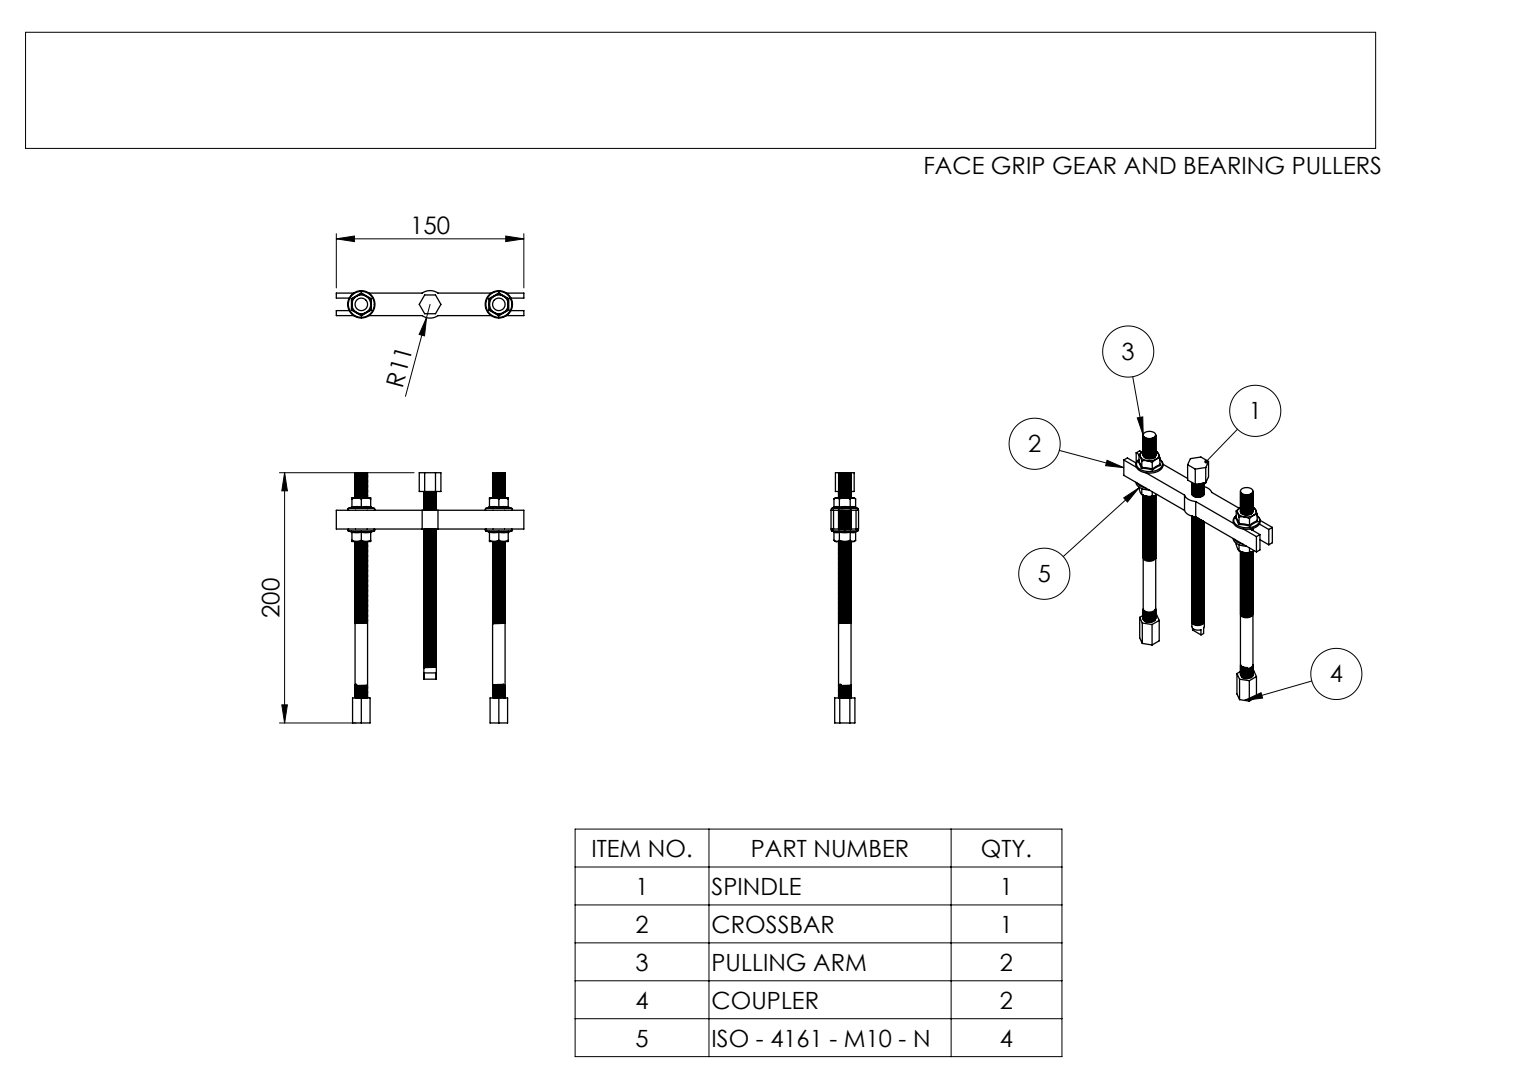
ISO-10303-21;
HEADER;
FILE_DESCRIPTION (('STEP AP214'),
    '1' );
FILE_NAME ('MAS-184',
    '2026-10-25T05:52:03',
    ( '' ),
    ( '' ),
    'SwSTEP 2.0',
    'SolidWorks 2026',
    '' );
FILE_SCHEMA (( 'AUTOMOTIVE_DESIGN' ));
ENDSEC;

DATA;
#1 = CARTESIAN_POINT ( 'NONE',  ( -5.000000000000000888, -163.4375000000000284, 2.071067811865474617 ) ) ;
#2 = AXIS2_PLACEMENT_3D ( 'NONE', #55045, #55372, #11606 ) ;
#3 = CARTESIAN_POINT ( 'NONE',  ( -59.29741812935640155, -128.8750000013656063, -2.196230717870135685 ) ) ;
#4 = ADVANCED_FACE ( 'NONE', ( #1643 ), #54385, .T. ) ;
#5 = CARTESIAN_POINT ( 'NONE',  ( -4.458734124999998549, -12.47916666530107221, 2.574251347313722516 ) ) ;
#6 = CARTESIAN_POINT ( 'NONE',  ( 2.229367062499998831, -45.89583333196774362, -3.861377020970580887 ) ) ;
#7 = ADVANCED_FACE ( 'NONE', ( #40534 ), #45685, .T. ) ;
#8 = ADVANCED_FACE ( 'NONE', ( #45365 ), #55019, .T. ) ;
#9 = CARTESIAN_POINT ( 'NONE',  ( -2.499999999999996447, -7.708333330602144429, 4.330127018922195425 ) ) ;
#10 = CARTESIAN_POINT ( 'NONE',  ( -4.458734124999999437, -146.9375000013656063, -5.460374474430324690E-16 ) ) ;
#11 = CARTESIAN_POINT ( 'NONE',  ( -4.458734124999999437, -91.56249999863440792, 0.000000000000000000 ) ) ;
#12 = CARTESIAN_POINT ( 'NONE',  ( 3.061616997868383141E-16, -166.8750000027312126, -5.000000000000000000 ) ) ;
#13 = ORIENTED_EDGE ( 'NONE', *, *, #42928, .F. ) ;
#14 = CARTESIAN_POINT ( 'NONE',  ( 4.330127018922154569, 30.00000000000000000, -7.499999999999971578 ) ) ;
#15 = CARTESIAN_POINT ( 'NONE',  ( -6.972266317189433020E-16, -69.12499999726880162, -5.000000000000000000 ) ) ;
#16 = CARTESIAN_POINT ( 'NONE',  ( -60.14911071818854538, -150.1875000027311842, 1.666127454062681368 ) ) ;
#17 = CARTESIAN_POINT ( 'NONE',  ( -6.972266317189433020E-16, -38.25000000000000000, -5.000000000000000000 ) ) ;
#18 = EDGE_LOOP ( 'NONE', ( #47508, #46479, #24387, #28082 ) ) ;
#19 = CARTESIAN_POINT ( 'NONE',  ( -2.229367062499996610, 0.8541666680322613781, 3.861377020970582219 ) ) ;
#20 = CARTESIAN_POINT ( 'NONE',  ( 0.000000000000000000, -120.0000000000000000, 0.000000000000000000 ) ) ;
#21 = CARTESIAN_POINT ( 'NONE',  ( -3.152548672688508926E-16, -17.81249999863440792, -5.148502694627439702 ) ) ;
#22 = EDGE_CURVE ( 'NONE', #55212, #17569, #39568, .T. ) ;
#23 = CARTESIAN_POINT ( 'NONE',  ( -5.000000000000000000, -51.00000000000000711, 0.000000000000000000 ) ) ;
#24 = CARTESIAN_POINT ( 'NONE',  ( -3.152548672688508926E-16, -0.5624999986344053626, -5.148502694627439702 ) ) ;
#25 = LINE ( 'NONE', #58862, #59314 ) ;
#26 = CARTESIAN_POINT ( 'NONE',  ( -8.190561711645485556E-16, -153.6875000013656063, 4.458734124999999437 ) ) ;
#27 =( BOUNDED_CURVE ( )  B_SPLINE_CURVE ( 2, ( #54507, #43875, #30044, #63521, #19445, #58375, #54824, #39058, #10756 ),
 .UNSPECIFIED., .F., .F. ) 
 B_SPLINE_CURVE_WITH_KNOTS ( ( 3, 2, 2, 2, 3 ),
 ( 0.2339285714285714302, 0.2345238095238095233, 0.2357142857142857095, 0.2369047619047618958, 0.2374999999999999889 ),
 .UNSPECIFIED. ) 
 CURVE ( )  GEOMETRIC_REPRESENTATION_ITEM ( )  RATIONAL_B_SPLINE_CURVE ( ( 0.9330127018922194093, 0.9330127018922194093, 1.000000000000000000, 0.8660254037844387076, 1.000000000000000000, 0.8660254037844387076, 1.000000000000000000, 0.9330127018922194093, 0.9330127018922194093 ) ) 
 REPRESENTATION_ITEM ( '' )  );
#28 = CARTESIAN_POINT ( 'NONE',  ( 2.229367062500001939, 22.77083333469892423, 3.861377020970579999 ) ) ;
#29 = ORIENTED_EDGE ( 'NONE', *, *, #3156, .T. ) ;
#30 = CARTESIAN_POINT ( 'NONE',  ( -2.229367062499996610, -99.14583333196773651, 3.861377020970582219 ) ) ;
#31 = CARTESIAN_POINT ( 'NONE',  ( -2.499999999999996447, -74.83333333333332860, 4.330127018922195425 ) ) ;
#32 = CARTESIAN_POINT ( 'NONE',  ( -5.000000000000000000, -103.9583333306021444, -2.886751345948128211 ) ) ;
#33 = CARTESIAN_POINT ( 'NONE',  ( -2.229367062499996610, -13.14583333196774007, 3.861377020970582219 ) ) ;
#34 = DIRECTION ( 'NONE',  ( 0.000000000000000000, 0.000000000000000000, 1.000000000000000000 ) ) ;
#35 = CARTESIAN_POINT ( 'NONE',  ( 2.499999999999998668, 29.66666666666666430, -4.330127018922193649 ) ) ;
#36 = CARTESIAN_POINT ( 'NONE',  ( 1.975475456537005874E-15, -87.75000000000001421, 5.000000000000000000 ) ) ;
#37 = CARTESIAN_POINT ( 'NONE',  ( -3.535250795749689387E-16, -41.12499999726880162, -5.773502691896257311 ) ) ;
#38 = CARTESIAN_POINT ( 'NONE',  ( -7.500000000000007105, 4.330127018922190096, -7.564335161054478895 ) ) ;
#39 = CARTESIAN_POINT ( 'NONE',  ( -4.458734124999999437, 14.68750000136559386, 0.000000000000000000 ) ) ;
#40 = CARTESIAN_POINT ( 'NONE',  ( 3.749999999999999112, -6.495190528383302464, -6.991905250253757309 ) ) ;
#41 = VERTEX_POINT ( 'NONE', #30888 ) ;
#42 = CARTESIAN_POINT ( 'NONE',  ( 4.458734124999999437, 16.18750000136559564, -5.460374474430324690E-16 ) ) ;
#43 = CARTESIAN_POINT ( 'NONE',  ( -4.458734124999999437, -60.31249999863440081, 0.000000000000000000 ) ) ;
#44 = AXIS2_PLACEMENT_3D ( 'NONE', #51313, #36828, #41317 ) ;
#45 = CARTESIAN_POINT ( 'NONE',  ( -4.458734124999999437, -10.64583333196773829, -2.574251347313719407 ) ) ;
#46 = CARTESIAN_POINT ( 'NONE',  ( 5.000000000000000888, -109.4583333306021444, 2.886751345948126879 ) ) ;
#47 = CARTESIAN_POINT ( 'NONE',  ( -5.000000000000000000, 6.999999999999999112, 0.000000000000000000 ) ) ;
#48 = CARTESIAN_POINT ( 'NONE',  ( 1.846868145590735200, -169.2500000013655779, -4.458734125000000326 ) ) ;
#49 = CARTESIAN_POINT ( 'NONE',  ( 1.339745962155612702, -63.16965819600734022, -5.000000000000000000 ) ) ;
#50 = AXIS2_PLACEMENT_3D ( 'NONE', #21966, #51867, #12316 ) ;
#51 = CARTESIAN_POINT ( 'NONE',  ( -4.458734124999998549, -53.22916666530107932, 2.574251347313722516 ) ) ;
#52 = CARTESIAN_POINT ( 'NONE',  ( 5.000000000000000000, -87.29166666393548724, -2.886751345948129988 ) ) ;
#53 = CARTESIAN_POINT ( 'NONE',  ( 4.458734124999999437, -32.81249999863440792, -5.460374474430324690E-16 ) ) ;
#54 = CARTESIAN_POINT ( 'NONE',  ( 4.336808689942017736E-16, 8.660254037844390851, -1.000000000000000888 ) ) ;
#55 = CARTESIAN_POINT ( 'NONE',  ( 0.000000000000000000, -170.0000000000000000, 5.000000000000000000 ) ) ;
#56 = CARTESIAN_POINT ( 'NONE',  ( -2.499999999999996447, -107.7083333306021444, 4.330127018922195425 ) ) ;
#57 = CARTESIAN_POINT ( 'NONE',  ( -1.846868145590734756, -152.3750000013655779, -4.458734124999999437 ) ) ;
#58 = CARTESIAN_POINT ( 'NONE',  ( -5.000000000000000000, -40.08333333333332860, -2.886751345948128211 ) ) ;
#59 = CARTESIAN_POINT ( 'NONE',  ( 5.000000000000000000, -46.50000000000000000, -6.123233995736766282E-16 ) ) ;
#60 = DIRECTION ( 'NONE',  ( -0.000000000000000000, 1.000000000000000000, -0.000000000000000000 ) ) ;
#61 = ORIENTED_EDGE ( 'NONE', *, *, #4808, .T. ) ;
#62 = CARTESIAN_POINT ( 'NONE',  ( -4.458734124999999437, -103.3958333319677365, -2.574251347313719407 ) ) ;
#63 = CARTESIAN_POINT ( 'NONE',  ( -4.458734124999999437, 1.437500001365592972, 0.000000000000000000 ) ) ;
#64 = DIRECTION ( 'NONE',  ( 0.000000000000000000, 0.000000000000000000, 1.000000000000000000 ) ) ;
#65 = CARTESIAN_POINT ( 'NONE',  ( 5.000000000000000000, -2.500000000000002220, -6.123233995736766282E-16 ) ) ;
#66 = CARTESIAN_POINT ( 'NONE',  ( 4.458734125000000326, -68.89583333196773651, 2.574251347313718519 ) ) ;
#67 = CARTESIAN_POINT ( 'NONE',  ( -6.972266317189433020E-16, -49.24999999999999289, -5.000000000000000000 ) ) ;
#68 = CARTESIAN_POINT ( 'NONE',  ( -2.499999999999996447, 0.2916666693978525737, 4.330127018922195425 ) ) ;
#70 = ORIENTED_EDGE ( 'NONE', *, *, #62981, .F. ) ;
#69 = CARTESIAN_POINT ( 'NONE',  ( -3.152548672688508926E-16, -36.56249999863441502, -5.148502694627439702 ) ) ;
#71 = CYLINDRICAL_SURFACE ( 'NONE', #27152, 5.000000000000000000 ) ;
#72 = CARTESIAN_POINT ( 'NONE',  ( 1.975475456537005874E-15, 5.250000000000000000, 5.000000000000000000 ) ) ;
#73 = CARTESIAN_POINT ( 'NONE',  ( 2.500000000000002220, -47.66666666666666430, 4.330127018922192761 ) ) ;
#75 = CARTESIAN_POINT ( 'NONE',  ( 2.229367062499998831, -23.89583333196773651, -3.861377020970580887 ) ) ;
#74 = CARTESIAN_POINT ( 'NONE',  ( 5.000000000000000000, -46.29166666393545881, -2.886751345948130876 ) ) ;
#76 = CARTESIAN_POINT ( 'NONE',  ( 1.464175926609780648E-14, 21.87500000273118062, -5.000000000000000000 ) ) ;
#77 = CARTESIAN_POINT ( 'NONE',  ( -4.458734124999999437, -71.39583333196773651, -2.574251347313719407 ) ) ;
#78 =( BOUNDED_CURVE ( )  B_SPLINE_CURVE ( 2, ( #57244, #32782, #8347, #47568, #3519, #57557, #53655, #9590, #43673 ),
 .UNSPECIFIED., .F., .F. ) 
 B_SPLINE_CURVE_WITH_KNOTS ( ( 3, 2, 2, 2, 3 ),
 ( 0.6562500000000000000, 0.6569444444444444420, 0.6583333333333333259, 0.6597222222222222099, 0.6604166666666666519 ),
 .UNSPECIFIED. ) 
 CURVE ( )  GEOMETRIC_REPRESENTATION_ITEM ( )  RATIONAL_B_SPLINE_CURVE ( ( 0.9330127018922194093, 0.9330127018922194093, 1.000000000000000000, 0.8660254037844387076, 1.000000000000000000, 0.8660254037844387076, 1.000000000000000000, 0.9330127018922194093, 0.9330127018922194093 ) ) 
 REPRESENTATION_ITEM ( '' )  );
#79 = CARTESIAN_POINT ( 'NONE',  ( 4.458734124999999437, -144.7500000013656063, 1.846868145590737864 ) ) ;
#80 = CARTESIAN_POINT ( 'NONE',  ( 2.229367062499998831, -80.64583333196773651, -3.861377020970580887 ) ) ;
#81 = CARTESIAN_POINT ( 'NONE',  ( -50.70258187064364108, -139.3750000013656063, 2.196230717870141014 ) ) ;
#82 = CARTESIAN_POINT ( 'NONE',  ( -2.229367062500000163, -28.72916666530107221, -3.861377020970580443 ) ) ;
#83 = CARTESIAN_POINT ( 'NONE',  ( 5.000000000000000888, -73.45833333060214443, 2.886751345948126879 ) ) ;
#85 = ORIENTED_EDGE ( 'NONE', *, *, #22562, .F. ) ;
#84 = ADVANCED_FACE ( 'NONE', ( #59208 ), #45044, .T. ) ;
#86 = ADVANCED_FACE ( 'NONE', ( #1332 ), #40849, .F. ) ;
#87 = CARTESIAN_POINT ( 'NONE',  ( 0.000000000000000000, -170.0000000000000000, 0.000000000000000000 ) ) ;
#88 = ORIENTED_EDGE ( 'NONE', *, *, #56635, .F. ) ;
#89 = CARTESIAN_POINT ( 'NONE',  ( -2.229367062500000163, -75.72916666530106511, -3.861377020970580443 ) ) ;
#90 = CARTESIAN_POINT ( 'NONE',  ( 0.000000000000000000, -120.0000000000000000, 5.000000000000000000 ) ) ;
#91 = EDGE_CURVE ( 'NONE', #38750, #62586, #59395, .T. ) ;
#92 = EDGE_LOOP ( 'NONE', ( #43267, #11517, #3797, #45500 ) ) ;
#93 = MECHANICAL_DESIGN_GEOMETRIC_PRESENTATION_REPRESENTATION (  '', ( #59644 ), #40104 ) ;
#94 = CARTESIAN_POINT ( 'NONE',  ( -54.60164318462004474, -140.3750000000000284, -4.984105922594373794 ) ) ;
#95 = EDGE_CURVE ( 'NONE', #8105, #59664, #19555, .T. ) ;
#96 = CARTESIAN_POINT ( 'NONE',  ( -5.000000000000000000, -83.08333333333332860, -2.886751345948128211 ) ) ;
#97 = CARTESIAN_POINT ( 'NONE',  ( -4.458734124999999437, -59.56249999863440081, 0.000000000000000000 ) ) ;
#98 = EDGE_CURVE ( 'NONE', #46757, #28361, #15466, .T. ) ;
#99 = CARTESIAN_POINT ( 'NONE',  ( -2.229367062499996610, 2.604166668032259491, 3.861377020970582219 ) ) ;
#100 = VERTEX_POINT ( 'NONE', #15137 ) ;
#101 = ADVANCED_FACE ( 'NONE', ( #35084 ), #10624, .T. ) ;
#102 = CARTESIAN_POINT ( 'NONE',  ( -5.000000000000000000, -19.99999999999999645, 0.000000000000000000 ) ) ;
#103 = CARTESIAN_POINT ( 'NONE',  ( -6.972266317189433020E-16, -41.12499999726880162, -5.000000000000000000 ) ) ;
#104 = ADVANCED_FACE ( 'NONE', ( #49860 ), #20614, .F. ) ;
#105 = CARTESIAN_POINT ( 'NONE',  ( 2.229367062500001939, 13.02083333469892779, 3.861377020970579999 ) ) ;
#106 = CARTESIAN_POINT ( 'NONE',  ( -58.39396692619412477, -139.4375000013656063, 2.891590998281057701 ) ) ;
#107 = CARTESIAN_POINT ( 'NONE',  ( 5.000000000000000888, -32.58333333333333570, 2.886751345948126879 ) ) ;
#108 = CARTESIAN_POINT ( 'NONE',  ( -4.458734124999999437, -165.9375000013655779, -5.460374474430324690E-16 ) ) ;
#110 = ADVANCED_FACE ( 'NONE', ( #11584 ), #11897, .T. ) ;
#109 = ORIENTED_EDGE ( 'NONE', *, *, #27518, .F. ) ;
#111 = CARTESIAN_POINT ( 'NONE',  ( 2.229367062500001939, -80.97916666530106511, 3.861377020970579999 ) ) ;
#112 = EDGE_CURVE ( 'NONE', #57087, #7190, #37304, .T. ) ;
#113 = CARTESIAN_POINT ( 'NONE',  ( 1.975475456537005874E-15, -0.6249999972688137229, 5.000000000000000000 ) ) ;
#114 = CARTESIAN_POINT ( 'NONE',  ( -2.229367062499996610, 0.8541666680322613781, 3.861377020970582219 ) ) ;
#115 = CARTESIAN_POINT ( 'NONE',  ( 5.000000000000000000, -83.41666666666667140, -2.886751345948129988 ) ) ;
#116 = CARTESIAN_POINT ( 'NONE',  ( -4.999999999999998224, 2.083333333333333037, 2.886751345948131764 ) ) ;
#117 = CARTESIAN_POINT ( 'NONE',  ( 4.458734125000001214, -63.14583333196774362, 2.574251347313718519 ) ) ;
#118 = CARTESIAN_POINT ( 'NONE',  ( 5.000000000000000000, -24.37499999726881228, -6.123233995736766282E-16 ) ) ;
#119 = CARTESIAN_POINT ( 'NONE',  ( 3.061616997868383141E-16, -154.8750000027311842, -5.000000000000000000 ) ) ;
#120 = CARTESIAN_POINT ( 'NONE',  ( 4.458734124999998549, 28.27083333469892779, -2.574251347313721627 ) ) ;
#121 = CARTESIAN_POINT ( 'NONE',  ( -5.000000000000000000, -64.87499999726881583, 0.000000000000000000 ) ) ;
#122 = CARTESIAN_POINT ( 'NONE',  ( -6.972266317189433020E-16, -58.24999999999999289, -5.000000000000000000 ) ) ;
#123 = CARTESIAN_POINT ( 'NONE',  ( -2.229367062499996610, -44.14583333196774362, 3.861377020970582219 ) ) ;
#124 = CARTESIAN_POINT ( 'NONE',  ( 4.458734124999998549, -31.97916666530107577, -2.574251347313721627 ) ) ;
#125 = CARTESIAN_POINT ( 'NONE',  ( 4.458734124999998549, 8.020833334698926009, -2.574251347313721627 ) ) ;
#126 = FACE_OUTER_BOUND ( 'NONE', #12177, .T. ) ;
#127 = CARTESIAN_POINT ( 'NONE',  ( -2.499999999999996447, 28.16666666666666785, 4.330127018922195425 ) ) ;
#128 = CARTESIAN_POINT ( 'NONE',  ( -9.184850993605147944E-16, -149.3750000027312126, 5.000000000000000000 ) ) ;
#129 = CARTESIAN_POINT ( 'NONE',  ( -6.972266317189433020E-16, -50.24999999999999289, -5.000000000000000000 ) ) ;
#130 = CARTESIAN_POINT ( 'NONE',  ( 4.458734124999998549, -37.72916666530107221, -2.574251347313721627 ) ) ;
#131 = CARTESIAN_POINT ( 'NONE',  ( -2.500000000000000444, -73.04166666393548724, -4.330127018922193649 ) ) ;
#132 = CARTESIAN_POINT ( 'NONE',  ( -51.60603307380591787, -145.1875000013656063, -2.891590998281053704 ) ) ;
#133 = CARTESIAN_POINT ( 'NONE',  ( -2.071067811865475061, -143.6875000000000284, -5.000000000000000888 ) ) ;
#134 = CARTESIAN_POINT ( 'NONE',  ( 9.457646018065525792E-16, -74.31249999863440792, 5.148502694627439702 ) ) ;
#135 = CARTESIAN_POINT ( 'NONE',  ( 4.458734124999999437, -165.6250000013656063, -1.846868145590734978 ) ) ;
#136 = CARTESIAN_POINT ( 'NONE',  ( 2.229367062499998831, -35.64583333196772941, -3.861377020970580887 ) ) ;
#137 = CYLINDRICAL_SURFACE ( 'NONE', #42021, 5.000000000000000000 ) ;
#138 = DIRECTION ( 'NONE',  ( 0.000000000000000000, 0.000000000000000000, 1.000000000000000000 ) ) ;
#139 = CARTESIAN_POINT ( 'NONE',  ( -5.000000000000000000, -20.08333333333333215, -2.886751345948128211 ) ) ;
#140 = CARTESIAN_POINT ( 'NONE',  ( 4.458734124999999437, -143.4375000013656063, 0.000000000000000000 ) ) ;
#141 = VERTEX_POINT ( 'NONE', #56933 ) ;
#142 = CARTESIAN_POINT ( 'NONE',  ( 4.458734125000001214, 28.85416666803225993, 2.574251347313718519 ) ) ;
#143 = VERTEX_POINT ( 'NONE', #12854 ) ;
#144 = CARTESIAN_POINT ( 'NONE',  ( -2.229367062499996610, -62.39583333196774362, 3.861377020970582219 ) ) ;
#145 = CARTESIAN_POINT ( 'NONE',  ( 5.000000000000000000, 22.70833333606451632, -2.886751345948129988 ) ) ;
#146 = CARTESIAN_POINT ( 'NONE',  ( 1.975475456537005874E-15, 4.375000002731185056, 5.000000000000000000 ) ) ;
#147 = CARTESIAN_POINT ( 'NONE',  ( -5.000000000000000000, 17.91666666666666430, -2.886751345948128211 ) ) ;
#148 = CARTESIAN_POINT ( 'NONE',  ( -3.152548672688508926E-16, -50.56249999863440792, -5.148502694627439702 ) ) ;
#149 = CARTESIAN_POINT ( 'NONE',  ( -4.458734124999999437, -8.395833331967736513, -2.574251347313719407 ) ) ;
#150 = CARTESIAN_POINT ( 'NONE',  ( 0.000000000000000000, 15.00000000000000000, 0.000000000000000000 ) ) ;
#151 = CARTESIAN_POINT ( 'NONE',  ( -4.999999999999998224, -40.79166666393548724, 2.886751345948131764 ) ) ;
#152 = CARTESIAN_POINT ( 'NONE',  ( -1.339745962155610925, 0.2053418012614791066, 5.000000000000000000 ) ) ;
#153 = CARTESIAN_POINT ( 'NONE',  ( 5.000000000000000000, -53.37499999726881583, -6.123233995736766282E-16 ) ) ;
#155 = CARTESIAN_POINT ( 'NONE',  ( 4.458734124999999437, -23.81249999863440436, -5.460374474430324690E-16 ) ) ;
#154 = CARTESIAN_POINT ( 'NONE',  ( -6.972266317189433020E-16, 0.7499999999999996669, -5.000000000000000000 ) ) ;
#156 = CARTESIAN_POINT ( 'NONE',  ( -1.339745962155613812, -72.08034179853027013, -5.000000000000000000 ) ) ;
#157 = CARTESIAN_POINT ( 'NONE',  ( -3.152548672688508926E-16, -54.56249999863439371, -5.148502694627439702 ) ) ;
#158 = CARTESIAN_POINT ( 'NONE',  ( -1.846868145590737420, -157.0000000013655779, 4.458734124999999437 ) ) ;
#159 =( BOUNDED_CURVE ( )  B_SPLINE_CURVE ( 2, ( #57542, #18604, #23441, #33707, #13470, #33086, #62682, #47554, #43658 ),
 .UNSPECIFIED., .F., .F. ) 
 B_SPLINE_CURVE_WITH_KNOTS ( ( 3, 2, 2, 2, 3 ),
 ( 0.8089285714285714413, 0.8095238095238095344, 0.8107142857142857206, 0.8119047619047619069, 0.8125000000000000000 ),
 .UNSPECIFIED. ) 
 CURVE ( )  GEOMETRIC_REPRESENTATION_ITEM ( )  RATIONAL_B_SPLINE_CURVE ( ( 0.9330127018922194093, 0.9330127018922194093, 1.000000000000000000, 0.8660254037844387076, 1.000000000000000000, 0.8660254037844387076, 1.000000000000000000, 0.9330127018922194093, 0.9330127018922194093 ) ) 
 REPRESENTATION_ITEM ( '' )  );
#160 = CARTESIAN_POINT ( 'NONE',  ( -2.500000000000000444, -56.04166666393548013, -4.330127018922193649 ) ) ;
#161 = EDGE_LOOP ( 'NONE', ( #40738, #29551, #10837, #16509 ) ) ;
#162 = CARTESIAN_POINT ( 'NONE',  ( -3.152548672688508926E-16, 6.187500001365593860, -5.148502694627439702 ) ) ;
#163 = ORIENTED_EDGE ( 'NONE', *, *, #35025, .F. ) ;
#165 = FACE_OUTER_BOUND ( 'NONE', #54429, .T. ) ;
#164 = CARTESIAN_POINT ( 'NONE',  ( 75.00000000000002842, 15.00000000000000000, -5.000000000000000000 ) ) ;
#166 = CARTESIAN_POINT ( 'NONE',  ( 2.730187237215162345E-16, -156.1875000013655779, -4.458734124999999437 ) ) ;
#167 = ORIENTED_EDGE ( 'NONE', *, *, #56942, .T. ) ;
#168 = CARTESIAN_POINT ( 'NONE',  ( 5.000000000000000000, -87.29166666393547303, -2.886751345948130876 ) ) ;
#169 = CARTESIAN_POINT ( 'NONE',  ( -50.18089887299979068, -133.6875000000000568, 2.462841084822635640 ) ) ;
#170 = CARTESIAN_POINT ( 'NONE',  ( 0.000000000000000000, -170.0000000000000000, 0.000000000000000000 ) ) ;
#171 = CARTESIAN_POINT ( 'NONE',  ( -4.458734124999999437, -45.56249999863440081, 0.000000000000000000 ) ) ;
#172 = EDGE_LOOP ( 'NONE', ( #31219, #33556, #46683, #22321 ) ) ;
#173 = CARTESIAN_POINT ( 'NONE',  ( 1.339745962155615144, 9.419658201469706782, 4.999999999999999112 ) ) ;
#174 = CARTESIAN_POINT ( 'NONE',  ( -3.152548672688508926E-16, 18.43750000136559564, -5.148502694627439702 ) ) ;
#175 = CARTESIAN_POINT ( 'NONE',  ( -5.000000000000000000, -156.6250000027311842, -6.123233995736766282E-16 ) ) ;
#176 = VERTEX_POINT ( 'NONE', #46964 ) ;
#177 = CARTESIAN_POINT ( 'NONE',  ( 9.457646018065525792E-16, -89.31249999863440792, 5.148502694627439702 ) ) ;
#178 = CARTESIAN_POINT ( 'NONE',  ( -60.14911071818854538, -125.1875000027312126, 1.666127454062681368 ) ) ;
#179 = CARTESIAN_POINT ( 'NONE',  ( -3.535533905932737309, -165.6250000000000284, -3.535533905932738197 ) ) ;
#180 = CARTESIAN_POINT ( 'NONE',  ( 75.00000000000000000, 15.00000000000000000, 8.999999999999998224 ) ) ;
#181 = CARTESIAN_POINT ( 'NONE',  ( 1.975475456537005874E-15, -52.62499999726880873, 5.000000000000000000 ) ) ;
#182 = CARTESIAN_POINT ( 'NONE',  ( 9.457646018065525792E-16, -58.06249999863440081, 5.148502694627439702 ) ) ;
#183 = DIRECTION ( 'NONE',  ( -0.000000000000000000, 1.000000000000000000, -0.000000000000000000 ) ) ;
#184 = CARTESIAN_POINT ( 'NONE',  ( -2.229367062499996610, 16.85416666803225993, 3.861377020970582219 ) ) ;
#185 = CARTESIAN_POINT ( 'NONE',  ( -5.000000000000000000, -78.95833333060213022, -2.886751345948128211 ) ) ;
#186 = ADVANCED_FACE ( 'NONE', ( #26707 ), #62074, .T. ) ;
#187 = CARTESIAN_POINT ( 'NONE',  ( 4.458734124999998549, -51.97916666530107221, -2.574251347313721627 ) ) ;
#188 = CARTESIAN_POINT ( 'NONE',  ( 5.000000000000000000, -11.37499999726881583, -6.123233995736766282E-16 ) ) ;
#189 = CARTESIAN_POINT ( 'NONE',  ( 2.500000000000002220, -42.54166666393548013, 4.330127018922192761 ) ) ;
#190 = CARTESIAN_POINT ( 'NONE',  ( -1.339745962155613812, -46.08034179853028434, -5.000000000000000000 ) ) ;
#191 = CARTESIAN_POINT ( 'NONE',  ( -2.500000000000000444, -74.16666666666665719, -4.330127018922193649 ) ) ;
#192 = CARTESIAN_POINT ( 'NONE',  ( -4.458734124999997661, -109.2291666653010509, 2.574251347313722516 ) ) ;
#193 = CARTESIAN_POINT ( 'NONE',  ( 4.458734124999998549, -12.97916666530107399, -2.574251347313721627 ) ) ;
#194 = ORIENTED_EDGE ( 'NONE', *, *, #3576, .F. ) ;
#195 = CARTESIAN_POINT ( 'NONE',  ( 1.339745962155608039, 23.29465819873852084, 5.000000000000003553 ) ) ;
#196 = CARTESIAN_POINT ( 'NONE',  ( -2.229367062500000163, -96.47916666530105090, -3.861377020970580443 ) ) ;
#197 = CARTESIAN_POINT ( 'NONE',  ( 5.000000000000000000, -162.1875000027311842, 2.071067811865478614 ) ) ;
#198 = CARTESIAN_POINT ( 'NONE',  ( 9.457646018065525792E-16, -97.31249999863440792, 5.148502694627439702 ) ) ;
#199 = FACE_OUTER_BOUND ( 'NONE', #51701, .T. ) ;
#200 = CARTESIAN_POINT ( 'NONE',  ( -2.499999999999996447, -58.70833333060214443, 4.330127018922195425 ) ) ;
#201 = CARTESIAN_POINT ( 'NONE',  ( -6.901579824520442941, 4.675625068323816080, -0.7022220667781327030 ) ) ;
#202 = CARTESIAN_POINT ( 'NONE',  ( -53.51423613279429503, -126.2500000013656063, 4.591703134518082763 ) ) ;
#203 = CARTESIAN_POINT ( 'NONE',  ( -52.10840900171896806, -147.1875000013656063, 3.393966926194110556 ) ) ;
#204 = CARTESIAN_POINT ( 'NONE',  ( -2.229367062500000163, -16.47916666530107577, -3.861377020970580443 ) ) ;
#205 = CARTESIAN_POINT ( 'NONE',  ( -3.152548672688508926E-16, 4.187500001365595637, -5.148502694627439702 ) ) ;
#206 = CARTESIAN_POINT ( 'NONE',  ( 9.457646018065525792E-16, -61.31249999863440792, 5.148502694627439702 ) ) ;
#207 = CARTESIAN_POINT ( 'NONE',  ( -6.972266317189433020E-16, -48.12499999726880873, -5.000000000000000000 ) ) ;
#208 = CARTESIAN_POINT ( 'NONE',  ( 9.457646018065525792E-16, -14.06249999863440436, 5.148502694627439702 ) ) ;
#209 = CARTESIAN_POINT ( 'NONE',  ( 2.499999999999998668, -71.33333333333332860, -4.330127018922193649 ) ) ;
#210 = CARTESIAN_POINT ( 'NONE',  ( -9.184850993605147944E-16, -153.2500000000000000, 5.000000000000000000 ) ) ;
#211 = CARTESIAN_POINT ( 'NONE',  ( -2.500000000000000444, -4.166666666666666075, -4.330127018922193649 ) ) ;
#212 = ORIENTED_EDGE ( 'NONE', *, *, #23608, .F. ) ;
#213 = CARTESIAN_POINT ( 'NONE',  ( -2.229367062499996610, -46.39583333196774362, 3.861377020970582219 ) ) ;
#214 = CARTESIAN_POINT ( 'NONE',  ( -55.35523342533222291, -125.5625000013655921, 4.444560631937231499 ) ) ;
#215 = CARTESIAN_POINT ( 'NONE',  ( -5.276498195231978272, 6.073236878017963747, -7.633618187056680604 ) ) ;
#216 = DIRECTION ( 'NONE',  ( -0.000000000000000000, 1.000000000000000000, -0.000000000000000000 ) ) ;
#217 = CARTESIAN_POINT ( 'NONE',  ( 2.229367062500001939, -84.97916666530107932, 3.861377020970579999 ) ) ;
#218 = CARTESIAN_POINT ( 'NONE',  ( -2.229367062499996610, 19.60416666803225993, 3.861377020970582219 ) ) ;
#219 = CARTESIAN_POINT ( 'NONE',  ( -2.229367062499996610, 11.85416666803225993, 3.861377020970582219 ) ) ;
#220 = CARTESIAN_POINT ( 'NONE',  ( -4.999999999999998224, -88.79166666393548724, 2.886751345948131764 ) ) ;
#221 = CYLINDRICAL_SURFACE ( 'NONE', #8092, 5.000000000000000000 ) ;
#222 = CARTESIAN_POINT ( 'NONE',  ( -2.229367062500000163, -88.72916666530106511, -3.861377020970580443 ) ) ;
#223 = CARTESIAN_POINT ( 'NONE',  ( -2.229367062500000163, 20.27083333469892779, -3.861377020970580443 ) ) ;
#224 = CARTESIAN_POINT ( 'NONE',  ( -3.535250795749689387E-16, -77.25000000000000000, -5.773502691896257311 ) ) ;
#225 = CARTESIAN_POINT ( 'NONE',  ( 5.000000000000000000, 8.708333336064518093, -2.886751345948129988 ) ) ;
#226 = ORIENTED_EDGE ( 'NONE', *, *, #26912, .F. ) ;
#227 = DIRECTION ( 'NONE',  ( 0.000000000000000000, 0.000000000000000000, 1.000000000000000000 ) ) ;
#228 = ORIENTED_EDGE ( 'NONE', *, *, #38170, .T. ) ;
#229 =( BOUNDED_CURVE ( )  B_SPLINE_CURVE ( 2, ( #7653, #61058, #50752, #27257, #26303, #46568, #45926, #60737, #46883 ),
 .UNSPECIFIED., .F., .F. ) 
 B_SPLINE_CURVE_WITH_KNOTS ( ( 3, 2, 2, 2, 3 ),
 ( 0.3562500000000000111, 0.3569444444444444531, 0.3583333333333333370, 0.3597222222222222210, 0.3604166666666666630 ),
 .UNSPECIFIED. ) 
 CURVE ( )  GEOMETRIC_REPRESENTATION_ITEM ( )  RATIONAL_B_SPLINE_CURVE ( ( 0.9330127018922194093, 0.9330127018922194093, 1.000000000000000000, 0.8660254037844387076, 1.000000000000000000, 0.8660254037844387076, 1.000000000000000000, 0.9330127018922194093, 0.9330127018922194093 ) ) 
 REPRESENTATION_ITEM ( '' )  );
#230 = CARTESIAN_POINT ( 'NONE',  ( 1.060575238724906964E-15, -36.75000000000000711, 5.773502691896257311 ) ) ;
#231 = CARTESIAN_POINT ( 'NONE',  ( 4.458734124999998549, -35.72916666530107221, -2.574251347313721627 ) ) ;
#232 = CARTESIAN_POINT ( 'NONE',  ( -3.535250795749689387E-16, -35.12499999726881583, -5.773502691896257311 ) ) ;
#234 = ORIENTED_EDGE ( 'NONE', *, *, #6265, .F. ) ;
#233 = CARTESIAN_POINT ( 'NONE',  ( -4.458734124999998549, -68.22916666530107932, 2.574251347313722516 ) ) ;
#235 = CARTESIAN_POINT ( 'NONE',  ( -59.44456063193725015, -149.8125000013656063, -0.3552334253322034230 ) ) ;
#236 = CARTESIAN_POINT ( 'NONE',  ( -3.152548672688508926E-16, -12.56249999863440081, -5.148502694627439702 ) ) ;
#238 = ORIENTED_EDGE ( 'NONE', *, *, #445, .F. ) ;
#237 = CARTESIAN_POINT ( 'NONE',  ( -3.152548672688508926E-16, -15.81249999863440436, -5.148502694627439702 ) ) ;
#239 = CARTESIAN_POINT ( 'NONE',  ( 2.500000000000002220, -83.66666666666667140, 4.330127018922192761 ) ) ;
#240 = CARTESIAN_POINT ( 'NONE',  ( -4.458734125000000326, -167.0000000013655779, -1.846868145590735644 ) ) ;
#241 = CARTESIAN_POINT ( 'NONE',  ( 2.229367062499998831, -55.89583333196773651, -3.861377020970580887 ) ) ;
#243 = CARTESIAN_POINT ( 'NONE',  ( 5.000000000000000000, -81.29166666393547303, -2.886751345948129988 ) ) ;
#242 = APPLICATION_CONTEXT ( 'automotive_design' ) ;
#245 = ORIENTED_EDGE ( 'NONE', *, *, #34105, .T. ) ;
#244 = LINE ( 'NONE', #10504, #18998 ) ;
#246 = CARTESIAN_POINT ( 'NONE',  ( -53.33387254593733928, -145.8125000000000284, 5.149110718188519620 ) ) ;
#247 = CARTESIAN_POINT ( 'NONE',  ( -4.458734124999998549, -29.47916666530106866, 2.574251347313722516 ) ) ;
#248 = VERTEX_POINT ( 'NONE', #17988 ) ;
#249 = PRODUCT_CONTEXT ( 'NONE', #29797, 'mechanical' ) ;
#250 = CARTESIAN_POINT ( 'NONE',  ( 1.846868145590736310, -167.8750000013656063, 4.458734124999999437 ) ) ;
#251 = CARTESIAN_POINT ( 'NONE',  ( 2.229367062500001939, -104.2291666653010651, 3.861377020970579999 ) ) ;
#252 = CYLINDRICAL_SURFACE ( 'NONE', #21504, 5.000000000000000000 ) ;
#253 = ORIENTED_EDGE ( 'NONE', *, *, #51599, .T. ) ;
#254 = CARTESIAN_POINT ( 'NONE',  ( -59.29741812935640155, -144.8750000013656063, -2.196230717870135685 ) ) ;
#255 = CARTESIAN_POINT ( 'NONE',  ( -49.85088928181150436, -137.6875000027312126, -1.666127454062680702 ) ) ;
#256 = CARTESIAN_POINT ( 'NONE',  ( -4.458734124999997661, -41.22916666530107932, 2.574251347313722516 ) ) ;
#257 = CARTESIAN_POINT ( 'NONE',  ( -1.846868145590734756, -147.3750000013656063, -4.458734124999999437 ) ) ;
#258 =( BOUNDED_CURVE ( )  B_SPLINE_CURVE ( 2, ( #61184, #52477, #22580, #23193, #34020, #53641, #56988, #29181, #48808 ),
 .UNSPECIFIED., .F., .F. ) 
 B_SPLINE_CURVE_WITH_KNOTS ( ( 3, 2, 2, 2, 3 ),
 ( 0.2267857142857142849, 0.2273809523809523780, 0.2285714285714285643, 0.2297619047619047505, 0.2303571428571428714 ),
 .UNSPECIFIED. ) 
 CURVE ( )  GEOMETRIC_REPRESENTATION_ITEM ( )  RATIONAL_B_SPLINE_CURVE ( ( 0.9330127018922194093, 0.9330127018922194093, 1.000000000000000000, 0.8660254037844387076, 1.000000000000000000, 0.8660254037844387076, 1.000000000000000000, 0.9330127018922178550, 0.9330127018922194093 ) ) 
 REPRESENTATION_ITEM ( '' )  );
#259 = CARTESIAN_POINT ( 'NONE',  ( 6.123233995736766282E-16, -170.0000000000000000, -5.000000000000000000 ) ) ;
#260 = CARTESIAN_POINT ( 'NONE',  ( 2.500000000000002220, 2.458333336064519870, 4.330127018922192761 ) ) ;
#261 = CARTESIAN_POINT ( 'NONE',  ( -3.152548672688508926E-16, -11.56249999863440792, -5.148502694627439702 ) ) ;
#262 = CARTESIAN_POINT ( 'NONE',  ( -4.458734124999999437, -101.5624999986344079, 0.000000000000000000 ) ) ;
#263 = ORIENTED_EDGE ( 'NONE', *, *, #11129, .F. ) ;
#264 = CARTESIAN_POINT ( 'NONE',  ( -4.458734125000001214, -141.1250000013655779, 1.846868145590734089 ) ) ;
#265 = CARTESIAN_POINT ( 'NONE',  ( 4.458734125000001214, -33.14583333196774362, 2.574251347313718519 ) ) ;
#266 = CARTESIAN_POINT ( 'NONE',  ( 1.060575238724906964E-15, 7.375000002731186832, 5.773502691896257311 ) ) ;
#267 = CARTESIAN_POINT ( 'NONE',  ( -49.85088928181150436, -153.5625000000000284, -1.666127454062680480 ) ) ;
#268 = CARTESIAN_POINT ( 'NONE',  ( -50.40829686548195099, -135.0000000013656347, -1.485763867205728284 ) ) ;
#269 = CARTESIAN_POINT ( 'NONE',  ( 4.458734125000001214, -75.14583333196775072, 2.574251347313718519 ) ) ;
#270 = DIRECTION ( 'NONE',  ( -0.000000000000000000, 1.000000000000000000, -0.000000000000000000 ) ) ;
#271 = CARTESIAN_POINT ( 'NONE',  ( 1.975475456537005874E-15, -69.74999999999998579, 5.000000000000000000 ) ) ;
#272 = CARTESIAN_POINT ( 'NONE',  ( -6.972266317189433020E-16, -58.12499999726880162, -5.000000000000000000 ) ) ;
#273 = CARTESIAN_POINT ( 'NONE',  ( 4.458734124999998549, 6.020833334698928674, -2.574251347313721627 ) ) ;
#274 = EDGE_LOOP ( 'NONE', ( #55468, #62906 ) ) ;
#275 = CARTESIAN_POINT ( 'NONE',  ( -6.972266317189433020E-16, 13.87500000273118594, -5.000000000000000000 ) ) ;
#276 = CARTESIAN_POINT ( 'NONE',  ( 1.339745962155615144, 9.294658198738520838, 4.999999999999999112 ) ) ;
#278 = CARTESIAN_POINT ( 'NONE',  ( -2.229367062499996610, -29.14583333196774007, 3.861377020970582219 ) ) ;
#277 = CARTESIAN_POINT ( 'NONE',  ( 5.000000000000000000, -96.41666666666664298, -2.886751345948129988 ) ) ;
#279 = CARTESIAN_POINT ( 'NONE',  ( -4.999999999999998224, -35.91666666666666430, 2.886751345948131764 ) ) ;
#280 = CARTESIAN_POINT ( 'NONE',  ( -3.152548672688508926E-16, -79.81249999863440792, -5.148502694627439702 ) ) ;
#281 = CARTESIAN_POINT ( 'NONE',  ( -4.458734124999999437, 16.43750000136559564, 0.000000000000000000 ) ) ;
#282 = CARTESIAN_POINT ( 'NONE',  ( 0.000000000000000000, -120.0000000000000000, 0.000000000000000000 ) ) ;
#283 = CARTESIAN_POINT ( 'NONE',  ( -59.59170313451811296, -138.5000000013656347, 1.485763867205729394 ) ) ;
#284 = CARTESIAN_POINT ( 'NONE',  ( -3.152548672688508926E-16, -3.562499998634408360, -5.148502694627439702 ) ) ;
#285 = CARTESIAN_POINT ( 'NONE',  ( 9.457646018065525792E-16, 21.68750000136559208, 5.148502694627439702 ) ) ;
#286 = CARTESIAN_POINT ( 'NONE',  ( 9.457646018065525792E-16, -42.31249999863440081, 5.148502694627439702 ) ) ;
#287 = DIRECTION ( 'NONE',  ( 0.000000000000000000, 0.000000000000000000, 1.000000000000000000 ) ) ;
#288 = CARTESIAN_POINT ( 'NONE',  ( -4.458734124999999437, 2.687500001365593860, 0.000000000000000000 ) ) ;
#289 = ORIENTED_EDGE ( 'NONE', *, *, #15037, .T. ) ;
#290 = CARTESIAN_POINT ( 'NONE',  ( 4.458734124999999437, -24.06249999863440436, -5.460374474430324690E-16 ) ) ;
#291 = CARTESIAN_POINT ( 'NONE',  ( 4.458734124999998549, -71.72916666530107932, -2.574251347313721627 ) ) ;
#292 = CARTESIAN_POINT ( 'NONE',  ( 1.060575238724906964E-15, -104.6249999972688158, 5.773502691896257311 ) ) ;
#293 = ADVANCED_FACE ( 'NONE', ( #61447 ), #37614, .T. ) ;
#294 = CARTESIAN_POINT ( 'NONE',  ( 4.458734125000001214, 25.10416666803225638, 2.574251347313718519 ) ) ;
#295 = CARTESIAN_POINT ( 'NONE',  ( -2.499999999999996447, 10.16666666666666785, 4.330127018922195425 ) ) ;
#296 = CARTESIAN_POINT ( 'NONE',  ( -4.330127018922205195, 45.00000000000000000, -7.499999999999943157 ) ) ;
#297 = CARTESIAN_POINT ( 'NONE',  ( -4.458734124999997661, -71.47916666530107932, 2.574251347313722516 ) ) ;
#298 = CARTESIAN_POINT ( 'NONE',  ( 1.060575238724906964E-15, -58.75000000000000000, 5.773502691896257311 ) ) ;
#299 = DIRECTION ( 'NONE',  ( -0.000000000000000000, 1.000000000000000000, -0.000000000000000000 ) ) ;
#300 = CARTESIAN_POINT ( 'NONE',  ( 2.499999999999998668, 27.79166666939785202, -4.330127018922193649 ) ) ;
#301 = ORIENTED_EDGE ( 'NONE', *, *, #22893, .T. ) ;
#302 = CARTESIAN_POINT ( 'NONE',  ( 2.499999999999998668, -67.33333333333332860, -4.330127018922193649 ) ) ;
#303 = CARTESIAN_POINT ( 'NONE',  ( 5.000000000000000000, -18.50000000000000355, -6.123233995736766282E-16 ) ) ;
#304 = CARTESIAN_POINT ( 'NONE',  ( -4.458734124999999437, -22.39583333196773651, -2.574251347313719407 ) ) ;
#305 = CARTESIAN_POINT ( 'NONE',  ( -2.229367062500000163, -81.47916666530106511, -3.861377020970580443 ) ) ;
#306 = CARTESIAN_POINT ( 'NONE',  ( 1.846868145590735200, -166.5000000013655779, -4.458734125000000326 ) ) ;
#307 = CARTESIAN_POINT ( 'NONE',  ( 1.060575238724906964E-15, -19.62499999726881583, 5.773502691896257311 ) ) ;
#309 = ORIENTED_EDGE ( 'NONE', *, *, #57908, .T. ) ;
#308 = CARTESIAN_POINT ( 'NONE',  ( 4.458734124999999437, -48.81249999863440792, -5.460374474430324690E-16 ) ) ;
#310 = CARTESIAN_POINT ( 'NONE',  ( -2.500000000000000444, -24.16666666666666430, -4.330127018922193649 ) ) ;
#311 = CARTESIAN_POINT ( 'NONE',  ( 5.000000000000000000, -98.50000000000000000, -6.123233995736766282E-16 ) ) ;
#313 = ORIENTED_EDGE ( 'NONE', *, *, #36524, .T. ) ;
#312 = CARTESIAN_POINT ( 'NONE',  ( -3.152548672688508926E-16, 3.187500001365594748, -5.148502694627439702 ) ) ;
#314 = CARTESIAN_POINT ( 'NONE',  ( -56.48576386720575471, -152.7500000013655779, -4.591703134518078322 ) ) ;
#315 = CARTESIAN_POINT ( 'NONE',  ( -2.500000000000000444, -64.16666666666665719, -4.330127018922193649 ) ) ;
#316 = CARTESIAN_POINT ( 'NONE',  ( -1.846868145590737420, -152.0000000013655779, 4.458734124999999437 ) ) ;
#317 = CARTESIAN_POINT ( 'NONE',  ( -3.152548672688508926E-16, -38.81249999863440081, -5.148502694627439702 ) ) ;
#318 = CARTESIAN_POINT ( 'NONE',  ( -6.972266317189433020E-16, -68.12499999726881583, -5.000000000000000000 ) ) ;
#319 = CARTESIAN_POINT ( 'NONE',  ( 5.000000000000000888, -161.9375000000000284, -2.071067811865475505 ) ) ;
#320 = FACE_OUTER_BOUND ( 'NONE', #3833, .T. ) ;
#321 = CARTESIAN_POINT ( 'NONE',  ( -57.19623071787017210, -127.6250000013656205, 4.297418129356382899 ) ) ;
#322 = CARTESIAN_POINT ( 'NONE',  ( 2.229367062499998831, -10.89583333196773829, -3.861377020970580887 ) ) ;
#323 = CARTESIAN_POINT ( 'NONE',  ( 4.458734124999998549, -45.97916666530106511, -2.574251347313721627 ) ) ;
#324 = CARTESIAN_POINT ( 'NONE',  ( -6.972266317189433020E-16, -8.124999997268814056, -5.000000000000000000 ) ) ;
#325 = CARTESIAN_POINT ( 'NONE',  ( -8.190561711645485556E-16, -149.6875000013656063, 4.458734124999999437 ) ) ;
#326 = CARTESIAN_POINT ( 'NONE',  ( -4.458734124999999437, -88.64583333196773651, -2.574251347313719407 ) ) ;
#327 = CARTESIAN_POINT ( 'NONE',  ( 6.123233995736766282E-16, -120.0000000000000000, -5.000000000000000000 ) ) ;
#328 = VERTEX_POINT ( 'NONE', #61131 ) ;
#329 = CARTESIAN_POINT ( 'NONE',  ( -6.972266317189433020E-16, -19.12499999726880873, -5.000000000000000000 ) ) ;
#330 = FACE_OUTER_BOUND ( 'NONE', #56792, .T. ) ;
#331 = CARTESIAN_POINT ( 'NONE',  ( -51.19402409849444524, -149.6250000027312126, -3.242614290531456334 ) ) ;
#332 = CARTESIAN_POINT ( 'NONE',  ( 5.000000000000000888, -29.45833333060214443, 2.886751345948126879 ) ) ;
#333 = ORIENTED_EDGE ( 'NONE', *, *, #57023, .T. ) ;
#334 =( BOUNDED_CURVE ( )  B_SPLINE_CURVE ( 2, ( #33009, #33633, #47175, #33318, #13071, #4059, #62915, #32690, #52322 ),
 .UNSPECIFIED., .F., .F. ) 
 B_SPLINE_CURVE_WITH_KNOTS ( ( 3, 2, 2, 2, 3 ),
 ( 0.05892857142857142738, 0.05952380952380952051, 0.06071428571428571369, 0.06190476190476190688, 0.06250000000000000000 ),
 .UNSPECIFIED. ) 
 CURVE ( )  GEOMETRIC_REPRESENTATION_ITEM ( )  RATIONAL_B_SPLINE_CURVE ( ( 0.9330127018922194093, 0.9330127018922194093, 1.000000000000000000, 0.8660254037844387076, 1.000000000000000000, 0.8660254037844387076, 1.000000000000000000, 0.9330127018922194093, 0.9330127018922194093 ) ) 
 REPRESENTATION_ITEM ( '' )  );
#335 = CARTESIAN_POINT ( 'NONE',  ( -3.152548672688508926E-16, 5.437500001365592084, -5.148502694627439702 ) ) ;
#336 = CARTESIAN_POINT ( 'NONE',  ( 2.500000000000002220, -1.541666663935480130, 4.330127018922192761 ) ) ;
#337 = CARTESIAN_POINT ( 'NONE',  ( -4.458734124999998549, -17.47916666530106866, 2.574251347313722516 ) ) ;
#338 = CARTESIAN_POINT ( 'NONE',  ( -5.147856630858197489E-14, 2.375000002731183724, 5.000000000000000000 ) ) ;
#339 = CARTESIAN_POINT ( 'NONE',  ( -4.458734124999999437, -4.395833331967740065, -2.574251347313719407 ) ) ;
#340 = DIRECTION ( 'NONE',  ( -0.000000000000000000, -1.000000000000000000, -0.000000000000000000 ) ) ;
#341 = CARTESIAN_POINT ( 'NONE',  ( 4.458734124999997661, -148.5000000013656347, 1.846868145590737864 ) ) ;
#342 = CARTESIAN_POINT ( 'NONE',  ( -4.458734124999999437, 21.35416666803225993, -2.574251347313719407 ) ) ;
#343 = ORIENTED_EDGE ( 'NONE', *, *, #36170, .F. ) ;
#344 = CARTESIAN_POINT ( 'NONE',  ( -4.458734124999999437, -97.31249999863440792, 0.000000000000000000 ) ) ;
#345 = CARTESIAN_POINT ( 'NONE',  ( 1.339745962155612702, -47.29465819873852439, -5.000000000000000000 ) ) ;
#346 = CARTESIAN_POINT ( 'NONE',  ( -2.499999999999996447, -103.7083333306021444, 4.330127018922195425 ) ) ;
#347 = CARTESIAN_POINT ( 'NONE',  ( -3.152548672688508926E-16, -14.56249999863440436, -5.148502694627439702 ) ) ;
#348 = CARTESIAN_POINT ( 'NONE',  ( 1.162044386198238837E-16, 28.37500000273118417, 5.000000000000000000 ) ) ;
#349 =( BOUNDED_CURVE ( )  B_SPLINE_CURVE ( 2, ( #32871, #48595, #37379, #53427, #52500, #18392, #37690, #3921, #43452 ),
 .UNSPECIFIED., .F., .F. ) 
 B_SPLINE_CURVE_WITH_KNOTS ( ( 3, 2, 2, 2, 3 ),
 ( 0.5229166666666666963, 0.5236111111111111382, 0.5250000000000000222, 0.5263888888888889062, 0.5270833333333333481 ),
 .UNSPECIFIED. ) 
 CURVE ( )  GEOMETRIC_REPRESENTATION_ITEM ( )  RATIONAL_B_SPLINE_CURVE ( ( 0.9330127018922194093, 0.9330127018922194093, 1.000000000000000000, 0.8660254037844387076, 1.000000000000000000, 0.8660254037844387076, 1.000000000000000000, 0.9330127018922194093, 0.9330127018922194093 ) ) 
 REPRESENTATION_ITEM ( '' )  );
#350 = CARTESIAN_POINT ( 'NONE',  ( -2.500000000000000444, -88.16666666666665719, -4.330127018922193649 ) ) ;
#351 = CARTESIAN_POINT ( 'NONE',  ( 2.499999999999998668, -40.20833333060214443, -4.330127018922193649 ) ) ;
#352 = CARTESIAN_POINT ( 'NONE',  ( -7.808218555861945021, 4.508077085120198113, -7.999534413642733988 ) ) ;
#353 = CARTESIAN_POINT ( 'NONE',  ( -2.229367062500000163, 11.52083333469892601, -3.861377020970580443 ) ) ;
#354 = CARTESIAN_POINT ( 'NONE',  ( 5.000000000000000888, -51.45833333060214443, 2.886751345948126879 ) ) ;
#355 = DIRECTION ( 'NONE',  ( -0.000000000000000000, 1.000000000000000000, -0.000000000000000000 ) ) ;
#356 = CARTESIAN_POINT ( 'NONE',  ( -2.229367062500000163, 18.52083333469892779, -3.861377020970580443 ) ) ;
#357 = CARTESIAN_POINT ( 'NONE',  ( -4.458734124999998549, -64.22916666530107932, 2.574251347313722516 ) ) ;
#358 = ORIENTED_EDGE ( 'NONE', *, *, #35301, .F. ) ;
#359 = CARTESIAN_POINT ( 'NONE',  ( 4.458734125000000326, -8.145833331967736513, 2.574251347313718519 ) ) ;
#360 = CARTESIAN_POINT ( 'NONE',  ( -55.00000000000002132, -155.0000000000000284, 1.734723475976807094E-15 ) ) ;
#361 = CARTESIAN_POINT ( 'NONE',  ( -4.999999999999999112, 2.083333333333333037, 2.886751345948131764 ) ) ;
#362 = CARTESIAN_POINT ( 'NONE',  ( -4.458734125000000326, -169.0000000013655779, -1.846868145590735644 ) ) ;
#363 = CARTESIAN_POINT ( 'NONE',  ( -5.000000000000000000, -59.95833333060214443, -2.886751345948128211 ) ) ;
#364 = CARTESIAN_POINT ( 'NONE',  ( -4.458734124999999437, -54.39583333196773651, -2.574251347313719407 ) ) ;
#365 = CARTESIAN_POINT ( 'NONE',  ( 2.499999999999998668, -87.20833333060214443, -4.330127018922193649 ) ) ;
#366 = ADVANCED_FACE ( 'NONE', ( #2909 ), #32473, .T. ) ;
#367 = CARTESIAN_POINT ( 'NONE',  ( 2.229367062500001939, -31.97916666530106866, 3.861377020970579999 ) ) ;
#368 = CARTESIAN_POINT ( 'NONE',  ( -5.000000000000000000, 20.12500000273118772, 0.000000000000000000 ) ) ;
#369 = CARTESIAN_POINT ( 'NONE',  ( 5.000000000000000000, -142.1875000027312126, 2.071067811865478614 ) ) ;
#370 = CARTESIAN_POINT ( 'NONE',  ( -2.500000000000000444, -108.0416666639354730, -4.330127018922193649 ) ) ;
#371 = CARTESIAN_POINT ( 'NONE',  ( 3.152801135295366208, -153.8125000013656063, 3.152801135295367985 ) ) ;
#372 = CARTESIAN_POINT ( 'NONE',  ( -4.999999999999999112, -42.91666666666665719, 2.886751345948131764 ) ) ;
#373 = CARTESIAN_POINT ( 'NONE',  ( 1.339745962155615144, -46.70534180126147561, 4.999999999999999112 ) ) ;
#374 = CARTESIAN_POINT ( 'NONE',  ( -59.77950423082105402, -135.0000000000000284, -0.4113032182319603658 ) ) ;
#375 = EDGE_LOOP ( 'NONE', ( #48769, #4276, #28632, #46133 ) ) ;
#376 = CARTESIAN_POINT ( 'NONE',  ( 4.458734124999999437, -100.8124999986344079, -5.460374474430324690E-16 ) ) ;
#377 = CARTESIAN_POINT ( 'NONE',  ( -4.458734124999999437, 3.437500001365594748, 0.000000000000000000 ) ) ;
#378 = CARTESIAN_POINT ( 'NONE',  ( 1.339745962155499015, -59.70534180126147561, 5.000000000000065725 ) ) ;
#379 = CARTESIAN_POINT ( 'NONE',  ( -2.500000000000000444, -2.166666666666663854, -4.330127018922193649 ) ) ;
#380 = EDGE_CURVE ( 'NONE', #47490, #35906, #55280, .T. ) ;
#381 = CARTESIAN_POINT ( 'NONE',  ( -4.458734124999999437, -67.39583333196773651, -2.574251347313719407 ) ) ;
#382 = AXIS2_PLACEMENT_3D ( 'NONE', #9332, #48570, #38915 ) ;
#383 = FACE_BOUND ( 'NONE', #44585, .T. ) ;
#384 = CARTESIAN_POINT ( 'NONE',  ( 5.000000000000000000, -1.291666663935479908, -2.886751345948129988 ) ) ;
#386 = ORIENTED_EDGE ( 'NONE', *, *, #25943, .F. ) ;
#385 = CARTESIAN_POINT ( 'NONE',  ( -4.458734124999999437, -36.31249999863440792, 0.000000000000000000 ) ) ;
#387 = CARTESIAN_POINT ( 'NONE',  ( -4.999999999999998224, -10.91666666666666607, 2.886751345948131764 ) ) ;
#388 = DIRECTION ( 'NONE',  ( -0.000000000000000000, 1.000000000000000000, -0.000000000000000000 ) ) ;
#389 = EDGE_CURVE ( 'NONE', #14198, #16286, #4716, .T. ) ;
#390 = ORIENTED_EDGE ( 'NONE', *, *, #14942, .T. ) ;
#391 = CARTESIAN_POINT ( 'NONE',  ( -6.972266317189433020E-16, 5.749999999999999112, -5.000000000000000000 ) ) ;
#392 = CARTESIAN_POINT ( 'NONE',  ( 2.500000000000002220, -50.66666666666666430, 4.330127018922192761 ) ) ;
#394 = CARTESIAN_POINT ( 'NONE',  ( -3.152548672688508926E-16, -22.81249999863440436, -5.148502694627439702 ) ) ;
#393 = CARTESIAN_POINT ( 'NONE',  ( 0.000000000000000000, -120.0000000000000000, 0.000000000000000000 ) ) ;
#395 = CARTESIAN_POINT ( 'NONE',  ( -5.000000000000000000, -4.083333333333334814, -2.886751345948128211 ) ) ;
#396 = CARTESIAN_POINT ( 'NONE',  ( 4.458734124999998549, -72.72916666530106511, -2.574251347313721627 ) ) ;
#397 = CARTESIAN_POINT ( 'NONE',  ( -3.152801135295367096, -143.3125000013655779, -3.152801135295367541 ) ) ;
#398 = CARTESIAN_POINT ( 'NONE',  ( -2.229367062499996610, -81.14583333196773651, 3.861377020970582219 ) ) ;
#399 = CARTESIAN_POINT ( 'NONE',  ( -51.60603307380591787, -141.1875000013656063, -2.891590998281053704 ) ) ;
#400 = CARTESIAN_POINT ( 'NONE',  ( 9.457646018065525792E-16, -31.31249999863440436, 5.148502694627439702 ) ) ;
#401 = CARTESIAN_POINT ( 'NONE',  ( -4.999999999999999112, -70.79166666393548724, 2.886751345948131764 ) ) ;
#402 = EDGE_LOOP ( 'NONE', ( #47162, #48030, #33761, #57243 ) ) ;
#403 = CARTESIAN_POINT ( 'NONE',  ( -5.000000000000000000, -82.87499999726881583, 0.000000000000000000 ) ) ;
#404 = ORIENTED_EDGE ( 'NONE', *, *, #32775, .T. ) ;
#405 = CARTESIAN_POINT ( 'NONE',  ( -2.229367062499996610, -71.39583333196773651, 3.861377020970582219 ) ) ;
#406 = CARTESIAN_POINT ( 'NONE',  ( 1.339745962155614256, 28.70534180126147561, -4.999999999999999112 ) ) ;
#407 = ORIENTED_EDGE ( 'NONE', *, *, #54703, .T. ) ;
#408 = CYLINDRICAL_SURFACE ( 'NONE', #17648, 5.000000000000000000 ) ;
#409 =( BOUNDED_CURVE ( )  B_SPLINE_CURVE ( 2, ( #59998, #10777, #6592, #50336, #36184, #21392, #31028, #50979, #30387 ),
 .UNSPECIFIED., .F., .F. ) 
 B_SPLINE_CURVE_WITH_KNOTS ( ( 3, 2, 2, 2, 3 ),
 ( 0.4083333333333336590, 0.4125000000000003109, 0.4166666666666670182, 0.4208333333333336701, 0.4250000000000003220 ),
 .UNSPECIFIED. ) 
 CURVE ( )  GEOMETRIC_REPRESENTATION_ITEM ( )  RATIONAL_B_SPLINE_CURVE ( ( 0.9999999999999938938, 0.9238795325112928447, 1.000000000000000000, 0.9238795325112867385, 1.000000000000000000, 0.9238795325112867385, 1.000000000000000000, 0.9238795325112806323, 1.000000000000005995 ) ) 
 REPRESENTATION_ITEM ( '' )  );
#410 = CARTESIAN_POINT ( 'NONE',  ( 5.000000000000000000, -31.37499999726880873, -6.123233995736766282E-16 ) ) ;
#411 = EDGE_CURVE ( 'NONE', #51356, #16274, #33465, .T. ) ;
#412 = CARTESIAN_POINT ( 'NONE',  ( 2.229367062499998831, -56.89583333196773651, -3.861377020970580887 ) ) ;
#413 = CARTESIAN_POINT ( 'NONE',  ( -3.152548672688508926E-16, -4.812499998634402587, -5.148502694627439702 ) ) ;
#414 = ORIENTED_EDGE ( 'NONE', *, *, #41306, .F. ) ;
#415 = CARTESIAN_POINT ( 'NONE',  ( -5.000000000000000888, -146.5625000000000000, -2.071067811865475949 ) ) ;
#416 = CARTESIAN_POINT ( 'NONE',  ( -1.339745962155613812, -45.20534180126146850, -5.000000000000000000 ) ) ;
#417 = CARTESIAN_POINT ( 'NONE',  ( -4.458734124999998549, 11.77083333469892601, 2.574251347313722516 ) ) ;
#418 = CARTESIAN_POINT ( 'NONE',  ( -52.10840900171896806, -139.1875000013656347, 3.393966926194110556 ) ) ;
#419 = CARTESIAN_POINT ( 'NONE',  ( -4.458734124999999437, -162.0000000013656063, -1.846868145590735644 ) ) ;
#420 = ORIENTED_EDGE ( 'NONE', *, *, #17481, .T. ) ;
#421 = CARTESIAN_POINT ( 'NONE',  ( -4.458734124999997661, -81.22916666530106511, 2.574251347313722516 ) ) ;
#422 = CARTESIAN_POINT ( 'NONE',  ( -5.000000000000000000, -69.87499999726880162, 0.000000000000000000 ) ) ;
#423 = CARTESIAN_POINT ( 'NONE',  ( 2.229367062500001939, 1.020833334698927120, 3.861377020970579999 ) ) ;
#424 = CARTESIAN_POINT ( 'NONE',  ( 5.000000000000000000, -86.50000000000000000, -6.123233995736766282E-16 ) ) ;
#425 = CARTESIAN_POINT ( 'NONE',  ( -6.972266317189433020E-16, -40.12499999726880162, -5.000000000000000000 ) ) ;
#426 = CARTESIAN_POINT ( 'NONE',  ( 9.457646018065525792E-16, -63.31249999863440081, 5.148502694627439702 ) ) ;
#427 = CARTESIAN_POINT ( 'NONE',  ( 5.000000000000000000, -27.37499999726880873, -6.123233995736766282E-16 ) ) ;
#428 = CARTESIAN_POINT ( 'NONE',  ( -6.972266317189433020E-16, 5.749999999999999112, -5.000000000000000000 ) ) ;
#429 = CARTESIAN_POINT ( 'NONE',  ( 5.000000000000000888, -78.45833333060214443, 2.886751345948126879 ) ) ;
#430 = CARTESIAN_POINT ( 'NONE',  ( 2.500000000000002220, -49.66666666666666430, 4.330127018922192761 ) ) ;
#431 =( NAMED_UNIT ( * ) SI_UNIT ( $, .STERADIAN. ) SOLID_ANGLE_UNIT ( ) );
#432 = CARTESIAN_POINT ( 'NONE',  ( -2.229367062500000163, -45.47916666530106511, -3.861377020970580443 ) ) ;
#433 = CARTESIAN_POINT ( 'NONE',  ( 9.457646018065525792E-16, -30.31249999863440436, 5.148502694627439702 ) ) ;
#434 = CARTESIAN_POINT ( 'NONE',  ( -3.152548672688508926E-16, 6.187500001365593860, -5.148502694627439702 ) ) ;
#435 = CARTESIAN_POINT ( 'NONE',  ( -4.999999999999998224, -9.791666663935476578, 2.886751345948131764 ) ) ;
#436 = CARTESIAN_POINT ( 'NONE',  ( -4.999999999999999112, 19.08333333333333570, 2.886751345948131764 ) ) ;
#437 = CARTESIAN_POINT ( 'NONE',  ( 2.071067811865475505, -147.9375000027312126, -5.000000000000000888 ) ) ;
#438 = CARTESIAN_POINT ( 'NONE',  ( 0.000000000000000000, -120.0000000000000000, 5.000000000000000000 ) ) ;
#439 = CARTESIAN_POINT ( 'NONE',  ( 2.229367062500001939, -35.97916666530107221, 3.861377020970579999 ) ) ;
#440 = CARTESIAN_POINT ( 'NONE',  ( -3.535250795749689387E-16, -73.12499999726881583, -5.773502691896257311 ) ) ;
#441 = CARTESIAN_POINT ( 'NONE',  ( -52.10840900171896806, -143.4375000013656063, 3.393966926194110556 ) ) ;
#442 = CYLINDRICAL_SURFACE ( 'NONE', #40067, 5.000000000000000000 ) ;
#443 = EDGE_CURVE ( 'NONE', #39270, #17071, #61863, .T. ) ;
#444 = CARTESIAN_POINT ( 'NONE',  ( 2.500000000000002220, -37.66666666666666430, 4.330127018922192761 ) ) ;
#445 = EDGE_CURVE ( 'NONE', #14245, #8450, #57255, .T. ) ;
#446 = CARTESIAN_POINT ( 'NONE',  ( -4.458734124999999437, -82.56249999863440792, 0.000000000000000000 ) ) ;
#447 = CARTESIAN_POINT ( 'NONE',  ( -1.846868145590737420, -166.0000000013656063, 4.458734124999997661 ) ) ;
#448 = CARTESIAN_POINT ( 'NONE',  ( -2.229367062500000163, -34.47916666530107221, -3.861377020970580443 ) ) ;
#449 = EDGE_CURVE ( 'NONE', #23480, #42348, #53192, .T. ) ;
#450 = DIRECTION ( 'NONE',  ( 0.000000000000000000, 0.000000000000000000, 1.000000000000000000 ) ) ;
#451 = FACE_OUTER_BOUND ( 'NONE', #62489, .T. ) ;
#452 = CARTESIAN_POINT ( 'NONE',  ( 2.500000000000002220, -26.66666666666666430, 4.330127018922192761 ) ) ;
#453 = CARTESIAN_POINT ( 'NONE',  ( 4.458734124999999437, -145.4375000013656063, 0.000000000000000000 ) ) ;
#454 = VERTEX_POINT ( 'NONE', #32796 ) ;
#455 = CARTESIAN_POINT ( 'NONE',  ( 2.229367062499998831, 29.10416666803225993, -3.861377020970580887 ) ) ;
#456 = VERTEX_POINT ( 'NONE', #52425 ) ;
#457 = CARTESIAN_POINT ( 'NONE',  ( -4.458734124999999437, -61.56249999863440081, 0.000000000000000000 ) ) ;
#458 = CARTESIAN_POINT ( 'NONE',  ( 5.000000000000000000, 19.62500000273118772, -6.123233995736766282E-16 ) ) ;
#459 =( BOUNDED_CURVE ( )  B_SPLINE_CURVE ( 2, ( #55262, #6684, #6374, #54615, #16335, #1554, #60409, #25980, #45595 ),
 .UNSPECIFIED., .F., .F. ) 
 B_SPLINE_CURVE_WITH_KNOTS ( ( 3, 2, 2, 2, 3 ),
 ( 0.03035714285714285685, 0.03095238095238095344, 0.03214285714285713969, 0.03333333333333333287, 0.03392857142857143293 ),
 .UNSPECIFIED. ) 
 CURVE ( )  GEOMETRIC_REPRESENTATION_ITEM ( )  RATIONAL_B_SPLINE_CURVE ( ( 0.9330127018922194093, 0.9330127018922194093, 1.000000000000000000, 0.8660254037844387076, 1.000000000000000000, 0.8660254037844387076, 1.000000000000000000, 0.9330127018922189652, 0.9330127018922194093 ) ) 
 REPRESENTATION_ITEM ( '' )  );
#460 = CARTESIAN_POINT ( 'NONE',  ( 5.000000000000000000, -48.37499999726880873, -6.123233995736766282E-16 ) ) ;
#461 = CARTESIAN_POINT ( 'NONE',  ( 5.000000000000000000, 12.58333333333333215, -2.886751345948129988 ) ) ;
#462 = ADVANCED_FACE ( 'NONE', ( #8357 ), #52728, .T. ) ;
#463 = CARTESIAN_POINT ( 'NONE',  ( -2.229367062500000163, -53.47916666530107221, -3.861377020970580443 ) ) ;
#464 = CARTESIAN_POINT ( 'NONE',  ( 2.229367062500001939, -6.979166665301073103, 3.861377020970579999 ) ) ;
#465 = CARTESIAN_POINT ( 'NONE',  ( -5.000000000000000000, 4.041666669397852019, -2.886751345948128211 ) ) ;
#466 = CARTESIAN_POINT ( 'NONE',  ( -1.339745962155610925, -8.794658198738519062, 5.000000000000000000 ) ) ;
#467 = CARTESIAN_POINT ( 'NONE',  ( -2.500000000000000444, -0.1666666666666656582, -4.330127018922193649 ) ) ;
#468 = EDGE_CURVE ( 'NONE', #15325, #14586, #24076, .T. ) ;
#469 = DIRECTION ( 'NONE',  ( -0.000000000000000000, 1.000000000000000000, -0.000000000000000000 ) ) ;
#471 = CARTESIAN_POINT ( 'NONE',  ( 4.458734124999999437, -19.81249999863440081, -5.460374474430324690E-16 ) ) ;
#470 = CARTESIAN_POINT ( 'NONE',  ( -60.14911071818854538, -151.0625000000000284, 1.666127454062681146 ) ) ;
#472 = CARTESIAN_POINT ( 'NONE',  ( 9.457646018065525792E-16, -52.06249999863440792, 5.148502694627439702 ) ) ;
#473 = CARTESIAN_POINT ( 'NONE',  ( 3.152801135295366208, -154.8125000013656063, 3.152801135295367985 ) ) ;
#474 = ADVANCED_FACE ( 'NONE', ( #38255 ), #24401, .T. ) ;
#475 = AXIS2_PLACEMENT_3D ( 'NONE', #22306, #28376, #22629 ) ;
#476 = CARTESIAN_POINT ( 'NONE',  ( 1.060575238724906964E-15, -53.62499999726880873, 5.773502691896257311 ) ) ;
#477 = ORIENTED_EDGE ( 'NONE', *, *, #63171, .F. ) ;
#478 = CARTESIAN_POINT ( 'NONE',  ( 4.458734125000001214, 2.854166668032259491, 2.574251347313718519 ) ) ;
#479 = ORIENTED_EDGE ( 'NONE', *, *, #43975, .F. ) ;
#481 = CARTESIAN_POINT ( 'NONE',  ( 5.000000000000000000, 11.70833333606451809, -2.886751345948130876 ) ) ;
#480 = CARTESIAN_POINT ( 'NONE',  ( -6.972266317189433020E-16, -87.25000000000001421, -5.000000000000000000 ) ) ;
#482 = CARTESIAN_POINT ( 'NONE',  ( 1.846868145590735200, -156.2500000013656063, -4.458734125000000326 ) ) ;
#483 = VERTEX_POINT ( 'NONE', #24090 ) ;
#484 = CARTESIAN_POINT ( 'NONE',  ( 2.499999999999998668, -83.33333333333332860, -4.330127018922193649 ) ) ;
#485 = CARTESIAN_POINT ( 'NONE',  ( -49.85088928181150436, -130.5625000000000568, -1.666127454062680702 ) ) ;
#486 = CARTESIAN_POINT ( 'NONE',  ( 2.499999999999998668, -86.33333333333332860, -4.330127018922193649 ) ) ;
#487 = CARTESIAN_POINT ( 'NONE',  ( 2.229367062499998831, -40.89583333196773651, -3.861377020970580887 ) ) ;
#488 = ORIENTED_EDGE ( 'NONE', *, *, #59618, .T. ) ;
#489 = CARTESIAN_POINT ( 'NONE',  ( -4.458734124999998549, 12.77083333469892601, 2.574251347313722516 ) ) ;
#490 = CARTESIAN_POINT ( 'NONE',  ( 1.339745962155612702, 3.830341803992665550, -5.000000000000000000 ) ) ;
#491 = ORIENTED_EDGE ( 'NONE', *, *, #46738, .F. ) ;
#492 = CARTESIAN_POINT ( 'NONE',  ( 4.458734124999999437, 28.18750000136559208, -5.460374474430324690E-16 ) ) ;
#493 = CARTESIAN_POINT ( 'NONE',  ( -51.60603307380591787, -152.9375000013656063, -2.891590998281053704 ) ) ;
#494 = CARTESIAN_POINT ( 'NONE',  ( 5.000000000000000000, -39.41666666666667851, -2.886751345948130876 ) ) ;
#495 = CARTESIAN_POINT ( 'NONE',  ( -4.999999999999998224, 24.08333333333333215, 2.886751345948131764 ) ) ;
#496 = CARTESIAN_POINT ( 'NONE',  ( 4.458734124999998549, -62.72916666530106511, -2.574251347313721627 ) ) ;
#497 = CARTESIAN_POINT ( 'NONE',  ( -2.500000000000000444, -62.04166666393547303, -4.330127018922193649 ) ) ;
#498 = CARTESIAN_POINT ( 'NONE',  ( 4.458734124999999437, 20.18750000136559208, -5.460374474430324690E-16 ) ) ;
#499 = CARTESIAN_POINT ( 'NONE',  ( 5.000000000000000000, -33.50000000000000000, -6.123233995736766282E-16 ) ) ;
#500 = CARTESIAN_POINT ( 'NONE',  ( -4.458734124999999437, -50.56249999863440792, 0.000000000000000000 ) ) ;
#501 = CARTESIAN_POINT ( 'NONE',  ( -2.500000000000000444, -12.04166666393547835, -4.330127018922193649 ) ) ;
#502 = CARTESIAN_POINT ( 'NONE',  ( -2.500000000000000444, 4.833333333333332149, -4.330127018922193649 ) ) ;
#503 = CARTESIAN_POINT ( 'NONE',  ( -5.147856630858197489E-14, 3.375000002731183280, 5.000000000000000000 ) ) ;
#504 = CARTESIAN_POINT ( 'NONE',  ( 4.458734124999999437, -88.06249999863439371, -5.460374474430324690E-16 ) ) ;
#505 = CARTESIAN_POINT ( 'NONE',  ( 1.975475456537005874E-15, -64.62499999726880162, 5.000000000000000000 ) ) ;
#506 = CARTESIAN_POINT ( 'NONE',  ( -2.229367062499996610, -15.39583333196773651, 3.861377020970582219 ) ) ;
#507 = EDGE_LOOP ( 'NONE', ( #44935, #18884, #62333, #60547 ) ) ;
#508 = CARTESIAN_POINT ( 'NONE',  ( -1.336351044127974539E-14, 23.24999999999999645, 5.000000000000000000 ) ) ;
#509 = CARTESIAN_POINT ( 'NONE',  ( -2.229367062500000163, -103.4791666653010651, -3.861377020970580443 ) ) ;
#510 = CARTESIAN_POINT ( 'NONE',  ( 2.071067811865476394, -163.3125000027311842, 5.000000000000000000 ) ) ;
#511 = CARTESIAN_POINT ( 'NONE',  ( -2.229367062500000163, -98.72916666530105090, -3.861377020970580443 ) ) ;
#512 = CARTESIAN_POINT ( 'NONE',  ( 6.123233995736766282E-16, -120.0000000000000000, -5.000000000000000000 ) ) ;
#513 = CARTESIAN_POINT ( 'NONE',  ( -3.535250795749689387E-16, -58.12499999726880162, -5.773502691896257311 ) ) ;
#514 = CARTESIAN_POINT ( 'NONE',  ( -4.999999999999998224, -66.91666666666667140, 2.886751345948131764 ) ) ;
#515 = CIRCLE ( 'NONE', #57003, 5.000000000000000000 ) ;
#516 = CARTESIAN_POINT ( 'NONE',  ( -50.70258187064364108, -154.3750000013656063, 2.196230717870141014 ) ) ;
#517 = CARTESIAN_POINT ( 'NONE',  ( -54.64476657466781973, -145.8125000013656063, -4.444560631937228834 ) ) ;
#518 = EDGE_CURVE ( 'NONE', #43968, #24595, #43685, .T. ) ;
#519 = CARTESIAN_POINT ( 'NONE',  ( 2.229367062500001939, -15.97916666530107399, 3.861377020970579999 ) ) ;
#520 = CARTESIAN_POINT ( 'NONE',  ( -4.458734124999999437, 5.437500001365592972, 0.000000000000000000 ) ) ;
#521 = CARTESIAN_POINT ( 'NONE',  ( -4.458734124999997661, -62.47916666530106511, 2.574251347313722516 ) ) ;
#522 = CARTESIAN_POINT ( 'NONE',  ( -3.535533905932737309, -141.7500000027311842, -3.535533905932738197 ) ) ;
#523 = CARTESIAN_POINT ( 'NONE',  ( -4.458734124999997661, -21.22916666530107221, 2.574251347313722516 ) ) ;
#524 = CARTESIAN_POINT ( 'NONE',  ( -5.000000000000000000, -79.95833333060213022, -2.886751345948128211 ) ) ;
#525 = CARTESIAN_POINT ( 'NONE',  ( 5.000000000000000000, -155.0625000000000284, 2.071067811865478614 ) ) ;
#526 = CARTESIAN_POINT ( 'NONE',  ( 1.060575238724906964E-15, -6.749999999999999112, 5.773502691896257311 ) ) ;
#527 = EDGE_LOOP ( 'NONE', ( #5913, #22407, #27837, #31617 ) ) ;
#528 = CARTESIAN_POINT ( 'NONE',  ( 2.229367062499998831, -45.89583333196774362, -3.861377020970580887 ) ) ;
#529 = CYLINDRICAL_SURFACE ( 'NONE', #46889, 5.000000000000000000 ) ;
#530 = CARTESIAN_POINT ( 'NONE',  ( -2.325424218463065351, 7.317669739334662360, -7.030005583190789054 ) ) ;
#531 = CARTESIAN_POINT ( 'NONE',  ( -4.999999999999999112, 28.08333333333333570, 2.886751345948131764 ) ) ;
#532 = CARTESIAN_POINT ( 'NONE',  ( -4.458734124999998549, -93.22916666530107932, 2.574251347313722516 ) ) ;
#533 = CARTESIAN_POINT ( 'NONE',  ( 9.457646018065525792E-16, 19.68750000136559208, 5.148502694627439702 ) ) ;
#534 =( BOUNDED_CURVE ( )  B_SPLINE_CURVE ( 2, ( #52700, #32767, #28246, #52401, #4434, #8333, #37911, #43043, #33393 ),
 .UNSPECIFIED., .F., .F. ) 
 B_SPLINE_CURVE_WITH_KNOTS ( ( 3, 2, 2, 2, 3 ),
 ( 0.1982142857142857040, 0.1988095238095237971, 0.2000000000000000111, 0.2011904761904761973, 0.2017857142857142905 ),
 .UNSPECIFIED. ) 
 CURVE ( )  GEOMETRIC_REPRESENTATION_ITEM ( )  RATIONAL_B_SPLINE_CURVE ( ( 0.9330127018922194093, 0.9330127018922194093, 1.000000000000000000, 0.8660254037844387076, 1.000000000000000000, 0.8660254037844387076, 1.000000000000000000, 0.9330127018922194093, 0.9330127018922194093 ) ) 
 REPRESENTATION_ITEM ( '' )  );
#535 = CARTESIAN_POINT ( 'NONE',  ( 4.458734125000001214, 8.104166668032261711, 2.574251347313718519 ) ) ;
#536 = CARTESIAN_POINT ( 'NONE',  ( 1.975475456537005874E-15, -0.7499999999999996669, 5.000000000000000000 ) ) ;
#537 = CARTESIAN_POINT ( 'NONE',  ( -5.000000000000000000, 12.00000000000000000, 0.000000000000000000 ) ) ;
#538 = CARTESIAN_POINT ( 'NONE',  ( 1.339745962155615144, -82.70534180126146850, 4.999999999999999112 ) ) ;
#539 = CARTESIAN_POINT ( 'NONE',  ( -4.458734124999999437, 19.35416666803225993, -2.574251347313719407 ) ) ;
#540 = CARTESIAN_POINT ( 'NONE',  ( -2.499999999999996447, -74.83333333333332860, 4.330127018922195425 ) ) ;
#541 = CARTESIAN_POINT ( 'NONE',  ( -3.535250795749689387E-16, 6.875000002731186832, -5.773502691896257311 ) ) ;
#543 = ORIENTED_EDGE ( 'NONE', *, *, #44898, .F. ) ;
#542 = EDGE_CURVE ( 'NONE', #41301, #34010, #1942, .T. ) ;
#544 = CARTESIAN_POINT ( 'NONE',  ( -4.999999999999998224, -97.91666666666667140, 2.886751345948131764 ) ) ;
#545 = ORIENTED_EDGE ( 'NONE', *, *, #24179, .T. ) ;
#546 = DIRECTION ( 'NONE',  ( 0.000000000000000000, -1.000000000000000000, 0.000000000000000000 ) ) ;
#547 = CARTESIAN_POINT ( 'NONE',  ( 4.458734125000001214, -40.89583333196773651, 2.574251347313718519 ) ) ;
#548 = EDGE_CURVE ( 'NONE', #7140, #8617, #11299, .T. ) ;
#549 = ADVANCED_FACE ( 'NONE', ( #45611 ), #44645, .T. ) ;
#550 = CARTESIAN_POINT ( 'NONE',  ( -2.500000000000000444, -39.04166666393548013, -4.330127018922193649 ) ) ;
#551 = VERTEX_POINT ( 'NONE', #605 ) ;
#552 = CARTESIAN_POINT ( 'NONE',  ( -52.10840900171896806, -146.4375000013656063, 3.393966926194110556 ) ) ;
#553 = CARTESIAN_POINT ( 'NONE',  ( 2.229367062500001939, -11.97916666530107044, 3.861377020970579999 ) ) ;
#555 = ORIENTED_EDGE ( 'NONE', *, *, #48721, .F. ) ;
#554 = CARTESIAN_POINT ( 'NONE',  ( 4.458734124999999437, -13.06249999863440259, -5.460374474430324690E-16 ) ) ;
#556 = CARTESIAN_POINT ( 'NONE',  ( -5.000000000000000000, -82.08333333333332860, -2.886751345948128211 ) ) ;
#557 = CARTESIAN_POINT ( 'NONE',  ( 3.152801135295366208, -168.5625000013656063, 3.152801135295367985 ) ) ;
#558 = CARTESIAN_POINT ( 'NONE',  ( 4.458734125000001214, -60.14583333196774362, 2.574251347313718519 ) ) ;
#559 = CARTESIAN_POINT ( 'NONE',  ( 2.500000000000002220, -86.54166666393547303, 4.330127018922192761 ) ) ;
#561 = ORIENTED_EDGE ( 'NONE', *, *, #9529, .F. ) ;
#560 = CARTESIAN_POINT ( 'NONE',  ( -1.339745962155613812, -18.20534180126147916, -5.000000000000000000 ) ) ;
#562 = CARTESIAN_POINT ( 'NONE',  ( -52.53715891517739323, -147.4375000000000284, -4.819101127000233298 ) ) ;
#563 = CARTESIAN_POINT ( 'NONE',  ( -2.229367062500000163, -24.72916666530106866, -3.861377020970580443 ) ) ;
#564 = CARTESIAN_POINT ( 'NONE',  ( 5.000000000000000000, -29.41666666666666785, -2.886751345948130876 ) ) ;
#565 = EDGE_LOOP ( 'NONE', ( #55291, #23421, #60900, #47144 ) ) ;
#566 = PRODUCT_CONTEXT ( 'NONE', #44181, 'mechanical' ) ;
#567 = CARTESIAN_POINT ( 'NONE',  ( 4.458734124999999437, -163.7500000013655779, 1.846868145590737864 ) ) ;
#568 = CARTESIAN_POINT ( 'NONE',  ( -4.458734124999998549, -105.4791666653010793, 2.574251347313722516 ) ) ;
#569 = CARTESIAN_POINT ( 'NONE',  ( 1.339745962155612702, -23.29465819873851729, -5.000000000000000000 ) ) ;
#570 = ORIENTED_EDGE ( 'NONE', *, *, #6344, .F. ) ;
#571 = CARTESIAN_POINT ( 'NONE',  ( -59.59170313451810586, -144.7500000013655779, 1.485763867205729394 ) ) ;
#572 = CARTESIAN_POINT ( 'NONE',  ( 2.229367062500001939, -75.22916666530106511, 3.861377020970579999 ) ) ;
#573 = CARTESIAN_POINT ( 'NONE',  ( -51.75738570946856498, -134.8750000027312126, 3.805975901505576964 ) ) ;
#574 = CARTESIAN_POINT ( 'NONE',  ( -4.458734124999999437, -44.31249999863440081, 0.000000000000000000 ) ) ;
#575 = CARTESIAN_POINT ( 'NONE',  ( 1.846868145590735200, -145.5000000013656063, -4.458734124999999437 ) ) ;
#576 = CARTESIAN_POINT ( 'NONE',  ( -7.894706624614703294, -0.7534108004380160040, -7.590222617908770175 ) ) ;
#577 = CARTESIAN_POINT ( 'NONE',  ( 2.229367062500001939, -46.97916666530106511, 3.861377020970579999 ) ) ;
#578 = CARTESIAN_POINT ( 'NONE',  ( -2.499999999999996447, -70.83333333333332860, 4.330127018922195425 ) ) ;
#579 = CARTESIAN_POINT ( 'NONE',  ( -4.458734124999999437, -10.39583333196773829, -2.574251347313719407 ) ) ;
#580 = CARTESIAN_POINT ( 'NONE',  ( 2.499999999999998668, -100.3333333333333286, -4.330127018922193649 ) ) ;
#581 = CARTESIAN_POINT ( 'NONE',  ( -3.152801135295367985, -140.0625000013655779, 3.152801135295367096 ) ) ;
#582 = CARTESIAN_POINT ( 'NONE',  ( -2.229367062499996610, -33.39583333196772941, 3.861377020970582219 ) ) ;
#583 = CARTESIAN_POINT ( 'NONE',  ( 1.060575238724906964E-15, 4.375000002731186832, 5.773502691896257311 ) ) ;
#584 = CARTESIAN_POINT ( 'NONE',  ( -1.339745962155613812, -40.08034179853028434, -5.000000000000000000 ) ) ;
#585 = CARTESIAN_POINT ( 'NONE',  ( -52.80376928212989185, -132.8750000013656063, -4.297418129356379346 ) ) ;
#586 =( BOUNDED_CURVE ( )  B_SPLINE_CURVE ( 2, ( #13509, #41564, #52436, #23474, #18325, #8370, #57884, #43077, #62715 ),
 .UNSPECIFIED., .F., .F. ) 
 B_SPLINE_CURVE_WITH_KNOTS ( ( 3, 2, 2, 2, 3 ),
 ( 0.1375000000000000111, 0.1380952380952381042, 0.1392857142857142905, 0.1404761904761904767, 0.1410714285714285698 ),
 .UNSPECIFIED. ) 
 CURVE ( )  GEOMETRIC_REPRESENTATION_ITEM ( )  RATIONAL_B_SPLINE_CURVE ( ( 0.9330127018922194093, 0.9330127018922194093, 1.000000000000000000, 0.8660254037844387076, 1.000000000000000000, 0.8660254037844387076, 1.000000000000000000, 0.9330127018922194093, 0.9330127018922194093 ) ) 
 REPRESENTATION_ITEM ( '' )  );
#587 = CARTESIAN_POINT ( 'NONE',  ( 9.457646018065525792E-16, -74.31249999863440792, 5.148502694627439702 ) ) ;
#588 = DIRECTION ( 'NONE',  ( 0.000000000000000000, 0.000000000000000000, 1.000000000000000000 ) ) ;
#589 = CARTESIAN_POINT ( 'NONE',  ( 2.499999999999998668, -54.20833333060213732, -4.330127018922193649 ) ) ;
#590 = LINE ( 'NONE', #44308, #43871 ) ;
#591 = CARTESIAN_POINT ( 'NONE',  ( -2.229367062500000163, -0.7291666653010709931, -3.861377020970580443 ) ) ;
#592 = VERTEX_POINT ( 'NONE', #20542 ) ;
#593 = DIRECTION ( 'NONE',  ( -0.000000000000000000, 1.000000000000000000, -0.000000000000000000 ) ) ;
#594 = CARTESIAN_POINT ( 'NONE',  ( -6.972266317189433020E-16, -76.24999999999998579, -5.000000000000000000 ) ) ;
#596 = CARTESIAN_POINT ( 'NONE',  ( 4.458734125000001214, -36.89583333196773651, 2.574251347313718519 ) ) ;
#595 = CARTESIAN_POINT ( 'NONE',  ( -5.000000000000000000, -95.08333333333334281, -2.886751345948128211 ) ) ;
#597 = CARTESIAN_POINT ( 'NONE',  ( -4.458734124999999437, -83.64583333196773651, -2.574251347313719407 ) ) ;
#598 = CARTESIAN_POINT ( 'NONE',  ( 4.458734124999998549, 19.02083333469892779, -2.574251347313721627 ) ) ;
#599 = CARTESIAN_POINT ( 'NONE',  ( -2.498395430326213474E-14, 20.37500000273118062, 5.000000000000000000 ) ) ;
#601 = EDGE_CURVE ( 'NONE', #58440, #60689, #40027, .T. ) ;
#600 = CARTESIAN_POINT ( 'NONE',  ( -59.44456063193725015, -138.5625000013656063, -0.3552334253322034230 ) ) ;
#602 = CARTESIAN_POINT ( 'NONE',  ( -2.229367062499996610, -0.1458333319677394824, 3.861377020970582219 ) ) ;
#603 = CARTESIAN_POINT ( 'NONE',  ( 9.457646018065525792E-16, 22.68750000136559564, 5.148502694627439702 ) ) ;
#604 = CARTESIAN_POINT ( 'NONE',  ( -2.229367062500000163, -42.72916666530107932, -3.861377020970580443 ) ) ;
#605 = CARTESIAN_POINT ( 'NONE',  ( 1.975475456537005874E-15, 19.37500000273118772, 5.000000000000000000 ) ) ;
#606 = CARTESIAN_POINT ( 'NONE',  ( -2.229367062500000163, -1.479166665301071770, -3.861377020970580443 ) ) ;
#607 = AXIS2_PLACEMENT_3D ( 'NONE', #36007, #55638, #7380 ) ;
#608 = ORIENTED_EDGE ( 'NONE', *, *, #31528, .F. ) ;
#609 = CARTESIAN_POINT ( 'NONE',  ( 4.458734124999998549, -29.97916666530107221, -2.574251347313721627 ) ) ;
#610 = CARTESIAN_POINT ( 'NONE',  ( -55.35523342533222291, -133.5625000013656063, 4.444560631937231499 ) ) ;
#611 = CARTESIAN_POINT ( 'NONE',  ( -4.458734124999999437, -76.39583333196775072, -2.574251347313719407 ) ) ;
#612 = CARTESIAN_POINT ( 'NONE',  ( -5.000000000000000000, -104.9583333306021444, -2.886751345948128211 ) ) ;
#613 = CARTESIAN_POINT ( 'NONE',  ( -4.458734124999999437, 23.68750000136559564, 0.000000000000000000 ) ) ;
#614 = CARTESIAN_POINT ( 'NONE',  ( 2.499999999999998668, 26.79166666939785202, -4.330127018922193649 ) ) ;
#615 = CARTESIAN_POINT ( 'NONE',  ( -1.975475456537005874E-15, 28.25000000000000000, 5.000000000000000000 ) ) ;
#616 = CARTESIAN_POINT ( 'NONE',  ( -2.229367062500000163, -73.72916666530106511, -3.861377020970580443 ) ) ;
#617 = CARTESIAN_POINT ( 'NONE',  ( -5.000000000000000000, -61.08333333333333570, -2.886751345948128211 ) ) ;
#618 = CARTESIAN_POINT ( 'NONE',  ( 1.975475456537005874E-15, -36.62499999726880873, 5.000000000000000000 ) ) ;
#619 = CARTESIAN_POINT ( 'NONE',  ( -5.000000000000000000, 24.12500000273118417, 0.000000000000000000 ) ) ;
#620 = ORIENTED_EDGE ( 'NONE', *, *, #55792, .F. ) ;
#621 = CARTESIAN_POINT ( 'NONE',  ( 0.000000000000000000, -120.0000000000000000, 5.000000000000000000 ) ) ;
#622 = CARTESIAN_POINT ( 'NONE',  ( -6.972266317189433020E-16, -71.12499999726878741, -5.000000000000000000 ) ) ;
#623 = CARTESIAN_POINT ( 'NONE',  ( 2.499999999999998668, -19.33333333333333570, -4.330127018922193649 ) ) ;
#624 = CARTESIAN_POINT ( 'NONE',  ( 2.229367062499998831, -20.64583333196774007, -3.861377020970580887 ) ) ;
#625 = CARTESIAN_POINT ( 'NONE',  ( 4.458734124999998549, -82.72916666530106511, -2.574251347313721627 ) ) ;
#626 = CARTESIAN_POINT ( 'NONE',  ( 5.000000000000000000, -22.29166666393548368, -2.886751345948129988 ) ) ;
#628 = EDGE_LOOP ( 'NONE', ( #892, #35676, #47248, #5295 ) ) ;
#627 = CARTESIAN_POINT ( 'NONE',  ( 4.458734125000001214, -50.89583333196772230, 2.574251347313718519 ) ) ;
#629 = CARTESIAN_POINT ( 'NONE',  ( 2.500000000000002220, -70.54166666393547303, 4.330127018922192761 ) ) ;
#630 = CARTESIAN_POINT ( 'NONE',  ( -5.000000000000000000, 11.12500000273118594, 0.000000000000000000 ) ) ;
#632 = ORIENTED_EDGE ( 'NONE', *, *, #44976, .T. ) ;
#631 = CARTESIAN_POINT ( 'NONE',  ( 4.458734124999999437, 3.937500001365595192, -5.460374474430324690E-16 ) ) ;
#633 = CARTESIAN_POINT ( 'NONE',  ( -59.44456063193725015, -151.5625000013656063, -0.3552334253322034230 ) ) ;
#634 = CARTESIAN_POINT ( 'NONE',  ( 5.000000000000000888, -68.58333333333334281, 2.886751345948126879 ) ) ;
#635 = CARTESIAN_POINT ( 'NONE',  ( 4.458734124999999437, -153.6875000013656063, 0.000000000000000000 ) ) ;
#636 = CARTESIAN_POINT ( 'NONE',  ( 9.457646018065525792E-16, -48.31249999863440081, 5.148502694627439702 ) ) ;
#637 = CARTESIAN_POINT ( 'NONE',  ( 5.000000000000000000, -23.50000000000000000, -6.123233995736766282E-16 ) ) ;
#638 =( BOUNDED_CURVE ( )  B_SPLINE_CURVE ( 2, ( #48959, #44134, #22729, #58938, #61967, #33863, #48646, #56828, #22412 ),
 .UNSPECIFIED., .F., .F. ) 
 B_SPLINE_CURVE_WITH_KNOTS ( ( 3, 2, 2, 2, 3 ),
 ( 0.4312500000000000222, 0.4319444444444444642, 0.4333333333333333481, 0.4347222222222222321, 0.4354166666666666741 ),
 .UNSPECIFIED. ) 
 CURVE ( )  GEOMETRIC_REPRESENTATION_ITEM ( )  RATIONAL_B_SPLINE_CURVE ( ( 0.9330127018922194093, 0.9330127018922194093, 1.000000000000000000, 0.8660254037844387076, 1.000000000000000000, 0.8660254037844387076, 1.000000000000000000, 0.9330127018922194093, 0.9330127018922194093 ) ) 
 REPRESENTATION_ITEM ( '' )  );
#639 = CARTESIAN_POINT ( 'NONE',  ( -3.535533905932737309, -161.6250000000000284, -3.535533905932738197 ) ) ;
#640 = DIRECTION ( 'NONE',  ( -0.000000000000000000, 1.000000000000000000, -0.000000000000000000 ) ) ;
#641 = CARTESIAN_POINT ( 'NONE',  ( -52.80376928212989185, -129.1250000013655779, -4.297418129356379346 ) ) ;
#642 = CARTESIAN_POINT ( 'NONE',  ( -2.229367062499996610, -12.39583333196774007, 3.861377020970582219 ) ) ;
#643 = CARTESIAN_POINT ( 'NONE',  ( 2.229367062499998831, -46.89583333196774362, -3.861377020970580887 ) ) ;
#644 = CARTESIAN_POINT ( 'NONE',  ( -50.01589407740564042, -136.7500000027312126, 0.3983568153799778022 ) ) ;
#645 = CARTESIAN_POINT ( 'NONE',  ( 4.458734125000000326, -145.3750000013656347, -1.846868145590734978 ) ) ;
#646 = CARTESIAN_POINT ( 'NONE',  ( -2.229367062500000163, -86.72916666530107932, -3.861377020970580443 ) ) ;
#647 = CARTESIAN_POINT ( 'NONE',  ( -2.498395430326213474E-14, 21.37500000273118062, 5.000000000000000000 ) ) ;
#648 = ORIENTED_EDGE ( 'NONE', *, *, #24773, .F. ) ;
#649 = CARTESIAN_POINT ( 'NONE',  ( 5.000000000000000000, -19.37499999726881583, -6.123233995736766282E-16 ) ) ;
#650 = CARTESIAN_POINT ( 'NONE',  ( -6.972266317189433020E-16, -12.12499999726881583, -5.000000000000000000 ) ) ;
#651 = CARTESIAN_POINT ( 'NONE',  ( -50.01589407740564042, -150.7500000027312410, 0.3983568153799778022 ) ) ;
#652 = AXIS2_PLACEMENT_3D ( 'NONE', #63511, #37888, #42069 ) ;
#653 = CARTESIAN_POINT ( 'NONE',  ( 1.339745962155612702, -38.29465819873851729, -5.000000000000000000 ) ) ;
#654 = EDGE_CURVE ( 'NONE', #27389, #30981, #20215, .T. ) ;
#655 = ORIENTED_EDGE ( 'NONE', *, *, #11941, .T. ) ;
#656 = AXIS2_PLACEMENT_3D ( 'NONE', #10891, #51098, #35667 ) ;
#657 = CARTESIAN_POINT ( 'NONE',  ( -3.152548672688508926E-16, 4.437500001365595637, -5.148502694627439702 ) ) ;
#658 = DIRECTION ( 'NONE',  ( 0.000000000000000000, 0.000000000000000000, 1.000000000000000000 ) ) ;
#659 = CARTESIAN_POINT ( 'NONE',  ( -3.152548672688508926E-16, -15.81249999863440436, -5.148502694627439702 ) ) ;
#660 = CARTESIAN_POINT ( 'NONE',  ( -1.339745962155613812, 8.794658198738519062, -5.000000000000000000 ) ) ;
#661 = CARTESIAN_POINT ( 'NONE',  ( -4.458734124999999437, -4.312499998634401699, 0.000000000000000000 ) ) ;
#662 = CARTESIAN_POINT ( 'NONE',  ( 5.000000000000000000, -73.29166666393548724, -2.886751345948130876 ) ) ;
#663 = CARTESIAN_POINT ( 'NONE',  ( -1.846868145590737420, -147.7500000013656063, 4.458734124999997661 ) ) ;
#664 = CARTESIAN_POINT ( 'NONE',  ( -4.458734124999999437, 19.35416666803225993, -2.574251347313719407 ) ) ;
#665 = ORIENTED_EDGE ( 'NONE', *, *, #42137, .T. ) ;
#666 = CARTESIAN_POINT ( 'NONE',  ( 4.458734124999999437, -96.81249999863440792, -5.460374474430324690E-16 ) ) ;
#667 = CARTESIAN_POINT ( 'NONE',  ( -4.999999999999998224, -26.79166666393547658, 2.886751345948131764 ) ) ;
#668 = CARTESIAN_POINT ( 'NONE',  ( 6.874999999999999112, 4.690970937165706900, -7.298562697733104621 ) ) ;
#669 = CARTESIAN_POINT ( 'NONE',  ( 2.229367062499998831, -15.64583333196773651, -3.861377020970580887 ) ) ;
#670 = CYLINDRICAL_SURFACE ( 'NONE', #55063, 5.000000000000000000 ) ;
#671 = CARTESIAN_POINT ( 'NONE',  ( 2.499999999999998668, 8.791666669397853795, -4.330127018922193649 ) ) ;
#672 = CARTESIAN_POINT ( 'NONE',  ( -54.64476657466781973, -150.8125000013656063, -4.444560631937228834 ) ) ;
#673 = CARTESIAN_POINT ( 'NONE',  ( 5.000000000000000000, -42.29166666393548724, -2.886751345948129988 ) ) ;
#674 = CARTESIAN_POINT ( 'NONE',  ( -50.01589407740564042, -148.6250000000000284, 0.3983568153799778022 ) ) ;
#675 = CARTESIAN_POINT ( 'NONE',  ( -2.229367062499996610, 12.85416666803226171, 3.861377020970582219 ) ) ;
#676 = CARTESIAN_POINT ( 'NONE',  ( -6.972266317189433020E-16, -90.12499999726880162, -5.000000000000000000 ) ) ;
#677 = CARTESIAN_POINT ( 'NONE',  ( -5.000000000000000000, -47.87499999726880873, 0.000000000000000000 ) ) ;
#678 = CARTESIAN_POINT ( 'NONE',  ( -4.458734124999999437, 16.60416666803225993, -2.574251347313719407 ) ) ;
#679 = CARTESIAN_POINT ( 'NONE',  ( 2.229367062499998831, -60.64583333196774362, -3.861377020970580887 ) ) ;
#680 = ORIENTED_EDGE ( 'NONE', *, *, #53512, .T. ) ;
#681 = CARTESIAN_POINT ( 'NONE',  ( 2.229367062500001939, -16.22916666530107577, 3.861377020970579999 ) ) ;
#682 = CARTESIAN_POINT ( 'NONE',  ( 5.000000000000000000, 4.583333333333331261, -2.886751345948129988 ) ) ;
#683 = CARTESIAN_POINT ( 'NONE',  ( -4.458734124999999437, -162.9375000013655779, -5.460374474430324690E-16 ) ) ;
#684 = CARTESIAN_POINT ( 'NONE',  ( -6.972266317189433020E-16, -88.25000000000000000, -5.000000000000000000 ) ) ;
#685 = CARTESIAN_POINT ( 'NONE',  ( -4.458734124999999437, -54.31249999863440081, 0.000000000000000000 ) ) ;
#686 = CARTESIAN_POINT ( 'NONE',  ( -2.500000000000000444, -88.04166666393548724, -4.330127018922193649 ) ) ;
#687 = CARTESIAN_POINT ( 'NONE',  ( 4.458734124999999437, -35.81249999863440792, -5.460374474430324690E-16 ) ) ;
#688 = CARTESIAN_POINT ( 'NONE',  ( -5.000000000000000000, -77.00000000000000000, 0.000000000000000000 ) ) ;
#689 = CARTESIAN_POINT ( 'NONE',  ( 5.000000000000000888, -142.0625000027312126, -2.071067811865475505 ) ) ;
#690 = CARTESIAN_POINT ( 'NONE',  ( -3.152801135295367096, -152.3125000013655779, -3.152801135295367541 ) ) ;
#691 = CARTESIAN_POINT ( 'NONE',  ( 2.500000000000002220, -43.66666666666665719, 4.330127018922192761 ) ) ;
#692 = CARTESIAN_POINT ( 'NONE',  ( -4.999999999999998224, -19.79166666393548013, 2.886751345948131764 ) ) ;
#693 = CARTESIAN_POINT ( 'NONE',  ( 2.499999999999998668, -6.208333330602149758, -4.330127018922193649 ) ) ;
#694 = ORIENTED_EDGE ( 'NONE', *, *, #17227, .T. ) ;
#695 = CARTESIAN_POINT ( 'NONE',  ( -2.229367062500000163, -99.47916666530106511, -3.861377020970580443 ) ) ;
#696 = CARTESIAN_POINT ( 'NONE',  ( 4.458734124999999437, 0.9375000013655959696, -5.460374474430324690E-16 ) ) ;
#697 = VECTOR ( 'NONE', #14487, 1000.000000000000114 ) ;
#698 = DIRECTION ( 'NONE',  ( -0.000000000000000000, 1.000000000000000000, -0.000000000000000000 ) ) ;
#699 = CARTESIAN_POINT ( 'NONE',  ( -3.535250795749689387E-16, -2.250000000000001776, -5.773502691896257311 ) ) ;
#700 = AXIS2_PLACEMENT_3D ( 'NONE', #30032, #21038, #15247 ) ;
#701 = CARTESIAN_POINT ( 'NONE',  ( -4.458734124999999437, -65.31249999863440792, 0.000000000000000000 ) ) ;
#702 = CARTESIAN_POINT ( 'NONE',  ( -6.972266317189433020E-16, -31.12499999726880873, -5.000000000000000000 ) ) ;
#703 = CARTESIAN_POINT ( 'NONE',  ( 5.000000000000000000, -4.374999997268816720, -6.123233995736766282E-16 ) ) ;
#705 = ORIENTED_EDGE ( 'NONE', *, *, #8739, .F. ) ;
#704 = CARTESIAN_POINT ( 'NONE',  ( 2.229367062499998831, -36.64583333196773651, -3.861377020970580887 ) ) ;
#706 = CARTESIAN_POINT ( 'NONE',  ( 5.000000000000000000, -33.41666666666666430, -2.886751345948130876 ) ) ;
#707 = CARTESIAN_POINT ( 'NONE',  ( -6.972266317189433020E-16, 12.75000000000000000, -5.000000000000000000 ) ) ;
#708 = ORIENTED_EDGE ( 'NONE', *, *, #40165, .T. ) ;
#709 = CARTESIAN_POINT ( 'NONE',  ( 1.975475456537005874E-15, -104.7500000000000000, 5.000000000000000000 ) ) ;
#710 = CARTESIAN_POINT ( 'NONE',  ( 1.060575238724906964E-15, -49.75000000000000000, 5.773502691896257311 ) ) ;
#712 = CARTESIAN_POINT ( 'NONE',  ( -2.229367062500000163, -27.72916666530107221, -3.861377020970580443 ) ) ;
#711 = CARTESIAN_POINT ( 'NONE',  ( 2.499999999999998668, -46.20833333060214443, -4.330127018922193649 ) ) ;
#713 = CARTESIAN_POINT ( 'NONE',  ( -1.049326080737009628E-13, -4.750000000000003553, 5.000000000000000000 ) ) ;
#714 = CARTESIAN_POINT ( 'NONE',  ( -2.229367062499996610, -76.14583333196773651, 3.861377020970582219 ) ) ;
#715 = CARTESIAN_POINT ( 'NONE',  ( -4.458734125000000326, -142.2500000013656063, -1.846868145590735644 ) ) ;
#716 = CARTESIAN_POINT ( 'NONE',  ( 2.229367062500001939, -82.97916666530106511, 3.861377020970579999 ) ) ;
#717 = CARTESIAN_POINT ( 'NONE',  ( -55.35523342533222291, -139.5625000013656063, 4.444560631937231499 ) ) ;
#718 =( BOUNDED_CURVE ( )  B_SPLINE_CURVE ( 2, ( #63086, #49224, #9661, #38930, #18996, #18689, #48584, #44388, #39244 ),
 .UNSPECIFIED., .F., .F. ) 
 B_SPLINE_CURVE_WITH_KNOTS ( ( 3, 2, 2, 2, 3 ),
 ( 0.4874999999999999889, 0.4880952380952380820, 0.4892857142857142683, 0.4904761904761904545, 0.4910714285714285476 ),
 .UNSPECIFIED. ) 
 CURVE ( )  GEOMETRIC_REPRESENTATION_ITEM ( )  RATIONAL_B_SPLINE_CURVE ( ( 0.9330127018922194093, 0.9330127018922194093, 1.000000000000000000, 0.8660254037844387076, 1.000000000000000000, 0.8660254037844387076, 1.000000000000000000, 0.9330127018922194093, 0.9330127018922194093 ) ) 
 REPRESENTATION_ITEM ( '' )  );
#719 = CARTESIAN_POINT ( 'NONE',  ( -4.458734124999999437, -30.56249999863440436, 0.000000000000000000 ) ) ;
#720 = CARTESIAN_POINT ( 'NONE',  ( 2.500000000000002220, -69.54166666393547303, 4.330127018922192761 ) ) ;
#721 = VERTEX_POINT ( 'NONE', #29522 ) ;
#722 = DIRECTION ( 'NONE',  ( -0.000000000000000000, 1.000000000000000000, -0.000000000000000000 ) ) ;
#723 = ORIENTED_EDGE ( 'NONE', *, *, #22917, .T. ) ;
#724 = CARTESIAN_POINT ( 'NONE',  ( 2.229367062500001939, -74.22916666530106511, 3.861377020970579999 ) ) ;
#725 = CARTESIAN_POINT ( 'NONE',  ( 4.458734124999999437, -139.4375000013656063, 0.000000000000000000 ) ) ;
#726 = SURFACE_SIDE_STYLE ('',( #44126 ) ) ;
#727 = VERTEX_POINT ( 'NONE', #55274 ) ;
#728 = CARTESIAN_POINT ( 'NONE',  ( -52.53715891517739323, -140.4375000000000000, -4.819101127000233298 ) ) ;
#729 = CARTESIAN_POINT ( 'NONE',  ( 1.975475456537005874E-15, 8.249999999999998224, 5.000000000000000000 ) ) ;
#731 = ADVANCED_FACE ( 'NONE', ( #5418 ), #49793, .T. ) ;
#730 = CARTESIAN_POINT ( 'NONE',  ( -2.229367062499996610, -57.39583333196773651, 3.861377020970582219 ) ) ;
#732 = CARTESIAN_POINT ( 'NONE',  ( 9.457646018065525792E-16, -6.312499998634404363, 5.148502694627439702 ) ) ;
#733 = VERTEX_POINT ( 'NONE', #1567 ) ;
#734 =( BOUNDED_CURVE ( )  B_SPLINE_CURVE ( 2, ( #5253, #25183, #5897, #6215, #53814, #24875, #40300, #44476, #54130 ),
 .UNSPECIFIED., .F., .F. ) 
 B_SPLINE_CURVE_WITH_KNOTS ( ( 3, 2, 2, 2, 3 ),
 ( 0.6249999999999996669, 0.6291666666666663188, 0.6333333333333328596, 0.6374999999999995115, 0.6416666666666662744 ),
 .UNSPECIFIED. ) 
 CURVE ( )  GEOMETRIC_REPRESENTATION_ITEM ( )  RATIONAL_B_SPLINE_CURVE ( ( 1.000000000000005995, 0.9238795325112806323, 1.000000000000000000, 0.9238795325112867385, 1.000000000000000000, 0.9238795325112867385, 1.000000000000000000, 0.9238795325112948431, 0.9999999999999918954 ) ) 
 REPRESENTATION_ITEM ( '' )  );
#735 = CARTESIAN_POINT ( 'NONE',  ( -3.535533905932737309, -146.6250000000000000, -3.535533905932738197 ) ) ;
#736 = CARTESIAN_POINT ( 'NONE',  ( 1.339745962155615144, -91.70534180126148271, 4.999999999999999112 ) ) ;
#737 = CARTESIAN_POINT ( 'NONE',  ( -4.458734124999999437, 13.68750000136559386, 0.000000000000000000 ) ) ;
#738 = CARTESIAN_POINT ( 'NONE',  ( -50.40829686548195099, -141.0000000013656063, -1.485763867205728284 ) ) ;
#739 = CARTESIAN_POINT ( 'NONE',  ( 1.339745962155612702, -47.16965819600733312, -5.000000000000000000 ) ) ;
#740 = CARTESIAN_POINT ( 'NONE',  ( -3.152801135295367985, -162.8125000013656063, 3.152801135295367096 ) ) ;
#741 = CARTESIAN_POINT ( 'NONE',  ( 0.000000000000000000, -170.0000000000000000, 5.000000000000000000 ) ) ;
#742 = ORIENTED_EDGE ( 'NONE', *, *, #8306, .T. ) ;
#743 = CARTESIAN_POINT ( 'NONE',  ( 4.458734125000000326, -83.89583333196773651, 2.574251347313718519 ) ) ;
#744 = CARTESIAN_POINT ( 'NONE',  ( 2.229367062500001939, 2.020833334698927786, 3.861377020970579999 ) ) ;
#745 = CARTESIAN_POINT ( 'NONE',  ( -6.972266317189433020E-16, -71.12499999726878741, -5.000000000000000000 ) ) ;
#746 = VECTOR ( 'NONE', #26616, 1000.000000000000000 ) ;
#747 = CARTESIAN_POINT ( 'NONE',  ( 2.500000000000002220, -85.66666666666667140, 4.330127018922192761 ) ) ;
#748 = EDGE_CURVE ( 'NONE', #5879, #5467, #50758, .T. ) ;
#749 = CARTESIAN_POINT ( 'NONE',  ( -7.500000000000000888, -3.608439182435167591, -7.298562697733108173 ) ) ;
#750 = CARTESIAN_POINT ( 'NONE',  ( -2.229367062499996610, -67.39583333196773651, 3.861377020970582219 ) ) ;
#751 = VECTOR ( 'NONE', #62223, 1000.000000000000000 ) ;
#752 = CARTESIAN_POINT ( 'NONE',  ( 5.000000000000000000, -26.29166666393547658, -2.886751345948129988 ) ) ;
#753 = EDGE_CURVE ( 'NONE', #43561, #42376, #30645, .T. ) ;
#754 = CARTESIAN_POINT ( 'NONE',  ( -5.000000000000000000, -21.08333333333333570, -2.886751345948128211 ) ) ;
#755 = CARTESIAN_POINT ( 'NONE',  ( 5.000000000000000000, -78.37499999726881583, -6.123233995736766282E-16 ) ) ;
#756 = CARTESIAN_POINT ( 'NONE',  ( -1.230605004983934782E-13, -37.62499999726881583, 5.000000000000000000 ) ) ;
#757 = CARTESIAN_POINT ( 'NONE',  ( 0.000000000000000000, -120.0000000000000000, 0.000000000000000000 ) ) ;
#758 = CARTESIAN_POINT ( 'NONE',  ( 4.458734125000001214, -44.89583333196774362, 2.574251347313718519 ) ) ;
#759 = CARTESIAN_POINT ( 'NONE',  ( 4.458734125000000326, -32.14583333196773651, 2.574251347313718519 ) ) ;
#760 = CARTESIAN_POINT ( 'NONE',  ( -3.152548672688508926E-16, 5.187500001365592972, -5.148502694627439702 ) ) ;
#761 = CARTESIAN_POINT ( 'NONE',  ( 3.061616997868383141E-16, -145.8750000027312126, -5.000000000000000000 ) ) ;
#762 = CARTESIAN_POINT ( 'NONE',  ( -4.999999999999999112, 18.08333333333333570, 2.886751345948131764 ) ) ;
#763 = CARTESIAN_POINT ( 'NONE',  ( 2.071067811865475505, -148.9375000027311842, -5.000000000000000888 ) ) ;
#764 = CARTESIAN_POINT ( 'NONE',  ( -49.85088928181150436, -154.5625000000000000, -1.666127454062680480 ) ) ;
#765 = CARTESIAN_POINT ( 'NONE',  ( -3.152548672688508926E-16, -37.56249999863440792, -5.148502694627439702 ) ) ;
#766 = CARTESIAN_POINT ( 'NONE',  ( 2.500000000000002220, -73.54166666393548724, 4.330127018922192761 ) ) ;
#767 = EDGE_CURVE ( 'NONE', #37188, #62028, #48666, .T. ) ;
#768 = CARTESIAN_POINT ( 'NONE',  ( -55.35523342533222291, -143.5625000013656063, 4.444560631937231499 ) ) ;
#769 = CARTESIAN_POINT ( 'NONE',  ( -55.00000000000002132, -155.0000000000000284, 1.734723475976807094E-15 ) ) ;
#770 = CARTESIAN_POINT ( 'NONE',  ( 1.211595439868046853, -7.960739084487661543, -0.4504974108212073114 ) ) ;
#771 = CARTESIAN_POINT ( 'NONE',  ( 2.229367062500001939, -81.22916666530106511, 3.861377020970579999 ) ) ;
#772 = CARTESIAN_POINT ( 'NONE',  ( 4.458734124999997661, -165.7500000013655779, 1.846868145590737864 ) ) ;
#773 = LINE ( 'NONE', #20380, #16323 ) ;
#774 = CARTESIAN_POINT ( 'NONE',  ( -58.24261429053147765, -136.2500000000000284, -3.805975901505573855 ) ) ;
#775 = CARTESIAN_POINT ( 'NONE',  ( 2.499999999999998668, -26.33333333333333215, -4.330127018922193649 ) ) ;
#776 = CARTESIAN_POINT ( 'NONE',  ( -8.190561711645485556E-16, -142.6875000013656063, 4.458734124999999437 ) ) ;
#777 = ORIENTED_EDGE ( 'NONE', *, *, #29470, .F. ) ;
#778 = CARTESIAN_POINT ( 'NONE',  ( -3.152548672688508926E-16, 27.18750000136559564, -5.148502694627439702 ) ) ;
#779 = ORIENTED_EDGE ( 'NONE', *, *, #28315, .T. ) ;
#780 = CARTESIAN_POINT ( 'NONE',  ( -4.458734124999999437, -63.56249999863440792, 0.000000000000000000 ) ) ;
#781 = CARTESIAN_POINT ( 'NONE',  ( 2.500000000000002220, 19.45833333606451632, 4.330127018922192761 ) ) ;
#782 = CARTESIAN_POINT ( 'NONE',  ( -54.60164318462004474, -138.5000000027312126, -4.984105922594373794 ) ) ;
#783 = CARTESIAN_POINT ( 'NONE',  ( -2.499999999999996447, 11.16666666666666430, 4.330127018922195425 ) ) ;
#784 = CARTESIAN_POINT ( 'NONE',  ( 2.229367062499998831, -48.64583333196772941, -3.861377020970580887 ) ) ;
#785 = CARTESIAN_POINT ( 'NONE',  ( -2.229367062499996610, -13.14583333196774007, 3.861377020970582219 ) ) ;
#786 = CARTESIAN_POINT ( 'NONE',  ( -5.000000000000000888, -168.5625000000000000, -2.071067811865475949 ) ) ;
#787 = EDGE_CURVE ( 'NONE', #24503, #3031, #46626, .T. ) ;
#788 = CARTESIAN_POINT ( 'NONE',  ( 2.499999999999998668, 15.79166666939785202, -4.330127018922193649 ) ) ;
#789 = CYLINDRICAL_SURFACE ( 'NONE', #24783, 5.000000000000000000 ) ;
#790 = FACE_OUTER_BOUND ( 'NONE', #10460, .T. ) ;
#792 = CARTESIAN_POINT ( 'NONE',  ( 4.458734124999999437, -18.81249999863440792, -5.460374474430324690E-16 ) ) ;
#791 =( BOUNDED_CURVE ( )  B_SPLINE_CURVE ( 2, ( #30635, #1396, #6523, #20997, #32143, #60247, #35791, #26135, #30955 ),
 .UNSPECIFIED., .F., .F. ) 
 B_SPLINE_CURVE_WITH_KNOTS ( ( 3, 2, 2, 2, 3 ),
 ( 0.8145833333333333259, 0.8152777777777777679, 0.8166666666666666519, 0.8180555555555555358, 0.8187499999999999778 ),
 .UNSPECIFIED. ) 
 CURVE ( )  GEOMETRIC_REPRESENTATION_ITEM ( )  RATIONAL_B_SPLINE_CURVE ( ( 0.9330127018922194093, 0.9330127018922194093, 1.000000000000000000, 0.8660254037844387076, 1.000000000000000000, 0.8660254037844387076, 1.000000000000000000, 0.9330127018922194093, 0.9330127018922194093 ) ) 
 REPRESENTATION_ITEM ( '' )  );
#793 = AXIS2_PLACEMENT_3D ( 'NONE', #44537, #6276, #15274 ) ;
#794 = CARTESIAN_POINT ( 'NONE',  ( 3.061616997868383141E-16, -140.8750000027312126, -5.000000000000000000 ) ) ;
#795 = CARTESIAN_POINT ( 'NONE',  ( -4.458734124999998549, -52.22916666530106511, 2.574251347313722516 ) ) ;
#796 = CARTESIAN_POINT ( 'NONE',  ( -4.458734124999999437, -157.1875000013655779, -5.460374474430324690E-16 ) ) ;
#797 = VECTOR ( 'NONE', #12996, 1000.000000000000000 ) ;
#798 = PRESENTATION_LAYER_ASSIGNMENT (  '', '', ( #36743 ) ) ;
#799 = CARTESIAN_POINT ( 'NONE',  ( -3.535250795749689387E-16, -56.12499999726880162, -5.773502691896257311 ) ) ;
#800 = VERTEX_POINT ( 'NONE', #21492 ) ;
#801 = CARTESIAN_POINT ( 'NONE',  ( 2.499999999999998668, 13.66666666666666785, -4.330127018922193649 ) ) ;
#802 = CARTESIAN_POINT ( 'NONE',  ( 9.457646018065525792E-16, 2.687500001365594304, 5.148502694627439702 ) ) ;
#803 = ORIENTED_EDGE ( 'NONE', *, *, #57131, .F. ) ;
#805 = CARTESIAN_POINT ( 'NONE',  ( -2.499999999999996447, -28.83333333333333570, 4.330127018922195425 ) ) ;
#804 = CARTESIAN_POINT ( 'NONE',  ( -56.66612745406293783, -141.3125000000000000, -5.149110718188535607 ) ) ;
#806 = CARTESIAN_POINT ( 'NONE',  ( -4.458734125000001214, -154.8750000013655779, 1.846868145590734089 ) ) ;
#807 = ORIENTED_EDGE ( 'NONE', *, *, #51943, .T. ) ;
#808 = CARTESIAN_POINT ( 'NONE',  ( 5.000000000000000888, -83.58333333333332860, 2.886751345948126879 ) ) ;
#809 = CARTESIAN_POINT ( 'NONE',  ( -58.80597590150559739, -130.0000000000000284, 3.242614290531460330 ) ) ;
#810 = CARTESIAN_POINT ( 'NONE',  ( 5.000000000000000888, 15.41666666666666607, 2.886751345948126879 ) ) ;
#812 = EDGE_CURVE ( 'NONE', #28481, #7216, #43781, .T. ) ;
#811 = CARTESIAN_POINT ( 'NONE',  ( -4.458734124999999437, -40.56249999863440081, 0.000000000000000000 ) ) ;
#813 = ORIENTED_EDGE ( 'NONE', *, *, #11033, .F. ) ;
#814 = EDGE_CURVE ( 'NONE', #10657, #17293, #229, .T. ) ;
#815 = EDGE_CURVE ( 'NONE', #26195, #10433, #15444, .T. ) ;
#816 = CARTESIAN_POINT ( 'NONE',  ( 1.975475456537005874E-15, 9.375000002731185944, 5.000000000000000000 ) ) ;
#817 = CARTESIAN_POINT ( 'NONE',  ( 4.458734124999998549, 12.27083333469892423, -2.574251347313721627 ) ) ;
#818 = CARTESIAN_POINT ( 'NONE',  ( -4.458734124999998549, -89.47916666530106511, 2.574251347313722516 ) ) ;
#819 = CARTESIAN_POINT ( 'NONE',  ( -57.19623071787017210, -154.3750000013656063, 4.297418129356382899 ) ) ;
#820 = CARTESIAN_POINT ( 'NONE',  ( -5.000000000000000888, -165.4375000000000284, 2.071067811865474617 ) ) ;
#821 = DIRECTION ( 'NONE',  ( 0.000000000000000000, -0.000000000000000000, -1.000000000000000000 ) ) ;
#822 = DIRECTION ( 'NONE',  ( 0.000000000000000000, -1.000000000000000000, 0.000000000000000000 ) ) ;
#823 = CARTESIAN_POINT ( 'NONE',  ( 9.457646018065525792E-16, -66.06249999863440792, 5.148502694627439702 ) ) ;
#824 = CARTESIAN_POINT ( 'NONE',  ( 6.658902113225075858, 5.287118297641098863, -7.776713651267108673 ) ) ;
#825 = CARTESIAN_POINT ( 'NONE',  ( 9.457646018065525792E-16, 17.93750000136559208, 5.148502694627439702 ) ) ;
#826 = EDGE_CURVE ( 'NONE', #33613, #46845, #17878, .T. ) ;
#827 = CARTESIAN_POINT ( 'NONE',  ( -1.339745962155613812, -79.08034179853028434, -5.000000000000000000 ) ) ;
#828 = CARTESIAN_POINT ( 'NONE',  ( 3.061616997868383141E-16, -156.8750000027311842, -5.000000000000000000 ) ) ;
#829 = CARTESIAN_POINT ( 'NONE',  ( -3.152548672688508926E-16, -47.81249999863440792, -5.148502694627439702 ) ) ;
#830 = CARTESIAN_POINT ( 'NONE',  ( 2.499999999999998668, -9.208333330602146205, -4.330127018922193649 ) ) ;
#831 = CARTESIAN_POINT ( 'NONE',  ( 2.499999999999998668, -42.20833333060214443, -4.330127018922193649 ) ) ;
#832 = ADVANCED_FACE ( 'NONE', ( #17290 ), #62370, .T. ) ;
#833 = CARTESIAN_POINT ( 'NONE',  ( 0.000000000000000000, -170.0000000000000000, 5.000000000000000000 ) ) ;
#834 = CARTESIAN_POINT ( 'NONE',  ( -3.152548672688508926E-16, -88.81249999863439371, -5.148502694627439702 ) ) ;
#835 = CARTESIAN_POINT ( 'NONE',  ( -6.972266317189433020E-16, -104.1249999972688016, -5.000000000000000000 ) ) ;
#836 = CARTESIAN_POINT ( 'NONE',  ( -4.458734124999999437, -18.56249999863440792, 0.000000000000000000 ) ) ;
#837 = ORIENTED_EDGE ( 'NONE', *, *, #19159, .T. ) ;
#838 = AXIS2_PLACEMENT_3D ( 'NONE', #60962, #8190, #7248 ) ;
#839 =( BOUNDED_CURVE ( )  B_SPLINE_CURVE ( 2, ( #2821, #22441, #42037, #31760, #12459, #52018, #26621, #2503, #46562 ),
 .UNSPECIFIED., .F., .F. ) 
 B_SPLINE_CURVE_WITH_KNOTS ( ( 3, 2, 2, 2, 3 ),
 ( 0.2232142857142857262, 0.2238095238095238193, 0.2250000000000000056, 0.2261904761904761918, 0.2267857142857142849 ),
 .UNSPECIFIED. ) 
 CURVE ( )  GEOMETRIC_REPRESENTATION_ITEM ( )  RATIONAL_B_SPLINE_CURVE ( ( 0.9330127018922194093, 0.9330127018922209636, 1.000000000000000000, 0.8660254037844387076, 1.000000000000000000, 0.8660254037844387076, 1.000000000000000000, 0.9330127018922194093, 0.9330127018922194093 ) ) 
 REPRESENTATION_ITEM ( '' )  );
#840 = CARTESIAN_POINT ( 'NONE',  ( -2.071067811865470620, -169.3125000000000000, 5.000000000000007105 ) ) ;
#841 = CARTESIAN_POINT ( 'NONE',  ( 9.457646018065525792E-16, -104.0624999986344221, 5.148502694627439702 ) ) ;
#842 = CARTESIAN_POINT ( 'NONE',  ( 3.535533905932736864, -162.2500000027312126, 3.535533905932738641 ) ) ;
#843 = ORIENTED_EDGE ( 'NONE', *, *, #20028, .F. ) ;
#844 = CARTESIAN_POINT ( 'NONE',  ( 4.458734124999998549, -95.97916666530107932, -2.574251347313721627 ) ) ;
#845 = LINE ( 'NONE', #44235, #60304 ) ;
#846 = CARTESIAN_POINT ( 'NONE',  ( 5.000000000000000000, -57.37499999726880162, -6.123233995736766282E-16 ) ) ;
#847 = FACE_OUTER_BOUND ( 'NONE', #58279, .T. ) ;
#848 = CARTESIAN_POINT ( 'NONE',  ( -56.48576386720575471, -124.7500000013655921, -4.591703134518078322 ) ) ;
#849 = CARTESIAN_POINT ( 'NONE',  ( -55.35523342533222291, -142.3125000013656063, 4.444560631937231499 ) ) ;
#850 = CARTESIAN_POINT ( 'NONE',  ( 2.229367062499998831, -19.64583333196774007, -3.861377020970580887 ) ) ;
#851 = CARTESIAN_POINT ( 'NONE',  ( -2.229367062499996610, 6.604166668032259935, 3.861377020970582219 ) ) ;
#852 = CARTESIAN_POINT ( 'NONE',  ( -3.152548672688508926E-16, -65.81249999863440792, -5.148502694627439702 ) ) ;
#853 = CYLINDRICAL_SURFACE ( 'NONE', #14086, 5.000000000000000000 ) ;
#854 = CARTESIAN_POINT ( 'NONE',  ( 9.457646018065525792E-16, -22.06249999863440436, 5.148502694627439702 ) ) ;
#855 = CYLINDRICAL_SURFACE ( 'NONE', #41979, 5.000000000000000000 ) ;
#856 = CARTESIAN_POINT ( 'NONE',  ( -2.071067811865475061, -156.6875000000000284, -5.000000000000000888 ) ) ;
#857 = CARTESIAN_POINT ( 'NONE',  ( -3.535250795749689387E-16, -11.25000000000000355, -5.773502691896257311 ) ) ;
#858 = CARTESIAN_POINT ( 'NONE',  ( -4.458734125000001214, -154.8750000013655779, 1.846868145590734089 ) ) ;
#859 = VERTEX_POINT ( 'NONE', #36915 ) ;
#860 = CARTESIAN_POINT ( 'NONE',  ( -2.229367062500000163, -44.72916666530106511, -3.861377020970580443 ) ) ;
#861 = CARTESIAN_POINT ( 'NONE',  ( -6.972266317189433020E-16, -2.250000000000000000, -5.000000000000000000 ) ) ;
#862 = CARTESIAN_POINT ( 'NONE',  ( 2.499999999999998668, -38.20833333060213732, -4.330127018922193649 ) ) ;
#863 = CARTESIAN_POINT ( 'NONE',  ( 4.458734124999998549, -89.72916666530106511, -2.574251347313721627 ) ) ;
#864 = CARTESIAN_POINT ( 'NONE',  ( 4.458734124999999437, 12.18750000136559564, -5.460374474430324690E-16 ) ) ;
#865 = CARTESIAN_POINT ( 'NONE',  ( -6.972266317189433020E-16, -89.12499999726880162, -5.000000000000000000 ) ) ;
#866 = CARTESIAN_POINT ( 'NONE',  ( -4.999999999999998224, -6.916666666666667851, 2.886751345948131764 ) ) ;
#867 = CARTESIAN_POINT ( 'NONE',  ( -5.000000000000000000, 25.91666666666666430, -2.886751345948128211 ) ) ;
#868 = CARTESIAN_POINT ( 'NONE',  ( 4.458734124999999437, 19.93750000136559208, -5.460374474430324690E-16 ) ) ;
#869 = CARTESIAN_POINT ( 'NONE',  ( 1.060575238724906964E-15, -76.74999999999998579, 5.773502691896257311 ) ) ;
#870 = CARTESIAN_POINT ( 'NONE',  ( -5.000000000000000000, 8.041666669397852019, -2.886751345948128211 ) ) ;
#871 = VERTEX_POINT ( 'NONE', #17616 ) ;
#872 = DIRECTION ( 'NONE',  ( 0.000000000000000000, 0.000000000000000000, 1.000000000000000000 ) ) ;
#873 = ORIENTED_EDGE ( 'NONE', *, *, #21285, .T. ) ;
#874 = CARTESIAN_POINT ( 'NONE',  ( 5.000000000000000888, 26.41666666666666430, 2.886751345948126879 ) ) ;
#875 = CARTESIAN_POINT ( 'NONE',  ( 2.229367062500001939, -37.97916666530107221, 3.861377020970579999 ) ) ;
#876 = CARTESIAN_POINT ( 'NONE',  ( -2.499999999999996447, -37.70833333060213732, 4.330127018922195425 ) ) ;
#877 = ORIENTED_EDGE ( 'NONE', *, *, #37498, .T. ) ;
#878 = CARTESIAN_POINT ( 'NONE',  ( 4.458734124999999437, -12.81249999863440259, -5.460374474430324690E-16 ) ) ;
#880 = EDGE_LOOP ( 'NONE', ( #32343, #38666, #26508, #29732 ) ) ;
#879 = CARTESIAN_POINT ( 'NONE',  ( -3.152548672688508926E-16, -20.81249999863440081, -5.148502694627439702 ) ) ;
#881 = CARTESIAN_POINT ( 'NONE',  ( -2.499999999999996447, -83.83333333333332860, 4.330127018922195425 ) ) ;
#882 = CARTESIAN_POINT ( 'NONE',  ( 2.730187237215162345E-16, -167.1875000013655779, -4.458734124999999437 ) ) ;
#883 = CARTESIAN_POINT ( 'NONE',  ( 2.229367062500001939, -60.22916666530106511, 3.861377020970579999 ) ) ;
#884 = VECTOR ( 'NONE', #20351, 1000.000000000000000 ) ;
#885 = CARTESIAN_POINT ( 'NONE',  ( -5.000000000000000000, -88.95833333060214443, -2.886751345948128211 ) ) ;
#887 = ORIENTED_EDGE ( 'NONE', *, *, #35445, .T. ) ;
#886 = CARTESIAN_POINT ( 'NONE',  ( -1.339745962155613812, -49.08034179853029144, -5.000000000000000000 ) ) ;
#888 = CARTESIAN_POINT ( 'NONE',  ( -51.75738570946856498, -139.7500000000000000, 3.805975901505576964 ) ) ;
#889 = VECTOR ( 'NONE', #11375, 1000.000000000000000 ) ;
#890 = CARTESIAN_POINT ( 'NONE',  ( -4.458734124999999437, -25.64583333196773651, -2.574251347313719407 ) ) ;
#891 = CARTESIAN_POINT ( 'NONE',  ( 5.000000000000000000, -5.374999997268811391, -6.123233995736766282E-16 ) ) ;
#892 = ORIENTED_EDGE ( 'NONE', *, *, #43199, .T. ) ;
#893 = EDGE_CURVE ( 'NONE', #33079, #5936, #31021, .T. ) ;
#894 = CARTESIAN_POINT ( 'NONE',  ( 3.152801135295366208, -164.8125000013656063, 3.152801135295367985 ) ) ;
#895 = CARTESIAN_POINT ( 'NONE',  ( 4.458734124999999437, -108.0624999986343937, -5.460374474430324690E-16 ) ) ;
#896 = CARTESIAN_POINT ( 'NONE',  ( 5.000000000000000000, -156.0625000000000284, 2.071067811865478614 ) ) ;
#897 = VERTEX_POINT ( 'NONE', #11818 ) ;
#898 = CARTESIAN_POINT ( 'NONE',  ( -59.59170313451810586, -146.7500000013656063, 1.485763867205729394 ) ) ;
#899 = CARTESIAN_POINT ( 'NONE',  ( -4.458734124999999437, -74.64583333196773651, -2.574251347313719407 ) ) ;
#900 = CARTESIAN_POINT ( 'NONE',  ( -60.14911071818854538, -134.1875000027312410, 1.666127454062681368 ) ) ;
#901 = CARTESIAN_POINT ( 'NONE',  ( 4.458734124999998549, -44.72916666530106511, -2.574251347313721627 ) ) ;
#902 = CARTESIAN_POINT ( 'NONE',  ( 2.730187237215162345E-16, -142.4375000013656063, -4.458734124999999437 ) ) ;
#903 = ADVANCED_FACE ( 'NONE', ( #7018 ), #46246, .T. ) ;
#904 = DIRECTION ( 'NONE',  ( -0.000000000000000000, 1.000000000000000000, -0.000000000000000000 ) ) ;
#905 = CARTESIAN_POINT ( 'NONE',  ( -4.458734124999999437, -49.39583333196772230, -2.574251347313719407 ) ) ;
#906 = CARTESIAN_POINT ( 'NONE',  ( 4.648177544792955347E-16, 29.75000000000000355, -5.000000000000000000 ) ) ;
#907 = ADVANCED_FACE ( 'NONE', ( #28824 ), #9520, .T. ) ;
#908 = CARTESIAN_POINT ( 'NONE',  ( 2.229367062499998831, -16.64583333196773651, -3.861377020970580887 ) ) ;
#909 = EDGE_CURVE ( 'NONE', #38980, #44900, #59788, .T. ) ;
#910 = AXIS2_PLACEMENT_3D ( 'NONE', #36745, #7477, #56375 ) ;
#911 = CARTESIAN_POINT ( 'NONE',  ( -2.499999999999996447, -102.8333333333333286, 4.330127018922195425 ) ) ;
#912 = CARTESIAN_POINT ( 'NONE',  ( 4.458734124999999437, -139.7500000013655779, 1.846868145590737864 ) ) ;
#913 = CARTESIAN_POINT ( 'NONE',  ( -3.152548672688508926E-16, -32.81249999863440792, -5.148502694627439702 ) ) ;
#914 = CARTESIAN_POINT ( 'NONE',  ( -2.500000000000000444, 5.958333336064519870, -4.330127018922193649 ) ) ;
#915 = CARTESIAN_POINT ( 'NONE',  ( -4.999999999999998224, -39.79166666393548013, 2.886751345948131764 ) ) ;
#916 = CARTESIAN_POINT ( 'NONE',  ( -52.80376928212989185, -128.8750000013656063, -4.297418129356379346 ) ) ;
#917 = CARTESIAN_POINT ( 'NONE',  ( 2.229367062500001939, -74.22916666530106511, 3.861377020970579999 ) ) ;
#918 = ADVANCED_FACE ( 'NONE', ( #38177 ), #14029, .T. ) ;
#919 = CARTESIAN_POINT ( 'NONE',  ( -5.000000000000000888, -166.5625000000000000, -2.071067811865475949 ) ) ;
#920 = CARTESIAN_POINT ( 'NONE',  ( -2.499999999999996447, -0.7083333306021483144, 4.330127018922195425 ) ) ;
#921 = DIRECTION ( 'NONE',  ( -0.000000000000000000, 1.000000000000000000, -0.000000000000000000 ) ) ;
#922 = CARTESIAN_POINT ( 'NONE',  ( 4.458734124999998549, -2.979166665301069106, -2.574251347313721627 ) ) ;
#923 = ORIENTED_EDGE ( 'NONE', *, *, #19611, .T. ) ;
#924 = CARTESIAN_POINT ( 'NONE',  ( 1.975475456537005874E-15, 16.37500000273118417, 5.000000000000000000 ) ) ;
#925 = ADVANCED_FACE ( 'NONE', ( #42359 ), #3454, .T. ) ;
#926 = CARTESIAN_POINT ( 'NONE',  ( -6.972266317189433020E-16, 14.87500000273118594, -5.000000000000000000 ) ) ;
#928 = CARTESIAN_POINT ( 'NONE',  ( 4.458734124999998549, -36.72916666530107221, -2.574251347313721627 ) ) ;
#927 = CARTESIAN_POINT ( 'NONE',  ( -4.458734124999998549, -90.22916666530106511, 2.574251347313722516 ) ) ;
#929 = CARTESIAN_POINT ( 'NONE',  ( -1.339745962155660663, -4.794658198738521726, 4.999999999999972466 ) ) ;
#930 = CARTESIAN_POINT ( 'NONE',  ( -3.152548672688508926E-16, -82.81249999863442213, -5.148502694627439702 ) ) ;
#931 = CARTESIAN_POINT ( 'NONE',  ( 2.229367062500001939, 18.77083333469892779, 3.861377020970579999 ) ) ;
#932 = FACE_OUTER_BOUND ( 'NONE', #29020, .T. ) ;
#933 =( BOUNDED_CURVE ( )  B_SPLINE_CURVE ( 2, ( #61186, #36731, #45181, #61505, #52157, #37669, #30381, #11955, #12285 ),
 .UNSPECIFIED., .F., .F. ) 
 B_SPLINE_CURVE_WITH_KNOTS ( ( 3, 2, 2, 2, 3 ),
 ( 0.2250000000000001998, 0.2291666666666668517, 0.2333333333333335313, 0.2375000000000001832, 0.2416666666666668628 ),
 .UNSPECIFIED. ) 
 CURVE ( )  GEOMETRIC_REPRESENTATION_ITEM ( )  RATIONAL_B_SPLINE_CURVE ( ( 0.9999999999999964473, 0.9238795325112902912, 1.000000000000000000, 0.9238795325112867385, 1.000000000000000000, 0.9238795325112867385, 1.000000000000000000, 0.9238795325112831858, 1.000000000000003553 ) ) 
 REPRESENTATION_ITEM ( '' )  );
#934 = CARTESIAN_POINT ( 'NONE',  ( -52.80376928212989185, -138.8750000013655779, -4.297418129356379346 ) ) ;
#935 = ADVANCED_FACE ( 'NONE', ( #47504 ), #8278, .T. ) ;
#936 = CARTESIAN_POINT ( 'NONE',  ( 2.229367062499998831, -0.6458333319677399542, -3.861377020970580887 ) ) ;
#937 = CARTESIAN_POINT ( 'NONE',  ( -4.458734124999999437, 19.35416666803225993, -2.574251347313719407 ) ) ;
#938 = CARTESIAN_POINT ( 'NONE',  ( -2.229367062500000163, -49.72916666530107221, -3.861377020970580443 ) ) ;
#939 = CARTESIAN_POINT ( 'NONE',  ( 1.339745962155612702, -11.29465819873852261, -5.000000000000000000 ) ) ;
#940 = CARTESIAN_POINT ( 'NONE',  ( 2.229367062500001939, -84.97916666530107932, 3.861377020970579999 ) ) ;
#941 = CARTESIAN_POINT ( 'NONE',  ( 4.458734125000000326, -2.895833331967738289, 2.574251347313718519 ) ) ;
#942 = VERTEX_POINT ( 'NONE', #28513 ) ;
#943 = CARTESIAN_POINT ( 'NONE',  ( -2.229367062499996610, -30.39583333196773651, 3.861377020970582219 ) ) ;
#944 = AXIS2_PLACEMENT_3D ( 'NONE', #18569, #57192, #3782 ) ;
#945 = CARTESIAN_POINT ( 'NONE',  ( -52.80376928212989185, -130.1250000013656347, -4.297418129356379346 ) ) ;
#946 = CARTESIAN_POINT ( 'NONE',  ( -4.458734124999998549, -73.22916666530106511, 2.574251347313722516 ) ) ;
#947 = CARTESIAN_POINT ( 'NONE',  ( -3.535250795749689387E-16, -109.1249999972687874, -5.773502691896257311 ) ) ;
#948 = VECTOR ( 'NONE', #51988, 1000.000000000000000 ) ;
#949 = CARTESIAN_POINT ( 'NONE',  ( -4.458734124999998549, 25.77083333469892779, 2.574251347313722516 ) ) ;
#950 = CARTESIAN_POINT ( 'NONE',  ( 5.000000000000000888, -58.45833333060214443, 2.886751345948126879 ) ) ;
#951 = DIRECTION ( 'NONE',  ( 0.000000000000000000, -1.000000000000000000, 0.000000000000000000 ) ) ;
#952 = CARTESIAN_POINT ( 'NONE',  ( -3.152548672688508926E-16, -80.81249999863440792, -5.148502694627439702 ) ) ;
#953 = CARTESIAN_POINT ( 'NONE',  ( -4.999999999999999112, -58.91666666666665719, 2.886751345948131764 ) ) ;
#954 = CARTESIAN_POINT ( 'NONE',  ( -5.000000000000000000, -75.08333333333332860, -2.886751345948128211 ) ) ;
#955 = CARTESIAN_POINT ( 'NONE',  ( -3.535250795749689387E-16, 21.87500000273118062, -5.773502691896257311 ) ) ;
#956 = ORIENTED_EDGE ( 'NONE', *, *, #28390, .F. ) ;
#957 = FACE_OUTER_BOUND ( 'NONE', #20802, .T. ) ;
#958 = CARTESIAN_POINT ( 'NONE',  ( 1.975475456537005874E-15, -98.74999999999998579, 5.000000000000000000 ) ) ;
#960 = CARTESIAN_POINT ( 'NONE',  ( -2.499999999999996447, -20.83333333333333570, 4.330127018922195425 ) ) ;
#959 = CARTESIAN_POINT ( 'NONE',  ( 5.000000000000000000, -170.0000000000000000, 0.000000000000000000 ) ) ;
#961 = CARTESIAN_POINT ( 'NONE',  ( 4.458734124999999437, -20.81249999863440081, -5.460374474430324690E-16 ) ) ;
#962 = CARTESIAN_POINT ( 'NONE',  ( -2.229367062499996610, -83.14583333196773651, 3.861377020970582219 ) ) ;
#963 = CARTESIAN_POINT ( 'NONE',  ( 2.499999999999998668, -26.20833333060214798, -4.330127018922193649 ) ) ;
#965 = EDGE_LOOP ( 'NONE', ( #38732, #27924, #12630, #34159 ) ) ;
#964 = CARTESIAN_POINT ( 'NONE',  ( 9.457646018065525792E-16, -52.06249999863440792, 5.148502694627439702 ) ) ;
#966 = CARTESIAN_POINT ( 'NONE',  ( 1.339745962155612702, -65.29465819873851729, -5.000000000000000000 ) ) ;
#967 = LINE ( 'NONE', #11540, #51850 ) ;
#969 = VERTEX_POINT ( 'NONE', #23705 ) ;
#968 = CARTESIAN_POINT ( 'NONE',  ( 9.457646018065525792E-16, -3.312499998634407472, 5.148502694627439702 ) ) ;
#970 = CARTESIAN_POINT ( 'NONE',  ( -59.59170313451810586, -151.5000000013655779, 1.485763867205729394 ) ) ;
#971 = CARTESIAN_POINT ( 'NONE',  ( -5.000000000000000000, -65.00000000000000000, 0.000000000000000000 ) ) ;
#972 = CARTESIAN_POINT ( 'NONE',  ( 1.846868145590735200, -153.5000000013656063, -4.458734125000000326 ) ) ;
#973 = CARTESIAN_POINT ( 'NONE',  ( 2.229367062500001939, -48.22916666530106511, 3.861377020970579999 ) ) ;
#974 = CARTESIAN_POINT ( 'NONE',  ( -4.999999999999998224, -15.79166666393548191, 2.886751345948131764 ) ) ;
#975 = CARTESIAN_POINT ( 'NONE',  ( 2.071067811865475505, -157.8125000000000284, -5.000000000000000888 ) ) ;
#976 = CARTESIAN_POINT ( 'NONE',  ( -2.500000000000000444, 10.83333333333333393, -4.330127018922193649 ) ) ;
#977 = CARTESIAN_POINT ( 'NONE',  ( -50.01589407740564042, -154.6250000000000284, 0.3983568153799778022 ) ) ;
#978 = CARTESIAN_POINT ( 'NONE',  ( 2.229367062499998831, -12.89583333196774007, -3.861377020970580887 ) ) ;
#979 = CARTESIAN_POINT ( 'NONE',  ( -2.229367062500000163, -45.72916666530106511, -3.861377020970580443 ) ) ;
#980 = CARTESIAN_POINT ( 'NONE',  ( 0.000000000000000000, -120.0000000000000000, 0.000000000000000000 ) ) ;
#981 = CARTESIAN_POINT ( 'NONE',  ( -4.458734124999999437, -145.9375000013656063, -5.460374474430324690E-16 ) ) ;
#982 = CARTESIAN_POINT ( 'NONE',  ( -4.458734124999998549, -94.47916666530106511, 2.574251347313722516 ) ) ;
#983 = CARTESIAN_POINT ( 'NONE',  ( -5.000000000000000000, 21.12500000273118417, 0.000000000000000000 ) ) ;
#984 =( BOUNDED_CURVE ( )  B_SPLINE_CURVE ( 2, ( #59068, #30097, #20468, #34605, #24972, #45223, #53603, #25608, #29453 ),
 .UNSPECIFIED., .F., .F. ) 
 B_SPLINE_CURVE_WITH_KNOTS ( ( 3, 2, 2, 2, 3 ),
 ( 0.8803571428571428381, 0.8809523809523809312, 0.8821428571428571175, 0.8833333333333333037, 0.8839285714285713969 ),
 .UNSPECIFIED. ) 
 CURVE ( )  GEOMETRIC_REPRESENTATION_ITEM ( )  RATIONAL_B_SPLINE_CURVE ( ( 0.9330127018922194093, 0.9330127018922194093, 1.000000000000000000, 0.8660254037844387076, 1.000000000000000000, 0.8660254037844387076, 1.000000000000000000, 0.9330127018922194093, 0.9330127018922194093 ) ) 
 REPRESENTATION_ITEM ( '' )  );
#985 = ORIENTED_EDGE ( 'NONE', *, *, #48987, .T. ) ;
#986 = CARTESIAN_POINT ( 'NONE',  ( 0.000000000000000000, -120.0000000000000000, 0.000000000000000000 ) ) ;
#987 = CARTESIAN_POINT ( 'NONE',  ( 2.229367062499998831, 28.10416666803225993, -3.861377020970580887 ) ) ;
#988 = CARTESIAN_POINT ( 'NONE',  ( -50.18089887299979068, -145.8125000027311842, 2.462841084822635640 ) ) ;
#989 = CARTESIAN_POINT ( 'NONE',  ( 1.975475456537005874E-15, -44.62499999726880162, 5.000000000000000000 ) ) ;
#990 = VECTOR ( 'NONE', #31777, 1000.000000000000000 ) ;
#991 = EDGE_LOOP ( 'NONE', ( #39298, #2335, #23008, #40199 ) ) ;
#992 = CARTESIAN_POINT ( 'NONE',  ( -2.229367062500000163, 4.520833334698926897, -3.861377020970580443 ) ) ;
#993 = CARTESIAN_POINT ( 'NONE',  ( 2.500000000000002220, -50.54166666393547303, 4.330127018922192761 ) ) ;
#994 = CARTESIAN_POINT ( 'NONE',  ( -2.229367062500000163, -19.72916666530107221, -3.861377020970580443 ) ) ;
#995 = CARTESIAN_POINT ( 'NONE',  ( -2.500000000000000444, -101.1666666666666572, -4.330127018922193649 ) ) ;
#996 = CARTESIAN_POINT ( 'NONE',  ( 4.458734124999999437, -7.812499998634405252, -5.460374474430324690E-16 ) ) ;
#997 = CARTESIAN_POINT ( 'NONE',  ( -5.000000000000000000, 4.041666669397852019, -2.886751345948128211 ) ) ;
#998 = CARTESIAN_POINT ( 'NONE',  ( 1.846868145590736310, -149.6250000013655779, 4.458734124999997661 ) ) ;
#999 = CARTESIAN_POINT ( 'NONE',  ( -2.229367062499996610, 16.60416666803225638, 3.861377020970582219 ) ) ;
#1000 = ORIENTED_EDGE ( 'NONE', *, *, #7134, .T. ) ;
#1001 = CARTESIAN_POINT ( 'NONE',  ( -1.339745962155613812, -19.08034179853029144, -5.000000000000000000 ) ) ;
#1002 = LINE ( 'NONE', #6128, #35999 ) ;
#1003 = CARTESIAN_POINT ( 'NONE',  ( -3.152548672688508926E-16, -21.56249999863440081, -5.148502694627439702 ) ) ;
#1004 = CARTESIAN_POINT ( 'NONE',  ( -56.66612745406288099, -143.3125000000000000, -5.149110718188529390 ) ) ;
#1005 = CARTESIAN_POINT ( 'NONE',  ( 1.339745962155614034, 29.29465819873852084, 5.000000000000000000 ) ) ;
#1006 = CARTESIAN_POINT ( 'NONE',  ( -57.89159099828107458, -149.6875000013656063, -3.393966926194107447 ) ) ;
#1007 = CARTESIAN_POINT ( 'NONE',  ( -4.999999999999999112, -44.79166666393547303, 2.886751345948131764 ) ) ;
#1008 = CARTESIAN_POINT ( 'NONE',  ( 2.500000000000002220, -67.54166666393547303, 4.330127018922192761 ) ) ;
#1009 = CARTESIAN_POINT ( 'NONE',  ( 4.458734124999998549, 14.27083333469892601, -2.574251347313721627 ) ) ;
#1010 = CARTESIAN_POINT ( 'NONE',  ( -1.339745962155610925, -8.669658196007331341, 5.000000000000000000 ) ) ;
#1011 = CARTESIAN_POINT ( 'NONE',  ( -2.500000000000000444, -48.04166666393547303, -4.330127018922193649 ) ) ;
#1012 = CARTESIAN_POINT ( 'NONE',  ( -4.458734124999999437, 10.68750000136559386, 0.000000000000000000 ) ) ;
#1013 = CARTESIAN_POINT ( 'NONE',  ( -4.458734124999998549, -69.22916666530107932, 2.574251347313722516 ) ) ;
#1014 = EDGE_LOOP ( 'NONE', ( #25292, #37955, #18501, #1392 ) ) ;
#1015 = CARTESIAN_POINT ( 'NONE',  ( -4.458734124999999437, -16.56249999863440436, 0.000000000000000000 ) ) ;
#1016 = CARTESIAN_POINT ( 'NONE',  ( -5.000000000000000000, 2.916666666666668739, -2.886751345948128211 ) ) ;
#1017 = CARTESIAN_POINT ( 'NONE',  ( 1.846868145590735200, -164.2500000013656063, -4.458734125000000326 ) ) ;
#1018 = CARTESIAN_POINT ( 'NONE',  ( -6.972266317189433020E-16, -17.25000000000000000, -5.000000000000000000 ) ) ;
#1019 = CARTESIAN_POINT ( 'NONE',  ( 4.458734125000001214, -59.89583333196774362, 2.574251347313718519 ) ) ;
#1020 = CARTESIAN_POINT ( 'NONE',  ( 5.000000000000000888, -90.45833333060214443, 2.886751345948126879 ) ) ;
#1021 = CARTESIAN_POINT ( 'NONE',  ( -4.458734124999997661, -33.22916666530106511, 2.574251347313722516 ) ) ;
#1022 = CARTESIAN_POINT ( 'NONE',  ( -1.339745962155610925, -41.66965819600731891, 5.000000000000000000 ) ) ;
#1023 = CARTESIAN_POINT ( 'NONE',  ( 1.975475456537005874E-15, -43.75000000000000000, 5.000000000000000000 ) ) ;
#1024 = CARTESIAN_POINT ( 'NONE',  ( -5.000000000000000000, -107.9583333306021444, -2.886751345948128211 ) ) ;
#1025 = CARTESIAN_POINT ( 'NONE',  ( -51.75738570946856498, -140.7500000000000000, 3.805975901505576964 ) ) ;
#1026 = CARTESIAN_POINT ( 'NONE',  ( -1.846868145590734756, -151.3750000013656063, -4.458734124999999437 ) ) ;
#1027 = CARTESIAN_POINT ( 'NONE',  ( -2.499999999999996447, -43.83333333333333570, 4.330127018922195425 ) ) ;
#1028 = CARTESIAN_POINT ( 'NONE',  ( -6.972266317189433020E-16, -14.24999999999999822, -5.000000000000000000 ) ) ;
#1029 = CARTESIAN_POINT ( 'NONE',  ( 2.499999999999998668, -68.20833333060214443, -4.330127018922193649 ) ) ;
#1030 = ORIENTED_EDGE ( 'NONE', *, *, #46844, .F. ) ;
#1031 = CARTESIAN_POINT ( 'NONE',  ( -2.229367062499996610, -106.1458333319677365, 3.861377020970582219 ) ) ;
#1032 = CARTESIAN_POINT ( 'NONE',  ( 4.458734125000001214, 3.854166668032260823, 2.574251347313718519 ) ) ;
#1033 = AXIS2_PLACEMENT_3D ( 'NONE', #4126, #23748, #43343 ) ;
#1034 =( BOUNDED_CURVE ( )  B_SPLINE_CURVE ( 2, ( #14476, #10930, #49533, #49847, #34097, #44379, #43745, #59193, #4835 ),
 .UNSPECIFIED., .F., .F. ) 
 B_SPLINE_CURVE_WITH_KNOTS ( ( 3, 2, 2, 2, 3 ),
 ( 0.6017857142857142572, 0.6023809523809523503, 0.6035714285714285365, 0.6047619047619047228, 0.6053571428571428159 ),
 .UNSPECIFIED. ) 
 CURVE ( )  GEOMETRIC_REPRESENTATION_ITEM ( )  RATIONAL_B_SPLINE_CURVE ( ( 0.9330127018922194093, 0.9330127018922194093, 1.000000000000000000, 0.8660254037844387076, 1.000000000000000000, 0.8660254037844387076, 1.000000000000000000, 0.9330127018922194093, 0.9330127018922194093 ) ) 
 REPRESENTATION_ITEM ( '' )  );
#1035 = CARTESIAN_POINT ( 'NONE',  ( -4.999999999999999112, -0.9166666666666664076, 2.886751345948131764 ) ) ;
#1036 = CARTESIAN_POINT ( 'NONE',  ( 4.458734125000000326, -66.89583333196773651, 2.574251347313718519 ) ) ;
#1037 = CARTESIAN_POINT ( 'NONE',  ( -51.19402409849444524, -147.6250000027312126, -3.242614290531456334 ) ) ;
#1038 = CARTESIAN_POINT ( 'NONE',  ( -3.535250795749689387E-16, -6.124999997268812280, -5.773502691896257311 ) ) ;
#1040 = VERTEX_POINT ( 'NONE', #58421 ) ;
#1039 = CARTESIAN_POINT ( 'NONE',  ( -4.458734124999999437, -33.31249999863440792, 0.000000000000000000 ) ) ;
#1041 = DIRECTION ( 'NONE',  ( -0.000000000000000000, 1.000000000000000000, -0.000000000000000000 ) ) ;
#1042 = CARTESIAN_POINT ( 'NONE',  ( -6.972266317189433020E-16, -6.249999999999999112, -5.000000000000000000 ) ) ;
#1043 = VERTEX_POINT ( 'NONE', #3767 ) ;
#1044 = CARTESIAN_POINT ( 'NONE',  ( -5.000000000000000000, -55.95833333060214443, -2.886751345948128211 ) ) ;
#1045 = CARTESIAN_POINT ( 'NONE',  ( 1.060575238724906964E-15, -50.75000000000000000, 5.773502691896257311 ) ) ;
#1047 = CARTESIAN_POINT ( 'NONE',  ( -4.458734124999998549, -30.47916666530107221, 2.574251347313722516 ) ) ;
#1046 = CARTESIAN_POINT ( 'NONE',  ( 2.500000000000002220, -46.54166666393547303, 4.330127018922192761 ) ) ;
#1048 = CARTESIAN_POINT ( 'NONE',  ( 0.000000000000000000, -120.0000000000000000, 0.000000000000000000 ) ) ;
#1049 = CARTESIAN_POINT ( 'NONE',  ( -3.152548672688508926E-16, -77.56249999863440792, -5.148502694627439702 ) ) ;
#1050 = CARTESIAN_POINT ( 'NONE',  ( 3.061616997868383141E-16, -169.7500000000000000, -5.000000000000000000 ) ) ;
#1051 = CARTESIAN_POINT ( 'NONE',  ( 4.458734124999998549, -81.72916666530106511, -2.574251347313721627 ) ) ;
#1052 = CARTESIAN_POINT ( 'NONE',  ( -51.60603307380591787, -134.1875000013656063, -2.891590998281053704 ) ) ;
#1053 = CARTESIAN_POINT ( 'NONE',  ( 4.458734125000001214, -32.14583333196773651, 2.574251347313718519 ) ) ;
#1054 = VERTEX_POINT ( 'NONE', #32716 ) ;
#1055 = CARTESIAN_POINT ( 'NONE',  ( 1.975475456537005874E-15, -20.62499999726881228, 5.000000000000000000 ) ) ;
#1056 = EDGE_LOOP ( 'NONE', ( #41680, #41288, #22154, #18984 ) ) ;
#1057 = CARTESIAN_POINT ( 'NONE',  ( -3.152548672688508926E-16, -78.81249999863440792, -5.148502694627439702 ) ) ;
#1058 = CARTESIAN_POINT ( 'NONE',  ( -55.00000000000002132, -155.0000000000000284, 1.734723475976807094E-15 ) ) ;
#1059 = VERTEX_POINT ( 'NONE', #43302 ) ;
#1060 = FACE_OUTER_BOUND ( 'NONE', #7597, .T. ) ;
#1061 = CARTESIAN_POINT ( 'NONE',  ( -1.339745962155613812, -76.08034179853028434, -5.000000000000000000 ) ) ;
#1062 = CARTESIAN_POINT ( 'NONE',  ( -4.458734124999999437, -64.56249999863440792, 0.000000000000000000 ) ) ;
#1063 = CARTESIAN_POINT ( 'NONE',  ( 2.229367062500001939, -3.229166665301069550, 3.861377020970579999 ) ) ;
#1064 = ORIENTED_EDGE ( 'NONE', *, *, #24039, .F. ) ;
#1065 = DIRECTION ( 'NONE',  ( -0.000000000000000000, 1.000000000000000000, -0.000000000000000000 ) ) ;
#1066 = CARTESIAN_POINT ( 'NONE',  ( 5.000000000000000000, -91.41666666666665719, -2.886751345948130876 ) ) ;
#1067 = CARTESIAN_POINT ( 'NONE',  ( 4.458734124999999437, 8.187500001365595637, -5.460374474430324690E-16 ) ) ;
#1069 = VECTOR ( 'NONE', #53193, 1000.000000000000000 ) ;
#1068 = CARTESIAN_POINT ( 'NONE',  ( -53.51423613279429503, -140.2500000013656063, 4.591703134518082763 ) ) ;
#1070 = CARTESIAN_POINT ( 'NONE',  ( 5.000000000000000000, -32.50000000000000000, -6.123233995736766282E-16 ) ) ;
#1071 = CARTESIAN_POINT ( 'NONE',  ( 4.458734124999997661, -162.5000000013655779, 1.846868145590737864 ) ) ;
#1072 = DIRECTION ( 'NONE',  ( -0.000000000000000000, 1.000000000000000000, -0.000000000000000000 ) ) ;
#1073 = ORIENTED_EDGE ( 'NONE', *, *, #41605, .F. ) ;
#1074 = CARTESIAN_POINT ( 'NONE',  ( -3.152548672688508926E-16, -80.56249999863440792, -5.148502694627439702 ) ) ;
#1075 = CYLINDRICAL_SURFACE ( 'NONE', #55203, 5.000000000000000000 ) ;
#1076 = CARTESIAN_POINT ( 'NONE',  ( -4.458734124999999437, -1.312499998634406140, 0.000000000000000000 ) ) ;
#1077 = AXIS2_PLACEMENT_3D ( 'NONE', #55433, #5576, #6538 ) ;
#1078 = CARTESIAN_POINT ( 'NONE',  ( 0.000000000000000000, -120.0000000000000000, 0.000000000000000000 ) ) ;
#1079 = CARTESIAN_POINT ( 'NONE',  ( 4.458734125000001214, -71.14583333196773651, 2.574251347313718519 ) ) ;
#1080 = CARTESIAN_POINT ( 'NONE',  ( -5.000000000000000000, -27.95833333060214798, -2.886751345948128211 ) ) ;
#1081 = CARTESIAN_POINT ( 'NONE',  ( 6.123233995736766282E-16, -170.0000000000000000, -5.000000000000000000 ) ) ;
#1082 = CARTESIAN_POINT ( 'NONE',  ( -3.152548672688508926E-16, 29.43750000136559564, -5.148502694627439702 ) ) ;
#1083 = CARTESIAN_POINT ( 'NONE',  ( -3.152548672688508926E-16, 27.43750000136559564, -5.148502694627439702 ) ) ;
#1084 = CARTESIAN_POINT ( 'NONE',  ( -2.229367062499996610, -48.14583333196772941, 3.861377020970582219 ) ) ;
#1085 = CARTESIAN_POINT ( 'NONE',  ( -2.229367062500000163, -33.72916666530107221, -3.861377020970580443 ) ) ;
#1086 = CARTESIAN_POINT ( 'NONE',  ( -2.229367062500000163, 1.270833334698927342, -3.861377020970580443 ) ) ;
#1087 = CARTESIAN_POINT ( 'NONE',  ( -1.336351044127974539E-14, 22.37500000273118417, 5.000000000000000000 ) ) ;
#1088 = CARTESIAN_POINT ( 'NONE',  ( -3.535250795749689387E-16, 18.75000000000000000, -5.773502691896257311 ) ) ;
#1089 = CARTESIAN_POINT ( 'NONE',  ( -2.071067811865475061, -146.8125000027312126, -5.000000000000000888 ) ) ;
#1090 = CARTESIAN_POINT ( 'NONE',  ( -56.66612745406272467, -154.3125000000000284, -5.149110718188517843 ) ) ;
#1091 = CARTESIAN_POINT ( 'NONE',  ( -2.229367062499996610, -42.14583333196773651, 3.861377020970582219 ) ) ;
#1092 = CARTESIAN_POINT ( 'NONE',  ( 2.499999999999998668, -73.20833333060214443, -4.330127018922193649 ) ) ;
#1093 = CARTESIAN_POINT ( 'NONE',  ( -50.55543936806279248, -145.3125000013656063, 0.3552334253322060320 ) ) ;
#1094 = DIRECTION ( 'NONE',  ( -0.000000000000000000, 1.000000000000000000, -0.000000000000000000 ) ) ;
#1095 = CARTESIAN_POINT ( 'NONE',  ( 3.535533905932736864, -141.2500000027311842, 3.535533905932738641 ) ) ;
#1096 = CARTESIAN_POINT ( 'NONE',  ( 4.458734124999999437, -78.06249999863440792, -5.460374474430324690E-16 ) ) ;
#1097 = CARTESIAN_POINT ( 'NONE',  ( -3.152801135295367096, -165.3125000013656063, -3.152801135295367541 ) ) ;
#1098 = DIRECTION ( 'NONE',  ( 0.000000000000000000, 0.000000000000000000, 1.000000000000000000 ) ) ;
#1099 = CARTESIAN_POINT ( 'NONE',  ( -6.523606932383669843, -4.893847819345372940, -7.213065638944913260 ) ) ;
#1100 = CARTESIAN_POINT ( 'NONE',  ( -2.499999999999996447, -25.83333333333333215, 4.330127018922195425 ) ) ;
#1101 = CARTESIAN_POINT ( 'NONE',  ( -4.458734125000000326, -140.0000000013655779, -1.846868145590735644 ) ) ;
#1102 = EDGE_LOOP ( 'NONE', ( #4070, #49426, #36519, #36845 ) ) ;
#1103 = CARTESIAN_POINT ( 'NONE',  ( -3.152548672688508926E-16, 22.18750000136559564, -5.148502694627439702 ) ) ;
#1104 = EDGE_LOOP ( 'NONE', ( #30665, #13987, #44017, #23834 ) ) ;
#1105 = CARTESIAN_POINT ( 'NONE',  ( -4.458734124999999437, -62.56249999863440792, 0.000000000000000000 ) ) ;
#1106 = CARTESIAN_POINT ( 'NONE',  ( -4.999999999999999112, 24.20833333606451987, 2.886751345948131764 ) ) ;
#1107 = CARTESIAN_POINT ( 'NONE',  ( 0.000000000000000000, -170.0000000000000000, 5.000000000000000000 ) ) ;
#1108 = CARTESIAN_POINT ( 'NONE',  ( -4.999999999999999112, 13.08333333333333037, 2.886751345948131764 ) ) ;
#1109 = EDGE_CURVE ( 'NONE', #6571, #34317, #42104, .T. ) ;
#1110 =( BOUNDED_CURVE ( )  B_SPLINE_CURVE ( 2, ( #33713, #52706, #63004, #19228, #38844, #58787, #33400, #14404, #9581 ),
 .UNSPECIFIED., .F., .F. ) 
 B_SPLINE_CURVE_WITH_KNOTS ( ( 3, 2, 2, 2, 3 ),
 ( 0.1267857142857142794, 0.1273809523809523725, 0.1285714285714285587, 0.1297619047619047727, 0.1303571428571428659 ),
 .UNSPECIFIED. ) 
 CURVE ( )  GEOMETRIC_REPRESENTATION_ITEM ( )  RATIONAL_B_SPLINE_CURVE ( ( 0.9330127018922194093, 0.9330127018922194093, 1.000000000000000000, 0.8660254037844387076, 1.000000000000000000, 0.8660254037844387076, 1.000000000000000000, 0.9330127018922194093, 0.9330127018922194093 ) ) 
 REPRESENTATION_ITEM ( '' )  );
#1111 = CARTESIAN_POINT ( 'NONE',  ( -3.152548672688508926E-16, -52.56249999863440792, -5.148502694627439702 ) ) ;
#1112 = CARTESIAN_POINT ( 'NONE',  ( -4.458734124999999437, -11.39583333196774007, -2.574251347313719407 ) ) ;
#1113 = CARTESIAN_POINT ( 'NONE',  ( 2.493747252781420335E-13, -91.12499999726880162, -5.000000000000000000 ) ) ;
#1114 = CARTESIAN_POINT ( 'NONE',  ( 1.339745962155612702, 15.83034180399266511, -5.000000000000000000 ) ) ;
#1115 = CARTESIAN_POINT ( 'NONE',  ( 5.000000000000000000, -33.37499999726880873, -6.123233995736766282E-16 ) ) ;
#1116 = CARTESIAN_POINT ( 'NONE',  ( -4.999999999999998224, -61.91666666666666430, 2.886751345948131764 ) ) ;
#1117 = CARTESIAN_POINT ( 'NONE',  ( 1.339745962155615144, -56.58034179853028434, 4.999999999999999112 ) ) ;
#1118 = VECTOR ( 'NONE', #28038, 1000.000000000000000 ) ;
#1120 = CARTESIAN_POINT ( 'NONE',  ( -2.229367062499996610, -15.39583333196773651, 3.861377020970582219 ) ) ;
#1119 = CARTESIAN_POINT ( 'NONE',  ( -2.500000000000000444, -79.16666666666665719, -4.330127018922193649 ) ) ;
#1121 = CARTESIAN_POINT ( 'NONE',  ( -1.339745962155497683, -78.08034179853028434, -5.000000000000066613 ) ) ;
#1122 = CARTESIAN_POINT ( 'NONE',  ( 2.229367062500001939, -57.97916666530107932, 3.861377020970579999 ) ) ;
#1123 = CARTESIAN_POINT ( 'NONE',  ( 4.458734124999999437, -155.6875000013655779, 0.000000000000000000 ) ) ;
#1124 = AXIS2_PLACEMENT_3D ( 'NONE', #5510, #698, #6795 ) ;
#1125 =( BOUNDED_CURVE ( )  B_SPLINE_CURVE ( 2, ( #57789, #19152, #62622, #58087, #43595, #52639, #43907, #62303, #18225 ),
 .UNSPECIFIED., .F., .F. ) 
 B_SPLINE_CURVE_WITH_KNOTS ( ( 3, 2, 2, 2, 3 ),
 ( 0.08958333333333333426, 0.09027777777777777624, 0.09166666666666666019, 0.09305555555555555802, 0.09375000000000000000 ),
 .UNSPECIFIED. ) 
 CURVE ( )  GEOMETRIC_REPRESENTATION_ITEM ( )  RATIONAL_B_SPLINE_CURVE ( ( 0.9330127018922194093, 0.9330127018922194093, 1.000000000000000000, 0.8660254037844387076, 1.000000000000000000, 0.8660254037844387076, 1.000000000000000000, 0.9330127018922194093, 0.9330127018922194093 ) ) 
 REPRESENTATION_ITEM ( '' )  );
#1126 = EDGE_CURVE ( 'NONE', #45557, #27450, #8856, .T. ) ;
#1127 = CARTESIAN_POINT ( 'NONE',  ( 5.000000000000000888, -54.45833333060214443, 2.886751345948126879 ) ) ;
#1128 = ORIENTED_EDGE ( 'NONE', *, *, #16124, .F. ) ;
#1129 = CARTESIAN_POINT ( 'NONE',  ( 1.339745962155615144, -26.70534180126147561, 4.999999999999999112 ) ) ;
#1131 = EDGE_CURVE ( 'NONE', #61397, #19898, #8913, .T. ) ;
#1130 = CARTESIAN_POINT ( 'NONE',  ( 9.457646018065525792E-16, 0.6875000013655957476, 5.148502694627439702 ) ) ;
#1132 = VERTEX_POINT ( 'NONE', #57799 ) ;
#1134 = CARTESIAN_POINT ( 'NONE',  ( -5.000000000000000000, -86.08333333333332860, -2.886751345948128211 ) ) ;
#1133 = CARTESIAN_POINT ( 'NONE',  ( 0.000000000000000000, 0.000000000000000000, 0.000000000000000000 ) ) ;
#1135 = CARTESIAN_POINT ( 'NONE',  ( -3.152801135295367096, -156.0625000013656063, -3.152801135295367541 ) ) ;
#1136 = ORIENTED_EDGE ( 'NONE', *, *, #27471, .T. ) ;
#1137 = CARTESIAN_POINT ( 'NONE',  ( 5.000000000000000000, -99.50000000000000000, -6.123233995736766282E-16 ) ) ;
#1138 = CARTESIAN_POINT ( 'NONE',  ( -50.01589407740564042, -128.6250000000000284, 0.3983568153799778022 ) ) ;
#1139 = CARTESIAN_POINT ( 'NONE',  ( 3.535533905932736864, -161.2500000027312126, 3.535533905932738641 ) ) ;
#1140 = CARTESIAN_POINT ( 'NONE',  ( -3.152548672688508926E-16, -46.81249999863440081, -5.148502694627439702 ) ) ;
#1141 = ORIENTED_EDGE ( 'NONE', *, *, #54678, .F. ) ;
#1142 = CARTESIAN_POINT ( 'NONE',  ( -6.972266317189433020E-16, 11.87500000273118594, -5.000000000000000000 ) ) ;
#1143 = CARTESIAN_POINT ( 'NONE',  ( -2.229367062500000163, 12.52083333469892601, -3.861377020970580443 ) ) ;
#1144 = CARTESIAN_POINT ( 'NONE',  ( -2.229367062499996610, -89.39583333196773651, 3.861377020970582219 ) ) ;
#1145 = CARTESIAN_POINT ( 'NONE',  ( -52.53715891517739323, -124.5625000027312268, -4.819101127000233298 ) ) ;
#1146 = CARTESIAN_POINT ( 'NONE',  ( 5.000000000000000000, -44.41666666666665719, -2.886751345948130876 ) ) ;
#1147 = CARTESIAN_POINT ( 'NONE',  ( 0.000000000000000000, -170.0000000000000000, 5.000000000000000000 ) ) ;
#1148 = CARTESIAN_POINT ( 'NONE',  ( 2.229367062499998831, -64.64583333196773651, -3.861377020970580887 ) ) ;
#1149 = CARTESIAN_POINT ( 'NONE',  ( -1.339745962155610925, 1.205341801261479828, 5.000000000000000000 ) ) ;
#1150 = CARTESIAN_POINT ( 'NONE',  ( -4.458734124999998549, 17.77083333469892779, 2.574251347313722516 ) ) ;
#1151 = CARTESIAN_POINT ( 'NONE',  ( -2.499999999999996447, 18.16666666666666430, 4.330127018922195425 ) ) ;
#1152 = CARTESIAN_POINT ( 'NONE',  ( 1.062108568985190270E-13, -27.25000000000000000, -4.999999999999999112 ) ) ;
#1153 = CARTESIAN_POINT ( 'NONE',  ( 2.229367062500001939, -52.22916666530107221, 3.861377020970579999 ) ) ;
#1154 = ADVANCED_FACE ( 'NONE', ( #33345 ), #853, .T. ) ;
#1155 = CARTESIAN_POINT ( 'NONE',  ( 5.000000000000000000, -7.374999997268813168, -6.123233995736766282E-16 ) ) ;
#1156 = CARTESIAN_POINT ( 'NONE',  ( -4.999999999999998224, 25.08333333333333215, 2.886751345948131764 ) ) ;
#1157 = CARTESIAN_POINT ( 'NONE',  ( 0.000000000000000000, -170.0000000000000000, 0.000000000000000000 ) ) ;
#1158 = CARTESIAN_POINT ( 'NONE',  ( 9.457646018065525792E-16, -89.31249999863440792, 5.148502694627439702 ) ) ;
#1159 = CARTESIAN_POINT ( 'NONE',  ( 0.000000000000000000, -120.0000000000000000, 5.000000000000000000 ) ) ;
#1160 = CARTESIAN_POINT ( 'NONE',  ( 9.457646018065525792E-16, -17.31249999863440792, 5.148502694627439702 ) ) ;
#1161 = ORIENTED_EDGE ( 'NONE', *, *, #40622, .F. ) ;
#1162 = CARTESIAN_POINT ( 'NONE',  ( -6.972266317189433020E-16, -47.12499999726880873, -5.000000000000000000 ) ) ;
#1163 = CARTESIAN_POINT ( 'NONE',  ( 2.229367062499998831, -105.6458333319677365, -3.861377020970580887 ) ) ;
#1164 = CARTESIAN_POINT ( 'NONE',  ( 5.000000000000000000, -157.1875000027312126, 2.071067811865478614 ) ) ;
#1165 = ORIENTED_EDGE ( 'NONE', *, *, #33801, .T. ) ;
#1166 = CARTESIAN_POINT ( 'NONE',  ( 9.457646018065525792E-16, -99.31249999863442213, 5.148502694627439702 ) ) ;
#1167 = VECTOR ( 'NONE', #55223, 1000.000000000000000 ) ;
#1168 = CARTESIAN_POINT ( 'NONE',  ( -3.535250795749689387E-16, -55.12499999726880162, -5.773502691896257311 ) ) ;
#1169 = CARTESIAN_POINT ( 'NONE',  ( -6.972266317189433020E-16, -67.25000000000000000, -5.000000000000000000 ) ) ;
#1170 = CARTESIAN_POINT ( 'NONE',  ( -55.35523342533222291, -126.3125000013655921, 4.444560631937231499 ) ) ;
#1171 = CARTESIAN_POINT ( 'NONE',  ( -55.35523342533222291, -141.3125000013656063, 4.444560631937231499 ) ) ;
#1172 = CARTESIAN_POINT ( 'NONE',  ( -2.229367062500000163, -25.47916666530106866, -3.861377020970580443 ) ) ;
#1173 = CARTESIAN_POINT ( 'NONE',  ( 9.457646018065525792E-16, 7.687500001365596525, 5.148502694627439702 ) ) ;
#1174 = CARTESIAN_POINT ( 'NONE',  ( 4.458734125000000326, -62.14583333196774362, 2.574251347313718519 ) ) ;
#1175 = FACE_OUTER_BOUND ( 'NONE', #36826, .T. ) ;
#1176 = CARTESIAN_POINT ( 'NONE',  ( 4.458734124999998549, -18.72916666530106866, -2.574251347313721627 ) ) ;
#1177 = CARTESIAN_POINT ( 'NONE',  ( 3.061616997868383141E-16, -159.7500000000000000, -5.000000000000000000 ) ) ;
#1178 = CARTESIAN_POINT ( 'NONE',  ( -9.184850993605147944E-16, -152.2500000000000000, 5.000000000000000000 ) ) ;
#1179 = CARTESIAN_POINT ( 'NONE',  ( 5.000000000000000888, -11.58333333333333570, 2.886751345948126879 ) ) ;
#1180 = CARTESIAN_POINT ( 'NONE',  ( 4.458734124999999437, -154.4375000013655779, 0.000000000000000000 ) ) ;
#1181 = EDGE_LOOP ( 'NONE', ( #9569, #56457, #6169, #33546 ) ) ;
#1182 = CARTESIAN_POINT ( 'NONE',  ( 4.458734124999999437, -44.06249999863440081, -5.460374474430324690E-16 ) ) ;
#1183 =( BOUNDED_CURVE ( )  B_SPLINE_CURVE ( 2, ( #28033, #13244, #17451, #56695, #22273, #7167, #56377, #26777, #61199 ),
 .UNSPECIFIED., .F., .F. ) 
 B_SPLINE_CURVE_WITH_KNOTS ( ( 3, 2, 2, 2, 3 ),
 ( 0.3553571428571428714, 0.3559523809523809645, 0.3571428571428571508, 0.3583333333333333370, 0.3589285714285714302 ),
 .UNSPECIFIED. ) 
 CURVE ( )  GEOMETRIC_REPRESENTATION_ITEM ( )  RATIONAL_B_SPLINE_CURVE ( ( 0.9330127018922194093, 0.9330127018922194093, 1.000000000000000000, 0.8660254037844387076, 1.000000000000000000, 0.8660254037844387076, 1.000000000000000000, 0.9330127018922194093, 0.9330127018922194093 ) ) 
 REPRESENTATION_ITEM ( '' )  );
#1184 = CARTESIAN_POINT ( 'NONE',  ( 6.123233995736766282E-16, -120.0000000000000000, -5.000000000000000000 ) ) ;
#1185 = CARTESIAN_POINT ( 'NONE',  ( 1.975475456537005874E-15, -92.74999999999998579, 5.000000000000000000 ) ) ;
#1186 = CARTESIAN_POINT ( 'NONE',  ( -2.500000000000000444, 27.83333333333333215, -4.330127018922193649 ) ) ;
#1187 = ADVANCED_FACE ( 'NONE', ( #1175 ), #59371, .T. ) ;
#1188 = CARTESIAN_POINT ( 'NONE',  ( -4.458734124999999437, 4.687500001365595637, 0.000000000000000000 ) ) ;
#1189 = LINE ( 'NONE', #15320, #62683 ) ;
#1190 = CARTESIAN_POINT ( 'NONE',  ( 1.339745962155612702, -95.16965819600731891, -5.000000000000000000 ) ) ;
#1191 = LINE ( 'NONE', #50372, #9804 ) ;
#1192 = CARTESIAN_POINT ( 'NONE',  ( -4.458734124999999437, 18.43750000136559564, 0.000000000000000000 ) ) ;
#1193 = CARTESIAN_POINT ( 'NONE',  ( -2.499999999999996447, -72.83333333333332860, 4.330127018922195425 ) ) ;
#1194 = CARTESIAN_POINT ( 'NONE',  ( 2.500000000000002220, 10.45833333606451987, 4.330127018922192761 ) ) ;
#1195 = ORIENTED_EDGE ( 'NONE', *, *, #5962, .T. ) ;
#1196 = CARTESIAN_POINT ( 'NONE',  ( -1.230605004983934782E-13, -25.75000000000000355, 5.000000000000000000 ) ) ;
#1197 = ORIENTED_EDGE ( 'NONE', *, *, #20141, .F. ) ;
#1198 = FACE_OUTER_BOUND ( 'NONE', #16752, .T. ) ;
#1199 = CARTESIAN_POINT ( 'NONE',  ( 9.457646018065525792E-16, -44.06249999863439371, 5.148502694627439702 ) ) ;
#1200 = EDGE_CURVE ( 'NONE', #32427, #18888, #37599, .T. ) ;
#1201 = CARTESIAN_POINT ( 'NONE',  ( 5.000000000000000000, -38.37499999726881583, -6.123233995736766282E-16 ) ) ;
#1202 = VERTEX_POINT ( 'NONE', #39414 ) ;
#1204 = EDGE_CURVE ( 'NONE', #32122, #25684, #59052, .T. ) ;
#1203 = CARTESIAN_POINT ( 'NONE',  ( 2.229367062500001939, -17.97916666530106866, 3.861377020970579999 ) ) ;
#1205 = ORIENTED_EDGE ( 'NONE', *, *, #3063, .F. ) ;
#1206 = CARTESIAN_POINT ( 'NONE',  ( -5.000000000000000000, -84.99999999999998579, 0.000000000000000000 ) ) ;
#1207 = CARTESIAN_POINT ( 'NONE',  ( -4.458734125000000326, -168.0000000013655779, -1.846868145590735644 ) ) ;
#1208 = EDGE_CURVE ( 'NONE', #47640, #6601, #61484, .T. ) ;
#1209 =( BOUNDED_CURVE ( )  B_SPLINE_CURVE ( 2, ( #48764, #28837, #29455, #4709, #5674, #39745, #29142, #58433, #43935 ),
 .UNSPECIFIED., .F., .F. ) 
 B_SPLINE_CURVE_WITH_KNOTS ( ( 3, 2, 2, 2, 3 ),
 ( 0.8229166666666666297, 0.8236111111111110716, 0.8249999999999999556, 0.8263888888888888395, 0.8270833333333332815 ),
 .UNSPECIFIED. ) 
 CURVE ( )  GEOMETRIC_REPRESENTATION_ITEM ( )  RATIONAL_B_SPLINE_CURVE ( ( 0.9330127018922194093, 0.9330127018922194093, 1.000000000000000000, 0.8660254037844387076, 1.000000000000000000, 0.8660254037844387076, 1.000000000000000000, 0.9330127018922194093, 0.9330127018922194093 ) ) 
 REPRESENTATION_ITEM ( '' )  );
#1210 = CARTESIAN_POINT ( 'NONE',  ( -5.000000000000000000, -87.87499999726880162, 0.000000000000000000 ) ) ;
#1211 = ORIENTED_EDGE ( 'NONE', *, *, #16225, .F. ) ;
#1212 = AXIS2_PLACEMENT_3D ( 'NONE', #22676, #47110, #1798 ) ;
#1213 = CARTESIAN_POINT ( 'NONE',  ( -58.24261429053147765, -140.2500000000000000, -3.805975901505573855 ) ) ;
#1214 = CARTESIAN_POINT ( 'NONE',  ( -4.458734124999998549, -27.47916666530106866, 2.574251347313722516 ) ) ;
#1215 = CARTESIAN_POINT ( 'NONE',  ( 0.000000000000000000, -120.0000000000000000, 0.000000000000000000 ) ) ;
#1216 = ORIENTED_EDGE ( 'NONE', *, *, #46137, .T. ) ;
#1217 = PRODUCT_CONTEXT ( 'NONE', #16684, 'mechanical' ) ;
#1218 = CARTESIAN_POINT ( 'NONE',  ( -1.846868145590737420, -164.0000000013656063, 4.458734124999999437 ) ) ;
#1219 = CARTESIAN_POINT ( 'NONE',  ( 4.458734124999999437, 29.18750000136559208, -5.460374474430324690E-16 ) ) ;
#1220 = CARTESIAN_POINT ( 'NONE',  ( 0.000000000000000000, -170.0000000000000000, 0.000000000000000000 ) ) ;
#1221 = EDGE_LOOP ( 'NONE', ( #11382, #38108, #36799, #29871 ) ) ;
#1222 = CARTESIAN_POINT ( 'NONE',  ( -3.535533905932738641, -166.5000000027312126, 3.535533905932737309 ) ) ;
#1223 = CARTESIAN_POINT ( 'NONE',  ( -57.89159099828107458, -144.9375000013656063, -3.393966926194107447 ) ) ;
#1224 = CARTESIAN_POINT ( 'NONE',  ( 9.457646018065525792E-16, -74.31249999863440792, 5.148502694627439702 ) ) ;
#1225 = CARTESIAN_POINT ( 'NONE',  ( -53.33387254593733928, -132.9375000027312126, 5.149110718188519620 ) ) ;
#1226 = CARTESIAN_POINT ( 'NONE',  ( -2.229367062500000163, -43.47916666530106511, -3.861377020970580443 ) ) ;
#1227 = CARTESIAN_POINT ( 'NONE',  ( 3.152801135295366208, -141.8125000013655779, 3.152801135295367985 ) ) ;
#1228 = CARTESIAN_POINT ( 'NONE',  ( -7.500000000000000000, -3.160302461882432024, -7.231849989190475725 ) ) ;
#1229 = CARTESIAN_POINT ( 'NONE',  ( -2.229367062500000163, -49.47916666530107221, -3.861377020970580443 ) ) ;
#1230 = LINE ( 'NONE', #50088, #56356 ) ;
#1231 = ADVANCED_FACE ( 'NONE', ( #34589 ), #45209, .T. ) ;
#1232 = CARTESIAN_POINT ( 'NONE',  ( -4.458734124999999437, -17.31249999863440792, 0.000000000000000000 ) ) ;
#1233 = CARTESIAN_POINT ( 'NONE',  ( 5.000000000000000000, -100.5000000000000000, -6.123233995736766282E-16 ) ) ;
#1234 = CARTESIAN_POINT ( 'NONE',  ( -2.229367062500000163, -35.72916666530107221, -3.861377020970580443 ) ) ;
#1235 = CARTESIAN_POINT ( 'NONE',  ( -4.999999999999999112, 4.208333336064518093, 2.886751345948131764 ) ) ;
#1236 = CARTESIAN_POINT ( 'NONE',  ( 1.975475456537005874E-15, -50.75000000000000000, 5.000000000000000000 ) ) ;
#1237 = CARTESIAN_POINT ( 'NONE',  ( -50.40829686548195099, -129.0000000013656063, -1.485763867205728284 ) ) ;
#1238 = CARTESIAN_POINT ( 'NONE',  ( -2.229367062500000163, -73.72916666530106511, -3.861377020970580443 ) ) ;
#1239 = CYLINDRICAL_SURFACE ( 'NONE', #24015, 5.000000000000000000 ) ;
#1240 = CARTESIAN_POINT ( 'NONE',  ( -6.972266317189433020E-16, -30.12499999726880873, -5.000000000000000000 ) ) ;
#1241 = CARTESIAN_POINT ( 'NONE',  ( 4.458734124999998549, -0.9791666653010712151, -2.574251347313721627 ) ) ;
#1242 = ORIENTED_EDGE ( 'NONE', *, *, #53664, .F. ) ;
#1243 = CARTESIAN_POINT ( 'NONE',  ( 5.000000000000000000, -146.0625000000000000, 2.071067811865478614 ) ) ;
#1244 = CARTESIAN_POINT ( 'NONE',  ( -6.972266317189433020E-16, -60.24999999999999289, -5.000000000000000000 ) ) ;
#1246 = CARTESIAN_POINT ( 'NONE',  ( -2.229367062500000163, -33.47916666530107221, -3.861377020970580443 ) ) ;
#1245 = CARTESIAN_POINT ( 'NONE',  ( -2.229367062500000163, -87.47916666530107932, -3.861377020970580443 ) ) ;
#1247 = CARTESIAN_POINT ( 'NONE',  ( 3.061616997868383141E-16, -167.8750000027312126, -5.000000000000000000 ) ) ;
#1248 = CARTESIAN_POINT ( 'NONE',  ( 2.229367062499998831, -83.89583333196773651, -3.861377020970580887 ) ) ;
#1249 = CARTESIAN_POINT ( 'NONE',  ( -4.458734124999999437, 16.35416666803225993, -2.574251347313719407 ) ) ;
#1250 = CARTESIAN_POINT ( 'NONE',  ( 5.000000000000000888, -77.45833333060213022, 2.886751345948126879 ) ) ;
#1251 = CARTESIAN_POINT ( 'NONE',  ( -53.51423613279429503, -138.2500000013656063, 4.591703134518082763 ) ) ;
#1252 = CARTESIAN_POINT ( 'NONE',  ( 4.458734124999998549, -5.729166665301072214, -2.574251347313721627 ) ) ;
#1253 = CARTESIAN_POINT ( 'NONE',  ( 4.458734125000001214, 21.85416666803225993, 2.574251347313718519 ) ) ;
#1254 = CARTESIAN_POINT ( 'NONE',  ( 4.458734124999999437, -49.06249999863440792, -5.460374474430324690E-16 ) ) ;
#1255 = CARTESIAN_POINT ( 'NONE',  ( -5.000000000000000000, -50.95833333060213732, -2.886751345948128211 ) ) ;
#1256 = CARTESIAN_POINT ( 'NONE',  ( 2.229367062499998831, -85.64583333196773651, -3.861377020970580887 ) ) ;
#1257 = CARTESIAN_POINT ( 'NONE',  ( 4.458734124999999437, -1.812499998634406584, -5.460374474430324690E-16 ) ) ;
#1258 = VERTEX_POINT ( 'NONE', #48750 ) ;
#1259 = CARTESIAN_POINT ( 'NONE',  ( 4.458734124999999437, -32.06249999863440792, -5.460374474430324690E-16 ) ) ;
#1260 = CARTESIAN_POINT ( 'NONE',  ( -58.39396692619412477, -133.6875000013656063, 2.891590998281057701 ) ) ;
#1261 = CARTESIAN_POINT ( 'NONE',  ( 4.458734124999999437, -76.81249999863440792, -5.460374474430324690E-16 ) ) ;
#1262 = CARTESIAN_POINT ( 'NONE',  ( 9.457646018065525792E-16, 28.68750000136559208, 5.148502694627439702 ) ) ;
#1263 = CARTESIAN_POINT ( 'NONE',  ( 4.458734124999999437, 19.18750000136559564, -5.460374474430324690E-16 ) ) ;
#1264 = EDGE_CURVE ( 'NONE', #13616, #57087, #22019, .T. ) ;
#1265 = EDGE_CURVE ( 'NONE', #38994, #15732, #40055, .T. ) ;
#1266 = CARTESIAN_POINT ( 'NONE',  ( -2.500000000000000444, 9.833333333333332149, -4.330127018922193649 ) ) ;
#1267 = CARTESIAN_POINT ( 'NONE',  ( 5.000000000000000888, -66.58333333333332860, 2.886751345948126879 ) ) ;
#1268 = CARTESIAN_POINT ( 'NONE',  ( -3.152548672688508926E-16, -79.81249999863440792, -5.148502694627439702 ) ) ;
#1269 = CARTESIAN_POINT ( 'NONE',  ( -2.500000000000000444, -58.16666666666665719, -4.330127018922193649 ) ) ;
#1270 = EDGE_CURVE ( 'NONE', #43575, #17248, #34927, .T. ) ;
#1271 = DIRECTION ( 'NONE',  ( -0.000000000000000000, 1.000000000000000000, -0.000000000000000000 ) ) ;
#1272 = CARTESIAN_POINT ( 'NONE',  ( -5.000000000000000000, 27.04166666939785202, -2.886751345948128211 ) ) ;
#1273 = ORIENTED_EDGE ( 'NONE', *, *, #56758, .T. ) ;
#1274 = CARTESIAN_POINT ( 'NONE',  ( -4.999999999999998224, -72.79166666393548724, 2.886751345948131764 ) ) ;
#1275 = CARTESIAN_POINT ( 'NONE',  ( 5.000000000000000000, -52.29166666393547303, -2.886751345948130876 ) ) ;
#1277 = CARTESIAN_POINT ( 'NONE',  ( 5.000000000000000000, -17.41666666666666430, -2.886751345948129988 ) ) ;
#1276 = CARTESIAN_POINT ( 'NONE',  ( -5.000000000000000000, -149.5000000000000284, -6.123233995736766282E-16 ) ) ;
#1278 = CARTESIAN_POINT ( 'NONE',  ( 4.458734124999998549, -20.72916666530106866, -2.574251347313721627 ) ) ;
#1279 = CARTESIAN_POINT ( 'NONE',  ( 4.458734125000000326, -87.89583333196773651, 2.574251347313718519 ) ) ;
#1280 = EDGE_CURVE ( 'NONE', #51312, #21022, #35166, .T. ) ;
#1281 = CARTESIAN_POINT ( 'NONE',  ( 1.060575238724906964E-15, -22.62499999726881228, 5.773502691896257311 ) ) ;
#1283 = ORIENTED_EDGE ( 'NONE', *, *, #51078, .F. ) ;
#1282 = CARTESIAN_POINT ( 'NONE',  ( -2.229367062500000163, -57.47916666530107932, -3.861377020970580443 ) ) ;
#1284 = CARTESIAN_POINT ( 'NONE',  ( 1.339745962155612702, -49.29465819873851018, -5.000000000000000000 ) ) ;
#1285 = FACE_OUTER_BOUND ( 'NONE', #43628, .T. ) ;
#1286 = EDGE_CURVE ( 'NONE', #12722, #37461, #37163, .T. ) ;
#1288 = ORIENTED_EDGE ( 'NONE', *, *, #28159, .F. ) ;
#1287 = CARTESIAN_POINT ( 'NONE',  ( -4.458734124999999437, -2.645833331967737845, -2.574251347313719407 ) ) ;
#1289 = CARTESIAN_POINT ( 'NONE',  ( -54.64476657466781973, -149.8125000013656063, -4.444560631937228834 ) ) ;
#1290 = CARTESIAN_POINT ( 'NONE',  ( 5.000000000000000000, -68.49999999999998579, -6.123233995736766282E-16 ) ) ;
#1291 = ADVANCED_FACE ( 'NONE', ( #21734 ), #1809, .T. ) ;
#1292 = CARTESIAN_POINT ( 'NONE',  ( 3.152801135295367541, -151.5625000013655779, -3.152801135295367541 ) ) ;
#1293 = CARTESIAN_POINT ( 'NONE',  ( 4.458734124999999437, -48.06249999863440792, -5.460374474430324690E-16 ) ) ;
#1294 = CARTESIAN_POINT ( 'NONE',  ( 5.000000000000000000, -23.41666666666667140, -2.886751345948130876 ) ) ;
#1295 = CARTESIAN_POINT ( 'NONE',  ( -9.184850993605147944E-16, -158.2500000000000000, 5.000000000000000000 ) ) ;
#1296 = EDGE_CURVE ( 'NONE', #19989, #11458, #56971, .T. ) ;
#1297 = ADVANCED_FACE ( 'NONE', ( #41638 ), #6305, .F. ) ;
#1298 = CARTESIAN_POINT ( 'NONE',  ( -6.972266317189433020E-16, 6.875000002731185944, -5.000000000000000000 ) ) ;
#1299 = CARTESIAN_POINT ( 'NONE',  ( -58.24261429053147765, -154.2500000000000284, -3.805975901505573855 ) ) ;
#1300 = CARTESIAN_POINT ( 'NONE',  ( -4.458734124999999437, -12.64583333196774007, -2.574251347313719407 ) ) ;
#1301 = CARTESIAN_POINT ( 'NONE',  ( -2.229367062499996610, -52.39583333196773651, 3.861377020970582219 ) ) ;
#1302 = CARTESIAN_POINT ( 'NONE',  ( 1.975475456537005874E-15, 10.24999999999999822, 5.000000000000000000 ) ) ;
#1303 = CARTESIAN_POINT ( 'NONE',  ( -4.458734124999999437, -143.9375000013656063, -5.460374474430324690E-16 ) ) ;
#1304 = CARTESIAN_POINT ( 'NONE',  ( 4.458734125000001214, -93.14583333196773651, 2.574251347313718519 ) ) ;
#1305 = CARTESIAN_POINT ( 'NONE',  ( 2.626220312808019583E-14, 20.87500000273118062, -5.000000000000000000 ) ) ;
#1306 = ORIENTED_EDGE ( 'NONE', *, *, #59063, .T. ) ;
#1307 = DIRECTION ( 'NONE',  ( 0.000000000000000000, 0.000000000000000000, 1.000000000000000000 ) ) ;
#1308 = CARTESIAN_POINT ( 'NONE',  ( 2.229367062499998831, 27.10416666803225993, -3.861377020970580887 ) ) ;
#1309 = CARTESIAN_POINT ( 'NONE',  ( -56.66612745406270335, -145.4375000027312694, -5.149110718188516067 ) ) ;
#1310 = CARTESIAN_POINT ( 'NONE',  ( 1.339745962155615144, -82.58034179853028434, 4.999999999999999112 ) ) ;
#1311 = ORIENTED_EDGE ( 'NONE', *, *, #48302, .T. ) ;
#1312 = CARTESIAN_POINT ( 'NONE',  ( -4.458734124999999437, -4.395833331967740065, -2.574251347313719407 ) ) ;
#1313 =( BOUNDED_CURVE ( )  B_SPLINE_CURVE ( 2, ( #50711, #6343, #25950, #564, #5379, #44604, #21127, #6654, #26260 ),
 .UNSPECIFIED., .F., .F. ) 
 B_SPLINE_CURVE_WITH_KNOTS ( ( 3, 2, 2, 2, 3 ),
 ( 0.4937500000000000222, 0.4944444444444444642, 0.4958333333333333481, 0.4972222222222222321, 0.4979166666666666741 ),
 .UNSPECIFIED. ) 
 CURVE ( )  GEOMETRIC_REPRESENTATION_ITEM ( )  RATIONAL_B_SPLINE_CURVE ( ( 0.9330127018922194093, 0.9330127018922194093, 1.000000000000000000, 0.8660254037844387076, 1.000000000000000000, 0.8660254037844387076, 1.000000000000000000, 0.9330127018922194093, 0.9330127018922194093 ) ) 
 REPRESENTATION_ITEM ( '' )  );
#1314 = CARTESIAN_POINT ( 'NONE',  ( 5.000000000000000000, -50.37499999726881583, -6.123233995736766282E-16 ) ) ;
#1315 = CARTESIAN_POINT ( 'NONE',  ( 4.458734124999998549, -19.97916666530106866, -2.574251347313721627 ) ) ;
#1316 = CARTESIAN_POINT ( 'NONE',  ( -5.000000000000000000, 2.041666669397854239, -2.886751345948128211 ) ) ;
#1317 = CARTESIAN_POINT ( 'NONE',  ( 2.229367062500001939, -7.979166665301073991, 3.861377020970579999 ) ) ;
#1318 = CARTESIAN_POINT ( 'NONE',  ( 4.599534470797546959, -6.460478697736932396, -7.590212325761396706 ) ) ;
#1319 = CARTESIAN_POINT ( 'NONE',  ( -3.152801135295367096, -148.0625000013655779, -3.152801135295367541 ) ) ;
#1320 = CARTESIAN_POINT ( 'NONE',  ( -2.229367062500000163, 15.27083333469892779, -3.861377020970580443 ) ) ;
#1321 = ORIENTED_EDGE ( 'NONE', *, *, #37875, .F. ) ;
#1322 = CARTESIAN_POINT ( 'NONE',  ( 3.749999999999998224, 6.495190528383290918, -6.991905250253753756 ) ) ;
#1323 = CARTESIAN_POINT ( 'NONE',  ( 4.458734124999998549, -21.72916666530107221, -2.574251347313721627 ) ) ;
#1324 = DIRECTION ( 'NONE',  ( -0.000000000000000000, 1.000000000000000000, -0.000000000000000000 ) ) ;
#1325 = CARTESIAN_POINT ( 'NONE',  ( -51.60603307380591787, -148.9375000013656063, -2.891590998281053704 ) ) ;
#1326 = CARTESIAN_POINT ( 'NONE',  ( 5.000000000000000000, -45.29166666393546592, -2.886751345948129988 ) ) ;
#1327 = CARTESIAN_POINT ( 'NONE',  ( -5.000000000000000000, 21.12500000273118417, 0.000000000000000000 ) ) ;
#1328 = CARTESIAN_POINT ( 'NONE',  ( -2.229367062500000163, 13.52083333469892779, -3.861377020970580443 ) ) ;
#1329 = FACE_OUTER_BOUND ( 'NONE', #38194, .T. ) ;
#1330 = AXIS2_PLACEMENT_3D ( 'NONE', #24006, #58732, #21415 ) ;
#1331 = PRODUCT_RELATED_PRODUCT_CATEGORY ( 'part', '', ( #18875 ) ) ;
#1332 = FACE_OUTER_BOUND ( 'NONE', #402, .T. ) ;
#1333 = CARTESIAN_POINT ( 'NONE',  ( -2.229367062499996610, 9.854166668032261711, 3.861377020970582219 ) ) ;
#1334 = CARTESIAN_POINT ( 'NONE',  ( -4.458734124999999437, -69.39583333196773651, -2.574251347313719407 ) ) ;
#1335 = CARTESIAN_POINT ( 'NONE',  ( -3.152548672688508926E-16, -14.81249999863440436, -5.148502694627439702 ) ) ;
#1336 = CARTESIAN_POINT ( 'NONE',  ( -5.000000000000000000, 5.000000000000000888, 0.000000000000000000 ) ) ;
#1337 = CARTESIAN_POINT ( 'NONE',  ( 4.458734124999999437, -165.5000000013655779, 1.846868145590737864 ) ) ;
#1338 = CARTESIAN_POINT ( 'NONE',  ( -4.458734124999999437, -60.39583333196773651, -2.574251347313719407 ) ) ;
#1339 = CARTESIAN_POINT ( 'NONE',  ( -4.999999999999999112, -95.79166666393548724, 2.886751345948131764 ) ) ;
#1340 = CARTESIAN_POINT ( 'NONE',  ( -4.458734124999999437, -34.31249999863440792, 0.000000000000000000 ) ) ;
#1341 = LINE ( 'NONE', #40544, #38061 ) ;
#1342 = CARTESIAN_POINT ( 'NONE',  ( -2.499999999999996447, -54.70833333060213732, 4.330127018922195425 ) ) ;
#1343 = CARTESIAN_POINT ( 'NONE',  ( 5.000000000000000000, -69.41666666666667140, -2.886751345948130876 ) ) ;
#1344 = DIRECTION ( 'NONE',  ( -1.000000000000000000, -0.000000000000000000, -0.000000000000000000 ) ) ;
#1345 = CARTESIAN_POINT ( 'NONE',  ( 4.458734124999999437, -150.6250000013655779, -1.846868145590734978 ) ) ;
#1346 = CARTESIAN_POINT ( 'NONE',  ( -4.999999999999999112, -40.91666666666667140, 2.886751345948131764 ) ) ;
#1347 = CARTESIAN_POINT ( 'NONE',  ( -1.339745962155613812, -58.08034179853029144, -5.000000000000000000 ) ) ;
#1348 = CARTESIAN_POINT ( 'NONE',  ( 1.339745962155612702, -17.16965819600733312, -5.000000000000000000 ) ) ;
#1349 = ORIENTED_EDGE ( 'NONE', *, *, #54312, .T. ) ;
#1350 = CARTESIAN_POINT ( 'NONE',  ( -4.458734124999999437, -108.3958333319677365, -2.574251347313719407 ) ) ;
#1351 = CARTESIAN_POINT ( 'NONE',  ( 2.229367062500001939, -3.229166665301069550, 3.861377020970579999 ) ) ;
#1352 = DIRECTION ( 'NONE',  ( -0.000000000000000000, 1.000000000000000000, -0.000000000000000000 ) ) ;
#1353 = CARTESIAN_POINT ( 'NONE',  ( 5.000000000000000000, -1.416666666666663188, -2.886751345948129988 ) ) ;
#1354 = CARTESIAN_POINT ( 'NONE',  ( 2.229367062499998831, -66.64583333196773651, -3.861377020970580887 ) ) ;
#1355 = CARTESIAN_POINT ( 'NONE',  ( 0.000000000000000000, -170.0000000000000000, 0.000000000000000000 ) ) ;
#1356 = CARTESIAN_POINT ( 'NONE',  ( -3.535250795749689387E-16, -10.12499999726881583, -5.773502691896257311 ) ) ;
#1358 = ORIENTED_EDGE ( 'NONE', *, *, #9494, .F. ) ;
#1357 = CARTESIAN_POINT ( 'NONE',  ( 4.458734125000001214, -41.89583333196773651, 2.574251347313718519 ) ) ;
#1359 = CARTESIAN_POINT ( 'NONE',  ( 5.000000000000000000, -33.50000000000000000, -6.123233995736766282E-16 ) ) ;
#1360 = CARTESIAN_POINT ( 'NONE',  ( -1.975475456537005874E-15, 28.37500000273118772, 5.000000000000000000 ) ) ;
#1362 = EDGE_LOOP ( 'NONE', ( #6334, #6963, #51446, #31577 ) ) ;
#1361 = CARTESIAN_POINT ( 'NONE',  ( 4.458734125000001214, 11.85416666803225993, 2.574251347313718519 ) ) ;
#1363 =( BOUNDED_CURVE ( )  B_SPLINE_CURVE ( 2, ( #26122, #14945, #56035, #36405, #34554, #39383, #16787, #16151, #11951 ),
 .UNSPECIFIED., .F., .F. ) 
 B_SPLINE_CURVE_WITH_KNOTS ( ( 3, 2, 2, 2, 3 ),
 ( 0.8196428571428571175, 0.8202380952380952106, 0.8214285714285713969, 0.8226190476190475831, 0.8232142857142856762 ),
 .UNSPECIFIED. ) 
 CURVE ( )  GEOMETRIC_REPRESENTATION_ITEM ( )  RATIONAL_B_SPLINE_CURVE ( ( 0.9330127018922194093, 0.9330127018922194093, 1.000000000000000000, 0.8660254037844387076, 1.000000000000000000, 0.8660254037844387076, 1.000000000000000000, 0.9330127018922194093, 0.9330127018922194093 ) ) 
 REPRESENTATION_ITEM ( '' )  );
#1364 = CARTESIAN_POINT ( 'NONE',  ( -57.46284108482265651, -141.0625000027312410, 4.819101127000238627 ) ) ;
#1365 = CARTESIAN_POINT ( 'NONE',  ( 2.499999999999998668, -51.33333333333332860, -4.330127018922193649 ) ) ;
#1366 = EDGE_CURVE ( 'NONE', #4014, #25951, #44155, .T. ) ;
#1367 = CARTESIAN_POINT ( 'NONE',  ( 2.229367062499998831, -32.89583333196773651, -3.861377020970580887 ) ) ;
#1368 = CARTESIAN_POINT ( 'NONE',  ( 4.458734124999999437, -77.81249999863440792, -5.460374474430324690E-16 ) ) ;
#1369 = CARTESIAN_POINT ( 'NONE',  ( -4.458734125000000326, -140.2500000013656063, -1.846868145590735644 ) ) ;
#1370 = EDGE_CURVE ( 'NONE', #3563, #63012, #37238, .T. ) ;
#1371 = CARTESIAN_POINT ( 'NONE',  ( 4.458734125000001214, -80.89583333196773651, 2.574251347313718519 ) ) ;
#1372 = CARTESIAN_POINT ( 'NONE',  ( -59.59170313451811296, -135.7500000013656063, 1.485763867205729394 ) ) ;
#1373 = CARTESIAN_POINT ( 'NONE',  ( 9.457646018065525792E-16, -35.31249999863440792, 5.148502694627439702 ) ) ;
#1374 = EDGE_CURVE ( 'NONE', #51281, #47780, #57350, .T. ) ;
#1375 = EDGE_LOOP ( 'NONE', ( #54448, #15901, #4722, #27782 ) ) ;
#1376 = CARTESIAN_POINT ( 'NONE',  ( -6.972266317189433020E-16, -51.25000000000000000, -5.000000000000000000 ) ) ;
#1377 = ORIENTED_EDGE ( 'NONE', *, *, #11489, .T. ) ;
#1378 = CARTESIAN_POINT ( 'NONE',  ( -4.458734124999998549, -76.47916666530105090, 2.574251347313722516 ) ) ;
#1379 = CARTESIAN_POINT ( 'NONE',  ( -6.972266317189433020E-16, 12.87500000273118417, -5.000000000000000000 ) ) ;
#1380 = ORIENTED_EDGE ( 'NONE', *, *, #33927, .T. ) ;
#1381 = CARTESIAN_POINT ( 'NONE',  ( 5.000000000000000000, -16.50000000000000000, -6.123233995736766282E-16 ) ) ;
#1382 = CARTESIAN_POINT ( 'NONE',  ( 1.062108568985190270E-13, -12.25000000000000000, -4.999999999999999112 ) ) ;
#1383 = CARTESIAN_POINT ( 'NONE',  ( 9.457646018065525792E-16, -64.31249999863440792, 5.148502694627439702 ) ) ;
#1384 = CARTESIAN_POINT ( 'NONE',  ( -4.458734124999998549, -4.479166665301070438, 2.574251347313722516 ) ) ;
#1385 = EDGE_LOOP ( 'NONE', ( #55922, #57745, #15564, #16254 ) ) ;
#1386 = CARTESIAN_POINT ( 'NONE',  ( 6.123233995736766282E-16, -120.0000000000000000, -5.000000000000000000 ) ) ;
#1387 = CARTESIAN_POINT ( 'NONE',  ( 9.457646018065525792E-16, 8.937500001365597413, 5.148502694627439702 ) ) ;
#1388 = CARTESIAN_POINT ( 'NONE',  ( -57.89159099828107458, -140.6875000013656063, -3.393966926194107447 ) ) ;
#1389 = CARTESIAN_POINT ( 'NONE',  ( -51.75738570946856498, -154.7500000000000284, 3.805975901505576964 ) ) ;
#1390 = CARTESIAN_POINT ( 'NONE',  ( 4.458734124999999437, -161.4375000013655779, 0.000000000000000000 ) ) ;
#1391 = FACE_OUTER_BOUND ( 'NONE', #60635, .T. ) ;
#1392 = ORIENTED_EDGE ( 'NONE', *, *, #63423, .T. ) ;
#1393 = CARTESIAN_POINT ( 'NONE',  ( 2.229367062499998831, -82.64583333196773651, -3.861377020970580887 ) ) ;
#1394 = CARTESIAN_POINT ( 'NONE',  ( -5.000000000000000000, -97.00000000000000000, 0.000000000000000000 ) ) ;
#1395 = CARTESIAN_POINT ( 'NONE',  ( 2.229367062500001939, -5.979166665301072214, 3.861377020970579999 ) ) ;
#1396 = CARTESIAN_POINT ( 'NONE',  ( -1.339745962155610925, -67.79465819873851729, 5.000000000000000000 ) ) ;
#1397 = CARTESIAN_POINT ( 'NONE',  ( -4.458734124999999437, -72.64583333196773651, -2.574251347313719407 ) ) ;
#1398 = CARTESIAN_POINT ( 'NONE',  ( -4.999999999999999112, -29.79166666393548368, 2.886751345948131764 ) ) ;
#1399 = CARTESIAN_POINT ( 'NONE',  ( 1.975475456537005874E-15, -84.74999999999998579, 5.000000000000000000 ) ) ;
#1400 = CARTESIAN_POINT ( 'NONE',  ( -2.500000000000000444, -41.16666666666667140, -4.330127018922193649 ) ) ;
#1401 = CARTESIAN_POINT ( 'NONE',  ( -1.339745962155613812, -83.08034179853028434, -5.000000000000000000 ) ) ;
#1402 = CARTESIAN_POINT ( 'NONE',  ( 4.458734124999998549, 27.27083333469892779, -2.574251347313721627 ) ) ;
#1403 = CARTESIAN_POINT ( 'NONE',  ( -4.458734124999999437, -49.39583333196773651, -2.574251347313719407 ) ) ;
#1404 = CARTESIAN_POINT ( 'NONE',  ( 4.458734124999999437, -32.06249999863440792, -5.460374474430324690E-16 ) ) ;
#1405 = CARTESIAN_POINT ( 'NONE',  ( -4.458734124999999437, 0.3541666680322609340, -2.574251347313719407 ) ) ;
#1406 =( BOUNDED_CURVE ( )  B_SPLINE_CURVE ( 2, ( #52966, #58106, #14034, #52656, #24010, #3774, #23397, #57805, #57502 ),
 .UNSPECIFIED., .F., .F. ) 
 B_SPLINE_CURVE_WITH_KNOTS ( ( 3, 2, 2, 2, 3 ),
 ( 0.8937500000000000444, 0.8944444444444444864, 0.8958333333333333703, 0.8972222222222222543, 0.8979166666666666963 ),
 .UNSPECIFIED. ) 
 CURVE ( )  GEOMETRIC_REPRESENTATION_ITEM ( )  RATIONAL_B_SPLINE_CURVE ( ( 0.9330127018922194093, 0.9330127018922194093, 1.000000000000000000, 0.8660254037844387076, 1.000000000000000000, 0.8660254037844387076, 1.000000000000000000, 0.9330127018922194093, 0.9330127018922194093 ) ) 
 REPRESENTATION_ITEM ( '' )  );
#1407 = CYLINDRICAL_SURFACE ( 'NONE', #30891, 4.250000000000000000 ) ;
#1408 = CARTESIAN_POINT ( 'NONE',  ( -4.999999999999999112, 20.08333333333333215, 2.886751345948131764 ) ) ;
#1409 = CARTESIAN_POINT ( 'NONE',  ( 5.000000000000000000, -144.1250000027312126, 0.000000000000000000 ) ) ;
#1410 = CARTESIAN_POINT ( 'NONE',  ( 0.000000000000000000, -120.0000000000000000, 0.000000000000000000 ) ) ;
#1411 = CARTESIAN_POINT ( 'NONE',  ( 2.229367062500001939, -42.97916666530107932, 3.861377020970579999 ) ) ;
#1412 = CARTESIAN_POINT ( 'NONE',  ( 1.060575238724906964E-15, -77.62499999726881583, 5.773502691896257311 ) ) ;
#1413 = CARTESIAN_POINT ( 'NONE',  ( -51.60603307380591787, -141.1875000013656063, -2.891590998281053704 ) ) ;
#1414 = AXIS2_PLACEMENT_3D ( 'NONE', #47704, #53165, #3658 ) ;
#1415 = DIRECTION ( 'NONE',  ( 0.000000000000000000, 0.000000000000000000, 1.000000000000000000 ) ) ;
#1416 = EDGE_CURVE ( 'NONE', #60061, #26022, #22367, .T. ) ;
#1417 = CARTESIAN_POINT ( 'NONE',  ( 1.339745962155615144, -37.70534180126148271, 4.999999999999999112 ) ) ;
#1418 = CARTESIAN_POINT ( 'NONE',  ( 4.458734124999998549, -79.97916666530106511, -2.574251347313721627 ) ) ;
#1419 = CARTESIAN_POINT ( 'NONE',  ( 4.458734124999999437, -161.6875000013655779, 0.000000000000000000 ) ) ;
#1420 = CARTESIAN_POINT ( 'NONE',  ( 5.000000000000000888, 7.416666666666665186, 2.886751345948126879 ) ) ;
#1421 = CARTESIAN_POINT ( 'NONE',  ( 2.499999999999998668, -29.33333333333332860, -4.330127018922193649 ) ) ;
#1422 = LINE ( 'NONE', #21021, #18188 ) ;
#1423 = VERTEX_POINT ( 'NONE', #56144 ) ;
#1424 = CARTESIAN_POINT ( 'NONE',  ( -4.458734124999998549, 24.52083333469892779, 2.574251347313722516 ) ) ;
#1425 = VERTEX_POINT ( 'NONE', #55825 ) ;
#1426 = CARTESIAN_POINT ( 'NONE',  ( 9.457646018065525792E-16, -60.31249999863441502, 5.148502694627439702 ) ) ;
#1427 = CARTESIAN_POINT ( 'NONE',  ( -5.000000000000000000, 21.04166666939785202, -2.886751345948128211 ) ) ;
#1428 = CARTESIAN_POINT ( 'NONE',  ( -2.499999999999996447, -60.70833333060214443, 4.330127018922195425 ) ) ;
#1429 = CARTESIAN_POINT ( 'NONE',  ( -5.000000000000000000, 13.00000000000000178, 0.000000000000000000 ) ) ;
#1430 = CARTESIAN_POINT ( 'NONE',  ( 4.458734124999998549, -52.72916666530107221, -2.574251347313721627 ) ) ;
#1431 = CARTESIAN_POINT ( 'NONE',  ( 4.458734125000001214, -11.89583333196774007, 2.574251347313718519 ) ) ;
#1432 = CARTESIAN_POINT ( 'NONE',  ( -58.24261429053147765, -151.3750000027312126, -3.805975901505573855 ) ) ;
#1433 = CARTESIAN_POINT ( 'NONE',  ( -4.999999999999998224, 14.08333333333333393, 2.886751345948131764 ) ) ;
#1434 = CARTESIAN_POINT ( 'NONE',  ( -1.339745962155613812, -64.20534180126146850, -5.000000000000000000 ) ) ;
#1435 = CARTESIAN_POINT ( 'NONE',  ( -1.510657702057710340E-15, 27.37500000273118417, 5.000000000000000000 ) ) ;
#1436 = CARTESIAN_POINT ( 'NONE',  ( -4.999999999999999112, -32.91666666666666430, 2.886751345948131764 ) ) ;
#1438 = CARTESIAN_POINT ( 'NONE',  ( 4.458734124999998549, -13.97916666530107221, -2.574251347313721627 ) ) ;
#1437 = CARTESIAN_POINT ( 'NONE',  ( -1.339745962155613812, -34.20534180126147561, -5.000000000000000000 ) ) ;
#1439 = CARTESIAN_POINT ( 'NONE',  ( -2.499999999999996447, -31.70833333060214798, 4.330127018922195425 ) ) ;
#1440 = CARTESIAN_POINT ( 'NONE',  ( 2.229367062500001939, -60.97916666530106511, 3.861377020970579999 ) ) ;
#1441 = CARTESIAN_POINT ( 'NONE',  ( 4.458734125000000326, -152.6250000013655495, -1.846868145590734978 ) ) ;
#1442 = CARTESIAN_POINT ( 'NONE',  ( -4.458734124999999437, -65.39583333196773651, -2.574251347313719407 ) ) ;
#1443 = CARTESIAN_POINT ( 'NONE',  ( -5.000000000000000000, -56.87499999726880162, 0.000000000000000000 ) ) ;
#1444 = AXIS2_PLACEMENT_3D ( 'NONE', #10621, #50516, #34419 ) ;
#1445 = VERTEX_POINT ( 'NONE', #31049 ) ;
#1446 = CARTESIAN_POINT ( 'NONE',  ( -54.60164318462004474, -137.3750000000000284, -4.984105922594373794 ) ) ;
#1447 = CARTESIAN_POINT ( 'NONE',  ( 4.458734124999998549, 1.020833334698927120, -2.574251347313721627 ) ) ;
#1448 = VERTEX_POINT ( 'NONE', #61609 ) ;
#1449 = CARTESIAN_POINT ( 'NONE',  ( -6.972266317189433020E-16, -58.24999999999999289, -5.000000000000000000 ) ) ;
#1450 = CARTESIAN_POINT ( 'NONE',  ( -4.458734125000001214, -152.8750000013655779, 1.846868145590734089 ) ) ;
#1451 = ORIENTED_EDGE ( 'NONE', *, *, #60890, .F. ) ;
#1452 = CARTESIAN_POINT ( 'NONE',  ( -5.000000000000000000, -10.00000000000000178, 0.000000000000000000 ) ) ;
#1453 = CARTESIAN_POINT ( 'NONE',  ( -51.19402409849444524, -129.5000000000000284, -3.242614290531456334 ) ) ;
#1454 = CARTESIAN_POINT ( 'NONE',  ( 5.000000000000000000, -161.1250000027311842, 0.000000000000000000 ) ) ;
#1455 = CARTESIAN_POINT ( 'NONE',  ( -3.152548672688508926E-16, -47.81249999863440792, -5.148502694627439702 ) ) ;
#1456 = ORIENTED_EDGE ( 'NONE', *, *, #51051, .T. ) ;
#1457 = VECTOR ( 'NONE', #822, 1000.000000000000000 ) ;
#1458 = CARTESIAN_POINT ( 'NONE',  ( 5.000000000000000000, 11.58333333333333393, -2.886751345948130876 ) ) ;
#1459 = CARTESIAN_POINT ( 'NONE',  ( -4.458734124999998549, 14.77083333469892779, 2.574251347313722516 ) ) ;
#1460 = CARTESIAN_POINT ( 'NONE',  ( 2.229367062500001939, 25.02083333469892779, 3.861377020970579999 ) ) ;
#1461 = CARTESIAN_POINT ( 'NONE',  ( -50.55543936806279248, -151.0625000013656063, 0.3552334253322060320 ) ) ;
#1462 = CARTESIAN_POINT ( 'NONE',  ( -6.972266317189433020E-16, -73.12499999726878741, -5.000000000000000000 ) ) ;
#1463 = ORIENTED_EDGE ( 'NONE', *, *, #60243, .T. ) ;
#1464 = CARTESIAN_POINT ( 'NONE',  ( -4.458734124999997661, -63.22916666530106511, 2.574251347313722516 ) ) ;
#1465 = CARTESIAN_POINT ( 'NONE',  ( 5.000000000000000000, -28.29166666393548013, -2.886751345948130876 ) ) ;
#1466 = CARTESIAN_POINT ( 'NONE',  ( -2.229367062499996610, 12.85416666803226171, 3.861377020970582219 ) ) ;
#1467 = EDGE_CURVE ( 'NONE', #46511, #2425, #9232, .T. ) ;
#1468 = CARTESIAN_POINT ( 'NONE',  ( 1.975475456537005874E-15, -80.62499999726881583, 5.000000000000000000 ) ) ;
#1469 = CARTESIAN_POINT ( 'NONE',  ( -4.458734124999998549, -52.47916666530107221, 2.574251347313722516 ) ) ;
#1470 = CARTESIAN_POINT ( 'NONE',  ( -2.500000000000000444, -15.04166666393548191, -4.330127018922193649 ) ) ;
#1471 = FACE_OUTER_BOUND ( 'NONE', #14492, .T. ) ;
#1472 = CARTESIAN_POINT ( 'NONE',  ( 7.500000000000000000, -3.988190556646209028, -0.8526458641284331286 ) ) ;
#1473 = CARTESIAN_POINT ( 'NONE',  ( 1.975475456537005874E-15, -87.75000000000001421, 5.000000000000000000 ) ) ;
#1474 = CARTESIAN_POINT ( 'NONE',  ( -4.999999999999998224, 11.20833333606451809, 2.886751345948131764 ) ) ;
#1475 = CARTESIAN_POINT ( 'NONE',  ( 9.457646018065525792E-16, -18.31249999863440792, 5.148502694627439702 ) ) ;
#1476 = ORIENTED_EDGE ( 'NONE', *, *, #16143, .T. ) ;
#1477 = CARTESIAN_POINT ( 'NONE',  ( -3.152548672688508926E-16, -102.5624999986344079, -5.148502694627439702 ) ) ;
#1478 = CARTESIAN_POINT ( 'NONE',  ( 3.535533905932738197, -156.0000000027312126, -3.535533905932738197 ) ) ;
#1479 = ORIENTED_EDGE ( 'NONE', *, *, #11487, .T. ) ;
#1480 = CARTESIAN_POINT ( 'NONE',  ( -4.458734124999999437, -100.6458333319677223, -2.574251347313719407 ) ) ;
#1481 = CARTESIAN_POINT ( 'NONE',  ( 2.229367062499998831, -25.64583333196773651, -3.861377020970580887 ) ) ;
#1482 = CARTESIAN_POINT ( 'NONE',  ( -5.000000000000000000, -58.95833333060213732, -2.886751345948128211 ) ) ;
#1483 =( BOUNDED_CURVE ( )  B_SPLINE_CURVE ( 2, ( #2069, #2377, #40642, #40955, #16522, #35830, #56083, #11368, #11053 ),
 .UNSPECIFIED., .F., .F. ) 
 B_SPLINE_CURVE_WITH_KNOTS ( ( 3, 2, 2, 2, 3 ),
 ( 0.5562500000000000222, 0.5569444444444444642, 0.5583333333333333481, 0.5597222222222222321, 0.5604166666666666741 ),
 .UNSPECIFIED. ) 
 CURVE ( )  GEOMETRIC_REPRESENTATION_ITEM ( )  RATIONAL_B_SPLINE_CURVE ( ( 0.9330127018922194093, 0.9330127018922194093, 1.000000000000000000, 0.8660254037844387076, 1.000000000000000000, 0.8660254037844387076, 1.000000000000000000, 0.9330127018922194093, 0.9330127018922194093 ) ) 
 REPRESENTATION_ITEM ( '' )  );
#1484 = CARTESIAN_POINT ( 'NONE',  ( -59.29741812935640155, -127.6250000013656205, -2.196230717870135685 ) ) ;
#1485 = CARTESIAN_POINT ( 'NONE',  ( -50.55543936806279248, -141.0625000013656063, 0.3552334253322060320 ) ) ;
#1486 = CARTESIAN_POINT ( 'NONE',  ( 2.229367062500001939, -21.97916666530107221, 3.861377020970579999 ) ) ;
#1487 = CARTESIAN_POINT ( 'NONE',  ( -4.458734124999997661, -65.47916666530106511, 2.574251347313722516 ) ) ;
#1488 = CARTESIAN_POINT ( 'NONE',  ( -50.18089887299979068, -153.8125000027311842, 2.462841084822631199 ) ) ;
#1489 = CARTESIAN_POINT ( 'NONE',  ( -2.229367062499996610, -19.14583333196774007, 3.861377020970582219 ) ) ;
#1490 = CARTESIAN_POINT ( 'NONE',  ( -4.999999999999998224, -79.79166666393545881, 2.886751345948131764 ) ) ;
#1491 = CARTESIAN_POINT ( 'NONE',  ( -2.071067811865475061, -150.6875000000000284, -5.000000000000000888 ) ) ;
#1492 = CARTESIAN_POINT ( 'NONE',  ( 5.000000000000000000, -11.49999999999999645, -6.123233995736766282E-16 ) ) ;
#1493 = CARTESIAN_POINT ( 'NONE',  ( -8.190561711645485556E-16, -153.6875000013656063, 4.458734124999999437 ) ) ;
#1494 = VERTEX_POINT ( 'NONE', #33583 ) ;
#1495 = CARTESIAN_POINT ( 'NONE',  ( 4.458734124999998549, -46.97916666530106511, -2.574251347313721627 ) ) ;
#1496 = DIRECTION ( 'NONE',  ( 0.000000000000000000, 0.000000000000000000, 1.000000000000000000 ) ) ;
#1497 = CARTESIAN_POINT ( 'NONE',  ( -6.972266317189433020E-16, -92.24999999999998579, -5.000000000000000000 ) ) ;
#1498 = CARTESIAN_POINT ( 'NONE',  ( 4.458734125000001214, -88.89583333196773651, 2.574251347313718519 ) ) ;
#1499 = AXIS2_PLACEMENT_3D ( 'NONE', #26170, #6879, #40327 ) ;
#1500 = CARTESIAN_POINT ( 'NONE',  ( 2.229367062500001939, 6.020833334698927786, 3.861377020970579999 ) ) ;
#1501 =( BOUNDED_CURVE ( )  B_SPLINE_CURVE ( 2, ( #6880, #21036, #31302, #45470, #15576, #11369, #26811, #59967, #1751 ),
 .UNSPECIFIED., .F., .F. ) 
 B_SPLINE_CURVE_WITH_KNOTS ( ( 3, 2, 2, 2, 3 ),
 ( 0.2874999999999999778, 0.2880952380952380709, 0.2892857142857143127, 0.2904761904761904989, 0.2910714285714285920 ),
 .UNSPECIFIED. ) 
 CURVE ( )  GEOMETRIC_REPRESENTATION_ITEM ( )  RATIONAL_B_SPLINE_CURVE ( ( 0.9330127018922194093, 0.9330127018922194093, 1.000000000000000000, 0.8660254037844387076, 1.000000000000000000, 0.8660254037844387076, 1.000000000000000000, 0.9330127018922194093, 0.9330127018922194093 ) ) 
 REPRESENTATION_ITEM ( '' )  );
#1502 = CYLINDRICAL_SURFACE ( 'NONE', #16298, 5.000000000000000000 ) ;
#1503 = CARTESIAN_POINT ( 'NONE',  ( -1.339745962155613812, 25.79465819873851729, -5.000000000000000000 ) ) ;
#1504 = CARTESIAN_POINT ( 'NONE',  ( -4.458734124999999437, 13.35416666803225993, -2.574251347313719407 ) ) ;
#1505 = CARTESIAN_POINT ( 'NONE',  ( 2.500000000000002220, -78.66666666666665719, 4.330127018922192761 ) ) ;
#1506 = CARTESIAN_POINT ( 'NONE',  ( -4.999999999999999112, 8.208333336064518093, 2.886751345948131764 ) ) ;
#1507 = VERTEX_POINT ( 'NONE', #19088 ) ;
#1508 = CARTESIAN_POINT ( 'NONE',  ( 5.000000000000000000, -80.29166666393547303, -2.886751345948130876 ) ) ;
#1509 = ORIENTED_EDGE ( 'NONE', *, *, #41308, .F. ) ;
#1510 = CARTESIAN_POINT ( 'NONE',  ( 4.458734124999998549, -43.72916666530106511, -2.574251347313721627 ) ) ;
#1511 = CARTESIAN_POINT ( 'NONE',  ( -8.190561711645485556E-16, -162.9375000013655779, 4.458734124999999437 ) ) ;
#1512 = CARTESIAN_POINT ( 'NONE',  ( 2.499999999999998668, -39.20833333060214443, -4.330127018922193649 ) ) ;
#1513 = VERTEX_POINT ( 'NONE', #57726 ) ;
#1514 = CARTESIAN_POINT ( 'NONE',  ( 9.457646018065525792E-16, -16.06249999863440436, 5.148502694627439702 ) ) ;
#1515 = ORIENTED_EDGE ( 'NONE', *, *, #26383, .T. ) ;
#1516 = CARTESIAN_POINT ( 'NONE',  ( -4.999999999999999112, -89.91666666666665719, 2.886751345948131764 ) ) ;
#1517 = CARTESIAN_POINT ( 'NONE',  ( 0.000000000000000000, -170.0000000000000000, 0.000000000000000000 ) ) ;
#1518 = CARTESIAN_POINT ( 'NONE',  ( 5.000000000000000888, -87.45833333060214443, 2.886751345948126879 ) ) ;
#1520 = ORIENTED_EDGE ( 'NONE', *, *, #31152, .F. ) ;
#1519 = CARTESIAN_POINT ( 'NONE',  ( -2.499999999999996447, -18.83333333333333215, 4.330127018922195425 ) ) ;
#1521 = CARTESIAN_POINT ( 'NONE',  ( -55.39835681537999790, -141.8750000000000284, 4.984105922594378235 ) ) ;
#1522 = CARTESIAN_POINT ( 'NONE',  ( 2.229367062499998831, -34.89583333196772941, -3.861377020970580887 ) ) ;
#1523 = CARTESIAN_POINT ( 'NONE',  ( -1.339745962155610925, -83.79465819873851729, 5.000000000000000000 ) ) ;
#1524 = EDGE_LOOP ( 'NONE', ( #16159, #35442, #61894, #52375 ) ) ;
#1525 = SHAPE_DEFINITION_REPRESENTATION ( #33781, #3639 ) ;
#1526 = CARTESIAN_POINT ( 'NONE',  ( -2.229367062500000163, -75.47916666530106511, -3.861377020970580443 ) ) ;
#1527 = CARTESIAN_POINT ( 'NONE',  ( 2.229367062500001939, -110.2291666653010651, 3.861377020970579999 ) ) ;
#1528 = CARTESIAN_POINT ( 'NONE',  ( 1.339745962155615144, 20.29465819873851729, 4.999999999999999112 ) ) ;
#1529 = EDGE_LOOP ( 'NONE', ( #40093, #8346, #38892, #9831 ) ) ;
#1530 = CARTESIAN_POINT ( 'NONE',  ( -57.89159099828107458, -140.9375000013656063, -3.393966926194107447 ) ) ;
#1531 = CARTESIAN_POINT ( 'NONE',  ( -4.458734124999999437, -81.56249999863440792, 0.000000000000000000 ) ) ;
#1532 = CARTESIAN_POINT ( 'NONE',  ( -50.01589407740564042, -133.7500000027312126, 0.3983568153799778022 ) ) ;
#1533 = CARTESIAN_POINT ( 'NONE',  ( 2.229367062500001939, -43.97916666530106511, 3.861377020970579999 ) ) ;
#1534 = CARTESIAN_POINT ( 'NONE',  ( -3.152801135295367096, -140.3125000013655779, -3.152801135295367541 ) ) ;
#1535 = CARTESIAN_POINT ( 'NONE',  ( -5.000000000000000000, -57.99999999999999289, 0.000000000000000000 ) ) ;
#1536 = CARTESIAN_POINT ( 'NONE',  ( 2.229367062499998831, -51.64583333196773651, -3.861377020970580887 ) ) ;
#1537 = CARTESIAN_POINT ( 'NONE',  ( 4.458734124999999437, -46.81249999863440792, -5.460374474430324690E-16 ) ) ;
#1538 = CARTESIAN_POINT ( 'NONE',  ( -5.000000000000000000, 27.99999999999999645, 0.000000000000000000 ) ) ;
#1539 = EDGE_CURVE ( 'NONE', #33853, #57375, #6812, .T. ) ;
#1540 = CARTESIAN_POINT ( 'NONE',  ( 2.229367062499998831, -15.64583333196773651, -3.861377020970580887 ) ) ;
#1541 = CARTESIAN_POINT ( 'NONE',  ( -5.000000000000000000, -102.0000000000000142, 0.000000000000000000 ) ) ;
#1542 = AXIS2_PLACEMENT_3D ( 'NONE', #31166, #26034, #35687 ) ;
#1543 = CARTESIAN_POINT ( 'NONE',  ( -3.152801135295367985, -141.0625000013655779, 3.152801135295367096 ) ) ;
#1544 = CARTESIAN_POINT ( 'NONE',  ( -4.458734124999999437, -37.64583333196773651, -2.574251347313719407 ) ) ;
#1545 = CARTESIAN_POINT ( 'NONE',  ( 5.000000000000000000, 5.708333336064518981, -2.886751345948129988 ) ) ;
#1546 = CARTESIAN_POINT ( 'NONE',  ( -1.339745962155610925, -39.66965819600733312, 5.000000000000000000 ) ) ;
#1547 = CARTESIAN_POINT ( 'NONE',  ( -55.35523342533222291, -128.3125000013656063, 4.444560631937231499 ) ) ;
#1548 = CARTESIAN_POINT ( 'NONE',  ( 2.229367062500001939, -73.22916666530107932, 3.861377020970579999 ) ) ;
#1549 = CARTESIAN_POINT ( 'NONE',  ( 5.000000000000000000, 24.58333333333333215, -2.886751345948130876 ) ) ;
#1550 = CARTESIAN_POINT ( 'NONE',  ( -6.972266317189433020E-16, -81.12499999726881583, -5.000000000000000000 ) ) ;
#1551 = CARTESIAN_POINT ( 'NONE',  ( -3.152548672688508926E-16, 1.187500001365596081, -5.148502694627439702 ) ) ;
#1552 =( BOUNDED_CURVE ( )  B_SPLINE_CURVE ( 2, ( #55304, #966, #2234, #25706, #40173, #6413, #15733, #59811, #26023 ),
 .UNSPECIFIED., .F., .F. ) 
 B_SPLINE_CURVE_WITH_KNOTS ( ( 3, 2, 2, 2, 3 ),
 ( 0.7937499999999999556, 0.7944444444444443976, 0.7958333333333332815, 0.7972222222222222765, 0.7979166666666667185 ),
 .UNSPECIFIED. ) 
 CURVE ( )  GEOMETRIC_REPRESENTATION_ITEM ( )  RATIONAL_B_SPLINE_CURVE ( ( 0.9330127018922194093, 0.9330127018922194093, 1.000000000000000000, 0.8660254037844387076, 1.000000000000000000, 0.8660254037844387076, 1.000000000000000000, 0.9330127018922194093, 0.9330127018922194093 ) ) 
 REPRESENTATION_ITEM ( '' )  );
#1553 = VERTEX_POINT ( 'NONE', #23312 ) ;
#1554 = CARTESIAN_POINT ( 'NONE',  ( 5.000000000000000888, 24.54166666939784847, 2.886751345948126879 ) ) ;
#1555 = CARTESIAN_POINT ( 'NONE',  ( 2.499999999999998668, -57.33333333333333570, -4.330127018922193649 ) ) ;
#1557 = CARTESIAN_POINT ( 'NONE',  ( -3.152548672688508926E-16, -37.56249999863440792, -5.148502694627439702 ) ) ;
#1556 = CARTESIAN_POINT ( 'NONE',  ( -2.229367062499996610, -90.14583333196773651, 3.861377020970582219 ) ) ;
#1558 = CARTESIAN_POINT ( 'NONE',  ( -2.071067811865478170, -168.4375000027311842, 5.000000000000000000 ) ) ;
#1559 = CARTESIAN_POINT ( 'NONE',  ( -2.229367062499996610, -81.39583333196773651, 3.861377020970582219 ) ) ;
#1560 = CARTESIAN_POINT ( 'NONE',  ( -2.229367062500000163, 15.27083333469892779, -3.861377020970580443 ) ) ;
#1561 = CARTESIAN_POINT ( 'NONE',  ( -4.999999999999998224, -52.91666666666666430, 2.886751345948131764 ) ) ;
#1562 = CARTESIAN_POINT ( 'NONE',  ( -50.40829686548195099, -138.0000000013656063, -1.485763867205728284 ) ) ;
#1563 = CARTESIAN_POINT ( 'NONE',  ( 9.457646018065525792E-16, -7.062499998634404363, 5.148502694627439702 ) ) ;
#1564 = CARTESIAN_POINT ( 'NONE',  ( -4.458734124999998549, 24.52083333469892779, 2.574251347313722516 ) ) ;
#1565 = EDGE_CURVE ( 'NONE', #60372, #41751, #41724, .T. ) ;
#1566 = CARTESIAN_POINT ( 'NONE',  ( 2.229367062499998831, -49.89583333196772941, -3.861377020970580887 ) ) ;
#1567 = CARTESIAN_POINT ( 'NONE',  ( 1.975475456537005874E-15, -36.75000000000000000, 5.000000000000000000 ) ) ;
#1568 = CARTESIAN_POINT ( 'NONE',  ( 4.458734124999998549, -83.72916666530107932, -2.574251347313721627 ) ) ;
#1569 = CARTESIAN_POINT ( 'NONE',  ( -4.458734124999997661, -5.229166665301072214, 2.574251347313722516 ) ) ;
#1570 = CARTESIAN_POINT ( 'NONE',  ( 1.339745962155612702, -109.1696581960073331, -5.000000000000000000 ) ) ;
#1571 = ORIENTED_EDGE ( 'NONE', *, *, #11677, .F. ) ;
#1572 = CARTESIAN_POINT ( 'NONE',  ( 2.229367062500001939, -28.22916666530107221, 3.861377020970579999 ) ) ;
#1573 = CARTESIAN_POINT ( 'NONE',  ( -52.10840900171896806, -132.4375000013656063, 3.393966926194110556 ) ) ;
#1574 = CARTESIAN_POINT ( 'NONE',  ( -2.229367062500000163, -72.47916666530107932, -3.861377020970580443 ) ) ;
#1575 = CARTESIAN_POINT ( 'NONE',  ( -4.458734124999999437, 27.43750000136559208, 0.000000000000000000 ) ) ;
#1576 = EDGE_CURVE ( 'NONE', #45853, #42676, #57102, .T. ) ;
#1577 = CARTESIAN_POINT ( 'NONE',  ( 4.458734125000001214, 22.10416666803225993, 2.574251347313718519 ) ) ;
#1578 = CARTESIAN_POINT ( 'NONE',  ( -6.972266317189433020E-16, -53.24999999999999289, -5.000000000000000000 ) ) ;
#1579 = CARTESIAN_POINT ( 'NONE',  ( 2.500000000000002220, -66.66666666666667140, 4.330127018922192761 ) ) ;
#1580 = CARTESIAN_POINT ( 'NONE',  ( -2.229367062499996610, -77.39583333196773651, 3.861377020970582219 ) ) ;
#1581 = CARTESIAN_POINT ( 'NONE',  ( 5.000000000000000888, -66.58333333333332860, 2.886751345948126879 ) ) ;
#1582 = CARTESIAN_POINT ( 'NONE',  ( 1.975475456537005874E-15, -74.75000000000000000, 5.000000000000000000 ) ) ;
#1583 = CARTESIAN_POINT ( 'NONE',  ( 2.499999999999998668, 22.79166666939785202, -4.330127018922193649 ) ) ;
#1584 = ORIENTED_EDGE ( 'NONE', *, *, #1635, .F. ) ;
#1585 = CARTESIAN_POINT ( 'NONE',  ( -4.999999999999998224, -65.91666666666667140, 2.886751345948131764 ) ) ;
#1586 =( BOUNDED_CURVE ( )  B_SPLINE_CURVE ( 2, ( #2293, #46016, #61144, #50530, #41813, #21580, #17392, #61460, #40862 ),
 .UNSPECIFIED., .F., .F. ) 
 B_SPLINE_CURVE_WITH_KNOTS ( ( 3, 2, 2, 2, 3 ),
 ( 0.7520833333333333259, 0.7527777777777777679, 0.7541666666666666519, 0.7555555555555555358, 0.7562499999999999778 ),
 .UNSPECIFIED. ) 
 CURVE ( )  GEOMETRIC_REPRESENTATION_ITEM ( )  RATIONAL_B_SPLINE_CURVE ( ( 0.9330127018922194093, 0.9330127018922194093, 1.000000000000000000, 0.8660254037844387076, 1.000000000000000000, 0.8660254037844387076, 1.000000000000000000, 0.9330127018922194093, 0.9330127018922194093 ) ) 
 REPRESENTATION_ITEM ( '' )  );
#1587 = CARTESIAN_POINT ( 'NONE',  ( 0.000000000000000000, -170.0000000000000000, 5.000000000000000000 ) ) ;
#1589 = CARTESIAN_POINT ( 'NONE',  ( 5.000000000000000000, -24.41666666666666430, -2.886751345948129988 ) ) ;
#1588 = CARTESIAN_POINT ( 'NONE',  ( -6.972266317189433020E-16, -107.1249999972687874, -5.000000000000000000 ) ) ;
#1590 = CARTESIAN_POINT ( 'NONE',  ( -4.458734124999999437, -25.31249999863440792, 0.000000000000000000 ) ) ;
#1591 = CARTESIAN_POINT ( 'NONE',  ( -6.972266317189433020E-16, -62.24999999999999289, -5.000000000000000000 ) ) ;
#1592 = CONICAL_SURFACE ( 'NONE', #39562, 7.500000000000001776, 0.8594454914424796144 ) ;
#1593 = CARTESIAN_POINT ( 'NONE',  ( 1.060575238724906964E-15, -21.62499999726881228, 5.773502691896257311 ) ) ;
#1594 = EDGE_CURVE ( 'NONE', #1054, #5665, #13371, .T. ) ;
#1596 = VERTEX_POINT ( 'NONE', #46851 ) ;
#1595 = CARTESIAN_POINT ( 'NONE',  ( 4.458734124999999437, -53.81249999863439371, -5.460374474430324690E-16 ) ) ;
#1597 = CARTESIAN_POINT ( 'NONE',  ( 0.000000000000000000, -120.0000000000000000, 5.000000000000000000 ) ) ;
#1598 = CARTESIAN_POINT ( 'NONE',  ( 5.000000000000000000, 27.62500000273118417, -6.123233995736766282E-16 ) ) ;
#1600 = ORIENTED_EDGE ( 'NONE', *, *, #34157, .F. ) ;
#1599 = CARTESIAN_POINT ( 'NONE',  ( 4.458734124999998549, -1.979166665301068662, -2.574251347313721627 ) ) ;
#1601 = CARTESIAN_POINT ( 'NONE',  ( 5.000000000000000000, -70.50000000000000000, -6.123233995736766282E-16 ) ) ;
#1602 = CARTESIAN_POINT ( 'NONE',  ( -3.152801135295367096, -151.3125000013655779, -3.152801135295367541 ) ) ;
#1603 = CARTESIAN_POINT ( 'NONE',  ( 4.458734124999998549, -43.97916666530105800, -2.574251347313721627 ) ) ;
#1604 = CARTESIAN_POINT ( 'NONE',  ( -6.972266317189433020E-16, -78.12499999726881583, -5.000000000000000000 ) ) ;
#1605 = CARTESIAN_POINT ( 'NONE',  ( -5.000000000000000000, -157.5000000000000000, -6.123233995736766282E-16 ) ) ;
#1606 = CARTESIAN_POINT ( 'NONE',  ( -6.972266317189433020E-16, -82.12499999726881583, -5.000000000000000000 ) ) ;
#1607 = CARTESIAN_POINT ( 'NONE',  ( -56.48576386720575471, -125.0000000013656205, -4.591703134518078322 ) ) ;
#1608 = CARTESIAN_POINT ( 'NONE',  ( -2.229367062499996610, -16.39583333196773651, 3.861377020970582219 ) ) ;
#1609 = CARTESIAN_POINT ( 'NONE',  ( 4.458734125000001214, -52.14583333196772941, 2.574251347313718519 ) ) ;
#1610 = PLANE ( 'NONE',  #61219 ) ;
#1611 = CARTESIAN_POINT ( 'NONE',  ( -3.152801135295367096, -146.0625000013655779, -3.152801135295367541 ) ) ;
#1612 = CARTESIAN_POINT ( 'NONE',  ( 2.229367062500001939, -95.22916666530106511, 3.861377020970579999 ) ) ;
#1613 = DIRECTION ( 'NONE',  ( -0.000000000000000000, 1.000000000000000000, -0.000000000000000000 ) ) ;
#1614 = ORIENTED_EDGE ( 'NONE', *, *, #46136, .T. ) ;
#1615 = CARTESIAN_POINT ( 'NONE',  ( -5.000000000000000000, -155.5000000000000000, -6.123233995736766282E-16 ) ) ;
#1616 = CARTESIAN_POINT ( 'NONE',  ( -4.458734124999998549, 24.52083333469892779, 2.574251347313722516 ) ) ;
#1617 = CARTESIAN_POINT ( 'NONE',  ( -58.24261429053147765, -145.3750000027312126, -3.805975901505573855 ) ) ;
#1618 = FACE_OUTER_BOUND ( 'NONE', #51809, .T. ) ;
#1619 = VERTEX_POINT ( 'NONE', #52623 ) ;
#1620 = CARTESIAN_POINT ( 'NONE',  ( -2.229367062500000163, -1.479166665301071770, -3.861377020970580443 ) ) ;
#1621 = ADVANCED_FACE ( 'NONE', ( #12750 ), #57773, .T. ) ;
#1622 = ADVANCED_FACE ( 'NONE', ( #51995 ), #17590, .T. ) ;
#1623 = CARTESIAN_POINT ( 'NONE',  ( 1.339745962155612702, -19.29465819873851729, -5.000000000000000000 ) ) ;
#1624 = CARTESIAN_POINT ( 'NONE',  ( -2.229367062499996610, -20.39583333196774007, 3.861377020970582219 ) ) ;
#1625 = CARTESIAN_POINT ( 'NONE',  ( -1.339745962155610925, 9.205341801261479162, 5.000000000000000000 ) ) ;
#1626 = CARTESIAN_POINT ( 'NONE',  ( 4.458734124999998549, -8.729166665301073991, -2.574251347313721627 ) ) ;
#1627 = CARTESIAN_POINT ( 'NONE',  ( 2.558993250143296372, -7.638875775590942219, -7.593821156097518177 ) ) ;
#1628 = CARTESIAN_POINT ( 'NONE',  ( 1.846868145590735200, -148.2500000013656347, -4.458734124999999437 ) ) ;
#1629 = CARTESIAN_POINT ( 'NONE',  ( 9.457646018065525792E-16, 17.68750000136559208, 5.148502694627439702 ) ) ;
#1630 = ORIENTED_EDGE ( 'NONE', *, *, #7870, .T. ) ;
#1631 = CARTESIAN_POINT ( 'NONE',  ( -3.535533905932738641, -148.3750000000000000, 3.535533905932737309 ) ) ;
#1632 = DIRECTION ( 'NONE',  ( -0.000000000000000000, 1.000000000000000000, -0.000000000000000000 ) ) ;
#1633 = CARTESIAN_POINT ( 'NONE',  ( 4.458734125000001214, -21.89583333196773296, 2.574251347313718519 ) ) ;
#1635 = EDGE_CURVE ( 'NONE', #41425, #23654, #2314, .T. ) ;
#1634 = CARTESIAN_POINT ( 'NONE',  ( 2.499999999999998668, -85.20833333060214443, -4.330127018922193649 ) ) ;
#1636 = CARTESIAN_POINT ( 'NONE',  ( -1.127183054612291972E-14, 25.24999999999999645, 4.999999999999999112 ) ) ;
#1637 = CARTESIAN_POINT ( 'NONE',  ( -58.39396692619412477, -149.4375000013656063, 2.891590998281057701 ) ) ;
#1638 = CARTESIAN_POINT ( 'NONE',  ( -4.999999999999999112, -48.79166666393547303, 2.886751345948131764 ) ) ;
#1639 = CARTESIAN_POINT ( 'NONE',  ( -1.339745962155585168, -2.080341798530294550, -5.000000000000015987 ) ) ;
#1640 = CARTESIAN_POINT ( 'NONE',  ( 2.229367062500001939, 9.020833334698927786, 3.861377020970579999 ) ) ;
#1641 = CARTESIAN_POINT ( 'NONE',  ( 0.000000000000000000, -120.0000000000000000, 5.000000000000000000 ) ) ;
#1642 = EDGE_CURVE ( 'NONE', #54415, #51386, #19932, .T. ) ;
#1643 = FACE_OUTER_BOUND ( 'NONE', #58770, .T. ) ;
#1644 = CARTESIAN_POINT ( 'NONE',  ( 4.458734125000000326, 12.10416666803226171, 2.574251347313718519 ) ) ;
#1645 = CARTESIAN_POINT ( 'NONE',  ( -2.229367062500000163, -69.47916666530107932, -3.861377020970580443 ) ) ;
#1646 = CARTESIAN_POINT ( 'NONE',  ( -4.458734124999999437, -11.64583333196774184, -2.574251347313719407 ) ) ;
#1647 = CARTESIAN_POINT ( 'NONE',  ( 5.000000000000000000, 0.5000000000000004441, -6.123233995736766282E-16 ) ) ;
#1648 = CARTESIAN_POINT ( 'NONE',  ( -3.152801135295367096, -165.0625000013656063, -3.152801135295367541 ) ) ;
#1649 = CARTESIAN_POINT ( 'NONE',  ( 1.255007937094098239E-14, 23.75000000000000000, -4.999999999999999112 ) ) ;
#1650 = CARTESIAN_POINT ( 'NONE',  ( -4.458734124999999437, -58.39583333196774362, -2.574251347313719407 ) ) ;
#1651 = CARTESIAN_POINT ( 'NONE',  ( 2.500000000000002220, -96.54166666393545881, 4.330127018922192761 ) ) ;
#1652 = CARTESIAN_POINT ( 'NONE',  ( -1.339745962155613812, -77.20534180126145429, -5.000000000000000000 ) ) ;
#1653 = CARTESIAN_POINT ( 'NONE',  ( -4.999999999999998224, -79.91666666666667140, 2.886751345948131764 ) ) ;
#1654 = CARTESIAN_POINT ( 'NONE',  ( 2.499999999999998668, -56.33333333333333570, -4.330127018922193649 ) ) ;
#1655 = CARTESIAN_POINT ( 'NONE',  ( 4.458734124999999437, -33.81249999863440792, -5.460374474430324690E-16 ) ) ;
#1656 = CARTESIAN_POINT ( 'NONE',  ( 1.339745962155612702, -51.16965819600732601, -5.000000000000000000 ) ) ;
#1657 = CARTESIAN_POINT ( 'NONE',  ( -5.000000000000000000, -41.08333333333333570, -2.886751345948128211 ) ) ;
#1658 = CARTESIAN_POINT ( 'NONE',  ( -4.999999999999998224, -13.91666666666666785, 2.886751345948131764 ) ) ;
#1659 = DIRECTION ( 'NONE',  ( 0.000000000000000000, 0.000000000000000000, 1.000000000000000000 ) ) ;
#1660 = VERTEX_POINT ( 'NONE', #26923 ) ;
#1661 = CARTESIAN_POINT ( 'NONE',  ( 4.458734125000001214, -107.8958333319677365, 2.574251347313718519 ) ) ;
#1662 = CARTESIAN_POINT ( 'NONE',  ( -2.229367062499996610, -1.395833331967737179, 3.861377020970582219 ) ) ;
#1663 = CARTESIAN_POINT ( 'NONE',  ( 5.000000000000000000, -59.41666666666665719, -2.886751345948130876 ) ) ;
#1664 = CARTESIAN_POINT ( 'NONE',  ( 2.499999999999998668, -9.333333333333332149, -4.330127018922193649 ) ) ;
#1665 = CARTESIAN_POINT ( 'NONE',  ( -2.229367062499996610, -73.14583333196773651, 3.861377020970582219 ) ) ;
#1666 = CARTESIAN_POINT ( 'NONE',  ( -50.01589407740564042, -147.7500000027312126, 0.3983568153799778022 ) ) ;
#1667 = CARTESIAN_POINT ( 'NONE',  ( 2.499999999999998668, -5.208333330602148870, -4.330127018922193649 ) ) ;
#1669 = ORIENTED_EDGE ( 'NONE', *, *, #62930, .T. ) ;
#1668 = CARTESIAN_POINT ( 'NONE',  ( -2.229367062499996610, -39.14583333196773651, 3.861377020970582219 ) ) ;
#1670 = CARTESIAN_POINT ( 'NONE',  ( 3.253724281355068545E-15, 27.87500000273118772, -5.000000000000000000 ) ) ;
#1672 = ORIENTED_EDGE ( 'NONE', *, *, #13075, .F. ) ;
#1671 = CARTESIAN_POINT ( 'NONE',  ( -4.458734124999999437, 11.35416666803225993, -2.574251347313719407 ) ) ;
#1673 = CARTESIAN_POINT ( 'NONE',  ( -2.500000000000000444, -56.04166666393548013, -4.330127018922193649 ) ) ;
#1674 = CARTESIAN_POINT ( 'NONE',  ( -5.000000000000000000, -50.00000000000000000, 0.000000000000000000 ) ) ;
#1675 = CARTESIAN_POINT ( 'NONE',  ( -4.458734124999999437, -29.64583333196773651, -2.574251347313719407 ) ) ;
#1676 = CARTESIAN_POINT ( 'NONE',  ( 3.061616997868383141E-16, -157.7500000000000000, -5.000000000000000000 ) ) ;
#1677 = CARTESIAN_POINT ( 'NONE',  ( 4.458734124999999437, -76.81249999863440792, -5.460374474430324690E-16 ) ) ;
#1678 = CARTESIAN_POINT ( 'NONE',  ( 3.535533905932736864, -169.1250000000000284, 3.535533905932738641 ) ) ;
#1679 = CARTESIAN_POINT ( 'NONE',  ( 9.457646018065525792E-16, -85.06249999863440792, 5.148502694627439702 ) ) ;
#1680 = CARTESIAN_POINT ( 'NONE',  ( -57.19623071787017210, -133.6250000013655779, 4.297418129356382899 ) ) ;
#1681 = VECTOR ( 'NONE', #20231, 1000.000000000000000 ) ;
#1682 = AXIS2_PLACEMENT_3D ( 'NONE', #16414, #13167, #22837 ) ;
#1683 = CARTESIAN_POINT ( 'NONE',  ( -4.458734124999999437, -37.64583333196773651, -2.574251347313719407 ) ) ;
#1684 =( BOUNDED_CURVE ( )  B_SPLINE_CURVE ( 2, ( #47397, #62205, #11707, #36481, #17177, #18121, #7537, #56747, #12671 ),
 .UNSPECIFIED., .F., .F. ) 
 B_SPLINE_CURVE_WITH_KNOTS ( ( 3, 2, 2, 2, 3 ),
 ( 0.8645833333333333703, 0.8652777777777778123, 0.8666666666666666963, 0.8680555555555555802, 0.8687500000000000222 ),
 .UNSPECIFIED. ) 
 CURVE ( )  GEOMETRIC_REPRESENTATION_ITEM ( )  RATIONAL_B_SPLINE_CURVE ( ( 0.9330127018922194093, 0.9330127018922194093, 1.000000000000000000, 0.8660254037844387076, 1.000000000000000000, 0.8660254037844387076, 1.000000000000000000, 0.9330127018922194093, 0.9330127018922194093 ) ) 
 REPRESENTATION_ITEM ( '' )  );
#1685 = CARTESIAN_POINT ( 'NONE',  ( -4.999999999999998224, -93.79166666393547303, 2.886751345948131764 ) ) ;
#1686 = ORIENTED_EDGE ( 'NONE', *, *, #60219, .F. ) ;
#1687 = CARTESIAN_POINT ( 'NONE',  ( 2.229367062500001939, -76.22916666530106511, 3.861377020970579999 ) ) ;
#1688 = CARTESIAN_POINT ( 'NONE',  ( -50.84841373685102184, -135.0000000000001137, -1.652645393539816210 ) ) ;
#1689 = ORIENTED_EDGE ( 'NONE', *, *, #14237, .T. ) ;
#1690 = CARTESIAN_POINT ( 'NONE',  ( 1.339745962155612702, -16.29465819873851729, -5.000000000000000000 ) ) ;
#1691 = LINE ( 'NONE', #11628, #28101 ) ;
#1692 = CARTESIAN_POINT ( 'NONE',  ( 4.458734124999998549, -64.97916666530106511, -2.574251347313721627 ) ) ;
#1693 = CARTESIAN_POINT ( 'NONE',  ( 4.458734124999999437, -3.062499998634407472, -5.460374474430324690E-16 ) ) ;
#1694 = ORIENTED_EDGE ( 'NONE', *, *, #16924, .F. ) ;
#1695 = CARTESIAN_POINT ( 'NONE',  ( -9.184850993605147944E-16, -156.3750000027311842, 5.000000000000000000 ) ) ;
#1696 = EDGE_CURVE ( 'NONE', #13658, #4410, #2677, .T. ) ;
#1697 = CARTESIAN_POINT ( 'NONE',  ( 5.000000000000000000, -62.50000000000000000, -6.123233995736766282E-16 ) ) ;
#1698 = VERTEX_POINT ( 'NONE', #56516 ) ;
#1699 = CYLINDRICAL_SURFACE ( 'NONE', #1770, 4.250000000000000000 ) ;
#1700 = CARTESIAN_POINT ( 'NONE',  ( -4.458734124999999437, 8.604166668032261711, -2.574251347313719407 ) ) ;
#1701 = DIRECTION ( 'NONE',  ( -0.000000000000000000, 1.000000000000000000, -0.000000000000000000 ) ) ;
#1702 = CARTESIAN_POINT ( 'NONE',  ( -3.152801135295367096, -160.0625000013656063, -3.152801135295367541 ) ) ;
#1703 = CARTESIAN_POINT ( 'NONE',  ( -6.972266317189433020E-16, 18.87500000273119127, -5.000000000000000000 ) ) ;
#1704 = ORIENTED_EDGE ( 'NONE', *, *, #34627, .F. ) ;
#1705 = CARTESIAN_POINT ( 'NONE',  ( -4.458734124999999437, -85.39583333196773651, -2.574251347313719407 ) ) ;
#1706 = CYLINDRICAL_SURFACE ( 'NONE', #25393, 5.000000000000000000 ) ;
#1707 = CARTESIAN_POINT ( 'NONE',  ( 2.229367062500001939, -2.979166665301069550, 3.861377020970579999 ) ) ;
#1708 = CARTESIAN_POINT ( 'NONE',  ( 6.042630808230842148E-15, 25.87500000273118062, -4.999999999999999112 ) ) ;
#1709 = CARTESIAN_POINT ( 'NONE',  ( -4.999999999999999112, -31.79166666393548724, 2.886751345948131764 ) ) ;
#1710 = CARTESIAN_POINT ( 'NONE',  ( 4.458734124999999437, 22.18750000136559564, -5.460374474430324690E-16 ) ) ;
#1711 = CARTESIAN_POINT ( 'NONE',  ( -1.339745962155613812, -38.08034179853029144, -5.000000000000000000 ) ) ;
#1712 = CARTESIAN_POINT ( 'NONE',  ( 4.458734124999999437, 26.18750000136559564, -5.460374474430324690E-16 ) ) ;
#1713 = ADVANCED_FACE ( 'NONE', ( #56833 ), #54171, .T. ) ;
#1714 = CARTESIAN_POINT ( 'NONE',  ( 4.458734124999998549, -51.72916666530107221, -2.574251347313721627 ) ) ;
#1715 = CARTESIAN_POINT ( 'NONE',  ( -4.458734124999997661, -37.47916666530107221, 2.574251347313722516 ) ) ;
#1716 = CARTESIAN_POINT ( 'NONE',  ( 4.458734124999998549, 1.020833334698927120, -2.574251347313721627 ) ) ;
#1717 = AXIS2_PLACEMENT_3D ( 'NONE', #19426, #24252, #13966 ) ;
#1718 = CARTESIAN_POINT ( 'NONE',  ( 6.123233995736766282E-16, -120.0000000000000000, -5.000000000000000000 ) ) ;
#1719 = CARTESIAN_POINT ( 'NONE',  ( 5.000000000000000000, 20.58333333333333570, -2.886751345948129988 ) ) ;
#1720 = EDGE_CURVE ( 'NONE', #13785, #44325, #15820, .T. ) ;
#1721 = CARTESIAN_POINT ( 'NONE',  ( -2.071067811865475061, -145.8125000027311842, -5.000000000000000888 ) ) ;
#1722 = CARTESIAN_POINT ( 'NONE',  ( 2.500000000000002220, -26.54166666393547658, 4.330127018922192761 ) ) ;
#1723 = CARTESIAN_POINT ( 'NONE',  ( -4.458734124999998549, -44.22916666530106511, 2.574251347313722516 ) ) ;
#1724 = CARTESIAN_POINT ( 'NONE',  ( -5.000000000000000000, -76.95833333060214443, -2.886751345948128211 ) ) ;
#1725 = VECTOR ( 'NONE', #54297, 1000.000000000000000 ) ;
#1726 = CARTESIAN_POINT ( 'NONE',  ( -50.40829686548195099, -141.2500000013656347, -1.485763867205728284 ) ) ;
#1727 = CARTESIAN_POINT ( 'NONE',  ( 0.000000000000000000, -170.0000000000000000, 0.000000000000000000 ) ) ;
#1728 = EDGE_CURVE ( 'NONE', #35208, #29222, #34787, .T. ) ;
#1729 = CARTESIAN_POINT ( 'NONE',  ( 7.894787914004607998, -0.7647108141804126458, -7.591390474663421095 ) ) ;
#1730 = CARTESIAN_POINT ( 'NONE',  ( 4.458734125000000326, -82.14583333196772230, 2.574251347313718519 ) ) ;
#1731 = CARTESIAN_POINT ( 'NONE',  ( 4.458734124999999437, -160.6875000013655779, 0.000000000000000000 ) ) ;
#1732 =( BOUNDED_CURVE ( )  B_SPLINE_CURVE ( 2, ( #30278, #59572, #25460, #54421, #10350, #15505, #30602, #35757, #49898 ),
 .UNSPECIFIED., .F., .F. ) 
 B_SPLINE_CURVE_WITH_KNOTS ( ( 3, 2, 2, 2, 3 ),
 ( 0.5895833333333333481, 0.5902777777777777901, 0.5916666666666666741, 0.5930555555555555580, 0.5937500000000000000 ),
 .UNSPECIFIED. ) 
 CURVE ( )  GEOMETRIC_REPRESENTATION_ITEM ( )  RATIONAL_B_SPLINE_CURVE ( ( 0.9330127018922194093, 0.9330127018922194093, 1.000000000000000000, 0.8660254037844387076, 1.000000000000000000, 0.8660254037844387076, 1.000000000000000000, 0.9330127018922194093, 0.9330127018922194093 ) ) 
 REPRESENTATION_ITEM ( '' )  );
#1733 = CARTESIAN_POINT ( 'NONE',  ( -5.335963852939856089, -6.035591050534137025, -7.593821156097342318 ) ) ;
#1734 = CARTESIAN_POINT ( 'NONE',  ( 1.060575238724906964E-15, -28.74999999999999645, 5.773502691896257311 ) ) ;
#1735 = CARTESIAN_POINT ( 'NONE',  ( 1.846868145590736310, -140.6250000013656063, 4.458734124999999437 ) ) ;
#1736 = EDGE_LOOP ( 'NONE', ( #48858, #39056, #46762, #36556 ) ) ;
#1737 = CARTESIAN_POINT ( 'NONE',  ( 9.457646018065525792E-16, 24.68750000136559208, 5.148502694627439702 ) ) ;
#1738 = VERTEX_POINT ( 'NONE', #43272 ) ;
#1739 = CARTESIAN_POINT ( 'NONE',  ( -2.229367062499996610, -90.14583333196773651, 3.861377020970582219 ) ) ;
#1740 = CARTESIAN_POINT ( 'NONE',  ( 2.229367062500001939, 14.77083333469892779, 3.861377020970579999 ) ) ;
#1741 =( BOUNDED_CURVE ( )  B_SPLINE_CURVE ( 2, ( #41175, #26079, #1654, #26718, #36681, #56315, #60187, #51171, #11275 ),
 .UNSPECIFIED., .F., .F. ) 
 B_SPLINE_CURVE_WITH_KNOTS ( ( 3, 2, 2, 2, 3 ),
 ( 0.6160714285714286031, 0.6166666666666666963, 0.6178571428571428825, 0.6190476190476190688, 0.6196428571428571619 ),
 .UNSPECIFIED. ) 
 CURVE ( )  GEOMETRIC_REPRESENTATION_ITEM ( )  RATIONAL_B_SPLINE_CURVE ( ( 0.9330127018922194093, 0.9330127018922194093, 1.000000000000000000, 0.8660254037844387076, 1.000000000000000000, 0.8660254037844387076, 1.000000000000000000, 0.9330127018922194093, 0.9330127018922194093 ) ) 
 REPRESENTATION_ITEM ( '' )  );
#1742 = CARTESIAN_POINT ( 'NONE',  ( -4.999999999999999112, 16.20833333606451987, 2.886751345948131764 ) ) ;
#1743 = CARTESIAN_POINT ( 'NONE',  ( -50.18089887299976937, -138.8125000027312126, 2.462841084822397164 ) ) ;
#1744 = CARTESIAN_POINT ( 'NONE',  ( 2.500000000000002220, 15.33333333333333215, 4.330127018922192761 ) ) ;
#1745 = CARTESIAN_POINT ( 'NONE',  ( -3.152548672688508926E-16, -56.56249999863439371, -5.148502694627439702 ) ) ;
#1746 = CARTESIAN_POINT ( 'NONE',  ( -4.458734124999999437, -10.39583333196773829, -2.574251347313719407 ) ) ;
#1747 = CARTESIAN_POINT ( 'NONE',  ( 7.499999999999999112, 4.652409454067514716, -7.929128589908465585 ) ) ;
#1748 = CARTESIAN_POINT ( 'NONE',  ( -59.44456063193725015, -136.8125000013656063, -0.3552334253322034230 ) ) ;
#1749 = CARTESIAN_POINT ( 'NONE',  ( -1.339745962155610925, -109.7946581987385315, 5.000000000000000000 ) ) ;
#1750 = CARTESIAN_POINT ( 'NONE',  ( -2.500000000000000444, -0.04166666393548221214, -4.330127018922193649 ) ) ;
#1751 = CARTESIAN_POINT ( 'NONE',  ( 1.975475456537005874E-15, -11.62499999726881406, 5.000000000000000000 ) ) ;
#1752 = CARTESIAN_POINT ( 'NONE',  ( 2.500000000000002220, -33.66666666666666430, 4.330127018922192761 ) ) ;
#1753 = CARTESIAN_POINT ( 'NONE',  ( 1.975475456537005874E-15, -74.75000000000000000, 5.000000000000000000 ) ) ;
#1755 = CARTESIAN_POINT ( 'NONE',  ( -2.229367062499996610, -16.39583333196773651, 3.861377020970582219 ) ) ;
#1754 = LINE ( 'NONE', #49662, #29496 ) ;
#1756 = CARTESIAN_POINT ( 'NONE',  ( -1.339745962155610925, -31.66965819600733312, 5.000000000000000000 ) ) ;
#1757 = CARTESIAN_POINT ( 'NONE',  ( -4.458734124999999437, -61.31249999863440081, 0.000000000000000000 ) ) ;
#1758 = CARTESIAN_POINT ( 'NONE',  ( -4.458734125000001214, -152.1250000013655779, 1.846868145590734089 ) ) ;
#1759 = CARTESIAN_POINT ( 'NONE',  ( 2.229367062500001939, -63.97916666530106511, 3.861377020970579999 ) ) ;
#1760 = CARTESIAN_POINT ( 'NONE',  ( -53.51423613279429503, -148.5000000013655779, 4.591703134518082763 ) ) ;
#1761 = CARTESIAN_POINT ( 'NONE',  ( 5.000000000000000888, -58.45833333060214443, 2.886751345948126879 ) ) ;
#1762 = VERTEX_POINT ( 'NONE', #48102 ) ;
#1763 = FACE_OUTER_BOUND ( 'NONE', #1385, .T. ) ;
#1764 = ORIENTED_EDGE ( 'NONE', *, *, #58262, .F. ) ;
#1765 =( BOUNDED_CURVE ( )  B_SPLINE_CURVE ( 2, ( #28669, #24484, #14503, #43771, #52507, #33197, #48286, #58889, #23856 ),
 .UNSPECIFIED., .F., .F. ) 
 B_SPLINE_CURVE_WITH_KNOTS ( ( 3, 2, 2, 2, 3 ),
 ( 0.3089285714285714413, 0.3095238095238095344, 0.3107142857142857206, 0.3119047619047619069, 0.3125000000000000000 ),
 .UNSPECIFIED. ) 
 CURVE ( )  GEOMETRIC_REPRESENTATION_ITEM ( )  RATIONAL_B_SPLINE_CURVE ( ( 0.9330127018922194093, 0.9330127018922194093, 1.000000000000000000, 0.8660254037844387076, 1.000000000000000000, 0.8660254037844387076, 1.000000000000000000, 0.9330127018922194093, 0.9330127018922194093 ) ) 
 REPRESENTATION_ITEM ( '' )  );
#1767 = CARTESIAN_POINT ( 'NONE',  ( 6.123233995736766282E-16, -120.0000000000000000, -5.000000000000000000 ) ) ;
#1766 = CARTESIAN_POINT ( 'NONE',  ( -1.339745962155610925, -27.79465819873851729, 5.000000000000000000 ) ) ;
#1768 = CARTESIAN_POINT ( 'NONE',  ( 2.730187237215162345E-16, -151.1875000013656063, -4.458734124999999437 ) ) ;
#1769 = VERTEX_POINT ( 'NONE', #4357 ) ;
#1770 = AXIS2_PLACEMENT_3D ( 'NONE', #29980, #60552, #44774 ) ;
#1771 = CARTESIAN_POINT ( 'NONE',  ( -4.999999999999998224, -9.916666666666662522, 2.886751345948131764 ) ) ;
#1772 = CARTESIAN_POINT ( 'NONE',  ( -59.81910112700025905, -131.1875000000000568, -2.462841084822630311 ) ) ;
#1773 = CARTESIAN_POINT ( 'NONE',  ( 2.229367062499998831, -46.89583333196774362, -3.861377020970580887 ) ) ;
#1774 = VECTOR ( 'NONE', #54158, 1000.000000000000000 ) ;
#1775 = VERTEX_POINT ( 'NONE', #23976 ) ;
#1776 = VECTOR ( 'NONE', #54934, 1000.000000000000000 ) ;
#1777 = CARTESIAN_POINT ( 'NONE',  ( -5.000000000000000888, -145.4375000000000000, 2.071067811865474617 ) ) ;
#1778 = AXIS2_PLACEMENT_3D ( 'NONE', #35397, #61762, #7412 ) ;
#1779 = CARTESIAN_POINT ( 'NONE',  ( -4.458734124999998549, 13.77083333469892779, 2.574251347313722516 ) ) ;
#1780 = CARTESIAN_POINT ( 'NONE',  ( 9.457646018065525792E-16, 24.93750000136559564, 5.148502694627439702 ) ) ;
#1781 = CARTESIAN_POINT ( 'NONE',  ( -50.55543936806279248, -153.0625000013656063, 0.3552334253322060320 ) ) ;
#1782 = CARTESIAN_POINT ( 'NONE',  ( -57.46284108482265651, -150.0625000027312126, 4.819101127000238627 ) ) ;
#1783 = CARTESIAN_POINT ( 'NONE',  ( -1.230605004983934782E-13, -25.75000000000000355, 5.000000000000000000 ) ) ;
#1784 =( BOUNDED_SURFACE ( )  B_SPLINE_SURFACE ( 1, 2, ( 
 ( #18999, #28654, #39246, #49226, #52797, #4527, #19635, #4227, #38932, #38612, #58248, #34108, #8733, #23841, #14174, #33800, #62771, #58873, #14803, #39563, #34417, #47958, #29595, #33489, #63399, #54046, #9983, #5167, #53418, #24785, #59204, #18691, #15132, #28341, #3913, #58567, #9351, #43131, #28963, #38317, #57945, #13865, #43444, #24152, #55013, #35392, #15775, #49544, #40843, #39883, #5484, #45996, #41159, #45039, #25745, #25420, #25099, #20923, #672, #10937, #60804, #16415, #55345, #35715, #50513, #45678, #26063, #36033, #11259, #54380, #6765, #30883, #55665, #6454, #11578, #1961, #1006, #34754, #20281, #30555, #1637, #21237, #50180, #6132, #60487, #31198, #44709, #50827, #1325, #40528, #26378, #45360, #35078, #54698, #21562, #10305, #29918, #59528, #60170, #20610, #30231, #15461, #16091, #10619, #49855, #5803, #40215, #59850, #11891, #21879, #61442, #22198, #12851, #31838, #32147, #7724, #27017, #46635, #2906, #55978, #17368, #51469, #16731, #36991, #32470, #37611, #42745, #36347, #42114, #41798, #22521, #27645, #52099, #12534, #51782, #2581, #27329, #46959, #61758, #17686, #52422, #8039, #31509, #37301, #17050, #56930, #56618, #47272, #3218, #22838, #42429, #51154, #62071, #26701, #2275, #36666, #7087, #41475, #27954, #17985, #57252, #13168, #8354, #46318, #32792, #47576, #3528, #23137, #61125, #56293, #12223, #7408, #14734, #53347, #43065, #43998, #24715, #53035, #43375, #62703, #33108, #18628, #18928, #19565, #8973, #62388, #9597, #19244, #52722, #29518, #38860, #58496, #9910, #9282, #14420, #38251, #57566, #63646, #34042, #53663, #63021, #8656, #48830, #18309, #28269, #28897, #24395, #29204, #24086, #13492, #4458, #4770, #13794, #14104, #48518, #28583, #48204, #43681, #37934, #38542, #33416, #47884, #58174, #39177, #58802, #3842, #23462, #63325, #23774, #34351, #53980, #49150, #33729, #5096, #4157, #57872, #15703, #35321, #50108, #16342, #35644, #59131, #30485, #44641, #6063, #20538, #25676, #5734, #25350, #934, #19882, #10868, #54298, #29843, #600, #283, #5414, #55590, #10549, #1251, #44970, #35964, #39495, #1562, #40135, #11509, #31125, #55270, #54942, #45285, #20852, #60417, #40456, #25031, #25988, #6692, #35009, #59777, #20210, #15066, #39812, #60096, #21164, #54624, #44319, #11188, #16017, #34679, #50748, #30811, #50441, #10238, #6382, #45605, #59454, #49476, #40771, #15385, #30159, #49788, #16654, #12772, #45921, #60732, #56540, #52019, #2823, #51708, #41086, #32071, #61364, #32394, #61679, #36279, #22442, #12460, #7649, #27562, #2504, #26622, #46241, #42039, #17612, #37228, #56854, #22122, #16974, #21807, #1884, #27252, #46879, #26297, #31433, #7963, #36585, #21488, #51073, #7336, #31761, #47195, #3138, #55903, #7014, #22757, #56220, #11814, #2203, #26947, #51394, #42355, #41402, #41714, #17286, #12140, #46564, #61994, #61053, #36909, #17914, #37535, #57175, #13092, #32712, #52340, #8274, #33653, #33338, #58093, #19158, #23999, #4077, #23700, #57795, #62933, #43297, #18847, #14024, #43915, #63245, #23064, #53271, #8579, #9206, #48126, #28819, #52955, #8893, #28508, #47497, #38467, #18231, #57490, #28191, #27878, #33030, #19483, #38173, #48440, #4380, #63563, #3450, #29122, #43601, #39096, #58725, #38777, #58416, #14343, #33964, #24309, #53585, #52646, #9515, #34270, #62629, #48745, #47806, #42669, #3763, #4687, #14651, #18551, #62308, #37857, #13409, #23387, #42986, #13715, #50027, #1484, #44887, #5985, #10153, #49065, #55186, #25590, #45203, #54543, #44238, #40375, #9821, #24631, #20450, #15939, #30404, #15625, #5011, #59694, #25266, #60016, #1170, #202, #20770, #40050, #35242, #11106, #30078, #54215, #29758, #35562, #30731, #50353, #6300, #49709, #44559, #49392, #29431, #10466, #25905, #19800, #45523, #5654, #21087, #40691, #60336, #848, #54861, #10792, #16264, #53896, #34583 ),
 ( #39408, #59047, #14975, #5336, #24953, #516, #20127, #39727, #59366, #15299, #34922, #36509, #26223, #22363, #55512, #6610, #2430, #61604, #12387, #61286, #50669, #41633, #7258, #41963, #7568, #45843, #32001, #22041, #17208, #37158, #12060, #36199, #55820, #51635, #27181, #46797, #2743, #31685, #26546, #31354, #11426, #36835, #56465, #35882, #41012, #17539, #46166, #31044, #60655, #16892, #41325, #56782, #50995, #51320, #26871, #2128, #21729, #12701, #1805, #56140, #6934, #21409, #46483, #32314, #51945, #61922, #16579, #7885, #60972, #27488, #47118, #3066, #22683, #42283, #11736, #8822, #52887, #28437, #23625, #53509, #9133, #32634, #4003, #18153, #43221, #57722, #37465, #32954, #62556, #52263, #23928, #22997, #8201, #29049, #24238, #28120, #48050, #8510, #27804, #9439, #28739, #62861, #18774, #38401, #33889, #58024, #62236, #63174, #43842, #47737, #18476, #37782, #47429, #57413, #38097, #38704, #3694, #17842, #48366, #13953, #3380, #48673, #33579, #53199, #4613, #4309, #43529, #13333, #13015, #19085, #58341, #14270, #13648, #42599, #57095, #52578, #23307, #42907, #33268, #39976, #25189, #14574, #5575, #34850, #5903, #35173, #9750, #59621, #30008, #49638, #1093, #39653, #132, #19726, #15553, #54789, #10719, #30326, #59290, #54136, #58968, #39026, #44805, #20375, #63488, #4937, #45129, #10075, #58654, #24560, #44482, #5260, #49950, #14896, #15221, #54471, #29687, #49317, #768, #34197, #441, #34504, #19412, #20048, #25510, #20702, #25833, #53821, #40306, #24881, #59944, #15867, #35488, #10398, #55107, #11029, #30653, #50276, #6221, #29357, #48990, #44164, #39335, #31609, #45769, #40931, #16814, #26788, #60579, #26471, #2046, #21013, #11981, #55432, #30971, #1726, #1413, #6536, #56704, #11660, #2356, #46086, #17462, #40620, #2664, #21652, #12622, #36434, #36122, #60264, #51244, #11349, #41244, #51866, #27104, #21964, #46407, #61210, #56388, #36759, #46719, #41559, #16182, #37084, #17136, #22285, #12315, #41884, #32235, #55744, #7809, #50596, #60891, #31927, #51555, #56064, #61530, #7491, #21331, #50914, #45449, #35807, #26150, #16500, #31280, #7180, #6857, #62478, #61849, #47664, #28354, #13880, #27411, #3616, #23855, #42205, #4240, #47356, #47974, #18076, #63103, #43458, #57650, #33508, #2991, #19015, #38628, #22927, #52181, #53435, #3928, #43146, #58270, #37385, #33815, #22609, #14190, #47042, #23223, #42836, #17768, #57338, #27729, #53124, #57019, #12934, #18398, #62786, #3305, #13578, #13254, #32878, #8749, #32558, #42519, #37697, #52506, #8126, #23546, #57959, #62156, #38330, #8440, #28044, #38019, #33196, #9058, #28668, #48285, #52811, #18705, #25999, #20219, #45617, #30822, #50453, #1260, #10879, #610, #15712, #11519, #1894, #36289, #30496, #21500, #28979, #25360, #54950, #24167, #16353, #15394, #43770, #41096, #16666, #20547, #6073, #1573, #10556, #40466, #40144, #35330, #55281, #48601, #5741, #59789, #50117, #39820, #6393, #40781, #60743, #21173, #4541, #50759, #54632, #20863, #60427, #35974, #55601, #25686, #31134, #6703, #59462, #26309, #45931, #9366, #60106, #45295, #35019, #16027, #30167, #49797, #44979, #35654, #945, #11200, #7345, #36921, #7024, #62004, #61064, #26633, #3461, #62319, #2515, #46890, #46574, #46253, #42048, #21816, #32081, #18244, #37545, #12782, #56864, #7974, #3149, #47206, #57185, #32404, #11824, #27888, #52031, #13104, #27572, #32722, #23074, #22131, #55912, #41413, #56550, #22769, #42365, #51718, #8284, #17923, #56231, #61374, #52350, #47510, #42678, #31443, #51086, #12471, #2213, #27264, #16984, #7659, #36596, #12152, #31771, #2833, #51403, #26956, #41725, #17295, #22451, #61691, #17622, #37239, #4391, #43928, #13418, #9833, #34283, #33351, #62641, #214, #14354, #53597, #29445, #47816, #44250, #33041, #53907, #49077, #33663, #53281, #5024, #4089, #38184, #24322 ) ),
 .UNSPECIFIED., .F., .F., .F. ) 
 B_SPLINE_SURFACE_WITH_KNOTS ( ( 2, 2 ),
 ( 3, 2, 2, 2, 2, 2, 2, 2, 2, 2, 2, 2, 2, 2, 2, 2, 2, 2, 2, 2, 2, 2, 2, 2, 2, 2, 2, 2, 2, 2, 2, 2, 2, 2, 2, 2, 2, 2, 2, 2, 2, 2, 2, 2, 2, 2, 2, 2, 2, 2, 2, 2, 2, 2, 2, 2, 2, 2, 2, 2, 2, 2, 2, 2, 2, 2, 2, 2, 2, 2, 2, 2, 2, 2, 2, 2, 2, 2, 2, 2, 2, 2, 2, 2, 2, 2, 2, 2, 2, 2, 2, 2, 2, 2, 2, 2, 2, 2, 2, 2, 2, 2, 2, 2, 2, 2, 2, 2, 2, 2, 2, 2, 2, 2, 2, 2, 2, 2, 2, 2, 2, 2, 2, 2, 2, 2, 2, 2, 2, 2, 2, 2, 2, 2, 2, 2, 2, 2, 2, 2, 2, 2, 2, 2, 2, 2, 2, 2, 2, 2, 2, 2, 2, 2, 2, 2, 2, 2, 2, 2, 2, 2, 2, 2, 2, 2, 2, 2, 2, 2, 2, 2, 2, 2, 2, 2, 2, 2, 2, 2, 2, 2, 2, 2, 2, 2, 2, 2, 2, 2, 2, 2, 2, 2, 2, 2, 2, 2, 2, 2, 2, 2, 2, 2, 2, 2, 2, 2, 2, 2, 2, 2, 2, 2, 2, 2, 2, 2, 2, 2, 2, 2, 2, 2, 2, 2, 2, 2, 2, 2, 2, 2, 2, 2, 2, 2, 2, 2, 2, 2, 3 ),
 ( 0.000000000000000000, 1.000000000000000000 ),
 ( 0.000000000000000000, 0.004166666666666666609, 0.008333333333333333218, 0.01250000000000000069, 0.01666666666666666644, 0.02083333333333333218, 0.02500000000000000139, 0.02916666666666666713, 0.03333333333333333287, 0.03749999999999999861, 0.04166666666666666435, 0.04583333333333333010, 0.05000000000000000278, 0.05416666666666666852, 0.05833333333333333426, 0.06250000000000000000, 0.06666666666666666574, 0.07083333333333333148, 0.07499999999999999722, 0.07916666666666666297, 0.08333333333333332871, 0.08749999999999999445, 0.09166666666666666019, 0.09583333333333333981, 0.1000000000000000056, 0.1041666666666666713, 0.1083333333333333370, 0.1125000000000000028, 0.1166666666666666685, 0.1208333333333333343, 0.1250000000000000000, 0.1291666666666666796, 0.1333333333333333315, 0.1375000000000000111, 0.1416666666666666630, 0.1458333333333333426, 0.1499999999999999944, 0.1541666666666666741, 0.1583333333333333259, 0.1625000000000000056, 0.1666666666666666574, 0.1708333333333333370, 0.1749999999999999889, 0.1791666666666666685, 0.1833333333333333204, 0.1875000000000000000, 0.1916666666666666796, 0.1958333333333333315, 0.2000000000000000111, 0.2041666666666666630, 0.2083333333333333426, 0.2124999999999999944, 0.2166666666666666741, 0.2208333333333333259, 0.2250000000000000056, 0.2291666666666666574, 0.2333333333333333370, 0.2374999999999999889, 0.2416666666666666685, 0.2458333333333333204, 0.2500000000000000000, 0.2541666666666666519, 0.2583333333333333592, 0.2625000000000000111, 0.2666666666666666630, 0.2708333333333333148, 0.2750000000000000222, 0.2791666666666666741, 0.2833333333333333259, 0.2874999999999999778, 0.2916666666666666852, 0.2958333333333333370, 0.2999999999999999889, 0.3041666666666666408, 0.3083333333333333481, 0.3125000000000000000, 0.3166666666666666519, 0.3208333333333333592, 0.3250000000000000111, 0.3291666666666666630, 0.3333333333333333148, 0.3375000000000000222, 0.3416666666666666741, 0.3458333333333333259, 0.3499999999999999778, 0.3541666666666666852, 0.3583333333333333370, 0.3624999999999999889, 0.3666666666666666408, 0.3708333333333333481, 0.3750000000000000000, 0.3791666666666666519, 0.3833333333333333592, 0.3875000000000000111, 0.3916666666666666630, 0.3958333333333333148, 0.4000000000000000222, 0.4041666666666666741, 0.4083333333333333259, 0.4124999999999999778, 0.4166666666666666852, 0.4208333333333333370, 0.4249999999999999889, 0.4291666666666666408, 0.4333333333333333481, 0.4375000000000000000, 0.4416666666666666519, 0.4458333333333333592, 0.4500000000000000111, 0.4541666666666666630, 0.4583333333333333148, 0.4625000000000000222, 0.4666666666666666741, 0.4708333333333333259, 0.4749999999999999778, 0.4791666666666666852, 0.4833333333333333370, 0.4874999999999999889, 0.4916666666666666408, 0.4958333333333333481, 0.5000000000000000000, 0.5041666666666666519, 0.5083333333333333037, 0.5124999999999999556, 0.5166666666666667185, 0.5208333333333333703, 0.5250000000000000222, 0.5291666666666666741, 0.5333333333333333259, 0.5374999999999999778, 0.5416666666666666297, 0.5458333333333332815, 0.5500000000000000444, 0.5541666666666666963, 0.5583333333333333481, 0.5625000000000000000, 0.5666666666666666519, 0.5708333333333333037, 0.5749999999999999556, 0.5791666666666667185, 0.5833333333333333703, 0.5875000000000000222, 0.5916666666666666741, 0.5958333333333333259, 0.5999999999999999778, 0.6041666666666666297, 0.6083333333333332815, 0.6125000000000000444, 0.6166666666666666963, 0.6208333333333333481, 0.6250000000000000000, 0.6291666666666666519, 0.6333333333333333037, 0.6374999999999999556, 0.6416666666666667185, 0.6458333333333333703, 0.6500000000000000222, 0.6541666666666666741, 0.6583333333333333259, 0.6624999999999999778, 0.6666666666666666297, 0.6708333333333332815, 0.6750000000000000444, 0.6791666666666666963, 0.6833333333333333481, 0.6875000000000000000, 0.6916666666666666519, 0.6958333333333333037, 0.6999999999999999556, 0.7041666666666667185, 0.7083333333333333703, 0.7125000000000000222, 0.7166666666666666741, 0.7208333333333333259, 0.7249999999999999778, 0.7291666666666666297, 0.7333333333333332815, 0.7375000000000000444, 0.7416666666666666963, 0.7458333333333333481, 0.7500000000000000000, 0.7541666666666666519, 0.7583333333333333037, 0.7624999999999999556, 0.7666666666666667185, 0.7708333333333333703, 0.7750000000000000222, 0.7791666666666666741, 0.7833333333333333259, 0.7874999999999999778, 0.7916666666666666297, 0.7958333333333332815, 0.8000000000000000444, 0.8041666666666666963, 0.8083333333333333481, 0.8125000000000000000, 0.8166666666666666519, 0.8208333333333333037, 0.8249999999999999556, 0.8291666666666667185, 0.8333333333333333703, 0.8375000000000000222, 0.8416666666666666741, 0.8458333333333333259, 0.8499999999999999778, 0.8541666666666666297, 0.8583333333333332815, 0.8625000000000000444, 0.8666666666666666963, 0.8708333333333333481, 0.8750000000000000000, 0.8791666666666666519, 0.8833333333333333037, 0.8874999999999999556, 0.8916666666666667185, 0.8958333333333333703, 0.9000000000000000222, 0.9041666666666666741, 0.9083333333333333259, 0.9124999999999999778, 0.9166666666666666297, 0.9208333333333332815, 0.9250000000000000444, 0.9291666666666666963, 0.9333333333333333481, 0.9375000000000000000, 0.9416666666666666519, 0.9458333333333333037, 0.9499999999999999556, 0.9541666666666667185, 0.9583333333333333703, 0.9625000000000000222, 0.9666666666666666741, 0.9708333333333333259, 0.9749999999999999778, 0.9791666666666666297, 0.9833333333333332815, 0.9875000000000000444, 0.9916666666666666963, 0.9958333333333333481, 1.000000000000000000 ),
 .UNSPECIFIED. ) 
 GEOMETRIC_REPRESENTATION_ITEM ( )  RATIONAL_B_SPLINE_SURFACE ( (
 ( 1.000000000000000000, 0.9238795325112867385, 1.000000000000000000, 0.9238795325112867385, 1.000000000000000000, 0.9238795325112867385, 1.000000000000000000, 0.9238795325112867385, 1.000000000000000000, 0.9238795325112867385, 1.000000000000000000, 0.9238795325112867385, 1.000000000000000000, 0.9238795325112867385, 1.000000000000000000, 0.9238795325112867385, 1.000000000000000000, 0.9238795325112867385, 1.000000000000000000, 0.9238795325112867385, 1.000000000000000000, 0.9238795325112867385, 1.000000000000000000, 0.9238795325112867385, 1.000000000000000000, 0.9238795325112867385, 1.000000000000000000, 0.9238795325112867385, 1.000000000000000000, 0.9238795325112867385, 1.000000000000000000, 0.9238795325112867385, 1.000000000000000000, 0.9238795325112867385, 1.000000000000000000, 0.9238795325112867385, 1.000000000000000000, 0.9238795325112867385, 1.000000000000000000, 0.9238795325112867385, 1.000000000000000000, 0.9238795325112867385, 1.000000000000000000, 0.9238795325112867385, 1.000000000000000000, 0.9238795325112867385, 1.000000000000000000, 0.9238795325112867385, 1.000000000000000000, 0.9238795325112867385, 1.000000000000000000, 0.9238795325112867385, 1.000000000000000000, 0.9238795325112867385, 1.000000000000000000, 0.9238795325112867385, 1.000000000000000000, 0.9238795325112867385, 1.000000000000000000, 0.9238795325112867385, 1.000000000000000000, 0.9238795325112867385, 1.000000000000000000, 0.9238795325112867385, 1.000000000000000000, 0.9238795325112867385, 1.000000000000000000, 0.9238795325112867385, 1.000000000000000000, 0.9238795325112867385, 1.000000000000000000, 0.9238795325112867385, 1.000000000000000000, 0.9238795325112867385, 1.000000000000000000, 0.9238795325112867385, 1.000000000000000000, 0.9238795325112867385, 1.000000000000000000, 0.9238795325112867385, 1.000000000000000000, 0.9238795325112867385, 1.000000000000000000, 0.9238795325112867385, 1.000000000000000000, 0.9238795325112867385, 1.000000000000000000, 0.9238795325112867385, 1.000000000000000000, 0.9238795325112867385, 1.000000000000000000, 0.9238795325112867385, 1.000000000000000000, 0.9238795325112867385, 1.000000000000000000, 0.9238795325112867385, 1.000000000000000000, 0.9238795325112867385, 1.000000000000000000, 0.9238795325112867385, 1.000000000000000000, 0.9238795325112867385, 1.000000000000000000, 0.9238795325112867385, 1.000000000000000000, 0.9238795325112867385, 1.000000000000000000, 0.9238795325112867385, 1.000000000000000000, 0.9238795325112867385, 1.000000000000000000, 0.9238795325112867385, 1.000000000000000000, 0.9238795325112867385, 1.000000000000000000, 0.9238795325112867385, 1.000000000000000000, 0.9238795325112867385, 1.000000000000000000, 0.9238795325112867385, 1.000000000000000000, 0.9238795325112867385, 1.000000000000000000, 0.9238795325112867385, 1.000000000000000000, 0.9238795325112867385, 1.000000000000000000, 0.9238795325112867385, 1.000000000000000000, 0.9238795325112867385, 1.000000000000000000, 0.9238795325112867385, 1.000000000000000000, 0.9238795325112867385, 1.000000000000000000, 0.9238795325112867385, 1.000000000000000000, 0.9238795325112867385, 1.000000000000000000, 0.9238795325112867385, 1.000000000000000000, 0.9238795325112867385, 1.000000000000000000, 0.9238795325112867385, 1.000000000000000000, 0.9238795325112867385, 1.000000000000000000, 0.9238795325112867385, 1.000000000000000000, 0.9238795325112867385, 1.000000000000000000, 0.9238795325112867385, 1.000000000000000000, 0.9238795325112867385, 1.000000000000000000, 0.9238795325112867385, 1.000000000000000000, 0.9238795325112867385, 1.000000000000000000, 0.9238795325112867385, 1.000000000000000000, 0.9238795325112867385, 1.000000000000000000, 0.9238795325112867385, 1.000000000000000000, 0.9238795325112867385, 1.000000000000000000, 0.9238795325112867385, 1.000000000000000000, 0.9238795325112867385, 1.000000000000000000, 0.9238795325112867385, 1.000000000000000000, 0.9238795325112867385, 1.000000000000000000, 0.9238795325112867385, 1.000000000000000000, 0.9238795325112867385, 1.000000000000000000, 0.9238795325112867385, 1.000000000000000000, 0.9238795325112867385, 1.000000000000000000, 0.9238795325112867385, 1.000000000000000000, 0.9238795325112867385, 1.000000000000000000, 0.9238795325112867385, 1.000000000000000000, 0.9238795325112867385, 1.000000000000000000, 0.9238795325112867385, 1.000000000000000000, 0.9238795325112867385, 1.000000000000000000, 0.9238795325112867385, 1.000000000000000000, 0.9238795325112867385, 1.000000000000000000, 0.9238795325112867385, 1.000000000000000000, 0.9238795325112867385, 1.000000000000000000, 0.9238795325112867385, 1.000000000000000000, 0.9238795325112867385, 1.000000000000000000, 0.9238795325112867385, 1.000000000000000000, 0.9238795325112867385, 1.000000000000000000, 0.9238795325112867385, 1.000000000000000000, 0.9238795325112867385, 1.000000000000000000, 0.9238795325112867385, 1.000000000000000000, 0.9238795325112867385, 1.000000000000000000, 0.9238795325112867385, 1.000000000000000000, 0.9238795325112867385, 1.000000000000000000, 0.9238795325112867385, 1.000000000000000000, 0.9238795325112867385, 1.000000000000000000, 0.9238795325112867385, 1.000000000000000000, 0.9238795325112867385, 1.000000000000000000, 0.9238795325112867385, 1.000000000000000000, 0.9238795325112867385, 1.000000000000000000, 0.9238795325112867385, 1.000000000000000000, 0.9238795325112867385, 1.000000000000000000, 0.9238795325112867385, 1.000000000000000000, 0.9238795325112867385, 1.000000000000000000, 0.9238795325112867385, 1.000000000000000000, 0.9238795325112867385, 1.000000000000000000, 0.9238795325112867385, 1.000000000000000000, 0.9238795325112867385, 1.000000000000000000, 0.9238795325112867385, 1.000000000000000000, 0.9238795325112867385, 1.000000000000000000, 0.9238795325112867385, 1.000000000000000000, 0.9238795325112867385, 1.000000000000000000, 0.9238795325112867385, 1.000000000000000000, 0.9238795325112867385, 1.000000000000000000, 0.9238795325112867385, 1.000000000000000000, 0.9238795325112867385, 1.000000000000000000, 0.9238795325112867385, 1.000000000000000000, 0.9238795325112867385, 1.000000000000000000, 0.9238795325112867385, 1.000000000000000000, 0.9238795325112867385, 1.000000000000000000, 0.9238795325112867385, 1.000000000000000000, 0.9238795325112867385, 1.000000000000000000, 0.9238795325112867385, 1.000000000000000000, 0.9238795325112867385, 1.000000000000000000, 0.9238795325112867385, 1.000000000000000000, 0.9238795325112867385, 1.000000000000000000, 0.9238795325112867385, 1.000000000000000000, 0.9238795325112867385, 1.000000000000000000, 0.9238795325112867385, 1.000000000000000000, 0.9238795325112867385, 1.000000000000000000, 0.9238795325112867385, 1.000000000000000000, 0.9238795325112867385, 1.000000000000000000, 0.9238795325112867385, 1.000000000000000000, 0.9238795325112867385, 1.000000000000000000, 0.9238795325112867385, 1.000000000000000000, 0.9238795325112867385, 1.000000000000000000, 0.9238795325112867385, 1.000000000000000000, 0.9238795325112867385, 1.000000000000000000, 0.9238795325112867385, 1.000000000000000000, 0.9238795325112867385, 1.000000000000000000, 0.9238795325112867385, 1.000000000000000000, 0.9238795325112867385, 1.000000000000000000, 0.9238795325112867385, 1.000000000000000000, 0.9238795325112867385, 1.000000000000000000, 0.9238795325112867385, 1.000000000000000000, 0.9238795325112867385, 1.000000000000000000, 0.9238795325112867385, 1.000000000000000000, 0.9238795325112867385, 1.000000000000000000, 0.9238795325112867385, 1.000000000000000000, 0.9238795325112867385, 1.000000000000000000, 0.9238795325112867385, 1.000000000000000000, 0.9238795325112867385, 1.000000000000000000, 0.9238795325112867385, 1.000000000000000000, 0.9238795325112867385, 1.000000000000000000, 0.9238795325112867385, 1.000000000000000000, 0.9238795325112867385, 1.000000000000000000, 0.9238795325112867385, 1.000000000000000000, 0.9238795325112867385, 1.000000000000000000, 0.9238795325112867385, 1.000000000000000000, 0.9238795325112867385, 1.000000000000000000, 0.9238795325112867385, 1.000000000000000000, 0.9238795325112867385, 1.000000000000000000, 0.9238795325112867385, 1.000000000000000000, 0.9238795325112867385, 1.000000000000000000, 0.9238795325112867385, 1.000000000000000000, 0.9238795325112867385, 1.000000000000000000, 0.9238795325112867385, 1.000000000000000000, 0.9238795325112867385, 1.000000000000000000, 0.9238795325112867385, 1.000000000000000000, 0.9238795325112867385, 1.000000000000000000, 0.9238795325112867385, 1.000000000000000000, 0.9238795325112867385, 1.000000000000000000, 0.9238795325112867385, 1.000000000000000000, 0.9238795325112867385, 1.000000000000000000, 0.9238795325112867385, 1.000000000000000000, 0.9238795325112867385, 1.000000000000000000, 0.9238795325112867385, 1.000000000000000000, 0.9238795325112867385, 1.000000000000000000, 0.9238795325112867385, 1.000000000000000000, 0.9238795325112867385, 1.000000000000000000, 0.9238795325112867385, 1.000000000000000000, 0.9238795325112867385, 1.000000000000000000, 0.9238795325112867385, 1.000000000000000000, 0.9238795325112867385, 1.000000000000000000, 0.9238795325112867385, 1.000000000000000000, 0.9238795325112867385, 1.000000000000000000, 0.9238795325112867385, 1.000000000000000000, 0.9238795325112867385, 1.000000000000000000, 0.9238795325112867385, 1.000000000000000000, 0.9238795325112867385, 1.000000000000000000, 0.9238795325112867385, 1.000000000000000000, 0.9238795325112867385, 1.000000000000000000, 0.9238795325112867385, 1.000000000000000000, 0.9238795325112867385, 1.000000000000000000, 0.9238795325112867385, 1.000000000000000000, 0.9238795325112867385, 1.000000000000000000, 0.9238795325112867385, 1.000000000000000000, 0.9238795325112867385, 1.000000000000000000, 0.9238795325112867385, 1.000000000000000000, 0.9238795325112867385, 1.000000000000000000, 0.9238795325112867385, 1.000000000000000000, 0.9238795325112867385, 1.000000000000000000, 0.9238795325112867385, 1.000000000000000000, 0.9238795325112867385, 1.000000000000000000, 0.9238795325112867385, 1.000000000000000000, 0.9238795325112867385, 1.000000000000000000, 0.9238795325112867385, 1.000000000000000000, 0.9238795325112867385, 1.000000000000000000, 0.9238795325112867385, 1.000000000000000000, 0.9238795325112867385, 1.000000000000000000, 0.9238795325112867385, 1.000000000000000000, 0.9238795325112867385, 1.000000000000000000, 0.9238795325112867385, 1.000000000000000000, 0.9238795325112867385, 1.000000000000000000, 0.9238795325112867385, 1.000000000000000000, 0.9238795325112867385, 1.000000000000000000, 0.9238795325112867385, 1.000000000000000000, 0.9238795325112867385, 1.000000000000000000, 0.9238795325112867385, 1.000000000000000000, 0.9238795325112867385, 1.000000000000000000, 0.9238795325112867385, 1.000000000000000000, 0.9238795325112867385, 1.000000000000000000, 0.9238795325112867385, 1.000000000000000000),
 ( 1.000000000000000000, 0.9238795325112867385, 1.000000000000000000, 0.9238795325112867385, 1.000000000000000000, 0.9238795325112867385, 1.000000000000000000, 0.9238795325112867385, 1.000000000000000000, 0.9238795325112867385, 1.000000000000000000, 0.9238795325112867385, 1.000000000000000000, 0.9238795325112867385, 1.000000000000000000, 0.9238795325112867385, 1.000000000000000000, 0.9238795325112867385, 1.000000000000000000, 0.9238795325112867385, 1.000000000000000000, 0.9238795325112867385, 1.000000000000000000, 0.9238795325112867385, 1.000000000000000000, 0.9238795325112867385, 1.000000000000000000, 0.9238795325112867385, 1.000000000000000000, 0.9238795325112867385, 1.000000000000000000, 0.9238795325112867385, 1.000000000000000000, 0.9238795325112867385, 1.000000000000000000, 0.9238795325112867385, 1.000000000000000000, 0.9238795325112867385, 1.000000000000000000, 0.9238795325112867385, 1.000000000000000000, 0.9238795325112867385, 1.000000000000000000, 0.9238795325112867385, 1.000000000000000000, 0.9238795325112867385, 1.000000000000000000, 0.9238795325112867385, 1.000000000000000000, 0.9238795325112867385, 1.000000000000000000, 0.9238795325112867385, 1.000000000000000000, 0.9238795325112867385, 1.000000000000000000, 0.9238795325112867385, 1.000000000000000000, 0.9238795325112867385, 1.000000000000000000, 0.9238795325112867385, 1.000000000000000000, 0.9238795325112867385, 1.000000000000000000, 0.9238795325112867385, 1.000000000000000000, 0.9238795325112867385, 1.000000000000000000, 0.9238795325112867385, 1.000000000000000000, 0.9238795325112867385, 1.000000000000000000, 0.9238795325112867385, 1.000000000000000000, 0.9238795325112867385, 1.000000000000000000, 0.9238795325112867385, 1.000000000000000000, 0.9238795325112867385, 1.000000000000000000, 0.9238795325112867385, 1.000000000000000000, 0.9238795325112867385, 1.000000000000000000, 0.9238795325112867385, 1.000000000000000000, 0.9238795325112867385, 1.000000000000000000, 0.9238795325112867385, 1.000000000000000000, 0.9238795325112867385, 1.000000000000000000, 0.9238795325112867385, 1.000000000000000000, 0.9238795325112867385, 1.000000000000000000, 0.9238795325112867385, 1.000000000000000000, 0.9238795325112867385, 1.000000000000000000, 0.9238795325112867385, 1.000000000000000000, 0.9238795325112867385, 1.000000000000000000, 0.9238795325112867385, 1.000000000000000000, 0.9238795325112867385, 1.000000000000000000, 0.9238795325112867385, 1.000000000000000000, 0.9238795325112867385, 1.000000000000000000, 0.9238795325112867385, 1.000000000000000000, 0.9238795325112867385, 1.000000000000000000, 0.9238795325112867385, 1.000000000000000000, 0.9238795325112867385, 1.000000000000000000, 0.9238795325112867385, 1.000000000000000000, 0.9238795325112867385, 1.000000000000000000, 0.9238795325112867385, 1.000000000000000000, 0.9238795325112867385, 1.000000000000000000, 0.9238795325112867385, 1.000000000000000000, 0.9238795325112867385, 1.000000000000000000, 0.9238795325112867385, 1.000000000000000000, 0.9238795325112867385, 1.000000000000000000, 0.9238795325112867385, 1.000000000000000000, 0.9238795325112867385, 1.000000000000000000, 0.9238795325112867385, 1.000000000000000000, 0.9238795325112867385, 1.000000000000000000, 0.9238795325112867385, 1.000000000000000000, 0.9238795325112867385, 1.000000000000000000, 0.9238795325112867385, 1.000000000000000000, 0.9238795325112867385, 1.000000000000000000, 0.9238795325112867385, 1.000000000000000000, 0.9238795325112867385, 1.000000000000000000, 0.9238795325112867385, 1.000000000000000000, 0.9238795325112867385, 1.000000000000000000, 0.9238795325112867385, 1.000000000000000000, 0.9238795325112867385, 1.000000000000000000, 0.9238795325112867385, 1.000000000000000000, 0.9238795325112867385, 1.000000000000000000, 0.9238795325112867385, 1.000000000000000000, 0.9238795325112867385, 1.000000000000000000, 0.9238795325112867385, 1.000000000000000000, 0.9238795325112867385, 1.000000000000000000, 0.9238795325112867385, 1.000000000000000000, 0.9238795325112867385, 1.000000000000000000, 0.9238795325112867385, 1.000000000000000000, 0.9238795325112867385, 1.000000000000000000, 0.9238795325112867385, 1.000000000000000000, 0.9238795325112867385, 1.000000000000000000, 0.9238795325112867385, 1.000000000000000000, 0.9238795325112867385, 1.000000000000000000, 0.9238795325112867385, 1.000000000000000000, 0.9238795325112867385, 1.000000000000000000, 0.9238795325112867385, 1.000000000000000000, 0.9238795325112867385, 1.000000000000000000, 0.9238795325112867385, 1.000000000000000000, 0.9238795325112867385, 1.000000000000000000, 0.9238795325112867385, 1.000000000000000000, 0.9238795325112867385, 1.000000000000000000, 0.9238795325112867385, 1.000000000000000000, 0.9238795325112867385, 1.000000000000000000, 0.9238795325112867385, 1.000000000000000000, 0.9238795325112867385, 1.000000000000000000, 0.9238795325112867385, 1.000000000000000000, 0.9238795325112867385, 1.000000000000000000, 0.9238795325112867385, 1.000000000000000000, 0.9238795325112867385, 1.000000000000000000, 0.9238795325112867385, 1.000000000000000000, 0.9238795325112867385, 1.000000000000000000, 0.9238795325112867385, 1.000000000000000000, 0.9238795325112867385, 1.000000000000000000, 0.9238795325112867385, 1.000000000000000000, 0.9238795325112867385, 1.000000000000000000, 0.9238795325112867385, 1.000000000000000000, 0.9238795325112867385, 1.000000000000000000, 0.9238795325112867385, 1.000000000000000000, 0.9238795325112867385, 1.000000000000000000, 0.9238795325112867385, 1.000000000000000000, 0.9238795325112867385, 1.000000000000000000, 0.9238795325112867385, 1.000000000000000000, 0.9238795325112867385, 1.000000000000000000, 0.9238795325112867385, 1.000000000000000000, 0.9238795325112867385, 1.000000000000000000, 0.9238795325112867385, 1.000000000000000000, 0.9238795325112867385, 1.000000000000000000, 0.9238795325112867385, 1.000000000000000000, 0.9238795325112867385, 1.000000000000000000, 0.9238795325112867385, 1.000000000000000000, 0.9238795325112867385, 1.000000000000000000, 0.9238795325112867385, 1.000000000000000000, 0.9238795325112867385, 1.000000000000000000, 0.9238795325112867385, 1.000000000000000000, 0.9238795325112867385, 1.000000000000000000, 0.9238795325112867385, 1.000000000000000000, 0.9238795325112867385, 1.000000000000000000, 0.9238795325112867385, 1.000000000000000000, 0.9238795325112867385, 1.000000000000000000, 0.9238795325112867385, 1.000000000000000000, 0.9238795325112867385, 1.000000000000000000, 0.9238795325112867385, 1.000000000000000000, 0.9238795325112867385, 1.000000000000000000, 0.9238795325112867385, 1.000000000000000000, 0.9238795325112867385, 1.000000000000000000, 0.9238795325112867385, 1.000000000000000000, 0.9238795325112867385, 1.000000000000000000, 0.9238795325112867385, 1.000000000000000000, 0.9238795325112867385, 1.000000000000000000, 0.9238795325112867385, 1.000000000000000000, 0.9238795325112867385, 1.000000000000000000, 0.9238795325112867385, 1.000000000000000000, 0.9238795325112867385, 1.000000000000000000, 0.9238795325112867385, 1.000000000000000000, 0.9238795325112867385, 1.000000000000000000, 0.9238795325112867385, 1.000000000000000000, 0.9238795325112867385, 1.000000000000000000, 0.9238795325112867385, 1.000000000000000000, 0.9238795325112867385, 1.000000000000000000, 0.9238795325112867385, 1.000000000000000000, 0.9238795325112867385, 1.000000000000000000, 0.9238795325112867385, 1.000000000000000000, 0.9238795325112867385, 1.000000000000000000, 0.9238795325112867385, 1.000000000000000000, 0.9238795325112867385, 1.000000000000000000, 0.9238795325112867385, 1.000000000000000000, 0.9238795325112867385, 1.000000000000000000, 0.9238795325112867385, 1.000000000000000000, 0.9238795325112867385, 1.000000000000000000, 0.9238795325112867385, 1.000000000000000000, 0.9238795325112867385, 1.000000000000000000, 0.9238795325112867385, 1.000000000000000000, 0.9238795325112867385, 1.000000000000000000, 0.9238795325112867385, 1.000000000000000000, 0.9238795325112867385, 1.000000000000000000, 0.9238795325112867385, 1.000000000000000000, 0.9238795325112867385, 1.000000000000000000, 0.9238795325112867385, 1.000000000000000000, 0.9238795325112867385, 1.000000000000000000, 0.9238795325112867385, 1.000000000000000000, 0.9238795325112867385, 1.000000000000000000, 0.9238795325112867385, 1.000000000000000000, 0.9238795325112867385, 1.000000000000000000, 0.9238795325112867385, 1.000000000000000000, 0.9238795325112867385, 1.000000000000000000, 0.9238795325112867385, 1.000000000000000000, 0.9238795325112867385, 1.000000000000000000, 0.9238795325112867385, 1.000000000000000000, 0.9238795325112867385, 1.000000000000000000, 0.9238795325112867385, 1.000000000000000000, 0.9238795325112867385, 1.000000000000000000, 0.9238795325112867385, 1.000000000000000000, 0.9238795325112867385, 1.000000000000000000, 0.9238795325112867385, 1.000000000000000000, 0.9238795325112867385, 1.000000000000000000, 0.9238795325112867385, 1.000000000000000000, 0.9238795325112867385, 1.000000000000000000, 0.9238795325112867385, 1.000000000000000000, 0.9238795325112867385, 1.000000000000000000, 0.9238795325112867385, 1.000000000000000000, 0.9238795325112867385, 1.000000000000000000, 0.9238795325112867385, 1.000000000000000000, 0.9238795325112867385, 1.000000000000000000, 0.9238795325112867385, 1.000000000000000000, 0.9238795325112867385, 1.000000000000000000, 0.9238795325112867385, 1.000000000000000000, 0.9238795325112867385, 1.000000000000000000, 0.9238795325112867385, 1.000000000000000000, 0.9238795325112867385, 1.000000000000000000, 0.9238795325112867385, 1.000000000000000000, 0.9238795325112867385, 1.000000000000000000, 0.9238795325112867385, 1.000000000000000000, 0.9238795325112867385, 1.000000000000000000, 0.9238795325112867385, 1.000000000000000000, 0.9238795325112867385, 1.000000000000000000, 0.9238795325112867385, 1.000000000000000000, 0.9238795325112867385, 1.000000000000000000, 0.9238795325112867385, 1.000000000000000000, 0.9238795325112867385, 1.000000000000000000, 0.9238795325112867385, 1.000000000000000000, 0.9238795325112867385, 1.000000000000000000, 0.9238795325112867385, 1.000000000000000000, 0.9238795325112867385, 1.000000000000000000, 0.9238795325112867385, 1.000000000000000000, 0.9238795325112867385, 1.000000000000000000, 0.9238795325112867385, 1.000000000000000000, 0.9238795325112867385, 1.000000000000000000, 0.9238795325112867385, 1.000000000000000000, 0.9238795325112867385, 1.000000000000000000, 0.9238795325112867385, 1.000000000000000000, 0.9238795325112867385, 1.000000000000000000, 0.9238795325112867385, 1.000000000000000000, 0.9238795325112867385, 1.000000000000000000, 0.9238795325112867385, 1.000000000000000000, 0.9238795325112867385, 1.000000000000000000, 0.9238795325112867385, 1.000000000000000000, 0.9238795325112867385, 1.000000000000000000, 0.9238795325112867385, 1.000000000000000000) ) ) 
 REPRESENTATION_ITEM ( '' )  SURFACE ( )  );
#1785 = ORIENTED_EDGE ( 'NONE', *, *, #19975, .F. ) ;
#1786 = CARTESIAN_POINT ( 'NONE',  ( -4.458734124999999437, -67.31249999863440792, 0.000000000000000000 ) ) ;
#1787 = CARTESIAN_POINT ( 'NONE',  ( 1.975475456537005874E-15, -28.62499999726881583, 5.000000000000000000 ) ) ;
#1788 = CARTESIAN_POINT ( 'NONE',  ( 4.458734125000001214, 15.10416666803225993, 2.574251347313718519 ) ) ;
#1789 = CARTESIAN_POINT ( 'NONE',  ( 5.000000000000000000, -63.50000000000000000, -6.123233995736766282E-16 ) ) ;
#1790 = CARTESIAN_POINT ( 'NONE',  ( -1.339745962155613812, -2.080341798530293662, -5.000000000000000000 ) ) ;
#1791 = CARTESIAN_POINT ( 'NONE',  ( 2.229367062499998831, -54.89583333196773651, -3.861377020970580887 ) ) ;
#1792 = CARTESIAN_POINT ( 'NONE',  ( -4.999999999999999112, -13.79166666393548191, 2.886751345948131764 ) ) ;
#1793 = CARTESIAN_POINT ( 'NONE',  ( -6.972266317189433020E-16, -77.25000000000000000, -5.000000000000000000 ) ) ;
#1794 = CARTESIAN_POINT ( 'NONE',  ( 7.500000000000001776, 0.000000000000000000, 0.000000000000000000 ) ) ;
#1795 = LINE ( 'NONE', #34911, #26498 ) ;
#1796 = CARTESIAN_POINT ( 'NONE',  ( -4.458734124999999437, -17.64583333196773651, -2.574251347313719407 ) ) ;
#1797 = ORIENTED_EDGE ( 'NONE', *, *, #35457, .F. ) ;
#1798 = DIRECTION ( 'NONE',  ( 0.000000000000000000, 0.000000000000000000, 1.000000000000000000 ) ) ;
#1799 = CARTESIAN_POINT ( 'NONE',  ( -4.458734124999999437, -101.3958333319677365, -2.574251347313719407 ) ) ;
#1800 = CARTESIAN_POINT ( 'NONE',  ( -2.071067811865478170, -159.4375000027312694, 5.000000000000000000 ) ) ;
#1801 = ORIENTED_EDGE ( 'NONE', *, *, #51159, .T. ) ;
#1802 = CARTESIAN_POINT ( 'NONE',  ( -4.458734124999999437, -104.6458333319677365, -2.574251347313719407 ) ) ;
#1803 = CARTESIAN_POINT ( 'NONE',  ( -2.229367062499996610, -29.14583333196774007, 3.861377020970582219 ) ) ;
#1804 = CARTESIAN_POINT ( 'NONE',  ( 5.000000000000000888, -61.45833333060214443, 2.886751345948126879 ) ) ;
#1805 = CARTESIAN_POINT ( 'NONE',  ( -54.64476657466781973, -151.0625000013656063, -4.444560631937228834 ) ) ;
#1806 = CARTESIAN_POINT ( 'NONE',  ( -50.70258187064364108, -142.1250000013656063, 2.196230717870141014 ) ) ;
#1807 = CARTESIAN_POINT ( 'NONE',  ( 4.458734125000000326, -21.89583333196773296, 2.574251347313718519 ) ) ;
#1808 = CARTESIAN_POINT ( 'NONE',  ( -4.458734124999999437, -65.64583333196773651, -2.574251347313719407 ) ) ;
#1809 = CYLINDRICAL_SURFACE ( 'NONE', #53128, 5.000000000000000000 ) ;
#1810 = CARTESIAN_POINT ( 'NONE',  ( 9.457646018065525792E-16, -19.06249999863440792, 5.148502694627439702 ) ) ;
#1811 = CARTESIAN_POINT ( 'NONE',  ( 0.000000000000000000, -170.0000000000000000, 0.000000000000000000 ) ) ;
#1812 = CARTESIAN_POINT ( 'NONE',  ( 2.071067811865476394, -149.1875000000000000, 5.000000000000000000 ) ) ;
#1813 = CARTESIAN_POINT ( 'NONE',  ( -2.500000000000000444, -10.16666666666666430, -4.330127018922193649 ) ) ;
#1814 = CARTESIAN_POINT ( 'NONE',  ( 1.846868145590736310, -153.6250000013655779, 4.458734124999999437 ) ) ;
#1815 = ORIENTED_EDGE ( 'NONE', *, *, #30216, .T. ) ;
#1816 = CARTESIAN_POINT ( 'NONE',  ( 4.458734124999999437, -51.06249999863440792, -5.460374474430324690E-16 ) ) ;
#1817 = CARTESIAN_POINT ( 'NONE',  ( 1.975475456537005874E-15, -84.62499999726880162, 5.000000000000000000 ) ) ;
#1818 = CARTESIAN_POINT ( 'NONE',  ( -58.24261429053147765, -136.2500000000000284, -3.805975901505573855 ) ) ;
#1819 = CARTESIAN_POINT ( 'NONE',  ( -4.458734124999999437, -89.31249999863440792, 0.000000000000000000 ) ) ;
#1820 = AXIS2_PLACEMENT_3D ( 'NONE', #30255, #49878, #35415 ) ;
#1821 = AXIS2_PLACEMENT_3D ( 'NONE', #44111, #19357, #38655 ) ;
#1822 = CARTESIAN_POINT ( 'NONE',  ( -4.458734124999999437, 2.604166668032263043, -2.574251347313719407 ) ) ;
#1823 = CARTESIAN_POINT ( 'NONE',  ( -4.729367062499999719, -90.15624999931721106, 0.000000000000000000 ) ) ;
#1824 = AXIS2_PLACEMENT_3D ( 'NONE', #23045, #61972, #17893 ) ;
#1825 = CARTESIAN_POINT ( 'NONE',  ( 5.000000000000000888, -95.45833333060213022, 2.886751345948126879 ) ) ;
#1826 = FACE_OUTER_BOUND ( 'NONE', #36269, .T. ) ;
#1827 = CARTESIAN_POINT ( 'NONE',  ( 4.458734124999999437, 12.93750000136559208, -5.460374474430324690E-16 ) ) ;
#1828 = CARTESIAN_POINT ( 'NONE',  ( 2.499999999999998668, 3.791666669397852019, -4.330127018922193649 ) ) ;
#1829 = ORIENTED_EDGE ( 'NONE', *, *, #16228, .T. ) ;
#1830 = DIRECTION ( 'NONE',  ( -0.000000000000000000, 1.000000000000000000, -0.000000000000000000 ) ) ;
#1831 = ORIENTED_EDGE ( 'NONE', *, *, #12665, .F. ) ;
#1832 = CARTESIAN_POINT ( 'NONE',  ( 1.339745962155616255, 26.70534180126147561, -4.999999999999997335 ) ) ;
#1833 = CARTESIAN_POINT ( 'NONE',  ( 4.458734124999999437, -43.81249999863440081, -5.460374474430324690E-16 ) ) ;
#1834 = CARTESIAN_POINT ( 'NONE',  ( 1.846868145590736310, -164.8750000013655779, 4.458734124999999437 ) ) ;
#1835 = CARTESIAN_POINT ( 'NONE',  ( 5.000000000000000000, -39.29166666393548724, -2.886751345948129988 ) ) ;
#1836 = EDGE_LOOP ( 'NONE', ( #48086, #31159, #39054, #10785 ) ) ;
#1837 = CARTESIAN_POINT ( 'NONE',  ( -2.229367062499996610, -16.14583333196773651, 3.861377020970582219 ) ) ;
#1838 = ORIENTED_EDGE ( 'NONE', *, *, #53172, .T. ) ;
#1839 = CARTESIAN_POINT ( 'NONE',  ( -6.972266317189433020E-16, -109.1249999972688016, -5.000000000000000000 ) ) ;
#1840 = CARTESIAN_POINT ( 'NONE',  ( -3.152801135295367985, -162.8125000013656063, 3.152801135295367096 ) ) ;
#1841 = CARTESIAN_POINT ( 'NONE',  ( -5.000000000000000000, -85.87499999726880162, 0.000000000000000000 ) ) ;
#1843 = VERTEX_POINT ( 'NONE', #9800 ) ;
#1842 = CARTESIAN_POINT ( 'NONE',  ( -6.972266317189433020E-16, -62.12499999726880162, -5.000000000000000000 ) ) ;
#1844 = CARTESIAN_POINT ( 'NONE',  ( -54.60164318462004474, -142.3750000000000284, -4.984105922594373794 ) ) ;
#1845 = CARTESIAN_POINT ( 'NONE',  ( 4.458734124999999437, -32.06249999863440792, -5.460374474430324690E-16 ) ) ;
#1846 = CARTESIAN_POINT ( 'NONE',  ( 3.061616997868383141E-16, -147.8750000027312126, -5.000000000000000000 ) ) ;
#1847 = ORIENTED_EDGE ( 'NONE', *, *, #37550, .T. ) ;
#1848 = CARTESIAN_POINT ( 'NONE',  ( -4.458734124999999437, -77.31249999863440792, 0.000000000000000000 ) ) ;
#1849 = CARTESIAN_POINT ( 'NONE',  ( 2.229367062499998831, 29.35416666803225993, -3.861377020970580887 ) ) ;
#1850 = CARTESIAN_POINT ( 'NONE',  ( -2.499999999999996447, -53.83333333333332860, 4.330127018922195425 ) ) ;
#1851 = ORIENTED_EDGE ( 'NONE', *, *, #12605, .F. ) ;
#1852 = CARTESIAN_POINT ( 'NONE',  ( -5.000000000000000888, -166.5625000027312126, 2.071067811865474617 ) ) ;
#1853 = CARTESIAN_POINT ( 'NONE',  ( -55.35523342533222291, -141.5625000013656063, 4.444560631937231499 ) ) ;
#1854 = CARTESIAN_POINT ( 'NONE',  ( 2.229367062500001939, -81.22916666530106511, 3.861377020970579999 ) ) ;
#1855 = CARTESIAN_POINT ( 'NONE',  ( -60.14911071818854538, -135.1875000027312410, 1.666127454062681368 ) ) ;
#1856 = CARTESIAN_POINT ( 'NONE',  ( 2.229367062500001939, -44.97916666530106511, 3.861377020970579999 ) ) ;
#1857 = CARTESIAN_POINT ( 'NONE',  ( -4.458734125000000326, -141.1250000013656063, 1.846868145590734089 ) ) ;
#1858 = DIRECTION ( 'NONE',  ( -0.000000000000000000, 1.000000000000000000, -0.000000000000000000 ) ) ;
#1859 = CARTESIAN_POINT ( 'NONE',  ( 4.458734125000000326, -48.89583333196772941, 2.574251347313718519 ) ) ;
#1860 = CARTESIAN_POINT ( 'NONE',  ( -4.458734124999999437, -43.31249999863440081, 0.000000000000000000 ) ) ;
#1861 = CARTESIAN_POINT ( 'NONE',  ( -4.458734124999999437, 26.60416666803225993, -2.574251347313719407 ) ) ;
#1862 = AXIS2_PLACEMENT_3D ( 'NONE', #35867, #40358, #56122 ) ;
#1863 =( BOUNDED_CURVE ( )  B_SPLINE_CURVE ( 2, ( #28925, #43403, #33446, #9938, #18656, #38574, #49187, #5125, #34710 ),
 .UNSPECIFIED., .F., .F. ) 
 B_SPLINE_CURVE_WITH_KNOTS ( ( 3, 2, 2, 2, 3 ),
 ( 0.3687500000000000222, 0.3694444444444444642, 0.3708333333333333481, 0.3722222222222222321, 0.3729166666666666741 ),
 .UNSPECIFIED. ) 
 CURVE ( )  GEOMETRIC_REPRESENTATION_ITEM ( )  RATIONAL_B_SPLINE_CURVE ( ( 0.9330127018922194093, 0.9330127018922194093, 1.000000000000000000, 0.8660254037844387076, 1.000000000000000000, 0.8660254037844387076, 1.000000000000000000, 0.9330127018922194093, 0.9330127018922194093 ) ) 
 REPRESENTATION_ITEM ( '' )  );
#1864 = CARTESIAN_POINT ( 'NONE',  ( -5.000000000000000000, -107.9999999999999858, 0.000000000000000000 ) ) ;
#1865 = DIRECTION ( 'NONE',  ( 0.000000000000000000, 0.000000000000000000, 1.000000000000000000 ) ) ;
#1866 = CARTESIAN_POINT ( 'NONE',  ( -4.458734124999999437, -39.64583333196774362, -2.574251347313719407 ) ) ;
#1867 = CARTESIAN_POINT ( 'NONE',  ( 2.500000000000002220, 2.458333336064519870, 4.330127018922192761 ) ) ;
#1868 = CARTESIAN_POINT ( 'NONE',  ( 75.00000000000002842, 15.00000000000000000, -5.000000000000000000 ) ) ;
#1869 = CARTESIAN_POINT ( 'NONE',  ( -50.55543936806279248, -127.0625000013655921, 0.3552334253322060320 ) ) ;
#1870 = CARTESIAN_POINT ( 'NONE',  ( 4.458734124999998549, -76.97916666530106511, -2.574251347313721627 ) ) ;
#1871 = CARTESIAN_POINT ( 'NONE',  ( 1.975475456537005874E-15, -34.75000000000000000, 5.000000000000000000 ) ) ;
#1872 = CARTESIAN_POINT ( 'NONE',  ( -3.152548672688508926E-16, -96.56249999863440792, -5.148502694627439702 ) ) ;
#1873 = CARTESIAN_POINT ( 'NONE',  ( 1.464175926609780648E-14, 24.74999999999999645, -5.000000000000000000 ) ) ;
#1874 = CARTESIAN_POINT ( 'NONE',  ( -4.458734124999997661, -0.4791666653010707710, 2.574251347313722516 ) ) ;
#1875 = ORIENTED_EDGE ( 'NONE', *, *, #27621, .F. ) ;
#1876 = LINE ( 'NONE', #21481, #1776 ) ;
#1877 = CARTESIAN_POINT ( 'NONE',  ( -5.000000000000000000, -76.00000000000000000, 0.000000000000000000 ) ) ;
#1878 = CARTESIAN_POINT ( 'NONE',  ( -2.229367062500000163, -85.47916666530107932, -3.861377020970580443 ) ) ;
#1879 = CARTESIAN_POINT ( 'NONE',  ( -2.071067811865475061, -167.8125000027311842, -5.000000000000000888 ) ) ;
#1880 = CARTESIAN_POINT ( 'NONE',  ( 9.457646018065525792E-16, -88.31249999863439371, 5.148502694627439702 ) ) ;
#1881 = CARTESIAN_POINT ( 'NONE',  ( -2.229367062500000163, 12.27083333469892601, -3.861377020970580443 ) ) ;
#1882 = CARTESIAN_POINT ( 'NONE',  ( 5.000000000000000000, -77.29166666393547303, -2.886751345948130876 ) ) ;
#1883 = AXIS2_PLACEMENT_3D ( 'NONE', #26755, #6824, #31573 ) ;
#1884 = CARTESIAN_POINT ( 'NONE',  ( -51.60603307380591787, -133.9375000013656063, -2.891590998281053704 ) ) ;
#1885 =( BOUNDED_CURVE ( )  B_SPLINE_CURVE ( 2, ( #3552, #23160, #24107, #63667, #58515, #8378, #8993, #44019, #34062 ),
 .UNSPECIFIED., .F., .F. ) 
 B_SPLINE_CURVE_WITH_KNOTS ( ( 3, 2, 2, 2, 3 ),
 ( 0.2937500000000000111, 0.2944444444444444531, 0.2958333333333333370, 0.2972222222222222210, 0.2979166666666666630 ),
 .UNSPECIFIED. ) 
 CURVE ( )  GEOMETRIC_REPRESENTATION_ITEM ( )  RATIONAL_B_SPLINE_CURVE ( ( 0.9330127018922194093, 0.9330127018922194093, 1.000000000000000000, 0.8660254037844387076, 1.000000000000000000, 0.8660254037844387076, 1.000000000000000000, 0.9330127018922194093, 0.9330127018922194093 ) ) 
 REPRESENTATION_ITEM ( '' )  );
#1886 = CARTESIAN_POINT ( 'NONE',  ( 4.458734125000000326, -7.895833331967735624, 2.574251347313718519 ) ) ;
#1887 = CARTESIAN_POINT ( 'NONE',  ( 4.458734124999998549, 19.02083333469892779, -2.574251347313721627 ) ) ;
#1888 = CARTESIAN_POINT ( 'NONE',  ( -2.229367062499996610, -50.39583333196772941, 3.861377020970582219 ) ) ;
#1889 = CARTESIAN_POINT ( 'NONE',  ( 4.458734125000001214, -82.89583333196772230, 2.574251347313718519 ) ) ;
#1890 = CARTESIAN_POINT ( 'NONE',  ( -4.458734124999999437, -5.395833331967740953, -2.574251347313719407 ) ) ;
#1891 = DIRECTION ( 'NONE',  ( -0.000000000000000000, -1.000000000000000000, -0.000000000000000000 ) ) ;
#1892 = ORIENTED_EDGE ( 'NONE', *, *, #62648, .T. ) ;
#1893 = CARTESIAN_POINT ( 'NONE',  ( -2.229367062500000163, -28.72916666530107221, -3.861377020970580443 ) ) ;
#1894 = CARTESIAN_POINT ( 'NONE',  ( -50.70258187064364108, -133.3750000013656063, 2.196230717870141014 ) ) ;
#1895 = CARTESIAN_POINT ( 'NONE',  ( -4.458734124999998549, -74.22916666530106511, 2.574251347313722516 ) ) ;
#1896 = CARTESIAN_POINT ( 'NONE',  ( 1.060575238724906964E-15, -109.6249999972688016, 5.773502691896257311 ) ) ;
#1897 = CARTESIAN_POINT ( 'NONE',  ( -2.229367062500000163, 18.52083333469892779, -3.861377020970580443 ) ) ;
#1898 = CARTESIAN_POINT ( 'NONE',  ( -2.499999999999996447, -43.70833333060214443, 4.330127018922195425 ) ) ;
#1899 = CARTESIAN_POINT ( 'NONE',  ( -2.500000000000000444, -26.04166666393547658, -4.330127018922193649 ) ) ;
#1900 = CARTESIAN_POINT ( 'NONE',  ( 2.229367062499998831, -75.89583333196773651, -3.861377020970580887 ) ) ;
#1901 = CARTESIAN_POINT ( 'NONE',  ( 1.060575238724906964E-15, -62.75000000000000000, 5.773502691896257311 ) ) ;
#1902 = CARTESIAN_POINT ( 'NONE',  ( 5.000000000000000888, -90.45833333060214443, 2.886751345948126879 ) ) ;
#1903 = CARTESIAN_POINT ( 'NONE',  ( -2.500000000000000444, 23.95833333606451987, -4.330127018922193649 ) ) ;
#1904 = ORIENTED_EDGE ( 'NONE', *, *, #54985, .T. ) ;
#1905 = DIRECTION ( 'NONE',  ( -0.000000000000000000, 1.000000000000000000, -0.000000000000000000 ) ) ;
#1906 = AXIS2_PLACEMENT_3D ( 'NONE', #49615, #58077, #23369 ) ;
#1907 = CARTESIAN_POINT ( 'NONE',  ( -53.33387254593710480, -138.9375000027312126, 5.149110718188539160 ) ) ;
#1909 = CARTESIAN_POINT ( 'NONE',  ( -5.000000000000000000, -26.08333333333333215, -2.886751345948128211 ) ) ;
#1908 = CARTESIAN_POINT ( 'NONE',  ( -6.972266317189433020E-16, -0.2500000000000001665, -5.000000000000000000 ) ) ;
#1910 = CARTESIAN_POINT ( 'NONE',  ( -4.458734124999999437, -29.39583333196773296, -2.574251347313719407 ) ) ;
#1911 = EDGE_CURVE ( 'NONE', #45549, #35107, #10129, .T. ) ;
#1912 = CARTESIAN_POINT ( 'NONE',  ( 9.457646018065525792E-16, -87.06249999863439371, 5.148502694627439702 ) ) ;
#1913 = CARTESIAN_POINT ( 'NONE',  ( -5.000000000000000000, -23.87499999726881228, 0.000000000000000000 ) ) ;
#1915 = ORIENTED_EDGE ( 'NONE', *, *, #21762, .T. ) ;
#1914 = CARTESIAN_POINT ( 'NONE',  ( 2.229367062499998831, -53.64583333196773651, -3.861377020970580887 ) ) ;
#1916 = CARTESIAN_POINT ( 'NONE',  ( 1.339745962155615144, -27.70534180126147561, 4.999999999999999112 ) ) ;
#1917 = CARTESIAN_POINT ( 'NONE',  ( 5.000000000000000888, -59.45833333060214443, 2.886751345948126879 ) ) ;
#1919 = VERTEX_POINT ( 'NONE', #29736 ) ;
#1918 = CARTESIAN_POINT ( 'NONE',  ( 4.458734124999998549, -2.979166665301069994, -2.574251347313721627 ) ) ;
#1920 = CARTESIAN_POINT ( 'NONE',  ( 5.000000000000000000, -73.41666666666665719, -2.886751345948129988 ) ) ;
#1921 = CARTESIAN_POINT ( 'NONE',  ( -58.39396692619412477, -138.4375000013656063, 2.891590998281057701 ) ) ;
#1922 = CARTESIAN_POINT ( 'NONE',  ( -3.152548672688508926E-16, -45.81249999863440081, -5.148502694627439702 ) ) ;
#1923 = CARTESIAN_POINT ( 'NONE',  ( -5.000000000000000000, -96.00000000000000000, 0.000000000000000000 ) ) ;
#1924 = CARTESIAN_POINT ( 'NONE',  ( -3.535533905932738641, -160.3750000000000284, 3.535533905932737309 ) ) ;
#1925 = CARTESIAN_POINT ( 'NONE',  ( 5.000000000000000888, -69.45833333060214443, 2.886751345948126879 ) ) ;
#1926 = CARTESIAN_POINT ( 'NONE',  ( -4.999999999999998224, -81.79166666393547303, 2.886751345948131764 ) ) ;
#1927 = CARTESIAN_POINT ( 'NONE',  ( -50.01589407740564042, -153.6250000000000284, 0.3983568153799778022 ) ) ;
#1928 = CARTESIAN_POINT ( 'NONE',  ( -4.458734124999999437, -14.64583333196773474, -2.574251347313719407 ) ) ;
#1929 = AXIS2_PLACEMENT_3D ( 'NONE', #26212, #25893, #35870 ) ;
#1930 = CARTESIAN_POINT ( 'NONE',  ( -4.458734124999999437, -50.56249999863440792, 0.000000000000000000 ) ) ;
#1931 = EDGE_CURVE ( 'NONE', #35992, #58774, #49368, .T. ) ;
#1932 = CARTESIAN_POINT ( 'NONE',  ( -6.972266317189433020E-16, -59.12499999726880873, -5.000000000000000000 ) ) ;
#1933 = PRESENTATION_STYLE_ASSIGNMENT (( #51754 ) ) ;
#1934 = CARTESIAN_POINT ( 'NONE',  ( 1.846868145590736310, -144.6250000013655779, 4.458734124999999437 ) ) ;
#1935 = EDGE_CURVE ( 'NONE', #9299, #58694, #23674, .T. ) ;
#1936 = CARTESIAN_POINT ( 'NONE',  ( -2.229367062500000163, -94.72916666530106511, -3.861377020970580443 ) ) ;
#1937 = CARTESIAN_POINT ( 'NONE',  ( 3.061616997868383141E-16, -157.7500000000000000, -5.000000000000000000 ) ) ;
#1938 = EDGE_LOOP ( 'NONE', ( #30187, #28325, #36191, #40566 ) ) ;
#1939 = CARTESIAN_POINT ( 'NONE',  ( -55.35523342533222291, -154.5625000013656347, 4.444560631937231499 ) ) ;
#1940 = CARTESIAN_POINT ( 'NONE',  ( 9.457646018065525792E-16, 24.68750000136559208, 5.148502694627439702 ) ) ;
#1941 = CARTESIAN_POINT ( 'NONE',  ( -59.98410592259440222, -145.2500000027312126, -0.3983568153799752487 ) ) ;
#1942 =( BOUNDED_CURVE ( )  B_SPLINE_CURVE ( 2, ( #9601, #63025, #14108, #63650, #63332, #34046, #28273, #4774, #47888 ),
 .UNSPECIFIED., .F., .F. ) 
 B_SPLINE_CURVE_WITH_KNOTS ( ( 3, 2, 2, 2, 3 ),
 ( 0.3416666666666669516, 0.3458333333333336035, 0.3500000000000002554, 0.3541666666666669627, 0.3583333333333336146 ),
 .UNSPECIFIED. ) 
 CURVE ( )  GEOMETRIC_REPRESENTATION_ITEM ( )  RATIONAL_B_SPLINE_CURVE ( ( 0.9999999999999948930, 0.9238795325112918455, 1.000000000000000000, 0.9238795325112867385, 1.000000000000000000, 0.9238795325112867385, 1.000000000000000000, 0.9238795325112816315, 1.000000000000005107 ) ) 
 REPRESENTATION_ITEM ( '' )  );
#1943 = CARTESIAN_POINT ( 'NONE',  ( 5.000000000000000888, -60.58333333333332860, 2.886751345948126879 ) ) ;
#1944 = EDGE_CURVE ( 'NONE', #5440, #14049, #63525, .T. ) ;
#1945 = CARTESIAN_POINT ( 'NONE',  ( -4.458734124999999437, -2.395833331967737845, -2.574251347313719407 ) ) ;
#1946 = CARTESIAN_POINT ( 'NONE',  ( 4.458734124999999437, -149.6875000013656063, 0.000000000000000000 ) ) ;
#1947 = CARTESIAN_POINT ( 'NONE',  ( -4.458734124999999437, -22.64583333196773296, -2.574251347313719407 ) ) ;
#1948 = CARTESIAN_POINT ( 'NONE',  ( 4.458734124999998549, -61.97916666530106511, -2.574251347313721627 ) ) ;
#1949 = CARTESIAN_POINT ( 'NONE',  ( -4.999999999999998224, -83.79166666393545881, 2.886751345948131764 ) ) ;
#1950 = CARTESIAN_POINT ( 'NONE',  ( -2.229367062499996610, -9.145833331967736513, 3.861377020970582219 ) ) ;
#1951 = CARTESIAN_POINT ( 'NONE',  ( 1.975475456537005874E-15, 17.25000000000000000, 5.000000000000000000 ) ) ;
#1952 = CARTESIAN_POINT ( 'NONE',  ( -1.846868145590734756, -145.1250000013656063, -4.458734124999999437 ) ) ;
#1953 = CARTESIAN_POINT ( 'NONE',  ( 2.229367062500001939, 14.77083333469892779, 3.861377020970579999 ) ) ;
#1954 = ORIENTED_EDGE ( 'NONE', *, *, #56312, .F. ) ;
#1955 = DIRECTION ( 'NONE',  ( 0.000000000000000000, 0.000000000000000000, 1.000000000000000000 ) ) ;
#1956 = CARTESIAN_POINT ( 'NONE',  ( 1.975475456537005874E-15, -57.62499999726880873, 5.000000000000000000 ) ) ;
#1958 = CARTESIAN_POINT ( 'NONE',  ( 4.458734125000001214, -17.89583333196774007, 2.574251347313718519 ) ) ;
#1957 = CARTESIAN_POINT ( 'NONE',  ( 1.060575238724906964E-15, -83.75000000000000000, 5.773502691896257311 ) ) ;
#1959 = CARTESIAN_POINT ( 'NONE',  ( 7.500000000000000888, 3.639598441879751345, -0.7155132341745285007 ) ) ;
#1960 = CARTESIAN_POINT ( 'NONE',  ( 2.500000000000002220, 1.458333336064519203, 4.330127018922192761 ) ) ;
#1961 = CARTESIAN_POINT ( 'NONE',  ( -56.48576386720575471, -149.7500000013656063, -4.591703134518078322 ) ) ;
#1962 = EDGE_CURVE ( 'NONE', #14760, #21496, #4343, .T. ) ;
#1963 = CARTESIAN_POINT ( 'NONE',  ( 2.500000000000002220, -47.54166666393547303, 4.330127018922192761 ) ) ;
#1964 = CARTESIAN_POINT ( 'NONE',  ( -4.458734124999999437, 9.604166668032259935, -2.574251347313719407 ) ) ;
#1965 = DIRECTION ( 'NONE',  ( 0.000000000000000000, 0.000000000000000000, 1.000000000000000000 ) ) ;
#1966 = CARTESIAN_POINT ( 'NONE',  ( -2.499999999999996447, -14.83333333333333037, 4.330127018922195425 ) ) ;
#1967 = CARTESIAN_POINT ( 'NONE',  ( 9.457646018065525792E-16, 12.93750000136559208, 5.148502694627439702 ) ) ;
#1968 = CARTESIAN_POINT ( 'NONE',  ( 4.458734124999998549, -65.72916666530106511, -2.574251347313721627 ) ) ;
#1969 = CARTESIAN_POINT ( 'NONE',  ( 4.458734125000000326, -15.14583333196773474, 2.574251347313718519 ) ) ;
#1970 =( BOUNDED_CURVE ( )  B_SPLINE_CURVE ( 2, ( #17741, #57310, #27074, #3587, #32207, #17106, #58472, #63300, #19219 ),
 .UNSPECIFIED., .F., .F. ) 
 B_SPLINE_CURVE_WITH_KNOTS ( ( 3, 2, 2, 2, 3 ),
 ( 0.7416666666666664742, 0.7458333333333331261, 0.7499999999999997780, 0.7541666666666664298, 0.7583333333333330817 ),
 .UNSPECIFIED. ) 
 CURVE ( )  GEOMETRIC_REPRESENTATION_ITEM ( )  RATIONAL_B_SPLINE_CURVE ( ( 1.000000000000003997, 0.9238795325112826307, 1.000000000000000000, 0.9238795325112867385, 1.000000000000000000, 0.9238795325112867385, 1.000000000000000000, 0.9238795325112908463, 0.9999999999999958922 ) ) 
 REPRESENTATION_ITEM ( '' )  );
#1971 = CARTESIAN_POINT ( 'NONE',  ( -2.500000000000000444, -2.166666666666663854, -4.330127018922193649 ) ) ;
#1972 = CARTESIAN_POINT ( 'NONE',  ( -8.190561711645485556E-16, -162.6875000013655779, 4.458734124999999437 ) ) ;
#1973 = CARTESIAN_POINT ( 'NONE',  ( -5.000000000000000000, -38.08333333333333570, -2.886751345948128211 ) ) ;
#1974 = CARTESIAN_POINT ( 'NONE',  ( -4.458734124999999437, -59.39583333196773651, -2.574251347313719407 ) ) ;
#1975 = CARTESIAN_POINT ( 'NONE',  ( -3.535250795749689387E-16, -97.12499999726881583, -5.773502691896257311 ) ) ;
#1976 = CARTESIAN_POINT ( 'NONE',  ( -2.500000000000000444, -28.16666666666666785, -4.330127018922193649 ) ) ;
#1977 = CARTESIAN_POINT ( 'NONE',  ( -58.80597590150559739, -152.1250000027312126, 3.242614290531460330 ) ) ;
#1978 = CARTESIAN_POINT ( 'NONE',  ( 9.457646018065525792E-16, -33.06249999863440792, 5.148502694627439702 ) ) ;
#1979 = CARTESIAN_POINT ( 'NONE',  ( -2.500000000000000444, -49.16666666666666430, -4.330127018922193649 ) ) ;
#1980 = LINE ( 'NONE', #21582, #16163 ) ;
#1981 = CARTESIAN_POINT ( 'NONE',  ( -5.000000000000000000, -108.0833333333333712, -2.886751345948128211 ) ) ;
#1982 = ORIENTED_EDGE ( 'NONE', *, *, #32984, .F. ) ;
#1983 = CARTESIAN_POINT ( 'NONE',  ( 4.458734124999999437, -106.8124999986343937, -5.460374474430324690E-16 ) ) ;
#1984 = CARTESIAN_POINT ( 'NONE',  ( -2.229367062500000163, -0.7291666653010709931, -3.861377020970580443 ) ) ;
#1985 = CARTESIAN_POINT ( 'NONE',  ( -5.000000000000000000, -67.87499999726881583, 0.000000000000000000 ) ) ;
#1986 = CARTESIAN_POINT ( 'NONE',  ( -2.499999999999996447, -5.833333333333336590, 4.330127018922195425 ) ) ;
#1987 = EDGE_CURVE ( 'NONE', #29821, #727, #46303, .T. ) ;
#1988 = CARTESIAN_POINT ( 'NONE',  ( 4.458734125000000326, -73.89583333196773651, 2.574251347313718519 ) ) ;
#1989 = CARTESIAN_POINT ( 'NONE',  ( 2.499999999999998668, -22.20833333060215153, -4.330127018922193649 ) ) ;
#1990 = CARTESIAN_POINT ( 'NONE',  ( 5.000000000000000000, -9.374999997268814056, -6.123233995736766282E-16 ) ) ;
#1992 = VERTEX_POINT ( 'NONE', #55165 ) ;
#1991 = CARTESIAN_POINT ( 'NONE',  ( -4.458734124999999437, -40.39583333196773651, -2.574251347313719407 ) ) ;
#1993 = CARTESIAN_POINT ( 'NONE',  ( 0.000000000000000000, -120.0000000000000000, 0.000000000000000000 ) ) ;
#1995 = EDGE_LOOP ( 'NONE', ( #51913, #30074, #14352, #18115 ) ) ;
#1994 = CARTESIAN_POINT ( 'NONE',  ( 2.229367062500001939, 13.77083333469892779, 3.861377020970579999 ) ) ;
#1996 = CARTESIAN_POINT ( 'NONE',  ( -1.339745962155610925, -48.66965819600732601, 5.000000000000000000 ) ) ;
#1997 = CARTESIAN_POINT ( 'NONE',  ( 5.000000000000000000, -54.41666666666666430, -2.886751345948129988 ) ) ;
#1998 = CARTESIAN_POINT ( 'NONE',  ( -2.229367062500000163, -30.72916666530107221, -3.861377020970580443 ) ) ;
#1999 = PRESENTATION_LAYER_ASSIGNMENT (  '', '', ( #14305 ) ) ;
#2000 = CARTESIAN_POINT ( 'NONE',  ( 3.535533905932738197, -144.8750000000000000, -3.535533905932738197 ) ) ;
#2001 = CARTESIAN_POINT ( 'NONE',  ( -2.229367062499996610, -77.14583333196773651, 3.861377020970582219 ) ) ;
#2002 = CARTESIAN_POINT ( 'NONE',  ( 3.152801135295366208, -141.8125000013655779, 3.152801135295367985 ) ) ;
#2003 = CARTESIAN_POINT ( 'NONE',  ( 2.229367062500001939, -87.97916666530107932, 3.861377020970579999 ) ) ;
#2004 = VECTOR ( 'NONE', #7384, 1000.000000000000000 ) ;
#2005 = CARTESIAN_POINT ( 'NONE',  ( -58.39396692619412477, -136.6875000013656063, 2.891590998281057701 ) ) ;
#2006 = CARTESIAN_POINT ( 'NONE',  ( 4.458734124999999437, -33.06249999863440792, -5.460374474430324690E-16 ) ) ;
#2007 = DIRECTION ( 'NONE',  ( 0.000000000000000000, 0.000000000000000000, 1.000000000000000000 ) ) ;
#2009 = EDGE_CURVE ( 'NONE', #54337, #24836, #6435, .T. ) ;
#2008 = ORIENTED_EDGE ( 'NONE', *, *, #60078, .F. ) ;
#2010 = CARTESIAN_POINT ( 'NONE',  ( 4.458734124999999437, -78.06249999863440792, -5.460374474430324690E-16 ) ) ;
#2011 = CARTESIAN_POINT ( 'NONE',  ( -1.339745962155613812, 12.91965820146970678, -5.000000000000000000 ) ) ;
#2012 = VERTEX_POINT ( 'NONE', #6586 ) ;
#2013 = CARTESIAN_POINT ( 'NONE',  ( 1.339745962155615144, -16.70534180126147561, 4.999999999999999112 ) ) ;
#2014 = CARTESIAN_POINT ( 'NONE',  ( 1.975475456537005874E-15, -11.62499999726881406, 5.000000000000000000 ) ) ;
#2015 = CARTESIAN_POINT ( 'NONE',  ( -2.229367062499996610, -65.39583333196773651, 3.861377020970582219 ) ) ;
#2016 = CARTESIAN_POINT ( 'NONE',  ( 4.458734124999999437, -8.062499998634404363, -5.460374474430324690E-16 ) ) ;
#2017 = EDGE_LOOP ( 'NONE', ( #6645, #32915, #9936, #10300 ) ) ;
#2018 = DIRECTION ( 'NONE',  ( 0.000000000000000000, 0.000000000000000000, -1.000000000000000000 ) ) ;
#2019 = CARTESIAN_POINT ( 'NONE',  ( -6.972266317189433020E-16, -62.24999999999999289, -5.000000000000000000 ) ) ;
#2020 = ORIENTED_EDGE ( 'NONE', *, *, #41778, .F. ) ;
#2021 = CARTESIAN_POINT ( 'NONE',  ( -2.229367062499996610, -4.395833331967740065, 3.861377020970582219 ) ) ;
#2022 = CARTESIAN_POINT ( 'NONE',  ( -3.152548672688508926E-16, 8.437500001365595637, -5.148502694627439702 ) ) ;
#2023 = CARTESIAN_POINT ( 'NONE',  ( -9.184850993605147944E-16, -154.2500000000000000, 5.000000000000000000 ) ) ;
#2024 = CARTESIAN_POINT ( 'NONE',  ( -8.190561711645485556E-16, -157.6875000013655779, 4.458734124999999437 ) ) ;
#2025 = DIRECTION ( 'NONE',  ( -0.000000000000000000, 1.000000000000000000, -0.000000000000000000 ) ) ;
#2026 = ORIENTED_EDGE ( 'NONE', *, *, #62327, .F. ) ;
#2027 = CARTESIAN_POINT ( 'NONE',  ( -4.458734124999999437, -89.31249999863440792, 0.000000000000000000 ) ) ;
#2028 = CARTESIAN_POINT ( 'NONE',  ( 5.000000000000000000, -164.1875000027312126, 2.071067811865478614 ) ) ;
#2029 = CARTESIAN_POINT ( 'NONE',  ( 4.458734124999998549, -0.7291666653010709931, -2.574251347313721627 ) ) ;
#2030 = FACE_OUTER_BOUND ( 'NONE', #31095, .T. ) ;
#2031 = CARTESIAN_POINT ( 'NONE',  ( -2.499999999999996447, -31.70833333060214798, 4.330127018922195425 ) ) ;
#2032 = CYLINDRICAL_SURFACE ( 'NONE', #39898, 5.000000000000000000 ) ;
#2033 = CARTESIAN_POINT ( 'NONE',  ( 2.229367062500001939, 26.02083333469892779, 3.861377020970579999 ) ) ;
#2034 = CARTESIAN_POINT ( 'NONE',  ( -1.339745962155613812, -56.20534180126148271, -5.000000000000000000 ) ) ;
#2035 = CARTESIAN_POINT ( 'NONE',  ( 4.458734125000000326, 29.10416666803226349, 2.574251347313718519 ) ) ;
#2036 = CARTESIAN_POINT ( 'NONE',  ( 2.229367062500001939, -51.97916666530107221, 3.861377020970579999 ) ) ;
#2037 = CARTESIAN_POINT ( 'NONE',  ( 4.458734124999998549, -37.97916666530107221, -2.574251347313721627 ) ) ;
#2038 = CARTESIAN_POINT ( 'NONE',  ( 4.458734125000000326, 3.854166668032260823, 2.574251347313718519 ) ) ;
#2039 = CARTESIAN_POINT ( 'NONE',  ( -2.229367062499996610, -39.39583333196773651, 3.861377020970582219 ) ) ;
#2040 = CARTESIAN_POINT ( 'NONE',  ( 5.000000000000000000, -160.1250000027311842, 0.000000000000000000 ) ) ;
#2041 = CARTESIAN_POINT ( 'NONE',  ( 5.000000000000000000, 13.58333333333333215, -2.886751345948129988 ) ) ;
#2042 = CARTESIAN_POINT ( 'NONE',  ( 2.071067811865476394, -144.3125000027312126, 5.000000000000000000 ) ) ;
#2043 = CARTESIAN_POINT ( 'NONE',  ( -8.660254037844341113, 45.00000000000000000, 6.047423072554883697E-14 ) ) ;
#2044 = CARTESIAN_POINT ( 'NONE',  ( -2.229367062499996610, -40.14583333196773651, 3.861377020970582219 ) ) ;
#2045 = CARTESIAN_POINT ( 'NONE',  ( -4.999999999999999112, -76.79166666393547303, 2.886751345948131764 ) ) ;
#2046 = CARTESIAN_POINT ( 'NONE',  ( -55.35523342533222291, -141.5625000013656063, 4.444560631937231499 ) ) ;
#2047 = DIRECTION ( 'NONE',  ( 0.8191520442889907994, 0.000000000000000000, 0.5735764363510474917 ) ) ;
#2048 = CARTESIAN_POINT ( 'NONE',  ( -6.972266317189433020E-16, -59.25000000000000000, -5.000000000000000000 ) ) ;
#2049 = CARTESIAN_POINT ( 'NONE',  ( 2.229367062499998831, -83.89583333196773651, -3.861377020970580887 ) ) ;
#2050 = CARTESIAN_POINT ( 'NONE',  ( 3.152801135295366208, -162.8125000013656063, 3.152801135295367985 ) ) ;
#2051 = CARTESIAN_POINT ( 'NONE',  ( -0.6169862416623524970, -8.783631307150855605, -7.913704048099795330 ) ) ;
#2052 = CARTESIAN_POINT ( 'NONE',  ( 2.499999999999998668, -30.33333333333332860, -4.330127018922193649 ) ) ;
#2053 = CARTESIAN_POINT ( 'NONE',  ( 1.846868145590735200, -140.2500000013656063, -4.458734125000000326 ) ) ;
#2054 = ORIENTED_EDGE ( 'NONE', *, *, #50275, .T. ) ;
#2055 = CARTESIAN_POINT ( 'NONE',  ( -2.229367062499996610, 22.60416666803225993, 3.861377020970582219 ) ) ;
#2056 = VERTEX_POINT ( 'NONE', #16554 ) ;
#2057 = CARTESIAN_POINT ( 'NONE',  ( -4.458734124999999437, -90.39583333196773651, -2.574251347313719407 ) ) ;
#2058 = CARTESIAN_POINT ( 'NONE',  ( 4.458734125000001214, 11.85416666803225993, 2.574251347313718519 ) ) ;
#2059 = VECTOR ( 'NONE', #54352, 1000.000000000000000 ) ;
#2060 = CARTESIAN_POINT ( 'NONE',  ( -5.000000000000000000, 18.04166666939785557, -2.886751345948128211 ) ) ;
#2061 = CARTESIAN_POINT ( 'NONE',  ( -5.000000000000000000, 8.916666666666666075, -2.886751345948128211 ) ) ;
#2062 = CARTESIAN_POINT ( 'NONE',  ( -2.229367062499996610, -58.14583333196773651, 3.861377020970582219 ) ) ;
#2063 = CARTESIAN_POINT ( 'NONE',  ( 9.457646018065525792E-16, -11.06249999863440969, 5.148502694627439702 ) ) ;
#2064 =( BOUNDED_CURVE ( )  B_SPLINE_CURVE ( 2, ( #15831, #36724, #60226, #50561, #56355, #55394, #50238, #25801, #36084 ),
 .UNSPECIFIED., .F., .F. ) 
 B_SPLINE_CURVE_WITH_KNOTS ( ( 3, 2, 2, 2, 3 ),
 ( 0.3125000000000000000, 0.3130952380952380931, 0.3142857142857142794, 0.3154761904761904656, 0.3160714285714285587 ),
 .UNSPECIFIED. ) 
 CURVE ( )  GEOMETRIC_REPRESENTATION_ITEM ( )  RATIONAL_B_SPLINE_CURVE ( ( 0.9330127018922194093, 0.9330127018922194093, 1.000000000000000000, 0.8660254037844387076, 1.000000000000000000, 0.8660254037844387076, 1.000000000000000000, 0.9330127018922194093, 0.9330127018922194093 ) ) 
 REPRESENTATION_ITEM ( '' )  );
#2065 = FACE_OUTER_BOUND ( 'NONE', #4715, .T. ) ;
#2066 = EDGE_CURVE ( 'NONE', #55117, #44647, #33098, .T. ) ;
#2067 = ADVANCED_FACE ( 'NONE', ( #50003 ), #60949, .T. ) ;
#2068 = CARTESIAN_POINT ( 'NONE',  ( -6.972266317189433020E-16, -52.12499999726880873, -5.000000000000000000 ) ) ;
#2069 = CARTESIAN_POINT ( 'NONE',  ( 1.975475456537005874E-15, -36.75000000000000000, 5.000000000000000000 ) ) ;
#2070 = EDGE_CURVE ( 'NONE', #4248, #1202, #45820, .T. ) ;
#2071 = CARTESIAN_POINT ( 'NONE',  ( 5.000000000000000000, 28.70833333606451987, -2.886751345948130876 ) ) ;
#2072 = CARTESIAN_POINT ( 'NONE',  ( 2.500000000000002220, -39.66666666666667140, 4.330127018922192761 ) ) ;
#2073 = CARTESIAN_POINT ( 'NONE',  ( -6.972266317189433020E-16, -96.25000000000000000, -5.000000000000000000 ) ) ;
#2075 = CARTESIAN_POINT ( 'NONE',  ( 4.458734125000001214, -17.14583333196773651, 2.574251347313718519 ) ) ;
#2074 = CYLINDRICAL_SURFACE ( 'NONE', #5782, 5.000000000000000000 ) ;
#2076 = EDGE_CURVE ( 'NONE', #14691, #5147, #48299, .T. ) ;
#2077 = FACE_OUTER_BOUND ( 'NONE', #22962, .T. ) ;
#2078 = CARTESIAN_POINT ( 'NONE',  ( 9.457646018065525792E-16, -57.06249999863440081, 5.148502694627439702 ) ) ;
#2079 = CARTESIAN_POINT ( 'NONE',  ( 4.458734124999999437, -151.7500000013655779, 1.846868145590737864 ) ) ;
#2080 = CARTESIAN_POINT ( 'NONE',  ( 2.229367062500001939, -69.97916666530107932, 3.861377020970579999 ) ) ;
#2081 = CARTESIAN_POINT ( 'NONE',  ( -54.64476657466781973, -148.0625000013656063, -4.444560631937228834 ) ) ;
#2082 = EDGE_CURVE ( 'NONE', #53065, #23818, #20747, .T. ) ;
#2083 = ADVANCED_FACE ( 'NONE', ( #40990 ), #34899, .T. ) ;
#2084 = CARTESIAN_POINT ( 'NONE',  ( 2.229367062500001939, -22.22916666530107221, 3.861377020970579999 ) ) ;
#2085 = CARTESIAN_POINT ( 'NONE',  ( -5.000000000000000000, -60.95833333060214443, -2.886751345948128211 ) ) ;
#2086 = ORIENTED_EDGE ( 'NONE', *, *, #4425, .T. ) ;
#2087 = CARTESIAN_POINT ( 'NONE',  ( 5.000000000000000888, -31.45833333060214798, 2.886751345948126879 ) ) ;
#2088 = ORIENTED_EDGE ( 'NONE', *, *, #51233, .T. ) ;
#2089 = CARTESIAN_POINT ( 'NONE',  ( -4.458734124999999437, -60.56249999863440081, 0.000000000000000000 ) ) ;
#2091 = CARTESIAN_POINT ( 'NONE',  ( 1.975475456537005874E-15, -85.75000000000000000, 5.000000000000000000 ) ) ;
#2090 = CARTESIAN_POINT ( 'NONE',  ( -3.535533905932737309, -157.7500000027312126, -3.535533905932738197 ) ) ;
#2092 = CARTESIAN_POINT ( 'NONE',  ( 3.152801135295367541, -154.3125000013656063, -3.152801135295367541 ) ) ;
#2093 = EDGE_CURVE ( 'NONE', #6014, #15910, #20426, .T. ) ;
#2094 = ORIENTED_EDGE ( 'NONE', *, *, #48422, .T. ) ;
#2095 = EDGE_CURVE ( 'NONE', #34156, #19872, #30705, .T. ) ;
#2096 = ADVANCED_FACE ( 'NONE', ( #27466 ), #7234, .T. ) ;
#2097 = CARTESIAN_POINT ( 'NONE',  ( -53.33387254593733928, -125.8125000000000142, 5.149110718188519620 ) ) ;
#2099 = AXIS2_PLACEMENT_3D ( 'NONE', #63432, #44421, #34786 ) ;
#2098 = DIRECTION ( 'NONE',  ( -0.000000000000000000, 1.000000000000000000, -0.000000000000000000 ) ) ;
#2100 = CARTESIAN_POINT ( 'NONE',  ( 4.458734124999999437, -49.06249999863440792, -5.460374474430324690E-16 ) ) ;
#2101 = ORIENTED_EDGE ( 'NONE', *, *, #34250, .F. ) ;
#2102 = CARTESIAN_POINT ( 'NONE',  ( -5.000000000000000888, -145.5625000000000568, -2.071067811865475949 ) ) ;
#2103 = CARTESIAN_POINT ( 'NONE',  ( -2.229367062500000163, 6.520833334698928674, -3.861377020970580443 ) ) ;
#2104 = CARTESIAN_POINT ( 'NONE',  ( -4.458734124999999437, 24.68750000136559208, 0.000000000000000000 ) ) ;
#2105 = CARTESIAN_POINT ( 'NONE',  ( -59.29741812935640155, -147.6250000013655779, -2.196230717870135685 ) ) ;
#2106 = CARTESIAN_POINT ( 'NONE',  ( -59.98410592259440222, -150.2500000027312126, -0.3983568153799752487 ) ) ;
#2107 = CARTESIAN_POINT ( 'NONE',  ( 0.000000000000000000, -170.0000000000000000, 0.000000000000000000 ) ) ;
#2108 = ORIENTED_EDGE ( 'NONE', *, *, #38873, .F. ) ;
#2109 = CARTESIAN_POINT ( 'NONE',  ( 2.229367062500001939, -72.97916666530107932, 3.861377020970579999 ) ) ;
#2110 = CARTESIAN_POINT ( 'NONE',  ( 6.123233995736766282E-16, -120.0000000000000000, -5.000000000000000000 ) ) ;
#2111 = CARTESIAN_POINT ( 'NONE',  ( 2.229367062500001939, 11.02083333469892956, 3.861377020970579999 ) ) ;
#2112 = CARTESIAN_POINT ( 'NONE',  ( -52.53715891517739323, -152.5625000027311842, -4.819101127000233298 ) ) ;
#2113 = CARTESIAN_POINT ( 'NONE',  ( 4.458734125000001214, -57.14583333196773651, 2.574251347313718519 ) ) ;
#2114 = CARTESIAN_POINT ( 'NONE',  ( -5.000000000000000000, -15.87499999726881406, 0.000000000000000000 ) ) ;
#2115 = CARTESIAN_POINT ( 'NONE',  ( -2.499999999999996447, -32.70833333060215153, 4.330127018922195425 ) ) ;
#2116 = CARTESIAN_POINT ( 'NONE',  ( -5.000000000000000000, -139.6250000027312126, -6.123233995736766282E-16 ) ) ;
#2117 =( BOUNDED_CURVE ( )  B_SPLINE_CURVE ( 2, ( #62044, #16709, #36324, #11866, #63613, #29175, #43653, #48492, #33082 ),
 .UNSPECIFIED., .F., .F. ) 
 B_SPLINE_CURVE_WITH_KNOTS ( ( 3, 2, 2, 2, 3 ),
 ( 0.3104166666666666741, 0.3111111111111111160, 0.3125000000000000000, 0.3138888888888888840, 0.3145833333333333259 ),
 .UNSPECIFIED. ) 
 CURVE ( )  GEOMETRIC_REPRESENTATION_ITEM ( )  RATIONAL_B_SPLINE_CURVE ( ( 0.9330127018922194093, 0.9330127018922194093, 1.000000000000000000, 0.8660254037844387076, 1.000000000000000000, 0.8660254037844387076, 1.000000000000000000, 0.9330127018922194093, 0.9330127018922194093 ) ) 
 REPRESENTATION_ITEM ( '' )  );
#2118 = DIRECTION ( 'NONE',  ( -0.000000000000000000, 1.000000000000000000, -0.000000000000000000 ) ) ;
#2119 = CARTESIAN_POINT ( 'NONE',  ( -3.152548672688508926E-16, -20.81249999863440081, -5.148502694627439702 ) ) ;
#2120 =( BOUNDED_CURVE ( )  B_SPLINE_CURVE ( 2, ( #43014, #52673, #32419, #36938, #12485, #62018, #61390, #32098, #52980 ),
 .UNSPECIFIED., .F., .F. ) 
 B_SPLINE_CURVE_WITH_KNOTS ( ( 3, 2, 2, 2, 3 ),
 ( 0.7267857142857142572, 0.7273809523809523503, 0.7285714285714285365, 0.7297619047619047228, 0.7303571428571428159 ),
 .UNSPECIFIED. ) 
 CURVE ( )  GEOMETRIC_REPRESENTATION_ITEM ( )  RATIONAL_B_SPLINE_CURVE ( ( 0.9330127018922194093, 0.9330127018922194093, 1.000000000000000000, 0.8660254037844387076, 1.000000000000000000, 0.8660254037844387076, 1.000000000000000000, 0.9330127018922194093, 0.9330127018922194093 ) ) 
 REPRESENTATION_ITEM ( '' )  );
#2121 = ORIENTED_EDGE ( 'NONE', *, *, #20497, .F. ) ;
#2122 = CARTESIAN_POINT ( 'NONE',  ( 2.229367062499998831, -108.6458333319677365, -3.861377020970580887 ) ) ;
#2123 = CARTESIAN_POINT ( 'NONE',  ( 3.535533905932738197, -157.0000000027312126, -3.535533905932738197 ) ) ;
#2124 = EDGE_LOOP ( 'NONE', ( #16966, #31387, #25754, #11709 ) ) ;
#2125 = CARTESIAN_POINT ( 'NONE',  ( -4.458734124999999437, -102.5624999986344079, 0.000000000000000000 ) ) ;
#2126 = CARTESIAN_POINT ( 'NONE',  ( -4.458734124999998549, -24.22916666530107577, 2.574251347313722516 ) ) ;
#2127 = CARTESIAN_POINT ( 'NONE',  ( 2.500000000000002220, -60.54166666393547303, 4.330127018922192761 ) ) ;
#2128 = CARTESIAN_POINT ( 'NONE',  ( -50.40829686548195099, -151.2500000013656063, -1.485763867205728284 ) ) ;
#2129 = CARTESIAN_POINT ( 'NONE',  ( -52.10840900171896806, -142.1875000013656063, 3.393966926194110556 ) ) ;
#2130 = CARTESIAN_POINT ( 'NONE',  ( 4.458734124999999437, -24.81249999863440436, -5.460374474430324690E-16 ) ) ;
#2131 = CARTESIAN_POINT ( 'NONE',  ( -3.152548672688508926E-16, -67.81249999863440792, -5.148502694627439702 ) ) ;
#2132 = CARTESIAN_POINT ( 'NONE',  ( 4.458734124999999437, -23.81249999863440436, -5.460374474430324690E-16 ) ) ;
#2133 = CARTESIAN_POINT ( 'NONE',  ( 2.071067811865392461, -147.1875000000000853, 5.000000000000084377 ) ) ;
#2134 = CARTESIAN_POINT ( 'NONE',  ( 3.535533905932738197, -152.8750000000000000, -3.535533905932738197 ) ) ;
#2135 = CARTESIAN_POINT ( 'NONE',  ( 1.060575238724906964E-15, -12.74999999999999822, 5.773502691896257311 ) ) ;
#2136 = CARTESIAN_POINT ( 'NONE',  ( 4.458734124999999437, -151.4375000013655779, 0.000000000000000000 ) ) ;
#2137 = ORIENTED_EDGE ( 'NONE', *, *, #32329, .T. ) ;
#2138 = CARTESIAN_POINT ( 'NONE',  ( -2.229367062499996610, -49.39583333196772941, 3.861377020970582219 ) ) ;
#2139 = CARTESIAN_POINT ( 'NONE',  ( 5.000000000000000888, -84.45833333060214443, 2.886751345948126879 ) ) ;
#2140 = CARTESIAN_POINT ( 'NONE',  ( -4.999999999999999112, 23.08333333333332860, 2.886751345948131764 ) ) ;
#2141 = VECTOR ( 'NONE', #37387, 1000.000000000000000 ) ;
#2142 = CARTESIAN_POINT ( 'NONE',  ( 1.975475456537005874E-15, 13.24999999999999822, 5.000000000000000000 ) ) ;
#2143 = CARTESIAN_POINT ( 'NONE',  ( -2.229367062500000163, 3.520833334698929118, -3.861377020970580443 ) ) ;
#2144 = CARTESIAN_POINT ( 'NONE',  ( 6.324555320336760822, 15.00000000000000000, 8.999999999999998224 ) ) ;
#2145 = CARTESIAN_POINT ( 'NONE',  ( -6.972266317189433020E-16, -41.12499999726880162, -5.000000000000000000 ) ) ;
#2146 = CARTESIAN_POINT ( 'NONE',  ( 0.000000000000000000, -120.0000000000000000, 0.000000000000000000 ) ) ;
#2147 = CARTESIAN_POINT ( 'NONE',  ( -3.152548672688508926E-16, 14.18750000136559386, -5.148502694627439702 ) ) ;
#2148 = CARTESIAN_POINT ( 'NONE',  ( 2.500000000000002220, 2.458333336064519870, 4.330127018922192761 ) ) ;
#2149 = ORIENTED_EDGE ( 'NONE', *, *, #40155, .F. ) ;
#2150 = CARTESIAN_POINT ( 'NONE',  ( 2.500000000000002220, 26.33333333333333215, 4.330127018922192761 ) ) ;
#2151 = VERTEX_POINT ( 'NONE', #8487 ) ;
#2152 = CARTESIAN_POINT ( 'NONE',  ( 1.975475456537005874E-15, -85.75000000000000000, 5.000000000000000000 ) ) ;
#2153 = CARTESIAN_POINT ( 'NONE',  ( -2.229367062500000163, -42.47916666530107932, -3.861377020970580443 ) ) ;
#2154 = AXIS2_PLACEMENT_3D ( 'NONE', #31969, #51605, #37127 ) ;
#2155 = CARTESIAN_POINT ( 'NONE',  ( -8.190561711645485556E-16, -163.9375000013655779, 4.458734124999999437 ) ) ;
#2156 = CARTESIAN_POINT ( 'NONE',  ( 2.500000000000002220, -45.54166666393547303, 4.330127018922192761 ) ) ;
#2157 = ORIENTED_EDGE ( 'NONE', *, *, #39804, .T. ) ;
#2158 = CARTESIAN_POINT ( 'NONE',  ( -4.458734124999999437, -19.31249999863440081, 0.000000000000000000 ) ) ;
#2159 = ORIENTED_EDGE ( 'NONE', *, *, #22101, .F. ) ;
#2160 = CARTESIAN_POINT ( 'NONE',  ( -5.000000000000000000, -87.08333333333331439, -2.886751345948128211 ) ) ;
#2161 = CARTESIAN_POINT ( 'NONE',  ( 4.458734124999999437, -165.4375000013655779, 0.000000000000000000 ) ) ;
#2162 =( BOUNDED_CURVE ( )  B_SPLINE_CURVE ( 2, ( #4261, #52529, #43482, #28999, #4563, #18103, #63127, #34147, #32905 ),
 .UNSPECIFIED., .F., .F. ) 
 B_SPLINE_CURVE_WITH_KNOTS ( ( 3, 2, 2, 2, 3 ),
 ( 0.1589285714285714191, 0.1595238095238095122, 0.1607142857142857262, 0.1619047619047619124, 0.1625000000000000056 ),
 .UNSPECIFIED. ) 
 CURVE ( )  GEOMETRIC_REPRESENTATION_ITEM ( )  RATIONAL_B_SPLINE_CURVE ( ( 0.9330127018922194093, 0.9330127018922194093, 1.000000000000000000, 0.8660254037844387076, 1.000000000000000000, 0.8660254037844387076, 1.000000000000000000, 0.9330127018922194093, 0.9330127018922194093 ) ) 
 REPRESENTATION_ITEM ( '' )  );
#2164 = ORIENTED_EDGE ( 'NONE', *, *, #52265, .F. ) ;
#2163 = LINE ( 'NONE', #41362, #48744 ) ;
#2165 = CARTESIAN_POINT ( 'NONE',  ( -56.66612745406270335, -139.3125000000000284, -5.149110718188516067 ) ) ;
#2166 = CARTESIAN_POINT ( 'NONE',  ( -4.458734124999999437, -33.56249999863440792, 0.000000000000000000 ) ) ;
#2167 = CARTESIAN_POINT ( 'NONE',  ( -2.071067811865306307, -147.8125000027311842, -5.000000000000171418 ) ) ;
#2168 = ORIENTED_EDGE ( 'NONE', *, *, #7515, .F. ) ;
#2169 = EDGE_CURVE ( 'NONE', #2464, #30447, #54888, .T. ) ;
#2170 = CARTESIAN_POINT ( 'NONE',  ( 4.458734124999999437, -77.81249999863440792, -5.460374474430324690E-16 ) ) ;
#2171 = CARTESIAN_POINT ( 'NONE',  ( -4.458734124999998549, 23.77083333469892423, 2.574251347313722516 ) ) ;
#2172 = CARTESIAN_POINT ( 'NONE',  ( 5.000000000000000888, -18.58333333333333215, 2.886751345948126879 ) ) ;
#2173 = ORIENTED_EDGE ( 'NONE', *, *, #3151, .F. ) ;
#2174 = CARTESIAN_POINT ( 'NONE',  ( -5.000000000000000000, 5.125000002731184168, 0.000000000000000000 ) ) ;
#2175 = CARTESIAN_POINT ( 'NONE',  ( -52.80376928212989185, -144.1250000013656063, -4.297418129356378458 ) ) ;
#2176 = PRESENTATION_LAYER_ASSIGNMENT (  '', '', ( #34979 ) ) ;
#2177 = CARTESIAN_POINT ( 'NONE',  ( 4.458734125000001214, -83.14583333196773651, 2.574251347313718519 ) ) ;
#2178 = CARTESIAN_POINT ( 'NONE',  ( -51.75738570946856498, -130.8750000027312126, 3.805975901505576964 ) ) ;
#2179 = CARTESIAN_POINT ( 'NONE',  ( 0.000000000000000000, 45.00000000000000000, 0.000000000000000000 ) ) ;
#2180 = CARTESIAN_POINT ( 'NONE',  ( 2.730187237215162345E-16, -143.4375000013656063, -4.458734124999999437 ) ) ;
#2181 = CARTESIAN_POINT ( 'NONE',  ( -2.499999999999996447, 6.291666669397851130, 4.330127018922195425 ) ) ;
#2182 = CARTESIAN_POINT ( 'NONE',  ( 4.458734124999999437, -56.81249999863440081, -5.460374474430324690E-16 ) ) ;
#2183 = CARTESIAN_POINT ( 'NONE',  ( 9.457646018065525792E-16, -47.06249999863440792, 5.148502694627439702 ) ) ;
#2184 = CARTESIAN_POINT ( 'NONE',  ( -3.152548672688508926E-16, 27.43750000136559564, -5.148502694627439702 ) ) ;
#2185 = CARTESIAN_POINT ( 'NONE',  ( 1.060575238724906964E-15, -105.7500000000000000, 5.773502691896257311 ) ) ;
#2186 = CARTESIAN_POINT ( 'NONE',  ( 1.339745962155615144, -3.705341801261480494, 4.999999999999999112 ) ) ;
#2187 = CARTESIAN_POINT ( 'NONE',  ( 4.458734124999999437, -37.06249999863440792, -5.460374474430324690E-16 ) ) ;
#2188 = CARTESIAN_POINT ( 'NONE',  ( -4.999999999999999112, 1.208333336064518759, 2.886751345948131764 ) ) ;
#2189 = CARTESIAN_POINT ( 'NONE',  ( -75.00000000000001421, 15.00000000000000000, -9.000000000000001776 ) ) ;
#2190 = CARTESIAN_POINT ( 'NONE',  ( -57.19623071787017210, -128.3750000013656631, 4.297418129356382899 ) ) ;
#2191 = CARTESIAN_POINT ( 'NONE',  ( 4.458734125000001214, -77.14583333196775072, 2.574251347313718519 ) ) ;
#2192 = CARTESIAN_POINT ( 'NONE',  ( 5.000000000000000000, -71.50000000000000000, -6.123233995736766282E-16 ) ) ;
#2193 = CARTESIAN_POINT ( 'NONE',  ( -2.229367062500000163, -98.47916666530105090, -3.861377020970580443 ) ) ;
#2194 = CARTESIAN_POINT ( 'NONE',  ( -2.229367062500000163, -7.729166665301073991, -3.861377020970580443 ) ) ;
#2195 = VERTEX_POINT ( 'NONE', #36812 ) ;
#2196 = CYLINDRICAL_SURFACE ( 'NONE', #3727, 5.000000000000000000 ) ;
#2197 = CARTESIAN_POINT ( 'NONE',  ( -4.999999999999998224, -85.79166666393547303, 2.886751345948131764 ) ) ;
#2198 = CARTESIAN_POINT ( 'NONE',  ( 2.229367062499998831, -89.64583333196773651, -3.861377020970580887 ) ) ;
#2199 = CARTESIAN_POINT ( 'NONE',  ( 5.000000000000000888, 27.41666666666666430, 2.886751345948126879 ) ) ;
#2200 = CARTESIAN_POINT ( 'NONE',  ( -4.458734124999999437, -88.64583333196773651, -2.574251347313719407 ) ) ;
#2201 = CARTESIAN_POINT ( 'NONE',  ( -2.229367062500000163, 10.27083333469892779, -3.861377020970580443 ) ) ;
#2202 = FACE_OUTER_BOUND ( 'NONE', #31709, .T. ) ;
#2203 = CARTESIAN_POINT ( 'NONE',  ( -54.64476657466781973, -132.8125000013656063, -4.444560631937228834 ) ) ;
#2204 = CARTESIAN_POINT ( 'NONE',  ( -4.458734124999997661, -7.229166665301073103, 2.574251347313722516 ) ) ;
#2205 = CARTESIAN_POINT ( 'NONE',  ( 2.229367062499998831, 16.10416666803225993, -3.861377020970580887 ) ) ;
#2206 = CARTESIAN_POINT ( 'NONE',  ( -3.152548672688508926E-16, -50.81249999863440792, -5.148502694627439702 ) ) ;
#2207 = CARTESIAN_POINT ( 'NONE',  ( -1.339745962155613812, -16.08034179853029499, -5.000000000000000000 ) ) ;
#2208 = CARTESIAN_POINT ( 'NONE',  ( 4.458734125000001214, -86.89583333196773651, 2.574251347313718519 ) ) ;
#2209 = CARTESIAN_POINT ( 'NONE',  ( 2.229367062500001939, -9.979166665301068662, 3.861377020970579999 ) ) ;
#2210 = FACE_OUTER_BOUND ( 'NONE', #52909, .T. ) ;
#2211 = EDGE_LOOP ( 'NONE', ( #28542, #61628, #21308, #51062 ) ) ;
#2212 = CARTESIAN_POINT ( 'NONE',  ( 4.458734125000000326, -38.14583333196773651, 2.574251347313718519 ) ) ;
#2213 = CARTESIAN_POINT ( 'NONE',  ( -56.48576386720575471, -127.0000000013656063, -4.591703134518078322 ) ) ;
#2214 = CARTESIAN_POINT ( 'NONE',  ( 4.458734124999999437, -78.81249999863440792, -5.460374474430324690E-16 ) ) ;
#2215 = CARTESIAN_POINT ( 'NONE',  ( 5.000000000000000888, -108.4583333306021444, 2.886751345948126879 ) ) ;
#2216 = CARTESIAN_POINT ( 'NONE',  ( 2.229367062500001939, 18.02083333469892779, 3.861377020970579999 ) ) ;
#2217 = CARTESIAN_POINT ( 'NONE',  ( 5.000000000000000000, -53.41666666666667140, -2.886751345948130876 ) ) ;
#2218 = CARTESIAN_POINT ( 'NONE',  ( 5.000000000000000000, 1.583333333333332371, -2.886751345948130876 ) ) ;
#2219 = CARTESIAN_POINT ( 'NONE',  ( 9.457646018065525792E-16, -81.31249999863440792, 5.148502694627439702 ) ) ;
#2220 = CARTESIAN_POINT ( 'NONE',  ( -5.000000000000000000, -65.00000000000000000, 0.000000000000000000 ) ) ;
#2221 = CARTESIAN_POINT ( 'NONE',  ( 1.339745962155615144, -63.58034179853028434, 4.999999999999999112 ) ) ;
#2222 = CARTESIAN_POINT ( 'NONE',  ( 5.000000000000000000, 18.62500000273118772, -6.123233995736766282E-16 ) ) ;
#2223 = ORIENTED_EDGE ( 'NONE', *, *, #18261, .T. ) ;
#2224 = CARTESIAN_POINT ( 'NONE',  ( -5.000000000000000000, -66.08333333333332860, -2.886751345948128211 ) ) ;
#2225 = CARTESIAN_POINT ( 'NONE',  ( -6.972266317189433020E-16, 7.750000000000000000, -5.000000000000000000 ) ) ;
#2227 = CARTESIAN_POINT ( 'NONE',  ( 1.060575238724906964E-15, -24.75000000000000355, 5.773502691896257311 ) ) ;
#2226 = CARTESIAN_POINT ( 'NONE',  ( -2.071067811865604735, -149.3125000000000284, 4.999999999999872990 ) ) ;
#2228 = CARTESIAN_POINT ( 'NONE',  ( 4.458734125000001214, -25.89583333196774007, 2.574251347313718519 ) ) ;
#2229 = AXIS2_PLACEMENT_3D ( 'NONE', #52684, #57525, #63602 ) ;
#2230 = CARTESIAN_POINT ( 'NONE',  ( -4.458734124999999437, -87.39583333196773651, -2.574251347313719407 ) ) ;
#2231 = CARTESIAN_POINT ( 'NONE',  ( 1.060575238724906964E-15, -28.62499999726881228, 5.773502691896257311 ) ) ;
#2233 = ORIENTED_EDGE ( 'NONE', *, *, #6777, .F. ) ;
#2232 = CARTESIAN_POINT ( 'NONE',  ( -4.458734124999999437, -55.39583333196773651, -2.574251347313719407 ) ) ;
#2234 = CARTESIAN_POINT ( 'NONE',  ( 2.499999999999998668, -65.33333333333332860, -4.330127018922193649 ) ) ;
#2235 = CARTESIAN_POINT ( 'NONE',  ( 1.339745962155612702, -28.29465819873851729, -5.000000000000000000 ) ) ;
#2237 = ORIENTED_EDGE ( 'NONE', *, *, #6708, .F. ) ;
#2236 = CARTESIAN_POINT ( 'NONE',  ( -3.152548672688508926E-16, -1.812499998634406362, -5.148502694627439702 ) ) ;
#2238 = CARTESIAN_POINT ( 'NONE',  ( -5.000000000000000000, -73.08333333333334281, -2.886751345948128211 ) ) ;
#2239 = CARTESIAN_POINT ( 'NONE',  ( -52.80376928212989185, -138.8750000013656063, -4.297418129356378458 ) ) ;
#2240 = CARTESIAN_POINT ( 'NONE',  ( -4.458734124999998549, -50.47916666530107221, 2.574251347313722516 ) ) ;
#2241 = DIRECTION ( 'NONE',  ( -0.000000000000000000, 1.000000000000000000, -0.000000000000000000 ) ) ;
#2242 = CARTESIAN_POINT ( 'NONE',  ( 5.000000000000000000, -69.29166666393548724, -2.886751345948129988 ) ) ;
#2243 = CARTESIAN_POINT ( 'NONE',  ( -51.75738570946856498, -148.7500000000000284, 3.805975901505576964 ) ) ;
#2244 = CARTESIAN_POINT ( 'NONE',  ( -59.81910112700025905, -154.1875000000000000, -2.462841084822630311 ) ) ;
#2245 = CARTESIAN_POINT ( 'NONE',  ( 4.458734124999999437, -14.06249999863440436, -5.460374474430324690E-16 ) ) ;
#2246 = CARTESIAN_POINT ( 'NONE',  ( 4.458734124999999437, -49.06249999863440792, -5.460374474430324690E-16 ) ) ;
#2247 =( BOUNDED_CURVE ( )  B_SPLINE_CURVE ( 2, ( #54981, #10910, #2547, #1926, #41127, #11859, #41443, #31475, #1606 ),
 .UNSPECIFIED., .F., .F. ) 
 B_SPLINE_CURVE_WITH_KNOTS ( ( 3, 2, 2, 2, 3 ),
 ( 0.7910714285714285365, 0.7916666666666666297, 0.7928571428571428159, 0.7940476190476190022, 0.7946428571428570953 ),
 .UNSPECIFIED. ) 
 CURVE ( )  GEOMETRIC_REPRESENTATION_ITEM ( )  RATIONAL_B_SPLINE_CURVE ( ( 0.9330127018922194093, 0.9330127018922194093, 1.000000000000000000, 0.8660254037844387076, 1.000000000000000000, 0.8660254037844387076, 1.000000000000000000, 0.9330127018922194093, 0.9330127018922194093 ) ) 
 REPRESENTATION_ITEM ( '' )  );
#2248 = CARTESIAN_POINT ( 'NONE',  ( 1.339745962155637349, 10.70534180126147739, -4.999999999999985789 ) ) ;
#2249 = CARTESIAN_POINT ( 'NONE',  ( 4.458734125000000326, -169.6250000013656063, -1.846868145590734978 ) ) ;
#2250 = CARTESIAN_POINT ( 'NONE',  ( 9.457646018065525792E-16, -92.31249999863439371, 5.148502694627439702 ) ) ;
#2251 = CARTESIAN_POINT ( 'NONE',  ( 5.000000000000000000, -158.0000000000000000, 0.000000000000000000 ) ) ;
#2252 = VERTEX_POINT ( 'NONE', #27158 ) ;
#2253 = LINE ( 'NONE', #6744, #62191 ) ;
#2254 = CARTESIAN_POINT ( 'NONE',  ( -2.229367062499996610, 23.60416666803225993, 3.861377020970582219 ) ) ;
#2255 = CARTESIAN_POINT ( 'NONE',  ( -50.18089887299979068, -147.8125000027312126, 2.462841084822635640 ) ) ;
#2256 = DIRECTION ( 'NONE',  ( -0.000000000000000000, 1.000000000000000000, -0.000000000000000000 ) ) ;
#2257 = CARTESIAN_POINT ( 'NONE',  ( 9.457646018065525792E-16, -1.062499998634405696, 5.148502694627439702 ) ) ;
#2258 = CARTESIAN_POINT ( 'NONE',  ( 4.458734125000000326, -97.14583333196773651, 2.574251347313718519 ) ) ;
#2259 =( BOUNDED_CURVE ( )  B_SPLINE_CURVE ( 2, ( #52182, #8127, #46720, #6858, #3306, #7493, #62158, #18077, #26472 ),
 .UNSPECIFIED., .F., .F. ) 
 B_SPLINE_CURVE_WITH_KNOTS ( ( 3, 2, 2, 2, 3 ),
 ( 0.9729166666666666519, 0.9736111111111110938, 0.9749999999999999778, 0.9763888888888888618, 0.9770833333333333037 ),
 .UNSPECIFIED. ) 
 CURVE ( )  GEOMETRIC_REPRESENTATION_ITEM ( )  RATIONAL_B_SPLINE_CURVE ( ( 0.9330127018922194093, 0.9330127018922194093, 1.000000000000000000, 0.8660254037844387076, 1.000000000000000000, 0.8660254037844387076, 1.000000000000000000, 0.9330127018922194093, 0.9330127018922194093 ) ) 
 REPRESENTATION_ITEM ( '' )  );
#2260 = CARTESIAN_POINT ( 'NONE',  ( -3.152801135295367985, -148.0625000013655779, 3.152801135295367096 ) ) ;
#2261 = CARTESIAN_POINT ( 'NONE',  ( 4.458734124999998549, -22.97916666530107221, -2.574251347313721627 ) ) ;
#2262 = CARTESIAN_POINT ( 'NONE',  ( -7.499999999999999112, 0.3744244963005040061, 1.590163186312071526E-15 ) ) ;
#2263 = CARTESIAN_POINT ( 'NONE',  ( -2.229367062500000163, -65.72916666530106511, -3.861377020970580443 ) ) ;
#2264 = CARTESIAN_POINT ( 'NONE',  ( -6.972266317189433020E-16, -72.25000000000000000, -5.000000000000000000 ) ) ;
#2265 = CARTESIAN_POINT ( 'NONE',  ( 1.975475456537005874E-15, 23.37500000273118417, 5.000000000000000000 ) ) ;
#2266 = CARTESIAN_POINT ( 'NONE',  ( -1.846868145590737420, -143.7500000013655779, 4.458734124999997661 ) ) ;
#2267 = CARTESIAN_POINT ( 'NONE',  ( -2.229367062499996610, 15.60416666803225993, 3.861377020970582219 ) ) ;
#2268 = ORIENTED_EDGE ( 'NONE', *, *, #4808, .F. ) ;
#2269 = CARTESIAN_POINT ( 'NONE',  ( -2.499999999999996447, -80.83333333333332860, 4.330127018922195425 ) ) ;
#2270 = CARTESIAN_POINT ( 'NONE',  ( 5.000000000000000888, 16.41666666666666785, 2.886751345948126879 ) ) ;
#2272 = CARTESIAN_POINT ( 'NONE',  ( -4.458734124999999437, -17.31249999863440792, 0.000000000000000000 ) ) ;
#2271 = CARTESIAN_POINT ( 'NONE',  ( 2.499999999999998668, -85.33333333333332860, -4.330127018922193649 ) ) ;
#2273 = ADVANCED_FACE ( 'NONE', ( #17818 ), #37443, .T. ) ;
#2274 = CARTESIAN_POINT ( 'NONE',  ( 4.458734125000000326, 26.85416666803225993, 2.574251347313718519 ) ) ;
#2275 = CARTESIAN_POINT ( 'NONE',  ( -54.64476657466781973, -144.8125000013656063, -4.444560631937228834 ) ) ;
#2276 = CARTESIAN_POINT ( 'NONE',  ( 5.000000000000000000, -48.37499999726880873, -6.123233995736766282E-16 ) ) ;
#2277 = CARTESIAN_POINT ( 'NONE',  ( 5.000000000000000888, -150.0625000027312126, -2.071067811865475505 ) ) ;
#2278 = CARTESIAN_POINT ( 'NONE',  ( -2.229367062500000163, 9.520833334698927786, -3.861377020970580443 ) ) ;
#2279 = CARTESIAN_POINT ( 'NONE',  ( -2.499999999999996447, -62.70833333060214443, 4.330127018922195425 ) ) ;
#2280 = CARTESIAN_POINT ( 'NONE',  ( -58.24261429053147765, -141.3750000027312126, -3.805975901505573855 ) ) ;
#2281 = CARTESIAN_POINT ( 'NONE',  ( -2.229367062500000163, 12.52083333469892601, -3.861377020970580443 ) ) ;
#2282 = CARTESIAN_POINT ( 'NONE',  ( 4.458734124999999437, -65.81249999863440792, -5.460374474430324690E-16 ) ) ;
#2283 = AXIS2_PLACEMENT_3D ( 'NONE', #9713, #54096, #35441 ) ;
#2284 = CARTESIAN_POINT ( 'NONE',  ( -4.458734124999999437, -19.64583333196774362, -2.574251347313719407 ) ) ;
#2285 = CARTESIAN_POINT ( 'NONE',  ( 5.000000000000000000, 1.583333333333332593, -2.886751345948129988 ) ) ;
#2286 = CARTESIAN_POINT ( 'NONE',  ( -3.152801135295367096, -161.0625000013656063, -3.152801135295367541 ) ) ;
#2287 = DIRECTION ( 'NONE',  ( -0.000000000000000000, 1.000000000000000000, -0.000000000000000000 ) ) ;
#2288 = CARTESIAN_POINT ( 'NONE',  ( -4.458734124999998549, -58.22916666530105800, 2.574251347313722516 ) ) ;
#2289 = CARTESIAN_POINT ( 'NONE',  ( -5.000000000000000000, -93.87499999726881583, 0.000000000000000000 ) ) ;
#2290 = CARTESIAN_POINT ( 'NONE',  ( 0.000000000000000000, -170.0000000000000000, 5.000000000000000000 ) ) ;
#2291 = CARTESIAN_POINT ( 'NONE',  ( -5.000000000000000000, -88.87499999726880162, 0.000000000000000000 ) ) ;
#2292 = CARTESIAN_POINT ( 'NONE',  ( -2.229367062500000163, -33.47916666530107221, -3.861377020970580443 ) ) ;
#2293 = CARTESIAN_POINT ( 'NONE',  ( -6.972266317189433020E-16, -60.24999999999999289, -5.000000000000000000 ) ) ;
#2294 = CARTESIAN_POINT ( 'NONE',  ( -5.000000000000000000, -49.00000000000000000, 0.000000000000000000 ) ) ;
#2295 = CARTESIAN_POINT ( 'NONE',  ( -1.339745962155599601, 18.79465819873852084, -5.000000000000007994 ) ) ;
#2296 = CARTESIAN_POINT ( 'NONE',  ( 1.975475456537005874E-15, -36.62499999726880873, 5.000000000000000000 ) ) ;
#2297 = ORIENTED_EDGE ( 'NONE', *, *, #4813, .T. ) ;
#2298 = CARTESIAN_POINT ( 'NONE',  ( -2.229367062500000163, -108.4791666653010651, -3.861377020970580443 ) ) ;
#2299 = CARTESIAN_POINT ( 'NONE',  ( 2.229367062500001939, -0.2291666653010705768, 3.861377020970579999 ) ) ;
#2300 = CARTESIAN_POINT ( 'NONE',  ( -2.499999999999996447, -99.70833333060214443, 4.330127018922195425 ) ) ;
#2301 = CARTESIAN_POINT ( 'NONE',  ( -5.000000000000000000, -10.08333333333333393, -2.886751345948128211 ) ) ;
#2302 = CARTESIAN_POINT ( 'NONE',  ( 4.458734124999998549, -74.72916666530106511, -2.574251347313721627 ) ) ;
#2303 = CARTESIAN_POINT ( 'NONE',  ( 0.000000000000000000, -170.0000000000000000, 0.000000000000000000 ) ) ;
#2304 = CARTESIAN_POINT ( 'NONE',  ( 2.499999999999998668, -7.208333330602150646, -4.330127018922193649 ) ) ;
#2306 = ORIENTED_EDGE ( 'NONE', *, *, #44904, .F. ) ;
#2305 = CARTESIAN_POINT ( 'NONE',  ( 2.229367062500001939, -37.97916666530107221, 3.861377020970579999 ) ) ;
#2308 = ORIENTED_EDGE ( 'NONE', *, *, #9368, .T. ) ;
#2307 = CARTESIAN_POINT ( 'NONE',  ( -2.229367062499996610, 13.60416666803226171, 3.861377020970582219 ) ) ;
#2309 = CARTESIAN_POINT ( 'NONE',  ( 2.499999999999998668, -81.33333333333332860, -4.330127018922193649 ) ) ;
#2310 = CARTESIAN_POINT ( 'NONE',  ( 2.500000000000002220, -54.66666666666667140, 4.330127018922192761 ) ) ;
#2311 = CARTESIAN_POINT ( 'NONE',  ( 3.152801135295367541, -159.5625000013656063, -3.152801135295367541 ) ) ;
#2312 = CARTESIAN_POINT ( 'NONE',  ( 9.457646018065525792E-16, -31.31249999863440436, 5.148502694627439702 ) ) ;
#2313 = CARTESIAN_POINT ( 'NONE',  ( 2.229367062499998831, -78.64583333196773651, -3.861377020970580887 ) ) ;
#2314 =( BOUNDED_CURVE ( )  B_SPLINE_CURVE ( 2, ( #47785, #3742, #23363, #32049, #7626, #12437, #37513, #42962, #27854 ),
 .UNSPECIFIED., .F., .F. ) 
 B_SPLINE_CURVE_WITH_KNOTS ( ( 3, 2, 2, 2, 3 ),
 ( 0.3416666666666669516, 0.3458333333333336035, 0.3500000000000002554, 0.3541666666666669627, 0.3583333333333336146 ),
 .UNSPECIFIED. ) 
 CURVE ( )  GEOMETRIC_REPRESENTATION_ITEM ( )  RATIONAL_B_SPLINE_CURVE ( ( 0.9999999999999948930, 0.9238795325112918455, 1.000000000000000000, 0.9238795325112867385, 1.000000000000000000, 0.9238795325112867385, 1.000000000000000000, 0.9238795325112816315, 1.000000000000005107 ) ) 
 REPRESENTATION_ITEM ( '' )  );
#2315 = CARTESIAN_POINT ( 'NONE',  ( 4.458734124999999437, -141.6875000013656063, 0.000000000000000000 ) ) ;
#2316 = CARTESIAN_POINT ( 'NONE',  ( 4.458734124999998549, -85.72916666530106511, -2.574251347313721627 ) ) ;
#2317 = CARTESIAN_POINT ( 'NONE',  ( -57.19623071787017210, -134.6250000013656347, 4.297418129356382899 ) ) ;
#2318 = CARTESIAN_POINT ( 'NONE',  ( 4.458734124999998549, -34.97916666530107221, -2.574251347313721627 ) ) ;
#2319 = CARTESIAN_POINT ( 'NONE',  ( -4.458734124999999437, -77.56249999863440792, 0.000000000000000000 ) ) ;
#2320 = CARTESIAN_POINT ( 'NONE',  ( 2.499999999999998668, -86.33333333333332860, -4.330127018922193649 ) ) ;
#2321 = EDGE_LOOP ( 'NONE', ( #44063, #41136, #26482, #32285 ) ) ;
#2322 = DIRECTION ( 'NONE',  ( -0.000000000000000000, 1.000000000000000000, -0.000000000000000000 ) ) ;
#2323 = CARTESIAN_POINT ( 'NONE',  ( -4.458734124999999437, -65.56249999863440792, 0.000000000000000000 ) ) ;
#2324 = CARTESIAN_POINT ( 'NONE',  ( -3.152548672688508926E-16, -8.812499998634406140, -5.148502694627439702 ) ) ;
#2325 = VERTEX_POINT ( 'NONE', #3356 ) ;
#2326 = DIRECTION ( 'NONE',  ( 0.000000000000000000, 0.000000000000000000, 1.000000000000000000 ) ) ;
#2327 = CARTESIAN_POINT ( 'NONE',  ( -2.499999999999996447, -92.70833333060214443, 4.330127018922195425 ) ) ;
#2328 = CARTESIAN_POINT ( 'NONE',  ( -4.458734124999999437, -8.562499998634406140, 0.000000000000000000 ) ) ;
#2329 = CARTESIAN_POINT ( 'NONE',  ( -6.972266317189433020E-16, 2.750000000000000000, -5.000000000000000000 ) ) ;
#2330 = CARTESIAN_POINT ( 'NONE',  ( 4.458734124999999437, 9.187500001365592084, -5.460374474430324690E-16 ) ) ;
#2331 = CARTESIAN_POINT ( 'NONE',  ( 2.071067811865645591, -154.1874999999999716, 4.999999999999830358 ) ) ;
#2332 = CARTESIAN_POINT ( 'NONE',  ( -4.458734124999999437, -156.0000000013656063, -1.846868145590735644 ) ) ;
#2333 =( BOUNDED_CURVE ( )  B_SPLINE_CURVE ( 2, ( #55407, #45107, #30628, #45749, #7157, #50250, #40911, #26767, #1703 ),
 .UNSPECIFIED., .F., .F. ) 
 B_SPLINE_CURVE_WITH_KNOTS ( ( 3, 2, 2, 2, 3 ),
 ( 0.08125000000000000278, 0.08194444444444444475, 0.08333333333333332871, 0.08472222222222222654, 0.08541666666666666852 ),
 .UNSPECIFIED. ) 
 CURVE ( )  GEOMETRIC_REPRESENTATION_ITEM ( )  RATIONAL_B_SPLINE_CURVE ( ( 0.9330127018922194093, 0.9330127018922194093, 1.000000000000000000, 0.8660254037844387076, 1.000000000000000000, 0.8660254037844387076, 1.000000000000000000, 0.9330127018922194093, 0.9330127018922194093 ) ) 
 REPRESENTATION_ITEM ( '' )  );
#2334 = CYLINDRICAL_SURFACE ( 'NONE', #24456, 5.000000000000000000 ) ;
#2335 = ORIENTED_EDGE ( 'NONE', *, *, #44341, .T. ) ;
#2336 = CARTESIAN_POINT ( 'NONE',  ( 4.458734124999998549, -87.72916666530107932, -2.574251347313721627 ) ) ;
#2337 = CARTESIAN_POINT ( 'NONE',  ( 0.000000000000000000, -120.0000000000000000, 0.000000000000000000 ) ) ;
#2338 = CARTESIAN_POINT ( 'NONE',  ( -2.229367062499996610, -1.145833331967736957, 3.861377020970582219 ) ) ;
#2339 = EDGE_CURVE ( 'NONE', #12432, #15117, #26524, .T. ) ;
#2340 = CARTESIAN_POINT ( 'NONE',  ( 6.902527771671632451, 4.675077770780898589, -0.7026937717022819774 ) ) ;
#2341 = CARTESIAN_POINT ( 'NONE',  ( 5.000000000000000888, -29.45833333060214798, 2.886751345948126879 ) ) ;
#2342 = CARTESIAN_POINT ( 'NONE',  ( 1.975475456537005874E-15, -78.74999999999998579, 5.000000000000000000 ) ) ;
#2343 = CARTESIAN_POINT ( 'NONE',  ( 2.229367062500001939, 23.02083333469892423, 3.861377020970579999 ) ) ;
#2344 = CARTESIAN_POINT ( 'NONE',  ( 2.500000000000002220, -10.66666666666666430, 4.330127018922192761 ) ) ;
#2345 = CARTESIAN_POINT ( 'NONE',  ( -2.229367062499996610, 27.85416666803225993, 3.861377020970582219 ) ) ;
#2346 = CARTESIAN_POINT ( 'NONE',  ( 4.458734125000001214, -49.89583333196772941, 2.574251347313718519 ) ) ;
#2347 = CARTESIAN_POINT ( 'NONE',  ( -4.458734124999997661, -39.47916666530106511, 2.574251347313722516 ) ) ;
#2348 = CARTESIAN_POINT ( 'NONE',  ( -2.229367062500000163, -0.7291666653010709931, -3.861377020970580443 ) ) ;
#2349 = CARTESIAN_POINT ( 'NONE',  ( -5.000000000000000000, -18.00000000000000355, 0.000000000000000000 ) ) ;
#2350 = CARTESIAN_POINT ( 'NONE',  ( 5.000000000000000888, 15.41666666666666607, 2.886751345948126879 ) ) ;
#2351 = CARTESIAN_POINT ( 'NONE',  ( -2.071067811865478170, -141.4375000027312410, 5.000000000000000000 ) ) ;
#2353 = EDGE_CURVE ( 'NONE', #27072, #23020, #12987, .T. ) ;
#2352 = DIRECTION ( 'NONE',  ( -0.000000000000000000, 1.000000000000000000, -0.000000000000000000 ) ) ;
#2354 = CARTESIAN_POINT ( 'NONE',  ( -3.152548672688508926E-16, -43.56249999863440081, -5.148502694627439702 ) ) ;
#2355 = CARTESIAN_POINT ( 'NONE',  ( -5.000000000000000000, -77.95833333060214443, -2.886751345948128211 ) ) ;
#2356 = CARTESIAN_POINT ( 'NONE',  ( -57.89159099828107458, -140.9375000013656063, -3.393966926194107447 ) ) ;
#2357 = CARTESIAN_POINT ( 'NONE',  ( 1.339745962155615144, -65.58034179853029855, 4.999999999999999112 ) ) ;
#2358 = CARTESIAN_POINT ( 'NONE',  ( -1.339745962155610925, -63.66965819600734022, 5.000000000000000000 ) ) ;
#2359 = ADVANCED_FACE ( 'NONE', ( #20525 ), #50429, .T. ) ;
#2360 = CARTESIAN_POINT ( 'NONE',  ( 9.457646018065525792E-16, -84.31249999863440792, 5.148502694627439702 ) ) ;
#2361 = CARTESIAN_POINT ( 'NONE',  ( 2.730187237215162345E-16, -161.4375000013655779, -4.458734124999999437 ) ) ;
#2362 = CARTESIAN_POINT ( 'NONE',  ( -6.972266317189433020E-16, -64.24999999999998579, -5.000000000000000000 ) ) ;
#2363 = CARTESIAN_POINT ( 'NONE',  ( 2.499999999999998668, -34.33333333333332860, -4.330127018922193649 ) ) ;
#2364 = CARTESIAN_POINT ( 'NONE',  ( 1.846868145590735200, -141.2500000013656063, -4.458734125000000326 ) ) ;
#2365 = ORIENTED_EDGE ( 'NONE', *, *, #42129, .T. ) ;
#2366 = CARTESIAN_POINT ( 'NONE',  ( 4.458734124999998549, 21.02083333469892779, -2.574251347313721627 ) ) ;
#2367 = VERTEX_POINT ( 'NONE', #20840 ) ;
#2368 = CARTESIAN_POINT ( 'NONE',  ( 4.458734125000001214, -90.89583333196772230, 2.574251347313718519 ) ) ;
#2369 = CARTESIAN_POINT ( 'NONE',  ( -3.152548672688508926E-16, 12.18750000136559564, -5.148502694627439702 ) ) ;
#2370 = CARTESIAN_POINT ( 'NONE',  ( -4.999999999999999112, 14.20833333606451809, 2.886751345948131764 ) ) ;
#2371 = CARTESIAN_POINT ( 'NONE',  ( -2.500000000000000444, -44.04166666393546592, -4.330127018922193649 ) ) ;
#2372 = CARTESIAN_POINT ( 'NONE',  ( 2.500000000000002220, 6.333333333333333037, 4.330127018922192761 ) ) ;
#2373 = CARTESIAN_POINT ( 'NONE',  ( 4.458734125000000326, -56.89583333196774362, 2.574251347313718519 ) ) ;
#2374 = CARTESIAN_POINT ( 'NONE',  ( -6.972266317189433020E-16, -89.24999999999998579, -5.000000000000000000 ) ) ;
#2375 = CARTESIAN_POINT ( 'NONE',  ( -5.000000000000000000, -52.00000000000000711, 0.000000000000000000 ) ) ;
#2376 = DIRECTION ( 'NONE',  ( 0.000000000000000000, 0.000000000000000000, 1.000000000000000000 ) ) ;
#2377 = CARTESIAN_POINT ( 'NONE',  ( -1.339745962155610925, -36.79465819873852439, 5.000000000000000000 ) ) ;
#2378 = CARTESIAN_POINT ( 'NONE',  ( 2.499999999999998668, -109.3333333333333428, -4.330127018922193649 ) ) ;
#2379 = CARTESIAN_POINT ( 'NONE',  ( -3.535250795749689387E-16, -39.24999999999999289, -5.773502691896257311 ) ) ;
#2380 = CARTESIAN_POINT ( 'NONE',  ( -9.184850993605147944E-16, -163.2500000000000000, 5.000000000000000000 ) ) ;
#2382 = CARTESIAN_POINT ( 'NONE',  ( 9.457646018065525792E-16, -16.31249999863440436, 5.148502694627439702 ) ) ;
#2381 = CARTESIAN_POINT ( 'NONE',  ( -2.500000000000000444, -43.16666666666665719, -4.330127018922193649 ) ) ;
#2383 = CARTESIAN_POINT ( 'NONE',  ( -6.972266317189433020E-16, 12.75000000000000178, -5.000000000000000000 ) ) ;
#2384 = CARTESIAN_POINT ( 'NONE',  ( 2.229367062499998831, -57.64583333196773651, -3.861377020970580887 ) ) ;
#2385 = CARTESIAN_POINT ( 'NONE',  ( -3.152801135295367985, -152.0625000013655779, 3.152801135295367096 ) ) ;
#2386 = CARTESIAN_POINT ( 'NONE',  ( -4.458734124999999437, -73.39583333196773651, -2.574251347313719407 ) ) ;
#2387 = CARTESIAN_POINT ( 'NONE',  ( -58.39396692619412477, -148.6875000013656063, 2.891590998281057701 ) ) ;
#2388 = CARTESIAN_POINT ( 'NONE',  ( 4.458734124999999437, -19.06249999863440792, -5.460374474430324690E-16 ) ) ;
#2389 = CARTESIAN_POINT ( 'NONE',  ( 1.060575238724906964E-15, -59.62499999726880873, 5.773502691896257311 ) ) ;
#2390 = ORIENTED_EDGE ( 'NONE', *, *, #52798, .F. ) ;
#2391 = CARTESIAN_POINT ( 'NONE',  ( -9.184850993605147944E-16, -150.2500000000000284, 5.000000000000000000 ) ) ;
#2392 = VERTEX_POINT ( 'NONE', #53967 ) ;
#2393 = CARTESIAN_POINT ( 'NONE',  ( 4.458734124999998549, -63.97916666530107221, -2.574251347313721627 ) ) ;
#2394 = DIRECTION ( 'NONE',  ( 0.000000000000000000, 1.000000000000000000, 0.000000000000000000 ) ) ;
#2395 = CARTESIAN_POINT ( 'NONE',  ( 4.458734125000000326, -151.3750000013656063, -1.846868145590734978 ) ) ;
#2396 = ORIENTED_EDGE ( 'NONE', *, *, #23242, .T. ) ;
#2397 = CARTESIAN_POINT ( 'NONE',  ( 5.000000000000000888, 25.41666666666666430, 2.886751345948126879 ) ) ;
#2398 = CARTESIAN_POINT ( 'NONE',  ( -59.98410592259440222, -126.1250000000000142, -0.3983568153799752487 ) ) ;
#2399 = CARTESIAN_POINT ( 'NONE',  ( -1.339745962155610925, -77.66965819600730470, 5.000000000000000000 ) ) ;
#2400 = CARTESIAN_POINT ( 'NONE',  ( 4.458734124999998549, -46.97916666530106511, -2.574251347313721627 ) ) ;
#2401 = ORIENTED_EDGE ( 'NONE', *, *, #36542, .T. ) ;
#2402 = CARTESIAN_POINT ( 'NONE',  ( 4.458734124999999437, 8.187500001365595637, -5.460374474430324690E-16 ) ) ;
#2403 = CARTESIAN_POINT ( 'NONE',  ( -4.458734124999998549, 23.77083333469892423, 2.574251347313722516 ) ) ;
#2404 = CARTESIAN_POINT ( 'NONE',  ( -59.29741812935640155, -148.6250000013656063, -2.196230717870135685 ) ) ;
#2405 = CARTESIAN_POINT ( 'NONE',  ( -1.846868145590734756, -167.1250000013656063, -4.458734124999999437 ) ) ;
#2406 = ORIENTED_EDGE ( 'NONE', *, *, #12488, .F. ) ;
#2407 = CARTESIAN_POINT ( 'NONE',  ( 2.229367062499998831, -70.64583333196773651, -3.861377020970580887 ) ) ;
#2408 = CARTESIAN_POINT ( 'NONE',  ( 2.229367062499998831, 12.35416666803226171, -3.861377020970580887 ) ) ;
#2409 =( BOUNDED_CURVE ( )  B_SPLINE_CURVE ( 2, ( #60001, #11092, #55497, #10139, #59678, #19788, #50339, #25575, #24940 ),
 .UNSPECIFIED., .F., .F. ) 
 B_SPLINE_CURVE_WITH_KNOTS ( ( 3, 2, 2, 2, 3 ),
 ( 0.3875000000000000111, 0.3880952380952381042, 0.3892857142857142905, 0.3904761904761904767, 0.3910714285714285698 ),
 .UNSPECIFIED. ) 
 CURVE ( )  GEOMETRIC_REPRESENTATION_ITEM ( )  RATIONAL_B_SPLINE_CURVE ( ( 0.9330127018922194093, 0.9330127018922194093, 1.000000000000000000, 0.8660254037844387076, 1.000000000000000000, 0.8660254037844387076, 1.000000000000000000, 0.9330127018922194093, 0.9330127018922194093 ) ) 
 REPRESENTATION_ITEM ( '' )  );
#2410 = CARTESIAN_POINT ( 'NONE',  ( 1.975475456537005874E-15, -69.62499999726880162, 5.000000000000000000 ) ) ;
#2411 = ADVANCED_FACE ( 'NONE', ( #60084 ), #30472, .T. ) ;
#2412 = CARTESIAN_POINT ( 'NONE',  ( -5.000000000000000000, -42.08333333333333570, -2.886751345948128211 ) ) ;
#2413 = EDGE_CURVE ( 'NONE', #58748, #60011, #44630, .T. ) ;
#2414 = CARTESIAN_POINT ( 'NONE',  ( -4.458734124999998549, -54.47916666530107932, 2.574251347313722516 ) ) ;
#2415 = CARTESIAN_POINT ( 'NONE',  ( -2.499999999999996447, -14.70833333060214976, 4.330127018922195425 ) ) ;
#2416 = CARTESIAN_POINT ( 'NONE',  ( -1.339745962155613812, -100.2053418012614685, -5.000000000000000000 ) ) ;
#2417 = CARTESIAN_POINT ( 'NONE',  ( 1.339745962155612702, -45.29465819873851729, -5.000000000000000000 ) ) ;
#2418 = EDGE_CURVE ( 'NONE', #23656, #50923, #19369, .T. ) ;
#2419 = DIRECTION ( 'NONE',  ( -1.000000000000000000, -0.000000000000000000, -0.000000000000000000 ) ) ;
#2420 = CARTESIAN_POINT ( 'NONE',  ( -4.458734124999999437, -19.64583333196774362, -2.574251347313719407 ) ) ;
#2421 = ORIENTED_EDGE ( 'NONE', *, *, #48347, .F. ) ;
#2422 = CARTESIAN_POINT ( 'NONE',  ( -4.999999999999998224, -101.9166666666666572, 2.886751345948131764 ) ) ;
#2423 = CARTESIAN_POINT ( 'NONE',  ( 4.458734125000001214, -106.8958333319677649, 2.574251347313718519 ) ) ;
#2424 = CARTESIAN_POINT ( 'NONE',  ( -5.000000000000000888, -157.5625000027311842, 2.071067811865474617 ) ) ;
#2425 = VERTEX_POINT ( 'NONE', #30148 ) ;
#2426 = CARTESIAN_POINT ( 'NONE',  ( 2.229367062500001939, -102.2291666653010651, 3.861377020970579999 ) ) ;
#2427 = CARTESIAN_POINT ( 'NONE',  ( -2.229367062500000163, -26.47916666530106866, -3.861377020970580443 ) ) ;
#2428 = CARTESIAN_POINT ( 'NONE',  ( 2.499999999999998668, -65.20833333060213022, -4.330127018922193649 ) ) ;
#2429 = EDGE_CURVE ( 'NONE', #8193, #59584, #22402, .T. ) ;
#2430 = CARTESIAN_POINT ( 'NONE',  ( -58.39396692619412477, -153.6875000013656063, 2.891590998281057701 ) ) ;
#2431 =( BOUNDED_SURFACE ( )  B_SPLINE_SURFACE ( 1, 2, ( 
 ( #33164, #56669, #12587, #31891, #32200, #8091, #7769, #8706, #32842, #52778, #12897, #52470, #7460, #32519, #52149, #37662, #57303, #8406, #28007, #47625, #3581, #23188, #18359, #37984, #28634, #33782, #10289, #29894, #39543, #4826, #5146, #58226, #49524, #24446, #9331, #53399, #48569, #44049, #24766, #5465, #53088, #4509, #59181, #15115, #24135, #34399, #13844, #34732, #54359, #63381, #9024, #19617, #25081, #44690, #651, #33464, #28944, #48251, #4207, #43738, #20263, #57926, #23820, #16, #44370, #14155, #43424, #39229, #19296, #38914, #58548, #58853, #331, #63068, #18980, #14470, #38593, #34090, #53714, #9646, #29576, #14784, #29255, #48880, #54027, #9963, #49207, #19931, #26354, #36014, #25402, #10598, #20905, #15443, #16071, #41139, #6114, #11560, #30865, #49838, #30538, #2255, #35062, #11870, #25729, #35699, #54994, #21216, #60787, #26045, #6746, #10920, #40508, #31486, #60150, #5781, #45660, #54674, #50159, #46298, #55326, #30213, #50494, #45976, #39862, #51131, #45340, #55646, #35371, #6434, #16395, #45021, #16712, #988, #20591, #11241, #36328, #40197, #7066, #1309, #1617, #40824, #1941, #59833, #60470, #31179, #50809, #21543, #15755, #55956, #26679, #59506, #42404, #47250, #2559, #36642, #26994, #47552, #32446, #3502, #41771, #27620, #42720, #46613, #22173, #37910, #61420, #17663, #31813, #18286, #22812, #17344, #57541, #3196, #22496, #12513, #36963, #28245, #32124, #56593, #51760, #56907, #7387, #47859, #7704, #23116, #13467, #33085, #56274, #62363, #52699, #8016, #27307, #8633, #12197, #46932, #62047, #21859, #17963, #37279, #41454, #2882, #61103, #17028, #42092, #51448, #61734, #12826, #37586, #52075, #57227, #13146, #32766, #52397, #8332, #27931, #18905, #28873, #48180, #53638, #48804, #58147, #23440, #4743, #34016, #63616, #34325, #53325, #9881, #19853, #9571, #10211, #57851, #59104, #53950, #48495, #18603, #14394, #29178, #38229, #39467, #19215, #14076, #8945, #19537, #24368, #15031, #29487, #4432, #24059, #49123, #43970, #38832, #13769, #43656, #39151, #33705, #34647, #63297, #33391, #58776, #14706, #58469, #255, #5065, #9258, #54271, #53006, #23754, #24685, #44293, #29814, #28559, #3817, #43041, #62681, #4132, #43349, #62995, #38519, #49761, #55564, #5388, #50720, #54913, #26271, #6664, #49446, #45893, #40106, #60065, #25003, #6355, #30132, #41061, #16315, #25643, #20182, #20824, #55240, #21137, #44613, #25959, #1855, #21461, #45576, #11162, #5707, #573, #54596, #11479, #15989, #31099, #25322, #30784, #60708, #10518, #44942, #16628, #900, #45259, #59427, #36249, #50407, #55876, #15674, #1532, #39780, #11788, #15356, #10840, #34981, #40742, #20507, #59749, #35293, #30456, #50081, #6038, #1225, #40425, #35614, #60389, #35936, #42014, #42330, #31738, #47473, #61654, #46538, #7309, #22092, #17588, #61970, #42646, #26599, #41691, #13066, #61338, #26922, #17261, #3114, #37205, #41375, #2479, #36884, #46215, #32686, #12435, #17891, #27539, #16947, #2178, #32047, #6987, #7624, #52317, #56514, #22732, #22415, #61021, #51683, #57464, #21783, #3427, #27228, #46849, #2796, #12749, #8252, #56831, #37511, #32369, #51993, #23043, #7937, #36560, #47171, #56191, #57151, #37830, #27852, #12111, #62287, #18209, #31406, #51044, #51368, #29096, #8869, #4355, #53560, #62603, #53871, #8555, #28168, #48411, #9798, #3740, #24607, #43270, #14001, #48100, #19459, #47783, #23975, #19135, #34242, #28484, #38442, #57771, #63220, #58391, #4054, #33004, #14317, #43577, #9485, #43888, #62910, #39073, #29406, #38752, #19778, #23361, #4984, #63536, #58069, #42960, #33939, #48723, #18526, #49039, #28795, #23672, #38146, #4663, #24285, #44213, #58701, #33628, #53247, #14629, #178, #39386, #13693, #9183, #13383, #18823, #52621, #33312, #52932, #25562, #1145, #40024, #55484, #20745, #49685, #31018, #24928, #15273 ),
 ( #60311, #819, #35858, #16239, #59017, #11400, #5630, #5952, #34558, #15914, #39702, #50646, #25881, #35217, #29734, #30378, #59342, #6584, #40349, #59668, #25241, #54519, #1781, #44856, #493, #20424, #50001, #44536, #21381, #15599, #40667, #26199, #45819, #49366, #21062, #14948, #45179, #10442, #54189, #5310, #30056, #59991, #10127, #35535, #10767, #20096, #34897, #54837, #55163, #11082, #30704, #50329, #6275, #45497, #1461, #36486, #36810, #56754, #3041, #55797, #17514, #41298, #47093, #60632, #42257, #46460, #17816, #61898, #40988, #37441, #31661, #51611, #16552, #61579, #21706, #32609, #7858, #17184, #11714, #12362, #60947, #57072, #46772, #41610, #51297, #56112, #47403, #7233, #46139, #26847, #31976, #26521, #3354, #2404, #22659, #52235, #12984, #31332, #8177, #27779, #27156, #12036, #36176, #50967, #22016, #22340, #6910, #2718, #56440, #2105, #16868, #61260, #7544, #41938, #37134, #12677, #32291, #51917, #27464, #18447, #18751, #38678, #48648, #37754, #43819, #38070, #48027, #3667, #9108, #4285, #13624, #42571, #23904, #53174, #19060, #53485, #8795, #29024, #39000, #28715, #29331, #13307, #14552, #9413, #3977, #57386, #33553, #48338, #32930, #58632, #38375, #33242, #28094, #58317, #43504, #34171, #4590, #23597, #43194, #24213, #63149, #58002, #52553, #62836, #14242, #52862, #53794, #13928, #8485, #33865, #63465, #19384, #9728, #48961, #28407, #22971, #47712, #42883, #62211, #18127, #23280, #62528, #57698, #55081, #4913, #5550, #40592, #39946, #12207, #58940, #61111, #35460, #49611, #19702, #15527, #54763, #39312, #20989, #20347, #15197, #10050, #20675, #10691, #17036, #30625, #29982, #25162, #11003, #49921, #59594, #14869, #44776, #30301, #59265, #36651, #738, #34478, #35147, #5874, #25482, #1388, #45103, #34822, #56281, #54110, #24854, #54445, #1068, #40281, #29663, #59920, #50247, #24533, #15841, #31825, #6195, #25810, #5234, #45423, #44136, #106, #10373, #49294, #44458, #418, #20021, #39627, #62056, #27001, #8339, #32131, #43049, #18295, #27629, #22180, #22823, #51767, #3826, #57237, #52085, #42098, #46943, #57858, #61744, #56603, #17672, #42413, #36975, #13779, #37286, #33092, #62689, #23446, #41783, #13476, #18610, #37593, #2891, #8641, #61428, #22503, #32773, #38238, #13153, #3203, #51457, #12520, #7394, #46620, #7711, #17351, #2566, #27315, #52408, #52707, #56915, #47258, #3512, #28254, #12833, #47867, #32453, #8023, #17969, #27938, #47562, #23123, #42727, #62372, #37918, #57548, #268, #19229, #39480, #49460, #63629, #58479, #14089, #19549, #14718, #24070, #53016, #34338, #39163, #29503, #19866, #38845, #59116, #5400, #58788, #39795, #23761, #25016, #15045, #14405, #48188, #43982, #53962, #4141, #44626, #48815, #43666, #38528, #49135, #9894, #585, #34664, #34027, #53648, #54283, #5078, #4753, #43358, #9582, #24700, #63307, #20193, #29188, #63005, #44304, #10221, #24381, #29827, #59441, #33401, #8957, #18914, #53333, #28567, #58156, #33714, #9267, #28882, #48503, #4440, #16003, #51057, #50425, #55577, #15687, #21473, #34993, #16641, #20837, #55889, #36263, #15370, #11803, #6050, #25973, #54608, #35949, #59761, #7001, #45907, #55255, #49773, #6368, #35307, #31418, #21151, #35627, #25658, #10853, #21794, #45271, #20521, #1237, #45589, #916, #41389, #40439, #60718, #26610, #46227, #5719, #41072, #2190, #1547, #30468, #10532, #25334, #50096, #60404, #30144, #40755, #30797, #44956, #40120, #54927, #60081, #11174, #16329, #11495, #31111, #50733, #6677, #26284, #1869, #13079, #23054, #12126, #18220, #12447, #41702, #52634, #27866, #37217, #31749, #32383, #61350, #13395, #3125, #61668, #51695, #56527, #3752, #7636, #2493, #27241, #52008, #46550, #23374, #46865, #42659, #8568, #33018, #51381, #62298, #28179, #47183, #32059, #37846, #7323, #2809, #42343, #47795, #22746, #12760, #61037, #22109 ) ),
 .UNSPECIFIED., .F., .F., .F. ) 
 B_SPLINE_SURFACE_WITH_KNOTS ( ( 2, 2 ),
 ( 3, 2, 2, 2, 2, 2, 2, 2, 2, 2, 2, 2, 2, 2, 2, 2, 2, 2, 2, 2, 2, 2, 2, 2, 2, 2, 2, 2, 2, 2, 2, 2, 2, 2, 2, 2, 2, 2, 2, 2, 2, 2, 2, 2, 2, 2, 2, 2, 2, 2, 2, 2, 2, 2, 2, 2, 2, 2, 2, 2, 2, 2, 2, 2, 2, 2, 2, 2, 2, 2, 2, 2, 2, 2, 2, 2, 2, 2, 2, 2, 2, 2, 2, 2, 2, 2, 2, 2, 2, 2, 2, 2, 2, 2, 2, 2, 2, 2, 2, 2, 2, 2, 2, 2, 2, 2, 2, 2, 2, 2, 2, 2, 2, 2, 2, 2, 2, 2, 2, 2, 2, 2, 2, 2, 2, 2, 2, 2, 2, 2, 2, 2, 2, 2, 2, 2, 2, 2, 2, 2, 2, 2, 2, 2, 2, 2, 2, 2, 2, 2, 2, 2, 2, 2, 2, 2, 2, 2, 2, 2, 2, 2, 2, 2, 2, 2, 2, 2, 2, 2, 2, 2, 2, 2, 2, 2, 2, 2, 2, 2, 2, 2, 2, 2, 2, 2, 2, 2, 2, 2, 2, 2, 2, 2, 2, 2, 2, 2, 2, 2, 2, 2, 2, 2, 2, 2, 2, 2, 2, 2, 2, 2, 2, 2, 2, 2, 2, 2, 2, 2, 2, 2, 2, 2, 2, 2, 2, 2, 2, 2, 2, 2, 2, 2, 2, 2, 2, 2, 2, 2, 3 ),
 ( 0.000000000000000000, 1.000000000000000000 ),
 ( 0.000000000000000000, 0.004166666666666666609, 0.008333333333333333218, 0.01250000000000000069, 0.01666666666666666644, 0.02083333333333333218, 0.02500000000000000139, 0.02916666666666666713, 0.03333333333333333287, 0.03749999999999999861, 0.04166666666666666435, 0.04583333333333333010, 0.05000000000000000278, 0.05416666666666666852, 0.05833333333333333426, 0.06250000000000000000, 0.06666666666666666574, 0.07083333333333333148, 0.07499999999999999722, 0.07916666666666666297, 0.08333333333333332871, 0.08749999999999999445, 0.09166666666666666019, 0.09583333333333333981, 0.1000000000000000056, 0.1041666666666666713, 0.1083333333333333370, 0.1125000000000000028, 0.1166666666666666685, 0.1208333333333333343, 0.1250000000000000000, 0.1291666666666666796, 0.1333333333333333315, 0.1375000000000000111, 0.1416666666666666630, 0.1458333333333333426, 0.1499999999999999944, 0.1541666666666666741, 0.1583333333333333259, 0.1625000000000000056, 0.1666666666666666574, 0.1708333333333333370, 0.1749999999999999889, 0.1791666666666666685, 0.1833333333333333204, 0.1875000000000000000, 0.1916666666666666796, 0.1958333333333333315, 0.2000000000000000111, 0.2041666666666666630, 0.2083333333333333426, 0.2124999999999999944, 0.2166666666666666741, 0.2208333333333333259, 0.2250000000000000056, 0.2291666666666666574, 0.2333333333333333370, 0.2374999999999999889, 0.2416666666666666685, 0.2458333333333333204, 0.2500000000000000000, 0.2541666666666666519, 0.2583333333333333592, 0.2625000000000000111, 0.2666666666666666630, 0.2708333333333333148, 0.2750000000000000222, 0.2791666666666666741, 0.2833333333333333259, 0.2874999999999999778, 0.2916666666666666852, 0.2958333333333333370, 0.2999999999999999889, 0.3041666666666666408, 0.3083333333333333481, 0.3125000000000000000, 0.3166666666666666519, 0.3208333333333333592, 0.3250000000000000111, 0.3291666666666666630, 0.3333333333333333148, 0.3375000000000000222, 0.3416666666666666741, 0.3458333333333333259, 0.3499999999999999778, 0.3541666666666666852, 0.3583333333333333370, 0.3624999999999999889, 0.3666666666666666408, 0.3708333333333333481, 0.3750000000000000000, 0.3791666666666666519, 0.3833333333333333592, 0.3875000000000000111, 0.3916666666666666630, 0.3958333333333333148, 0.4000000000000000222, 0.4041666666666666741, 0.4083333333333333259, 0.4124999999999999778, 0.4166666666666666852, 0.4208333333333333370, 0.4249999999999999889, 0.4291666666666666408, 0.4333333333333333481, 0.4375000000000000000, 0.4416666666666666519, 0.4458333333333333592, 0.4500000000000000111, 0.4541666666666666630, 0.4583333333333333148, 0.4625000000000000222, 0.4666666666666666741, 0.4708333333333333259, 0.4749999999999999778, 0.4791666666666666852, 0.4833333333333333370, 0.4874999999999999889, 0.4916666666666666408, 0.4958333333333333481, 0.5000000000000000000, 0.5041666666666666519, 0.5083333333333333037, 0.5124999999999999556, 0.5166666666666667185, 0.5208333333333333703, 0.5250000000000000222, 0.5291666666666666741, 0.5333333333333333259, 0.5374999999999999778, 0.5416666666666666297, 0.5458333333333332815, 0.5500000000000000444, 0.5541666666666666963, 0.5583333333333333481, 0.5625000000000000000, 0.5666666666666666519, 0.5708333333333333037, 0.5749999999999999556, 0.5791666666666667185, 0.5833333333333333703, 0.5875000000000000222, 0.5916666666666666741, 0.5958333333333333259, 0.5999999999999999778, 0.6041666666666666297, 0.6083333333333332815, 0.6125000000000000444, 0.6166666666666666963, 0.6208333333333333481, 0.6250000000000000000, 0.6291666666666666519, 0.6333333333333333037, 0.6374999999999999556, 0.6416666666666667185, 0.6458333333333333703, 0.6500000000000000222, 0.6541666666666666741, 0.6583333333333333259, 0.6624999999999999778, 0.6666666666666666297, 0.6708333333333332815, 0.6750000000000000444, 0.6791666666666666963, 0.6833333333333333481, 0.6875000000000000000, 0.6916666666666666519, 0.6958333333333333037, 0.6999999999999999556, 0.7041666666666667185, 0.7083333333333333703, 0.7125000000000000222, 0.7166666666666666741, 0.7208333333333333259, 0.7249999999999999778, 0.7291666666666666297, 0.7333333333333332815, 0.7375000000000000444, 0.7416666666666666963, 0.7458333333333333481, 0.7500000000000000000, 0.7541666666666666519, 0.7583333333333333037, 0.7624999999999999556, 0.7666666666666667185, 0.7708333333333333703, 0.7750000000000000222, 0.7791666666666666741, 0.7833333333333333259, 0.7874999999999999778, 0.7916666666666666297, 0.7958333333333332815, 0.8000000000000000444, 0.8041666666666666963, 0.8083333333333333481, 0.8125000000000000000, 0.8166666666666666519, 0.8208333333333333037, 0.8249999999999999556, 0.8291666666666667185, 0.8333333333333333703, 0.8375000000000000222, 0.8416666666666666741, 0.8458333333333333259, 0.8499999999999999778, 0.8541666666666666297, 0.8583333333333332815, 0.8625000000000000444, 0.8666666666666666963, 0.8708333333333333481, 0.8750000000000000000, 0.8791666666666666519, 0.8833333333333333037, 0.8874999999999999556, 0.8916666666666667185, 0.8958333333333333703, 0.9000000000000000222, 0.9041666666666666741, 0.9083333333333333259, 0.9124999999999999778, 0.9166666666666666297, 0.9208333333333332815, 0.9250000000000000444, 0.9291666666666666963, 0.9333333333333333481, 0.9375000000000000000, 0.9416666666666666519, 0.9458333333333333037, 0.9499999999999999556, 0.9541666666666667185, 0.9583333333333333703, 0.9625000000000000222, 0.9666666666666666741, 0.9708333333333333259, 0.9749999999999999778, 0.9791666666666666297, 0.9833333333333332815, 0.9875000000000000444, 0.9916666666666666963, 0.9958333333333333481, 1.000000000000000000 ),
 .UNSPECIFIED. ) 
 GEOMETRIC_REPRESENTATION_ITEM ( )  RATIONAL_B_SPLINE_SURFACE ( (
 ( 1.000000000000000000, 0.9238795325112867385, 1.000000000000000000, 0.9238795325112867385, 1.000000000000000000, 0.9238795325112867385, 1.000000000000000000, 0.9238795325112867385, 1.000000000000000000, 0.9238795325112867385, 1.000000000000000000, 0.9238795325112867385, 1.000000000000000000, 0.9238795325112867385, 1.000000000000000000, 0.9238795325112867385, 1.000000000000000000, 0.9238795325112867385, 1.000000000000000000, 0.9238795325112867385, 1.000000000000000000, 0.9238795325112867385, 1.000000000000000000, 0.9238795325112867385, 1.000000000000000000, 0.9238795325112867385, 1.000000000000000000, 0.9238795325112867385, 1.000000000000000000, 0.9238795325112867385, 1.000000000000000000, 0.9238795325112867385, 1.000000000000000000, 0.9238795325112867385, 1.000000000000000000, 0.9238795325112867385, 1.000000000000000000, 0.9238795325112867385, 1.000000000000000000, 0.9238795325112867385, 1.000000000000000000, 0.9238795325112867385, 1.000000000000000000, 0.9238795325112867385, 1.000000000000000000, 0.9238795325112867385, 1.000000000000000000, 0.9238795325112867385, 1.000000000000000000, 0.9238795325112867385, 1.000000000000000000, 0.9238795325112867385, 1.000000000000000000, 0.9238795325112867385, 1.000000000000000000, 0.9238795325112867385, 1.000000000000000000, 0.9238795325112867385, 1.000000000000000000, 0.9238795325112867385, 1.000000000000000000, 0.9238795325112867385, 1.000000000000000000, 0.9238795325112867385, 1.000000000000000000, 0.9238795325112867385, 1.000000000000000000, 0.9238795325112867385, 1.000000000000000000, 0.9238795325112867385, 1.000000000000000000, 0.9238795325112867385, 1.000000000000000000, 0.9238795325112867385, 1.000000000000000000, 0.9238795325112867385, 1.000000000000000000, 0.9238795325112867385, 1.000000000000000000, 0.9238795325112867385, 1.000000000000000000, 0.9238795325112867385, 1.000000000000000000, 0.9238795325112867385, 1.000000000000000000, 0.9238795325112867385, 1.000000000000000000, 0.9238795325112867385, 1.000000000000000000, 0.9238795325112867385, 1.000000000000000000, 0.9238795325112867385, 1.000000000000000000, 0.9238795325112867385, 1.000000000000000000, 0.9238795325112867385, 1.000000000000000000, 0.9238795325112867385, 1.000000000000000000, 0.9238795325112867385, 1.000000000000000000, 0.9238795325112867385, 1.000000000000000000, 0.9238795325112867385, 1.000000000000000000, 0.9238795325112867385, 1.000000000000000000, 0.9238795325112867385, 1.000000000000000000, 0.9238795325112867385, 1.000000000000000000, 0.9238795325112867385, 1.000000000000000000, 0.9238795325112867385, 1.000000000000000000, 0.9238795325112867385, 1.000000000000000000, 0.9238795325112867385, 1.000000000000000000, 0.9238795325112867385, 1.000000000000000000, 0.9238795325112867385, 1.000000000000000000, 0.9238795325112867385, 1.000000000000000000, 0.9238795325112867385, 1.000000000000000000, 0.9238795325112867385, 1.000000000000000000, 0.9238795325112867385, 1.000000000000000000, 0.9238795325112867385, 1.000000000000000000, 0.9238795325112867385, 1.000000000000000000, 0.9238795325112867385, 1.000000000000000000, 0.9238795325112867385, 1.000000000000000000, 0.9238795325112867385, 1.000000000000000000, 0.9238795325112867385, 1.000000000000000000, 0.9238795325112867385, 1.000000000000000000, 0.9238795325112867385, 1.000000000000000000, 0.9238795325112867385, 1.000000000000000000, 0.9238795325112867385, 1.000000000000000000, 0.9238795325112867385, 1.000000000000000000, 0.9238795325112867385, 1.000000000000000000, 0.9238795325112867385, 1.000000000000000000, 0.9238795325112867385, 1.000000000000000000, 0.9238795325112867385, 1.000000000000000000, 0.9238795325112867385, 1.000000000000000000, 0.9238795325112867385, 1.000000000000000000, 0.9238795325112867385, 1.000000000000000000, 0.9238795325112867385, 1.000000000000000000, 0.9238795325112867385, 1.000000000000000000, 0.9238795325112867385, 1.000000000000000000, 0.9238795325112867385, 1.000000000000000000, 0.9238795325112867385, 1.000000000000000000, 0.9238795325112867385, 1.000000000000000000, 0.9238795325112867385, 1.000000000000000000, 0.9238795325112867385, 1.000000000000000000, 0.9238795325112867385, 1.000000000000000000, 0.9238795325112867385, 1.000000000000000000, 0.9238795325112867385, 1.000000000000000000, 0.9238795325112867385, 1.000000000000000000, 0.9238795325112867385, 1.000000000000000000, 0.9238795325112867385, 1.000000000000000000, 0.9238795325112867385, 1.000000000000000000, 0.9238795325112867385, 1.000000000000000000, 0.9238795325112867385, 1.000000000000000000, 0.9238795325112867385, 1.000000000000000000, 0.9238795325112867385, 1.000000000000000000, 0.9238795325112867385, 1.000000000000000000, 0.9238795325112867385, 1.000000000000000000, 0.9238795325112867385, 1.000000000000000000, 0.9238795325112867385, 1.000000000000000000, 0.9238795325112867385, 1.000000000000000000, 0.9238795325112867385, 1.000000000000000000, 0.9238795325112867385, 1.000000000000000000, 0.9238795325112867385, 1.000000000000000000, 0.9238795325112867385, 1.000000000000000000, 0.9238795325112867385, 1.000000000000000000, 0.9238795325112867385, 1.000000000000000000, 0.9238795325112867385, 1.000000000000000000, 0.9238795325112867385, 1.000000000000000000, 0.9238795325112867385, 1.000000000000000000, 0.9238795325112867385, 1.000000000000000000, 0.9238795325112867385, 1.000000000000000000, 0.9238795325112867385, 1.000000000000000000, 0.9238795325112867385, 1.000000000000000000, 0.9238795325112867385, 1.000000000000000000, 0.9238795325112867385, 1.000000000000000000, 0.9238795325112867385, 1.000000000000000000, 0.9238795325112867385, 1.000000000000000000, 0.9238795325112867385, 1.000000000000000000, 0.9238795325112867385, 1.000000000000000000, 0.9238795325112867385, 1.000000000000000000, 0.9238795325112867385, 1.000000000000000000, 0.9238795325112867385, 1.000000000000000000, 0.9238795325112867385, 1.000000000000000000, 0.9238795325112867385, 1.000000000000000000, 0.9238795325112867385, 1.000000000000000000, 0.9238795325112867385, 1.000000000000000000, 0.9238795325112867385, 1.000000000000000000, 0.9238795325112867385, 1.000000000000000000, 0.9238795325112867385, 1.000000000000000000, 0.9238795325112867385, 1.000000000000000000, 0.9238795325112867385, 1.000000000000000000, 0.9238795325112867385, 1.000000000000000000, 0.9238795325112867385, 1.000000000000000000, 0.9238795325112867385, 1.000000000000000000, 0.9238795325112867385, 1.000000000000000000, 0.9238795325112867385, 1.000000000000000000, 0.9238795325112867385, 1.000000000000000000, 0.9238795325112867385, 1.000000000000000000, 0.9238795325112867385, 1.000000000000000000, 0.9238795325112867385, 1.000000000000000000, 0.9238795325112867385, 1.000000000000000000, 0.9238795325112867385, 1.000000000000000000, 0.9238795325112867385, 1.000000000000000000, 0.9238795325112867385, 1.000000000000000000, 0.9238795325112867385, 1.000000000000000000, 0.9238795325112867385, 1.000000000000000000, 0.9238795325112867385, 1.000000000000000000, 0.9238795325112867385, 1.000000000000000000, 0.9238795325112867385, 1.000000000000000000, 0.9238795325112867385, 1.000000000000000000, 0.9238795325112867385, 1.000000000000000000, 0.9238795325112867385, 1.000000000000000000, 0.9238795325112867385, 1.000000000000000000, 0.9238795325112867385, 1.000000000000000000, 0.9238795325112867385, 1.000000000000000000, 0.9238795325112867385, 1.000000000000000000, 0.9238795325112867385, 1.000000000000000000, 0.9238795325112867385, 1.000000000000000000, 0.9238795325112867385, 1.000000000000000000, 0.9238795325112867385, 1.000000000000000000, 0.9238795325112867385, 1.000000000000000000, 0.9238795325112867385, 1.000000000000000000, 0.9238795325112867385, 1.000000000000000000, 0.9238795325112867385, 1.000000000000000000, 0.9238795325112867385, 1.000000000000000000, 0.9238795325112867385, 1.000000000000000000, 0.9238795325112867385, 1.000000000000000000, 0.9238795325112867385, 1.000000000000000000, 0.9238795325112867385, 1.000000000000000000, 0.9238795325112867385, 1.000000000000000000, 0.9238795325112867385, 1.000000000000000000, 0.9238795325112867385, 1.000000000000000000, 0.9238795325112867385, 1.000000000000000000, 0.9238795325112867385, 1.000000000000000000, 0.9238795325112867385, 1.000000000000000000, 0.9238795325112867385, 1.000000000000000000, 0.9238795325112867385, 1.000000000000000000, 0.9238795325112867385, 1.000000000000000000, 0.9238795325112867385, 1.000000000000000000, 0.9238795325112867385, 1.000000000000000000, 0.9238795325112867385, 1.000000000000000000, 0.9238795325112867385, 1.000000000000000000, 0.9238795325112867385, 1.000000000000000000, 0.9238795325112867385, 1.000000000000000000, 0.9238795325112867385, 1.000000000000000000, 0.9238795325112867385, 1.000000000000000000, 0.9238795325112867385, 1.000000000000000000, 0.9238795325112867385, 1.000000000000000000, 0.9238795325112867385, 1.000000000000000000, 0.9238795325112867385, 1.000000000000000000, 0.9238795325112867385, 1.000000000000000000, 0.9238795325112867385, 1.000000000000000000, 0.9238795325112867385, 1.000000000000000000, 0.9238795325112867385, 1.000000000000000000, 0.9238795325112867385, 1.000000000000000000, 0.9238795325112867385, 1.000000000000000000, 0.9238795325112867385, 1.000000000000000000, 0.9238795325112867385, 1.000000000000000000, 0.9238795325112867385, 1.000000000000000000, 0.9238795325112867385, 1.000000000000000000, 0.9238795325112867385, 1.000000000000000000, 0.9238795325112867385, 1.000000000000000000, 0.9238795325112867385, 1.000000000000000000, 0.9238795325112867385, 1.000000000000000000, 0.9238795325112867385, 1.000000000000000000, 0.9238795325112867385, 1.000000000000000000, 0.9238795325112867385, 1.000000000000000000, 0.9238795325112867385, 1.000000000000000000, 0.9238795325112867385, 1.000000000000000000, 0.9238795325112867385, 1.000000000000000000, 0.9238795325112867385, 1.000000000000000000, 0.9238795325112867385, 1.000000000000000000, 0.9238795325112867385, 1.000000000000000000, 0.9238795325112867385, 1.000000000000000000, 0.9238795325112867385, 1.000000000000000000, 0.9238795325112867385, 1.000000000000000000, 0.9238795325112867385, 1.000000000000000000, 0.9238795325112867385, 1.000000000000000000, 0.9238795325112867385, 1.000000000000000000, 0.9238795325112867385, 1.000000000000000000, 0.9238795325112867385, 1.000000000000000000, 0.9238795325112867385, 1.000000000000000000, 0.9238795325112867385, 1.000000000000000000, 0.9238795325112867385, 1.000000000000000000, 0.9238795325112867385, 1.000000000000000000, 0.9238795325112867385, 1.000000000000000000, 0.9238795325112867385, 1.000000000000000000, 0.9238795325112867385, 1.000000000000000000, 0.9238795325112867385, 1.000000000000000000, 0.9238795325112867385, 1.000000000000000000, 0.9238795325112867385, 1.000000000000000000, 0.9238795325112867385, 1.000000000000000000, 0.9238795325112867385, 1.000000000000000000),
 ( 1.000000000000000000, 0.9238795325112867385, 1.000000000000000000, 0.9238795325112867385, 1.000000000000000000, 0.9238795325112867385, 1.000000000000000000, 0.9238795325112867385, 1.000000000000000000, 0.9238795325112867385, 1.000000000000000000, 0.9238795325112867385, 1.000000000000000000, 0.9238795325112867385, 1.000000000000000000, 0.9238795325112867385, 1.000000000000000000, 0.9238795325112867385, 1.000000000000000000, 0.9238795325112867385, 1.000000000000000000, 0.9238795325112867385, 1.000000000000000000, 0.9238795325112867385, 1.000000000000000000, 0.9238795325112867385, 1.000000000000000000, 0.9238795325112867385, 1.000000000000000000, 0.9238795325112867385, 1.000000000000000000, 0.9238795325112867385, 1.000000000000000000, 0.9238795325112867385, 1.000000000000000000, 0.9238795325112867385, 1.000000000000000000, 0.9238795325112867385, 1.000000000000000000, 0.9238795325112867385, 1.000000000000000000, 0.9238795325112867385, 1.000000000000000000, 0.9238795325112867385, 1.000000000000000000, 0.9238795325112867385, 1.000000000000000000, 0.9238795325112867385, 1.000000000000000000, 0.9238795325112867385, 1.000000000000000000, 0.9238795325112867385, 1.000000000000000000, 0.9238795325112867385, 1.000000000000000000, 0.9238795325112867385, 1.000000000000000000, 0.9238795325112867385, 1.000000000000000000, 0.9238795325112867385, 1.000000000000000000, 0.9238795325112867385, 1.000000000000000000, 0.9238795325112867385, 1.000000000000000000, 0.9238795325112867385, 1.000000000000000000, 0.9238795325112867385, 1.000000000000000000, 0.9238795325112867385, 1.000000000000000000, 0.9238795325112867385, 1.000000000000000000, 0.9238795325112867385, 1.000000000000000000, 0.9238795325112867385, 1.000000000000000000, 0.9238795325112867385, 1.000000000000000000, 0.9238795325112867385, 1.000000000000000000, 0.9238795325112867385, 1.000000000000000000, 0.9238795325112867385, 1.000000000000000000, 0.9238795325112867385, 1.000000000000000000, 0.9238795325112867385, 1.000000000000000000, 0.9238795325112867385, 1.000000000000000000, 0.9238795325112867385, 1.000000000000000000, 0.9238795325112867385, 1.000000000000000000, 0.9238795325112867385, 1.000000000000000000, 0.9238795325112867385, 1.000000000000000000, 0.9238795325112867385, 1.000000000000000000, 0.9238795325112867385, 1.000000000000000000, 0.9238795325112867385, 1.000000000000000000, 0.9238795325112867385, 1.000000000000000000, 0.9238795325112867385, 1.000000000000000000, 0.9238795325112867385, 1.000000000000000000, 0.9238795325112867385, 1.000000000000000000, 0.9238795325112867385, 1.000000000000000000, 0.9238795325112867385, 1.000000000000000000, 0.9238795325112867385, 1.000000000000000000, 0.9238795325112867385, 1.000000000000000000, 0.9238795325112867385, 1.000000000000000000, 0.9238795325112867385, 1.000000000000000000, 0.9238795325112867385, 1.000000000000000000, 0.9238795325112867385, 1.000000000000000000, 0.9238795325112867385, 1.000000000000000000, 0.9238795325112867385, 1.000000000000000000, 0.9238795325112867385, 1.000000000000000000, 0.9238795325112867385, 1.000000000000000000, 0.9238795325112867385, 1.000000000000000000, 0.9238795325112867385, 1.000000000000000000, 0.9238795325112867385, 1.000000000000000000, 0.9238795325112867385, 1.000000000000000000, 0.9238795325112867385, 1.000000000000000000, 0.9238795325112867385, 1.000000000000000000, 0.9238795325112867385, 1.000000000000000000, 0.9238795325112867385, 1.000000000000000000, 0.9238795325112867385, 1.000000000000000000, 0.9238795325112867385, 1.000000000000000000, 0.9238795325112867385, 1.000000000000000000, 0.9238795325112867385, 1.000000000000000000, 0.9238795325112867385, 1.000000000000000000, 0.9238795325112867385, 1.000000000000000000, 0.9238795325112867385, 1.000000000000000000, 0.9238795325112867385, 1.000000000000000000, 0.9238795325112867385, 1.000000000000000000, 0.9238795325112867385, 1.000000000000000000, 0.9238795325112867385, 1.000000000000000000, 0.9238795325112867385, 1.000000000000000000, 0.9238795325112867385, 1.000000000000000000, 0.9238795325112867385, 1.000000000000000000, 0.9238795325112867385, 1.000000000000000000, 0.9238795325112867385, 1.000000000000000000, 0.9238795325112867385, 1.000000000000000000, 0.9238795325112867385, 1.000000000000000000, 0.9238795325112867385, 1.000000000000000000, 0.9238795325112867385, 1.000000000000000000, 0.9238795325112867385, 1.000000000000000000, 0.9238795325112867385, 1.000000000000000000, 0.9238795325112867385, 1.000000000000000000, 0.9238795325112867385, 1.000000000000000000, 0.9238795325112867385, 1.000000000000000000, 0.9238795325112867385, 1.000000000000000000, 0.9238795325112867385, 1.000000000000000000, 0.9238795325112867385, 1.000000000000000000, 0.9238795325112867385, 1.000000000000000000, 0.9238795325112867385, 1.000000000000000000, 0.9238795325112867385, 1.000000000000000000, 0.9238795325112867385, 1.000000000000000000, 0.9238795325112867385, 1.000000000000000000, 0.9238795325112867385, 1.000000000000000000, 0.9238795325112867385, 1.000000000000000000, 0.9238795325112867385, 1.000000000000000000, 0.9238795325112867385, 1.000000000000000000, 0.9238795325112867385, 1.000000000000000000, 0.9238795325112867385, 1.000000000000000000, 0.9238795325112867385, 1.000000000000000000, 0.9238795325112867385, 1.000000000000000000, 0.9238795325112867385, 1.000000000000000000, 0.9238795325112867385, 1.000000000000000000, 0.9238795325112867385, 1.000000000000000000, 0.9238795325112867385, 1.000000000000000000, 0.9238795325112867385, 1.000000000000000000, 0.9238795325112867385, 1.000000000000000000, 0.9238795325112867385, 1.000000000000000000, 0.9238795325112867385, 1.000000000000000000, 0.9238795325112867385, 1.000000000000000000, 0.9238795325112867385, 1.000000000000000000, 0.9238795325112867385, 1.000000000000000000, 0.9238795325112867385, 1.000000000000000000, 0.9238795325112867385, 1.000000000000000000, 0.9238795325112867385, 1.000000000000000000, 0.9238795325112867385, 1.000000000000000000, 0.9238795325112867385, 1.000000000000000000, 0.9238795325112867385, 1.000000000000000000, 0.9238795325112867385, 1.000000000000000000, 0.9238795325112867385, 1.000000000000000000, 0.9238795325112867385, 1.000000000000000000, 0.9238795325112867385, 1.000000000000000000, 0.9238795325112867385, 1.000000000000000000, 0.9238795325112867385, 1.000000000000000000, 0.9238795325112867385, 1.000000000000000000, 0.9238795325112867385, 1.000000000000000000, 0.9238795325112867385, 1.000000000000000000, 0.9238795325112867385, 1.000000000000000000, 0.9238795325112867385, 1.000000000000000000, 0.9238795325112867385, 1.000000000000000000, 0.9238795325112867385, 1.000000000000000000, 0.9238795325112867385, 1.000000000000000000, 0.9238795325112867385, 1.000000000000000000, 0.9238795325112867385, 1.000000000000000000, 0.9238795325112867385, 1.000000000000000000, 0.9238795325112867385, 1.000000000000000000, 0.9238795325112867385, 1.000000000000000000, 0.9238795325112867385, 1.000000000000000000, 0.9238795325112867385, 1.000000000000000000, 0.9238795325112867385, 1.000000000000000000, 0.9238795325112867385, 1.000000000000000000, 0.9238795325112867385, 1.000000000000000000, 0.9238795325112867385, 1.000000000000000000, 0.9238795325112867385, 1.000000000000000000, 0.9238795325112867385, 1.000000000000000000, 0.9238795325112867385, 1.000000000000000000, 0.9238795325112867385, 1.000000000000000000, 0.9238795325112867385, 1.000000000000000000, 0.9238795325112867385, 1.000000000000000000, 0.9238795325112867385, 1.000000000000000000, 0.9238795325112867385, 1.000000000000000000, 0.9238795325112867385, 1.000000000000000000, 0.9238795325112867385, 1.000000000000000000, 0.9238795325112867385, 1.000000000000000000, 0.9238795325112867385, 1.000000000000000000, 0.9238795325112867385, 1.000000000000000000, 0.9238795325112867385, 1.000000000000000000, 0.9238795325112867385, 1.000000000000000000, 0.9238795325112867385, 1.000000000000000000, 0.9238795325112867385, 1.000000000000000000, 0.9238795325112867385, 1.000000000000000000, 0.9238795325112867385, 1.000000000000000000, 0.9238795325112867385, 1.000000000000000000, 0.9238795325112867385, 1.000000000000000000, 0.9238795325112867385, 1.000000000000000000, 0.9238795325112867385, 1.000000000000000000, 0.9238795325112867385, 1.000000000000000000, 0.9238795325112867385, 1.000000000000000000, 0.9238795325112867385, 1.000000000000000000, 0.9238795325112867385, 1.000000000000000000, 0.9238795325112867385, 1.000000000000000000, 0.9238795325112867385, 1.000000000000000000, 0.9238795325112867385, 1.000000000000000000, 0.9238795325112867385, 1.000000000000000000, 0.9238795325112867385, 1.000000000000000000, 0.9238795325112867385, 1.000000000000000000, 0.9238795325112867385, 1.000000000000000000, 0.9238795325112867385, 1.000000000000000000, 0.9238795325112867385, 1.000000000000000000, 0.9238795325112867385, 1.000000000000000000, 0.9238795325112867385, 1.000000000000000000, 0.9238795325112867385, 1.000000000000000000, 0.9238795325112867385, 1.000000000000000000, 0.9238795325112867385, 1.000000000000000000, 0.9238795325112867385, 1.000000000000000000, 0.9238795325112867385, 1.000000000000000000, 0.9238795325112867385, 1.000000000000000000, 0.9238795325112867385, 1.000000000000000000, 0.9238795325112867385, 1.000000000000000000, 0.9238795325112867385, 1.000000000000000000, 0.9238795325112867385, 1.000000000000000000, 0.9238795325112867385, 1.000000000000000000, 0.9238795325112867385, 1.000000000000000000, 0.9238795325112867385, 1.000000000000000000, 0.9238795325112867385, 1.000000000000000000, 0.9238795325112867385, 1.000000000000000000, 0.9238795325112867385, 1.000000000000000000, 0.9238795325112867385, 1.000000000000000000, 0.9238795325112867385, 1.000000000000000000, 0.9238795325112867385, 1.000000000000000000, 0.9238795325112867385, 1.000000000000000000, 0.9238795325112867385, 1.000000000000000000, 0.9238795325112867385, 1.000000000000000000, 0.9238795325112867385, 1.000000000000000000, 0.9238795325112867385, 1.000000000000000000, 0.9238795325112867385, 1.000000000000000000, 0.9238795325112867385, 1.000000000000000000, 0.9238795325112867385, 1.000000000000000000, 0.9238795325112867385, 1.000000000000000000, 0.9238795325112867385, 1.000000000000000000, 0.9238795325112867385, 1.000000000000000000, 0.9238795325112867385, 1.000000000000000000, 0.9238795325112867385, 1.000000000000000000, 0.9238795325112867385, 1.000000000000000000, 0.9238795325112867385, 1.000000000000000000, 0.9238795325112867385, 1.000000000000000000, 0.9238795325112867385, 1.000000000000000000, 0.9238795325112867385, 1.000000000000000000, 0.9238795325112867385, 1.000000000000000000, 0.9238795325112867385, 1.000000000000000000, 0.9238795325112867385, 1.000000000000000000, 0.9238795325112867385, 1.000000000000000000, 0.9238795325112867385, 1.000000000000000000, 0.9238795325112867385, 1.000000000000000000) ) ) 
 REPRESENTATION_ITEM ( '' )  SURFACE ( )  );
#2432 = CARTESIAN_POINT ( 'NONE',  ( 3.535533905932736864, -147.1250000000000000, 3.535533905932738641 ) ) ;
#2433 = CARTESIAN_POINT ( 'NONE',  ( 4.458734124999998549, -25.72916666530107221, -2.574251347313721627 ) ) ;
#2434 = EDGE_CURVE ( 'NONE', #16392, #5665, #590, .T. ) ;
#2435 = CARTESIAN_POINT ( 'NONE',  ( 4.458734124999999437, -70.06249999863439371, -5.460374474430324690E-16 ) ) ;
#2436 = CARTESIAN_POINT ( 'NONE',  ( -2.499999999999996447, -89.83333333333332860, 4.330127018922195425 ) ) ;
#2437 = CARTESIAN_POINT ( 'NONE',  ( -2.229367062500000163, -23.47916666530107221, -3.861377020970580443 ) ) ;
#2438 = CARTESIAN_POINT ( 'NONE',  ( -6.972266317189433020E-16, 6.750000000000000000, -5.000000000000000000 ) ) ;
#2439 = CARTESIAN_POINT ( 'NONE',  ( -5.000000000000000888, -152.4375000000000284, 2.071067811865474617 ) ) ;
#2440 = CARTESIAN_POINT ( 'NONE',  ( 5.000000000000000000, -17.50000000000000000, -6.123233995736766282E-16 ) ) ;
#2441 = CARTESIAN_POINT ( 'NONE',  ( 4.458734124999999437, -153.4375000013655779, 0.000000000000000000 ) ) ;
#2442 = VERTEX_POINT ( 'NONE', #272 ) ;
#2443 = CARTESIAN_POINT ( 'NONE',  ( 3.061616997868383141E-16, -149.7500000000000284, -5.000000000000000000 ) ) ;
#2444 = CARTESIAN_POINT ( 'NONE',  ( 4.458734125000000326, -51.14583333196772941, 2.574251347313718519 ) ) ;
#2445 = LINE ( 'NONE', #36848, #63314 ) ;
#2446 = CARTESIAN_POINT ( 'NONE',  ( 0.000000000000000000, -120.0000000000000000, 0.000000000000000000 ) ) ;
#2447 = ADVANCED_FACE ( 'NONE', ( #11177 ), #20197, .T. ) ;
#2448 = CARTESIAN_POINT ( 'NONE',  ( 2.500000000000002220, 26.33333333333333215, 4.330127018922192761 ) ) ;
#2449 = DIRECTION ( 'NONE',  ( -0.000000000000000000, 1.000000000000000000, -0.000000000000000000 ) ) ;
#2450 = CARTESIAN_POINT ( 'NONE',  ( -2.229367062499996610, 4.854166668032261711, 3.861377020970582219 ) ) ;
#2451 = CARTESIAN_POINT ( 'NONE',  ( 1.975475456537005874E-15, -5.750000000000000000, 5.000000000000000000 ) ) ;
#2452 = CARTESIAN_POINT ( 'NONE',  ( 5.000000000000000888, -11.45833333060214976, 2.886751345948126879 ) ) ;
#2453 = CARTESIAN_POINT ( 'NONE',  ( 9.457646018065525792E-16, 17.68750000136559564, 5.148502694627439702 ) ) ;
#2454 = CARTESIAN_POINT ( 'NONE',  ( -4.999999999999999112, 1.208333336064518759, 2.886751345948131764 ) ) ;
#2455 = ORIENTED_EDGE ( 'NONE', *, *, #3063, .T. ) ;
#2456 = CARTESIAN_POINT ( 'NONE',  ( 5.000000000000000000, -42.41666666666667140, -2.886751345948130876 ) ) ;
#2457 = ORIENTED_EDGE ( 'NONE', *, *, #26383, .F. ) ;
#2458 = CARTESIAN_POINT ( 'NONE',  ( -58.39396692619412477, -154.6875000013656063, 2.891590998281057701 ) ) ;
#2459 = CARTESIAN_POINT ( 'NONE',  ( 9.457646018065525792E-16, -41.06249999863440792, 5.148502694627439702 ) ) ;
#2460 = CARTESIAN_POINT ( 'NONE',  ( 4.458734124999999437, -165.7500000013655495, 1.846868145590737864 ) ) ;
#2461 = CARTESIAN_POINT ( 'NONE',  ( -4.999999999999999112, -45.79166666393547303, 2.886751345948131764 ) ) ;
#2462 = ORIENTED_EDGE ( 'NONE', *, *, #3084, .T. ) ;
#2463 = CARTESIAN_POINT ( 'NONE',  ( 4.458734124999998549, -19.72916666530107221, -2.574251347313721627 ) ) ;
#2464 = VERTEX_POINT ( 'NONE', #59765 ) ;
#2465 = CARTESIAN_POINT ( 'NONE',  ( -5.000000000000000000, -86.08333333333334281, -2.886751345948128211 ) ) ;
#2466 = CARTESIAN_POINT ( 'NONE',  ( 4.458734124999999437, -166.4375000013655779, 0.000000000000000000 ) ) ;
#2468 = ORIENTED_EDGE ( 'NONE', *, *, #14861, .T. ) ;
#2467 = CARTESIAN_POINT ( 'NONE',  ( 2.500000000000002220, -20.54166666393548013, 4.330127018922192761 ) ) ;
#2469 = CARTESIAN_POINT ( 'NONE',  ( -55.39835681537999790, -135.8750000000000284, 4.984105922594378235 ) ) ;
#2470 = CARTESIAN_POINT ( 'NONE',  ( -4.458734124999998549, -30.47916666530107221, 2.574251347313722516 ) ) ;
#2471 = ORIENTED_EDGE ( 'NONE', *, *, #25040, .T. ) ;
#2472 = CARTESIAN_POINT ( 'NONE',  ( -2.229367062500000163, -78.47916666530106511, -3.861377020970580443 ) ) ;
#2473 = CARTESIAN_POINT ( 'NONE',  ( -4.458734124999999437, 25.60416666803225993, -2.574251347313719407 ) ) ;
#2474 = CARTESIAN_POINT ( 'NONE',  ( 5.000000000000000000, 24.62500000273118417, -6.123233995736766282E-16 ) ) ;
#2475 = ORIENTED_EDGE ( 'NONE', *, *, #50260, .T. ) ;
#2476 = DIRECTION ( 'NONE',  ( -0.000000000000000000, 1.000000000000000000, -0.000000000000000000 ) ) ;
#2477 = CARTESIAN_POINT ( 'NONE',  ( -52.80376928212989185, -141.1250000013656063, -4.297418129356378458 ) ) ;
#2478 = CARTESIAN_POINT ( 'NONE',  ( 4.458734124999998549, -77.97916666530106511, -2.574251347313721627 ) ) ;
#2479 = CARTESIAN_POINT ( 'NONE',  ( -58.24261429053147765, -131.3750000027312126, -3.805975901505573855 ) ) ;
#2480 = CARTESIAN_POINT ( 'NONE',  ( 2.500000000000002220, 0.4583333360645182042, 4.330127018922192761 ) ) ;
#2481 = CARTESIAN_POINT ( 'NONE',  ( -1.339745962155610925, -82.79465819873851729, 5.000000000000000000 ) ) ;
#2482 =( BOUNDED_CURVE ( )  B_SPLINE_CURVE ( 2, ( #63473, #34830, #58640, #14878, #24220, #10058, #34486, #54120, #53802 ),
 .UNSPECIFIED., .F., .F. ) 
 B_SPLINE_CURVE_WITH_KNOTS ( ( 3, 2, 2, 2, 3 ),
 ( 0.5124999999999999556, 0.5130952380952380487, 0.5142857142857142350, 0.5154761904761904212, 0.5160714285714286254 ),
 .UNSPECIFIED. ) 
 CURVE ( )  GEOMETRIC_REPRESENTATION_ITEM ( )  RATIONAL_B_SPLINE_CURVE ( ( 0.9330127018922194093, 0.9330127018922194093, 1.000000000000000000, 0.8660254037844387076, 1.000000000000000000, 0.8660254037844387076, 1.000000000000000000, 0.9330127018922130810, 0.9330127018922194093 ) ) 
 REPRESENTATION_ITEM ( '' )  );
#2483 = CARTESIAN_POINT ( 'NONE',  ( 6.123233995736766282E-16, -170.0000000000000000, -5.000000000000000000 ) ) ;
#2484 = CARTESIAN_POINT ( 'NONE',  ( 9.457646018065525792E-16, -54.06249999863440081, 5.148502694627439702 ) ) ;
#2485 = CARTESIAN_POINT ( 'NONE',  ( 2.229367062500001939, -42.97916666530107932, 3.861377020970579999 ) ) ;
#2486 = CARTESIAN_POINT ( 'NONE',  ( -4.458734124999999437, 28.60416666803226349, -2.574251347313719407 ) ) ;
#2487 = CARTESIAN_POINT ( 'NONE',  ( -2.499999999999996447, -106.8333333333333428, 4.330127018922195425 ) ) ;
#2488 = CARTESIAN_POINT ( 'NONE',  ( -6.972266317189433020E-16, 20.74999999999999645, -5.000000000000000000 ) ) ;
#2489 = ADVANCED_FACE ( 'NONE', ( #10225 ), #15050, .T. ) ;
#2490 = CARTESIAN_POINT ( 'NONE',  ( 2.229367062500001939, -36.22916666530107221, 3.861377020970579999 ) ) ;
#2491 = CARTESIAN_POINT ( 'NONE',  ( 2.500000000000002220, 3.458333336064517205, 4.330127018922192761 ) ) ;
#2492 = CARTESIAN_POINT ( 'NONE',  ( -3.535533905932737309, -153.7500000027312126, -3.535533905932738197 ) ) ;
#2493 = CARTESIAN_POINT ( 'NONE',  ( -54.64476657466781973, -125.8125000013655921, -4.444560631937228834 ) ) ;
#2494 = CARTESIAN_POINT ( 'NONE',  ( -2.229367062500000163, -78.72916666530106511, -3.861377020970580443 ) ) ;
#2495 = CARTESIAN_POINT ( 'NONE',  ( -51.75738570946856498, -141.8750000027312126, 3.805975901505576964 ) ) ;
#2496 = CARTESIAN_POINT ( 'NONE',  ( 4.458734124999999437, -104.8124999986344079, -5.460374474430324690E-16 ) ) ;
#2497 = CARTESIAN_POINT ( 'NONE',  ( 4.458734124999998549, -7.979166665301073991, -2.574251347313721627 ) ) ;
#2498 = ORIENTED_EDGE ( 'NONE', *, *, #33570, .T. ) ;
#2499 = CARTESIAN_POINT ( 'NONE',  ( -2.229367062500000163, -95.47916666530107932, -3.861377020970580443 ) ) ;
#2500 = CYLINDRICAL_SURFACE ( 'NONE', #20251, 5.000000000000000000 ) ;
#2501 = CARTESIAN_POINT ( 'NONE',  ( -4.458734124999999437, -87.64583333196773651, -2.574251347313719407 ) ) ;
#2502 = CARTESIAN_POINT ( 'NONE',  ( -4.458734124999999437, 11.43750000136559564, 0.000000000000000000 ) ) ;
#2503 = CARTESIAN_POINT ( 'NONE',  ( 1.339745962155615144, -2.580341798530292774, 4.999999999999999112 ) ) ;
#2504 = CARTESIAN_POINT ( 'NONE',  ( -59.44456063193725015, -134.5625000013656063, -0.3552334253322034230 ) ) ;
#2505 = CARTESIAN_POINT ( 'NONE',  ( 4.458734125000000326, -9.895833331967738289, 2.574251347313718519 ) ) ;
#2506 = CARTESIAN_POINT ( 'NONE',  ( 9.457646018065525792E-16, 17.68750000136559564, 5.148502694627439702 ) ) ;
#2507 = CARTESIAN_POINT ( 'NONE',  ( -2.229367062500000163, -51.72916666530107221, -3.861377020970580443 ) ) ;
#2508 = CARTESIAN_POINT ( 'NONE',  ( -2.916731409357579869E-14, 17.37500000273118417, 5.000000000000000888 ) ) ;
#2509 = FACE_OUTER_BOUND ( 'NONE', #36769, .T. ) ;
#2510 = CARTESIAN_POINT ( 'NONE',  ( -2.229367062500000163, -11.47916666530107044, -3.861377020970580443 ) ) ;
#2511 = CARTESIAN_POINT ( 'NONE',  ( 1.975475456537005874E-15, -38.75000000000000000, 5.000000000000000000 ) ) ;
#2512 = EDGE_CURVE ( 'NONE', #22662, #34612, #29831, .T. ) ;
#2513 = ORIENTED_EDGE ( 'NONE', *, *, #57459, .T. ) ;
#2514 = CARTESIAN_POINT ( 'NONE',  ( 4.458734125000000326, -34.14583333196772941, 2.574251347313718519 ) ) ;
#2515 = CARTESIAN_POINT ( 'NONE',  ( -53.51423613279429503, -129.5000000013656347, 4.591703134518082763 ) ) ;
#2516 = EDGE_CURVE ( 'NONE', #47219, #23230, #28945, .T. ) ;
#2517 = CARTESIAN_POINT ( 'NONE',  ( -4.458734124999999437, -82.39583333196773651, -2.574251347313719407 ) ) ;
#2518 = CARTESIAN_POINT ( 'NONE',  ( 4.458734124999999437, 22.93750000136559564, -5.460374474430324690E-16 ) ) ;
#2519 = CARTESIAN_POINT ( 'NONE',  ( 2.730187237215162345E-16, -149.4375000013656063, -4.458734124999999437 ) ) ;
#2520 = CARTESIAN_POINT ( 'NONE',  ( -4.458734124999998549, 22.77083333469892423, 2.574251347313722516 ) ) ;
#2521 = EDGE_CURVE ( 'NONE', #37292, #8165, #8808, .T. ) ;
#2522 = CARTESIAN_POINT ( 'NONE',  ( 1.975475456537005874E-15, -93.74999999999998579, 5.000000000000000000 ) ) ;
#2523 = CARTESIAN_POINT ( 'NONE',  ( 0.000000000000000000, 0.000000000000000000, 0.000000000000000000 ) ) ;
#2524 = CARTESIAN_POINT ( 'NONE',  ( -3.152548672688508926E-16, -82.81249999863442213, -5.148502694627439702 ) ) ;
#2525 = CARTESIAN_POINT ( 'NONE',  ( -5.000000000000000000, -64.00000000000000000, 0.000000000000000000 ) ) ;
#2526 = FACE_OUTER_BOUND ( 'NONE', #42486, .T. ) ;
#2527 = CARTESIAN_POINT ( 'NONE',  ( 2.499999999999998668, 16.79166666939785202, -4.330127018922193649 ) ) ;
#2528 = ORIENTED_EDGE ( 'NONE', *, *, #40622, .T. ) ;
#2529 = CARTESIAN_POINT ( 'NONE',  ( 1.975475456537005874E-15, -25.75000000000000355, 5.000000000000000000 ) ) ;
#2530 = CARTESIAN_POINT ( 'NONE',  ( -1.339745962155610259, 27.79465819873852084, -5.000000000000002665 ) ) ;
#2531 =( BOUNDED_CURVE ( )  B_SPLINE_CURVE ( 2, ( #32216, #12913, #12603, #36739, #8107, #51537, #61827, #28338, #3597 ),
 .UNSPECIFIED., .F., .F. ) 
 B_SPLINE_CURVE_WITH_KNOTS ( ( 3, 2, 2, 2, 3 ),
 ( 0.4562499999999999889, 0.4569444444444444309, 0.4583333333333333148, 0.4597222222222221988, 0.4604166666666666963 ),
 .UNSPECIFIED. ) 
 CURVE ( )  GEOMETRIC_REPRESENTATION_ITEM ( )  RATIONAL_B_SPLINE_CURVE ( ( 0.9330127018922194093, 0.9330127018922194093, 1.000000000000000000, 0.8660254037844387076, 1.000000000000000000, 0.8660254037844387076, 1.000000000000000000, 0.9330127018922167448, 0.9330127018922194093 ) ) 
 REPRESENTATION_ITEM ( '' )  );
#2533 = CARTESIAN_POINT ( 'NONE',  ( -5.000000000000000000, -24.00000000000000000, 0.000000000000000000 ) ) ;
#2532 = CARTESIAN_POINT ( 'NONE',  ( 2.500000000000002220, -52.66666666666666430, 4.330127018922192761 ) ) ;
#2534 = CARTESIAN_POINT ( 'NONE',  ( -2.229367062500000163, -26.47916666530106866, -3.861377020970580443 ) ) ;
#2535 = CARTESIAN_POINT ( 'NONE',  ( 9.457646018065525792E-16, -86.06249999863439371, 5.148502694627439702 ) ) ;
#2536 = CARTESIAN_POINT ( 'NONE',  ( 2.499999999999998668, -31.20833333060214443, -4.330127018922193649 ) ) ;
#2538 = VERTEX_POINT ( 'NONE', #1873 ) ;
#2537 = CARTESIAN_POINT ( 'NONE',  ( -2.229367062499996610, -56.14583333196773651, 3.861377020970582219 ) ) ;
#2539 = CARTESIAN_POINT ( 'NONE',  ( -51.75738570946856498, -137.8750000027312126, 3.805975901505576964 ) ) ;
#2541 = ORIENTED_EDGE ( 'NONE', *, *, #4646, .T. ) ;
#2540 = CARTESIAN_POINT ( 'NONE',  ( -3.152548672688508926E-16, -9.812499998634406140, -5.148502694627439702 ) ) ;
#2542 = CARTESIAN_POINT ( 'NONE',  ( 5.000000000000000000, -73.50000000000000000, -6.123233995736766282E-16 ) ) ;
#2543 = CARTESIAN_POINT ( 'NONE',  ( -59.59170313451810586, -137.5000000013656063, 1.485763867205729394 ) ) ;
#2544 = CARTESIAN_POINT ( 'NONE',  ( -2.229367062499996610, -51.39583333196773651, 3.861377020970582219 ) ) ;
#2545 = CARTESIAN_POINT ( 'NONE',  ( 0.000000000000000000, -170.0000000000000000, 0.000000000000000000 ) ) ;
#2546 = CARTESIAN_POINT ( 'NONE',  ( 2.500000000000002220, -77.54166666393547303, 4.330127018922192761 ) ) ;
#2548 = ORIENTED_EDGE ( 'NONE', *, *, #10235, .T. ) ;
#2547 = CARTESIAN_POINT ( 'NONE',  ( -2.499999999999996447, -81.70833333060213022, 4.330127018922195425 ) ) ;
#2549 = CARTESIAN_POINT ( 'NONE',  ( -51.19402409849444524, -149.5000000000000284, -3.242614290531456334 ) ) ;
#2550 = CARTESIAN_POINT ( 'NONE',  ( 4.458734124999998549, -15.97916666530107221, -2.574251347313721627 ) ) ;
#2551 = CARTESIAN_POINT ( 'NONE',  ( -2.229367062499996610, -51.39583333196773651, 3.861377020970582219 ) ) ;
#2552 = CARTESIAN_POINT ( 'NONE',  ( 1.975475456537005874E-15, 1.250000000000000000, 5.000000000000000000 ) ) ;
#2553 = PRESENTATION_STYLE_ASSIGNMENT (( #31807 ) ) ;
#2554 = CARTESIAN_POINT ( 'NONE',  ( -4.458734125000001214, -139.8750000013656063, 1.846868145590734089 ) ) ;
#2555 = CARTESIAN_POINT ( 'NONE',  ( 2.229367062500001939, -99.22916666530105090, 3.861377020970579999 ) ) ;
#2556 = CARTESIAN_POINT ( 'NONE',  ( 1.975475456537005874E-15, -35.62499999726880162, 5.000000000000000000 ) ) ;
#2557 = VERTEX_POINT ( 'NONE', #32302 ) ;
#2558 = CARTESIAN_POINT ( 'NONE',  ( -57.19623071787016499, -154.6250000013656063, 4.297418129356382899 ) ) ;
#2559 = CARTESIAN_POINT ( 'NONE',  ( -54.60164318462004474, -144.5000000027312126, -4.984105922594373794 ) ) ;
#2560 = CARTESIAN_POINT ( 'NONE',  ( 5.000000000000000000, -60.41666666666665719, -2.886751345948130876 ) ) ;
#2561 = CARTESIAN_POINT ( 'NONE',  ( 2.229367062499998831, 0.3541666680322609340, -3.861377020970580887 ) ) ;
#2562 = CARTESIAN_POINT ( 'NONE',  ( 9.457646018065525792E-16, -94.31249999863440792, 5.148502694627439702 ) ) ;
#2563 = CARTESIAN_POINT ( 'NONE',  ( 4.458734125000000326, -148.6250000013655779, -1.846868145590734978 ) ) ;
#2564 = CARTESIAN_POINT ( 'NONE',  ( 9.457646018065525792E-16, -21.31249999863440081, 5.148502694627439702 ) ) ;
#2565 = CARTESIAN_POINT ( 'NONE',  ( -5.000000000000000000, -67.08333333333332860, -2.886751345948128211 ) ) ;
#2566 = CARTESIAN_POINT ( 'NONE',  ( -53.51423613279429503, -136.2500000013656063, 4.591703134518082763 ) ) ;
#2567 = CARTESIAN_POINT ( 'NONE',  ( 9.457646018065525792E-16, -61.31249999863440792, 5.148502694627439702 ) ) ;
#2568 = CARTESIAN_POINT ( 'NONE',  ( -5.000000000000000888, -154.6875000027312126, -2.071067811865475949 ) ) ;
#2569 = CARTESIAN_POINT ( 'NONE',  ( 5.000000000000000000, 23.62500000273118417, -6.123233995736766282E-16 ) ) ;
#2570 = CARTESIAN_POINT ( 'NONE',  ( 4.458734124999997661, -146.5000000013656347, 1.846868145590737864 ) ) ;
#2571 = CARTESIAN_POINT ( 'NONE',  ( 2.229367062500001939, 11.77083333469892601, 3.861377020970579999 ) ) ;
#2572 = VERTEX_POINT ( 'NONE', #1550 ) ;
#2573 = CARTESIAN_POINT ( 'NONE',  ( -1.339745962155610925, -4.794658198738520838, 5.000000000000000000 ) ) ;
#2574 = CARTESIAN_POINT ( 'NONE',  ( 1.339745962155612702, -61.29465819873851729, -5.000000000000000000 ) ) ;
#2576 = CARTESIAN_POINT ( 'NONE',  ( -4.458734124999999437, -27.31249999863440081, 0.000000000000000000 ) ) ;
#2575 = CARTESIAN_POINT ( 'NONE',  ( -2.500000000000000444, -92.16666666666665719, -4.330127018922193649 ) ) ;
#2577 = CARTESIAN_POINT ( 'NONE',  ( 0.000000000000000000, -170.0000000000000000, 0.000000000000000000 ) ) ;
#2578 = CARTESIAN_POINT ( 'NONE',  ( -4.458734124999999437, -70.64583333196773651, -2.574251347313719407 ) ) ;
#2579 = CARTESIAN_POINT ( 'NONE',  ( 4.458734124999998549, 28.02083333469893134, -2.574251347313721627 ) ) ;
#2580 = DIRECTION ( 'NONE',  ( -0.000000000000000000, 1.000000000000000000, -0.000000000000000000 ) ) ;
#2581 = CARTESIAN_POINT ( 'NONE',  ( -50.40829686548195099, -146.0000000013656347, -1.485763867205728284 ) ) ;
#2582 = CARTESIAN_POINT ( 'NONE',  ( -3.535250795749689387E-16, -52.12499999726881583, -5.773502691896257311 ) ) ;
#2583 = CARTESIAN_POINT ( 'NONE',  ( 5.000000000000000000, -24.41666666666666430, -2.886751345948130876 ) ) ;
#2584 = CARTESIAN_POINT ( 'NONE',  ( -2.229367062500000163, 10.52083333469892779, -3.861377020970580443 ) ) ;
#2585 = CARTESIAN_POINT ( 'NONE',  ( 0.000000000000000000, -120.0000000000000000, 0.000000000000000000 ) ) ;
#2586 = CARTESIAN_POINT ( 'NONE',  ( 4.458734124999998549, 9.270833334698927786, -2.574251347313721627 ) ) ;
#2587 = CARTESIAN_POINT ( 'NONE',  ( 4.458734124999999437, -73.81249999863440792, -5.460374474430324690E-16 ) ) ;
#2588 = CARTESIAN_POINT ( 'NONE',  ( -3.152548672688508926E-16, -19.81249999863440081, -5.148502694627439702 ) ) ;
#2589 = CARTESIAN_POINT ( 'NONE',  ( 5.000000000000000888, 1.416666666666666741, 2.886751345948126879 ) ) ;
#2590 = CARTESIAN_POINT ( 'NONE',  ( -3.152801135295367985, -160.8125000013656063, 3.152801135295367096 ) ) ;
#2591 = CARTESIAN_POINT ( 'NONE',  ( 5.000000000000000888, 15.54166666939785202, 2.886751345948126879 ) ) ;
#2592 = CARTESIAN_POINT ( 'NONE',  ( -4.458734124999998549, -65.22916666530106511, 2.574251347313722516 ) ) ;
#2593 = CARTESIAN_POINT ( 'NONE',  ( 5.000000000000000000, -94.29166666393547303, -2.886751345948129988 ) ) ;
#2594 = AXIS2_PLACEMENT_3D ( 'NONE', #44281, #15661, #14382 ) ;
#2595 = CARTESIAN_POINT ( 'NONE',  ( -2.500000000000000444, -36.16666666666666430, -4.330127018922193649 ) ) ;
#2596 = CARTESIAN_POINT ( 'NONE',  ( 4.458734125000000326, -39.89583333196772941, 2.574251347313718519 ) ) ;
#2597 = CARTESIAN_POINT ( 'NONE',  ( -2.229367062499996610, -68.39583333196773651, 3.861377020970582219 ) ) ;
#2598 = CARTESIAN_POINT ( 'NONE',  ( 5.000000000000000000, -49.41666666666667140, -2.886751345948129988 ) ) ;
#2599 = CARTESIAN_POINT ( 'NONE',  ( 1.975475456537005874E-15, -22.74999999999999645, 5.000000000000000000 ) ) ;
#2600 = CARTESIAN_POINT ( 'NONE',  ( -6.972266317189433020E-16, 15.75000000000000000, -5.000000000000000000 ) ) ;
#2601 = ORIENTED_EDGE ( 'NONE', *, *, #27108, .F. ) ;
#2602 = CARTESIAN_POINT ( 'NONE',  ( -2.500000000000000444, -85.16666666666667140, -4.330127018922193649 ) ) ;
#2603 = CARTESIAN_POINT ( 'NONE',  ( -3.152548672688508926E-16, 0.1875000013655953035, -5.148502694627439702 ) ) ;
#2604 = CARTESIAN_POINT ( 'NONE',  ( -2.500000000000000444, -68.04166666393547303, -4.330127018922193649 ) ) ;
#2605 = CARTESIAN_POINT ( 'NONE',  ( -4.999999999999999112, -6.916666666666667851, 2.886751345948131764 ) ) ;
#2606 = CARTESIAN_POINT ( 'NONE',  ( 4.458734124999998549, -71.72916666530107932, -2.574251347313721627 ) ) ;
#2607 =( BOUNDED_CURVE ( )  B_SPLINE_CURVE ( 2, ( #61040, #21796, #55579, #1549, #16331, #26935, #56529, #55891, #51697 ),
 .UNSPECIFIED., .F., .F. ) 
 B_SPLINE_CURVE_WITH_KNOTS ( ( 3, 2, 2, 2, 3 ),
 ( 0.03750000000000000555, 0.03809523809523809867, 0.03928571428571428492, 0.04047619047619047811, 0.04107142857142857123 ),
 .UNSPECIFIED. ) 
 CURVE ( )  GEOMETRIC_REPRESENTATION_ITEM ( )  RATIONAL_B_SPLINE_CURVE ( ( 0.9330127018922194093, 0.9330127018922197424, 1.000000000000000000, 0.8660254037844387076, 1.000000000000000000, 0.8660254037844387076, 1.000000000000000000, 0.9330127018922194093, 0.9330127018922194093 ) ) 
 REPRESENTATION_ITEM ( '' )  );
#2608 = CARTESIAN_POINT ( 'NONE',  ( -4.999999999999998224, -5.916666666666666963, 2.886751345948131764 ) ) ;
#2609 = CARTESIAN_POINT ( 'NONE',  ( 1.060575238724906964E-15, -13.62499999726881050, 5.773502691896257311 ) ) ;
#2611 = VERTEX_POINT ( 'NONE', #13635 ) ;
#2610 = CARTESIAN_POINT ( 'NONE',  ( -4.458734124999999437, -41.31249999863440081, 0.000000000000000000 ) ) ;
#2612 = CARTESIAN_POINT ( 'NONE',  ( 2.500000000000002220, -100.5416666639354588, 4.330127018922192761 ) ) ;
#2614 = ORIENTED_EDGE ( 'NONE', *, *, #24363, .T. ) ;
#2613 = CARTESIAN_POINT ( 'NONE',  ( 4.458734124999999437, 9.937500001365593860, -5.460374474430324690E-16 ) ) ;
#2615 = CARTESIAN_POINT ( 'NONE',  ( -6.972266317189433020E-16, -53.24999999999999289, -5.000000000000000000 ) ) ;
#2616 = CARTESIAN_POINT ( 'NONE',  ( 2.499999999999998668, -53.33333333333332860, -4.330127018922193649 ) ) ;
#2617 = CARTESIAN_POINT ( 'NONE',  ( 1.846868145590735200, -160.5000000013656347, -4.458734125000000326 ) ) ;
#2618 = CARTESIAN_POINT ( 'NONE',  ( -2.229367062499996610, -36.39583333196773651, 3.861377020970582219 ) ) ;
#2619 = CARTESIAN_POINT ( 'NONE',  ( 0.000000000000000000, -170.0000000000000000, 5.000000000000000000 ) ) ;
#2620 = CARTESIAN_POINT ( 'NONE',  ( 4.458734124999999437, -80.81249999863440792, -5.460374474430324690E-16 ) ) ;
#2621 = CARTESIAN_POINT ( 'NONE',  ( -5.000000000000000888, -165.4375000000000000, 2.071067811865474617 ) ) ;
#2623 = ADVANCED_FACE ( 'NONE', ( #52248 ), #45910, .T. ) ;
#2622 = CARTESIAN_POINT ( 'NONE',  ( -4.458734124999998549, -88.22916666530107932, 2.574251347313722516 ) ) ;
#2624 = CARTESIAN_POINT ( 'NONE',  ( -57.89159099828107458, -130.9375000013656063, -3.393966926194107447 ) ) ;
#2625 = CARTESIAN_POINT ( 'NONE',  ( 4.458734125000001214, -1.145833331967740509, 2.574251347313718519 ) ) ;
#2626 = CARTESIAN_POINT ( 'NONE',  ( 4.458734124999998549, -36.97916666530107221, -2.574251347313721627 ) ) ;
#2627 = CARTESIAN_POINT ( 'NONE',  ( 5.000000000000000000, -70.29166666393547303, -2.886751345948130876 ) ) ;
#2628 = CARTESIAN_POINT ( 'NONE',  ( 9.457646018065525792E-16, -83.31249999863440792, 5.148502694627439702 ) ) ;
#2629 = CARTESIAN_POINT ( 'NONE',  ( -5.000000000000000000, 16.12500000273118417, 0.000000000000000000 ) ) ;
#2630 = ORIENTED_EDGE ( 'NONE', *, *, #56762, .F. ) ;
#2631 = LINE ( 'NONE', #27695, #20357 ) ;
#2632 = DIRECTION ( 'NONE',  ( -0.000000000000000000, 1.000000000000000000, -0.000000000000000000 ) ) ;
#2633 = CARTESIAN_POINT ( 'NONE',  ( 4.458734124999998549, -71.97916666530107932, -2.574251347313721627 ) ) ;
#2634 = CARTESIAN_POINT ( 'NONE',  ( -4.458734124999999437, -8.562499998634406140, 0.000000000000000000 ) ) ;
#2635 = ORIENTED_EDGE ( 'NONE', *, *, #62620, .F. ) ;
#2636 = VECTOR ( 'NONE', #36962, 1000.000000000000000 ) ;
#2637 = CARTESIAN_POINT ( 'NONE',  ( 2.500000000000002220, -5.666666666666666963, 4.330127018922192761 ) ) ;
#2638 = CARTESIAN_POINT ( 'NONE',  ( 2.499999999999998668, 2.791666669397851130, -4.330127018922193649 ) ) ;
#2639 = CARTESIAN_POINT ( 'NONE',  ( 4.458734124999998549, -6.979166665301073103, -2.574251347313721627 ) ) ;
#2640 = CARTESIAN_POINT ( 'NONE',  ( -58.24261429053147765, -148.3750000027312126, -3.805975901505573855 ) ) ;
#2641 = CARTESIAN_POINT ( 'NONE',  ( 2.229367062500001939, 5.020833334698926897, 3.861377020970579999 ) ) ;
#2642 = CARTESIAN_POINT ( 'NONE',  ( -2.499999999999996447, -32.70833333060215153, 4.330127018922195425 ) ) ;
#2643 = CARTESIAN_POINT ( 'NONE',  ( 1.846868145590735200, -155.2500000013656063, -4.458734124999999437 ) ) ;
#2644 = CARTESIAN_POINT ( 'NONE',  ( -2.229367062499996610, 26.60416666803225993, 3.861377020970582219 ) ) ;
#2645 = VERTEX_POINT ( 'NONE', #57400 ) ;
#2646 = CARTESIAN_POINT ( 'NONE',  ( -4.458734124999997661, -86.22916666530107932, 2.574251347313722516 ) ) ;
#2647 = CARTESIAN_POINT ( 'NONE',  ( -6.972266317189433020E-16, -97.24999999999998579, -5.000000000000000000 ) ) ;
#2648 = CARTESIAN_POINT ( 'NONE',  ( -4.458734124999999437, -10.31249999863440792, 0.000000000000000000 ) ) ;
#2649 = DIRECTION ( 'NONE',  ( -0.000000000000000000, 1.000000000000000000, -0.000000000000000000 ) ) ;
#2650 = FACE_OUTER_BOUND ( 'NONE', #1836, .T. ) ;
#2651 = CARTESIAN_POINT ( 'NONE',  ( 2.500000000000002220, -31.54166666393548724, 4.330127018922192761 ) ) ;
#2652 = CARTESIAN_POINT ( 'NONE',  ( -6.972266317189433020E-16, -23.24999999999999645, -5.000000000000000000 ) ) ;
#2653 = CARTESIAN_POINT ( 'NONE',  ( 2.229367062499998831, 24.35416666803225993, -3.861377020970580887 ) ) ;
#2654 = CARTESIAN_POINT ( 'NONE',  ( 5.000000000000000000, -7.500000000000000000, -6.123233995736766282E-16 ) ) ;
#2655 = CARTESIAN_POINT ( 'NONE',  ( 4.458734125000000326, 22.10416666803225993, 2.574251347313718519 ) ) ;
#2656 = CARTESIAN_POINT ( 'NONE',  ( 4.458734125000001214, -51.89583333196773651, 2.574251347313718519 ) ) ;
#2657 = CARTESIAN_POINT ( 'NONE',  ( -2.229367062499996610, -5.395833331967740953, 3.861377020970582219 ) ) ;
#2658 = FACE_OUTER_BOUND ( 'NONE', #50703, .T. ) ;
#2659 = CARTESIAN_POINT ( 'NONE',  ( -5.000000000000000000, 12.91666666666666785, -2.886751345948128211 ) ) ;
#2660 = CARTESIAN_POINT ( 'NONE',  ( 2.071067811865476394, -143.3125000027312126, 5.000000000000000000 ) ) ;
#2661 = CARTESIAN_POINT ( 'NONE',  ( 5.000000000000000000, -159.0625000000000284, 2.071067811865478614 ) ) ;
#2662 = CARTESIAN_POINT ( 'NONE',  ( -2.229367062499996610, -49.14583333196772941, 3.861377020970582219 ) ) ;
#2663 = CARTESIAN_POINT ( 'NONE',  ( -3.535250795749689387E-16, -81.12499999726881583, -5.773502691896257311 ) ) ;
#2664 = CARTESIAN_POINT ( 'NONE',  ( -58.39396692619412477, -140.6875000013656063, 2.891590998281057701 ) ) ;
#2665 = CARTESIAN_POINT ( 'NONE',  ( 0.000000000000000000, 0.000000000000000000, -9.974600000000000577 ) ) ;
#2666 = CARTESIAN_POINT ( 'NONE',  ( -4.999999999999998224, -87.91666666666667140, 2.886751345948131764 ) ) ;
#2667 = CARTESIAN_POINT ( 'NONE',  ( -2.229367062499996610, -83.39583333196773651, 3.861377020970582219 ) ) ;
#2668 = CARTESIAN_POINT ( 'NONE',  ( -3.152801135295367096, -163.3125000013656063, -3.152801135295367541 ) ) ;
#2669 = CARTESIAN_POINT ( 'NONE',  ( -2.499999999999996447, -30.83333333333333215, 4.330127018922195425 ) ) ;
#2670 = CARTESIAN_POINT ( 'NONE',  ( 0.000000000000000000, -120.0000000000000000, 0.000000000000000000 ) ) ;
#2671 = ORIENTED_EDGE ( 'NONE', *, *, #9855, .T. ) ;
#2672 = CARTESIAN_POINT ( 'NONE',  ( 9.457646018065525792E-16, 15.68750000136559386, 5.148502694627439702 ) ) ;
#2673 = ORIENTED_EDGE ( 'NONE', *, *, #4895, .F. ) ;
#2674 = CARTESIAN_POINT ( 'NONE',  ( 2.229367062499998831, -88.64583333196773651, -3.861377020970580887 ) ) ;
#2675 = CARTESIAN_POINT ( 'NONE',  ( 2.229367062499998831, 15.10416666803225993, -3.861377020970580887 ) ) ;
#2676 = CARTESIAN_POINT ( 'NONE',  ( -2.500000000000000444, 16.95833333606451987, -4.330127018922193649 ) ) ;
#2677 =( BOUNDED_CURVE ( )  B_SPLINE_CURVE ( 2, ( #42016, #2481, #46540, #61656, #22094, #18211, #37832, #41693, #37207 ),
 .UNSPECIFIED., .F., .F. ) 
 B_SPLINE_CURVE_WITH_KNOTS ( ( 3, 2, 2, 2, 3 ),
 ( 0.8053571428571428825, 0.8059523809523809756, 0.8071428571428571619, 0.8083333333333333481, 0.8089285714285714413 ),
 .UNSPECIFIED. ) 
 CURVE ( )  GEOMETRIC_REPRESENTATION_ITEM ( )  RATIONAL_B_SPLINE_CURVE ( ( 0.9330127018922194093, 0.9330127018922194093, 1.000000000000000000, 0.8660254037844387076, 1.000000000000000000, 0.8660254037844387076, 1.000000000000000000, 0.9330127018922194093, 0.9330127018922194093 ) ) 
 REPRESENTATION_ITEM ( '' )  );
#2678 = CARTESIAN_POINT ( 'NONE',  ( -2.499999999999996447, -34.70833333060213732, 4.330127018922195425 ) ) ;
#2679 = CARTESIAN_POINT ( 'NONE',  ( 1.060575238724906964E-15, 10.24999999999999822, 5.773502691896257311 ) ) ;
#2680 = CARTESIAN_POINT ( 'NONE',  ( -2.229367062499996610, -56.14583333196773651, 3.861377020970582219 ) ) ;
#2681 = AXIS2_PLACEMENT_3D ( 'NONE', #2146, #22705, #31706 ) ;
#2682 = CARTESIAN_POINT ( 'NONE',  ( -1.339745962155613812, 14.91965820146970678, -5.000000000000000000 ) ) ;
#2683 = CARTESIAN_POINT ( 'NONE',  ( 5.000000000000000000, -79.50000000000000000, -6.123233995736766282E-16 ) ) ;
#2684 = CARTESIAN_POINT ( 'NONE',  ( -5.000000000000000000, 19.99999999999999645, 0.000000000000000000 ) ) ;
#2685 = DIRECTION ( 'NONE',  ( 0.000000000000000000, 0.000000000000000000, 1.000000000000000000 ) ) ;
#2686 = FACE_OUTER_BOUND ( 'NONE', #1104, .T. ) ;
#2687 = CYLINDRICAL_SURFACE ( 'NONE', #7363, 5.000000000000000000 ) ;
#2688 = CARTESIAN_POINT ( 'NONE',  ( 2.500000000000002220, -40.66666666666667140, 4.330127018922192761 ) ) ;
#2689 = CARTESIAN_POINT ( 'NONE',  ( 3.535533905932736864, -149.1250000000000000, 3.535533905932738641 ) ) ;
#2691 = CARTESIAN_POINT ( 'NONE',  ( 4.458734124999999437, -19.06249999863440792, -5.460374474430324690E-16 ) ) ;
#2690 = CARTESIAN_POINT ( 'NONE',  ( -4.999999999999998224, -47.91666666666667140, 2.886751345948131764 ) ) ;
#2692 = CARTESIAN_POINT ( 'NONE',  ( -5.000000000000000888, -143.5625000000000568, -2.071067811865475949 ) ) ;
#2693 = CARTESIAN_POINT ( 'NONE',  ( 4.458734125000001214, -62.89583333196775072, 2.574251347313718519 ) ) ;
#2694 = CARTESIAN_POINT ( 'NONE',  ( 4.458734124999999437, -150.6875000013656063, 0.000000000000000000 ) ) ;
#2696 = EDGE_CURVE ( 'NONE', #42590, #21128, #32721, .T. ) ;
#2695 = CARTESIAN_POINT ( 'NONE',  ( -4.458734124999998549, -71.22916666530106511, 2.574251347313722516 ) ) ;
#2697 = CARTESIAN_POINT ( 'NONE',  ( -51.60603307380591787, -149.1875000013656063, -2.891590998281053704 ) ) ;
#2698 = CARTESIAN_POINT ( 'NONE',  ( -2.229367062499996610, -20.39583333196774007, 3.861377020970582219 ) ) ;
#2699 = CARTESIAN_POINT ( 'NONE',  ( -2.500000000000000444, -62.04166666393547303, -4.330127018922193649 ) ) ;
#2700 = VERTEX_POINT ( 'NONE', #3054 ) ;
#2701 = CARTESIAN_POINT ( 'NONE',  ( 6.123233995736766282E-16, -120.0000000000000000, -5.000000000000000000 ) ) ;
#2702 = ORIENTED_EDGE ( 'NONE', *, *, #18187, .T. ) ;
#2703 = CARTESIAN_POINT ( 'NONE',  ( 2.229367062499998831, -60.89583333196774362, -3.861377020970580887 ) ) ;
#2704 = CARTESIAN_POINT ( 'NONE',  ( 1.339745962155612702, -7.169658196007335782, -5.000000000000000000 ) ) ;
#2705 = CARTESIAN_POINT ( 'NONE',  ( 7.914973979435151463, 3.817460047930444134, -7.907502498112419786 ) ) ;
#2706 = CARTESIAN_POINT ( 'NONE',  ( 4.458734124999999437, -151.5000000013655779, 1.846868145590737864 ) ) ;
#2707 = VERTEX_POINT ( 'NONE', #13002 ) ;
#2708 =( BOUNDED_CURVE ( )  B_SPLINE_CURVE ( 2, ( #53966, #14408, #34030, #29830, #49462, #25019, #53651, #49138, #58791 ),
 .UNSPECIFIED., .F., .F. ) 
 B_SPLINE_CURVE_WITH_KNOTS ( ( 3, 2, 2, 2, 3 ),
 ( 0.2416666666666668628, 0.2458333333333335147, 0.2500000000000002220, 0.2541666666666668739, 0.2583333333333335813 ),
 .UNSPECIFIED. ) 
 CURVE ( )  GEOMETRIC_REPRESENTATION_ITEM ( )  RATIONAL_B_SPLINE_CURVE ( ( 0.9999999999999964473, 0.9238795325112902912, 1.000000000000000000, 0.9238795325112867385, 1.000000000000000000, 0.9238795325112867385, 1.000000000000000000, 0.9238795325112826307, 1.000000000000003997 ) ) 
 REPRESENTATION_ITEM ( '' )  );
#2709 = CARTESIAN_POINT ( 'NONE',  ( -54.60164318462004474, -127.3750000000000142, -4.984105922594373794 ) ) ;
#2710 = DIRECTION ( 'NONE',  ( 0.000000000000000000, 0.000000000000000000, 1.000000000000000000 ) ) ;
#2711 = CARTESIAN_POINT ( 'NONE',  ( 2.229367062499998831, -54.89583333196773651, -3.861377020970580887 ) ) ;
#2712 = ORIENTED_EDGE ( 'NONE', *, *, #56737, .T. ) ;
#2713 = EDGE_CURVE ( 'NONE', #51834, #61074, #13321, .T. ) ;
#2714 = CARTESIAN_POINT ( 'NONE',  ( 1.975475456537005874E-15, -45.74999999999999289, 5.000000000000000000 ) ) ;
#2715 = EDGE_CURVE ( 'NONE', #21692, #17887, #31115, .T. ) ;
#2716 = CARTESIAN_POINT ( 'NONE',  ( 2.229367062499998831, 9.354166668032261711, -3.861377020970580887 ) ) ;
#2717 = CARTESIAN_POINT ( 'NONE',  ( -2.229367062499996610, 23.85416666803225993, 3.861377020970582219 ) ) ;
#2718 = CARTESIAN_POINT ( 'NONE',  ( -56.48576386720575471, -147.7500000013655779, -4.591703134518078322 ) ) ;
#2719 = CARTESIAN_POINT ( 'NONE',  ( -4.458734124999999437, -169.0000000013655779, -1.846868145590735644 ) ) ;
#2720 = AXIS2_PLACEMENT_3D ( 'NONE', #6000, #60350, #59706 ) ;
#2721 = VERTEX_POINT ( 'NONE', #47104 ) ;
#2722 = CARTESIAN_POINT ( 'NONE',  ( 4.458734124999998549, -68.72916666530107932, -2.574251347313721627 ) ) ;
#2723 = CARTESIAN_POINT ( 'NONE',  ( 5.000000000000000000, -10.29166666393547658, -2.886751345948130876 ) ) ;
#2724 = CARTESIAN_POINT ( 'NONE',  ( 2.229367062499998831, 11.35416666803225993, -3.861377020970580887 ) ) ;
#2725 = AXIS2_PLACEMENT_3D ( 'NONE', #11968, #7798, #51231 ) ;
#2726 = EDGE_CURVE ( 'NONE', #20337, #16995, #39645, .T. ) ;
#2727 = VECTOR ( 'NONE', #57635, 1000.000000000000000 ) ;
#2728 = CARTESIAN_POINT ( 'NONE',  ( 5.000000000000000000, -69.29166666393547303, -2.886751345948130876 ) ) ;
#2729 = CARTESIAN_POINT ( 'NONE',  ( -4.458734124999999437, -57.64583333196773651, -2.574251347313719407 ) ) ;
#2730 = CARTESIAN_POINT ( 'NONE',  ( -3.535250795749689387E-16, -16.12499999726881228, -5.773502691896257311 ) ) ;
#2731 = CARTESIAN_POINT ( 'NONE',  ( -6.972266317189433020E-16, -77.12499999726881583, -5.000000000000000000 ) ) ;
#2732 = CARTESIAN_POINT ( 'NONE',  ( 1.975475456537005874E-15, -57.62499999726880873, 5.000000000000000000 ) ) ;
#2733 = CARTESIAN_POINT ( 'NONE',  ( -4.458734124999999437, -34.39583333196772941, -2.574251347313719407 ) ) ;
#2734 = CARTESIAN_POINT ( 'NONE',  ( 4.458734124999998549, -23.97916666530107577, -2.574251347313721627 ) ) ;
#2735 = ORIENTED_EDGE ( 'NONE', *, *, #20076, .F. ) ;
#2736 = CARTESIAN_POINT ( 'NONE',  ( -5.000000000000000000, -4.874999997268810503, 0.000000000000000000 ) ) ;
#2737 = CARTESIAN_POINT ( 'NONE',  ( 2.229367062500001939, -107.9791666653010651, 3.861377020970579999 ) ) ;
#2738 = CARTESIAN_POINT ( 'NONE',  ( -5.000000000000000000, -153.6250000027312126, -6.123233995736766282E-16 ) ) ;
#2739 = ORIENTED_EDGE ( 'NONE', *, *, #44055, .F. ) ;
#2740 = CARTESIAN_POINT ( 'NONE',  ( -2.229367062500000163, -103.7291666653010651, -3.861377020970580443 ) ) ;
#2741 = CARTESIAN_POINT ( 'NONE',  ( -4.458734124999999437, -25.31249999863440792, 0.000000000000000000 ) ) ;
#2742 = CARTESIAN_POINT ( 'NONE',  ( 5.000000000000000000, -61.37499999726880873, -6.123233995736766282E-16 ) ) ;
#2743 = CARTESIAN_POINT ( 'NONE',  ( -52.10840900171896806, -152.4375000013656063, 3.393966926194110556 ) ) ;
#2744 = CARTESIAN_POINT ( 'NONE',  ( 2.071067811865476394, -146.1875000000000284, 5.000000000000000000 ) ) ;
#2745 = EDGE_CURVE ( 'NONE', #1059, #23096, #39273, .T. ) ;
#2746 = CARTESIAN_POINT ( 'NONE',  ( -2.229367062499996610, -31.14583333196773651, 3.861377020970582219 ) ) ;
#2747 = CARTESIAN_POINT ( 'NONE',  ( 9.457646018065525792E-16, -72.31249999863439371, 5.148502694627439702 ) ) ;
#2748 = CARTESIAN_POINT ( 'NONE',  ( -1.339745962155613812, -40.08034179853028434, -5.000000000000000000 ) ) ;
#2749 = CARTESIAN_POINT ( 'NONE',  ( 4.458734125000000326, -24.89583333196773651, 2.574251347313718519 ) ) ;
#2750 = CARTESIAN_POINT ( 'NONE',  ( 5.000000000000000000, -32.29166666393548724, -2.886751345948130876 ) ) ;
#2751 = FACE_OUTER_BOUND ( 'NONE', #28852, .T. ) ;
#2752 = CARTESIAN_POINT ( 'NONE',  ( -4.999999999999999112, -16.91666666666666430, 2.886751345948131764 ) ) ;
#2753 = CARTESIAN_POINT ( 'NONE',  ( 1.846868145590735200, -151.2500000013656063, -4.458734125000000326 ) ) ;
#2754 = VERTEX_POINT ( 'NONE', #18463 ) ;
#2755 = CARTESIAN_POINT ( 'NONE',  ( -4.458734124999999437, -49.64583333196772941, -2.574251347313719407 ) ) ;
#2756 = CYLINDRICAL_SURFACE ( 'NONE', #57184, 5.000000000000000000 ) ;
#2757 = CARTESIAN_POINT ( 'NONE',  ( -6.972266317189433020E-16, -8.124999997268814056, -5.000000000000000000 ) ) ;
#2758 = CARTESIAN_POINT ( 'NONE',  ( 2.500000000000002220, 25.33333333333333215, 4.330127018922192761 ) ) ;
#2759 = CARTESIAN_POINT ( 'NONE',  ( -6.972266317189433020E-16, 7.750000000000000000, -5.000000000000000000 ) ) ;
#2760 = CARTESIAN_POINT ( 'NONE',  ( -4.458734124999998549, -0.2291666653010705768, 2.574251347313722516 ) ) ;
#2761 = CARTESIAN_POINT ( 'NONE',  ( 1.243387493232115550E-13, -20.12499999726881228, -5.000000000000000000 ) ) ;
#2762 = CARTESIAN_POINT ( 'NONE',  ( -5.000000000000000000, -80.95833333060214443, -2.886751345948128211 ) ) ;
#2763 = CARTESIAN_POINT ( 'NONE',  ( 0.000000000000000000, -120.0000000000000000, 5.000000000000000000 ) ) ;
#2764 = CARTESIAN_POINT ( 'NONE',  ( 4.458734124999998549, 15.02083333469892601, -2.574251347313721627 ) ) ;
#2765 = CARTESIAN_POINT ( 'NONE',  ( -4.999999999999999112, 5.208333336064518981, 2.886751345948131764 ) ) ;
#2766 = ORIENTED_EDGE ( 'NONE', *, *, #63624, .T. ) ;
#2767 = CARTESIAN_POINT ( 'NONE',  ( -2.500000000000000444, -30.04166666393548013, -4.330127018922193649 ) ) ;
#2768 = ORIENTED_EDGE ( 'NONE', *, *, #17370, .T. ) ;
#2769 = VECTOR ( 'NONE', #9044, 1000.000000000000000 ) ;
#2770 = CARTESIAN_POINT ( 'NONE',  ( -2.499999999999996447, -23.70833333060214443, 4.330127018922195425 ) ) ;
#2771 = CARTESIAN_POINT ( 'NONE',  ( -3.152548672688508926E-16, -50.56249999863440792, -5.148502694627439702 ) ) ;
#2772 = CARTESIAN_POINT ( 'NONE',  ( 4.458734124999999437, -163.6875000013655779, 0.000000000000000000 ) ) ;
#2773 = ADVANCED_FACE ( 'NONE', ( #21478 ), #57710, .T. ) ;
#2774 = EDGE_CURVE ( 'NONE', #57091, #47264, #46252, .T. ) ;
#2775 = CARTESIAN_POINT ( 'NONE',  ( -3.535250795749689387E-16, -46.12499999726881583, -5.773502691896257311 ) ) ;
#2776 = EDGE_CURVE ( 'NONE', #21697, #14134, #35538, .T. ) ;
#2777 = ORIENTED_EDGE ( 'NONE', *, *, #27801, .T. ) ;
#2778 = CARTESIAN_POINT ( 'NONE',  ( -4.458734124999999437, -22.31249999863440436, 0.000000000000000000 ) ) ;
#2779 = ORIENTED_EDGE ( 'NONE', *, *, #35022, .F. ) ;
#2780 = CARTESIAN_POINT ( 'NONE',  ( 5.000000000000000888, -85.58333333333332860, 2.886751345948126879 ) ) ;
#2781 = CARTESIAN_POINT ( 'NONE',  ( -8.190561711645485556E-16, -162.6875000013655779, 4.458734124999999437 ) ) ;
#2782 = CARTESIAN_POINT ( 'NONE',  ( -1.339745962155613812, -39.08034179853028434, -5.000000000000000000 ) ) ;
#2783 = CARTESIAN_POINT ( 'NONE',  ( -56.66612745406270335, -136.3125000000000000, -5.149110718188516067 ) ) ;
#2784 = CARTESIAN_POINT ( 'NONE',  ( -4.458734124999999437, -34.64583333196773651, -2.574251347313719407 ) ) ;
#2785 = CARTESIAN_POINT ( 'NONE',  ( -2.498395430326213474E-14, 20.37500000273118062, 5.000000000000000000 ) ) ;
#2786 = VERTEX_POINT ( 'NONE', #4602 ) ;
#2787 =( BOUNDED_CURVE ( )  B_SPLINE_CURVE ( 2, ( #37216, #12125, #52328, #56842, #41071, #47485, #2808, #51056, #7000 ),
 .UNSPECIFIED., .F., .F. ) 
 B_SPLINE_CURVE_WITH_KNOTS ( ( 3, 2, 2, 2, 3 ),
 ( 0.8562499999999999556, 0.8569444444444443976, 0.8583333333333332815, 0.8597222222222222765, 0.8604166666666667185 ),
 .UNSPECIFIED. ) 
 CURVE ( )  GEOMETRIC_REPRESENTATION_ITEM ( )  RATIONAL_B_SPLINE_CURVE ( ( 0.9330127018922194093, 0.9330127018922194093, 1.000000000000000000, 0.8660254037844387076, 1.000000000000000000, 0.8660254037844387076, 1.000000000000000000, 0.9330127018922194093, 0.9330127018922194093 ) ) 
 REPRESENTATION_ITEM ( '' )  );
#2788 = CARTESIAN_POINT ( 'NONE',  ( -2.229367062500000163, -81.47916666530106511, -3.861377020970580443 ) ) ;
#2789 = ADVANCED_FACE ( 'NONE', ( #54460 ), #39016, .F. ) ;
#2790 = CARTESIAN_POINT ( 'NONE',  ( 9.457646018065525792E-16, 21.93750000136559208, 5.148502694627439702 ) ) ;
#2791 = CARTESIAN_POINT ( 'NONE',  ( 1.339745962155612702, -18.29465819873851729, -5.000000000000000000 ) ) ;
#2792 = VERTEX_POINT ( 'NONE', #19715 ) ;
#2793 = DIRECTION ( 'NONE',  ( -0.000000000000000000, 1.000000000000000000, -0.000000000000000000 ) ) ;
#2794 = CARTESIAN_POINT ( 'NONE',  ( -53.51423613279429503, -140.5000000013655779, 4.591703134518083651 ) ) ;
#2795 = CARTESIAN_POINT ( 'NONE',  ( -4.458734124999999437, -78.64583333196773651, -2.574251347313719407 ) ) ;
#2796 = CARTESIAN_POINT ( 'NONE',  ( -53.33387254593733928, -129.9375000027312126, 5.149110718188519620 ) ) ;
#2797 = CARTESIAN_POINT ( 'NONE',  ( 5.000000000000000000, -74.37499999726880162, -6.123233995736766282E-16 ) ) ;
#2798 = CARTESIAN_POINT ( 'NONE',  ( -6.972266317189433020E-16, -9.250000000000000000, -5.000000000000000000 ) ) ;
#2799 = CARTESIAN_POINT ( 'NONE',  ( 2.071067811865560326, -144.9375000027311842, -4.999999999999914735 ) ) ;
#2800 = CARTESIAN_POINT ( 'NONE',  ( -2.229367062500000163, -53.47916666530107221, -3.861377020970580443 ) ) ;
#2801 = CARTESIAN_POINT ( 'NONE',  ( -1.339745962155613812, -85.08034179853028434, -5.000000000000000000 ) ) ;
#2802 = CARTESIAN_POINT ( 'NONE',  ( -2.229367062499996610, 28.85416666803226349, 3.861377020970582219 ) ) ;
#2803 = CARTESIAN_POINT ( 'NONE',  ( -3.535250795749689387E-16, -109.2499999999999858, -5.773502691896257311 ) ) ;
#2804 =( BOUNDED_CURVE ( )  B_SPLINE_CURVE ( 2, ( #31119, #16336, #45915, #49468, #1877, #39488, #54616, #15057, #594 ),
 .UNSPECIFIED., .F., .F. ) 
 B_SPLINE_CURVE_WITH_KNOTS ( ( 3, 2, 2, 2, 3 ),
 ( 0.7553571428571428381, 0.7559523809523809312, 0.7571428571428571175, 0.7583333333333333037, 0.7589285714285713969 ),
 .UNSPECIFIED. ) 
 CURVE ( )  GEOMETRIC_REPRESENTATION_ITEM ( )  RATIONAL_B_SPLINE_CURVE ( ( 0.9330127018922194093, 0.9330127018922194093, 1.000000000000000000, 0.8660254037844387076, 1.000000000000000000, 0.8660254037844387076, 1.000000000000000000, 0.9330127018922194093, 0.9330127018922194093 ) ) 
 REPRESENTATION_ITEM ( '' )  );
#2805 = CARTESIAN_POINT ( 'NONE',  ( 0.000000000000000000, -120.0000000000000000, 5.000000000000000000 ) ) ;
#2806 = CARTESIAN_POINT ( 'NONE',  ( 4.458734124999999437, -38.06249999863440792, -5.460374474430324690E-16 ) ) ;
#2807 = CARTESIAN_POINT ( 'NONE',  ( 1.060575238724906964E-15, 0.3750000027311871098, 5.773502691896257311 ) ) ;
#2808 = CARTESIAN_POINT ( 'NONE',  ( -2.500000000000000444, -73.16666666666665719, -4.330127018922193649 ) ) ;
#2809 = CARTESIAN_POINT ( 'NONE',  ( -54.64476657466781973, -124.8125000013655921, -4.444560631937228834 ) ) ;
#2810 = CARTESIAN_POINT ( 'NONE',  ( 2.229367062500001939, -80.22916666530106511, 3.861377020970579999 ) ) ;
#2811 = CARTESIAN_POINT ( 'NONE',  ( 4.458734124999999437, -102.8124999986344079, -5.460374474430324690E-16 ) ) ;
#2812 = CARTESIAN_POINT ( 'NONE',  ( -4.458734124999999437, -4.645833331967739177, -2.574251347313719407 ) ) ;
#2813 = ORIENTED_EDGE ( 'NONE', *, *, #32159, .F. ) ;
#2814 = CIRCLE ( 'NONE', #11006, 5.000000000000000000 ) ;
#2815 = CARTESIAN_POINT ( 'NONE',  ( 0.000000000000000000, -170.0000000000000000, 5.000000000000000000 ) ) ;
#2816 = CARTESIAN_POINT ( 'NONE',  ( 4.458734124999999437, -93.81249999863440792, -5.460374474430324690E-16 ) ) ;
#2817 = CARTESIAN_POINT ( 'NONE',  ( 3.535533905932736864, -164.2500000027312126, 3.535533905932738641 ) ) ;
#2818 = CARTESIAN_POINT ( 'NONE',  ( -3.152548672688508926E-16, -88.81249999863439371, -5.148502694627439702 ) ) ;
#2819=STYLED_ITEM('',(#63698),#7586);
#2820 = CARTESIAN_POINT ( 'NONE',  ( 9.457646018065525792E-16, 12.68750000136559208, 5.148502694627439702 ) ) ;
#2821 = CARTESIAN_POINT ( 'NONE',  ( 6.158835246850667461E-14, -2.124999997268816276, -4.999999999999999112 ) ) ;
#2822 = VECTOR ( 'NONE', #33796, 1000.000000000000000 ) ;
#2823 = CARTESIAN_POINT ( 'NONE',  ( -55.35523342533222291, -135.3125000013656063, 4.444560631937231499 ) ) ;
#2824 = CARTESIAN_POINT ( 'NONE',  ( 2.229367062500001939, -11.97916666530107044, 3.861377020970579999 ) ) ;
#2825 = CARTESIAN_POINT ( 'NONE',  ( -4.458734124999999437, 18.35416666803225993, -2.574251347313719407 ) ) ;
#2826 = CARTESIAN_POINT ( 'NONE',  ( 4.458734124999999437, -52.06249999863440792, -5.460374474430324690E-16 ) ) ;
#2827 = DIRECTION ( 'NONE',  ( 0.000000000000000000, 0.000000000000000000, -1.000000000000000000 ) ) ;
#2828 = CARTESIAN_POINT ( 'NONE',  ( -1.339745962155610925, -105.7946581987385315, 5.000000000000000000 ) ) ;
#2829 = CARTESIAN_POINT ( 'NONE',  ( 9.457646018065525792E-16, -8.062499998634404363, 5.148502694627439702 ) ) ;
#2830 = DIRECTION ( 'NONE',  ( -0.000000000000000000, 1.000000000000000000, -0.000000000000000000 ) ) ;
#2831 = ORIENTED_EDGE ( 'NONE', *, *, #18533, .T. ) ;
#2832 = CARTESIAN_POINT ( 'NONE',  ( -2.229367062499996610, -34.39583333196772941, 3.861377020970582219 ) ) ;
#2833 = CARTESIAN_POINT ( 'NONE',  ( -55.35523342533222291, -126.5625000013655921, 4.444560631937231499 ) ) ;
#2834 = CARTESIAN_POINT ( 'NONE',  ( 5.000000000000000000, 26.70833333606451632, -2.886751345948130876 ) ) ;
#2835 = CARTESIAN_POINT ( 'NONE',  ( -3.152548672688508926E-16, -77.56249999863440792, -5.148502694627439702 ) ) ;
#2836 = CARTESIAN_POINT ( 'NONE',  ( -3.152548672688508926E-16, 24.18750000136559564, -5.148502694627439702 ) ) ;
#2837 = CARTESIAN_POINT ( 'NONE',  ( -4.458734124999999437, -149.1875000013656063, -5.460374474430324690E-16 ) ) ;
#2838 = CARTESIAN_POINT ( 'NONE',  ( -2.229367062500000163, 17.52083333469892779, -3.861377020970580443 ) ) ;
#2839 = LINE ( 'NONE', #37245, #25673 ) ;
#2840 = CARTESIAN_POINT ( 'NONE',  ( -54.60164318462004474, -137.5000000027312126, -4.984105922594373794 ) ) ;
#2841 = CARTESIAN_POINT ( 'NONE',  ( -4.458734124999997661, -82.47916666530106511, 2.574251347313722516 ) ) ;
#2842 = CARTESIAN_POINT ( 'NONE',  ( 5.000000000000000888, -62.58333333333333570, 2.886751345948126879 ) ) ;
#2843 = CARTESIAN_POINT ( 'NONE',  ( 0.000000000000000000, -120.0000000000000000, 0.000000000000000000 ) ) ;
#2844 = CARTESIAN_POINT ( 'NONE',  ( 5.000000000000000888, 16.54166666939785202, 2.886751345948126879 ) ) ;
#2845 = ORIENTED_EDGE ( 'NONE', *, *, #59869, .T. ) ;
#2846 = CARTESIAN_POINT ( 'NONE',  ( 1.975475456537005874E-15, -18.62499999726881228, 5.000000000000000000 ) ) ;
#2847 = CARTESIAN_POINT ( 'NONE',  ( 2.500000000000002220, 7.333333333333333925, 4.330127018922192761 ) ) ;
#2849 = CARTESIAN_POINT ( 'NONE',  ( 2.500000000000002220, -21.66666666666666785, 4.330127018922192761 ) ) ;
#2848 = CARTESIAN_POINT ( 'NONE',  ( -5.000000000000000000, -108.9583333306021586, -2.886751345948128211 ) ) ;
#2850 = CARTESIAN_POINT ( 'NONE',  ( -3.152548672688508926E-16, -25.56249999863440436, -5.148502694627439702 ) ) ;
#2851 = CYLINDRICAL_SURFACE ( 'NONE', #652, 5.000000000000000000 ) ;
#2852 = ADVANCED_FACE ( 'NONE', ( #39324 ), #58956, .T. ) ;
#2853 = CARTESIAN_POINT ( 'NONE',  ( -4.999999999999999112, -28.79166666393548013, 2.886751345948131764 ) ) ;
#2855 = VERTEX_POINT ( 'NONE', #34186 ) ;
#2854 = CARTESIAN_POINT ( 'NONE',  ( 4.458734124999998549, -61.72916666530106511, -2.574251347313721627 ) ) ;
#2856 = CARTESIAN_POINT ( 'NONE',  ( -59.44456063193725015, -153.8125000013656347, -0.3552334253322034230 ) ) ;
#2858 = EDGE_LOOP ( 'NONE', ( #51614, #47847, #21108, #28499 ) ) ;
#2857 = CARTESIAN_POINT ( 'NONE',  ( -3.152548672688508926E-16, -10.81249999863440792, -5.148502694627439702 ) ) ;
#2859 = CARTESIAN_POINT ( 'NONE',  ( 5.000000000000000888, -69.58333333333332860, 2.886751345948126879 ) ) ;
#2860 = CARTESIAN_POINT ( 'NONE',  ( -50.55543936806279248, -138.0625000013656063, 0.3552334253322060320 ) ) ;
#2861 = CARTESIAN_POINT ( 'NONE',  ( -4.458734124999998549, -53.47916666530106511, 2.574251347313722516 ) ) ;
#2862 =( BOUNDED_CURVE ( )  B_SPLINE_CURVE ( 2, ( #8989, #13814, #33746, #53363, #39511, #63346, #14749, #23478, #43081 ),
 .UNSPECIFIED., .F., .F. ) 
 B_SPLINE_CURVE_WITH_KNOTS ( ( 3, 2, 2, 2, 3 ),
 ( 0.8604166666666667185, 0.8611111111111111605, 0.8625000000000000444, 0.8638888888888889284, 0.8645833333333333703 ),
 .UNSPECIFIED. ) 
 CURVE ( )  GEOMETRIC_REPRESENTATION_ITEM ( )  RATIONAL_B_SPLINE_CURVE ( ( 0.9330127018922194093, 0.9330127018922194093, 1.000000000000000000, 0.8660254037844387076, 1.000000000000000000, 0.8660254037844387076, 1.000000000000000000, 0.9330127018922194093, 0.9330127018922194093 ) ) 
 REPRESENTATION_ITEM ( '' )  );
#2863 = EDGE_CURVE ( 'NONE', #20764, #3550, #59279, .T. ) ;
#2864 = AXIS2_PLACEMENT_3D ( 'NONE', #6988, #26600, #46216 ) ;
#2865 = CARTESIAN_POINT ( 'NONE',  ( -5.000000000000000000, -74.95833333060214443, -2.886751345948128211 ) ) ;
#2867 = VERTEX_POINT ( 'NONE', #53808 ) ;
#2866 = CARTESIAN_POINT ( 'NONE',  ( -6.972266317189433020E-16, -86.25000000000001421, -5.000000000000000000 ) ) ;
#2868 = CARTESIAN_POINT ( 'NONE',  ( -51.19402409849444524, -148.5000000000000284, -3.242614290531456334 ) ) ;
#2869 = VECTOR ( 'NONE', #6150, 1000.000000000000000 ) ;
#2870 = EDGE_CURVE ( 'NONE', #45174, #20081, #52824, .T. ) ;
#2871 = CARTESIAN_POINT ( 'NONE',  ( 2.229367062499998831, -13.89583333196774184, -3.861377020970580887 ) ) ;
#2872 = ADVANCED_FACE ( 'NONE', ( #4299 ), #23612, .T. ) ;
#2873 = CARTESIAN_POINT ( 'NONE',  ( 9.457646018065525792E-16, -58.31249999863440792, 5.148502694627439702 ) ) ;
#2874 = CARTESIAN_POINT ( 'NONE',  ( 1.975475456537005874E-15, -23.75000000000000000, 5.000000000000000000 ) ) ;
#2875 = SURFACE_SIDE_STYLE ('',( #16706 ) ) ;
#2876 = CARTESIAN_POINT ( 'NONE',  ( -3.152801135295367985, -169.0625000013656063, 3.152801135295367096 ) ) ;
#2877 = CARTESIAN_POINT ( 'NONE',  ( 9.457646018065525792E-16, -99.31249999863442213, 5.148502694627439702 ) ) ;
#2878 = CARTESIAN_POINT ( 'NONE',  ( 5.000000000000000000, -148.1875000027312126, 2.071067811865478614 ) ) ;
#2879 = ORIENTED_EDGE ( 'NONE', *, *, #15258, .F. ) ;
#2880 = EDGE_CURVE ( 'NONE', #63081, #9589, #45866, .T. ) ;
#2881 = CARTESIAN_POINT ( 'NONE',  ( -58.39396692619412477, -153.6875000013656063, 2.891590998281057701 ) ) ;
#2882 = CARTESIAN_POINT ( 'NONE',  ( -52.53715891517739323, -141.5625000027312126, -4.819101127000233298 ) ) ;
#2883 = EDGE_CURVE ( 'NONE', #30981, #63093, #28573, .T. ) ;
#2884 = CARTESIAN_POINT ( 'NONE',  ( -6.972266317189433020E-16, -60.24999999999999289, -5.000000000000000000 ) ) ;
#2885 = CARTESIAN_POINT ( 'NONE',  ( 2.229367062500001939, -6.979166665301073103, 3.861377020970579999 ) ) ;
#2886 = CARTESIAN_POINT ( 'NONE',  ( -4.458734124999997661, -94.47916666530106511, 2.574251347313722516 ) ) ;
#2887 = EDGE_CURVE ( 'NONE', #483, #4248, #10921, .T. ) ;
#2888 = CARTESIAN_POINT ( 'NONE',  ( 3.152801135295367541, -146.5625000013655779, -3.152801135295367541 ) ) ;
#2889 = CARTESIAN_POINT ( 'NONE',  ( -4.458734124999999437, -20.64583333196774007, -2.574251347313719407 ) ) ;
#2890 = CARTESIAN_POINT ( 'NONE',  ( -7.500000000000000000, 0.7513028741560130452, -0.02472015219302865774 ) ) ;
#2891 = CARTESIAN_POINT ( 'NONE',  ( -50.70258187064364108, -137.1250000013655779, 2.196230717870141014 ) ) ;
#2892 = CARTESIAN_POINT ( 'NONE',  ( 4.458734125000001214, -61.14583333196773651, 2.574251347313718519 ) ) ;
#2893 = CARTESIAN_POINT ( 'NONE',  ( 7.808623696107353851, 4.508310992947591522, -7.999704684617483963 ) ) ;
#2894 = CYLINDRICAL_SURFACE ( 'NONE', #47020, 5.000000000000000000 ) ;
#2895 = CARTESIAN_POINT ( 'NONE',  ( 4.458734124999999437, -145.3750000013656063, -1.846868145590734978 ) ) ;
#2896 = CARTESIAN_POINT ( 'NONE',  ( 9.457646018065525792E-16, 9.687500001365593860, 5.148502694627439702 ) ) ;
#2897 = VERTEX_POINT ( 'NONE', #40295 ) ;
#2898 = DIRECTION ( 'NONE',  ( 0.000000000000000000, 0.000000000000000000, 1.000000000000000000 ) ) ;
#2899 = CARTESIAN_POINT ( 'NONE',  ( 1.975475456537005874E-15, -61.74999999999999289, 5.000000000000000000 ) ) ;
#2901 = CARTESIAN_POINT ( 'NONE',  ( -2.229367062499996610, -23.14583333196773651, 3.861377020970582219 ) ) ;
#2900 = CARTESIAN_POINT ( 'NONE',  ( 2.500000000000002220, -91.66666666666665719, 4.330127018922192761 ) ) ;
#2902 = FACE_OUTER_BOUND ( 'NONE', #19370, .T. ) ;
#2903 = CARTESIAN_POINT ( 'NONE',  ( 2.229367062500001939, -73.22916666530107932, 3.861377020970579999 ) ) ;
#2904 = CARTESIAN_POINT ( 'NONE',  ( 2.229367062500001939, 27.77083333469892779, 3.861377020970579999 ) ) ;
#2905 = CARTESIAN_POINT ( 'NONE',  ( 0.000000000000000000, -170.0000000000000000, 0.000000000000000000 ) ) ;
#2906 = CARTESIAN_POINT ( 'NONE',  ( -50.55543936806279248, -147.0625000013656063, 0.3552334253322060320 ) ) ;
#2907 = CARTESIAN_POINT ( 'NONE',  ( 4.458734125000000326, 6.104166668032262599, 2.574251347313718519 ) ) ;
#2908 = DIRECTION ( 'NONE',  ( 0.000000000000000000, 0.000000000000000000, 1.000000000000000000 ) ) ;
#2909 = FACE_OUTER_BOUND ( 'NONE', #15655, .T. ) ;
#2910 = CARTESIAN_POINT ( 'NONE',  ( -4.458734124999997661, 8.770833334698927786, 2.574251347313722516 ) ) ;
#2911 = CARTESIAN_POINT ( 'NONE',  ( -4.458734124999999437, -73.39583333196773651, -2.574251347313719407 ) ) ;
#2912 = CARTESIAN_POINT ( 'NONE',  ( 9.457646018065525792E-16, -17.31249999863440792, 5.148502694627439702 ) ) ;
#2913 = VECTOR ( 'NONE', #14624, 1000.000000000000000 ) ;
#2914 =( BOUNDED_CURVE ( )  B_SPLINE_CURVE ( 2, ( #20101, #5316, #49689, #59673, #5635, #48416, #53876, #63225, #24933 ),
 .UNSPECIFIED., .F., .F. ) 
 B_SPLINE_CURVE_WITH_KNOTS ( ( 3, 2, 2, 2, 3 ),
 ( 0.2916666666666669072, 0.2958333333333335591, 0.3000000000000002665, 0.3041666666666669183, 0.3083333333333336257 ),
 .UNSPECIFIED. ) 
 CURVE ( )  GEOMETRIC_REPRESENTATION_ITEM ( )  RATIONAL_B_SPLINE_CURVE ( ( 0.9999999999999958922, 0.9238795325112908463, 1.000000000000000000, 0.9238795325112867385, 1.000000000000000000, 0.9238795325112867385, 1.000000000000000000, 0.9238795325112816315, 1.000000000000005107 ) ) 
 REPRESENTATION_ITEM ( '' )  );
#2915 = CARTESIAN_POINT ( 'NONE',  ( 2.499999999999998668, -1.333333333333332149, -4.330127018922193649 ) ) ;
#2916 = CARTESIAN_POINT ( 'NONE',  ( 1.846868145590736310, -158.6250000013655779, 4.458734124999999437 ) ) ;
#2917 = CARTESIAN_POINT ( 'NONE',  ( -9.184850993605147944E-16, -158.2500000000000000, 5.000000000000000000 ) ) ;
#2918 = CARTESIAN_POINT ( 'NONE',  ( 4.458734124999998549, -66.72916666530106511, -2.574251347313721627 ) ) ;
#2919 = CARTESIAN_POINT ( 'NONE',  ( 5.000000000000000000, -100.3749999972688158, -6.123233995736766282E-16 ) ) ;
#2920 = CARTESIAN_POINT ( 'NONE',  ( 1.975475456537005874E-15, -37.74999999999999289, 5.000000000000000000 ) ) ;
#2921 = CARTESIAN_POINT ( 'NONE',  ( 2.229367062499998831, -41.64583333196773651, -3.861377020970580887 ) ) ;
#2922 = CARTESIAN_POINT ( 'NONE',  ( 1.339745962155612702, 19.83034180399266688, -5.000000000000000000 ) ) ;
#2923 = CARTESIAN_POINT ( 'NONE',  ( -4.458734124999999437, -69.64583333196773651, -2.574251347313719407 ) ) ;
#2924 = CARTESIAN_POINT ( 'NONE',  ( -3.535250795749689387E-16, -46.25000000000000000, -5.773502691896257311 ) ) ;
#2925 = CARTESIAN_POINT ( 'NONE',  ( -1.339745962155610925, -22.79465819873851729, 5.000000000000000000 ) ) ;
#2926 = CARTESIAN_POINT ( 'NONE',  ( -1.339745962155610925, 16.20534180126147916, 5.000000000000000000 ) ) ;
#2927 = ORIENTED_EDGE ( 'NONE', *, *, #14223, .F. ) ;
#2928 = CARTESIAN_POINT ( 'NONE',  ( -2.480964764533239819E-13, -94.75000000000000000, 5.000000000000000000 ) ) ;
#2929 = CARTESIAN_POINT ( 'NONE',  ( 6.123233995736766282E-16, -170.0000000000000000, -5.000000000000000000 ) ) ;
#2930 = CARTESIAN_POINT ( 'NONE',  ( 1.060575238724906964E-15, -5.749999999999998224, 5.773502691896257311 ) ) ;
#2931 = CARTESIAN_POINT ( 'NONE',  ( 2.229367062500001939, -70.97916666530107932, 3.861377020970579999 ) ) ;
#2932 = AXIS2_PLACEMENT_3D ( 'NONE', #9738, #29342, #44147 ) ;
#2933 = CARTESIAN_POINT ( 'NONE',  ( 1.975475456537005874E-15, -5.750000000000000000, 5.000000000000000000 ) ) ;
#2934 = CARTESIAN_POINT ( 'NONE',  ( -3.535250795749689387E-16, -14.12499999726881050, -5.773502691896257311 ) ) ;
#2936 = ORIENTED_EDGE ( 'NONE', *, *, #22841, .T. ) ;
#2935 = CARTESIAN_POINT ( 'NONE',  ( 2.229367062500001939, -46.97916666530106511, 3.861377020970579999 ) ) ;
#2937 = CARTESIAN_POINT ( 'NONE',  ( 5.000000000000000000, -41.49999999999999289, -6.123233995736766282E-16 ) ) ;
#2939 = ORIENTED_EDGE ( 'NONE', *, *, #37679, .T. ) ;
#2938 = CARTESIAN_POINT ( 'NONE',  ( -3.152548672688508926E-16, 5.187500001365592972, -5.148502694627439702 ) ) ;
#2940 = CARTESIAN_POINT ( 'NONE',  ( 3.061616997868383141E-16, -151.7500000000000284, -5.000000000000000000 ) ) ;
#2941 = CARTESIAN_POINT ( 'NONE',  ( -5.000000000000000000, -55.08333333333332860, -2.886751345948128211 ) ) ;
#2942 = CARTESIAN_POINT ( 'NONE',  ( -4.458734125000000326, -161.2500000013655779, -1.846868145590735644 ) ) ;
#2943 = CARTESIAN_POINT ( 'NONE',  ( 2.229367062500001939, -36.22916666530107221, 3.861377020970579999 ) ) ;
#2944 = LINE ( 'NONE', #61166, #46103 ) ;
#2945 = CARTESIAN_POINT ( 'NONE',  ( -2.229367062500000163, -80.47916666530106511, -3.861377020970580443 ) ) ;
#2946 = CARTESIAN_POINT ( 'NONE',  ( -5.000000000000000888, -167.4375000000000284, 2.071067811865474617 ) ) ;
#2947 = CARTESIAN_POINT ( 'NONE',  ( -3.152548672688508926E-16, -87.56249999863440792, -5.148502694627439702 ) ) ;
#2948 = CARTESIAN_POINT ( 'NONE',  ( -56.48576386720575471, -131.0000000013656063, -4.591703134518078322 ) ) ;
#2949 = CARTESIAN_POINT ( 'NONE',  ( 4.458734125000001214, 0.8541666680322613781, 2.574251347313718519 ) ) ;
#2950 = CARTESIAN_POINT ( 'NONE',  ( 4.458734124999999437, -39.06249999863440081, -5.460374474430324690E-16 ) ) ;
#2951 = CARTESIAN_POINT ( 'NONE',  ( -2.500000000000000444, 23.95833333606451987, -4.330127018922193649 ) ) ;
#2952 = CARTESIAN_POINT ( 'NONE',  ( 2.229367062500001939, -82.22916666530106511, 3.861377020970579999 ) ) ;
#2953 = CARTESIAN_POINT ( 'NONE',  ( -1.339745962155610925, 16.33034180399266333, 5.000000000000000000 ) ) ;
#2954 = ORIENTED_EDGE ( 'NONE', *, *, #32208, .T. ) ;
#2955 = FACE_OUTER_BOUND ( 'NONE', #59978, .T. ) ;
#2956 = AXIS2_PLACEMENT_3D ( 'NONE', #15838, #36406, #16471 ) ;
#2957 = DIRECTION ( 'NONE',  ( -0.000000000000000000, 1.000000000000000000, -0.000000000000000000 ) ) ;
#2958 = CARTESIAN_POINT ( 'NONE',  ( -2.229367062499996610, -72.39583333196773651, 3.861377020970582219 ) ) ;
#2959 = CARTESIAN_POINT ( 'NONE',  ( 4.458734124999999437, -39.81249999863440081, -5.460374474430324690E-16 ) ) ;
#2960 = CARTESIAN_POINT ( 'NONE',  ( 4.458734124999998549, -10.97916666530107044, -2.574251347313721627 ) ) ;
#2961 = ORIENTED_EDGE ( 'NONE', *, *, #12199, .F. ) ;
#2962 = DIRECTION ( 'NONE',  ( -0.000000000000000000, 1.000000000000000000, -0.000000000000000000 ) ) ;
#2963 = EDGE_CURVE ( 'NONE', #7464, #1553, #17517, .T. ) ;
#2964 = DIRECTION ( 'NONE',  ( -0.000000000000000000, 1.000000000000000000, -0.000000000000000000 ) ) ;
#2965 = CARTESIAN_POINT ( 'NONE',  ( 2.229367062499998831, -4.895833331967740065, -3.861377020970580887 ) ) ;
#2966 = CARTESIAN_POINT ( 'NONE',  ( -52.53715891517739323, -148.5625000027311842, -4.819101127000233298 ) ) ;
#2967 = CARTESIAN_POINT ( 'NONE',  ( 9.457646018065525792E-16, 0.9375000013655959696, 5.148502694627439702 ) ) ;
#2968 = CARTESIAN_POINT ( 'NONE',  ( -4.999999999999998224, -75.91666666666665719, 2.886751345948131764 ) ) ;
#2969 = CARTESIAN_POINT ( 'NONE',  ( 2.730187237215162345E-16, -155.1875000013655779, -4.458734124999999437 ) ) ;
#2970 = CARTESIAN_POINT ( 'NONE',  ( 4.458734124999999437, 26.93750000136559564, -5.460374474430324690E-16 ) ) ;
#2971 = ORIENTED_EDGE ( 'NONE', *, *, #32783, .T. ) ;
#2972 = CARTESIAN_POINT ( 'NONE',  ( 4.458734124999999437, -86.81249999863439371, -5.460374474430324690E-16 ) ) ;
#2973 = CARTESIAN_POINT ( 'NONE',  ( -2.499999999999996447, -46.83333333333333570, 4.330127018922195425 ) ) ;
#2974 = CARTESIAN_POINT ( 'NONE',  ( 2.229367062500001939, -10.97916666530107044, 3.861377020970579999 ) ) ;
#2975 = FACE_OUTER_BOUND ( 'NONE', #41973, .T. ) ;
#2976 = CARTESIAN_POINT ( 'NONE',  ( -55.00000000000002132, -155.0000000000000284, 1.734723475976807094E-15 ) ) ;
#2977 = CARTESIAN_POINT ( 'NONE',  ( 5.000000000000000000, -67.50000000000000000, -6.123233995736766282E-16 ) ) ;
#2978 = CARTESIAN_POINT ( 'NONE',  ( 2.500000000000002220, -35.54166666393547303, 4.330127018922192761 ) ) ;
#2979 = CARTESIAN_POINT ( 'NONE',  ( -51.75738570946856498, -138.8750000027312126, 3.805975901505576964 ) ) ;
#2980 = CARTESIAN_POINT ( 'NONE',  ( -4.458734124999997661, 24.77083333469893134, 2.574251347313722516 ) ) ;
#2981 = CYLINDRICAL_SURFACE ( 'NONE', #2725, 5.000000000000000000 ) ;
#2982 = CARTESIAN_POINT ( 'NONE',  ( -2.229367062499996610, 22.85416666803225993, 3.861377020970582219 ) ) ;
#2983 = CARTESIAN_POINT ( 'NONE',  ( -2.229367062499996610, -59.14583333196773651, 3.861377020970582219 ) ) ;
#2984 = CARTESIAN_POINT ( 'NONE',  ( 2.229367062499998831, -4.895833331967740065, -3.861377020970580887 ) ) ;
#2985 = CARTESIAN_POINT ( 'NONE',  ( 2.500000000000002220, -0.5416666639354792423, 4.330127018922192761 ) ) ;
#2986 = CARTESIAN_POINT ( 'NONE',  ( 2.500000000000002220, 16.33333333333333215, 4.330127018922192761 ) ) ;
#2987 = CARTESIAN_POINT ( 'NONE',  ( -5.000000000000000888, -141.5625000027312126, 2.071067811865474617 ) ) ;
#2988 = CARTESIAN_POINT ( 'NONE',  ( -5.000000000000000000, -46.08333333333333570, -2.886751345948128211 ) ) ;
#2989 = CARTESIAN_POINT ( 'NONE',  ( -4.458734124999999437, -48.39583333196772941, -2.574251347313719407 ) ) ;
#2990 = CARTESIAN_POINT ( 'NONE',  ( 5.000000000000000000, -84.37499999726880162, -6.123233995736766282E-16 ) ) ;
#2991 = CARTESIAN_POINT ( 'NONE',  ( -57.89159099828107458, -136.9375000013655779, -3.393966926194107447 ) ) ;
#2992 =( BOUNDED_CURVE ( )  B_SPLINE_CURVE ( 2, ( #61025, #56194, #7312, #27231, #25962, #11791, #15993, #31740, #46541 ),
 .UNSPECIFIED., .F., .F. ) 
 B_SPLINE_CURVE_WITH_KNOTS ( ( 3, 2, 2, 2, 3 ),
 ( 0.9437499999999999778, 0.9444444444444444198, 0.9458333333333333037, 0.9472222222222221877, 0.9479166666666666297 ),
 .UNSPECIFIED. ) 
 CURVE ( )  GEOMETRIC_REPRESENTATION_ITEM ( )  RATIONAL_B_SPLINE_CURVE ( ( 0.9330127018922194093, 0.9330127018922194093, 1.000000000000000000, 0.8660254037844387076, 1.000000000000000000, 0.8660254037844387076, 1.000000000000000000, 0.9330127018922194093, 0.9330127018922194093 ) ) 
 REPRESENTATION_ITEM ( '' )  );
#2993 = CARTESIAN_POINT ( 'NONE',  ( 5.000000000000000000, -37.37499999726881583, -6.123233995736766282E-16 ) ) ;
#2994 = CARTESIAN_POINT ( 'NONE',  ( 1.975475456537005874E-15, -63.62499999726880873, 5.000000000000000000 ) ) ;
#2995 = CARTESIAN_POINT ( 'NONE',  ( -4.458734124999997661, -84.47916666530107932, 2.574251347313722516 ) ) ;
#2996 = CARTESIAN_POINT ( 'NONE',  ( 3.152801135295366208, -156.8125000013656063, 3.152801135295367985 ) ) ;
#2997 = CARTESIAN_POINT ( 'NONE',  ( -4.999999999999999112, -33.91666666666666430, 2.886751345948131764 ) ) ;
#2998 = CARTESIAN_POINT ( 'NONE',  ( 5.000000000000000888, 8.541666669397853795, 2.886751345948126879 ) ) ;
#2999 = EDGE_LOOP ( 'NONE', ( #61011, #60381, #46824, #52985 ) ) ;
#3000 = CARTESIAN_POINT ( 'NONE',  ( 2.229367062500001939, 18.77083333469892779, 3.861377020970579999 ) ) ;
#3001 = EDGE_LOOP ( 'NONE', ( #31996, #50141, #52598, #35426 ) ) ;
#3002 = CARTESIAN_POINT ( 'NONE',  ( -4.458734124999999437, -94.39583333196773651, -2.574251347313719407 ) ) ;
#3003 = CARTESIAN_POINT ( 'NONE',  ( -4.458734124999999437, 13.43750000136559386, 0.000000000000000000 ) ) ;
#3004 = CARTESIAN_POINT ( 'NONE',  ( -2.500000000000000444, 17.95833333606451632, -4.330127018922193649 ) ) ;
#3005 = CARTESIAN_POINT ( 'NONE',  ( 1.339745962155612702, -16.29465819873851729, -5.000000000000000000 ) ) ;
#3006 = CARTESIAN_POINT ( 'NONE',  ( 2.500000000000002220, 10.33333333333333393, 4.330127018922192761 ) ) ;
#3007 = VECTOR ( 'NONE', #37825, 1000.000000000000000 ) ;
#3008 = CARTESIAN_POINT ( 'NONE',  ( 9.457646018065525792E-16, -58.06249999863440081, 5.148502694627439702 ) ) ;
#3009 = CARTESIAN_POINT ( 'NONE',  ( -5.000000000000000000, -52.87499999726881583, 0.000000000000000000 ) ) ;
#3010 = CARTESIAN_POINT ( 'NONE',  ( -5.000000000000000000, -82.08333333333332860, -2.886751345948128211 ) ) ;
#3011 = CARTESIAN_POINT ( 'NONE',  ( 0.000000000000000000, -170.0000000000000000, 0.000000000000000000 ) ) ;
#3012 = CARTESIAN_POINT ( 'NONE',  ( 5.000000000000000888, -40.45833333060214443, 2.886751345948126879 ) ) ;
#3013 = CARTESIAN_POINT ( 'NONE',  ( -1.339745962155610925, -25.66965819600733312, 5.000000000000000000 ) ) ;
#3014 = CARTESIAN_POINT ( 'NONE',  ( 5.000000000000000000, -109.4166666666666572, -2.886751345948130876 ) ) ;
#3015 = CARTESIAN_POINT ( 'NONE',  ( -2.499999999999996447, -41.83333333333333570, 4.330127018922195425 ) ) ;
#3016 = CARTESIAN_POINT ( 'NONE',  ( 0.000000000000000000, -170.0000000000000000, 0.000000000000000000 ) ) ;
#3018 = CARTESIAN_POINT ( 'NONE',  ( -2.229367062499996610, -21.39583333196774007, 3.861377020970582219 ) ) ;
#3017 = CARTESIAN_POINT ( 'NONE',  ( -5.000000000000000000, -43.00000000000000000, 0.000000000000000000 ) ) ;
#3019 = PLANE ( 'NONE',  #29643 ) ;
#3020 = CARTESIAN_POINT ( 'NONE',  ( 4.458734125000001214, -66.89583333196773651, 2.574251347313718519 ) ) ;
#3021 = CARTESIAN_POINT ( 'NONE',  ( 4.458734124999999437, -146.7500000013656063, 1.846868145590737864 ) ) ;
#3022 = CARTESIAN_POINT ( 'NONE',  ( -3.152548672688508926E-16, -70.56249999863439371, -5.148502694627439702 ) ) ;
#3023 = CARTESIAN_POINT ( 'NONE',  ( -50.40829686548195099, -142.2500000013656063, -1.485763867205728284 ) ) ;
#3024 = CARTESIAN_POINT ( 'NONE',  ( 4.458734124999999437, -21.06249999863440436, -5.460374474430324690E-16 ) ) ;
#3025 = CARTESIAN_POINT ( 'NONE',  ( -3.535250795749689387E-16, -61.12499999726880873, -5.773502691896257311 ) ) ;
#3026 = EDGE_LOOP ( 'NONE', ( #61086, #11746, #10990, #62857 ) ) ;
#3027 = CARTESIAN_POINT ( 'NONE',  ( -5.000000000000000000, -150.5000000000000284, -6.123233995736766282E-16 ) ) ;
#3028 = ORIENTED_EDGE ( 'NONE', *, *, #23709, .F. ) ;
#3029 = CARTESIAN_POINT ( 'NONE',  ( 2.229367062500001939, -66.22916666530106511, 3.861377020970579999 ) ) ;
#3030 = CARTESIAN_POINT ( 'NONE',  ( 7.894787914004607998, 0.7661396099416312166, -7.591390474663430865 ) ) ;
#3031 = VERTEX_POINT ( 'NONE', #49628 ) ;
#3032 = CARTESIAN_POINT ( 'NONE',  ( 2.071067811865645591, -155.3125000027311557, 4.999999999999830358 ) ) ;
#3033 = CARTESIAN_POINT ( 'NONE',  ( -51.75738570946856498, -126.7500000000000284, 3.805975901505576964 ) ) ;
#3034 = DIRECTION ( 'NONE',  ( -0.000000000000000000, 1.000000000000000000, -0.000000000000000000 ) ) ;
#3035 = CARTESIAN_POINT ( 'NONE',  ( 4.458734124999998549, -52.97916666530107932, -2.574251347313721627 ) ) ;
#3036 = ORIENTED_EDGE ( 'NONE', *, *, #29373, .T. ) ;
#3037 = FACE_OUTER_BOUND ( 'NONE', #57444, .T. ) ;
#3038 = CARTESIAN_POINT ( 'NONE',  ( -4.458734124999999437, 9.604166668032259935, -2.574251347313719407 ) ) ;
#3039 =( BOUNDED_CURVE ( )  B_SPLINE_CURVE ( 2, ( #29731, #490, #20093, #40587, #60232, #35777, #55399, #11316, #18043 ),
 .UNSPECIFIED., .F., .F. ) 
 B_SPLINE_CURVE_WITH_KNOTS ( ( 3, 2, 2, 2, 3 ),
 ( 0.2104166666666666685, 0.2111111111111111105, 0.2124999999999999944, 0.2138888888888888784, 0.2145833333333333481 ),
 .UNSPECIFIED. ) 
 CURVE ( )  GEOMETRIC_REPRESENTATION_ITEM ( )  RATIONAL_B_SPLINE_CURVE ( ( 0.9330127018922194093, 0.9330127018922194093, 1.000000000000000000, 0.8660254037844387076, 1.000000000000000000, 0.8660254037844387076, 1.000000000000000000, 0.9330127018922180770, 0.9330127018922194093 ) ) 
 REPRESENTATION_ITEM ( '' )  );
#3040 = CARTESIAN_POINT ( 'NONE',  ( 2.229367062499998831, 19.35416666803225993, -3.861377020970580887 ) ) ;
#3041 = CARTESIAN_POINT ( 'NONE',  ( -54.64476657466781973, -150.8125000013656063, -4.444560631937228834 ) ) ;
#3042 = CARTESIAN_POINT ( 'NONE',  ( 1.975475456537005874E-15, -77.75000000000000000, 5.000000000000000000 ) ) ;
#3043 = CARTESIAN_POINT ( 'NONE',  ( 0.000000000000000000, -120.0000000000000000, 0.000000000000000000 ) ) ;
#3044 = EDGE_LOOP ( 'NONE', ( #48836, #28789, #53241 ) ) ;
#3045 = CARTESIAN_POINT ( 'NONE',  ( -4.458734124999999437, -70.39583333196773651, -2.574251347313719407 ) ) ;
#3046 = CARTESIAN_POINT ( 'NONE',  ( -1.339745962155610925, -39.79465819873851729, 5.000000000000000000 ) ) ;
#3047 = CARTESIAN_POINT ( 'NONE',  ( 9.457646018065525792E-16, 7.937500001365594748, 5.148502694627439702 ) ) ;
#3048 = AXIS2_PLACEMENT_3D ( 'NONE', #19419, #24888, #38709 ) ;
#3049 = CARTESIAN_POINT ( 'NONE',  ( -6.972266317189433020E-16, -89.24999999999998579, -5.000000000000000000 ) ) ;
#3050 = CARTESIAN_POINT ( 'NONE',  ( 2.229367062499998831, -59.89583333196774362, -3.861377020970580887 ) ) ;
#3051 = CARTESIAN_POINT ( 'NONE',  ( -3.535250795749689387E-16, -20.12499999726881228, -5.773502691896257311 ) ) ;
#3052 = DIRECTION ( 'NONE',  ( 1.000000000000000000, -0.000000000000000000, -0.000000000000000000 ) ) ;
#3053 = CARTESIAN_POINT ( 'NONE',  ( -5.000000000000000888, -139.6875000027311842, -2.071067811865475949 ) ) ;
#3054 = CARTESIAN_POINT ( 'NONE',  ( -5.000000000000000000, 29.12500000273118417, 0.000000000000000000 ) ) ;
#3055 = CARTESIAN_POINT ( 'NONE',  ( -4.458734124999999437, -38.39583333196773651, -2.574251347313719407 ) ) ;
#3056 = CARTESIAN_POINT ( 'NONE',  ( 2.229367062499998831, -23.89583333196773651, -3.861377020970580887 ) ) ;
#3057 = ORIENTED_EDGE ( 'NONE', *, *, #41664, .F. ) ;
#3058 = CARTESIAN_POINT ( 'NONE',  ( -1.339745962155610925, -4.669658196007337558, 5.000000000000000000 ) ) ;
#3059 = CARTESIAN_POINT ( 'NONE',  ( 9.457646018065525792E-16, -108.0624999986343937, 5.148502694627439702 ) ) ;
#3060 = CARTESIAN_POINT ( 'NONE',  ( 3.535533905932736864, -154.2500000027312126, 3.535533905932738641 ) ) ;
#3061 = ORIENTED_EDGE ( 'NONE', *, *, #32988, .F. ) ;
#3062 = CARTESIAN_POINT ( 'NONE',  ( 2.229367062499998831, -108.8958333319677365, -3.861377020970580887 ) ) ;
#3063 = EDGE_CURVE ( 'NONE', #59413, #24823, #50379, .T. ) ;
#3064 = CARTESIAN_POINT ( 'NONE',  ( 2.229367062499998831, -31.64583333196773651, -3.861377020970580887 ) ) ;
#3065 = CARTESIAN_POINT ( 'NONE',  ( -2.499999999999996447, -61.70833333060214443, 4.330127018922195425 ) ) ;
#3066 = CARTESIAN_POINT ( 'NONE',  ( -50.40829686548195099, -150.2500000013656063, -1.485763867205728284 ) ) ;
#3067 = CARTESIAN_POINT ( 'NONE',  ( -5.000000000000000888, -145.4375000000000000, 2.071067811865474617 ) ) ;
#3068 = CARTESIAN_POINT ( 'NONE',  ( -4.458734124999999437, -30.39583333196773651, -2.574251347313719407 ) ) ;
#3069 = CARTESIAN_POINT ( 'NONE',  ( 2.229367062500001939, -67.22916666530106511, 3.861377020970579999 ) ) ;
#3070 = CARTESIAN_POINT ( 'NONE',  ( 2.499999999999998668, 22.79166666939785202, -4.330127018922193649 ) ) ;
#3071 = CARTESIAN_POINT ( 'NONE',  ( 4.458734125000000326, -22.89583333196773651, 2.574251347313718519 ) ) ;
#3072 = CARTESIAN_POINT ( 'NONE',  ( 1.339745962155615144, -32.70534180126148271, 4.999999999999999112 ) ) ;
#3073 = LINE ( 'NONE', #22370, #17419 ) ;
#3074 = CARTESIAN_POINT ( 'NONE',  ( -2.499999999999996447, -16.83333333333333215, 4.330127018922195425 ) ) ;
#3075 = CARTESIAN_POINT ( 'NONE',  ( 4.458734124999999437, -147.4375000013656063, 0.000000000000000000 ) ) ;
#3076 = ORIENTED_EDGE ( 'NONE', *, *, #62096, .F. ) ;
#3077 = CARTESIAN_POINT ( 'NONE',  ( -2.499999999999996447, -81.83333333333332860, 4.330127018922195425 ) ) ;
#3078 = CARTESIAN_POINT ( 'NONE',  ( 4.458734125000000326, -50.14583333196772230, 2.574251347313718519 ) ) ;
#3079 = CARTESIAN_POINT ( 'NONE',  ( -4.999999999999998224, -86.79166666393547303, 2.886751345948131764 ) ) ;
#3080 = DIRECTION ( 'NONE',  ( -0.000000000000000000, 1.000000000000000000, -0.000000000000000000 ) ) ;
#3081 = CARTESIAN_POINT ( 'NONE',  ( -3.535250795749689387E-16, 24.75000000000000355, -5.773502691896257311 ) ) ;
#3082 = CARTESIAN_POINT ( 'NONE',  ( 2.500000000000002220, 25.33333333333333215, 4.330127018922192761 ) ) ;
#3083 = CARTESIAN_POINT ( 'NONE',  ( -4.458734124999999437, -0.3124999986344051406, 0.000000000000000000 ) ) ;
#3084 = EDGE_CURVE ( 'NONE', #41255, #41671, #52460, .T. ) ;
#3085 = CARTESIAN_POINT ( 'NONE',  ( 1.339745962155615144, 19.29465819873852439, 4.999999999999999112 ) ) ;
#3086 = CARTESIAN_POINT ( 'NONE',  ( 1.339745962155615144, -14.70534180126147916, 4.999999999999999112 ) ) ;
#3087 = CARTESIAN_POINT ( 'NONE',  ( -6.972266317189433020E-16, -74.25000000000000000, -5.000000000000000000 ) ) ;
#3088 = CARTESIAN_POINT ( 'NONE',  ( 9.457646018065525792E-16, 7.687500001365596525, 5.148502694627439702 ) ) ;
#3089 = ORIENTED_EDGE ( 'NONE', *, *, #49591, .T. ) ;
#3090 = DIRECTION ( 'NONE',  ( -1.000000000000000000, 0.000000000000000000, 0.000000000000000000 ) ) ;
#3091 = ORIENTED_EDGE ( 'NONE', *, *, #41313, .T. ) ;
#3092 =( BOUNDED_CURVE ( )  B_SPLINE_CURVE ( 2, ( #13625, #47713, #12985, #33243, #9109, #33866, #32610, #52236, #13929 ),
 .UNSPECIFIED., .F., .F. ) 
 B_SPLINE_CURVE_WITH_KNOTS ( ( 3, 2, 2, 2, 3 ),
 ( 0.06875000000000000555, 0.06944444444444444753, 0.07083333333333333148, 0.07222222222222221544, 0.07291666666666667129 ),
 .UNSPECIFIED. ) 
 CURVE ( )  GEOMETRIC_REPRESENTATION_ITEM ( )  RATIONAL_B_SPLINE_CURVE ( ( 0.9330127018922194093, 0.9330127018922200755, 1.000000000000000000, 0.8660254037844387076, 1.000000000000000000, 0.8660254037844387076, 1.000000000000000000, 0.9330127018922187432, 0.9330127018922194093 ) ) 
 REPRESENTATION_ITEM ( '' )  );
#3093 = CYLINDRICAL_SURFACE ( 'NONE', #39880, 5.000000000000000000 ) ;
#3094 = CARTESIAN_POINT ( 'NONE',  ( -3.152548672688508926E-16, -46.56249999863440792, -5.148502694627439702 ) ) ;
#3095 = CARTESIAN_POINT ( 'NONE',  ( 4.458734125000000326, -159.6250000013656063, -1.846868145590734978 ) ) ;
#3096 = CIRCLE ( 'NONE', #24648, 4.250000000000000000 ) ;
#3097 = CARTESIAN_POINT ( 'NONE',  ( 2.500000000000002220, -43.54166666393548013, 4.330127018922192761 ) ) ;
#3098 = ORIENTED_EDGE ( 'NONE', *, *, #19331, .F. ) ;
#3099 = CARTESIAN_POINT ( 'NONE',  ( -4.458734124999999437, -24.39583333196773651, -2.574251347313719407 ) ) ;
#3100 = ORIENTED_EDGE ( 'NONE', *, *, #5883, .T. ) ;
#3101 = CARTESIAN_POINT ( 'NONE',  ( -5.000000000000000000, -12.08333333333333570, -2.886751345948128211 ) ) ;
#3102 = CARTESIAN_POINT ( 'NONE',  ( -4.458734124999999437, -164.9375000013655779, -5.460374474430324690E-16 ) ) ;
#3103 = CARTESIAN_POINT ( 'NONE',  ( 1.975475456537005874E-15, -12.74999999999999822, 5.000000000000000000 ) ) ;
#3104 = CARTESIAN_POINT ( 'NONE',  ( -56.66612745406270335, -137.3125000000000284, -5.149110718188516067 ) ) ;
#3105 = CARTESIAN_POINT ( 'NONE',  ( 4.458734125000001214, -40.14583333196772941, 2.574251347313718519 ) ) ;
#3106 = CARTESIAN_POINT ( 'NONE',  ( -2.500000000000000444, 22.95833333606451632, -4.330127018922193649 ) ) ;
#3107 = VERTEX_POINT ( 'NONE', #21320 ) ;
#3108 = CARTESIAN_POINT ( 'NONE',  ( -2.229367062499996610, -81.14583333196773651, 3.861377020970582219 ) ) ;
#3109 = CARTESIAN_POINT ( 'NONE',  ( 2.229367062499998831, 26.35416666803225993, -3.861377020970580887 ) ) ;
#3110 = CARTESIAN_POINT ( 'NONE',  ( -2.499999999999996447, -28.70833333060214798, 4.330127018922195425 ) ) ;
#3111 = EDGE_LOOP ( 'NONE', ( #55303, #24448, #48634, #52654 ) ) ;
#3112 = CARTESIAN_POINT ( 'NONE',  ( -58.39396692619412477, -137.6875000013656063, 2.891590998281057701 ) ) ;
#3113 = CARTESIAN_POINT ( 'NONE',  ( 9.457646018065525792E-16, -84.31249999863437949, 5.148502694627439702 ) ) ;
#3114 = CARTESIAN_POINT ( 'NONE',  ( -52.53715891517739323, -131.5625000027312410, -4.819101127000233298 ) ) ;
#3115 = CARTESIAN_POINT ( 'NONE',  ( 0.000000000000000000, -170.0000000000000000, 0.000000000000000000 ) ) ;
#3116 = DIRECTION ( 'NONE',  ( -0.000000000000000000, -0.000000000000000000, 1.000000000000000000 ) ) ;
#3117 = CARTESIAN_POINT ( 'NONE',  ( 9.457646018065525792E-16, -56.06249999863440792, 5.148502694627439702 ) ) ;
#3118 = CARTESIAN_POINT ( 'NONE',  ( -4.999999999999998224, -71.79166666393547303, 2.886751345948131764 ) ) ;
#3119 = CARTESIAN_POINT ( 'NONE',  ( 2.229367062500001939, 22.02083333469892779, 3.861377020970579999 ) ) ;
#3120 = CARTESIAN_POINT ( 'NONE',  ( -2.500000000000000444, -107.1666666666666572, -4.330127018922193649 ) ) ;
#3121 = CARTESIAN_POINT ( 'NONE',  ( 3.061616997868383141E-16, -158.8750000027311842, -5.000000000000000000 ) ) ;
#3122 = CARTESIAN_POINT ( 'NONE',  ( -3.152548672688508926E-16, -46.81249999863440081, -5.148502694627439702 ) ) ;
#3123 = CARTESIAN_POINT ( 'NONE',  ( -2.499999999999996447, -3.708333330602147537, 4.330127018922195425 ) ) ;
#3124 = DIRECTION ( 'NONE',  ( -0.000000000000000000, 1.000000000000000000, -0.000000000000000000 ) ) ;
#3125 = CARTESIAN_POINT ( 'NONE',  ( -52.10840900171896806, -126.1875000013656063, 3.393966926194110556 ) ) ;
#3126 = CARTESIAN_POINT ( 'NONE',  ( -4.458734124999999437, -81.64583333196773651, -2.574251347313719407 ) ) ;
#3127 = CARTESIAN_POINT ( 'NONE',  ( 4.458734124999998549, -103.7291666653010651, -2.574251347313721627 ) ) ;
#3128 = AXIS2_PLACEMENT_3D ( 'NONE', #42970, #38155, #52942 ) ;
#3129 = CARTESIAN_POINT ( 'NONE',  ( -4.458734124999999437, -6.645833331967741842, -2.574251347313719407 ) ) ;
#3130 = VERTEX_POINT ( 'NONE', #11648 ) ;
#3131 = CARTESIAN_POINT ( 'NONE',  ( -1.339745962155610925, -35.66965819600732601, 5.000000000000000000 ) ) ;
#3132 = CARTESIAN_POINT ( 'NONE',  ( 4.458734124999998549, -95.72916666530109353, -2.574251347313721627 ) ) ;
#3133 = CARTESIAN_POINT ( 'NONE',  ( -9.184850993605147944E-16, -167.3750000027312126, 5.000000000000000000 ) ) ;
#3134 = CARTESIAN_POINT ( 'NONE',  ( -2.229367062500000163, -91.72916666530106511, -3.861377020970580443 ) ) ;
#3135 = EDGE_CURVE ( 'NONE', #43948, #34069, #59007, .T. ) ;
#3136 = CARTESIAN_POINT ( 'NONE',  ( -3.152548672688508926E-16, 10.18750000136559208, -5.148502694627439702 ) ) ;
#3137 = DIRECTION ( 'NONE',  ( -0.000000000000000000, 1.000000000000000000, -0.000000000000000000 ) ) ;
#3138 = CARTESIAN_POINT ( 'NONE',  ( -52.10840900171896806, -133.1875000013656063, 3.393966926194110556 ) ) ;
#3139 = AXIS2_PLACEMENT_3D ( 'NONE', #24468, #52495, #62143 ) ;
#3140 = CARTESIAN_POINT ( 'NONE',  ( -2.229367062499996610, -14.14583333196774184, 3.861377020970582219 ) ) ;
#3141 = CARTESIAN_POINT ( 'NONE',  ( -4.458734124999998549, 17.52083333469892779, 2.574251347313722516 ) ) ;
#3142 = CARTESIAN_POINT ( 'NONE',  ( -4.458734124999999437, -55.64583333196773651, -2.574251347313719407 ) ) ;
#3143 = CARTESIAN_POINT ( 'NONE',  ( 1.975475456537005874E-15, -68.74999999999998579, 5.000000000000000000 ) ) ;
#3144 = CARTESIAN_POINT ( 'NONE',  ( -5.000000000000000888, -152.5625000000000284, -2.071067811865475949 ) ) ;
#3145 = CARTESIAN_POINT ( 'NONE',  ( 4.458734125000000326, -9.895833331967738289, 2.574251347313718519 ) ) ;
#3146 = DIRECTION ( 'NONE',  ( 0.000000000000000000, 0.000000000000000000, 1.000000000000000000 ) ) ;
#3147 = ORIENTED_EDGE ( 'NONE', *, *, #61347, .F. ) ;
#3148 = CARTESIAN_POINT ( 'NONE',  ( 4.458734124999999437, -35.06249999863440792, -5.460374474430324690E-16 ) ) ;
#3149 = CARTESIAN_POINT ( 'NONE',  ( -59.59170313451811296, -128.7500000013656063, 1.485763867205729394 ) ) ;
#3150 = CARTESIAN_POINT ( 'NONE',  ( 5.000000000000000888, -76.58333333333335702, 2.886751345948126879 ) ) ;
#3151 = EDGE_CURVE ( 'NONE', #26615, #14537, #10538, .T. ) ;
#3152 = CARTESIAN_POINT ( 'NONE',  ( -2.229367062499996610, -80.14583333196773651, 3.861377020970582219 ) ) ;
#3153 = CARTESIAN_POINT ( 'NONE',  ( -2.229367062499996610, 23.60416666803225993, 3.861377020970582219 ) ) ;
#3154 = CARTESIAN_POINT ( 'NONE',  ( 9.457646018065525792E-16, 13.93750000136559564, 5.148502694627439702 ) ) ;
#3155 = LINE ( 'NONE', #28527, #6161 ) ;
#3156 = EDGE_CURVE ( 'NONE', #49359, #15910, #1183, .T. ) ;
#3157 = CARTESIAN_POINT ( 'NONE',  ( -49.85088928181150436, -137.6875000027311842, -1.666127454062680480 ) ) ;
#3158 = CARTESIAN_POINT ( 'NONE',  ( -2.229367062500000163, -81.72916666530106511, -3.861377020970580443 ) ) ;
#3159 = CARTESIAN_POINT ( 'NONE',  ( -5.000000000000000000, -68.99999999999998579, 0.000000000000000000 ) ) ;
#3160 = LINE ( 'NONE', #37555, #39787 ) ;
#3161 = CARTESIAN_POINT ( 'NONE',  ( -5.000000000000000000, 19.04166666939785202, -2.886751345948128211 ) ) ;
#3162 = ORIENTED_EDGE ( 'NONE', *, *, #43472, .F. ) ;
#3163 = ADVANCED_FACE ( 'NONE', ( #21952 ), #2981, .F. ) ;
#3164 = CARTESIAN_POINT ( 'NONE',  ( -6.972266317189433020E-16, -34.25000000000000000, -5.000000000000000000 ) ) ;
#3166 = CARTESIAN_POINT ( 'NONE',  ( -2.500000000000000444, -27.16666666666666430, -4.330127018922193649 ) ) ;
#3165 = CARTESIAN_POINT ( 'NONE',  ( 2.499999999999998668, -40.33333333333332860, -4.330127018922193649 ) ) ;
#3167 = CARTESIAN_POINT ( 'NONE',  ( 4.458734125000001214, -30.89583333196773296, 2.574251347313718519 ) ) ;
#3168 = CARTESIAN_POINT ( 'NONE',  ( -7.922281120364393914, -4.573931137438277617, -8.047472243342932430 ) ) ;
#3169 =( BOUNDED_CURVE ( )  B_SPLINE_CURVE ( 2, ( #33180, #43129, #53730, #23839, #4843, #14172, #43442, #9981, #28961 ),
 .UNSPECIFIED., .F., .F. ) 
 B_SPLINE_CURVE_WITH_KNOTS ( ( 3, 2, 2, 2, 3 ),
 ( 0.8125000000000000000, 0.8130952380952380931, 0.8142857142857142794, 0.8154761904761904656, 0.8160714285714285587 ),
 .UNSPECIFIED. ) 
 CURVE ( )  GEOMETRIC_REPRESENTATION_ITEM ( )  RATIONAL_B_SPLINE_CURVE ( ( 0.9330127018922194093, 0.9330127018922194093, 1.000000000000000000, 0.8660254037844387076, 1.000000000000000000, 0.8660254037844387076, 1.000000000000000000, 0.9330127018922194093, 0.9330127018922194093 ) ) 
 REPRESENTATION_ITEM ( '' )  );
#3170 = CARTESIAN_POINT ( 'NONE',  ( -4.999999999999999112, -29.79166666393548368, 2.886751345948131764 ) ) ;
#3172 = ORIENTED_EDGE ( 'NONE', *, *, #35301, .T. ) ;
#3171 = CARTESIAN_POINT ( 'NONE',  ( -4.458734124999999437, -61.31249999863440081, 0.000000000000000000 ) ) ;
#3173 = CARTESIAN_POINT ( 'NONE',  ( -50.55543936806279248, -154.3125000013656347, 0.3552334253322060320 ) ) ;
#3175 = ORIENTED_EDGE ( 'NONE', *, *, #41664, .T. ) ;
#3174 = CARTESIAN_POINT ( 'NONE',  ( 2.229367062499998831, -9.895833331967738289, -3.861377020970580887 ) ) ;
#3176 = CARTESIAN_POINT ( 'NONE',  ( -2.500000000000000444, -76.16666666666665719, -4.330127018922193649 ) ) ;
#3177 = CARTESIAN_POINT ( 'NONE',  ( -55.35523342533222291, -139.3125000013656063, 4.444560631937231499 ) ) ;
#3178 = VECTOR ( 'NONE', #16349, 1000.000000000000000 ) ;
#3179 = CARTESIAN_POINT ( 'NONE',  ( -3.152548672688508926E-16, -53.81249999863439371, -5.148502694627439702 ) ) ;
#3180 = CARTESIAN_POINT ( 'NONE',  ( 1.060575238724906964E-15, -74.62499999726880162, 5.773502691896257311 ) ) ;
#3182 = ORIENTED_EDGE ( 'NONE', *, *, #38985, .T. ) ;
#3181 = CYLINDRICAL_SURFACE ( 'NONE', #41592, 5.000000000000000000 ) ;
#3183 = AXIS2_PLACEMENT_3D ( 'NONE', #41821, #17708, #61467 ) ;
#3184 = CARTESIAN_POINT ( 'NONE',  ( -53.33387254593733928, -150.8125000000000000, 5.149110718188519620 ) ) ;
#3185 = ADVANCED_FACE ( 'NONE', ( #41874 ), #52171, .T. ) ;
#3186 = CARTESIAN_POINT ( 'NONE',  ( -4.458734124999999437, -19.64583333196774362, -2.574251347313719407 ) ) ;
#3188 = ORIENTED_EDGE ( 'NONE', *, *, #35006, .T. ) ;
#3187 = CARTESIAN_POINT ( 'NONE',  ( -3.152548672688508926E-16, -58.81249999863440081, -5.148502694627439702 ) ) ;
#3189 =( BOUNDED_CURVE ( )  B_SPLINE_CURVE ( 2, ( #4670, #33948, #14009, #23050, #53256, #33013, #3435, #63229, #23680 ),
 .UNSPECIFIED., .F., .F. ) 
 B_SPLINE_CURVE_WITH_KNOTS ( ( 3, 2, 2, 2, 3 ),
 ( 0.9312500000000000222, 0.9319444444444444642, 0.9333333333333333481, 0.9347222222222222321, 0.9354166666666666741 ),
 .UNSPECIFIED. ) 
 CURVE ( )  GEOMETRIC_REPRESENTATION_ITEM ( )  RATIONAL_B_SPLINE_CURVE ( ( 0.9330127018922194093, 0.9330127018922194093, 1.000000000000000000, 0.8660254037844387076, 1.000000000000000000, 0.8660254037844387076, 1.000000000000000000, 0.9330127018922194093, 0.9330127018922194093 ) ) 
 REPRESENTATION_ITEM ( '' )  );
#3190 = FACE_OUTER_BOUND ( 'NONE', #21725, .T. ) ;
#3191 = CARTESIAN_POINT ( 'NONE',  ( 4.458734124999999437, -139.5000000013655779, 1.846868145590737864 ) ) ;
#3192 = CARTESIAN_POINT ( 'NONE',  ( 4.458734124999999437, -98.06249999863440792, -5.460374474430324690E-16 ) ) ;
#3193 = CARTESIAN_POINT ( 'NONE',  ( -58.24261429053147765, -149.3750000027312126, -3.805975901505573855 ) ) ;
#3194 = ORIENTED_EDGE ( 'NONE', *, *, #27163, .F. ) ;
#3195 = CARTESIAN_POINT ( 'NONE',  ( -50.70258187064364108, -151.3750000013656063, 2.196230717870141014 ) ) ;
#3196 = CARTESIAN_POINT ( 'NONE',  ( -59.81910112700025905, -143.3125000027312126, -2.462841084822630311 ) ) ;
#3197 = CYLINDRICAL_SURFACE ( 'NONE', #58905, 5.000000000000000000 ) ;
#3198 = CARTESIAN_POINT ( 'NONE',  ( 2.229367062499998831, -6.645833331967741842, -3.861377020970580887 ) ) ;
#3199 = CARTESIAN_POINT ( 'NONE',  ( 2.229367062500001939, -93.22916666530106511, 3.861377020970579999 ) ) ;
#3200 = CARTESIAN_POINT ( 'NONE',  ( 4.458734125000000326, -149.6250000013655779, -1.846868145590734978 ) ) ;
#3201 = CARTESIAN_POINT ( 'NONE',  ( 4.458734124999999437, -28.06249999863440081, -5.460374474430324690E-16 ) ) ;
#3202 = CARTESIAN_POINT ( 'NONE',  ( -6.972266317189433020E-16, -69.24999999999998579, -5.000000000000000000 ) ) ;
#3203 = CARTESIAN_POINT ( 'NONE',  ( -57.89159099828107458, -136.6875000013656063, -3.393966926194107447 ) ) ;
#3204 = CARTESIAN_POINT ( 'NONE',  ( -4.458734124999998549, -64.47916666530106511, 2.574251347313722516 ) ) ;
#3205 = CARTESIAN_POINT ( 'NONE',  ( 0.000000000000000000, -170.0000000000000000, 0.000000000000000000 ) ) ;
#3206 = CARTESIAN_POINT ( 'NONE',  ( -6.972266317189433020E-16, -43.12499999726880873, -5.000000000000000000 ) ) ;
#3207 = CARTESIAN_POINT ( 'NONE',  ( 3.152801135295366208, -146.5625000013655779, 3.152801135295367985 ) ) ;
#3208 = CARTESIAN_POINT ( 'NONE',  ( -2.229367062499996610, 11.60416666803225993, 3.861377020970582219 ) ) ;
#3209 = ORIENTED_EDGE ( 'NONE', *, *, #53820, .F. ) ;
#3210 = CARTESIAN_POINT ( 'NONE',  ( -1.339745962155610925, -52.66965819600733312, 5.000000000000000000 ) ) ;
#3211 = CARTESIAN_POINT ( 'NONE',  ( 2.499999999999998668, -61.33333333333333570, -4.330127018922193649 ) ) ;
#3213 = CARTESIAN_POINT ( 'NONE',  ( 9.457646018065525792E-16, -27.06249999863440081, 5.148502694627439702 ) ) ;
#3212 = CARTESIAN_POINT ( 'NONE',  ( 5.000000000000000000, -92.50000000000000000, -6.123233995736766282E-16 ) ) ;
#3214 = CARTESIAN_POINT ( 'NONE',  ( -1.339745962155613812, 6.919658201469707670, -5.000000000000000000 ) ) ;
#3215 = CARTESIAN_POINT ( 'NONE',  ( 4.458734125000001214, -70.14583333196773651, 2.574251347313718519 ) ) ;
#3216 = CYLINDRICAL_SURFACE ( 'NONE', #48840, 5.000000000000000000 ) ;
#3217 = CARTESIAN_POINT ( 'NONE',  ( -75.00000000000002842, 15.00000000000000000, 5.000000000000000000 ) ) ;
#3218 = CARTESIAN_POINT ( 'NONE',  ( -52.10840900171896806, -145.1875000013656063, 3.393966926194110556 ) ) ;
#3219 = EDGE_CURVE ( 'NONE', #28403, #43327, #40978, .T. ) ;
#3220 = EDGE_CURVE ( 'NONE', #61158, #22662, #34388, .T. ) ;
#3221 = CARTESIAN_POINT ( 'NONE',  ( -3.152548672688508926E-16, 4.437500001365595637, -5.148502694627439702 ) ) ;
#3222 = CARTESIAN_POINT ( 'NONE',  ( 0.000000000000000000, -170.0000000000000000, 0.000000000000000000 ) ) ;
#3224 = EDGE_CURVE ( 'NONE', #42594, #4186, #20892, .T. ) ;
#3223 = CARTESIAN_POINT ( 'NONE',  ( -5.000000000000000000, -15.00000000000000000, 0.000000000000000000 ) ) ;
#3225 = CARTESIAN_POINT ( 'NONE',  ( 2.229367062500001939, 6.020833334698927786, 3.861377020970579999 ) ) ;
#3226 = CARTESIAN_POINT ( 'NONE',  ( -4.458734124999998549, -72.22916666530107932, 2.574251347313722516 ) ) ;
#3227 = CARTESIAN_POINT ( 'NONE',  ( 4.458734125000000326, -19.14583333196774007, 2.574251347313718519 ) ) ;
#3228 = CARTESIAN_POINT ( 'NONE',  ( 2.500000000000002220, -4.666666666666666075, 4.330127018922192761 ) ) ;
#3229 = CARTESIAN_POINT ( 'NONE',  ( -3.152801135295367096, -158.0625000013656063, -3.152801135295367541 ) ) ;
#3230 = CARTESIAN_POINT ( 'NONE',  ( 1.339745962155609149, 23.29465819873852084, 5.000000000000003553 ) ) ;
#3231 = CARTESIAN_POINT ( 'NONE',  ( 2.229367062500001939, -61.97916666530106511, 3.861377020970579999 ) ) ;
#3232 = CARTESIAN_POINT ( 'NONE',  ( 5.000000000000000000, -98.37499999726881583, -6.123233995736766282E-16 ) ) ;
#3233 = EDGE_CURVE ( 'NONE', #4714, #42402, #36478, .T. ) ;
#3234 = CARTESIAN_POINT ( 'NONE',  ( -59.98410592259440222, -149.1250000000000284, -0.3983568153799752487 ) ) ;
#3235 = CARTESIAN_POINT ( 'NONE',  ( 4.458734124999999437, -39.81249999863440081, -5.460374474430324690E-16 ) ) ;
#3236 = EDGE_CURVE ( 'NONE', #13010, #29821, #22475, .T. ) ;
#3237 = CARTESIAN_POINT ( 'NONE',  ( -2.229367062499996610, -106.3958333319677365, 3.861377020970582219 ) ) ;
#3238 = CARTESIAN_POINT ( 'NONE',  ( 4.458734125000000326, -65.14583333196773651, 2.574251347313718519 ) ) ;
#3239 = CARTESIAN_POINT ( 'NONE',  ( 5.000000000000000000, -47.50000000000000000, -6.123233995736766282E-16 ) ) ;
#3240 = CARTESIAN_POINT ( 'NONE',  ( -1.339745962155610925, -40.79465819873852439, 5.000000000000000000 ) ) ;
#3241 = EDGE_CURVE ( 'NONE', #14051, #10657, #38007, .T. ) ;
#3242 = CARTESIAN_POINT ( 'NONE',  ( 2.071067811865645591, -152.3125000027312126, 4.999999999999830358 ) ) ;
#3243 = ORIENTED_EDGE ( 'NONE', *, *, #3971, .F. ) ;
#3244 = CARTESIAN_POINT ( 'NONE',  ( -1.339745962155623360, 15.33034180399266333, 4.999999999999991118 ) ) ;
#3245 =( BOUNDED_CURVE ( )  B_SPLINE_CURVE ( 2, ( #58511, #49491, #63036, #53680, #5112, #33433, #48536, #14120, #59148 ),
 .UNSPECIFIED., .F., .F. ) 
 B_SPLINE_CURVE_WITH_KNOTS ( ( 3, 2, 2, 2, 3 ),
 ( 0.6839285714285714413, 0.6845238095238095344, 0.6857142857142857206, 0.6869047619047619069, 0.6875000000000000000 ),
 .UNSPECIFIED. ) 
 CURVE ( )  GEOMETRIC_REPRESENTATION_ITEM ( )  RATIONAL_B_SPLINE_CURVE ( ( 0.9330127018922194093, 0.9330127018922194093, 1.000000000000000000, 0.8660254037844387076, 1.000000000000000000, 0.8660254037844387076, 1.000000000000000000, 0.9330127018922194093, 0.9330127018922194093 ) ) 
 REPRESENTATION_ITEM ( '' )  );
#3246 = CARTESIAN_POINT ( 'NONE',  ( 0.000000000000000000, -120.0000000000000000, 0.000000000000000000 ) ) ;
#3247 = CARTESIAN_POINT ( 'NONE',  ( -3.535250795749689387E-16, -13.24999999999999822, -5.773502691896257311 ) ) ;
#3248 = CARTESIAN_POINT ( 'NONE',  ( 2.229367062499998831, -18.64583333196774007, -3.861377020970580887 ) ) ;
#3249 = EDGE_CURVE ( 'NONE', #40250, #22002, #18796, .T. ) ;
#3250 = CARTESIAN_POINT ( 'NONE',  ( 4.458734125000000326, -74.89583333196773651, 2.574251347313718519 ) ) ;
#3251 = CARTESIAN_POINT ( 'NONE',  ( 6.123233995736766282E-16, -120.0000000000000000, -5.000000000000000000 ) ) ;
#3252 = CARTESIAN_POINT ( 'NONE',  ( -2.499999999999996447, -11.70833333060214798, 4.330127018922195425 ) ) ;
#3254 = ORIENTED_EDGE ( 'NONE', *, *, #38398, .T. ) ;
#3253 = CARTESIAN_POINT ( 'NONE',  ( 4.458734125000001214, -44.89583333196774362, 2.574251347313718519 ) ) ;
#3255 = CARTESIAN_POINT ( 'NONE',  ( 5.000000000000000000, -144.0625000000000000, 2.071067811865478614 ) ) ;
#3257 = ORIENTED_EDGE ( 'NONE', *, *, #9421, .F. ) ;
#3256 = CARTESIAN_POINT ( 'NONE',  ( -4.458734124999999437, 4.354166668032260823, -2.574251347313719407 ) ) ;
#3258 = CARTESIAN_POINT ( 'NONE',  ( -2.071067811865604735, -151.3125000000000284, 4.999999999999872990 ) ) ;
#3259 = CARTESIAN_POINT ( 'NONE',  ( 2.500000000000002220, -55.66666666666667140, 4.330127018922192761 ) ) ;
#3260 = CARTESIAN_POINT ( 'NONE',  ( 3.152801135295367541, -158.5625000013656063, -3.152801135295367541 ) ) ;
#3261 = CARTESIAN_POINT ( 'NONE',  ( 4.458734124999998549, -37.97916666530107932, -2.574251347313721627 ) ) ;
#3262 = CARTESIAN_POINT ( 'NONE',  ( 3.535533905932736864, -145.1250000000000000, 3.535533905932738641 ) ) ;
#3263 = CARTESIAN_POINT ( 'NONE',  ( -4.458734124999999437, -79.31249999863440792, 0.000000000000000000 ) ) ;
#3264 = CARTESIAN_POINT ( 'NONE',  ( -2.071067811865478170, -165.3125000000000284, 5.000000000000000000 ) ) ;
#3265 = CARTESIAN_POINT ( 'NONE',  ( 1.339745962155612702, -11.29465819873852261, -5.000000000000000000 ) ) ;
#3266 = CARTESIAN_POINT ( 'NONE',  ( -53.51423613279429503, -130.5000000013656063, 4.591703134518082763 ) ) ;
#3267 = CARTESIAN_POINT ( 'NONE',  ( 2.229367062499998831, -2.895833331967738289, -3.861377020970580887 ) ) ;
#3268 = CARTESIAN_POINT ( 'NONE',  ( -2.229367062500000163, -41.72916666530107932, -3.861377020970580443 ) ) ;
#3269 = CARTESIAN_POINT ( 'NONE',  ( -9.184850993605147944E-16, -151.3750000027311842, 5.000000000000000000 ) ) ;
#3270 = CARTESIAN_POINT ( 'NONE',  ( -3.152548672688508926E-16, -84.81249999863439371, -5.148502694627439702 ) ) ;
#3271 = CARTESIAN_POINT ( 'NONE',  ( -4.999999999999998224, 16.20833333606451987, 2.886751345948131764 ) ) ;
#3272 = EDGE_LOOP ( 'NONE', ( #36500, #63136, #61501, #59483 ) ) ;
#3273 = CARTESIAN_POINT ( 'NONE',  ( -1.339745962155613812, -95.08034179853028434, -5.000000000000000000 ) ) ;
#3274 =( BOUNDED_CURVE ( )  B_SPLINE_CURVE ( 2, ( #8834, #9451, #48378, #50200, #20630, #53210, #55033, #5824, #28753 ),
 .UNSPECIFIED., .F., .F. ) 
 B_SPLINE_CURVE_WITH_KNOTS ( ( 3, 2, 2, 2, 3 ),
 ( 0.2017857142857142905, 0.2023809523809523836, 0.2035714285714285698, 0.2047619047619047561, 0.2053571428571428492 ),
 .UNSPECIFIED. ) 
 CURVE ( )  GEOMETRIC_REPRESENTATION_ITEM ( )  RATIONAL_B_SPLINE_CURVE ( ( 0.9330127018922194093, 0.9330127018922194093, 1.000000000000000000, 0.8660254037844387076, 1.000000000000000000, 0.8660254037844387076, 1.000000000000000000, 0.9330127018922194093, 0.9330127018922194093 ) ) 
 REPRESENTATION_ITEM ( '' )  );
#3275 = VECTOR ( 'NONE', #5087, 1000.000000000000000 ) ;
#3276 = CARTESIAN_POINT ( 'NONE',  ( 4.458734125000001214, -71.14583333196773651, 2.574251347313718519 ) ) ;
#3277 = CARTESIAN_POINT ( 'NONE',  ( 4.458734124999998549, -8.979166665301073991, -2.574251347313721627 ) ) ;
#3278 = EDGE_LOOP ( 'NONE', ( #3963, #17331, #27113 ) ) ;
#3279 = CARTESIAN_POINT ( 'NONE',  ( 1.975475456537005874E-15, -5.750000000000000000, 5.000000000000000000 ) ) ;
#3280 = CARTESIAN_POINT ( 'NONE',  ( 2.229367062499998831, -6.895833331967741842, -3.861377020970580887 ) ) ;
#3281 = CARTESIAN_POINT ( 'NONE',  ( -51.19402409849444524, -148.6250000027312126, -3.242614290531456334 ) ) ;
#3282 = CARTESIAN_POINT ( 'NONE',  ( -2.229367062500000163, 3.520833334698929118, -3.861377020970580443 ) ) ;
#3283 = CARTESIAN_POINT ( 'NONE',  ( -1.339745962155613812, -43.20534180126148271, -5.000000000000000000 ) ) ;
#3284 = CARTESIAN_POINT ( 'NONE',  ( -1.846868145590734756, -157.1250000013656063, -4.458734124999999437 ) ) ;
#3285 = CARTESIAN_POINT ( 'NONE',  ( 4.458734124999999437, 27.93750000136559208, -5.460374474430324690E-16 ) ) ;
#3286 = ORIENTED_EDGE ( 'NONE', *, *, #61844, .F. ) ;
#3287 = CARTESIAN_POINT ( 'NONE',  ( 9.457646018065525792E-16, -92.06249999863439371, 5.148502694627439702 ) ) ;
#3288 = CARTESIAN_POINT ( 'NONE',  ( -5.000000000000000000, -47.00000000000000000, 0.000000000000000000 ) ) ;
#3289 = CARTESIAN_POINT ( 'NONE',  ( 4.458734125000001214, -9.895833331967736513, 2.574251347313718519 ) ) ;
#3290 = CARTESIAN_POINT ( 'NONE',  ( 5.000000000000000000, -140.0000000000000000, 0.000000000000000000 ) ) ;
#3291 = DIRECTION ( 'NONE',  ( 0.000000000000000000, 1.000000000000000000, 0.000000000000000000 ) ) ;
#3292 = CARTESIAN_POINT ( 'NONE',  ( -2.500000000000000444, 14.83333333333333215, -4.330127018922193649 ) ) ;
#3293 = CARTESIAN_POINT ( 'NONE',  ( 5.000000000000000888, -33.45833333060215153, 2.886751345948126879 ) ) ;
#3294 = CARTESIAN_POINT ( 'NONE',  ( 1.339745962155612702, -78.29465819873851729, -5.000000000000000000 ) ) ;
#3295 = CARTESIAN_POINT ( 'NONE',  ( -4.458734124999997661, 18.77083333469892779, 2.574251347313722516 ) ) ;
#3296 = CARTESIAN_POINT ( 'NONE',  ( -2.229367062500000163, 20.52083333469892779, -3.861377020970580443 ) ) ;
#3297 = CARTESIAN_POINT ( 'NONE',  ( 4.458734125000001214, -55.89583333196773651, 2.574251347313718519 ) ) ;
#3298 = CARTESIAN_POINT ( 'NONE',  ( 2.229367062499998831, -5.895833331967740953, -3.861377020970580887 ) ) ;
#3299 = DIRECTION ( 'NONE',  ( 0.8660254037844382635, 0.5000000000000004441, 0.000000000000000000 ) ) ;
#3300 = CARTESIAN_POINT ( 'NONE',  ( 5.000000000000000000, 12.58333333333333215, -2.886751345948129988 ) ) ;
#3301 = CARTESIAN_POINT ( 'NONE',  ( 2.071067811865475505, -140.9375000027311842, -5.000000000000000888 ) ) ;
#3302 = CARTESIAN_POINT ( 'NONE',  ( -5.000000000000000000, -46.00000000000000000, 0.000000000000000000 ) ) ;
#3303 = CARTESIAN_POINT ( 'NONE',  ( 4.458734124999998549, -50.72916666530107932, -2.574251347313721627 ) ) ;
#3304 = CARTESIAN_POINT ( 'NONE',  ( 2.500000000000002220, -85.54166666393547303, 4.330127018922192761 ) ) ;
#3305 = CARTESIAN_POINT ( 'NONE',  ( -52.10840900171896806, -135.4375000013656063, 3.393966926194110556 ) ) ;
#3306 = CARTESIAN_POINT ( 'NONE',  ( -5.000000000000000000, -87.00000000000000000, 0.000000000000000000 ) ) ;
#3307 = CARTESIAN_POINT ( 'NONE',  ( -56.66612745406286678, -145.3125000000000284, -5.149110718188528502 ) ) ;
#3308 = CARTESIAN_POINT ( 'NONE',  ( -3.152548672688508926E-16, -86.81249999863439371, -5.148502694627439702 ) ) ;
#3309 = CARTESIAN_POINT ( 'NONE',  ( 4.458734124999997661, -157.7500000013656063, 1.846868145590737864 ) ) ;
#3310 = CARTESIAN_POINT ( 'NONE',  ( 5.000000000000000888, -33.58333333333332860, 2.886751345948126879 ) ) ;
#3311 = DIRECTION ( 'NONE',  ( -0.000000000000000000, 1.000000000000000000, -0.000000000000000000 ) ) ;
#3312 = ORIENTED_EDGE ( 'NONE', *, *, #48802, .F. ) ;
#3313 = EDGE_CURVE ( 'NONE', #44876, #44350, #45106, .T. ) ;
#3314 = CARTESIAN_POINT ( 'NONE',  ( 4.458734124999998549, 15.02083333469892601, -2.574251347313721627 ) ) ;
#3315 = ORIENTED_EDGE ( 'NONE', *, *, #51602, .T. ) ;
#3316 = CARTESIAN_POINT ( 'NONE',  ( -2.229367062499996610, -98.14583333196773651, 3.861377020970582219 ) ) ;
#3317 = CARTESIAN_POINT ( 'NONE',  ( 2.229367062499998831, 7.104166668032259935, -3.861377020970580887 ) ) ;
#3318 = CARTESIAN_POINT ( 'NONE',  ( -2.499999999999996447, 10.29166666939785024, 4.330127018922195425 ) ) ;
#3319 = CARTESIAN_POINT ( 'NONE',  ( -4.999999999999998224, -43.79166666393546592, 2.886751345948131764 ) ) ;
#3320 = EDGE_CURVE ( 'NONE', #51834, #16219, #36862, .T. ) ;
#3321 = CARTESIAN_POINT ( 'NONE',  ( 5.000000000000000000, 8.583333333333330373, -2.886751345948129988 ) ) ;
#3322 = CARTESIAN_POINT ( 'NONE',  ( 4.458734124999999437, -59.81249999863440081, -5.460374474430324690E-16 ) ) ;
#3323 = CARTESIAN_POINT ( 'NONE',  ( -4.999999999999998224, -39.91666666666667140, 2.886751345948131764 ) ) ;
#3324 = CARTESIAN_POINT ( 'NONE',  ( -2.499999999999996447, -80.83333333333332860, 4.330127018922195425 ) ) ;
#3325 = EDGE_CURVE ( 'NONE', #42376, #58224, #10165, .T. ) ;
#3326 = CARTESIAN_POINT ( 'NONE',  ( -2.229367062500000163, -26.47916666530106866, -3.861377020970580443 ) ) ;
#3327 = CARTESIAN_POINT ( 'NONE',  ( -6.972266317189433020E-16, 7.875000002731185056, -5.000000000000000000 ) ) ;
#3328 = CARTESIAN_POINT ( 'NONE',  ( 1.339745962155612702, -63.29465819873851729, -5.000000000000000000 ) ) ;
#3329 = DIRECTION ( 'NONE',  ( -0.6485228581062915110, 0.000000000000000000, -0.7611951803011149931 ) ) ;
#3330 = CARTESIAN_POINT ( 'NONE',  ( 2.500000000000002220, -37.66666666666666430, 4.330127018922192761 ) ) ;
#3331 = CARTESIAN_POINT ( 'NONE',  ( 5.000000000000000000, -149.0000000000000284, 0.000000000000000000 ) ) ;
#3333 = CARTESIAN_POINT ( 'NONE',  ( 2.229367062500001939, -19.22916666530106866, 3.861377020970579999 ) ) ;
#3332 = CARTESIAN_POINT ( 'NONE',  ( -6.972266317189433020E-16, -48.24999999999999289, -5.000000000000000000 ) ) ;
#3334 = CARTESIAN_POINT ( 'NONE',  ( 3.061616997868383141E-16, -143.7500000000000284, -5.000000000000000000 ) ) ;
#3335 = CARTESIAN_POINT ( 'NONE',  ( -4.458734124999998549, -66.22916666530107932, 2.574251347313722516 ) ) ;
#3336 = CARTESIAN_POINT ( 'NONE',  ( 4.458734125000000326, -147.6250000013655779, -1.846868145590734978 ) ) ;
#3337 = CARTESIAN_POINT ( 'NONE',  ( 2.229367062499998831, -76.64583333196773651, -3.861377020970580887 ) ) ;
#3338 = CARTESIAN_POINT ( 'NONE',  ( -52.10840900171896806, -144.4375000013656063, 3.393966926194110556 ) ) ;
#3339 = CARTESIAN_POINT ( 'NONE',  ( 2.229367062500001939, -26.22916666530106866, 3.861377020970579999 ) ) ;
#3340 = CARTESIAN_POINT ( 'NONE',  ( 5.000000000000000888, -64.45833333060213022, 2.886751345948126879 ) ) ;
#3341 = ORIENTED_EDGE ( 'NONE', *, *, #11857, .F. ) ;
#3342 = CARTESIAN_POINT ( 'NONE',  ( -5.000000000000000000, -22.08333333333333215, -2.886751345948128211 ) ) ;
#3343 = ORIENTED_EDGE ( 'NONE', *, *, #42928, .T. ) ;
#3344 = CARTESIAN_POINT ( 'NONE',  ( -4.458734124999999437, -67.56249999863440792, 0.000000000000000000 ) ) ;
#3345 = CARTESIAN_POINT ( 'NONE',  ( -6.972266317189433020E-16, -16.25000000000000000, -5.000000000000000000 ) ) ;
#3346 = ORIENTED_EDGE ( 'NONE', *, *, #38919, .T. ) ;
#3347 = CARTESIAN_POINT ( 'NONE',  ( -54.60164318462004474, -125.3750000000000142, -4.984105922594373794 ) ) ;
#3348 = CARTESIAN_POINT ( 'NONE',  ( -5.000000000000000000, -55.95833333060214443, -2.886751345948128211 ) ) ;
#3349 = CARTESIAN_POINT ( 'NONE',  ( -2.229367062499996610, -52.39583333196773651, 3.861377020970582219 ) ) ;
#3350 = ORIENTED_EDGE ( 'NONE', *, *, #9525, .T. ) ;
#3351 = CARTESIAN_POINT ( 'NONE',  ( 0.000000000000000000, -120.0000000000000000, 0.000000000000000000 ) ) ;
#3352 = CARTESIAN_POINT ( 'NONE',  ( -4.458734124999999437, 10.60416666803225993, -2.574251347313719407 ) ) ;
#3353 = CARTESIAN_POINT ( 'NONE',  ( -4.458734124999999437, 20.60416666803225993, -2.574251347313719407 ) ) ;
#3354 = CARTESIAN_POINT ( 'NONE',  ( -57.89159099828107458, -148.6875000013656063, -3.393966926194107447 ) ) ;
#3355 = CARTESIAN_POINT ( 'NONE',  ( -5.000000000000000000, 6.125000002731185056, 0.000000000000000000 ) ) ;
#3356 = CARTESIAN_POINT ( 'NONE',  ( 1.975475456537005874E-15, -8.750000000000000000, 5.000000000000000000 ) ) ;
#3357 = ORIENTED_EDGE ( 'NONE', *, *, #61839, .F. ) ;
#3358 = CARTESIAN_POINT ( 'NONE',  ( -4.458734124999999437, -72.39583333196773651, -2.574251347313719407 ) ) ;
#3359 = CARTESIAN_POINT ( 'NONE',  ( -1.336351044127974539E-14, 22.24999999999999645, 5.000000000000000000 ) ) ;
#3360 = CARTESIAN_POINT ( 'NONE',  ( -2.229367062500000163, 8.520833334698926009, -3.861377020970580443 ) ) ;
#3361 =( BOUNDED_CURVE ( )  B_SPLINE_CURVE ( 2, ( #35283, #15978, #15021, #54904, #15347, #39769, #55229, #31088, #45247 ),
 .UNSPECIFIED., .F., .F. ) 
 B_SPLINE_CURVE_WITH_KNOTS ( ( 3, 2, 2, 2, 3 ),
 ( 0.6645833333333333037, 0.6652777777777777457, 0.6666666666666666297, 0.6680555555555555136, 0.6687499999999999556 ),
 .UNSPECIFIED. ) 
 CURVE ( )  GEOMETRIC_REPRESENTATION_ITEM ( )  RATIONAL_B_SPLINE_CURVE ( ( 0.9330127018922194093, 0.9330127018922194093, 1.000000000000000000, 0.8660254037844387076, 1.000000000000000000, 0.8660254037844387076, 1.000000000000000000, 0.9330127018922194093, 0.9330127018922194093 ) ) 
 REPRESENTATION_ITEM ( '' )  );
#3362 = CARTESIAN_POINT ( 'NONE',  ( 1.975475456537005874E-15, -88.74999999999998579, 5.000000000000000000 ) ) ;
#3363 = CARTESIAN_POINT ( 'NONE',  ( 2.229367062500001939, -60.22916666530106511, 3.861377020970579999 ) ) ;
#3364 = CARTESIAN_POINT ( 'NONE',  ( 2.499999999999998668, -19.20833333060214798, -4.330127018922193649 ) ) ;
#3365 = CARTESIAN_POINT ( 'NONE',  ( 5.000000000000000888, 4.416666666666666075, 2.886751345948126879 ) ) ;
#3366 = LINE ( 'NONE', #35310, #56306 ) ;
#3367 = CARTESIAN_POINT ( 'NONE',  ( 5.000000000000000000, -30.37499999726881228, -6.123233995736766282E-16 ) ) ;
#3368 = DIRECTION ( 'NONE',  ( -0.000000000000000000, 1.000000000000000000, -0.000000000000000000 ) ) ;
#3369 = CARTESIAN_POINT ( 'NONE',  ( -52.53715891517739323, -146.4375000000000000, -4.819101127000233298 ) ) ;
#3370 = CARTESIAN_POINT ( 'NONE',  ( -4.458734124999998549, -43.22916666530105800, 2.574251347313722516 ) ) ;
#3371 = CARTESIAN_POINT ( 'NONE',  ( 4.458734125000000326, -23.14583333196772941, 2.574251347313718519 ) ) ;
#3372 = ORIENTED_EDGE ( 'NONE', *, *, #49435, .T. ) ;
#3373 = DIRECTION ( 'NONE',  ( -0.000000000000000000, 1.000000000000000000, -0.000000000000000000 ) ) ;
#3374 = CARTESIAN_POINT ( 'NONE',  ( -2.229367062500000163, -108.4791666653010651, -3.861377020970580443 ) ) ;
#3375 = CARTESIAN_POINT ( 'NONE',  ( -3.535533905932737309, -152.7500000027312126, -3.535533905932738197 ) ) ;
#3376 = EDGE_LOOP ( 'NONE', ( #43952, #19473, #42253, #25414 ) ) ;
#3377 = CARTESIAN_POINT ( 'NONE',  ( -2.229367062499996610, -108.3958333319677365, 3.861377020970582219 ) ) ;
#3378 = CARTESIAN_POINT ( 'NONE',  ( 2.229367062500001939, -30.97916666530107221, 3.861377020970579999 ) ) ;
#3379 = CARTESIAN_POINT ( 'NONE',  ( -5.000000000000000000, -66.95833333060214443, -2.886751345948128211 ) ) ;
#3380 = CARTESIAN_POINT ( 'NONE',  ( -51.60603307380591787, -147.1875000013656063, -2.891590998281053704 ) ) ;
#3381 = CARTESIAN_POINT ( 'NONE',  ( -2.071067811865475061, -148.6875000000000568, -5.000000000000000888 ) ) ;
#3382 = ADVANCED_BREP_SHAPE_REPRESENTATION ( '', ( #7586, #43054 ), #38957 ) ;
#3383 = CARTESIAN_POINT ( 'NONE',  ( 4.458734124999998549, -29.72916666530107221, -2.574251347313721627 ) ) ;
#3384 = CARTESIAN_POINT ( 'NONE',  ( 2.229367062499998831, -69.89583333196773651, -3.861377020970580887 ) ) ;
#3385 = CARTESIAN_POINT ( 'NONE',  ( -51.75738570946856498, -136.7500000000000284, 3.805975901505576964 ) ) ;
#3386 = CARTESIAN_POINT ( 'NONE',  ( 4.458734125000000326, -26.89583333196774007, 2.574251347313718519 ) ) ;
#3387 = CARTESIAN_POINT ( 'NONE',  ( 5.000000000000000000, -32.37499999726880873, -6.123233995736766282E-16 ) ) ;
#3388 = CARTESIAN_POINT ( 'NONE',  ( 0.000000000000000000, -120.0000000000000000, 0.000000000000000000 ) ) ;
#3389 = CARTESIAN_POINT ( 'NONE',  ( 1.060575238724906964E-15, -14.75000000000000000, 5.773502691896257311 ) ) ;
#3390 = CARTESIAN_POINT ( 'NONE',  ( 1.846868145590736310, -147.6250000013655779, 4.458734124999999437 ) ) ;
#3391 = ORIENTED_EDGE ( 'NONE', *, *, #468, .F. ) ;
#3392 = CARTESIAN_POINT ( 'NONE',  ( -4.999999999999998224, -81.91666666666667140, 2.886751345948131764 ) ) ;
#3393 = CARTESIAN_POINT ( 'NONE',  ( -2.229367062499996610, -55.39583333196773651, 3.861377020970582219 ) ) ;
#3394 = CARTESIAN_POINT ( 'NONE',  ( -3.535250795749689387E-16, 25.87500000273118772, -5.773502691896257311 ) ) ;
#3395 = CARTESIAN_POINT ( 'NONE',  ( 1.339745962155612702, -81.16965819600734733, -5.000000000000000000 ) ) ;
#3396 = CARTESIAN_POINT ( 'NONE',  ( 2.499999999999998668, 21.66666666666666785, -4.330127018922193649 ) ) ;
#3397 = CARTESIAN_POINT ( 'NONE',  ( -50.01589407740564042, -152.6250000000000284, 0.3983568153799778022 ) ) ;
#3398 = CARTESIAN_POINT ( 'NONE',  ( 4.458734124999999437, 0.1875000013655953035, -5.460374474430324690E-16 ) ) ;
#3399 = CARTESIAN_POINT ( 'NONE',  ( 1.975475456537005874E-15, -48.74999999999999289, 5.000000000000000000 ) ) ;
#3400 = CARTESIAN_POINT ( 'NONE',  ( -5.000000000000000000, -164.5000000000000000, -6.123233995736766282E-16 ) ) ;
#3401 = CARTESIAN_POINT ( 'NONE',  ( -2.229367062499996610, 11.60416666803225993, 3.861377020970582219 ) ) ;
#3402 = ORIENTED_EDGE ( 'NONE', *, *, #2883, .F. ) ;
#3403 = CARTESIAN_POINT ( 'NONE',  ( 1.975475456537005874E-15, -32.74999999999999289, 5.000000000000000000 ) ) ;
#3404 = ORIENTED_EDGE ( 'NONE', *, *, #38840, .T. ) ;
#3405 = CARTESIAN_POINT ( 'NONE',  ( 5.000000000000000000, -168.1250000027312126, 0.000000000000000000 ) ) ;
#3406 = CARTESIAN_POINT ( 'NONE',  ( 9.457646018065525792E-16, -51.06249999863440792, 5.148502694627439702 ) ) ;
#3407 = CARTESIAN_POINT ( 'NONE',  ( 3.152801135295366208, -159.8125000013656063, 3.152801135295367985 ) ) ;
#3408 = CARTESIAN_POINT ( 'NONE',  ( -5.000000000000000000, -46.87499999726880873, 0.000000000000000000 ) ) ;
#3409 = ORIENTED_EDGE ( 'NONE', *, *, #31803, .T. ) ;
#3410 = CARTESIAN_POINT ( 'NONE',  ( 4.458734124999998549, -21.72916666530107221, -2.574251347313721627 ) ) ;
#3411 = ORIENTED_EDGE ( 'NONE', *, *, #17799, .F. ) ;
#3412 =( BOUNDED_CURVE ( )  B_SPLINE_CURVE ( 2, ( #11523, #60747, #55607, #7351, #45622, #16672, #21820, #27272, #36293 ),
 .UNSPECIFIED., .F., .F. ) 
 B_SPLINE_CURVE_WITH_KNOTS ( ( 3, 2, 2, 2, 3 ),
 ( 0.6196428571428571619, 0.6202380952380952550, 0.6214285714285714413, 0.6226190476190476275, 0.6232142857142857206 ),
 .UNSPECIFIED. ) 
 CURVE ( )  GEOMETRIC_REPRESENTATION_ITEM ( )  RATIONAL_B_SPLINE_CURVE ( ( 0.9330127018922194093, 0.9330127018922194093, 1.000000000000000000, 0.8660254037844387076, 1.000000000000000000, 0.8660254037844387076, 1.000000000000000000, 0.9330127018922194093, 0.9330127018922194093 ) ) 
 REPRESENTATION_ITEM ( '' )  );
#3413 = CARTESIAN_POINT ( 'NONE',  ( 1.975475456537005874E-15, -11.74999999999999645, 5.000000000000000000 ) ) ;
#3414 = CARTESIAN_POINT ( 'NONE',  ( -4.458734124999999437, -159.9375000013655779, -5.460374474430324690E-16 ) ) ;
#3415 = CARTESIAN_POINT ( 'NONE',  ( -50.01589407740564042, -136.6250000000000284, 0.3983568153799778022 ) ) ;
#3416 = EDGE_CURVE ( 'NONE', #54097, #21555, #54510, .T. ) ;
#3417 = CARTESIAN_POINT ( 'NONE',  ( 2.229367062500001939, -38.22916666530107221, 3.861377020970579999 ) ) ;
#3418 = CARTESIAN_POINT ( 'NONE',  ( -50.01589407740564042, -140.6250000000000284, 0.3983568153799778022 ) ) ;
#3419 = ORIENTED_EDGE ( 'NONE', *, *, #28398, .T. ) ;
#3420 = CARTESIAN_POINT ( 'NONE',  ( 2.229367062499998831, -80.64583333196773651, -3.861377020970580887 ) ) ;
#3421 = CARTESIAN_POINT ( 'NONE',  ( 4.458734124999999437, 23.18750000136559564, -5.460374474430324690E-16 ) ) ;
#3422 = DIRECTION ( 'NONE',  ( 0.000000000000000000, 0.000000000000000000, 1.000000000000000000 ) ) ;
#3423 = ORIENTED_EDGE ( 'NONE', *, *, #31816, .F. ) ;
#3424 = CARTESIAN_POINT ( 'NONE',  ( 2.499999999999998668, -69.20833333060214443, -4.330127018922193649 ) ) ;
#3425 = CARTESIAN_POINT ( 'NONE',  ( -56.48576386720575471, -138.0000000013656063, -4.591703134518078322 ) ) ;
#3426 = CARTESIAN_POINT ( 'NONE',  ( 4.458734125000001214, -84.14583333196772230, 2.574251347313718519 ) ) ;
#3427 = CARTESIAN_POINT ( 'NONE',  ( -58.80597590150559739, -130.1250000027312126, 3.242614290531460330 ) ) ;
#3428 = DIRECTION ( 'NONE',  ( -0.000000000000000000, 1.000000000000000000, -0.000000000000000000 ) ) ;
#3429 = CARTESIAN_POINT ( 'NONE',  ( 3.152801135295366208, -139.8125000013655779, 3.152801135295367985 ) ) ;
#3430 = CARTESIAN_POINT ( 'NONE',  ( 2.500000000000002220, 4.333333333333331261, 4.330127018922192761 ) ) ;
#3431 = CARTESIAN_POINT ( 'NONE',  ( 4.458734124999998549, -53.72916666530107932, -2.574251347313721627 ) ) ;
#3432 = CARTESIAN_POINT ( 'NONE',  ( -6.972266317189433020E-16, -72.12499999726878741, -5.000000000000000000 ) ) ;
#3433 = CARTESIAN_POINT ( 'NONE',  ( -4.458734124999999437, 22.68750000136559564, 0.000000000000000000 ) ) ;
#3434 = CARTESIAN_POINT ( 'NONE',  ( 5.000000000000000888, -97.58333333333332860, 2.886751345948126879 ) ) ;
#3435 = CARTESIAN_POINT ( 'NONE',  ( -2.500000000000000444, -82.16666666666667140, -4.330127018922193649 ) ) ;
#3436 = CARTESIAN_POINT ( 'NONE',  ( 2.229367062499998831, -42.89583333196773651, -3.861377020970580887 ) ) ;
#3437 = CARTESIAN_POINT ( 'NONE',  ( -2.499999999999996447, -2.708333330602146649, 4.330127018922195425 ) ) ;
#3438 = CARTESIAN_POINT ( 'NONE',  ( 0.000000000000000000, -170.0000000000000000, 5.000000000000000000 ) ) ;
#3439 = CARTESIAN_POINT ( 'NONE',  ( -4.999999999999998224, -45.79166666393547303, 2.886751345948131764 ) ) ;
#3440 = CARTESIAN_POINT ( 'NONE',  ( 2.229367062499998831, -86.89583333196773651, -3.861377020970580887 ) ) ;
#3441 = CARTESIAN_POINT ( 'NONE',  ( -4.458734124999999437, -100.3958333319677365, -2.574251347313719407 ) ) ;
#3442 = CARTESIAN_POINT ( 'NONE',  ( 4.458734124999998549, -6.979166665301073103, -2.574251347313721627 ) ) ;
#3443 = ORIENTED_EDGE ( 'NONE', *, *, #61012, .T. ) ;
#3444 = CARTESIAN_POINT ( 'NONE',  ( 1.339745962155615144, -9.580341798530296771, 4.999999999999999112 ) ) ;
#3445 = CARTESIAN_POINT ( 'NONE',  ( 9.457646018065525792E-16, -91.06249999863439371, 5.148502694627439702 ) ) ;
#3446 = CARTESIAN_POINT ( 'NONE',  ( -3.535533905932737309, -163.7500000027312126, -3.535533905932738197 ) ) ;
#3447 = CARTESIAN_POINT ( 'NONE',  ( -3.152548672688508926E-16, -93.81249999863440792, -5.148502694627439702 ) ) ;
#3448 = CARTESIAN_POINT ( 'NONE',  ( 9.457646018065525792E-16, 6.687500001365594748, 5.148502694627439702 ) ) ;
#3449 = CARTESIAN_POINT ( 'NONE',  ( -5.000000000000000000, -16.00000000000000000, 0.000000000000000000 ) ) ;
#3450 = CARTESIAN_POINT ( 'NONE',  ( -58.39396692619412477, -129.4375000013656063, 2.891590998281057701 ) ) ;
#3451 = CARTESIAN_POINT ( 'NONE',  ( -4.458734124999999437, -12.31249999863440259, 0.000000000000000000 ) ) ;
#3452 = CARTESIAN_POINT ( 'NONE',  ( -3.152548672688508926E-16, 11.18750000136559564, -5.148502694627439702 ) ) ;
#3453 = CARTESIAN_POINT ( 'NONE',  ( -4.458734124999999437, -53.56249999863439371, 0.000000000000000000 ) ) ;
#3454 = CYLINDRICAL_SURFACE ( 'NONE', #36649, 5.000000000000000000 ) ;
#3455 = DIRECTION ( 'NONE',  ( 0.000000000000000000, 0.000000000000000000, 1.000000000000000000 ) ) ;
#3456 = CARTESIAN_POINT ( 'NONE',  ( 2.229367062499998831, -10.64583333196773829, -3.861377020970580887 ) ) ;
#3457 = LINE ( 'NONE', #27885, #15470 ) ;
#3458 = ORIENTED_EDGE ( 'NONE', *, *, #37048, .T. ) ;
#3459 = CARTESIAN_POINT ( 'NONE',  ( -4.458734124999999437, -37.64583333196774362, -2.574251347313719407 ) ) ;
#3460 =( BOUNDED_CURVE ( )  B_SPLINE_CURVE ( 2, ( #45855, #29770, #14987, #34597, #54227, #49404, #30417, #25604, #5348 ),
 .UNSPECIFIED., .F., .F. ) 
 B_SPLINE_CURVE_WITH_KNOTS ( ( 3, 2, 2, 2, 3 ),
 ( 0.03125000000000000000, 0.03194444444444444198, 0.03333333333333333287, 0.03472222222222222376, 0.03541666666666666574 ),
 .UNSPECIFIED. ) 
 CURVE ( )  GEOMETRIC_REPRESENTATION_ITEM ( )  RATIONAL_B_SPLINE_CURVE ( ( 0.9330127018922194093, 0.9330127018922195203, 1.000000000000000000, 0.8660254037844387076, 1.000000000000000000, 0.8660254037844387076, 1.000000000000000000, 0.9330127018922194093, 0.9330127018922194093 ) ) 
 REPRESENTATION_ITEM ( '' )  );
#3461 = CARTESIAN_POINT ( 'NONE',  ( -57.19623071787017210, -129.6250000013655779, 4.297418129356382899 ) ) ;
#3462 = CYLINDRICAL_SURFACE ( 'NONE', #45221, 5.000000000000000000 ) ;
#3463 = DIRECTION ( 'NONE',  ( -0.000000000000000000, 1.000000000000000000, -0.000000000000000000 ) ) ;
#3464 = CARTESIAN_POINT ( 'NONE',  ( -4.458734124999999437, -81.39583333196773651, -2.574251347313719407 ) ) ;
#3465 = CARTESIAN_POINT ( 'NONE',  ( -4.458734124999998549, 24.52083333469892779, 2.574251347313722516 ) ) ;
#3466 = AXIS2_PLACEMENT_3D ( 'NONE', #63142, #28087, #43187 ) ;
#3467 = CARTESIAN_POINT ( 'NONE',  ( 4.458734124999999437, 14.18750000136559386, -5.460374474430324690E-16 ) ) ;
#3468 = CYLINDRICAL_SURFACE ( 'NONE', #13361, 5.000000000000000000 ) ;
#3469 = CARTESIAN_POINT ( 'NONE',  ( -6.972266317189433020E-16, -55.24999999999999289, -5.000000000000000000 ) ) ;
#3470 = CARTESIAN_POINT ( 'NONE',  ( -4.458734124999999437, -81.64583333196773651, -2.574251347313719407 ) ) ;
#3471 = CARTESIAN_POINT ( 'NONE',  ( -5.000000000000000000, -72.08333333333332860, -2.886751345948128211 ) ) ;
#3472 = CARTESIAN_POINT ( 'NONE',  ( 5.000000000000000888, 18.54166666939785202, 2.886751345948126879 ) ) ;
#3473 = ORIENTED_EDGE ( 'NONE', *, *, #45337, .F. ) ;
#3474 = CARTESIAN_POINT ( 'NONE',  ( 1.062108568985190270E-13, -25.25000000000000355, -4.999999999999999112 ) ) ;
#3475 = CARTESIAN_POINT ( 'NONE',  ( 0.000000000000000000, -120.0000000000000000, 0.000000000000000000 ) ) ;
#3477 = CARTESIAN_POINT ( 'NONE',  ( 2.500000000000002220, -26.66666666666666430, 4.330127018922192761 ) ) ;
#3476 = CARTESIAN_POINT ( 'NONE',  ( -4.999999999999998224, -108.7916666639354730, 2.886751345948131764 ) ) ;
#3478 = CARTESIAN_POINT ( 'NONE',  ( 2.229367062500001939, -30.97916666530107221, 3.861377020970579999 ) ) ;
#3479 = LINE ( 'NONE', #12803, #11933 ) ;
#3480 = CARTESIAN_POINT ( 'NONE',  ( -2.499999999999996447, -30.70833333060214443, 4.330127018922195425 ) ) ;
#3482 = VERTEX_POINT ( 'NONE', #15779 ) ;
#3481 = CARTESIAN_POINT ( 'NONE',  ( 9.457646018065525792E-16, -59.06249999863439371, 5.148502694627439702 ) ) ;
#3483 = FACE_OUTER_BOUND ( 'NONE', #3376, .T. ) ;
#3485 = ORIENTED_EDGE ( 'NONE', *, *, #31168, .F. ) ;
#3484 = CARTESIAN_POINT ( 'NONE',  ( 2.229367062499998831, -6.895833331967741842, -3.861377020970580887 ) ) ;
#3486 = CARTESIAN_POINT ( 'NONE',  ( 1.060575238724906964E-15, -75.75000000000000000, 5.773502691896257311 ) ) ;
#3487 = CARTESIAN_POINT ( 'NONE',  ( -2.499999999999996447, 1.291666669397853351, 4.330127018922195425 ) ) ;
#3488 = CARTESIAN_POINT ( 'NONE',  ( 2.229367062500001939, -51.22916666530107221, 3.861377020970579999 ) ) ;
#3489 = CARTESIAN_POINT ( 'NONE',  ( -2.499999999999996447, -77.70833333060214443, 4.330127018922195425 ) ) ;
#3491 = VERTEX_POINT ( 'NONE', #6771 ) ;
#3490 = CARTESIAN_POINT ( 'NONE',  ( 2.500000000000002220, -65.54166666393547303, 4.330127018922192761 ) ) ;
#3492 = CARTESIAN_POINT ( 'NONE',  ( -58.24261429053147765, -150.2500000000000284, -3.805975901505573855 ) ) ;
#3493 = EDGE_CURVE ( 'NONE', #57905, #6259, #7745, .T. ) ;
#3494 = CARTESIAN_POINT ( 'NONE',  ( -4.458734124999999437, -22.56249999863440436, 0.000000000000000000 ) ) ;
#3496 = ORIENTED_EDGE ( 'NONE', *, *, #18968, .T. ) ;
#3495 = CARTESIAN_POINT ( 'NONE',  ( -2.229367062499996610, -59.39583333196773651, 3.861377020970582219 ) ) ;
#3497 = CARTESIAN_POINT ( 'NONE',  ( -4.458734125000000326, -140.0000000013655779, -1.846868145590735644 ) ) ;
#3498 = CARTESIAN_POINT ( 'NONE',  ( -2.229367062499996610, -99.39583333196773651, 3.861377020970582219 ) ) ;
#3499 = CARTESIAN_POINT ( 'NONE',  ( -1.339745962155613812, 17.79465819873852439, -5.000000000000000000 ) ) ;
#3500 = ORIENTED_EDGE ( 'NONE', *, *, #62930, .F. ) ;
#3501 = CARTESIAN_POINT ( 'NONE',  ( -59.59170313451810586, -150.7500000013655779, 1.485763867205729394 ) ) ;
#3502 = CARTESIAN_POINT ( 'NONE',  ( -60.14911071818854538, -144.1875000027312410, 1.666127454062681368 ) ) ;
#3503 = CARTESIAN_POINT ( 'NONE',  ( 6.123233995736766282E-16, -120.0000000000000000, -5.000000000000000000 ) ) ;
#3504 = CARTESIAN_POINT ( 'NONE',  ( 2.229367062499998831, -7.645833331967735624, -3.861377020970580887 ) ) ;
#3505 = CARTESIAN_POINT ( 'NONE',  ( 2.229367062499998831, -92.89583333196773651, -3.861377020970580887 ) ) ;
#3506 = AXIS2_PLACEMENT_3D ( 'NONE', #21936, #46383, #51216 ) ;
#3507 = EDGE_CURVE ( 'NONE', #8539, #41687, #56207, .T. ) ;
#3508 = CARTESIAN_POINT ( 'NONE',  ( 1.846868145590736310, -143.8750000013656063, 4.458734124999999437 ) ) ;
#3509 = CARTESIAN_POINT ( 'NONE',  ( 9.457646018065525792E-16, -30.31249999863440436, 5.148502694627439702 ) ) ;
#3510 = ADVANCED_FACE ( 'NONE', ( #1329 ), #16096, .T. ) ;
#3511 = CARTESIAN_POINT ( 'NONE',  ( -2.499999999999996447, -66.83333333333332860, 4.330127018922195425 ) ) ;
#3512 = CARTESIAN_POINT ( 'NONE',  ( -52.80376928212989185, -135.8750000013655779, -4.297418129356379346 ) ) ;
#3513 = CARTESIAN_POINT ( 'NONE',  ( 4.458734124999999437, -67.06249999863440792, -5.460374474430324690E-16 ) ) ;
#3514 = CARTESIAN_POINT ( 'NONE',  ( 5.000000000000000000, -43.50000000000000000, -6.123233995736766282E-16 ) ) ;
#3515 = CARTESIAN_POINT ( 'NONE',  ( -5.000000000000000000, -34.00000000000000000, 0.000000000000000000 ) ) ;
#3516 = CARTESIAN_POINT ( 'NONE',  ( -4.458734124999999437, -140.0000000013655779, -1.846868145590735644 ) ) ;
#3517 = CARTESIAN_POINT ( 'NONE',  ( 4.458734125000000326, 10.85416666803225993, 2.574251347313718519 ) ) ;
#3518 = ORIENTED_EDGE ( 'NONE', *, *, #54318, .F. ) ;
#3519 = CARTESIAN_POINT ( 'NONE',  ( -5.000000000000000000, -49.87499999726881583, 0.000000000000000000 ) ) ;
#3520 = CARTESIAN_POINT ( 'NONE',  ( 0.000000000000000000, -170.0000000000000000, 0.000000000000000000 ) ) ;
#3522 = CARTESIAN_POINT ( 'NONE',  ( -3.152548672688508926E-16, -24.56249999863440792, -5.148502694627439702 ) ) ;
#3521 = CARTESIAN_POINT ( 'NONE',  ( 1.060575238724906964E-15, -88.74999999999998579, 5.773502691896257311 ) ) ;
#3523 = FACE_OUTER_BOUND ( 'NONE', #29654, .T. ) ;
#3524 = CARTESIAN_POINT ( 'NONE',  ( 2.229367062499998831, -73.89583333196773651, -3.861377020970580887 ) ) ;
#3525 = CARTESIAN_POINT ( 'NONE',  ( 2.229367062499998831, 27.10416666803225993, -3.861377020970580887 ) ) ;
#3526 = DIRECTION ( 'NONE',  ( 1.000000000000000000, 0.000000000000000000, 0.000000000000000000 ) ) ;
#3527 = EDGE_CURVE ( 'NONE', #39251, #38768, #46894, .T. ) ;
#3528 = CARTESIAN_POINT ( 'NONE',  ( -50.55543936806279248, -144.0625000013656063, 0.3552334253322060320 ) ) ;
#3529 = CARTESIAN_POINT ( 'NONE',  ( -4.458734124999999437, 0.6875000013655957476, 0.000000000000000000 ) ) ;
#3530 = CARTESIAN_POINT ( 'NONE',  ( 4.458734124999998549, 28.02083333469892779, -2.574251347313721627 ) ) ;
#3531 = CARTESIAN_POINT ( 'NONE',  ( -4.458734124999999437, -36.56249999863440792, 0.000000000000000000 ) ) ;
#3532 = CARTESIAN_POINT ( 'NONE',  ( -1.339745962155610925, -3.669658196007335338, 5.000000000000000000 ) ) ;
#3533 = CARTESIAN_POINT ( 'NONE',  ( 4.458734124999998549, 7.270833334698930450, -2.574251347313721627 ) ) ;
#3534 = CARTESIAN_POINT ( 'NONE',  ( -2.229367062500000163, -70.47916666530107932, -3.861377020970580443 ) ) ;
#3535 = CARTESIAN_POINT ( 'NONE',  ( -3.152548672688508926E-16, -21.81249999863440436, -5.148502694627439702 ) ) ;
#3536 = CARTESIAN_POINT ( 'NONE',  ( -5.000000000000000000, -8.000000000000000000, 0.000000000000000000 ) ) ;
#3537 = CARTESIAN_POINT ( 'NONE',  ( -8.190561711645485556E-16, -161.6875000013655779, 4.458734124999999437 ) ) ;
#3538 = CARTESIAN_POINT ( 'NONE',  ( -3.535533905932738641, -158.3750000000000284, 3.535533905932737309 ) ) ;
#3539 = CARTESIAN_POINT ( 'NONE',  ( -2.229367062499996610, -65.14583333196773651, 3.861377020970582219 ) ) ;
#3540 = CARTESIAN_POINT ( 'NONE',  ( -5.000000000000000000, -100.8749999972688158, 0.000000000000000000 ) ) ;
#3541 =( BOUNDED_CURVE ( )  B_SPLINE_CURVE ( 2, ( #44303, #29187, #48814, #267, #63628, #38527, #9893, #19548, #58155 ),
 .UNSPECIFIED., .F., .F. ) 
 B_SPLINE_CURVE_WITH_KNOTS ( ( 3, 2, 2, 2, 3 ),
 ( 0.04166666666666670599, 0.04583333333333337173, 0.05000000000000004441, 0.05416666666666671709, 0.05833333333333338283 ),
 .UNSPECIFIED. ) 
 CURVE ( )  GEOMETRIC_REPRESENTATION_ITEM ( )  RATIONAL_B_SPLINE_CURVE ( ( 0.9999999999999992228, 0.9238795325112875156, 1.000000000000000000, 0.9238795325112867385, 1.000000000000000000, 0.9238795325112867385, 1.000000000000000000, 0.9238795325112858503, 1.000000000000000888 ) ) 
 REPRESENTATION_ITEM ( '' )  );
#3542 = CARTESIAN_POINT ( 'NONE',  ( 2.500000000000002220, 15.33333333333333215, 4.330127018922192761 ) ) ;
#3543 = CARTESIAN_POINT ( 'NONE',  ( 2.229367062500001939, -41.97916666530107932, 3.861377020970579999 ) ) ;
#3544 = EDGE_CURVE ( 'NONE', #28828, #31465, #43411, .T. ) ;
#3545 = CARTESIAN_POINT ( 'NONE',  ( -4.458734124999999437, -106.5624999986343937, 0.000000000000000000 ) ) ;
#3546 = CARTESIAN_POINT ( 'NONE',  ( 9.457646018065525792E-16, -66.31249999863440792, 5.148502694627439702 ) ) ;
#3547 = CARTESIAN_POINT ( 'NONE',  ( -2.500000000000000444, -56.16666666666667140, -4.330127018922193649 ) ) ;
#3548 = CARTESIAN_POINT ( 'NONE',  ( -5.000000000000000000, -23.00000000000000000, 0.000000000000000000 ) ) ;
#3549 = CARTESIAN_POINT ( 'NONE',  ( 2.499999999999998668, -89.33333333333332860, -4.330127018922193649 ) ) ;
#3550 = VERTEX_POINT ( 'NONE', #54702 ) ;
#3551 = DIRECTION ( 'NONE',  ( -0.000000000000000000, 1.000000000000000000, -0.000000000000000000 ) ) ;
#3552 = CARTESIAN_POINT ( 'NONE',  ( -6.972266317189433020E-16, -6.124999997268813168, -5.000000000000000000 ) ) ;
#3553 = CARTESIAN_POINT ( 'NONE',  ( 5.000000000000000000, -13.41666666666666607, -2.886751345948129988 ) ) ;
#3554 = CARTESIAN_POINT ( 'NONE',  ( -4.458734124999999437, -17.39583333196773651, -2.574251347313719407 ) ) ;
#3555 = CARTESIAN_POINT ( 'NONE',  ( 9.457646018065525792E-16, -75.06249999863440792, 5.148502694627439702 ) ) ;
#3556 = AXIS2_PLACEMENT_3D ( 'NONE', #37023, #17408, #27355 ) ;
#3557 =( BOUNDED_CURVE ( )  B_SPLINE_CURVE ( 2, ( #44109, #54085, #44430, #14210, #58912, #49269, #53145, #34453, #53456 ),
 .UNSPECIFIED., .F., .F. ) 
 B_SPLINE_CURVE_WITH_KNOTS ( ( 3, 2, 2, 2, 3 ),
 ( 0.3589285714285714302, 0.3595238095238095233, 0.3607142857142857095, 0.3619047619047618958, 0.3624999999999999889 ),
 .UNSPECIFIED. ) 
 CURVE ( )  GEOMETRIC_REPRESENTATION_ITEM ( )  RATIONAL_B_SPLINE_CURVE ( ( 0.9330127018922194093, 0.9330127018922194093, 1.000000000000000000, 0.8660254037844387076, 1.000000000000000000, 0.8660254037844387076, 1.000000000000000000, 0.9330127018922194093, 0.9330127018922194093 ) ) 
 REPRESENTATION_ITEM ( '' )  );
#3558 = CARTESIAN_POINT ( 'NONE',  ( 2.500000000000002220, -10.54166666393547835, 4.330127018922192761 ) ) ;
#3560 = VERTEX_POINT ( 'NONE', #46000 ) ;
#3559 = CARTESIAN_POINT ( 'NONE',  ( -2.229367062499996610, -46.14583333196774362, 3.861377020970582219 ) ) ;
#3561 = CARTESIAN_POINT ( 'NONE',  ( -9.184850993605147944E-16, -144.2500000000000284, 5.000000000000000000 ) ) ;
#3563 = VERTEX_POINT ( 'NONE', #50518 ) ;
#3562 = CARTESIAN_POINT ( 'NONE',  ( 4.458734124999999437, 4.937500001365595637, -5.460374474430324690E-16 ) ) ;
#3564 = LINE ( 'NONE', #42782, #39141 ) ;
#3565 = CARTESIAN_POINT ( 'NONE',  ( 2.500000000000002220, -62.66666666666666430, 4.330127018922192761 ) ) ;
#3566 = CARTESIAN_POINT ( 'NONE',  ( 2.730187237215162345E-16, -159.4375000013655779, -4.458734124999999437 ) ) ;
#3567 = CARTESIAN_POINT ( 'NONE',  ( -4.458734124999999437, -36.64583333196773651, -2.574251347313719407 ) ) ;
#3568 = CARTESIAN_POINT ( 'NONE',  ( 1.975475456537005874E-15, -14.74999999999999822, 5.000000000000000000 ) ) ;
#3569 = CARTESIAN_POINT ( 'NONE',  ( 3.061616997868383141E-16, -167.7500000000000000, -5.000000000000000000 ) ) ;
#3570 = CARTESIAN_POINT ( 'NONE',  ( 5.000000000000000888, -11.58333333333333393, 2.886751345948126879 ) ) ;
#3571 = CARTESIAN_POINT ( 'NONE',  ( -59.44456063193725015, -130.8125000013656063, -0.3552334253322034230 ) ) ;
#3572 = EDGE_CURVE ( 'NONE', #48999, #18747, #6817, .T. ) ;
#3573 = CARTESIAN_POINT ( 'NONE',  ( 4.458734124999998549, -3.979166665301070438, -2.574251347313721627 ) ) ;
#3574 = CARTESIAN_POINT ( 'NONE',  ( -4.458734124999999437, -41.56249999863440081, 0.000000000000000000 ) ) ;
#3575 = ADVANCED_FACE ( 'NONE', ( #59207 ), #26067, .T. ) ;
#3576 = EDGE_CURVE ( 'NONE', #36690, #31117, #59855, .T. ) ;
#3577 = CARTESIAN_POINT ( 'NONE',  ( 2.499999999999998668, -67.20833333060214443, -4.330127018922193649 ) ) ;
#3578 = CARTESIAN_POINT ( 'NONE',  ( 4.458734125000001214, -84.14583333196772230, 2.574251347313718519 ) ) ;
#3579 = CARTESIAN_POINT ( 'NONE',  ( 2.500000000000002220, -84.66666666666667140, 4.330127018922192761 ) ) ;
#3580 = EDGE_LOOP ( 'NONE', ( #14311, #22974, #57435, #14940 ) ) ;
#3581 = CARTESIAN_POINT ( 'NONE',  ( -51.75738570946856498, -152.8750000027312126, 3.805975901505576964 ) ) ;
#3582 = CARTESIAN_POINT ( 'NONE',  ( -2.500000000000000444, -12.04166666393547835, -4.330127018922193649 ) ) ;
#3583 = CARTESIAN_POINT ( 'NONE',  ( -4.458734124999999437, -67.64583333196773651, -2.574251347313719407 ) ) ;
#3584 = CARTESIAN_POINT ( 'NONE',  ( -8.190561711645485556E-16, -146.9375000013656063, 4.458734124999999437 ) ) ;
#3585 = VERTEX_POINT ( 'NONE', #15136 ) ;
#3586 = ADVANCED_FACE ( 'NONE', ( #34758 ), #29922, .T. ) ;
#3587 = CARTESIAN_POINT ( 'NONE',  ( -5.000000000000000888, -146.6875000027312126, -2.071067811865475949 ) ) ;
#3588 = CARTESIAN_POINT ( 'NONE',  ( -3.152548672688508926E-16, -14.81249999863440436, -5.148502694627439702 ) ) ;
#3589 = ADVANCED_FACE ( 'NONE', ( #5807 ), #25424, .T. ) ;
#3590 = CARTESIAN_POINT ( 'NONE',  ( 0.000000000000000000, -120.0000000000000000, 0.000000000000000000 ) ) ;
#3591 = CARTESIAN_POINT ( 'NONE',  ( -4.458734124999999437, 0.6041666680322611560, -2.574251347313719407 ) ) ;
#3592 = CARTESIAN_POINT ( 'NONE',  ( 5.000000000000000000, -30.37499999726881228, -6.123233995736766282E-16 ) ) ;
#3593 = CARTESIAN_POINT ( 'NONE',  ( -4.458734124999999437, -153.0000000013656063, -1.846868145590735644 ) ) ;
#3594 = CARTESIAN_POINT ( 'NONE',  ( 9.457646018065525792E-16, 24.68750000136559208, 5.148502694627439702 ) ) ;
#3595 = ORIENTED_EDGE ( 'NONE', *, *, #20124, .T. ) ;
#3596 = CARTESIAN_POINT ( 'NONE',  ( -3.152548672688508926E-16, -91.56249999863440792, -5.148502694627439702 ) ) ;
#3597 = CARTESIAN_POINT ( 'NONE',  ( 1.062108568985190270E-13, -25.25000000000000355, -4.999999999999999112 ) ) ;
#3598 = DIRECTION ( 'NONE',  ( 0.000000000000000000, 0.000000000000000000, 1.000000000000000000 ) ) ;
#3599 = CARTESIAN_POINT ( 'NONE',  ( -4.458734124999998549, -6.229166665301072214, 2.574251347313722516 ) ) ;
#3600 = CARTESIAN_POINT ( 'NONE',  ( 1.975475456537005874E-15, -51.75000000000000000, 5.000000000000000000 ) ) ;
#3601 = CARTESIAN_POINT ( 'NONE',  ( 1.339745962155612702, -87.29465819873851729, -5.000000000000000000 ) ) ;
#3602 = CARTESIAN_POINT ( 'NONE',  ( 5.000000000000000888, -36.45833333060214443, 2.886751345948126879 ) ) ;
#3603 = CARTESIAN_POINT ( 'NONE',  ( 5.000000000000000000, -64.37499999726881583, -6.123233995736766282E-16 ) ) ;
#3604 = CARTESIAN_POINT ( 'NONE',  ( -4.458734124999997661, 19.77083333469893134, 2.574251347313722516 ) ) ;
#3605 = CARTESIAN_POINT ( 'NONE',  ( -2.500000000000000444, -4.166666666666666075, -4.330127018922193649 ) ) ;
#3606 = CARTESIAN_POINT ( 'NONE',  ( 4.458734124999998549, 24.27083333469892779, -2.574251347313721627 ) ) ;
#3607 = CARTESIAN_POINT ( 'NONE',  ( 2.229367062499998831, -58.64583333196773651, -3.861377020970580887 ) ) ;
#3608 = CARTESIAN_POINT ( 'NONE',  ( 2.229367062500001939, -3.229166665301069550, 3.861377020970579999 ) ) ;
#3609 =( BOUNDED_CURVE ( )  B_SPLINE_CURVE ( 2, ( #25379, #18102, #57358, #58524, #13279, #44669, #629, #49502, #53693 ),
 .UNSPECIFIED., .F., .F. ) 
 B_SPLINE_CURVE_WITH_KNOTS ( ( 3, 2, 2, 2, 3 ),
 ( 0.8270833333333332815, 0.8277777777777777235, 0.8291666666666667185, 0.8305555555555556024, 0.8312500000000000444 ),
 .UNSPECIFIED. ) 
 CURVE ( )  GEOMETRIC_REPRESENTATION_ITEM ( )  RATIONAL_B_SPLINE_CURVE ( ( 0.9330127018922194093, 0.9330127018922194093, 1.000000000000000000, 0.8660254037844387076, 1.000000000000000000, 0.8660254037844387076, 1.000000000000000000, 0.9330127018922194093, 0.9330127018922194093 ) ) 
 REPRESENTATION_ITEM ( '' )  );
#3610 = CYLINDRICAL_SURFACE ( 'NONE', #49380, 5.000000000000000000 ) ;
#3611 = CARTESIAN_POINT ( 'NONE',  ( 2.500000000000002220, 9.333333333333332149, 4.330127018922192761 ) ) ;
#3612 = CARTESIAN_POINT ( 'NONE',  ( -3.535533905932737309, -139.7500000027311842, -3.535533905932738197 ) ) ;
#3613 = CARTESIAN_POINT ( 'NONE',  ( -6.972266317189433020E-16, -52.25000000000000711, -5.000000000000000000 ) ) ;
#3614 = CARTESIAN_POINT ( 'NONE',  ( 2.229367062500001939, -45.97916666530106511, 3.861377020970579999 ) ) ;
#3615 = CARTESIAN_POINT ( 'NONE',  ( -3.535250795749689387E-16, -86.12499999726880162, -5.773502691896257311 ) ) ;
#3616 = CARTESIAN_POINT ( 'NONE',  ( -57.19623071787017210, -137.6250000013655779, 4.297418129356382899 ) ) ;
#3617 = CARTESIAN_POINT ( 'NONE',  ( -51.75738570946856498, -155.0000000000000284, 3.805975901505577408 ) ) ;
#3618 = CARTESIAN_POINT ( 'NONE',  ( -5.000000000000000000, -104.9583333306021444, -2.886751345948128211 ) ) ;
#3619 = CARTESIAN_POINT ( 'NONE',  ( -4.458734124999997661, -88.47916666530107932, 2.574251347313722516 ) ) ;
#3620 = CARTESIAN_POINT ( 'NONE',  ( -4.458734124999999437, -159.1875000013655779, -5.460374474430324690E-16 ) ) ;
#3621 = CARTESIAN_POINT ( 'NONE',  ( 5.000000000000000000, -37.50000000000000711, -6.123233995736766282E-16 ) ) ;
#3622 = CARTESIAN_POINT ( 'NONE',  ( 1.339745962155615144, 8.419658201469706782, 4.999999999999999112 ) ) ;
#3623 = VERTEX_POINT ( 'NONE', #56622 ) ;
#3624 = CARTESIAN_POINT ( 'NONE',  ( -4.458734124999998549, 17.52083333469892779, 2.574251347313722516 ) ) ;
#3625 = ORIENTED_EDGE ( 'NONE', *, *, #53182, .F. ) ;
#3626 = CARTESIAN_POINT ( 'NONE',  ( -4.458734124999998549, -97.22916666530105090, 2.574251347313722516 ) ) ;
#3627 = CARTESIAN_POINT ( 'NONE',  ( -4.458734124999999437, 6.437500001365593860, 0.000000000000000000 ) ) ;
#3628 = CARTESIAN_POINT ( 'NONE',  ( 5.000000000000000000, 10.70833333606452165, -2.886751345948129988 ) ) ;
#3629 = LINE ( 'NONE', #22939, #55570 ) ;
#3630 = CARTESIAN_POINT ( 'NONE',  ( 2.500000000000002220, 1.333333333333332149, 4.330127018922192761 ) ) ;
#3631 = CARTESIAN_POINT ( 'NONE',  ( -3.152548672688508926E-16, -63.56249999863440792, -5.148502694627439702 ) ) ;
#3632 = DIRECTION ( 'NONE',  ( -0.000000000000000000, 1.000000000000000000, -0.000000000000000000 ) ) ;
#3633 = CARTESIAN_POINT ( 'NONE',  ( 2.229367062500001939, -28.97916666530107221, 3.861377020970579999 ) ) ;
#3634 = CARTESIAN_POINT ( 'NONE',  ( 1.975475456537005874E-15, 5.249999999999999112, 5.000000000000000000 ) ) ;
#3635 = LINE ( 'NONE', #27749, #37437 ) ;
#3636 = CARTESIAN_POINT ( 'NONE',  ( -6.972266317189433020E-16, -109.2499999999999716, -5.000000000000000000 ) ) ;
#3637 = CARTESIAN_POINT ( 'NONE',  ( 1.060575238724906964E-15, -43.75000000000000000, 5.773502691896257311 ) ) ;
#3638 = CARTESIAN_POINT ( 'NONE',  ( -6.972266317189433020E-16, -101.1249999972688158, -5.000000000000000000 ) ) ;
#3639 = SHAPE_REPRESENTATION ( 'spindle', ( #43054 ), #29681 ) ;
#3641 = CARTESIAN_POINT ( 'NONE',  ( 9.457646018065525792E-16, -17.31249999863440436, 5.148502694627439702 ) ) ;
#3640 = CARTESIAN_POINT ( 'NONE',  ( -5.000000000000000000, 24.04166666939785202, -2.886751345948128211 ) ) ;
#3642 = DIRECTION ( 'NONE',  ( -0.000000000000000000, 1.000000000000000000, -0.000000000000000000 ) ) ;
#3643 = CARTESIAN_POINT ( 'NONE',  ( -2.229367062500000163, -62.47916666530106511, -3.861377020970580443 ) ) ;
#3644 = CARTESIAN_POINT ( 'NONE',  ( -1.846868145590737420, -147.0000000013655779, 4.458734124999999437 ) ) ;
#3645 = CARTESIAN_POINT ( 'NONE',  ( 9.457646018065525792E-16, -77.06249999863440792, 5.148502694627439702 ) ) ;
#3646 = CARTESIAN_POINT ( 'NONE',  ( -55.35523342533222291, -143.5625000013656063, 4.444560631937231499 ) ) ;
#3647 = AXIS2_PLACEMENT_3D ( 'NONE', #57760, #4043, #23031 ) ;
#3648 = CARTESIAN_POINT ( 'NONE',  ( -4.458734124999999437, -24.64583333196773651, -2.574251347313719407 ) ) ;
#3649 = CARTESIAN_POINT ( 'NONE',  ( -4.999999999999999112, -63.79166666393547303, 2.886751345948131764 ) ) ;
#3651 = ORIENTED_EDGE ( 'NONE', *, *, #41308, .T. ) ;
#3650 = ADVANCED_FACE ( 'NONE', ( #11895 ), #17987, .T. ) ;
#3652 = CARTESIAN_POINT ( 'NONE',  ( -1.339745962155613812, -22.20534180126147561, -5.000000000000000000 ) ) ;
#3653 = ORIENTED_EDGE ( 'NONE', *, *, #12294, .F. ) ;
#3654 = CARTESIAN_POINT ( 'NONE',  ( -4.458734124999998549, -70.47916666530107932, 2.574251347313722516 ) ) ;
#3655 = CARTESIAN_POINT ( 'NONE',  ( -9.184850993605147944E-16, -149.3750000027312126, 5.000000000000000000 ) ) ;
#3656 = ORIENTED_EDGE ( 'NONE', *, *, #55776, .F. ) ;
#3657 = EDGE_CURVE ( 'NONE', #44744, #47006, #61104, .T. ) ;
#3658 = DIRECTION ( 'NONE',  ( 0.000000000000000000, 0.000000000000000000, 1.000000000000000000 ) ) ;
#3659 = CARTESIAN_POINT ( 'NONE',  ( 4.458734124999998549, -51.97916666530107221, -2.574251347313721627 ) ) ;
#3660 = EDGE_CURVE ( 'NONE', #11945, #53004, #27021, .T. ) ;
#3661 = CARTESIAN_POINT ( 'NONE',  ( -3.152548672688508926E-16, 3.187500001365594748, -5.148502694627439702 ) ) ;
#3662 = ORIENTED_EDGE ( 'NONE', *, *, #24049, .T. ) ;
#3663 = CARTESIAN_POINT ( 'NONE',  ( -5.000000000000000000, -54.99999999999999289, 0.000000000000000000 ) ) ;
#3664 = CARTESIAN_POINT ( 'NONE',  ( -4.458734124999999437, 1.687500001365593194, 0.000000000000000000 ) ) ;
#3665 = ADVANCED_FACE ( 'NONE', ( #60808 ), #27647, .T. ) ;
#3666 = CARTESIAN_POINT ( 'NONE',  ( -4.458734124999999437, 20.68750000136559208, 0.000000000000000000 ) ) ;
#3667 = CARTESIAN_POINT ( 'NONE',  ( -59.59170313451811296, -146.5000000013656347, 1.485763867205729394 ) ) ;
#3668 = CARTESIAN_POINT ( 'NONE',  ( -6.972266317189433020E-16, 5.875000002731184168, -5.000000000000000000 ) ) ;
#3669 = CARTESIAN_POINT ( 'NONE',  ( 4.458734124999997661, -167.5000000013655779, 1.846868145590737864 ) ) ;
#3671 = EDGE_CURVE ( 'NONE', #62900, #4805, #57254, .T. ) ;
#3670 = VERTEX_POINT ( 'NONE', #17374 ) ;
#3672 = CARTESIAN_POINT ( 'NONE',  ( 4.458734125000000326, -73.89583333196773651, 2.574251347313718519 ) ) ;
#3673 = CYLINDRICAL_SURFACE ( 'NONE', #48970, 5.000000000000000000 ) ;
#3674 = CARTESIAN_POINT ( 'NONE',  ( -2.229367062499996610, 4.854166668032261711, 3.861377020970582219 ) ) ;
#3675 = ADVANCED_FACE ( 'NONE', ( #17688 ), #16735, .T. ) ;
#3676 = CARTESIAN_POINT ( 'NONE',  ( 5.000000000000000000, -140.1875000027311842, 2.071067811865478614 ) ) ;
#3677 = CARTESIAN_POINT ( 'NONE',  ( -4.458734124999999437, -58.56249999863440081, 0.000000000000000000 ) ) ;
#3678 = CARTESIAN_POINT ( 'NONE',  ( -5.000000000000000000, -18.87499999726881583, 0.000000000000000000 ) ) ;
#3679 = CARTESIAN_POINT ( 'NONE',  ( -49.85088928181150436, -142.6875000027312126, -1.666127454062680480 ) ) ;
#3680 = CARTESIAN_POINT ( 'NONE',  ( 5.000000000000000000, -42.29166666393548724, -2.886751345948130876 ) ) ;
#3681 = CARTESIAN_POINT ( 'NONE',  ( 5.000000000000000000, -76.50000000000000000, -6.123233995736766282E-16 ) ) ;
#3682 = CARTESIAN_POINT ( 'NONE',  ( -6.972266317189433020E-16, -106.1249999972688016, -5.000000000000000000 ) ) ;
#3683 = LINE ( 'NONE', #52876, #59319 ) ;
#3684 = CARTESIAN_POINT ( 'NONE',  ( 4.458734125000001214, -41.89583333196773651, 2.574251347313718519 ) ) ;
#3685 = CARTESIAN_POINT ( 'NONE',  ( -3.152548672688508926E-16, -28.81249999863440792, -5.148502694627439702 ) ) ;
#3686 = CARTESIAN_POINT ( 'NONE',  ( -58.80597590150559739, -140.1250000027312126, 3.242614290531460330 ) ) ;
#3687 = CARTESIAN_POINT ( 'NONE',  ( -5.000000000000000000, 25.91666666666666430, -2.886751345948128211 ) ) ;
#3688 = CARTESIAN_POINT ( 'NONE',  ( -5.000000000000000888, -153.6875000027312126, -2.071067811865475949 ) ) ;
#3689 = ORIENTED_EDGE ( 'NONE', *, *, #18863, .F. ) ;
#3690 = CARTESIAN_POINT ( 'NONE',  ( 4.458734125000001214, -110.1458333319677507, 2.574251347313718519 ) ) ;
#3691 = CARTESIAN_POINT ( 'NONE',  ( 2.229367062499998831, -34.64583333196772941, -3.861377020970580887 ) ) ;
#3692 = CARTESIAN_POINT ( 'NONE',  ( -2.499999999999996447, -68.70833333060214443, 4.330127018922195425 ) ) ;
#3693 = VECTOR ( 'NONE', #27014, 1000.000000000000000 ) ;
#3694 = CARTESIAN_POINT ( 'NONE',  ( -52.10840900171896806, -147.4375000013656063, 3.393966926194110556 ) ) ;
#3695 = CARTESIAN_POINT ( 'NONE',  ( -3.535533905932737309, -148.6250000000000000, -3.535533905932738197 ) ) ;
#3696 = CARTESIAN_POINT ( 'NONE',  ( -3.152548672688508926E-16, -27.56249999863440081, -5.148502694627439702 ) ) ;
#3697 = CARTESIAN_POINT ( 'NONE',  ( -2.229367062500000163, -72.72916666530107932, -3.861377020970580443 ) ) ;
#3698 = CARTESIAN_POINT ( 'NONE',  ( -4.999999999999998224, -54.91666666666667140, 2.886751345948131764 ) ) ;
#3699 = CARTESIAN_POINT ( 'NONE',  ( 9.457646018065525792E-16, -30.06249999863440436, 5.148502694627439702 ) ) ;
#3700 = CARTESIAN_POINT ( 'NONE',  ( -57.46284108482265651, -147.9375000000000284, 4.819101127000238627 ) ) ;
#3701 = DIRECTION ( 'NONE',  ( 0.000000000000000000, 0.000000000000000000, -1.000000000000000000 ) ) ;
#3702 = CARTESIAN_POINT ( 'NONE',  ( -5.000000000000000000, -18.99999999999999645, 0.000000000000000000 ) ) ;
#3703 = CARTESIAN_POINT ( 'NONE',  ( 3.152801135295367541, -148.3125000013655779, -3.152801135295367541 ) ) ;
#3704 = ORIENTED_EDGE ( 'NONE', *, *, #49603, .T. ) ;
#3705 = LINE ( 'NONE', #27815, #46142 ) ;
#3706 = CARTESIAN_POINT ( 'NONE',  ( -2.229367062499996610, -58.39583333196773651, 3.861377020970582219 ) ) ;
#3707 = CARTESIAN_POINT ( 'NONE',  ( -2.499999999999996447, 26.29166666939785202, 4.330127018922195425 ) ) ;
#3708 = DIRECTION ( 'NONE',  ( 0.000000000000000000, 0.000000000000000000, 1.000000000000000000 ) ) ;
#3709 = CARTESIAN_POINT ( 'NONE',  ( -5.000000000000000000, 19.99999999999999645, 0.000000000000000000 ) ) ;
#3710 = FACE_OUTER_BOUND ( 'NONE', #8135, .T. ) ;
#3711 = CARTESIAN_POINT ( 'NONE',  ( -2.229367062500000163, -1.479166665301071770, -3.861377020970580443 ) ) ;
#3712 = CARTESIAN_POINT ( 'NONE',  ( 5.000000000000000000, -48.50000000000000000, -6.123233995736766282E-16 ) ) ;
#3713 = CARTESIAN_POINT ( 'NONE',  ( 1.975475456537005874E-15, -80.62499999726881583, 5.000000000000000000 ) ) ;
#3714 = CARTESIAN_POINT ( 'NONE',  ( -4.458734124999999437, 9.354166668032261711, -2.574251347313719407 ) ) ;
#3715 = CARTESIAN_POINT ( 'NONE',  ( -6.972266317189433020E-16, -12.24999999999999645, -5.000000000000000000 ) ) ;
#3716 = ORIENTED_EDGE ( 'NONE', *, *, #34943, .F. ) ;
#3717 = CARTESIAN_POINT ( 'NONE',  ( 4.458734124999999437, -169.4375000013656063, 0.000000000000000000 ) ) ;
#3718 = CARTESIAN_POINT ( 'NONE',  ( 2.229367062500001939, -47.97916666530106511, 3.861377020970579999 ) ) ;
#3719 = CARTESIAN_POINT ( 'NONE',  ( -1.846868145590737420, -162.0000000013655779, 4.458734124999999437 ) ) ;
#3720 = CARTESIAN_POINT ( 'NONE',  ( -5.000000000000000000, -48.87499999726880873, 0.000000000000000000 ) ) ;
#3721 = EDGE_LOOP ( 'NONE', ( #43039, #8029, #29160, #50605 ) ) ;
#3722 = CARTESIAN_POINT ( 'NONE',  ( 9.457646018065525792E-16, -24.06249999863440436, 5.148502694627439702 ) ) ;
#3723 = ORIENTED_EDGE ( 'NONE', *, *, #46043, .F. ) ;
#3725 = CARTESIAN_POINT ( 'NONE',  ( -1.339745962155610925, -102.6696581960073331, 5.000000000000000000 ) ) ;
#3724 = CARTESIAN_POINT ( 'NONE',  ( 0.000000000000000000, 15.00000000000000000, 0.000000000000000000 ) ) ;
#3726 = CARTESIAN_POINT ( 'NONE',  ( -4.458734125000001214, -160.8750000013655779, 1.846868145590734089 ) ) ;
#3727 = AXIS2_PLACEMENT_3D ( 'NONE', #32943, #41395, #36578 ) ;
#3728 = CARTESIAN_POINT ( 'NONE',  ( -6.972266317189433020E-16, -46.12499999726880873, -5.000000000000000000 ) ) ;
#3729 = CARTESIAN_POINT ( 'NONE',  ( -49.85088928181150436, -134.5625000000000568, -1.666127454062680702 ) ) ;
#3730 = CARTESIAN_POINT ( 'NONE',  ( 4.458734124999998549, -38.97916666530107221, -2.574251347313721627 ) ) ;
#3731 = ORIENTED_EDGE ( 'NONE', *, *, #30650, .F. ) ;
#3732 = VECTOR ( 'NONE', #38002, 1000.000000000000000 ) ;
#3733 =( BOUNDED_CURVE ( )  B_SPLINE_CURVE ( 2, ( #10042, #45096, #29974, #49601, #16147, #26118, #5543, #1061, #20667 ),
 .UNSPECIFIED., .F., .F. ) 
 B_SPLINE_CURVE_WITH_KNOTS ( ( 3, 2, 2, 2, 3 ),
 ( 0.8729166666666666741, 0.8736111111111111160, 0.8750000000000000000, 0.8763888888888888840, 0.8770833333333333259 ),
 .UNSPECIFIED. ) 
 CURVE ( )  GEOMETRIC_REPRESENTATION_ITEM ( )  RATIONAL_B_SPLINE_CURVE ( ( 0.9330127018922194093, 0.9330127018922194093, 1.000000000000000000, 0.8660254037844387076, 1.000000000000000000, 0.8660254037844387076, 1.000000000000000000, 0.9330127018922194093, 0.9330127018922194093 ) ) 
 REPRESENTATION_ITEM ( '' )  );
#3734 = CARTESIAN_POINT ( 'NONE',  ( -2.229367062499996610, -84.14583333196773651, 3.861377020970582219 ) ) ;
#3735 = CARTESIAN_POINT ( 'NONE',  ( 2.229367062499998831, 20.35416666803225993, -3.861377020970580887 ) ) ;
#3736 = CARTESIAN_POINT ( 'NONE',  ( 5.000000000000000000, -12.37499999726881050, -6.123233995736766282E-16 ) ) ;
#3737 = ORIENTED_EDGE ( 'NONE', *, *, #54173, .F. ) ;
#3738 = CARTESIAN_POINT ( 'NONE',  ( -52.80376928212989185, -138.1250000013656063, -4.297418129356378458 ) ) ;
#3739 = CARTESIAN_POINT ( 'NONE',  ( -4.458734124999998549, -84.47916666530107932, 2.574251347313722516 ) ) ;
#3740 = CARTESIAN_POINT ( 'NONE',  ( -55.39835681537999790, -128.0000000027312126, 4.984105922594378235 ) ) ;
#3741 = CARTESIAN_POINT ( 'NONE',  ( -6.972266317189433020E-16, -35.12499999726880873, -5.000000000000000000 ) ) ;
#3742 = CARTESIAN_POINT ( 'NONE',  ( -2.071067811865580754, -158.8125000027312126, -4.999999999999894307 ) ) ;
#3743 = CARTESIAN_POINT ( 'NONE',  ( 2.500000000000002220, -57.66666666666667140, 4.330127018922192761 ) ) ;
#3744 = CARTESIAN_POINT ( 'NONE',  ( 9.457646018065525792E-16, -61.06249999863440081, 5.148502694627439702 ) ) ;
#3745 = CARTESIAN_POINT ( 'NONE',  ( 5.000000000000000888, -37.58333333333332860, 2.886751345948126879 ) ) ;
#3746 = CARTESIAN_POINT ( 'NONE',  ( 4.458734125000001214, 24.10416666803226349, 2.574251347313718519 ) ) ;
#3747 = CARTESIAN_POINT ( 'NONE',  ( 2.493747252781420335E-13, -42.25000000000000711, -5.000000000000000000 ) ) ;
#3748 = DIRECTION ( 'NONE',  ( 0.000000000000000000, 1.000000000000000000, 0.000000000000000000 ) ) ;
#3749 = CARTESIAN_POINT ( 'NONE',  ( -2.229367062500000163, -44.72916666530106511, -3.861377020970580443 ) ) ;
#3750 = CARTESIAN_POINT ( 'NONE',  ( 5.000000000000000000, -3.291666663935477910, -2.886751345948129988 ) ) ;
#3751 = DIRECTION ( 'NONE',  ( -0.000000000000000000, 1.000000000000000000, -0.000000000000000000 ) ) ;
#3752 = CARTESIAN_POINT ( 'NONE',  ( -51.60603307380591787, -125.9375000013656063, -2.891590998281053704 ) ) ;
#3753 = CARTESIAN_POINT ( 'NONE',  ( 9.457646018065525792E-16, -87.31249999863440792, 5.148502694627439702 ) ) ;
#3754 = CARTESIAN_POINT ( 'NONE',  ( 4.458734125000000326, -104.8958333319677365, 2.574251347313718519 ) ) ;
#3755 = CARTESIAN_POINT ( 'NONE',  ( -2.229367062499996610, -12.39583333196774007, 3.861377020970582219 ) ) ;
#3756 = VERTEX_POINT ( 'NONE', #41479 ) ;
#3757 = LINE ( 'NONE', #9200, #47426 ) ;
#3758 = CARTESIAN_POINT ( 'NONE',  ( 4.458734124999999437, -90.81249999863440792, -5.460374474430324690E-16 ) ) ;
#3759 = CARTESIAN_POINT ( 'NONE',  ( 3.061616997868383141E-16, -165.8750000027312126, -5.000000000000000000 ) ) ;
#3760 = CARTESIAN_POINT ( 'NONE',  ( -2.229367062500000163, -89.72916666530106511, -3.861377020970580443 ) ) ;
#3761 = CARTESIAN_POINT ( 'NONE',  ( 2.499999999999998668, -53.20833333060213732, -4.330127018922193649 ) ) ;
#3762 = CARTESIAN_POINT ( 'NONE',  ( -6.972266317189433020E-16, -23.24999999999999645, -5.000000000000000000 ) ) ;
#3763 = CARTESIAN_POINT ( 'NONE',  ( -55.35523342533222291, -128.3125000013656063, 4.444560631937231499 ) ) ;
#3764 = CARTESIAN_POINT ( 'NONE',  ( -2.229367062500000163, -11.47916666530107044, -3.861377020970580443 ) ) ;
#3765 = CARTESIAN_POINT ( 'NONE',  ( 4.458734124999999437, 10.93750000136559386, -5.460374474430324690E-16 ) ) ;
#3766 = CARTESIAN_POINT ( 'NONE',  ( 9.457646018065525792E-16, -56.31249999863440081, 5.148502694627439702 ) ) ;
#3767 = CARTESIAN_POINT ( 'NONE',  ( -6.972266317189433020E-16, -46.24999999999999289, -5.000000000000000000 ) ) ;
#3768 = CARTESIAN_POINT ( 'NONE',  ( 3.061616997868383141E-16, -152.7500000000000000, -5.000000000000000000 ) ) ;
#3769 = CARTESIAN_POINT ( 'NONE',  ( 2.229367062499998831, -12.64583333196774007, -3.861377020970580887 ) ) ;
#3770 = CARTESIAN_POINT ( 'NONE',  ( 1.975475456537005874E-15, -63.74999999999998579, 5.000000000000000000 ) ) ;
#3771 = EDGE_LOOP ( 'NONE', ( #48876, #9479, #16547, #41357 ) ) ;
#3772 = CARTESIAN_POINT ( 'NONE',  ( 4.458734124999998549, -39.97916666530107221, -2.574251347313721627 ) ) ;
#3773 = VECTOR ( 'NONE', #60, 1000.000000000000000 ) ;
#3774 = CARTESIAN_POINT ( 'NONE',  ( 5.000000000000000888, -77.58333333333334281, 2.886751345948126879 ) ) ;
#3775 = CARTESIAN_POINT ( 'NONE',  ( -2.500000000000000444, 26.95833333606451632, -4.330127018922193649 ) ) ;
#3776 = CARTESIAN_POINT ( 'NONE',  ( -4.458734124999999437, -84.39583333196773651, -2.574251347313719407 ) ) ;
#3777 = CARTESIAN_POINT ( 'NONE',  ( -3.152548672688508926E-16, 23.18750000136559208, -5.148502694627439702 ) ) ;
#3778 = AXIS2_PLACEMENT_3D ( 'NONE', #53921, #5360, #48770 ) ;
#3779 = AXIS2_PLACEMENT_3D ( 'NONE', #35008, #30158, #5733 ) ;
#3780 = CARTESIAN_POINT ( 'NONE',  ( 4.458734124999998549, 15.27083333469893134, -2.574251347313721627 ) ) ;
#3781 = CARTESIAN_POINT ( 'NONE',  ( 6.123233995736766282E-16, -120.0000000000000000, -5.000000000000000000 ) ) ;
#3782 = DIRECTION ( 'NONE',  ( 0.000000000000000000, 0.000000000000000000, 1.000000000000000000 ) ) ;
#3783 = CARTESIAN_POINT ( 'NONE',  ( 9.457646018065525792E-16, -88.31249999863439371, 5.148502694627439702 ) ) ;
#3784 = CARTESIAN_POINT ( 'NONE',  ( 5.000000000000000888, -70.58333333333332860, 2.886751345948126879 ) ) ;
#3785 =( BOUNDED_CURVE ( )  B_SPLINE_CURVE ( 2, ( #4565, #34149, #24511, #19040, #23253, #43796, #38972, #38044, #28383 ),
 .UNSPECIFIED., .F., .F. ) 
 B_SPLINE_CURVE_WITH_KNOTS ( ( 3, 2, 2, 2, 3 ),
 ( 0.2770833333333333481, 0.2777777777777777901, 0.2791666666666666741, 0.2805555555555555580, 0.2812500000000000000 ),
 .UNSPECIFIED. ) 
 CURVE ( )  GEOMETRIC_REPRESENTATION_ITEM ( )  RATIONAL_B_SPLINE_CURVE ( ( 0.9330127018922194093, 0.9330127018922194093, 1.000000000000000000, 0.8660254037844387076, 1.000000000000000000, 0.8660254037844387076, 1.000000000000000000, 0.9330127018922194093, 0.9330127018922194093 ) ) 
 REPRESENTATION_ITEM ( '' )  );
#3786 = CARTESIAN_POINT ( 'NONE',  ( -4.999999999999999112, 12.20833333606451632, 2.886751345948131764 ) ) ;
#3787 = ORIENTED_EDGE ( 'NONE', *, *, #58331, .F. ) ;
#3788 = CARTESIAN_POINT ( 'NONE',  ( 5.000000000000000000, -18.37499999726881583, -6.123233995736766282E-16 ) ) ;
#3789 =( BOUNDED_CURVE ( )  B_SPLINE_CURVE ( 2, ( #49664, #35512, #6562, #55133, #25220, #50944, #34876, #26499, #46114 ),
 .UNSPECIFIED., .F., .F. ) 
 B_SPLINE_CURVE_WITH_KNOTS ( ( 3, 2, 2, 2, 3 ),
 ( 0.08035714285714286309, 0.08095238095238095621, 0.08214285714285714246, 0.08333333333333332871, 0.08392857142857143571 ),
 .UNSPECIFIED. ) 
 CURVE ( )  GEOMETRIC_REPRESENTATION_ITEM ( )  RATIONAL_B_SPLINE_CURVE ( ( 0.9330127018922192983, 0.9330127018922200755, 1.000000000000000000, 0.8660254037844387076, 1.000000000000000000, 0.8660254037844387076, 1.000000000000000000, 0.9330127018922185211, 0.9330127018922192983 ) ) 
 REPRESENTATION_ITEM ( '' )  );
#3790 = CARTESIAN_POINT ( 'NONE',  ( -5.000000000000000000, 15.91666666666666430, -2.886751345948128211 ) ) ;
#3792 = CARTESIAN_POINT ( 'NONE',  ( -3.535250795749689387E-16, -29.25000000000000000, -5.773502691896257311 ) ) ;
#3791 = CARTESIAN_POINT ( 'NONE',  ( 1.975475456537005874E-15, 16.24999999999999645, 5.000000000000000000 ) ) ;
#3793 = CARTESIAN_POINT ( 'NONE',  ( 4.458734125000001214, -32.89583333196774362, 2.574251347313718519 ) ) ;
#3794 = FACE_OUTER_BOUND ( 'NONE', #3890, .T. ) ;
#3795 = CARTESIAN_POINT ( 'NONE',  ( -2.499999999999996447, -31.70833333060214798, 4.330127018922195425 ) ) ;
#3797 = ORIENTED_EDGE ( 'NONE', *, *, #28405, .T. ) ;
#3796 = CARTESIAN_POINT ( 'NONE',  ( -4.458734124999999437, -62.39583333196774362, -2.574251347313719407 ) ) ;
#3798 = CARTESIAN_POINT ( 'NONE',  ( -57.19623071787017210, -150.6250000013656063, 4.297418129356382899 ) ) ;
#3800 = VERTEX_POINT ( 'NONE', #61130 ) ;
#3799 = CARTESIAN_POINT ( 'NONE',  ( -4.458734124999998549, -8.479166665301073991, 2.574251347313722516 ) ) ;
#3801 = CARTESIAN_POINT ( 'NONE',  ( -2.500000000000000444, -77.16666666666665719, -4.330127018922193649 ) ) ;
#3802 = CARTESIAN_POINT ( 'NONE',  ( 9.457646018065525792E-16, -57.31249999863440081, 5.148502694627439702 ) ) ;
#3803 = CARTESIAN_POINT ( 'NONE',  ( -3.535250795749689387E-16, -76.12499999726881583, -5.773502691896257311 ) ) ;
#3805 = VERTEX_POINT ( 'NONE', #8356 ) ;
#3804 = CARTESIAN_POINT ( 'NONE',  ( 2.500000000000002220, -13.66666666666666785, 4.330127018922192761 ) ) ;
#3806 = CARTESIAN_POINT ( 'NONE',  ( -52.53715891517739323, -150.4375000000000000, -4.819101127000233298 ) ) ;
#3807 = CARTESIAN_POINT ( 'NONE',  ( -2.229367062500000163, -19.72916666530107221, -3.861377020970580443 ) ) ;
#3809 = VERTEX_POINT ( 'NONE', #46639 ) ;
#3808 = CARTESIAN_POINT ( 'NONE',  ( -4.458734124999998549, -55.47916666530107221, 2.574251347313722516 ) ) ;
#3810 = CARTESIAN_POINT ( 'NONE',  ( -55.00000000000002132, 14.99999999999998934, 1.734723475976807094E-15 ) ) ;
#3811 = CARTESIAN_POINT ( 'NONE',  ( -4.458734125000001214, -168.1250000013656063, 1.846868145590734089 ) ) ;
#3812 = CARTESIAN_POINT ( 'NONE',  ( 2.229367062500001939, -102.2291666653010651, 3.861377020970579999 ) ) ;
#3813 = CARTESIAN_POINT ( 'NONE',  ( -6.972266317189433020E-16, -50.12499999726881583, -5.000000000000000000 ) ) ;
#3814 =( BOUNDED_CURVE ( )  B_SPLINE_CURVE ( 2, ( #34936, #29771, #43310, #63576, #15314, #5349, #54228, #62945, #24011 ),
 .UNSPECIFIED., .F., .F. ) 
 B_SPLINE_CURVE_WITH_KNOTS ( ( 3, 2, 2, 2, 3 ),
 ( 0.6875000000000000000, 0.6880952380952380931, 0.6892857142857142794, 0.6904761904761904656, 0.6910714285714285587 ),
 .UNSPECIFIED. ) 
 CURVE ( )  GEOMETRIC_REPRESENTATION_ITEM ( )  RATIONAL_B_SPLINE_CURVE ( ( 0.9330127018922194093, 0.9330127018922194093, 1.000000000000000000, 0.8660254037844387076, 1.000000000000000000, 0.8660254037844387076, 1.000000000000000000, 0.9330127018922194093, 0.9330127018922194093 ) ) 
 REPRESENTATION_ITEM ( '' )  );
#3815 = EDGE_LOOP ( 'NONE', ( #61954, #23823, #32039, #46530 ) ) ;
#3816 = CARTESIAN_POINT ( 'NONE',  ( -56.48576386720575471, -149.0000000013656063, -4.591703134518078322 ) ) ;
#3817 = CARTESIAN_POINT ( 'NONE',  ( -57.46284108482265651, -137.0625000027312126, 4.819101127000239515 ) ) ;
#3818 = VECTOR ( 'NONE', #8253, 1000.000000000000000 ) ;
#3819 = DIRECTION ( 'NONE',  ( -0.8660254037844382635, -0.5000000000000004441, 0.000000000000000000 ) ) ;
#3820 = VECTOR ( 'NONE', #27949, 1000.000000000000000 ) ;
#3821 = CARTESIAN_POINT ( 'NONE',  ( -4.458734124999999437, -6.395833331967740953, -2.574251347313719407 ) ) ;
#3822 = CARTESIAN_POINT ( 'NONE',  ( -3.152548672688508926E-16, -102.8124999986344079, -5.148502694627439702 ) ) ;
#3823 = CARTESIAN_POINT ( 'NONE',  ( -3.152801135295367096, -145.3125000013655779, -3.152801135295367541 ) ) ;
#3824 = CARTESIAN_POINT ( 'NONE',  ( 4.458734125000001214, -29.14583333196774362, 2.574251347313718519 ) ) ;
#3825 = LINE ( 'NONE', #57857, #26262 ) ;
#3826 = CARTESIAN_POINT ( 'NONE',  ( -57.19623071787017210, -138.3750000013656063, 4.297418129356382899 ) ) ;
#3827 = CARTESIAN_POINT ( 'NONE',  ( 4.458734124999999437, -71.06249999863439371, -5.460374474430324690E-16 ) ) ;
#3828 = CARTESIAN_POINT ( 'NONE',  ( -2.499999999999996447, -90.83333333333332860, 4.330127018922195425 ) ) ;
#3829 = FACE_OUTER_BOUND ( 'NONE', #54106, .T. ) ;
#3830 = CARTESIAN_POINT ( 'NONE',  ( 3.152801135295366208, -140.5625000013655779, 3.152801135295367985 ) ) ;
#3831 =( BOUNDED_CURVE ( )  B_SPLINE_CURVE ( 2, ( #6948, #60984, #12074, #46811, #26559, #52277, #8214, #27817, #46178 ),
 .UNSPECIFIED., .F., .F. ) 
 B_SPLINE_CURVE_WITH_KNOTS ( ( 3, 2, 2, 2, 3 ),
 ( 0.2267857142857142849, 0.2273809523809523780, 0.2285714285714285643, 0.2297619047619047505, 0.2303571428571428714 ),
 .UNSPECIFIED. ) 
 CURVE ( )  GEOMETRIC_REPRESENTATION_ITEM ( )  RATIONAL_B_SPLINE_CURVE ( ( 0.9330127018922194093, 0.9330127018922194093, 1.000000000000000000, 0.8660254037844387076, 1.000000000000000000, 0.8660254037844387076, 1.000000000000000000, 0.9330127018922178550, 0.9330127018922194093 ) ) 
 REPRESENTATION_ITEM ( '' )  );
#3832 = CARTESIAN_POINT ( 'NONE',  ( 4.458734125000000326, 5.854166668032262599, 2.574251347313718519 ) ) ;
#3833 = EDGE_LOOP ( 'NONE', ( #26978, #17584, #61966, #11244 ) ) ;
#3834 = CARTESIAN_POINT ( 'NONE',  ( 1.975475456537005874E-15, -7.624999997268812280, 5.000000000000000000 ) ) ;
#3835 = FACE_OUTER_BOUND ( 'NONE', #45418, .T. ) ;
#3837 = CARTESIAN_POINT ( 'NONE',  ( 9.457646018065525792E-16, -26.06249999863440792, 5.148502694627439702 ) ) ;
#3836 = CARTESIAN_POINT ( 'NONE',  ( -5.000000000000000000, -91.00000000000000000, 0.000000000000000000 ) ) ;
#3838 = CARTESIAN_POINT ( 'NONE',  ( -5.000000000000000000, -76.95833333060214443, -2.886751345948128211 ) ) ;
#3839 = CARTESIAN_POINT ( 'NONE',  ( -4.458734124999999437, -75.64583333196775072, -2.574251347313719407 ) ) ;
#3840 = CARTESIAN_POINT ( 'NONE',  ( 4.458734124999999437, 21.93750000136559208, -5.460374474430324690E-16 ) ) ;
#3841 = CARTESIAN_POINT ( 'NONE',  ( 1.975475456537005874E-15, -79.62499999726881583, 5.000000000000000000 ) ) ;
#3842 = CARTESIAN_POINT ( 'NONE',  ( -57.19623071787017210, -140.3750000013656063, 4.297418129356382899 ) ) ;
#3843 = CARTESIAN_POINT ( 'NONE',  ( -2.229367062500000163, 5.520833334698927786, -3.861377020970580443 ) ) ;
#3844 = CARTESIAN_POINT ( 'NONE',  ( 9.457646018065525792E-16, 27.68750000136559208, 5.148502694627439702 ) ) ;
#3845 = CARTESIAN_POINT ( 'NONE',  ( 2.229367062499998831, -39.89583333196773651, -3.861377020970580887 ) ) ;
#3846 = CARTESIAN_POINT ( 'NONE',  ( -2.229367062500000163, 4.520833334698926897, -3.861377020970580443 ) ) ;
#3847 = CARTESIAN_POINT ( 'NONE',  ( -4.458734124999999437, -26.56249999863440792, 0.000000000000000000 ) ) ;
#3848 = CARTESIAN_POINT ( 'NONE',  ( -8.190561711645485556E-16, -155.6875000013655779, 4.458734124999999437 ) ) ;
#3849 = CARTESIAN_POINT ( 'NONE',  ( 9.457646018065525792E-16, -63.06249999863440081, 5.148502694627439702 ) ) ;
#3850 = CARTESIAN_POINT ( 'NONE',  ( 1.060575238724906964E-15, -99.62499999726880162, 5.773502691896257311 ) ) ;
#3851 = EDGE_CURVE ( 'NONE', #63425, #7768, #63152, .T. ) ;
#3852 = CARTESIAN_POINT ( 'NONE',  ( 1.339745962155615144, -41.70534180126147561, 4.999999999999999112 ) ) ;
#3853 = CARTESIAN_POINT ( 'NONE',  ( -1.339745962155613812, -64.20534180126146850, -5.000000000000000000 ) ) ;
#3854 = CARTESIAN_POINT ( 'NONE',  ( 4.458734124999999437, -105.0624999986344079, -5.460374474430324690E-16 ) ) ;
#3855 = CARTESIAN_POINT ( 'NONE',  ( 2.229367062499998831, -67.89583333196773651, -3.861377020970580887 ) ) ;
#3856 = CARTESIAN_POINT ( 'NONE',  ( 5.000000000000000000, -52.41666666666666430, -2.886751345948129988 ) ) ;
#3857 = CARTESIAN_POINT ( 'NONE',  ( -6.972266317189433020E-16, -75.25000000000000000, -5.000000000000000000 ) ) ;
#3858 = CARTESIAN_POINT ( 'NONE',  ( 5.000000000000000000, 27.62500000273118417, -6.123233995736766282E-16 ) ) ;
#3859 = VERTEX_POINT ( 'NONE', #36670 ) ;
#3860 = LINE ( 'NONE', #27040, #55105 ) ;
#3861 = AXIS2_PLACEMENT_3D ( 'NONE', #23044, #42647, #37831 ) ;
#3862 = CARTESIAN_POINT ( 'NONE',  ( -5.000000000000000000, -13.99999999999999822, 0.000000000000000000 ) ) ;
#3863 = CARTESIAN_POINT ( 'NONE',  ( -4.458734124999998549, -19.22916666530106866, 2.574251347313722516 ) ) ;
#3864 = CARTESIAN_POINT ( 'NONE',  ( 2.229367062499998831, -79.64583333196773651, -3.861377020970580887 ) ) ;
#3865 = VECTOR ( 'NONE', #61236, 1000.000000000000000 ) ;
#3866 = CARTESIAN_POINT ( 'NONE',  ( -5.000000000000000000, -30.87499999726881228, 0.000000000000000000 ) ) ;
#3867 = EDGE_CURVE ( 'NONE', #42419, #44127, #7727, .T. ) ;
#3868 = CARTESIAN_POINT ( 'NONE',  ( 5.000000000000000000, -15.37499999726881228, -6.123233995736766282E-16 ) ) ;
#3870 = ORIENTED_EDGE ( 'NONE', *, *, #62642, .T. ) ;
#3869 = CARTESIAN_POINT ( 'NONE',  ( -2.229367062500000163, -44.47916666530106511, -3.861377020970580443 ) ) ;
#3871 = DIRECTION ( 'NONE',  ( 0.000000000000000000, 0.000000000000000000, 1.000000000000000000 ) ) ;
#3872 = EDGE_CURVE ( 'NONE', #35072, #29621, #51785, .T. ) ;
#3874 = EDGE_LOOP ( 'NONE', ( #21814, #9313, #31557, #7235 ) ) ;
#3873 = CARTESIAN_POINT ( 'NONE',  ( -3.152548672688508926E-16, 6.187500001365593860, -5.148502694627439702 ) ) ;
#3875 = CARTESIAN_POINT ( 'NONE',  ( -55.35523342533222291, -153.3125000013656063, 4.444560631937231499 ) ) ;
#3876 = CARTESIAN_POINT ( 'NONE',  ( 2.499999999999998668, -60.33333333333333570, -4.330127018922193649 ) ) ;
#3877 = CARTESIAN_POINT ( 'NONE',  ( -4.458734125000000326, -157.2500000013656063, -1.846868145590735644 ) ) ;
#3878 = CARTESIAN_POINT ( 'NONE',  ( -4.458734124999998549, -33.47916666530107221, 2.574251347313722516 ) ) ;
#3879 = FACE_OUTER_BOUND ( 'NONE', #42621, .T. ) ;
#3880 = CARTESIAN_POINT ( 'NONE',  ( -2.071067811865475061, -165.6875000000000284, -5.000000000000000888 ) ) ;
#3881 = DIRECTION ( 'NONE',  ( -0.000000000000000000, 1.000000000000000000, -0.000000000000000000 ) ) ;
#3882 = CARTESIAN_POINT ( 'NONE',  ( -52.80376928212989185, -132.1250000013656347, -4.297418129356379346 ) ) ;
#3883 = CARTESIAN_POINT ( 'NONE',  ( 2.229367062500001939, -8.229166665301073991, 3.861377020970579999 ) ) ;
#3884 = EDGE_CURVE ( 'NONE', #23270, #21555, #26706, .T. ) ;
#3885 = CARTESIAN_POINT ( 'NONE',  ( -4.458734124999999437, -38.64583333196772941, -2.574251347313719407 ) ) ;
#3886 = CARTESIAN_POINT ( 'NONE',  ( -1.339745962155610925, -24.66965819600733667, 5.000000000000000000 ) ) ;
#3887 = CARTESIAN_POINT ( 'NONE',  ( 3.152801135295367541, -150.3125000013655779, -3.152801135295367541 ) ) ;
#3888 = CARTESIAN_POINT ( 'NONE',  ( -4.458734124999999437, -84.56249999863439371, 0.000000000000000000 ) ) ;
#3889 = CARTESIAN_POINT ( 'NONE',  ( 2.071067811865455077, -166.9375000027312126, -5.000000000000022204 ) ) ;
#3890 = EDGE_LOOP ( 'NONE', ( #53784, #7300, #13847, #48952 ) ) ;
#3891 = CARTESIAN_POINT ( 'NONE',  ( -3.535533905932738641, -148.5000000027311842, 3.535533905932737309 ) ) ;
#3892 = CARTESIAN_POINT ( 'NONE',  ( -7.914984360234579519, 3.818534719232089980, -7.907701344400639876 ) ) ;
#3893 = CARTESIAN_POINT ( 'NONE',  ( 9.457646018065525792E-16, -70.31249999863439371, 5.148502694627439702 ) ) ;
#3894 = CARTESIAN_POINT ( 'NONE',  ( 3.152801135295366208, -144.8125000013655779, 3.152801135295367985 ) ) ;
#3895 = ORIENTED_EDGE ( 'NONE', *, *, #27956, .F. ) ;
#3896 = LINE ( 'NONE', #58858, #7240 ) ;
#3897 = ADVANCED_FACE ( 'NONE', ( #56299 ), #22203, .T. ) ;
#3898 = CARTESIAN_POINT ( 'NONE',  ( 4.458734125000001214, -12.14583333196774007, 2.574251347313718519 ) ) ;
#3899 = CARTESIAN_POINT ( 'NONE',  ( -58.24261429053147765, -150.3750000027312126, -3.805975901505573855 ) ) ;
#3900 = CARTESIAN_POINT ( 'NONE',  ( -2.229367062499996610, 4.854166668032261711, 3.861377020970582219 ) ) ;
#3901 = CARTESIAN_POINT ( 'NONE',  ( -6.972266317189433020E-16, -77.12499999726881583, -5.000000000000000000 ) ) ;
#3902 = CARTESIAN_POINT ( 'NONE',  ( -1.846868145590734756, -153.1250000013656063, -4.458734124999999437 ) ) ;
#3903 = CARTESIAN_POINT ( 'NONE',  ( 4.458734124999998549, 24.02083333469892423, -2.574251347313721627 ) ) ;
#3904 = EDGE_LOOP ( 'NONE', ( #33694, #33349, #12495, #21799 ) ) ;
#3905 = CARTESIAN_POINT ( 'NONE',  ( 2.229367062499998831, -92.64583333196773651, -3.861377020970580887 ) ) ;
#3906 = CARTESIAN_POINT ( 'NONE',  ( -6.972266317189433020E-16, -75.25000000000000000, -5.000000000000000000 ) ) ;
#3907 = CARTESIAN_POINT ( 'NONE',  ( 3.288228914120474133, -7.217643567644815406, -7.591235721156641247 ) ) ;
#3908 = CARTESIAN_POINT ( 'NONE',  ( -4.458734124999998549, -7.229166665301073103, 2.574251347313722516 ) ) ;
#3909 = AXIS2_PLACEMENT_3D ( 'NONE', #38429, #62589, #42632 ) ;
#3910 = DIRECTION ( 'NONE',  ( 0.000000000000000000, 0.000000000000000000, 1.000000000000000000 ) ) ;
#3911 = DIRECTION ( 'NONE',  ( 0.000000000000000000, 0.000000000000000000, 1.000000000000000000 ) ) ;
#3912 =( BOUNDED_CURVE ( )  B_SPLINE_CURVE ( 2, ( #6243, #25853, #21987, #45469, #17155, #21351, #56411, #1434, #60603 ),
 .UNSPECIFIED., .F., .F. ) 
 B_SPLINE_CURVE_WITH_KNOTS ( ( 3, 2, 2, 2, 3 ),
 ( 0.7812500000000000000, 0.7819444444444444420, 0.7833333333333333259, 0.7847222222222222099, 0.7854166666666666519 ),
 .UNSPECIFIED. ) 
 CURVE ( )  GEOMETRIC_REPRESENTATION_ITEM ( )  RATIONAL_B_SPLINE_CURVE ( ( 0.9330127018922194093, 0.9330127018922194093, 1.000000000000000000, 0.8660254037844387076, 1.000000000000000000, 0.8660254037844387076, 1.000000000000000000, 0.9330127018922194093, 0.9330127018922194093 ) ) 
 REPRESENTATION_ITEM ( '' )  );
#3913 = CARTESIAN_POINT ( 'NONE',  ( -55.35523342533222291, -152.3125000013656063, 4.444560631937231499 ) ) ;
#3914 = CARTESIAN_POINT ( 'NONE',  ( 1.060575238724906964E-15, -35.62499999726881583, 5.773502691896257311 ) ) ;
#3915 = CARTESIAN_POINT ( 'NONE',  ( 1.339745962155612702, -29.29465819873852084, -5.000000000000000000 ) ) ;
#3916 = CARTESIAN_POINT ( 'NONE',  ( -3.152548672688508926E-16, 17.43750000136559564, -5.148502694627439702 ) ) ;
#3917 = CARTESIAN_POINT ( 'NONE',  ( -2.499999999999996447, -71.83333333333332860, 4.330127018922195425 ) ) ;
#3918 = CARTESIAN_POINT ( 'NONE',  ( -2.229367062500000163, 25.52083333469892779, -3.861377020970580443 ) ) ;
#3919 = CARTESIAN_POINT ( 'NONE',  ( 4.458734124999999437, -55.81249999863440081, -5.460374474430324690E-16 ) ) ;
#3920 = CARTESIAN_POINT ( 'NONE',  ( 4.458734124999999437, -5.062499998634402587, -5.460374474430324690E-16 ) ) ;
#3921 = CARTESIAN_POINT ( 'NONE',  ( -1.339745962155613812, -34.08034179853029144, -5.000000000000000000 ) ) ;
#3922 = CARTESIAN_POINT ( 'NONE',  ( 2.499999999999998668, 8.666666666666666075, -4.330127018922193649 ) ) ;
#3923 = CARTESIAN_POINT ( 'NONE',  ( 1.846868145590736310, -168.6250000013655779, 4.458734124999999437 ) ) ;
#3924 = CARTESIAN_POINT ( 'NONE',  ( -1.339745962155613812, -46.20534180126146850, -5.000000000000000000 ) ) ;
#3925 = CARTESIAN_POINT ( 'NONE',  ( -3.152548672688508926E-16, -46.56249999863440792, -5.148502694627439702 ) ) ;
#3926 = CARTESIAN_POINT ( 'NONE',  ( -5.000000000000000000, -81.95833333060213022, -2.886751345948128211 ) ) ;
#3927 = EDGE_CURVE ( 'NONE', #5440, #34951, #42747, .T. ) ;
#3928 = CARTESIAN_POINT ( 'NONE',  ( -55.35523342533222291, -136.5625000013656063, 4.444560631937231499 ) ) ;
#3929 = FACE_OUTER_BOUND ( 'NONE', #47982, .T. ) ;
#3930 =( BOUNDED_CURVE ( )  B_SPLINE_CURVE ( 2, ( #62335, #13119, #63270, #38196, #4404, #18256, #62960, #37559, #52671 ),
 .UNSPECIFIED., .F., .F. ) 
 B_SPLINE_CURVE_WITH_KNOTS ( ( 3, 2, 2, 2, 3 ),
 ( 0.8553571428571428159, 0.8559523809523809090, 0.8571428571428570953, 0.8583333333333332815, 0.8589285714285714857 ),
 .UNSPECIFIED. ) 
 CURVE ( )  GEOMETRIC_REPRESENTATION_ITEM ( )  RATIONAL_B_SPLINE_CURVE ( ( 0.9330127018922194093, 0.9330127018922194093, 1.000000000000000000, 0.8660254037844387076, 1.000000000000000000, 0.8660254037844387076, 1.000000000000000000, 0.9330127018922130810, 0.9330127018922194093 ) ) 
 REPRESENTATION_ITEM ( '' )  );
#3931 = CARTESIAN_POINT ( 'NONE',  ( -1.339745962155613812, -105.0803417985302843, -5.000000000000000000 ) ) ;
#3932 = CARTESIAN_POINT ( 'NONE',  ( -4.458734124999999437, -88.56249999863439371, 0.000000000000000000 ) ) ;
#3933 = CARTESIAN_POINT ( 'NONE',  ( -4.458734124999999437, -157.1875000013655779, -5.460374474430324690E-16 ) ) ;
#3934 = CARTESIAN_POINT ( 'NONE',  ( 1.060575238724906964E-15, -36.75000000000000711, 5.773502691896257311 ) ) ;
#3935 = FACE_OUTER_BOUND ( 'NONE', #43740, .T. ) ;
#3936 = ORIENTED_EDGE ( 'NONE', *, *, #8369, .T. ) ;
#3937 = CARTESIAN_POINT ( 'NONE',  ( 2.500000000000002220, -22.66666666666666785, 4.330127018922192761 ) ) ;
#3938 = VERTEX_POINT ( 'NONE', #53983 ) ;
#3939 = CARTESIAN_POINT ( 'NONE',  ( 4.458734124999998549, -93.72916666530105090, -2.574251347313721627 ) ) ;
#3940 = CARTESIAN_POINT ( 'NONE',  ( 4.458734125000001214, 5.854166668032262599, 2.574251347313718519 ) ) ;
#3941 = CARTESIAN_POINT ( 'NONE',  ( 5.000000000000000000, 13.70833333606451987, -2.886751345948129988 ) ) ;
#3942 = CARTESIAN_POINT ( 'NONE',  ( 5.000000000000000888, 12.41666666666666607, 2.886751345948126879 ) ) ;
#3943 = CARTESIAN_POINT ( 'NONE',  ( 5.000000000000000000, 2.499999999999998668, -6.123233995736766282E-16 ) ) ;
#3944 = CARTESIAN_POINT ( 'NONE',  ( 4.458734125000000326, -63.89583333196772941, 2.574251347313718519 ) ) ;
#3945 = DIRECTION ( 'NONE',  ( 0.000000000000000000, -1.000000000000000000, 0.000000000000000000 ) ) ;
#3946 = CARTESIAN_POINT ( 'NONE',  ( 2.499999999999998668, 1.791666669397853795, -4.330127018922193649 ) ) ;
#3947 = CARTESIAN_POINT ( 'NONE',  ( 4.458734124999999437, -26.81249999863440081, -5.460374474430324690E-16 ) ) ;
#3948 = DIRECTION ( 'NONE',  ( -0.000000000000000000, 1.000000000000000000, -0.000000000000000000 ) ) ;
#3949 = CARTESIAN_POINT ( 'NONE',  ( -1.339745962155611370, 25.91965820146970856, -5.000000000000000888 ) ) ;
#3950 = ADVANCED_FACE ( 'NONE', ( #14736 ), #30260, .T. ) ;
#3951 = CARTESIAN_POINT ( 'NONE',  ( 2.499999999999998668, -19.33333333333333570, -4.330127018922193649 ) ) ;
#3952 = CARTESIAN_POINT ( 'NONE',  ( 2.499999999999998668, -44.33333333333333570, -4.330127018922193649 ) ) ;
#3954 = CARTESIAN_POINT ( 'NONE',  ( -4.458734124999998549, -17.47916666530106866, 2.574251347313722516 ) ) ;
#3953 = DIRECTION ( 'NONE',  ( -1.000000000000000000, 0.000000000000000000, 0.000000000000000000 ) ) ;
#3955 = VECTOR ( 'NONE', #24371, 1000.000000000000000 ) ;
#3956 = CARTESIAN_POINT ( 'NONE',  ( 4.458734124999999437, -63.81249999863440792, -5.460374474430324690E-16 ) ) ;
#3957 = CARTESIAN_POINT ( 'NONE',  ( -3.152801135295367985, -146.0625000013655779, 3.152801135295367096 ) ) ;
#3958 = CARTESIAN_POINT ( 'NONE',  ( -4.458734124999998549, -75.22916666530106511, 2.574251347313722516 ) ) ;
#3959 = VECTOR ( 'NONE', #9156, 1000.000000000000000 ) ;
#3960 = CARTESIAN_POINT ( 'NONE',  ( -51.60603307380591787, -145.1875000013656063, -2.891590998281053704 ) ) ;
#3961 = CARTESIAN_POINT ( 'NONE',  ( -4.458734124999998549, -27.47916666530106866, 2.574251347313722516 ) ) ;
#3962 = CARTESIAN_POINT ( 'NONE',  ( -5.000000000000000000, -65.95833333060213022, -2.886751345948128211 ) ) ;
#3963 = ORIENTED_EDGE ( 'NONE', *, *, #10765, .T. ) ;
#3964 = CARTESIAN_POINT ( 'NONE',  ( 1.975475456537005874E-15, -51.75000000000000711, 5.000000000000000000 ) ) ;
#3965 = ORIENTED_EDGE ( 'NONE', *, *, #22115, .F. ) ;
#3966 = CARTESIAN_POINT ( 'NONE',  ( 9.457646018065525792E-16, -65.31249999863440792, 5.148502694627439702 ) ) ;
#3967 = CARTESIAN_POINT ( 'NONE',  ( 2.788906526875773208E-15, 28.75000000000000000, -5.000000000000000000 ) ) ;
#3968 = DIRECTION ( 'NONE',  ( -1.000000000000000000, 0.000000000000000000, 0.000000000000000000 ) ) ;
#3969 = ORIENTED_EDGE ( 'NONE', *, *, #18886, .T. ) ;
#3970 = CARTESIAN_POINT ( 'NONE',  ( -58.24261429053147765, -143.3750000027312126, -3.805975901505573855 ) ) ;
#3971 = EDGE_CURVE ( 'NONE', #35606, #62202, #62722, .T. ) ;
#3972 = CARTESIAN_POINT ( 'NONE',  ( 2.229367062500001939, -52.22916666530107221, 3.861377020970579999 ) ) ;
#3973 = CARTESIAN_POINT ( 'NONE',  ( 4.458734125000001214, -0.1458333319677394824, 2.574251347313718519 ) ) ;
#3974 = ORIENTED_EDGE ( 'NONE', *, *, #52664, .F. ) ;
#3975 = CARTESIAN_POINT ( 'NONE',  ( -1.339745962155610925, -54.79465819873851018, 5.000000000000000000 ) ) ;
#3976 = CARTESIAN_POINT ( 'NONE',  ( -4.458734124999999437, 17.68750000136559208, 0.000000000000000000 ) ) ;
#3977 = CARTESIAN_POINT ( 'NONE',  ( -58.39396692619412477, -145.4375000013656063, 2.891590998281057701 ) ) ;
#3978 = CARTESIAN_POINT ( 'NONE',  ( -6.972266317189433020E-16, 16.74999999999999645, -5.000000000000000000 ) ) ;
#3979 = CARTESIAN_POINT ( 'NONE',  ( -1.846868145590737420, -165.7500000013655779, 4.458734124999997661 ) ) ;
#3980 =( BOUNDED_CURVE ( )  B_SPLINE_CURVE ( 2, ( #21109, #20796, #40399, #544, #6324, #16287, #49735, #50056, #25615 ),
 .UNSPECIFIED., .F., .F. ) 
 B_SPLINE_CURVE_WITH_KNOTS ( ( 3, 2, 2, 2, 3 ),
 ( 0.9124999999999999778, 0.9130952380952380709, 0.9142857142857142572, 0.9154761904761904434, 0.9160714285714285365 ),
 .UNSPECIFIED. ) 
 CURVE ( )  GEOMETRIC_REPRESENTATION_ITEM ( )  RATIONAL_B_SPLINE_CURVE ( ( 0.9330127018922194093, 0.9330127018922194093, 1.000000000000000000, 0.8660254037844387076, 1.000000000000000000, 0.8660254037844387076, 1.000000000000000000, 0.9330127018922194093, 0.9330127018922194093 ) ) 
 REPRESENTATION_ITEM ( '' )  );
#3981 = ORIENTED_EDGE ( 'NONE', *, *, #60913, .F. ) ;
#3982 = CARTESIAN_POINT ( 'NONE',  ( -2.229367062500000163, -78.47916666530106511, -3.861377020970580443 ) ) ;
#3983 = CARTESIAN_POINT ( 'NONE',  ( 3.750000000000004441, -6.495190528383289141, 0.000000000000000000 ) ) ;
#3984 = CARTESIAN_POINT ( 'NONE',  ( 9.457646018065525792E-16, 9.937500001365592084, 5.148502694627439702 ) ) ;
#3985 = CARTESIAN_POINT ( 'NONE',  ( 5.000000000000000000, -19.37499999726881583, -6.123233995736766282E-16 ) ) ;
#3986 = CARTESIAN_POINT ( 'NONE',  ( 2.229367062499998831, -57.89583333196773651, -3.861377020970580887 ) ) ;
#3987 = CARTESIAN_POINT ( 'NONE',  ( -2.499999999999996447, -21.70833333060214798, 4.330127018922195425 ) ) ;
#3988 = CYLINDRICAL_SURFACE ( 'NONE', #2932, 5.000000000000000000 ) ;
#3989 = CARTESIAN_POINT ( 'NONE',  ( 5.000000000000000000, -42.37499999726880873, -6.123233995736766282E-16 ) ) ;
#3990 = CARTESIAN_POINT ( 'NONE',  ( -4.458734124999999437, 29.68750000136559208, 0.000000000000000000 ) ) ;
#3991 = CARTESIAN_POINT ( 'NONE',  ( 4.458734124999998549, -38.72916666530106511, -2.574251347313721627 ) ) ;
#3992 = PRODUCT_DEFINITION_SHAPE ( 'NONE', 'NONE',  #63681 ) ;
#3993 = CARTESIAN_POINT ( 'NONE',  ( 4.458734124999998549, -28.97916666530108287, -2.574251347313721627 ) ) ;
#3994 = AXIS2_PLACEMENT_3D ( 'NONE', #44911, #63582, #30098 ) ;
#3995 = CARTESIAN_POINT ( 'NONE',  ( -59.98410592259440222, -140.2500000027312126, -0.3983568153799752487 ) ) ;
#3996 = CARTESIAN_POINT ( 'NONE',  ( -2.499999999999996447, 24.16666666666666785, 4.330127018922195425 ) ) ;
#3997 = CARTESIAN_POINT ( 'NONE',  ( -5.000000000000000888, -151.5625000027311842, 2.071067811865474617 ) ) ;
#3998 = ORIENTED_EDGE ( 'NONE', *, *, #41247, .T. ) ;
#3999 = CARTESIAN_POINT ( 'NONE',  ( -2.229367062499996610, -109.3958333319677365, 3.861377020970582219 ) ) ;
#4000 = AXIS2_PLACEMENT_3D ( 'NONE', #37123, #42246, #17171 ) ;
#4001 = CARTESIAN_POINT ( 'NONE',  ( 2.229367062499998831, -32.64583333196773651, -3.861377020970580887 ) ) ;
#4002 = CARTESIAN_POINT ( 'NONE',  ( 1.060575238724906964E-15, -68.62499999726881583, 5.773502691896257311 ) ) ;
#4003 = CARTESIAN_POINT ( 'NONE',  ( -55.35523342533222291, -149.5625000013656063, 4.444560631937231499 ) ) ;
#4004 = CARTESIAN_POINT ( 'NONE',  ( 3.535533905932738197, -141.8750000000000000, -3.535533905932738197 ) ) ;
#4005 = EDGE_CURVE ( 'NONE', #32177, #5681, #30432, .T. ) ;
#4006 = EDGE_CURVE ( 'NONE', #37366, #29442, #57589, .T. ) ;
#4007 = CARTESIAN_POINT ( 'NONE',  ( 9.457646018065525792E-16, -77.31249999863440792, 5.148502694627439702 ) ) ;
#4008 = CARTESIAN_POINT ( 'NONE',  ( -1.339745962155610925, -54.79465819873851018, 5.000000000000000000 ) ) ;
#4009 = CARTESIAN_POINT ( 'NONE',  ( 4.458734125000000326, -32.89583333196774362, 2.574251347313718519 ) ) ;
#4010 = EDGE_CURVE ( 'NONE', #37866, #62194, #3860, .T. ) ;
#4011 = CARTESIAN_POINT ( 'NONE',  ( -5.000000000000000000, -27.87499999726880873, 0.000000000000000000 ) ) ;
#4012 = CARTESIAN_POINT ( 'NONE',  ( 5.000000000000000888, -21.58333333333332860, 2.886751345948126879 ) ) ;
#4013 = CARTESIAN_POINT ( 'NONE',  ( 4.458734124999999437, -146.4375000013656063, 0.000000000000000000 ) ) ;
#4014 = VERTEX_POINT ( 'NONE', #61779 ) ;
#4015 = CARTESIAN_POINT ( 'NONE',  ( 2.229367062499998831, -58.89583333196773651, -3.861377020970580887 ) ) ;
#4016 =( BOUNDED_CURVE ( )  B_SPLINE_CURVE ( 2, ( #2019, #35455, #45100, #56036, #1697, #31253, #20986, #54760, #46058 ),
 .UNSPECIFIED., .F., .F. ) 
 B_SPLINE_CURVE_WITH_KNOTS ( ( 3, 2, 2, 2, 3 ),
 ( 0.7687500000000000444, 0.7694444444444444864, 0.7708333333333333703, 0.7722222222222222543, 0.7729166666666666963 ),
 .UNSPECIFIED. ) 
 CURVE ( )  GEOMETRIC_REPRESENTATION_ITEM ( )  RATIONAL_B_SPLINE_CURVE ( ( 0.9330127018922194093, 0.9330127018922194093, 1.000000000000000000, 0.8660254037844387076, 1.000000000000000000, 0.8660254037844387076, 1.000000000000000000, 0.9330127018922194093, 0.9330127018922194093 ) ) 
 REPRESENTATION_ITEM ( '' )  );
#4017 = EDGE_CURVE ( 'NONE', #61397, #8313, #22859, .T. ) ;
#4018 = CARTESIAN_POINT ( 'NONE',  ( 2.499999999999998668, 24.79166666939785202, -4.330127018922193649 ) ) ;
#4019 = CARTESIAN_POINT ( 'NONE',  ( -6.972266317189433020E-16, 0.8750000027311866102, -5.000000000000000000 ) ) ;
#4020 = CARTESIAN_POINT ( 'NONE',  ( -3.535250795749689387E-16, 17.75000000000000355, -5.773502691896257311 ) ) ;
#4021 = ADVANCED_FACE ( 'NONE', ( #41819 ), #33436, .T. ) ;
#4022 = EDGE_CURVE ( 'NONE', #24536, #2392, #18332, .T. ) ;
#4023 = CARTESIAN_POINT ( 'NONE',  ( -2.229367062499996610, -8.145833331967736513, 3.861377020970582219 ) ) ;
#4024 = CARTESIAN_POINT ( 'NONE',  ( -4.999999999999998224, -51.79166666393547303, 2.886751345948131764 ) ) ;
#4025 = CARTESIAN_POINT ( 'NONE',  ( 5.000000000000000888, -14.58333333333333215, 2.886751345948126879 ) ) ;
#4026 = CARTESIAN_POINT ( 'NONE',  ( 4.458734125000001214, 9.854166668032263487, 2.574251347313718519 ) ) ;
#4027 = EDGE_CURVE ( 'NONE', #31959, #12417, #29881, .T. ) ;
#4028 = ORIENTED_EDGE ( 'NONE', *, *, #7875, .T. ) ;
#4029 = CARTESIAN_POINT ( 'NONE',  ( -50.01589407740564042, -135.6250000000000284, 0.3983568153799778022 ) ) ;
#4030 = CARTESIAN_POINT ( 'NONE',  ( -4.458734124999999437, -47.31249999863440792, 0.000000000000000000 ) ) ;
#4031 = EDGE_CURVE ( 'NONE', #49961, #4714, #8119, .T. ) ;
#4032 = CARTESIAN_POINT ( 'NONE',  ( -1.846868145590734756, -160.3750000013656063, -4.458734125000000326 ) ) ;
#4033 = EDGE_CURVE ( 'NONE', #13136, #8193, #38898, .T. ) ;
#4034 = CARTESIAN_POINT ( 'NONE',  ( 2.500000000000002220, -48.54166666393547303, 4.330127018922192761 ) ) ;
#4035 = ORIENTED_EDGE ( 'NONE', *, *, #40149, .T. ) ;
#4036 = CARTESIAN_POINT ( 'NONE',  ( -4.458734124999999437, -21.39583333196774007, -2.574251347313719407 ) ) ;
#4037 = ORIENTED_EDGE ( 'NONE', *, *, #26102, .F. ) ;
#4039 = CARTESIAN_POINT ( 'NONE',  ( -1.339745962155613812, -12.20534180126147739, -5.000000000000000000 ) ) ;
#4038 = DIRECTION ( 'NONE',  ( -0.000000000000000000, 1.000000000000000000, -0.000000000000000000 ) ) ;
#4040 = CARTESIAN_POINT ( 'NONE',  ( 1.846868145590736310, -161.6250000013656063, 4.458734124999999437 ) ) ;
#4041 = ORIENTED_EDGE ( 'NONE', *, *, #59246, .F. ) ;
#4042 = AXIS2_PLACEMENT_3D ( 'NONE', #23320, #42921, #28447 ) ;
#4043 = DIRECTION ( 'NONE',  ( -0.000000000000000000, 1.000000000000000000, -0.000000000000000000 ) ) ;
#4044 = CARTESIAN_POINT ( 'NONE',  ( -54.60164318462004474, -132.3750000000000284, -4.984105922594373794 ) ) ;
#4045 = VECTOR ( 'NONE', #49167, 1000.000000000000000 ) ;
#4046 = CARTESIAN_POINT ( 'NONE',  ( 9.457646018065525792E-16, -37.31249999863440792, 5.148502694627439702 ) ) ;
#4047 = EDGE_LOOP ( 'NONE', ( #37236, #3028, #58834, #32365 ) ) ;
#4048 = CARTESIAN_POINT ( 'NONE',  ( -4.458734124999998549, -84.22916666530107932, 2.574251347313722516 ) ) ;
#4049 = CARTESIAN_POINT ( 'NONE',  ( 2.229367062499998831, 19.35416666803225993, -3.861377020970580887 ) ) ;
#4050 = CARTESIAN_POINT ( 'NONE',  ( -6.972266317189433020E-16, -18.12499999726881228, -5.000000000000000000 ) ) ;
#4051 = EDGE_LOOP ( 'NONE', ( #543, #39844, #14713 ) ) ;
#4052 = CARTESIAN_POINT ( 'NONE',  ( -53.51423613279429503, -137.5000000013656063, 4.591703134518083651 ) ) ;
#4053 = CARTESIAN_POINT ( 'NONE',  ( 9.457646018065525792E-16, -86.31249999863440792, 5.148502694627439702 ) ) ;
#4054 = CARTESIAN_POINT ( 'NONE',  ( -57.46284108482265651, -127.0625000027312410, 4.819101127000239515 ) ) ;
#4055 = CARTESIAN_POINT ( 'NONE',  ( 1.339745962155615144, -4.580341798530294994, 4.999999999999999112 ) ) ;
#4056 = CARTESIAN_POINT ( 'NONE',  ( -5.000000000000000000, -6.999999999999999112, 0.000000000000000000 ) ) ;
#4057 = CARTESIAN_POINT ( 'NONE',  ( -1.339745962155610925, -44.66965819600733312, 5.000000000000000000 ) ) ;
#4058 = CARTESIAN_POINT ( 'NONE',  ( -4.458734124999997661, -61.22916666530106511, 2.574251347313722516 ) ) ;
#4059 = CARTESIAN_POINT ( 'NONE',  ( 5.000000000000000888, 21.41666666666666430, 2.886751345948126879 ) ) ;
#4060 = CARTESIAN_POINT ( 'NONE',  ( 4.458734124999999437, 23.18750000136559564, -5.460374474430324690E-16 ) ) ;
#4061 = CARTESIAN_POINT ( 'NONE',  ( 5.000000000000000000, -42.41666666666667140, -2.886751345948130876 ) ) ;
#4062 = DIRECTION ( 'NONE',  ( -0.000000000000000000, -0.000000000000000000, 1.000000000000000000 ) ) ;
#4063 = CARTESIAN_POINT ( 'NONE',  ( -4.458734124999999437, -44.56249999863440081, 0.000000000000000000 ) ) ;
#4064 = CARTESIAN_POINT ( 'NONE',  ( 5.000000000000000000, -2.291666663935477466, -2.886751345948129988 ) ) ;
#4065 = CARTESIAN_POINT ( 'NONE',  ( 0.000000000000000000, -170.0000000000000000, 5.000000000000000000 ) ) ;
#4066 = CARTESIAN_POINT ( 'NONE',  ( -1.339745962155613812, -61.20534180126147561, -5.000000000000000000 ) ) ;
#4067 = CARTESIAN_POINT ( 'NONE',  ( 2.229367062500001939, -85.22916666530107932, 3.861377020970579999 ) ) ;
#4068 = CARTESIAN_POINT ( 'NONE',  ( -4.458734124999999437, -106.3958333319677365, -2.574251347313719407 ) ) ;
#4069 = CARTESIAN_POINT ( 'NONE',  ( -2.229367062500000163, -9.729166665301068662, -3.861377020970580443 ) ) ;
#4070 = ORIENTED_EDGE ( 'NONE', *, *, #3320, .F. ) ;
#4071 = CARTESIAN_POINT ( 'NONE',  ( -6.972266317189433020E-16, -46.24999999999999289, -5.000000000000000000 ) ) ;
#4072 = CARTESIAN_POINT ( 'NONE',  ( 9.457646018065525792E-16, -98.06249999863440792, 5.148502694627439702 ) ) ;
#4073 = CARTESIAN_POINT ( 'NONE',  ( 3.061616997868383141E-16, -166.8750000027312126, -5.000000000000000000 ) ) ;
#4074 = CARTESIAN_POINT ( 'NONE',  ( 4.458734124999998549, -91.97916666530107932, -2.574251347313721627 ) ) ;
#4075 = CARTESIAN_POINT ( 'NONE',  ( 2.499999999999998668, -54.20833333060213732, -4.330127018922193649 ) ) ;
#4076 = CARTESIAN_POINT ( 'NONE',  ( -5.047120108843199837, 5.746297884371392328, -0.1007566405101777279 ) ) ;
#4077 = CARTESIAN_POINT ( 'NONE',  ( -55.35523342533222291, -131.3125000013656063, 4.444560631937231499 ) ) ;
#4078 = CARTESIAN_POINT ( 'NONE',  ( -59.29741812935640155, -147.6250000013655779, -2.196230717870135685 ) ) ;
#4079 = CARTESIAN_POINT ( 'NONE',  ( -4.458734124999999437, -13.39583333196774007, -2.574251347313719407 ) ) ;
#4080 = CARTESIAN_POINT ( 'NONE',  ( 2.229367062499998831, 10.10416666803225993, -3.861377020970580887 ) ) ;
#4081 = CARTESIAN_POINT ( 'NONE',  ( -2.229367062499996610, -59.39583333196773651, 3.861377020970582219 ) ) ;
#4082 = CARTESIAN_POINT ( 'NONE',  ( -1.339745962155610925, -68.79465819873850307, 5.000000000000000000 ) ) ;
#4083 = CARTESIAN_POINT ( 'NONE',  ( 2.499999999999998668, -15.20833333060214443, -4.330127018922193649 ) ) ;
#4084 = CARTESIAN_POINT ( 'NONE',  ( 2.229367062499998831, -13.64583333196774184, -3.861377020970580887 ) ) ;
#4085 = DIRECTION ( 'NONE',  ( -0.000000000000000000, 1.000000000000000000, -0.000000000000000000 ) ) ;
#4086 = VERTEX_POINT ( 'NONE', #53998 ) ;
#4087 = CARTESIAN_POINT ( 'NONE',  ( 9.457646018065525792E-16, -40.31249999863440081, 5.148502694627439702 ) ) ;
#4088 = AXIS2_PLACEMENT_3D ( 'NONE', #52390, #18899, #38513 ) ;
#4089 = CARTESIAN_POINT ( 'NONE',  ( -59.44456063193725015, -124.8125000013655921, -0.3552334253322034230 ) ) ;
#4090 = DIRECTION ( 'NONE',  ( 0.000000000000000000, 1.000000000000000000, 0.000000000000000000 ) ) ;
#4091 = CARTESIAN_POINT ( 'NONE',  ( -1.305263714129178521, 8.377797850839286298, -7.792447862505335721 ) ) ;
#4092 = CARTESIAN_POINT ( 'NONE',  ( 4.458734124999998549, -84.72916666530106511, -2.574251347313721627 ) ) ;
#4093 = CARTESIAN_POINT ( 'NONE',  ( -2.229367062499996610, 18.60416666803225993, 3.861377020970582219 ) ) ;
#4094 = AXIS2_PLACEMENT_3D ( 'NONE', #55763, #7197, #55125 ) ;
#4095 = CARTESIAN_POINT ( 'NONE',  ( 2.229367062500001939, 14.02083333469892779, 3.861377020970579999 ) ) ;
#4096 = CARTESIAN_POINT ( 'NONE',  ( -5.000000000000000000, -81.87499999726881583, 0.000000000000000000 ) ) ;
#4097 = CARTESIAN_POINT ( 'NONE',  ( -51.19402409849444524, -137.6250000027312410, -3.242614290531456334 ) ) ;
#4098 = CARTESIAN_POINT ( 'NONE',  ( -4.458734124999997661, -88.47916666530107932, 2.574251347313722516 ) ) ;
#4099 = CARTESIAN_POINT ( 'NONE',  ( 2.499999999999998668, -70.33333333333332860, -4.330127018922193649 ) ) ;
#4100 = CARTESIAN_POINT ( 'NONE',  ( 5.000000000000000000, 13.70833333606451987, -2.886751345948129988 ) ) ;
#4102 = VERTEX_POINT ( 'NONE', #44018 ) ;
#4101 = ADVANCED_FACE ( 'NONE', ( #8992 ), #37608, .T. ) ;
#4103 = CARTESIAN_POINT ( 'NONE',  ( 2.500000000000002220, -79.66666666666665719, 4.330127018922192761 ) ) ;
#4104 = CARTESIAN_POINT ( 'NONE',  ( -4.999999999999998224, -79.79166666393545881, 2.886751345948131764 ) ) ;
#4106 = CARTESIAN_POINT ( 'NONE',  ( -2.499999999999996447, -28.83333333333333570, 4.330127018922195425 ) ) ;
#4105 = FACE_BOUND ( 'NONE', #26594, .T. ) ;
#4107 = CARTESIAN_POINT ( 'NONE',  ( -4.458734124999998549, -31.22916666530107221, 2.574251347313722516 ) ) ;
#4108 =( BOUNDED_CURVE ( )  B_SPLINE_CURVE ( 2, ( #46172, #57105, #55827, #11742, #32007, #13022, #23004, #3072, #17545 ),
 .UNSPECIFIED., .F., .F. ) 
 B_SPLINE_CURVE_WITH_KNOTS ( ( 3, 2, 2, 2, 3 ),
 ( 0.4446428571428571175, 0.4452380952380952106, 0.4464285714285714524, 0.4476190476190476386, 0.4482142857142857317 ),
 .UNSPECIFIED. ) 
 CURVE ( )  GEOMETRIC_REPRESENTATION_ITEM ( )  RATIONAL_B_SPLINE_CURVE ( ( 0.9330127018922194093, 0.9330127018922194093, 1.000000000000000000, 0.8660254037844387076, 1.000000000000000000, 0.8660254037844387076, 1.000000000000000000, 0.9330127018922194093, 0.9330127018922194093 ) ) 
 REPRESENTATION_ITEM ( '' )  );
#4109 = EDGE_CURVE ( 'NONE', #44442, #20861, #49990, .T. ) ;
#4110 = CARTESIAN_POINT ( 'NONE',  ( 2.499999999999998668, -36.20833333060213732, -4.330127018922193649 ) ) ;
#4112 = ORIENTED_EDGE ( 'NONE', *, *, #40875, .F. ) ;
#4111 = CARTESIAN_POINT ( 'NONE',  ( 9.457646018065525792E-16, -63.06249999863440081, 5.148502694627439702 ) ) ;
#4113 = CARTESIAN_POINT ( 'NONE',  ( -52.80376928212989185, -151.1250000013655779, -4.297418129356379346 ) ) ;
#4115 = VERTEX_POINT ( 'NONE', #5115 ) ;
#4114 = CARTESIAN_POINT ( 'NONE',  ( -3.152548672688508926E-16, -13.81249999863440436, -5.148502694627439702 ) ) ;
#4116 = CARTESIAN_POINT ( 'NONE',  ( -4.999999999999999112, -78.91666666666665719, 2.886751345948131764 ) ) ;
#4117 = CARTESIAN_POINT ( 'NONE',  ( -50.55543936806279248, -135.0625000013656063, 0.3552334253322060320 ) ) ;
#4118 = CARTESIAN_POINT ( 'NONE',  ( 2.229367062500001939, -57.22916666530107932, 3.861377020970579999 ) ) ;
#4119 = CARTESIAN_POINT ( 'NONE',  ( 5.000000000000000888, -83.45833333060213022, 2.886751345948126879 ) ) ;
#4121 = ORIENTED_EDGE ( 'NONE', *, *, #11770, .F. ) ;
#4120 = LINE ( 'NONE', #8622, #6672 ) ;
#4122 = CARTESIAN_POINT ( 'NONE',  ( -58.80597590150559739, -146.0000000000000284, 3.242614290531460330 ) ) ;
#4123 = CARTESIAN_POINT ( 'NONE',  ( -4.458734124999998549, -22.47916666530107577, 2.574251347313722516 ) ) ;
#4125 = ORIENTED_EDGE ( 'NONE', *, *, #22819, .T. ) ;
#4124 = CARTESIAN_POINT ( 'NONE',  ( -4.458734124999999437, -55.56249999863440081, 0.000000000000000000 ) ) ;
#4126 = CARTESIAN_POINT ( 'NONE',  ( 0.000000000000000000, 0.000000000000000000, 0.000000000000000000 ) ) ;
#4127 = CARTESIAN_POINT ( 'NONE',  ( -8.190561711645485556E-16, -167.9375000013655779, 4.458734124999999437 ) ) ;
#4128 = CARTESIAN_POINT ( 'NONE',  ( 2.229367062499998831, -104.8958333319677365, -3.861377020970580887 ) ) ;
#4129 = CARTESIAN_POINT ( 'NONE',  ( -2.499999999999996447, 18.16666666666666430, 4.330127018922195425 ) ) ;
#4130 = ORIENTED_EDGE ( 'NONE', *, *, #42035, .F. ) ;
#4131 = CARTESIAN_POINT ( 'NONE',  ( -52.80376928212989185, -152.1250000013656063, -4.297418129356378458 ) ) ;
#4132 = CARTESIAN_POINT ( 'NONE',  ( -51.75738570946856498, -136.8750000027312126, 3.805975901505576964 ) ) ;
#4133 = CARTESIAN_POINT ( 'NONE',  ( -2.229367062499996610, -39.14583333196773651, 3.861377020970582219 ) ) ;
#4134 = CARTESIAN_POINT ( 'NONE',  ( -55.00000000000002132, -155.0000000000000284, 1.734723475976807094E-15 ) ) ;
#4135 = VECTOR ( 'NONE', #36854, 1000.000000000000000 ) ;
#4136 = CARTESIAN_POINT ( 'NONE',  ( 2.229367062499998831, -12.64583333196774007, -3.861377020970580887 ) ) ;
#4137 = CARTESIAN_POINT ( 'NONE',  ( 4.458734124999999437, -99.06249999863440792, -5.460374474430324690E-16 ) ) ;
#4138 = CARTESIAN_POINT ( 'NONE',  ( 4.458734124999999437, -142.7500000013656063, 1.846868145590737864 ) ) ;
#4139 = CARTESIAN_POINT ( 'NONE',  ( 4.458734125000001214, -28.14583333196774007, 2.574251347313718519 ) ) ;
#4140 = CARTESIAN_POINT ( 'NONE',  ( 1.339745962155615144, -70.70534180126148271, 4.999999999999999112 ) ) ;
#4141 = CARTESIAN_POINT ( 'NONE',  ( -55.35523342533222291, -133.3125000013656063, 4.444560631937231499 ) ) ;
#4142 = CARTESIAN_POINT ( 'NONE',  ( -2.229367062500000163, -69.72916666530107932, -3.861377020970580443 ) ) ;
#4143 = CARTESIAN_POINT ( 'NONE',  ( 1.339745962155615144, -21.58034179853029855, 4.999999999999999112 ) ) ;
#4144 = CARTESIAN_POINT ( 'NONE',  ( -1.339745962155610925, -42.66965819600731891, 5.000000000000000000 ) ) ;
#4145 = CARTESIAN_POINT ( 'NONE',  ( -4.458734125000000326, -141.8750000013656063, 1.846868145590734089 ) ) ;
#4146 = CARTESIAN_POINT ( 'NONE',  ( 9.457646018065525792E-16, 3.687500001365594748, 5.148502694627439702 ) ) ;
#4147 = ORIENTED_EDGE ( 'NONE', *, *, #28311, .F. ) ;
#4148 = FACE_OUTER_BOUND ( 'NONE', #35499, .T. ) ;
#4149 = AXIS2_PLACEMENT_3D ( 'NONE', #6578, #3034, #22009 ) ;
#4150 = CARTESIAN_POINT ( 'NONE',  ( -5.000000000000000000, 16.12500000273118417, 0.000000000000000000 ) ) ;
#4152 = CARTESIAN_POINT ( 'NONE',  ( 4.458734124999998549, -30.72916666530107221, -2.574251347313721627 ) ) ;
#4151 = CARTESIAN_POINT ( 'NONE',  ( 5.000000000000000000, -95.41666666666667140, -2.886751345948129988 ) ) ;
#4153 = CARTESIAN_POINT ( 'NONE',  ( 5.000000000000000000, -14.37499999726881228, -6.123233995736766282E-16 ) ) ;
#4154 = CARTESIAN_POINT ( 'NONE',  ( 9.457646018065525792E-16, -76.31249999863439371, 5.148502694627439702 ) ) ;
#4155 = CARTESIAN_POINT ( 'NONE',  ( 9.457646018065525792E-16, 22.68750000136559564, 5.148502694627439702 ) ) ;
#4156 = CARTESIAN_POINT ( 'NONE',  ( 0.000000000000000000, -170.0000000000000000, 0.000000000000000000 ) ) ;
#4157 = CARTESIAN_POINT ( 'NONE',  ( -54.64476657466781973, -139.8125000013656063, -4.444560631937228834 ) ) ;
#4158 = CARTESIAN_POINT ( 'NONE',  ( -2.229367062500000163, 4.520833334698926897, -3.861377020970580443 ) ) ;
#4159 = CARTESIAN_POINT ( 'NONE',  ( -2.229367062500000163, 29.27083333469892779, -3.861377020970580443 ) ) ;
#4160 = CARTESIAN_POINT ( 'NONE',  ( 4.458734124999999437, -44.06249999863440081, -5.460374474430324690E-16 ) ) ;
#4161 =( BOUNDED_CURVE ( )  B_SPLINE_CURVE ( 2, ( #3655, #12351, #13294, #7532, #42558, #27144, #42872, #37429, #18435 ),
 .UNSPECIFIED., .F., .F. ) 
 B_SPLINE_CURVE_WITH_KNOTS ( ( 3, 2, 2, 2, 3 ),
 ( 0.6583333333333329929, 0.6624999999999996447, 0.6666666666666662966, 0.6708333333333328374, 0.6749999999999996003 ),
 .UNSPECIFIED. ) 
 CURVE ( )  GEOMETRIC_REPRESENTATION_ITEM ( )  RATIONAL_B_SPLINE_CURVE ( ( 1.000000000000005995, 0.9238795325112806323, 1.000000000000000000, 0.9238795325112867385, 1.000000000000000000, 0.9238795325112867385, 1.000000000000000000, 0.9238795325112948431, 0.9999999999999918954 ) ) 
 REPRESENTATION_ITEM ( '' )  );
#4162 = CARTESIAN_POINT ( 'NONE',  ( 1.975475456537005874E-15, -60.62499999726880162, 5.000000000000000000 ) ) ;
#4163 = CARTESIAN_POINT ( 'NONE',  ( 4.458734124999998549, 0.2708333346989263979, -2.574251347313721627 ) ) ;
#4164 = CARTESIAN_POINT ( 'NONE',  ( 2.229367062499998831, -24.89583333196773651, -3.861377020970580887 ) ) ;
#4165 =( BOUNDED_CURVE ( )  B_SPLINE_CURVE ( 2, ( #57438, #37183, #17238, #56808, #3405, #41661, #62580, #42624, #47762 ),
 .UNSPECIFIED., .F., .F. ) 
 B_SPLINE_CURVE_WITH_KNOTS ( ( 3, 2, 2, 2, 3 ),
 ( 0.02500000000000002220, 0.02916666666666669488, 0.03333333333333336757, 0.03750000000000003331, 0.04166666666666670599 ),
 .UNSPECIFIED. ) 
 CURVE ( )  GEOMETRIC_REPRESENTATION_ITEM ( )  RATIONAL_B_SPLINE_CURVE ( ( 0.9999999999999996669, 0.9238795325112870716, 1.000000000000000000, 0.9238795325112867385, 1.000000000000000000, 0.9238795325112867385, 1.000000000000000000, 0.9238795325112859613, 1.000000000000000666 ) ) 
 REPRESENTATION_ITEM ( '' )  );
#4166 = CARTESIAN_POINT ( 'NONE',  ( 2.730187237215162345E-16, -155.1875000013655779, -4.458734124999999437 ) ) ;
#4167 = CARTESIAN_POINT ( 'NONE',  ( 4.458734124999999437, -66.81249999863440792, -5.460374474430324690E-16 ) ) ;
#4168 = CARTESIAN_POINT ( 'NONE',  ( 5.000000000000000888, -102.4583333306021444, 2.886751345948126879 ) ) ;
#4169 = FACE_OUTER_BOUND ( 'NONE', #6587, .T. ) ;
#4170 = CARTESIAN_POINT ( 'NONE',  ( 0.000000000000000000, -120.0000000000000000, 0.000000000000000000 ) ) ;
#4171 = CARTESIAN_POINT ( 'NONE',  ( -4.458734124999997661, -107.4791666653010651, 2.574251347313722516 ) ) ;
#4172 = CARTESIAN_POINT ( 'NONE',  ( 4.458734125000000326, -74.14583333196773651, 2.574251347313718519 ) ) ;
#4173 = CARTESIAN_POINT ( 'NONE',  ( -2.499999999999996447, -55.83333333333332860, 4.330127018922195425 ) ) ;
#4174 = CARTESIAN_POINT ( 'NONE',  ( -6.972266317189433020E-16, -66.12499999726881583, -5.000000000000000000 ) ) ;
#4175 = CARTESIAN_POINT ( 'NONE',  ( -5.000000000000000000, 27.12500000273118772, 0.000000000000000000 ) ) ;
#4176 = ORIENTED_EDGE ( 'NONE', *, *, #46858, .F. ) ;
#4177 = CARTESIAN_POINT ( 'NONE',  ( 5.000000000000000000, 6.583333333333333037, -2.886751345948130876 ) ) ;
#4178 = CARTESIAN_POINT ( 'NONE',  ( -6.972266317189433020E-16, 20.74999999999999645, -5.000000000000000000 ) ) ;
#4179 = CARTESIAN_POINT ( 'NONE',  ( 5.000000000000000888, -11.58333333333333570, 2.886751345948126879 ) ) ;
#4180 = CARTESIAN_POINT ( 'NONE',  ( 2.229367062500001939, -14.97916666530107399, 3.861377020970579999 ) ) ;
#4181 = VECTOR ( 'NONE', #37085, 1000.000000000000000 ) ;
#4182 = CARTESIAN_POINT ( 'NONE',  ( 2.229367062499998831, -76.64583333196773651, -3.861377020970580887 ) ) ;
#4183 = CARTESIAN_POINT ( 'NONE',  ( 2.730187237215162345E-16, -166.4375000013655779, -4.458734124999999437 ) ) ;
#4184 = CARTESIAN_POINT ( 'NONE',  ( -5.000000000000000000, -17.95833333060214798, -2.886751345948128211 ) ) ;
#4186 = VERTEX_POINT ( 'NONE', #38565 ) ;
#4185 = CARTESIAN_POINT ( 'NONE',  ( 4.458734124999998549, -44.72916666530106511, -2.574251347313721627 ) ) ;
#4187 = LINE ( 'NONE', #19596, #44621 ) ;
#4189 = ORIENTED_EDGE ( 'NONE', *, *, #46406, .F. ) ;
#4188 = CARTESIAN_POINT ( 'NONE',  ( 4.458734124999999437, 7.937500001365595637, -5.460374474430324690E-16 ) ) ;
#4190 =( BOUNDED_CURVE ( )  B_SPLINE_CURVE ( 2, ( #42932, #33286, #52905, #27508, #13972, #48069, #53219, #9151, #28763 ),
 .UNSPECIFIED., .F., .F. ) 
 B_SPLINE_CURVE_WITH_KNOTS ( ( 3, 2, 2, 2, 3 ),
 ( 0.5083333333333337478, 0.5125000000000003997, 0.5166666666666671626, 0.5208333333333338144, 0.5250000000000004663 ),
 .UNSPECIFIED. ) 
 CURVE ( )  GEOMETRIC_REPRESENTATION_ITEM ( )  RATIONAL_B_SPLINE_CURVE ( ( 0.9999999999999918954, 0.9238795325112948431, 1.000000000000000000, 0.9238795325112867385, 1.000000000000000000, 0.9238795325112867385, 1.000000000000000000, 0.9238795325112786339, 1.000000000000008216 ) ) 
 REPRESENTATION_ITEM ( '' )  );
#4191 = CARTESIAN_POINT ( 'NONE',  ( -52.10840900171896806, -153.1875000013656063, 3.393966926194110556 ) ) ;
#4192 = CARTESIAN_POINT ( 'NONE',  ( -5.000000000000000000, -62.08333333333332860, -2.886751345948128211 ) ) ;
#4193 = CARTESIAN_POINT ( 'NONE',  ( 1.846868145590736310, -154.8750000013655779, 4.458734124999999437 ) ) ;
#4194 = CARTESIAN_POINT ( 'NONE',  ( -2.229367062499996610, -40.39583333196773651, 3.861377020970582219 ) ) ;
#4195 = CARTESIAN_POINT ( 'NONE',  ( -4.999999999999998224, -78.91666666666665719, 2.886751345948131764 ) ) ;
#4196 = CARTESIAN_POINT ( 'NONE',  ( -5.000000000000000000, -163.5000000000000000, -6.123233995736766282E-16 ) ) ;
#4197 = CARTESIAN_POINT ( 'NONE',  ( 1.975475456537005874E-15, 5.375000002731185944, 5.000000000000000000 ) ) ;
#4198 = CARTESIAN_POINT ( 'NONE',  ( -59.44456063193725015, -125.8125000013655921, -0.3552334253322034230 ) ) ;
#4199 = CARTESIAN_POINT ( 'NONE',  ( -4.458734124999998549, -8.479166665301073991, 2.574251347313722516 ) ) ;
#4200 = CARTESIAN_POINT ( 'NONE',  ( -2.229367062499996610, -41.39583333196773651, 3.861377020970582219 ) ) ;
#4201 = CARTESIAN_POINT ( 'NONE',  ( 1.975475456537005874E-15, -26.74999999999999645, 5.000000000000000000 ) ) ;
#4202 = CARTESIAN_POINT ( 'NONE',  ( -4.458734124999999437, -148.9375000013656063, -5.460374474430324690E-16 ) ) ;
#4203 = CARTESIAN_POINT ( 'NONE',  ( -3.152548672688508926E-16, -89.81249999863439371, -5.148502694627439702 ) ) ;
#4204 = DIRECTION ( 'NONE',  ( -0.6485228581062915110, 0.000000000000000000, -0.7611951803011149931 ) ) ;
#4205 = ORIENTED_EDGE ( 'NONE', *, *, #4017, .F. ) ;
#4206 = LINE ( 'NONE', #29253, #60123 ) ;
#4207 = CARTESIAN_POINT ( 'NONE',  ( -54.60164318462004474, -150.5000000027312126, -4.984105922594373794 ) ) ;
#4208 =( BOUNDED_CURVE ( )  B_SPLINE_CURVE ( 2, ( #32220, #57004, #37682, #42504, #2977, #22594, #56691, #61833, #42191 ),
 .UNSPECIFIED., .F., .F. ) 
 B_SPLINE_CURVE_WITH_KNOTS ( ( 3, 2, 2, 2, 3 ),
 ( 0.8104166666666666741, 0.8111111111111111160, 0.8125000000000000000, 0.8138888888888888840, 0.8145833333333333259 ),
 .UNSPECIFIED. ) 
 CURVE ( )  GEOMETRIC_REPRESENTATION_ITEM ( )  RATIONAL_B_SPLINE_CURVE ( ( 0.9330127018922194093, 0.9330127018922194093, 1.000000000000000000, 0.8660254037844387076, 1.000000000000000000, 0.8660254037844387076, 1.000000000000000000, 0.9330127018922194093, 0.9330127018922194093 ) ) 
 REPRESENTATION_ITEM ( '' )  );
#4209 = CARTESIAN_POINT ( 'NONE',  ( 1.975475456537005874E-15, -104.7500000000000000, 5.000000000000000000 ) ) ;
#4211 = EDGE_CURVE ( 'NONE', #8687, #17322, #47553, .T. ) ;
#4210 = CARTESIAN_POINT ( 'NONE',  ( -2.229367062499996610, -76.39583333196773651, 3.861377020970582219 ) ) ;
#4212 = ORIENTED_EDGE ( 'NONE', *, *, #58230, .T. ) ;
#4213 = CARTESIAN_POINT ( 'NONE',  ( -5.000000000000000000, -14.08333333333333037, -2.886751345948128211 ) ) ;
#4214 = CARTESIAN_POINT ( 'NONE',  ( -3.152548672688508926E-16, -9.812499998634406140, -5.148502694627439702 ) ) ;
#4215 = CARTESIAN_POINT ( 'NONE',  ( 2.500000000000002220, -79.54166666393547303, 4.330127018922192761 ) ) ;
#4216 = CARTESIAN_POINT ( 'NONE',  ( 4.458734125000001214, -2.895833331967738289, 2.574251347313718519 ) ) ;
#4217 = CARTESIAN_POINT ( 'NONE',  ( -5.000000000000000000, -43.00000000000000000, 0.000000000000000000 ) ) ;
#4218 = CARTESIAN_POINT ( 'NONE',  ( -8.190561711645485556E-16, -152.6875000013656063, 4.458734124999999437 ) ) ;
#4219 = CARTESIAN_POINT ( 'NONE',  ( 2.229367062500001939, 18.77083333469892779, 3.861377020970579999 ) ) ;
#4220 = EDGE_LOOP ( 'NONE', ( #33309, #40510, #36918, #37503 ) ) ;
#4221 = CARTESIAN_POINT ( 'NONE',  ( -2.229367062499996610, -93.14583333196773651, 3.861377020970582219 ) ) ;
#4222 = DIRECTION ( 'NONE',  ( -0.000000000000000000, 1.000000000000000000, -0.000000000000000000 ) ) ;
#4223 = LINE ( 'NONE', #9039, #45216 ) ;
#4224 = CARTESIAN_POINT ( 'NONE',  ( 4.458734124999998549, -11.72916666530107044, -2.574251347313721627 ) ) ;
#4225 = VECTOR ( 'NONE', #31624, 1000.000000000000000 ) ;
#4226 = LINE ( 'NONE', #49225, #63324 ) ;
#4227 = CARTESIAN_POINT ( 'NONE',  ( -50.40829686548195099, -154.0000000013655779, -1.485763867205728284 ) ) ;
#4228 = CARTESIAN_POINT ( 'NONE',  ( -3.535250795749689387E-16, -43.12499999726880162, -5.773502691896257311 ) ) ;
#4229 = CARTESIAN_POINT ( 'NONE',  ( 2.229367062499998831, 17.35416666803225993, -3.861377020970580887 ) ) ;
#4230 = CARTESIAN_POINT ( 'NONE',  ( 5.000000000000000888, -46.45833333060214443, 2.886751345948126879 ) ) ;
#4231 = CARTESIAN_POINT ( 'NONE',  ( 2.229367062500001939, 17.02083333469892779, 3.861377020970579999 ) ) ;
#4232 = CARTESIAN_POINT ( 'NONE',  ( 2.229367062499998831, -57.64583333196773651, -3.861377020970580887 ) ) ;
#4233 = CARTESIAN_POINT ( 'NONE',  ( -4.458734124999999437, -6.562499998634403475, 0.000000000000000000 ) ) ;
#4234 = PLANE ( 'NONE',  #54494 ) ;
#4235 = CARTESIAN_POINT ( 'NONE',  ( -5.000000000000000000, 8.000000000000000000, 0.000000000000000000 ) ) ;
#4236 = CARTESIAN_POINT ( 'NONE',  ( 5.000000000000000000, -139.1875000027312126, 2.071067811865478614 ) ) ;
#4237 = CARTESIAN_POINT ( 'NONE',  ( -56.66612745406288099, -142.3125000000000000, -5.149110718188529390 ) ) ;
#4238 = CARTESIAN_POINT ( 'NONE',  ( -2.229367062500000163, -51.47916666530107221, -3.861377020970580443 ) ) ;
#4239 = CARTESIAN_POINT ( 'NONE',  ( -4.999999999999999112, -82.79166666393547303, 2.886751345948131764 ) ) ;
#4240 = CARTESIAN_POINT ( 'NONE',  ( -52.10840900171896806, -137.4375000013656063, 3.393966926194110556 ) ) ;
#4241 = CARTESIAN_POINT ( 'NONE',  ( -6.972266317189433020E-16, -87.25000000000001421, -5.000000000000000000 ) ) ;
#4242 = CARTESIAN_POINT ( 'NONE',  ( 6.123233995736766282E-16, -170.0000000000000000, -5.000000000000000000 ) ) ;
#4243 = CARTESIAN_POINT ( 'NONE',  ( -3.152548672688508926E-16, -90.81249999863440792, -5.148502694627439702 ) ) ;
#4244 = CARTESIAN_POINT ( 'NONE',  ( 4.458734124999999437, -153.6875000013656063, 0.000000000000000000 ) ) ;
#4245 = CARTESIAN_POINT ( 'NONE',  ( 5.000000000000000888, -36.58333333333332149, 2.886751345948126879 ) ) ;
#4246 = CARTESIAN_POINT ( 'NONE',  ( -2.499999999999996447, -19.70833333060214798, 4.330127018922195425 ) ) ;
#4247 = LINE ( 'NONE', #34777, #3773 ) ;
#4248 = VERTEX_POINT ( 'NONE', #38880 ) ;
#4249 = CARTESIAN_POINT ( 'NONE',  ( 2.229367062499998831, -93.64583333196772230, -3.861377020970580887 ) ) ;
#4250 = CARTESIAN_POINT ( 'NONE',  ( 2.229367062500001939, 9.770833334698927786, 3.861377020970579999 ) ) ;
#4251 = CARTESIAN_POINT ( 'NONE',  ( 2.500000000000002220, 13.45833333606451987, 4.330127018922192761 ) ) ;
#4252 = LINE ( 'NONE', #33520, #41171 ) ;
#4253 = CARTESIAN_POINT ( 'NONE',  ( 2.499999999999998668, 0.6666666666666660745, -4.330127018922193649 ) ) ;
#4254 = CARTESIAN_POINT ( 'NONE',  ( -2.229367062500000163, -59.47916666530106511, -3.861377020970580443 ) ) ;
#4255 = CARTESIAN_POINT ( 'NONE',  ( -1.339745962155640457, 3.205341801261477830, 4.999999999999984901 ) ) ;
#4256 = CARTESIAN_POINT ( 'NONE',  ( 1.060575238724906964E-15, 0.3750000027311871098, 5.773502691896257311 ) ) ;
#4257 = CARTESIAN_POINT ( 'NONE',  ( -3.152548672688508926E-16, -26.56249999863440792, -5.148502694627439702 ) ) ;
#4258 = CARTESIAN_POINT ( 'NONE',  ( 5.000000000000000888, -153.0625000027311842, -2.071067811865475505 ) ) ;
#4259 = CARTESIAN_POINT ( 'NONE',  ( 0.000000000000000000, 0.000000000000000000, -9.974600000000000577 ) ) ;
#4260 = CARTESIAN_POINT ( 'NONE',  ( 5.000000000000000888, -45.58333333333333570, 2.886751345948126879 ) ) ;
#4262 = CARTESIAN_POINT ( 'NONE',  ( 9.457646018065525792E-16, -23.31249999863440436, 5.148502694627439702 ) ) ;
#4261 = CARTESIAN_POINT ( 'NONE',  ( -6.972266317189433020E-16, 6.875000002731185944, -5.000000000000000000 ) ) ;
#4263 = CARTESIAN_POINT ( 'NONE',  ( -2.499999999999996447, 22.29166666939785202, 4.330127018922195425 ) ) ;
#4264 = CARTESIAN_POINT ( 'NONE',  ( 4.458734124999999437, -70.81249999863439371, -5.460374474430324690E-16 ) ) ;
#4265 = CARTESIAN_POINT ( 'NONE',  ( -4.458734125000000326, -146.2500000013656063, -1.846868145590735644 ) ) ;
#4266 = AXIS2_PLACEMENT_3D ( 'NONE', #61233, #17156, #22307 ) ;
#4267 = CARTESIAN_POINT ( 'NONE',  ( 2.229367062499998831, -74.64583333196773651, -3.861377020970580887 ) ) ;
#4268 = CARTESIAN_POINT ( 'NONE',  ( -52.80376928212989185, -144.1250000013656063, -4.297418129356379346 ) ) ;
#4269 = CARTESIAN_POINT ( 'NONE',  ( -4.458734124999998549, -24.47916666530107577, 2.574251347313722516 ) ) ;
#4270 = CARTESIAN_POINT ( 'NONE',  ( -4.999999999999999112, -64.79166666393547303, 2.886751345948131764 ) ) ;
#4271 = VERTEX_POINT ( 'NONE', #14437 ) ;
#4272 = CARTESIAN_POINT ( 'NONE',  ( -5.000000000000000000, -22.00000000000000000, 0.000000000000000000 ) ) ;
#4273 = EDGE_LOOP ( 'NONE', ( #27067, #46203, #5073, #44052 ) ) ;
#4274 = CARTESIAN_POINT ( 'NONE',  ( -4.458734124999999437, -69.56249999863439371, 0.000000000000000000 ) ) ;
#4275 = SURFACE_SIDE_STYLE ('',( #38986 ) ) ;
#4276 = ORIENTED_EDGE ( 'NONE', *, *, #50870, .F. ) ;
#4277 = DIRECTION ( 'NONE',  ( 0.000000000000000000, 1.000000000000000000, 0.000000000000000000 ) ) ;
#4279 = EDGE_CURVE ( 'NONE', #42594, #6575, #53054, .T. ) ;
#4278 = CARTESIAN_POINT ( 'NONE',  ( -2.229367062500000163, -60.72916666530106511, -3.861377020970580443 ) ) ;
#4280 = CARTESIAN_POINT ( 'NONE',  ( -4.458734124999999437, -0.6458333319677399542, -2.574251347313719407 ) ) ;
#4281 = ORIENTED_EDGE ( 'NONE', *, *, #45553, .F. ) ;
#4282 =( BOUNDED_CURVE ( )  B_SPLINE_CURVE ( 2, ( #21909, #41506, #35428, #23169, #42152, #27674, #27049, #32823, #13201 ),
 .UNSPECIFIED., .F., .F. ) 
 B_SPLINE_CURVE_WITH_KNOTS ( ( 3, 2, 2, 2, 3 ),
 ( 0.7946428571428570953, 0.7952380952380951884, 0.7964285714285713746, 0.7976190476190476719, 0.7982142857142857650 ),
 .UNSPECIFIED. ) 
 CURVE ( )  GEOMETRIC_REPRESENTATION_ITEM ( )  RATIONAL_B_SPLINE_CURVE ( ( 0.9330127018922194093, 0.9330127018922194093, 1.000000000000000000, 0.8660254037844387076, 1.000000000000000000, 0.8660254037844387076, 1.000000000000000000, 0.9330127018922194093, 0.9330127018922194093 ) ) 
 REPRESENTATION_ITEM ( '' )  );
#4283 = LINE ( 'NONE', #9725, #17313 ) ;
#4284 = CARTESIAN_POINT ( 'NONE',  ( -4.458734124999999437, 16.68750000136559564, 0.000000000000000000 ) ) ;
#4285 = CARTESIAN_POINT ( 'NONE',  ( -57.19623071787017210, -146.3750000013655779, 4.297418129356382899 ) ) ;
#4286 = CARTESIAN_POINT ( 'NONE',  ( 1.339745962155615144, 16.29465819873851729, 4.999999999999999112 ) ) ;
#4287 = CARTESIAN_POINT ( 'NONE',  ( -3.152801135295367096, -164.0625000013656063, -3.152801135295367541 ) ) ;
#4288 = ORIENTED_EDGE ( 'NONE', *, *, #9399, .F. ) ;
#4289 = CARTESIAN_POINT ( 'NONE',  ( -2.229367062499996610, -75.14583333196773651, 3.861377020970582219 ) ) ;
#4290 = ADVANCED_FACE ( 'NONE', ( #24734 ), #34369, .T. ) ;
#4291 = CARTESIAN_POINT ( 'NONE',  ( -4.458734124999999437, 6.687500001365593860, 0.000000000000000000 ) ) ;
#4292 =( BOUNDED_CURVE ( )  B_SPLINE_CURVE ( 2, ( #59380, #14035, #53282, #53908, #54557, #19174, #10480, #48758, #10167 ),
 .UNSPECIFIED., .F., .F. ) 
 B_SPLINE_CURVE_WITH_KNOTS ( ( 3, 2, 2, 2, 3 ),
 ( 0.8625000000000000444, 0.8630952380952381375, 0.8642857142857143238, 0.8654761904761905100, 0.8660714285714286031 ),
 .UNSPECIFIED. ) 
 CURVE ( )  GEOMETRIC_REPRESENTATION_ITEM ( )  RATIONAL_B_SPLINE_CURVE ( ( 0.9330127018922194093, 0.9330127018922194093, 1.000000000000000000, 0.8660254037844387076, 1.000000000000000000, 0.8660254037844387076, 1.000000000000000000, 0.9330127018922194093, 0.9330127018922194093 ) ) 
 REPRESENTATION_ITEM ( '' )  );
#4293 = DIRECTION ( 'NONE',  ( -0.000000000000000000, 1.000000000000000000, -0.000000000000000000 ) ) ;
#4294 = CARTESIAN_POINT ( 'NONE',  ( 4.458734125000001214, -66.14583333196772230, 2.574251347313718519 ) ) ;
#4295 = CARTESIAN_POINT ( 'NONE',  ( 5.000000000000000000, -18.37499999726881583, -6.123233995736766282E-16 ) ) ;
#4296 = EDGE_CURVE ( 'NONE', #61790, #9668, #31966, .T. ) ;
#4297 = CARTESIAN_POINT ( 'NONE',  ( -50.01589407740564042, -142.7500000027312126, 0.3983568153799778022 ) ) ;
#4298 = FACE_OUTER_BOUND ( 'NONE', #20781, .T. ) ;
#4299 = FACE_OUTER_BOUND ( 'NONE', #41758, .T. ) ;
#4300 = CARTESIAN_POINT ( 'NONE',  ( -2.071067811865622943, -156.6875000000000000, -4.999999999999850786 ) ) ;
#4301 = CARTESIAN_POINT ( 'NONE',  ( -2.229367062500000163, -42.47916666530107932, -3.861377020970580443 ) ) ;
#4302 = CARTESIAN_POINT ( 'NONE',  ( -4.458734124999999437, -29.56249999863440436, 0.000000000000000000 ) ) ;
#4303 = CYLINDRICAL_SURFACE ( 'NONE', #56576, 5.000000000000000000 ) ;
#4304 = CARTESIAN_POINT ( 'NONE',  ( 5.000000000000000000, 23.50000000000000000, -6.123233995736766282E-16 ) ) ;
#4305 = CARTESIAN_POINT ( 'NONE',  ( -5.000000000000000000, -150.6250000027312126, -6.123233995736766282E-16 ) ) ;
#4306 = CARTESIAN_POINT ( 'NONE',  ( -2.229367062500000163, -107.7291666653010651, -3.861377020970580443 ) ) ;
#4307 = CARTESIAN_POINT ( 'NONE',  ( -4.458734124999999437, -37.39583333196773651, -2.574251347313719407 ) ) ;
#4308 = CARTESIAN_POINT ( 'NONE',  ( 2.499999999999998668, -68.20833333060214443, -4.330127018922193649 ) ) ;
#4309 = CARTESIAN_POINT ( 'NONE',  ( -59.29741812935640155, -146.8750000013656063, -2.196230717870135685 ) ) ;
#4310 = CARTESIAN_POINT ( 'NONE',  ( -3.535533905932737309, -141.6250000000000000, -3.535533905932738197 ) ) ;
#4311 = CARTESIAN_POINT ( 'NONE',  ( -3.152548672688508926E-16, -72.81249999863439371, -5.148502694627439702 ) ) ;
#4312 = CARTESIAN_POINT ( 'NONE',  ( 3.152801135295366208, -168.8125000013656063, 3.152801135295367985 ) ) ;
#4313 = CARTESIAN_POINT ( 'NONE',  ( -4.458734124999999437, -29.39583333196773296, -2.574251347313719407 ) ) ;
#4314 = CARTESIAN_POINT ( 'NONE',  ( 6.123233995736766282E-16, -170.0000000000000000, -5.000000000000000000 ) ) ;
#4315 = CARTESIAN_POINT ( 'NONE',  ( 5.000000000000000000, -45.29166666393547303, -2.886751345948130876 ) ) ;
#4316 = CARTESIAN_POINT ( 'NONE',  ( -5.000000000000000000, -20.99999999999999645, 0.000000000000000000 ) ) ;
#4317 = CARTESIAN_POINT ( 'NONE',  ( -4.458734124999999437, -144.9375000013656063, -5.460374474430324690E-16 ) ) ;
#4318 = EDGE_LOOP ( 'NONE', ( #52133, #40142, #37149, #20318 ) ) ;
#4319 = CARTESIAN_POINT ( 'NONE',  ( 4.458734124999999437, 28.93750000136559208, -5.460374474430324690E-16 ) ) ;
#4320 = CARTESIAN_POINT ( 'NONE',  ( -6.972266317189433020E-16, -16.12499999726881228, -5.000000000000000000 ) ) ;
#4321 = CARTESIAN_POINT ( 'NONE',  ( -4.458734124999999437, -58.56249999863440081, 0.000000000000000000 ) ) ;
#4322 = FACE_OUTER_BOUND ( 'NONE', #21709, .T. ) ;
#4323 = CARTESIAN_POINT ( 'NONE',  ( -5.000000000000000000, -110.8749999972688016, 0.000000000000000000 ) ) ;
#4324 = CARTESIAN_POINT ( 'NONE',  ( -4.999999999999999112, 18.08333333333333570, 2.886751345948131764 ) ) ;
#4325 = DIRECTION ( 'NONE',  ( 0.8660254037844385966, 0.000000000000000000, 0.4999999999999999445 ) ) ;
#4326 = CARTESIAN_POINT ( 'NONE',  ( -3.152548672688508926E-16, -6.562499998634404363, -5.148502694627439702 ) ) ;
#4327 = CARTESIAN_POINT ( 'NONE',  ( -6.972266317189433020E-16, 3.875000002731185500, -5.000000000000000000 ) ) ;
#4328 = ADVANCED_FACE ( 'NONE', ( #29223 ), #33749, .T. ) ;
#4329 = CARTESIAN_POINT ( 'NONE',  ( -2.499999999999996447, -8.833333333333332149, 4.330127018922195425 ) ) ;
#4330 = CARTESIAN_POINT ( 'NONE',  ( 2.229367062500001939, 12.77083333469892779, 3.861377020970579999 ) ) ;
#4331 = CARTESIAN_POINT ( 'NONE',  ( -2.499999999999996447, -87.70833333060214443, 4.330127018922195425 ) ) ;
#4332 = CARTESIAN_POINT ( 'NONE',  ( 1.975475456537005874E-15, 0.2500000000000001665, 5.000000000000000000 ) ) ;
#4333 = CARTESIAN_POINT ( 'NONE',  ( -2.229367062499996610, -55.14583333196773651, 3.861377020970582219 ) ) ;
#4334 = CARTESIAN_POINT ( 'NONE',  ( -8.190561711645485556E-16, -158.9375000013655779, 4.458734124999999437 ) ) ;
#4335 = CARTESIAN_POINT ( 'NONE',  ( -2.499999999999996447, -52.70833333060213732, 4.330127018922195425 ) ) ;
#4336 = ORIENTED_EDGE ( 'NONE', *, *, #30666, .F. ) ;
#4337 = CARTESIAN_POINT ( 'NONE',  ( 4.458734125000001214, 4.854166668032262599, 2.574251347313718519 ) ) ;
#4338 = ORIENTED_EDGE ( 'NONE', *, *, #22028, .T. ) ;
#4340 = DIRECTION ( 'NONE',  ( -0.000000000000000000, 1.000000000000000000, -0.000000000000000000 ) ) ;
#4339 = CYLINDRICAL_SURFACE ( 'NONE', #40947, 5.000000000000000000 ) ;
#4341 = CARTESIAN_POINT ( 'NONE',  ( -4.458734124999999437, -158.9375000013655779, -5.460374474430324690E-16 ) ) ;
#4342 = ORIENTED_EDGE ( 'NONE', *, *, #36617, .T. ) ;
#4343 =( BOUNDED_CURVE ( )  B_SPLINE_CURVE ( 2, ( #33941, #24287, #39075, #58703, #29408, #49041, #4986, #24609, #35860 ),
 .UNSPECIFIED., .F., .F. ) 
 B_SPLINE_CURVE_WITH_KNOTS ( ( 3, 2, 2, 2, 3 ),
 ( 0.9303571428571428825, 0.9309523809523809756, 0.9321428571428571619, 0.9333333333333333481, 0.9339285714285714413 ),
 .UNSPECIFIED. ) 
 CURVE ( )  GEOMETRIC_REPRESENTATION_ITEM ( )  RATIONAL_B_SPLINE_CURVE ( ( 0.9330127018922194093, 0.9330127018922194093, 1.000000000000000000, 0.8660254037844387076, 1.000000000000000000, 0.8660254037844387076, 1.000000000000000000, 0.9330127018922194093, 0.9330127018922194093 ) ) 
 REPRESENTATION_ITEM ( '' )  );
#4344 = CARTESIAN_POINT ( 'NONE',  ( -53.33387254593733928, -131.8125000000000284, 5.149110718188519620 ) ) ;
#4345 = CARTESIAN_POINT ( 'NONE',  ( 1.339745962155615144, -47.58034179853029144, 4.999999999999999112 ) ) ;
#4346 = CARTESIAN_POINT ( 'NONE',  ( 4.458734125000001214, -38.14583333196773651, 2.574251347313718519 ) ) ;
#4347 = EDGE_LOOP ( 'NONE', ( #43672, #54574, #61495, #61330, #10180, #1892, #43428 ) ) ;
#4348 = EDGE_CURVE ( 'NONE', #55556, #52254, #44659, .T. ) ;
#4349 = EDGE_CURVE ( 'NONE', #40158, #8193, #15408, .T. ) ;
#4350 = FACE_OUTER_BOUND ( 'NONE', #34825, .T. ) ;
#4351 = CARTESIAN_POINT ( 'NONE',  ( -3.152548672688508926E-16, 21.43750000136559564, -5.148502694627439702 ) ) ;
#4352 = CARTESIAN_POINT ( 'NONE',  ( 5.000000000000000000, -59.41666666666665719, -2.886751345948130876 ) ) ;
#4353 = ORIENTED_EDGE ( 'NONE', *, *, #25660, .T. ) ;
#4354 = CARTESIAN_POINT ( 'NONE',  ( -4.458734124999999437, -85.56249999863439371, 0.000000000000000000 ) ) ;
#4355 = CARTESIAN_POINT ( 'NONE',  ( -54.60164318462004474, -128.5000000027312126, -4.984105922594373794 ) ) ;
#4356 = CARTESIAN_POINT ( 'NONE',  ( 5.000000000000000000, -4.374999997268816720, -6.123233995736766282E-16 ) ) ;
#4357 = CARTESIAN_POINT ( 'NONE',  ( -6.972266317189433020E-16, -26.25000000000000355, -5.000000000000000000 ) ) ;
#4358 = CARTESIAN_POINT ( 'NONE',  ( 5.000000000000000000, -52.37499999726881583, -6.123233995736766282E-16 ) ) ;
#4359 = CARTESIAN_POINT ( 'NONE',  ( 4.458734125000000326, -61.89583333196774362, 2.574251347313718519 ) ) ;
#4360 = CARTESIAN_POINT ( 'NONE',  ( 5.275681513340003914E-14, 9.875000002731184168, -5.000000000000000000 ) ) ;
#4361 = CARTESIAN_POINT ( 'NONE',  ( 2.229367062499998831, 22.35416666803225993, -3.861377020970580887 ) ) ;
#4362 = EDGE_CURVE ( 'NONE', #12432, #1054, #9300, .T. ) ;
#4363 = CARTESIAN_POINT ( 'NONE',  ( 2.499999999999998668, -102.2083333306021444, -4.330127018922193649 ) ) ;
#4364 = DIRECTION ( 'NONE',  ( 0.000000000000000000, 1.000000000000000000, 0.000000000000000000 ) ) ;
#4365 = CARTESIAN_POINT ( 'NONE',  ( -4.458734124999999437, -46.56249999863440792, 0.000000000000000000 ) ) ;
#4366 = CARTESIAN_POINT ( 'NONE',  ( -4.999999999999999112, -1.791666663935480353, 2.886751345948131764 ) ) ;
#4367 = CARTESIAN_POINT ( 'NONE',  ( -1.339745962155617365, 25.20534180126147916, 4.999999999999998224 ) ) ;
#4368 = ADVANCED_FACE ( 'NONE', ( #10568 ), #5753, .F. ) ;
#4369 = DIRECTION ( 'NONE',  ( -0.000000000000000000, 1.000000000000000000, -0.000000000000000000 ) ) ;
#4370 = CARTESIAN_POINT ( 'NONE',  ( 4.458734124999999437, -85.06249999863439371, -5.460374474430324690E-16 ) ) ;
#4371 = CARTESIAN_POINT ( 'NONE',  ( 6.123233995736766282E-16, -120.0000000000000000, -5.000000000000000000 ) ) ;
#4372 =( BOUNDED_CURVE ( )  B_SPLINE_CURVE ( 2, ( #32527, #42177, #2638, #37359, #60071, #30461, #260, #9886, #20830 ),
 .UNSPECIFIED., .F., .F. ) 
 B_SPLINE_CURVE_WITH_KNOTS ( ( 3, 2, 2, 2, 3 ),
 ( 0.1875000000000000000, 0.1880952380952380931, 0.1892857142857142794, 0.1904761904761904656, 0.1910714285714285865 ),
 .UNSPECIFIED. ) 
 CURVE ( )  GEOMETRIC_REPRESENTATION_ITEM ( )  RATIONAL_B_SPLINE_CURVE ( ( 0.9330127018922194093, 0.9330127018922194093, 1.000000000000000000, 0.8660254037844387076, 1.000000000000000000, 0.8660254037844387076, 1.000000000000000000, 0.9330127018922178550, 0.9330127018922194093 ) ) 
 REPRESENTATION_ITEM ( '' )  );
#4373 = CARTESIAN_POINT ( 'NONE',  ( -3.152548672688508926E-16, -12.81249999863440259, -5.148502694627439702 ) ) ;
#4374 = ORIENTED_EDGE ( 'NONE', *, *, #21746, .T. ) ;
#4375 = CARTESIAN_POINT ( 'NONE',  ( -4.458734124999998549, -98.22916666530105090, 2.574251347313722516 ) ) ;
#4376 = CARTESIAN_POINT ( 'NONE',  ( -5.000000000000000000, -162.6250000027311842, -6.123233995736766282E-16 ) ) ;
#4377 = CARTESIAN_POINT ( 'NONE',  ( 4.458734124999998549, -89.97916666530105090, -2.574251347313721627 ) ) ;
#4378 = CARTESIAN_POINT ( 'NONE',  ( -5.000000000000000000, -52.95833333060214443, -2.886751345948128211 ) ) ;
#4379 = CARTESIAN_POINT ( 'NONE',  ( -4.999999999999998224, -36.79166666393548013, 2.886751345948131764 ) ) ;
#4380 = CARTESIAN_POINT ( 'NONE',  ( -59.44456063193725015, -129.5625000013656063, -0.3552334253322034230 ) ) ;
#4381 = CARTESIAN_POINT ( 'NONE',  ( -50.40829686548195099, -147.0000000013656063, -1.485763867205728284 ) ) ;
#4382 = CARTESIAN_POINT ( 'NONE',  ( -4.458734124999999437, -19.39583333196774007, -2.574251347313719407 ) ) ;
#4383 = CARTESIAN_POINT ( 'NONE',  ( 4.458734125000001214, 8.854166668032261711, 2.574251347313718519 ) ) ;
#4384 = CARTESIAN_POINT ( 'NONE',  ( 2.229367062499998831, -58.89583333196773651, -3.861377020970580887 ) ) ;
#4385 = CARTESIAN_POINT ( 'NONE',  ( -6.972266317189433020E-16, -20.24999999999999289, -5.000000000000000000 ) ) ;
#4386 = CARTESIAN_POINT ( 'NONE',  ( -4.458734124999999437, -14.31249999863440436, 0.000000000000000000 ) ) ;
#4387 = CARTESIAN_POINT ( 'NONE',  ( -6.972266317189433020E-16, -71.25000000000000000, -5.000000000000000000 ) ) ;
#4388 = CARTESIAN_POINT ( 'NONE',  ( 3.535533905932738197, -153.8750000000000000, -3.535533905932738197 ) ) ;
#4389 = ORIENTED_EDGE ( 'NONE', *, *, #22773, .T. ) ;
#4390 = CARTESIAN_POINT ( 'NONE',  ( -2.229367062499996610, -38.39583333196773651, 3.861377020970582219 ) ) ;
#4391 = CARTESIAN_POINT ( 'NONE',  ( -56.48576386720575471, -126.0000000013656063, -4.591703134518078322 ) ) ;
#4392 = CARTESIAN_POINT ( 'NONE',  ( -1.339745962155610925, -8.794658198738519062, 5.000000000000000000 ) ) ;
#4393 = CARTESIAN_POINT ( 'NONE',  ( -4.999999999999998224, 27.20833333606451276, 2.886751345948131764 ) ) ;
#4394 = CARTESIAN_POINT ( 'NONE',  ( 4.458734124999999437, -86.81249999863439371, -5.460374474430324690E-16 ) ) ;
#4395 = CARTESIAN_POINT ( 'NONE',  ( -4.458734124999998549, 17.52083333469892779, 2.574251347313722516 ) ) ;
#4396 = CARTESIAN_POINT ( 'NONE',  ( -2.229367062499996610, 9.854166668032261711, 3.861377020970582219 ) ) ;
#4397 = DIRECTION ( 'NONE',  ( -0.000000000000000000, 1.000000000000000000, -0.000000000000000000 ) ) ;
#4398 = CARTESIAN_POINT ( 'NONE',  ( -2.499999999999996447, 12.16666666666666607, 4.330127018922195425 ) ) ;
#4399 = CARTESIAN_POINT ( 'NONE',  ( -4.458734124999999437, -87.56249999863439371, 0.000000000000000000 ) ) ;
#4400 = CARTESIAN_POINT ( 'NONE',  ( 5.000000000000000000, -70.50000000000000000, -6.123233995736766282E-16 ) ) ;
#4401 = CARTESIAN_POINT ( 'NONE',  ( 5.000000000000000888, 12.54166666939785202, 2.886751345948126879 ) ) ;
#4402 = ORIENTED_EDGE ( 'NONE', *, *, #62174, .F. ) ;
#4403 = ORIENTED_EDGE ( 'NONE', *, *, #35438, .F. ) ;
#4404 = CARTESIAN_POINT ( 'NONE',  ( -5.000000000000000000, -90.00000000000000000, 0.000000000000000000 ) ) ;
#4406 = CARTESIAN_POINT ( 'NONE',  ( 2.500000000000002220, -30.66666666666666785, 4.330127018922192761 ) ) ;
#4405 = CARTESIAN_POINT ( 'NONE',  ( 1.339745962155612702, -85.29465819873851729, -5.000000000000000000 ) ) ;
#4407 = CARTESIAN_POINT ( 'NONE',  ( 2.229367062500001939, -33.97916666530107221, 3.861377020970579999 ) ) ;
#4408 = CARTESIAN_POINT ( 'NONE',  ( 5.000000000000000000, -35.37499999726881583, -6.123233995736766282E-16 ) ) ;
#4410 = VERTEX_POINT ( 'NONE', #35985 ) ;
#4409 = CARTESIAN_POINT ( 'NONE',  ( -2.229367062500000163, -66.47916666530106511, -3.861377020970580443 ) ) ;
#4411 = CARTESIAN_POINT ( 'NONE',  ( -57.89159099828107458, -149.9375000013656063, -3.393966926194107447 ) ) ;
#4412 = CARTESIAN_POINT ( 'NONE',  ( -3.152548672688508926E-16, -11.56249999863440792, -5.148502694627439702 ) ) ;
#4414 = ORIENTED_EDGE ( 'NONE', *, *, #12655, .F. ) ;
#4413 = CARTESIAN_POINT ( 'NONE',  ( 2.229367062499998831, -15.89583333196773651, -3.861377020970580887 ) ) ;
#4415 = CARTESIAN_POINT ( 'NONE',  ( -4.999999999999999112, -77.91666666666665719, 2.886751345948131764 ) ) ;
#4416 = DIRECTION ( 'NONE',  ( -0.000000000000000000, 1.000000000000000000, -0.000000000000000000 ) ) ;
#4417 = CARTESIAN_POINT ( 'NONE',  ( -2.229367062499996610, -59.39583333196773651, 3.861377020970582219 ) ) ;
#4418 = CARTESIAN_POINT ( 'NONE',  ( -5.000000000000000000, -83.87499999726880162, 0.000000000000000000 ) ) ;
#4420 = ORIENTED_EDGE ( 'NONE', *, *, #6002, .F. ) ;
#4419 = DIRECTION ( 'NONE',  ( 0.000000000000000000, 0.000000000000000000, 1.000000000000000000 ) ) ;
#4421 = CARTESIAN_POINT ( 'NONE',  ( -57.46284108482265651, -146.9375000000000284, 4.819101127000239515 ) ) ;
#4422 = CARTESIAN_POINT ( 'NONE',  ( 4.458734124999998549, -23.97916666530107221, -2.574251347313721627 ) ) ;
#4424 = ORIENTED_EDGE ( 'NONE', *, *, #9501, .T. ) ;
#4423 = CARTESIAN_POINT ( 'NONE',  ( -4.458734124999998549, -60.47916666530105800, 2.574251347313722516 ) ) ;
#4425 = EDGE_CURVE ( 'NONE', #2855, #56096, #38521, .T. ) ;
#4426 = CARTESIAN_POINT ( 'NONE',  ( 0.000000000000000000, 0.000000000000000000, 0.000000000000000000 ) ) ;
#4427 = CARTESIAN_POINT ( 'NONE',  ( 4.458734124999999437, -167.6875000013655779, 0.000000000000000000 ) ) ;
#4428 = CARTESIAN_POINT ( 'NONE',  ( -4.458734124999998549, -104.4791666653010651, 2.574251347313722516 ) ) ;
#4429 = CARTESIAN_POINT ( 'NONE',  ( -2.500000000000000444, -27.04166666393548013, -4.330127018922193649 ) ) ;
#4430 = ORIENTED_EDGE ( 'NONE', *, *, #31510, .F. ) ;
#4431 = CARTESIAN_POINT ( 'NONE',  ( -50.70258187064364108, -150.3750000013656063, 2.196230717870141014 ) ) ;
#4432 = CARTESIAN_POINT ( 'NONE',  ( -51.19402409849444524, -138.6250000027312410, -3.242614290531456334 ) ) ;
#4433 = CARTESIAN_POINT ( 'NONE',  ( -2.229367062499996610, -38.14583333196773651, 3.861377020970582219 ) ) ;
#4434 = CARTESIAN_POINT ( 'NONE',  ( -5.000000000000000000, 1.125000002731184390, 0.000000000000000000 ) ) ;
#4435 = CARTESIAN_POINT ( 'NONE',  ( 4.458734124999998549, -12.72916666530107044, -2.574251347313721627 ) ) ;
#4436 = CARTESIAN_POINT ( 'NONE',  ( 4.458734124999999437, -103.0624999986344079, -5.460374474430324690E-16 ) ) ;
#4437 = CARTESIAN_POINT ( 'NONE',  ( 4.458734124999999437, -145.6875000013656063, 0.000000000000000000 ) ) ;
#4438 = CARTESIAN_POINT ( 'NONE',  ( 4.458734125000001214, -27.14583333196774717, 2.574251347313718519 ) ) ;
#4439 = CARTESIAN_POINT ( 'NONE',  ( -55.00000000000001421, -155.0000000000000284, 8.082903768654762899 ) ) ;
#4440 = CARTESIAN_POINT ( 'NONE',  ( -50.55543936806279248, -131.0625000013656063, 0.3552334253322060320 ) ) ;
#4441 = CARTESIAN_POINT ( 'NONE',  ( 4.458734124999998549, -68.97916666530106511, -2.574251347313721627 ) ) ;
#4442 = ADVANCED_FACE ( 'NONE', ( #957 ), #31457, .T. ) ;
#4443 = CARTESIAN_POINT ( 'NONE',  ( 2.499999999999998668, -17.33333333333333215, -4.330127018922193649 ) ) ;
#4444 = CARTESIAN_POINT ( 'NONE',  ( -1.339745962155610925, -0.6696581960073348938, 5.000000000000000000 ) ) ;
#4445 = CARTESIAN_POINT ( 'NONE',  ( 4.458734124999997661, -140.5000000013655779, 1.846868145590737864 ) ) ;
#4446 = CARTESIAN_POINT ( 'NONE',  ( 4.458734124999999437, 2.937500001365594304, -5.460374474430324690E-16 ) ) ;
#4447 = EDGE_LOOP ( 'NONE', ( #60557, #30535, #51293, #60827 ) ) ;
#4448 = CARTESIAN_POINT ( 'NONE',  ( -2.499999999999996447, -70.70833333060214443, 4.330127018922195425 ) ) ;
#4449 = ADVANCED_FACE ( 'NONE', ( #41426 ), #20557, .T. ) ;
#4450 = CARTESIAN_POINT ( 'NONE',  ( 6.123233995736766282E-16, -120.0000000000000000, -5.000000000000000000 ) ) ;
#4452 = CARTESIAN_POINT ( 'NONE',  ( 4.458734125000001214, -27.89583333196774007, 2.574251347313718519 ) ) ;
#4451 = CARTESIAN_POINT ( 'NONE',  ( 2.499999999999998668, -96.33333333333332860, -4.330127018922193649 ) ) ;
#4453 = CARTESIAN_POINT ( 'NONE',  ( 5.000000000000000000, -73.50000000000000000, -6.123233995736766282E-16 ) ) ;
#4454 = CARTESIAN_POINT ( 'NONE',  ( -2.229367062500000163, -74.72916666530106511, -3.861377020970580443 ) ) ;
#4455 = CARTESIAN_POINT ( 'NONE',  ( 4.458734124999999437, 23.93750000136559564, -5.460374474430324690E-16 ) ) ;
#4456 = DIRECTION ( 'NONE',  ( 0.000000000000000000, 0.000000000000000000, 1.000000000000000000 ) ) ;
#4457 = AXIS2_PLACEMENT_3D ( 'NONE', #16713, #2256, #46299 ) ;
#4458 = CARTESIAN_POINT ( 'NONE',  ( -55.35523342533222291, -141.3125000013656063, 4.444560631937231499 ) ) ;
#4459 = ADVANCED_FACE ( 'NONE', ( #60754 ), #40792, .T. ) ;
#4460 = CARTESIAN_POINT ( 'NONE',  ( 2.229367062499998831, 2.354166668032262599, -3.861377020970580887 ) ) ;
#4461 = CARTESIAN_POINT ( 'NONE',  ( -2.229367062500000163, 25.27083333469892779, -3.861377020970580443 ) ) ;
#4462 = CARTESIAN_POINT ( 'NONE',  ( 4.458734125000000326, -45.14583333196774362, 2.574251347313718519 ) ) ;
#4463 = DIRECTION ( 'NONE',  ( -0.000000000000000000, 1.000000000000000000, -0.000000000000000000 ) ) ;
#4464 = CARTESIAN_POINT ( 'NONE',  ( 4.458734125000000326, -0.8958333319677401763, 2.574251347313718519 ) ) ;
#4465 = ORIENTED_EDGE ( 'NONE', *, *, #63072, .T. ) ;
#4466 = CARTESIAN_POINT ( 'NONE',  ( 9.457646018065525792E-16, -27.31249999863440081, 5.148502694627439702 ) ) ;
#4467 = CARTESIAN_POINT ( 'NONE',  ( 1.846868145590736310, -157.6250000013655779, 4.458734124999999437 ) ) ;
#4468 = CARTESIAN_POINT ( 'NONE',  ( 4.458734125000001214, -70.89583333196773651, 2.574251347313718519 ) ) ;
#4469 = CARTESIAN_POINT ( 'NONE',  ( 5.000000000000000000, -104.3749999972688158, -6.123233995736766282E-16 ) ) ;
#4470 =( BOUNDED_CURVE ( )  B_SPLINE_CURVE ( 2, ( #42801, #56981, #17427, #42482, #62121, #37042, #62753, #3273, #37351 ),
 .UNSPECIFIED., .F., .F. ) 
 B_SPLINE_CURVE_WITH_KNOTS ( ( 3, 2, 2, 2, 3 ),
 ( 0.8839285714285713969, 0.8845238095238094900, 0.8857142857142856762, 0.8869047619047618625, 0.8874999999999999556 ),
 .UNSPECIFIED. ) 
 CURVE ( )  GEOMETRIC_REPRESENTATION_ITEM ( )  RATIONAL_B_SPLINE_CURVE ( ( 0.9330127018922194093, 0.9330127018922194093, 1.000000000000000000, 0.8660254037844387076, 1.000000000000000000, 0.8660254037844387076, 1.000000000000000000, 0.9330127018922194093, 0.9330127018922194093 ) ) 
 REPRESENTATION_ITEM ( '' )  );
#4471 = CARTESIAN_POINT ( 'NONE',  ( 2.229367062499998831, 24.35416666803225993, -3.861377020970580887 ) ) ;
#4472 = CARTESIAN_POINT ( 'NONE',  ( 0.000000000000000000, -170.0000000000000000, 0.000000000000000000 ) ) ;
#4473 = CARTESIAN_POINT ( 'NONE',  ( 2.229367062500001939, -74.22916666530106511, 3.861377020970579999 ) ) ;
#4474 = CARTESIAN_POINT ( 'NONE',  ( -4.999999999999999112, -51.91666666666667140, 2.886751345948131764 ) ) ;
#4475 = DIRECTION ( 'NONE',  ( -0.000000000000000000, 1.000000000000000000, -0.000000000000000000 ) ) ;
#4476 = CARTESIAN_POINT ( 'NONE',  ( 0.000000000000000000, -170.0000000000000000, 0.000000000000000000 ) ) ;
#4477 = ORIENTED_EDGE ( 'NONE', *, *, #9853, .F. ) ;
#4478 = CARTESIAN_POINT ( 'NONE',  ( 5.000000000000000888, 6.416666666666667851, 2.886751345948126879 ) ) ;
#4479 = CARTESIAN_POINT ( 'NONE',  ( 1.339745962155615144, -89.58034179853028434, 4.999999999999999112 ) ) ;
#4480 = CARTESIAN_POINT ( 'NONE',  ( -2.500000000000000444, -15.16666666666666785, -4.330127018922193649 ) ) ;
#4481 = CARTESIAN_POINT ( 'NONE',  ( -4.458734124999999437, -15.39583333196773474, -2.574251347313719407 ) ) ;
#4482 = CARTESIAN_POINT ( 'NONE',  ( 2.229367062499998831, -78.64583333196773651, -3.861377020970580887 ) ) ;
#4483 = CARTESIAN_POINT ( 'NONE',  ( -1.846868145590734756, -168.3750000013655779, -4.458734125000000326 ) ) ;
#4484 = CARTESIAN_POINT ( 'NONE',  ( 1.060575238724906964E-15, -15.62499999726881406, 5.773502691896257311 ) ) ;
#4486 = ORIENTED_EDGE ( 'NONE', *, *, #55946, .T. ) ;
#4485 = CARTESIAN_POINT ( 'NONE',  ( 2.229367062499998831, -47.64583333196774362, -3.861377020970580887 ) ) ;
#4487 = DIRECTION ( 'NONE',  ( -0.000000000000000000, 1.000000000000000000, -0.000000000000000000 ) ) ;
#4489 = ORIENTED_EDGE ( 'NONE', *, *, #23699, .T. ) ;
#4488 = CARTESIAN_POINT ( 'NONE',  ( -4.458734124999998549, -0.4791666653010707710, 2.574251347313722516 ) ) ;
#4490 = CARTESIAN_POINT ( 'NONE',  ( -50.55543936806279248, -152.0625000013656063, 0.3552334253322060320 ) ) ;
#4491 = CARTESIAN_POINT ( 'NONE',  ( 5.000000000000000888, -59.58333333333334281, 2.886751345948126879 ) ) ;
#4492 = CARTESIAN_POINT ( 'NONE',  ( -1.846868145590734756, -154.3750000013655779, -4.458734125000000326 ) ) ;
#4493 = CARTESIAN_POINT ( 'NONE',  ( -4.458734124999999437, -42.64583333196773651, -2.574251347313719407 ) ) ;
#4494 = CARTESIAN_POINT ( 'NONE',  ( -2.500000000000000444, -65.16666666666667140, -4.330127018922193649 ) ) ;
#4495 = CARTESIAN_POINT ( 'NONE',  ( -5.000000000000000000, -162.5000000000000000, -6.123233995736766282E-16 ) ) ;
#4496 = CARTESIAN_POINT ( 'NONE',  ( 1.975475456537005874E-15, -29.74999999999999645, 5.000000000000000000 ) ) ;
#4497 = CARTESIAN_POINT ( 'NONE',  ( -50.40829686548195099, -125.2500000013656347, -1.485763867205728284 ) ) ;
#4498 = CARTESIAN_POINT ( 'NONE',  ( 2.229367062499998831, -3.895833331967739177, -3.861377020970580887 ) ) ;
#4499 = CARTESIAN_POINT ( 'NONE',  ( -2.229367062499996610, -45.39583333196774362, 3.861377020970582219 ) ) ;
#4500 = AXIS2_PLACEMENT_3D ( 'NONE', #34995, #35309, #54285 ) ;
#4501 = EDGE_CURVE ( 'NONE', #36690, #26096, #27451, .T. ) ;
#4502 = CARTESIAN_POINT ( 'NONE',  ( 0.000000000000000000, -170.0000000000000000, 5.000000000000000000 ) ) ;
#4503 = CARTESIAN_POINT ( 'NONE',  ( 4.458734124999999437, -149.5000000013655779, 1.846868145590737864 ) ) ;
#4504 = CARTESIAN_POINT ( 'NONE',  ( 4.458734125000001214, -88.14583333196773651, 2.574251347313718519 ) ) ;
#4505 = CARTESIAN_POINT ( 'NONE',  ( -57.46284108482265651, -142.9375000000000000, 4.819101127000238627 ) ) ;
#4506 = ORIENTED_EDGE ( 'NONE', *, *, #59887, .F. ) ;
#4507 = CARTESIAN_POINT ( 'NONE',  ( 2.071067811865306751, -154.9375000027311842, -5.000000000000171418 ) ) ;
#4508 = CARTESIAN_POINT ( 'NONE',  ( -5.000000000000000000, -68.95833333060214443, -2.886751345948128211 ) ) ;
#4509 = CARTESIAN_POINT ( 'NONE',  ( -52.53715891517739323, -151.5625000027312126, -4.819101127000233298 ) ) ;
#4510 = CARTESIAN_POINT ( 'NONE',  ( -6.972266317189433020E-16, -12.12499999726881406, -5.000000000000000000 ) ) ;
#4511 = ORIENTED_EDGE ( 'NONE', *, *, #52265, .T. ) ;
#4512 = CARTESIAN_POINT ( 'NONE',  ( -6.972266317189433020E-16, -71.12499999726878741, -5.000000000000000000 ) ) ;
#4513 = CARTESIAN_POINT ( 'NONE',  ( -2.229367062500000163, -12.72916666530107044, -3.861377020970580443 ) ) ;
#4514 = CYLINDRICAL_SURFACE ( 'NONE', #46662, 5.000000000000000000 ) ;
#4515 = CARTESIAN_POINT ( 'NONE',  ( 9.457646018065525792E-16, -3.062499998634407472, 5.148502694627439702 ) ) ;
#4516 = CARTESIAN_POINT ( 'NONE',  ( -1.339745962155613812, 3.919658201469705894, -5.000000000000000000 ) ) ;
#4517 = CARTESIAN_POINT ( 'NONE',  ( -4.458734124999999437, -152.9375000013655779, -5.460374474430324690E-16 ) ) ;
#4518 =( BOUNDED_CURVE ( )  B_SPLINE_CURVE ( 2, ( #45378, #35100, #56, #10638, #10956, #1024, #370, #39583, #10326 ),
 .UNSPECIFIED., .F., .F. ) 
 B_SPLINE_CURVE_WITH_KNOTS ( ( 3, 2, 2, 2, 3 ),
 ( 0.9767857142857142572, 0.9773809523809523503, 0.9785714285714285365, 0.9797619047619047228, 0.9803571428571428159 ),
 .UNSPECIFIED. ) 
 CURVE ( )  GEOMETRIC_REPRESENTATION_ITEM ( )  RATIONAL_B_SPLINE_CURVE ( ( 0.9330127018922194093, 0.9330127018922194093, 1.000000000000000000, 0.8660254037844387076, 1.000000000000000000, 0.8660254037844387076, 1.000000000000000000, 0.9330127018922194093, 0.9330127018922194093 ) ) 
 REPRESENTATION_ITEM ( '' )  );
#4519 = CARTESIAN_POINT ( 'NONE',  ( 4.458734125000000326, 21.85416666803225993, 2.574251347313718519 ) ) ;
#4520 = ORIENTED_EDGE ( 'NONE', *, *, #47358, .F. ) ;
#4521 = CARTESIAN_POINT ( 'NONE',  ( 4.458734125000000326, -90.89583333196773651, 2.574251347313718519 ) ) ;
#4522 = CARTESIAN_POINT ( 'NONE',  ( -5.000000000000000000, -47.08333333333333570, -2.886751345948128211 ) ) ;
#4523 = CARTESIAN_POINT ( 'NONE',  ( 5.000000000000000000, -40.41666666666667140, -2.886751345948130876 ) ) ;
#4524 = CARTESIAN_POINT ( 'NONE',  ( 9.457646018065525792E-16, -15.06249999863440259, 5.148502694627439702 ) ) ;
#4525 = CARTESIAN_POINT ( 'NONE',  ( 3.253724281355068545E-15, 28.75000000000000000, -5.000000000000000000 ) ) ;
#4526 = DIRECTION ( 'NONE',  ( -0.000000000000000000, 1.000000000000000000, -0.000000000000000000 ) ) ;
#4527 = CARTESIAN_POINT ( 'NONE',  ( -50.70258187064364108, -154.1250000013656347, 2.196230717870141014 ) ) ;
#4528 = CARTESIAN_POINT ( 'NONE',  ( 1.060575238724906964E-15, -40.62499999726880162, 5.773502691896257311 ) ) ;
#4529 = CARTESIAN_POINT ( 'NONE',  ( 2.500000000000002220, -49.54166666393547303, 4.330127018922192761 ) ) ;
#4530 = CARTESIAN_POINT ( 'NONE',  ( -2.229367062499996610, 16.85416666803225993, 3.861377020970582219 ) ) ;
#4531 = CARTESIAN_POINT ( 'NONE',  ( -5.000000000000000000, 12.04166666939785202, -2.886751345948128211 ) ) ;
#4532 = ORIENTED_EDGE ( 'NONE', *, *, #9074, .T. ) ;
#4533 = CARTESIAN_POINT ( 'NONE',  ( 2.229367062499998831, 18.35416666803225993, -3.861377020970580887 ) ) ;
#4534 = CARTESIAN_POINT ( 'NONE',  ( 2.229367062499998831, -64.64583333196773651, -3.861377020970580887 ) ) ;
#4535 = CARTESIAN_POINT ( 'NONE',  ( 2.229367062500001939, -7.229166665301073103, 3.861377020970579999 ) ) ;
#4536 = CARTESIAN_POINT ( 'NONE',  ( -2.500000000000000444, 8.833333333333332149, -4.330127018922193649 ) ) ;
#4537 = CARTESIAN_POINT ( 'NONE',  ( -4.458734125000001214, -165.8750000013656063, 1.846868145590734089 ) ) ;
#4538 = CARTESIAN_POINT ( 'NONE',  ( 1.975475456537005874E-15, -35.62499999726880162, 5.000000000000000000 ) ) ;
#4539 = CARTESIAN_POINT ( 'NONE',  ( 2.229367062499998831, -53.64583333196773651, -3.861377020970580887 ) ) ;
#4540 = CARTESIAN_POINT ( 'NONE',  ( 1.060575238724906964E-15, -89.62499999726881583, 5.773502691896257311 ) ) ;
#4541 = CARTESIAN_POINT ( 'NONE',  ( -53.51423613279429503, -131.5000000013656347, 4.591703134518082763 ) ) ;
#4542 = AXIS2_PLACEMENT_3D ( 'NONE', #54084, #58911, #24822 ) ;
#4543 = DIRECTION ( 'NONE',  ( -0.6485228581062915110, 0.000000000000000000, -0.7611951803011149931 ) ) ;
#4544 = CARTESIAN_POINT ( 'NONE',  ( 9.457646018065525792E-16, -90.31249999863439371, 5.148502694627439702 ) ) ;
#4545 = CARTESIAN_POINT ( 'NONE',  ( -4.458734124999999437, -152.2500000013656063, -1.846868145590735644 ) ) ;
#4546 = CARTESIAN_POINT ( 'NONE',  ( 5.000000000000000888, -35.58333333333332860, 2.886751345948126879 ) ) ;
#4547 = CARTESIAN_POINT ( 'NONE',  ( -1.339745962155610925, 19.20534180126147916, 5.000000000000000000 ) ) ;
#4548 = CARTESIAN_POINT ( 'NONE',  ( 0.000000000000000000, -170.0000000000000000, 5.000000000000000000 ) ) ;
#4549 = ORIENTED_EDGE ( 'NONE', *, *, #748, .T. ) ;
#4550 = CARTESIAN_POINT ( 'NONE',  ( -4.458734124999998549, -103.2291666653010509, 2.574251347313722516 ) ) ;
#4551 = CARTESIAN_POINT ( 'NONE',  ( 9.457646018065525792E-16, 10.68750000136559386, 5.148502694627439702 ) ) ;
#4552 = CARTESIAN_POINT ( 'NONE',  ( -1.339745962155613812, -44.08034179853027723, -5.000000000000000000 ) ) ;
#4553 = CARTESIAN_POINT ( 'NONE',  ( -4.999999999999999112, 1.083333333333331927, 2.886751345948131764 ) ) ;
#4554 = CARTESIAN_POINT ( 'NONE',  ( -3.152548672688508926E-16, -62.56249999863440792, -5.148502694627439702 ) ) ;
#4555 = CARTESIAN_POINT ( 'NONE',  ( -5.000000000000000000, 19.99999999999999645, 0.000000000000000000 ) ) ;
#4556 = CARTESIAN_POINT ( 'NONE',  ( 5.000000000000000000, -3.374999997268816276, -6.123233995736766282E-16 ) ) ;
#4558 = ORIENTED_EDGE ( 'NONE', *, *, #49892, .T. ) ;
#4557 = CARTESIAN_POINT ( 'NONE',  ( -3.152548672688508926E-16, -30.56249999863440436, -5.148502694627439702 ) ) ;
#4559 = CARTESIAN_POINT ( 'NONE',  ( -1.339745962155610925, -10.79465819873852261, 5.000000000000000000 ) ) ;
#4560 = CARTESIAN_POINT ( 'NONE',  ( 5.000000000000000000, -157.0000000000000000, 0.000000000000000000 ) ) ;
#4561 = CARTESIAN_POINT ( 'NONE',  ( 0.000000000000000000, -170.0000000000000000, 0.000000000000000000 ) ) ;
#4562 = CARTESIAN_POINT ( 'NONE',  ( 2.499999999999998668, -46.33333333333333570, -4.330127018922193649 ) ) ;
#4564 = CARTESIAN_POINT ( 'NONE',  ( -2.229367062500000163, -26.72916666530106866, -3.861377020970580443 ) ) ;
#4563 = CARTESIAN_POINT ( 'NONE',  ( 5.000000000000000000, 6.625000002731185944, -6.123233995736766282E-16 ) ) ;
#4565 = CARTESIAN_POINT ( 'NONE',  ( -6.972266317189433020E-16, -4.124999997268814056, -5.000000000000000000 ) ) ;
#4566 = CARTESIAN_POINT ( 'NONE',  ( 4.458734125000001214, -67.89583333196773651, 2.574251347313718519 ) ) ;
#4567 =( BOUNDED_CURVE ( )  B_SPLINE_CURVE ( 2, ( #7718, #31832, #2269, #22511, #32460, #42106, #12215, #7401, #37601 ),
 .UNSPECIFIED., .F., .F. ) 
 B_SPLINE_CURVE_WITH_KNOTS ( ( 3, 2, 2, 2, 3 ),
 ( 0.7910714285714285365, 0.7916666666666666297, 0.7928571428571428159, 0.7940476190476190022, 0.7946428571428570953 ),
 .UNSPECIFIED. ) 
 CURVE ( )  GEOMETRIC_REPRESENTATION_ITEM ( )  RATIONAL_B_SPLINE_CURVE ( ( 0.9330127018922194093, 0.9330127018922194093, 1.000000000000000000, 0.8660254037844387076, 1.000000000000000000, 0.8660254037844387076, 1.000000000000000000, 0.9330127018922194093, 0.9330127018922194093 ) ) 
 REPRESENTATION_ITEM ( '' )  );
#4568 = CARTESIAN_POINT ( 'NONE',  ( 3.152801135295367541, -143.5625000013655779, -3.152801135295367541 ) ) ;
#4569 = CARTESIAN_POINT ( 'NONE',  ( -2.229367062499996610, -75.14583333196773651, 3.861377020970582219 ) ) ;
#4570 = CARTESIAN_POINT ( 'NONE',  ( -54.64476657466781973, -141.0625000013656063, -4.444560631937228834 ) ) ;
#4571 = CARTESIAN_POINT ( 'NONE',  ( 4.458734124999998549, -24.97916666530106511, -2.574251347313721627 ) ) ;
#4572 = CARTESIAN_POINT ( 'NONE',  ( -2.499999999999996447, -67.70833333060214443, 4.330127018922195425 ) ) ;
#4573 = VERTEX_POINT ( 'NONE', #11211 ) ;
#4574 = CARTESIAN_POINT ( 'NONE',  ( -2.071067811865308972, -152.4375000027312126, 5.000000000000169642 ) ) ;
#4575 = ORIENTED_EDGE ( 'NONE', *, *, #26301, .F. ) ;
#4576 = CARTESIAN_POINT ( 'NONE',  ( 2.229367062499998831, -73.89583333196773651, -3.861377020970580887 ) ) ;
#4577 = CARTESIAN_POINT ( 'NONE',  ( 3.061616997868383141E-16, -147.8750000027312126, -5.000000000000000000 ) ) ;
#4578 = PRESENTATION_STYLE_ASSIGNMENT (( #54434 ) ) ;
#4579 = VERTEX_POINT ( 'NONE', #61075 ) ;
#4580 = EDGE_CURVE ( 'NONE', #35184, #13144, #21644, .T. ) ;
#4581 = CARTESIAN_POINT ( 'NONE',  ( -5.000000000000000000, -39.08333333333332860, -2.886751345948128211 ) ) ;
#4582 = CYLINDRICAL_SURFACE ( 'NONE', #14733, 5.000000000000000000 ) ;
#4583 = CARTESIAN_POINT ( 'NONE',  ( 4.458734125000001214, -59.14583333196773651, 2.574251347313718519 ) ) ;
#4584 = CARTESIAN_POINT ( 'NONE',  ( -2.229367062499996610, -0.3958333319677397322, 3.861377020970582219 ) ) ;
#4585 = ORIENTED_EDGE ( 'NONE', *, *, #50779, .F. ) ;
#4586 = VECTOR ( 'NONE', #28624, 1000.000000000000000 ) ;
#4587 = CARTESIAN_POINT ( 'NONE',  ( -2.071067811865562991, -146.3124999999999716, 4.999999999999913847 ) ) ;
#4588 = CARTESIAN_POINT ( 'NONE',  ( 5.000000000000000000, -69.37499999726880162, -6.123233995736766282E-16 ) ) ;
#4589 = CARTESIAN_POINT ( 'NONE',  ( -4.458734124999998549, 10.77083333469892956, 2.574251347313722516 ) ) ;
#4590 = CARTESIAN_POINT ( 'NONE',  ( -57.89159099828107458, -144.6875000013656063, -3.393966926194107447 ) ) ;
#4591 = CARTESIAN_POINT ( 'NONE',  ( 1.975475456537005874E-15, 6.375000002731185944, 5.000000000000000000 ) ) ;
#4592 = CARTESIAN_POINT ( 'NONE',  ( -1.846868145590737420, -164.7500000013655779, 4.458734124999997661 ) ) ;
#4593 = VERTEX_POINT ( 'NONE', #54961 ) ;
#4594 = CARTESIAN_POINT ( 'NONE',  ( 4.458734124999999437, -73.81249999863440792, -5.460374474430324690E-16 ) ) ;
#4595 = DIRECTION ( 'NONE',  ( -0.000000000000000000, 1.000000000000000000, -0.000000000000000000 ) ) ;
#4596 = CARTESIAN_POINT ( 'NONE',  ( 9.457646018065525792E-16, 1.937500001365593416, 5.148502694627439702 ) ) ;
#4597 = CARTESIAN_POINT ( 'NONE',  ( -3.535533905932737309, -162.7500000027312126, -3.535533905932738197 ) ) ;
#4598 = CARTESIAN_POINT ( 'NONE',  ( 9.457646018065525792E-16, -67.31249999863440792, 5.148502694627439702 ) ) ;
#4599 = CARTESIAN_POINT ( 'NONE',  ( -3.535250795749689387E-16, -27.12499999726881583, -5.773502691896257311 ) ) ;
#4600 = CARTESIAN_POINT ( 'NONE',  ( -5.000000000000000000, 5.999999999999998224, 0.000000000000000000 ) ) ;
#4601 = FACE_OUTER_BOUND ( 'NONE', #46987, .T. ) ;
#4602 = CARTESIAN_POINT ( 'NONE',  ( -6.972266317189433020E-16, -31.24999999999999645, -5.000000000000000000 ) ) ;
#4603 = CARTESIAN_POINT ( 'NONE',  ( 2.499999999999998668, -58.33333333333333570, -4.330127018922193649 ) ) ;
#4604 = CARTESIAN_POINT ( 'NONE',  ( 4.458734124999998549, -45.72916666530106511, -2.574251347313721627 ) ) ;
#4605 = CARTESIAN_POINT ( 'NONE',  ( 4.458734124999999437, -28.06249999863440081, -5.460374474430324690E-16 ) ) ;
#4606 = CARTESIAN_POINT ( 'NONE',  ( 2.229367062499998831, 8.104166668032261711, -3.861377020970580887 ) ) ;
#4607 = CYLINDRICAL_SURFACE ( 'NONE', #25713, 5.000000000000000000 ) ;
#4608 = CARTESIAN_POINT ( 'NONE',  ( 1.060575238724906964E-15, 28.24999999999999645, 5.773502691896257311 ) ) ;
#4609 = CARTESIAN_POINT ( 'NONE',  ( -3.535533905932738641, -150.5000000027312126, 3.535533905932737309 ) ) ;
#4610 = CARTESIAN_POINT ( 'NONE',  ( -6.972266317189433020E-16, -54.12499999726880162, -5.000000000000000000 ) ) ;
#4611 = CARTESIAN_POINT ( 'NONE',  ( -3.152548672688508926E-16, -35.56249999863440792, -5.148502694627439702 ) ) ;
#4612 = CARTESIAN_POINT ( 'NONE',  ( -2.500000000000000444, -67.04166666393547303, -4.330127018922193649 ) ) ;
#4613 = CARTESIAN_POINT ( 'NONE',  ( -57.89159099828107458, -146.9375000013656063, -3.393966926194107447 ) ) ;
#4614 = CARTESIAN_POINT ( 'NONE',  ( 3.535533905932738197, -143.8750000000000000, -3.535533905932738197 ) ) ;
#4615 = CARTESIAN_POINT ( 'NONE',  ( -3.152548672688508926E-16, -76.81249999863440792, -5.148502694627439702 ) ) ;
#4616 = CARTESIAN_POINT ( 'NONE',  ( 1.846868145590736310, -164.8750000013656063, 4.458734124999997661 ) ) ;
#4617 = CARTESIAN_POINT ( 'NONE',  ( -4.458734124999999437, -31.31249999863440436, 0.000000000000000000 ) ) ;
#4618 = CARTESIAN_POINT ( 'NONE',  ( -4.999999999999998224, -27.79166666393548013, 2.886751345948131764 ) ) ;
#4619 = CARTESIAN_POINT ( 'NONE',  ( 0.000000000000000000, -120.0000000000000000, 0.000000000000000000 ) ) ;
#4620 = CARTESIAN_POINT ( 'NONE',  ( -5.000000000000000000, -21.08333333333333570, -2.886751345948128211 ) ) ;
#4621 = CARTESIAN_POINT ( 'NONE',  ( 4.458734124999999437, -144.4375000013656063, 0.000000000000000000 ) ) ;
#4622 = ORIENTED_EDGE ( 'NONE', *, *, #18187, .F. ) ;
#4623 = CARTESIAN_POINT ( 'NONE',  ( 4.458734124999998549, 27.02083333469892423, -2.574251347313721627 ) ) ;
#4624 = CARTESIAN_POINT ( 'NONE',  ( 1.975475456537005874E-15, -58.75000000000000000, 5.000000000000000000 ) ) ;
#4625 = CARTESIAN_POINT ( 'NONE',  ( 4.458734124999998549, -54.97916666530107221, -2.574251347313721627 ) ) ;
#4626 = CARTESIAN_POINT ( 'NONE',  ( 1.060575238724906964E-15, 26.37500000273118417, 5.773502691896257311 ) ) ;
#4627 = CARTESIAN_POINT ( 'NONE',  ( 1.339745962155612702, -90.16965819600733312, -5.000000000000000000 ) ) ;
#4628 = CARTESIAN_POINT ( 'NONE',  ( 2.499999999999998668, 19.66666666666666430, -4.330127018922193649 ) ) ;
#4629 = EDGE_CURVE ( 'NONE', #51386, #30756, #25696, .T. ) ;
#4630 = LINE ( 'NONE', #19429, #48024 ) ;
#4631 = AXIS2_PLACEMENT_3D ( 'NONE', #62462, #13238, #51848 ) ;
#4632 = CARTESIAN_POINT ( 'NONE',  ( -2.229367062500000163, -4.479166665301070438, -3.861377020970580443 ) ) ;
#4633 = CARTESIAN_POINT ( 'NONE',  ( 5.000000000000000000, -166.1875000027311842, 2.071067811865478614 ) ) ;
#4634 = LINE ( 'NONE', #24258, #26583 ) ;
#4635 = CARTESIAN_POINT ( 'NONE',  ( 5.000000000000000000, -89.29166666393547303, -2.886751345948130876 ) ) ;
#4636 = CARTESIAN_POINT ( 'NONE',  ( -6.972266317189433020E-16, -51.12499999726880873, -5.000000000000000000 ) ) ;
#4637 = CARTESIAN_POINT ( 'NONE',  ( 9.457646018065525792E-16, -23.06249999863440792, 5.148502694627439702 ) ) ;
#4638 = CARTESIAN_POINT ( 'NONE',  ( 1.339745962155615144, -97.58034179853028434, 4.999999999999999112 ) ) ;
#4639 = CARTESIAN_POINT ( 'NONE',  ( 4.458734124999999437, -52.81249999863440792, -5.460374474430324690E-16 ) ) ;
#4640 = CARTESIAN_POINT ( 'NONE',  ( 3.152801135295366208, -156.8125000013656063, 3.152801135295367985 ) ) ;
#4641 =( BOUNDED_CURVE ( )  B_SPLINE_CURVE ( 2, ( #31113, #51383, #56204, #45591, #21476, #6679, #36266, #16963, #2495 ),
 .UNSPECIFIED., .F., .F. ) 
 B_SPLINE_CURVE_WITH_KNOTS ( ( 3, 2, 2, 2, 3 ),
 ( 0.3916666666666669960, 0.3958333333333336479, 0.4000000000000003553, 0.4041666666666670071, 0.4083333333333336590 ),
 .UNSPECIFIED. ) 
 CURVE ( )  GEOMETRIC_REPRESENTATION_ITEM ( )  RATIONAL_B_SPLINE_CURVE ( ( 0.9999999999999938938, 0.9238795325112928447, 1.000000000000000000, 0.9238795325112867385, 1.000000000000000000, 0.9238795325112867385, 1.000000000000000000, 0.9238795325112806323, 1.000000000000005995 ) ) 
 REPRESENTATION_ITEM ( '' )  );
#4642 = EDGE_CURVE ( 'NONE', #5304, #16689, #28201, .T. ) ;
#4643 = CARTESIAN_POINT ( 'NONE',  ( 2.500000000000002220, -49.54166666393547303, 4.330127018922192761 ) ) ;
#4644 = ORIENTED_EDGE ( 'NONE', *, *, #1370, .F. ) ;
#4646 = EDGE_CURVE ( 'NONE', #26438, #46520, #27830, .T. ) ;
#4645 = CARTESIAN_POINT ( 'NONE',  ( -4.458734124999999437, 6.437500001365593860, 0.000000000000000000 ) ) ;
#4647 = EDGE_LOOP ( 'NONE', ( #40631, #25304, #24848, #59086 ) ) ;
#4649 = CARTESIAN_POINT ( 'NONE',  ( -5.000000000000000000, -28.99999999999999645, 0.000000000000000000 ) ) ;
#4648 = FACE_OUTER_BOUND ( 'NONE', #37201, .T. ) ;
#4650 = CARTESIAN_POINT ( 'NONE',  ( 4.458734125000000326, -159.3750000013656347, -1.846868145590734978 ) ) ;
#4651 = ORIENTED_EDGE ( 'NONE', *, *, #26359, .F. ) ;
#4652 = DIRECTION ( 'NONE',  ( 1.000000000000000000, 0.000000000000000000, 0.000000000000000000 ) ) ;
#4653 = CARTESIAN_POINT ( 'NONE',  ( -50.01589407740564042, -131.6250000000000284, 0.3983568153799778022 ) ) ;
#4654 = CARTESIAN_POINT ( 'NONE',  ( 1.975475456537005874E-15, -86.62499999726880162, 5.000000000000000000 ) ) ;
#4655 = CARTESIAN_POINT ( 'NONE',  ( 4.458734125000001214, -43.14583333196773651, 2.574251347313718519 ) ) ;
#4656 = VERTEX_POINT ( 'NONE', #47828 ) ;
#4657 = ADVANCED_FACE ( 'NONE', ( #61388 ), #27902, .T. ) ;
#4658 = CARTESIAN_POINT ( 'NONE',  ( 5.000000000000000000, -143.1250000027312126, 0.000000000000000000 ) ) ;
#4659 = CARTESIAN_POINT ( 'NONE',  ( -4.458734124999998549, 19.77083333469892779, 2.574251347313722516 ) ) ;
#4660 = CARTESIAN_POINT ( 'NONE',  ( -51.75738570946856498, -155.0000000000000284, 3.805975901505577408 ) ) ;
#4661 = ORIENTED_EDGE ( 'NONE', *, *, #53617, .T. ) ;
#4662 = CARTESIAN_POINT ( 'NONE',  ( -4.458734124999999437, -90.56249999863440792, 0.000000000000000000 ) ) ;
#4663 = CARTESIAN_POINT ( 'NONE',  ( -51.19402409849444524, -125.6250000027312126, -3.242614290531456334 ) ) ;
#4664 = CARTESIAN_POINT ( 'NONE',  ( -6.972266317189433020E-16, -79.12499999726881583, -5.000000000000000000 ) ) ;
#4665 = CARTESIAN_POINT ( 'NONE',  ( 2.071067811865484387, -169.1875000000000284, 4.999999999999991118 ) ) ;
#4666 = CARTESIAN_POINT ( 'NONE',  ( 2.229367062500001939, -57.97916666530107932, 3.861377020970579999 ) ) ;
#4667 = CARTESIAN_POINT ( 'NONE',  ( -4.999999999999998224, -61.79166666393547303, 2.886751345948131764 ) ) ;
#4668 = CARTESIAN_POINT ( 'NONE',  ( -4.458734124999999437, 16.68750000136559564, 0.000000000000000000 ) ) ;
#4669 = AXIS2_PLACEMENT_3D ( 'NONE', #35470, #40289, #55413 ) ;
#4670 = CARTESIAN_POINT ( 'NONE',  ( 1.975475456537005874E-15, -81.74999999999998579, 5.000000000000000000 ) ) ;
#4671 = CARTESIAN_POINT ( 'NONE',  ( -3.152548672688508926E-16, -49.81249999863440081, -5.148502694627439702 ) ) ;
#4672 = EDGE_CURVE ( 'NONE', #33371, #35072, #62779, .T. ) ;
#4673 = CARTESIAN_POINT ( 'NONE',  ( -5.000000000000000000, -9.958333330602144429, -2.886751345948128211 ) ) ;
#4674 = LINE ( 'NONE', #9194, #23240 ) ;
#4675 = CARTESIAN_POINT ( 'NONE',  ( 1.975475456537005874E-15, -19.62499999726881228, 5.000000000000000000 ) ) ;
#4676 = CARTESIAN_POINT ( 'NONE',  ( -4.458734124999999437, -82.56249999863440792, 0.000000000000000000 ) ) ;
#4677 = CARTESIAN_POINT ( 'NONE',  ( -4.458734124999997661, -108.2291666653010651, 2.574251347313722516 ) ) ;
#4678 = CARTESIAN_POINT ( 'NONE',  ( 4.458734124999998549, -9.979166665301068662, -2.574251347313721627 ) ) ;
#4679 = ORIENTED_EDGE ( 'NONE', *, *, #8923, .F. ) ;
#4680 = CARTESIAN_POINT ( 'NONE',  ( 5.000000000000000000, -9.374999997268814056, -6.123233995736766282E-16 ) ) ;
#4681 = CARTESIAN_POINT ( 'NONE',  ( 4.458734125000001214, -100.8958333319677365, 2.574251347313718519 ) ) ;
#4682 = CARTESIAN_POINT ( 'NONE',  ( 2.071067811865475505, -161.9375000027311842, -5.000000000000000888 ) ) ;
#4683 = CARTESIAN_POINT ( 'NONE',  ( -4.458734124999999437, -95.56249999863440792, 0.000000000000000000 ) ) ;
#4684 = CARTESIAN_POINT ( 'NONE',  ( 5.000000000000000888, -163.0625000027312410, -2.071067811865475505 ) ) ;
#4685 = CARTESIAN_POINT ( 'NONE',  ( -3.535250795749689387E-16, -50.12499999726881583, -5.773502691896257311 ) ) ;
#4686 = CARTESIAN_POINT ( 'NONE',  ( -1.339745962155610925, -36.66965819600732601, 5.000000000000000000 ) ) ;
#4687 = CARTESIAN_POINT ( 'NONE',  ( -53.51423613279429503, -128.2500000013656063, 4.591703134518082763 ) ) ;
#4688 = CARTESIAN_POINT ( 'NONE',  ( -50.55543936806279248, -145.0625000013656063, 0.3552334253322060320 ) ) ;
#4689 = CARTESIAN_POINT ( 'NONE',  ( -2.229367062500000163, -20.47916666530107221, -3.861377020970580443 ) ) ;
#4690 = CARTESIAN_POINT ( 'NONE',  ( -2.229367062500000163, 11.27083333469892601, -3.861377020970580443 ) ) ;
#4691 = CARTESIAN_POINT ( 'NONE',  ( 2.229367062500001939, -61.22916666530106511, 3.861377020970579999 ) ) ;
#4692 = CARTESIAN_POINT ( 'NONE',  ( -2.499999999999996447, -53.83333333333332860, 4.330127018922195425 ) ) ;
#4693 = CARTESIAN_POINT ( 'NONE',  ( -4.458734124999997661, -14.22916666530107221, 2.574251347313722516 ) ) ;
#4694 = CARTESIAN_POINT ( 'NONE',  ( -9.184850993605147944E-16, -146.2500000000000284, 5.000000000000000000 ) ) ;
#4695 = CARTESIAN_POINT ( 'NONE',  ( -2.071067811865478170, -155.3125000000000284, 5.000000000000000000 ) ) ;
#4696 = CARTESIAN_POINT ( 'NONE',  ( -5.000000000000000000, -3.999999999999996447, 0.000000000000000000 ) ) ;
#4697 = EDGE_LOOP ( 'NONE', ( #61118, #37356, #57344, #313 ) ) ;
#4698 = CARTESIAN_POINT ( 'NONE',  ( -4.458734124999999437, -40.56249999863440081, 0.000000000000000000 ) ) ;
#4699 = CARTESIAN_POINT ( 'NONE',  ( 2.500000000000002220, -83.54166666393547303, 4.330127018922192761 ) ) ;
#4700 = CARTESIAN_POINT ( 'NONE',  ( -4.999999999999998224, -8.916666666666662522, 2.886751345948131764 ) ) ;
#4701 = CARTESIAN_POINT ( 'NONE',  ( -6.972266317189433020E-16, -67.12499999726881583, -5.000000000000000000 ) ) ;
#4702 = CARTESIAN_POINT ( 'NONE',  ( 4.458734124999999437, -82.81249999863440792, -5.460374474430324690E-16 ) ) ;
#4703 = CARTESIAN_POINT ( 'NONE',  ( 4.458734125000001214, 20.85416666803226349, 2.574251347313718519 ) ) ;
#4704 = EDGE_CURVE ( 'NONE', #42419, #7188, #6055, .T. ) ;
#4705 = CARTESIAN_POINT ( 'NONE',  ( -4.458734124999999437, 11.60416666803225993, -2.574251347313719407 ) ) ;
#4706 = EDGE_CURVE ( 'NONE', #54885, #42214, #34018, .T. ) ;
#4707 = EDGE_CURVE ( 'NONE', #63145, #49750, #17126, .T. ) ;
#4708 = CARTESIAN_POINT ( 'NONE',  ( -5.000000000000000000, -44.08333333333333570, -2.886751345948128211 ) ) ;
#4709 = CARTESIAN_POINT ( 'NONE',  ( -4.999999999999998224, -68.91666666666667140, 2.886751345948131764 ) ) ;
#4710 = CARTESIAN_POINT ( 'NONE',  ( 2.229367062500001939, -89.22916666530106511, 3.861377020970579999 ) ) ;
#4711 = CARTESIAN_POINT ( 'NONE',  ( 9.457646018065525792E-16, 21.68750000136559208, 5.148502694627439702 ) ) ;
#4712 = CARTESIAN_POINT ( 'NONE',  ( 2.500000000000002220, -73.66666666666665719, 4.330127018922192761 ) ) ;
#4713 = CARTESIAN_POINT ( 'NONE',  ( 1.060575238724906964E-15, 12.37500000273118417, 5.773502691896257311 ) ) ;
#4714 = VERTEX_POINT ( 'NONE', #22466 ) ;
#4715 = EDGE_LOOP ( 'NONE', ( #9155, #47606, #55221, #837 ) ) ;
#4716 =( BOUNDED_CURVE ( )  B_SPLINE_CURVE ( 2, ( #51475, #50833, #56300, #27648, #22842, #46640, #31843, #27333, #2280 ),
 .UNSPECIFIED., .F., .F. ) 
 B_SPLINE_CURVE_WITH_KNOTS ( ( 3, 2, 2, 2, 3 ),
 ( 0.4083333333333336590, 0.4125000000000003109, 0.4166666666666670182, 0.4208333333333336701, 0.4250000000000003220 ),
 .UNSPECIFIED. ) 
 CURVE ( )  GEOMETRIC_REPRESENTATION_ITEM ( )  RATIONAL_B_SPLINE_CURVE ( ( 0.9999999999999938938, 0.9238795325112928447, 1.000000000000000000, 0.9238795325112867385, 1.000000000000000000, 0.9238795325112867385, 1.000000000000000000, 0.9238795325112806323, 1.000000000000005995 ) ) 
 REPRESENTATION_ITEM ( '' )  );
#4718 = CARTESIAN_POINT ( 'NONE',  ( 5.000000000000000000, -32.41666666666665719, -2.886751345948129988 ) ) ;
#4717 = CARTESIAN_POINT ( 'NONE',  ( -6.972266317189433020E-16, -82.24999999999998579, -5.000000000000000000 ) ) ;
#4719 = CARTESIAN_POINT ( 'NONE',  ( 4.458734125000001214, -37.89583333196772941, 2.574251347313718519 ) ) ;
#4720 = CARTESIAN_POINT ( 'NONE',  ( 5.000000000000000000, -32.37499999726880873, -6.123233995736766282E-16 ) ) ;
#4722 = ORIENTED_EDGE ( 'NONE', *, *, #40871, .T. ) ;
#4721 = CARTESIAN_POINT ( 'NONE',  ( 2.229367062499998831, -67.64583333196773651, -3.861377020970580887 ) ) ;
#4723 = CARTESIAN_POINT ( 'NONE',  ( -50.70258187064364108, -151.3750000013656063, 2.196230717870141014 ) ) ;
#4725 = EDGE_CURVE ( 'NONE', #3130, #12680, #47922, .T. ) ;
#4724 = CARTESIAN_POINT ( 'NONE',  ( 4.458734124999999437, -10.81249999863440792, -5.460374474430324690E-16 ) ) ;
#4727 = EDGE_LOOP ( 'NONE', ( #46555, #26307, #57460, #4558 ) ) ;
#4726 = CARTESIAN_POINT ( 'NONE',  ( 4.458734124999999437, -14.06249999863440436, -5.460374474430324690E-16 ) ) ;
#4728 = CARTESIAN_POINT ( 'NONE',  ( 1.060575238724906964E-15, -80.75000000000000000, 5.773502691896257311 ) ) ;
#4729 = DIRECTION ( 'NONE',  ( -0.000000000000000000, 1.000000000000000000, -0.000000000000000000 ) ) ;
#4730 = CARTESIAN_POINT ( 'NONE',  ( -4.458734124999998549, -57.47916666530108643, 2.574251347313722516 ) ) ;
#4732 = CARTESIAN_POINT ( 'NONE',  ( -5.000000000000000000, -80.95833333060214443, -2.886751345948128211 ) ) ;
#4731 = APPLICATION_CONTEXT ( 'automotive_design' ) ;
#4733 = ORIENTED_EDGE ( 'NONE', *, *, #14068, .T. ) ;
#4734 = CARTESIAN_POINT ( 'NONE',  ( -58.80597590150559739, -147.0000000000000284, 3.242614290531460330 ) ) ;
#4735 = CARTESIAN_POINT ( 'NONE',  ( -2.229367062499996610, -27.39583333196774007, 3.861377020970582219 ) ) ;
#4736 = ORIENTED_EDGE ( 'NONE', *, *, #23349, .F. ) ;
#4737 = DIRECTION ( 'NONE',  ( 0.000000000000000000, 1.000000000000000000, 0.000000000000000000 ) ) ;
#4738 = CARTESIAN_POINT ( 'NONE',  ( 4.458734124999999437, -165.6875000013655779, 0.000000000000000000 ) ) ;
#4739 = CARTESIAN_POINT ( 'NONE',  ( 9.457646018065525792E-16, -103.3124999986344079, 5.148502694627439702 ) ) ;
#4740 = CARTESIAN_POINT ( 'NONE',  ( -58.80597590150559739, -135.1250000027312410, 3.242614290531460330 ) ) ;
#4741 = EDGE_LOOP ( 'NONE', ( #40553, #39140, #17407, #11318, #17810, #18038, #21123, #14304, #38965, #6332, #38364, #22396, #29462, #54225, #15827, #36407, #47450, #1288, #39597, #40912, #28006, #36483, #19441, #10313, #7657, #33022, #5219, #41022, #16609, #56847, #45706, #8481, #54766, #25915, #21213, #23735, #9959, #31393, #30071, #7284, #52065, #32630, #1584, #42554, #10046, #50286, #44747, #30436, #18795, #45138, #5370, #17571, #33589, #14298, #17359, #3076, #15012, #38277, #20556, #62956, #1128, #25257, #40097, #6743 ) ) ;
#4742 = CARTESIAN_POINT ( 'NONE',  ( -53.51423613279429503, -144.5000000013656063, 4.591703134518083651 ) ) ;
#4743 = CARTESIAN_POINT ( 'NONE',  ( -60.14911071818854538, -140.1875000027312126, 1.666127454062681368 ) ) ;
#4744 = CARTESIAN_POINT ( 'NONE',  ( 4.458734124999999437, -38.81249999863440081, -5.460374474430324690E-16 ) ) ;
#4745 =( BOUNDED_CURVE ( )  B_SPLINE_CURVE ( 2, ( #21784, #37206, #7938, #17892, #31407, #17262, #32370, #41376, #51684 ),
 .UNSPECIFIED., .F., .F. ) 
 B_SPLINE_CURVE_WITH_KNOTS ( ( 3, 2, 2, 2, 3 ),
 ( 0.8916666666666664964, 0.8958333333333331483, 0.8999999999999999112, 0.9041666666666665630, 0.9083333333333332149 ),
 .UNSPECIFIED. ) 
 CURVE ( )  GEOMETRIC_REPRESENTATION_ITEM ( )  RATIONAL_B_SPLINE_CURVE ( ( 1.000000000000003997, 0.9238795325112826307, 1.000000000000000000, 0.9238795325112867385, 1.000000000000000000, 0.9238795325112867385, 1.000000000000000000, 0.9238795325112887369, 0.9999999999999980016 ) ) 
 REPRESENTATION_ITEM ( '' )  );
#4746 = CARTESIAN_POINT ( 'NONE',  ( -7.894955577759523280, 1.603085139988202901, -7.593799241562120272 ) ) ;
#4747 = CARTESIAN_POINT ( 'NONE',  ( -4.458734124999998549, -13.22916666530107221, 2.574251347313722516 ) ) ;
#4748 = CARTESIAN_POINT ( 'NONE',  ( -3.152548672688508926E-16, -100.8124999986343937, -5.148502694627439702 ) ) ;
#4749 = ORIENTED_EDGE ( 'NONE', *, *, #23243, .F. ) ;
#4750 = CARTESIAN_POINT ( 'NONE',  ( 3.152801135295367541, -145.5625000013655779, -3.152801135295367541 ) ) ;
#4751 = CARTESIAN_POINT ( 'NONE',  ( 2.229367062499998831, -33.89583333196772941, -3.861377020970580887 ) ) ;
#4752 = DIRECTION ( 'NONE',  ( 1.000000000000000000, 0.000000000000000000, -3.614007241618347908E-17 ) ) ;
#4753 = CARTESIAN_POINT ( 'NONE',  ( -59.59170313451811296, -132.5000000013656063, 1.485763867205729394 ) ) ;
#4754 = CARTESIAN_POINT ( 'NONE',  ( -2.229367062500000163, -68.72916666530107932, -3.861377020970580443 ) ) ;
#4755 = CARTESIAN_POINT ( 'NONE',  ( -9.184850993605147944E-16, -154.2500000000000000, 5.000000000000000000 ) ) ;
#4756 = CARTESIAN_POINT ( 'NONE',  ( 5.000000000000000000, -54.37499999726880162, -6.123233995736766282E-16 ) ) ;
#4757 = CARTESIAN_POINT ( 'NONE',  ( -4.458734124999999437, 2.354166668032262599, -2.574251347313719407 ) ) ;
#4758 = ORIENTED_EDGE ( 'NONE', *, *, #48798, .T. ) ;
#4759 = VECTOR ( 'NONE', #48137, 1000.000000000000000 ) ;
#4760 = CARTESIAN_POINT ( 'NONE',  ( -2.499999999999996447, 2.166666666666667407, 4.330127018922195425 ) ) ;
#4761 = CARTESIAN_POINT ( 'NONE',  ( -1.339745962155610925, 16.33034180399266333, 5.000000000000000000 ) ) ;
#4763 = CARTESIAN_POINT ( 'NONE',  ( -3.152548672688508926E-16, -32.56249999863440792, -5.148502694627439702 ) ) ;
#4762 = CARTESIAN_POINT ( 'NONE',  ( -3.535250795749689387E-16, -94.25000000000000000, -5.773502691896257311 ) ) ;
#4764 = CARTESIAN_POINT ( 'NONE',  ( -1.127183054612291972E-14, 23.37500000273118772, 4.999999999999999112 ) ) ;
#4765 = CARTESIAN_POINT ( 'NONE',  ( 4.458734125000001214, -78.14583333196775072, 2.574251347313718519 ) ) ;
#4766 = VECTOR ( 'NONE', #3551, 1000.000000000000000 ) ;
#4767 = CARTESIAN_POINT ( 'NONE',  ( 9.457646018065525792E-16, 21.68750000136559208, 5.148502694627439702 ) ) ;
#4768 = CARTESIAN_POINT ( 'NONE',  ( -4.999999999999998224, 27.08333333333333215, 2.886751345948131764 ) ) ;
#4769 = VECTOR ( 'NONE', #10133, 1000.000000000000000 ) ;
#4770 = CARTESIAN_POINT ( 'NONE',  ( -53.51423613279429503, -141.2500000013656347, 4.591703134518082763 ) ) ;
#4771 = CARTESIAN_POINT ( 'NONE',  ( 4.458734124999999437, 0.1875000013655953035, -5.460374474430324690E-16 ) ) ;
#4772 = CARTESIAN_POINT ( 'NONE',  ( 4.458734125000001214, 24.85416666803225993, 2.574251347313718519 ) ) ;
#4773 = CARTESIAN_POINT ( 'NONE',  ( 2.229367062500001939, -42.22916666530107932, 3.861377020970579999 ) ) ;
#4774 = CARTESIAN_POINT ( 'NONE',  ( -56.66612745406286678, -144.3125000000000000, -5.149110718188528502 ) ) ;
#4775 = CARTESIAN_POINT ( 'NONE',  ( 4.458734124999999437, 1.187500001365596081, -5.460374474430324690E-16 ) ) ;
#4776 = EDGE_LOOP ( 'NONE', ( #31730, #57028, #46594, #62025 ) ) ;
#4777 = CARTESIAN_POINT ( 'NONE',  ( 2.229367062499998831, -22.89583333196773651, -3.861377020970580887 ) ) ;
#4778 = CARTESIAN_POINT ( 'NONE',  ( 4.458734124999998549, -69.72916666530107932, -2.574251347313721627 ) ) ;
#4779 = CARTESIAN_POINT ( 'NONE',  ( -2.500000000000000444, -108.0416666639354730, -4.330127018922193649 ) ) ;
#4780 = CARTESIAN_POINT ( 'NONE',  ( -2.229367062500000163, 26.52083333469892779, -3.861377020970580443 ) ) ;
#4781 = ADVANCED_FACE ( 'NONE', ( #34298 ), #62655, .T. ) ;
#4782 = ADVANCED_FACE ( 'NONE', ( #9229 ), #29148, .T. ) ;
#4783 = CARTESIAN_POINT ( 'NONE',  ( -6.972266317189433020E-16, -58.12499999726880162, -5.000000000000000000 ) ) ;
#4784 = CARTESIAN_POINT ( 'NONE',  ( 2.229367062500001939, -109.2291666653010651, 3.861377020970579999 ) ) ;
#4785 = CARTESIAN_POINT ( 'NONE',  ( 2.229367062499998831, -73.89583333196773651, -3.861377020970580887 ) ) ;
#4786 = CARTESIAN_POINT ( 'NONE',  ( -5.000000000000000000, -55.08333333333332860, -2.886751345948128211 ) ) ;
#4787 = ADVANCED_FACE ( 'NONE', ( #49417 ), #53293, .T. ) ;
#4788 = CARTESIAN_POINT ( 'NONE',  ( 6.123233995736766282E-16, -120.0000000000000000, -5.000000000000000000 ) ) ;
#4789 = CARTESIAN_POINT ( 'NONE',  ( -4.999999999999998224, -10.79166666393547835, 2.886751345948131764 ) ) ;
#4790 = ORIENTED_EDGE ( 'NONE', *, *, #47134, .T. ) ;
#4791 = DIRECTION ( 'NONE',  ( 0.000000000000000000, 0.000000000000000000, 1.000000000000000000 ) ) ;
#4792 = CARTESIAN_POINT ( 'NONE',  ( -2.499999999999996447, 13.16666666666666607, 4.330127018922195425 ) ) ;
#4793 = CARTESIAN_POINT ( 'NONE',  ( -2.500000000000000444, -16.16666666666666785, -4.330127018922193649 ) ) ;
#4794 = CARTESIAN_POINT ( 'NONE',  ( 2.229367062500001939, -21.97916666530107221, 3.861377020970579999 ) ) ;
#4795 = EDGE_CURVE ( 'NONE', #456, #10433, #18874, .T. ) ;
#4796 = CARTESIAN_POINT ( 'NONE',  ( -4.458734124999999437, -82.39583333196773651, -2.574251347313719407 ) ) ;
#4797 = EDGE_CURVE ( 'NONE', #26724, #14472, #25387, .T. ) ;
#4798 = CARTESIAN_POINT ( 'NONE',  ( 3.152801135295367541, -167.5625000013656063, -3.152801135295367541 ) ) ;
#4799 = CARTESIAN_POINT ( 'NONE',  ( -4.999999999999999112, -16.79166666393548368, 2.886751345948131764 ) ) ;
#4801 = ORIENTED_EDGE ( 'NONE', *, *, #10679, .F. ) ;
#4800 = CARTESIAN_POINT ( 'NONE',  ( 2.229367062499998831, -49.64583333196772941, -3.861377020970580887 ) ) ;
#4802 = CARTESIAN_POINT ( 'NONE',  ( 1.339745962155615144, 5.294658198738519950, 4.999999999999999112 ) ) ;
#4803 = CARTESIAN_POINT ( 'NONE',  ( -4.999999999999998224, -27.79166666393548013, 2.886751345948131764 ) ) ;
#4805 = VERTEX_POINT ( 'NONE', #8919 ) ;
#4804 = CARTESIAN_POINT ( 'NONE',  ( 4.458734124999999437, -0.06249999863440491854, -5.460374474430324690E-16 ) ) ;
#4806 = CARTESIAN_POINT ( 'NONE',  ( -50.40829686548195099, -153.0000000013656063, -1.485763867205728284 ) ) ;
#4807 = CARTESIAN_POINT ( 'NONE',  ( -2.499999999999996447, -60.83333333333333570, 4.330127018922195425 ) ) ;
#4808 = EDGE_CURVE ( 'NONE', #33230, #23099, #14292, .T. ) ;
#4809 = CARTESIAN_POINT ( 'NONE',  ( -4.458734125000000326, -155.2500000013656063, -1.846868145590735644 ) ) ;
#4810 = CARTESIAN_POINT ( 'NONE',  ( -4.458734124999999437, -40.56249999863440081, 0.000000000000000000 ) ) ;
#4811 = CARTESIAN_POINT ( 'NONE',  ( -50.01589407740564042, -149.7500000027312126, 0.3983568153799778022 ) ) ;
#4812 = CARTESIAN_POINT ( 'NONE',  ( 5.000000000000000000, -161.0000000000000000, 0.000000000000000000 ) ) ;
#4813 = EDGE_CURVE ( 'NONE', #27768, #11599, #43042, .T. ) ;
#4814 = CARTESIAN_POINT ( 'NONE',  ( -5.000000000000000000, -56.95833333060214443, -2.886751345948128211 ) ) ;
#4815 = CARTESIAN_POINT ( 'NONE',  ( -59.44456063193725015, -126.8125000013655921, -0.3552334253322034230 ) ) ;
#4816 = CIRCLE ( 'NONE', #6856, 4.250000000000000000 ) ;
#4817 = CARTESIAN_POINT ( 'NONE',  ( 2.229367062500001939, -5.229166665301071326, 3.861377020970579999 ) ) ;
#4818 = CARTESIAN_POINT ( 'NONE',  ( -3.152548672688508926E-16, -48.81249999863440792, -5.148502694627439702 ) ) ;
#4819 = ADVANCED_FACE ( 'NONE', ( #49092 ), #5038, .T. ) ;
#4820 = CARTESIAN_POINT ( 'NONE',  ( -52.53715891517739323, -136.5625000027311842, -4.819101127000233298 ) ) ;
#4821 = CARTESIAN_POINT ( 'NONE',  ( -4.458734125000000326, -147.0000000013655779, -1.846868145590735644 ) ) ;
#4822 = CARTESIAN_POINT ( 'NONE',  ( 4.458734125000001214, -91.14583333196773651, 2.574251347313718519 ) ) ;
#4823 = CARTESIAN_POINT ( 'NONE',  ( 1.339745962155612702, -108.2946581987385315, -5.000000000000000000 ) ) ;
#4824 = EDGE_LOOP ( 'NONE', ( #234, #18241, #24008, #34143 ) ) ;
#4825 = CARTESIAN_POINT ( 'NONE',  ( -2.500000000000000444, -69.04166666393547303, -4.330127018922193649 ) ) ;
#4826 = CARTESIAN_POINT ( 'NONE',  ( -59.81910112700025905, -152.3125000027312410, -2.462841084822630311 ) ) ;
#4827 = DIRECTION ( 'NONE',  ( -0.000000000000000000, 1.000000000000000000, -0.000000000000000000 ) ) ;
#4828 = ORIENTED_EDGE ( 'NONE', *, *, #39442, .T. ) ;
#4829 =( BOUNDED_CURVE ( )  B_SPLINE_CURVE ( 2, ( #15131, #20280, #59203, #33488, #38931, #53107, #9982, #33799, #48585 ),
 .UNSPECIFIED., .F., .F. ) 
 B_SPLINE_CURVE_WITH_KNOTS ( ( 3, 2, 2, 2, 3 ),
 ( 0.3562500000000000111, 0.3569444444444444531, 0.3583333333333333370, 0.3597222222222222210, 0.3604166666666666630 ),
 .UNSPECIFIED. ) 
 CURVE ( )  GEOMETRIC_REPRESENTATION_ITEM ( )  RATIONAL_B_SPLINE_CURVE ( ( 0.9330127018922194093, 0.9330127018922194093, 1.000000000000000000, 0.8660254037844387076, 1.000000000000000000, 0.8660254037844387076, 1.000000000000000000, 0.9330127018922194093, 0.9330127018922194093 ) ) 
 REPRESENTATION_ITEM ( '' )  );
#4830 = CARTESIAN_POINT ( 'NONE',  ( 4.458734124999999437, 4.187500001365595637, -5.460374474430324690E-16 ) ) ;
#4831 = CARTESIAN_POINT ( 'NONE',  ( -1.339745962155610925, -70.66965819600731891, 5.000000000000000000 ) ) ;
#4832 = CARTESIAN_POINT ( 'NONE',  ( -2.229367062499996610, -14.39583333196774184, 3.861377020970582219 ) ) ;
#4833 = CARTESIAN_POINT ( 'NONE',  ( 1.975475456537005874E-15, -105.6249999972688016, 5.000000000000000000 ) ) ;
#4834 = CARTESIAN_POINT ( 'NONE',  ( 9.457646018065525792E-16, -4.062499998634408804, 5.148502694627439702 ) ) ;
#4835 = CARTESIAN_POINT ( 'NONE',  ( 1.975475456537005874E-15, -55.62499999726880873, 5.000000000000000000 ) ) ;
#4836 = CARTESIAN_POINT ( 'NONE',  ( -3.152801135295367985, -153.8125000013656063, 3.152801135295367096 ) ) ;
#4837 = CARTESIAN_POINT ( 'NONE',  ( 4.458734124999999437, 20.93750000136559208, -5.460374474430324690E-16 ) ) ;
#4838 = EDGE_LOOP ( 'NONE', ( #46377, #17472, #45316, #21399 ) ) ;
#4839 = CARTESIAN_POINT ( 'NONE',  ( 4.458734125000000326, -98.89583333196773651, 2.574251347313718519 ) ) ;
#4840 = LINE ( 'NONE', #59199, #11013 ) ;
#4841 = DIRECTION ( 'NONE',  ( -0.000000000000000000, 1.000000000000000000, -0.000000000000000000 ) ) ;
#4842 = CARTESIAN_POINT ( 'NONE',  ( 2.229367062499998831, -13.64583333196774184, -3.861377020970580887 ) ) ;
#4843 = CARTESIAN_POINT ( 'NONE',  ( -5.000000000000000000, -84.87499999726880162, 0.000000000000000000 ) ) ;
#4844 = CARTESIAN_POINT ( 'NONE',  ( 5.000000000000000888, 8.541666669397853795, 2.886751345948126879 ) ) ;
#4845 =( BOUNDED_CURVE ( )  B_SPLINE_CURVE ( 2, ( #53265, #24302, #38166, #62926, #38770, #29115, #53889, #63556, #13402 ),
 .UNSPECIFIED., .F., .F. ) 
 B_SPLINE_CURVE_WITH_KNOTS ( ( 3, 2, 2, 2, 3 ),
 ( 0.9229166666666667185, 0.9236111111111111605, 0.9250000000000000444, 0.9263888888888889284, 0.9270833333333333703 ),
 .UNSPECIFIED. ) 
 CURVE ( )  GEOMETRIC_REPRESENTATION_ITEM ( )  RATIONAL_B_SPLINE_CURVE ( ( 0.9330127018922194093, 0.9330127018922194093, 1.000000000000000000, 0.8660254037844387076, 1.000000000000000000, 0.8660254037844387076, 1.000000000000000000, 0.9330127018922194093, 0.9330127018922194093 ) ) 
 REPRESENTATION_ITEM ( '' )  );
#4846 = CARTESIAN_POINT ( 'NONE',  ( -5.000000000000000000, -88.08333333333332860, -2.886751345948128211 ) ) ;
#4847 = CARTESIAN_POINT ( 'NONE',  ( -3.535250795749689387E-16, -42.12499999726880873, -5.773502691896257311 ) ) ;
#4848 = CARTESIAN_POINT ( 'NONE',  ( 1.339745962155612702, -64.16965819600731891, -5.000000000000000000 ) ) ;
#4849 = CARTESIAN_POINT ( 'NONE',  ( 2.229367062500001939, 13.02083333469892779, 3.861377020970579999 ) ) ;
#4850 = CARTESIAN_POINT ( 'NONE',  ( 2.499999999999998668, -44.33333333333333570, -4.330127018922193649 ) ) ;
#4851 = VERTEX_POINT ( 'NONE', #19825 ) ;
#4852 = CARTESIAN_POINT ( 'NONE',  ( 9.457646018065525792E-16, 18.93750000136559564, 5.148502694627439702 ) ) ;
#4853 = CARTESIAN_POINT ( 'NONE',  ( 4.458734125000001214, -63.89583333196772941, 2.574251347313718519 ) ) ;
#4854 = CARTESIAN_POINT ( 'NONE',  ( 4.458734124999998549, -8.979166665301075767, -2.574251347313721627 ) ) ;
#4855 = VECTOR ( 'NONE', #17110, 1000.000000000000000 ) ;
#4856 = CARTESIAN_POINT ( 'NONE',  ( 1.975475456537005874E-15, -45.74999999999999289, 5.000000000000000000 ) ) ;
#4857 = CARTESIAN_POINT ( 'NONE',  ( -5.000000000000000000, 12.00000000000000000, 0.000000000000000000 ) ) ;
#4858 = CARTESIAN_POINT ( 'NONE',  ( 2.730187237215162345E-16, -167.1875000013655779, -4.458734124999999437 ) ) ;
#4859 = CARTESIAN_POINT ( 'NONE',  ( 2.229367062500001939, -50.97916666530107221, 3.861377020970579999 ) ) ;
#4860 = CARTESIAN_POINT ( 'NONE',  ( -5.000000000000000000, -91.87499999726880162, 0.000000000000000000 ) ) ;
#4861 = AXIS2_PLACEMENT_3D ( 'NONE', #9735, #23910, #29031 ) ;
#4862 = CARTESIAN_POINT ( 'NONE',  ( -3.152548672688508926E-16, -26.56249999863440436, -5.148502694627439702 ) ) ;
#4863 = AXIS2_PLACEMENT_3D ( 'NONE', #49467, #40127, #50432 ) ;
#4864 = CARTESIAN_POINT ( 'NONE',  ( -1.339745962155610925, -16.79465819873852084, 5.000000000000000000 ) ) ;
#4865 = CARTESIAN_POINT ( 'NONE',  ( -5.000000000000000000, -54.87499999726880162, 0.000000000000000000 ) ) ;
#4866 = CARTESIAN_POINT ( 'NONE',  ( -56.66612745406274598, -151.4375000027312126, -5.149110718188520508 ) ) ;
#4867 = VECTOR ( 'NONE', #28108, 1000.000000000000000 ) ;
#4868 = CARTESIAN_POINT ( 'NONE',  ( 3.152801135295366208, -154.8125000013656063, 3.152801135295367985 ) ) ;
#4869 = CARTESIAN_POINT ( 'NONE',  ( -2.500000000000000444, -36.16666666666666430, -4.330127018922193649 ) ) ;
#4870 = CARTESIAN_POINT ( 'NONE',  ( 2.499999999999998668, -46.33333333333333570, -4.330127018922193649 ) ) ;
#4871 = DIRECTION ( 'NONE',  ( -0.000000000000000000, 1.000000000000000000, -0.000000000000000000 ) ) ;
#4872 = ORIENTED_EDGE ( 'NONE', *, *, #43262, .T. ) ;
#4873 = CARTESIAN_POINT ( 'NONE',  ( -4.458734124999999437, -99.31249999863440792, 0.000000000000000000 ) ) ;
#4874 = CARTESIAN_POINT ( 'NONE',  ( -4.458734124999999437, 2.354166668032262599, -2.574251347313719407 ) ) ;
#4875 = CARTESIAN_POINT ( 'NONE',  ( 1.975475456537005874E-15, -87.62499999726880162, 5.000000000000000000 ) ) ;
#4876 = CARTESIAN_POINT ( 'NONE',  ( 2.499999999999998668, -4.333333333333334814, -4.330127018922193649 ) ) ;
#4877 = CARTESIAN_POINT ( 'NONE',  ( -4.458734124999997661, -65.22916666530106511, 2.574251347313722516 ) ) ;
#4878 = CARTESIAN_POINT ( 'NONE',  ( -4.999999999999998224, -30.79166666393548013, 2.886751345948131764 ) ) ;
#4879 = CARTESIAN_POINT ( 'NONE',  ( 2.499999999999998668, -0.2083333306021478704, -4.330127018922193649 ) ) ;
#4881 = VERTEX_POINT ( 'NONE', #39435 ) ;
#4880 = CARTESIAN_POINT ( 'NONE',  ( -4.458734124999999437, -36.39583333196772941, -2.574251347313719407 ) ) ;
#4882 = LINE ( 'NONE', #58910, #22508 ) ;
#4883 = FACE_OUTER_BOUND ( 'NONE', #375, .T. ) ;
#4884 = CARTESIAN_POINT ( 'NONE',  ( 2.499999999999998668, 5.666666666666666963, -4.330127018922193649 ) ) ;
#4885 = CARTESIAN_POINT ( 'NONE',  ( -4.999999999999999112, -44.91666666666666430, 2.886751345948131764 ) ) ;
#4887 = CARTESIAN_POINT ( 'NONE',  ( -4.458734124999999437, -22.64583333196773296, -2.574251347313719407 ) ) ;
#4886 = CARTESIAN_POINT ( 'NONE',  ( -1.339745962155610925, -89.66965819600733312, 5.000000000000000000 ) ) ;
#4888 = CARTESIAN_POINT ( 'NONE',  ( -1.339745962155618253, 22.33034180399266333, 4.999999999999996447 ) ) ;
#4889 = CARTESIAN_POINT ( 'NONE',  ( 2.229367062500001939, -69.97916666530107932, 3.861377020970579999 ) ) ;
#4890 = CARTESIAN_POINT ( 'NONE',  ( 1.846868145590736310, -144.8750000013655779, 4.458734124999999437 ) ) ;
#4891 = CARTESIAN_POINT ( 'NONE',  ( -3.152548672688508926E-16, -84.56249999863439371, -5.148502694627439702 ) ) ;
#4892 = CARTESIAN_POINT ( 'NONE',  ( -56.48576386720575471, -140.0000000013656063, -4.591703134518078322 ) ) ;
#4893 = CARTESIAN_POINT ( 'NONE',  ( -4.458734124999999437, -32.64583333196774362, -2.574251347313719407 ) ) ;
#4894 = CARTESIAN_POINT ( 'NONE',  ( 2.499999999999998668, -73.20833333060214443, -4.330127018922193649 ) ) ;
#4895 = EDGE_CURVE ( 'NONE', #11599, #62971, #59075, .T. ) ;
#4896 = ORIENTED_EDGE ( 'NONE', *, *, #62203, .T. ) ;
#4897 = CARTESIAN_POINT ( 'NONE',  ( 1.975475456537005874E-15, -51.75000000000000000, 5.000000000000000000 ) ) ;
#4898 = EDGE_LOOP ( 'NONE', ( #55155, #25428, #63452, #40701 ) ) ;
#4899 = CARTESIAN_POINT ( 'NONE',  ( -4.458734124999999437, -75.64583333196775072, -2.574251347313719407 ) ) ;
#4900 = CARTESIAN_POINT ( 'NONE',  ( -49.85088928181150436, -150.5625000000000284, -1.666127454062680480 ) ) ;
#4901 =( LENGTH_UNIT ( ) NAMED_UNIT ( * ) SI_UNIT ( .MILLI., .METRE. ) );
#4902 = VERTEX_POINT ( 'NONE', #50377 ) ;
#4903 = CARTESIAN_POINT ( 'NONE',  ( 5.000000000000000888, 12.41666666666666607, 2.886751345948126879 ) ) ;
#4904 =( BOUNDED_CURVE ( )  B_SPLINE_CURVE ( 2, ( #9818, #29428, #20122, #5979, #34919, #39405, #48741, #39724, #25587 ),
 .UNSPECIFIED., .F., .F. ) 
 B_SPLINE_CURVE_WITH_KNOTS ( ( 3, 2, 2, 2, 3 ),
 ( 0.2696428571428571286, 0.2702380952380952217, 0.2714285714285714080, 0.2726190476190475942, 0.2732142857142857428 ),
 .UNSPECIFIED. ) 
 CURVE ( )  GEOMETRIC_REPRESENTATION_ITEM ( )  RATIONAL_B_SPLINE_CURVE ( ( 0.9330127018922194093, 0.9330127018922194093, 1.000000000000000000, 0.8660254037844387076, 1.000000000000000000, 0.8660254037844387076, 1.000000000000000000, 0.9330127018922163007, 0.9330127018922194093 ) ) 
 REPRESENTATION_ITEM ( '' )  );
#4905 = VECTOR ( 'NONE', #10783, 1000.000000000000000 ) ;
#4906 = CARTESIAN_POINT ( 'NONE',  ( -5.000000000000000000, -3.083333333333333925, -2.886751345948128211 ) ) ;
#4907 = CARTESIAN_POINT ( 'NONE',  ( -4.458734124999998549, -60.47916666530105800, 2.574251347313722516 ) ) ;
#4908 = CARTESIAN_POINT ( 'NONE',  ( 2.229367062500001939, 3.770833334698926009, 3.861377020970579999 ) ) ;
#4909 = ORIENTED_EDGE ( 'NONE', *, *, #60890, .T. ) ;
#4910 = FACE_OUTER_BOUND ( 'NONE', #50234, .T. ) ;
#4911 = DIRECTION ( 'NONE',  ( 0.000000000000000000, -1.000000000000000000, 0.000000000000000000 ) ) ;
#4912 = CARTESIAN_POINT ( 'NONE',  ( 9.457646018065525792E-16, 13.93750000136559564, 5.148502694627439702 ) ) ;
#4913 = CARTESIAN_POINT ( 'NONE',  ( -51.60603307380591787, -142.9375000013656063, -2.891590998281053704 ) ) ;
#4914 = CARTESIAN_POINT ( 'NONE',  ( 2.500000000000002220, -24.66666666666666430, 4.330127018922192761 ) ) ;
#4915 = CARTESIAN_POINT ( 'NONE',  ( 4.458734124999999437, -164.3750000013656063, -1.846868145590734978 ) ) ;
#4916 = VECTOR ( 'NONE', #24128, 1000.000000000000000 ) ;
#4917 = EDGE_LOOP ( 'NONE', ( #4281, #56889, #33435, #10917 ) ) ;
#4918 = CARTESIAN_POINT ( 'NONE',  ( 9.457646018065525792E-16, -77.06249999863440792, 5.148502694627439702 ) ) ;
#4919 = CARTESIAN_POINT ( 'NONE',  ( -5.000000000000000888, -153.4375000000000000, 2.071067811865474617 ) ) ;
#4920 = CARTESIAN_POINT ( 'NONE',  ( -2.229367062500000163, 1.520833334698927564, -3.861377020970580443 ) ) ;
#4921 = CARTESIAN_POINT ( 'NONE',  ( 2.500000000000002220, -87.66666666666667140, 4.330127018922192761 ) ) ;
#4922 = DIRECTION ( 'NONE',  ( -0.000000000000000000, 1.000000000000000000, -0.000000000000000000 ) ) ;
#4923 = CARTESIAN_POINT ( 'NONE',  ( -3.152548672688508926E-16, -63.81249999863440792, -5.148502694627439702 ) ) ;
#4924 = CARTESIAN_POINT ( 'NONE',  ( -2.500000000000000444, -24.04166666393548368, -4.330127018922193649 ) ) ;
#4925 = DIRECTION ( 'NONE',  ( 0.000000000000000000, 0.000000000000000000, 1.000000000000000000 ) ) ;
#4926 = CARTESIAN_POINT ( 'NONE',  ( -6.972266317189433020E-16, -0.2500000000000001665, -5.000000000000000000 ) ) ;
#4927 = CARTESIAN_POINT ( 'NONE',  ( 2.500000000000002220, -61.66666666666666430, 4.330127018922192761 ) ) ;
#4928 = CARTESIAN_POINT ( 'NONE',  ( 5.000000000000000000, -3.374999997268816276, -6.123233995736766282E-16 ) ) ;
#4929 = CARTESIAN_POINT ( 'NONE',  ( 2.229367062500001939, -47.97916666530106511, 3.861377020970579999 ) ) ;
#4930 = CARTESIAN_POINT ( 'NONE',  ( 4.458734124999999437, -31.06249999863440436, -5.460374474430324690E-16 ) ) ;
#4931 = CARTESIAN_POINT ( 'NONE',  ( 2.229367062500001939, 8.770833334698927786, 3.861377020970579999 ) ) ;
#4932 = CARTESIAN_POINT ( 'NONE',  ( 1.975475456537005874E-15, -96.75000000000000000, 5.000000000000000000 ) ) ;
#4933 = CARTESIAN_POINT ( 'NONE',  ( 1.060575238724906964E-15, 26.25000000000000000, 5.773502691896257311 ) ) ;
#4934 = CARTESIAN_POINT ( 'NONE',  ( 2.071067811865476394, -151.3125000027311842, 5.000000000000000000 ) ) ;
#4935 = CARTESIAN_POINT ( 'NONE',  ( 9.457646018065525792E-16, -40.06249999863439371, 5.148502694627439702 ) ) ;
#4936 = CARTESIAN_POINT ( 'NONE',  ( 5.000000000000000888, -72.45833333060213022, 2.886751345948126879 ) ) ;
#4937 = CARTESIAN_POINT ( 'NONE',  ( -50.70258187064364108, -144.3750000013656063, 2.196230717870141014 ) ) ;
#4938 = CARTESIAN_POINT ( 'NONE',  ( -2.071067811865475061, -141.6875000000000000, -5.000000000000000888 ) ) ;
#4939 = CARTESIAN_POINT ( 'NONE',  ( 9.457646018065525792E-16, -73.31249999863439371, 5.148502694627439702 ) ) ;
#4940 = CARTESIAN_POINT ( 'NONE',  ( -3.152801135295367985, -167.0625000013656063, 3.152801135295367096 ) ) ;
#4941 = CARTESIAN_POINT ( 'NONE',  ( 4.458734125000000326, -30.89583333196773651, 2.574251347313718519 ) ) ;
#4942 = CYLINDRICAL_SURFACE ( 'NONE', #62573, 5.000000000000000000 ) ;
#4943 = DIRECTION ( 'NONE',  ( -0.000000000000000000, 1.000000000000000000, -0.000000000000000000 ) ) ;
#4944 = CARTESIAN_POINT ( 'NONE',  ( -3.535250795749689387E-16, -22.24999999999999645, -5.773502691896257311 ) ) ;
#4945 = CARTESIAN_POINT ( 'NONE',  ( -3.152801135295367985, -143.8125000013655779, 3.152801135295367096 ) ) ;
#4946 = ORIENTED_EDGE ( 'NONE', *, *, #24234, .F. ) ;
#4947 = CARTESIAN_POINT ( 'NONE',  ( 9.457646018065525792E-16, 25.68750000136559208, 5.148502694627439702 ) ) ;
#4948 = VERTEX_POINT ( 'NONE', #45229 ) ;
#4949 = CARTESIAN_POINT ( 'NONE',  ( 4.458734124999999437, -60.06249999863440081, -5.460374474430324690E-16 ) ) ;
#4950 = CARTESIAN_POINT ( 'NONE',  ( -5.000000000000000000, 21.12500000273118417, 0.000000000000000000 ) ) ;
#4951 =( BOUNDED_CURVE ( )  B_SPLINE_CURVE ( 2, ( #23525, #15127, #31, #24781, #58867, #5161, #34748, #14169, #3906 ),
 .UNSPECIFIED., .F., .F. ) 
 B_SPLINE_CURVE_WITH_KNOTS ( ( 3, 2, 2, 2, 3 ),
 ( 0.8729166666666666741, 0.8736111111111111160, 0.8750000000000000000, 0.8763888888888888840, 0.8770833333333333259 ),
 .UNSPECIFIED. ) 
 CURVE ( )  GEOMETRIC_REPRESENTATION_ITEM ( )  RATIONAL_B_SPLINE_CURVE ( ( 0.9330127018922194093, 0.9330127018922194093, 1.000000000000000000, 0.8660254037844387076, 1.000000000000000000, 0.8660254037844387076, 1.000000000000000000, 0.9330127018922194093, 0.9330127018922194093 ) ) 
 REPRESENTATION_ITEM ( '' )  );
#4952 = CARTESIAN_POINT ( 'NONE',  ( 5.000000000000000000, -90.29166666393547303, -2.886751345948130876 ) ) ;
#4953 = CARTESIAN_POINT ( 'NONE',  ( 2.500000000000002220, 19.33333333333333570, 4.330127018922192761 ) ) ;
#4954 = AXIS2_PLACEMENT_3D ( 'NONE', #40234, #59871, #15793 ) ;
#4955 = CYLINDRICAL_SURFACE ( 'NONE', #56267, 5.000000000000000000 ) ;
#4956 = CARTESIAN_POINT ( 'NONE',  ( 2.229367062499998831, -3.645833331967739177, -3.861377020970580887 ) ) ;
#4957 = CYLINDRICAL_SURFACE ( 'NONE', #7226, 5.000000000000000000 ) ;
#4958 = CYLINDRICAL_SURFACE ( 'NONE', #33783, 5.000000000000000000 ) ;
#4959 = LINE ( 'NONE', #19748, #50802 ) ;
#4960 = DIRECTION ( 'NONE',  ( -0.000000000000000000, 1.000000000000000000, -0.000000000000000000 ) ) ;
#4962 = CARTESIAN_POINT ( 'NONE',  ( 2.229367062499998831, -23.64583333196773651, -3.861377020970580887 ) ) ;
#4961 = CARTESIAN_POINT ( 'NONE',  ( 2.500000000000002220, 0.3333333333333348136, 4.330127018922192761 ) ) ;
#4963 = CARTESIAN_POINT ( 'NONE',  ( -2.499999999999996447, -71.70833333060214443, 4.330127018922195425 ) ) ;
#4964 = CARTESIAN_POINT ( 'NONE',  ( 4.458734124999999437, -53.81249999863439371, -5.460374474430324690E-16 ) ) ;
#4965 = CARTESIAN_POINT ( 'NONE',  ( -3.152801135295367096, -157.3125000013656063, -3.152801135295367541 ) ) ;
#4966 = CARTESIAN_POINT ( 'NONE',  ( -5.000000000000000000, -50.95833333060213732, -2.886751345948128211 ) ) ;
#4967 = ORIENTED_EDGE ( 'NONE', *, *, #23606, .F. ) ;
#4968 = CARTESIAN_POINT ( 'NONE',  ( 2.229367062500001939, 6.770833334698928674, 3.861377020970579999 ) ) ;
#4969 = ORIENTED_EDGE ( 'NONE', *, *, #42806, .T. ) ;
#4971 = CARTESIAN_POINT ( 'NONE',  ( -1.339745962155610925, -67.66965819600733312, 5.000000000000000000 ) ) ;
#4970 = CARTESIAN_POINT ( 'NONE',  ( -6.972266317189433020E-16, -87.25000000000001421, -5.000000000000000000 ) ) ;
#4972 = CARTESIAN_POINT ( 'NONE',  ( 1.846868145590736310, -157.6250000013655779, 4.458734124999999437 ) ) ;
#4973 = VERTEX_POINT ( 'NONE', #40714 ) ;
#4974 = CARTESIAN_POINT ( 'NONE',  ( -5.000000000000000000, 11.00000000000000000, 0.000000000000000000 ) ) ;
#4975 = CARTESIAN_POINT ( 'NONE',  ( -49.85088928181150436, -135.5625000000000284, -1.666127454062680702 ) ) ;
#4976 = CARTESIAN_POINT ( 'NONE',  ( 5.000000000000000888, -47.45833333060215153, 2.886751345948126879 ) ) ;
#4977 = CARTESIAN_POINT ( 'NONE',  ( -3.152548672688508926E-16, -41.81249999863440081, -5.148502694627439702 ) ) ;
#4978 = VERTEX_POINT ( 'NONE', #31380 ) ;
#4979 = CARTESIAN_POINT ( 'NONE',  ( -5.000000000000000000, -46.08333333333333570, -2.886751345948128211 ) ) ;
#4980 = CARTESIAN_POINT ( 'NONE',  ( -2.229367062500000163, 20.52083333469892779, -3.861377020970580443 ) ) ;
#4981 = CARTESIAN_POINT ( 'NONE',  ( -3.535533905932738641, -156.5000000027312126, 3.535533905932737309 ) ) ;
#4982 = ORIENTED_EDGE ( 'NONE', *, *, #60733, .T. ) ;
#4983 = CARTESIAN_POINT ( 'NONE',  ( 4.458734124999998549, -89.97916666530105090, -2.574251347313721627 ) ) ;
#4984 = CARTESIAN_POINT ( 'NONE',  ( -59.81910112700025905, -126.3125000027312268, -2.462841084822630311 ) ) ;
#4985 = DIRECTION ( 'NONE',  ( 0.000000000000000000, 0.000000000000000000, 1.000000000000000000 ) ) ;
#4986 = CARTESIAN_POINT ( 'NONE',  ( 2.500000000000002220, -100.6666666666666572, 4.330127018922192761 ) ) ;
#4987 = VECTOR ( 'NONE', #27748, 1000.000000000000000 ) ;
#4988 = CARTESIAN_POINT ( 'NONE',  ( -6.972266317189433020E-16, -70.25000000000000000, -5.000000000000000000 ) ) ;
#4989 = CARTESIAN_POINT ( 'NONE',  ( 4.458734125000000326, -58.89583333196773651, 2.574251347313718519 ) ) ;
#4990 = CARTESIAN_POINT ( 'NONE',  ( -5.000000000000000000, 10.12500000273118594, 0.000000000000000000 ) ) ;
#4991 = CARTESIAN_POINT ( 'NONE',  ( -4.458734124999998549, 16.77083333469892779, 2.574251347313722516 ) ) ;
#4992 = EDGE_CURVE ( 'NONE', #46250, #43716, #54886, .T. ) ;
#4993 = VECTOR ( 'NONE', #2241, 1000.000000000000000 ) ;
#4994 = B_SPLINE_CURVE_WITH_KNOTS ( 'NONE', 3,
 ( #55712, #30933, #50559, #60223, #11625, #44764, #20979, #36082, #31245, #25152, #30290, #59909, #26116, #50879, #6503, #20335, #1688, #39937 ),
 .UNSPECIFIED., .F., .F.,
 ( 4, 2, 2, 2, 2, 2, 2, 2, 4 ),
 ( 0.000000000000000000, 0.0008814191908704200945, 0.001762838381740840189, 0.002644257572611260609, 0.003525676763481680378, 0.004407095954352101448, 0.005288515145222522085, 0.006169934336092942721, 0.007051353526963364225 ),
 .UNSPECIFIED. ) ;
#4995 = CARTESIAN_POINT ( 'NONE',  ( -1.339745962155625802, 18.20534180126147206, 4.999999999999991118 ) ) ;
#4996 = CARTESIAN_POINT ( 'NONE',  ( -2.229367062500000163, -51.72916666530107221, -3.861377020970580443 ) ) ;
#4997 = CARTESIAN_POINT ( 'NONE',  ( -3.535250795749689387E-16, -8.124999997268814056, -5.773502691896257311 ) ) ;
#4998 = CARTESIAN_POINT ( 'NONE',  ( -2.480964764533239819E-13, -72.75000000000000000, 5.000000000000000000 ) ) ;
#4999 = CARTESIAN_POINT ( 'NONE',  ( 0.000000000000000000, 30.00000000000000000, 0.000000000000000000 ) ) ;
#5000 = CARTESIAN_POINT ( 'NONE',  ( -5.000000000000000000, -74.08333333333330017, -2.886751345948128211 ) ) ;
#5001 = CARTESIAN_POINT ( 'NONE',  ( -2.229367062499996610, -106.1458333319677365, 3.861377020970582219 ) ) ;
#5002 = CARTESIAN_POINT ( 'NONE',  ( 9.457646018065525792E-16, -11.31249999863440792, 5.148502694627439702 ) ) ;
#5003 = ORIENTED_EDGE ( 'NONE', *, *, #14955, .T. ) ;
#5004 = CARTESIAN_POINT ( 'NONE',  ( 2.499999999999998668, 23.66666666666666430, -4.330127018922193649 ) ) ;
#5005 = CARTESIAN_POINT ( 'NONE',  ( -4.458734124999999437, -96.39583333196772230, -2.574251347313719407 ) ) ;
#5006 = CARTESIAN_POINT ( 'NONE',  ( -5.000000000000000888, -159.6875000027312126, -2.071067811865475949 ) ) ;
#5007 = CARTESIAN_POINT ( 'NONE',  ( 2.229367062499998831, -97.89583333196773651, -3.861377020970580887 ) ) ;
#5008 = CARTESIAN_POINT ( 'NONE',  ( 5.000000000000000000, -163.1250000027311842, 0.000000000000000000 ) ) ;
#5009 = CARTESIAN_POINT ( 'NONE',  ( -5.000000000000000000, -55.95833333060215153, -2.886751345948128211 ) ) ;
#5010 = CARTESIAN_POINT ( 'NONE',  ( -7.914973979435149687, -3.817460047930451239, -7.907502498112421563 ) ) ;
#5011 = CARTESIAN_POINT ( 'NONE',  ( -59.44456063193725015, -126.5625000013655921, -0.3552334253322034230 ) ) ;
#5012 = EDGE_CURVE ( 'NONE', #58623, #8918, #16755, .T. ) ;
#5013 = CARTESIAN_POINT ( 'NONE',  ( -52.80376928212989185, -145.8750000013655779, -4.297418129356378458 ) ) ;
#5014 = CARTESIAN_POINT ( 'NONE',  ( -2.229367062500000163, -17.47916666530106866, -3.861377020970580443 ) ) ;
#5015 = CARTESIAN_POINT ( 'NONE',  ( -2.229367062500000163, 7.270833334698929562, -3.861377020970580443 ) ) ;
#5016 = CARTESIAN_POINT ( 'NONE',  ( 9.457646018065525792E-16, -59.31249999863440081, 5.148502694627439702 ) ) ;
#5017 = DIRECTION ( 'NONE',  ( 0.000000000000000000, 0.000000000000000000, 1.000000000000000000 ) ) ;
#5018 = CARTESIAN_POINT ( 'NONE',  ( -2.229367062499996610, -13.14583333196774007, 3.861377020970582219 ) ) ;
#5019 = CARTESIAN_POINT ( 'NONE',  ( -6.972266317189433020E-16, -8.124999997268814056, -5.000000000000000000 ) ) ;
#5020 = CARTESIAN_POINT ( 'NONE',  ( 2.071067811865475505, -154.8125000000000000, -5.000000000000000888 ) ) ;
#5021 = CARTESIAN_POINT ( 'NONE',  ( -5.000000000000000000, -4.083333333333334814, -2.886751345948128211 ) ) ;
#5022 = VERTEX_POINT ( 'NONE', #11450 ) ;
#5023 = CARTESIAN_POINT ( 'NONE',  ( -4.458734124999999437, -38.64583333196773651, -2.574251347313719407 ) ) ;
#5024 = CARTESIAN_POINT ( 'NONE',  ( -59.29741812935640155, -124.8750000013656205, -2.196230717870135685 ) ) ;
#5025 = CARTESIAN_POINT ( 'NONE',  ( -2.352174619740013739, 7.302225387956623237, -7.450218641348505422 ) ) ;
#5026 = CARTESIAN_POINT ( 'NONE',  ( -5.276765049035075705, 6.073111908730296271, -7.634085501268424778 ) ) ;
#5027 = CARTESIAN_POINT ( 'NONE',  ( -4.458734124999998549, -83.22916666530106511, 2.574251347313722516 ) ) ;
#5028 = CARTESIAN_POINT ( 'NONE',  ( -3.152548672688508926E-16, 21.18750000136559208, -5.148502694627439702 ) ) ;
#5029 =( BOUNDED_CURVE ( )  B_SPLINE_CURVE ( 2, ( #25087, #49845, #10606, #24774, #20599, #45028, #995, #40203, #59839 ),
 .UNSPECIFIED., .F., .F. ) 
 B_SPLINE_CURVE_WITH_KNOTS ( ( 3, 2, 2, 2, 3 ),
 ( 0.9339285714285714413, 0.9345238095238095344, 0.9357142857142857206, 0.9369047619047619069, 0.9375000000000000000 ),
 .UNSPECIFIED. ) 
 CURVE ( )  GEOMETRIC_REPRESENTATION_ITEM ( )  RATIONAL_B_SPLINE_CURVE ( ( 0.9330127018922194093, 0.9330127018922194093, 1.000000000000000000, 0.8660254037844387076, 1.000000000000000000, 0.8660254037844387076, 1.000000000000000000, 0.9330127018922194093, 0.9330127018922194093 ) ) 
 REPRESENTATION_ITEM ( '' )  );
#5030 = CARTESIAN_POINT ( 'NONE',  ( -4.458734124999998549, 10.77083333469892956, 2.574251347313722516 ) ) ;
#5031 = CARTESIAN_POINT ( 'NONE',  ( 1.975475456537005874E-15, -48.62499999726880162, 5.000000000000000000 ) ) ;
#5032 = CARTESIAN_POINT ( 'NONE',  ( -2.071067811865507036, -165.8125000027312126, -4.999999999999968914 ) ) ;
#5033 = CARTESIAN_POINT ( 'NONE',  ( 2.229367062499998831, -89.89583333196773651, -3.861377020970580887 ) ) ;
#5034 = CARTESIAN_POINT ( 'NONE',  ( -4.458734124999998549, 21.52083333469893134, 2.574251347313722516 ) ) ;
#5035 = CARTESIAN_POINT ( 'NONE',  ( 5.000000000000000888, -75.58333333333334281, 2.886751345948126879 ) ) ;
#5036 = CARTESIAN_POINT ( 'NONE',  ( -5.000000000000000000, 8.125000002731187720, 0.000000000000000000 ) ) ;
#5037 = VERTEX_POINT ( 'NONE', #30104 ) ;
#5038 = CYLINDRICAL_SURFACE ( 'NONE', #33560, 5.000000000000000000 ) ;
#5039 = PRODUCT ( 'spindle', 'spindle', '', ( #1217 ) ) ;
#5040 = ORIENTED_EDGE ( 'NONE', *, *, #13898, .F. ) ;
#5042 = CARTESIAN_POINT ( 'NONE',  ( 5.000000000000000000, -36.50000000000000711, -6.123233995736766282E-16 ) ) ;
#5041 = CARTESIAN_POINT ( 'NONE',  ( 3.061616997868383141E-16, -160.8750000027311842, -5.000000000000000000 ) ) ;
#5043 = CARTESIAN_POINT ( 'NONE',  ( -4.458734124999998549, -39.22916666530107221, 2.574251347313722516 ) ) ;
#5044 = CARTESIAN_POINT ( 'NONE',  ( -5.000000000000000000, -33.95833333060213732, -2.886751345948128211 ) ) ;
#5046 = ORIENTED_EDGE ( 'NONE', *, *, #53080, .F. ) ;
#5045 = CARTESIAN_POINT ( 'NONE',  ( 2.229367062500001939, -65.97916666530106511, 3.861377020970579999 ) ) ;
#5047 = CARTESIAN_POINT ( 'NONE',  ( -50.70258187064364108, -150.3750000013656063, 2.196230717870141014 ) ) ;
#5048 = CARTESIAN_POINT ( 'NONE',  ( -2.229367062499996610, -11.14583333196773829, 3.861377020970582219 ) ) ;
#5050 = ORIENTED_EDGE ( 'NONE', *, *, #43708, .F. ) ;
#5049 = CARTESIAN_POINT ( 'NONE',  ( -3.152548672688508926E-16, -14.81249999863440436, -5.148502694627439702 ) ) ;
#5051 = CARTESIAN_POINT ( 'NONE',  ( -2.499999999999996447, -81.83333333333332860, 4.330127018922195425 ) ) ;
#5052 = CARTESIAN_POINT ( 'NONE',  ( -8.190561711645485556E-16, -167.6875000013655779, 4.458734124999999437 ) ) ;
#5053 = CARTESIAN_POINT ( 'NONE',  ( -4.458734124999999437, -55.64583333196773651, -2.574251347313719407 ) ) ;
#5054 = CARTESIAN_POINT ( 'NONE',  ( -2.500000000000000444, -83.04166666393547303, -4.330127018922193649 ) ) ;
#5056 = ORIENTED_EDGE ( 'NONE', *, *, #8243, .T. ) ;
#5055 = CARTESIAN_POINT ( 'NONE',  ( 0.000000000000000000, -170.0000000000000000, 0.000000000000000000 ) ) ;
#5057 = CARTESIAN_POINT ( 'NONE',  ( -51.75738570946856498, -146.7500000000000284, 3.805975901505576964 ) ) ;
#5058 = CARTESIAN_POINT ( 'NONE',  ( -2.229367062499996610, -25.39583333196773651, 3.861377020970582219 ) ) ;
#5059 = ORIENTED_EDGE ( 'NONE', *, *, #55068, .F. ) ;
#5060 = CARTESIAN_POINT ( 'NONE',  ( 1.846868145590735200, -167.5000000013655779, -4.458734125000000326 ) ) ;
#5061 = CARTESIAN_POINT ( 'NONE',  ( -3.152548672688508926E-16, -103.8124999986344221, -5.148502694627439702 ) ) ;
#5062 = CARTESIAN_POINT ( 'NONE',  ( 5.000000000000000000, -55.29166666393548013, -2.886751345948130876 ) ) ;
#5063 = ORIENTED_EDGE ( 'NONE', *, *, #11108, .T. ) ;
#5064 = CARTESIAN_POINT ( 'NONE',  ( -51.60603307380591787, -145.1875000013656063, -2.891590998281053704 ) ) ;
#5065 = CARTESIAN_POINT ( 'NONE',  ( -51.19402409849444524, -137.6250000027312410, -3.242614290531456334 ) ) ;
#5066 = CARTESIAN_POINT ( 'NONE',  ( 9.457646018065525792E-16, -41.06249999863440081, 5.148502694627439702 ) ) ;
#5067 = CARTESIAN_POINT ( 'NONE',  ( -4.458734124999999437, -145.2500000013656347, -1.846868145590735644 ) ) ;
#5068 = CARTESIAN_POINT ( 'NONE',  ( -7.922811899608408481, -4.628803996615321381, -8.057669882367649805 ) ) ;
#5069 = DIRECTION ( 'NONE',  ( -0.000000000000000000, 1.000000000000000000, -0.000000000000000000 ) ) ;
#5070 = EDGE_CURVE ( 'NONE', #28793, #57369, #3980, .T. ) ;
#5071 = CARTESIAN_POINT ( 'NONE',  ( 4.458734125000001214, -10.89583333196773651, 2.574251347313718519 ) ) ;
#5072 = CARTESIAN_POINT ( 'NONE',  ( -2.229367062500000163, -102.7291666653010651, -3.861377020970580443 ) ) ;
#5073 = ORIENTED_EDGE ( 'NONE', *, *, #45977, .T. ) ;
#5074 = CARTESIAN_POINT ( 'NONE',  ( 4.458734124999999437, -141.6875000013656063, 0.000000000000000000 ) ) ;
#5075 = CARTESIAN_POINT ( 'NONE',  ( 2.229367062500001939, -33.22916666530106511, 3.861377020970579999 ) ) ;
#5076 = CARTESIAN_POINT ( 'NONE',  ( -5.000000000000000000, 5.041666669397853795, -2.886751345948128211 ) ) ;
#5077 = CARTESIAN_POINT ( 'NONE',  ( 1.975475456537005874E-15, -19.75000000000000000, 5.000000000000000000 ) ) ;
#5078 = CARTESIAN_POINT ( 'NONE',  ( -59.44456063193725015, -132.5625000013656063, -0.3552334253322034230 ) ) ;
#5079 =( BOUNDED_CURVE ( )  B_SPLINE_CURVE ( 2, ( #35669, #21831, #6716, #12168, #50775, #7360, #30837, #26969, #1588 ),
 .UNSPECIFIED., .F., .F. ) 
 B_SPLINE_CURVE_WITH_KNOTS ( ( 3, 2, 2, 2, 3 ),
 ( 0.9696428571428571397, 0.9702380952380952328, 0.9714285714285714191, 0.9726190476190476053, 0.9732142857142856984 ),
 .UNSPECIFIED. ) 
 CURVE ( )  GEOMETRIC_REPRESENTATION_ITEM ( )  RATIONAL_B_SPLINE_CURVE ( ( 0.9330127018922194093, 0.9330127018922194093, 1.000000000000000000, 0.8660254037844387076, 1.000000000000000000, 0.8660254037844387076, 1.000000000000000000, 0.9330127018922194093, 0.9330127018922194093 ) ) 
 REPRESENTATION_ITEM ( '' )  );
#5080 = CARTESIAN_POINT ( 'NONE',  ( -4.458734124999999437, -74.56249999863440792, 0.000000000000000000 ) ) ;
#5081 = CARTESIAN_POINT ( 'NONE',  ( 1.339745962155615144, -54.58034179853029144, 4.999999999999999112 ) ) ;
#5082 = CARTESIAN_POINT ( 'NONE',  ( 5.000000000000000000, 14.70833333606451809, -2.886751345948130876 ) ) ;
#5083 = MECHANICAL_DESIGN_GEOMETRIC_PRESENTATION_REPRESENTATION (  '', ( #31814 ), #11284 ) ;
#5084 = CARTESIAN_POINT ( 'NONE',  ( 2.229367062499998831, 4.104166668032260823, -3.861377020970580887 ) ) ;
#5085 = EDGE_LOOP ( 'NONE', ( #50063, #46655, #12453, #6831 ) ) ;
#5086 = CARTESIAN_POINT ( 'NONE',  ( -5.000000000000000000, -70.95833333060214443, -2.886751345948128211 ) ) ;
#5087 = DIRECTION ( 'NONE',  ( -1.000000000000000000, -0.000000000000000000, -0.000000000000000000 ) ) ;
#5089 = CARTESIAN_POINT ( 'NONE',  ( 2.229367062500001939, -29.97916666530107221, 3.861377020970579999 ) ) ;
#5088 = CARTESIAN_POINT ( 'NONE',  ( 1.060575238724906964E-15, -93.75000000000000000, 5.773502691896257311 ) ) ;
#5090 = EDGE_CURVE ( 'NONE', #34156, #11358, #12615, .T. ) ;
#5091 = CARTESIAN_POINT ( 'NONE',  ( -2.499999999999996447, -35.83333333333332860, 4.330127018922195425 ) ) ;
#5092 = CARTESIAN_POINT ( 'NONE',  ( -2.229367062500000163, -82.72916666530106511, -3.861377020970580443 ) ) ;
#5093 = AXIS2_PLACEMENT_3D ( 'NONE', #29055, #58348, #19091 ) ;
#5094 = CARTESIAN_POINT ( 'NONE',  ( -2.229367062499996610, 20.60416666803225993, 3.861377020970582219 ) ) ;
#5095 = LINE ( 'NONE', #62702, #1725 ) ;
#5096 = CARTESIAN_POINT ( 'NONE',  ( -52.80376928212989185, -139.8750000013655779, -4.297418129356379346 ) ) ;
#5097 = CARTESIAN_POINT ( 'NONE',  ( -4.458734124999997661, -3.229166665301069550, 2.574251347313722516 ) ) ;
#5098 = CARTESIAN_POINT ( 'NONE',  ( 4.458734124999998549, 24.02083333469892423, -2.574251347313721627 ) ) ;
#5099 = EDGE_CURVE ( 'NONE', #22073, #56652, #45864, .T. ) ;
#5100 = CARTESIAN_POINT ( 'NONE',  ( -3.152548672688508926E-16, -41.81249999863440081, -5.148502694627439702 ) ) ;
#5101 = CARTESIAN_POINT ( 'NONE',  ( -2.500000000000000444, -46.04166666393547303, -4.330127018922193649 ) ) ;
#5102 = CARTESIAN_POINT ( 'NONE',  ( -3.152548672688508926E-16, 0.4375000013655955255, -5.148502694627439702 ) ) ;
#5103 = ORIENTED_EDGE ( 'NONE', *, *, #28849, .F. ) ;
#5104 = CARTESIAN_POINT ( 'NONE',  ( -4.458734124999999437, -24.64583333196773651, -2.574251347313719407 ) ) ;
#5105 = CARTESIAN_POINT ( 'NONE',  ( -3.152548672688508926E-16, -71.56249999863440792, -5.148502694627439702 ) ) ;
#5106 = CARTESIAN_POINT ( 'NONE',  ( 5.000000000000000888, -105.4583333306021444, 2.886751345948126879 ) ) ;
#5107 = CARTESIAN_POINT ( 'NONE',  ( 2.229367062500001939, 24.02083333469892779, 3.861377020970579999 ) ) ;
#5108 = CARTESIAN_POINT ( 'NONE',  ( 7.204675194429079505E-15, 26.74999999999999645, -5.000000000000000000 ) ) ;
#5109 = CARTESIAN_POINT ( 'NONE',  ( 0.000000000000000000, -120.0000000000000000, 5.000000000000000000 ) ) ;
#5110 = CARTESIAN_POINT ( 'NONE',  ( 4.458734124999999437, -71.06249999863439371, -5.460374474430324690E-16 ) ) ;
#5111 = CARTESIAN_POINT ( 'NONE',  ( -2.499999999999996447, -61.83333333333333570, 4.330127018922195425 ) ) ;
#5112 = CARTESIAN_POINT ( 'NONE',  ( -5.000000000000000000, -66.00000000000000000, 0.000000000000000000 ) ) ;
#5113 = CARTESIAN_POINT ( 'NONE',  ( -5.000000000000000000, -10.87499999726881583, 0.000000000000000000 ) ) ;
#5114 = ORIENTED_EDGE ( 'NONE', *, *, #48302, .F. ) ;
#5115 = CARTESIAN_POINT ( 'NONE',  ( 1.975475456537005874E-15, -62.74999999999998579, 5.000000000000000000 ) ) ;
#5116 = CARTESIAN_POINT ( 'NONE',  ( -1.339745962155610925, -56.66965819600733312, 5.000000000000000000 ) ) ;
#5117 = CARTESIAN_POINT ( 'NONE',  ( -2.499999999999996447, -17.83333333333333215, 4.330127018922195425 ) ) ;
#5118 = CARTESIAN_POINT ( 'NONE',  ( 2.229367062499998831, -23.64583333196773651, -3.861377020970580887 ) ) ;
#5119 = EDGE_CURVE ( 'NONE', #32095, #51645, #58259, .T. ) ;
#5120 = CARTESIAN_POINT ( 'NONE',  ( -4.458734124999999437, -81.31249999863440792, 0.000000000000000000 ) ) ;
#5121 = CARTESIAN_POINT ( 'NONE',  ( -5.000000000000000000, -19.87499999726880873, 0.000000000000000000 ) ) ;
#5123 = ORIENTED_EDGE ( 'NONE', *, *, #19159, .F. ) ;
#5122 = CARTESIAN_POINT ( 'NONE',  ( 4.458734124999998549, -47.72916666530106511, -2.574251347313721627 ) ) ;
#5124 = DIRECTION ( 'NONE',  ( -0.000000000000000000, 1.000000000000000000, -0.000000000000000000 ) ) ;
#5125 = CARTESIAN_POINT ( 'NONE',  ( 1.339745962155615144, -15.58034179853029499, 4.999999999999999112 ) ) ;
#5127 = ORIENTED_EDGE ( 'NONE', *, *, #40874, .T. ) ;
#5126 = CARTESIAN_POINT ( 'NONE',  ( -4.458734124999999437, 1.354166668032261933, -2.574251347313719407 ) ) ;
#5128 = CARTESIAN_POINT ( 'NONE',  ( -53.51423613279429503, -152.2500000013656063, 4.591703134518083651 ) ) ;
#5129 = CARTESIAN_POINT ( 'NONE',  ( -2.499999999999996447, -67.83333333333332860, 4.330127018922195425 ) ) ;
#5130 = CARTESIAN_POINT ( 'NONE',  ( 4.458734125000000326, -156.6250000013655779, -1.846868145590734978 ) ) ;
#5131 = CARTESIAN_POINT ( 'NONE',  ( -4.458734124999999437, -43.64583333196774362, -2.574251347313719407 ) ) ;
#5132 = CARTESIAN_POINT ( 'NONE',  ( -2.500000000000000444, -16.04166666393548368, -4.330127018922193649 ) ) ;
#5133 =( BOUNDED_CURVE ( )  B_SPLINE_CURVE ( 2, ( #15915, #49367, #54520, #1146, #35536, #35859, #55485, #55164, #49686 ),
 .UNSPECIFIED., .F., .F. ) 
 B_SPLINE_CURVE_WITH_KNOTS ( ( 3, 2, 2, 2, 3 ),
 ( 0.5303571428571428603, 0.5309523809523809534, 0.5321428571428571397, 0.5333333333333333259, 0.5339285714285714191 ),
 .UNSPECIFIED. ) 
 CURVE ( )  GEOMETRIC_REPRESENTATION_ITEM ( )  RATIONAL_B_SPLINE_CURVE ( ( 0.9330127018922194093, 0.9330127018922194093, 1.000000000000000000, 0.8660254037844387076, 1.000000000000000000, 0.8660254037844387076, 1.000000000000000000, 0.9330127018922194093, 0.9330127018922194093 ) ) 
 REPRESENTATION_ITEM ( '' )  );
#5134 = CARTESIAN_POINT ( 'NONE',  ( 5.000000000000000000, -163.0000000000000000, 0.000000000000000000 ) ) ;
#5135 = CARTESIAN_POINT ( 'NONE',  ( -2.500000000000000444, -57.04166666393548013, -4.330127018922193649 ) ) ;
#5136 = VECTOR ( 'NONE', #40247, 1000.000000000000000 ) ;
#5137 = CARTESIAN_POINT ( 'NONE',  ( -50.55543936806279248, -128.3125000013656063, 0.3552334253322060320 ) ) ;
#5138 = CARTESIAN_POINT ( 'NONE',  ( 4.458734124999998549, -11.97916666530107044, -2.574251347313721627 ) ) ;
#5139 = CARTESIAN_POINT ( 'NONE',  ( 2.229367062500001939, -45.22916666530106511, 3.861377020970579999 ) ) ;
#5140 = CARTESIAN_POINT ( 'NONE',  ( 2.071067811865602959, -150.9375000027312126, -4.999999999999874767 ) ) ;
#5141 = CARTESIAN_POINT ( 'NONE',  ( 4.458734124999999437, -150.4375000013656063, 0.000000000000000000 ) ) ;
#5142 = CARTESIAN_POINT ( 'NONE',  ( 4.458734125000001214, -87.14583333196772230, 2.574251347313718519 ) ) ;
#5143 = CARTESIAN_POINT ( 'NONE',  ( -3.093157300003891663, -6.874418838041293611, -6.051203375184721622E-15 ) ) ;
#5144 = ORIENTED_EDGE ( 'NONE', *, *, #11330, .T. ) ;
#5145 = CARTESIAN_POINT ( 'NONE',  ( -1.339745962155613812, 13.91965820146970678, -5.000000000000000000 ) ) ;
#5146 = CARTESIAN_POINT ( 'NONE',  ( -59.98410592259440222, -152.2500000027312410, -0.3983568153799752487 ) ) ;
#5147 = VERTEX_POINT ( 'NONE', #1196 ) ;
#5148 = CARTESIAN_POINT ( 'NONE',  ( 2.229367062499998831, 3.354166668032259935, -3.861377020970580887 ) ) ;
#5149 = EDGE_CURVE ( 'NONE', #28986, #55261, #41034, .T. ) ;
#5150 = ADVANCED_FACE ( 'NONE', ( #55845 ), #11761, .T. ) ;
#5151 = CARTESIAN_POINT ( 'NONE',  ( 0.000000000000000000, 15.00000000000000000, 0.000000000000000000 ) ) ;
#5152 = CARTESIAN_POINT ( 'NONE',  ( -2.229367062500000163, -18.72916666530106866, -3.861377020970580443 ) ) ;
#5153 = EDGE_CURVE ( 'NONE', #63596, #53365, #15649, .T. ) ;
#5154 = CARTESIAN_POINT ( 'NONE',  ( -2.499999999999996447, 2.291666669397850686, 4.330127018922195425 ) ) ;
#5155 = CARTESIAN_POINT ( 'NONE',  ( -3.152548672688508926E-16, -3.562499998634408360, -5.148502694627439702 ) ) ;
#5156 = CARTESIAN_POINT ( 'NONE',  ( -6.972266317189433020E-16, -49.24999999999999289, -5.000000000000000000 ) ) ;
#5157 = CARTESIAN_POINT ( 'NONE',  ( -3.152801135295367096, -151.0625000013655779, -3.152801135295367541 ) ) ;
#5158 = CARTESIAN_POINT ( 'NONE',  ( -4.458734124999999437, 23.35416666803226349, -2.574251347313719407 ) ) ;
#5159 = ORIENTED_EDGE ( 'NONE', *, *, #57455, .F. ) ;
#5160 = CARTESIAN_POINT ( 'NONE',  ( 4.458734124999999437, -98.81249999863440792, -5.460374474430324690E-16 ) ) ;
#5161 = CARTESIAN_POINT ( 'NONE',  ( -5.000000000000000000, -75.08333333333332860, -2.886751345948128211 ) ) ;
#5162 = CARTESIAN_POINT ( 'NONE',  ( 1.975475456537005874E-15, -12.62499999726881050, 5.000000000000000000 ) ) ;
#5163 = CARTESIAN_POINT ( 'NONE',  ( -4.458734124999999437, -13.31249999863440259, 0.000000000000000000 ) ) ;
#5165 = EDGE_CURVE ( 'NONE', #10357, #48933, #56594, .T. ) ;
#5164 = CARTESIAN_POINT ( 'NONE',  ( -6.972266317189433020E-16, -110.1249999972688158, -5.000000000000000000 ) ) ;
#5166 = CARTESIAN_POINT ( 'NONE',  ( 0.000000000000000000, -170.0000000000000000, 0.000000000000000000 ) ) ;
#5167 = CARTESIAN_POINT ( 'NONE',  ( -56.48576386720575471, -152.7500000013655779, -4.591703134518078322 ) ) ;
#5168 = CARTESIAN_POINT ( 'NONE',  ( -4.999999999999999112, -42.79166666393548013, 2.886751345948131764 ) ) ;
#5169 = DIRECTION ( 'NONE',  ( -0.000000000000000000, 1.000000000000000000, -0.000000000000000000 ) ) ;
#5170 = CARTESIAN_POINT ( 'NONE',  ( -4.458734124999997661, 11.77083333469892601, 2.574251347313722516 ) ) ;
#5171 = CARTESIAN_POINT ( 'NONE',  ( 0.6249999999999994449, -8.299410119600885594, -7.298562697733110838 ) ) ;
#5172 = EDGE_CURVE ( 'NONE', #61334, #29222, #35640, .T. ) ;
#5173 = CARTESIAN_POINT ( 'NONE',  ( 5.000000000000000000, 9.583333333333332149, -2.886751345948130876 ) ) ;
#5174 = CARTESIAN_POINT ( 'NONE',  ( 2.229367062499998831, 17.35416666803225993, -3.861377020970580887 ) ) ;
#5175 = CARTESIAN_POINT ( 'NONE',  ( -4.458734124999999437, -64.39583333196772230, -2.574251347313719407 ) ) ;
#5176 = EDGE_LOOP ( 'NONE', ( #57452, #32675, #25731, #15825 ) ) ;
#5177 = VECTOR ( 'NONE', #6927, 1000.000000000000000 ) ;
#5178 = CARTESIAN_POINT ( 'NONE',  ( -2.229367062499996610, -6.395833331967741842, 3.861377020970582219 ) ) ;
#5179 = CARTESIAN_POINT ( 'NONE',  ( 2.500000000000002220, 6.333333333333333037, 4.330127018922192761 ) ) ;
#5180 = CARTESIAN_POINT ( 'NONE',  ( -4.458734125000000326, -167.0000000013655779, -1.846868145590735644 ) ) ;
#5182 = EDGE_CURVE ( 'NONE', #15732, #14179, #58448, .T. ) ;
#5181 = FACE_OUTER_BOUND ( 'NONE', #38865, .T. ) ;
#5183 = AXIS2_PLACEMENT_3D ( 'NONE', #63256, #44573, #39422 ) ;
#5184 = CARTESIAN_POINT ( 'NONE',  ( -4.458734124999999437, -52.31249999863440792, 0.000000000000000000 ) ) ;
#5185 = CARTESIAN_POINT ( 'NONE',  ( 5.000000000000000000, -91.29166666393547303, -2.886751345948129988 ) ) ;
#5186 = CARTESIAN_POINT ( 'NONE',  ( -3.152548672688508926E-16, -33.56249999863440792, -5.148502694627439702 ) ) ;
#5187 = CARTESIAN_POINT ( 'NONE',  ( 5.000000000000000000, -38.49999999999999289, -6.123233995736766282E-16 ) ) ;
#5188 = CARTESIAN_POINT ( 'NONE',  ( 5.000000000000000000, 25.62500000273118417, -6.123233995736766282E-16 ) ) ;
#5189 = CARTESIAN_POINT ( 'NONE',  ( 2.499999999999998668, -69.33333333333332860, -4.330127018922193649 ) ) ;
#5190 = CARTESIAN_POINT ( 'NONE',  ( -4.458734125000000326, -154.1250000013655779, 1.846868145590734089 ) ) ;
#5191 = CARTESIAN_POINT ( 'NONE',  ( -3.535250795749689387E-16, -43.24999999999999289, -5.773502691896257311 ) ) ;
#5192 = CARTESIAN_POINT ( 'NONE',  ( -59.80389192646541119, -135.0000000000000853, 0.7536779647045089847 ) ) ;
#5193 = ORIENTED_EDGE ( 'NONE', *, *, #9420, .F. ) ;
#5194 = CARTESIAN_POINT ( 'NONE',  ( -4.458734124999998549, -100.2291666653010509, 2.574251347313722516 ) ) ;
#5195 = CARTESIAN_POINT ( 'NONE',  ( -2.229367062499996610, 5.604166668032261711, 3.861377020970582219 ) ) ;
#5196 = CARTESIAN_POINT ( 'NONE',  ( 0.000000000000000000, -170.0000000000000000, 0.000000000000000000 ) ) ;
#5197 = CARTESIAN_POINT ( 'NONE',  ( 2.500000000000002220, -1.666666666666663410, 4.330127018922192761 ) ) ;
#5198 = CARTESIAN_POINT ( 'NONE',  ( 4.458734124999999437, -68.81249999863439371, -5.460374474430324690E-16 ) ) ;
#5199 = CARTESIAN_POINT ( 'NONE',  ( -6.972266317189433020E-16, 19.75000000000000000, -5.000000000000000000 ) ) ;
#5200 = CARTESIAN_POINT ( 'NONE',  ( 1.060575238724906964E-15, -0.6249999972688138339, 5.773502691896257311 ) ) ;
#5202 = ORIENTED_EDGE ( 'NONE', *, *, #13548, .T. ) ;
#5201 = CARTESIAN_POINT ( 'NONE',  ( 2.229367062499998831, -34.64583333196772941, -3.861377020970580887 ) ) ;
#5203 = CYLINDRICAL_SURFACE ( 'NONE', #18360, 5.000000000000000000 ) ;
#5204 = DIRECTION ( 'NONE',  ( -0.000000000000000000, 1.000000000000000000, -0.000000000000000000 ) ) ;
#5205 = VERTEX_POINT ( 'NONE', #36860 ) ;
#5206 = CARTESIAN_POINT ( 'NONE',  ( 5.000000000000000888, -51.58333333333332149, 2.886751345948126879 ) ) ;
#5208 = CARTESIAN_POINT ( 'NONE',  ( -2.229367062499996610, -24.39583333196773651, 3.861377020970582219 ) ) ;
#5207 = CYLINDRICAL_SURFACE ( 'NONE', #34656, 5.000000000000000000 ) ;
#5209 = CARTESIAN_POINT ( 'NONE',  ( -6.972266317189433020E-16, -81.24999999999998579, -5.000000000000000000 ) ) ;
#5210 = CARTESIAN_POINT ( 'NONE',  ( -4.458734124999999437, -72.39583333196775072, -2.574251347313719407 ) ) ;
#5211 = CARTESIAN_POINT ( 'NONE',  ( 4.458734124999999437, -142.7500000013656063, 1.846868145590737864 ) ) ;
#5212 = CARTESIAN_POINT ( 'NONE',  ( 9.457646018065525792E-16, -83.06249999863439371, 5.148502694627439702 ) ) ;
#5213 = CARTESIAN_POINT ( 'NONE',  ( -57.89159099828107458, -140.9375000013656063, -3.393966926194107447 ) ) ;
#5214 =( BOUNDED_CURVE ( )  B_SPLINE_CURVE ( 2, ( #32754, #57215, #12814, #57529, #47540, #56894, #42080, #13451, #23104 ),
 .UNSPECIFIED., .F., .F. ) 
 B_SPLINE_CURVE_WITH_KNOTS ( ( 3, 2, 2, 2, 3 ),
 ( 0.5982142857142856984, 0.5988095238095237915, 0.5999999999999999778, 0.6011904761904761640, 0.6017857142857142572 ),
 .UNSPECIFIED. ) 
 CURVE ( )  GEOMETRIC_REPRESENTATION_ITEM ( )  RATIONAL_B_SPLINE_CURVE ( ( 0.9330127018922194093, 0.9330127018922194093, 1.000000000000000000, 0.8660254037844387076, 1.000000000000000000, 0.8660254037844387076, 1.000000000000000000, 0.9330127018922194093, 0.9330127018922194093 ) ) 
 REPRESENTATION_ITEM ( '' )  );
#5215 = CARTESIAN_POINT ( 'NONE',  ( -2.229367062499996610, -29.39583333196774007, 3.861377020970582219 ) ) ;
#5216 = CARTESIAN_POINT ( 'NONE',  ( -4.999999999999999112, -73.79166666393547303, 2.886751345948131764 ) ) ;
#5217 = ORIENTED_EDGE ( 'NONE', *, *, #31984, .F. ) ;
#5218 = DIRECTION ( 'NONE',  ( -0.000000000000000000, 1.000000000000000000, -0.000000000000000000 ) ) ;
#5219 = ORIENTED_EDGE ( 'NONE', *, *, #16937, .F. ) ;
#5220 = CARTESIAN_POINT ( 'NONE',  ( -2.229367062499996610, -72.39583333196773651, 3.861377020970582219 ) ) ;
#5221 = CARTESIAN_POINT ( 'NONE',  ( -58.24261429053147765, -150.2500000000000284, -3.805975901505573855 ) ) ;
#5222 = CARTESIAN_POINT ( 'NONE',  ( 0.000000000000000000, 0.000000000000000000, 0.000000000000000000 ) ) ;
#5223 = EDGE_LOOP ( 'NONE', ( #33673, #19911, #54933, #8223 ) ) ;
#5224 = CARTESIAN_POINT ( 'NONE',  ( -55.00000000000002132, -155.0000000000000284, 1.734723475976807094E-15 ) ) ;
#5225 = AXIS2_PLACEMENT_3D ( 'NONE', #12714, #42297, #61937 ) ;
#5226 = CARTESIAN_POINT ( 'NONE',  ( -3.152548672688508926E-16, -58.81249999863440081, -5.148502694627439702 ) ) ;
#5227 = CARTESIAN_POINT ( 'NONE',  ( 4.458734124999998549, -2.979166665301069994, -2.574251347313721627 ) ) ;
#5228 = ORIENTED_EDGE ( 'NONE', *, *, #42909, .F. ) ;
#5229 =( BOUNDED_CURVE ( )  B_SPLINE_CURVE ( 2, ( #36501, #6602, #46476, #36192, #61279, #31993, #7251, #55813, #37150 ),
 .UNSPECIFIED., .F., .F. ) 
 B_SPLINE_CURVE_WITH_KNOTS ( ( 3, 2, 2, 2, 3 ),
 ( 0.6482142857142857428, 0.6488095238095238360, 0.6500000000000000222, 0.6511904761904762085, 0.6517857142857143016 ),
 .UNSPECIFIED. ) 
 CURVE ( )  GEOMETRIC_REPRESENTATION_ITEM ( )  RATIONAL_B_SPLINE_CURVE ( ( 0.9330127018922194093, 0.9330127018922194093, 1.000000000000000000, 0.8660254037844387076, 1.000000000000000000, 0.8660254037844387076, 1.000000000000000000, 0.9330127018922194093, 0.9330127018922194093 ) ) 
 REPRESENTATION_ITEM ( '' )  );
#5230 = ADVANCED_FACE ( 'NONE', ( #37181 ), #37808, .T. ) ;
#5231 = DIRECTION ( 'NONE',  ( -0.000000000000000000, 1.000000000000000000, -0.000000000000000000 ) ) ;
#5232 = CYLINDRICAL_SURFACE ( 'NONE', #55149, 5.000000000000000000 ) ;
#5233 = CARTESIAN_POINT ( 'NONE',  ( 4.458734124999999437, 12.18750000136559564, -5.460374474430324690E-16 ) ) ;
#5234 = CARTESIAN_POINT ( 'NONE',  ( -59.29741812935640155, -139.6250000013655779, -2.196230717870135685 ) ) ;
#5235 = CARTESIAN_POINT ( 'NONE',  ( 5.000000000000000000, -24.50000000000000000, -6.123233995736766282E-16 ) ) ;
#5236 = CARTESIAN_POINT ( 'NONE',  ( -1.846868145590734756, -166.1250000013656063, -4.458734124999999437 ) ) ;
#5237 = VERTEX_POINT ( 'NONE', #17235 ) ;
#5238 = CARTESIAN_POINT ( 'NONE',  ( -2.229367062499996610, -83.14583333196773651, 3.861377020970582219 ) ) ;
#5239 = CARTESIAN_POINT ( 'NONE',  ( -3.535533905932737309, -153.6250000000000000, -3.535533905932738197 ) ) ;
#5240 = CARTESIAN_POINT ( 'NONE',  ( 4.458734125000001214, 4.104166668032260823, 2.574251347313718519 ) ) ;
#5241 = CARTESIAN_POINT ( 'NONE',  ( 2.500000000000002220, -84.66666666666667140, 4.330127018922192761 ) ) ;
#5242 = CARTESIAN_POINT ( 'NONE',  ( 4.458734124999999437, -67.06249999863440792, -5.460374474430324690E-16 ) ) ;
#5243 = CARTESIAN_POINT ( 'NONE',  ( -2.499999999999996447, -24.70833333060214443, 4.330127018922195425 ) ) ;
#5244 = CARTESIAN_POINT ( 'NONE',  ( -2.500000000000000444, -29.16666666666666785, -4.330127018922193649 ) ) ;
#5245 = CARTESIAN_POINT ( 'NONE',  ( 4.458734125000000326, 28.10416666803225993, 2.574251347313718519 ) ) ;
#5246 = CARTESIAN_POINT ( 'NONE',  ( -1.339745962155613812, -65.08034179853029855, -5.000000000000000000 ) ) ;
#5247 = CARTESIAN_POINT ( 'NONE',  ( 6.158835246850667461E-14, -3.124999997268814944, -4.999999999999999112 ) ) ;
#5248 = EDGE_CURVE ( 'NONE', #27379, #22002, #36533, .T. ) ;
#5249 = CARTESIAN_POINT ( 'NONE',  ( -4.458734124999999437, -47.39583333196774362, -2.574251347313719407 ) ) ;
#5250 = EDGE_CURVE ( 'NONE', #39875, #21118, #5667, .T. ) ;
#5251 = CARTESIAN_POINT ( 'NONE',  ( 4.458734125000000326, -34.14583333196772941, 2.574251347313718519 ) ) ;
#5252 = CARTESIAN_POINT ( 'NONE',  ( 4.458734124999998549, 5.020833334698926897, -2.574251347313721627 ) ) ;
#5253 = CARTESIAN_POINT ( 'NONE',  ( -9.184850993605147944E-16, -151.2500000000000284, 5.000000000000000000 ) ) ;
#5254 = CARTESIAN_POINT ( 'NONE',  ( 1.060575238724906964E-15, 21.24999999999999645, 5.773502691896257311 ) ) ;
#5255 = EDGE_CURVE ( 'NONE', #61639, #47219, #12249, .T. ) ;
#5256 = CARTESIAN_POINT ( 'NONE',  ( 3.535533905932738197, -149.0000000027311842, -3.535533905932738197 ) ) ;
#5257 = CARTESIAN_POINT ( 'NONE',  ( 5.000000000000000000, -54.29166666393549434, -2.886751345948130876 ) ) ;
#5258 = CARTESIAN_POINT ( 'NONE',  ( 4.458734124999999437, -34.81249999863440792, -5.460374474430324690E-16 ) ) ;
#5259 = CARTESIAN_POINT ( 'NONE',  ( -4.999999999999999112, -72.79166666393547303, 2.886751345948131764 ) ) ;
#5260 = CARTESIAN_POINT ( 'NONE',  ( -56.48576386720575471, -144.0000000013656063, -4.591703134518078322 ) ) ;
#5261 = CARTESIAN_POINT ( 'NONE',  ( 0.000000000000000000, -170.0000000000000000, 0.000000000000000000 ) ) ;
#5262 = ADVANCED_FACE ( 'NONE', ( #56806 ), #20206, .T. ) ;
#5263 = CARTESIAN_POINT ( 'NONE',  ( -7.500000000000000000, -4.330127018922198090, -7.422398894150034288 ) ) ;
#5264 = CARTESIAN_POINT ( 'NONE',  ( 4.458734124999998549, -78.97916666530106511, -2.574251347313721627 ) ) ;
#5265 = CARTESIAN_POINT ( 'NONE',  ( -3.152801135295367096, -164.3125000013656063, -3.152801135295367541 ) ) ;
#5266 = CARTESIAN_POINT ( 'NONE',  ( 4.458734125000000326, -36.89583333196773651, 2.574251347313718519 ) ) ;
#5267 = DIRECTION ( 'NONE',  ( 0.000000000000000000, 0.000000000000000000, 1.000000000000000000 ) ) ;
#5268 = CARTESIAN_POINT ( 'NONE',  ( 5.000000000000000000, -23.50000000000000000, -6.123233995736766282E-16 ) ) ;
#5269 = CARTESIAN_POINT ( 'NONE',  ( 4.458734125000000326, -142.3750000013656063, -1.846868145590734978 ) ) ;
#5270 = VERTEX_POINT ( 'NONE', #3403 ) ;
#5271 = CARTESIAN_POINT ( 'NONE',  ( 4.458734124999998549, 28.02083333469892779, -2.574251347313721627 ) ) ;
#5272 = ORIENTED_EDGE ( 'NONE', *, *, #34846, .F. ) ;
#5273 = CARTESIAN_POINT ( 'NONE',  ( -2.229367062499996610, -61.39583333196774362, 3.861377020970582219 ) ) ;
#5274 = CARTESIAN_POINT ( 'NONE',  ( -3.535250795749689387E-16, 19.87500000273118417, -5.773502691896257311 ) ) ;
#5275 = CARTESIAN_POINT ( 'NONE',  ( -6.972266317189433020E-16, -48.12499999726880873, -5.000000000000000000 ) ) ;
#5276 = CARTESIAN_POINT ( 'NONE',  ( -2.500000000000000444, 15.83333333333333037, -4.330127018922193649 ) ) ;
#5277 = VECTOR ( 'NONE', #27237, 1000.000000000000000 ) ;
#5278 = CARTESIAN_POINT ( 'NONE',  ( -4.458734124999999437, -52.31249999863440792, 0.000000000000000000 ) ) ;
#5279 = CARTESIAN_POINT ( 'NONE',  ( -2.229367062499996610, -7.145833331967735624, 3.861377020970582219 ) ) ;
#5280 = CARTESIAN_POINT ( 'NONE',  ( -1.339745962155613812, 3.794658198738521282, -5.000000000000000000 ) ) ;
#5281 = CARTESIAN_POINT ( 'NONE',  ( -2.500000000000000444, -9.166666666666662522, -4.330127018922193649 ) ) ;
#5282 = DIRECTION ( 'NONE',  ( -0.000000000000000000, 1.000000000000000000, -0.000000000000000000 ) ) ;
#5283 = CARTESIAN_POINT ( 'NONE',  ( -4.999999999999998224, -9.916666666666662522, 2.886751345948131764 ) ) ;
#5284 = VECTOR ( 'NONE', #17882, 1000.000000000000000 ) ;
#5287 = CARTESIAN_POINT ( 'NONE',  ( 2.229367062500001939, -21.97916666530107221, 3.861377020970579999 ) ) ;
#5286 =( BOUNDED_CURVE ( )  B_SPLINE_CURVE ( 2, ( #30713, #59675, #45186, #54845, #40675, #36493, #20435, #15922, #1152 ),
 .UNSPECIFIED., .F., .F. ) 
 B_SPLINE_CURVE_WITH_KNOTS ( ( 3, 2, 2, 2, 3 ),
 ( 0.4729166666666666519, 0.4736111111111110938, 0.4749999999999999778, 0.4763888888888888618, 0.4770833333333333592 ),
 .UNSPECIFIED. ) 
 CURVE ( )  GEOMETRIC_REPRESENTATION_ITEM ( )  RATIONAL_B_SPLINE_CURVE ( ( 0.9330127018922194093, 0.9330127018922194093, 1.000000000000000000, 0.8660254037844387076, 1.000000000000000000, 0.8660254037844387076, 1.000000000000000000, 0.9330127018922167448, 0.9330127018922194093 ) ) 
 REPRESENTATION_ITEM ( '' )  );
#5285 = CARTESIAN_POINT ( 'NONE',  ( -58.80597590150559739, -151.0000000000000284, 3.242614290531460330 ) ) ;
#5288 = CARTESIAN_POINT ( 'NONE',  ( -58.24261429053147765, -135.2500000000000284, -3.805975901505573855 ) ) ;
#5289 = CARTESIAN_POINT ( 'NONE',  ( -4.458734124999999437, -54.39583333196773651, -2.574251347313719407 ) ) ;
#5290 = CARTESIAN_POINT ( 'NONE',  ( -8.190561711645485556E-16, -154.9375000013655779, 4.458734124999999437 ) ) ;
#5291 = CARTESIAN_POINT ( 'NONE',  ( -5.000000000000000000, -54.95833333060213732, -2.886751345948128211 ) ) ;
#5292 = VERTEX_POINT ( 'NONE', #23019 ) ;
#5293 = CARTESIAN_POINT ( 'NONE',  ( 1.975475456537005874E-15, -48.74999999999999289, 5.000000000000000000 ) ) ;
#5294 = CARTESIAN_POINT ( 'NONE',  ( 9.457646018065525792E-16, 3.687500001365594748, 5.148502694627439702 ) ) ;
#5295 = ORIENTED_EDGE ( 'NONE', *, *, #1204, .T. ) ;
#5297 = CARTESIAN_POINT ( 'NONE',  ( 3.044556291839386294E-14, 11.87500000273118417, -5.000000000000000000 ) ) ;
#5296 = CARTESIAN_POINT ( 'NONE',  ( 2.499999999999998668, -56.33333333333333570, -4.330127018922193649 ) ) ;
#5298 = CARTESIAN_POINT ( 'NONE',  ( 3.152801135295367541, -156.3125000013656063, -3.152801135295367541 ) ) ;
#5299 = EDGE_LOOP ( 'NONE', ( #56424, #10490, #36132, #61597 ) ) ;
#5300 = CARTESIAN_POINT ( 'NONE',  ( -75.00000000000002842, 15.00000000000000000, -5.000000000000000000 ) ) ;
#5301 = CARTESIAN_POINT ( 'NONE',  ( -51.75738570946856498, -129.7500000000000284, 3.805975901505576964 ) ) ;
#5302 = CARTESIAN_POINT ( 'NONE',  ( 0.000000000000000000, -120.0000000000000000, 0.000000000000000000 ) ) ;
#5303 = CARTESIAN_POINT ( 'NONE',  ( -4.458734124999999437, -41.64583333196773651, -2.574251347313719407 ) ) ;
#5304 = VERTEX_POINT ( 'NONE', #42622 ) ;
#5305 = DIRECTION ( 'NONE',  ( 0.000000000000000000, 0.000000000000000000, 1.000000000000000000 ) ) ;
#5306 = CARTESIAN_POINT ( 'NONE',  ( 2.229367062499998831, 12.35416666803226171, -3.861377020970580887 ) ) ;
#5307 = CARTESIAN_POINT ( 'NONE',  ( 6.123233995736766282E-16, -170.0000000000000000, -5.000000000000000000 ) ) ;
#5308 = VERTEX_POINT ( 'NONE', #62260 ) ;
#5309 = CARTESIAN_POINT ( 'NONE',  ( 4.458734125000001214, 29.10416666803225993, 2.574251347313718519 ) ) ;
#5310 = CARTESIAN_POINT ( 'NONE',  ( -50.40829686548195099, -152.0000000013655779, -1.485763867205728284 ) ) ;
#5311 = FACE_OUTER_BOUND ( 'NONE', #50057, .T. ) ;
#5312 = DIRECTION ( 'NONE',  ( -0.000000000000000000, 1.000000000000000000, -0.000000000000000000 ) ) ;
#5313 =( BOUNDED_CURVE ( )  B_SPLINE_CURVE ( 2, ( #59547, #24249, #33591, #20946, #15482, #19096, #14281, #9144, #13659 ),
 .UNSPECIFIED., .F., .F. ) 
 B_SPLINE_CURVE_WITH_KNOTS ( ( 3, 2, 2, 2, 3 ),
 ( 0.5625000000000000000, 0.5630952380952380931, 0.5642857142857142794, 0.5654761904761904656, 0.5660714285714285587 ),
 .UNSPECIFIED. ) 
 CURVE ( )  GEOMETRIC_REPRESENTATION_ITEM ( )  RATIONAL_B_SPLINE_CURVE ( ( 0.9330127018922194093, 0.9330127018922194093, 1.000000000000000000, 0.8660254037844387076, 1.000000000000000000, 0.8660254037844387076, 1.000000000000000000, 0.9330127018922194093, 0.9330127018922194093 ) ) 
 REPRESENTATION_ITEM ( '' )  );
#5314 = CARTESIAN_POINT ( 'NONE',  ( 5.000000000000000000, -169.0000000000000000, 0.000000000000000000 ) ) ;
#5315 = CARTESIAN_POINT ( 'NONE',  ( -4.458734124999999437, -66.39583333196773651, -2.574251347313719407 ) ) ;
#5316 = CARTESIAN_POINT ( 'NONE',  ( -59.81910112700026616, -146.1875000000000000, -2.462841084822510851 ) ) ;
#5317 = CARTESIAN_POINT ( 'NONE',  ( -4.458734124999999437, 19.60416666803225993, -2.574251347313719407 ) ) ;
#5318 = CARTESIAN_POINT ( 'NONE',  ( 1.339745962155612702, -33.29465819873851729, -5.000000000000000000 ) ) ;
#5319 = CARTESIAN_POINT ( 'NONE',  ( -2.229367062499996610, -47.39583333196774362, 3.861377020970582219 ) ) ;
#5320 = CARTESIAN_POINT ( 'NONE',  ( 2.499999999999998668, -8.208333330602144429, -4.330127018922193649 ) ) ;
#5321 = CARTESIAN_POINT ( 'NONE',  ( -5.000000000000000000, 5.000000000000000888, 0.000000000000000000 ) ) ;
#5322 = CARTESIAN_POINT ( 'NONE',  ( -6.972266317189433020E-16, -67.12499999726881583, -5.000000000000000000 ) ) ;
#5323 = CARTESIAN_POINT ( 'NONE',  ( -2.229367062500000163, -89.72916666530106511, -3.861377020970580443 ) ) ;
#5324 = CARTESIAN_POINT ( 'NONE',  ( 4.458734124999999437, -107.8124999986343937, -5.460374474430324690E-16 ) ) ;
#5325 = VECTOR ( 'NONE', #49906, 1000.000000000000000 ) ;
#5326 = CARTESIAN_POINT ( 'NONE',  ( -2.229367062500000163, -13.72916666530107221, -3.861377020970580443 ) ) ;
#5327 = ORIENTED_EDGE ( 'NONE', *, *, #61815, .T. ) ;
#5328 =( BOUNDED_CURVE ( )  B_SPLINE_CURVE ( 2, ( #12991, #46777, #32614, #2723, #56760, #47717, #12682, #52240, #22345 ),
 .UNSPECIFIED., .F., .F. ) 
 B_SPLINE_CURVE_WITH_KNOTS ( ( 3, 2, 2, 2, 3 ),
 ( 0.2803571428571428603, 0.2809523809523809534, 0.2821428571428571397, 0.2833333333333333259, 0.2839285714285714191 ),
 .UNSPECIFIED. ) 
 CURVE ( )  GEOMETRIC_REPRESENTATION_ITEM ( )  RATIONAL_B_SPLINE_CURVE ( ( 0.9330127018922194093, 0.9330127018922194093, 1.000000000000000000, 0.8660254037844387076, 1.000000000000000000, 0.8660254037844387076, 1.000000000000000000, 0.9330127018922194093, 0.9330127018922194093 ) ) 
 REPRESENTATION_ITEM ( '' )  );
#5329 = CARTESIAN_POINT ( 'NONE',  ( -1.339745962155613812, -47.08034179853029144, -5.000000000000000000 ) ) ;
#5330 = CARTESIAN_POINT ( 'NONE',  ( -4.458734124999998549, -100.2291666653010509, 2.574251347313722516 ) ) ;
#5331 = CARTESIAN_POINT ( 'NONE',  ( -5.000000000000000888, -160.6875000027311842, -2.071067811865475949 ) ) ;
#5332 = CARTESIAN_POINT ( 'NONE',  ( -2.229367062499996610, -97.39583333196773651, 3.861377020970582219 ) ) ;
#5333 = CARTESIAN_POINT ( 'NONE',  ( 1.975475456537005874E-15, -49.62499999726880873, 5.000000000000000000 ) ) ;
#5334 = CARTESIAN_POINT ( 'NONE',  ( 5.000000000000000888, -57.45833333060214443, 2.886751345948126879 ) ) ;
#5335 = DIRECTION ( 'NONE',  ( -0.000000000000000000, 1.000000000000000000, -0.000000000000000000 ) ) ;
#5336 = CARTESIAN_POINT ( 'NONE',  ( -53.51423613279429503, -154.5000000013655779, 4.591703134518082763 ) ) ;
#5337 = CARTESIAN_POINT ( 'NONE',  ( -50.70258187064364108, -148.1250000013656063, 2.196230717870141014 ) ) ;
#5338 = CARTESIAN_POINT ( 'NONE',  ( -2.229367062500000163, -19.47916666530106866, -3.861377020970580443 ) ) ;
#5339 = CARTESIAN_POINT ( 'NONE',  ( -4.458734124999999437, 6.437500001365593860, 0.000000000000000000 ) ) ;
#5340 = CARTESIAN_POINT ( 'NONE',  ( -4.458734124999997661, -58.47916666530106511, 2.574251347313722516 ) ) ;
#5341 = DIRECTION ( 'NONE',  ( -0.000000000000000000, 1.000000000000000000, -0.000000000000000000 ) ) ;
#5342 = CARTESIAN_POINT ( 'NONE',  ( -3.152548672688508926E-16, -18.56249999863440792, -5.148502694627439702 ) ) ;
#5343 = CARTESIAN_POINT ( 'NONE',  ( -1.127183054612291972E-14, 23.25000000000000000, 4.999999999999999112 ) ) ;
#5344 = CARTESIAN_POINT ( 'NONE',  ( -5.000000000000000000, -155.5000000000000000, -6.123233995736766282E-16 ) ) ;
#5345 = CARTESIAN_POINT ( 'NONE',  ( 5.000000000000000000, -4.499999999999997335, -6.123233995736766282E-16 ) ) ;
#5346 = ORIENTED_EDGE ( 'NONE', *, *, #1728, .T. ) ;
#5347 = CARTESIAN_POINT ( 'NONE',  ( -2.229367062500000163, -46.72916666530106511, -3.861377020970580443 ) ) ;
#5348 = CARTESIAN_POINT ( 'NONE',  ( -6.972266317189433020E-16, 25.74999999999999645, -5.000000000000000000 ) ) ;
#5349 = CARTESIAN_POINT ( 'NONE',  ( 5.000000000000000888, -66.58333333333332860, 2.886751345948126879 ) ) ;
#5350 = CARTESIAN_POINT ( 'NONE',  ( 9.457646018065525792E-16, -89.06249999863439371, 5.148502694627439702 ) ) ;
#5351 = CARTESIAN_POINT ( 'NONE',  ( 4.458734124999999437, -91.81249999863440792, -5.460374474430324690E-16 ) ) ;
#5352 = CARTESIAN_POINT ( 'NONE',  ( -2.229367062500000163, 17.27083333469892779, -3.861377020970580443 ) ) ;
#5353 = CARTESIAN_POINT ( 'NONE',  ( -4.458734124999998549, 7.770833334698925121, 2.574251347313722516 ) ) ;
#5354 = CARTESIAN_POINT ( 'NONE',  ( -6.972266317189433020E-16, -48.24999999999999289, -5.000000000000000000 ) ) ;
#5355 = CARTESIAN_POINT ( 'NONE',  ( -9.184850993605147944E-16, -165.3750000027312126, 5.000000000000000000 ) ) ;
#5356 = CARTESIAN_POINT ( 'NONE',  ( -2.229367062499996610, 21.60416666803226349, 3.861377020970582219 ) ) ;
#5357 = CARTESIAN_POINT ( 'NONE',  ( 5.000000000000000888, -77.58333333333334281, 2.886751345948126879 ) ) ;
#5358 = CARTESIAN_POINT ( 'NONE',  ( -2.499999999999996447, 9.291666669397853795, 4.330127018922195425 ) ) ;
#5359 = ORIENTED_EDGE ( 'NONE', *, *, #46706, .T. ) ;
#5360 = DIRECTION ( 'NONE',  ( -0.000000000000000000, 1.000000000000000000, -0.000000000000000000 ) ) ;
#5361 = ORIENTED_EDGE ( 'NONE', *, *, #55412, .T. ) ;
#5362 = CARTESIAN_POINT ( 'NONE',  ( 5.000000000000000000, -85.49999999999998579, -6.123233995736766282E-16 ) ) ;
#5363 = CARTESIAN_POINT ( 'NONE',  ( 2.229367062499998831, -40.64583333196773651, -3.861377020970580887 ) ) ;
#5364 = EDGE_CURVE ( 'NONE', #32593, #49211, #46190, .T. ) ;
#5365 = CARTESIAN_POINT ( 'NONE',  ( -5.000000000000000000, -39.95833333060213732, -2.886751345948128211 ) ) ;
#5366 = ORIENTED_EDGE ( 'NONE', *, *, #26102, .T. ) ;
#5367 = CARTESIAN_POINT ( 'NONE',  ( -59.44456063193725015, -146.8125000013656063, -0.3552334253322034230 ) ) ;
#5368 = CARTESIAN_POINT ( 'NONE',  ( -4.458734124999999437, -11.31249999863440792, 0.000000000000000000 ) ) ;
#5370 = ORIENTED_EDGE ( 'NONE', *, *, #6689, .F. ) ;
#5369 = CARTESIAN_POINT ( 'NONE',  ( -4.458734124999999437, -12.56249999863440259, 0.000000000000000000 ) ) ;
#5371 = CARTESIAN_POINT ( 'NONE',  ( 1.060575238724906964E-15, -82.75000000000001421, 5.773502691896257311 ) ) ;
#5372 = CARTESIAN_POINT ( 'NONE',  ( -3.152801135295367985, -168.8125000013656063, 3.152801135295367096 ) ) ;
#5373 = CARTESIAN_POINT ( 'NONE',  ( -2.229367062500000163, -64.72916666530106511, -3.861377020970580443 ) ) ;
#5374 = CARTESIAN_POINT ( 'NONE',  ( -2.499999999999996447, -83.70833333060214443, 4.330127018922195425 ) ) ;
#5376 = ORIENTED_EDGE ( 'NONE', *, *, #35458, .F. ) ;
#5375 = CARTESIAN_POINT ( 'NONE',  ( -2.500000000000000444, -32.16666666666666430, -4.330127018922193649 ) ) ;
#5377 = CARTESIAN_POINT ( 'NONE',  ( -53.33387254593733928, -143.8125000000000000, 5.149110718188519620 ) ) ;
#5378 = CARTESIAN_POINT ( 'NONE',  ( -3.152548672688508926E-16, -26.81249999863440436, -5.148502694627439702 ) ) ;
#5379 = CARTESIAN_POINT ( 'NONE',  ( 5.000000000000000000, -29.50000000000000000, -6.123233995736766282E-16 ) ) ;
#5380 = ORIENTED_EDGE ( 'NONE', *, *, #29018, .F. ) ;
#5381 = DIRECTION ( 'NONE',  ( 1.000000000000000000, 0.000000000000000000, 0.000000000000000000 ) ) ;
#5382 = CARTESIAN_POINT ( 'NONE',  ( 4.458734125000000326, -164.6250000013655779, -1.846868145590734978 ) ) ;
#5383 = CARTESIAN_POINT ( 'NONE',  ( 9.457646018065525792E-16, -105.3124999986344221, 5.148502694627439702 ) ) ;
#5384 = CARTESIAN_POINT ( 'NONE',  ( 1.339745962155612702, 20.70534180126147916, -5.000000000000000000 ) ) ;
#5385 = ORIENTED_EDGE ( 'NONE', *, *, #27823, .F. ) ;
#5386 = CARTESIAN_POINT ( 'NONE',  ( -50.40829686548195099, -146.2500000013656347, -1.485763867205728284 ) ) ;
#5387 = CARTESIAN_POINT ( 'NONE',  ( 4.458734124999998549, -72.97916666530107932, -2.574251347313721627 ) ) ;
#5388 = CARTESIAN_POINT ( 'NONE',  ( -54.60164318462004474, -136.5000000027312126, -4.984105922594373794 ) ) ;
#5389 = CARTESIAN_POINT ( 'NONE',  ( 9.457646018065525792E-16, -42.06249999863440081, 5.148502694627439702 ) ) ;
#5390 = CARTESIAN_POINT ( 'NONE',  ( -4.458734124999999437, -147.1875000013656063, -5.460374474430324690E-16 ) ) ;
#5391 = CARTESIAN_POINT ( 'NONE',  ( -7.500000000000000000, 1.644753667986373458, -7.029983668655349405 ) ) ;
#5392 = CARTESIAN_POINT ( 'NONE',  ( -2.499999999999996447, 28.16666666666666785, 4.330127018922195425 ) ) ;
#5393 = CARTESIAN_POINT ( 'NONE',  ( 4.458734124999999437, -10.81249999863440792, -5.460374474430324690E-16 ) ) ;
#5394 = CARTESIAN_POINT ( 'NONE',  ( -5.000000000000000000, -103.0833333333333428, -2.886751345948128211 ) ) ;
#5395 = ORIENTED_EDGE ( 'NONE', *, *, #23605, .F. ) ;
#5396 = CARTESIAN_POINT ( 'NONE',  ( -4.458734125000001214, -142.1250000013656063, 1.846868145590734089 ) ) ;
#5397 = CARTESIAN_POINT ( 'NONE',  ( 4.458734124999999437, -33.06249999863440792, -5.460374474430324690E-16 ) ) ;
#5398 = CARTESIAN_POINT ( 'NONE',  ( -4.999999999999999112, 7.208333336064517205, 2.886751345948131764 ) ) ;
#5399 = CARTESIAN_POINT ( 'NONE',  ( -5.000000000000000000, -53.08333333333332860, -2.886751345948128211 ) ) ;
#5400 = CARTESIAN_POINT ( 'NONE',  ( -51.60603307380591787, -133.9375000013656063, -2.891590998281053704 ) ) ;
#5401 = CARTESIAN_POINT ( 'NONE',  ( -2.229367062500000163, -71.72916666530107932, -3.861377020970580443 ) ) ;
#5402 = CARTESIAN_POINT ( 'NONE',  ( -2.071067811865562991, -144.4375000027311842, 4.999999999999913847 ) ) ;
#5403 = CARTESIAN_POINT ( 'NONE',  ( -2.500000000000000444, -70.16666666666667140, -4.330127018922193649 ) ) ;
#5404 = CARTESIAN_POINT ( 'NONE',  ( -4.458734124999999437, 1.354166668032261933, -2.574251347313719407 ) ) ;
#5405 = ORIENTED_EDGE ( 'NONE', *, *, #46516, .T. ) ;
#5406 = CARTESIAN_POINT ( 'NONE',  ( 5.000000000000000000, -30.50000000000000000, -6.123233995736766282E-16 ) ) ;
#5407 = CARTESIAN_POINT ( 'NONE',  ( 1.339745962155612702, -57.29465819873851729, -5.000000000000000000 ) ) ;
#5409 = CARTESIAN_POINT ( 'NONE',  ( 4.458734125000001214, -31.89583333196773651, 2.574251347313718519 ) ) ;
#5408 = CARTESIAN_POINT ( 'NONE',  ( 5.000000000000000000, -94.50000000000000000, -6.123233995736766282E-16 ) ) ;
#5410 = CARTESIAN_POINT ( 'NONE',  ( 4.458734124999998549, -79.97916666530107932, -2.574251347313721627 ) ) ;
#5411 = CARTESIAN_POINT ( 'NONE',  ( -4.458734124999997661, 19.52083333469893134, 2.574251347313722516 ) ) ;
#5412 = CARTESIAN_POINT ( 'NONE',  ( -6.972266317189433020E-16, -63.12499999726880873, -5.000000000000000000 ) ) ;
#5413 =( BOUNDED_CURVE ( )  B_SPLINE_CURVE ( 2, ( #22723, #7299, #16618, #27220, #13057, #42321, #3106, #41051, #16936 ),
 .UNSPECIFIED., .F., .F. ) 
 B_SPLINE_CURVE_WITH_KNOTS ( ( 3, 2, 2, 2, 3 ),
 ( 0.04107142857142857123, 0.04166666666666666435, 0.04285714285714285754, 0.04404761904761905073, 0.04464285714285714385 ),
 .UNSPECIFIED. ) 
 CURVE ( )  GEOMETRIC_REPRESENTATION_ITEM ( )  RATIONAL_B_SPLINE_CURVE ( ( 0.9330127018922194093, 0.9330127018922194093, 1.000000000000000000, 0.8660254037844387076, 1.000000000000000000, 0.8660254037844387076, 1.000000000000000000, 0.9330127018922194093, 0.9330127018922194093 ) ) 
 REPRESENTATION_ITEM ( '' )  );
#5414 = CARTESIAN_POINT ( 'NONE',  ( -58.39396692619412477, -138.4375000013656063, 2.891590998281057701 ) ) ;
#5415 = CARTESIAN_POINT ( 'NONE',  ( 2.229367062499998831, -2.645833331967738289, -3.861377020970580887 ) ) ;
#5416 = CARTESIAN_POINT ( 'NONE',  ( -4.458734124999999437, 22.35416666803225638, -2.574251347313719407 ) ) ;
#5417 = CARTESIAN_POINT ( 'NONE',  ( -4.458734124999999437, -41.56249999863440081, 0.000000000000000000 ) ) ;
#5418 = FACE_OUTER_BOUND ( 'NONE', #40906, .T. ) ;
#5419 = CARTESIAN_POINT ( 'NONE',  ( -4.458734124999999437, 1.687500001365593194, 0.000000000000000000 ) ) ;
#5420 = ORIENTED_EDGE ( 'NONE', *, *, #35544, .T. ) ;
#5421 = CARTESIAN_POINT ( 'NONE',  ( 4.458734124999998549, -31.97916666530107577, -2.574251347313721627 ) ) ;
#5422 = CARTESIAN_POINT ( 'NONE',  ( 2.229367062500001939, -75.97916666530106511, 3.861377020970579999 ) ) ;
#5423 = CARTESIAN_POINT ( 'NONE',  ( 2.499999999999998668, -107.2083333306021444, -4.330127018922193649 ) ) ;
#5424 = CARTESIAN_POINT ( 'NONE',  ( -2.229367062499996610, 27.85416666803225993, 3.861377020970582219 ) ) ;
#5425 = CARTESIAN_POINT ( 'NONE',  ( 1.975475456537005874E-15, -64.74999999999998579, 5.000000000000000000 ) ) ;
#5426 = CARTESIAN_POINT ( 'NONE',  ( -4.458734124999999437, -109.6458333319677365, -2.574251347313719407 ) ) ;
#5427 = CARTESIAN_POINT ( 'NONE',  ( -2.229367062499996610, -74.39583333196773651, 3.861377020970582219 ) ) ;
#5428 = CARTESIAN_POINT ( 'NONE',  ( -5.000000000000000000, -60.00000000000000000, 0.000000000000000000 ) ) ;
#5429 = CARTESIAN_POINT ( 'NONE',  ( 2.500000000000002220, -36.54166666393547303, 4.330127018922192761 ) ) ;
#5430 = CARTESIAN_POINT ( 'NONE',  ( -3.535250795749689387E-16, 25.87500000273118772, -5.773502691896257311 ) ) ;
#5431 = ORIENTED_EDGE ( 'NONE', *, *, #47833, .T. ) ;
#5432 = DIRECTION ( 'NONE',  ( -0.000000000000000000, 1.000000000000000000, -0.000000000000000000 ) ) ;
#5433 = CARTESIAN_POINT ( 'NONE',  ( 5.000000000000000888, -67.58333333333332860, 2.886751345948126879 ) ) ;
#5434 = CARTESIAN_POINT ( 'NONE',  ( -2.500000000000000444, -18.16666666666666430, -4.330127018922193649 ) ) ;
#5435 = CARTESIAN_POINT ( 'NONE',  ( 4.458734125000001214, -21.89583333196773296, 2.574251347313718519 ) ) ;
#5436 = EDGE_CURVE ( 'NONE', #10376, #41255, #21756, .T. ) ;
#5437 = CARTESIAN_POINT ( 'NONE',  ( -4.458734124999997661, -81.22916666530106511, 2.574251347313722516 ) ) ;
#5438 = CARTESIAN_POINT ( 'NONE',  ( -2.500000000000000444, -19.04166666393547658, -4.330127018922193649 ) ) ;
#5440 = VERTEX_POINT ( 'NONE', #28143 ) ;
#5439 = CARTESIAN_POINT ( 'NONE',  ( -4.458734124999999437, -51.31249999863440792, 0.000000000000000000 ) ) ;
#5441 = CARTESIAN_POINT ( 'NONE',  ( 2.499999999999998668, -35.20833333060213732, -4.330127018922193649 ) ) ;
#5442 = CARTESIAN_POINT ( 'NONE',  ( -2.500000000000000444, -28.04166666393548013, -4.330127018922193649 ) ) ;
#5444 = ORIENTED_EDGE ( 'NONE', *, *, #33469, .F. ) ;
#5443 = CARTESIAN_POINT ( 'NONE',  ( 4.458734124999998549, 0.02083333469892617584, -2.574251347313721627 ) ) ;
#5445 = CARTESIAN_POINT ( 'NONE',  ( -55.35523342533222291, -151.3125000013656063, 4.444560631937231499 ) ) ;
#5446 = CARTESIAN_POINT ( 'NONE',  ( 2.500000000000002220, -64.66666666666665719, 4.330127018922192761 ) ) ;
#5447 = CARTESIAN_POINT ( 'NONE',  ( -4.458734124999999437, -153.1875000013656063, -5.460374474430324690E-16 ) ) ;
#5448 = CARTESIAN_POINT ( 'NONE',  ( 4.458734124999999437, -42.06249999863440081, -5.460374474430324690E-16 ) ) ;
#5449 = CARTESIAN_POINT ( 'NONE',  ( 1.339745962155615144, -68.58034179853028434, 4.999999999999999112 ) ) ;
#5450 = CARTESIAN_POINT ( 'NONE',  ( 3.535533905932736864, -161.1250000000000284, 3.535533905932738641 ) ) ;
#5451 = CARTESIAN_POINT ( 'NONE',  ( -1.339745962155610925, 7.330341803992665994, 5.000000000000000000 ) ) ;
#5452 = CARTESIAN_POINT ( 'NONE',  ( -57.89159099828107458, -126.9375000013656063, -3.393966926194107447 ) ) ;
#5453 = CARTESIAN_POINT ( 'NONE',  ( 4.458734124999999437, -9.062499998634406140, -5.460374474430324690E-16 ) ) ;
#5454 = CARTESIAN_POINT ( 'NONE',  ( -4.458734124999999437, -46.64583333196774362, -2.574251347313719407 ) ) ;
#5455 = EDGE_CURVE ( 'NONE', #16461, #59581, #51700, .T. ) ;
#5456 = FACE_OUTER_BOUND ( 'NONE', #61812, .T. ) ;
#5457 = CARTESIAN_POINT ( 'NONE',  ( -4.458734125000000326, -145.0000000013656063, -1.846868145590735644 ) ) ;
#5458 = EDGE_CURVE ( 'NONE', #29318, #50188, #38121, .T. ) ;
#5459 = CARTESIAN_POINT ( 'NONE',  ( 9.457646018065525792E-16, -91.31249999863440792, 5.148502694627439702 ) ) ;
#5460 = CARTESIAN_POINT ( 'NONE',  ( -6.972266317189433020E-16, -107.2499999999999858, -5.000000000000000000 ) ) ;
#5461 =( BOUNDED_CURVE ( )  B_SPLINE_CURVE ( 2, ( #62403, #8671, #38557, #28284, #37949, #47897, #47592, #37625, #43694 ),
 .UNSPECIFIED., .F., .F. ) 
 B_SPLINE_CURVE_WITH_KNOTS ( ( 3, 2, 2, 2, 3 ),
 ( 0.9479166666666666297, 0.9486111111111110716, 0.9499999999999999556, 0.9513888888888888395, 0.9520833333333332815 ),
 .UNSPECIFIED. ) 
 CURVE ( )  GEOMETRIC_REPRESENTATION_ITEM ( )  RATIONAL_B_SPLINE_CURVE ( ( 0.9330127018922194093, 0.9330127018922194093, 1.000000000000000000, 0.8660254037844387076, 1.000000000000000000, 0.8660254037844387076, 1.000000000000000000, 0.9330127018922194093, 0.9330127018922194093 ) ) 
 REPRESENTATION_ITEM ( '' )  );
#5462 = ORIENTED_EDGE ( 'NONE', *, *, #3884, .F. ) ;
#5463 = CARTESIAN_POINT ( 'NONE',  ( -4.999999999999998224, -31.91666666666666430, 2.886751345948131764 ) ) ;
#5464 = CARTESIAN_POINT ( 'NONE',  ( -2.229367062499996610, 28.60416666803226349, 3.861377020970582219 ) ) ;
#5465 = CARTESIAN_POINT ( 'NONE',  ( -49.85088928181150436, -151.6875000027311842, -1.666127454062680702 ) ) ;
#5466 = CARTESIAN_POINT ( 'NONE',  ( 1.339745962155612702, -30.29465819873851729, -5.000000000000000000 ) ) ;
#5467 = VERTEX_POINT ( 'NONE', #4636 ) ;
#5468 = ADVANCED_FACE ( 'NONE', ( #33910 ), #9771, .F. ) ;
#5469 = CARTESIAN_POINT ( 'NONE',  ( 2.229367062500001939, 4.020833334698926009, 3.861377020970579999 ) ) ;
#5470 = CARTESIAN_POINT ( 'NONE',  ( -6.972266317189433020E-16, -50.12499999726881583, -5.000000000000000000 ) ) ;
#5471 = CARTESIAN_POINT ( 'NONE',  ( 9.457646018065525792E-16, -19.31249999863440792, 5.148502694627439702 ) ) ;
#5472 = CARTESIAN_POINT ( 'NONE',  ( -1.339745962155610925, -100.6696581960073331, 5.000000000000000000 ) ) ;
#5473 = CARTESIAN_POINT ( 'NONE',  ( 2.229367062499998831, -4.645833331967740065, -3.861377020970580887 ) ) ;
#5474 = DIRECTION ( 'NONE',  ( -0.000000000000000000, 1.000000000000000000, -0.000000000000000000 ) ) ;
#5475 = CARTESIAN_POINT ( 'NONE',  ( 2.730187237215162345E-16, -148.1875000013656063, -4.458734124999999437 ) ) ;
#5476 = CARTESIAN_POINT ( 'NONE',  ( -2.229367062499996610, 23.60416666803225993, 3.861377020970582219 ) ) ;
#5477 = ORIENTED_EDGE ( 'NONE', *, *, #18788, .T. ) ;
#5478 = CARTESIAN_POINT ( 'NONE',  ( 4.458734125000000326, -96.89583333196773651, 2.574251347313718519 ) ) ;
#5479 = FACE_OUTER_BOUND ( 'NONE', #12056, .T. ) ;
#5480 = CARTESIAN_POINT ( 'NONE',  ( -5.000000000000000000, -20.99999999999999645, 0.000000000000000000 ) ) ;
#5481 = CARTESIAN_POINT ( 'NONE',  ( -4.458734124999998549, -15.22916666530107754, 2.574251347313722516 ) ) ;
#5482 = CARTESIAN_POINT ( 'NONE',  ( 1.339745962155615144, -85.58034179853028434, 4.999999999999999112 ) ) ;
#5483 = DIRECTION ( 'NONE',  ( -0.000000000000000000, 1.000000000000000000, -0.000000000000000000 ) ) ;
#5484 = CARTESIAN_POINT ( 'NONE',  ( -55.35523342533222291, -151.3125000013656063, 4.444560631937231499 ) ) ;
#5485 = EDGE_CURVE ( 'NONE', #53762, #22221, #7088, .T. ) ;
#5486 = CARTESIAN_POINT ( 'NONE',  ( 5.000000000000000888, -40.45833333060214443, 2.886751345948126879 ) ) ;
#5487 = CARTESIAN_POINT ( 'NONE',  ( 1.975475456537005874E-15, -22.74999999999999645, 5.000000000000000000 ) ) ;
#5488 = CARTESIAN_POINT ( 'NONE',  ( 2.229367062499998831, 12.35416666803226171, -3.861377020970580887 ) ) ;
#5489 = CARTESIAN_POINT ( 'NONE',  ( -2.499999999999996447, -89.70833333060214443, 4.330127018922195425 ) ) ;
#5490 = DIRECTION ( 'NONE',  ( -0.000000000000000000, 1.000000000000000000, -0.000000000000000000 ) ) ;
#5491 = CARTESIAN_POINT ( 'NONE',  ( 2.229367062499998831, 16.35416666803225993, -3.861377020970580887 ) ) ;
#5492 = CARTESIAN_POINT ( 'NONE',  ( -4.458734124999998549, -60.22916666530106511, 2.574251347313722516 ) ) ;
#5493 = VERTEX_POINT ( 'NONE', #38419 ) ;
#5494 = CARTESIAN_POINT ( 'NONE',  ( 2.229367062499998831, -10.89583333196773829, -3.861377020970580887 ) ) ;
#5495 = CARTESIAN_POINT ( 'NONE',  ( -2.499999999999996447, 5.166666666666666963, 4.330127018922195425 ) ) ;
#5496 = CARTESIAN_POINT ( 'NONE',  ( -4.458734124999999437, -164.9375000013655779, -5.460374474430324690E-16 ) ) ;
#5497 = CARTESIAN_POINT ( 'NONE',  ( 3.061616997868383141E-16, -166.8750000027312126, -5.000000000000000000 ) ) ;
#5498 = CARTESIAN_POINT ( 'NONE',  ( -3.152548672688508926E-16, -53.56249999863439371, -5.148502694627439702 ) ) ;
#5499 = CARTESIAN_POINT ( 'NONE',  ( -2.499999999999996447, -89.70833333060214443, 4.330127018922195425 ) ) ;
#5500 = CARTESIAN_POINT ( 'NONE',  ( 2.229367062500001939, -32.97916666530106511, 3.861377020970579999 ) ) ;
#5501 = DIRECTION ( 'NONE',  ( 0.000000000000000000, 0.000000000000000000, 1.000000000000000000 ) ) ;
#5502 = CARTESIAN_POINT ( 'NONE',  ( -4.458734124999999437, -154.2500000013656063, -1.846868145590735644 ) ) ;
#5503 = CARTESIAN_POINT ( 'NONE',  ( -5.000000000000000000, -41.99999999999999289, 0.000000000000000000 ) ) ;
#5504 = CARTESIAN_POINT ( 'NONE',  ( -5.000000000000000000, -110.8749999972688016, 0.000000000000000000 ) ) ;
#5505 = DIRECTION ( 'NONE',  ( 0.000000000000000000, 0.000000000000000000, 1.000000000000000000 ) ) ;
#5506 = ORIENTED_EDGE ( 'NONE', *, *, #4027, .T. ) ;
#5507 = CARTESIAN_POINT ( 'NONE',  ( 4.458734125000001214, -98.89583333196775072, 2.574251347313718519 ) ) ;
#5508 = CARTESIAN_POINT ( 'NONE',  ( 9.457646018065525792E-16, 1.687500001365593194, 5.148502694627439702 ) ) ;
#5509 =( BOUNDED_CURVE ( )  B_SPLINE_CURVE ( 2, ( #12049, #41622, #10856, #3053, #2116, #59764, #22030, #30471, #32301 ),
 .UNSPECIFIED., .F., .F. ) 
 B_SPLINE_CURVE_WITH_KNOTS ( ( 3, 2, 2, 2, 3 ),
 ( 0.9749999999999998668, 0.9791666666666665186, 0.9833333333333331705, 0.9874999999999999334, 0.9916666666666665853 ),
 .UNSPECIFIED. ) 
 CURVE ( )  GEOMETRIC_REPRESENTATION_ITEM ( )  RATIONAL_B_SPLINE_CURVE ( ( 1.000000000000001998, 0.9238795325112847401, 1.000000000000000000, 0.9238795325112867385, 1.000000000000000000, 0.9238795325112867385, 1.000000000000000000, 0.9238795325112887369, 0.9999999999999980016 ) ) 
 REPRESENTATION_ITEM ( '' )  );
#5510 = CARTESIAN_POINT ( 'NONE',  ( 0.000000000000000000, -120.0000000000000000, 0.000000000000000000 ) ) ;
#5511 = CARTESIAN_POINT ( 'NONE',  ( 5.000000000000000888, -4.583333333333334814, 2.886751345948126879 ) ) ;
#5512 = EDGE_CURVE ( 'NONE', #6430, #63596, #49614, .T. ) ;
#5513 = CARTESIAN_POINT ( 'NONE',  ( 4.458734124999998549, -65.72916666530106511, -2.574251347313721627 ) ) ;
#5514 = VECTOR ( 'NONE', #57229, 1000.000000000000114 ) ;
#5515 = EDGE_CURVE ( 'NONE', #8855, #5467, #9154, .T. ) ;
#5516 = EDGE_CURVE ( 'NONE', #27844, #32427, #58675, .T. ) ;
#5517 = CARTESIAN_POINT ( 'NONE',  ( -3.535250795749689387E-16, -4.124999997268816720, -5.773502691896257311 ) ) ;
#5519 = EDGE_LOOP ( 'NONE', ( #51401, #36659, #50820, #39465 ) ) ;
#5518 = CARTESIAN_POINT ( 'NONE',  ( -4.458734124999999437, -35.39583333196773651, -2.574251347313719407 ) ) ;
#5520 = DIRECTION ( 'NONE',  ( 0.000000000000000000, 0.000000000000000000, 1.000000000000000000 ) ) ;
#5521 = CARTESIAN_POINT ( 'NONE',  ( -2.499999999999996447, -47.70833333060215153, 4.330127018922195425 ) ) ;
#5522 = ORIENTED_EDGE ( 'NONE', *, *, #1296, .F. ) ;
#5523 = CARTESIAN_POINT ( 'NONE',  ( 5.000000000000000888, -48.58333333333332149, 2.886751345948126879 ) ) ;
#5525 = CARTESIAN_POINT ( 'NONE',  ( -4.458734124999999437, -27.64583333196774007, -2.574251347313719407 ) ) ;
#5524 = DIRECTION ( 'NONE',  ( -0.000000000000000000, 1.000000000000000000, -0.000000000000000000 ) ) ;
#5526 = CARTESIAN_POINT ( 'NONE',  ( 5.000000000000000000, -4.499999999999997335, -6.123233995736766282E-16 ) ) ;
#5527 = CARTESIAN_POINT ( 'NONE',  ( -4.458734124999999437, -70.39583333196773651, -2.574251347313719407 ) ) ;
#5528 = CARTESIAN_POINT ( 'NONE',  ( 4.458734124999999437, -143.7500000013655779, 1.846868145590737864 ) ) ;
#5529 = CARTESIAN_POINT ( 'NONE',  ( 4.458734124999998549, -79.72916666530107932, -2.574251347313721627 ) ) ;
#5530 = CARTESIAN_POINT ( 'NONE',  ( -52.80376928212989185, -140.1250000013655779, -4.297418129356379346 ) ) ;
#5531 = ADVANCED_FACE ( 'NONE', ( #28768 ), #34217, .T. ) ;
#5532 = CARTESIAN_POINT ( 'NONE',  ( 4.458734124999998549, -31.97916666530107577, -2.574251347313721627 ) ) ;
#5533 = CARTESIAN_POINT ( 'NONE',  ( 2.500000000000002220, -73.54166666393548724, 4.330127018922192761 ) ) ;
#5534 = EDGE_LOOP ( 'NONE', ( #22129, #51968, #9111, #25877 ) ) ;
#5535 = CARTESIAN_POINT ( 'NONE',  ( 2.500000000000002220, -20.54166666393548013, 4.330127018922192761 ) ) ;
#5537 = EDGE_CURVE ( 'NONE', #34977, #43111, #40595, .T. ) ;
#5536 = ORIENTED_EDGE ( 'NONE', *, *, #40165, .F. ) ;
#5538 = CARTESIAN_POINT ( 'NONE',  ( -2.229367062500000163, -73.72916666530106511, -3.861377020970580443 ) ) ;
#5539 = DIRECTION ( 'NONE',  ( -0.000000000000000000, 1.000000000000000000, -0.000000000000000000 ) ) ;
#5540 =( NAMED_UNIT ( * ) PLANE_ANGLE_UNIT ( ) SI_UNIT ( $, .RADIAN. ) );
#5541 = ORIENTED_EDGE ( 'NONE', *, *, #48776, .T. ) ;
#5542 = CARTESIAN_POINT ( 'NONE',  ( -1.339745962155613812, -39.20534180126147561, -5.000000000000000000 ) ) ;
#5543 = CARTESIAN_POINT ( 'NONE',  ( -2.500000000000000444, -76.04166666393547303, -4.330127018922193649 ) ) ;
#5544 = CARTESIAN_POINT ( 'NONE',  ( 4.458734124999998549, -57.97916666530107221, -2.574251347313721627 ) ) ;
#5545 = CARTESIAN_POINT ( 'NONE',  ( 4.458734124999999437, -6.062499998634403475, -5.460374474430324690E-16 ) ) ;
#5546 = ORIENTED_EDGE ( 'NONE', *, *, #50260, .F. ) ;
#5547 = CARTESIAN_POINT ( 'NONE',  ( -2.500000000000000444, -20.16666666666666430, -4.330127018922193649 ) ) ;
#5548 = DIRECTION ( 'NONE',  ( -0.000000000000000000, 1.000000000000000000, -0.000000000000000000 ) ) ;
#5549 = CARTESIAN_POINT ( 'NONE',  ( -2.229367062500000163, 15.52083333469892779, -3.861377020970580443 ) ) ;
#5550 = CARTESIAN_POINT ( 'NONE',  ( -52.80376928212989185, -142.8750000013656063, -4.297418129356379346 ) ) ;
#5551 = CARTESIAN_POINT ( 'NONE',  ( -5.000000000000000000, -1.000000000000000888, 0.000000000000000000 ) ) ;
#5552 = CARTESIAN_POINT ( 'NONE',  ( 2.730187237215162345E-16, -159.1875000013655779, -4.458734124999999437 ) ) ;
#5553 = CARTESIAN_POINT ( 'NONE',  ( 0.000000000000000000, -170.0000000000000000, 0.000000000000000000 ) ) ;
#5554 = ORIENTED_EDGE ( 'NONE', *, *, #59026, .F. ) ;
#5555 = CARTESIAN_POINT ( 'NONE',  ( 4.458734124999998549, -83.72916666530106511, -2.574251347313721627 ) ) ;
#5556 = CARTESIAN_POINT ( 'NONE',  ( 5.000000000000000000, -0.2916666639354824619, -2.886751345948130876 ) ) ;
#5557 = CARTESIAN_POINT ( 'NONE',  ( -2.229367062500000163, 0.5208333346989266754, -3.861377020970580443 ) ) ;
#5558 = CYLINDRICAL_SURFACE ( 'NONE', #63274, 5.000000000000000000 ) ;
#5559 = CARTESIAN_POINT ( 'NONE',  ( -2.500000000000000444, -84.16666666666667140, -4.330127018922193649 ) ) ;
#5560 = FACE_OUTER_BOUND ( 'NONE', #9988, .T. ) ;
#5561 = CARTESIAN_POINT ( 'NONE',  ( -4.458734124999999437, -66.64583333196773651, -2.574251347313719407 ) ) ;
#5562 = CARTESIAN_POINT ( 'NONE',  ( -3.535250795749689387E-16, -23.12499999726881228, -5.773502691896257311 ) ) ;
#5563 = CARTESIAN_POINT ( 'NONE',  ( -5.000000000000000000, -41.08333333333333570, -2.886751345948128211 ) ) ;
#5564 = CARTESIAN_POINT ( 'NONE',  ( -2.499999999999996447, -37.70833333060213732, 4.330127018922195425 ) ) ;
#5565 = CARTESIAN_POINT ( 'NONE',  ( 2.500000000000002220, -43.54166666393548013, 4.330127018922192761 ) ) ;
#5566 = CARTESIAN_POINT ( 'NONE',  ( 9.457646018065525792E-16, -44.06249999863439371, 5.148502694627439702 ) ) ;
#5567 = CARTESIAN_POINT ( 'NONE',  ( -2.229367062499996610, -33.39583333196772941, 3.861377020970582219 ) ) ;
#5568 = CARTESIAN_POINT ( 'NONE',  ( 2.229367062500001939, 4.770833334698926897, 3.861377020970579999 ) ) ;
#5569 = DIRECTION ( 'NONE',  ( 0.000000000000000000, 0.000000000000000000, 1.000000000000000000 ) ) ;
#5570 = CARTESIAN_POINT ( 'NONE',  ( -2.499999999999996447, 18.16666666666666430, 4.330127018922195425 ) ) ;
#5571 = CARTESIAN_POINT ( 'NONE',  ( 3.061616997868383141E-16, -148.8750000027312126, -5.000000000000000000 ) ) ;
#5572 = DIRECTION ( 'NONE',  ( -0.000000000000000000, 1.000000000000000000, -0.000000000000000000 ) ) ;
#5573 = CARTESIAN_POINT ( 'NONE',  ( -4.458734124999999437, -38.31249999863439371, 0.000000000000000000 ) ) ;
#5574 = CARTESIAN_POINT ( 'NONE',  ( 5.000000000000000000, -75.29166666393547303, -2.886751345948129988 ) ) ;
#5575 = CARTESIAN_POINT ( 'NONE',  ( -59.44456063193725015, -145.8125000013656063, -0.3552334253322034230 ) ) ;
#5576 = DIRECTION ( 'NONE',  ( -0.000000000000000000, 1.000000000000000000, -0.000000000000000000 ) ) ;
#5577 = CARTESIAN_POINT ( 'NONE',  ( 0.000000000000000000, -120.0000000000000000, 5.000000000000000000 ) ) ;
#5578 = CARTESIAN_POINT ( 'NONE',  ( 2.229367062499998831, -82.89583333196773651, -3.861377020970580887 ) ) ;
#5579 = CARTESIAN_POINT ( 'NONE',  ( -4.458734125000000326, -166.1250000013656063, 1.846868145590734089 ) ) ;
#5580 = CARTESIAN_POINT ( 'NONE',  ( -3.535533905932737309, -160.6250000000000284, -3.535533905932738197 ) ) ;
#5581 = CARTESIAN_POINT ( 'NONE',  ( 1.339745962155615144, -45.58034179853028434, 4.999999999999999112 ) ) ;
#5582 = CARTESIAN_POINT ( 'NONE',  ( -5.000000000000000000, -27.99999999999999645, 0.000000000000000000 ) ) ;
#5583 = CARTESIAN_POINT ( 'NONE',  ( 3.152801135295366208, -142.5625000013655779, 3.152801135295367985 ) ) ;
#5584 = ORIENTED_EDGE ( 'NONE', *, *, #62908, .T. ) ;
#5585 = CARTESIAN_POINT ( 'NONE',  ( -4.458734124999999437, 27.43750000136559208, 0.000000000000000000 ) ) ;
#5586 = ORIENTED_EDGE ( 'NONE', *, *, #55068, .T. ) ;
#5587 = CARTESIAN_POINT ( 'NONE',  ( 4.458734125000000326, -64.14583333196773651, 2.574251347313718519 ) ) ;
#5588 = CARTESIAN_POINT ( 'NONE',  ( -2.500000000000000444, 21.95833333606451987, -4.330127018922193649 ) ) ;
#5589 = CARTESIAN_POINT ( 'NONE',  ( -5.000000000000000000, -60.95833333060214443, -2.886751345948128211 ) ) ;
#5590 = CARTESIAN_POINT ( 'NONE',  ( -4.999999999999999112, 12.08333333333333037, 2.886751345948131764 ) ) ;
#5591 = APPLICATION_CONTEXT ( 'automotive_design' ) ;
#5592 =( BOUNDED_CURVE ( )  B_SPLINE_CURVE ( 2, ( #49355, #63526, #28785, #15264, #34888, #43565, #58691, #49030, #39691 ),
 .UNSPECIFIED., .F., .F. ) 
 B_SPLINE_CURVE_WITH_KNOTS ( ( 3, 2, 2, 2, 3 ),
 ( 0.3732142857142857206, 0.3738095238095238138, 0.3750000000000000000, 0.3761904761904761862, 0.3767857142857142794 ),
 .UNSPECIFIED. ) 
 CURVE ( )  GEOMETRIC_REPRESENTATION_ITEM ( )  RATIONAL_B_SPLINE_CURVE ( ( 0.9330127018922194093, 0.9330127018922194093, 1.000000000000000000, 0.8660254037844387076, 1.000000000000000000, 0.8660254037844387076, 1.000000000000000000, 0.9330127018922194093, 0.9330127018922194093 ) ) 
 REPRESENTATION_ITEM ( '' )  );
#5593 = CARTESIAN_POINT ( 'NONE',  ( 2.229367062499998831, -50.64583333196772941, -3.861377020970580887 ) ) ;
#5594 = CARTESIAN_POINT ( 'NONE',  ( -4.458734124999999437, -12.39583333196774184, -2.574251347313719407 ) ) ;
#5595 = CARTESIAN_POINT ( 'NONE',  ( -5.000000000000000000, -168.5000000000000000, -6.123233995736766282E-16 ) ) ;
#5596 = EDGE_CURVE ( 'NONE', #1202, #31117, #8488, .T. ) ;
#5597 = CARTESIAN_POINT ( 'NONE',  ( 1.975475456537005874E-15, -22.62499999726880873, 5.000000000000000000 ) ) ;
#5598 = CARTESIAN_POINT ( 'NONE',  ( 6.293430271071537518, -5.026740376715104652, -0.4524126574264552558 ) ) ;
#5599 = CARTESIAN_POINT ( 'NONE',  ( -1.339745962155610925, -79.66965819600731891, 5.000000000000000000 ) ) ;
#5600 = CARTESIAN_POINT ( 'NONE',  ( 1.339745962155615144, -74.70534180126148271, 4.999999999999999112 ) ) ;
#5602 = CARTESIAN_POINT ( 'NONE',  ( -4.458734124999999437, -22.31249999863440436, 0.000000000000000000 ) ) ;
#5601 = CARTESIAN_POINT ( 'NONE',  ( -53.33387254593727533, -150.8125000000000000, 5.149110718188522284 ) ) ;
#5603 = EDGE_CURVE ( 'NONE', #51386, #61158, #23712, .T. ) ;
#5604 = CARTESIAN_POINT ( 'NONE',  ( -5.000000000000000000, -77.95833333060214443, -2.886751345948128211 ) ) ;
#5605 = CARTESIAN_POINT ( 'NONE',  ( -4.458734124999999437, -56.31249999863440081, 0.000000000000000000 ) ) ;
#5606 = CARTESIAN_POINT ( 'NONE',  ( -3.152801135295367096, -155.3125000013656063, -3.152801135295367541 ) ) ;
#5607 = ADVANCED_FACE ( 'NONE', ( #790 ), #25535, .T. ) ;
#5608 = VECTOR ( 'NONE', #49659, 1000.000000000000000 ) ;
#5609 =( BOUNDED_CURVE ( )  B_SPLINE_CURVE ( 2, ( #30992, #39996, #21352, #1116, #11684, #40957, #16523, #20722, #55453 ),
 .UNSPECIFIED., .F., .F. ) 
 B_SPLINE_CURVE_WITH_KNOTS ( ( 3, 2, 2, 2, 3 ),
 ( 0.6553571428571428603, 0.6559523809523809534, 0.6571428571428571397, 0.6583333333333333259, 0.6589285714285714191 ),
 .UNSPECIFIED. ) 
 CURVE ( )  GEOMETRIC_REPRESENTATION_ITEM ( )  RATIONAL_B_SPLINE_CURVE ( ( 0.9330127018922194093, 0.9330127018922194093, 1.000000000000000000, 0.8660254037844387076, 1.000000000000000000, 0.8660254037844387076, 1.000000000000000000, 0.9330127018922194093, 0.9330127018922194093 ) ) 
 REPRESENTATION_ITEM ( '' )  );
#5610 = CARTESIAN_POINT ( 'NONE',  ( 1.060575238724906964E-15, -56.62499999726880162, 5.773502691896257311 ) ) ;
#5611 = EDGE_LOOP ( 'NONE', ( #59915, #55148, #5619, #18113 ) ) ;
#5612 = CARTESIAN_POINT ( 'NONE',  ( 1.339745962155612702, 13.70534180126148094, -5.000000000000000000 ) ) ;
#5613 = CARTESIAN_POINT ( 'NONE',  ( -4.458734124999998549, 2.520833334698928674, 2.574251347313722516 ) ) ;
#5614 = ORIENTED_EDGE ( 'NONE', *, *, #35780, .T. ) ;
#5616 = DIRECTION ( 'NONE',  ( 0.000000000000000000, 0.000000000000000000, 1.000000000000000000 ) ) ;
#5615 = CARTESIAN_POINT ( 'NONE',  ( 5.000000000000000888, -21.58333333333332860, 2.886751345948126879 ) ) ;
#5617 = CARTESIAN_POINT ( 'NONE',  ( -4.458734124999999437, -154.9375000013655779, -5.460374474430324690E-16 ) ) ;
#5618 = EDGE_CURVE ( 'NONE', #33683, #29077, #21354, .T. ) ;
#5619 = ORIENTED_EDGE ( 'NONE', *, *, #41684, .T. ) ;
#5620 = ADVANCED_FACE ( 'NONE', ( #39675 ), #59311, .T. ) ;
#5621 = CARTESIAN_POINT ( 'NONE',  ( -2.499999999999996447, 11.16666666666666430, 4.330127018922195425 ) ) ;
#5622 = CARTESIAN_POINT ( 'NONE',  ( -55.39835681537999790, -130.8750000000000284, 4.984105922594378235 ) ) ;
#5623 = CARTESIAN_POINT ( 'NONE',  ( 1.339745962155615144, -86.70534180126148271, 4.999999999999999112 ) ) ;
#5624 = CARTESIAN_POINT ( 'NONE',  ( 9.457646018065525792E-16, -44.31249999863440081, 5.148502694627439702 ) ) ;
#5625 = ORIENTED_EDGE ( 'NONE', *, *, #19746, .F. ) ;
#5626 = EDGE_CURVE ( 'NONE', #47522, #36723, #20723, .T. ) ;
#5627 = CYLINDRICAL_SURFACE ( 'NONE', #49055, 5.000000000000000000 ) ;
#5628 = CARTESIAN_POINT ( 'NONE',  ( -2.229367062499996610, 13.85416666803226171, 3.861377020970582219 ) ) ;
#5629 = CARTESIAN_POINT ( 'NONE',  ( -4.458734124999999437, -89.56249999863440792, 0.000000000000000000 ) ) ;
#5630 = CARTESIAN_POINT ( 'NONE',  ( -50.55543936806279248, -154.0625000013656347, 0.3552334253322060320 ) ) ;
#5631 = CARTESIAN_POINT ( 'NONE',  ( 2.499999999999998668, 12.79166666939785379, -4.330127018922193649 ) ) ;
#5632 = CARTESIAN_POINT ( 'NONE',  ( 0.000000000000000000, -170.0000000000000000, 0.000000000000000000 ) ) ;
#5633 = LINE ( 'NONE', #44859, #1457 ) ;
#5634 = CARTESIAN_POINT ( 'NONE',  ( 4.458734124999998549, -67.72916666530106511, -2.574251347313721627 ) ) ;
#5635 = CARTESIAN_POINT ( 'NONE',  ( -58.80597590150559739, -146.0000000000000284, 3.242614290531460330 ) ) ;
#5636 = CARTESIAN_POINT ( 'NONE',  ( 4.458734125000001214, 19.10416666803225638, 2.574251347313718519 ) ) ;
#5637 = CARTESIAN_POINT ( 'NONE',  ( 4.458734124999999437, -50.06249999863440792, -5.460374474430324690E-16 ) ) ;
#5638 = CARTESIAN_POINT ( 'NONE',  ( 1.060575238724906964E-15, -8.624999997268814056, 5.773502691896257311 ) ) ;
#5639 = CARTESIAN_POINT ( 'NONE',  ( 1.255007937094098239E-14, 24.75000000000000000, -4.999999999999999112 ) ) ;
#5640 = CARTESIAN_POINT ( 'NONE',  ( 0.000000000000000000, -170.0000000000000000, 0.000000000000000000 ) ) ;
#5641 = DIRECTION ( 'NONE',  ( -0.000000000000000000, 1.000000000000000000, -0.000000000000000000 ) ) ;
#5642 = CARTESIAN_POINT ( 'NONE',  ( 1.339745962155615144, -64.58034179853029855, 4.999999999999999112 ) ) ;
#5643 = CARTESIAN_POINT ( 'NONE',  ( -4.458734124999997661, -18.47916666530106511, 2.574251347313722516 ) ) ;
#5644 = VERTEX_POINT ( 'NONE', #34873 ) ;
#5645 = CARTESIAN_POINT ( 'NONE',  ( 5.000000000000000000, 23.50000000000000000, -6.123233995736766282E-16 ) ) ;
#5646 = CARTESIAN_POINT ( 'NONE',  ( -4.458734124999999437, -102.3958333319677365, -2.574251347313719407 ) ) ;
#5647 = CARTESIAN_POINT ( 'NONE',  ( -5.000000000000000000, -159.6250000027311842, -6.123233995736766282E-16 ) ) ;
#5648 = ORIENTED_EDGE ( 'NONE', *, *, #47152, .T. ) ;
#5649 = CARTESIAN_POINT ( 'NONE',  ( 2.229367062500001939, -97.22916666530105090, 3.861377020970579999 ) ) ;
#5650 = CARTESIAN_POINT ( 'NONE',  ( -1.339745962155623360, 22.20534180126147561, 4.999999999999991118 ) ) ;
#5651 = CARTESIAN_POINT ( 'NONE',  ( -5.000000000000000000, -54.87499999726880162, 0.000000000000000000 ) ) ;
#5652 = CARTESIAN_POINT ( 'NONE',  ( -1.339745962155610925, -71.66965819600733312, 5.000000000000000000 ) ) ;
#5653 = VECTOR ( 'NONE', #54026, 1000.000000000000000 ) ;
#5654 = CARTESIAN_POINT ( 'NONE',  ( -50.40829686548195099, -125.0000000013656205, -1.485763867205728284 ) ) ;
#5655 = CARTESIAN_POINT ( 'NONE',  ( -56.48576386720575471, -143.7500000013656063, -4.591703134518078322 ) ) ;
#5656 = CARTESIAN_POINT ( 'NONE',  ( -3.152548672688508926E-16, -17.56249999863440792, -5.148502694627439702 ) ) ;
#5657 = CARTESIAN_POINT ( 'NONE',  ( -4.458734124999998549, 8.520833334698926009, 2.574251347313722516 ) ) ;
#5658 = CARTESIAN_POINT ( 'NONE',  ( -2.229367062500000163, -65.72916666530106511, -3.861377020970580443 ) ) ;
#5659 = DIRECTION ( 'NONE',  ( -0.000000000000000000, -1.000000000000000000, -0.000000000000000000 ) ) ;
#5660 = CARTESIAN_POINT ( 'NONE',  ( 4.458734125000000326, -21.89583333196773296, 2.574251347313718519 ) ) ;
#5661 = CARTESIAN_POINT ( 'NONE',  ( 2.500000000000002220, -75.66666666666665719, 4.330127018922192761 ) ) ;
#5662 = CARTESIAN_POINT ( 'NONE',  ( -5.000000000000000888, -155.5625000000000568, -2.071067811865475949 ) ) ;
#5663 = CARTESIAN_POINT ( 'NONE',  ( 5.000000000000000000, -9.416666666666662522, -2.886751345948129988 ) ) ;
#5664 = CARTESIAN_POINT ( 'NONE',  ( 3.152801135295367541, -155.3125000013656063, -3.152801135295367541 ) ) ;
#5665 = VERTEX_POINT ( 'NONE', #30994 ) ;
#5666 = CARTESIAN_POINT ( 'NONE',  ( 4.458734125000000326, -47.14583333196774362, 2.574251347313718519 ) ) ;
#5667 =( BOUNDED_CURVE ( )  B_SPLINE_CURVE ( 2, ( #26572, #12411, #22708, #2456, #57436, #32659, #52287, #7908, #32023 ),
 .UNSPECIFIED., .F., .F. ) 
 B_SPLINE_CURVE_WITH_KNOTS ( ( 3, 2, 2, 2, 3 ),
 ( 0.6020833333333333037, 0.6027777777777777457, 0.6041666666666666297, 0.6055555555555555136, 0.6062499999999999556 ),
 .UNSPECIFIED. ) 
 CURVE ( )  GEOMETRIC_REPRESENTATION_ITEM ( )  RATIONAL_B_SPLINE_CURVE ( ( 0.9330127018922194093, 0.9330127018922194093, 1.000000000000000000, 0.8660254037844387076, 1.000000000000000000, 0.8660254037844387076, 1.000000000000000000, 0.9330127018922194093, 0.9330127018922194093 ) ) 
 REPRESENTATION_ITEM ( '' )  );
#5668 = CARTESIAN_POINT ( 'NONE',  ( 1.339745962155615144, -44.58034179853027723, 4.999999999999999112 ) ) ;
#5669 = CARTESIAN_POINT ( 'NONE',  ( -5.000000000000000000, -9.083333333333333925, -2.886751345948128211 ) ) ;
#5670 = CARTESIAN_POINT ( 'NONE',  ( -3.535250795749689387E-16, 27.75000000000000000, -5.773502691896257311 ) ) ;
#5671 = CARTESIAN_POINT ( 'NONE',  ( 2.229367062500001939, -89.97916666530106511, 3.861377020970579999 ) ) ;
#5672 = CARTESIAN_POINT ( 'NONE',  ( -4.458734124999998549, 8.770833334698927786, 2.574251347313722516 ) ) ;
#5673 = CARTESIAN_POINT ( 'NONE',  ( 5.000000000000000888, -0.5833333333333350357, 2.886751345948126879 ) ) ;
#5674 = CARTESIAN_POINT ( 'NONE',  ( -5.000000000000000000, -68.99999999999998579, 0.000000000000000000 ) ) ;
#5675 = CARTESIAN_POINT ( 'NONE',  ( 5.000000000000000888, 20.54166666939784847, 2.886751345948126879 ) ) ;
#5676 = CARTESIAN_POINT ( 'NONE',  ( -4.458734124999998549, 20.52083333469892423, 2.574251347313722516 ) ) ;
#5677 = CARTESIAN_POINT ( 'NONE',  ( 2.500000000000002220, -76.66666666666665719, 4.330127018922192761 ) ) ;
#5678 = CARTESIAN_POINT ( 'NONE',  ( -2.499999999999996447, 6.291666669397851130, 4.330127018922195425 ) ) ;
#5679 = EDGE_LOOP ( 'NONE', ( #1672, #52977, #6660, #48571 ) ) ;
#5680 = CARTESIAN_POINT ( 'NONE',  ( 5.000000000000000000, -162.1875000027311842, 2.071067811865478614 ) ) ;
#5681 = VERTEX_POINT ( 'NONE', #11056 ) ;
#5682 = CARTESIAN_POINT ( 'NONE',  ( 5.000000000000000000, 26.58333333333333215, -2.886751345948130876 ) ) ;
#5683 = CARTESIAN_POINT ( 'NONE',  ( 4.458734124999999437, -39.81249999863440081, -5.460374474430324690E-16 ) ) ;
#5684 = CARTESIAN_POINT ( 'NONE',  ( -5.000000000000000000, -40.95833333060215153, -2.886751345948128211 ) ) ;
#5685 = ORIENTED_EDGE ( 'NONE', *, *, #21379, .F. ) ;
#5686 = CARTESIAN_POINT ( 'NONE',  ( -2.229367062500000163, -12.47916666530107044, -3.861377020970580443 ) ) ;
#5688 = ORIENTED_EDGE ( 'NONE', *, *, #24345, .F. ) ;
#5687 = CARTESIAN_POINT ( 'NONE',  ( -2.229367062499996610, -17.39583333196773651, 3.861377020970582219 ) ) ;
#5689 = CARTESIAN_POINT ( 'NONE',  ( 2.499999999999998668, -83.33333333333332860, -4.330127018922193649 ) ) ;
#5690 = CARTESIAN_POINT ( 'NONE',  ( -3.152801135295367985, -166.8125000013656063, 3.152801135295367096 ) ) ;
#5691 = CARTESIAN_POINT ( 'NONE',  ( 2.229367062500001939, -61.22916666530106511, 3.861377020970579999 ) ) ;
#5692 =( BOUNDED_CURVE ( )  B_SPLINE_CURVE ( 2, ( #34292, #49729, #20469, #9840, #19819, #39428, #59069, #35899, #56160 ),
 .UNSPECIFIED., .F., .F. ) 
 B_SPLINE_CURVE_WITH_KNOTS ( ( 3, 2, 2, 2, 3 ),
 ( 0.5520833333333333703, 0.5527777777777778123, 0.5541666666666666963, 0.5555555555555555802, 0.5562500000000000222 ),
 .UNSPECIFIED. ) 
 CURVE ( )  GEOMETRIC_REPRESENTATION_ITEM ( )  RATIONAL_B_SPLINE_CURVE ( ( 0.9330127018922194093, 0.9330127018922194093, 1.000000000000000000, 0.8660254037844387076, 1.000000000000000000, 0.8660254037844387076, 1.000000000000000000, 0.9330127018922194093, 0.9330127018922194093 ) ) 
 REPRESENTATION_ITEM ( '' )  );
#5693 = CARTESIAN_POINT ( 'NONE',  ( 2.500000000000002220, -88.54166666393548724, 4.330127018922192761 ) ) ;
#5695 = ORIENTED_EDGE ( 'NONE', *, *, #31000, .T. ) ;
#5694 = CARTESIAN_POINT ( 'NONE',  ( -2.500000000000000444, -49.04166666393547303, -4.330127018922193649 ) ) ;
#5696 = CARTESIAN_POINT ( 'NONE',  ( -57.46284108482265651, -141.9375000000000000, 4.819101127000239515 ) ) ;
#5697 = CARTESIAN_POINT ( 'NONE',  ( 4.458734125000001214, -29.14583333196774362, 2.574251347313718519 ) ) ;
#5698 = CARTESIAN_POINT ( 'NONE',  ( -51.75738570946856498, -143.8750000027312126, 3.805975901505576964 ) ) ;
#5699 = ORIENTED_EDGE ( 'NONE', *, *, #44705, .T. ) ;
#5700 = VECTOR ( 'NONE', #12295, 1000.000000000000000 ) ;
#5701 = CARTESIAN_POINT ( 'NONE',  ( 1.846868145590735200, -162.5000000013655779, -4.458734125000000326 ) ) ;
#5702 = CARTESIAN_POINT ( 'NONE',  ( 4.458734125000001214, 28.10416666803225993, 2.574251347313718519 ) ) ;
#5703 = CARTESIAN_POINT ( 'NONE',  ( 2.499999999999998668, -23.33333333333333215, -4.330127018922193649 ) ) ;
#5704 = ORIENTED_EDGE ( 'NONE', *, *, #7073, .T. ) ;
#5705 = CARTESIAN_POINT ( 'NONE',  ( -56.48576386720575471, -145.0000000013656063, -4.591703134518078322 ) ) ;
#5706 = CARTESIAN_POINT ( 'NONE',  ( -2.229367062500000163, -76.72916666530106511, -3.861377020970580443 ) ) ;
#5707 = CARTESIAN_POINT ( 'NONE',  ( -53.33387254593733928, -134.9375000027312126, 5.149110718188519620 ) ) ;
#5708 = CARTESIAN_POINT ( 'NONE',  ( 4.458734124999998549, -41.72916666530107932, -2.574251347313721627 ) ) ;
#5709 = CARTESIAN_POINT ( 'NONE',  ( 2.730187237215162345E-16, -145.4375000013656063, -4.458734124999999437 ) ) ;
#5710 = DIRECTION ( 'NONE',  ( -0.000000000000000000, 1.000000000000000000, -0.000000000000000000 ) ) ;
#5711 = CARTESIAN_POINT ( 'NONE',  ( 2.229367062500001939, -47.97916666530106511, 3.861377020970579999 ) ) ;
#5712 = CARTESIAN_POINT ( 'NONE',  ( 1.975475456537005874E-15, -70.75000000000000000, 5.000000000000000000 ) ) ;
#5713 = CARTESIAN_POINT ( 'NONE',  ( 4.458734124999999437, -15.81249999863440436, -5.460374474430324690E-16 ) ) ;
#5714 = CARTESIAN_POINT ( 'NONE',  ( 5.000000000000000888, -101.5833333333333286, 2.886751345948126879 ) ) ;
#5715 = CARTESIAN_POINT ( 'NONE',  ( 2.730187237215162345E-16, -140.4375000013656063, -4.458734124999999437 ) ) ;
#5716 = CARTESIAN_POINT ( 'NONE',  ( 4.458734125000001214, -32.14583333196773651, 2.574251347313718519 ) ) ;
#5717 = CARTESIAN_POINT ( 'NONE',  ( 2.499999999999998668, 7.791666669397852019, -4.330127018922193649 ) ) ;
#5718 = DIRECTION ( 'NONE',  ( -0.000000000000000000, 1.000000000000000000, -0.000000000000000000 ) ) ;
#5719 = CARTESIAN_POINT ( 'NONE',  ( -59.59170313451811296, -128.5000000013656063, 1.485763867205729394 ) ) ;
#5720 = CARTESIAN_POINT ( 'NONE',  ( -4.458734124999999437, -75.56249999863440792, 0.000000000000000000 ) ) ;
#5721 = CARTESIAN_POINT ( 'NONE',  ( 0.000000000000000000, -120.0000000000000000, 0.000000000000000000 ) ) ;
#5722 = DIRECTION ( 'NONE',  ( 0.000000000000000000, 0.000000000000000000, 1.000000000000000000 ) ) ;
#5723 = CARTESIAN_POINT ( 'NONE',  ( 2.499999999999998668, 14.79166666939785202, -4.330127018922193649 ) ) ;
#5724 = CARTESIAN_POINT ( 'NONE',  ( 2.229367062500001939, -2.229166665301068662, 3.861377020970579999 ) ) ;
#5725 = ORIENTED_EDGE ( 'NONE', *, *, #56583, .F. ) ;
#5726 = CARTESIAN_POINT ( 'NONE',  ( 5.000000000000000000, 16.62500000273118417, -6.123233995736766282E-16 ) ) ;
#5727 = CARTESIAN_POINT ( 'NONE',  ( -2.499999999999996447, -14.70833333060214976, 4.330127018922195425 ) ) ;
#5729 = CARTESIAN_POINT ( 'NONE',  ( 2.229367062500001939, -37.97916666530107221, 3.861377020970579999 ) ) ;
#5728 = CARTESIAN_POINT ( 'NONE',  ( -4.458734124999999437, -88.39583333196773651, -2.574251347313719407 ) ) ;
#5730 = CARTESIAN_POINT ( 'NONE',  ( -1.339745962155613812, -36.20534180126147561, -5.000000000000000000 ) ) ;
#5731 = CARTESIAN_POINT ( 'NONE',  ( -2.229367062499996610, -79.39583333196773651, 3.861377020970582219 ) ) ;
#5732 = CARTESIAN_POINT ( 'NONE',  ( -4.458734124999997661, 16.52083333469892779, 2.574251347313722516 ) ) ;
#5733 = DIRECTION ( 'NONE',  ( 0.000000000000000000, 0.000000000000000000, 1.000000000000000000 ) ) ;
#5734 = CARTESIAN_POINT ( 'NONE',  ( -50.40829686548195099, -139.0000000013655779, -1.485763867205728284 ) ) ;
#5735 = CARTESIAN_POINT ( 'NONE',  ( 4.458734124999998549, 0.2708333346989263979, -2.574251347313721627 ) ) ;
#5736 = CARTESIAN_POINT ( 'NONE',  ( -2.229367062499996610, 19.60416666803225993, 3.861377020970582219 ) ) ;
#5737 = CARTESIAN_POINT ( 'NONE',  ( 2.229367062500001939, -47.22916666530106511, 3.861377020970579999 ) ) ;
#5738 = CARTESIAN_POINT ( 'NONE',  ( 5.000000000000000000, -15.41666666666666963, -2.886751345948130876 ) ) ;
#5739 = CARTESIAN_POINT ( 'NONE',  ( 9.457646018065525792E-16, -6.062499998634404363, 5.148502694627439702 ) ) ;
#5740 = CARTESIAN_POINT ( 'NONE',  ( -4.458734124999999437, -30.64583333196774007, -2.574251347313719407 ) ) ;
#5741 = CARTESIAN_POINT ( 'NONE',  ( -56.48576386720575471, -132.0000000013656063, -4.591703134518078322 ) ) ;
#5742 = CARTESIAN_POINT ( 'NONE',  ( -2.229367062499996610, -76.14583333196773651, 3.861377020970582219 ) ) ;
#5743 = CARTESIAN_POINT ( 'NONE',  ( -5.000000000000000000, -105.9583333306021586, -2.886751345948128211 ) ) ;
#5744 = AXIS2_PLACEMENT_3D ( 'NONE', #48462, #49087, #39429 ) ;
#5745 = CARTESIAN_POINT ( 'NONE',  ( -3.152548672688508926E-16, 23.43750000136559564, -5.148502694627439702 ) ) ;
#5746 = FACE_OUTER_BOUND ( 'NONE', #38244, .T. ) ;
#5747 = CARTESIAN_POINT ( 'NONE',  ( -2.229367062499996610, -109.3958333319677365, 3.861377020970582219 ) ) ;
#5748 = CARTESIAN_POINT ( 'NONE',  ( -4.458734124999999437, -77.56249999863440792, 0.000000000000000000 ) ) ;
#5749 = CARTESIAN_POINT ( 'NONE',  ( 2.500000000000002220, -61.66666666666666430, 4.330127018922192761 ) ) ;
#5750 = CYLINDRICAL_SURFACE ( 'NONE', #54165, 5.000000000000000000 ) ;
#5751 = CARTESIAN_POINT ( 'NONE',  ( 2.499999999999998668, 23.79166666939785202, -4.330127018922193649 ) ) ;
#5752 = ORIENTED_EDGE ( 'NONE', *, *, #13866, .F. ) ;
#5753 = CYLINDRICAL_SURFACE ( 'NONE', #656, 5.000000000000000000 ) ;
#5754 = CARTESIAN_POINT ( 'NONE',  ( -1.339745962155613812, -57.08034179853028434, -5.000000000000000000 ) ) ;
#5755 = CARTESIAN_POINT ( 'NONE',  ( -5.000000000000000000, -19.08333333333333570, -2.886751345948128211 ) ) ;
#5756 = CARTESIAN_POINT ( 'NONE',  ( -3.152548672688508926E-16, -24.56249999863440792, -5.148502694627439702 ) ) ;
#5757 = CARTESIAN_POINT ( 'NONE',  ( 9.457646018065525792E-16, -84.06249999863439371, 5.148502694627439702 ) ) ;
#5758 = CARTESIAN_POINT ( 'NONE',  ( 2.499999999999998668, -25.20833333060214443, -4.330127018922193649 ) ) ;
#5760 = VERTEX_POINT ( 'NONE', #49661 ) ;
#5759 = CARTESIAN_POINT ( 'NONE',  ( 4.458734124999999437, -47.81249999863440792, -5.460374474430324690E-16 ) ) ;
#5761 = CARTESIAN_POINT ( 'NONE',  ( -1.339745962155613812, -76.08034179853028434, -5.000000000000000000 ) ) ;
#5762 = CARTESIAN_POINT ( 'NONE',  ( 0.000000000000000000, -170.0000000000000000, 0.000000000000000000 ) ) ;
#5764 = ORIENTED_EDGE ( 'NONE', *, *, #35467, .F. ) ;
#5763 = CARTESIAN_POINT ( 'NONE',  ( 2.229367062499998831, -1.895833331967737623, -3.861377020970580887 ) ) ;
#5765 = CARTESIAN_POINT ( 'NONE',  ( -50.55543936806279248, -150.0625000013656063, 0.3552334253322060320 ) ) ;
#5766 = CARTESIAN_POINT ( 'NONE',  ( -4.999999999999999112, -65.91666666666665719, 2.886751345948131764 ) ) ;
#5767 = CARTESIAN_POINT ( 'NONE',  ( 4.458734125000000326, -151.6250000013656063, -1.846868145590734978 ) ) ;
#5768 = CARTESIAN_POINT ( 'NONE',  ( -3.152548672688508926E-16, -48.81249999863440792, -5.148502694627439702 ) ) ;
#5769 = LINE ( 'NONE', #30523, #9089 ) ;
#5770 = CARTESIAN_POINT ( 'NONE',  ( 5.000000000000000888, -159.9375000000000000, -2.071067811865475505 ) ) ;
#5771 = CARTESIAN_POINT ( 'NONE',  ( -1.339745962155613812, 6.919658201469707670, -5.000000000000000000 ) ) ;
#5772 = CARTESIAN_POINT ( 'NONE',  ( -54.60164318462004474, -153.3750000000000284, -4.984105922594373794 ) ) ;
#5773 = CARTESIAN_POINT ( 'NONE',  ( -3.152548672688508926E-16, -12.81249999863440259, -5.148502694627439702 ) ) ;
#5774 = CARTESIAN_POINT ( 'NONE',  ( 4.458734124999998549, -44.97916666530107221, -2.574251347313721627 ) ) ;
#5775 = CARTESIAN_POINT ( 'NONE',  ( -1.846868145590737420, -142.7500000013656063, 4.458734124999999437 ) ) ;
#5776 = CARTESIAN_POINT ( 'NONE',  ( 2.229367062500001939, -93.22916666530106511, 3.861377020970579999 ) ) ;
#5777 = CARTESIAN_POINT ( 'NONE',  ( 1.975475456537005874E-15, 4.375000002731185056, 5.000000000000000000 ) ) ;
#5778 = ORIENTED_EDGE ( 'NONE', *, *, #50340, .T. ) ;
#5779 = CARTESIAN_POINT ( 'NONE',  ( -6.972266317189433020E-16, -33.12499999726880873, -5.000000000000000000 ) ) ;
#5780 = DIRECTION ( 'NONE',  ( -0.8660254037844505870, -0.4999999999999792388, 0.000000000000000000 ) ) ;
#5781 = CARTESIAN_POINT ( 'NONE',  ( -53.33387254593733928, -146.9375000027311842, 5.149110718188519620 ) ) ;
#5782 = AXIS2_PLACEMENT_3D ( 'NONE', #31949, #11687, #57048 ) ;
#5783 = CARTESIAN_POINT ( 'NONE',  ( -2.499999999999996447, -61.83333333333333570, 4.330127018922195425 ) ) ;
#5784 = EDGE_LOOP ( 'NONE', ( #54539, #7926, #8477, #60385 ) ) ;
#5785 = AXIS2_PLACEMENT_3D ( 'NONE', #45684, #30236, #40848 ) ;
#5786 = CARTESIAN_POINT ( 'NONE',  ( 9.457646018065525792E-16, 1.937500001365593416, 5.148502694627439702 ) ) ;
#5787 = VECTOR ( 'NONE', #42026, 1000.000000000000000 ) ;
#5788 =( BOUNDED_CURVE ( )  B_SPLINE_CURVE ( 2, ( #47931, #62748, #18355, #47621, #8701, #13538, #47319, #43107, #28316 ),
 .UNSPECIFIED., .F., .F. ) 
 B_SPLINE_CURVE_WITH_KNOTS ( ( 3, 2, 2, 2, 3 ),
 ( 0.6017857142857142572, 0.6023809523809523503, 0.6035714285714285365, 0.6047619047619047228, 0.6053571428571428159 ),
 .UNSPECIFIED. ) 
 CURVE ( )  GEOMETRIC_REPRESENTATION_ITEM ( )  RATIONAL_B_SPLINE_CURVE ( ( 0.9330127018922194093, 0.9330127018922194093, 1.000000000000000000, 0.8660254037844387076, 1.000000000000000000, 0.8660254037844387076, 1.000000000000000000, 0.9330127018922194093, 0.9330127018922194093 ) ) 
 REPRESENTATION_ITEM ( '' )  );
#5789 = CARTESIAN_POINT ( 'NONE',  ( 1.975475456537005874E-15, -1.624999997268813834, 5.000000000000000000 ) ) ;
#5790 = CARTESIAN_POINT ( 'NONE',  ( -4.458734124999999437, -16.64583333196773651, -2.574251347313719407 ) ) ;
#5791 = CARTESIAN_POINT ( 'NONE',  ( -2.500000000000000444, 1.958333336064519647, -4.330127018922193649 ) ) ;
#5792 = CARTESIAN_POINT ( 'NONE',  ( -4.458734124999999437, -7.395833331967734736, -2.574251347313719407 ) ) ;
#5793 = CARTESIAN_POINT ( 'NONE',  ( -2.499999999999996447, -73.70833333060214443, 4.330127018922195425 ) ) ;
#5794 = CARTESIAN_POINT ( 'NONE',  ( 4.458734124999999437, -150.4375000013656063, 0.000000000000000000 ) ) ;
#5795 = CARTESIAN_POINT ( 'NONE',  ( -4.458734124999997661, 16.52083333469892779, 2.574251347313722516 ) ) ;
#5796 = ORIENTED_EDGE ( 'NONE', *, *, #47579, .F. ) ;
#5797 = CARTESIAN_POINT ( 'NONE',  ( -5.000000000000000000, -13.87499999726881228, 0.000000000000000000 ) ) ;
#5798 = CARTESIAN_POINT ( 'NONE',  ( 6.250000000000000888, 5.051814855409225480, -7.198902722707425816 ) ) ;
#5799 = CARTESIAN_POINT ( 'NONE',  ( -2.229367062499996610, -20.14583333196774007, 3.861377020970582219 ) ) ;
#5800 = EDGE_CURVE ( 'NONE', #58830, #45091, #15052, .T. ) ;
#5801 = CARTESIAN_POINT ( 'NONE',  ( 7.499999999999999112, 2.575910028905302074, -0.3641256808890108720 ) ) ;
#5802 = CARTESIAN_POINT ( 'NONE',  ( 6.123233995736766282E-16, -120.0000000000000000, -5.000000000000000000 ) ) ;
#5803 = CARTESIAN_POINT ( 'NONE',  ( -52.80376928212989185, -147.8750000013656063, -4.297418129356379346 ) ) ;
#5804 = CARTESIAN_POINT ( 'NONE',  ( -5.000000000000000000, -45.95833333060214443, -2.886751345948128211 ) ) ;
#5805 = CARTESIAN_POINT ( 'NONE',  ( -75.00000000000000000, 15.00000000000000000, 8.999999999999998224 ) ) ;
#5806 = CARTESIAN_POINT ( 'NONE',  ( -4.458734124999999437, 15.68750000136559564, 0.000000000000000000 ) ) ;
#5807 = FACE_OUTER_BOUND ( 'NONE', #9168, .T. ) ;
#5808 = DIRECTION ( 'NONE',  ( 0.8660254037844387076, 0.000000000000000000, 0.4999999999999997780 ) ) ;
#5809 = CARTESIAN_POINT ( 'NONE',  ( 2.229367062500001939, 12.02083333469892601, 3.861377020970579999 ) ) ;
#5810 = CARTESIAN_POINT ( 'NONE',  ( -2.229367062499996610, -60.14583333196774362, 3.861377020970582219 ) ) ;
#5811 = EDGE_LOOP ( 'NONE', ( #46094, #27357, #2845, #56498 ) ) ;
#5812 = CARTESIAN_POINT ( 'NONE',  ( -4.458734124999999437, -14.56249999863440436, 0.000000000000000000 ) ) ;
#5813 = CARTESIAN_POINT ( 'NONE',  ( -3.535250795749689387E-16, 4.750000000000000888, -5.773502691896257311 ) ) ;
#5814 = CARTESIAN_POINT ( 'NONE',  ( 4.458734124999999437, -165.4375000013655779, 0.000000000000000000 ) ) ;
#5815 = CARTESIAN_POINT ( 'NONE',  ( 1.975475456537005874E-15, -40.62499999726879452, 5.000000000000000000 ) ) ;
#5816 = CARTESIAN_POINT ( 'NONE',  ( 4.458734124999998549, -59.72916666530106511, -2.574251347313721627 ) ) ;
#5817 = CARTESIAN_POINT ( 'NONE',  ( -2.500000000000000444, -92.04166666393547303, -4.330127018922193649 ) ) ;
#5818 = CARTESIAN_POINT ( 'NONE',  ( -4.458734124999999437, -32.39583333196773651, -2.574251347313719407 ) ) ;
#5819 = CARTESIAN_POINT ( 'NONE',  ( -6.972266317189433020E-16, -9.250000000000000000, -5.000000000000000000 ) ) ;
#5820 = EDGE_CURVE ( 'NONE', #23906, #25310, #54113, .T. ) ;
#5821 = CARTESIAN_POINT ( 'NONE',  ( -4.729367062499999719, 29.28125000204839168, 0.000000000000000000 ) ) ;
#5822 = DIRECTION ( 'NONE',  ( 0.000000000000000000, 0.000000000000000000, 1.000000000000000000 ) ) ;
#5823 = EDGE_CURVE ( 'NONE', #49290, #19824, #4816, .T. ) ;
#5824 = CARTESIAN_POINT ( 'NONE',  ( 1.339745962155615144, 1.294658198738520172, 4.999999999999999112 ) ) ;
#5825 = CARTESIAN_POINT ( 'NONE',  ( 2.730187237215162345E-16, -151.4375000013656063, -4.458734124999999437 ) ) ;
#5826 = CARTESIAN_POINT ( 'NONE',  ( -5.000000000000000000, -45.08333333333333570, -2.886751345948128211 ) ) ;
#5827 = CARTESIAN_POINT ( 'NONE',  ( 6.123233995736766282E-16, -170.0000000000000000, -5.000000000000000000 ) ) ;
#5828 = FACE_OUTER_BOUND ( 'NONE', #991, .T. ) ;
#5829 = ORIENTED_EDGE ( 'NONE', *, *, #57324, .F. ) ;
#5830 = CARTESIAN_POINT ( 'NONE',  ( 2.229367062499998831, -99.64583333196773651, -3.861377020970580887 ) ) ;
#5831 = CARTESIAN_POINT ( 'NONE',  ( -2.229367062500000163, 4.270833334698926897, -3.861377020970580443 ) ) ;
#5832 = VECTOR ( 'NONE', #14664, 1000.000000000000000 ) ;
#5833 = CARTESIAN_POINT ( 'NONE',  ( -4.999999999999998224, -8.791666663935483683, 2.886751345948131764 ) ) ;
#5834 = CARTESIAN_POINT ( 'NONE',  ( -4.999999999999999112, 0.08333333333333457771, 2.886751345948131764 ) ) ;
#5835 = VECTOR ( 'NONE', #27828, 1000.000000000000000 ) ;
#5836 = CARTESIAN_POINT ( 'NONE',  ( -2.229367062499996610, -66.14583333196773651, 3.861377020970582219 ) ) ;
#5837 = VECTOR ( 'NONE', #57469, 1000.000000000000000 ) ;
#5838 = CARTESIAN_POINT ( 'NONE',  ( -56.66612745406280993, -147.4375000027312126, -5.149110718188524061 ) ) ;
#5839 = CARTESIAN_POINT ( 'NONE',  ( 2.499999999999998668, -9.208333330602146205, -4.330127018922193649 ) ) ;
#5841 = VERTEX_POINT ( 'NONE', #16206 ) ;
#5840 = CARTESIAN_POINT ( 'NONE',  ( -4.458734124999998549, -33.22916666530107221, 2.574251347313722516 ) ) ;
#5842 = CLOSED_SHELL ( 'NONE', ( #55137, #46871, #24407, #32603, #18518, #104, #37699, #36450, #47631, #44739, #46150, #20564, #58599, #28766, #21225, #20217, #86, #5468, #41517, #20481, #33343, #2789, #18178, #60671, #7509, #8261, #25863, #50241, #15404, #14683, #10685, #11137, #25934, #15056, #3163, #43204, #19589, #4368, #25135, #60551, #32523, #11935, #7795, #60536, #40952, #14676, #101, #27875, #40956, #53092, #30827, #38078, #7160 ) ) ;
#5843 = CARTESIAN_POINT ( 'NONE',  ( 1.975475456537005874E-15, -33.75000000000000000, 5.000000000000000000 ) ) ;
#5844 = CYLINDRICAL_SURFACE ( 'NONE', #63146, 5.000000000000000000 ) ;
#5845 = ORIENTED_EDGE ( 'NONE', *, *, #2776, .T. ) ;
#5846 =( BOUNDED_CURVE ( )  B_SPLINE_CURVE ( 2, ( #39289, #4888, #4263, #23881, #54088, #53771, #44113, #18730, #76 ),
 .UNSPECIFIED., .F., .F. ) 
 B_SPLINE_CURVE_WITH_KNOTS ( ( 3, 2, 2, 2, 3 ),
 ( 0.04821428571428571647, 0.04880952380952380959, 0.05000000000000000278, 0.05119047619047618902, 0.05178571428571428908 ),
 .UNSPECIFIED. ) 
 CURVE ( )  GEOMETRIC_REPRESENTATION_ITEM ( )  RATIONAL_B_SPLINE_CURVE ( ( 0.9330127018922194093, 0.9330127018922197424, 1.000000000000000000, 0.8660254037844387076, 1.000000000000000000, 0.8660254037844387076, 1.000000000000000000, 0.9330127018922189652, 0.9330127018922194093 ) ) 
 REPRESENTATION_ITEM ( '' )  );
#5847 = CARTESIAN_POINT ( 'NONE',  ( -5.000000000000000000, -48.87499999726880873, 0.000000000000000000 ) ) ;
#5848 = CARTESIAN_POINT ( 'NONE',  ( 2.499999999999998668, -52.33333333333332860, -4.330127018922193649 ) ) ;
#5851 = CARTESIAN_POINT ( 'NONE',  ( -4.458734124999999437, -29.56249999863440436, 0.000000000000000000 ) ) ;
#5850 =( BOUNDED_CURVE ( )  B_SPLINE_CURVE ( 2, ( #3334, #27131, #7206, #2692, #12961, #22634, #42233, #26817, #61238 ),
 .UNSPECIFIED., .F., .F. ) 
 B_SPLINE_CURVE_WITH_KNOTS ( ( 3, 2, 2, 2, 3 ),
 ( 0.8749999999999998890, 0.8791666666666665408, 0.8833333333333330817, 0.8874999999999997335, 0.8916666666666664964 ),
 .UNSPECIFIED. ) 
 CURVE ( )  GEOMETRIC_REPRESENTATION_ITEM ( )  RATIONAL_B_SPLINE_CURVE ( ( 1.000000000000001998, 0.9238795325112847401, 1.000000000000000000, 0.9238795325112867385, 1.000000000000000000, 0.9238795325112867385, 1.000000000000000000, 0.9238795325112908463, 0.9999999999999958922 ) ) 
 REPRESENTATION_ITEM ( '' )  );
#5849 = DIRECTION ( 'NONE',  ( -0.000000000000000000, 1.000000000000000000, -0.000000000000000000 ) ) ;
#5852 = FACE_OUTER_BOUND ( 'NONE', #56182, .T. ) ;
#5853 = CARTESIAN_POINT ( 'NONE',  ( -2.229367062500000163, -77.47916666530106511, -3.861377020970580443 ) ) ;
#5854 = CARTESIAN_POINT ( 'NONE',  ( -1.846868145590737420, -144.0000000013655779, 4.458734124999999437 ) ) ;
#5855 = CARTESIAN_POINT ( 'NONE',  ( 2.229367062499998831, -82.64583333196773651, -3.861377020970580887 ) ) ;
#5856 = CARTESIAN_POINT ( 'NONE',  ( -50.70258187064364108, -137.3750000013656063, 2.196230717870141014 ) ) ;
#5857 = CARTESIAN_POINT ( 'NONE',  ( -2.229367062499996610, -30.39583333196773651, 3.861377020970582219 ) ) ;
#5858 = EDGE_LOOP ( 'NONE', ( #24339, #2168, #263, #56580 ) ) ;
#5859 = ADVANCED_FACE ( 'NONE', ( #35834 ), #55455, .T. ) ;
#5860 = CARTESIAN_POINT ( 'NONE',  ( 0.000000000000000000, -120.0000000000000000, 5.000000000000000000 ) ) ;
#5861 = ORIENTED_EDGE ( 'NONE', *, *, #52575, .T. ) ;
#5862 = CARTESIAN_POINT ( 'NONE',  ( 4.458734125000001214, -72.14583333196773651, 2.574251347313718519 ) ) ;
#5863 = FACE_OUTER_BOUND ( 'NONE', #9027, .T. ) ;
#5864 = VERTEX_POINT ( 'NONE', #50940 ) ;
#5865 = CARTESIAN_POINT ( 'NONE',  ( 1.975475456537005874E-15, -16.74999999999999645, 5.000000000000000000 ) ) ;
#5866 = DIRECTION ( 'NONE',  ( 0.000000000000000000, -1.000000000000000000, 0.000000000000000000 ) ) ;
#5867 = CARTESIAN_POINT ( 'NONE',  ( -2.229367062500000163, -62.72916666530106511, -3.861377020970580443 ) ) ;
#5868 = CARTESIAN_POINT ( 'NONE',  ( -4.458734124999998549, -2.479166665301069550, 2.574251347313722516 ) ) ;
#5869 = ORIENTED_EDGE ( 'NONE', *, *, #23163, .F. ) ;
#5870 = CARTESIAN_POINT ( 'NONE',  ( 6.123233995736766282E-16, -170.0000000000000000, -5.000000000000000000 ) ) ;
#5871 = CARTESIAN_POINT ( 'NONE',  ( 5.000000000000000888, -27.58333333333333570, 2.886751345948126879 ) ) ;
#5872 =( BOUNDED_CURVE ( )  B_SPLINE_CURVE ( 2, ( #28992, #15163, #48616, #19665, #4555, #24180, #53140, #43475, #5199 ),
 .UNSPECIFIED., .F., .F. ) 
 B_SPLINE_CURVE_WITH_KNOTS ( ( 3, 2, 2, 2, 3 ),
 ( 0.08125000000000000278, 0.08194444444444444475, 0.08333333333333332871, 0.08472222222222222654, 0.08541666666666666852 ),
 .UNSPECIFIED. ) 
 CURVE ( )  GEOMETRIC_REPRESENTATION_ITEM ( )  RATIONAL_B_SPLINE_CURVE ( ( 0.9330127018922194093, 0.9330127018922194093, 1.000000000000000000, 0.8660254037844387076, 1.000000000000000000, 0.8660254037844387076, 1.000000000000000000, 0.9330127018922194093, 0.9330127018922194093 ) ) 
 REPRESENTATION_ITEM ( '' )  );
#5873 = CARTESIAN_POINT ( 'NONE',  ( 9.457646018065525792E-16, 10.93750000136559208, 5.148502694627439702 ) ) ;
#5874 = CARTESIAN_POINT ( 'NONE',  ( -54.64476657466781973, -140.8125000013656063, -4.444560631937228834 ) ) ;
#5875 = CARTESIAN_POINT ( 'NONE',  ( 1.975475456537005874E-15, -47.62499999726880873, 5.000000000000000000 ) ) ;
#5876 = CARTESIAN_POINT ( 'NONE',  ( -4.458734124999999437, -160.0000000013656063, -1.846868145590735644 ) ) ;
#5877 = VECTOR ( 'NONE', #8745, 1000.000000000000000 ) ;
#5878 = FACE_OUTER_BOUND ( 'NONE', #9161, .T. ) ;
#5879 = VERTEX_POINT ( 'NONE', #46433 ) ;
#5880 = CARTESIAN_POINT ( 'NONE',  ( 4.458734125000000326, -81.89583333196773651, 2.574251347313718519 ) ) ;
#5881 = FACE_OUTER_BOUND ( 'NONE', #33937, .T. ) ;
#5882 = CARTESIAN_POINT ( 'NONE',  ( 4.458734124999998549, -4.729166665301071326, -2.574251347313721627 ) ) ;
#5883 = EDGE_CURVE ( 'NONE', #60539, #47703, #34781, .T. ) ;
#5884 = DIRECTION ( 'NONE',  ( -0.000000000000000000, 1.000000000000000000, -0.000000000000000000 ) ) ;
#5885 = COLOUR_RGB ( '',1.000000000000000000, 0.9490196078431372140, 0.9098039215686274384 ) ;
#5886 = CYLINDRICAL_SURFACE ( 'NONE', #51068, 5.000000000000000000 ) ;
#5887 = CARTESIAN_POINT ( 'NONE',  ( -3.152548672688508926E-16, -69.81249999863439371, -5.148502694627439702 ) ) ;
#5888 = CARTESIAN_POINT ( 'NONE',  ( 5.000000000000000000, -26.37499999726881583, -6.123233995736766282E-16 ) ) ;
#5889 = CARTESIAN_POINT ( 'NONE',  ( -1.339745962155613812, -73.08034179853029855, -5.000000000000000000 ) ) ;
#5890 = CARTESIAN_POINT ( 'NONE',  ( 4.458734124999999437, 29.18750000136559208, -5.460374474430324690E-16 ) ) ;
#5891 = CARTESIAN_POINT ( 'NONE',  ( -1.339745962155606929, 22.79465819873851729, -5.000000000000004441 ) ) ;
#5892 = CARTESIAN_POINT ( 'NONE',  ( 1.975475456537005874E-15, -58.75000000000000000, 5.000000000000000000 ) ) ;
#5893 = CARTESIAN_POINT ( 'NONE',  ( 4.458734125000001214, -47.89583333196775072, 2.574251347313718519 ) ) ;
#5894 = CARTESIAN_POINT ( 'NONE',  ( 4.458734124999998549, -29.97916666530107221, -2.574251347313721627 ) ) ;
#5895 = CARTESIAN_POINT ( 'NONE',  ( -3.152548672688508926E-16, -0.8124999986344056957, -5.148502694627439702 ) ) ;
#5896 =( BOUNDED_CURVE ( )  B_SPLINE_CURVE ( 2, ( #54711, #58264, #23852, #24164, #44084, #44722, #14499, #4237, #15145 ),
 .UNSPECIFIED., .F., .F. ) 
 B_SPLINE_CURVE_WITH_KNOTS ( ( 3, 2, 2, 2, 3 ),
 ( 0.4083333333333336590, 0.4125000000000003109, 0.4166666666666670182, 0.4208333333333336701, 0.4250000000000003220 ),
 .UNSPECIFIED. ) 
 CURVE ( )  GEOMETRIC_REPRESENTATION_ITEM ( )  RATIONAL_B_SPLINE_CURVE ( ( 0.9999999999999938938, 0.9238795325112928447, 1.000000000000000000, 0.9238795325112867385, 1.000000000000000000, 0.9238795325112867385, 1.000000000000000000, 0.9238795325112806323, 1.000000000000005995 ) ) 
 REPRESENTATION_ITEM ( '' )  );
#5897 = CARTESIAN_POINT ( 'NONE',  ( 3.535533905932736864, -151.1250000000000000, 3.535533905932738641 ) ) ;
#5898 = CARTESIAN_POINT ( 'NONE',  ( -5.000000000000000000, 21.91666666666666785, -2.886751345948128211 ) ) ;
#5899 = CARTESIAN_POINT ( 'NONE',  ( 3.535533905932738197, -147.0000000027311842, -3.535533905932738197 ) ) ;
#5900 = CARTESIAN_POINT ( 'NONE',  ( -54.60164318462004474, -154.3750000000000284, -4.984105922594373794 ) ) ;
#5901 = CARTESIAN_POINT ( 'NONE',  ( 4.458734124999999437, -43.81249999863440081, -5.460374474430324690E-16 ) ) ;
#5902 = CARTESIAN_POINT ( 'NONE',  ( 2.500000000000002220, -72.54166666393548724, 4.330127018922192761 ) ) ;
#5903 = CARTESIAN_POINT ( 'NONE',  ( -58.39396692619412477, -145.6875000013656063, 2.891590998281057701 ) ) ;
#5904 = FACE_OUTER_BOUND ( 'NONE', #55077, .T. ) ;
#5905 = CARTESIAN_POINT ( 'NONE',  ( 1.975475456537005874E-15, -37.74999999999999289, 5.000000000000000000 ) ) ;
#5906 = EDGE_CURVE ( 'NONE', #29467, #44762, #17789, .T. ) ;
#5907 = CARTESIAN_POINT ( 'NONE',  ( -4.458734124999997661, -82.47916666530106511, 2.574251347313722516 ) ) ;
#5908 = CARTESIAN_POINT ( 'NONE',  ( 1.846868145590736310, -163.8750000013656063, 4.458734124999997661 ) ) ;
#5909 = CARTESIAN_POINT ( 'NONE',  ( -6.972266317189433020E-16, -33.24999999999999289, -5.000000000000000000 ) ) ;
#5910 = FACE_OUTER_BOUND ( 'NONE', #10291, .T. ) ;
#5911 = CARTESIAN_POINT ( 'NONE',  ( 2.500000000000002220, -28.66666666666666785, 4.330127018922192761 ) ) ;
#5912 = CARTESIAN_POINT ( 'NONE',  ( 4.458734124999999437, -139.4375000013656063, 0.000000000000000000 ) ) ;
#5913 = ORIENTED_EDGE ( 'NONE', *, *, #1944, .F. ) ;
#5914 = CARTESIAN_POINT ( 'NONE',  ( 4.458734125000001214, 20.85416666803226349, 2.574251347313718519 ) ) ;
#5916 = EDGE_CURVE ( 'NONE', #8062, #45518, #32583, .T. ) ;
#5915 = ORIENTED_EDGE ( 'NONE', *, *, #30182, .F. ) ;
#5917 = CARTESIAN_POINT ( 'NONE',  ( 2.229367062500001939, -63.22916666530106511, 3.861377020970579999 ) ) ;
#5918 = CARTESIAN_POINT ( 'NONE',  ( -5.000000000000000000, 24.04166666939785202, -2.886751345948128211 ) ) ;
#5919 = CARTESIAN_POINT ( 'NONE',  ( -50.01589407740564042, -138.7500000027312126, 0.3983568153799778022 ) ) ;
#5920 = CARTESIAN_POINT ( 'NONE',  ( -4.999999999999999112, 16.08333333333333215, 2.886751345948131764 ) ) ;
#5921 = CARTESIAN_POINT ( 'NONE',  ( 2.229367062500001939, -49.97916666530107221, 3.861377020970579999 ) ) ;
#5922 = CARTESIAN_POINT ( 'NONE',  ( -3.152548672688508926E-16, -10.56249999863440792, -5.148502694627439702 ) ) ;
#5923 = CARTESIAN_POINT ( 'NONE',  ( 7.499999999999999112, 3.105728215500122680, -7.659336188854854122 ) ) ;
#5924 = CARTESIAN_POINT ( 'NONE',  ( -9.184850993605147944E-16, -158.3750000027311842, 5.000000000000000000 ) ) ;
#5925 = CARTESIAN_POINT ( 'NONE',  ( -9.184850993605147944E-16, -147.2500000000000284, 5.000000000000000000 ) ) ;
#5926 = CARTESIAN_POINT ( 'NONE',  ( -2.500000000000000444, -10.16666666666666430, -4.330127018922193649 ) ) ;
#5928 = CARTESIAN_POINT ( 'NONE',  ( -3.152548672688508926E-16, -19.56249999863440081, -5.148502694627439702 ) ) ;
#5927 = CARTESIAN_POINT ( 'NONE',  ( -2.499999999999996447, -58.83333333333333570, 4.330127018922195425 ) ) ;
#5929 = VECTOR ( 'NONE', #48890, 1000.000000000000000 ) ;
#5930 = CARTESIAN_POINT ( 'NONE',  ( 2.493747252781420335E-13, -78.12499999726881583, -5.000000000000000000 ) ) ;
#5931 = CARTESIAN_POINT ( 'NONE',  ( -2.229367062499996610, -59.14583333196773651, 3.861377020970582219 ) ) ;
#5932 = CARTESIAN_POINT ( 'NONE',  ( 4.458734124999999437, -156.6875000013655779, 0.000000000000000000 ) ) ;
#5933 = EDGE_CURVE ( 'NONE', #31664, #15327, #31304, .T. ) ;
#5934 = VECTOR ( 'NONE', #43303, 1000.000000000000000 ) ;
#5935 = CARTESIAN_POINT ( 'NONE',  ( 5.000000000000000000, -54.37499999726880162, -6.123233995736766282E-16 ) ) ;
#5936 = VERTEX_POINT ( 'NONE', #2380 ) ;
#5937 = CARTESIAN_POINT ( 'NONE',  ( 5.000000000000000000, 13.58333333333333215, -2.886751345948130876 ) ) ;
#5938 = CARTESIAN_POINT ( 'NONE',  ( 4.458734124999998549, -2.979166665301069994, -2.574251347313721627 ) ) ;
#5939 = ORIENTED_EDGE ( 'NONE', *, *, #49606, .F. ) ;
#5941 = DIRECTION ( 'NONE',  ( 0.000000000000000000, -1.000000000000000000, 0.000000000000000000 ) ) ;
#5940 = CARTESIAN_POINT ( 'NONE',  ( 3.061616997868383141E-16, -157.8750000027311842, -5.000000000000000000 ) ) ;
#5942 = CARTESIAN_POINT ( 'NONE',  ( -4.458734124999999437, -155.9375000013655779, -5.460374474430324690E-16 ) ) ;
#5943 = ORIENTED_EDGE ( 'NONE', *, *, #56408, .T. ) ;
#5944 = CARTESIAN_POINT ( 'NONE',  ( 1.339745962155612702, -99.29465819873853150, -5.000000000000000000 ) ) ;
#5945 = CARTESIAN_POINT ( 'NONE',  ( -59.81910112700025905, -129.1875000000000284, -2.462841084822630311 ) ) ;
#5946 = CARTESIAN_POINT ( 'NONE',  ( 1.339745962155615144, 15.29465819873851906, 4.999999999999999112 ) ) ;
#5947 = CARTESIAN_POINT ( 'NONE',  ( 2.229367062500001939, -45.22916666530106511, 3.861377020970579999 ) ) ;
#5948 = ORIENTED_EDGE ( 'NONE', *, *, #20136, .T. ) ;
#5949 = CARTESIAN_POINT ( 'NONE',  ( 2.500000000000002220, 10.45833333606451987, 4.330127018922192761 ) ) ;
#5950 = CARTESIAN_POINT ( 'NONE',  ( 2.229367062500001939, 13.02083333469892779, 3.861377020970579999 ) ) ;
#5951 = CARTESIAN_POINT ( 'NONE',  ( 2.229367062500001939, 27.02083333469892423, 3.861377020970579999 ) ) ;
#5952 = CARTESIAN_POINT ( 'NONE',  ( -50.40829686548195099, -154.0000000013655779, -1.485763867205728284 ) ) ;
#5953 = CARTESIAN_POINT ( 'NONE',  ( 0.000000000000000000, -120.0000000000000000, 0.000000000000000000 ) ) ;
#5954 = DIRECTION ( 'NONE',  ( 0.000000000000000000, 0.000000000000000000, 1.000000000000000000 ) ) ;
#5955 = CARTESIAN_POINT ( 'NONE',  ( 0.000000000000000000, -120.0000000000000000, 0.000000000000000000 ) ) ;
#5956 = CARTESIAN_POINT ( 'NONE',  ( 2.229367062500001939, -67.97916666530106511, 3.861377020970579999 ) ) ;
#5957 = LINE ( 'NONE', #40993, #25349 ) ;
#5958 = CARTESIAN_POINT ( 'NONE',  ( 9.457646018065525792E-16, 18.93750000136559208, 5.148502694627439702 ) ) ;
#5959 = CARTESIAN_POINT ( 'NONE',  ( 1.975475456537005874E-15, -33.75000000000000000, 5.000000000000000000 ) ) ;
#5960 = ADVANCED_FACE ( 'NONE', ( #42543 ), #61235, .T. ) ;
#5961 = CARTESIAN_POINT ( 'NONE',  ( -56.66612745406273888, -152.4375000027312126, -5.149110718188518732 ) ) ;
#5962 = EDGE_CURVE ( 'NONE', #35597, #28144, #52076, .T. ) ;
#5963 = CARTESIAN_POINT ( 'NONE',  ( 4.458734124999999437, -48.06249999863440792, -5.460374474430324690E-16 ) ) ;
#5964 = CARTESIAN_POINT ( 'NONE',  ( 5.000000000000000000, -8.291666663935481907, -2.886751345948129988 ) ) ;
#5965 = CARTESIAN_POINT ( 'NONE',  ( -5.000000000000000000, -108.9999999999999858, 0.000000000000000000 ) ) ;
#5966 = FACE_OUTER_BOUND ( 'NONE', #28260, .T. ) ;
#5967 = CARTESIAN_POINT ( 'NONE',  ( 2.229367062500001939, -88.22916666530107932, 3.861377020970579999 ) ) ;
#5968 = EDGE_CURVE ( 'NONE', #62355, #55212, #41352, .T. ) ;
#5969 = CARTESIAN_POINT ( 'NONE',  ( 5.000000000000000000, -64.29166666393547303, -2.886751345948130876 ) ) ;
#5970 = CARTESIAN_POINT ( 'NONE',  ( 4.458734125000000326, -16.14583333196773651, 2.574251347313718519 ) ) ;
#5972 = VERTEX_POINT ( 'NONE', #27128 ) ;
#5971 = EDGE_CURVE ( 'NONE', #39210, #32568, #60723, .T. ) ;
#5973 = CARTESIAN_POINT ( 'NONE',  ( -2.071067811865562991, -143.4375000027312410, 4.999999999999913847 ) ) ;
#5974 = CARTESIAN_POINT ( 'NONE',  ( 2.229367062499998831, -104.6458333319677365, -3.861377020970580887 ) ) ;
#5975 = CARTESIAN_POINT ( 'NONE',  ( 5.000000000000000888, -156.0625000027312126, -2.071067811865475505 ) ) ;
#5976 = ORIENTED_EDGE ( 'NONE', *, *, #8142, .T. ) ;
#5977 = CARTESIAN_POINT ( 'NONE',  ( -2.229367062499996610, -95.39583333196773651, 3.861377020970582219 ) ) ;
#5978 = VECTOR ( 'NONE', #17876, 1000.000000000000000 ) ;
#5979 = CARTESIAN_POINT ( 'NONE',  ( -4.999999999999998224, -7.916666666666668739, 2.886751345948131764 ) ) ;
#5981 = ADVANCED_FACE ( 'NONE', ( #42230 ), #46744, .T. ) ;
#5980 = CARTESIAN_POINT ( 'NONE',  ( -2.500000000000000444, -60.04166666393547303, -4.330127018922193649 ) ) ;
#5982 = CARTESIAN_POINT ( 'NONE',  ( -5.000000000000000000, -67.00000000000000000, 0.000000000000000000 ) ) ;
#5983 = EDGE_CURVE ( 'NONE', #28793, #28403, #23250, .T. ) ;
#5984 =( BOUNDED_CURVE ( )  B_SPLINE_CURVE ( 2, ( #22550, #12256, #37642, #57598, #47914 ),
 .UNSPECIFIED., .F., .F. ) 
 B_SPLINE_CURVE_WITH_KNOTS ( ( 3, 2, 3 ),
 ( 0.000000000000000000, 0.001388888888888888942, 0.002083333333333333738 ),
 .UNSPECIFIED. ) 
 CURVE ( )  GEOMETRIC_REPRESENTATION_ITEM ( )  RATIONAL_B_SPLINE_CURVE ( ( 1.000000000000000000, 0.8660254037844387076, 1.000000000000000000, 0.9330127018922192983, 0.9330127018922194093 ) ) 
 REPRESENTATION_ITEM ( '' )  );
#5985 = CARTESIAN_POINT ( 'NONE',  ( -59.59170313451811296, -127.5000000013656347, 1.485763867205729394 ) ) ;
#5986 = CARTESIAN_POINT ( 'NONE',  ( -59.59170313451810586, -141.5000000013656063, 1.485763867205729394 ) ) ;
#5987 = CARTESIAN_POINT ( 'NONE',  ( 4.458734125000000326, -20.89583333196774007, 2.574251347313718519 ) ) ;
#5988 = CARTESIAN_POINT ( 'NONE',  ( 2.229367062499998831, 7.104166668032259935, -3.861377020970580887 ) ) ;
#5989 = EDGE_CURVE ( 'NONE', #57220, #57225, #52079, .T. ) ;
#5990 = CARTESIAN_POINT ( 'NONE',  ( -4.458734124999997661, -63.47916666530106511, 2.574251347313722516 ) ) ;
#5991 = CARTESIAN_POINT ( 'NONE',  ( 1.975475456537005874E-15, -48.62499999726880162, 5.000000000000000000 ) ) ;
#5992 = CARTESIAN_POINT ( 'NONE',  ( 2.229367062499998831, -18.64583333196774007, -3.861377020970580887 ) ) ;
#5993 = CARTESIAN_POINT ( 'NONE',  ( -2.499999999999996447, -32.83333333333332860, 4.330127018922195425 ) ) ;
#5994 = CARTESIAN_POINT ( 'NONE',  ( 2.071067811865475505, -149.8125000000000284, -5.000000000000000888 ) ) ;
#5995 = CARTESIAN_POINT ( 'NONE',  ( 2.500000000000002220, -13.66666666666666785, 4.330127018922192761 ) ) ;
#5996 = EDGE_CURVE ( 'NONE', #43569, #38517, #19171, .T. ) ;
#5997 = CARTESIAN_POINT ( 'NONE',  ( -4.458734125000001214, -153.8750000013655779, 1.846868145590734089 ) ) ;
#5998 = ORIENTED_EDGE ( 'NONE', *, *, #53865, .T. ) ;
#5999 = CARTESIAN_POINT ( 'NONE',  ( -4.458734124999997661, -48.47916666530106511, 2.574251347313722516 ) ) ;
#6000 = CARTESIAN_POINT ( 'NONE',  ( 0.000000000000000000, -120.0000000000000000, 0.000000000000000000 ) ) ;
#6001 = EDGE_CURVE ( 'NONE', #20671, #10973, #3609, .T. ) ;
#6002 = EDGE_CURVE ( 'NONE', #52361, #5879, #47687, .T. ) ;
#6003 = CARTESIAN_POINT ( 'NONE',  ( -2.229367062499996610, -90.14583333196773651, 3.861377020970582219 ) ) ;
#6004 = CARTESIAN_POINT ( 'NONE',  ( 2.229367062499998831, 5.354166668032261711, -3.861377020970580887 ) ) ;
#6005 =( BOUNDED_CURVE ( )  B_SPLINE_CURVE ( 2, ( #33676, #23726, #54492, #43629, #43013, #18575, #48468, #38802, #33057 ),
 .UNSPECIFIED., .F., .F. ) 
 B_SPLINE_CURVE_WITH_KNOTS ( ( 3, 2, 2, 2, 3 ),
 ( 0.3083333333333336257, 0.3125000000000002776, 0.3166666666666669294, 0.3208333333333336368, 0.3250000000000002887 ),
 .UNSPECIFIED. ) 
 CURVE ( )  GEOMETRIC_REPRESENTATION_ITEM ( )  RATIONAL_B_SPLINE_CURVE ( ( 0.9999999999999948930, 0.9238795325112918455, 1.000000000000000000, 0.9238795325112867385, 1.000000000000000000, 0.9238795325112867385, 1.000000000000000000, 0.9238795325112816315, 1.000000000000005107 ) ) 
 REPRESENTATION_ITEM ( '' )  );
#6006 = CARTESIAN_POINT ( 'NONE',  ( -1.339745962155613812, -44.20534180126147561, -5.000000000000000000 ) ) ;
#6007 = CARTESIAN_POINT ( 'NONE',  ( 0.000000000000000000, -120.0000000000000000, 0.000000000000000000 ) ) ;
#6008 = CARTESIAN_POINT ( 'NONE',  ( 1.975475456537005874E-15, -82.74999999999998579, 5.000000000000000000 ) ) ;
#6009 = CARTESIAN_POINT ( 'NONE',  ( -4.458734124999998549, 18.52083333469892779, 2.574251347313722516 ) ) ;
#6010 = CARTESIAN_POINT ( 'NONE',  ( -4.999999999999999112, -72.91666666666665719, 2.886751345948131764 ) ) ;
#6011 = CARTESIAN_POINT ( 'NONE',  ( 5.000000000000000000, 10.70833333606452165, -2.886751345948129988 ) ) ;
#6012 = EDGE_LOOP ( 'NONE', ( #16142, #7599, #62247, #13225 ) ) ;
#6013 = CARTESIAN_POINT ( 'NONE',  ( -5.000000000000000000, 7.916666666666665186, -2.886751345948128211 ) ) ;
#6014 = VERTEX_POINT ( 'NONE', #28070 ) ;
#6015 = CARTESIAN_POINT ( 'NONE',  ( -1.339745962155610925, -53.66965819600733312, 5.000000000000000000 ) ) ;
#6016 = CARTESIAN_POINT ( 'NONE',  ( -4.458734124999999437, -45.39583333196773651, -2.574251347313719407 ) ) ;
#6017 = CARTESIAN_POINT ( 'NONE',  ( -3.535250795749689387E-16, -38.12499999726881583, -5.773502691896257311 ) ) ;
#6018 = ORIENTED_EDGE ( 'NONE', *, *, #18800, .T. ) ;
#6019 = CARTESIAN_POINT ( 'NONE',  ( 4.458734125000001214, -16.89583333196773651, 2.574251347313718519 ) ) ;
#6020 = ORIENTED_EDGE ( 'NONE', *, *, #25040, .F. ) ;
#6021 = CARTESIAN_POINT ( 'NONE',  ( -4.999999999999999112, -81.91666666666665719, 2.886751345948131764 ) ) ;
#6022 = CARTESIAN_POINT ( 'NONE',  ( 3.152801135295367541, -168.3125000013656063, -3.152801135295367541 ) ) ;
#6023 = AXIS2_PLACEMENT_3D ( 'NONE', #38676, #58315, #24210 ) ;
#6024 = CARTESIAN_POINT ( 'NONE',  ( 5.000000000000000000, -85.29166666393547303, -2.886751345948129988 ) ) ;
#6026 = VERTEX_POINT ( 'NONE', #3638 ) ;
#6025 = CARTESIAN_POINT ( 'NONE',  ( 5.000000000000000000, -20.37499999726880873, -6.123233995736766282E-16 ) ) ;
#6027 = CARTESIAN_POINT ( 'NONE',  ( -50.18089887299979068, -142.6875000000000284, 2.462841084822635640 ) ) ;
#6028 = VECTOR ( 'NONE', #41913, 1000.000000000000000 ) ;
#6029 = CARTESIAN_POINT ( 'NONE',  ( -4.458734124999998549, -26.47916666530107221, 2.574251347313722516 ) ) ;
#6030 = CARTESIAN_POINT ( 'NONE',  ( -2.500000000000000444, -84.16666666666667140, -4.330127018922193649 ) ) ;
#6031 = ORIENTED_EDGE ( 'NONE', *, *, #18172, .F. ) ;
#6032 = PRODUCT_CONTEXT ( 'NONE', #56132, 'mechanical' ) ;
#6033 = CARTESIAN_POINT ( 'NONE',  ( -1.846868145590734756, -164.3750000013656063, -4.458734125000000326 ) ) ;
#6034 = CARTESIAN_POINT ( 'NONE',  ( -2.229367062500000163, 27.52083333469892779, -3.861377020970580443 ) ) ;
#6035 = ORIENTED_EDGE ( 'NONE', *, *, #23566, .T. ) ;
#6036 = CARTESIAN_POINT ( 'NONE',  ( -50.70258187064364108, -148.3750000013656063, 2.196230717870141014 ) ) ;
#6037 = CARTESIAN_POINT ( 'NONE',  ( 4.458734125000001214, -76.14583333196773651, 2.574251347313718519 ) ) ;
#6038 = CARTESIAN_POINT ( 'NONE',  ( -55.39835681537999790, -133.0000000027312126, 4.984105922594378235 ) ) ;
#6039 = CARTESIAN_POINT ( 'NONE',  ( 4.458734125000000326, -42.89583333196773651, 2.574251347313718519 ) ) ;
#6040 = CARTESIAN_POINT ( 'NONE',  ( -4.458734125000000326, -143.1250000013656063, 1.846868145590734089 ) ) ;
#6041 = CARTESIAN_POINT ( 'NONE',  ( -4.999999999999998224, 23.08333333333333215, 2.886751345948131764 ) ) ;
#6042 = CARTESIAN_POINT ( 'NONE',  ( 4.458734124999999437, -46.81249999863440792, -5.460374474430324690E-16 ) ) ;
#6043 = CARTESIAN_POINT ( 'NONE',  ( -2.352990130084580066E-16, 8.660254037844390851, -10.00000000000000000 ) ) ;
#6044 = CARTESIAN_POINT ( 'NONE',  ( -2.229367062499996610, -16.14583333196773651, 3.861377020970582219 ) ) ;
#6045 = CARTESIAN_POINT ( 'NONE',  ( 5.000000000000000888, -103.5833333333333428, 2.886751345948126879 ) ) ;
#6046 = CARTESIAN_POINT ( 'NONE',  ( 2.730187237215162345E-16, -141.4375000013656063, -4.458734124999999437 ) ) ;
#6047 = CARTESIAN_POINT ( 'NONE',  ( 2.229367062500001939, -35.22916666530107221, 3.861377020970579999 ) ) ;
#6048 = CARTESIAN_POINT ( 'NONE',  ( 2.500000000000002220, 6.458333336064519870, 4.330127018922192761 ) ) ;
#6049 = CARTESIAN_POINT ( 'NONE',  ( -6.972266317189433020E-16, -40.12499999726880162, -5.000000000000000000 ) ) ;
#6050 = CARTESIAN_POINT ( 'NONE',  ( -52.10840900171896806, -130.1875000013656063, 3.393966926194110556 ) ) ;
#6051 = CARTESIAN_POINT ( 'NONE',  ( 4.458734124999998549, -75.97916666530106511, -2.574251347313721627 ) ) ;
#6052 = CARTESIAN_POINT ( 'NONE',  ( -55.39835681537999790, -146.0000000027312126, 4.984105922594378235 ) ) ;
#6053 = CARTESIAN_POINT ( 'NONE',  ( 1.339745962155602488, 14.41965820146970501, 5.000000000000007105 ) ) ;
#6054 = CARTESIAN_POINT ( 'NONE',  ( -3.152548672688508926E-16, 2.187500001365593416, -5.148502694627439702 ) ) ;
#6055 =( BOUNDED_CURVE ( )  B_SPLINE_CURVE ( 2, ( #62334, #17310, #18255, #36936, #42063, #27585, #52670, #37882, #61705 ),
 .UNSPECIFIED., .F., .F. ) 
 B_SPLINE_CURVE_WITH_KNOTS ( ( 3, 2, 2, 2, 3 ),
 ( 0.5437499999999999556, 0.5444444444444443976, 0.5458333333333332815, 0.5472222222222222765, 0.5479166666666667185 ),
 .UNSPECIFIED. ) 
 CURVE ( )  GEOMETRIC_REPRESENTATION_ITEM ( )  RATIONAL_B_SPLINE_CURVE ( ( 0.9330127018922194093, 0.9330127018922194093, 1.000000000000000000, 0.8660254037844387076, 1.000000000000000000, 0.8660254037844387076, 1.000000000000000000, 0.9330127018922194093, 0.9330127018922194093 ) ) 
 REPRESENTATION_ITEM ( '' )  );
#6056 = VERTEX_POINT ( 'NONE', #54334 ) ;
#6057 = CARTESIAN_POINT ( 'NONE',  ( -3.535533905932737309, -159.6250000000000284, -3.535533905932738197 ) ) ;
#6058 = CARTESIAN_POINT ( 'NONE',  ( -5.000000000000000000, -60.00000000000000000, 0.000000000000000000 ) ) ;
#6060 = CARTESIAN_POINT ( 'NONE',  ( -4.458734124999998549, -33.22916666530107221, 2.574251347313722516 ) ) ;
#6059 = CARTESIAN_POINT ( 'NONE',  ( -2.229367062500000163, -88.47916666530106511, -3.861377020970580443 ) ) ;
#6061 = CARTESIAN_POINT ( 'NONE',  ( 2.229367062500001939, -82.22916666530106511, 3.861377020970579999 ) ) ;
#6062 = CARTESIAN_POINT ( 'NONE',  ( -4.458734124999999437, 19.35416666803225993, -2.574251347313719407 ) ) ;
#6063 = CARTESIAN_POINT ( 'NONE',  ( -52.10840900171896806, -139.1875000013656347, 3.393966926194110556 ) ) ;
#6064 = CARTESIAN_POINT ( 'NONE',  ( 4.458734125000000326, -3.895833331967739177, 2.574251347313718519 ) ) ;
#6065 = CARTESIAN_POINT ( 'NONE',  ( -4.458734124999999437, 23.35416666803226349, -2.574251347313719407 ) ) ;
#6066 = CARTESIAN_POINT ( 'NONE',  ( -2.229367062500000163, -45.72916666530106511, -3.861377020970580443 ) ) ;
#6067 = DIRECTION ( 'NONE',  ( -0.000000000000000000, 1.000000000000000000, -0.000000000000000000 ) ) ;
#6068 = CARTESIAN_POINT ( 'NONE',  ( 4.458734124999999437, -87.81249999863439371, -5.460374474430324690E-16 ) ) ;
#6069 = CARTESIAN_POINT ( 'NONE',  ( -4.458734124999999437, -4.395833331967740065, -2.574251347313719407 ) ) ;
#6070 = EDGE_CURVE ( 'NONE', #29896, #2056, #23333, .T. ) ;
#6071 = ORIENTED_EDGE ( 'NONE', *, *, #30714, .F. ) ;
#6072 = CARTESIAN_POINT ( 'NONE',  ( -4.458734124999997661, -30.47916666530107221, 2.574251347313722516 ) ) ;
#6073 = CARTESIAN_POINT ( 'NONE',  ( -53.51423613279429503, -132.5000000013656063, 4.591703134518082763 ) ) ;
#6074 = CARTESIAN_POINT ( 'NONE',  ( 2.229367062499998831, -76.64583333196773651, -3.861377020970580887 ) ) ;
#6075 = CARTESIAN_POINT ( 'NONE',  ( 4.458734125000001214, 28.85416666803225993, 2.574251347313718519 ) ) ;
#6076 = AXIS2_PLACEMENT_3D ( 'NONE', #33000, #47468, #33308 ) ;
#6077 = CARTESIAN_POINT ( 'NONE',  ( 4.458734124999998549, 19.27083333469893134, -2.574251347313721627 ) ) ;
#6078 = EDGE_CURVE ( 'NONE', #2252, #14226, #25775, .T. ) ;
#6079 = DIRECTION ( 'NONE',  ( 0.000000000000000000, 1.000000000000000000, 0.000000000000000000 ) ) ;
#6080 = CARTESIAN_POINT ( 'NONE',  ( -2.499999999999996447, -25.70833333060214798, 4.330127018922195425 ) ) ;
#6081 = CARTESIAN_POINT ( 'NONE',  ( 2.229367062500001939, -79.22916666530106511, 3.861377020970579999 ) ) ;
#6082 = CARTESIAN_POINT ( 'NONE',  ( -5.000000000000000000, -57.08333333333333570, -2.886751345948128211 ) ) ;
#6083 = CARTESIAN_POINT ( 'NONE',  ( 5.000000000000000888, 24.54166666939784847, 2.886751345948126879 ) ) ;
#6084 = ORIENTED_EDGE ( 'NONE', *, *, #7605, .F. ) ;
#6085 =( BOUNDED_CURVE ( )  B_SPLINE_CURVE ( 2, ( #6787, #1656, #16748, #12241, #16110, #55681, #31854, #35736, #36365 ),
 .UNSPECIFIED., .F., .F. ) 
 B_SPLINE_CURVE_WITH_KNOTS ( ( 3, 2, 2, 2, 3 ),
 ( 0.6687499999999999556, 0.6694444444444443976, 0.6708333333333332815, 0.6722222222222222765, 0.6729166666666667185 ),
 .UNSPECIFIED. ) 
 CURVE ( )  GEOMETRIC_REPRESENTATION_ITEM ( )  RATIONAL_B_SPLINE_CURVE ( ( 0.9330127018922194093, 0.9330127018922194093, 1.000000000000000000, 0.8660254037844387076, 1.000000000000000000, 0.8660254037844387076, 1.000000000000000000, 0.9330127018922194093, 0.9330127018922194093 ) ) 
 REPRESENTATION_ITEM ( '' )  );
#6087 = CARTESIAN_POINT ( 'NONE',  ( -3.535250795749689387E-16, -17.25000000000000000, -5.773502691896257311 ) ) ;
#6086 = CARTESIAN_POINT ( 'NONE',  ( 2.499999999999998668, -0.3333333333333348136, -4.330127018922193649 ) ) ;
#6088 = CARTESIAN_POINT ( 'NONE',  ( -2.229367062499996610, -21.14583333196774007, 3.861377020970582219 ) ) ;
#6089 = CARTESIAN_POINT ( 'NONE',  ( 2.229367062500001939, -84.97916666530107932, 3.861377020970579999 ) ) ;
#6090 = CARTESIAN_POINT ( 'NONE',  ( 2.499999999999998668, -24.20833333060214443, -4.330127018922193649 ) ) ;
#6092 = ORIENTED_EDGE ( 'NONE', *, *, #29563, .F. ) ;
#6091 = CARTESIAN_POINT ( 'NONE',  ( 2.229367062500001939, -56.97916666530107932, 3.861377020970579999 ) ) ;
#6093 = CARTESIAN_POINT ( 'NONE',  ( 5.000000000000000000, -49.41666666666666430, -2.886751345948130876 ) ) ;
#6094 = CARTESIAN_POINT ( 'NONE',  ( -6.972266317189433020E-16, -59.12499999726880873, -5.000000000000000000 ) ) ;
#6096 = ORIENTED_EDGE ( 'NONE', *, *, #9100, .T. ) ;
#6095 = CARTESIAN_POINT ( 'NONE',  ( -4.458734124999999437, -1.645833331967737401, -2.574251347313719407 ) ) ;
#6097 = CARTESIAN_POINT ( 'NONE',  ( -53.51423613279429503, -149.2500000013656063, 4.591703134518083651 ) ) ;
#6098 = CARTESIAN_POINT ( 'NONE',  ( 1.060575238724906964E-15, -66.75000000000000000, 5.773502691896257311 ) ) ;
#6099 = CARTESIAN_POINT ( 'NONE',  ( 3.152801135295367541, -153.5625000013656063, -3.152801135295367541 ) ) ;
#6100 = CARTESIAN_POINT ( 'NONE',  ( -4.458734124999999437, -45.64583333196774362, -2.574251347313719407 ) ) ;
#6101 = CARTESIAN_POINT ( 'NONE',  ( 2.500000000000002220, -23.66666666666666785, 4.330127018922192761 ) ) ;
#6102 = CARTESIAN_POINT ( 'NONE',  ( -3.535533905932738641, -158.3750000000000284, 3.535533905932737309 ) ) ;
#6103 = DIRECTION ( 'NONE',  ( -0.6485228581062915110, 0.000000000000000000, -0.7611951803011149931 ) ) ;
#6104 = CARTESIAN_POINT ( 'NONE',  ( -49.85088928181150436, -152.5625000000000284, -1.666127454062680702 ) ) ;
#6105 = CARTESIAN_POINT ( 'NONE',  ( -4.458734124999999437, -12.56249999863440259, 0.000000000000000000 ) ) ;
#6106 = CARTESIAN_POINT ( 'NONE',  ( -2.229367062499996610, -49.39583333196772941, 3.861377020970582219 ) ) ;
#6107 = CARTESIAN_POINT ( 'NONE',  ( 1.339745962155615144, -89.70534180126146850, 4.999999999999999112 ) ) ;
#6108 = CARTESIAN_POINT ( 'NONE',  ( 1.846868145590735200, -145.2500000013655779, -4.458734125000000326 ) ) ;
#6109 = CARTESIAN_POINT ( 'NONE',  ( -2.229367062500000163, -95.72916666530107932, -3.861377020970580443 ) ) ;
#6110 = CARTESIAN_POINT ( 'NONE',  ( -1.339745962155623360, 21.33034180399265978, 4.999999999999991118 ) ) ;
#6111 = ORIENTED_EDGE ( 'NONE', *, *, #3135, .T. ) ;
#6112 = CARTESIAN_POINT ( 'NONE',  ( -1.339745962155610259, 26.91965820146970501, -5.000000000000002665 ) ) ;
#6113 = CARTESIAN_POINT ( 'NONE',  ( -4.458734124999999437, 26.35416666803226349, -2.574251347313719407 ) ) ;
#6114 = CARTESIAN_POINT ( 'NONE',  ( -58.80597590150559739, -148.1250000027312126, 3.242614290531460330 ) ) ;
#6115 = CARTESIAN_POINT ( 'NONE',  ( 1.975475456537005874E-15, -30.74999999999999645, 5.000000000000000000 ) ) ;
#6116 = AXIS2_PLACEMENT_3D ( 'NONE', #16506, #11988, #35494 ) ;
#6117 = ORIENTED_EDGE ( 'NONE', *, *, #42476, .F. ) ;
#6118 = CARTESIAN_POINT ( 'NONE',  ( 2.229367062499998831, -2.645833331967738289, -3.861377020970580887 ) ) ;
#6119 = EDGE_CURVE ( 'NONE', #17008, #41671, #14761, .T. ) ;
#6120 = CARTESIAN_POINT ( 'NONE',  ( 1.339745962155612702, -106.2946581987385173, -5.000000000000000000 ) ) ;
#6121 = CARTESIAN_POINT ( 'NONE',  ( 2.229367062499998831, -19.89583333196774007, -3.861377020970580887 ) ) ;
#6122 = CARTESIAN_POINT ( 'NONE',  ( 1.975475456537005874E-15, 11.37500000273118239, 5.000000000000000000 ) ) ;
#6123 = CARTESIAN_POINT ( 'NONE',  ( 4.458734124999998549, -6.729166665301073103, -2.574251347313721627 ) ) ;
#6124 = CARTESIAN_POINT ( 'NONE',  ( 2.730187237215162345E-16, -149.1875000013656063, -4.458734124999999437 ) ) ;
#6125 = CARTESIAN_POINT ( 'NONE',  ( -3.152548672688508926E-16, 15.18750000136559564, -5.148502694627439702 ) ) ;
#6126 = ORIENTED_EDGE ( 'NONE', *, *, #31958, .F. ) ;
#6127 = CARTESIAN_POINT ( 'NONE',  ( -5.000000000000000000, -13.95833333060214976, -2.886751345948128211 ) ) ;
#6128 = CARTESIAN_POINT ( 'NONE',  ( 6.123233995736766282E-16, -120.0000000000000000, -5.000000000000000000 ) ) ;
#6129 = CARTESIAN_POINT ( 'NONE',  ( -3.152548672688508926E-16, -19.56249999863440081, -5.148502694627439702 ) ) ;
#6130 = CARTESIAN_POINT ( 'NONE',  ( 7.500000000000001776, 0.000000000000000000, 0.000000000000000000 ) ) ;
#6131 = CARTESIAN_POINT ( 'NONE',  ( 5.000000000000000888, -88.45833333060214443, 2.886751345948126879 ) ) ;
#6132 = CARTESIAN_POINT ( 'NONE',  ( -53.51423613279429503, -149.2500000013655779, 4.591703134518082763 ) ) ;
#6133 = CARTESIAN_POINT ( 'NONE',  ( -5.000000000000000000, -45.87499999726880873, 0.000000000000000000 ) ) ;
#6134 = CARTESIAN_POINT ( 'NONE',  ( -6.972266317189433020E-16, 20.87500000273118062, -5.000000000000000000 ) ) ;
#6135 = CARTESIAN_POINT ( 'NONE',  ( 2.229367062499998831, 15.35416666803225993, -3.861377020970580887 ) ) ;
#6136 = DIRECTION ( 'NONE',  ( 0.000000000000000000, 0.000000000000000000, 1.000000000000000000 ) ) ;
#6137 = DIRECTION ( 'NONE',  ( 0.000000000000000000, 1.000000000000000000, 0.000000000000000000 ) ) ;
#6138 = CARTESIAN_POINT ( 'NONE',  ( -4.458734124999997661, 13.77083333469892779, 2.574251347313722516 ) ) ;
#6139 = CARTESIAN_POINT ( 'NONE',  ( -4.458734124999999437, -67.39583333196773651, -2.574251347313719407 ) ) ;
#6140 = ORIENTED_EDGE ( 'NONE', *, *, #30712, .T. ) ;
#6141 = CARTESIAN_POINT ( 'NONE',  ( 4.458734124999998549, -13.97916666530107221, -2.574251347313721627 ) ) ;
#6142 = CARTESIAN_POINT ( 'NONE',  ( 5.000000000000000888, 2.416666666666667851, 2.886751345948126879 ) ) ;
#6143 = CARTESIAN_POINT ( 'NONE',  ( 4.458734124999999437, -162.4375000013655779, 0.000000000000000000 ) ) ;
#6144 = CARTESIAN_POINT ( 'NONE',  ( -5.000000000000000000, 21.91666666666666785, -2.886751345948128211 ) ) ;
#6145 = CARTESIAN_POINT ( 'NONE',  ( 2.229367062499998831, -59.64583333196774362, -3.861377020970580887 ) ) ;
#6146 = CARTESIAN_POINT ( 'NONE',  ( 5.000000000000000888, -95.45833333060213022, 2.886751345948126879 ) ) ;
#6147 = CARTESIAN_POINT ( 'NONE',  ( 4.458734125000000326, -34.89583333196772941, 2.574251347313718519 ) ) ;
#6148 = CARTESIAN_POINT ( 'NONE',  ( -4.999999999999998224, -41.79166666393548013, 2.886751345948131764 ) ) ;
#6149 = CARTESIAN_POINT ( 'NONE',  ( 1.339745962155616255, 25.83034180399265622, -4.999999999999997335 ) ) ;
#6150 = DIRECTION ( 'NONE',  ( -0.000000000000000000, 1.000000000000000000, -0.000000000000000000 ) ) ;
#6151 = CARTESIAN_POINT ( 'NONE',  ( -6.972266317189433020E-16, -18.12499999726881228, -5.000000000000000000 ) ) ;
#6152 = CARTESIAN_POINT ( 'NONE',  ( 4.458734124999997661, -148.7500000013656063, 1.846868145590737864 ) ) ;
#6153 = CARTESIAN_POINT ( 'NONE',  ( 5.000000000000000888, -43.58333333333333570, 2.886751345948126879 ) ) ;
#6154 = CARTESIAN_POINT ( 'NONE',  ( -5.000000000000000000, 19.00000000000000000, 0.000000000000000000 ) ) ;
#6155 = CARTESIAN_POINT ( 'NONE',  ( 1.339745962155615144, -86.58034179853028434, 4.999999999999999112 ) ) ;
#6156 = ORIENTED_EDGE ( 'NONE', *, *, #32619, .F. ) ;
#6157 = CARTESIAN_POINT ( 'NONE',  ( 4.458734124999999437, -104.8124999986344079, -5.460374474430324690E-16 ) ) ;
#6158 = CARTESIAN_POINT ( 'NONE',  ( 2.229367062499998831, 2.104166668032262599, -3.861377020970580887 ) ) ;
#6159 = CARTESIAN_POINT ( 'NONE',  ( -1.339745962155613812, -9.080341798530296771, -5.000000000000000000 ) ) ;
#6160 = CARTESIAN_POINT ( 'NONE',  ( 5.000000000000000000, -1.500000000000001332, -6.123233995736766282E-16 ) ) ;
#6161 = VECTOR ( 'NONE', #8598, 1000.000000000000000 ) ;
#6162 = CARTESIAN_POINT ( 'NONE',  ( 2.229367062499998831, -67.64583333196773651, -3.861377020970580887 ) ) ;
#6163 = CARTESIAN_POINT ( 'NONE',  ( -5.000000000000000000, -8.958333330602146205, -2.886751345948128211 ) ) ;
#6165 = VERTEX_POINT ( 'NONE', #34379 ) ;
#6164 = CARTESIAN_POINT ( 'NONE',  ( 2.229367062500001939, -35.97916666530107221, 3.861377020970579999 ) ) ;
#6166 = CARTESIAN_POINT ( 'NONE',  ( -6.972266317189433020E-16, -33.24999999999999289, -5.000000000000000000 ) ) ;
#6167 = DIRECTION ( 'NONE',  ( -0.000000000000000000, 1.000000000000000000, -0.000000000000000000 ) ) ;
#6169 = ORIENTED_EDGE ( 'NONE', *, *, #35440, .T. ) ;
#6168 = CARTESIAN_POINT ( 'NONE',  ( -4.458734124999999437, 13.43750000136559386, 0.000000000000000000 ) ) ;
#6170 = CARTESIAN_POINT ( 'NONE',  ( -60.14911071818854538, -141.1875000027312126, 1.666127454062681146 ) ) ;
#6171 = CARTESIAN_POINT ( 'NONE',  ( 5.000000000000000000, -52.41666666666666430, -2.886751345948129988 ) ) ;
#6172 = CARTESIAN_POINT ( 'NONE',  ( -4.458734124999999437, -32.56249999863440792, 0.000000000000000000 ) ) ;
#6173 = LINE ( 'NONE', #59898, #18364 ) ;
#6174 = CARTESIAN_POINT ( 'NONE',  ( -4.458734124999999437, -76.31249999863440792, 0.000000000000000000 ) ) ;
#6175 = CARTESIAN_POINT ( 'NONE',  ( -3.152801135295367985, -141.0625000013655779, 3.152801135295367096 ) ) ;
#6177 = EDGE_CURVE ( 'NONE', #19698, #15898, #32346, .T. ) ;
#6176 = CARTESIAN_POINT ( 'NONE',  ( 4.458734125000001214, -82.89583333196772230, 2.574251347313718519 ) ) ;
#6178 = CARTESIAN_POINT ( 'NONE',  ( -54.64476657466781973, -135.0625000013656063, -4.444560631937228834 ) ) ;
#6179 = AXIS2_PLACEMENT_3D ( 'NONE', #13849, #9335, #58552 ) ;
#6180 = CARTESIAN_POINT ( 'NONE',  ( -4.458734124999999437, -31.56249999863440436, 0.000000000000000000 ) ) ;
#6181 =( BOUNDED_CURVE ( )  B_SPLINE_CURVE ( 2, ( #50341, #25577, #15611, #20438, #24941, #35229, #30067, #30391, #60002 ),
 .UNSPECIFIED., .F., .F. ) 
 B_SPLINE_CURVE_WITH_KNOTS ( ( 3, 2, 2, 2, 3 ),
 ( 0.6767857142857143238, 0.6773809523809524169, 0.6785714285714286031, 0.6797619047619047894, 0.6803571428571428825 ),
 .UNSPECIFIED. ) 
 CURVE ( )  GEOMETRIC_REPRESENTATION_ITEM ( )  RATIONAL_B_SPLINE_CURVE ( ( 0.9330127018922194093, 0.9330127018922194093, 1.000000000000000000, 0.8660254037844387076, 1.000000000000000000, 0.8660254037844387076, 1.000000000000000000, 0.9330127018922194093, 0.9330127018922194093 ) ) 
 REPRESENTATION_ITEM ( '' )  );
#6182 = ORIENTED_EDGE ( 'NONE', *, *, #11770, .T. ) ;
#6183 = CARTESIAN_POINT ( 'NONE',  ( 8.660254037844342889, 45.00000000000000000, 0.000000000000000000 ) ) ;
#6184 = ORIENTED_EDGE ( 'NONE', *, *, #35022, .T. ) ;
#6185 = CARTESIAN_POINT ( 'NONE',  ( -4.458734124999999437, -76.64583333196775072, -2.574251347313719407 ) ) ;
#6186 = DIRECTION ( 'NONE',  ( 0.000000000000000000, 1.000000000000000000, 0.000000000000000000 ) ) ;
#6187 = ORIENTED_EDGE ( 'NONE', *, *, #1987, .T. ) ;
#6188 = CYLINDRICAL_SURFACE ( 'NONE', #1883, 5.000000000000000000 ) ;
#6189 = CARTESIAN_POINT ( 'NONE',  ( -62.00000000000001421, -135.0000000000000284, 4.041451884327384114 ) ) ;
#6190 = CARTESIAN_POINT ( 'NONE',  ( 4.458734124999998549, -63.97916666530107221, -2.574251347313721627 ) ) ;
#6191 = CARTESIAN_POINT ( 'NONE',  ( -4.458734124999999437, -3.562499998634407916, 0.000000000000000000 ) ) ;
#6192 = ORIENTED_EDGE ( 'NONE', *, *, #29090, .T. ) ;
#6193 = CARTESIAN_POINT ( 'NONE',  ( -1.339745962155613812, 4.919658201469705006, -5.000000000000000000 ) ) ;
#6194 = CARTESIAN_POINT ( 'NONE',  ( -4.458734124999999437, 9.604166668032259935, -2.574251347313719407 ) ) ;
#6195 = CARTESIAN_POINT ( 'NONE',  ( -56.48576386720575471, -139.7500000013656347, -4.591703134518078322 ) ) ;
#6196 = CARTESIAN_POINT ( 'NONE',  ( -1.339745962155613812, -1.205341801261479828, -5.000000000000000000 ) ) ;
#6197 = CARTESIAN_POINT ( 'NONE',  ( 1.846868145590736310, -161.6250000013656063, 4.458734124999997661 ) ) ;
#6198 = DIRECTION ( 'NONE',  ( -0.000000000000000000, 1.000000000000000000, -0.000000000000000000 ) ) ;
#6199 = EDGE_LOOP ( 'NONE', ( #49567, #694, #63153, #44672 ) ) ;
#6200 = CARTESIAN_POINT ( 'NONE',  ( 9.457646018065525792E-16, -80.06249999863440792, 5.148502694627439702 ) ) ;
#6201 = CARTESIAN_POINT ( 'NONE',  ( 2.071067811865540342, -164.3125000027312410, 4.999999999999936051 ) ) ;
#6202 = CARTESIAN_POINT ( 'NONE',  ( -4.458734124999998549, -1.229166665301071326, 2.574251347313722516 ) ) ;
#6203 = VECTOR ( 'NONE', #42521, 1000.000000000000000 ) ;
#6204 = CARTESIAN_POINT ( 'NONE',  ( 5.000000000000000888, 25.54166666939784847, 2.886751345948126879 ) ) ;
#6205 = DIRECTION ( 'NONE',  ( -0.000000000000000000, 1.000000000000000000, -0.000000000000000000 ) ) ;
#6206 = CARTESIAN_POINT ( 'NONE',  ( 9.457646018065525792E-16, -68.31249999863442213, 5.148502694627439702 ) ) ;
#6207 = CARTESIAN_POINT ( 'NONE',  ( 5.000000000000000000, -33.29166666393547303, -2.886751345948129988 ) ) ;
#6208 = CARTESIAN_POINT ( 'NONE',  ( -5.000000000000000000, -28.99999999999999645, 0.000000000000000000 ) ) ;
#6209 = CARTESIAN_POINT ( 'NONE',  ( -2.229367062500000163, 29.52083333469892779, -3.861377020970580443 ) ) ;
#6210 = CARTESIAN_POINT ( 'NONE',  ( -5.000000000000000000, -82.95833333060214443, -2.886751345948128211 ) ) ;
#6211 = CARTESIAN_POINT ( 'NONE',  ( 9.457646018065525792E-16, 26.93750000136559564, 5.148502694627439702 ) ) ;
#6212 = CARTESIAN_POINT ( 'NONE',  ( -4.458734124999999437, -51.39583333196772941, -2.574251347313719407 ) ) ;
#6213 = CARTESIAN_POINT ( 'NONE',  ( 4.458734124999999437, -33.06249999863440792, -5.460374474430324690E-16 ) ) ;
#6214 = CARTESIAN_POINT ( 'NONE',  ( 2.229367062499998831, 1.104166668032261711, -3.861377020970580887 ) ) ;
#6215 = CARTESIAN_POINT ( 'NONE',  ( 5.000000000000000000, -151.0625000000000284, 2.071067811865478614 ) ) ;
#6216 = CARTESIAN_POINT ( 'NONE',  ( -2.499999999999996447, 21.16666666666666785, 4.330127018922195425 ) ) ;
#6217 = CARTESIAN_POINT ( 'NONE',  ( 2.071067811865475505, -144.9375000027311842, -5.000000000000000888 ) ) ;
#6218 = FACE_OUTER_BOUND ( 'NONE', #42278, .T. ) ;
#6219 = CARTESIAN_POINT ( 'NONE',  ( -4.458734124999999437, -41.31249999863440081, 0.000000000000000000 ) ) ;
#6220 = CARTESIAN_POINT ( 'NONE',  ( -4.999999999999999112, -78.79166666393547303, 2.886751345948131764 ) ) ;
#6221 = CARTESIAN_POINT ( 'NONE',  ( -50.55543936806279248, -142.3125000013656063, 0.3552334253322060320 ) ) ;
#6222 = LINE ( 'NONE', #40621, #2141 ) ;
#6223 = CARTESIAN_POINT ( 'NONE',  ( 2.499999999999998668, 3.666666666666665186, -4.330127018922193649 ) ) ;
#6224 = CARTESIAN_POINT ( 'NONE',  ( -4.458734124999999437, -79.64583333196773651, -2.574251347313719407 ) ) ;
#6225 = CARTESIAN_POINT ( 'NONE',  ( -3.152801135295367985, -162.0625000013656063, 3.152801135295367096 ) ) ;
#6226 =( BOUNDED_CURVE ( )  B_SPLINE_CURVE ( 2, ( #57614, #52776, #14779, #48248, #28319, #44045, #47936, #3889, #12 ),
 .UNSPECIFIED., .F., .F. ) 
 B_SPLINE_CURVE_WITH_KNOTS ( ( 3, 2, 2, 2, 3 ),
 ( 0.05833333333333338283, 0.06250000000000005551, 0.06666666666666672125, 0.07083333333333338699, 0.07500000000000005274 ),
 .UNSPECIFIED. ) 
 CURVE ( )  GEOMETRIC_REPRESENTATION_ITEM ( )  RATIONAL_B_SPLINE_CURVE ( ( 0.9999999999999991118, 0.9238795325112876267, 1.000000000000000000, 0.9238795325112867385, 1.000000000000000000, 0.9238795325112867385, 1.000000000000000000, 0.9238795325112857393, 1.000000000000001110 ) ) 
 REPRESENTATION_ITEM ( '' )  );
#6227 = CARTESIAN_POINT ( 'NONE',  ( 1.975475456537005874E-15, -43.75000000000000000, 5.000000000000000000 ) ) ;
#6228 = CARTESIAN_POINT ( 'NONE',  ( -2.621328321948020346, -7.606199919102354379, -7.633618187056584681 ) ) ;
#6229 = CARTESIAN_POINT ( 'NONE',  ( -4.999999999999999112, -24.91666666666666075, 2.886751345948131764 ) ) ;
#6230 = CARTESIAN_POINT ( 'NONE',  ( 1.975475456537005874E-15, -90.62499999726880162, 5.000000000000000000 ) ) ;
#6231 = ORIENTED_EDGE ( 'NONE', *, *, #36604, .T. ) ;
#6232 = CARTESIAN_POINT ( 'NONE',  ( -4.458734124999998549, 25.52083333469893134, 2.574251347313722516 ) ) ;
#6233 = ORIENTED_EDGE ( 'NONE', *, *, #13436, .T. ) ;
#6234 = CARTESIAN_POINT ( 'NONE',  ( 9.457646018065525792E-16, -64.31249999863440792, 5.148502694627439702 ) ) ;
#6235 =( BOUNDED_CURVE ( )  B_SPLINE_CURVE ( 2, ( #22534, #8669, #63031, #42130, #62084, #18000, #13507, #3852, #48214 ),
 .UNSPECIFIED., .F., .F. ) 
 B_SPLINE_CURVE_WITH_KNOTS ( ( 3, 2, 2, 2, 3 ),
 ( 0.5089285714285713969, 0.5095238095238094900, 0.5107142857142856762, 0.5119047619047618625, 0.5124999999999999556 ),
 .UNSPECIFIED. ) 
 CURVE ( )  GEOMETRIC_REPRESENTATION_ITEM ( )  RATIONAL_B_SPLINE_CURVE ( ( 0.9330127018922194093, 0.9330127018922194093, 1.000000000000000000, 0.8660254037844387076, 1.000000000000000000, 0.8660254037844387076, 1.000000000000000000, 0.9330127018922194093, 0.9330127018922194093 ) ) 
 REPRESENTATION_ITEM ( '' )  );
#6236 = CARTESIAN_POINT ( 'NONE',  ( -3.535250795749689387E-16, 20.87500000273118417, -5.773502691896257311 ) ) ;
#6237 = CARTESIAN_POINT ( 'NONE',  ( -6.972266317189433020E-16, -3.124999997268813612, -5.000000000000000000 ) ) ;
#6238 = CARTESIAN_POINT ( 'NONE',  ( -5.000000000000000000, 15.91666666666666430, -2.886751345948128211 ) ) ;
#6239 = CARTESIAN_POINT ( 'NONE',  ( 4.458734124999999437, -50.81249999863440792, -5.460374474430324690E-16 ) ) ;
#6240 = CARTESIAN_POINT ( 'NONE',  ( -4.458734124999999437, -13.39583333196774184, -2.574251347313719407 ) ) ;
#6241 = CARTESIAN_POINT ( 'NONE',  ( 1.975475456537005874E-15, -6.749999999999999112, 5.000000000000000000 ) ) ;
#6242 = CARTESIAN_POINT ( 'NONE',  ( 5.000000000000000888, -99.45833333060214443, 2.886751345948126879 ) ) ;
#6243 = CARTESIAN_POINT ( 'NONE',  ( 1.975475456537005874E-15, -63.74999999999998579, 5.000000000000000000 ) ) ;
#6244 = LINE ( 'NONE', #25854, #41211 ) ;
#6245 = CARTESIAN_POINT ( 'NONE',  ( 2.499999999999998668, -34.33333333333332860, -4.330127018922193649 ) ) ;
#6246 = CARTESIAN_POINT ( 'NONE',  ( 2.500000000000002220, -66.54166666393547303, 4.330127018922192761 ) ) ;
#6248 = CARTESIAN_POINT ( 'NONE',  ( 9.457646018065525792E-16, -12.31249999863440259, 5.148502694627439702 ) ) ;
#6247 = CARTESIAN_POINT ( 'NONE',  ( -2.500000000000000444, -34.16666666666666430, -4.330127018922193649 ) ) ;
#6249 = CARTESIAN_POINT ( 'NONE',  ( -6.972266317189433020E-16, 2.875000002731185500, -5.000000000000000000 ) ) ;
#6250 = CARTESIAN_POINT ( 'NONE',  ( 4.458734124999998549, -60.72916666530106511, -2.574251347313721627 ) ) ;
#6251 = CARTESIAN_POINT ( 'NONE',  ( -4.458734125000001214, -150.1250000013655779, 1.846868145590734089 ) ) ;
#6252 = VECTOR ( 'NONE', #19345, 1000.000000000000000 ) ;
#6254 = ADVANCED_FACE ( 'NONE', ( #50474 ), #10900, .T. ) ;
#6253 = CARTESIAN_POINT ( 'NONE',  ( 9.457646018065525792E-16, -64.06249999863440792, 5.148502694627439702 ) ) ;
#6255 = CARTESIAN_POINT ( 'NONE',  ( -4.999999999999999112, -56.79166666393548013, 2.886751345948131764 ) ) ;
#6256 = VERTEX_POINT ( 'NONE', #31156 ) ;
#6257 = CARTESIAN_POINT ( 'NONE',  ( -6.972266317189433020E-16, 13.74999999999999822, -5.000000000000000000 ) ) ;
#6258 = CARTESIAN_POINT ( 'NONE',  ( -2.229367062499996610, -1.395833331967737179, 3.861377020970582219 ) ) ;
#6259 = VERTEX_POINT ( 'NONE', #50138 ) ;
#6260 =( BOUNDED_CURVE ( )  B_SPLINE_CURVE ( 2, ( #14284, #4627, #63503, #4952, #34520, #39667, #49332, #38413, #15237 ),
 .UNSPECIFIED., .F., .F. ) 
 B_SPLINE_CURVE_WITH_KNOTS ( ( 3, 2, 2, 2, 3 ),
 ( 0.9937500000000000222, 0.9944444444444444642, 0.9958333333333333481, 0.9972222222222222321, 0.9979166666666666741 ),
 .UNSPECIFIED. ) 
 CURVE ( )  GEOMETRIC_REPRESENTATION_ITEM ( )  RATIONAL_B_SPLINE_CURVE ( ( 0.9330127018922194093, 0.9330127018922194093, 1.000000000000000000, 0.8660254037844387076, 1.000000000000000000, 0.8660254037844387076, 1.000000000000000000, 0.9330127018922194093, 0.9330127018922194093 ) ) 
 REPRESENTATION_ITEM ( '' )  );
#6262 = CARTESIAN_POINT ( 'NONE',  ( 1.975475456537005874E-15, -70.62499999726880162, 5.000000000000000000 ) ) ;
#6261 = CARTESIAN_POINT ( 'NONE',  ( -1.339745962155613812, -28.20534180126147916, -5.000000000000000000 ) ) ;
#6263 = CARTESIAN_POINT ( 'NONE',  ( -4.458734125000000326, -157.0000000013655779, -1.846868145590735644 ) ) ;
#6264 = ORIENTED_EDGE ( 'NONE', *, *, #13364, .T. ) ;
#6265 = EDGE_CURVE ( 'NONE', #19960, #43823, #45488, .T. ) ;
#6266 = CARTESIAN_POINT ( 'NONE',  ( -1.339745962155610925, -7.669658196007332229, 5.000000000000000000 ) ) ;
#6267 = CARTESIAN_POINT ( 'NONE',  ( -56.66612745406270335, -128.3125000000000284, -5.149110718188516067 ) ) ;
#6268 = CARTESIAN_POINT ( 'NONE',  ( 2.499999999999998668, -80.20833333060213022, -4.330127018922193649 ) ) ;
#6269 = CARTESIAN_POINT ( 'NONE',  ( 9.457646018065525792E-16, -50.31249999863440792, 5.148502694627439702 ) ) ;
#6270 = EDGE_LOOP ( 'NONE', ( #20058, #30046, #61888, #24145 ) ) ;
#6271 = CARTESIAN_POINT ( 'NONE',  ( -1.339745962155610925, 17.33034180399266688, 5.000000000000000000 ) ) ;
#6272 = EDGE_CURVE ( 'NONE', #47088, #29634, #54076, .T. ) ;
#6273 = CARTESIAN_POINT ( 'NONE',  ( 4.458734125000001214, 15.10416666803225993, 2.574251347313718519 ) ) ;
#6274 = CARTESIAN_POINT ( 'NONE',  ( 4.458734125000001214, 23.10416666803225993, 2.574251347313718519 ) ) ;
#6275 = CARTESIAN_POINT ( 'NONE',  ( -52.10840900171896806, -151.1875000013656063, 3.393966926194110556 ) ) ;
#6276 = DIRECTION ( 'NONE',  ( -0.000000000000000000, 1.000000000000000000, -0.000000000000000000 ) ) ;
#6277 = CARTESIAN_POINT ( 'NONE',  ( 5.000000000000000000, -25.41666666666666430, -2.886751345948130876 ) ) ;
#6278 =( BOUNDED_CURVE ( )  B_SPLINE_CURVE ( 2, ( #59878, #15799, #35739, #25120, #50205, #20634, #49566, #6155, #45705 ),
 .UNSPECIFIED., .F., .F. ) 
 B_SPLINE_CURVE_WITH_KNOTS ( ( 3, 2, 2, 2, 3 ),
 ( 0.8232142857142856762, 0.8238095238095237693, 0.8249999999999999556, 0.8261904761904761418, 0.8267857142857142350 ),
 .UNSPECIFIED. ) 
 CURVE ( )  GEOMETRIC_REPRESENTATION_ITEM ( )  RATIONAL_B_SPLINE_CURVE ( ( 0.9330127018922194093, 0.9330127018922194093, 1.000000000000000000, 0.8660254037844387076, 1.000000000000000000, 0.8660254037844387076, 1.000000000000000000, 0.9330127018922194093, 0.9330127018922194093 ) ) 
 REPRESENTATION_ITEM ( '' )  );
#6279 = CARTESIAN_POINT ( 'NONE',  ( -4.458734124999999437, -65.31249999863440792, 0.000000000000000000 ) ) ;
#6280 = FACE_OUTER_BOUND ( 'NONE', #42689, .T. ) ;
#6281 = CARTESIAN_POINT ( 'NONE',  ( 2.229367062500001939, 15.02083333469892779, 3.861377020970579999 ) ) ;
#6282 = EDGE_CURVE ( 'NONE', #14071, #897, #58635, .T. ) ;
#6283 = CARTESIAN_POINT ( 'NONE',  ( -1.339745962155610925, -78.66965819600731891, 5.000000000000000000 ) ) ;
#6284 = CARTESIAN_POINT ( 'NONE',  ( 5.000000000000000000, -157.1875000027312126, 2.071067811865478614 ) ) ;
#6285 = CARTESIAN_POINT ( 'NONE',  ( 4.458734124999998549, -55.97916666530107932, -2.574251347313721627 ) ) ;
#6286 = CARTESIAN_POINT ( 'NONE',  ( 1.060575238724906964E-15, -13.62499999726881050, 5.773502691896257311 ) ) ;
#6287 = CARTESIAN_POINT ( 'NONE',  ( -4.999999999999998224, -108.9166666666666572, 2.886751345948131764 ) ) ;
#6288 = CARTESIAN_POINT ( 'NONE',  ( -6.972266317189433020E-16, -9.124999997268814056, -5.000000000000000000 ) ) ;
#6289 = DIRECTION ( 'NONE',  ( -0.000000000000000000, 1.000000000000000000, -0.000000000000000000 ) ) ;
#6290 = DIRECTION ( 'NONE',  ( 0.000000000000000000, 1.000000000000000000, 0.000000000000000000 ) ) ;
#6291 = CARTESIAN_POINT ( 'NONE',  ( 4.458734124999998549, -16.97916666530107577, -2.574251347313721627 ) ) ;
#6292 = ORIENTED_EDGE ( 'NONE', *, *, #4725, .F. ) ;
#6293 = CARTESIAN_POINT ( 'NONE',  ( -6.972266317189433020E-16, 23.75000000000000000, -5.000000000000000000 ) ) ;
#6294 = CARTESIAN_POINT ( 'NONE',  ( -4.458734124999998549, -103.2291666653010509, 2.574251347313722516 ) ) ;
#6295 = CARTESIAN_POINT ( 'NONE',  ( 3.535533905932736864, -156.2500000027312126, 3.535533905932738641 ) ) ;
#6296 = VERTEX_POINT ( 'NONE', #26657 ) ;
#6297 = CARTESIAN_POINT ( 'NONE',  ( 9.457646018065525792E-16, -105.3124999986344221, 5.148502694627439702 ) ) ;
#6298 = CARTESIAN_POINT ( 'NONE',  ( -2.229367062500000163, -24.47916666530106866, -3.861377020970580443 ) ) ;
#6299 = CARTESIAN_POINT ( 'NONE',  ( 2.499999999999998668, -56.20833333060214443, -4.330127018922193649 ) ) ;
#6300 = CARTESIAN_POINT ( 'NONE',  ( -59.44456063193725015, -125.5625000013655921, -0.3552334253322034230 ) ) ;
#6301 = CARTESIAN_POINT ( 'NONE',  ( -59.29741812935640155, -141.6250000013655495, -2.196230717870135685 ) ) ;
#6302 = EDGE_CURVE ( 'NONE', #9342, #5864, #16048, .T. ) ;
#6303 = CARTESIAN_POINT ( 'NONE',  ( -4.458734124999999437, -21.31249999863440436, 0.000000000000000000 ) ) ;
#6304 = CARTESIAN_POINT ( 'NONE',  ( -3.152548672688508926E-16, -64.81249999863440792, -5.148502694627439702 ) ) ;
#6305 = PLANE ( 'NONE',  #50048 ) ;
#6306 = CARTESIAN_POINT ( 'NONE',  ( 2.229367062500001939, -20.97916666530107221, 3.861377020970579999 ) ) ;
#6307 = DIRECTION ( 'NONE',  ( 0.000000000000000000, 0.000000000000000000, 1.000000000000000000 ) ) ;
#6308 = CARTESIAN_POINT ( 'NONE',  ( 3.061616997868383141E-16, -151.7500000000000284, -5.000000000000000000 ) ) ;
#6309 = CARTESIAN_POINT ( 'NONE',  ( 2.499999999999998668, -12.33333333333333570, -4.330127018922193649 ) ) ;
#6310 = CARTESIAN_POINT ( 'NONE',  ( -3.152801135295367096, -150.0625000013655779, -3.152801135295367541 ) ) ;
#6311 = ORIENTED_EDGE ( 'NONE', *, *, #16922, .T. ) ;
#6312 = CARTESIAN_POINT ( 'NONE',  ( -4.458734124999999437, -48.56249999863440792, 0.000000000000000000 ) ) ;
#6313 = DIRECTION ( 'NONE',  ( -0.000000000000000000, 1.000000000000000000, -0.000000000000000000 ) ) ;
#6314 = CARTESIAN_POINT ( 'NONE',  ( 1.339745962155615144, -90.70534180126146850, 4.999999999999999112 ) ) ;
#6315 = CARTESIAN_POINT ( 'NONE',  ( 2.499999999999998668, 29.66666666666666430, -4.330127018922193649 ) ) ;
#6316 = CARTESIAN_POINT ( 'NONE',  ( 2.229367062499998831, 2.354166668032262599, -3.861377020970580887 ) ) ;
#6317 = CARTESIAN_POINT ( 'NONE',  ( -6.972266317189433020E-16, 1.875000002731185722, -5.000000000000000000 ) ) ;
#6318 = CARTESIAN_POINT ( 'NONE',  ( 2.499999999999998668, 13.66666666666666785, -4.330127018922193649 ) ) ;
#6319 = CARTESIAN_POINT ( 'NONE',  ( 1.339745962155615144, 20.41965820146970501, 4.999999999999999112 ) ) ;
#6320 = CARTESIAN_POINT ( 'NONE',  ( -2.229367062499996610, 13.60416666803226171, 3.861377020970582219 ) ) ;
#6321 = CARTESIAN_POINT ( 'NONE',  ( 1.060575238724906964E-15, -79.74999999999998579, 5.773502691896257311 ) ) ;
#6322 = CARTESIAN_POINT ( 'NONE',  ( 2.499999999999998668, 10.79166666939785202, -4.330127018922193649 ) ) ;
#6323 = ORIENTED_EDGE ( 'NONE', *, *, #11677, .T. ) ;
#6324 = CARTESIAN_POINT ( 'NONE',  ( -5.000000000000000000, -98.00000000000000000, 0.000000000000000000 ) ) ;
#6325 = ORIENTED_EDGE ( 'NONE', *, *, #26107, .F. ) ;
#6326 = CARTESIAN_POINT ( 'NONE',  ( -5.000000000000000000, -53.87499999726880162, 0.000000000000000000 ) ) ;
#6327 = CARTESIAN_POINT ( 'NONE',  ( 2.229367062499998831, -43.64583333196773651, -3.861377020970580887 ) ) ;
#6328 = CARTESIAN_POINT ( 'NONE',  ( 3.152801135295367541, -165.5625000013656063, -3.152801135295367541 ) ) ;
#6329 = EDGE_CURVE ( 'NONE', #49174, #48477, #45639, .T. ) ;
#6330 = CARTESIAN_POINT ( 'NONE',  ( 2.500000000000002220, -40.54166666393548013, 4.330127018922192761 ) ) ;
#6331 = EDGE_CURVE ( 'NONE', #3031, #48295, #35677, .T. ) ;
#6332 = ORIENTED_EDGE ( 'NONE', *, *, #11330, .F. ) ;
#6333 = CARTESIAN_POINT ( 'NONE',  ( 2.229367062500001939, -16.97916666530106866, 3.861377020970579999 ) ) ;
#6334 = ORIENTED_EDGE ( 'NONE', *, *, #4349, .F. ) ;
#6335 = CARTESIAN_POINT ( 'NONE',  ( 2.500000000000002220, -85.66666666666667140, 4.330127018922192761 ) ) ;
#6336 = CARTESIAN_POINT ( 'NONE',  ( 4.458734124999999437, -168.4375000013656063, 0.000000000000000000 ) ) ;
#6337 = CARTESIAN_POINT ( 'NONE',  ( 2.499999999999998668, -87.20833333060214443, -4.330127018922193649 ) ) ;
#6339 = VERTEX_POINT ( 'NONE', #55933 ) ;
#6338 = CARTESIAN_POINT ( 'NONE',  ( -6.972266317189433020E-16, -35.12499999726880873, -5.000000000000000000 ) ) ;
#6340 = AXIS2_PLACEMENT_3D ( 'NONE', #55896, #51702, #27556 ) ;
#6341 = CARTESIAN_POINT ( 'NONE',  ( -52.53715891517739323, -141.4375000000000284, -4.819101127000233298 ) ) ;
#6342 = CARTESIAN_POINT ( 'NONE',  ( -4.458734124999998549, -34.47916666530107221, 2.574251347313722516 ) ) ;
#6343 = CARTESIAN_POINT ( 'NONE',  ( 1.339745962155612702, -29.29465819873852084, -5.000000000000000000 ) ) ;
#6344 = EDGE_CURVE ( 'NONE', #38431, #5304, #1552, .T. ) ;
#6345 = ORIENTED_EDGE ( 'NONE', *, *, #52295, .T. ) ;
#6346 = CONTEXT_DEPENDENT_SHAPE_REPRESENTATION ( #14592, #58959 ) ;
#6347 = CARTESIAN_POINT ( 'NONE',  ( -4.458734124999998549, -78.22916666530106511, 2.574251347313722516 ) ) ;
#6348 = EDGE_CURVE ( 'NONE', #49819, #11304, #14663, .T. ) ;
#6349 = CARTESIAN_POINT ( 'NONE',  ( 4.458734124999998549, -108.9791666653010651, -2.574251347313721627 ) ) ;
#6350 = CARTESIAN_POINT ( 'NONE',  ( 3.061616997868383141E-16, -147.7500000000000284, -5.000000000000000000 ) ) ;
#6351 = ORIENTED_EDGE ( 'NONE', *, *, #40525, .F. ) ;
#6352 = FACE_OUTER_BOUND ( 'NONE', #5519, .T. ) ;
#6353 = CARTESIAN_POINT ( 'NONE',  ( -58.39396692619412477, -141.6875000013656063, 2.891590998281057701 ) ) ;
#6354 = CARTESIAN_POINT ( 'NONE',  ( -4.458734124999999437, -72.56249999863439371, 0.000000000000000000 ) ) ;
#6355 = CARTESIAN_POINT ( 'NONE',  ( -51.75738570946856498, -135.8750000027312410, 3.805975901505576964 ) ) ;
#6356 = CARTESIAN_POINT ( 'NONE',  ( -2.229367062500000163, -41.47916666530107932, -3.861377020970580443 ) ) ;
#6357 = CARTESIAN_POINT ( 'NONE',  ( 1.846868145590735200, -140.5000000013655779, -4.458734124999999437 ) ) ;
#6358 = CARTESIAN_POINT ( 'NONE',  ( -2.499999999999996447, -57.83333333333333570, 4.330127018922195425 ) ) ;
#6359 = CARTESIAN_POINT ( 'NONE',  ( 4.458734125000000326, -51.89583333196773651, 2.574251347313718519 ) ) ;
#6360 = CARTESIAN_POINT ( 'NONE',  ( -3.152548672688508926E-16, -44.56249999863440081, -5.148502694627439702 ) ) ;
#6361 = CARTESIAN_POINT ( 'NONE',  ( -6.972266317189433020E-16, -41.12499999726880162, -5.000000000000000000 ) ) ;
#6362 = CARTESIAN_POINT ( 'NONE',  ( 2.229367062500001939, -16.97916666530106866, 3.861377020970579999 ) ) ;
#6363 =( BOUNDED_CURVE ( )  B_SPLINE_CURVE ( 2, ( #12659, #7843, #27445, #12017, #3027, #42243, #22643, #60617, #2391 ),
 .UNSPECIFIED., .F., .F. ) 
 B_SPLINE_CURVE_WITH_KNOTS ( ( 3, 2, 2, 2, 3 ),
 ( 0.6416666666666662744, 0.6458333333333329263, 0.6499999999999996891, 0.6541666666666663410, 0.6583333333333329929 ),
 .UNSPECIFIED. ) 
 CURVE ( )  GEOMETRIC_REPRESENTATION_ITEM ( )  RATIONAL_B_SPLINE_CURVE ( ( 1.000000000000008216, 0.9238795325112786339, 1.000000000000000000, 0.9238795325112867385, 1.000000000000000000, 0.9238795325112867385, 1.000000000000000000, 0.9238795325112928447, 0.9999999999999938938 ) ) 
 REPRESENTATION_ITEM ( '' )  );
#6364 = CARTESIAN_POINT ( 'NONE',  ( -2.500000000000000444, -99.16666666666665719, -4.330127018922193649 ) ) ;
#6365 = LINE ( 'NONE', #60400, #57679 ) ;
#6366 = CARTESIAN_POINT ( 'NONE',  ( -2.229367062500000163, -36.72916666530107221, -3.861377020970580443 ) ) ;
#6367 = CARTESIAN_POINT ( 'NONE',  ( 5.000000000000000000, 6.625000002731185944, -6.123233995736766282E-16 ) ) ;
#6368 = CARTESIAN_POINT ( 'NONE',  ( -59.29741812935640155, -129.6250000013655779, -2.196230717870135685 ) ) ;
#6369 = CARTESIAN_POINT ( 'NONE',  ( 2.229367062500001939, -72.22916666530107932, 3.861377020970579999 ) ) ;
#6370 = CYLINDRICAL_SURFACE ( 'NONE', #50747, 5.000000000000000000 ) ;
#6371 = CARTESIAN_POINT ( 'NONE',  ( -2.498395430326213474E-14, 14.37500000273118417, 5.000000000000000000 ) ) ;
#6372 = CARTESIAN_POINT ( 'NONE',  ( 2.229367062500001939, 1.770833334698927786, 3.861377020970579999 ) ) ;
#6373 = ORIENTED_EDGE ( 'NONE', *, *, #40167, .T. ) ;
#6374 = CARTESIAN_POINT ( 'NONE',  ( 2.499999999999998668, 24.79166666939785202, -4.330127018922193649 ) ) ;
#6375 = CARTESIAN_POINT ( 'NONE',  ( 5.000000000000000000, 23.62500000273118417, -6.123233995736766282E-16 ) ) ;
#6377 = CARTESIAN_POINT ( 'NONE',  ( -2.229367062500000163, -37.47916666530107221, -3.861377020970580443 ) ) ;
#6376 = CARTESIAN_POINT ( 'NONE',  ( -4.458734124999999437, -87.31249999863439371, 0.000000000000000000 ) ) ;
#6378 = FACE_OUTER_BOUND ( 'NONE', #1014, .T. ) ;
#6379 = CARTESIAN_POINT ( 'NONE',  ( -4.458734124999999437, -80.56249999863440792, 0.000000000000000000 ) ) ;
#6380 = CARTESIAN_POINT ( 'NONE',  ( 4.458734125000000326, 16.85416666803225993, 2.574251347313718519 ) ) ;
#6381 = CARTESIAN_POINT ( 'NONE',  ( 1.975475456537005874E-15, -49.74999999999999289, 5.000000000000000000 ) ) ;
#6382 = CARTESIAN_POINT ( 'NONE',  ( -52.10840900171896806, -136.1875000013656063, 3.393966926194110556 ) ) ;
#6383 =( BOUNDED_CURVE ( )  B_SPLINE_CURVE ( 2, ( #36773, #8454, #17780, #32251, #37399, #32573, #52194, #56404, #57351 ),
 .UNSPECIFIED., .F., .F. ) 
 B_SPLINE_CURVE_WITH_KNOTS ( ( 3, 2, 2, 2, 3 ),
 ( 0.4124999999999999778, 0.4130952380952380709, 0.4142857142857143127, 0.4154761904761904989, 0.4160714285714285920 ),
 .UNSPECIFIED. ) 
 CURVE ( )  GEOMETRIC_REPRESENTATION_ITEM ( )  RATIONAL_B_SPLINE_CURVE ( ( 0.9330127018922194093, 0.9330127018922194093, 1.000000000000000000, 0.8660254037844387076, 1.000000000000000000, 0.8660254037844387076, 1.000000000000000000, 0.9330127018922194093, 0.9330127018922194093 ) ) 
 REPRESENTATION_ITEM ( '' )  );
#6384 = CARTESIAN_POINT ( 'NONE',  ( 9.457646018065525792E-16, -10.06249999863440614, 5.148502694627439702 ) ) ;
#6385 = CARTESIAN_POINT ( 'NONE',  ( -4.458734124999999437, 19.43750000136559208, 0.000000000000000000 ) ) ;
#6386 = CARTESIAN_POINT ( 'NONE',  ( 4.458734125000000326, -47.14583333196774362, 2.574251347313718519 ) ) ;
#6387 = CARTESIAN_POINT ( 'NONE',  ( 1.339745962155615144, -105.7053418012614685, 4.999999999999999112 ) ) ;
#6388 = CARTESIAN_POINT ( 'NONE',  ( 2.229367062500001939, -87.97916666530107932, 3.861377020970579999 ) ) ;
#6389 = CARTESIAN_POINT ( 'NONE',  ( 2.229367062500001939, -3.979166665301070438, 3.861377020970579999 ) ) ;
#6390 = LINE ( 'NONE', #55597, #29862 ) ;
#6391 = EDGE_LOOP ( 'NONE', ( #33069, #16377, #9474, #4205 ) ) ;
#6392 = CARTESIAN_POINT ( 'NONE',  ( 4.458734125000000326, -29.14583333196774007, 2.574251347313718519 ) ) ;
#6393 = CARTESIAN_POINT ( 'NONE',  ( -59.59170313451811296, -131.7500000013656063, 1.485763867205729394 ) ) ;
#6394 = CARTESIAN_POINT ( 'NONE',  ( 4.458734125000001214, -74.89583333196773651, 2.574251347313718519 ) ) ;
#6395 = CARTESIAN_POINT ( 'NONE',  ( 9.457646018065525792E-16, 27.68750000136559208, 5.148502694627439702 ) ) ;
#6396 = CARTESIAN_POINT ( 'NONE',  ( 4.458734124999998549, 18.27083333469893134, -2.574251347313721627 ) ) ;
#6397 = DIRECTION ( 'NONE',  ( -0.000000000000000000, 1.000000000000000000, -0.000000000000000000 ) ) ;
#6398 = CARTESIAN_POINT ( 'NONE',  ( -6.972266317189433020E-16, -44.12499999726880162, -5.000000000000000000 ) ) ;
#6399 = CARTESIAN_POINT ( 'NONE',  ( -2.229367062500000163, -77.72916666530106511, -3.861377020970580443 ) ) ;
#6400 = CARTESIAN_POINT ( 'NONE',  ( -5.000000000000000000, -62.08333333333332860, -2.886751345948128211 ) ) ;
#6401 = CARTESIAN_POINT ( 'NONE',  ( 1.339745962155612702, -90.16965819600733312, -5.000000000000000000 ) ) ;
#6402 = CARTESIAN_POINT ( 'NONE',  ( 5.000000000000000000, 24.62500000273118417, -6.123233995736766282E-16 ) ) ;
#6403 = VERTEX_POINT ( 'NONE', #24950 ) ;
#6404 = CARTESIAN_POINT ( 'NONE',  ( 1.975475456537005874E-15, -65.74999999999998579, 5.000000000000000000 ) ) ;
#6406 = CARTESIAN_POINT ( 'NONE',  ( -2.500000000000000444, -21.16666666666666785, -4.330127018922193649 ) ) ;
#6405 = CARTESIAN_POINT ( 'NONE',  ( -59.81910112700027327, -138.3125000027311842, -2.462841084822392279 ) ) ;
#6407 = CARTESIAN_POINT ( 'NONE',  ( -4.458734124999999437, -28.31249999863440081, 0.000000000000000000 ) ) ;
#6408 = CARTESIAN_POINT ( 'NONE',  ( -4.458734124999999437, -90.31249999863440792, 0.000000000000000000 ) ) ;
#6409 = EDGE_CURVE ( 'NONE', #54241, #47490, #21262, .T. ) ;
#6410 = CARTESIAN_POINT ( 'NONE',  ( 2.500000000000002220, -23.54166666393548368, 4.330127018922192761 ) ) ;
#6412 = ORIENTED_EDGE ( 'NONE', *, *, #48712, .T. ) ;
#6411 = CARTESIAN_POINT ( 'NONE',  ( -2.229367062500000163, -55.47916666530107221, -3.861377020970580443 ) ) ;
#6413 = CARTESIAN_POINT ( 'NONE',  ( 5.000000000000000888, -65.58333333333332860, 2.886751345948126879 ) ) ;
#6414 = CARTESIAN_POINT ( 'NONE',  ( 0.000000000000000000, -170.0000000000000000, 0.000000000000000000 ) ) ;
#6415 = AXIS2_PLACEMENT_3D ( 'NONE', #29129, #48752, #18855 ) ;
#6417 = ORIENTED_EDGE ( 'NONE', *, *, #28314, .F. ) ;
#6416 = CARTESIAN_POINT ( 'NONE',  ( 9.457646018065525792E-16, -1.312499998634405918, 5.148502694627439702 ) ) ;
#6418 = CARTESIAN_POINT ( 'NONE',  ( 5.000000000000000000, -66.50000000000000000, -6.123233995736766282E-16 ) ) ;
#6419 = CARTESIAN_POINT ( 'NONE',  ( 4.458734124999999437, -151.6875000013656063, 0.000000000000000000 ) ) ;
#6420 = CARTESIAN_POINT ( 'NONE',  ( 4.458734125000001214, -48.14583333196773651, 2.574251347313718519 ) ) ;
#6421 = CARTESIAN_POINT ( 'NONE',  ( 5.000000000000000000, -157.0625000000000000, 2.071067811865478614 ) ) ;
#6422 = CARTESIAN_POINT ( 'NONE',  ( 1.339745962155615144, -10.58034179853029144, 4.999999999999999112 ) ) ;
#6423 = CARTESIAN_POINT ( 'NONE',  ( -50.01589407740564042, -151.6250000000000284, 0.3983568153799778022 ) ) ;
#6424 = CARTESIAN_POINT ( 'NONE',  ( -4.458734124999999437, -18.64583333196774007, -2.574251347313719407 ) ) ;
#6425 = CARTESIAN_POINT ( 'NONE',  ( -2.229367062500000163, -53.72916666530107221, -3.861377020970580443 ) ) ;
#6426 = CARTESIAN_POINT ( 'NONE',  ( -5.000000000000000000, 1.000000000000000888, 0.000000000000000000 ) ) ;
#6427 = CARTESIAN_POINT ( 'NONE',  ( -4.458734124999999437, -142.9375000013656063, -5.460374474430324690E-16 ) ) ;
#6428 = CARTESIAN_POINT ( 'NONE',  ( -2.229367062499996610, -93.39583333196773651, 3.861377020970582219 ) ) ;
#6429 = DIRECTION ( 'NONE',  ( 0.000000000000000000, -1.000000000000000000, 0.000000000000000000 ) ) ;
#6430 = VERTEX_POINT ( 'NONE', #15296 ) ;
#6431 = EDGE_CURVE ( 'NONE', #45099, #23665, #20510, .T. ) ;
#6432 = CARTESIAN_POINT ( 'NONE',  ( -58.39396692619412477, -154.6875000013656063, 2.891590998281057701 ) ) ;
#6433 = CARTESIAN_POINT ( 'NONE',  ( -4.458734124999998549, 27.52083333469892779, 2.574251347313722516 ) ) ;
#6434 = CARTESIAN_POINT ( 'NONE',  ( -57.46284108482265651, -146.0625000027312126, 4.819101127000239515 ) ) ;
#6435 =( BOUNDED_CURVE ( )  B_SPLINE_CURVE ( 2, ( #30058, #46141, #35219, #54839, #55799, #54521, #60634, #25883, #55486 ),
 .UNSPECIFIED., .F., .F. ) 
 B_SPLINE_CURVE_WITH_KNOTS ( ( 3, 2, 2, 2, 3 ),
 ( 0.5395833333333333037, 0.5402777777777777457, 0.5416666666666666297, 0.5430555555555555136, 0.5437499999999999556 ),
 .UNSPECIFIED. ) 
 CURVE ( )  GEOMETRIC_REPRESENTATION_ITEM ( )  RATIONAL_B_SPLINE_CURVE ( ( 0.9330127018922194093, 0.9330127018922194093, 1.000000000000000000, 0.8660254037844387076, 1.000000000000000000, 0.8660254037844387076, 1.000000000000000000, 0.9330127018922194093, 0.9330127018922194093 ) ) 
 REPRESENTATION_ITEM ( '' )  );
#6436 = EDGE_CURVE ( 'NONE', #33038, #16025, #845, .T. ) ;
#6437 = CARTESIAN_POINT ( 'NONE',  ( -6.972266317189433020E-16, -63.25000000000000000, -5.000000000000000000 ) ) ;
#6438 = EDGE_LOOP ( 'NONE', ( #8572, #17535, #31971, #23025 ) ) ;
#6439 = CARTESIAN_POINT ( 'NONE',  ( -2.229367062500000163, -2.479166665301069106, -3.861377020970580443 ) ) ;
#6440 = EDGE_CURVE ( 'NONE', #14985, #43493, #63560, .T. ) ;
#6441 = CARTESIAN_POINT ( 'NONE',  ( 5.000000000000000000, -1.374999997268814500, -6.123233995736766282E-16 ) ) ;
#6442 = CARTESIAN_POINT ( 'NONE',  ( 4.458734125000001214, -18.14583333196773651, 2.574251347313718519 ) ) ;
#6443 = CARTESIAN_POINT ( 'NONE',  ( 1.339745962155615144, 11.41965820146970501, 4.999999999999999112 ) ) ;
#6444 = CARTESIAN_POINT ( 'NONE',  ( -2.229367062499996610, -8.145833331967736513, 3.861377020970582219 ) ) ;
#6445 = CARTESIAN_POINT ( 'NONE',  ( 2.325424218458714165, -7.317669739337183898, -7.030005583191490715 ) ) ;
#6446 = CARTESIAN_POINT ( 'NONE',  ( -4.458734125000000326, -150.8750000013655779, 1.846868145590734089 ) ) ;
#6447 = CARTESIAN_POINT ( 'NONE',  ( 4.458734124999998549, 15.02083333469892779, -2.574251347313721627 ) ) ;
#6448 = ORIENTED_EDGE ( 'NONE', *, *, #8391, .T. ) ;
#6449 = CARTESIAN_POINT ( 'NONE',  ( 1.975475456537005874E-15, -62.62499999726880873, 5.000000000000000000 ) ) ;
#6450 = CARTESIAN_POINT ( 'NONE',  ( -51.75738570946856498, -144.8750000027312126, 3.805975901505576964 ) ) ;
#6451 = CARTESIAN_POINT ( 'NONE',  ( 2.229367062500001939, -18.97916666530106866, 3.861377020970579999 ) ) ;
#6452 = DIRECTION ( 'NONE',  ( -0.000000000000000000, 1.000000000000000000, -0.000000000000000000 ) ) ;
#6453 = CARTESIAN_POINT ( 'NONE',  ( -6.972266317189433020E-16, -88.12499999726880162, -5.000000000000000000 ) ) ;
#6454 = CARTESIAN_POINT ( 'NONE',  ( -52.80376928212989185, -149.8750000013655779, -4.297418129356379346 ) ) ;
#6455 = CARTESIAN_POINT ( 'NONE',  ( 5.000000000000000888, -45.45833333060214443, 2.886751345948126879 ) ) ;
#6456 = CARTESIAN_POINT ( 'NONE',  ( 5.000000000000000000, -67.37499999726881583, -6.123233995736766282E-16 ) ) ;
#6457 = CARTESIAN_POINT ( 'NONE',  ( -4.458734124999999437, 7.687500001365594748, 0.000000000000000000 ) ) ;
#6458 = DIRECTION ( 'NONE',  ( 0.000000000000000000, 0.000000000000000000, 1.000000000000000000 ) ) ;
#6459 = DIRECTION ( 'NONE',  ( 0.000000000000000000, 0.000000000000000000, 1.000000000000000000 ) ) ;
#6460 = CARTESIAN_POINT ( 'NONE',  ( 4.458734125000000326, 14.10416666803226349, 2.574251347313718519 ) ) ;
#6461 = CARTESIAN_POINT ( 'NONE',  ( -3.152548672688508926E-16, -67.56249999863440792, -5.148502694627439702 ) ) ;
#6462 = CARTESIAN_POINT ( 'NONE',  ( 9.457646018065525792E-16, -15.31249999863440436, 5.148502694627439702 ) ) ;
#6463 =( BOUNDED_CURVE ( )  B_SPLINE_CURVE ( 2, ( #22984, #12050, #37146, #56770, #51932, #37770, #57401, #22031, #57084 ),
 .UNSPECIFIED., .F., .F. ) 
 B_SPLINE_CURVE_WITH_KNOTS ( ( 3, 2, 2, 2, 3 ),
 ( 0.8053571428571428825, 0.8059523809523809756, 0.8071428571428571619, 0.8083333333333333481, 0.8089285714285714413 ),
 .UNSPECIFIED. ) 
 CURVE ( )  GEOMETRIC_REPRESENTATION_ITEM ( )  RATIONAL_B_SPLINE_CURVE ( ( 0.9330127018922194093, 0.9330127018922194093, 1.000000000000000000, 0.8660254037844387076, 1.000000000000000000, 0.8660254037844387076, 1.000000000000000000, 0.9330127018922194093, 0.9330127018922194093 ) ) 
 REPRESENTATION_ITEM ( '' )  );
#6464 = CARTESIAN_POINT ( 'NONE',  ( -5.000000000000000000, 4.916666666666666075, -2.886751345948128211 ) ) ;
#6465 = CARTESIAN_POINT ( 'NONE',  ( 3.152801135295367541, -162.3125000013656063, -3.152801135295367541 ) ) ;
#6466 = CARTESIAN_POINT ( 'NONE',  ( -4.999999999999998224, 22.08333333333333215, 2.886751345948131764 ) ) ;
#6467 = CARTESIAN_POINT ( 'NONE',  ( 4.458734124999999437, -56.81249999863440081, -5.460374474430324690E-16 ) ) ;
#6468 = CARTESIAN_POINT ( 'NONE',  ( -2.499999999999996447, -95.70833333060213022, 4.330127018922195425 ) ) ;
#6469 = CARTESIAN_POINT ( 'NONE',  ( 5.000000000000000888, -38.58333333333332149, 2.886751345948126879 ) ) ;
#6470 = CARTESIAN_POINT ( 'NONE',  ( -5.000000000000000000, -80.08333333333332860, -2.886751345948128211 ) ) ;
#6471 = DIRECTION ( 'NONE',  ( 0.000000000000000000, 0.000000000000000000, 1.000000000000000000 ) ) ;
#6472 = CARTESIAN_POINT ( 'NONE',  ( -2.229367062499996610, -37.14583333196773651, 3.861377020970582219 ) ) ;
#6473 = DIRECTION ( 'NONE',  ( -0.000000000000000000, 1.000000000000000000, -0.000000000000000000 ) ) ;
#6474 = CARTESIAN_POINT ( 'NONE',  ( 1.060575238724906964E-15, -41.74999999999999289, 5.773502691896257311 ) ) ;
#6475 = DIRECTION ( 'NONE',  ( -0.000000000000000000, 1.000000000000000000, -0.000000000000000000 ) ) ;
#6476 = DIRECTION ( 'NONE',  ( -0.000000000000000000, 1.000000000000000000, -0.000000000000000000 ) ) ;
#6477 = ORIENTED_EDGE ( 'NONE', *, *, #36714, .F. ) ;
#6478 = CARTESIAN_POINT ( 'NONE',  ( -2.229367062500000163, -104.4791666653010651, -3.861377020970580443 ) ) ;
#6479 = CARTESIAN_POINT ( 'NONE',  ( -2.229367062499996610, -2.395833331967737845, 3.861377020970582219 ) ) ;
#6480 = FACE_OUTER_BOUND ( 'NONE', #27499, .T. ) ;
#6481 = CARTESIAN_POINT ( 'NONE',  ( 1.060575238724906964E-15, -7.749999999999999112, 5.773502691896257311 ) ) ;
#6482 = CARTESIAN_POINT ( 'NONE',  ( 2.229367062500001939, -71.97916666530107932, 3.861377020970579999 ) ) ;
#6483 = CARTESIAN_POINT ( 'NONE',  ( 2.500000000000002220, -22.54166666393548013, 4.330127018922192761 ) ) ;
#6484 = CARTESIAN_POINT ( 'NONE',  ( -2.499999999999996447, -7.708333330602144429, 4.330127018922195425 ) ) ;
#6486 = ORIENTED_EDGE ( 'NONE', *, *, #58534, .T. ) ;
#6485 = CARTESIAN_POINT ( 'NONE',  ( 4.458734124999998549, -39.72916666530107932, -2.574251347313721627 ) ) ;
#6487 = CARTESIAN_POINT ( 'NONE',  ( 5.000000000000000888, -22.45833333060214443, 2.886751345948126879 ) ) ;
#6489 = ORIENTED_EDGE ( 'NONE', *, *, #19267, .T. ) ;
#6488 = CARTESIAN_POINT ( 'NONE',  ( 9.457646018065525792E-16, 11.68750000136559564, 5.148502694627439702 ) ) ;
#6490 = DIRECTION ( 'NONE',  ( -0.000000000000000000, 1.000000000000000000, -0.000000000000000000 ) ) ;
#6491 = CARTESIAN_POINT ( 'NONE',  ( -4.999999999999999112, -47.91666666666667140, 2.886751345948131764 ) ) ;
#6492 = CARTESIAN_POINT ( 'NONE',  ( 4.458734124999999437, -29.06249999863440436, -5.460374474430324690E-16 ) ) ;
#6493 = DIRECTION ( 'NONE',  ( -0.000000000000000000, 1.000000000000000000, -0.000000000000000000 ) ) ;
#6494 = CARTESIAN_POINT ( 'NONE',  ( -4.458734124999998549, -73.22916666530106511, 2.574251347313722516 ) ) ;
#6495 = CARTESIAN_POINT ( 'NONE',  ( 4.458734124999999437, -140.6875000013656063, 0.000000000000000000 ) ) ;
#6496 = CARTESIAN_POINT ( 'NONE',  ( -2.229367062499996610, -86.14583333196773651, 3.861377020970582219 ) ) ;
#6497 = CARTESIAN_POINT ( 'NONE',  ( -59.44456063193725015, -135.8125000013656063, -0.3552334253322034230 ) ) ;
#6498 = CARTESIAN_POINT ( 'NONE',  ( 2.229367062500001939, -37.22916666530107221, 3.861377020970579999 ) ) ;
#6499 = ORIENTED_EDGE ( 'NONE', *, *, #23952, .T. ) ;
#6500 = CARTESIAN_POINT ( 'NONE',  ( 2.499999999999998668, -70.20833333060214443, -4.330127018922193649 ) ) ;
#6501 = ORIENTED_EDGE ( 'NONE', *, *, #15413, .F. ) ;
#6502 = CARTESIAN_POINT ( 'NONE',  ( -2.229367062499996610, -79.39583333196773651, 3.861377020970582219 ) ) ;
#6503 = CARTESIAN_POINT ( 'NONE',  ( -51.25142410359330114, -135.0000000000000568, -2.431704782982593294 ) ) ;
#6504 = ORIENTED_EDGE ( 'NONE', *, *, #27461, .T. ) ;
#6505 = DIRECTION ( 'NONE',  ( -0.000000000000000000, 1.000000000000000000, -0.000000000000000000 ) ) ;
#6506 = DIRECTION ( 'NONE',  ( 0.000000000000000000, 1.000000000000000000, 0.000000000000000000 ) ) ;
#6507 = CARTESIAN_POINT ( 'NONE',  ( 4.458734124999999437, -62.06249999863440792, -5.460374474430324690E-16 ) ) ;
#6508 = CARTESIAN_POINT ( 'NONE',  ( 9.457646018065525792E-16, -5.312499998634402587, 5.148502694627439702 ) ) ;
#6509 = ORIENTED_EDGE ( 'NONE', *, *, #18968, .F. ) ;
#6510 = DIRECTION ( 'NONE',  ( 0.000000000000000000, -1.000000000000000000, 0.000000000000000000 ) ) ;
#6511 = DIRECTION ( 'NONE',  ( -0.000000000000000000, 1.000000000000000000, -0.000000000000000000 ) ) ;
#6512 = ORIENTED_EDGE ( 'NONE', *, *, #41590, .T. ) ;
#6513 = CARTESIAN_POINT ( 'NONE',  ( 2.499999999999998668, -91.33333333333334281, -4.330127018922193649 ) ) ;
#6514 = CARTESIAN_POINT ( 'NONE',  ( 2.229367062499998831, 6.354166668032262599, -3.861377020970580887 ) ) ;
#6515 = CARTESIAN_POINT ( 'NONE',  ( -2.500000000000000444, -76.16666666666665719, -4.330127018922193649 ) ) ;
#6516 = CARTESIAN_POINT ( 'NONE',  ( -1.846868145590734756, -159.1250000013656063, -4.458734124999999437 ) ) ;
#6517 = DIRECTION ( 'NONE',  ( 0.000000000000000000, 0.000000000000000000, 1.000000000000000000 ) ) ;
#6518 = ORIENTED_EDGE ( 'NONE', *, *, #58551, .F. ) ;
#6519 = CARTESIAN_POINT ( 'NONE',  ( -4.458734124999997661, -83.22916666530106511, 2.574251347313722516 ) ) ;
#6520 = CARTESIAN_POINT ( 'NONE',  ( -9.184850993605147944E-16, -164.3750000027311842, 5.000000000000000000 ) ) ;
#6521 = CARTESIAN_POINT ( 'NONE',  ( 4.458734124999999437, -3.812499998634408360, -5.460374474430324690E-16 ) ) ;
#6522 = CARTESIAN_POINT ( 'NONE',  ( -4.764381983412779477E-15, 25.37500000273118062, 5.000000000000000000 ) ) ;
#6523 = CARTESIAN_POINT ( 'NONE',  ( -2.499999999999996447, -67.83333333333332860, 4.330127018922195425 ) ) ;
#6524 = CARTESIAN_POINT ( 'NONE',  ( -2.499999999999996447, -30.70833333060214443, 4.330127018922195425 ) ) ;
#6525 = CARTESIAN_POINT ( 'NONE',  ( 2.229367062500001939, 24.02083333469892779, 3.861377020970579999 ) ) ;
#6526 = CARTESIAN_POINT ( 'NONE',  ( 1.339745962155612702, -104.2946581987385315, -5.000000000000000000 ) ) ;
#6527 = CARTESIAN_POINT ( 'NONE',  ( 2.229367062499998831, -53.64583333196773651, -3.861377020970580887 ) ) ;
#6528 = CARTESIAN_POINT ( 'NONE',  ( -2.229367062499996610, -36.39583333196773651, 3.861377020970582219 ) ) ;
#6529 = CARTESIAN_POINT ( 'NONE',  ( -3.152548672688508926E-16, 3.187500001365594304, -5.148502694627439702 ) ) ;
#6530 = CARTESIAN_POINT ( 'NONE',  ( -4.999999999999998224, -17.91666666666666430, 2.886751345948131764 ) ) ;
#6531 = CARTESIAN_POINT ( 'NONE',  ( -5.000000000000000000, 22.00000000000000000, 0.000000000000000000 ) ) ;
#6532 = CARTESIAN_POINT ( 'NONE',  ( -5.000000000000000888, -146.5625000027311842, 2.071067811865474617 ) ) ;
#6533 = CARTESIAN_POINT ( 'NONE',  ( 5.000000000000000000, -33.29166666393547303, -2.886751345948130876 ) ) ;
#6534 = CARTESIAN_POINT ( 'NONE',  ( 2.229367062499998831, -43.64583333196773651, -3.861377020970580887 ) ) ;
#6535 = CARTESIAN_POINT ( 'NONE',  ( 5.000000000000000000, -76.29166666393547303, -2.886751345948129988 ) ) ;
#6536 = CARTESIAN_POINT ( 'NONE',  ( -52.80376928212989185, -141.1250000013655779, -4.297418129356379346 ) ) ;
#6537 = VECTOR ( 'NONE', #21294, 1000.000000000000000 ) ;
#6538 = DIRECTION ( 'NONE',  ( 0.000000000000000000, 0.000000000000000000, 1.000000000000000000 ) ) ;
#6539 = CARTESIAN_POINT ( 'NONE',  ( 7.922281120364393914, -4.573931137438282057, -8.047472243342932430 ) ) ;
#6540 = CARTESIAN_POINT ( 'NONE',  ( 2.229367062499998831, -80.89583333196773651, -3.861377020970580887 ) ) ;
#6541 = CARTESIAN_POINT ( 'NONE',  ( -4.458734125000000326, -161.1250000013656063, 1.846868145590734089 ) ) ;
#6542 = CARTESIAN_POINT ( 'NONE',  ( 1.060575238724906964E-15, -27.74999999999999645, 5.773502691896257311 ) ) ;
#6543 = CARTESIAN_POINT ( 'NONE',  ( 1.975475456537005874E-15, -26.74999999999999645, 5.000000000000000000 ) ) ;
#6544 = VERTEX_POINT ( 'NONE', #10149 ) ;
#6545 = CARTESIAN_POINT ( 'NONE',  ( 2.229367062499998831, 23.10416666803225993, -3.861377020970580887 ) ) ;
#6546 = ORIENTED_EDGE ( 'NONE', *, *, #54313, .F. ) ;
#6547 = CARTESIAN_POINT ( 'NONE',  ( 4.458734124999998549, 13.02083333469892779, -2.574251347313721627 ) ) ;
#6548 = CARTESIAN_POINT ( 'NONE',  ( 5.000000000000000000, 16.62500000273118417, -6.123233995736766282E-16 ) ) ;
#6549 = CARTESIAN_POINT ( 'NONE',  ( -2.480964764533239819E-13, -60.62499999726880873, 5.000000000000000000 ) ) ;
#6550 = CARTESIAN_POINT ( 'NONE',  ( -4.999999999999999112, 14.08333333333333393, 2.886751345948131764 ) ) ;
#6551 = CARTESIAN_POINT ( 'NONE',  ( -4.458734124999999437, -58.31249999863440081, 0.000000000000000000 ) ) ;
#6552 = CARTESIAN_POINT ( 'NONE',  ( -4.458734124999999437, -9.395833331967736513, -2.574251347313719407 ) ) ;
#6553 =( BOUNDED_CURVE ( )  B_SPLINE_CURVE ( 2, ( #18693, #4848, #23843, #19318, #3603, #62466, #14489, #23210, #57947 ),
 .UNSPECIFIED., .F., .F. ) 
 B_SPLINE_CURVE_WITH_KNOTS ( ( 3, 2, 2, 2, 3 ),
 ( 0.7770833333333333481, 0.7777777777777777901, 0.7791666666666666741, 0.7805555555555555580, 0.7812500000000000000 ),
 .UNSPECIFIED. ) 
 CURVE ( )  GEOMETRIC_REPRESENTATION_ITEM ( )  RATIONAL_B_SPLINE_CURVE ( ( 0.9330127018922194093, 0.9330127018922194093, 1.000000000000000000, 0.8660254037844387076, 1.000000000000000000, 0.8660254037844387076, 1.000000000000000000, 0.9330127018922194093, 0.9330127018922194093 ) ) 
 REPRESENTATION_ITEM ( '' )  );
#6554 = CARTESIAN_POINT ( 'NONE',  ( -50.70258187064364108, -136.3750000013656063, 2.196230717870141014 ) ) ;
#6555 = CARTESIAN_POINT ( 'NONE',  ( 1.975475456537005874E-15, -109.7499999999999858, 5.000000000000000000 ) ) ;
#6556 = CYLINDRICAL_SURFACE ( 'NONE', #11753, 5.000000000000000000 ) ;
#6557 = CARTESIAN_POINT ( 'NONE',  ( 0.000000000000000000, -170.0000000000000000, 5.000000000000000000 ) ) ;
#6558 = CARTESIAN_POINT ( 'NONE',  ( -2.500000000000000444, -36.16666666666666430, -4.330127018922193649 ) ) ;
#6559 = CARTESIAN_POINT ( 'NONE',  ( 0.000000000000000000, -170.0000000000000000, 0.000000000000000000 ) ) ;
#6561 = CARTESIAN_POINT ( 'NONE',  ( 4.458734125000001214, -13.14583333196774184, 2.574251347313718519 ) ) ;
#6560 = CARTESIAN_POINT ( 'NONE',  ( -4.999999999999998224, -58.91666666666665009, 2.886751345948131764 ) ) ;
#6562 = CARTESIAN_POINT ( 'NONE',  ( 2.499999999999998668, 17.79166666939785557, -4.330127018922193649 ) ) ;
#6563 = CARTESIAN_POINT ( 'NONE',  ( -2.229367062500000163, -58.47916666530106511, -3.861377020970580443 ) ) ;
#6564 = CARTESIAN_POINT ( 'NONE',  ( -8.190561711645485556E-16, -152.9375000013655779, 4.458734124999999437 ) ) ;
#6565 = CARTESIAN_POINT ( 'NONE',  ( -4.458734124999999437, -67.31249999863440792, 0.000000000000000000 ) ) ;
#6566 = CARTESIAN_POINT ( 'NONE',  ( -56.48576386720575471, -149.0000000013656063, -4.591703134518078322 ) ) ;
#6567 = CARTESIAN_POINT ( 'NONE',  ( -5.000000000000000000, -57.95833333060215153, -2.886751345948128211 ) ) ;
#6568 = VECTOR ( 'NONE', #5169, 1000.000000000000000 ) ;
#6569 = ORIENTED_EDGE ( 'NONE', *, *, #40160, .T. ) ;
#6570 = CARTESIAN_POINT ( 'NONE',  ( -4.999999999999998224, 25.20833333606451987, 2.886751345948131764 ) ) ;
#6571 = VERTEX_POINT ( 'NONE', #40047 ) ;
#6573 = CARTESIAN_POINT ( 'NONE',  ( 5.000000000000000000, -103.5000000000000142, -6.123233995736766282E-16 ) ) ;
#6572 = CARTESIAN_POINT ( 'NONE',  ( -55.39835681537999790, -149.0000000027312126, 4.984105922594378235 ) ) ;
#6574 = CARTESIAN_POINT ( 'NONE',  ( -4.458734125000001214, -151.8750000013655779, 1.846868145590734089 ) ) ;
#6575 = VERTEX_POINT ( 'NONE', #29755 ) ;
#6576 = CARTESIAN_POINT ( 'NONE',  ( 0.000000000000000000, -170.0000000000000000, 0.000000000000000000 ) ) ;
#6577 = CARTESIAN_POINT ( 'NONE',  ( -60.14911071818854538, -128.0625000000000284, 1.666127454062681368 ) ) ;
#6578 = CARTESIAN_POINT ( 'NONE',  ( 0.000000000000000000, -120.0000000000000000, 0.000000000000000000 ) ) ;
#6579 = CARTESIAN_POINT ( 'NONE',  ( -3.152548672688508926E-16, -49.81249999863440081, -5.148502694627439702 ) ) ;
#6580 = ORIENTED_EDGE ( 'NONE', *, *, #62460, .T. ) ;
#6581 = CARTESIAN_POINT ( 'NONE',  ( 75.00000000000002842, 15.00000000000000000, 5.000000000000000000 ) ) ;
#6582 = CARTESIAN_POINT ( 'NONE',  ( -4.458734124999999437, 14.60416666803226171, -2.574251347313719407 ) ) ;
#6583 = CARTESIAN_POINT ( 'NONE',  ( 4.458734124999998549, 22.27083333469893134, -2.574251347313721627 ) ) ;
#6584 = CARTESIAN_POINT ( 'NONE',  ( -57.19623071787017210, -153.3750000013656347, 4.297418129356382899 ) ) ;
#6585 = CARTESIAN_POINT ( 'NONE',  ( -1.339745962155613812, -24.08034179853029499, -5.000000000000000000 ) ) ;
#6586 = CARTESIAN_POINT ( 'NONE',  ( 5.275681513340003914E-14, 10.74999999999999645, -5.000000000000000000 ) ) ;
#6587 = EDGE_LOOP ( 'NONE', ( #2879, #11073, #18018, #13981 ) ) ;
#6588 = CARTESIAN_POINT ( 'NONE',  ( -4.458734124999997661, -65.22916666530106511, 2.574251347313722516 ) ) ;
#6589 = CARTESIAN_POINT ( 'NONE',  ( -6.972266317189433020E-16, -19.12499999726880873, -5.000000000000000000 ) ) ;
#6590 = CARTESIAN_POINT ( 'NONE',  ( 4.458734124999999437, 15.18750000136559564, -5.460374474430324690E-16 ) ) ;
#6591 = CARTESIAN_POINT ( 'NONE',  ( 5.000000000000000000, -63.41666666666666430, -2.886751345948130876 ) ) ;
#6592 = CARTESIAN_POINT ( 'NONE',  ( -3.535533905932737309, -157.6250000000000284, -3.535533905932738197 ) ) ;
#6593 = CARTESIAN_POINT ( 'NONE',  ( -2.229367062500000163, -52.72916666530107221, -3.861377020970580443 ) ) ;
#6594 = CARTESIAN_POINT ( 'NONE',  ( 5.000000000000000888, -16.45833333060214443, 2.886751345948126879 ) ) ;
#6595 = CARTESIAN_POINT ( 'NONE',  ( 0.000000000000000000, -120.0000000000000000, 0.000000000000000000 ) ) ;
#6596 = CARTESIAN_POINT ( 'NONE',  ( -2.500000000000000444, -20.04166666393548013, -4.330127018922193649 ) ) ;
#6597 = CARTESIAN_POINT ( 'NONE',  ( -51.75738570946856498, -138.7500000000000000, 3.805975901505576964 ) ) ;
#6598 = CARTESIAN_POINT ( 'NONE',  ( 1.339745962155612702, -64.16965819600731891, -5.000000000000000000 ) ) ;
#6599 = CARTESIAN_POINT ( 'NONE',  ( -4.458734124999997661, -15.47916666530107399, 2.574251347313722516 ) ) ;
#6600 =( BOUNDED_CURVE ( )  B_SPLINE_CURVE ( 2, ( #49563, #25117, #44728, #20944, #2291, #21578, #46649, #36051, #31214 ),
 .UNSPECIFIED., .F., .F. ) 
 B_SPLINE_CURVE_WITH_KNOTS ( ( 3, 2, 2, 2, 3 ),
 ( 0.9812499999999999556, 0.9819444444444443976, 0.9833333333333332815, 0.9847222222222222765, 0.9854166666666667185 ),
 .UNSPECIFIED. ) 
 CURVE ( )  GEOMETRIC_REPRESENTATION_ITEM ( )  RATIONAL_B_SPLINE_CURVE ( ( 0.9330127018922194093, 0.9330127018922194093, 1.000000000000000000, 0.8660254037844387076, 1.000000000000000000, 0.8660254037844387076, 1.000000000000000000, 0.9330127018922194093, 0.9330127018922194093 ) ) 
 REPRESENTATION_ITEM ( '' )  );
#6601 = VERTEX_POINT ( 'NONE', #34265 ) ;
#6602 = CARTESIAN_POINT ( 'NONE',  ( -1.339745962155610925, -60.79465819873851729, 5.000000000000000000 ) ) ;
#6603 = CARTESIAN_POINT ( 'NONE',  ( 4.458734124999999437, -105.8124999986344221, -5.460374474430324690E-16 ) ) ;
#6604 = CARTESIAN_POINT ( 'NONE',  ( 5.000000000000000000, -158.1250000027311842, 0.000000000000000000 ) ) ;
#6605 = ORIENTED_EDGE ( 'NONE', *, *, #9441, .T. ) ;
#6606 = CARTESIAN_POINT ( 'NONE',  ( -2.229367062499996610, -103.3958333319677365, 3.861377020970582219 ) ) ;
#6607 = ADVANCED_FACE ( 'NONE', ( #199 ), #9510, .T. ) ;
#6608 = CARTESIAN_POINT ( 'NONE',  ( 4.458734125000001214, -28.89583333196774007, 2.574251347313718519 ) ) ;
#6609 = CARTESIAN_POINT ( 'NONE',  ( -2.500000000000000444, -62.04166666393547303, -4.330127018922193649 ) ) ;
#6610 = CARTESIAN_POINT ( 'NONE',  ( -59.59170313451811296, -153.7500000013656063, 1.485763867205729394 ) ) ;
#6611 = CARTESIAN_POINT ( 'NONE',  ( -54.64476657466781973, -140.8125000013656063, -4.444560631937228834 ) ) ;
#6612 = CARTESIAN_POINT ( 'NONE',  ( -4.458734124999997661, -24.22916666530107577, 2.574251347313722516 ) ) ;
#6613 = CARTESIAN_POINT ( 'NONE',  ( 2.229367062500001939, -65.22916666530106511, 3.861377020970579999 ) ) ;
#6614 = CARTESIAN_POINT ( 'NONE',  ( -58.24261429053147765, -137.2500000000000000, -3.805975901505573855 ) ) ;
#6615 = CARTESIAN_POINT ( 'NONE',  ( 9.457646018065525792E-16, -17.06249999863440792, 5.148502694627439702 ) ) ;
#6616 = DIRECTION ( 'NONE',  ( 0.000000000000000000, 0.000000000000000000, 1.000000000000000000 ) ) ;
#6617 = CARTESIAN_POINT ( 'NONE',  ( 2.071067811865475505, -150.8125000000000000, -5.000000000000000888 ) ) ;
#6618 = CARTESIAN_POINT ( 'NONE',  ( -3.535250795749689387E-16, -12.24999999999999645, -5.773502691896257311 ) ) ;
#6619 = CARTESIAN_POINT ( 'NONE',  ( 3.152801135295367541, -152.3125000013655779, -3.152801135295367541 ) ) ;
#6620 = ORIENTED_EDGE ( 'NONE', *, *, #63624, .F. ) ;
#6621 = CARTESIAN_POINT ( 'NONE',  ( -4.458734124999997661, -46.47916666530106511, 2.574251347313722516 ) ) ;
#6622 = CARTESIAN_POINT ( 'NONE',  ( 2.500000000000002220, 21.45833333606451987, 4.330127018922192761 ) ) ;
#6623 = CYLINDRICAL_SURFACE ( 'NONE', #62727, 5.000000000000000000 ) ;
#6624 = CARTESIAN_POINT ( 'NONE',  ( 5.000000000000000888, 27.41666666666666785, 2.886751345948126879 ) ) ;
#6625 = VECTOR ( 'NONE', #29553, 1000.000000000000000 ) ;
#6626 = CARTESIAN_POINT ( 'NONE',  ( -3.152548672688508926E-16, 4.437500001365595637, -5.148502694627439702 ) ) ;
#6627 = EDGE_CURVE ( 'NONE', #61600, #26190, #59691, .T. ) ;
#6628 = CARTESIAN_POINT ( 'NONE',  ( -9.184850993605147944E-16, -142.2500000000000284, 5.000000000000000000 ) ) ;
#6629 = EDGE_CURVE ( 'NONE', #4186, #12980, #4904, .T. ) ;
#6630 = CARTESIAN_POINT ( 'NONE',  ( 1.975475456537005874E-15, -11.62499999726881406, 5.000000000000000000 ) ) ;
#6631 = DIRECTION ( 'NONE',  ( 0.000000000000000000, 1.000000000000000000, 0.000000000000000000 ) ) ;
#6632 = CARTESIAN_POINT ( 'NONE',  ( -2.229367062499996610, 17.60416666803225993, 3.861377020970582219 ) ) ;
#6633 = CARTESIAN_POINT ( 'NONE',  ( -5.000000000000000000, -80.00000000000000000, 0.000000000000000000 ) ) ;
#6634 = CARTESIAN_POINT ( 'NONE',  ( 5.000000000000000000, 4.708333336064518093, -2.886751345948129988 ) ) ;
#6635 = ORIENTED_EDGE ( 'NONE', *, *, #1911, .F. ) ;
#6636 = CARTESIAN_POINT ( 'NONE',  ( 5.000000000000000000, -162.1250000027311842, 0.000000000000000000 ) ) ;
#6637 = ORIENTED_EDGE ( 'NONE', *, *, #2863, .T. ) ;
#6638 = CARTESIAN_POINT ( 'NONE',  ( 2.788906526875773208E-15, 27.87500000273118417, -5.000000000000000000 ) ) ;
#6639 = CARTESIAN_POINT ( 'NONE',  ( -4.458734124999999437, -43.31249999863440081, 0.000000000000000000 ) ) ;
#6640 = CARTESIAN_POINT ( 'NONE',  ( -1.846868145590734756, -162.3750000013655779, -4.458734125000000326 ) ) ;
#6641 = EDGE_CURVE ( 'NONE', #51343, #59835, #22586, .T. ) ;
#6642 = CARTESIAN_POINT ( 'NONE',  ( -5.000000000000000000, -36.95833333060213732, -2.886751345948128211 ) ) ;
#6643 = ORIENTED_EDGE ( 'NONE', *, *, #9778, .T. ) ;
#6644 = CARTESIAN_POINT ( 'NONE',  ( -4.458734124999999437, -18.39583333196774007, -2.574251347313719407 ) ) ;
#6645 = ORIENTED_EDGE ( 'NONE', *, *, #33048, .F. ) ;
#6646 = CARTESIAN_POINT ( 'NONE',  ( -2.499999999999996447, -88.83333333333332860, 4.330127018922195425 ) ) ;
#6647 = CARTESIAN_POINT ( 'NONE',  ( -4.458734125000001214, -162.8750000013655779, 1.846868145590734089 ) ) ;
#6648 =( BOUNDED_CURVE ( )  B_SPLINE_CURVE ( 2, ( #13559, #41541, #47338, #41866, #61193, #61513, #17442, #37060, #22590 ),
 .UNSPECIFIED., .F., .F. ) 
 B_SPLINE_CURVE_WITH_KNOTS ( ( 3, 2, 2, 2, 3 ),
 ( 0.7696428571428571841, 0.7702380952380952772, 0.7714285714285714635, 0.7726190476190476497, 0.7732142857142857428 ),
 .UNSPECIFIED. ) 
 CURVE ( )  GEOMETRIC_REPRESENTATION_ITEM ( )  RATIONAL_B_SPLINE_CURVE ( ( 0.9330127018922194093, 0.9330127018922194093, 1.000000000000000000, 0.8660254037844387076, 1.000000000000000000, 0.8660254037844387076, 1.000000000000000000, 0.9330127018922194093, 0.9330127018922194093 ) ) 
 REPRESENTATION_ITEM ( '' )  );
#6649 = CARTESIAN_POINT ( 'NONE',  ( 5.000000000000000000, -87.37499999726880162, -6.123233995736766282E-16 ) ) ;
#6651 = VERTEX_POINT ( 'NONE', #48034 ) ;
#6650 = CARTESIAN_POINT ( 'NONE',  ( 1.975475456537005874E-15, -75.74999999999998579, 5.000000000000000000 ) ) ;
#6652 = CARTESIAN_POINT ( 'NONE',  ( -57.46284108482265651, -142.9375000000000000, 4.819101127000239515 ) ) ;
#6653 = CARTESIAN_POINT ( 'NONE',  ( -3.152548672688508926E-16, -32.81249999863440792, -5.148502694627439702 ) ) ;
#6654 = CARTESIAN_POINT ( 'NONE',  ( 1.339745962155615144, -29.70534180126147561, 4.999999999999999112 ) ) ;
#6655 = ORIENTED_EDGE ( 'NONE', *, *, #2082, .F. ) ;
#6656 = ADVANCED_FACE ( 'NONE', ( #39635 ), #33873, .T. ) ;
#6657 = CARTESIAN_POINT ( 'NONE',  ( 4.458734124999998549, -75.72916666530106511, -2.574251347313721627 ) ) ;
#6658 = CARTESIAN_POINT ( 'NONE',  ( -4.458734124999999437, -110.5624999986343937, 0.000000000000000000 ) ) ;
#6659 = CARTESIAN_POINT ( 'NONE',  ( 5.000000000000000000, -18.50000000000000355, -6.123233995736766282E-16 ) ) ;
#6660 = ORIENTED_EDGE ( 'NONE', *, *, #32321, .T. ) ;
#6661 = CARTESIAN_POINT ( 'NONE',  ( -5.000000000000000888, -161.5625000000000284, -2.071067811865475949 ) ) ;
#6662 = CARTESIAN_POINT ( 'NONE',  ( -50.40829686548195099, -142.2500000013656063, -1.485763867205728284 ) ) ;
#6663 = CARTESIAN_POINT ( 'NONE',  ( 4.458734124999998549, -82.97916666530107932, -2.574251347313721627 ) ) ;
#6664 = CARTESIAN_POINT ( 'NONE',  ( -59.98410592259440222, -136.2500000027312126, -0.3983568153799752487 ) ) ;
#6665 = CARTESIAN_POINT ( 'NONE',  ( -3.152548672688508926E-16, -45.56249999863439371, -5.148502694627439702 ) ) ;
#6666 = CARTESIAN_POINT ( 'NONE',  ( -4.458734125000000326, -144.1250000013655779, 1.846868145590734089 ) ) ;
#6667 = CARTESIAN_POINT ( 'NONE',  ( -2.500000000000000444, 5.958333336064519870, -4.330127018922193649 ) ) ;
#6668 = CARTESIAN_POINT ( 'NONE',  ( 9.457646018065525792E-16, -48.06249999863440792, 5.148502694627439702 ) ) ;
#6669 = CARTESIAN_POINT ( 'NONE',  ( 9.457646018065525792E-16, -45.06249999863440081, 5.148502694627439702 ) ) ;
#6670 = CARTESIAN_POINT ( 'NONE',  ( 4.458734124999998549, 29.27083333469892423, -2.574251347313721627 ) ) ;
#6671 = CARTESIAN_POINT ( 'NONE',  ( -4.999999999999999112, -103.9166666666666430, 2.886751345948131764 ) ) ;
#6672 = VECTOR ( 'NONE', #33074, 1000.000000000000000 ) ;
#6673 = DIRECTION ( 'NONE',  ( 0.000000000000000000, 0.000000000000000000, 1.000000000000000000 ) ) ;
#6674 = CARTESIAN_POINT ( 'NONE',  ( 2.229367062500001939, -37.22916666530107221, 3.861377020970579999 ) ) ;
#6675 = CARTESIAN_POINT ( 'NONE',  ( 5.000000000000000000, -0.2916666639354824619, -2.886751345948129988 ) ) ;
#6676 = LINE ( 'NONE', #34663, #50977 ) ;
#6677 = CARTESIAN_POINT ( 'NONE',  ( -52.10840900171896806, -127.1875000013656063, 3.393966926194110556 ) ) ;
#6678 = CARTESIAN_POINT ( 'NONE',  ( -4.458734124999999437, -80.64583333196773651, -2.574251347313719407 ) ) ;
#6679 = CARTESIAN_POINT ( 'NONE',  ( -57.46284108482265651, -142.0625000027312126, 4.819101127000238627 ) ) ;
#6680 = CARTESIAN_POINT ( 'NONE',  ( -3.152548672688508926E-16, -95.56249999863439371, -5.148502694627439702 ) ) ;
#6681 = CARTESIAN_POINT ( 'NONE',  ( 1.339745962155612702, -76.29465819873853150, -5.000000000000000000 ) ) ;
#6682 = CARTESIAN_POINT ( 'NONE',  ( 2.229367062499998831, 2.104166668032262599, -3.861377020970580887 ) ) ;
#6683 = ORIENTED_EDGE ( 'NONE', *, *, #39433, .F. ) ;
#6684 = CARTESIAN_POINT ( 'NONE',  ( 1.339745962155612702, 24.83034180399266333, -5.000000000000000000 ) ) ;
#6685 = CARTESIAN_POINT ( 'NONE',  ( -1.339745962155610925, -59.79465819873851729, 5.000000000000000000 ) ) ;
#6686 = CARTESIAN_POINT ( 'NONE',  ( -3.152548672688508926E-16, -87.56249999863440792, -5.148502694627439702 ) ) ;
#6687 = CARTESIAN_POINT ( 'NONE',  ( 5.000000000000000000, -168.1875000027311842, 2.071067811865478614 ) ) ;
#6688 = CARTESIAN_POINT ( 'NONE',  ( -2.229367062500000163, -87.72916666530107932, -3.861377020970580443 ) ) ;
#6689 = EDGE_CURVE ( 'NONE', #23665, #34156, #18438, .T. ) ;
#6690 = CARTESIAN_POINT ( 'NONE',  ( 2.229367062499998831, 13.10416666803226171, -3.861377020970580887 ) ) ;
#6691 = DIRECTION ( 'NONE',  ( -0.000000000000000000, 1.000000000000000000, -0.000000000000000000 ) ) ;
#6692 = CARTESIAN_POINT ( 'NONE',  ( -53.51423613279429503, -137.2500000013656063, 4.591703134518082763 ) ) ;
#6693 = EDGE_CURVE ( 'NONE', #35135, #9375, #28418, .T. ) ;
#6694 = CARTESIAN_POINT ( 'NONE',  ( -3.152548672688508926E-16, -6.562499998634404363, -5.148502694627439702 ) ) ;
#6695 = CARTESIAN_POINT ( 'NONE',  ( 4.458734124999998549, 16.02083333469892423, -2.574251347313721627 ) ) ;
#6696 = CARTESIAN_POINT ( 'NONE',  ( 4.458734124999998549, -45.97916666530106511, -2.574251347313721627 ) ) ;
#6697 = CARTESIAN_POINT ( 'NONE',  ( -9.184850993605147944E-16, -163.2500000000000000, 5.000000000000000000 ) ) ;
#6698 = CARTESIAN_POINT ( 'NONE',  ( -4.458734124999998549, -86.22916666530106511, 2.574251347313722516 ) ) ;
#6699 = CARTESIAN_POINT ( 'NONE',  ( -3.152548672688508926E-16, -4.562499998634401699, -5.148502694627439702 ) ) ;
#6700 = DIRECTION ( 'NONE',  ( -0.6485228581062915110, 0.000000000000000000, -0.7611951803011149931 ) ) ;
#6701 = EDGE_LOOP ( 'NONE', ( #51330, #53753, #24980, #13443 ) ) ;
#6702 = CARTESIAN_POINT ( 'NONE',  ( -2.229367062500000163, -32.72916666530106511, -3.861377020970580443 ) ) ;
#6703 = CARTESIAN_POINT ( 'NONE',  ( -57.89159099828107458, -130.9375000013656063, -3.393966926194107447 ) ) ;
#6704 = CARTESIAN_POINT ( 'NONE',  ( -4.458734124999998549, -76.22916666530107932, 2.574251347313722516 ) ) ;
#6705 = CARTESIAN_POINT ( 'NONE',  ( 2.229367062499998831, 27.10416666803225993, -3.861377020970580887 ) ) ;
#6706 = CARTESIAN_POINT ( 'NONE',  ( -2.229367062500000163, 19.52083333469893134, -3.861377020970580443 ) ) ;
#6707 = DIRECTION ( 'NONE',  ( -0.000000000000000000, 1.000000000000000000, -0.000000000000000000 ) ) ;
#6708 = EDGE_CURVE ( 'NONE', #12164, #37331, #57892, .T. ) ;
#6709 = CARTESIAN_POINT ( 'NONE',  ( 1.339745962155615144, -28.70534180126147561, 4.999999999999999112 ) ) ;
#6710 = CARTESIAN_POINT ( 'NONE',  ( 4.458734125000000326, -80.14583333196773651, 2.574251347313718519 ) ) ;
#6711 = CARTESIAN_POINT ( 'NONE',  ( -2.500000000000000444, -67.16666666666667140, -4.330127018922193649 ) ) ;
#6712 = CARTESIAN_POINT ( 'NONE',  ( 1.975475456537005874E-15, -103.6249999972688016, 5.000000000000000000 ) ) ;
#6713 = CARTESIAN_POINT ( 'NONE',  ( 2.500000000000002220, 25.45833333606451987, 4.330127018922192761 ) ) ;
#6714 = ORIENTED_EDGE ( 'NONE', *, *, #31089, .F. ) ;
#6715 = CARTESIAN_POINT ( 'NONE',  ( -1.339745962155610925, -72.66965819600733312, 5.000000000000000000 ) ) ;
#6717 = CARTESIAN_POINT ( 'NONE',  ( 2.500000000000002220, -25.66666666666666430, 4.330127018922192761 ) ) ;
#6716 = CARTESIAN_POINT ( 'NONE',  ( -2.499999999999996447, -106.7083333306021444, 4.330127018922195425 ) ) ;
#6718 = CARTESIAN_POINT ( 'NONE',  ( -2.229367062499996610, -26.14583333196773651, 3.861377020970582219 ) ) ;
#6719 = CARTESIAN_POINT ( 'NONE',  ( 2.229367062499998831, -88.64583333196773651, -3.861377020970580887 ) ) ;
#6720 = AXIS2_PLACEMENT_3D ( 'NONE', #6576, #55787, #30697 ) ;
#6721 = CARTESIAN_POINT ( 'NONE',  ( -2.500000000000000444, -23.04166666393548013, -4.330127018922193649 ) ) ;
#6723 = EDGE_LOOP ( 'NONE', ( #29423, #58239, #51661, #15930 ) ) ;
#6722 = CARTESIAN_POINT ( 'NONE',  ( -2.229367062499996610, -57.14583333196773651, 3.861377020970582219 ) ) ;
#6724 = CARTESIAN_POINT ( 'NONE',  ( 1.339745962155661996, -27.29465819873851729, -4.999999999999970690 ) ) ;
#6725 = DIRECTION ( 'NONE',  ( -0.000000000000000000, 1.000000000000000000, -0.000000000000000000 ) ) ;
#6727 = VERTEX_POINT ( 'NONE', #14559 ) ;
#6726 = CARTESIAN_POINT ( 'NONE',  ( -4.458734124999999437, -3.645833331967739621, -2.574251347313719407 ) ) ;
#6728 = CARTESIAN_POINT ( 'NONE',  ( -2.500000000000000444, -70.16666666666667140, -4.330127018922193649 ) ) ;
#6729 = CARTESIAN_POINT ( 'NONE',  ( -3.152801135295367096, -153.3125000013656063, -3.152801135295367541 ) ) ;
#6730 = CARTESIAN_POINT ( 'NONE',  ( 2.229367062500001939, -45.22916666530106511, 3.861377020970579999 ) ) ;
#6731 = LINE ( 'NONE', #58055, #10135 ) ;
#6732 = CARTESIAN_POINT ( 'NONE',  ( 3.061616997868383141E-16, -158.7500000000000000, -5.000000000000000000 ) ) ;
#6733 = CARTESIAN_POINT ( 'NONE',  ( 5.000000000000000000, -72.29166666393547303, -2.886751345948129988 ) ) ;
#6734 = CARTESIAN_POINT ( 'NONE',  ( 2.500000000000002220, -10.54166666393547835, 4.330127018922192761 ) ) ;
#6735 = CARTESIAN_POINT ( 'NONE',  ( -60.14911071818854538, -154.0625000000000000, 1.666127454062681368 ) ) ;
#6736 = CARTESIAN_POINT ( 'NONE',  ( -3.152548672688508926E-16, -15.81249999863440436, -5.148502694627439702 ) ) ;
#6737 = CARTESIAN_POINT ( 'NONE',  ( 9.457646018065525792E-16, -49.31249999863441502, 5.148502694627439702 ) ) ;
#6738 =( BOUNDED_CURVE ( )  B_SPLINE_CURVE ( 2, ( #2014, #27696, #21617, #41210, #22252, #42802, #3582, #18982, #4510 ),
 .UNSPECIFIED., .F., .F. ) 
 B_SPLINE_CURVE_WITH_KNOTS ( ( 3, 2, 2, 2, 3 ),
 ( 0.3395833333333333481, 0.3402777777777777901, 0.3416666666666666741, 0.3430555555555555580, 0.3437500000000000000 ),
 .UNSPECIFIED. ) 
 CURVE ( )  GEOMETRIC_REPRESENTATION_ITEM ( )  RATIONAL_B_SPLINE_CURVE ( ( 0.9330127018922194093, 0.9330127018922194093, 1.000000000000000000, 0.8660254037844387076, 1.000000000000000000, 0.8660254037844387076, 1.000000000000000000, 0.9330127018922194093, 0.9330127018922194093 ) ) 
 REPRESENTATION_ITEM ( '' )  );
#6739 = CARTESIAN_POINT ( 'NONE',  ( 2.500000000000002220, 10.33333333333333393, 4.330127018922192761 ) ) ;
#6740 = CARTESIAN_POINT ( 'NONE',  ( 3.152801135295367541, -144.3125000013655779, -3.152801135295367541 ) ) ;
#6741 = CARTESIAN_POINT ( 'NONE',  ( -3.152548672688508926E-16, -92.81249999863439371, -5.148502694627439702 ) ) ;
#6742 = CARTESIAN_POINT ( 'NONE',  ( 5.000000000000000000, -158.0625000000000284, 2.071067811865478614 ) ) ;
#6743 = ORIENTED_EDGE ( 'NONE', *, *, #28771, .F. ) ;
#6744 = CARTESIAN_POINT ( 'NONE',  ( 6.123233995736766282E-16, -120.0000000000000000, -5.000000000000000000 ) ) ;
#6745 = CARTESIAN_POINT ( 'NONE',  ( 4.458734125000001214, 26.85416666803225993, 2.574251347313718519 ) ) ;
#6746 = CARTESIAN_POINT ( 'NONE',  ( -59.98410592259440222, -147.2500000027312126, -0.3983568153799752487 ) ) ;
#6747 = DIRECTION ( 'NONE',  ( -0.000000000000000000, 1.000000000000000000, -0.000000000000000000 ) ) ;
#6748 = CARTESIAN_POINT ( 'NONE',  ( -2.229367062500000163, -0.4791666653010707710, -3.861377020970580443 ) ) ;
#6749 = CARTESIAN_POINT ( 'NONE',  ( 6.123233995736766282E-16, -120.0000000000000000, -5.000000000000000000 ) ) ;
#6750 = CARTESIAN_POINT ( 'NONE',  ( 4.458734124999999437, -24.06249999863440436, -5.460374474430324690E-16 ) ) ;
#6751 = CARTESIAN_POINT ( 'NONE',  ( 4.458734125000001214, -63.14583333196774362, 2.574251347313718519 ) ) ;
#6752 = DIRECTION ( 'NONE',  ( -0.000000000000000000, 1.000000000000000000, -0.000000000000000000 ) ) ;
#6753 = CARTESIAN_POINT ( 'NONE',  ( 9.457646018065525792E-16, -9.062499998634406140, 5.148502694627439702 ) ) ;
#6754 = CARTESIAN_POINT ( 'NONE',  ( 0.9763930676190096802, -8.096533237419681228, -7.213065638943101376 ) ) ;
#6755 = CARTESIAN_POINT ( 'NONE',  ( 2.730187237215162345E-16, -144.1875000013656063, -4.458734124999999437 ) ) ;
#6756 = CARTESIAN_POINT ( 'NONE',  ( -4.458734124999997661, 15.52083333469892779, 2.574251347313722516 ) ) ;
#6757 = ORIENTED_EDGE ( 'NONE', *, *, #44391, .F. ) ;
#6758 = LINE ( 'NONE', #26371, #63417 ) ;
#6759 = CARTESIAN_POINT ( 'NONE',  ( 5.000000000000000000, -71.29166666393547303, -2.886751345948130876 ) ) ;
#6761 = CARTESIAN_POINT ( 'NONE',  ( 9.457646018065525792E-16, -19.06249999863440792, 5.148502694627439702 ) ) ;
#6760 = CARTESIAN_POINT ( 'NONE',  ( -3.535250795749689387E-16, -84.24999999999998579, -5.773502691896257311 ) ) ;
#6762 = CARTESIAN_POINT ( 'NONE',  ( -62.00000000000001421, -135.0000000000000284, 4.041451884327384114 ) ) ;
#6763 = CARTESIAN_POINT ( 'NONE',  ( 1.975475456537005874E-15, -3.750000000000001776, 5.000000000000000000 ) ) ;
#6764 = AXIS2_PLACEMENT_3D ( 'NONE', #48268, #9348, #63397 ) ;
#6765 = CARTESIAN_POINT ( 'NONE',  ( -50.55543936806279248, -150.0625000013656063, 0.3552334253322060320 ) ) ;
#6766 = EDGE_CURVE ( 'NONE', #26829, #43493, #2482, .T. ) ;
#6767 = EDGE_CURVE ( 'NONE', #61101, #6968, #11482, .T. ) ;
#6768 = CARTESIAN_POINT ( 'NONE',  ( 5.000000000000000000, -46.29166666393547303, -2.886751345948129988 ) ) ;
#6769 = CARTESIAN_POINT ( 'NONE',  ( -1.339745962155610925, -1.669658196007333784, 5.000000000000000000 ) ) ;
#6770 = CARTESIAN_POINT ( 'NONE',  ( 4.458734125000000326, 11.10416666803225993, 2.574251347313718519 ) ) ;
#6771 = CARTESIAN_POINT ( 'NONE',  ( 1.975475456537005874E-15, -3.750000000000001776, 5.000000000000000000 ) ) ;
#6773 = EDGE_CURVE ( 'NONE', #53481, #48999, #58010, .T. ) ;
#6772 = CARTESIAN_POINT ( 'NONE',  ( 1.975475456537005874E-15, -14.74999999999999822, 5.000000000000000000 ) ) ;
#6774 = CARTESIAN_POINT ( 'NONE',  ( -3.152548672688508926E-16, 14.43750000136559386, -5.148502694627439702 ) ) ;
#6775 = CARTESIAN_POINT ( 'NONE',  ( 9.457646018065525792E-16, -69.06249999863439371, 5.148502694627439702 ) ) ;
#6776 = CARTESIAN_POINT ( 'NONE',  ( -4.458734124999999437, -13.56249999863440259, 0.000000000000000000 ) ) ;
#6777 = EDGE_CURVE ( 'NONE', #13925, #63218, #50045, .T. ) ;
#6778 = CARTESIAN_POINT ( 'NONE',  ( 5.000000000000000000, -1.416666666666663188, -2.886751345948129988 ) ) ;
#6779 = CARTESIAN_POINT ( 'NONE',  ( 3.152801135295367541, -163.3125000013656063, -3.152801135295367541 ) ) ;
#6780 = CARTESIAN_POINT ( 'NONE',  ( 4.458734124999999437, -58.81249999863440081, -5.460374474430324690E-16 ) ) ;
#6781 = CARTESIAN_POINT ( 'NONE',  ( -5.000000000000000000, -96.95833333060213022, -2.886751345948128211 ) ) ;
#6782 = EDGE_CURVE ( 'NONE', #10271, #5022, #29113, .T. ) ;
#6783 = ADVANCED_FACE ( 'NONE', ( #5560 ), #39957, .T. ) ;
#6784 = CARTESIAN_POINT ( 'NONE',  ( -5.000000000000000000, 9.916666666666667851, -2.886751345948128211 ) ) ;
#6785 = CYLINDRICAL_SURFACE ( 'NONE', #22423, 5.000000000000000000 ) ;
#6786 = CARTESIAN_POINT ( 'NONE',  ( -4.458734124999999437, -36.31249999863440792, 0.000000000000000000 ) ) ;
#6787 = CARTESIAN_POINT ( 'NONE',  ( -6.972266317189433020E-16, -51.12499999726880873, -5.000000000000000000 ) ) ;
#6788 = CARTESIAN_POINT ( 'NONE',  ( 2.500000000000002220, -49.66666666666666430, 4.330127018922192761 ) ) ;
#6789 = CARTESIAN_POINT ( 'NONE',  ( 5.000000000000000000, -13.49999999999999822, -6.123233995736766282E-16 ) ) ;
#6790 = EDGE_CURVE ( 'NONE', #37182, #733, #9406, .T. ) ;
#6791 = CYLINDRICAL_SURFACE ( 'NONE', #40716, 5.000000000000000000 ) ;
#6792 = ORIENTED_EDGE ( 'NONE', *, *, #48143, .F. ) ;
#6793 = CARTESIAN_POINT ( 'NONE',  ( -2.229367062500000163, -105.4791666653010651, -3.861377020970580443 ) ) ;
#6794 = CARTESIAN_POINT ( 'NONE',  ( -3.152548672688508926E-16, -1.812499998634406362, -5.148502694627439702 ) ) ;
#6795 = DIRECTION ( 'NONE',  ( 0.000000000000000000, 0.000000000000000000, 1.000000000000000000 ) ) ;
#6796 = ADVANCED_FACE ( 'NONE', ( #2902 ), #40602, .T. ) ;
#6797 = CARTESIAN_POINT ( 'NONE',  ( 2.499999999999998668, -5.333333333333335702, -4.330127018922193649 ) ) ;
#6798 = ADVANCED_FACE ( 'NONE', ( #20684 ), #30310, .T. ) ;
#6799 = CARTESIAN_POINT ( 'NONE',  ( 2.229367062499998831, -72.64583333196773651, -3.861377020970580887 ) ) ;
#6800 = DIRECTION ( 'NONE',  ( 0.000000000000000000, 1.000000000000000000, 0.000000000000000000 ) ) ;
#6801 = CARTESIAN_POINT ( 'NONE',  ( -2.500000000000000444, -5.041666663935480130, -4.330127018922193649 ) ) ;
#6803 = ORIENTED_EDGE ( 'NONE', *, *, #28742, .F. ) ;
#6802 = CARTESIAN_POINT ( 'NONE',  ( -2.229367062499996610, -37.14583333196773651, 3.861377020970582219 ) ) ;
#6804 = CARTESIAN_POINT ( 'NONE',  ( -5.000000000000000000, -16.95833333060214443, -2.886751345948128211 ) ) ;
#6806 = ORIENTED_EDGE ( 'NONE', *, *, #30575, .T. ) ;
#6805 = CARTESIAN_POINT ( 'NONE',  ( -4.458734124999999437, 10.35416666803225816, -2.574251347313719407 ) ) ;
#6807 = CARTESIAN_POINT ( 'NONE',  ( -1.339745962155610925, -55.66965819600732601, 5.000000000000000000 ) ) ;
#6808 = CARTESIAN_POINT ( 'NONE',  ( -2.500000000000000444, -54.16666666666667140, -4.330127018922193649 ) ) ;
#6809 = CARTESIAN_POINT ( 'NONE',  ( 9.457646018065525792E-16, -28.31249999863440081, 5.148502694627439702 ) ) ;
#6810 = CARTESIAN_POINT ( 'NONE',  ( -6.972266317189433020E-16, -60.24999999999999289, -5.000000000000000000 ) ) ;
#6811 = CARTESIAN_POINT ( 'NONE',  ( 9.457646018065525792E-16, -78.06249999863440792, 5.148502694627439702 ) ) ;
#6812 =( BOUNDED_CURVE ( )  B_SPLINE_CURVE ( 2, ( #32319, #4008, #7889, #3698, #13652, #38102, #23629, #63177, #33272 ),
 .UNSPECIFIED., .F., .F. ) 
 B_SPLINE_CURVE_WITH_KNOTS ( ( 3, 2, 2, 2, 3 ),
 ( 0.7062500000000000444, 0.7069444444444444864, 0.7083333333333333703, 0.7097222222222222543, 0.7104166666666666963 ),
 .UNSPECIFIED. ) 
 CURVE ( )  GEOMETRIC_REPRESENTATION_ITEM ( )  RATIONAL_B_SPLINE_CURVE ( ( 0.9330127018922194093, 0.9330127018922194093, 1.000000000000000000, 0.8660254037844387076, 1.000000000000000000, 0.8660254037844387076, 1.000000000000000000, 0.9330127018922194093, 0.9330127018922194093 ) ) 
 REPRESENTATION_ITEM ( '' )  );
#6813 = AXIS2_PLACEMENT_3D ( 'NONE', #52280, #23014, #13033 ) ;
#6814 = CARTESIAN_POINT ( 'NONE',  ( 2.071067811865475505, -168.8125000000000000, -5.000000000000000888 ) ) ;
#6815 = CARTESIAN_POINT ( 'NONE',  ( -4.458734124999999437, -87.31249999863439371, 0.000000000000000000 ) ) ;
#6816 = CARTESIAN_POINT ( 'NONE',  ( -56.48576386720575471, -136.0000000013656063, -4.591703134518078322 ) ) ;
#6817 = CIRCLE ( 'NONE', #53030, 5.000000000000000000 ) ;
#6818 = CARTESIAN_POINT ( 'NONE',  ( 4.458734124999999437, -35.06249999863440792, -5.460374474430324690E-16 ) ) ;
#6819 = CARTESIAN_POINT ( 'NONE',  ( 1.975475456537005874E-15, -74.62499999726880162, 5.000000000000000000 ) ) ;
#6820 = ORIENTED_EDGE ( 'NONE', *, *, #62648, .F. ) ;
#6821 = CARTESIAN_POINT ( 'NONE',  ( -4.458734124999998549, -77.47916666530106511, 2.574251347313722516 ) ) ;
#6822 = CARTESIAN_POINT ( 'NONE',  ( -2.499999999999996447, 13.29166666939785379, 4.330127018922195425 ) ) ;
#6823 = ORIENTED_EDGE ( 'NONE', *, *, #7951, .T. ) ;
#6824 = DIRECTION ( 'NONE',  ( -0.000000000000000000, 1.000000000000000000, -0.000000000000000000 ) ) ;
#6825 = CARTESIAN_POINT ( 'NONE',  ( -1.049326080737009628E-13, -18.62499999726881583, 5.000000000000000000 ) ) ;
#6826 = CARTESIAN_POINT ( 'NONE',  ( -4.458734124999999437, -63.64583333196773651, -2.574251347313719407 ) ) ;
#6827 = CARTESIAN_POINT ( 'NONE',  ( 2.229367062499998831, -6.895833331967741842, -3.861377020970580887 ) ) ;
#6828 = ORIENTED_EDGE ( 'NONE', *, *, #27140, .T. ) ;
#6829 = CARTESIAN_POINT ( 'NONE',  ( -1.975475456537005874E-15, 27.37500000273118417, 5.000000000000000000 ) ) ;
#6830 = CARTESIAN_POINT ( 'NONE',  ( -5.000000000000000000, 3.125000002731185944, 0.000000000000000000 ) ) ;
#6831 = ORIENTED_EDGE ( 'NONE', *, *, #11412, .F. ) ;
#6832 = CARTESIAN_POINT ( 'NONE',  ( 9.457646018065525792E-16, -7.312499998634405252, 5.148502694627439702 ) ) ;
#6833 = CARTESIAN_POINT ( 'NONE',  ( -4.458734124999999437, 5.687500001365592972, 0.000000000000000000 ) ) ;
#6834 = CARTESIAN_POINT ( 'NONE',  ( -5.000000000000000000, -32.95833333060215153, -2.886751345948128211 ) ) ;
#6835 = CARTESIAN_POINT ( 'NONE',  ( 4.458734124999999437, -160.4375000013655779, 0.000000000000000000 ) ) ;
#6836 =( BOUNDED_CURVE ( )  B_SPLINE_CURVE ( 2, ( #50726, #7630, #17266, #41382, #41696, #56837, #36891, #51050, #56520 ),
 .UNSPECIFIED., .F., .F. ) 
 B_SPLINE_CURVE_WITH_KNOTS ( ( 3, 2, 2, 2, 3 ),
 ( 0.07291666666666667129, 0.07361111111111111327, 0.07499999999999999722, 0.07638888888888889506, 0.07708333333333333703 ),
 .UNSPECIFIED. ) 
 CURVE ( )  GEOMETRIC_REPRESENTATION_ITEM ( )  RATIONAL_B_SPLINE_CURVE ( ( 0.9330127018922194093, 0.9330127018922200755, 1.000000000000000000, 0.8660254037844387076, 1.000000000000000000, 0.8660254037844387076, 1.000000000000000000, 0.9330127018922194093, 0.9330127018922194093 ) ) 
 REPRESENTATION_ITEM ( '' )  );
#6837 = DIRECTION ( 'NONE',  ( 0.000000000000000000, 0.000000000000000000, 1.000000000000000000 ) ) ;
#6838 = ORIENTED_EDGE ( 'NONE', *, *, #22536, .T. ) ;
#6839 = CARTESIAN_POINT ( 'NONE',  ( -2.229367062499996610, -87.14583333196773651, 3.861377020970582219 ) ) ;
#6840 = CARTESIAN_POINT ( 'NONE',  ( 1.975475456537005874E-15, -31.62499999726880873, 5.000000000000000000 ) ) ;
#6841 = CARTESIAN_POINT ( 'NONE',  ( 4.458734124999999437, -2.812499998634407472, -5.460374474430324690E-16 ) ) ;
#6842 = CARTESIAN_POINT ( 'NONE',  ( 5.000000000000000000, -28.37499999726881228, -6.123233995736766282E-16 ) ) ;
#6843 = DIRECTION ( 'NONE',  ( 0.000000000000000000, 0.000000000000000000, 1.000000000000000000 ) ) ;
#6844 = CARTESIAN_POINT ( 'NONE',  ( 9.457646018065525792E-16, 26.93750000136559564, 5.148502694627439702 ) ) ;
#6845 = CARTESIAN_POINT ( 'NONE',  ( 1.464175926609780648E-14, 22.74999999999999645, -5.000000000000000000 ) ) ;
#6846 = CARTESIAN_POINT ( 'NONE',  ( -2.229367062500000163, 29.52083333469892779, -3.861377020970580443 ) ) ;
#6847 = CARTESIAN_POINT ( 'NONE',  ( 4.458734125000001214, -48.89583333196772941, 2.574251347313718519 ) ) ;
#6848 = CARTESIAN_POINT ( 'NONE',  ( -4.458734124999999437, -36.64583333196773651, -2.574251347313719407 ) ) ;
#6849 = CARTESIAN_POINT ( 'NONE',  ( 4.458734124999999437, -0.06249999863440491854, -5.460374474430324690E-16 ) ) ;
#6850 = CARTESIAN_POINT ( 'NONE',  ( -1.339745962155585168, 8.919658201469705006, -5.000000000000015987 ) ) ;
#6851 = CARTESIAN_POINT ( 'NONE',  ( -2.499999999999996447, 16.16666666666666430, 4.330127018922195425 ) ) ;
#6852 = CARTESIAN_POINT ( 'NONE',  ( -2.071067811865475061, -144.8125000027312410, -5.000000000000000888 ) ) ;
#6853 = CARTESIAN_POINT ( 'NONE',  ( 0.000000000000000000, -170.0000000000000000, 0.000000000000000000 ) ) ;
#6854 = CARTESIAN_POINT ( 'NONE',  ( 4.458734124999998549, -44.72916666530106511, -2.574251347313721627 ) ) ;
#6855 = CARTESIAN_POINT ( 'NONE',  ( -4.999999999999999112, -77.79166666393547303, 2.886751345948131764 ) ) ;
#6856 = AXIS2_PLACEMENT_3D ( 'NONE', #50299, #45472, #60284 ) ;
#6857 = CARTESIAN_POINT ( 'NONE',  ( -54.64476657466781973, -138.0625000013656063, -4.444560631937228834 ) ) ;
#6858 = CARTESIAN_POINT ( 'NONE',  ( -4.999999999999998224, -86.91666666666667140, 2.886751345948131764 ) ) ;
#6859 = CARTESIAN_POINT ( 'NONE',  ( 7.914984360234579519, -3.818534719232097974, -7.907701344400643428 ) ) ;
#6860 = CARTESIAN_POINT ( 'NONE',  ( 2.229367062500001939, -84.22916666530107932, 3.861377020970579999 ) ) ;
#6861 = CARTESIAN_POINT ( 'NONE',  ( -4.458734124999999437, -162.1875000013655779, -5.460374474430324690E-16 ) ) ;
#6862 = CARTESIAN_POINT ( 'NONE',  ( -3.535533905932737309, -159.7500000027312126, -3.535533905932738197 ) ) ;
#6863 = CARTESIAN_POINT ( 'NONE',  ( 2.499999999999998668, -25.33333333333333215, -4.330127018922193649 ) ) ;
#6864 = CARTESIAN_POINT ( 'NONE',  ( -4.458734125000001214, -140.8750000013656063, 1.846868145590734089 ) ) ;
#6865 = ORIENTED_EDGE ( 'NONE', *, *, #49530, .F. ) ;
#6866 = CARTESIAN_POINT ( 'NONE',  ( 4.458734124999999437, 22.93750000136559564, -5.460374474430324690E-16 ) ) ;
#6867 = ORIENTED_EDGE ( 'NONE', *, *, #23901, .T. ) ;
#6868 = CARTESIAN_POINT ( 'NONE',  ( 4.458734124999999437, -88.81249999863439371, -5.460374474430324690E-16 ) ) ;
#6869 = CARTESIAN_POINT ( 'NONE',  ( 4.458734124999998549, 12.02083333469892601, -2.574251347313721627 ) ) ;
#6870 = CARTESIAN_POINT ( 'NONE',  ( 1.060575238724906964E-15, 17.37500000273118417, 5.773502691896257311 ) ) ;
#6871 = CARTESIAN_POINT ( 'NONE',  ( -51.19402409849444524, -138.6250000027312410, -3.242614290531456334 ) ) ;
#6872 = CARTESIAN_POINT ( 'NONE',  ( -2.499999999999996447, 10.16666666666666785, 4.330127018922195425 ) ) ;
#6873 = CARTESIAN_POINT ( 'NONE',  ( -4.458734124999997661, -55.22916666530107932, 2.574251347313722516 ) ) ;
#6874 = CARTESIAN_POINT ( 'NONE',  ( 9.457646018065525792E-16, -14.06249999863440259, 5.148502694627439702 ) ) ;
#6875 = CARTESIAN_POINT ( 'NONE',  ( 5.000000000000000000, -6.499999999999999112, -6.123233995736766282E-16 ) ) ;
#6876 = EDGE_CURVE ( 'NONE', #4851, #38994, #17237, .T. ) ;
#6877 = CARTESIAN_POINT ( 'NONE',  ( -59.59170313451810586, -135.7500000013656063, 1.485763867205729394 ) ) ;
#6878 = CARTESIAN_POINT ( 'NONE',  ( -2.499999999999996447, 14.16666666666666785, 4.330127018922195425 ) ) ;
#6879 = DIRECTION ( 'NONE',  ( -0.000000000000000000, 1.000000000000000000, -0.000000000000000000 ) ) ;
#6880 = CARTESIAN_POINT ( 'NONE',  ( -6.972266317189433020E-16, -11.12499999726881406, -5.000000000000000000 ) ) ;
#6881 = CARTESIAN_POINT ( 'NONE',  ( 1.060575238724906964E-15, -38.74999999999998579, 5.773502691896257311 ) ) ;
#6882 = CARTESIAN_POINT ( 'NONE',  ( 3.535533905932738197, -148.8750000000000000, -3.535533905932738197 ) ) ;
#6884 = CARTESIAN_POINT ( 'NONE',  ( 4.458734124999999437, -17.06249999863440792, -5.460374474430324690E-16 ) ) ;
#6883 = CARTESIAN_POINT ( 'NONE',  ( -60.14911071818854538, -139.0625000000000284, 1.666127454062681146 ) ) ;
#6885 = CARTESIAN_POINT ( 'NONE',  ( 6.123233995736766282E-16, -170.0000000000000000, -5.000000000000000000 ) ) ;
#6886 = CARTESIAN_POINT ( 'NONE',  ( -4.458734124999999437, -60.39583333196773651, -2.574251347313719407 ) ) ;
#6887 = CARTESIAN_POINT ( 'NONE',  ( 4.458734124999999437, -152.7500000013656063, 1.846868145590737864 ) ) ;
#6888 = CARTESIAN_POINT ( 'NONE',  ( -2.229367062499996610, -71.14583333196773651, 3.861377020970582219 ) ) ;
#6889 = CARTESIAN_POINT ( 'NONE',  ( -59.44456063193725015, -148.8125000013656063, -0.3552334253322034230 ) ) ;
#6890 = CARTESIAN_POINT ( 'NONE',  ( 2.229367062499998831, -18.89583333196774007, -3.861377020970580887 ) ) ;
#6891 = CARTESIAN_POINT ( 'NONE',  ( 5.000000000000000000, -60.37499999726880873, -6.123233995736766282E-16 ) ) ;
#6892 = ORIENTED_EDGE ( 'NONE', *, *, #42758, .F. ) ;
#6893 = DIRECTION ( 'NONE',  ( -0.000000000000000000, 1.000000000000000000, -0.000000000000000000 ) ) ;
#6894 = ORIENTED_EDGE ( 'NONE', *, *, #41762, .T. ) ;
#6895 = CARTESIAN_POINT ( 'NONE',  ( 4.458734125000001214, -64.14583333196773651, 2.574251347313718519 ) ) ;
#6896 = CARTESIAN_POINT ( 'NONE',  ( 1.975475456537005874E-15, 11.37500000273118239, 5.000000000000000000 ) ) ;
#6897 = CARTESIAN_POINT ( 'NONE',  ( 3.152801135295366208, -152.5625000013655779, 3.152801135295367985 ) ) ;
#6898 = VERTEX_POINT ( 'NONE', #15537 ) ;
#6899 = AXIS2_PLACEMENT_3D ( 'NONE', #61335, #2476, #60062 ) ;
#6900 = CARTESIAN_POINT ( 'NONE',  ( -2.500000000000000444, -8.041666663935481907, -4.330127018922193649 ) ) ;
#6901 = CARTESIAN_POINT ( 'NONE',  ( -59.81910112700025905, -126.1875000000000426, -2.462841084822630311 ) ) ;
#6902 = DIRECTION ( 'NONE',  ( -0.000000000000000000, 1.000000000000000000, -0.000000000000000000 ) ) ;
#6903 = CARTESIAN_POINT ( 'NONE',  ( -4.458734124999999437, -48.64583333196773651, -2.574251347313719407 ) ) ;
#6904 = AXIS2_PLACEMENT_3D ( 'NONE', #9613, #24414, #53996 ) ;
#6905 = EDGE_LOOP ( 'NONE', ( #29170, #59405, #17218, #45973 ) ) ;
#6906 = VECTOR ( 'NONE', #29987, 1000.000000000000000 ) ;
#6907 = DIRECTION ( 'NONE',  ( -1.000000000000000000, 0.000000000000000000, 0.000000000000000000 ) ) ;
#6908 = CARTESIAN_POINT ( 'NONE',  ( 4.458734124999999437, 6.187500001365593860, -5.460374474430324690E-16 ) ) ;
#6909 = CARTESIAN_POINT ( 'NONE',  ( 2.229367062500001939, 23.02083333469892423, 3.861377020970579999 ) ) ;
#6910 = CARTESIAN_POINT ( 'NONE',  ( -54.64476657466781973, -147.8125000013656063, -4.444560631937228834 ) ) ;
#6911 = CARTESIAN_POINT ( 'NONE',  ( 5.000000000000000000, -108.3749999972688016, -6.123233995736766282E-16 ) ) ;
#6912 = CARTESIAN_POINT ( 'NONE',  ( 2.499999999999998668, -25.33333333333333215, -4.330127018922193649 ) ) ;
#6913 = ORIENTED_EDGE ( 'NONE', *, *, #28761, .F. ) ;
#6914 = CARTESIAN_POINT ( 'NONE',  ( 4.458734125000000326, -72.89583333196775072, 2.574251347313718519 ) ) ;
#6915 = LINE ( 'NONE', #35540, #12994 ) ;
#6916 = CARTESIAN_POINT ( 'NONE',  ( -3.152548672688508926E-16, 13.43750000136559386, -5.148502694627439702 ) ) ;
#6917 =( BOUNDED_SURFACE ( )  B_SPLINE_SURFACE ( 3, 2, ( 
 ( #43893, #44861, #44218 ),
 ( #39707, #10773, #824 ),
 ( #59347, #53565, #9490 ),
 ( #63542, #19463, #59022 ),
 ( #14953, #59995, #60953 ),
 ( #31666, #31336, #16244 ),
 ( #51303, #55489, #60637 ),
 ( #21387, #56117, #26852 ) ),
 .UNSPECIFIED., .F., .F., .F. ) 
 B_SPLINE_SURFACE_WITH_KNOTS ( ( 4, 2, 2, 4 ),
 ( 3, 3 ),
 ( 0.03861844051980969222, 0.04325213341840641185, 0.04556897986770477166, 0.04788582631700313147 ),
 ( 0.000000000000000000, 1.000000000000000000 ),
 .UNSPECIFIED. ) 
 GEOMETRIC_REPRESENTATION_ITEM ( )  RATIONAL_B_SPLINE_SURFACE ( (
 ( 1.000000000000000000, 0.8047781759831921233, 1.000000000000000000),
 ( 1.000000000000000000, 0.8123762462806503049, 1.000000000000000000),
 ( 1.000000000000000000, 0.8190659850614813164, 1.000000000000000000),
 ( 1.000000000000000000, 0.8191937571014595854, 1.000000000000000000),
 ( 1.000000000000000000, 0.8176092952779865364, 1.000000000000000000),
 ( 1.000000000000000000, 0.8122962088597069918, 1.000000000000000000),
 ( 1.000000000000000000, 0.8086311330827506971, 1.000000000000000000),
 ( 1.000000000000000000, 0.8047712282214323221, 1.000000000000000000) ) ) 
 REPRESENTATION_ITEM ( '' )  SURFACE ( )  );
#6918 = CARTESIAN_POINT ( 'NONE',  ( 1.975475456537005874E-15, -31.75000000000000000, 5.000000000000000000 ) ) ;
#6919 = CARTESIAN_POINT ( 'NONE',  ( -58.24261429053147765, -152.3750000027312126, -3.805975901505573855 ) ) ;
#6920 = CARTESIAN_POINT ( 'NONE',  ( -2.229367062499996610, -56.39583333196773651, 3.861377020970582219 ) ) ;
#6921 = CARTESIAN_POINT ( 'NONE',  ( -5.000000000000000000, -13.95833333060215153, -2.886751345948128211 ) ) ;
#6922 = DIRECTION ( 'NONE',  ( -0.000000000000000000, 1.000000000000000000, -0.000000000000000000 ) ) ;
#6923 = CARTESIAN_POINT ( 'NONE',  ( 1.975475456537005874E-15, -89.62499999726880162, 5.000000000000000000 ) ) ;
#6924 = DIRECTION ( 'NONE',  ( -0.000000000000000000, 1.000000000000000000, -0.000000000000000000 ) ) ;
#6925 = CARTESIAN_POINT ( 'NONE',  ( -3.152548672688508926E-16, -21.81249999863440436, -5.148502694627439702 ) ) ;
#6926 = ORIENTED_EDGE ( 'NONE', *, *, #26360, .F. ) ;
#6927 = DIRECTION ( 'NONE',  ( -0.000000000000000000, 1.000000000000000000, -0.000000000000000000 ) ) ;
#6928 = CARTESIAN_POINT ( 'NONE',  ( 2.229367062499998831, -107.6458333319677365, -3.861377020970580887 ) ) ;
#6929 = CARTESIAN_POINT ( 'NONE',  ( 3.061616997868383141E-16, -156.8750000027311842, -5.000000000000000000 ) ) ;
#6930 = ORIENTED_EDGE ( 'NONE', *, *, #14786, .F. ) ;
#6931 = CARTESIAN_POINT ( 'NONE',  ( 2.229367062500001939, -103.2291666653010651, 3.861377020970579999 ) ) ;
#6932 = CARTESIAN_POINT ( 'NONE',  ( 2.229367062499998831, -27.64583333196774007, -3.861377020970580887 ) ) ;
#6933 = CARTESIAN_POINT ( 'NONE',  ( -4.999999999999999112, -61.79166666393546592, 2.886751345948131764 ) ) ;
#6934 = CARTESIAN_POINT ( 'NONE',  ( -57.89159099828107458, -150.9375000013656063, -3.393966926194107447 ) ) ;
#6935 =( BOUNDED_CURVE ( )  B_SPLINE_CURVE ( 2, ( #55425, #51549, #21325, #11654, #27097, #11342, #30965, #31274, #62780 ),
 .UNSPECIFIED., .F., .F. ) 
 B_SPLINE_CURVE_WITH_KNOTS ( ( 3, 2, 2, 2, 3 ),
 ( 0.6416666666666662744, 0.6458333333333329263, 0.6499999999999996891, 0.6541666666666663410, 0.6583333333333329929 ),
 .UNSPECIFIED. ) 
 CURVE ( )  GEOMETRIC_REPRESENTATION_ITEM ( )  RATIONAL_B_SPLINE_CURVE ( ( 1.000000000000008216, 0.9238795325112786339, 1.000000000000000000, 0.9238795325112867385, 1.000000000000000000, 0.9238795325112867385, 1.000000000000000000, 0.9238795325112928447, 0.9999999999999938938 ) ) 
 REPRESENTATION_ITEM ( '' )  );
#6936 = CARTESIAN_POINT ( 'NONE',  ( -57.19623071787016499, -143.3750000013656063, 4.297418129356382899 ) ) ;
#6937 = CARTESIAN_POINT ( 'NONE',  ( 4.458734124999998549, -22.72916666530107221, -2.574251347313721627 ) ) ;
#6938 = CARTESIAN_POINT ( 'NONE',  ( -4.458734124999999437, -71.64583333196773651, -2.574251347313719407 ) ) ;
#6939 = CARTESIAN_POINT ( 'NONE',  ( -57.46284108482265651, -136.9375000000000000, 4.819101127000238627 ) ) ;
#6940 = CARTESIAN_POINT ( 'NONE',  ( 4.458734124999999437, -26.81249999863440081, -5.460374474430324690E-16 ) ) ;
#6941 = LINE ( 'NONE', #51001, #60502 ) ;
#6942 = CARTESIAN_POINT ( 'NONE',  ( -5.000000000000000888, -150.4375000000000000, 2.071067811865474617 ) ) ;
#6943 = CARTESIAN_POINT ( 'NONE',  ( 5.000000000000000000, -12.41666666666666607, -2.886751345948129988 ) ) ;
#6944 = CARTESIAN_POINT ( 'NONE',  ( -3.152801135295367096, -153.0625000013656063, -3.152801135295367541 ) ) ;
#6945 = ORIENTED_EDGE ( 'NONE', *, *, #33776, .T. ) ;
#6946 = CARTESIAN_POINT ( 'NONE',  ( -2.229367062499996610, -52.39583333196773651, 3.861377020970582219 ) ) ;
#6947 = AXIS2_PLACEMENT_3D ( 'NONE', #49216, #5474, #20271 ) ;
#6948 = CARTESIAN_POINT ( 'NONE',  ( 1.975475456537005874E-15, -2.624999997268813168, 5.000000000000000000 ) ) ;
#6949 = CARTESIAN_POINT ( 'NONE',  ( 2.499999999999998668, -92.33333333333334281, -4.330127018922193649 ) ) ;
#6950 = CARTESIAN_POINT ( 'NONE',  ( -2.499999999999996447, 22.16666666666666785, 4.330127018922195425 ) ) ;
#6951 = VECTOR ( 'NONE', #299, 1000.000000000000000 ) ;
#6952 = VECTOR ( 'NONE', #37802, 1000.000000000000000 ) ;
#6953 = CARTESIAN_POINT ( 'NONE',  ( 0.000000000000000000, -170.0000000000000000, 0.000000000000000000 ) ) ;
#6954 = CARTESIAN_POINT ( 'NONE',  ( 9.457646018065525792E-16, 6.937500001365594748, 5.148502694627439702 ) ) ;
#6955 = CARTESIAN_POINT ( 'NONE',  ( -6.972266317189433020E-16, 19.75000000000000000, -5.000000000000000000 ) ) ;
#6956 = VECTOR ( 'NONE', #5341, 1000.000000000000000 ) ;
#6957 = CARTESIAN_POINT ( 'NONE',  ( 5.000000000000000000, 13.49999999999999822, -6.123233995736766282E-16 ) ) ;
#6958 = CARTESIAN_POINT ( 'NONE',  ( 1.339745962155612702, -7.294658198738518173, -5.000000000000000000 ) ) ;
#6959 = CARTESIAN_POINT ( 'NONE',  ( 2.229367062500001939, 17.77083333469892779, 3.861377020970579999 ) ) ;
#6960 = CARTESIAN_POINT ( 'NONE',  ( -5.000000000000000000, 5.125000002731184168, 0.000000000000000000 ) ) ;
#6961 = EDGE_LOOP ( 'NONE', ( #31831, #62520 ) ) ;
#6962 = DIRECTION ( 'NONE',  ( -0.000000000000000000, 1.000000000000000000, -0.000000000000000000 ) ) ;
#6963 = ORIENTED_EDGE ( 'NONE', *, *, #51137, .F. ) ;
#6964 = CARTESIAN_POINT ( 'NONE',  ( -5.926426369611017623E-15, 26.25000000000000000, 5.000000000000000000 ) ) ;
#6965 = CARTESIAN_POINT ( 'NONE',  ( -2.229367062500000163, -41.47916666530107932, -3.861377020970580443 ) ) ;
#6966 = CARTESIAN_POINT ( 'NONE',  ( -3.152801135295367096, -164.3125000013656063, -3.152801135295367541 ) ) ;
#6967 = CARTESIAN_POINT ( 'NONE',  ( 5.000000000000000888, -44.45833333060214443, 2.886751345948126879 ) ) ;
#6968 = VERTEX_POINT ( 'NONE', #49931 ) ;
#6969 = CARTESIAN_POINT ( 'NONE',  ( 4.458734125000001214, -15.89583333196773651, 2.574251347313718519 ) ) ;
#6970 = ORIENTED_EDGE ( 'NONE', *, *, #36265, .T. ) ;
#6971 = CARTESIAN_POINT ( 'NONE',  ( -3.535250795749689387E-16, -88.25000000000000000, -5.773502691896257311 ) ) ;
#6972 = CARTESIAN_POINT ( 'NONE',  ( 1.846868145590736310, -163.6250000013656063, 4.458734124999999437 ) ) ;
#6974 = ORIENTED_EDGE ( 'NONE', *, *, #32342, .T. ) ;
#6973 = CARTESIAN_POINT ( 'NONE',  ( -4.999999999999998224, -18.91666666666666430, 2.886751345948131764 ) ) ;
#6975 = CARTESIAN_POINT ( 'NONE',  ( -59.98410592259440222, -141.1250000000000284, -0.3983568153799752487 ) ) ;
#6976 = ADVANCED_FACE ( 'NONE', ( #25819 ), #5886, .T. ) ;
#6977 = CARTESIAN_POINT ( 'NONE',  ( 2.229367062499998831, -29.89583333196773296, -3.861377020970580887 ) ) ;
#6978 = CYLINDRICAL_SURFACE ( 'NONE', #18647, 5.000000000000000000 ) ;
#6979 = ORIENTED_EDGE ( 'NONE', *, *, #15409, .T. ) ;
#6980 = CARTESIAN_POINT ( 'NONE',  ( -3.152548672688508926E-16, -77.56249999863440792, -5.148502694627439702 ) ) ;
#6981 = CARTESIAN_POINT ( 'NONE',  ( 2.229367062500001939, 29.02083333469892779, 3.861377020970579999 ) ) ;
#6982 = CARTESIAN_POINT ( 'NONE',  ( -60.14911071818854538, -137.1875000027312126, 1.666127454062681146 ) ) ;
#6983 = ORIENTED_EDGE ( 'NONE', *, *, #7932, .F. ) ;
#6984 = CARTESIAN_POINT ( 'NONE',  ( -3.535533905932737309, -166.7500000027312126, -3.535533905932738197 ) ) ;
#6985 = CARTESIAN_POINT ( 'NONE',  ( -56.48576386720575471, -144.0000000013656063, -4.591703134518078322 ) ) ;
#6986 = CARTESIAN_POINT ( 'NONE',  ( 4.458734125000001214, -82.14583333196772230, 2.574251347313718519 ) ) ;
#6987 = CARTESIAN_POINT ( 'NONE',  ( -50.01589407740564042, -130.7500000027312126, 0.3983568153799778022 ) ) ;
#6988 = CARTESIAN_POINT ( 'NONE',  ( 0.000000000000000000, -120.0000000000000000, 0.000000000000000000 ) ) ;
#6989 = CARTESIAN_POINT ( 'NONE',  ( -8.190561711645485556E-16, -140.9375000013656063, 4.458734124999999437 ) ) ;
#6990 =( BOUNDED_CURVE ( )  B_SPLINE_CURVE ( 2, ( #19561, #39173, #25026, #45281, #25344, #53976, #15060, #44315, #49471 ),
 .UNSPECIFIED., .F., .F. ) 
 B_SPLINE_CURVE_WITH_KNOTS ( ( 3, 2, 2, 2, 3 ),
 ( 0.8946428571428571841, 0.8952380952380952772, 0.8964285714285714635, 0.8976190476190476497, 0.8982142857142857428 ),
 .UNSPECIFIED. ) 
 CURVE ( )  GEOMETRIC_REPRESENTATION_ITEM ( )  RATIONAL_B_SPLINE_CURVE ( ( 0.9330127018922194093, 0.9330127018922194093, 1.000000000000000000, 0.8660254037844387076, 1.000000000000000000, 0.8660254037844387076, 1.000000000000000000, 0.9330127018922194093, 0.9330127018922194093 ) ) 
 REPRESENTATION_ITEM ( '' )  );
#6991 = VECTOR ( 'NONE', #45192, 1000.000000000000000 ) ;
#6992 = DIRECTION ( 'NONE',  ( -0.000000000000000000, 1.000000000000000000, -0.000000000000000000 ) ) ;
#6993 = CARTESIAN_POINT ( 'NONE',  ( 4.458734124999999437, -53.81249999863439371, -5.460374474430324690E-16 ) ) ;
#6994 = CARTESIAN_POINT ( 'NONE',  ( 4.458734124999998549, -44.72916666530106511, -2.574251347313721627 ) ) ;
#6995 = CARTESIAN_POINT ( 'NONE',  ( 4.458734125000001214, 29.10416666803225993, 2.574251347313718519 ) ) ;
#6996 = CARTESIAN_POINT ( 'NONE',  ( 2.499999999999998668, -107.3333333333333428, -4.330127018922193649 ) ) ;
#6997 = CARTESIAN_POINT ( 'NONE',  ( 5.000000000000000888, -3.583333333333333925, 2.886751345948126879 ) ) ;
#6998 = CARTESIAN_POINT ( 'NONE',  ( -2.229367062499996610, -41.39583333196773651, 3.861377020970582219 ) ) ;
#6999 = CARTESIAN_POINT ( 'NONE',  ( -5.000000000000000000, 2.041666669397854239, -2.886751345948128211 ) ) ;
#7000 = CARTESIAN_POINT ( 'NONE',  ( -6.972266317189433020E-16, -73.25000000000000000, -5.000000000000000000 ) ) ;
#7001 = CARTESIAN_POINT ( 'NONE',  ( -52.80376928212989185, -129.8750000013656063, -4.297418129356379346 ) ) ;
#7002 = CARTESIAN_POINT ( 'NONE',  ( -3.152548672688508926E-16, -76.81249999863440792, -5.148502694627439702 ) ) ;
#7003 = CARTESIAN_POINT ( 'NONE',  ( -5.000000000000000000, 5.916666666666666963, -2.886751345948128211 ) ) ;
#7004 = CARTESIAN_POINT ( 'NONE',  ( 2.229367062500001939, -94.97916666530106511, 3.861377020970579999 ) ) ;
#7005 = CARTESIAN_POINT ( 'NONE',  ( -2.229367062499996610, -7.395833331967735624, 3.861377020970582219 ) ) ;
#7006 = ORIENTED_EDGE ( 'NONE', *, *, #38613, .F. ) ;
#7007 = CARTESIAN_POINT ( 'NONE',  ( -54.60164318462004474, -146.3750000000000284, -4.984105922594373794 ) ) ;
#7008 = CARTESIAN_POINT ( 'NONE',  ( 5.000000000000000000, -47.50000000000000000, -6.123233995736766282E-16 ) ) ;
#7009 = CARTESIAN_POINT ( 'NONE',  ( -3.152548672688508926E-16, -88.56249999863439371, -5.148502694627439702 ) ) ;
#7010 = CARTESIAN_POINT ( 'NONE',  ( 5.000000000000000000, 27.50000000000000000, -6.123233995736766282E-16 ) ) ;
#7011 = CARTESIAN_POINT ( 'NONE',  ( -4.458734124999999437, -88.56249999863439371, 0.000000000000000000 ) ) ;
#7012 = CARTESIAN_POINT ( 'NONE',  ( 4.458734125000000326, 13.85416666803225993, 2.574251347313718519 ) ) ;
#7013 = CARTESIAN_POINT ( 'NONE',  ( 6.123233995736766282E-16, -120.0000000000000000, -5.000000000000000000 ) ) ;
#7014 = CARTESIAN_POINT ( 'NONE',  ( -50.55543936806279248, -133.0625000013656063, 0.3552334253322060320 ) ) ;
#7015 = CARTESIAN_POINT ( 'NONE',  ( 4.458734125000000326, -5.895833331967740953, 2.574251347313718519 ) ) ;
#7016 = CARTESIAN_POINT ( 'NONE',  ( 4.458734124999999437, 18.93750000136559564, -5.460374474430324690E-16 ) ) ;
#7017 = CARTESIAN_POINT ( 'NONE',  ( -4.458734124999999437, -50.64583333196773651, -2.574251347313719407 ) ) ;
#7018 = FACE_OUTER_BOUND ( 'NONE', #47108, .T. ) ;
#7019 = CARTESIAN_POINT ( 'NONE',  ( 2.229367062500001939, -85.97916666530107932, 3.861377020970579999 ) ) ;
#7020 = CARTESIAN_POINT ( 'NONE',  ( 2.229367062500001939, -10.97916666530107044, 3.861377020970579999 ) ) ;
#7021 = CARTESIAN_POINT ( 'NONE',  ( 1.339745962155612702, -84.29465819873850307, -5.000000000000000000 ) ) ;
#7022 = VERTEX_POINT ( 'NONE', #35472 ) ;
#7023 = CARTESIAN_POINT ( 'NONE',  ( 2.229367062499998831, -33.89583333196772941, -3.861377020970580887 ) ) ;
#7024 = CARTESIAN_POINT ( 'NONE',  ( -59.29741812935640155, -129.8750000013656063, -2.196230717870135685 ) ) ;
#7025 = CARTESIAN_POINT ( 'NONE',  ( -2.229367062499996610, -79.14583333196773651, 3.861377020970582219 ) ) ;
#7026 = CARTESIAN_POINT ( 'NONE',  ( -2.229367062500000163, 28.27083333469892779, -3.861377020970580443 ) ) ;
#7027 = CARTESIAN_POINT ( 'NONE',  ( 4.458734124999999437, 18.18750000136559564, -5.460374474430324690E-16 ) ) ;
#7028 = CARTESIAN_POINT ( 'NONE',  ( -5.000000000000000000, -94.00000000000000000, 0.000000000000000000 ) ) ;
#7029 = CARTESIAN_POINT ( 'NONE',  ( 0.000000000000000000, -120.0000000000000000, 5.000000000000000000 ) ) ;
#7030 = CARTESIAN_POINT ( 'NONE',  ( 4.458734124999998549, -77.97916666530106511, -2.574251347313721627 ) ) ;
#7031 = CARTESIAN_POINT ( 'NONE',  ( -2.500000000000000444, -63.16666666666666430, -4.330127018922193649 ) ) ;
#7032 = CARTESIAN_POINT ( 'NONE',  ( 0.000000000000000000, -170.0000000000000000, 5.000000000000000000 ) ) ;
#7033 = CARTESIAN_POINT ( 'NONE',  ( 5.000000000000000000, 21.70833333606451987, -2.886751345948129988 ) ) ;
#7034 = ORIENTED_EDGE ( 'NONE', *, *, #40264, .T. ) ;
#7035 = CARTESIAN_POINT ( 'NONE',  ( 5.000000000000000000, -1.374999997268814500, -6.123233995736766282E-16 ) ) ;
#7036 = CARTESIAN_POINT ( 'NONE',  ( 1.339745962155615144, 7.294658198738519950, 4.999999999999999112 ) ) ;
#7037 =( BOUNDED_CURVE ( )  B_SPLINE_CURVE ( 2, ( #51336, #36213, #57117, #8218, #56481, #12404, #32652, #26886, #60988 ),
 .UNSPECIFIED., .F., .F. ) 
 B_SPLINE_CURVE_WITH_KNOTS ( ( 3, 2, 2, 2, 3 ),
 ( 0.7517857142857142794, 0.7523809523809523725, 0.7535714285714285587, 0.7547619047619047450, 0.7553571428571428381 ),
 .UNSPECIFIED. ) 
 CURVE ( )  GEOMETRIC_REPRESENTATION_ITEM ( )  RATIONAL_B_SPLINE_CURVE ( ( 0.9330127018922194093, 0.9330127018922194093, 1.000000000000000000, 0.8660254037844387076, 1.000000000000000000, 0.8660254037844387076, 1.000000000000000000, 0.9330127018922194093, 0.9330127018922194093 ) ) 
 REPRESENTATION_ITEM ( '' )  );
#7039 = CARTESIAN_POINT ( 'NONE',  ( -2.499999999999996447, -22.83333333333333215, 4.330127018922195425 ) ) ;
#7038 = CYLINDRICAL_SURFACE ( 'NONE', #15382, 5.000000000000000000 ) ;
#7040 = CARTESIAN_POINT ( 'NONE',  ( -2.229367062499996610, -27.14583333196774007, 3.861377020970582219 ) ) ;
#7041 = CARTESIAN_POINT ( 'NONE',  ( 2.229367062500001939, -88.97916666530106511, 3.861377020970579999 ) ) ;
#7042 = CARTESIAN_POINT ( 'NONE',  ( -4.999999999999999112, -30.79166666393548013, 2.886751345948131764 ) ) ;
#7044 = VERTEX_POINT ( 'NONE', #55089 ) ;
#7043 = CARTESIAN_POINT ( 'NONE',  ( -2.229367062499996610, -55.14583333196773651, 3.861377020970582219 ) ) ;
#7045 = CARTESIAN_POINT ( 'NONE',  ( 5.000000000000000000, -27.49999999999999645, -6.123233995736766282E-16 ) ) ;
#7047 = ORIENTED_EDGE ( 'NONE', *, *, #58246, .T. ) ;
#7046 = CARTESIAN_POINT ( 'NONE',  ( -3.152548672688508926E-16, -4.812499998634402587, -5.148502694627439702 ) ) ;
#7048 = CARTESIAN_POINT ( 'NONE',  ( -2.499999999999996447, -69.83333333333332860, 4.330127018922195425 ) ) ;
#7049 = CARTESIAN_POINT ( 'NONE',  ( -51.60603307380591787, -136.9375000013655779, -2.891590998281053704 ) ) ;
#7050 = CARTESIAN_POINT ( 'NONE',  ( -3.152548672688508926E-16, -44.81249999863440792, -5.148502694627439702 ) ) ;
#7051 = FACE_OUTER_BOUND ( 'NONE', #53473, .T. ) ;
#7052 = CARTESIAN_POINT ( 'NONE',  ( -4.999999999999999112, -69.79166666393547303, 2.886751345948131764 ) ) ;
#7053 = CARTESIAN_POINT ( 'NONE',  ( -1.339745962155613812, -22.08034179853029855, -5.000000000000000000 ) ) ;
#7054 = CARTESIAN_POINT ( 'NONE',  ( -57.46284108482265651, -152.9375000000000000, 4.819101127000239515 ) ) ;
#7055 = EDGE_CURVE ( 'NONE', #59659, #27072, #791, .T. ) ;
#7056 = CARTESIAN_POINT ( 'NONE',  ( 4.458734125000001214, -14.14583333196774184, 2.574251347313718519 ) ) ;
#7057 = AXIS2_PLACEMENT_3D ( 'NONE', #35794, #34833, #44470 ) ;
#7058 = CARTESIAN_POINT ( 'NONE',  ( -4.458734124999999437, -52.64583333196773651, -2.574251347313719407 ) ) ;
#7059 = CARTESIAN_POINT ( 'NONE',  ( -4.999999999999998224, -58.79166666393546592, 2.886751345948131764 ) ) ;
#7060 = CARTESIAN_POINT ( 'NONE',  ( -3.152801135295367985, -141.8125000013655779, 3.152801135295367096 ) ) ;
#7061 = CARTESIAN_POINT ( 'NONE',  ( 4.458734125000001214, -95.14583333196772230, 2.574251347313718519 ) ) ;
#7062 = CARTESIAN_POINT ( 'NONE',  ( 2.071067811865603403, -158.1874999999999716, 4.999999999999872990 ) ) ;
#7063 = ORIENTED_EDGE ( 'NONE', *, *, #49954, .F. ) ;
#7064 = CARTESIAN_POINT ( 'NONE',  ( -50.40829686548195099, -154.2500000013656063, -1.485763867205728284 ) ) ;
#7065 = CARTESIAN_POINT ( 'NONE',  ( 4.458734125000001214, 23.85416666803225993, 2.574251347313718519 ) ) ;
#7066 = CARTESIAN_POINT ( 'NONE',  ( -54.60164318462004474, -145.5000000027312126, -4.984105922594373794 ) ) ;
#7067 = ADVANCED_FACE ( 'NONE', ( #45755 ), #17364, .T. ) ;
#7068 = CARTESIAN_POINT ( 'NONE',  ( 1.339745962155615144, -50.70534180126148271, 4.999999999999999112 ) ) ;
#7069 = CARTESIAN_POINT ( 'NONE',  ( -4.458734124999998549, -1.229166665301071326, 2.574251347313722516 ) ) ;
#7070 = CARTESIAN_POINT ( 'NONE',  ( 2.229367062499998831, -97.89583333196773651, -3.861377020970580887 ) ) ;
#7071 = CARTESIAN_POINT ( 'NONE',  ( 2.730187237215162345E-16, -147.4375000013656063, -4.458734124999999437 ) ) ;
#7072 = CARTESIAN_POINT ( 'NONE',  ( -3.152548672688508926E-16, -24.81249999863440436, -5.148502694627439702 ) ) ;
#7073 = EDGE_CURVE ( 'NONE', #17293, #53696, #25006, .T. ) ;
#7074 = DIRECTION ( 'NONE',  ( 0.000000000000000000, 0.000000000000000000, 1.000000000000000000 ) ) ;
#7075 = CARTESIAN_POINT ( 'NONE',  ( 4.458734124999999437, -63.06249999863440792, -5.460374474430324690E-16 ) ) ;
#7076 = CARTESIAN_POINT ( 'NONE',  ( 1.975475456537005874E-15, -70.75000000000000000, 5.000000000000000000 ) ) ;
#7077 = CARTESIAN_POINT ( 'NONE',  ( 4.419133455864432847, -6.108866147516184952, -7.026396753507086146 ) ) ;
#7078 = CARTESIAN_POINT ( 'NONE',  ( 4.458734124999999437, -144.4375000013656063, 0.000000000000000000 ) ) ;
#7079 = AXIS2_PLACEMENT_3D ( 'NONE', #8521, #31696, #46808 ) ;
#7080 = CARTESIAN_POINT ( 'NONE',  ( -2.229367062499996610, 13.60416666803226171, 3.861377020970582219 ) ) ;
#7081 = EDGE_LOOP ( 'NONE', ( #54082, #49054, #26434, #5050 ) ) ;
#7082 = CARTESIAN_POINT ( 'NONE',  ( -3.535533905932737309, -164.7500000027312126, -3.535533905932738197 ) ) ;
#7084 = CARTESIAN_POINT ( 'NONE',  ( 2.229367062500001939, -19.97916666530107221, 3.861377020970579999 ) ) ;
#7083 = CARTESIAN_POINT ( 'NONE',  ( -2.499999999999996447, -84.83333333333332860, 4.330127018922195425 ) ) ;
#7085 = CARTESIAN_POINT ( 'NONE',  ( -4.458734124999999437, 28.35416666803225993, -2.574251347313719407 ) ) ;
#7086 = CARTESIAN_POINT ( 'NONE',  ( -6.972266317189433020E-16, -3.250000000000001332, -5.000000000000000000 ) ) ;
#7087 = CARTESIAN_POINT ( 'NONE',  ( -57.89159099828107458, -144.6875000013656063, -3.393966926194107447 ) ) ;
#7088 = B_SPLINE_CURVE_WITH_KNOTS ( 'NONE', 3,
 ( #24260, #13975, #53222, #14920, #39046, #34526 ),
 .UNSPECIFIED., .F., .F.,
 ( 4, 2, 4 ),
 ( -5.145455527296316946E-06, 0.0004153350442917489458, 0.0008358155441107941331 ),
 .UNSPECIFIED. ) ;
#7089 = CARTESIAN_POINT ( 'NONE',  ( 1.060575238724906964E-15, -46.62499999726880873, 5.773502691896257311 ) ) ;
#7090 = CARTESIAN_POINT ( 'NONE',  ( -2.500000000000000444, -2.041666663935480575, -4.330127018922193649 ) ) ;
#7091 = CARTESIAN_POINT ( 'NONE',  ( -2.229367062499996610, 7.854166668032260823, 3.861377020970582219 ) ) ;
#7092 = DIRECTION ( 'NONE',  ( -0.000000000000000000, 1.000000000000000000, -0.000000000000000000 ) ) ;
#7093 = CARTESIAN_POINT ( 'NONE',  ( 2.626220312808019583E-14, 21.75000000000000000, -5.000000000000000000 ) ) ;
#7094 = CARTESIAN_POINT ( 'NONE',  ( 9.457646018065525792E-16, 10.93750000136559208, 5.148502694627439702 ) ) ;
#7095 = CARTESIAN_POINT ( 'NONE',  ( 2.229367062499998831, -66.64583333196773651, -3.861377020970580887 ) ) ;
#7096 = CARTESIAN_POINT ( 'NONE',  ( 4.458734125000000326, -14.14583333196774184, 2.574251347313718519 ) ) ;
#7097 = CARTESIAN_POINT ( 'NONE',  ( 1.060575238724906964E-15, -0.7500000000000007772, 5.773502691896257311 ) ) ;
#7098 = CARTESIAN_POINT ( 'NONE',  ( -4.458734125000001214, -160.8750000013655779, 1.846868145590734089 ) ) ;
#7099 = CARTESIAN_POINT ( 'NONE',  ( -1.336351044127974539E-14, 22.24999999999999645, 5.000000000000000000 ) ) ;
#7100 = CARTESIAN_POINT ( 'NONE',  ( 2.229367062499998831, -57.64583333196773651, -3.861377020970580887 ) ) ;
#7101 = CARTESIAN_POINT ( 'NONE',  ( 5.000000000000000000, -92.37499999726880162, -6.123233995736766282E-16 ) ) ;
#7102 = ADVANCED_FACE ( 'NONE', ( #28579 ), #53343, .T. ) ;
#7103 = CARTESIAN_POINT ( 'NONE',  ( -2.500000000000000444, -80.16666666666665719, -4.330127018922193649 ) ) ;
#7104 = CARTESIAN_POINT ( 'NONE',  ( -5.000000000000000000, -36.00000000000000711, 0.000000000000000000 ) ) ;
#7105 = CARTESIAN_POINT ( 'NONE',  ( 2.229367062500001939, -34.97916666530107221, 3.861377020970579999 ) ) ;
#7106 = CARTESIAN_POINT ( 'NONE',  ( -1.339745962155610925, -90.66965819600733312, 5.000000000000000000 ) ) ;
#7107 = CARTESIAN_POINT ( 'NONE',  ( -5.000000000000000000, -51.00000000000000711, 0.000000000000000000 ) ) ;
#7108 = DIRECTION ( 'NONE',  ( -0.000000000000000000, 1.000000000000000000, -0.000000000000000000 ) ) ;
#7109 = ORIENTED_EDGE ( 'NONE', *, *, #23709, .T. ) ;
#7110 = CARTESIAN_POINT ( 'NONE',  ( 9.457646018065525792E-16, -109.0624999986344221, 5.148502694627439702 ) ) ;
#7111 = CARTESIAN_POINT ( 'NONE',  ( 9.457646018065525792E-16, -0.3124999986344051961, 5.148502694627439702 ) ) ;
#7112 = CARTESIAN_POINT ( 'NONE',  ( 2.071067811865392461, -144.3125000027312410, 5.000000000000084377 ) ) ;
#7113 = CARTESIAN_POINT ( 'NONE',  ( 2.500000000000002220, -8.666666666666669627, 4.330127018922192761 ) ) ;
#7114 = CARTESIAN_POINT ( 'NONE',  ( -3.152548672688508926E-16, -74.56249999863442213, -5.148502694627439702 ) ) ;
#7115 =( BOUNDED_CURVE ( )  B_SPLINE_CURVE ( 2, ( #57774, #14004, #13695, #37514, #23675, #28487, #3430, #33007, #51996 ),
 .UNSPECIFIED., .F., .F. ) 
 B_SPLINE_CURVE_WITH_KNOTS ( ( 3, 2, 2, 2, 3 ),
 ( 0.1803571428571428548, 0.1809523809523809479, 0.1821428571428571341, 0.1833333333333333204, 0.1839285714285714413 ),
 .UNSPECIFIED. ) 
 CURVE ( )  GEOMETRIC_REPRESENTATION_ITEM ( )  RATIONAL_B_SPLINE_CURVE ( ( 0.9330127018922194093, 0.9330127018922194093, 1.000000000000000000, 0.8660254037844387076, 1.000000000000000000, 0.8660254037844387076, 1.000000000000000000, 0.9330127018922178550, 0.9330127018922194093 ) ) 
 REPRESENTATION_ITEM ( '' )  );
#7116 = CARTESIAN_POINT ( 'NONE',  ( -5.000000000000000000, -26.08333333333332860, -2.886751345948128211 ) ) ;
#7117 = CARTESIAN_POINT ( 'NONE',  ( -4.999999999999999112, -6.791666663935481907, 2.886751345948131764 ) ) ;
#7119 = ORIENTED_EDGE ( 'NONE', *, *, #52826, .F. ) ;
#7118 = CARTESIAN_POINT ( 'NONE',  ( 4.458734125000001214, -38.89583333196773651, 2.574251347313718519 ) ) ;
#7120 = CARTESIAN_POINT ( 'NONE',  ( -2.500000000000000444, 27.95833333606451987, -4.330127018922193649 ) ) ;
#7122 = EDGE_LOOP ( 'NONE', ( #38425, #4575, #40285, #11179 ) ) ;
#7121 = CARTESIAN_POINT ( 'NONE',  ( 2.229367062500001939, 12.77083333469892779, 3.861377020970579999 ) ) ;
#7123 = CARTESIAN_POINT ( 'NONE',  ( 2.500000000000002220, -81.54166666393547303, 4.330127018922192761 ) ) ;
#7124 = CARTESIAN_POINT ( 'NONE',  ( 5.000000000000000000, -56.49999999999999289, -6.123233995736766282E-16 ) ) ;
#7125 = CARTESIAN_POINT ( 'NONE',  ( 3.152801135295366208, -161.8125000013656063, 3.152801135295367985 ) ) ;
#7126 = CARTESIAN_POINT ( 'NONE',  ( 4.458734124999998549, -31.97916666530107577, -2.574251347313721627 ) ) ;
#7127 = CARTESIAN_POINT ( 'NONE',  ( -6.972266317189433020E-16, -35.25000000000000000, -5.000000000000000000 ) ) ;
#7128 = CARTESIAN_POINT ( 'NONE',  ( -2.229367062500000163, -82.47916666530106511, -3.861377020970580443 ) ) ;
#7129 = CARTESIAN_POINT ( 'NONE',  ( 5.000000000000000000, -170.0000000000000000, 0.000000000000000000 ) ) ;
#7130 = CARTESIAN_POINT ( 'NONE',  ( 4.458734124999999437, -88.81249999863439371, -5.460374474430324690E-16 ) ) ;
#7131 = CARTESIAN_POINT ( 'NONE',  ( -57.19623071787017210, -136.6250000013655779, 4.297418129356382899 ) ) ;
#7132 = CARTESIAN_POINT ( 'NONE',  ( -3.152548672688508926E-16, -34.81249999863440792, -5.148502694627439702 ) ) ;
#7133 = EDGE_CURVE ( 'NONE', #7022, #25814, #18624, .T. ) ;
#7134 = EDGE_CURVE ( 'NONE', #9564, #32043, #18051, .T. ) ;
#7135 = CARTESIAN_POINT ( 'NONE',  ( 5.000000000000000000, -83.37499999726881583, -6.123233995736766282E-16 ) ) ;
#7136 = ORIENTED_EDGE ( 'NONE', *, *, #12788, .T. ) ;
#7137 = CARTESIAN_POINT ( 'NONE',  ( -4.458734124999998549, -78.47916666530107932, 2.574251347313722516 ) ) ;
#7138 = CARTESIAN_POINT ( 'NONE',  ( -1.250000000000000444, 7.938566201357357244, -7.198902722707429369 ) ) ;
#7139 = EDGE_CURVE ( 'NONE', #57442, #9470, #33280, .T. ) ;
#7140 = VERTEX_POINT ( 'NONE', #52418 ) ;
#7141 = CARTESIAN_POINT ( 'NONE',  ( -5.000000000000000000, -3.874999997268816720, 0.000000000000000000 ) ) ;
#7142 = DIRECTION ( 'NONE',  ( 0.000000000000000000, 0.000000000000000000, 1.000000000000000000 ) ) ;
#7143 = CARTESIAN_POINT ( 'NONE',  ( -4.458734124999999437, -66.64583333196773651, -2.574251347313719407 ) ) ;
#7144 = CARTESIAN_POINT ( 'NONE',  ( 4.458734124999998549, -6.979166665301073103, -2.574251347313721627 ) ) ;
#7145 = ORIENTED_EDGE ( 'NONE', *, *, #28761, .T. ) ;
#7146 = EDGE_CURVE ( 'NONE', #60305, #27444, #38164, .T. ) ;
#7147 = VECTOR ( 'NONE', #44056, 1000.000000000000114 ) ;
#7148 = DIRECTION ( 'NONE',  ( -0.000000000000000000, 1.000000000000000000, -0.000000000000000000 ) ) ;
#7149 = CARTESIAN_POINT ( 'NONE',  ( -5.000000000000000000, -92.95833333060214443, -2.886751345948128211 ) ) ;
#7150 = ORIENTED_EDGE ( 'NONE', *, *, #21762, .F. ) ;
#7151 = CARTESIAN_POINT ( 'NONE',  ( 2.229367062500001939, -8.229166665301073991, 3.861377020970579999 ) ) ;
#7152 = EDGE_CURVE ( 'NONE', #11069, #32964, #37297, .T. ) ;
#7153 = FACE_OUTER_BOUND ( 'NONE', #24183, .T. ) ;
#7154 = CARTESIAN_POINT ( 'NONE',  ( -2.229367062500000163, 9.520833334698927786, -3.861377020970580443 ) ) ;
#7155 = DIRECTION ( 'NONE',  ( 0.000000000000000000, 0.000000000000000000, 1.000000000000000000 ) ) ;
#7156 = CARTESIAN_POINT ( 'NONE',  ( -4.458734125000000326, -156.8750000013655779, 1.846868145590734089 ) ) ;
#7157 = CARTESIAN_POINT ( 'NONE',  ( -5.000000000000000000, 19.12500000273118772, 0.000000000000000000 ) ) ;
#7158 = VERTEX_POINT ( 'NONE', #47572 ) ;
#7159 = CARTESIAN_POINT ( 'NONE',  ( 4.458734124999998549, -84.72916666530106511, -2.574251347313721627 ) ) ;
#7160 = ADVANCED_FACE ( 'NONE', ( #3523 ), #23133, .T. ) ;
#7161 = DIRECTION ( 'NONE',  ( 0.000000000000000000, 0.000000000000000000, 1.000000000000000000 ) ) ;
#7162 = CARTESIAN_POINT ( 'NONE',  ( -4.458734124999999437, -1.395833331967737179, -2.574251347313719407 ) ) ;
#7163 = CARTESIAN_POINT ( 'NONE',  ( 5.000000000000000888, -51.58333333333332149, 2.886751345948126879 ) ) ;
#7164 = CARTESIAN_POINT ( 'NONE',  ( -3.535250795749689387E-16, -29.12499999726881228, -5.773502691896257311 ) ) ;
#7165 = DIRECTION ( 'NONE',  ( 0.000000000000000000, -1.000000000000000000, 0.000000000000000000 ) ) ;
#7166 = CARTESIAN_POINT ( 'NONE',  ( 2.229367062499998831, 26.35416666803225993, -3.861377020970580887 ) ) ;
#7167 = CARTESIAN_POINT ( 'NONE',  ( -5.000000000000000000, -20.95833333060214798, -2.886751345948128211 ) ) ;
#7168 =( BOUNDED_CURVE ( )  B_SPLINE_CURVE ( 2, ( #61930, #8208, #32008, #57106, #37790, #18780, #23316, #12393, #62868 ),
 .UNSPECIFIED., .F., .F. ) 
 B_SPLINE_CURVE_WITH_KNOTS ( ( 3, 2, 2, 2, 3 ),
 ( 0.2446428571428571341, 0.2452380952380952273, 0.2464285714285714413, 0.2476190476190476275, 0.2482142857142857206 ),
 .UNSPECIFIED. ) 
 CURVE ( )  GEOMETRIC_REPRESENTATION_ITEM ( )  RATIONAL_B_SPLINE_CURVE ( ( 0.9330127018922194093, 0.9330127018922194093, 1.000000000000000000, 0.8660254037844387076, 1.000000000000000000, 0.8660254037844387076, 1.000000000000000000, 0.9330127018922194093, 0.9330127018922194093 ) ) 
 REPRESENTATION_ITEM ( '' )  );
#7169 = CARTESIAN_POINT ( 'NONE',  ( 4.458734124999999437, 29.18750000136559208, -5.460374474430324690E-16 ) ) ;
#7170 = CARTESIAN_POINT ( 'NONE',  ( 2.229367062500001939, -53.97916666530107221, 3.861377020970579999 ) ) ;
#7171 = CARTESIAN_POINT ( 'NONE',  ( 2.229367062500001939, -39.22916666530107221, 3.861377020970579999 ) ) ;
#7172 = CARTESIAN_POINT ( 'NONE',  ( -4.458734124999997661, 3.520833334698929118, 2.574251347313722516 ) ) ;
#7173 = CYLINDRICAL_SURFACE ( 'NONE', #14438, 5.000000000000000888 ) ;
#7174 = CARTESIAN_POINT ( 'NONE',  ( 2.499999999999998668, 17.66666666666666430, -4.330127018922193649 ) ) ;
#7175 = CARTESIAN_POINT ( 'NONE',  ( 3.061616997868383141E-16, -146.8750000027312126, -5.000000000000000000 ) ) ;
#7176 = CYLINDRICAL_SURFACE ( 'NONE', #32549, 5.000000000000000000 ) ;
#7177 = VECTOR ( 'NONE', #35024, 1000.000000000000000 ) ;
#7178 = CARTESIAN_POINT ( 'NONE',  ( -4.458734124999999437, -45.31249999863440081, 0.000000000000000000 ) ) ;
#7179 = CARTESIAN_POINT ( 'NONE',  ( 5.000000000000000000, -80.37499999726881583, -6.123233995736766282E-16 ) ) ;
#7180 = CARTESIAN_POINT ( 'NONE',  ( -52.80376928212989185, -138.1250000013656063, -4.297418129356379346 ) ) ;
#7181 = CARTESIAN_POINT ( 'NONE',  ( 1.339745962155612702, -65.16965819600733312, -5.000000000000000000 ) ) ;
#7182 = CARTESIAN_POINT ( 'NONE',  ( -1.339745962155613812, -88.20534180126146850, -5.000000000000000000 ) ) ;
#7183 = CARTESIAN_POINT ( 'NONE',  ( 4.458734125000000326, -88.14583333196773651, 2.574251347313718519 ) ) ;
#7184 = CARTESIAN_POINT ( 'NONE',  ( 4.458734124999999437, -163.6250000013656063, -1.846868145590734978 ) ) ;
#7185 = CARTESIAN_POINT ( 'NONE',  ( -6.972266317189433020E-16, 13.87500000273118594, -5.000000000000000000 ) ) ;
#7186 = CARTESIAN_POINT ( 'NONE',  ( 2.500000000000002220, -30.66666666666666785, 4.330127018922192761 ) ) ;
#7187 = CARTESIAN_POINT ( 'NONE',  ( -4.458734125000001214, -139.8750000013656063, 1.846868145590734089 ) ) ;
#7188 = VERTEX_POINT ( 'NONE', #37929 ) ;
#7189 = CARTESIAN_POINT ( 'NONE',  ( -4.458734124999999437, 21.43750000136559208, 0.000000000000000000 ) ) ;
#7190 = VERTEX_POINT ( 'NONE', #57562 ) ;
#7191 = CARTESIAN_POINT ( 'NONE',  ( -3.152548672688508926E-16, -88.56249999863439371, -5.148502694627439702 ) ) ;
#7192 = CARTESIAN_POINT ( 'NONE',  ( -4.458734124999999437, 11.43750000136559564, 0.000000000000000000 ) ) ;
#7193 = CARTESIAN_POINT ( 'NONE',  ( 2.500000000000002220, 14.45833333606451809, 4.330127018922192761 ) ) ;
#7194 = CARTESIAN_POINT ( 'NONE',  ( 1.975475456537005874E-15, -101.6249999972688158, 5.000000000000000000 ) ) ;
#7195 = CARTESIAN_POINT ( 'NONE',  ( -3.535250795749689387E-16, 6.749999999999999112, -5.773502691896257311 ) ) ;
#7196 = CARTESIAN_POINT ( 'NONE',  ( 4.458734124999998549, -53.72916666530107932, -2.574251347313721627 ) ) ;
#7197 = DIRECTION ( 'NONE',  ( -0.000000000000000000, 1.000000000000000000, -0.000000000000000000 ) ) ;
#7198 = FACE_OUTER_BOUND ( 'NONE', #59652, .T. ) ;
#7199 = CARTESIAN_POINT ( 'NONE',  ( 5.000000000000000888, 7.541666669397851130, 2.886751345948126879 ) ) ;
#7200 = CARTESIAN_POINT ( 'NONE',  ( -6.972266317189433020E-16, -0.1249999972688142363, -5.000000000000000000 ) ) ;
#7201 = CARTESIAN_POINT ( 'NONE',  ( -2.500000000000000444, 17.95833333606451632, -4.330127018922193649 ) ) ;
#7202 = CARTESIAN_POINT ( 'NONE',  ( -5.000000000000000000, -41.08333333333333570, -2.886751345948128211 ) ) ;
#7203 = CARTESIAN_POINT ( 'NONE',  ( 1.339745962155499015, -107.7053418012614543, 5.000000000000065725 ) ) ;
#7205 = CARTESIAN_POINT ( 'NONE',  ( -2.229367062499996610, -14.39583333196774184, 3.861377020970582219 ) ) ;
#7204 = CARTESIAN_POINT ( 'NONE',  ( -5.000000000000000000, -45.08333333333333570, -2.886751345948128211 ) ) ;
#7206 = CARTESIAN_POINT ( 'NONE',  ( -3.535533905932737309, -143.6250000000000000, -3.535533905932738197 ) ) ;
#7207 = CARTESIAN_POINT ( 'NONE',  ( 4.458734124999999437, -60.81249999863440081, -5.460374474430324690E-16 ) ) ;
#7208 = CARTESIAN_POINT ( 'NONE',  ( -4.458734124999999437, -151.1875000013656063, -5.460374474430324690E-16 ) ) ;
#7209 = CARTESIAN_POINT ( 'NONE',  ( 4.458734124999999437, -70.81249999863439371, -5.460374474430324690E-16 ) ) ;
#7210 = CARTESIAN_POINT ( 'NONE',  ( -52.10840900171896806, -145.4375000013656063, 3.393966926194110556 ) ) ;
#7211 = CARTESIAN_POINT ( 'NONE',  ( 2.229367062500001939, -17.22916666530106866, 3.861377020970579999 ) ) ;
#7212 = CARTESIAN_POINT ( 'NONE',  ( 5.000000000000000000, -58.29166666393548724, -2.886751345948129988 ) ) ;
#7214 = ORIENTED_EDGE ( 'NONE', *, *, #4813, .F. ) ;
#7213 = EDGE_CURVE ( 'NONE', #32181, #39986, #13487, .T. ) ;
#7215 = DIRECTION ( 'NONE',  ( 0.000000000000000000, 0.000000000000000000, 1.000000000000000000 ) ) ;
#7216 = VERTEX_POINT ( 'NONE', #10233 ) ;
#7217 = CARTESIAN_POINT ( 'NONE',  ( -3.152548672688508926E-16, -60.81249999863440081, -5.148502694627439702 ) ) ;
#7219 = CARTESIAN_POINT ( 'NONE',  ( 5.000000000000000888, -8.583333333333332149, 2.886751345948126879 ) ) ;
#7218 = CARTESIAN_POINT ( 'NONE',  ( -62.00000000000001421, -135.0000000000000284, 4.041451884327384114 ) ) ;
#7220 = CARTESIAN_POINT ( 'NONE',  ( 2.730187237215162345E-16, -154.1875000013656063, -4.458734124999999437 ) ) ;
#7221 = VERTEX_POINT ( 'NONE', #58491 ) ;
#7222 =( BOUNDED_CURVE ( )  B_SPLINE_CURVE ( 2, ( #20987, #40590, #16154, #30299, #49919, #5871, #42015, #32048, #7310 ),
 .UNSPECIFIED., .F., .F. ) 
 B_SPLINE_CURVE_WITH_KNOTS ( ( 3, 2, 2, 2, 3 ),
 ( 0.4089285714285714191, 0.4095238095238095122, 0.4107142857142856984, 0.4119047619047618847, 0.4124999999999999778 ),
 .UNSPECIFIED. ) 
 CURVE ( )  GEOMETRIC_REPRESENTATION_ITEM ( )  RATIONAL_B_SPLINE_CURVE ( ( 0.9330127018922194093, 0.9330127018922194093, 1.000000000000000000, 0.8660254037844387076, 1.000000000000000000, 0.8660254037844387076, 1.000000000000000000, 0.9330127018922194093, 0.9330127018922194093 ) ) 
 REPRESENTATION_ITEM ( '' )  );
#7223 = LINE ( 'NONE', #46452, #57055 ) ;
#7224 = CARTESIAN_POINT ( 'NONE',  ( -50.18089887299979068, -126.6875000000000426, 2.462841084822635640 ) ) ;
#7226 = AXIS2_PLACEMENT_3D ( 'NONE', #34869, #25212, #39043 ) ;
#7225 = CARTESIAN_POINT ( 'NONE',  ( 1.339745962155612702, -8.294658198738519062, -5.000000000000000000 ) ) ;
#7227 = CARTESIAN_POINT ( 'NONE',  ( 4.458734124999999437, -46.06249999863440081, -5.460374474430324690E-16 ) ) ;
#7228 = ORIENTED_EDGE ( 'NONE', *, *, #10330, .F. ) ;
#7229 = CARTESIAN_POINT ( 'NONE',  ( 1.975475456537005874E-15, -77.75000000000000000, 5.000000000000000000 ) ) ;
#7230 = CARTESIAN_POINT ( 'NONE',  ( -3.152548672688508926E-16, 6.437500001365592972, -5.148502694627439702 ) ) ;
#7231 = EDGE_CURVE ( 'NONE', #21367, #721, #49236, .T. ) ;
#7232 = CARTESIAN_POINT ( 'NONE',  ( 4.458734125000001214, 22.10416666803225993, 2.574251347313718519 ) ) ;
#7233 = CARTESIAN_POINT ( 'NONE',  ( -50.40829686548195099, -149.0000000013656063, -1.485763867205728284 ) ) ;
#7234 = CYLINDRICAL_SURFACE ( 'NONE', #30532, 5.000000000000000000 ) ;
#7236 = EDGE_CURVE ( 'NONE', #41687, #27676, #7375, .T. ) ;
#7235 = ORIENTED_EDGE ( 'NONE', *, *, #10335, .T. ) ;
#7237 = CARTESIAN_POINT ( 'NONE',  ( -2.229367062499996610, -68.14583333196773651, 3.861377020970582219 ) ) ;
#7238 = LINE ( 'NONE', #2110, #54078 ) ;
#7239 = CARTESIAN_POINT ( 'NONE',  ( 4.458734124999999437, 14.18750000136559386, -5.460374474430324690E-16 ) ) ;
#7240 = VECTOR ( 'NONE', #14790, 1000.000000000000000 ) ;
#7241 = CARTESIAN_POINT ( 'NONE',  ( 1.339745962155612702, -63.29465819873851729, -5.000000000000000000 ) ) ;
#7242 = EDGE_CURVE ( 'NONE', #42402, #17975, #6990, .T. ) ;
#7243 = CARTESIAN_POINT ( 'NONE',  ( 3.535533905932738197, -157.0000000027312126, -3.535533905932738197 ) ) ;
#7244 = CARTESIAN_POINT ( 'NONE',  ( 4.458734124999999437, -54.06249999863440081, -5.460374474430324690E-16 ) ) ;
#7245 = CARTESIAN_POINT ( 'NONE',  ( 1.060575238724906964E-15, -15.62499999726881406, 5.773502691896257311 ) ) ;
#7246 = CARTESIAN_POINT ( 'NONE',  ( -2.499999999999996447, -99.83333333333332860, 4.330127018922195425 ) ) ;
#7247 = LINE ( 'NONE', #15690, #15188 ) ;
#7248 = DIRECTION ( 'NONE',  ( 0.000000000000000000, 0.000000000000000000, 1.000000000000000000 ) ) ;
#7249 = CARTESIAN_POINT ( 'NONE',  ( -2.229367062500000163, -20.72916666530107221, -3.861377020970580443 ) ) ;
#7250 = VERTEX_POINT ( 'NONE', #44637 ) ;
#7251 = CARTESIAN_POINT ( 'NONE',  ( -2.500000000000000444, -61.16666666666666430, -4.330127018922193649 ) ) ;
#7252 = CARTESIAN_POINT ( 'NONE',  ( -3.152548672688508926E-16, -108.5624999986343937, -5.148502694627439702 ) ) ;
#7253 = CARTESIAN_POINT ( 'NONE',  ( -9.184850993605147944E-16, -159.3750000027311842, 5.000000000000000000 ) ) ;
#7254 = VERTEX_POINT ( 'NONE', #39808 ) ;
#7255 = CARTESIAN_POINT ( 'NONE',  ( -3.152548672688508926E-16, -100.8124999986343937, -5.148502694627439702 ) ) ;
#7256 = CARTESIAN_POINT ( 'NONE',  ( -4.458734124999999437, -25.39583333196773651, -2.574251347313719407 ) ) ;
#7257 = CARTESIAN_POINT ( 'NONE',  ( -5.000000000000000000, -61.87499999726880873, 0.000000000000000000 ) ) ;
#7258 = CARTESIAN_POINT ( 'NONE',  ( -50.55543936806279248, -153.3125000013656063, 0.3552334253322060320 ) ) ;
#7259 = CARTESIAN_POINT ( 'NONE',  ( -2.071067811865475061, -147.6875000000000284, -5.000000000000000888 ) ) ;
#7260 = CARTESIAN_POINT ( 'NONE',  ( -3.152548672688508926E-16, -25.56249999863440792, -5.148502694627439702 ) ) ;
#7261 = CARTESIAN_POINT ( 'NONE',  ( 2.229367062499998831, -71.89583333196773651, -3.861377020970580887 ) ) ;
#7262 = CARTESIAN_POINT ( 'NONE',  ( -2.499999999999996447, -39.70833333060214443, 4.330127018922195425 ) ) ;
#7263 = CARTESIAN_POINT ( 'NONE',  ( 2.229367062499998831, -24.64583333196773651, -3.861377020970580887 ) ) ;
#7264 = DIRECTION ( 'NONE',  ( -0.000000000000000000, 1.000000000000000000, -0.000000000000000000 ) ) ;
#7265 = CARTESIAN_POINT ( 'NONE',  ( -5.000000000000000888, -150.5625000000000284, -2.071067811865475949 ) ) ;
#7266 = CARTESIAN_POINT ( 'NONE',  ( -4.999999999999999112, -14.91666666666666785, 2.886751345948131764 ) ) ;
#7267 = CARTESIAN_POINT ( 'NONE',  ( -1.846868145590737420, -153.7500000013656063, 4.458734124999999437 ) ) ;
#7268 = ORIENTED_EDGE ( 'NONE', *, *, #54712, .F. ) ;
#7269 = CARTESIAN_POINT ( 'NONE',  ( -59.81910112700025905, -153.1875000000000000, -2.462841084822604110 ) ) ;
#7270 = CARTESIAN_POINT ( 'NONE',  ( 4.458734124999998549, -50.97916666530107221, -2.574251347313721627 ) ) ;
#7271 = DIRECTION ( 'NONE',  ( 0.000000000000000000, 0.000000000000000000, 1.000000000000000000 ) ) ;
#7272 = CARTESIAN_POINT ( 'NONE',  ( -2.499999999999996447, -110.7083333306021444, 4.330127018922195425 ) ) ;
#7273 = CARTESIAN_POINT ( 'NONE',  ( -4.999999999999999112, 25.08333333333333215, 2.886751345948131764 ) ) ;
#7274 = CIRCLE ( 'NONE', #28774, 7.500000000000001776 ) ;
#7275 = DIRECTION ( 'NONE',  ( -0.000000000000000000, 1.000000000000000000, 0.000000000000000000 ) ) ;
#7276 = CARTESIAN_POINT ( 'NONE',  ( -4.458734124999998549, 6.770833334698928674, 2.574251347313722516 ) ) ;
#7277 = CARTESIAN_POINT ( 'NONE',  ( 5.000000000000000000, 19.58333333333333215, -2.886751345948130876 ) ) ;
#7278 = CARTESIAN_POINT ( 'NONE',  ( 5.000000000000000000, -11.29166666393547835, -2.886751345948130876 ) ) ;
#7279 = DIRECTION ( 'NONE',  ( -0.000000000000000000, 1.000000000000000000, -0.000000000000000000 ) ) ;
#7280 = CARTESIAN_POINT ( 'NONE',  ( 4.458734124999998549, 16.02083333469892423, -2.574251347313721627 ) ) ;
#7281 = CARTESIAN_POINT ( 'NONE',  ( -4.999999999999999112, 2.208333336064519870, 2.886751345948131764 ) ) ;
#7282 = ORIENTED_EDGE ( 'NONE', *, *, #53511, .T. ) ;
#7283 = CARTESIAN_POINT ( 'NONE',  ( -7.500000000000000000, -2.571118828324945760, -0.3627527587569098766 ) ) ;
#7284 = ORIENTED_EDGE ( 'NONE', *, *, #8824, .F. ) ;
#7285 = CARTESIAN_POINT ( 'NONE',  ( -5.000000000000000000, -71.00000000000000000, 0.000000000000000000 ) ) ;
#7286 = CARTESIAN_POINT ( 'NONE',  ( 9.457646018065525792E-16, -43.06249999863440081, 5.148502694627439702 ) ) ;
#7287 = CARTESIAN_POINT ( 'NONE',  ( 3.152801135295366208, -164.8125000013656063, 3.152801135295367985 ) ) ;
#7288 = EDGE_CURVE ( 'NONE', #62194, #4978, #15992, .T. ) ;
#7289 = CARTESIAN_POINT ( 'NONE',  ( -5.000000000000000000, -45.95833333060214443, -2.886751345948128211 ) ) ;
#7290 = ORIENTED_EDGE ( 'NONE', *, *, #29069, .F. ) ;
#7291 = CARTESIAN_POINT ( 'NONE',  ( -3.152548672688508926E-16, -15.56249999863440614, -5.148502694627439702 ) ) ;
#7292 = ORIENTED_EDGE ( 'NONE', *, *, #44069, .T. ) ;
#7293 = CARTESIAN_POINT ( 'NONE',  ( -4.999999999999999112, -86.91666666666667140, 2.886751345948131764 ) ) ;
#7294 = CARTESIAN_POINT ( 'NONE',  ( -1.846868145590737420, -162.7500000013655779, 4.458734124999999437 ) ) ;
#7296 = ORIENTED_EDGE ( 'NONE', *, *, #26443, .F. ) ;
#7295 = CARTESIAN_POINT ( 'NONE',  ( -5.000000000000000000, -60.95833333060214443, -2.886751345948128211 ) ) ;
#7297 = CARTESIAN_POINT ( 'NONE',  ( -58.80597590150559739, -136.0000000000000284, 3.242614290531460330 ) ) ;
#7298 = CARTESIAN_POINT ( 'NONE',  ( -2.229367062499996610, -33.39583333196772941, 3.861377020970582219 ) ) ;
#7299 = CARTESIAN_POINT ( 'NONE',  ( -1.339745962155610925, 23.33034180399266333, 5.000000000000000000 ) ) ;
#7300 = ORIENTED_EDGE ( 'NONE', *, *, #3671, .T. ) ;
#7301 =( BOUNDED_CURVE ( )  B_SPLINE_CURVE ( 2, ( #20279, #54695, #10935, #39881, #40524, #25418, #16089, #1004, #45036 ),
 .UNSPECIFIED., .F., .F. ) 
 B_SPLINE_CURVE_WITH_KNOTS ( ( 3, 2, 2, 2, 3 ),
 ( 0.3750000000000002776, 0.3791666666666669294, 0.3833333333333336368, 0.3875000000000003442, 0.3916666666666669960 ),
 .UNSPECIFIED. ) 
 CURVE ( )  GEOMETRIC_REPRESENTATION_ITEM ( )  RATIONAL_B_SPLINE_CURVE ( ( 0.9999999999999948930, 0.9238795325112918455, 1.000000000000000000, 0.9238795325112867385, 1.000000000000000000, 0.9238795325112867385, 1.000000000000000000, 0.9238795325112806323, 1.000000000000005995 ) ) 
 REPRESENTATION_ITEM ( '' )  );
#7302 = CARTESIAN_POINT ( 'NONE',  ( 4.458734125000001214, -75.89583333196775072, 2.574251347313718519 ) ) ;
#7303 = CARTESIAN_POINT ( 'NONE',  ( 4.458734125000001214, 24.10416666803226349, 2.574251347313718519 ) ) ;
#7304 = CARTESIAN_POINT ( 'NONE',  ( -4.999999999999998224, -53.91666666666667140, 2.886751345948131764 ) ) ;
#7305 = VERTEX_POINT ( 'NONE', #4764 ) ;
#7306 = CARTESIAN_POINT ( 'NONE',  ( -5.000000000000000888, -166.6875000027311842, -2.071067811865475949 ) ) ;
#7307 = CARTESIAN_POINT ( 'NONE',  ( -53.51423613279429503, -141.5000000013656063, 4.591703134518083651 ) ) ;
#7308 = CARTESIAN_POINT ( 'NONE',  ( -4.458734124999999437, -81.64583333196773651, -2.574251347313719407 ) ) ;
#7309 = CARTESIAN_POINT ( 'NONE',  ( -59.98410592259440222, -132.2500000027312126, -0.3983568153799752487 ) ) ;
#7310 = CARTESIAN_POINT ( 'NONE',  ( 1.975475456537005874E-15, -27.74999999999999645, 5.000000000000000000 ) ) ;
#7311 = CARTESIAN_POINT ( 'NONE',  ( 4.458734124999999437, -139.6875000013656063, 0.000000000000000000 ) ) ;
#7312 = CARTESIAN_POINT ( 'NONE',  ( 2.499999999999998668, -84.20833333060214443, -4.330127018922193649 ) ) ;
#7313 = CARTESIAN_POINT ( 'NONE',  ( -4.458734124999997661, -52.22916666530107932, 2.574251347313722516 ) ) ;
#7314 = CARTESIAN_POINT ( 'NONE',  ( 4.458734125000000326, -44.89583333196774362, 2.574251347313718519 ) ) ;
#7315 = AXIS2_PLACEMENT_3D ( 'NONE', #51495, #56326, #31542 ) ;
#7316 = CARTESIAN_POINT ( 'NONE',  ( 4.458734124999999437, 26.18750000136559564, -5.460374474430324690E-16 ) ) ;
#7317 = CARTESIAN_POINT ( 'NONE',  ( -5.000000000000000000, -105.0833333333333286, -2.886751345948128211 ) ) ;
#7318 =( BOUNDED_CURVE ( )  B_SPLINE_CURVE ( 2, ( #19474, #23991, #8573, #63238, #42979, #33023, #39088, #14018, #34261 ),
 .UNSPECIFIED., .F., .F. ) 
 B_SPLINE_CURVE_WITH_KNOTS ( ( 3, 2, 2, 2, 3 ),
 ( 0.3812499999999999778, 0.3819444444444444198, 0.3833333333333333592, 0.3847222222222222432, 0.3854166666666666852 ),
 .UNSPECIFIED. ) 
 CURVE ( )  GEOMETRIC_REPRESENTATION_ITEM ( )  RATIONAL_B_SPLINE_CURVE ( ( 0.9330127018922194093, 0.9330127018922194093, 1.000000000000000000, 0.8660254037844387076, 1.000000000000000000, 0.8660254037844387076, 1.000000000000000000, 0.9330127018922194093, 0.9330127018922194093 ) ) 
 REPRESENTATION_ITEM ( '' )  );
#7319 = CARTESIAN_POINT ( 'NONE',  ( 0.000000000000000000, -170.0000000000000000, 0.000000000000000000 ) ) ;
#7320 = CARTESIAN_POINT ( 'NONE',  ( -4.458734124999998549, -40.47916666530107221, 2.574251347313722516 ) ) ;
#7321 = CARTESIAN_POINT ( 'NONE',  ( -3.535250795749689387E-16, 1.875000002731185056, -5.773502691896257311 ) ) ;
#7322 = CARTESIAN_POINT ( 'NONE',  ( -59.98410592259440222, -154.1250000000000284, -0.3983568153799752487 ) ) ;
#7323 = CARTESIAN_POINT ( 'NONE',  ( -52.80376928212989185, -124.8750000013656205, -4.297418129356379346 ) ) ;
#7324 = CARTESIAN_POINT ( 'NONE',  ( 2.229367062500001939, -79.22916666530106511, 3.861377020970579999 ) ) ;
#7325 = CARTESIAN_POINT ( 'NONE',  ( -2.499999999999996447, 6.166666666666667851, 4.330127018922195425 ) ) ;
#7326 = CARTESIAN_POINT ( 'NONE',  ( -3.152548672688508926E-16, -100.5624999986344079, -5.148502694627439702 ) ) ;
#7327 = CARTESIAN_POINT ( 'NONE',  ( -3.152548672688508926E-16, -7.812499998634405252, -5.148502694627439702 ) ) ;
#7328 = ORIENTED_EDGE ( 'NONE', *, *, #60224, .T. ) ;
#7329 = CARTESIAN_POINT ( 'NONE',  ( 0.000000000000000000, -120.0000000000000000, 0.000000000000000000 ) ) ;
#7330 = CARTESIAN_POINT ( 'NONE',  ( 1.975475456537005874E-15, -35.62499999726880162, 5.000000000000000000 ) ) ;
#7331 = CARTESIAN_POINT ( 'NONE',  ( -4.458734124999999437, -93.31249999863440792, 0.000000000000000000 ) ) ;
#7332 = CARTESIAN_POINT ( 'NONE',  ( -5.000000000000000888, -167.6875000027311842, -2.071067811865475949 ) ) ;
#7333 = CARTESIAN_POINT ( 'NONE',  ( -2.229367062499996610, -87.39583333196773651, 3.861377020970582219 ) ) ;
#7334 = CARTESIAN_POINT ( 'NONE',  ( -3.152548672688508926E-16, 14.18750000136559386, -5.148502694627439702 ) ) ;
#7335 = LINE ( 'NONE', #56539, #62325 ) ;
#7336 = CARTESIAN_POINT ( 'NONE',  ( -57.19623071787017210, -133.3750000013656063, 4.297418129356382899 ) ) ;
#7337 = CARTESIAN_POINT ( 'NONE',  ( -3.152548672688508926E-16, -9.562499998634409692, -5.148502694627439702 ) ) ;
#7338 = CARTESIAN_POINT ( 'NONE',  ( -4.458734124999998549, 15.52083333469892779, 2.574251347313722516 ) ) ;
#7339 = CARTESIAN_POINT ( 'NONE',  ( 4.458734125000000326, -54.14583333196773651, 2.574251347313718519 ) ) ;
#7340 = CARTESIAN_POINT ( 'NONE',  ( 9.457646018065525792E-16, -85.06249999863440792, 5.148502694627439702 ) ) ;
#7341 = CARTESIAN_POINT ( 'NONE',  ( -2.229367062500000163, -10.47916666530106866, -3.861377020970580443 ) ) ;
#7342 = CARTESIAN_POINT ( 'NONE',  ( 2.500000000000002220, -84.66666666666667140, 4.330127018922192761 ) ) ;
#7343 = ORIENTED_EDGE ( 'NONE', *, *, #7055, .T. ) ;
#7344 = CARTESIAN_POINT ( 'NONE',  ( -3.152548672688508926E-16, -34.81249999863440792, -5.148502694627439702 ) ) ;
#7345 = CARTESIAN_POINT ( 'NONE',  ( -56.48576386720575471, -130.0000000013656063, -4.591703134518078322 ) ) ;
#7346 = CARTESIAN_POINT ( 'NONE',  ( 2.229367062499998831, -80.64583333196773651, -3.861377020970580887 ) ) ;
#7347 = CARTESIAN_POINT ( 'NONE',  ( 4.458734124999998549, 23.02083333469892423, -2.574251347313721627 ) ) ;
#7348 = EDGE_CURVE ( 'NONE', #32996, #25453, #13921, .T. ) ;
#7349 = CARTESIAN_POINT ( 'NONE',  ( 3.152801135295366208, -150.8125000013655779, 3.152801135295367985 ) ) ;
#7350 = CARTESIAN_POINT ( 'NONE',  ( -4.458734124999998549, 17.77083333469892779, 2.574251347313722516 ) ) ;
#7351 = CARTESIAN_POINT ( 'NONE',  ( -4.999999999999998224, -57.79166666393548013, 2.886751345948131764 ) ) ;
#7352 = CARTESIAN_POINT ( 'NONE',  ( 1.975475456537005874E-15, -25.62499999726881228, 5.000000000000000000 ) ) ;
#7353 = CARTESIAN_POINT ( 'NONE',  ( 2.229367062500001939, -84.22916666530107932, 3.861377020970579999 ) ) ;
#7354 = CARTESIAN_POINT ( 'NONE',  ( 2.500000000000002220, -62.66666666666666430, 4.330127018922192761 ) ) ;
#7355 = CARTESIAN_POINT ( 'NONE',  ( 2.500000000000002220, -72.54166666393548724, 4.330127018922192761 ) ) ;
#7356 = CARTESIAN_POINT ( 'NONE',  ( 2.499999999999998668, 18.79166666939785202, -4.330127018922193649 ) ) ;
#7357 = ORIENTED_EDGE ( 'NONE', *, *, #29069, .T. ) ;
#7358 = CARTESIAN_POINT ( 'NONE',  ( 5.000000000000000000, -147.1250000027312126, 0.000000000000000000 ) ) ;
#7359 = CARTESIAN_POINT ( 'NONE',  ( -2.499999999999996447, 28.16666666666666785, 4.330127018922195425 ) ) ;
#7361 = CARTESIAN_POINT ( 'NONE',  ( -5.000000000000000000, -21.08333333333333570, -2.886751345948128211 ) ) ;
#7360 = CARTESIAN_POINT ( 'NONE',  ( -5.000000000000000000, -106.9583333306021444, -2.886751345948128211 ) ) ;
#7362 = CARTESIAN_POINT ( 'NONE',  ( -4.458734124999999437, -27.39583333196773651, -2.574251347313719407 ) ) ;
#7363 = AXIS2_PLACEMENT_3D ( 'NONE', #32581, #8769, #52835 ) ;
#7364 = CARTESIAN_POINT ( 'NONE',  ( -4.458734124999997661, -87.22916666530107932, 2.574251347313722516 ) ) ;
#7365 = CARTESIAN_POINT ( 'NONE',  ( -2.500000000000000444, -27.04166666393548013, -4.330127018922193649 ) ) ;
#7367 = EDGE_LOOP ( 'NONE', ( #14906, #42399, #35386, #23747 ) ) ;
#7366 = CARTESIAN_POINT ( 'NONE',  ( 4.458734124999998549, -55.72916666530107221, -2.574251347313721627 ) ) ;
#7368 = CARTESIAN_POINT ( 'NONE',  ( -50.55543936806279248, -153.3125000013656063, 0.3552334253322060320 ) ) ;
#7370 = ORIENTED_EDGE ( 'NONE', *, *, #33473, .T. ) ;
#7369 = CARTESIAN_POINT ( 'NONE',  ( 9.457646018065525792E-16, -7.312499998634405252, 5.148502694627439702 ) ) ;
#7371 = CARTESIAN_POINT ( 'NONE',  ( -5.000000000000000000, -72.08333333333332860, -2.886751345948128211 ) ) ;
#7372 = CARTESIAN_POINT ( 'NONE',  ( -59.29741812935640155, -137.6250000013655779, -2.196230717870135685 ) ) ;
#7373 = CARTESIAN_POINT ( 'NONE',  ( -4.458734124999998549, -54.47916666530107932, 2.574251347313722516 ) ) ;
#7374 = CARTESIAN_POINT ( 'NONE',  ( 6.123233995736766282E-16, -170.0000000000000000, -5.000000000000000000 ) ) ;
#7375 =( BOUNDED_CURVE ( )  B_SPLINE_CURVE ( 2, ( #30155, #49145, #5091, #279, #35318, #29839, #20204, #5730, #29201 ),
 .UNSPECIFIED., .F., .F. ) 
 B_SPLINE_CURVE_WITH_KNOTS ( ( 3, 2, 2, 2, 3 ),
 ( 0.4696428571428571397, 0.4702380952380952328, 0.4714285714285714191, 0.4726190476190476053, 0.4732142857142856984 ),
 .UNSPECIFIED. ) 
 CURVE ( )  GEOMETRIC_REPRESENTATION_ITEM ( )  RATIONAL_B_SPLINE_CURVE ( ( 0.9330127018922194093, 0.9330127018922194093, 1.000000000000000000, 0.8660254037844387076, 1.000000000000000000, 0.8660254037844387076, 1.000000000000000000, 0.9330127018922194093, 0.9330127018922194093 ) ) 
 REPRESENTATION_ITEM ( '' )  );
#7376 = CARTESIAN_POINT ( 'NONE',  ( -5.000000000000000000, -77.95833333060214443, -2.886751345948128211 ) ) ;
#7377 = CARTESIAN_POINT ( 'NONE',  ( -55.39835681537999790, -150.8750000000000284, 4.984105922594378235 ) ) ;
#7378 = CARTESIAN_POINT ( 'NONE',  ( 2.229367062499998831, -16.89583333196773651, -3.861377020970580887 ) ) ;
#7379 = CARTESIAN_POINT ( 'NONE',  ( -2.229367062499996610, -50.39583333196772941, 3.861377020970582219 ) ) ;
#7380 = DIRECTION ( 'NONE',  ( 0.000000000000000000, 0.000000000000000000, 1.000000000000000000 ) ) ;
#7381 = FILL_AREA_STYLE ('',( #46291 ) ) ;
#7382 = CARTESIAN_POINT ( 'NONE',  ( -3.152801135295367096, -142.0625000013655779, -3.152801135295367541 ) ) ;
#7383 = CARTESIAN_POINT ( 'NONE',  ( -4.458734124999998549, -97.47916666530106511, 2.574251347313722516 ) ) ;
#7384 = DIRECTION ( 'NONE',  ( -0.000000000000000000, 1.000000000000000000, -0.000000000000000000 ) ) ;
#7385 = ORIENTED_EDGE ( 'NONE', *, *, #6790, .F. ) ;
#7386 = CARTESIAN_POINT ( 'NONE',  ( 0.000000000000000000, -170.0000000000000000, 0.000000000000000000 ) ) ;
#7387 = CARTESIAN_POINT ( 'NONE',  ( -50.01589407740564042, -142.7500000027312126, 0.3983568153799778022 ) ) ;
#7388 = CARTESIAN_POINT ( 'NONE',  ( 0.000000000000000000, -170.0000000000000000, 0.000000000000000000 ) ) ;
#7389 = CARTESIAN_POINT ( 'NONE',  ( 4.458734124999998549, -0.7291666653010709931, -2.574251347313721627 ) ) ;
#7390 = CARTESIAN_POINT ( 'NONE',  ( 9.457646018065525792E-16, -97.31249999863440792, 5.148502694627439702 ) ) ;
#7391 = CARTESIAN_POINT ( 'NONE',  ( -4.458734124999999437, -148.1875000013656063, -5.460374474430324690E-16 ) ) ;
#7392 = CARTESIAN_POINT ( 'NONE',  ( -2.229367062499996610, -25.39583333196773651, 3.861377020970582219 ) ) ;
#7393 = CARTESIAN_POINT ( 'NONE',  ( 1.339745962155612702, -46.29465819873851729, -5.000000000000000000 ) ) ;
#7394 = CARTESIAN_POINT ( 'NONE',  ( -59.59170313451811296, -136.5000000013656347, 1.485763867205729394 ) ) ;
#7395 = CARTESIAN_POINT ( 'NONE',  ( -4.458734124999999437, -62.64583333196774362, -2.574251347313719407 ) ) ;
#7396 = CARTESIAN_POINT ( 'NONE',  ( -5.000000000000000000, -154.6250000027311842, -6.123233995736766282E-16 ) ) ;
#7397 = CARTESIAN_POINT ( 'NONE',  ( 6.123233995736766282E-16, -170.0000000000000000, -5.000000000000000000 ) ) ;
#7398 = CARTESIAN_POINT ( 'NONE',  ( 4.458734124999997661, -143.5000000013655779, 1.846868145590737864 ) ) ;
#7399 = CARTESIAN_POINT ( 'NONE',  ( -4.458734124999997661, 8.520833334698926009, 2.574251347313722516 ) ) ;
#7400 = ORIENTED_EDGE ( 'NONE', *, *, #6641, .F. ) ;
#7401 = CARTESIAN_POINT ( 'NONE',  ( -1.339745962155613812, -81.20534180126146850, -5.000000000000000000 ) ) ;
#7402 = CARTESIAN_POINT ( 'NONE',  ( 5.000000000000000888, -66.45833333060213022, 2.886751345948126879 ) ) ;
#7404 = CARTESIAN_POINT ( 'NONE',  ( 2.229367062499998831, -23.64583333196773651, -3.861377020970580887 ) ) ;
#7403 = CARTESIAN_POINT ( 'NONE',  ( -3.535250795749689387E-16, -89.25000000000000000, -5.773502691896257311 ) ) ;
#7405 = CARTESIAN_POINT ( 'NONE',  ( -2.229367062499996610, -71.39583333196773651, 3.861377020970582219 ) ) ;
#7406 = CARTESIAN_POINT ( 'NONE',  ( -6.972266317189433020E-16, -7.249999999999998224, -5.000000000000000000 ) ) ;
#7407 = CARTESIAN_POINT ( 'NONE',  ( 5.000000000000000000, -76.37499999726880162, -6.123233995736766282E-16 ) ) ;
#7408 = CARTESIAN_POINT ( 'NONE',  ( -56.48576386720575471, -143.7500000013656063, -4.591703134518078322 ) ) ;
#7409 = CARTESIAN_POINT ( 'NONE',  ( 5.000000000000000888, -51.45833333060214443, 2.886751345948126879 ) ) ;
#7410 = CARTESIAN_POINT ( 'NONE',  ( 2.229367062499998831, 8.354166668032261711, -3.861377020970580887 ) ) ;
#7411 = CARTESIAN_POINT ( 'NONE',  ( 6.123233995736766282E-16, -170.0000000000000000, -5.000000000000000000 ) ) ;
#7412 = DIRECTION ( 'NONE',  ( -0.6485228581062915110, 0.000000000000000000, -0.7611951803011149931 ) ) ;
#7413 = CARTESIAN_POINT ( 'NONE',  ( -2.229367062499996610, 6.854166668032259935, 3.861377020970582219 ) ) ;
#7414 = CARTESIAN_POINT ( 'NONE',  ( -2.229367062499996610, -69.14583333196773651, 3.861377020970582219 ) ) ;
#7415 = CARTESIAN_POINT ( 'NONE',  ( -4.458734124999999437, -18.64583333196774362, -2.574251347313719407 ) ) ;
#7416 =( BOUNDED_CURVE ( )  B_SPLINE_CURVE ( 2, ( #12138, #17912, #52339, #8273, #3449, #23063, #42668, #46878, #18230 ),
 .UNSPECIFIED., .F., .F. ) 
 B_SPLINE_CURVE_WITH_KNOTS ( ( 3, 2, 2, 2, 3 ),
 ( 0.3812499999999999778, 0.3819444444444444198, 0.3833333333333333592, 0.3847222222222222432, 0.3854166666666666852 ),
 .UNSPECIFIED. ) 
 CURVE ( )  GEOMETRIC_REPRESENTATION_ITEM ( )  RATIONAL_B_SPLINE_CURVE ( ( 0.9330127018922194093, 0.9330127018922194093, 1.000000000000000000, 0.8660254037844387076, 1.000000000000000000, 0.8660254037844387076, 1.000000000000000000, 0.9330127018922194093, 0.9330127018922194093 ) ) 
 REPRESENTATION_ITEM ( '' )  );
#7417 = CARTESIAN_POINT ( 'NONE',  ( -3.535250795749689387E-16, 0.7500000000000007772, -5.773502691896257311 ) ) ;
#7418 = CARTESIAN_POINT ( 'NONE',  ( 3.152801135295366208, -160.5625000013656063, 3.152801135295367985 ) ) ;
#7419 = CARTESIAN_POINT ( 'NONE',  ( -6.972266317189433020E-16, -31.24999999999999645, -5.000000000000000000 ) ) ;
#7420 = CARTESIAN_POINT ( 'NONE',  ( 2.229367062499998831, -63.64583333196772941, -3.861377020970580887 ) ) ;
#7421 = CARTESIAN_POINT ( 'NONE',  ( -2.499999999999996447, -94.70833333060213022, 4.330127018922195425 ) ) ;
#7422 = ADVANCED_FACE ( 'NONE', ( #54938 ), #63640, .T. ) ;
#7423 = CARTESIAN_POINT ( 'NONE',  ( 6.123233995736766282E-16, -120.0000000000000000, -5.000000000000000000 ) ) ;
#7424 = CARTESIAN_POINT ( 'NONE',  ( 2.229367062500001939, -37.97916666530107221, 3.861377020970579999 ) ) ;
#7425 = CARTESIAN_POINT ( 'NONE',  ( -55.00000000000002132, -155.0000000000000284, 1.734723475976807094E-15 ) ) ;
#7426 = CARTESIAN_POINT ( 'NONE',  ( 2.229367062499998831, -65.89583333196773651, -3.861377020970580887 ) ) ;
#7427 = CARTESIAN_POINT ( 'NONE',  ( 5.000000000000000000, -48.50000000000000000, -6.123233995736766282E-16 ) ) ;
#7428 = CARTESIAN_POINT ( 'NONE',  ( -2.500000000000000444, 15.83333333333333037, -4.330127018922193649 ) ) ;
#7429 = VERTEX_POINT ( 'NONE', #54620 ) ;
#7430 = DIRECTION ( 'NONE',  ( 0.000000000000000000, 0.000000000000000000, 1.000000000000000000 ) ) ;
#7431 = CARTESIAN_POINT ( 'NONE',  ( -4.458734124999998549, -2.479166665301069550, 2.574251347313722516 ) ) ;
#7432 = CARTESIAN_POINT ( 'NONE',  ( -9.184850993605147944E-16, -144.3750000027312126, 5.000000000000000000 ) ) ;
#7433 = CARTESIAN_POINT ( 'NONE',  ( 5.000000000000000888, -6.583333333333329485, 2.886751345948126879 ) ) ;
#7434 = CARTESIAN_POINT ( 'NONE',  ( -2.229367062499996610, -71.14583333196773651, 3.861377020970582219 ) ) ;
#7435 = CARTESIAN_POINT ( 'NONE',  ( 0.000000000000000000, -120.0000000000000000, 0.000000000000000000 ) ) ;
#7436 = EDGE_CURVE ( 'NONE', #38838, #51005, #27080, .T. ) ;
#7437 = CARTESIAN_POINT ( 'NONE',  ( -5.000000000000000000, -11.95833333060214976, -2.886751345948128211 ) ) ;
#7439 = VERTEX_POINT ( 'NONE', #40766 ) ;
#7438 = CARTESIAN_POINT ( 'NONE',  ( 2.229367062499998831, -38.64583333196773651, -3.861377020970580887 ) ) ;
#7440 = FACE_OUTER_BOUND ( 'NONE', #1102, .T. ) ;
#7441 = ADVANCED_FACE ( 'NONE', ( #31428 ), #2500, .T. ) ;
#7443 = VERTEX_POINT ( 'NONE', #26293 ) ;
#7442 = CARTESIAN_POINT ( 'NONE',  ( -3.152548672688508926E-16, 10.18750000136559564, -5.148502694627439702 ) ) ;
#7444 = CARTESIAN_POINT ( 'NONE',  ( 1.339745962155612702, -81.29465819873850307, -5.000000000000000000 ) ) ;
#7445 = CARTESIAN_POINT ( 'NONE',  ( 5.000000000000000000, -53.49999999999999289, -6.123233995736766282E-16 ) ) ;
#7446 = CARTESIAN_POINT ( 'NONE',  ( -4.458734124999999437, -161.1875000013655779, -5.460374474430324690E-16 ) ) ;
#7447 = CARTESIAN_POINT ( 'NONE',  ( 4.458734124999999437, -37.06249999863440792, -5.460374474430324690E-16 ) ) ;
#7448 = CARTESIAN_POINT ( 'NONE',  ( 5.000000000000000888, -144.9375000000000000, -2.071067811865475505 ) ) ;
#7449 = CARTESIAN_POINT ( 'NONE',  ( 4.458734125000001214, -78.89583333196772230, 2.574251347313718519 ) ) ;
#7450 = CARTESIAN_POINT ( 'NONE',  ( -9.184850993605147944E-16, -165.2500000000000000, 5.000000000000000000 ) ) ;
#7451 = CARTESIAN_POINT ( 'NONE',  ( 2.229367062499998831, -87.64583333196773651, -3.861377020970580887 ) ) ;
#7452 = CARTESIAN_POINT ( 'NONE',  ( -53.51423613279429503, -133.5000000013656347, 4.591703134518082763 ) ) ;
#7453 = CARTESIAN_POINT ( 'NONE',  ( -2.229367062499996610, 0.6041666680322611560, 3.861377020970582219 ) ) ;
#7454 = ADVANCED_FACE ( 'NONE', ( #6378 ), #16650, .T. ) ;
#7455 = CARTESIAN_POINT ( 'NONE',  ( 2.229367062500001939, -33.22916666530106511, 3.861377020970579999 ) ) ;
#7456 = CARTESIAN_POINT ( 'NONE',  ( 1.975475456537005874E-15, -72.75000000000000000, 5.000000000000000000 ) ) ;
#7457 = CARTESIAN_POINT ( 'NONE',  ( 9.457646018065525792E-16, -77.31249999863440792, 5.148502694627439702 ) ) ;
#7458 = CARTESIAN_POINT ( 'NONE',  ( 1.975475456537005874E-15, -86.75000000000001421, 5.000000000000000000 ) ) ;
#7459 = ORIENTED_EDGE ( 'NONE', *, *, #34461, .F. ) ;
#7460 = CARTESIAN_POINT ( 'NONE',  ( -58.24261429053147765, -153.3750000027312126, -3.805975901505573855 ) ) ;
#7461 = FACE_OUTER_BOUND ( 'NONE', #2999, .T. ) ;
#7462 = CARTESIAN_POINT ( 'NONE',  ( -2.229367062500000163, -71.72916666530107932, -3.861377020970580443 ) ) ;
#7463 = CARTESIAN_POINT ( 'NONE',  ( 9.457646018065525792E-16, -7.312499998634405252, 5.148502694627439702 ) ) ;
#7464 = VERTEX_POINT ( 'NONE', #41710 ) ;
#7465 = ADVANCED_FACE ( 'NONE', ( #55898 ), #30806, .T. ) ;
#7466 = CARTESIAN_POINT ( 'NONE',  ( 4.458734124999998549, -8.979166665301073991, -2.574251347313721627 ) ) ;
#7467 = DIRECTION ( 'NONE',  ( 0.000000000000000000, -0.000000000000000000, 1.000000000000000000 ) ) ;
#7468 = CARTESIAN_POINT ( 'NONE',  ( 4.458734124999998549, 10.27083333469892779, -2.574251347313721627 ) ) ;
#7469 = LINE ( 'NONE', #47018, #56261 ) ;
#7470 = CARTESIAN_POINT ( 'NONE',  ( -3.152801135295367096, -157.0625000013656063, -3.152801135295367541 ) ) ;
#7471 = CARTESIAN_POINT ( 'NONE',  ( -2.229367062500000163, 26.27083333469892779, -3.861377020970580443 ) ) ;
#7472 = ORIENTED_EDGE ( 'NONE', *, *, #43238, .T. ) ;
#7473 = CARTESIAN_POINT ( 'NONE',  ( -3.152548672688508926E-16, -85.56249999863439371, -5.148502694627439702 ) ) ;
#7474 = CARTESIAN_POINT ( 'NONE',  ( 4.458734125000001214, -8.895833331967736513, 2.574251347313718519 ) ) ;
#7475 = CARTESIAN_POINT ( 'NONE',  ( 5.000000000000000000, -140.0625000000000000, 2.071067811865478614 ) ) ;
#7476 = CARTESIAN_POINT ( 'NONE',  ( -4.999999999999999112, -32.79166666393547303, 2.886751345948131764 ) ) ;
#7477 = DIRECTION ( 'NONE',  ( -0.000000000000000000, 0.000000000000000000, -1.000000000000000000 ) ) ;
#7478 = CARTESIAN_POINT ( 'NONE',  ( -4.458734124999999437, 23.68750000136559564, 0.000000000000000000 ) ) ;
#7479 = CARTESIAN_POINT ( 'NONE',  ( 5.000000000000000000, -7.416666666666667851, -2.886751345948130876 ) ) ;
#7480 = CARTESIAN_POINT ( 'NONE',  ( -4.458734124999999437, 24.60416666803225993, -2.574251347313719407 ) ) ;
#7481 = CARTESIAN_POINT ( 'NONE',  ( -4.458734124999998549, -51.22916666530107221, 2.574251347313722516 ) ) ;
#7482 = CARTESIAN_POINT ( 'NONE',  ( 4.458734124999998549, -35.97916666530107221, -2.574251347313721627 ) ) ;
#7483 = CARTESIAN_POINT ( 'NONE',  ( 2.229367062499998831, -3.895833331967739177, -3.861377020970580887 ) ) ;
#7484 = CARTESIAN_POINT ( 'NONE',  ( 5.000000000000000000, -0.2916666639354824619, -2.886751345948130876 ) ) ;
#7485 = CARTESIAN_POINT ( 'NONE',  ( 1.060575238724906964E-15, 16.25000000000000000, 5.773502691896257311 ) ) ;
#7486 = CARTESIAN_POINT ( 'NONE',  ( 5.000000000000000000, -141.1875000027312126, 2.071067811865478614 ) ) ;
#7487 = CARTESIAN_POINT ( 'NONE',  ( 2.499999999999998668, -33.20833333060215153, -4.330127018922193649 ) ) ;
#7488 = CARTESIAN_POINT ( 'NONE',  ( 9.457646018065525792E-16, -47.06249999863440792, 5.148502694627439702 ) ) ;
#7489 = CARTESIAN_POINT ( 'NONE',  ( -3.535250795749689387E-16, -76.12499999726881583, -5.773502691896257311 ) ) ;
#7490 = EDGE_CURVE ( 'NONE', #20484, #35996, #24622, .T. ) ;
#7491 = CARTESIAN_POINT ( 'NONE',  ( -57.19623071787017210, -138.6250000013655779, 4.297418129356382899 ) ) ;
#7492 =( BOUNDED_CURVE ( )  B_SPLINE_CURVE ( 2, ( #22897, #56039, #38305, #23828, #23195, #28951, #9337, #8414, #3899 ),
 .UNSPECIFIED., .F., .F. ) 
 B_SPLINE_CURVE_WITH_KNOTS ( ( 3, 2, 2, 2, 3 ),
 ( 0.1083333333333334203, 0.1125000000000000999, 0.1166666666666667657, 0.1208333333333334314, 0.1250000000000001110 ),
 .UNSPECIFIED. ) 
 CURVE ( )  GEOMETRIC_REPRESENTATION_ITEM ( )  RATIONAL_B_SPLINE_CURVE ( ( 0.9999999999999984457, 0.9238795325112882928, 1.000000000000000000, 0.9238795325112867385, 1.000000000000000000, 0.9238795325112867385, 1.000000000000000000, 0.9238795325112847401, 1.000000000000001998 ) ) 
 REPRESENTATION_ITEM ( '' )  );
#7493 = CARTESIAN_POINT ( 'NONE',  ( -5.000000000000000000, -87.08333333333331439, -2.886751345948128211 ) ) ;
#7494 = ADVANCED_FACE ( 'NONE', ( #25984 ), #33644, .T. ) ;
#7495 = CARTESIAN_POINT ( 'NONE',  ( -2.499999999999996447, -63.70833333060215153, 4.330127018922195425 ) ) ;
#7496 = EDGE_CURVE ( 'NONE', #20545, #11671, #31207, .T. ) ;
#7497 = CARTESIAN_POINT ( 'NONE',  ( 4.458734125000000326, -83.14583333196773651, 2.574251347313718519 ) ) ;
#7498 = CARTESIAN_POINT ( 'NONE',  ( 1.846868145590735200, -163.5000000013655779, -4.458734124999999437 ) ) ;
#7499 = CARTESIAN_POINT ( 'NONE',  ( 5.000000000000000000, -35.41666666666667140, -2.886751345948129988 ) ) ;
#7500 = CARTESIAN_POINT ( 'NONE',  ( -5.000000000000000888, -147.4375000000000000, 2.071067811865474617 ) ) ;
#7501 = ORIENTED_EDGE ( 'NONE', *, *, #29899, .F. ) ;
#7502 = CARTESIAN_POINT ( 'NONE',  ( 2.229367062500001939, 17.77083333469892779, 3.861377020970579999 ) ) ;
#7503 = ORIENTED_EDGE ( 'NONE', *, *, #45964, .F. ) ;
#7504 = CARTESIAN_POINT ( 'NONE',  ( -4.458734124999998549, -91.22916666530106511, 2.574251347313722516 ) ) ;
#7505 = CARTESIAN_POINT ( 'NONE',  ( -3.152548672688508926E-16, 15.18750000136559386, -5.148502694627439702 ) ) ;
#7506 = CARTESIAN_POINT ( 'NONE',  ( 5.000000000000000888, 16.54166666939785202, 2.886751345948126879 ) ) ;
#7507 = CARTESIAN_POINT ( 'NONE',  ( -6.972266317189433020E-16, -35.12499999726880873, -5.000000000000000000 ) ) ;
#7508 = CARTESIAN_POINT ( 'NONE',  ( 1.060575238724906964E-15, 7.249999999999999112, 5.773502691896257311 ) ) ;
#7509 = ADVANCED_FACE ( 'NONE', ( #55751 ), #49960, .F. ) ;
#7510 = CARTESIAN_POINT ( 'NONE',  ( 2.229367062500001939, -56.97916666530107932, 3.861377020970579999 ) ) ;
#7511 = CARTESIAN_POINT ( 'NONE',  ( -5.000000000000000000, 15.12500000273118417, 0.000000000000000000 ) ) ;
#7512 = CARTESIAN_POINT ( 'NONE',  ( 1.975475456537005874E-15, -45.62499999726880873, 5.000000000000000000 ) ) ;
#7513 = CARTESIAN_POINT ( 'NONE',  ( -1.339745962155613812, -38.08034179853029144, -5.000000000000000000 ) ) ;
#7514 = CARTESIAN_POINT ( 'NONE',  ( -6.972266317189433020E-16, -26.12499999726881583, -5.000000000000000000 ) ) ;
#7515 = EDGE_CURVE ( 'NONE', #8991, #14704, #1422, .T. ) ;
#7516 = DIRECTION ( 'NONE',  ( -0.000000000000000000, 1.000000000000000000, -0.000000000000000000 ) ) ;
#7517 = CARTESIAN_POINT ( 'NONE',  ( -4.999999999999999112, -38.91666666666667140, 2.886751345948131764 ) ) ;
#7518 = CARTESIAN_POINT ( 'NONE',  ( -6.972266317189433020E-16, 12.87500000273118417, -5.000000000000000000 ) ) ;
#7520 = CARTESIAN_POINT ( 'NONE',  ( -2.229367062500000163, -21.72916666530107221, -3.861377020970580443 ) ) ;
#7519 = CARTESIAN_POINT ( 'NONE',  ( 1.975475456537005874E-15, -47.74999999999999289, 5.000000000000000000 ) ) ;
#7521 = DIRECTION ( 'NONE',  ( 1.000000000000000000, 0.000000000000000000, -0.000000000000000000 ) ) ;
#7522 = CARTESIAN_POINT ( 'NONE',  ( -2.229367062499996610, -67.14583333196773651, 3.861377020970582219 ) ) ;
#7523 = CARTESIAN_POINT ( 'NONE',  ( 2.730187237215162345E-16, -151.4375000013656063, -4.458734124999999437 ) ) ;
#7524 = CARTESIAN_POINT ( 'NONE',  ( 4.458734124999998549, -68.72916666530106511, -2.574251347313721627 ) ) ;
#7525 = CARTESIAN_POINT ( 'NONE',  ( -52.10840900171896806, -148.4375000013656063, 3.393966926194110556 ) ) ;
#7526 = CARTESIAN_POINT ( 'NONE',  ( -3.152548672688508926E-16, -19.81249999863440436, -5.148502694627439702 ) ) ;
#7527 = CARTESIAN_POINT ( 'NONE',  ( -3.535250795749689387E-16, -62.12499999726880873, -5.773502691896257311 ) ) ;
#7528 = VERTEX_POINT ( 'NONE', #21973 ) ;
#7529 = CARTESIAN_POINT ( 'NONE',  ( -1.339745962155613812, -49.20534180126148271, -5.000000000000000000 ) ) ;
#7530 = ORIENTED_EDGE ( 'NONE', *, *, #27611, .T. ) ;
#7531 = CARTESIAN_POINT ( 'NONE',  ( -4.458734124999999437, -62.56249999863440792, 0.000000000000000000 ) ) ;
#7532 = CARTESIAN_POINT ( 'NONE',  ( 5.000000000000000000, -149.1875000027312410, 2.071067811865478614 ) ) ;
#7533 = CARTESIAN_POINT ( 'NONE',  ( -1.846868145590737420, -153.7500000013656063, 4.458734124999999437 ) ) ;
#7534 = ORIENTED_EDGE ( 'NONE', *, *, #56397, .T. ) ;
#7535 = LINE ( 'NONE', #43736, #59097 ) ;
#7536 = CARTESIAN_POINT ( 'NONE',  ( -59.81910112700025905, -125.1875000000000284, -2.462841084822630311 ) ) ;
#7537 = CARTESIAN_POINT ( 'NONE',  ( -2.500000000000000444, -75.04166666393547303, -4.330127018922193649 ) ) ;
#7538 = CARTESIAN_POINT ( 'NONE',  ( -3.152548672688508926E-16, -55.81249999863440081, -5.148502694627439702 ) ) ;
#7539 = ORIENTED_EDGE ( 'NONE', *, *, #27180, .T. ) ;
#7540 = CYLINDRICAL_SURFACE ( 'NONE', #55243, 5.000000000000000000 ) ;
#7541 = CARTESIAN_POINT ( 'NONE',  ( -4.458734124999998549, 6.770833334698928674, 2.574251347313722516 ) ) ;
#7542 =( BOUNDED_CURVE ( )  B_SPLINE_CURVE ( 2, ( #49728, #53913, #58743, #9839, #14670, #5673, #48763, #49084, #536 ),
 .UNSPECIFIED., .F., .F. ) 
 B_SPLINE_CURVE_WITH_KNOTS ( ( 3, 2, 2, 2, 3 ),
 ( 0.2160714285714285809, 0.2166666666666666741, 0.2178571428571428603, 0.2190476190476190466, 0.2196428571428571397 ),
 .UNSPECIFIED. ) 
 CURVE ( )  GEOMETRIC_REPRESENTATION_ITEM ( )  RATIONAL_B_SPLINE_CURVE ( ( 0.9330127018922194093, 0.9330127018922194093, 1.000000000000000000, 0.8660254037844387076, 1.000000000000000000, 0.8660254037844387076, 1.000000000000000000, 0.9330127018922194093, 0.9330127018922194093 ) ) 
 REPRESENTATION_ITEM ( '' )  );
#7543 = CARTESIAN_POINT ( 'NONE',  ( -3.152548672688508926E-16, 21.43750000136559564, -5.148502694627439702 ) ) ;
#7544 = CARTESIAN_POINT ( 'NONE',  ( -58.39396692619412477, -147.4375000013656063, 2.891590998281057701 ) ) ;
#7545 = CARTESIAN_POINT ( 'NONE',  ( 2.500000000000002220, -77.66666666666665719, 4.330127018922192761 ) ) ;
#7546 = CARTESIAN_POINT ( 'NONE',  ( -1.846868145590737420, -167.7500000013655779, 4.458734124999997661 ) ) ;
#7547 = ORIENTED_EDGE ( 'NONE', *, *, #25532, .T. ) ;
#7548 = CARTESIAN_POINT ( 'NONE',  ( 2.229367062499998831, -68.64583333196773651, -3.861377020970580887 ) ) ;
#7549 = CARTESIAN_POINT ( 'NONE',  ( 2.499999999999998668, 14.79166666939785202, -4.330127018922193649 ) ) ;
#7550 = CARTESIAN_POINT ( 'NONE',  ( -4.458734124999999437, 14.68750000136559386, 0.000000000000000000 ) ) ;
#7551 = AXIS2_PLACEMENT_3D ( 'NONE', #61178, #17101, #36085 ) ;
#7552 = CARTESIAN_POINT ( 'NONE',  ( 0.000000000000000000, -170.0000000000000000, 0.000000000000000000 ) ) ;
#7553 = CARTESIAN_POINT ( 'NONE',  ( 2.229367062500001939, -56.22916666530107221, 3.861377020970579999 ) ) ;
#7554 = CARTESIAN_POINT ( 'NONE',  ( 2.499999999999998668, -16.20833333060214443, -4.330127018922193649 ) ) ;
#7555 = CARTESIAN_POINT ( 'NONE',  ( -5.000000000000000000, -100.0833333333333144, -2.886751345948128211 ) ) ;
#7556 = CARTESIAN_POINT ( 'NONE',  ( 2.071067811865370256, -160.8125000000000284, -5.000000000000105693 ) ) ;
#7557 = CARTESIAN_POINT ( 'NONE',  ( -4.769696007084728073, -120.0000000000000000, -1.500000000000000000 ) ) ;
#7558 = CARTESIAN_POINT ( 'NONE',  ( 4.458734125000001214, -33.89583333196773651, 2.574251347313718519 ) ) ;
#7559 = CARTESIAN_POINT ( 'NONE',  ( 4.458734124999998549, -22.97916666530107221, -2.574251347313721627 ) ) ;
#7560 = VERTEX_POINT ( 'NONE', #6543 ) ;
#7561 = CARTESIAN_POINT ( 'NONE',  ( 1.975475456537005874E-15, -26.62499999726881228, 5.000000000000000000 ) ) ;
#7562 = CARTESIAN_POINT ( 'NONE',  ( 9.457646018065525792E-16, -110.0624999986343795, 5.148502694627439702 ) ) ;
#7563 = CARTESIAN_POINT ( 'NONE',  ( -3.535533905932737309, -154.7500000027312126, -3.535533905932738197 ) ) ;
#7564 = ORIENTED_EDGE ( 'NONE', *, *, #48070, .F. ) ;
#7565 = CARTESIAN_POINT ( 'NONE',  ( -4.458734124999998549, -101.4791666653010651, 2.574251347313722516 ) ) ;
#7566 = CARTESIAN_POINT ( 'NONE',  ( -3.152548672688508926E-16, -28.56249999863440436, -5.148502694627439702 ) ) ;
#7567 = CARTESIAN_POINT ( 'NONE',  ( -4.999999999999999112, -62.79166666393546592, 2.886751345948131764 ) ) ;
#7568 = CARTESIAN_POINT ( 'NONE',  ( -51.60603307380591787, -153.1875000013656063, -2.891590998281053704 ) ) ;
#7569 = CARTESIAN_POINT ( 'NONE',  ( -3.535533905932738641, -148.3750000000000000, 3.535533905932737309 ) ) ;
#7570 = EDGE_CURVE ( 'NONE', #39600, #9299, #35724, .T. ) ;
#7571 = CARTESIAN_POINT ( 'NONE',  ( 2.229367062499998831, -26.64583333196774007, -3.861377020970580887 ) ) ;
#7572 = CARTESIAN_POINT ( 'NONE',  ( -3.152548672688508926E-16, -68.81249999863439371, -5.148502694627439702 ) ) ;
#7573 = CARTESIAN_POINT ( 'NONE',  ( 1.975475456537005874E-15, 8.249999999999998224, 5.000000000000000000 ) ) ;
#7574 = CARTESIAN_POINT ( 'NONE',  ( 4.458734125000000326, -23.89583333196773651, 2.574251347313718519 ) ) ;
#7575 = CARTESIAN_POINT ( 'NONE',  ( -6.972266317189433020E-16, -32.12499999726880873, -5.000000000000000000 ) ) ;
#7576 = CARTESIAN_POINT ( 'NONE',  ( -58.80597590150559739, -138.1250000027312410, 3.242614290531460330 ) ) ;
#7577 = CARTESIAN_POINT ( 'NONE',  ( 1.060575238724906964E-15, -16.75000000000000355, 5.773502691896257311 ) ) ;
#7578 = CARTESIAN_POINT ( 'NONE',  ( -3.152801135295367096, -152.0625000013655779, -3.152801135295367541 ) ) ;
#7579 = ORIENTED_EDGE ( 'NONE', *, *, #51779, .T. ) ;
#7580 = CYLINDRICAL_SURFACE ( 'NONE', #7079, 5.000000000000000000 ) ;
#7581 = CARTESIAN_POINT ( 'NONE',  ( -2.229367062500000163, -49.72916666530107221, -3.861377020970580443 ) ) ;
#7582 = ADVANCED_FACE ( 'NONE', ( #3935 ), #42210, .T. ) ;
#7583 = CARTESIAN_POINT ( 'NONE',  ( -5.000000000000000000, -86.87499999726880162, 0.000000000000000000 ) ) ;
#7584 = CARTESIAN_POINT ( 'NONE',  ( 0.000000000000000000, -120.0000000000000000, 0.000000000000000000 ) ) ;
#7585 = CARTESIAN_POINT ( 'NONE',  ( -5.000000000000000000, 22.00000000000000000, 0.000000000000000000 ) ) ;
#7586 = MANIFOLD_SOLID_BREP ( 'Thread2', #31553 ) ;
#7587 = EDGE_CURVE ( 'NONE', #58058, #25203, #37796, .T. ) ;
#7588 = EDGE_CURVE ( 'NONE', #51364, #24132, #31586, .T. ) ;
#7589 = CARTESIAN_POINT ( 'NONE',  ( 0.000000000000000000, -170.0000000000000000, 5.000000000000000000 ) ) ;
#7590 = CARTESIAN_POINT ( 'NONE',  ( 4.458734124999998549, 1.270833334698927342, -2.574251347313721627 ) ) ;
#7591 = CARTESIAN_POINT ( 'NONE',  ( -2.071067811865559882, -160.8125000027312126, -4.999999999999914735 ) ) ;
#7592 = CARTESIAN_POINT ( 'NONE',  ( -2.500000000000000444, -81.04166666393547303, -4.330127018922193649 ) ) ;
#7593 = DIRECTION ( 'NONE',  ( -0.6485228581062915110, 0.000000000000000000, -0.7611951803011149931 ) ) ;
#7594 = CARTESIAN_POINT ( 'NONE',  ( -4.458734124999999437, 15.35416666803225993, -2.574251347313719407 ) ) ;
#7595 = CARTESIAN_POINT ( 'NONE',  ( -2.499999999999996447, 3.291666669397851575, 4.330127018922195425 ) ) ;
#7597 = EDGE_LOOP ( 'NONE', ( #55390, #56950, #21620, #62267 ) ) ;
#7596 = ADVANCED_FACE ( 'NONE', ( #62792 ), #18404, .T. ) ;
#7598 = CARTESIAN_POINT ( 'NONE',  ( -7.500000000000000000, -4.330127018922199866, -1.000000000000000888 ) ) ;
#7599 = ORIENTED_EDGE ( 'NONE', *, *, #21436, .T. ) ;
#7600 =( BOUNDED_CURVE ( )  B_SPLINE_CURVE ( 2, ( #34406, #9973, #53722, #662, #35069, #59841, #54686, #63389, #20601 ),
 .UNSPECIFIED., .F., .F. ) 
 B_SPLINE_CURVE_WITH_KNOTS ( ( 3, 2, 2, 2, 3 ),
 ( 0.8520833333333333037, 0.8527777777777777457, 0.8541666666666666297, 0.8555555555555555136, 0.8562499999999999556 ),
 .UNSPECIFIED. ) 
 CURVE ( )  GEOMETRIC_REPRESENTATION_ITEM ( )  RATIONAL_B_SPLINE_CURVE ( ( 0.9330127018922194093, 0.9330127018922194093, 1.000000000000000000, 0.8660254037844387076, 1.000000000000000000, 0.8660254037844387076, 1.000000000000000000, 0.9330127018922194093, 0.9330127018922194093 ) ) 
 REPRESENTATION_ITEM ( '' )  );
#7601 = CARTESIAN_POINT ( 'NONE',  ( -2.229367062500000163, -46.47916666530106511, -3.861377020970580443 ) ) ;
#7602 = ADVANCED_FACE ( 'NONE', ( #27112 ), #47981, .T. ) ;
#7603 = CARTESIAN_POINT ( 'NONE',  ( 3.152801135295366208, -162.8125000013656063, 3.152801135295367985 ) ) ;
#7604 = AXIS2_PLACEMENT_3D ( 'NONE', #9971, #34740, #45349 ) ;
#7605 = EDGE_CURVE ( 'NONE', #37393, #59890, #22963, .T. ) ;
#7606 = CARTESIAN_POINT ( 'NONE',  ( 2.499999999999998668, -43.20833333060214443, -4.330127018922193649 ) ) ;
#7607 = VERTEX_POINT ( 'NONE', #39586 ) ;
#7608 = CARTESIAN_POINT ( 'NONE',  ( -4.458734124999999437, -24.31249999863440436, 0.000000000000000000 ) ) ;
#7609 = EDGE_LOOP ( 'NONE', ( #34633, #61310, #4342, #27176 ) ) ;
#7610 = CARTESIAN_POINT ( 'NONE',  ( 1.060575238724906964E-15, -85.74999999999998579, 5.773502691896257311 ) ) ;
#7611 = CARTESIAN_POINT ( 'NONE',  ( 2.730187237215162345E-16, -164.1875000013655779, -4.458734124999999437 ) ) ;
#7612 = CARTESIAN_POINT ( 'NONE',  ( -4.999999999999998224, -50.79166666393547303, 2.886751345948131764 ) ) ;
#7613 = CARTESIAN_POINT ( 'NONE',  ( -59.81910112700025905, -139.1874999999999716, -2.462841084822630311 ) ) ;
#7614 = CARTESIAN_POINT ( 'NONE',  ( 9.457646018065525792E-16, -33.31249999863440792, 5.148502694627439702 ) ) ;
#7615 = CARTESIAN_POINT ( 'NONE',  ( -9.184850993605147944E-16, -147.3750000027312126, 5.000000000000000000 ) ) ;
#7616 = VERTEX_POINT ( 'NONE', #59223 ) ;
#7617 = CARTESIAN_POINT ( 'NONE',  ( -2.229367062499996610, -77.14583333196773651, 3.861377020970582219 ) ) ;
#7618 = CARTESIAN_POINT ( 'NONE',  ( -3.152548672688508926E-16, 22.43750000136559208, -5.148502694627439702 ) ) ;
#7619 = CARTESIAN_POINT ( 'NONE',  ( -2.500000000000000444, -29.04166666393548013, -4.330127018922193649 ) ) ;
#7620 = ORIENTED_EDGE ( 'NONE', *, *, #10529, .T. ) ;
#7621 = CARTESIAN_POINT ( 'NONE',  ( 1.339745962155615144, 14.29465819873852084, 4.999999999999999112 ) ) ;
#7622 = CARTESIAN_POINT ( 'NONE',  ( -50.55543936806279248, -141.3125000013656063, 0.3552334253322060320 ) ) ;
#7623 = CARTESIAN_POINT ( 'NONE',  ( 2.229367062499998831, -78.89583333196773651, -3.861377020970580887 ) ) ;
#7624 = CARTESIAN_POINT ( 'NONE',  ( -49.85088928181150436, -130.6875000027312410, -1.666127454062680702 ) ) ;
#7625 = PLANE ( 'NONE',  #49014 ) ;
#7626 = CARTESIAN_POINT ( 'NONE',  ( -5.000000000000000000, -158.6250000027311842, -6.123233995736766282E-16 ) ) ;
#7627 = CARTESIAN_POINT ( 'NONE',  ( 5.000000000000000000, 20.58333333333333215, -2.886751345948130876 ) ) ;
#7628 = CARTESIAN_POINT ( 'NONE',  ( -2.229367062500000163, -55.47916666530107221, -3.861377020970580443 ) ) ;
#7629 = CARTESIAN_POINT ( 'NONE',  ( 9.457646018065525792E-16, -48.06249999863440792, 5.148502694627439702 ) ) ;
#7630 = CARTESIAN_POINT ( 'NONE',  ( -1.339745962155623360, 21.20534180126147561, 4.999999999999991118 ) ) ;
#7631 = CARTESIAN_POINT ( 'NONE',  ( -5.000000000000000000, -108.9999999999999858, 0.000000000000000000 ) ) ;
#7632 = CARTESIAN_POINT ( 'NONE',  ( -1.339745962155636017, 4.205341801261478274, 4.999999999999985789 ) ) ;
#7633 = CARTESIAN_POINT ( 'NONE',  ( 2.229367062500001939, -39.22916666530107221, 3.861377020970579999 ) ) ;
#7634 = CARTESIAN_POINT ( 'NONE',  ( -2.499999999999996447, 2.291666669397850686, 4.330127018922195425 ) ) ;
#7635 = CARTESIAN_POINT ( 'NONE',  ( 6.123233995736766282E-16, -170.0000000000000000, -5.000000000000000000 ) ) ;
#7636 = CARTESIAN_POINT ( 'NONE',  ( -52.80376928212989185, -125.8750000013656063, -4.297418129356379346 ) ) ;
#7637 = CARTESIAN_POINT ( 'NONE',  ( -3.152548672688508926E-16, -78.81249999863440792, -5.148502694627439702 ) ) ;
#7638 = FACE_OUTER_BOUND ( 'NONE', #18358, .T. ) ;
#7639 = CARTESIAN_POINT ( 'NONE',  ( 4.458734125000000326, -101.8958333319677365, 2.574251347313718519 ) ) ;
#7640 = CARTESIAN_POINT ( 'NONE',  ( 4.458734124999999437, -3.062499998634407472, -5.460374474430324690E-16 ) ) ;
#7641 = VERTEX_POINT ( 'NONE', #33514 ) ;
#7642 = CARTESIAN_POINT ( 'NONE',  ( -51.75738570946856498, -139.8750000027312126, 3.805975901505576964 ) ) ;
#7643 = CARTESIAN_POINT ( 'NONE',  ( -2.229367062499996610, -92.14583333196773651, 3.861377020970582219 ) ) ;
#7644 = DIRECTION ( 'NONE',  ( 0.000000000000000000, 0.000000000000000000, 1.000000000000000000 ) ) ;
#7645 = CARTESIAN_POINT ( 'NONE',  ( 2.229367062500001939, -84.22916666530107932, 3.861377020970579999 ) ) ;
#7646 = CARTESIAN_POINT ( 'NONE',  ( 4.458734124999999437, 14.93750000136559386, -5.460374474430324690E-16 ) ) ;
#7647 = DIRECTION ( 'NONE',  ( 0.000000000000000000, 1.000000000000000000, 0.000000000000000000 ) ) ;
#7648 = AXIS2_PLACEMENT_3D ( 'NONE', #10110, #15256, #40334 ) ;
#7649 = CARTESIAN_POINT ( 'NONE',  ( -57.89159099828107458, -134.6875000013656063, -3.393966926194107447 ) ) ;
#7650 = CARTESIAN_POINT ( 'NONE',  ( 9.457646018065525792E-16, -11.06249999863440969, 5.148502694627439702 ) ) ;
#7651 = CARTESIAN_POINT ( 'NONE',  ( 9.457646018065525792E-16, 15.68750000136559386, 5.148502694627439702 ) ) ;
#7652 = CARTESIAN_POINT ( 'NONE',  ( 4.458734124999999437, -51.06249999863440792, -5.460374474430324690E-16 ) ) ;
#7653 = CARTESIAN_POINT ( 'NONE',  ( 1.975475456537005874E-15, -13.62499999726881228, 5.000000000000000000 ) ) ;
#7654 = CARTESIAN_POINT ( 'NONE',  ( 1.339745962155615144, 17.29465819873852084, 4.999999999999999112 ) ) ;
#7655 = CARTESIAN_POINT ( 'NONE',  ( -2.229367062500000163, -6.479166665301072214, -3.861377020970580443 ) ) ;
#7656 = CARTESIAN_POINT ( 'NONE',  ( 2.499999999999998668, -84.33333333333332860, -4.330127018922193649 ) ) ;
#7657 = ORIENTED_EDGE ( 'NONE', *, *, #28417, .F. ) ;
#7658 = CARTESIAN_POINT ( 'NONE',  ( 2.229367062500001939, -33.22916666530106511, 3.861377020970579999 ) ) ;
#7659 = CARTESIAN_POINT ( 'NONE',  ( -59.44456063193725015, -126.8125000013655921, -0.3552334253322034230 ) ) ;
#7660 = CARTESIAN_POINT ( 'NONE',  ( -6.972266317189433020E-16, -76.24999999999998579, -5.000000000000000000 ) ) ;
#7661 = CARTESIAN_POINT ( 'NONE',  ( 4.458734124999999437, -81.81249999863440792, -5.460374474430324690E-16 ) ) ;
#7662 = CARTESIAN_POINT ( 'NONE',  ( -4.458734124999999437, 23.35416666803226349, -2.574251347313719407 ) ) ;
#7663 = CARTESIAN_POINT ( 'NONE',  ( -4.458734125000000326, -150.1250000013655779, 1.846868145590734089 ) ) ;
#7664 = CARTESIAN_POINT ( 'NONE',  ( -3.152548672688508926E-16, 12.43750000136559564, -5.148502694627439702 ) ) ;
#7665 = LINE ( 'NONE', #16358, #990 ) ;
#7666 = CARTESIAN_POINT ( 'NONE',  ( 1.975475456537005874E-15, -28.74999999999999645, 5.000000000000000000 ) ) ;
#7667 = CARTESIAN_POINT ( 'NONE',  ( -4.458734124999999437, -85.64583333196773651, -2.574251347313719407 ) ) ;
#7668 = CARTESIAN_POINT ( 'NONE',  ( 2.500000000000002220, -63.66666666666666430, 4.330127018922192761 ) ) ;
#7669 = DIRECTION ( 'NONE',  ( 0.000000000000000000, 0.000000000000000000, 1.000000000000000000 ) ) ;
#7670 = CARTESIAN_POINT ( 'NONE',  ( -5.000000000000000000, 19.12500000273118772, 0.000000000000000000 ) ) ;
#7671 = ORIENTED_EDGE ( 'NONE', *, *, #38989, .T. ) ;
#7672 = CARTESIAN_POINT ( 'NONE',  ( -5.000000000000000000, -61.95833333060213732, -2.886751345948128211 ) ) ;
#7673 = CARTESIAN_POINT ( 'NONE',  ( 1.975475456537005874E-15, 9.250000000000000000, 5.000000000000000000 ) ) ;
#7675 = CARTESIAN_POINT ( 'NONE',  ( 2.500000000000002220, -23.66666666666666785, 4.330127018922192761 ) ) ;
#7674 = CARTESIAN_POINT ( 'NONE',  ( -2.499999999999996447, -108.7083333306021444, 4.330127018922195425 ) ) ;
#7676 = CARTESIAN_POINT ( 'NONE',  ( -4.458734124999998549, -30.22916666530106866, 2.574251347313722516 ) ) ;
#7677 = CARTESIAN_POINT ( 'NONE',  ( 1.339745962155615144, 0.2946581987385212820, 4.999999999999999112 ) ) ;
#7678 =( BOUNDED_CURVE ( )  B_SPLINE_CURVE ( 2, ( #31110, #1546, #59440, #915, #30796, #40754, #45906, #584, #6049 ),
 .UNSPECIFIED., .F., .F. ) 
 B_SPLINE_CURVE_WITH_KNOTS ( ( 3, 2, 2, 2, 3 ),
 ( 0.5729166666666666297, 0.5736111111111110716, 0.5749999999999999556, 0.5763888888888888395, 0.5770833333333332815 ),
 .UNSPECIFIED. ) 
 CURVE ( )  GEOMETRIC_REPRESENTATION_ITEM ( )  RATIONAL_B_SPLINE_CURVE ( ( 0.9330127018922194093, 0.9330127018922194093, 1.000000000000000000, 0.8660254037844387076, 1.000000000000000000, 0.8660254037844387076, 1.000000000000000000, 0.9330127018922194093, 0.9330127018922194093 ) ) 
 REPRESENTATION_ITEM ( '' )  );
#7679 = EDGE_CURVE ( 'NONE', #43327, #11325, #44337, .T. ) ;
#7680 = CARTESIAN_POINT ( 'NONE',  ( 5.000000000000000888, -28.45833333060214443, 2.886751345948126879 ) ) ;
#7682 = ORIENTED_EDGE ( 'NONE', *, *, #52400, .T. ) ;
#7681 = CARTESIAN_POINT ( 'NONE',  ( 2.229367062499998831, -58.64583333196773651, -3.861377020970580887 ) ) ;
#7683 = DIRECTION ( 'NONE',  ( -0.4999999999999998890, 0.000000000000000000, -0.8660254037844387076 ) ) ;
#7685 = ORIENTED_EDGE ( 'NONE', *, *, #50325, .T. ) ;
#7684 = CARTESIAN_POINT ( 'NONE',  ( 2.229367062500001939, -10.22916666530106866, 3.861377020970579999 ) ) ;
#7686 = CARTESIAN_POINT ( 'NONE',  ( 5.000000000000000000, -71.41666666666665719, -2.886751345948129988 ) ) ;
#7687 = CARTESIAN_POINT ( 'NONE',  ( -57.89159099828107458, -137.6875000013656063, -3.393966926194107447 ) ) ;
#7688 = CARTESIAN_POINT ( 'NONE',  ( -4.458734124999999437, -52.64583333196773651, -2.574251347313719407 ) ) ;
#7689 = CARTESIAN_POINT ( 'NONE',  ( 5.000000000000000000, -79.29166666393548724, -2.886751345948129988 ) ) ;
#7691 = ORIENTED_EDGE ( 'NONE', *, *, #22457, .F. ) ;
#7690 = CARTESIAN_POINT ( 'NONE',  ( 5.000000000000000000, -10.29166666393547658, -2.886751345948130876 ) ) ;
#7692 = CARTESIAN_POINT ( 'NONE',  ( -60.14911071818854538, -150.0625000000000000, 1.666127454062681368 ) ) ;
#7693 = CARTESIAN_POINT ( 'NONE',  ( -4.458734124999999437, -14.56249999863440436, 0.000000000000000000 ) ) ;
#7694 = CARTESIAN_POINT ( 'NONE',  ( 2.229367062500001939, -58.22916666530107932, 3.861377020970579999 ) ) ;
#7695 = VECTOR ( 'NONE', #640, 1000.000000000000000 ) ;
#7696 =( BOUNDED_CURVE ( )  B_SPLINE_CURVE ( 2, ( #21390, #7241, #23203, #6591, #1789, #18378, #26207, #60955, #11407 ),
 .UNSPECIFIED., .F., .F. ) 
 B_SPLINE_CURVE_WITH_KNOTS ( ( 3, 2, 2, 2, 3 ),
 ( 0.7770833333333333481, 0.7777777777777777901, 0.7791666666666666741, 0.7805555555555555580, 0.7812500000000000000 ),
 .UNSPECIFIED. ) 
 CURVE ( )  GEOMETRIC_REPRESENTATION_ITEM ( )  RATIONAL_B_SPLINE_CURVE ( ( 0.9330127018922194093, 0.9330127018922194093, 1.000000000000000000, 0.8660254037844387076, 1.000000000000000000, 0.8660254037844387076, 1.000000000000000000, 0.9330127018922194093, 0.9330127018922194093 ) ) 
 REPRESENTATION_ITEM ( '' )  );
#7697 = CARTESIAN_POINT ( 'NONE',  ( -5.000000000000000000, -29.95833333060214443, -2.886751345948128211 ) ) ;
#7698 =( LENGTH_UNIT ( ) NAMED_UNIT ( * ) SI_UNIT ( .MILLI., .METRE. ) );
#7699 = CARTESIAN_POINT ( 'NONE',  ( 2.730187237215162345E-16, -169.4375000013656063, -4.458734124999999437 ) ) ;
#7700 = CARTESIAN_POINT ( 'NONE',  ( 2.229367062499998831, -100.8958333319677365, -3.861377020970580887 ) ) ;
#7701 = CARTESIAN_POINT ( 'NONE',  ( 5.000000000000000000, -2.500000000000002220, -6.123233995736766282E-16 ) ) ;
#7702 = ORIENTED_EDGE ( 'NONE', *, *, #33394, .F. ) ;
#7703 = CARTESIAN_POINT ( 'NONE',  ( -59.59170313451810586, -153.7500000013656063, 1.485763867205729394 ) ) ;
#7704 = CARTESIAN_POINT ( 'NONE',  ( -51.19402409849444524, -142.6250000027312126, -3.242614290531456334 ) ) ;
#7705 = FACE_OUTER_BOUND ( 'NONE', #62871, .T. ) ;
#7706 = CARTESIAN_POINT ( 'NONE',  ( 4.458734124999998549, -6.729166665301073103, -2.574251347313721627 ) ) ;
#7707 = CARTESIAN_POINT ( 'NONE',  ( 4.458734125000000326, -94.14583333196772230, 2.574251347313718519 ) ) ;
#7708 = CARTESIAN_POINT ( 'NONE',  ( -8.190561711645485556E-16, -146.9375000013656063, 4.458734124999999437 ) ) ;
#7709 = CARTESIAN_POINT ( 'NONE',  ( 4.458734124999999437, -21.06249999863440436, -5.460374474430324690E-16 ) ) ;
#7710 = CYLINDRICAL_SURFACE ( 'NONE', #45786, 5.000000000000000000 ) ;
#7711 = CARTESIAN_POINT ( 'NONE',  ( -57.19623071787017210, -136.3750000013656063, 4.297418129356382899 ) ) ;
#7712 = CARTESIAN_POINT ( 'NONE',  ( -2.229367062499996610, -62.39583333196774362, 3.861377020970582219 ) ) ;
#7713 = DIRECTION ( 'NONE',  ( 0.000000000000000000, 0.000000000000000000, -1.000000000000000000 ) ) ;
#7714 = CARTESIAN_POINT ( 'NONE',  ( -2.499999999999996447, 17.16666666666666430, 4.330127018922195425 ) ) ;
#7715 = CARTESIAN_POINT ( 'NONE',  ( -4.458734124999999437, -146.9375000013656063, -5.460374474430324690E-16 ) ) ;
#7716 = CARTESIAN_POINT ( 'NONE',  ( 4.458734124999998549, 10.02083333469892779, -2.574251347313721627 ) ) ;
#7717 = ORIENTED_EDGE ( 'NONE', *, *, #5820, .T. ) ;
#7718 = CARTESIAN_POINT ( 'NONE',  ( 1.975475456537005874E-15, -80.74999999999998579, 5.000000000000000000 ) ) ;
#7719 = FACE_OUTER_BOUND ( 'NONE', #31648, .T. ) ;
#7721 = CARTESIAN_POINT ( 'NONE',  ( -2.229367062500000163, -23.47916666530107221, -3.861377020970580443 ) ) ;
#7720 = CARTESIAN_POINT ( 'NONE',  ( 2.499999999999998668, -92.33333333333334281, -4.330127018922193649 ) ) ;
#7722 = CARTESIAN_POINT ( 'NONE',  ( 4.458734124999999437, -72.06249999863439371, -5.460374474430324690E-16 ) ) ;
#7723 = CARTESIAN_POINT ( 'NONE',  ( -4.458734124999997661, 28.52083333469892423, 2.574251347313722516 ) ) ;
#7724 = CARTESIAN_POINT ( 'NONE',  ( -53.51423613279429503, -147.2500000013656063, 4.591703134518082763 ) ) ;
#7725 = CARTESIAN_POINT ( 'NONE',  ( -5.000000000000000000, -1.958333330602145983, -2.886751345948128211 ) ) ;
#7726 = CARTESIAN_POINT ( 'NONE',  ( 4.458734124999998549, 6.270833334698928674, -2.574251347313721627 ) ) ;
#7727 = LINE ( 'NONE', #41802, #61268 ) ;
#7728 = CARTESIAN_POINT ( 'NONE',  ( -2.500000000000000444, -15.16666666666666785, -4.330127018922193649 ) ) ;
#7729 = CARTESIAN_POINT ( 'NONE',  ( 4.458734125000000326, 9.104166668032261711, 2.574251347313718519 ) ) ;
#7730 = CARTESIAN_POINT ( 'NONE',  ( -3.152548672688508926E-16, -71.56249999863440792, -5.148502694627439702 ) ) ;
#7731 = CARTESIAN_POINT ( 'NONE',  ( -4.458734124999999437, -19.56249999863440081, 0.000000000000000000 ) ) ;
#7732 = CARTESIAN_POINT ( 'NONE',  ( -4.999999999999999112, -1.916666666666663854, 2.886751345948131764 ) ) ;
#7733 = CARTESIAN_POINT ( 'NONE',  ( -1.846868145590737420, -161.7500000013655495, 4.458734124999999437 ) ) ;
#7734 = CARTESIAN_POINT ( 'NONE',  ( 1.975475456537005874E-15, -61.62499999726880162, 5.000000000000000000 ) ) ;
#7735 = CARTESIAN_POINT ( 'NONE',  ( 2.229367062499998831, -65.64583333196773651, -3.861377020970580887 ) ) ;
#7736 = CARTESIAN_POINT ( 'NONE',  ( -5.000000000000000000, -98.87499999726881583, 0.000000000000000000 ) ) ;
#7737 = CARTESIAN_POINT ( 'NONE',  ( 5.000000000000000000, -139.1250000027312126, 0.000000000000000000 ) ) ;
#7738 = CARTESIAN_POINT ( 'NONE',  ( -4.458734124999999437, -39.31249999863440081, 0.000000000000000000 ) ) ;
#7739 = CARTESIAN_POINT ( 'NONE',  ( -7.894787914004607998, -1.230850257101226302E-13, -7.591390474663425536 ) ) ;
#7740 = CARTESIAN_POINT ( 'NONE',  ( -4.458734124999999437, -65.56249999863440792, 0.000000000000000000 ) ) ;
#7741 = CARTESIAN_POINT ( 'NONE',  ( -4.999999999999999112, -48.91666666666666430, 2.886751345948131764 ) ) ;
#7742 = CARTESIAN_POINT ( 'NONE',  ( 7.204675194429079505E-15, 25.87500000273118062, -5.000000000000000000 ) ) ;
#7743 = ORIENTED_EDGE ( 'NONE', *, *, #13991, .T. ) ;
#7744 = DIRECTION ( 'NONE',  ( -0.000000000000000000, 1.000000000000000000, -0.000000000000000000 ) ) ;
#7745 =( BOUNDED_CURVE ( )  B_SPLINE_CURVE ( 2, ( #54384, #25103, #5489, #10623, #35396, #39887, #26382, #50831, #676 ),
 .UNSPECIFIED., .F., .F. ) 
 B_SPLINE_CURVE_WITH_KNOTS ( ( 3, 2, 2, 2, 3 ),
 ( 0.9895833333333333703, 0.9902777777777778123, 0.9916666666666666963, 0.9930555555555555802, 0.9937500000000000222 ),
 .UNSPECIFIED. ) 
 CURVE ( )  GEOMETRIC_REPRESENTATION_ITEM ( )  RATIONAL_B_SPLINE_CURVE ( ( 0.9330127018922194093, 0.9330127018922194093, 1.000000000000000000, 0.8660254037844387076, 1.000000000000000000, 0.8660254037844387076, 1.000000000000000000, 0.9330127018922194093, 0.9330127018922194093 ) ) 
 REPRESENTATION_ITEM ( '' )  );
#7746 = CARTESIAN_POINT ( 'NONE',  ( -4.999999999999999112, -9.916666666666662522, 2.886751345948131764 ) ) ;
#7747 = CARTESIAN_POINT ( 'NONE',  ( -4.458734124999999437, -72.39583333196773651, -2.574251347313719407 ) ) ;
#7748 = DIRECTION ( 'NONE',  ( 0.000000000000000000, 0.000000000000000000, 1.000000000000000000 ) ) ;
#7749 = CARTESIAN_POINT ( 'NONE',  ( -4.999999999999999112, -13.79166666393548191, 2.886751345948131764 ) ) ;
#7751 = ORIENTED_EDGE ( 'NONE', *, *, #5971, .T. ) ;
#7750 = CARTESIAN_POINT ( 'NONE',  ( 2.229367062500001939, -41.97916666530107932, 3.861377020970579999 ) ) ;
#7752 = DIRECTION ( 'NONE',  ( 0.000000000000000000, 0.000000000000000000, 1.000000000000000000 ) ) ;
#7754 = VERTEX_POINT ( 'NONE', #10007 ) ;
#7753 = CARTESIAN_POINT ( 'NONE',  ( 2.229367062499998831, 8.104166668032261711, -3.861377020970580887 ) ) ;
#7755 = CARTESIAN_POINT ( 'NONE',  ( 5.000000000000000000, -34.29166666393547303, -2.886751345948130876 ) ) ;
#7756 = CARTESIAN_POINT ( 'NONE',  ( 5.000000000000000888, -54.58333333333332860, 2.886751345948126879 ) ) ;
#7757 = CARTESIAN_POINT ( 'NONE',  ( 4.458734125000000326, -161.6250000013656063, -1.846868145590734978 ) ) ;
#7758 = CARTESIAN_POINT ( 'NONE',  ( 9.457646018065525792E-16, -33.31249999863440792, 5.148502694627439702 ) ) ;
#7759 = CARTESIAN_POINT ( 'NONE',  ( 2.500000000000002220, -10.66666666666666430, 4.330127018922192761 ) ) ;
#7760 = CARTESIAN_POINT ( 'NONE',  ( 2.229367062500001939, -81.97916666530106511, 3.861377020970579999 ) ) ;
#7761 = CARTESIAN_POINT ( 'NONE',  ( -5.000000000000000888, -164.4375000000000284, 2.071067811865474617 ) ) ;
#7762 = CARTESIAN_POINT ( 'NONE',  ( 9.457646018065525792E-16, -89.06249999863439371, 5.148502694627439702 ) ) ;
#7763 = CARTESIAN_POINT ( 'NONE',  ( -55.35523342533222291, -129.5625000013656063, 4.444560631937231499 ) ) ;
#7764 = CARTESIAN_POINT ( 'NONE',  ( -4.458734124999999437, -1.645833331967737401, -2.574251347313719407 ) ) ;
#7765 = CARTESIAN_POINT ( 'NONE',  ( 4.458734124999999437, -42.06249999863440081, -5.460374474430324690E-16 ) ) ;
#7766 = CARTESIAN_POINT ( 'NONE',  ( 2.500000000000002220, -16.54166666393548368, 4.330127018922192761 ) ) ;
#7767 = CARTESIAN_POINT ( 'NONE',  ( 4.458734124999999437, -85.06249999863439371, -5.460374474430324690E-16 ) ) ;
#7768 = VERTEX_POINT ( 'NONE', #58277 ) ;
#7769 = CARTESIAN_POINT ( 'NONE',  ( -50.01589407740564042, -153.7500000027312410, 0.3983568153799778022 ) ) ;
#7770 =( BOUNDED_CURVE ( )  B_SPLINE_CURVE ( 2, ( #52851, #42873, #12974, #8785, #17502, #27449, #23589, #43184, #57374 ),
 .UNSPECIFIED., .F., .F. ) 
 B_SPLINE_CURVE_WITH_KNOTS ( ( 3, 2, 2, 2, 3 ),
 ( 0.2482142857142857206, 0.2488095238095238138, 0.2500000000000000000, 0.2511904761904761862, 0.2517857142857142794 ),
 .UNSPECIFIED. ) 
 CURVE ( )  GEOMETRIC_REPRESENTATION_ITEM ( )  RATIONAL_B_SPLINE_CURVE ( ( 0.9330127018922194093, 0.9330127018922194093, 1.000000000000000000, 0.8660254037844387076, 1.000000000000000000, 0.8660254037844387076, 1.000000000000000000, 0.9330127018922194093, 0.9330127018922194093 ) ) 
 REPRESENTATION_ITEM ( '' )  );
#7771 = LINE ( 'NONE', #56030, #16815 ) ;
#7773 = ADVANCED_FACE ( 'NONE', ( #44412 ), #19656, .T. ) ;
#7772 = CARTESIAN_POINT ( 'NONE',  ( -2.229367062500000163, -67.72916666530106511, -3.861377020970580443 ) ) ;
#7774 = CARTESIAN_POINT ( 'NONE',  ( 9.457646018065525792E-16, -37.06249999863440792, 5.148502694627439702 ) ) ;
#7775 = CARTESIAN_POINT ( 'NONE',  ( -2.229367062500000163, -10.72916666530106866, -3.861377020970580443 ) ) ;
#7776 = ORIENTED_EDGE ( 'NONE', *, *, #57913, .T. ) ;
#7777 = AXIS2_PLACEMENT_3D ( 'NONE', #22627, #12641, #32256 ) ;
#7778 = LINE ( 'NONE', #17740, #12268 ) ;
#7779 = CARTESIAN_POINT ( 'NONE',  ( 3.044556291839386294E-14, 17.75000000000000355, -5.000000000000000000 ) ) ;
#7780 = CARTESIAN_POINT ( 'NONE',  ( -2.229367062500000163, -7.729166665301073991, -3.861377020970580443 ) ) ;
#7781 = CYLINDRICAL_SURFACE ( 'NONE', #34289, 5.000000000000000000 ) ;
#7782 = CARTESIAN_POINT ( 'NONE',  ( -3.152548672688508926E-16, 4.437500001365595637, -5.148502694627439702 ) ) ;
#7783 = CARTESIAN_POINT ( 'NONE',  ( 3.535533905932736864, -154.1250000000000000, 3.535533905932738641 ) ) ;
#7784 = CARTESIAN_POINT ( 'NONE',  ( -3.152801135295367096, -158.0625000013656063, -3.152801135295367541 ) ) ;
#7785 = CARTESIAN_POINT ( 'NONE',  ( 2.229367062500001939, 27.77083333469892779, 3.861377020970579999 ) ) ;
#7786 = ORIENTED_EDGE ( 'NONE', *, *, #39305, .T. ) ;
#7787 = CARTESIAN_POINT ( 'NONE',  ( -4.458734124999999437, -84.39583333196773651, -2.574251347313719407 ) ) ;
#7788 = CARTESIAN_POINT ( 'NONE',  ( 4.250000000000000000, 0.000000000000000000, -9.449444346342714240 ) ) ;
#7789 = CARTESIAN_POINT ( 'NONE',  ( 4.458734124999998549, -10.72916666530106866, -2.574251347313721627 ) ) ;
#7790 = CARTESIAN_POINT ( 'NONE',  ( 1.339745962155612702, -51.29465819873851729, -5.000000000000000000 ) ) ;
#7791 = CARTESIAN_POINT ( 'NONE',  ( 5.000000000000000000, -48.41666666666666430, -2.886751345948130876 ) ) ;
#7792 = ADVANCED_FACE ( 'NONE', ( #10329 ), #29619, .T. ) ;
#7793 = CARTESIAN_POINT ( 'NONE',  ( -52.53715891517739323, -138.4375000000000000, -4.819101127000233298 ) ) ;
#7794 = CARTESIAN_POINT ( 'NONE',  ( -5.000000000000000000, -33.87499999726880873, 0.000000000000000000 ) ) ;
#7795 = ADVANCED_FACE ( 'NONE', ( #44732 ), #63422, .T. ) ;
#7796 = CARTESIAN_POINT ( 'NONE',  ( 1.975475456537005874E-15, -16.74999999999999645, 5.000000000000000000 ) ) ;
#7797 = CARTESIAN_POINT ( 'NONE',  ( 2.229367062500001939, 25.02083333469892779, 3.861377020970579999 ) ) ;
#7798 = DIRECTION ( 'NONE',  ( 0.000000000000000000, 1.000000000000000000, 0.000000000000000000 ) ) ;
#7799 = CARTESIAN_POINT ( 'NONE',  ( 4.458734124999998549, 23.27083333469892423, -2.574251347313721627 ) ) ;
#7800 = CARTESIAN_POINT ( 'NONE',  ( 2.229367062499998831, -56.64583333196773651, -3.861377020970580887 ) ) ;
#7801 = CARTESIAN_POINT ( 'NONE',  ( -3.152548672688508926E-16, -2.812499998634407472, -5.148502694627439702 ) ) ;
#7802 = CARTESIAN_POINT ( 'NONE',  ( -1.339745962155610925, -17.79465819873852439, 5.000000000000000000 ) ) ;
#7803 = CARTESIAN_POINT ( 'NONE',  ( 5.000000000000000888, 17.41666666666666430, 2.886751345948126879 ) ) ;
#7804 = CARTESIAN_POINT ( 'NONE',  ( 3.061616997868383141E-16, -140.8750000027312126, -5.000000000000000000 ) ) ;
#7806 = VECTOR ( 'NONE', #32542, 1000.000000000000000 ) ;
#7805 = CARTESIAN_POINT ( 'NONE',  ( -4.999999999999998224, -20.79166666393548013, 2.886751345948131764 ) ) ;
#7807 = CARTESIAN_POINT ( 'NONE',  ( 4.458734124999998549, -48.72916666530107221, -2.574251347313721627 ) ) ;
#7808 = CARTESIAN_POINT ( 'NONE',  ( 1.060575238724906964E-15, -81.62499999726881583, 5.773502691896257311 ) ) ;
#7809 = CARTESIAN_POINT ( 'NONE',  ( -54.64476657466781973, -139.0625000013656063, -4.444560631937228834 ) ) ;
#7810 = CARTESIAN_POINT ( 'NONE',  ( 0.000000000000000000, -170.0000000000000000, 5.000000000000000000 ) ) ;
#7811 = CARTESIAN_POINT ( 'NONE',  ( 2.500000000000002220, -36.66666666666666430, 4.330127018922192761 ) ) ;
#7812 = CARTESIAN_POINT ( 'NONE',  ( -2.229367062499996610, -85.39583333196773651, 3.861377020970582219 ) ) ;
#7813 = CARTESIAN_POINT ( 'NONE',  ( -4.458734124999999437, -156.1875000013655779, -5.460374474430324690E-16 ) ) ;
#7814 = CARTESIAN_POINT ( 'NONE',  ( -5.000000000000000000, -32.00000000000000000, 0.000000000000000000 ) ) ;
#7815 = ORIENTED_EDGE ( 'NONE', *, *, #31398, .F. ) ;
#7816 = CARTESIAN_POINT ( 'NONE',  ( -2.229367062500000163, 16.27083333469892779, -3.861377020970580443 ) ) ;
#7817 = ORIENTED_EDGE ( 'NONE', *, *, #51420, .F. ) ;
#7818 = CARTESIAN_POINT ( 'NONE',  ( 4.458734124999999437, -97.81249999863440792, -5.460374474430324690E-16 ) ) ;
#7819 = CARTESIAN_POINT ( 'NONE',  ( -4.458734124999999437, 15.43750000136559386, 0.000000000000000000 ) ) ;
#7820 = CARTESIAN_POINT ( 'NONE',  ( 2.500000000000002220, 18.45833333606451632, 4.330127018922192761 ) ) ;
#7821 = DIRECTION ( 'NONE',  ( -0.000000000000000000, 1.000000000000000000, -0.000000000000000000 ) ) ;
#7822 = CARTESIAN_POINT ( 'NONE',  ( -5.000000000000000000, 5.916666666666666963, -2.886751345948128211 ) ) ;
#7823 = CARTESIAN_POINT ( 'NONE',  ( 4.458734124999999437, -57.81249999863440081, -5.460374474430324690E-16 ) ) ;
#7824 = VECTOR ( 'NONE', #35713, 1000.000000000000000 ) ;
#7825 = CARTESIAN_POINT ( 'NONE',  ( 5.000000000000000000, -61.29166666393548013, -2.886751345948130876 ) ) ;
#7826 = CARTESIAN_POINT ( 'NONE',  ( 5.000000000000000000, -82.41666666666665719, -2.886751345948129988 ) ) ;
#7827 = CARTESIAN_POINT ( 'NONE',  ( -50.70258187064364108, -135.3750000013656063, 2.196230717870141014 ) ) ;
#7828 = CARTESIAN_POINT ( 'NONE',  ( 1.975475456537005874E-15, -40.62499999726879452, 5.000000000000000000 ) ) ;
#7829 = CARTESIAN_POINT ( 'NONE',  ( 2.499999999999998668, -63.33333333333332149, -4.330127018922193649 ) ) ;
#7830 = CARTESIAN_POINT ( 'NONE',  ( -1.339745962155599601, 17.91965820146970501, -5.000000000000007994 ) ) ;
#7831 = CARTESIAN_POINT ( 'NONE',  ( -5.000000000000000000, -38.08333333333333570, -2.886751345948128211 ) ) ;
#7832 = CARTESIAN_POINT ( 'NONE',  ( -5.000000000000000000, 13.12500000273118417, 0.000000000000000000 ) ) ;
#7834 = CARTESIAN_POINT ( 'NONE',  ( -3.152548672688508926E-16, -19.81249999863440436, -5.148502694627439702 ) ) ;
#7833 = CARTESIAN_POINT ( 'NONE',  ( -1.339745962155613812, -43.20534180126148271, -5.000000000000000000 ) ) ;
#7835 = CARTESIAN_POINT ( 'NONE',  ( 1.339745962155612702, -107.1696581960073189, -5.000000000000000000 ) ) ;
#7836 = CARTESIAN_POINT ( 'NONE',  ( -2.229367062499996610, -64.14583333196773651, 3.861377020970582219 ) ) ;
#7837 = CARTESIAN_POINT ( 'NONE',  ( -8.190561711645485556E-16, -148.9375000013656063, 4.458734124999999437 ) ) ;
#7838 = CARTESIAN_POINT ( 'NONE',  ( 4.458734124999999437, -72.81249999863439371, -5.460374474430324690E-16 ) ) ;
#7839 = CARTESIAN_POINT ( 'NONE',  ( -52.10840900171896806, -143.4375000013656063, 3.393966926194110556 ) ) ;
#7840 = CARTESIAN_POINT ( 'NONE',  ( -4.458734124999999437, -17.64583333196773651, -2.574251347313719407 ) ) ;
#7841 = CARTESIAN_POINT ( 'NONE',  ( 5.000000000000000888, -60.45833333060213732, 2.886751345948126879 ) ) ;
#7842 = ORIENTED_EDGE ( 'NONE', *, *, #38979, .T. ) ;
#7843 = CARTESIAN_POINT ( 'NONE',  ( -2.071067811865306307, -150.6875000000000853, -5.000000000000171418 ) ) ;
#7844 = VERTEX_POINT ( 'NONE', #5504 ) ;
#7845 = CARTESIAN_POINT ( 'NONE',  ( 9.457646018065525792E-16, -66.31249999863440792, 5.148502694627439702 ) ) ;
#7846 = LINE ( 'NONE', #57062, #15281 ) ;
#7847 = CARTESIAN_POINT ( 'NONE',  ( -5.000000000000000888, 6.123233995736767268E-16, -10.00000000000000000 ) ) ;
#7848 = ORIENTED_EDGE ( 'NONE', *, *, #43115, .T. ) ;
#7849 = CARTESIAN_POINT ( 'NONE',  ( -58.80597590150559739, -152.0000000000000284, 3.242614290531460330 ) ) ;
#7850 = CARTESIAN_POINT ( 'NONE',  ( -55.39835681537999790, -126.8750000000000142, 4.984105922594378235 ) ) ;
#7851 = CARTESIAN_POINT ( 'NONE',  ( -6.972266317189433020E-16, -43.25000000000000000, -5.000000000000000000 ) ) ;
#7853 = EDGE_CURVE ( 'NONE', #1043, #21692, #26711, .T. ) ;
#7852 = CARTESIAN_POINT ( 'NONE',  ( 4.458734124999999437, -56.06249999863440081, -5.460374474430324690E-16 ) ) ;
#7854 = ORIENTED_EDGE ( 'NONE', *, *, #10968, .F. ) ;
#7855 = CARTESIAN_POINT ( 'NONE',  ( 5.000000000000000000, -45.41666666666665719, -2.886751345948130876 ) ) ;
#7856 = CARTESIAN_POINT ( 'NONE',  ( 4.458734125000001214, 10.10416666803226171, 2.574251347313718519 ) ) ;
#7857 = CARTESIAN_POINT ( 'NONE',  ( -4.458734124999998549, 18.77083333469893134, 2.574251347313722516 ) ) ;
#7858 = CARTESIAN_POINT ( 'NONE',  ( -57.89159099828107458, -149.6875000013656063, -3.393966926194107447 ) ) ;
#7859 = CARTESIAN_POINT ( 'NONE',  ( 1.339745962155615144, -13.58034179853029322, 4.999999999999999112 ) ) ;
#7860 = CARTESIAN_POINT ( 'NONE',  ( 4.458734124999999437, -168.4375000013656063, 0.000000000000000000 ) ) ;
#7861 = EDGE_LOOP ( 'NONE', ( #46627, #11784, #26267, #6913, #29257, #27467 ) ) ;
#7862 = CARTESIAN_POINT ( 'NONE',  ( 2.229367062500001939, -69.97916666530107932, 3.861377020970579999 ) ) ;
#7863 = EDGE_CURVE ( 'NONE', #41928, #19133, #42663, .T. ) ;
#7864 = CARTESIAN_POINT ( 'NONE',  ( 1.975475456537005874E-15, -30.62499999726881228, 5.000000000000000000 ) ) ;
#7865 = CARTESIAN_POINT ( 'NONE',  ( -2.229367062499996610, 9.854166668032261711, 3.861377020970582219 ) ) ;
#7866 =( BOUNDED_CURVE ( )  B_SPLINE_CURVE ( 2, ( #36668, #6769, #16417, #31200, #61444, #7725, #7090, #1639, #56297 ),
 .UNSPECIFIED., .F., .F. ) 
 B_SPLINE_CURVE_WITH_KNOTS ( ( 3, 2, 2, 2, 3 ),
 ( 0.2196428571428571397, 0.2202380952380952328, 0.2214285714285714191, 0.2226190476190476053, 0.2232142857142857262 ),
 .UNSPECIFIED. ) 
 CURVE ( )  GEOMETRIC_REPRESENTATION_ITEM ( )  RATIONAL_B_SPLINE_CURVE ( ( 0.9330127018922194093, 0.9330127018922194093, 1.000000000000000000, 0.8660254037844387076, 1.000000000000000000, 0.8660254037844387076, 1.000000000000000000, 0.9330127018922178550, 0.9330127018922194093 ) ) 
 REPRESENTATION_ITEM ( '' )  );
#7867 = CARTESIAN_POINT ( 'NONE',  ( -4.999999999999998224, -88.91666666666667140, 2.886751345948131764 ) ) ;
#7868 = CARTESIAN_POINT ( 'NONE',  ( -4.458734124999998549, -61.47916666530107221, 2.574251347313722516 ) ) ;
#7869 = CARTESIAN_POINT ( 'NONE',  ( -4.999999999999999112, -20.79166666393548013, 2.886751345948131764 ) ) ;
#7870 = EDGE_CURVE ( 'NONE', #10962, #58935, #40226, .T. ) ;
#7871 = FACE_OUTER_BOUND ( 'NONE', #44717, .T. ) ;
#7872 = CARTESIAN_POINT ( 'NONE',  ( -56.66612745406293783, -140.4375000027311842, -5.149110718188535607 ) ) ;
#7873 = CARTESIAN_POINT ( 'NONE',  ( 2.499999999999998668, -65.33333333333332860, -4.330127018922193649 ) ) ;
#7874 = CARTESIAN_POINT ( 'NONE',  ( 2.229367062500001939, -39.97916666530107221, 3.861377020970579999 ) ) ;
#7875 = EDGE_CURVE ( 'NONE', #52469, #4573, #44719, .T. ) ;
#7876 = CARTESIAN_POINT ( 'NONE',  ( 2.229367062500001939, -19.22916666530106866, 3.861377020970579999 ) ) ;
#7877 = EDGE_LOOP ( 'NONE', ( #5385, #57966, #29265, #47841 ) ) ;
#7878 = CARTESIAN_POINT ( 'NONE',  ( -2.499999999999996447, -101.8333333333333286, 4.330127018922195425 ) ) ;
#7879 = CARTESIAN_POINT ( 'NONE',  ( -2.229367062499996610, -110.1458333319677365, 3.861377020970582219 ) ) ;
#7880 = CARTESIAN_POINT ( 'NONE',  ( 3.061616997868383141E-16, -153.8750000027311842, -5.000000000000000000 ) ) ;
#7881 = VERTEX_POINT ( 'NONE', #20949 ) ;
#7882 = CARTESIAN_POINT ( 'NONE',  ( -2.229367062500000163, -108.7291666653010651, -3.861377020970580443 ) ) ;
#7883 = CARTESIAN_POINT ( 'NONE',  ( -4.458734124999999437, -33.39583333196772941, -2.574251347313719407 ) ) ;
#7884 = CARTESIAN_POINT ( 'NONE',  ( -5.000000000000000000, -60.95833333060214443, -2.886751345948128211 ) ) ;
#7885 = CARTESIAN_POINT ( 'NONE',  ( -53.51423613279429503, -150.5000000013655779, 4.591703134518082763 ) ) ;
#7886 = CARTESIAN_POINT ( 'NONE',  ( 2.071067811865475505, -145.8125000000000284, -5.000000000000000888 ) ) ;
#7887 = CARTESIAN_POINT ( 'NONE',  ( -4.458734124999997661, -28.22916666530107221, 2.574251347313722516 ) ) ;
#7888 = CARTESIAN_POINT ( 'NONE',  ( 4.458734124999999437, -67.06249999863440792, -5.460374474430324690E-16 ) ) ;
#7889 = CARTESIAN_POINT ( 'NONE',  ( -2.499999999999996447, -54.83333333333332860, 4.330127018922195425 ) ) ;
#7890 = CARTESIAN_POINT ( 'NONE',  ( -3.152548672688508926E-16, -25.56249999863440792, -5.148502694627439702 ) ) ;
#7891 = CARTESIAN_POINT ( 'NONE',  ( -4.999999999999998224, 9.208333336064519870, 2.886751345948131764 ) ) ;
#7892 = CARTESIAN_POINT ( 'NONE',  ( -2.499999999999996447, -18.83333333333333215, 4.330127018922195425 ) ) ;
#7893 = CARTESIAN_POINT ( 'NONE',  ( 3.152801135295366208, -148.5625000013655779, 3.152801135295367985 ) ) ;
#7894 = ORIENTED_EDGE ( 'NONE', *, *, #55866, .F. ) ;
#7895 = CARTESIAN_POINT ( 'NONE',  ( -59.98410592259440222, -153.1250000000000284, -0.3983568153799752487 ) ) ;
#7896 = CARTESIAN_POINT ( 'NONE',  ( -4.458734124999997661, -53.47916666530107221, 2.574251347313722516 ) ) ;
#7897 = CARTESIAN_POINT ( 'NONE',  ( 5.000000000000000000, -58.37499999726880873, -6.123233995736766282E-16 ) ) ;
#7898 = DIRECTION ( 'NONE',  ( -0.000000000000000000, 1.000000000000000000, -0.000000000000000000 ) ) ;
#7899 = CARTESIAN_POINT ( 'NONE',  ( 5.000000000000000888, 25.41666666666666430, 2.886751345948126879 ) ) ;
#7900 = EDGE_CURVE ( 'NONE', #56115, #33543, #15104, .T. ) ;
#7901 = CARTESIAN_POINT ( 'NONE',  ( 1.339745962155612702, 25.70534180126147916, -5.000000000000000000 ) ) ;
#7902 = CARTESIAN_POINT ( 'NONE',  ( 4.458734124999999437, -2.812499998634407472, -5.460374474430324690E-16 ) ) ;
#7903 = CARTESIAN_POINT ( 'NONE',  ( -6.972266317189433020E-16, -52.12499999726880873, -5.000000000000000000 ) ) ;
#7904 = CARTESIAN_POINT ( 'NONE',  ( 3.535533905932738197, -140.8750000000000000, -3.535533905932738197 ) ) ;
#7905 = CARTESIAN_POINT ( 'NONE',  ( 1.975475456537005874E-15, -60.75000000000000000, 5.000000000000000000 ) ) ;
#7906 = CARTESIAN_POINT ( 'NONE',  ( 4.458734125000001214, 7.854166668032260823, 2.574251347313718519 ) ) ;
#7907 = ORIENTED_EDGE ( 'NONE', *, *, #12317, .T. ) ;
#7908 = CARTESIAN_POINT ( 'NONE',  ( 1.339745962155615144, -42.70534180126148982, 4.999999999999999112 ) ) ;
#7909 = ORIENTED_EDGE ( 'NONE', *, *, #37702, .T. ) ;
#7910 = CARTESIAN_POINT ( 'NONE',  ( 0.000000000000000000, -120.0000000000000000, 0.000000000000000000 ) ) ;
#7911 = CARTESIAN_POINT ( 'NONE',  ( 4.458734125000001214, -46.89583333196773651, 2.574251347313718519 ) ) ;
#7912 = CARTESIAN_POINT ( 'NONE',  ( -3.152801135295367985, -159.0625000013656063, 3.152801135295367096 ) ) ;
#7913 = AXIS2_PLACEMENT_3D ( 'NONE', #6559, #26173, #46111 ) ;
#7914 = VECTOR ( 'NONE', #41713, 1000.000000000000000 ) ;
#7915 = CARTESIAN_POINT ( 'NONE',  ( 2.499999999999998668, -44.20833333060214443, -4.330127018922193649 ) ) ;
#7916 = ORIENTED_EDGE ( 'NONE', *, *, #37869, .F. ) ;
#7917 = CARTESIAN_POINT ( 'NONE',  ( -2.229367062500000163, -25.47916666530106866, -3.861377020970580443 ) ) ;
#7918 = VERTEX_POINT ( 'NONE', #40239 ) ;
#7919 =( BOUNDED_CURVE ( )  B_SPLINE_CURVE ( 2, ( #37666, #8097, #12903, #31898, #61502, #27381, #28013, #41853, #17432 ),
 .UNSPECIFIED., .F., .F. ) 
 B_SPLINE_CURVE_WITH_KNOTS ( ( 3, 2, 2, 2, 3 ),
 ( 0.1916666666666668462, 0.1958333333333334980, 0.2000000000000001776, 0.2041666666666668295, 0.2083333333333335091 ),
 .UNSPECIFIED. ) 
 CURVE ( )  GEOMETRIC_REPRESENTATION_ITEM ( )  RATIONAL_B_SPLINE_CURVE ( ( 0.9999999999999970024, 0.9238795325112897361, 1.000000000000000000, 0.9238795325112867385, 1.000000000000000000, 0.9238795325112867385, 1.000000000000000000, 0.9238795325112837409, 1.000000000000003109 ) ) 
 REPRESENTATION_ITEM ( '' )  );
#7920 = CARTESIAN_POINT ( 'NONE',  ( -1.339745962155610925, -11.79465819873851906, 5.000000000000000000 ) ) ;
#7921 = CARTESIAN_POINT ( 'NONE',  ( -3.152801135295367985, -165.8125000013656063, 3.152801135295367096 ) ) ;
#7922 = DIRECTION ( 'NONE',  ( 0.000000000000000000, 0.000000000000000000, 1.000000000000000000 ) ) ;
#7923 = CARTESIAN_POINT ( 'NONE',  ( -53.33387254593733928, -138.8125000000000284, 5.149110718188519620 ) ) ;
#7924 = CARTESIAN_POINT ( 'NONE',  ( 2.229367062499998831, -39.89583333196773651, -3.861377020970580887 ) ) ;
#7925 = DIRECTION ( 'NONE',  ( 0.000000000000000000, 0.000000000000000000, 1.000000000000000000 ) ) ;
#7926 = ORIENTED_EDGE ( 'NONE', *, *, #13807, .F. ) ;
#7927 = EDGE_CURVE ( 'NONE', #14051, #592, #46810, .T. ) ;
#7928 = EDGE_CURVE ( 'NONE', #13658, #49915, #21257, .T. ) ;
#7929 = CARTESIAN_POINT ( 'NONE',  ( 4.458734124999999437, -82.81249999863440792, -5.460374474430324690E-16 ) ) ;
#7930 = CARTESIAN_POINT ( 'NONE',  ( 4.458734124999999437, 24.18750000136559564, -5.460374474430324690E-16 ) ) ;
#7931 = CARTESIAN_POINT ( 'NONE',  ( 5.000000000000000000, -140.0000000000000000, 0.000000000000000000 ) ) ;
#7932 = EDGE_CURVE ( 'NONE', #33925, #20951, #50532, .T. ) ;
#7933 = VERTEX_POINT ( 'NONE', #59876 ) ;
#7934 = DIRECTION ( 'NONE',  ( 0.000000000000000000, 1.000000000000000000, 0.000000000000000000 ) ) ;
#7935 = CARTESIAN_POINT ( 'NONE',  ( -52.80376928212989185, -137.1250000013656063, -4.297418129356378458 ) ) ;
#7936 = CARTESIAN_POINT ( 'NONE',  ( 4.458734125000001214, -81.14583333196773651, 2.574251347313718519 ) ) ;
#7937 = CARTESIAN_POINT ( 'NONE',  ( -56.66612745406270335, -129.4375000027312126, -5.149110718188516067 ) ) ;
#7938 = CARTESIAN_POINT ( 'NONE',  ( 3.535533905932736864, -143.1250000000000000, 3.535533905932738641 ) ) ;
#7939 = CARTESIAN_POINT ( 'NONE',  ( 4.458734125000000326, -54.89583333196774362, 2.574251347313718519 ) ) ;
#7940 = CARTESIAN_POINT ( 'NONE',  ( 1.339745962155612702, 10.70534180126147739, -5.000000000000000000 ) ) ;
#7941 = CARTESIAN_POINT ( 'NONE',  ( 4.458734125000001214, 21.10416666803226349, 2.574251347313718519 ) ) ;
#7942 = EDGE_CURVE ( 'NONE', #29821, #3756, #60198, .T. ) ;
#7943 = CARTESIAN_POINT ( 'NONE',  ( 2.500000000000002220, -106.6666666666666572, 4.330127018922192761 ) ) ;
#7944 = CARTESIAN_POINT ( 'NONE',  ( 1.339745962155612702, -3.294658198738522170, -5.000000000000000000 ) ) ;
#7945 = CARTESIAN_POINT ( 'NONE',  ( -3.152548672688508926E-16, -45.81249999863440081, -5.148502694627439702 ) ) ;
#7946 = CARTESIAN_POINT ( 'NONE',  ( -5.000000000000000000, 0.1250000027311869155, 0.000000000000000000 ) ) ;
#7947 = LINE ( 'NONE', #27550, #16077 ) ;
#7948 = EDGE_CURVE ( 'NONE', #51032, #3809, #50848, .T. ) ;
#7949 = DIRECTION ( 'NONE',  ( 0.000000000000000000, 0.000000000000000000, 1.000000000000000000 ) ) ;
#7950 = CARTESIAN_POINT ( 'NONE',  ( 4.458734124999999437, -81.06249999863440792, -5.460374474430324690E-16 ) ) ;
#7951 = EDGE_CURVE ( 'NONE', #49521, #2442, #39832, .T. ) ;
#7952 = CARTESIAN_POINT ( 'NONE',  ( -2.229367062499996610, -100.1458333319677365, 3.861377020970582219 ) ) ;
#7953 = CARTESIAN_POINT ( 'NONE',  ( -2.229367062499996610, -6.395833331967741842, 3.861377020970582219 ) ) ;
#7954 = ORIENTED_EDGE ( 'NONE', *, *, #58672, .T. ) ;
#7955 = CARTESIAN_POINT ( 'NONE',  ( -5.000000000000000000, -85.95833333060214443, -2.886751345948128211 ) ) ;
#7956 = CARTESIAN_POINT ( 'NONE',  ( 2.229367062499998831, -92.64583333196773651, -3.861377020970580887 ) ) ;
#7957 = EDGE_CURVE ( 'NONE', #34574, #52846, #53739, .T. ) ;
#7958 = CARTESIAN_POINT ( 'NONE',  ( -5.000000000000000888, -163.6875000027311842, -2.071067811865475949 ) ) ;
#7959 = CARTESIAN_POINT ( 'NONE',  ( 9.457646018065525792E-16, -86.31249999863440792, 5.148502694627439702 ) ) ;
#7960 = CARTESIAN_POINT ( 'NONE',  ( 4.458734124999998549, 15.02083333469892779, -2.574251347313721627 ) ) ;
#7961 = DIRECTION ( 'NONE',  ( 0.000000000000000000, 0.000000000000000000, 1.000000000000000000 ) ) ;
#7962 = AXIS2_PLACEMENT_3D ( 'NONE', #30879, #20276, #1955 ) ;
#7963 = CARTESIAN_POINT ( 'NONE',  ( -59.29741812935640155, -133.6250000013655779, -2.196230717870135685 ) ) ;
#7964 = VECTOR ( 'NONE', #29763, 1000.000000000000000 ) ;
#7965 = CARTESIAN_POINT ( 'NONE',  ( 4.458734124999998549, -10.72916666530106866, -2.574251347313721627 ) ) ;
#7966 = CARTESIAN_POINT ( 'NONE',  ( 4.458734124999998549, 15.02083333469892601, -2.574251347313721627 ) ) ;
#7967 = CARTESIAN_POINT ( 'NONE',  ( 4.458734124999998549, -54.97916666530107221, -2.574251347313721627 ) ) ;
#7968 = CARTESIAN_POINT ( 'NONE',  ( -6.972266317189433020E-16, 17.75000000000000355, -5.000000000000000000 ) ) ;
#7969 = CARTESIAN_POINT ( 'NONE',  ( -2.229367062500000163, -9.479166665301068662, -3.861377020970580443 ) ) ;
#7970 = CARTESIAN_POINT ( 'NONE',  ( -5.000000000000000000, -39.08333333333332860, -2.886751345948128211 ) ) ;
#7971 = ORIENTED_EDGE ( 'NONE', *, *, #21290, .F. ) ;
#7972 = CARTESIAN_POINT ( 'NONE',  ( 4.458734124999999437, -37.06249999863440792, -5.460374474430324690E-16 ) ) ;
#7973 =( BOUNDED_CURVE ( )  B_SPLINE_CURVE ( 2, ( #18561, #43613, #63255, #8904, #48757, #28520, #4699, #19173, #38788 ),
 .UNSPECIFIED., .F., .F. ) 
 B_SPLINE_CURVE_WITH_KNOTS ( ( 3, 2, 2, 2, 3 ),
 ( 0.9354166666666666741, 0.9361111111111111160, 0.9375000000000000000, 0.9388888888888888840, 0.9395833333333333259 ),
 .UNSPECIFIED. ) 
 CURVE ( )  GEOMETRIC_REPRESENTATION_ITEM ( )  RATIONAL_B_SPLINE_CURVE ( ( 0.9330127018922194093, 0.9330127018922194093, 1.000000000000000000, 0.8660254037844387076, 1.000000000000000000, 0.8660254037844387076, 1.000000000000000000, 0.9330127018922194093, 0.9330127018922194093 ) ) 
 REPRESENTATION_ITEM ( '' )  );
#7974 = CARTESIAN_POINT ( 'NONE',  ( -59.44456063193725015, -128.8125000013656063, -0.3552334253322034230 ) ) ;
#7975 = DIRECTION ( 'NONE',  ( -0.000000000000000000, 1.000000000000000000, -0.000000000000000000 ) ) ;
#7976 = CARTESIAN_POINT ( 'NONE',  ( -2.229367062499996610, -78.14583333196773651, 3.861377020970582219 ) ) ;
#7977 = CARTESIAN_POINT ( 'NONE',  ( 4.458734124999999437, 26.93750000136559564, -5.460374474430324690E-16 ) ) ;
#7978 = CARTESIAN_POINT ( 'NONE',  ( -4.458734124999999437, -150.1875000013656063, -5.460374474430324690E-16 ) ) ;
#7979 = CARTESIAN_POINT ( 'NONE',  ( -4.458734124999999437, 14.68750000136559386, 0.000000000000000000 ) ) ;
#7980 = CARTESIAN_POINT ( 'NONE',  ( -6.972266317189433020E-16, -82.12499999726881583, -5.000000000000000000 ) ) ;
#7981 = CARTESIAN_POINT ( 'NONE',  ( 6.123233995736766282E-16, -120.0000000000000000, -5.000000000000000000 ) ) ;
#7982 = CARTESIAN_POINT ( 'NONE',  ( -3.152548672688508926E-16, -85.81249999863440792, -5.148502694627439702 ) ) ;
#7983 = CARTESIAN_POINT ( 'NONE',  ( -2.499999999999996447, -64.83333333333332860, 4.330127018922195425 ) ) ;
#7984 = CARTESIAN_POINT ( 'NONE',  ( -2.499999999999996447, -1.708333330602145761, 4.330127018922195425 ) ) ;
#7985 = CARTESIAN_POINT ( 'NONE',  ( -4.999999999999999112, 21.20833333606451987, 2.886751345948131764 ) ) ;
#7986 = ORIENTED_EDGE ( 'NONE', *, *, #53178, .T. ) ;
#7987 = CARTESIAN_POINT ( 'NONE',  ( -55.39835681537999790, -139.0000000027312126, 4.984105922594378235 ) ) ;
#7989 = CARTESIAN_POINT ( 'NONE',  ( 5.000000000000000000, -27.41666666666666785, -2.886751345948129988 ) ) ;
#7988 = CARTESIAN_POINT ( 'NONE',  ( 1.975475456537005874E-15, -52.75000000000000000, 5.000000000000000000 ) ) ;
#7990 = CARTESIAN_POINT ( 'NONE',  ( -2.229367062499996610, -33.14583333196772941, 3.861377020970582219 ) ) ;
#7991 = CYLINDRICAL_SURFACE ( 'NONE', #57279, 5.000000000000000000 ) ;
#7992 = CARTESIAN_POINT ( 'NONE',  ( -3.535250795749689387E-16, -29.12499999726881228, -5.773502691896257311 ) ) ;
#7994 = ORIENTED_EDGE ( 'NONE', *, *, #3657, .T. ) ;
#7993 = CARTESIAN_POINT ( 'NONE',  ( 2.229367062499998831, -59.64583333196774362, -3.861377020970580887 ) ) ;
#7995 = CARTESIAN_POINT ( 'NONE',  ( 5.000000000000000000, -62.29166666393547303, -2.886751345948130876 ) ) ;
#7997 = EDGE_LOOP ( 'NONE', ( #47229, #56548, #6979, #55844 ) ) ;
#7996 = CARTESIAN_POINT ( 'NONE',  ( -4.458734124999999437, -9.562499998634406140, 0.000000000000000000 ) ) ;
#7998 = CARTESIAN_POINT ( 'NONE',  ( -3.535250795749689387E-16, -75.25000000000001421, -5.773502691896257311 ) ) ;
#7999 = CARTESIAN_POINT ( 'NONE',  ( -57.89159099828107458, -138.6875000013656347, -3.393966926194107447 ) ) ;
#8000 = CARTESIAN_POINT ( 'NONE',  ( -2.229367062500000163, -50.72916666530107221, -3.861377020970580443 ) ) ;
#8001 = VECTOR ( 'NONE', #51309, 1000.000000000000114 ) ;
#8002 = CARTESIAN_POINT ( 'NONE',  ( 1.060575238724906964E-15, -76.62499999726881583, 5.773502691896257311 ) ) ;
#8004 = ORIENTED_EDGE ( 'NONE', *, *, #14116, .T. ) ;
#8003 = DIRECTION ( 'NONE',  ( -0.000000000000000000, 1.000000000000000000, -0.000000000000000000 ) ) ;
#8005 = CARTESIAN_POINT ( 'NONE',  ( -51.75738570946856498, -148.7500000000000284, 3.805975901505576964 ) ) ;
#8006 = VECTOR ( 'NONE', #19017, 1000.000000000000000 ) ;
#8007 = CARTESIAN_POINT ( 'NONE',  ( -2.229367062499996610, -19.39583333196774007, 3.861377020970582219 ) ) ;
#8008 = CARTESIAN_POINT ( 'NONE',  ( 4.458734124999998549, -56.97916666530107932, -2.574251347313721627 ) ) ;
#8009 = DIRECTION ( 'NONE',  ( -0.000000000000000000, 1.000000000000000000, -0.000000000000000000 ) ) ;
#8010 = FILL_AREA_STYLE ('',( #27613 ) ) ;
#8011 = CARTESIAN_POINT ( 'NONE',  ( 3.152801135295366208, -141.5625000013655779, 3.152801135295367985 ) ) ;
#8012 = CARTESIAN_POINT ( 'NONE',  ( 9.457646018065525792E-16, -101.3124999986344079, 5.148502694627439702 ) ) ;
#8013 = LINE ( 'NONE', #60783, #15331 ) ;
#8014 = ORIENTED_EDGE ( 'NONE', *, *, #26443, .T. ) ;
#8015 = CARTESIAN_POINT ( 'NONE',  ( -53.51423613279429503, -151.5000000013655779, 4.591703134518083651 ) ) ;
#8016 = CARTESIAN_POINT ( 'NONE',  ( -60.14911071818854538, -142.1875000027312410, 1.666127454062681368 ) ) ;
#8017 = CARTESIAN_POINT ( 'NONE',  ( -2.229367062500000163, -6.479166665301072214, -3.861377020970580443 ) ) ;
#8018 = VECTOR ( 'NONE', #40272, 1000.000000000000000 ) ;
#8019 = CARTESIAN_POINT ( 'NONE',  ( -2.229367062500000163, -95.72916666530107932, -3.861377020970580443 ) ) ;
#8020 = CARTESIAN_POINT ( 'NONE',  ( -1.846868145590734756, -146.3750000013655779, -4.458734125000000326 ) ) ;
#8021 = CARTESIAN_POINT ( 'NONE',  ( -2.229367062500000163, -22.72916666530107221, -3.861377020970580443 ) ) ;
#8022 = FACE_OUTER_BOUND ( 'NONE', #92, .T. ) ;
#8023 = CARTESIAN_POINT ( 'NONE',  ( -59.44456063193725015, -135.5625000013656063, -0.3552334253322034230 ) ) ;
#8024 = CARTESIAN_POINT ( 'NONE',  ( -3.152548672688508926E-16, -63.81249999863440792, -5.148502694627439702 ) ) ;
#8025 = EDGE_CURVE ( 'NONE', #53443, #38064, #1980, .T. ) ;
#8026 = FACE_OUTER_BOUND ( 'NONE', #10163, .T. ) ;
#8027 = CARTESIAN_POINT ( 'NONE',  ( 1.846868145590736310, -144.6250000013655779, 4.458734124999997661 ) ) ;
#8028 = CARTESIAN_POINT ( 'NONE',  ( -2.229367062499996610, 8.604166668032261711, 3.861377020970582219 ) ) ;
#8029 = ORIENTED_EDGE ( 'NONE', *, *, #60224, .F. ) ;
#8030 = CARTESIAN_POINT ( 'NONE',  ( -6.972266317189433020E-16, -58.12499999726880162, -5.000000000000000000 ) ) ;
#8031 = EDGE_CURVE ( 'NONE', #34574, #62346, #36367, .T. ) ;
#8032 = CARTESIAN_POINT ( 'NONE',  ( 1.339745962155602488, 16.29465819873851373, 5.000000000000007105 ) ) ;
#8034 = CARTESIAN_POINT ( 'NONE',  ( -4.458734124999998549, -25.22916666530106866, 2.574251347313722516 ) ) ;
#8033 = CARTESIAN_POINT ( 'NONE',  ( -3.535250795749689387E-16, -91.25000000000000000, -5.773502691896257311 ) ) ;
#8035 = CARTESIAN_POINT ( 'NONE',  ( 1.975475456537005874E-15, -73.75000000000000000, 5.000000000000000000 ) ) ;
#8036 = CARTESIAN_POINT ( 'NONE',  ( -2.229367062500000163, -72.72916666530107932, -3.861377020970580443 ) ) ;
#8037 = CARTESIAN_POINT ( 'NONE',  ( -2.229367062500000163, 26.27083333469892779, -3.861377020970580443 ) ) ;
#8038 = CARTESIAN_POINT ( 'NONE',  ( 1.975475456537005874E-15, -17.62499999726881938, 5.000000000000000000 ) ) ;
#8039 = CARTESIAN_POINT ( 'NONE',  ( -59.29741812935640155, -145.6250000013655779, -2.196230717870135685 ) ) ;
#8040 = EDGE_CURVE ( 'NONE', #42363, #2855, #51332, .T. ) ;
#8041 = CARTESIAN_POINT ( 'NONE',  ( -2.229367062500000163, 1.520833334698927564, -3.861377020970580443 ) ) ;
#8042 = CARTESIAN_POINT ( 'NONE',  ( 6.123233995736766282E-16, -120.0000000000000000, -5.000000000000000000 ) ) ;
#8043 = DIRECTION ( 'NONE',  ( -0.000000000000000000, 1.000000000000000000, -0.000000000000000000 ) ) ;
#8044 = CARTESIAN_POINT ( 'NONE',  ( -4.458734124999999437, 5.604166668032261711, -2.574251347313719407 ) ) ;
#8045 = CARTESIAN_POINT ( 'NONE',  ( -2.229367062499996610, -74.14583333196773651, 3.861377020970582219 ) ) ;
#8046 = CARTESIAN_POINT ( 'NONE',  ( -2.229367062500000163, -20.72916666530107221, -3.861377020970580443 ) ) ;
#8047 = AXIS2_PLACEMENT_3D ( 'NONE', #4472, #38874, #54638 ) ;
#8048 = CARTESIAN_POINT ( 'NONE',  ( 2.500000000000002220, -3.666666666666665186, 4.330127018922192761 ) ) ;
#8049 = CARTESIAN_POINT ( 'NONE',  ( 2.730187237215162345E-16, -159.1875000013655779, -4.458734124999999437 ) ) ;
#8050 = DIRECTION ( 'NONE',  ( -0.000000000000000000, 1.000000000000000000, -0.000000000000000000 ) ) ;
#8051 = CARTESIAN_POINT ( 'NONE',  ( 4.458734124999999437, -62.81249999863440792, -5.460374474430324690E-16 ) ) ;
#8052 = CARTESIAN_POINT ( 'NONE',  ( -2.499999999999996447, -98.70833333060214443, 4.330127018922195425 ) ) ;
#8053 = VECTOR ( 'NONE', #36163, 1000.000000000000000 ) ;
#8054 =( BOUNDED_CURVE ( )  B_SPLINE_CURVE ( 2, ( #49891, #25455, #10975, #51188, #16448, #6487, #59892, #55376, #40879 ),
 .UNSPECIFIED., .F., .F. ) 
 B_SPLINE_CURVE_WITH_KNOTS ( ( 3, 2, 2, 2, 3 ),
 ( 0.3660714285714285476, 0.3666666666666666408, 0.3678571428571428825, 0.3690476190476190688, 0.3696428571428571619 ),
 .UNSPECIFIED. ) 
 CURVE ( )  GEOMETRIC_REPRESENTATION_ITEM ( )  RATIONAL_B_SPLINE_CURVE ( ( 0.9330127018922194093, 0.9330127018922194093, 1.000000000000000000, 0.8660254037844387076, 1.000000000000000000, 0.8660254037844387076, 1.000000000000000000, 0.9330127018922194093, 0.9330127018922194093 ) ) 
 REPRESENTATION_ITEM ( '' )  );
#8055 = CARTESIAN_POINT ( 'NONE',  ( -59.81910112700027327, -149.1875000000000284, -2.462841084822540605 ) ) ;
#8056 = CARTESIAN_POINT ( 'NONE',  ( -2.229367062500000163, -40.47916666530107221, -3.861377020970580443 ) ) ;
#8057 = CARTESIAN_POINT ( 'NONE',  ( -2.229367062500000163, -104.7291666653010651, -3.861377020970580443 ) ) ;
#8058 = CARTESIAN_POINT ( 'NONE',  ( 4.458734125000000326, -70.14583333196773651, 2.574251347313718519 ) ) ;
#8059 = CARTESIAN_POINT ( 'NONE',  ( -2.500000000000000444, -51.16666666666666430, -4.330127018922193649 ) ) ;
#8060 = CARTESIAN_POINT ( 'NONE',  ( -4.999999999999998224, 27.08333333333333215, 2.886751345948131764 ) ) ;
#8061 = CARTESIAN_POINT ( 'NONE',  ( 5.000000000000000000, -36.29166666393547303, -2.886751345948130876 ) ) ;
#8062 = VERTEX_POINT ( 'NONE', #3857 ) ;
#8063 = CARTESIAN_POINT ( 'NONE',  ( -2.229367062499996610, -110.1458333319677365, 3.861377020970582219 ) ) ;
#8064 = CARTESIAN_POINT ( 'NONE',  ( -6.972266317189433020E-16, -100.1249999972688016, -5.000000000000000000 ) ) ;
#8065 = CARTESIAN_POINT ( 'NONE',  ( -5.000000000000000000, -15.00000000000000000, 0.000000000000000000 ) ) ;
#8066 = CARTESIAN_POINT ( 'NONE',  ( -4.458734124999998549, -16.22916666530107577, 2.574251347313722516 ) ) ;
#8067 = CARTESIAN_POINT ( 'NONE',  ( 2.229367062500001939, -76.97916666530106511, 3.861377020970579999 ) ) ;
#8069 = LINE ( 'NONE', #52755, #13406 ) ;
#8068 =( BOUNDED_CURVE ( )  B_SPLINE_CURVE ( 2, ( #60282, #55128, #60917, #2071, #35194, #11055, #10741, #30349, #30678 ),
 .UNSPECIFIED., .F., .F. ) 
 B_SPLINE_CURVE_WITH_KNOTS ( ( 3, 2, 2, 2, 3 ),
 ( 0.001785714285714286092, 0.002380952380952381167, 0.003571428571428571317, 0.004761904761904762334, 0.005357142857142858060 ),
 .UNSPECIFIED. ) 
 CURVE ( )  GEOMETRIC_REPRESENTATION_ITEM ( )  RATIONAL_B_SPLINE_CURVE ( ( 0.9330127018922194093, 0.9330127018922194093, 1.000000000000000000, 0.8660254037844387076, 1.000000000000000000, 0.8660254037844387076, 1.000000000000000000, 0.9330127018922191873, 0.9330127018922192983 ) ) 
 REPRESENTATION_ITEM ( '' )  );
#8070 = CARTESIAN_POINT ( 'NONE',  ( -3.535250795749689387E-16, -15.12499999726881406, -5.773502691896257311 ) ) ;
#8072 = ORIENTED_EDGE ( 'NONE', *, *, #17948, .T. ) ;
#8071 = CARTESIAN_POINT ( 'NONE',  ( -4.458734124999999437, -45.31249999863440081, 0.000000000000000000 ) ) ;
#8073 = CARTESIAN_POINT ( 'NONE',  ( 2.071067811865517694, -143.8125000000000000, -4.999999999999958256 ) ) ;
#8075 = ORIENTED_EDGE ( 'NONE', *, *, #61113, .F. ) ;
#8074 = CARTESIAN_POINT ( 'NONE',  ( -2.229367062499996610, 6.604166668032259935, 3.861377020970582219 ) ) ;
#8076 = CARTESIAN_POINT ( 'NONE',  ( -5.000000000000000000, -151.5000000000000284, -6.123233995736766282E-16 ) ) ;
#8077 = CARTESIAN_POINT ( 'NONE',  ( 2.500000000000002220, -53.66666666666667140, 4.330127018922192761 ) ) ;
#8078 = CARTESIAN_POINT ( 'NONE',  ( 2.730187237215162345E-16, -160.4375000013655779, -4.458734124999999437 ) ) ;
#8079 = CARTESIAN_POINT ( 'NONE',  ( 4.458734124999999437, -38.06249999863440792, -5.460374474430324690E-16 ) ) ;
#8080 = CARTESIAN_POINT ( 'NONE',  ( -2.499999999999996447, -10.70833333060214621, 4.330127018922195425 ) ) ;
#8081 = CARTESIAN_POINT ( 'NONE',  ( -3.152548672688508926E-16, -78.56249999863440792, -5.148502694627439702 ) ) ;
#8082 = CARTESIAN_POINT ( 'NONE',  ( -3.535533905932738641, -167.3750000000000284, 3.535533905932737309 ) ) ;
#8083 = CARTESIAN_POINT ( 'NONE',  ( -1.339745962155610925, -29.79465819873851729, 5.000000000000000000 ) ) ;
#8084 = CARTESIAN_POINT ( 'NONE',  ( -50.55543936806279248, -132.3125000013656063, 0.3552334253322060320 ) ) ;
#8085 = CARTESIAN_POINT ( 'NONE',  ( -2.229367062500000163, -2.729166665301069550, -3.861377020970580443 ) ) ;
#8086 = CARTESIAN_POINT ( 'NONE',  ( 4.458734124999999437, -41.06249999863440081, -5.460374474430324690E-16 ) ) ;
#8087 = CARTESIAN_POINT ( 'NONE',  ( -6.972266317189433020E-16, -47.25000000000000000, -5.000000000000000000 ) ) ;
#8088 = CARTESIAN_POINT ( 'NONE',  ( -4.458734124999999437, -85.64583333196773651, -2.574251347313719407 ) ) ;
#8089 = DIRECTION ( 'NONE',  ( -0.000000000000000000, 1.000000000000000000, -0.000000000000000000 ) ) ;
#8090 = ORIENTED_EDGE ( 'NONE', *, *, #33768, .F. ) ;
#8091 = CARTESIAN_POINT ( 'NONE',  ( -50.18089887299979068, -153.8125000027312126, 2.462841084822635640 ) ) ;
#8092 = AXIS2_PLACEMENT_3D ( 'NONE', #59387, #53604, #54563 ) ;
#8093 = CARTESIAN_POINT ( 'NONE',  ( -4.458734124999999437, -67.56249999863440792, 0.000000000000000000 ) ) ;
#8094 = AXIS2_PLACEMENT_3D ( 'NONE', #33290, #39363, #28769 ) ;
#8095 = CARTESIAN_POINT ( 'NONE',  ( -4.458734124999999437, -7.645833331967735624, -2.574251347313719407 ) ) ;
#8096 = ORIENTED_EDGE ( 'NONE', *, *, #14246, .T. ) ;
#8097 = CARTESIAN_POINT ( 'NONE',  ( 2.071067811865540342, -164.1875000000000000, 4.999999999999936051 ) ) ;
#8098 = DIRECTION ( 'NONE',  ( 0.000000000000000000, 0.000000000000000000, 1.000000000000000000 ) ) ;
#8099 = CARTESIAN_POINT ( 'NONE',  ( -3.152548672688508926E-16, -5.812499998634404363, -5.148502694627439702 ) ) ;
#8100 = DIRECTION ( 'NONE',  ( 1.000000000000000000, 0.000000000000000000, -0.000000000000000000 ) ) ;
#8101 = CARTESIAN_POINT ( 'NONE',  ( 4.458734124999999437, 0.1875000013655953035, -5.460374474430324690E-16 ) ) ;
#8102 = CARTESIAN_POINT ( 'NONE',  ( 1.975475456537005874E-15, -42.75000000000000000, 5.000000000000000000 ) ) ;
#8103 = CARTESIAN_POINT ( 'NONE',  ( -8.190561711645485556E-16, -156.6875000013655779, 4.458734124999999437 ) ) ;
#8104 = CARTESIAN_POINT ( 'NONE',  ( -2.229367062499996610, 25.60416666803225993, 3.861377020970582219 ) ) ;
#8105 = VERTEX_POINT ( 'NONE', #37010 ) ;
#8106 = CARTESIAN_POINT ( 'NONE',  ( -2.229367062499996610, -90.14583333196773651, 3.861377020970582219 ) ) ;
#8107 = CARTESIAN_POINT ( 'NONE',  ( -5.000000000000000000, -25.00000000000000000, 0.000000000000000000 ) ) ;
#8108 = CARTESIAN_POINT ( 'NONE',  ( -2.229367062500000163, -8.479166665301073991, -3.861377020970580443 ) ) ;
#8109 = CARTESIAN_POINT ( 'NONE',  ( 5.040301471719072168, 5.750234626350511746, -0.09933465333851003443 ) ) ;
#8110 = DIRECTION ( 'NONE',  ( -0.000000000000000000, 1.000000000000000000, -0.000000000000000000 ) ) ;
#8111 = DIRECTION ( 'NONE',  ( 0.000000000000000000, 0.000000000000000000, 1.000000000000000000 ) ) ;
#8112 = CARTESIAN_POINT ( 'NONE',  ( 1.060575238724906964E-15, -37.62499999726881583, 5.773502691896257311 ) ) ;
#8113 = CARTESIAN_POINT ( 'NONE',  ( 0.000000000000000000, -120.0000000000000000, 0.000000000000000000 ) ) ;
#8114 = CARTESIAN_POINT ( 'NONE',  ( -2.229367062499996610, 19.85416666803225993, 3.861377020970582219 ) ) ;
#8115 = CARTESIAN_POINT ( 'NONE',  ( -2.499999999999996447, -97.70833333060213022, 4.330127018922195425 ) ) ;
#8116 = CARTESIAN_POINT ( 'NONE',  ( -4.458734124999997661, 20.77083333469892779, 2.574251347313722516 ) ) ;
#8117 = CARTESIAN_POINT ( 'NONE',  ( 4.458734124999998549, -56.72916666530107932, -2.574251347313721627 ) ) ;
#8118 = CARTESIAN_POINT ( 'NONE',  ( 4.458734125000000326, -3.145833331967738289, 2.574251347313718519 ) ) ;
#8119 =( BOUNDED_CURVE ( )  B_SPLINE_CURVE ( 2, ( #62410, #56642, #12556, #13516, #8678, #32814, #56951, #46980, #2928 ),
 .UNSPECIFIED., .F., .F. ) 
 B_SPLINE_CURVE_WITH_KNOTS ( ( 3, 2, 2, 2, 3 ),
 ( 0.8874999999999999556, 0.8880952380952380487, 0.8892857142857142350, 0.8904761904761904212, 0.8910714285714286254 ),
 .UNSPECIFIED. ) 
 CURVE ( )  GEOMETRIC_REPRESENTATION_ITEM ( )  RATIONAL_B_SPLINE_CURVE ( ( 0.9330127018922194093, 0.9330127018922194093, 1.000000000000000000, 0.8660254037844387076, 1.000000000000000000, 0.8660254037844387076, 1.000000000000000000, 0.9330127018922130810, 0.9330127018922194093 ) ) 
 REPRESENTATION_ITEM ( '' )  );
#8120 = LINE ( 'NONE', #42828, #48329 ) ;
#8121 = CARTESIAN_POINT ( 'NONE',  ( -2.500000000000000444, 12.83333333333333215, -4.330127018922193649 ) ) ;
#8122 = CARTESIAN_POINT ( 'NONE',  ( 5.000000000000000000, -143.1875000027312126, 2.071067811865478614 ) ) ;
#8123 = CARTESIAN_POINT ( 'NONE',  ( 0.000000000000000000, -170.0000000000000000, 5.000000000000000000 ) ) ;
#8124 = CARTESIAN_POINT ( 'NONE',  ( -4.458734124999998549, -50.22916666530107221, 2.574251347313722516 ) ) ;
#8125 = CARTESIAN_POINT ( 'NONE',  ( -5.000000000000000000, -83.87499999726880162, 0.000000000000000000 ) ) ;
#8126 = CARTESIAN_POINT ( 'NONE',  ( -59.29741812935640155, -134.8750000013656063, -2.196230717870135685 ) ) ;
#8127 = CARTESIAN_POINT ( 'NONE',  ( -1.339745962155610925, -86.79465819873851729, 5.000000000000000000 ) ) ;
#8128 = DIRECTION ( 'NONE',  ( -0.000000000000000000, 1.000000000000000000, -0.000000000000000000 ) ) ;
#8129 = CARTESIAN_POINT ( 'NONE',  ( -4.458734124999999437, -85.56249999863439371, 0.000000000000000000 ) ) ;
#8130 = CARTESIAN_POINT ( 'NONE',  ( 4.458734124999997661, -155.7500000013656063, 1.846868145590737864 ) ) ;
#8131 = CARTESIAN_POINT ( 'NONE',  ( -2.499999999999996447, -33.83333333333332860, 4.330127018922195425 ) ) ;
#8132 = CARTESIAN_POINT ( 'NONE',  ( -5.000000000000000000, -147.5000000000000284, -6.123233995736766282E-16 ) ) ;
#8133 = ORIENTED_EDGE ( 'NONE', *, *, #7073, .F. ) ;
#8134 = CARTESIAN_POINT ( 'NONE',  ( 4.458734125000001214, 17.85416666803225993, 2.574251347313718519 ) ) ;
#8135 = EDGE_LOOP ( 'NONE', ( #50665, #37197, #38735 ) ) ;
#8136 = CARTESIAN_POINT ( 'NONE',  ( 2.229367062500001939, -93.97916666530106511, 3.861377020970579999 ) ) ;
#8137 = CARTESIAN_POINT ( 'NONE',  ( -4.458734124999999437, 7.437500001365594748, 0.000000000000000000 ) ) ;
#8138 = VECTOR ( 'NONE', #55451, 1000.000000000000000 ) ;
#8139 = CARTESIAN_POINT ( 'NONE',  ( -2.500000000000000444, 11.95833333606451809, -4.330127018922193649 ) ) ;
#8140 = CARTESIAN_POINT ( 'NONE',  ( -1.339745962155610925, -43.66965819600732601, 5.000000000000000000 ) ) ;
#8141 = CARTESIAN_POINT ( 'NONE',  ( -2.500000000000000444, 8.833333333333332149, -4.330127018922193649 ) ) ;
#8142 = EDGE_CURVE ( 'NONE', #35996, #18224, #60348, .T. ) ;
#8143 = AXIS2_PLACEMENT_3D ( 'NONE', #43885, #39069, #58698 ) ;
#8144 = CARTESIAN_POINT ( 'NONE',  ( -4.458734124999999437, -61.31249999863440081, 0.000000000000000000 ) ) ;
#8145 = CARTESIAN_POINT ( 'NONE',  ( -6.972266317189433020E-16, -8.249999999999998224, -5.000000000000000000 ) ) ;
#8146 = CARTESIAN_POINT ( 'NONE',  ( -3.535250795749689387E-16, -79.25000000000000000, -5.773502691896257311 ) ) ;
#8147 = CARTESIAN_POINT ( 'NONE',  ( 4.458734124999999437, -30.81249999863440436, -5.460374474430324690E-16 ) ) ;
#8148 = CARTESIAN_POINT ( 'NONE',  ( -6.972266317189433020E-16, -38.12499999726880873, -5.000000000000000000 ) ) ;
#8149 = CARTESIAN_POINT ( 'NONE',  ( -2.499999999999996447, -12.70833333060214798, 4.330127018922195425 ) ) ;
#8150 = CARTESIAN_POINT ( 'NONE',  ( -55.00000000000002132, -155.0000000000000284, 1.734723475976807094E-15 ) ) ;
#8151 = CARTESIAN_POINT ( 'NONE',  ( -2.499999999999996447, -40.83333333333333570, 4.330127018922195425 ) ) ;
#8152 = CARTESIAN_POINT ( 'NONE',  ( 1.339745962155612702, -107.2946581987385315, -5.000000000000000000 ) ) ;
#8153 =( BOUNDED_CURVE ( )  B_SPLINE_CURVE ( 2, ( #22628, #37407, #57042, #29632, #59234, #4258, #47996, #48620, #23873 ),
 .UNSPECIFIED., .F., .F. ) 
 B_SPLINE_CURVE_WITH_KNOTS ( ( 3, 2, 2, 2, 3 ),
 ( 0.5250000000000004663, 0.5291666666666671182, 0.5333333333333338810, 0.5375000000000005329, 0.5416666666666671848 ),
 .UNSPECIFIED. ) 
 CURVE ( )  GEOMETRIC_REPRESENTATION_ITEM ( )  RATIONAL_B_SPLINE_CURVE ( ( 0.9999999999999918954, 0.9238795325112948431, 1.000000000000000000, 0.9238795325112867385, 1.000000000000000000, 0.9238795325112867385, 1.000000000000000000, 0.9238795325112766355, 1.000000000000010214 ) ) 
 REPRESENTATION_ITEM ( '' )  );
#8155 = CARTESIAN_POINT ( 'NONE',  ( -2.229367062499996610, -22.39583333196773651, 3.861377020970582219 ) ) ;
#8154 = CARTESIAN_POINT ( 'NONE',  ( -5.000000000000000000, -48.08333333333332860, -2.886751345948128211 ) ) ;
#8156 = CARTESIAN_POINT ( 'NONE',  ( -2.500000000000000444, 12.83333333333333215, -4.330127018922193649 ) ) ;
#8157 = CARTESIAN_POINT ( 'NONE',  ( -2.229367062500000163, -67.47916666530106511, -3.861377020970580443 ) ) ;
#8158 = CARTESIAN_POINT ( 'NONE',  ( -1.846868145590737420, -148.0000000013655779, 4.458734124999999437 ) ) ;
#8159 = CARTESIAN_POINT ( 'NONE',  ( -4.458734124999998549, -72.22916666530107932, 2.574251347313722516 ) ) ;
#8160 = CARTESIAN_POINT ( 'NONE',  ( -59.44456063193725015, -142.8125000013656063, -0.3552334253322034230 ) ) ;
#8161 = CARTESIAN_POINT ( 'NONE',  ( 4.458734124999998549, -25.97916666530106866, -2.574251347313721627 ) ) ;
#8162 = CARTESIAN_POINT ( 'NONE',  ( -3.535250795749689387E-16, -64.12499999726881583, -5.773502691896257311 ) ) ;
#8163 = ORIENTED_EDGE ( 'NONE', *, *, #20453, .F. ) ;
#8164 = CARTESIAN_POINT ( 'NONE',  ( -55.39835681537999790, -148.0000000027312126, 4.984105922594378235 ) ) ;
#8165 = VERTEX_POINT ( 'NONE', #32166 ) ;
#8166 = CARTESIAN_POINT ( 'NONE',  ( -4.458734124999998549, -66.47916666530106511, 2.574251347313722516 ) ) ;
#8167 = CARTESIAN_POINT ( 'NONE',  ( 2.500000000000002220, -21.54166666393548013, 4.330127018922192761 ) ) ;
#8168 = CARTESIAN_POINT ( 'NONE',  ( 0.000000000000000000, 0.000000000000000000, -9.974600000000000577 ) ) ;
#8169 = ORIENTED_EDGE ( 'NONE', *, *, #43621, .T. ) ;
#8170 = CARTESIAN_POINT ( 'NONE',  ( -60.14911071818854538, -125.0625000000000142, 1.666127454062681368 ) ) ;
#8171 = PLANE ( 'NONE',  #2154 ) ;
#8172 = CARTESIAN_POINT ( 'NONE',  ( -4.458734124999998549, -52.47916666530107221, 2.574251347313722516 ) ) ;
#8173 = VERTEX_POINT ( 'NONE', #57586 ) ;
#8174 = DIRECTION ( 'NONE',  ( -0.000000000000000000, 1.000000000000000000, -0.000000000000000000 ) ) ;
#8175 = CARTESIAN_POINT ( 'NONE',  ( 4.458734124999998549, 7.270833334698928674, -2.574251347313721627 ) ) ;
#8176 = CARTESIAN_POINT ( 'NONE',  ( -4.458734124999999437, 18.60416666803225993, -2.574251347313719407 ) ) ;
#8177 = CARTESIAN_POINT ( 'NONE',  ( -55.35523342533222291, -148.3125000013656063, 4.444560631937231499 ) ) ;
#8178 = DIRECTION ( 'NONE',  ( -0.000000000000000000, 1.000000000000000000, -0.000000000000000000 ) ) ;
#8179 = ORIENTED_EDGE ( 'NONE', *, *, #36256, .F. ) ;
#8180 = CARTESIAN_POINT ( 'NONE',  ( -4.458734124999997661, -72.22916666530107932, 2.574251347313722516 ) ) ;
#8181 = CARTESIAN_POINT ( 'NONE',  ( -1.339745962155613812, -40.20534180126147561, -5.000000000000000000 ) ) ;
#8182 = CARTESIAN_POINT ( 'NONE',  ( -4.458734124999999437, 5.687500001365592972, 0.000000000000000000 ) ) ;
#8183 = VECTOR ( 'NONE', #20867, 1000.000000000000000 ) ;
#8184 = CARTESIAN_POINT ( 'NONE',  ( 2.499999999999998668, -69.20833333060214443, -4.330127018922193649 ) ) ;
#8185 = CARTESIAN_POINT ( 'NONE',  ( 4.458734125000001214, -62.14583333196774362, 2.574251347313718519 ) ) ;
#8186 = CARTESIAN_POINT ( 'NONE',  ( -3.535250795749689387E-16, -21.12499999726881228, -5.773502691896257311 ) ) ;
#8187 = CARTESIAN_POINT ( 'NONE',  ( 2.500000000000002220, 4.333333333333331261, 4.330127018922192761 ) ) ;
#8188 = LINE ( 'NONE', #46155, #22418 ) ;
#8189 = CARTESIAN_POINT ( 'NONE',  ( 5.000000000000000000, -76.41666666666665719, -2.886751345948130876 ) ) ;
#8190 = DIRECTION ( 'NONE',  ( -0.000000000000000000, 1.000000000000000000, -0.000000000000000000 ) ) ;
#8191 = CARTESIAN_POINT ( 'NONE',  ( 4.458734124999998549, -42.72916666530107221, -2.574251347313721627 ) ) ;
#8192 = CARTESIAN_POINT ( 'NONE',  ( -4.458734124999999437, -22.56249999863440436, 0.000000000000000000 ) ) ;
#8193 = VERTEX_POINT ( 'NONE', #32811 ) ;
#8194 = DIRECTION ( 'NONE',  ( 0.000000000000000000, 1.000000000000000000, 0.000000000000000000 ) ) ;
#8195 = CARTESIAN_POINT ( 'NONE',  ( 4.458734124999998549, -108.7291666653010651, -2.574251347313721627 ) ) ;
#8196 = CARTESIAN_POINT ( 'NONE',  ( 2.071067811865476394, -153.3125000027311842, 5.000000000000000000 ) ) ;
#8197 = ORIENTED_EDGE ( 'NONE', *, *, #14608, .F. ) ;
#8198 = CARTESIAN_POINT ( 'NONE',  ( 4.458734124999999437, -109.0624999986343937, -5.460374474430324690E-16 ) ) ;
#8199 = CARTESIAN_POINT ( 'NONE',  ( 9.457646018065525792E-16, -32.06249999863440792, 5.148502694627439702 ) ) ;
#8200 = CARTESIAN_POINT ( 'NONE',  ( 5.000000000000000888, -68.45833333060214443, 2.886751345948126879 ) ) ;
#8201 = CARTESIAN_POINT ( 'NONE',  ( -57.89159099828107458, -148.9375000013656063, -3.393966926194107447 ) ) ;
#8202 = CARTESIAN_POINT ( 'NONE',  ( 3.535533905932736864, -146.1250000000000000, 3.535533905932738641 ) ) ;
#8203 = CARTESIAN_POINT ( 'NONE',  ( 2.229367062499998831, -27.64583333196774007, -3.861377020970580887 ) ) ;
#8204 = CARTESIAN_POINT ( 'NONE',  ( 2.229367062499998831, -70.89583333196773651, -3.861377020970580887 ) ) ;
#8205 = CARTESIAN_POINT ( 'NONE',  ( 4.458734124999999437, -168.6875000013656063, 0.000000000000000000 ) ) ;
#8206 = CARTESIAN_POINT ( 'NONE',  ( -4.458734124999999437, -22.39583333196773651, -2.574251347313719407 ) ) ;
#8207 = CARTESIAN_POINT ( 'NONE',  ( 5.000000000000000000, -147.0625000000000000, 2.071067811865478614 ) ) ;
#8208 = CARTESIAN_POINT ( 'NONE',  ( 1.339745962155612702, -5.169658196007333117, -5.000000000000000000 ) ) ;
#8209 = CARTESIAN_POINT ( 'NONE',  ( 2.500000000000002220, -16.66666666666666430, 4.330127018922192761 ) ) ;
#8210 = CARTESIAN_POINT ( 'NONE',  ( -4.458734125000000326, -147.0000000013655779, -1.846868145590735644 ) ) ;
#8211 = ORIENTED_EDGE ( 'NONE', *, *, #29539, .F. ) ;
#8212 = LINE ( 'NONE', #37170, #54307 ) ;
#8213 = CARTESIAN_POINT ( 'NONE',  ( 4.458734124999999437, -54.06249999863440081, -5.460374474430324690E-16 ) ) ;
#8214 = CARTESIAN_POINT ( 'NONE',  ( -2.500000000000000444, -3.041666663935477910, -4.330127018922193649 ) ) ;
#8215 = CARTESIAN_POINT ( 'NONE',  ( -2.500000000000000444, -1.166666666666666519, -4.330127018922193649 ) ) ;
#8216 = CARTESIAN_POINT ( 'NONE',  ( -5.000000000000000000, 23.91666666666666785, -2.886751345948128211 ) ) ;
#8217 = EDGE_CURVE ( 'NONE', #4014, #57905, #47290, .T. ) ;
#8218 = CARTESIAN_POINT ( 'NONE',  ( 5.000000000000000000, -76.29166666393547303, -2.886751345948130876 ) ) ;
#8219 = CARTESIAN_POINT ( 'NONE',  ( -4.458734124999998549, -1.229166665301071326, 2.574251347313722516 ) ) ;
#8220 = CARTESIAN_POINT ( 'NONE',  ( 1.975475456537005874E-15, -51.62499999726880873, 5.000000000000000000 ) ) ;
#8221 = CARTESIAN_POINT ( 'NONE',  ( 5.000000000000000000, -14.41666666666666785, -2.886751345948130876 ) ) ;
#8222 = CARTESIAN_POINT ( 'NONE',  ( -4.458734124999999437, 12.43750000136559564, 0.000000000000000000 ) ) ;
#8223 = ORIENTED_EDGE ( 'NONE', *, *, #10605, .T. ) ;
#8224 = ORIENTED_EDGE ( 'NONE', *, *, #42758, .T. ) ;
#8225 = AXIS2_PLACEMENT_3D ( 'NONE', #57221, #8325, #48489 ) ;
#8226 = DIRECTION ( 'NONE',  ( -1.000000000000000000, 0.000000000000000000, 0.000000000000000000 ) ) ;
#8227 = CARTESIAN_POINT ( 'NONE',  ( 2.229367062499998831, -47.64583333196774362, -3.861377020970580887 ) ) ;
#8228 = CARTESIAN_POINT ( 'NONE',  ( -4.458734124999999437, -161.1875000013655779, -5.460374474430324690E-16 ) ) ;
#8229 = VECTOR ( 'NONE', #45713, 1000.000000000000000 ) ;
#8230 = EDGE_CURVE ( 'NONE', #1775, #52605, #53367, .T. ) ;
#8231 = CARTESIAN_POINT ( 'NONE',  ( -5.000000000000000000, -42.95833333060214443, -2.886751345948128211 ) ) ;
#8232 = ORIENTED_EDGE ( 'NONE', *, *, #2887, .T. ) ;
#8234 = EDGE_CURVE ( 'NONE', #37866, #31992, #42295, .T. ) ;
#8233 = CARTESIAN_POINT ( 'NONE',  ( -2.229367062500000163, -24.47916666530106866, -3.861377020970580443 ) ) ;
#8235 = EDGE_LOOP ( 'NONE', ( #8723, #3372, #29083, #6820, #20413, #58877, #47439 ) ) ;
#8236 = CARTESIAN_POINT ( 'NONE',  ( 1.339745962155612702, -53.29465819873850307, -5.000000000000000000 ) ) ;
#8237 = CARTESIAN_POINT ( 'NONE',  ( 2.730187237215162345E-16, -162.1875000013655779, -4.458734124999999437 ) ) ;
#8238 = CARTESIAN_POINT ( 'NONE',  ( -58.24261429053147765, -155.0000000000000284, -3.805975901505573411 ) ) ;
#8239 = CARTESIAN_POINT ( 'NONE',  ( -54.60164318462004474, -139.3750000000000284, -4.984105922594373794 ) ) ;
#8240 = CARTESIAN_POINT ( 'NONE',  ( -4.458734124999999437, -39.56249999863440081, 0.000000000000000000 ) ) ;
#8241 = CARTESIAN_POINT ( 'NONE',  ( -5.000000000000000000, 20.12500000273118772, 0.000000000000000000 ) ) ;
#8242 = ORIENTED_EDGE ( 'NONE', *, *, #4501, .F. ) ;
#8243 = EDGE_CURVE ( 'NONE', #58694, #49521, #62411, .T. ) ;
#8244 =( BOUNDED_CURVE ( )  B_SPLINE_CURVE ( 2, ( #44129, #38369, #57995, #43498, #48020, #96, #57378, #58310, #33858 ),
 .UNSPECIFIED., .F., .F. ) 
 B_SPLINE_CURVE_WITH_KNOTS ( ( 3, 2, 2, 2, 3 ),
 ( 0.9395833333333333259, 0.9402777777777777679, 0.9416666666666666519, 0.9430555555555555358, 0.9437499999999999778 ),
 .UNSPECIFIED. ) 
 CURVE ( )  GEOMETRIC_REPRESENTATION_ITEM ( )  RATIONAL_B_SPLINE_CURVE ( ( 0.9330127018922194093, 0.9330127018922194093, 1.000000000000000000, 0.8660254037844387076, 1.000000000000000000, 0.8660254037844387076, 1.000000000000000000, 0.9330127018922194093, 0.9330127018922194093 ) ) 
 REPRESENTATION_ITEM ( '' )  );
#8245 = CARTESIAN_POINT ( 'NONE',  ( 9.457646018065525792E-16, -85.06249999863440792, 5.148502694627439702 ) ) ;
#8246 = CARTESIAN_POINT ( 'NONE',  ( -2.229367062499996610, 23.85416666803225993, 3.861377020970582219 ) ) ;
#8247 = DIRECTION ( 'NONE',  ( -0.000000000000000000, 1.000000000000000000, -0.000000000000000000 ) ) ;
#8248 = ORIENTED_EDGE ( 'NONE', *, *, #20126, .T. ) ;
#8249 = FACE_OUTER_BOUND ( 'NONE', #52274, .T. ) ;
#8250 = CARTESIAN_POINT ( 'NONE',  ( -50.55543936806279248, -140.3125000013656063, 0.3552334253322060320 ) ) ;
#8251 = CARTESIAN_POINT ( 'NONE',  ( -4.458734124999998549, -88.47916666530107932, 2.574251347313722516 ) ) ;
#8252 = CARTESIAN_POINT ( 'NONE',  ( -50.18089887299979068, -129.8125000027312126, 2.462841084822635640 ) ) ;
#8253 = DIRECTION ( 'NONE',  ( -0.000000000000000000, 1.000000000000000000, -0.000000000000000000 ) ) ;
#8254 = CARTESIAN_POINT ( 'NONE',  ( -4.458734125000000326, -140.1250000013656347, 1.846868145590734089 ) ) ;
#8255 = CARTESIAN_POINT ( 'NONE',  ( 1.975475456537005874E-15, -57.74999999999999289, 5.000000000000000000 ) ) ;
#8256 = CARTESIAN_POINT ( 'NONE',  ( -4.458734124999999437, -52.39583333196773651, -2.574251347313719407 ) ) ;
#8257 = CARTESIAN_POINT ( 'NONE',  ( 2.229367062499998831, 23.35416666803225993, -3.861377020970580887 ) ) ;
#8258 = CARTESIAN_POINT ( 'NONE',  ( -2.499999999999996447, -107.8333333333333428, 4.330127018922195425 ) ) ;
#8259 = CARTESIAN_POINT ( 'NONE',  ( -5.000000000000000000, -44.08333333333333570, -2.886751345948128211 ) ) ;
#8260 = CARTESIAN_POINT ( 'NONE',  ( 9.457646018065525792E-16, -43.31249999863440792, 5.148502694627439702 ) ) ;
#8261 = ADVANCED_FACE ( 'NONE', ( #61147 ), #52440, .F. ) ;
#8262 = CARTESIAN_POINT ( 'NONE',  ( -5.000000000000000000, -5.874999997268811391, 0.000000000000000000 ) ) ;
#8263 = DIRECTION ( 'NONE',  ( -0.000000000000000000, 1.000000000000000000, -0.000000000000000000 ) ) ;
#8264 = CARTESIAN_POINT ( 'NONE',  ( -1.339745962155610925, -45.66965819600733312, 5.000000000000000000 ) ) ;
#8265 = CARTESIAN_POINT ( 'NONE',  ( 2.229367062499998831, -84.89583333196773651, -3.861377020970580887 ) ) ;
#8266 = CARTESIAN_POINT ( 'NONE',  ( -4.458734124999999437, -103.3124999986344079, 0.000000000000000000 ) ) ;
#8267 = CARTESIAN_POINT ( 'NONE',  ( 4.458734125000000326, -5.145833331967740065, 2.574251347313718519 ) ) ;
#8268 = ORIENTED_EDGE ( 'NONE', *, *, #7152, .F. ) ;
#8269 = CARTESIAN_POINT ( 'NONE',  ( -2.229367062500000163, -91.47916666530106511, -3.861377020970580443 ) ) ;
#8270 = CARTESIAN_POINT ( 'NONE',  ( 3.535533905932738197, -167.0000000027312126, -3.535533905932738197 ) ) ;
#8271 = CARTESIAN_POINT ( 'NONE',  ( -3.152548672688508926E-16, -90.81249999863440792, -5.148502694627439702 ) ) ;
#8272 = CARTESIAN_POINT ( 'NONE',  ( -4.458734124999999437, 8.354166668032261711, -2.574251347313719407 ) ) ;
#8273 = CARTESIAN_POINT ( 'NONE',  ( -4.999999999999998224, -15.91666666666666963, 2.886751345948131764 ) ) ;
#8274 = CARTESIAN_POINT ( 'NONE',  ( -57.89159099828107458, -131.6875000013656063, -3.393966926194107447 ) ) ;
#8275 = CARTESIAN_POINT ( 'NONE',  ( 4.458734124999998549, -13.72916666530107399, -2.574251347313721627 ) ) ;
#8276 = CARTESIAN_POINT ( 'NONE',  ( 4.458734125000001214, 13.85416666803226171, 2.574251347313718519 ) ) ;
#8277 = CARTESIAN_POINT ( 'NONE',  ( 4.458734124999999437, -56.06249999863440081, -5.460374474430324690E-16 ) ) ;
#8278 = CYLINDRICAL_SURFACE ( 'NONE', #24380, 5.000000000000000000 ) ;
#8279 = CARTESIAN_POINT ( 'NONE',  ( -6.972266317189433020E-16, -57.25000000000000000, -5.000000000000000000 ) ) ;
#8280 = CARTESIAN_POINT ( 'NONE',  ( 9.457646018065525792E-16, -7.062499998634404363, 5.148502694627439702 ) ) ;
#8281 = CARTESIAN_POINT ( 'NONE',  ( -6.972266317189433020E-16, -84.24999999999998579, -5.000000000000000000 ) ) ;
#8282 = ORIENTED_EDGE ( 'NONE', *, *, #6766, .F. ) ;
#8283 = CARTESIAN_POINT ( 'NONE',  ( 9.457646018065525792E-16, -33.31249999863440792, 5.148502694627439702 ) ) ;
#8284 = CARTESIAN_POINT ( 'NONE',  ( -57.19623071787017210, -127.6250000013656205, 4.297418129356382899 ) ) ;
#8285 = CARTESIAN_POINT ( 'NONE',  ( 2.500000000000002220, 26.45833333606451632, 4.330127018922192761 ) ) ;
#8286 = LINE ( 'NONE', #21893, #25476 ) ;
#8287 = CARTESIAN_POINT ( 'NONE',  ( -3.152548672688508926E-16, -78.56249999863440792, -5.148502694627439702 ) ) ;
#8288 = CARTESIAN_POINT ( 'NONE',  ( -3.152548672688508926E-16, 25.18750000136558853, -5.148502694627439702 ) ) ;
#8289 = EDGE_CURVE ( 'NONE', #29366, #24051, #59970, .T. ) ;
#8290 = CARTESIAN_POINT ( 'NONE',  ( -4.458734124999999437, 17.60416666803225993, -2.574251347313719407 ) ) ;
#8291 = EDGE_CURVE ( 'NONE', #39751, #32568, #34366, .T. ) ;
#8292 = EDGE_CURVE ( 'NONE', #34281, #23906, #46435, .T. ) ;
#8293 = CARTESIAN_POINT ( 'NONE',  ( -1.339745962155613812, 6.794658198738520838, -5.000000000000000000 ) ) ;
#8294 = FACE_OUTER_BOUND ( 'NONE', #507, .T. ) ;
#8295 = CARTESIAN_POINT ( 'NONE',  ( -4.458734124999999437, -83.64583333196773651, -2.574251347313719407 ) ) ;
#8296 = CARTESIAN_POINT ( 'NONE',  ( -5.000000000000000000, -68.08333333333332860, -2.886751345948128211 ) ) ;
#8297 =( BOUNDED_CURVE ( )  B_SPLINE_CURVE ( 2, ( #21604, #27682, #27056, #17089, #42159, #36710, #18027, #11931, #32186 ),
 .UNSPECIFIED., .F., .F. ) 
 B_SPLINE_CURVE_WITH_KNOTS ( ( 3, 2, 2, 2, 3 ),
 ( 0.8339285714285714635, 0.8345238095238095566, 0.8357142857142857428, 0.8369047619047619291, 0.8375000000000000222 ),
 .UNSPECIFIED. ) 
 CURVE ( )  GEOMETRIC_REPRESENTATION_ITEM ( )  RATIONAL_B_SPLINE_CURVE ( ( 0.9330127018922194093, 0.9330127018922194093, 1.000000000000000000, 0.8660254037844387076, 1.000000000000000000, 0.8660254037844387076, 1.000000000000000000, 0.9330127018922194093, 0.9330127018922194093 ) ) 
 REPRESENTATION_ITEM ( '' )  );
#8298 = CARTESIAN_POINT ( 'NONE',  ( -2.499999999999996447, 18.29166666939785202, 4.330127018922195425 ) ) ;
#8299 = EDGE_LOOP ( 'NONE', ( #44587, #31261, #60241, #38502 ) ) ;
#8300 = CARTESIAN_POINT ( 'NONE',  ( 0.000000000000000000, -120.0000000000000000, 0.000000000000000000 ) ) ;
#8301 =( BOUNDED_CURVE ( )  B_SPLINE_CURVE ( 2, ( #19496, #38790, #57807, #54229, #39111, #43311, #23399, #18860, #4701 ),
 .UNSPECIFIED., .F., .F. ) 
 B_SPLINE_CURVE_WITH_KNOTS ( ( 3, 2, 2, 2, 3 ),
 ( 0.6839285714285714413, 0.6845238095238095344, 0.6857142857142857206, 0.6869047619047619069, 0.6875000000000000000 ),
 .UNSPECIFIED. ) 
 CURVE ( )  GEOMETRIC_REPRESENTATION_ITEM ( )  RATIONAL_B_SPLINE_CURVE ( ( 0.9330127018922194093, 0.9330127018922194093, 1.000000000000000000, 0.8660254037844387076, 1.000000000000000000, 0.8660254037844387076, 1.000000000000000000, 0.9330127018922194093, 0.9330127018922194093 ) ) 
 REPRESENTATION_ITEM ( '' )  );
#8302 = FACE_OUTER_BOUND ( 'NONE', #42062, .T. ) ;
#8304 = CARTESIAN_POINT ( 'NONE',  ( -2.499999999999996447, -30.83333333333333215, 4.330127018922195425 ) ) ;
#8303 = DIRECTION ( 'NONE',  ( -0.000000000000000000, 1.000000000000000000, -0.000000000000000000 ) ) ;
#8305 = CARTESIAN_POINT ( 'NONE',  ( -4.458734124999999437, -35.31249999863440792, 0.000000000000000000 ) ) ;
#8306 = EDGE_CURVE ( 'NONE', #35972, #37904, #3245, .T. ) ;
#8307 = CARTESIAN_POINT ( 'NONE',  ( 5.000000000000000000, -30.29166666393548013, -2.886751345948129988 ) ) ;
#8309 = ORIENTED_EDGE ( 'NONE', *, *, #27600, .T. ) ;
#8308 = CARTESIAN_POINT ( 'NONE',  ( 4.458734124999998549, -58.72916666530106511, -2.574251347313721627 ) ) ;
#8310 = CARTESIAN_POINT ( 'NONE',  ( 1.339745962155615144, -62.58034179853028434, 4.999999999999999112 ) ) ;
#8311 = ADVANCED_FACE ( 'NONE', ( #34058 ), #44333, .F. ) ;
#8313 = VERTEX_POINT ( 'NONE', #9924 ) ;
#8312 = CARTESIAN_POINT ( 'NONE',  ( -2.229367062500000163, -6.729166665301073103, -3.861377020970580443 ) ) ;
#8314 = CARTESIAN_POINT ( 'NONE',  ( -5.000000000000000000, -78.00000000000000000, 0.000000000000000000 ) ) ;
#8315 = CARTESIAN_POINT ( 'NONE',  ( -56.48576386720575471, -139.7500000013656347, -4.591703134518078322 ) ) ;
#8316 = VECTOR ( 'NONE', #18699, 1000.000000000000000 ) ;
#8317 = CARTESIAN_POINT ( 'NONE',  ( 4.458734125000001214, -53.14583333196773651, 2.574251347313718519 ) ) ;
#8318 = CARTESIAN_POINT ( 'NONE',  ( -2.499999999999996447, -76.70833333060214443, 4.330127018922195425 ) ) ;
#8319 = ORIENTED_EDGE ( 'NONE', *, *, #60942, .F. ) ;
#8320 = VECTOR ( 'NONE', #20232, 1000.000000000000000 ) ;
#8321 = CARTESIAN_POINT ( 'NONE',  ( -54.60164318462004474, -150.3750000000000284, -4.984105922594373794 ) ) ;
#8322 = CARTESIAN_POINT ( 'NONE',  ( -2.229367062499996610, -22.39583333196773651, 3.861377020970582219 ) ) ;
#8324 = EDGE_LOOP ( 'NONE', ( #18507, #1669, #56165, #24416 ) ) ;
#8323 = CARTESIAN_POINT ( 'NONE',  ( -4.458734124999999437, -58.64583333196774362, -2.574251347313719407 ) ) ;
#8325 = DIRECTION ( 'NONE',  ( 0.000000000000000000, -1.000000000000000000, 0.000000000000000000 ) ) ;
#8326 = CARTESIAN_POINT ( 'NONE',  ( -3.152801135295367096, -169.3125000013656063, -3.152801135295367541 ) ) ;
#8327 = CARTESIAN_POINT ( 'NONE',  ( -4.458734124999999437, -98.56249999863440792, 0.000000000000000000 ) ) ;
#8328 = CARTESIAN_POINT ( 'NONE',  ( -1.339745962155610925, -68.66965819600733312, 5.000000000000000000 ) ) ;
#8329 =( BOUNDED_CURVE ( )  B_SPLINE_CURVE ( 2, ( #12623, #32237, #27412, #47043, #2993, #22610, #28355, #13881, #23224 ),
 .UNSPECIFIED., .F., .F. ) 
 B_SPLINE_CURVE_WITH_KNOTS ( ( 3, 2, 2, 2, 3 ),
 ( 0.4732142857142856984, 0.4738095238095237915, 0.4749999999999999778, 0.4761904761904761640, 0.4767857142857143127 ),
 .UNSPECIFIED. ) 
 CURVE ( )  GEOMETRIC_REPRESENTATION_ITEM ( )  RATIONAL_B_SPLINE_CURVE ( ( 0.9330127018922194093, 0.9330127018922194093, 1.000000000000000000, 0.8660254037844387076, 1.000000000000000000, 0.8660254037844387076, 1.000000000000000000, 0.9330127018922163007, 0.9330127018922194093 ) ) 
 REPRESENTATION_ITEM ( '' )  );
#8330 = ORIENTED_EDGE ( 'NONE', *, *, #25196, .T. ) ;
#8331 = CARTESIAN_POINT ( 'NONE',  ( -59.29741812935640155, -149.8750000013655779, -2.196230717870135685 ) ) ;
#8332 = CARTESIAN_POINT ( 'NONE',  ( -50.01589407740564042, -140.7500000027312126, 0.3983568153799778022 ) ) ;
#8333 = CARTESIAN_POINT ( 'NONE',  ( -5.000000000000000000, 1.041666669397853351, -2.886751345948128211 ) ) ;
#8334 = CARTESIAN_POINT ( 'NONE',  ( 2.229367062499998831, -9.645833331967738289, -3.861377020970580887 ) ) ;
#8335 = CARTESIAN_POINT ( 'NONE',  ( 4.458734125000000326, -95.14583333196772230, 2.574251347313718519 ) ) ;
#8336 = CARTESIAN_POINT ( 'NONE',  ( -4.458734125000000326, -147.2500000013656063, -1.846868145590735644 ) ) ;
#8337 = CARTESIAN_POINT ( 'NONE',  ( 2.229367062500001939, -27.22916666530106866, 3.861377020970579999 ) ) ;
#8338 = CARTESIAN_POINT ( 'NONE',  ( 0.000000000000000000, -170.0000000000000000, 5.000000000000000000 ) ) ;
#8339 = CARTESIAN_POINT ( 'NONE',  ( -52.80376928212989185, -138.8750000013655779, -4.297418129356379346 ) ) ;
#8340 = CARTESIAN_POINT ( 'NONE',  ( 9.457646018065525792E-16, -69.31249999863440792, 5.148502694627439702 ) ) ;
#8341 = CARTESIAN_POINT ( 'NONE',  ( 1.975475456537005874E-15, -21.62499999726880873, 5.000000000000000000 ) ) ;
#8342 = DIRECTION ( 'NONE',  ( 0.000000000000000000, 0.000000000000000000, 1.000000000000000000 ) ) ;
#8343 = CARTESIAN_POINT ( 'NONE',  ( -3.152801135295367096, -142.0625000013655779, -3.152801135295367541 ) ) ;
#8344 =( BOUNDED_CURVE ( )  B_SPLINE_CURVE ( 2, ( #26235, #59060, #31058, #50680, #35254, #54874, #6622, #49722, #20140 ),
 .UNSPECIFIED., .F., .F. ) 
 B_SPLINE_CURVE_WITH_KNOTS ( ( 3, 2, 2, 2, 3 ),
 ( 0.05178571428571428908, 0.05238095238095238221, 0.05357142857142856845, 0.05476190476190476164, 0.05535714285714286170 ),
 .UNSPECIFIED. ) 
 CURVE ( )  GEOMETRIC_REPRESENTATION_ITEM ( )  RATIONAL_B_SPLINE_CURVE ( ( 0.9330127018922194093, 0.9330127018922197424, 1.000000000000000000, 0.8660254037844387076, 1.000000000000000000, 0.8660254037844387076, 1.000000000000000000, 0.9330127018922189652, 0.9330127018922194093 ) ) 
 REPRESENTATION_ITEM ( '' )  );
#8345 = CARTESIAN_POINT ( 'NONE',  ( -4.458734124999999437, 12.35416666803226171, -2.574251347313719407 ) ) ;
#8346 = ORIENTED_EDGE ( 'NONE', *, *, #18460, .T. ) ;
#8347 = CARTESIAN_POINT ( 'NONE',  ( -2.499999999999996447, -49.70833333060213732, 4.330127018922195425 ) ) ;
#8348 = CYLINDRICAL_SURFACE ( 'NONE', #53566, 5.000000000000000000 ) ;
#8350 = CARTESIAN_POINT ( 'NONE',  ( -2.229367062500000163, -24.47916666530106866, -3.861377020970580443 ) ) ;
#8349 = CARTESIAN_POINT ( 'NONE',  ( 5.000000000000000888, -90.58333333333334281, 2.886751345948126879 ) ) ;
#8351 = CARTESIAN_POINT ( 'NONE',  ( -4.458734124999998549, -78.47916666530107932, 2.574251347313722516 ) ) ;
#8352 = CARTESIAN_POINT ( 'NONE',  ( 2.229367062499998831, 28.10416666803225993, -3.861377020970580887 ) ) ;
#8353 = DIRECTION ( 'NONE',  ( 0.000000000000000000, 0.000000000000000000, 1.000000000000000000 ) ) ;
#8354 = CARTESIAN_POINT ( 'NONE',  ( -55.35523342533222291, -144.3125000013656063, 4.444560631937231499 ) ) ;
#8355 = CARTESIAN_POINT ( 'NONE',  ( -3.152548672688508926E-16, 2.437500001365593860, -5.148502694627439702 ) ) ;
#8356 = CARTESIAN_POINT ( 'NONE',  ( -51.75738570946856498, -135.8750000027312410, 3.805975901505576964 ) ) ;
#8357 = FACE_OUTER_BOUND ( 'NONE', #53938, .T. ) ;
#8358 = CARTESIAN_POINT ( 'NONE',  ( -4.458734124999997661, 7.770833334698926009, 2.574251347313722516 ) ) ;
#8359 = CARTESIAN_POINT ( 'NONE',  ( -4.458734124999999437, -70.31249999863439371, 0.000000000000000000 ) ) ;
#8360 = CARTESIAN_POINT ( 'NONE',  ( 2.229367062500001939, -19.22916666530106866, 3.861377020970579999 ) ) ;
#8361 = CARTESIAN_POINT ( 'NONE',  ( 5.000000000000000888, -4.583333333333334814, 2.886751345948126879 ) ) ;
#8362 = CARTESIAN_POINT ( 'NONE',  ( 1.846868145590735200, -160.2500000013656063, -4.458734125000000326 ) ) ;
#8363 = DIRECTION ( 'NONE',  ( -0.000000000000000000, 1.000000000000000000, -0.000000000000000000 ) ) ;
#8364 = AXIS2_PLACEMENT_3D ( 'NONE', #23248, #7516, #52526 ) ;
#8365 = CARTESIAN_POINT ( 'NONE',  ( -4.458734124999998549, -64.22916666530107932, 2.574251347313722516 ) ) ;
#8366 = CARTESIAN_POINT ( 'NONE',  ( 2.500000000000002220, -99.54166666393545881, 4.330127018922192761 ) ) ;
#8367 = CARTESIAN_POINT ( 'NONE',  ( -2.229367062500000163, 29.52083333469892779, -3.861377020970580443 ) ) ;
#8368 = CARTESIAN_POINT ( 'NONE',  ( 4.458734125000000326, -41.89583333196772941, 2.574251347313718519 ) ) ;
#8369 = EDGE_CURVE ( 'NONE', #2611, #56591, #2862, .T. ) ;
#8370 = CARTESIAN_POINT ( 'NONE',  ( 5.000000000000000888, 9.541666669397852019, 2.886751345948126879 ) ) ;
#8371 = CARTESIAN_POINT ( 'NONE',  ( -4.458734124999999437, -108.6458333319677365, -2.574251347313719407 ) ) ;
#8372 = CARTESIAN_POINT ( 'NONE',  ( -4.458734124999999437, -66.56249999863440792, 0.000000000000000000 ) ) ;
#8373 = CARTESIAN_POINT ( 'NONE',  ( -2.500000000000000444, -54.16666666666667140, -4.330127018922193649 ) ) ;
#8374 = CARTESIAN_POINT ( 'NONE',  ( 1.339745962155612702, -72.16965819600733312, -5.000000000000000000 ) ) ;
#8375 = CARTESIAN_POINT ( 'NONE',  ( 5.000000000000000000, -89.50000000000000000, -6.123233995736766282E-16 ) ) ;
#8376 = ORIENTED_EDGE ( 'NONE', *, *, #7957, .F. ) ;
#8377 = CARTESIAN_POINT ( 'NONE',  ( -1.339745962155610925, -84.79465819873851729, 5.000000000000000000 ) ) ;
#8378 = CARTESIAN_POINT ( 'NONE',  ( 5.000000000000000888, -6.458333330602150646, 2.886751345948126879 ) ) ;
#8379 = CARTESIAN_POINT ( 'NONE',  ( 5.000000000000000888, -12.58333333333333570, 2.886751345948126879 ) ) ;
#8380 = CARTESIAN_POINT ( 'NONE',  ( 4.458734124999999437, -16.81249999863440436, -5.460374474430324690E-16 ) ) ;
#8381 = ADVANCED_FACE ( 'NONE', ( #18644 ), #29220, .T. ) ;
#8382 = CARTESIAN_POINT ( 'NONE',  ( 4.458734124999998549, -79.72916666530106511, -2.574251347313721627 ) ) ;
#8383 = CARTESIAN_POINT ( 'NONE',  ( -1.339745962155610925, -5.794658198738521726, 5.000000000000000000 ) ) ;
#8384 = CARTESIAN_POINT ( 'NONE',  ( -4.999999999999999112, -10.79166666393547658, 2.886751345948131764 ) ) ;
#8386 = EDGE_LOOP ( 'NONE', ( #30287, #34861, #16786, #58999 ) ) ;
#8385 = CARTESIAN_POINT ( 'NONE',  ( 9.457646018065525792E-16, -46.06249999863440081, 5.148502694627439702 ) ) ;
#8388 = ORIENTED_EDGE ( 'NONE', *, *, #2963, .T. ) ;
#8387 = CARTESIAN_POINT ( 'NONE',  ( -2.229367062500000163, 5.270833334698927786, -3.861377020970580443 ) ) ;
#8389 = CARTESIAN_POINT ( 'NONE',  ( -51.75738570946856498, -140.8750000027312126, 3.805975901505576964 ) ) ;
#8390 = CARTESIAN_POINT ( 'NONE',  ( -2.499999999999996447, -61.83333333333333570, 4.330127018922195425 ) ) ;
#8391 = EDGE_CURVE ( 'NONE', #46887, #26939, #38877, .T. ) ;
#8392 = CARTESIAN_POINT ( 'NONE',  ( -3.152801135295367096, -161.3125000013656063, -3.152801135295367541 ) ) ;
#8393 = CARTESIAN_POINT ( 'NONE',  ( -4.458734124999998549, -37.47916666530107221, 2.574251347313722516 ) ) ;
#8394 = CARTESIAN_POINT ( 'NONE',  ( 5.000000000000000000, -14.49999999999999822, -6.123233995736766282E-16 ) ) ;
#8395 = CARTESIAN_POINT ( 'NONE',  ( 9.457646018065525792E-16, -81.06249999863440792, 5.148502694627439702 ) ) ;
#8396 = CARTESIAN_POINT ( 'NONE',  ( -5.000000000000000000, -164.5000000000000000, -6.123233995736766282E-16 ) ) ;
#8397 = ADVANCED_FACE ( 'NONE', ( #44015 ), #49172, .T. ) ;
#8398 = CARTESIAN_POINT ( 'NONE',  ( 5.000000000000000888, 0.000000000000000000, -10.00000000000000000 ) ) ;
#8399 = CARTESIAN_POINT ( 'NONE',  ( -52.80376928212989185, -130.1250000013656347, -4.297418129356379346 ) ) ;
#8400 = CARTESIAN_POINT ( 'NONE',  ( -4.458734124999999437, -3.645833331967739621, -2.574251347313719407 ) ) ;
#8401 = CARTESIAN_POINT ( 'NONE',  ( -2.229367062499996610, -39.39583333196773651, 3.861377020970582219 ) ) ;
#8402 = EDGE_CURVE ( 'NONE', #15905, #1425, #48850, .T. ) ;
#8403 = CARTESIAN_POINT ( 'NONE',  ( -2.500000000000000444, -25.04166666393547658, -4.330127018922193649 ) ) ;
#8404 = CARTESIAN_POINT ( 'NONE',  ( -4.458734124999999437, -82.56249999863440792, 0.000000000000000000 ) ) ;
#8405 = ORIENTED_EDGE ( 'NONE', *, *, #34651, .F. ) ;
#8406 = CARTESIAN_POINT ( 'NONE',  ( -57.46284108482265651, -153.0625000027312126, 4.819101127000239515 ) ) ;
#8407 = CARTESIAN_POINT ( 'NONE',  ( 5.000000000000000000, -43.50000000000000000, -6.123233995736766282E-16 ) ) ;
#8408 = CARTESIAN_POINT ( 'NONE',  ( 9.457646018065525792E-16, -69.31249999863440792, 5.148502694627439702 ) ) ;
#8409 = CARTESIAN_POINT ( 'NONE',  ( -4.458734124999999437, -148.2500000013656347, -1.846868145590735644 ) ) ;
#8410 = EDGE_LOOP ( 'NONE', ( #34007, #59252, #7370, #43942 ) ) ;
#8411 = CYLINDRICAL_SURFACE ( 'NONE', #43103, 5.000000000000000000 ) ;
#8412 = DIRECTION ( 'NONE',  ( -0.000000000000000000, 1.000000000000000000, -0.000000000000000000 ) ) ;
#8413 = CARTESIAN_POINT ( 'NONE',  ( -4.458734124999999437, -14.64583333196773474, -2.574251347313719407 ) ) ;
#8414 = CARTESIAN_POINT ( 'NONE',  ( -56.66612745406273888, -150.4375000027311842, -5.149110718188520508 ) ) ;
#8415 = CARTESIAN_POINT ( 'NONE',  ( 9.457646018065525792E-16, -0.06249999863440491854, 5.148502694627439702 ) ) ;
#8416 = CARTESIAN_POINT ( 'NONE',  ( -3.152801135295367096, -155.0625000013656063, -3.152801135295367541 ) ) ;
#8417 = CARTESIAN_POINT ( 'NONE',  ( 2.229367062500001939, 25.77083333469892779, 3.861377020970579999 ) ) ;
#8418 = ORIENTED_EDGE ( 'NONE', *, *, #39340, .F. ) ;
#8419 = CARTESIAN_POINT ( 'NONE',  ( -2.229367062500000163, -94.47916666530106511, -3.861377020970580443 ) ) ;
#8420 = CARTESIAN_POINT ( 'NONE',  ( 1.975475456537005874E-15, -30.74999999999999645, 5.000000000000000000 ) ) ;
#8421 = CARTESIAN_POINT ( 'NONE',  ( -6.972266317189433020E-16, -85.12499999726880162, -5.000000000000000000 ) ) ;
#8422 = CARTESIAN_POINT ( 'NONE',  ( 2.229367062500001939, -8.979166665301075767, 3.861377020970579999 ) ) ;
#8423 = DIRECTION ( 'NONE',  ( -0.000000000000000000, 1.000000000000000000, -0.000000000000000000 ) ) ;
#8424 = LINE ( 'NONE', #45831, #45826 ) ;
#8425 =( BOUNDED_CURVE ( )  B_SPLINE_CURVE ( 2, ( #6094, #60450, #15734, #11848, #31467, #1917, #11221, #35351, #20884 ),
 .UNSPECIFIED., .F., .F. ) 
 B_SPLINE_CURVE_WITH_KNOTS ( ( 3, 2, 2, 2, 3 ),
 ( 0.6303571428571428381, 0.6309523809523809312, 0.6321428571428571175, 0.6333333333333333037, 0.6339285714285713969 ),
 .UNSPECIFIED. ) 
 CURVE ( )  GEOMETRIC_REPRESENTATION_ITEM ( )  RATIONAL_B_SPLINE_CURVE ( ( 0.9330127018922194093, 0.9330127018922194093, 1.000000000000000000, 0.8660254037844387076, 1.000000000000000000, 0.8660254037844387076, 1.000000000000000000, 0.9330127018922194093, 0.9330127018922194093 ) ) 
 REPRESENTATION_ITEM ( '' )  );
#8426 = CARTESIAN_POINT ( 'NONE',  ( -5.000000000000000000, 14.91666666666666607, -2.886751345948128211 ) ) ;
#8427 = CARTESIAN_POINT ( 'NONE',  ( 2.499999999999998668, -35.20833333060213732, -4.330127018922193649 ) ) ;
#8428 = CARTESIAN_POINT ( 'NONE',  ( -6.972266317189433020E-16, -49.12499999726880162, -5.000000000000000000 ) ) ;
#8429 = CARTESIAN_POINT ( 'NONE',  ( -2.229367062500000163, 16.52083333469892779, -3.861377020970580443 ) ) ;
#8430 = CARTESIAN_POINT ( 'NONE',  ( 5.000000000000000000, -10.50000000000000178, -6.123233995736766282E-16 ) ) ;
#8431 = CARTESIAN_POINT ( 'NONE',  ( -4.458734124999999437, 20.60416666803225993, -2.574251347313719407 ) ) ;
#8432 = CARTESIAN_POINT ( 'NONE',  ( -3.152548672688508926E-16, -55.56249999863440081, -5.148502694627439702 ) ) ;
#8433 = CARTESIAN_POINT ( 'NONE',  ( 2.229367062500001939, -1.229166665301071548, 3.861377020970579999 ) ) ;
#8434 = CARTESIAN_POINT ( 'NONE',  ( -5.000000000000000000, -63.08333333333331439, -2.886751345948128211 ) ) ;
#8435 = CARTESIAN_POINT ( 'NONE',  ( -2.499999999999996447, 11.16666666666666430, 4.330127018922195425 ) ) ;
#8436 = CARTESIAN_POINT ( 'NONE',  ( 3.061616997868383141E-16, -142.8750000027312126, -5.000000000000000000 ) ) ;
#8437 = CARTESIAN_POINT ( 'NONE',  ( -58.80597590150559739, -145.1250000027312126, 3.242614290531460330 ) ) ;
#8438 = CARTESIAN_POINT ( 'NONE',  ( 4.458734124999998549, -47.72916666530106511, -2.574251347313721627 ) ) ;
#8439 = CARTESIAN_POINT ( 'NONE',  ( 2.499999999999998668, -84.20833333060214443, -4.330127018922193649 ) ) ;
#8440 = CARTESIAN_POINT ( 'NONE',  ( -55.35523342533222291, -134.5625000013656063, 4.444560631937231499 ) ) ;
#8441 = DIRECTION ( 'NONE',  ( 0.000000000000000000, 0.000000000000000000, 1.000000000000000000 ) ) ;
#8442 = ADVANCED_FACE ( 'NONE', ( #40789 ), #5750, .T. ) ;
#8443 =( BOUNDED_CURVE ( )  B_SPLINE_CURVE ( 2, ( #44417, #39910, #45386, #5833, #54727, #35110, #60199, #6159, #16440 ),
 .UNSPECIFIED., .F., .F. ) 
 B_SPLINE_CURVE_WITH_KNOTS ( ( 3, 2, 2, 2, 3 ),
 ( 0.3145833333333333259, 0.3152777777777777679, 0.3166666666666666519, 0.3180555555555555358, 0.3187499999999999778 ),
 .UNSPECIFIED. ) 
 CURVE ( )  GEOMETRIC_REPRESENTATION_ITEM ( )  RATIONAL_B_SPLINE_CURVE ( ( 0.9330127018922194093, 0.9330127018922194093, 1.000000000000000000, 0.8660254037844387076, 1.000000000000000000, 0.8660254037844387076, 1.000000000000000000, 0.9330127018922194093, 0.9330127018922194093 ) ) 
 REPRESENTATION_ITEM ( '' )  );
#8444 = CARTESIAN_POINT ( 'NONE',  ( 2.229367062499998831, -90.89583333196773651, -3.861377020970580887 ) ) ;
#8445 = CARTESIAN_POINT ( 'NONE',  ( 2.730187237215162345E-16, -156.4375000013655779, -4.458734124999999437 ) ) ;
#8446 = CARTESIAN_POINT ( 'NONE',  ( 1.060575238724906964E-15, -34.75000000000000711, 5.773502691896257311 ) ) ;
#8447 = DIRECTION ( 'NONE',  ( -0.000000000000000000, 1.000000000000000000, -0.000000000000000000 ) ) ;
#8448 = ORIENTED_EDGE ( 'NONE', *, *, #12788, .F. ) ;
#8449 = CARTESIAN_POINT ( 'NONE',  ( -4.458734124999998549, 16.52083333469892779, 2.574251347313722516 ) ) ;
#8450 = VERTEX_POINT ( 'NONE', #60436 ) ;
#8451 = CARTESIAN_POINT ( 'NONE',  ( 4.458734124999999437, -94.81249999863440792, -5.460374474430324690E-16 ) ) ;
#8452 = CARTESIAN_POINT ( 'NONE',  ( -2.229367062500000163, 8.270833334698926009, -3.861377020970580443 ) ) ;
#8453 = CARTESIAN_POINT ( 'NONE',  ( -5.000000000000000000, 10.04166666939785202, -2.886751345948128211 ) ) ;
#8454 = CARTESIAN_POINT ( 'NONE',  ( -1.339745962155610925, -28.66965819600733312, 5.000000000000000000 ) ) ;
#8455 = CARTESIAN_POINT ( 'NONE',  ( 5.000000000000000000, 4.500000000000000888, -6.123233995736766282E-16 ) ) ;
#8456 = CARTESIAN_POINT ( 'NONE',  ( -4.458734124999997661, -61.22916666530106511, 2.574251347313722516 ) ) ;
#8457 = CARTESIAN_POINT ( 'NONE',  ( 1.339745962155615144, -61.58034179853027723, 4.999999999999999112 ) ) ;
#8458 = CARTESIAN_POINT ( 'NONE',  ( 9.457646018065525792E-16, -28.06249999863440081, 5.148502694627439702 ) ) ;
#8459 = CARTESIAN_POINT ( 'NONE',  ( 5.000000000000000000, 7.708333336064518093, -2.886751345948130876 ) ) ;
#8460 = CARTESIAN_POINT ( 'NONE',  ( -4.999999999999998224, -25.79166666393547658, 2.886751345948131764 ) ) ;
#8461 = CARTESIAN_POINT ( 'NONE',  ( -3.535250795749689387E-16, -46.25000000000000000, -5.773502691896257311 ) ) ;
#8462 = CARTESIAN_POINT ( 'NONE',  ( -2.499999999999996447, -75.70833333060214443, 4.330127018922195425 ) ) ;
#8464 = CARTESIAN_POINT ( 'NONE',  ( -4.458734124999999437, -17.64583333196773651, -2.574251347313719407 ) ) ;
#8463 = CARTESIAN_POINT ( 'NONE',  ( 1.339745962155661996, -26.16965819600733667, -4.999999999999970690 ) ) ;
#8465 = DIRECTION ( 'NONE',  ( 0.000000000000000000, 0.000000000000000000, 1.000000000000000000 ) ) ;
#8466 = CARTESIAN_POINT ( 'NONE',  ( -4.458734124999999437, -63.31249999863440792, 0.000000000000000000 ) ) ;
#8467 = CARTESIAN_POINT ( 'NONE',  ( -3.152801135295367985, -147.0625000013655779, 3.152801135295367096 ) ) ;
#8468 = CARTESIAN_POINT ( 'NONE',  ( -4.458734124999998549, -74.22916666530106511, 2.574251347313722516 ) ) ;
#8469 = CARTESIAN_POINT ( 'NONE',  ( -58.39396692619412477, -141.6875000013656063, 2.891590998281057701 ) ) ;
#8470 = CARTESIAN_POINT ( 'NONE',  ( -3.152548672688508926E-16, -23.81249999863440792, -5.148502694627439702 ) ) ;
#8471 = CARTESIAN_POINT ( 'NONE',  ( 5.000000000000000888, -67.45833333060213022, 2.886751345948126879 ) ) ;
#8472 = ORIENTED_EDGE ( 'NONE', *, *, #10072, .F. ) ;
#8473 = CARTESIAN_POINT ( 'NONE',  ( -51.75738570946856498, -147.8750000027312126, 3.805975901505576964 ) ) ;
#8474 = ORIENTED_EDGE ( 'NONE', *, *, #24306, .F. ) ;
#8475 = CARTESIAN_POINT ( 'NONE',  ( 4.458734125000001214, -70.14583333196773651, 2.574251347313718519 ) ) ;
#8476 = CARTESIAN_POINT ( 'NONE',  ( 1.975475456537005874E-15, -21.62499999726880873, 5.000000000000000000 ) ) ;
#8477 = ORIENTED_EDGE ( 'NONE', *, *, #59318, .F. ) ;
#8478 = CARTESIAN_POINT ( 'NONE',  ( 0.000000000000000000, -170.0000000000000000, 0.000000000000000000 ) ) ;
#8479 = CARTESIAN_POINT ( 'NONE',  ( 4.458734124999999437, -53.06249999863440792, -5.460374474430324690E-16 ) ) ;
#8480 = CARTESIAN_POINT ( 'NONE',  ( -4.458734124999998549, 0.5208333346989265644, 2.574251347313722516 ) ) ;
#8481 = ORIENTED_EDGE ( 'NONE', *, *, #62538, .F. ) ;
#8482 = CARTESIAN_POINT ( 'NONE',  ( -1.339745962155497683, -55.20534180126147561, -5.000000000000066613 ) ) ;
#8483 = CARTESIAN_POINT ( 'NONE',  ( 4.458734124999998549, 2.270833334698928230, -2.574251347313721627 ) ) ;
#8484 = CARTESIAN_POINT ( 'NONE',  ( -4.458734124999999437, 18.68750000136559564, 0.000000000000000000 ) ) ;
#8485 = CARTESIAN_POINT ( 'NONE',  ( -51.60603307380591787, -143.9375000013656063, -2.891590998281053704 ) ) ;
#8486 = CARTESIAN_POINT ( 'NONE',  ( 1.975475456537005874E-15, 16.24999999999999645, 5.000000000000000000 ) ) ;
#8487 = CARTESIAN_POINT ( 'NONE',  ( -9.184850993605147944E-16, -148.2500000000000284, 5.000000000000000000 ) ) ;
#8488 =( BOUNDED_CURVE ( )  B_SPLINE_CURVE ( 2, ( #39360, #48389, #14291, #49975, #15577, #45152, #11371, #1117, #16525 ),
 .UNSPECIFIED., .F., .F. ) 
 B_SPLINE_CURVE_WITH_KNOTS ( ( 3, 2, 2, 2, 3 ),
 ( 0.6089285714285714857, 0.6095238095238095788, 0.6107142857142857650, 0.6119047619047619513, 0.6125000000000000444 ),
 .UNSPECIFIED. ) 
 CURVE ( )  GEOMETRIC_REPRESENTATION_ITEM ( )  RATIONAL_B_SPLINE_CURVE ( ( 0.9330127018922194093, 0.9330127018922256266, 1.000000000000000000, 0.8660254037844387076, 1.000000000000000000, 0.8660254037844387076, 1.000000000000000000, 0.9330127018922194093, 0.9330127018922194093 ) ) 
 REPRESENTATION_ITEM ( '' )  );
#8489 = ORIENTED_EDGE ( 'NONE', *, *, #16582, .T. ) ;
#8490 = CARTESIAN_POINT ( 'NONE',  ( 2.229367062499998831, -77.64583333196773651, -3.861377020970580887 ) ) ;
#8491 = CARTESIAN_POINT ( 'NONE',  ( -2.500000000000000444, -40.16666666666667140, -4.330127018922193649 ) ) ;
#8492 = CARTESIAN_POINT ( 'NONE',  ( 4.458734124999998549, 7.270833334698928674, -2.574251347313721627 ) ) ;
#8493 = CARTESIAN_POINT ( 'NONE',  ( -1.339745962155610925, -88.79465819873851729, 5.000000000000000000 ) ) ;
#8494 = CARTESIAN_POINT ( 'NONE',  ( -2.229367062500000163, -62.72916666530106511, -3.861377020970580443 ) ) ;
#8495 = CARTESIAN_POINT ( 'NONE',  ( 1.060575238724906964E-15, -22.62499999726881228, 5.773502691896257311 ) ) ;
#8496 = FACE_OUTER_BOUND ( 'NONE', #9398, .T. ) ;
#8497 = CARTESIAN_POINT ( 'NONE',  ( 1.339745962155612702, -42.16965819600732601, -5.000000000000000000 ) ) ;
#8498 = CARTESIAN_POINT ( 'NONE',  ( 6.123233995736766282E-16, -170.0000000000000000, -5.000000000000000000 ) ) ;
#8499 = FACE_OUTER_BOUND ( 'NONE', #46368, .T. ) ;
#8500 = CARTESIAN_POINT ( 'NONE',  ( -5.000000000000000888, -159.4375000000000000, 2.071067811865474617 ) ) ;
#8501 = CARTESIAN_POINT ( 'NONE',  ( -4.458734124999999437, -39.39583333196773651, -2.574251347313719407 ) ) ;
#8502 = CARTESIAN_POINT ( 'NONE',  ( 4.458734125000000326, -28.14583333196774007, 2.574251347313718519 ) ) ;
#8503 = DIRECTION ( 'NONE',  ( 0.000000000000000000, 0.000000000000000000, 1.000000000000000000 ) ) ;
#8504 = CARTESIAN_POINT ( 'NONE',  ( 2.500000000000002220, 24.33333333333333215, 4.330127018922192761 ) ) ;
#8505 = CARTESIAN_POINT ( 'NONE',  ( 3.535533905932736864, -152.2500000027312126, 3.535533905932738641 ) ) ;
#8506 = ORIENTED_EDGE ( 'NONE', *, *, #13449, .T. ) ;
#8507 = CARTESIAN_POINT ( 'NONE',  ( 4.458734124999998549, -109.9791666653010793, -2.574251347313721627 ) ) ;
#8508 = CARTESIAN_POINT ( 'NONE',  ( 4.458734124999999437, -31.81249999863440436, -5.460374474430324690E-16 ) ) ;
#8509 = CARTESIAN_POINT ( 'NONE',  ( 2.499999999999998668, -70.20833333060214443, -4.330127018922193649 ) ) ;
#8510 = CARTESIAN_POINT ( 'NONE',  ( -57.19623071787017210, -148.6250000013656063, 4.297418129356382899 ) ) ;
#8511 = CARTESIAN_POINT ( 'NONE',  ( 5.000000000000000888, -147.9374999999999716, -2.071067811865475505 ) ) ;
#8512 = CARTESIAN_POINT ( 'NONE',  ( 4.458734124999998549, -27.72916666530107221, -2.574251347313721627 ) ) ;
#8513 = CARTESIAN_POINT ( 'NONE',  ( -4.458734124999999437, -75.56249999863440792, 0.000000000000000000 ) ) ;
#8514 = CARTESIAN_POINT ( 'NONE',  ( 1.255007937094098239E-14, 22.87500000273118772, -4.999999999999999112 ) ) ;
#8515 = CARTESIAN_POINT ( 'NONE',  ( -3.152548672688508926E-16, -28.56249999863440081, -5.148502694627439702 ) ) ;
#8516 = CARTESIAN_POINT ( 'NONE',  ( -58.80597590150559739, -136.1250000027312410, 3.242614290531460330 ) ) ;
#8517 = CARTESIAN_POINT ( 'NONE',  ( 1.975475456537005874E-15, 9.375000002731185944, 5.000000000000000000 ) ) ;
#8518 = CARTESIAN_POINT ( 'NONE',  ( 5.000000000000000000, -15.41666666666666963, -2.886751345948129988 ) ) ;
#8519 = CARTESIAN_POINT ( 'NONE',  ( -1.846868145590737420, -149.7500000013656063, 4.458734124999999437 ) ) ;
#8520 = ORIENTED_EDGE ( 'NONE', *, *, #63627, .T. ) ;
#8521 = CARTESIAN_POINT ( 'NONE',  ( 0.000000000000000000, -120.0000000000000000, 0.000000000000000000 ) ) ;
#8522 = CARTESIAN_POINT ( 'NONE',  ( -3.152548672688508926E-16, -58.81249999863440081, -5.148502694627439702 ) ) ;
#8523 =( BOUNDED_CURVE ( )  B_SPLINE_CURVE ( 2, ( #59796, #15717, #35336, #10885, #41420, #16673, #12159, #26640, #11831 ),
 .UNSPECIFIED., .F., .F. ) 
 B_SPLINE_CURVE_WITH_KNOTS ( ( 3, 2, 2, 2, 3 ),
 ( 0.7749999999999998002, 0.7791666666666664520, 0.7833333333333331039, 0.7874999999999997558, 0.7916666666666664076 ),
 .UNSPECIFIED. ) 
 CURVE ( )  GEOMETRIC_REPRESENTATION_ITEM ( )  RATIONAL_B_SPLINE_CURVE ( ( 1.000000000000003997, 0.9238795325112826307, 1.000000000000000000, 0.9238795325112867385, 1.000000000000000000, 0.9238795325112867385, 1.000000000000000000, 0.9238795325112908463, 0.9999999999999958922 ) ) 
 REPRESENTATION_ITEM ( '' )  );
#8524 = CARTESIAN_POINT ( 'NONE',  ( -2.499999999999996447, 25.29166666939785202, 4.330127018922195425 ) ) ;
#8525 = LINE ( 'NONE', #17856, #20668 ) ;
#8526 = CARTESIAN_POINT ( 'NONE',  ( -4.999999999999999112, 20.08333333333333215, 2.886751345948131764 ) ) ;
#8527 = LINE ( 'NONE', #14595, #49941 ) ;
#8528 = CARTESIAN_POINT ( 'NONE',  ( 2.229367062499998831, 1.354166668032261933, -3.861377020970580887 ) ) ;
#8529 = CARTESIAN_POINT ( 'NONE',  ( 1.975475456537005874E-15, -10.75000000000000000, 5.000000000000000000 ) ) ;
#8530 = CYLINDRICAL_SURFACE ( 'NONE', #11199, 5.000000000000000000 ) ;
#8531 = CARTESIAN_POINT ( 'NONE',  ( -2.229367062500000163, 9.270833334698927786, -3.861377020970580443 ) ) ;
#8532 = ORIENTED_EDGE ( 'NONE', *, *, #1374, .F. ) ;
#8533 = CARTESIAN_POINT ( 'NONE',  ( 5.000000000000000000, -12.49999999999999645, -6.123233995736766282E-16 ) ) ;
#8534 = ORIENTED_EDGE ( 'NONE', *, *, #19984, .F. ) ;
#8535 = CARTESIAN_POINT ( 'NONE',  ( 5.000000000000000888, -7.458333330602142652, 2.886751345948126879 ) ) ;
#8536 = CARTESIAN_POINT ( 'NONE',  ( 2.229367062500001939, -48.97916666530107221, 3.861377020970579999 ) ) ;
#8537 = CARTESIAN_POINT ( 'NONE',  ( 4.458734124999999437, -160.6875000013655779, 0.000000000000000000 ) ) ;
#8538 = CARTESIAN_POINT ( 'NONE',  ( 1.060575238724906964E-15, -51.62499999726881583, 5.773502691896257311 ) ) ;
#8539 = VERTEX_POINT ( 'NONE', #30175 ) ;
#8540 = CARTESIAN_POINT ( 'NONE',  ( 4.458734124999999437, -20.81249999863440081, -5.460374474430324690E-16 ) ) ;
#8541 = VERTEX_POINT ( 'NONE', #15405 ) ;
#8543 = CARTESIAN_POINT ( 'NONE',  ( -4.999999999999998224, -102.7916666639354730, 2.886751345948131764 ) ) ;
#8542 = CARTESIAN_POINT ( 'NONE',  ( -6.972266317189433020E-16, -0.1249999972688142363, -5.000000000000000000 ) ) ;
#8544 = CARTESIAN_POINT ( 'NONE',  ( 3.152801135295366208, -161.5625000013656063, 3.152801135295367985 ) ) ;
#8545 = CARTESIAN_POINT ( 'NONE',  ( -6.972266317189433020E-16, -39.12499999726880162, -5.000000000000000000 ) ) ;
#8546 = CARTESIAN_POINT ( 'NONE',  ( -59.98410592259440222, -136.1250000000000284, -0.3983568153799752487 ) ) ;
#8547 = CARTESIAN_POINT ( 'NONE',  ( 2.229367062500001939, -36.22916666530107221, 3.861377020970579999 ) ) ;
#8548 = ORIENTED_EDGE ( 'NONE', *, *, #51420, .T. ) ;
#8549 = CARTESIAN_POINT ( 'NONE',  ( -3.152548672688508926E-16, -83.56249999863440792, -5.148502694627439702 ) ) ;
#8550 = CARTESIAN_POINT ( 'NONE',  ( 9.457646018065525792E-16, 22.93750000136559919, 5.148502694627439702 ) ) ;
#8551 = CARTESIAN_POINT ( 'NONE',  ( 2.499999999999998668, -12.20833333060214798, -4.330127018922193649 ) ) ;
#8552 = ORIENTED_EDGE ( 'NONE', *, *, #13887, .F. ) ;
#8553 = CARTESIAN_POINT ( 'NONE',  ( -57.19623071787016499, -139.6250000013655779, 4.297418129356382899 ) ) ;
#8554 = CARTESIAN_POINT ( 'NONE',  ( 4.458734125000001214, -86.14583333196775072, 2.574251347313718519 ) ) ;
#8555 = CARTESIAN_POINT ( 'NONE',  ( -59.98410592259440222, -128.2500000027312126, -0.3983568153799752487 ) ) ;
#8556 = CARTESIAN_POINT ( 'NONE',  ( 5.000000000000000000, -88.41666666666665719, -2.886751345948130876 ) ) ;
#8557 = CARTESIAN_POINT ( 'NONE',  ( -4.458734124999999437, -140.2500000013656063, -1.846868145590735644 ) ) ;
#8558 = CARTESIAN_POINT ( 'NONE',  ( 5.000000000000000888, -57.58333333333332860, 2.886751345948126879 ) ) ;
#8559 = CARTESIAN_POINT ( 'NONE',  ( -4.458734124999999437, -57.39583333196773651, -2.574251347313719407 ) ) ;
#8560 = CARTESIAN_POINT ( 'NONE',  ( -51.75738570946856498, -150.8750000027312126, 3.805975901505576964 ) ) ;
#8561 = CARTESIAN_POINT ( 'NONE',  ( -4.458734124999998549, 25.77083333469892779, 2.574251347313722516 ) ) ;
#8562 = ADVANCED_FACE ( 'NONE', ( #40156 ), #60114, .T. ) ;
#8563 = DIRECTION ( 'NONE',  ( -0.000000000000000000, 1.000000000000000000, -0.000000000000000000 ) ) ;
#8564 = DIRECTION ( 'NONE',  ( 0.000000000000000000, 1.000000000000000000, 0.000000000000000000 ) ) ;
#8565 = CARTESIAN_POINT ( 'NONE',  ( -4.458734124999999437, -44.64583333196773651, -2.574251347313719407 ) ) ;
#8566 = CARTESIAN_POINT ( 'NONE',  ( -4.999999999999999112, -2.791666663935477466, 2.886751345948131764 ) ) ;
#8567 = CARTESIAN_POINT ( 'NONE',  ( 5.000000000000000000, -31.50000000000000000, -6.123233995736766282E-16 ) ) ;
#8568 = CARTESIAN_POINT ( 'NONE',  ( -57.19623071787017210, -125.3750000013656205, 4.297418129356382899 ) ) ;
#8569 = CARTESIAN_POINT ( 'NONE',  ( 4.458734124999999437, -87.06249999863439371, -5.460374474430324690E-16 ) ) ;
#8570 = CARTESIAN_POINT ( 'NONE',  ( 9.457646018065525792E-16, -101.0624999986344079, 5.148502694627439702 ) ) ;
#8571 = CARTESIAN_POINT ( 'NONE',  ( 2.229367062500001939, -12.22916666530107044, 3.861377020970579999 ) ) ;
#8572 = ORIENTED_EDGE ( 'NONE', *, *, #60231, .F. ) ;
#8573 = CARTESIAN_POINT ( 'NONE',  ( -2.499999999999996447, -16.70833333060214443, 4.330127018922195425 ) ) ;
#8574 = CARTESIAN_POINT ( 'NONE',  ( -4.458734124999998549, -94.22916666530106511, 2.574251347313722516 ) ) ;
#8575 = CARTESIAN_POINT ( 'NONE',  ( 2.071067811865476394, -166.3125000027312410, 5.000000000000000000 ) ) ;
#8576 = CARTESIAN_POINT ( 'NONE',  ( 2.229367062499998831, -89.89583333196773651, -3.861377020970580887 ) ) ;
#8577 = CARTESIAN_POINT ( 'NONE',  ( -5.000000000000000000, -50.87499999726881583, 0.000000000000000000 ) ) ;
#8578 = CARTESIAN_POINT ( 'NONE',  ( -2.500000000000000444, -30.16666666666666785, -4.330127018922193649 ) ) ;
#8579 = CARTESIAN_POINT ( 'NONE',  ( -59.29741812935640155, -130.6250000013656347, -2.196230717870135685 ) ) ;
#8580 = EDGE_CURVE ( 'NONE', #46979, #24361, #55833, .T. ) ;
#8581 = CARTESIAN_POINT ( 'NONE',  ( 9.457646018065525792E-16, -15.06249999863440259, 5.148502694627439702 ) ) ;
#8582 = CARTESIAN_POINT ( 'NONE',  ( 2.229367062500001939, 12.77083333469892779, 3.861377020970579999 ) ) ;
#8583 = EDGE_CURVE ( 'NONE', #45091, #8062, #55457, .T. ) ;
#8584 = CARTESIAN_POINT ( 'NONE',  ( -2.229367062500000163, -54.72916666530107221, -3.861377020970580443 ) ) ;
#8585 = CARTESIAN_POINT ( 'NONE',  ( 1.975475456537005874E-15, -86.62499999726880162, 5.000000000000000000 ) ) ;
#8586 = CARTESIAN_POINT ( 'NONE',  ( -9.184850993605147944E-16, -152.2500000000000000, 5.000000000000000000 ) ) ;
#8587 = CARTESIAN_POINT ( 'NONE',  ( 2.229367062500001939, -13.97916666530107221, 3.861377020970579999 ) ) ;
#8588 = CYLINDRICAL_SURFACE ( 'NONE', #36041, 5.000000000000000000 ) ;
#8589 = VERTEX_POINT ( 'NONE', #6712 ) ;
#8590 = CARTESIAN_POINT ( 'NONE',  ( -4.458734124999999437, -39.64583333196773651, -2.574251347313719407 ) ) ;
#8591 = UNCERTAINTY_MEASURE_WITH_UNIT (LENGTH_MEASURE( 1.000000000000000082E-05 ), #9273, 'distance_accuracy_value', 'NONE');
#8592 = CYLINDRICAL_SURFACE ( 'NONE', #41772, 5.000000000000000000 ) ;
#8593 = CARTESIAN_POINT ( 'NONE',  ( -6.972266317189433020E-16, -28.25000000000000000, -5.000000000000000000 ) ) ;
#8594 = CARTESIAN_POINT ( 'NONE',  ( 2.229367062499998831, -84.64583333196773651, -3.861377020970580887 ) ) ;
#8595 = CARTESIAN_POINT ( 'NONE',  ( 4.458734125000001214, 24.85416666803225993, 2.574251347313718519 ) ) ;
#8596 = EDGE_CURVE ( 'NONE', #49029, #53577, #52992, .T. ) ;
#8597 = CARTESIAN_POINT ( 'NONE',  ( 2.229367062499998831, 16.35416666803225993, -3.861377020970580887 ) ) ;
#8598 = DIRECTION ( 'NONE',  ( 1.000000000000000000, 0.000000000000000000, -1.061635649774262664E-14 ) ) ;
#8599 = CARTESIAN_POINT ( 'NONE',  ( -2.499999999999996447, -64.70833333060213022, 4.330127018922195425 ) ) ;
#8600 = CARTESIAN_POINT ( 'NONE',  ( 4.458734125000000326, -84.14583333196773651, 2.574251347313718519 ) ) ;
#8601 = CARTESIAN_POINT ( 'NONE',  ( -2.500000000000000444, -69.16666666666667140, -4.330127018922193649 ) ) ;
#8602 = CARTESIAN_POINT ( 'NONE',  ( -2.499999999999996447, 13.29166666939785379, 4.330127018922195425 ) ) ;
#8603 = VERTEX_POINT ( 'NONE', #26321 ) ;
#8604 = CARTESIAN_POINT ( 'NONE',  ( 1.339745962155661996, -25.29465819873852794, -4.999999999999970690 ) ) ;
#8605 = CARTESIAN_POINT ( 'NONE',  ( -2.498395430326213474E-14, 16.24999999999999645, 5.000000000000000000 ) ) ;
#8607 = CARTESIAN_POINT ( 'NONE',  ( 2.499999999999998668, -30.33333333333332860, -4.330127018922193649 ) ) ;
#8606 = CARTESIAN_POINT ( 'NONE',  ( -6.972266317189433020E-16, -109.1249999972688016, -5.000000000000000000 ) ) ;
#8608 = CARTESIAN_POINT ( 'NONE',  ( -4.458734124999999437, -30.31249999863440436, 0.000000000000000000 ) ) ;
#8609 = DIRECTION ( 'NONE',  ( 0.000000000000000000, 0.000000000000000000, 1.000000000000000000 ) ) ;
#8610 =( BOUNDED_CURVE ( )  B_SPLINE_CURVE ( 2, ( #32960, #53826, #9445, #38406, #8516, #38708, #28126, #13654, #14275 ),
 .UNSPECIFIED., .F., .F. ) 
 B_SPLINE_CURVE_WITH_KNOTS ( ( 3, 2, 2, 2, 3 ),
 ( 0.5916666666666671182, 0.5958333333333335480, 0.6000000000000000888, 0.6041666666666665186, 0.6083333333333329485 ),
 .UNSPECIFIED. ) 
 CURVE ( )  GEOMETRIC_REPRESENTATION_ITEM ( )  RATIONAL_B_SPLINE_CURVE ( ( 0.9999999999999918954, 0.9238795325112948431, 1.000000000000000000, 0.9238795325112867385, 1.000000000000000000, 0.9238795325112867385, 1.000000000000000000, 0.9238795325112928447, 0.9999999999999938938 ) ) 
 REPRESENTATION_ITEM ( '' )  );
#8611 = CARTESIAN_POINT ( 'NONE',  ( -4.999999999999999112, -32.79166666393547303, 2.886751345948131764 ) ) ;
#8612 = EDGE_CURVE ( 'NONE', #51084, #29252, #62032, .T. ) ;
#8614 = ORIENTED_EDGE ( 'NONE', *, *, #449, .F. ) ;
#8613 = CARTESIAN_POINT ( 'NONE',  ( 9.457646018065525792E-16, -61.06249999863440081, 5.148502694627439702 ) ) ;
#8615 = CARTESIAN_POINT ( 'NONE',  ( -58.39396692619412477, -151.6875000013656063, 2.891590998281057701 ) ) ;
#8617 = VERTEX_POINT ( 'NONE', #20872 ) ;
#8616 = CARTESIAN_POINT ( 'NONE',  ( -4.458734124999999437, -7.562499998634404363, 0.000000000000000000 ) ) ;
#8618 = CARTESIAN_POINT ( 'NONE',  ( 5.000000000000000000, -75.41666666666667140, -2.886751345948129988 ) ) ;
#8619 = CARTESIAN_POINT ( 'NONE',  ( -59.44456063193725015, -135.5625000013656063, -0.3552334253322034230 ) ) ;
#8620 = CARTESIAN_POINT ( 'NONE',  ( -2.229367062500000163, -56.72916666530107221, -3.861377020970580443 ) ) ;
#8621 = CARTESIAN_POINT ( 'NONE',  ( 5.000000000000000888, -74.45833333060214443, 2.886751345948126879 ) ) ;
#8623 = ORIENTED_EDGE ( 'NONE', *, *, #7348, .T. ) ;
#8622 = CARTESIAN_POINT ( 'NONE',  ( 6.123233995736766282E-16, -170.0000000000000000, -5.000000000000000000 ) ) ;
#8624 = CARTESIAN_POINT ( 'NONE',  ( -50.18089887299979068, -147.6875000000000284, 2.462841084822635640 ) ) ;
#8625 = CARTESIAN_POINT ( 'NONE',  ( 2.229367062500001939, -23.22916666530107221, 3.861377020970579999 ) ) ;
#8627 = ORIENTED_EDGE ( 'NONE', *, *, #6629, .T. ) ;
#8626 = CARTESIAN_POINT ( 'NONE',  ( 2.229367062499998831, -56.89583333196773651, -3.861377020970580887 ) ) ;
#8628 = CARTESIAN_POINT ( 'NONE',  ( -1.846868145590737420, -167.0000000013655779, 4.458734124999999437 ) ) ;
#8629 = CARTESIAN_POINT ( 'NONE',  ( 4.458734125000001214, -102.1458333319677365, 2.574251347313718519 ) ) ;
#8630 = CARTESIAN_POINT ( 'NONE',  ( -2.071067811865459518, -167.4375000027312126, 5.000000000000019540 ) ) ;
#8631 = ORIENTED_EDGE ( 'NONE', *, *, #61486, .T. ) ;
#8632 = CARTESIAN_POINT ( 'NONE',  ( -52.10840900171896806, -151.4375000013656063, 3.393966926194110556 ) ) ;
#8633 = CARTESIAN_POINT ( 'NONE',  ( -57.46284108482265651, -142.0625000027311842, 4.819101127000239515 ) ) ;
#8634 = DIRECTION ( 'NONE',  ( -0.000000000000000000, 1.000000000000000000, -0.000000000000000000 ) ) ;
#8635 = EDGE_CURVE ( 'NONE', #45572, #20487, #59586, .T. ) ;
#8636 = CARTESIAN_POINT ( 'NONE',  ( 4.458734124999998549, -9.729166665301068662, -2.574251347313721627 ) ) ;
#8637 = CARTESIAN_POINT ( 'NONE',  ( 4.458734124999999437, -100.0624999986344079, -5.460374474430324690E-16 ) ) ;
#8638 = CARTESIAN_POINT ( 'NONE',  ( 4.458734125000000326, -144.6250000013655779, -1.846868145590734978 ) ) ;
#8639 = CARTESIAN_POINT ( 'NONE',  ( -4.458734124999998549, -28.47916666530107221, 2.574251347313722516 ) ) ;
#8640 = CARTESIAN_POINT ( 'NONE',  ( 6.123233995736766282E-16, -170.0000000000000000, -5.000000000000000000 ) ) ;
#8641 = CARTESIAN_POINT ( 'NONE',  ( -50.55543936806279248, -137.0625000013656063, 0.3552334253322060320 ) ) ;
#8642 = CARTESIAN_POINT ( 'NONE',  ( -4.458734124999999437, -70.64583333196773651, -2.574251347313719407 ) ) ;
#8643 = CARTESIAN_POINT ( 'NONE',  ( -1.339745962155610925, -90.79465819873853150, 5.000000000000000000 ) ) ;
#8644 = CARTESIAN_POINT ( 'NONE',  ( 1.975475456537005874E-15, -33.75000000000000000, 5.000000000000000000 ) ) ;
#8645 = CARTESIAN_POINT ( 'NONE',  ( -1.846868145590737420, -141.7500000013655779, 4.458734124999997661 ) ) ;
#8646 = CARTESIAN_POINT ( 'NONE',  ( -4.458734124999999437, 11.35416666803225993, -2.574251347313719407 ) ) ;
#8647 = ORIENTED_EDGE ( 'NONE', *, *, #35025, .T. ) ;
#8648 = CARTESIAN_POINT ( 'NONE',  ( -5.926426369611017623E-15, 26.25000000000000000, 5.000000000000000000 ) ) ;
#8649 = CARTESIAN_POINT ( 'NONE',  ( 5.000000000000000000, 2.583333333333333481, -2.886751345948130876 ) ) ;
#8651 = CARTESIAN_POINT ( 'NONE',  ( 2.229367062500001939, -23.97916666530107577, 3.861377020970579999 ) ) ;
#8650 = CARTESIAN_POINT ( 'NONE',  ( 1.060575238724906964E-15, -90.75000000000000000, 5.773502691896257311 ) ) ;
#8652 = CARTESIAN_POINT ( 'NONE',  ( -4.999999999999998224, 7.208333336064517205, 2.886751345948131764 ) ) ;
#8653 = CARTESIAN_POINT ( 'NONE',  ( 4.458734125000001214, -76.14583333196773651, 2.574251347313718519 ) ) ;
#8654 = CARTESIAN_POINT ( 'NONE',  ( -4.458734124999999437, 23.43750000136559564, 0.000000000000000000 ) ) ;
#8655 = CARTESIAN_POINT ( 'NONE',  ( 5.000000000000000888, -79.45833333060213022, 2.886751345948126879 ) ) ;
#8656 = CARTESIAN_POINT ( 'NONE',  ( -52.80376928212989185, -141.8750000013655779, -4.297418129356379346 ) ) ;
#8657 = CARTESIAN_POINT ( 'NONE',  ( 9.457646018065525792E-16, 4.937500001365595637, 5.148502694627439702 ) ) ;
#8658 = EDGE_CURVE ( 'NONE', #47006, #50188, #50942, .T. ) ;
#8659 = CARTESIAN_POINT ( 'NONE',  ( -4.458734124999999437, -35.64583333196772941, -2.574251347313719407 ) ) ;
#8660 =( BOUNDED_CURVE ( )  B_SPLINE_CURVE ( 2, ( #48800, #53322, #28870, #33702, #4740, #18283, #58144 ),
 .UNSPECIFIED., .F., .F. ) 
 B_SPLINE_CURVE_WITH_KNOTS ( ( 3, 2, 2, 3 ),
 ( 0.6249999999999996669, 0.6291666666666664298, 0.6333333333333331927, 0.6375000000985409088 ),
 .UNSPECIFIED. ) 
 CURVE ( )  GEOMETRIC_REPRESENTATION_ITEM ( )  RATIONAL_B_SPLINE_CURVE ( ( 1.000000000000005995, 0.9238795325112806323, 1.000000000000000000, 0.9238795325112867385, 1.000000000000000000, 0.9238795325112867385, 1.000000000000000000 ) ) 
 REPRESENTATION_ITEM ( '' )  );
#8661 = DIRECTION ( 'NONE',  ( 0.000000000000000000, 0.000000000000000000, 1.000000000000000000 ) ) ;
#8662 = CARTESIAN_POINT ( 'NONE',  ( 9.457646018065525792E-16, 4.937500001365595637, 5.148502694627439702 ) ) ;
#8663 = CARTESIAN_POINT ( 'NONE',  ( -2.229367062500000163, -73.47916666530106511, -3.861377020970580443 ) ) ;
#8664 = CARTESIAN_POINT ( 'NONE',  ( -2.229367062500000163, -25.72916666530106866, -3.861377020970580443 ) ) ;
#8665 =( BOUNDED_CURVE ( )  B_SPLINE_CURVE ( 2, ( #52364, #42693, #7674, #3476, #37560, #2848, #38197, #22469, #8606 ),
 .UNSPECIFIED., .F., .F. ) 
 B_SPLINE_CURVE_WITH_KNOTS ( ( 3, 2, 2, 2, 3 ),
 ( 0.9839285714285714857, 0.9845238095238095788, 0.9857142857142857650, 0.9869047619047619513, 0.9875000000000000444 ),
 .UNSPECIFIED. ) 
 CURVE ( )  GEOMETRIC_REPRESENTATION_ITEM ( )  RATIONAL_B_SPLINE_CURVE ( ( 0.9330127018922194093, 0.9330127018922256266, 1.000000000000000000, 0.8660254037844387076, 1.000000000000000000, 0.8660254037844387076, 1.000000000000000000, 0.9330127018922194093, 0.9330127018922194093 ) ) 
 REPRESENTATION_ITEM ( '' )  );
#8666 = CARTESIAN_POINT ( 'NONE',  ( 1.846868145590735200, -157.2500000013656063, -4.458734125000000326 ) ) ;
#8667 = CARTESIAN_POINT ( 'NONE',  ( -2.229367062500000163, -64.47916666530106511, -3.861377020970580443 ) ) ;
#8668 = CARTESIAN_POINT ( 'NONE',  ( 2.499999999999998668, -99.20833333060214443, -4.330127018922193649 ) ) ;
#8669 = CARTESIAN_POINT ( 'NONE',  ( 1.339745962155612702, -41.29465819873852439, -5.000000000000000000 ) ) ;
#8670 = CARTESIAN_POINT ( 'NONE',  ( 2.229367062499998831, -39.64583333196773651, -3.861377020970580887 ) ) ;
#8671 = CARTESIAN_POINT ( 'NONE',  ( -1.339745962155610925, -83.79465819873851729, 5.000000000000000000 ) ) ;
#8672 = CARTESIAN_POINT ( 'NONE',  ( 4.458734124999998549, -105.9791666653010651, -2.574251347313721627 ) ) ;
#8673 = CARTESIAN_POINT ( 'NONE',  ( 2.229367062500001939, -69.22916666530107932, 3.861377020970579999 ) ) ;
#8674 = CARTESIAN_POINT ( 'NONE',  ( 1.060575238724906964E-15, -56.74999999999999289, 5.773502691896257311 ) ) ;
#8675 = CARTESIAN_POINT ( 'NONE',  ( 5.000000000000000000, -72.29166666393548724, -2.886751345948130876 ) ) ;
#8676 = CYLINDRICAL_SURFACE ( 'NONE', #15054, 5.000000000000000000 ) ;
#8677 = ORIENTED_EDGE ( 'NONE', *, *, #59480, .T. ) ;
#8678 = CARTESIAN_POINT ( 'NONE',  ( 5.000000000000000000, -94.50000000000000000, -6.123233995736766282E-16 ) ) ;
#8679 = CARTESIAN_POINT ( 'NONE',  ( -5.147856630858197489E-14, 2.375000002731183724, 5.000000000000000000 ) ) ;
#8680 = CARTESIAN_POINT ( 'NONE',  ( 5.000000000000000000, -15.50000000000000000, -6.123233995736766282E-16 ) ) ;
#8681 = CARTESIAN_POINT ( 'NONE',  ( 4.458734125000001214, -18.89583333196773651, 2.574251347313718519 ) ) ;
#8682 = EDGE_CURVE ( 'NONE', #54505, #38362, #17307, .T. ) ;
#8683 = CARTESIAN_POINT ( 'NONE',  ( 4.458734125000000326, -78.89583333196775072, 2.574251347313718519 ) ) ;
#8684 = CARTESIAN_POINT ( 'NONE',  ( -6.972266317189433020E-16, -59.12499999726880873, -5.000000000000000000 ) ) ;
#8685 = CARTESIAN_POINT ( 'NONE',  ( 2.499999999999998668, -14.20833333060214976, -4.330127018922193649 ) ) ;
#8687 = VERTEX_POINT ( 'NONE', #12480 ) ;
#8686 = CARTESIAN_POINT ( 'NONE',  ( 4.458734125000001214, -46.89583333196773651, 2.574251347313718519 ) ) ;
#8688 = CARTESIAN_POINT ( 'NONE',  ( 0.000000000000000000, -120.0000000000000000, 0.000000000000000000 ) ) ;
#8690 = ORIENTED_EDGE ( 'NONE', *, *, #4017, .T. ) ;
#8689 = CARTESIAN_POINT ( 'NONE',  ( 4.458734125000001214, 6.854166668032259935, 2.574251347313718519 ) ) ;
#8691 = CARTESIAN_POINT ( 'NONE',  ( -59.44456063193725015, -153.5625000013656063, -0.3552334253322034230 ) ) ;
#8692 = CARTESIAN_POINT ( 'NONE',  ( 1.060575238724906964E-15, -58.75000000000000000, 5.773502691896257311 ) ) ;
#8693 = CARTESIAN_POINT ( 'NONE',  ( -4.458734124999999437, -156.1875000013655779, -5.460374474430324690E-16 ) ) ;
#8694 = CARTESIAN_POINT ( 'NONE',  ( -2.229367062499996610, -34.39583333196772941, 3.861377020970582219 ) ) ;
#8695 = CARTESIAN_POINT ( 'NONE',  ( -51.75738570946856498, -149.8750000027312126, 3.805975901505576964 ) ) ;
#8696 = CARTESIAN_POINT ( 'NONE',  ( -5.000000000000000888, -166.4375000000000568, 2.071067811865474617 ) ) ;
#8697 = CARTESIAN_POINT ( 'NONE',  ( 5.000000000000000000, -168.0000000000000000, 0.000000000000000000 ) ) ;
#8698 = CARTESIAN_POINT ( 'NONE',  ( -52.80376928212989185, -131.1250000013655779, -4.297418129356379346 ) ) ;
#8699 = CARTESIAN_POINT ( 'NONE',  ( 4.458734124999998549, -7.979166665301073991, -2.574251347313721627 ) ) ;
#8700 = CARTESIAN_POINT ( 'NONE',  ( 2.229367062499998831, -41.89583333196773651, -3.861377020970580887 ) ) ;
#8701 = CARTESIAN_POINT ( 'NONE',  ( 5.000000000000000000, -54.49999999999999289, -6.123233995736766282E-16 ) ) ;
#8702 = CARTESIAN_POINT ( 'NONE',  ( -4.458734125000000326, -154.0000000013655779, -1.846868145590735644 ) ) ;
#8703 = CARTESIAN_POINT ( 'NONE',  ( -4.458734124999998549, -82.47916666530106511, 2.574251347313722516 ) ) ;
#8704 = CARTESIAN_POINT ( 'NONE',  ( -53.33387254593716875, -142.8125000000000284, 5.149110718188532942 ) ) ;
#8705 = ORIENTED_EDGE ( 'NONE', *, *, #46518, .F. ) ;
#8706 = CARTESIAN_POINT ( 'NONE',  ( -49.85088928181150436, -153.6875000027311842, -1.666127454062680702 ) ) ;
#8707 =( BOUNDED_CURVE ( )  B_SPLINE_CURVE ( 2, ( #55727, #49927, #11642, #60559, #16481, #36102, #50577, #16798, #35468 ),
 .UNSPECIFIED., .F., .F. ) 
 B_SPLINE_CURVE_WITH_KNOTS ( ( 3, 2, 2, 2, 3 ),
 ( 0.4160714285714285920, 0.4166666666666666852, 0.4178571428571428714, 0.4190476190476190577, 0.4196428571428571508 ),
 .UNSPECIFIED. ) 
 CURVE ( )  GEOMETRIC_REPRESENTATION_ITEM ( )  RATIONAL_B_SPLINE_CURVE ( ( 0.9330127018922194093, 0.9330127018922194093, 1.000000000000000000, 0.8660254037844387076, 1.000000000000000000, 0.8660254037844387076, 1.000000000000000000, 0.9330127018922194093, 0.9330127018922194093 ) ) 
 REPRESENTATION_ITEM ( '' )  );
#8708 = CARTESIAN_POINT ( 'NONE',  ( -1.339745962155613812, -105.2053418012614827, -5.000000000000000000 ) ) ;
#8709 = CARTESIAN_POINT ( 'NONE',  ( 4.458734124999998549, -69.97916666530107932, -2.574251347313721627 ) ) ;
#8710 = CARTESIAN_POINT ( 'NONE',  ( -4.458734124999999437, -145.1875000013656063, -5.460374474430324690E-16 ) ) ;
#8711 = ORIENTED_EDGE ( 'NONE', *, *, #8292, .F. ) ;
#8712 = ADVANCED_FACE ( 'NONE', ( #2526 ), #26965, .T. ) ;
#8713 = EDGE_CURVE ( 'NONE', #58923, #37814, #47217, .T. ) ;
#8714 = CYLINDRICAL_SURFACE ( 'NONE', #32894, 5.000000000000000000 ) ;
#8715 = CARTESIAN_POINT ( 'NONE',  ( -4.458734124999999437, -10.64583333196773829, -2.574251347313719407 ) ) ;
#8716 = ADVANCED_FACE ( 'NONE', ( #36610 ), #17931, .T. ) ;
#8717 = CARTESIAN_POINT ( 'NONE',  ( 1.975475456537005874E-15, 17.25000000000000000, 5.000000000000000000 ) ) ;
#8718 = CARTESIAN_POINT ( 'NONE',  ( -2.229367062500000163, 4.520833334698926897, -3.861377020970580443 ) ) ;
#8719 = CARTESIAN_POINT ( 'NONE',  ( -5.000000000000000000, -80.08333333333332860, -2.886751345948128211 ) ) ;
#8720 = CARTESIAN_POINT ( 'NONE',  ( 2.730187237215162345E-16, -152.1875000013656063, -4.458734124999999437 ) ) ;
#8721 = ADVANCED_FACE ( 'NONE', ( #27276 ), #32414, .T. ) ;
#8722 = CARTESIAN_POINT ( 'NONE',  ( 4.458734125000000326, 24.85416666803225993, 2.574251347313718519 ) ) ;
#8723 = ORIENTED_EDGE ( 'NONE', *, *, #63433, .T. ) ;
#8724 = CARTESIAN_POINT ( 'NONE',  ( -3.152548672688508926E-16, -89.56249999863439371, -5.148502694627439702 ) ) ;
#8725 = CARTESIAN_POINT ( 'NONE',  ( -5.000000000000000000, -68.08333333333332860, -2.886751345948128211 ) ) ;
#8726 = CARTESIAN_POINT ( 'NONE',  ( 5.000000000000000888, 7.541666669397851130, 2.886751345948126879 ) ) ;
#8727 = CARTESIAN_POINT ( 'NONE',  ( -2.229367062500000163, -6.479166665301072214, -3.861377020970580443 ) ) ;
#8728 = EDGE_CURVE ( 'NONE', #7140, #60995, #3160, .T. ) ;
#8730 = EDGE_CURVE ( 'NONE', #10267, #5205, #57527, .T. ) ;
#8729 = CARTESIAN_POINT ( 'NONE',  ( 1.975475456537005874E-15, -37.74999999999999289, 5.000000000000000000 ) ) ;
#8731 = CARTESIAN_POINT ( 'NONE',  ( -51.75738570946856498, -144.7500000000000284, 3.805975901505576964 ) ) ;
#8732 = AXIS2_PLACEMENT_3D ( 'NONE', #54348, #35051, #44357 ) ;
#8733 = CARTESIAN_POINT ( 'NONE',  ( -57.89159099828107458, -153.6875000013656063, -3.393966926194107447 ) ) ;
#8734 = CARTESIAN_POINT ( 'NONE',  ( -4.999999999999999112, -37.79166666393547303, 2.886751345948131764 ) ) ;
#8735 = CARTESIAN_POINT ( 'NONE',  ( 1.339745962155615144, -29.70534180126147561, 4.999999999999999112 ) ) ;
#8736 = CARTESIAN_POINT ( 'NONE',  ( 2.229367062500001939, 20.02083333469892779, 3.861377020970579999 ) ) ;
#8737 = CARTESIAN_POINT ( 'NONE',  ( 1.975475456537005874E-15, -51.62499999726880873, 5.000000000000000000 ) ) ;
#8738 = CARTESIAN_POINT ( 'NONE',  ( 2.229367062499998831, 24.35416666803225993, -3.861377020970580887 ) ) ;
#8739 = EDGE_CURVE ( 'NONE', #13144, #55337, #15615, .T. ) ;
#8740 = CARTESIAN_POINT ( 'NONE',  ( -4.458734124999999437, -57.31249999863440081, 0.000000000000000000 ) ) ;
#8741 = CARTESIAN_POINT ( 'NONE',  ( -2.229367062499996610, -3.395833331967738733, 3.861377020970582219 ) ) ;
#8742 = CARTESIAN_POINT ( 'NONE',  ( 2.500000000000002220, 11.33333333333333393, 4.330127018922192761 ) ) ;
#8743 = EDGE_CURVE ( 'NONE', #7560, #14071, #5286, .T. ) ;
#8744 = CARTESIAN_POINT ( 'NONE',  ( -3.535533905932737309, -140.7500000027311842, -3.535533905932738197 ) ) ;
#8746 = ADVANCED_FACE ( 'NONE', ( #55806 ), #20752, .T. ) ;
#8745 = DIRECTION ( 'NONE',  ( 0.000000000000000000, 1.000000000000000000, 0.000000000000000000 ) ) ;
#8747 = CARTESIAN_POINT ( 'NONE',  ( 2.229367062499998831, -50.64583333196772941, -3.861377020970580887 ) ) ;
#8748 = CARTESIAN_POINT ( 'NONE',  ( 2.500000000000002220, -82.54166666393547303, 4.330127018922192761 ) ) ;
#8749 = CARTESIAN_POINT ( 'NONE',  ( -51.60603307380591787, -135.1875000013656063, -2.891590998281053704 ) ) ;
#8750 = DIRECTION ( 'NONE',  ( 0.000000000000000000, 0.000000000000000000, 1.000000000000000000 ) ) ;
#8751 = LINE ( 'NONE', #43148, #63459 ) ;
#8752 = CARTESIAN_POINT ( 'NONE',  ( -4.458734124999997661, -92.47916666530106511, 2.574251347313722516 ) ) ;
#8753 = CARTESIAN_POINT ( 'NONE',  ( 4.458734124999999437, -158.6875000013655779, 0.000000000000000000 ) ) ;
#8754 = CARTESIAN_POINT ( 'NONE',  ( 2.499999999999998668, -40.33333333333332860, -4.330127018922193649 ) ) ;
#8755 = EDGE_LOOP ( 'NONE', ( #42090, #4424, #49121, #32813 ) ) ;
#8756 = CARTESIAN_POINT ( 'NONE',  ( -4.458734124999999437, 16.35416666803225993, -2.574251347313719407 ) ) ;
#8757 = ORIENTED_EDGE ( 'NONE', *, *, #34543, .F. ) ;
#8758 = CARTESIAN_POINT ( 'NONE',  ( -2.229367062499996610, -94.14583333196772230, 3.861377020970582219 ) ) ;
#8759 = CARTESIAN_POINT ( 'NONE',  ( -4.458734124999998549, 6.520833334698930450, 2.574251347313722516 ) ) ;
#8760 = CARTESIAN_POINT ( 'NONE',  ( -3.535250795749689387E-16, 11.87500000273118594, -5.773502691896257311 ) ) ;
#8761 = CARTESIAN_POINT ( 'NONE',  ( 1.975475456537005874E-15, 7.249999999999998224, 5.000000000000000000 ) ) ;
#8762 = CARTESIAN_POINT ( 'NONE',  ( -2.499999999999996447, 4.166666666666666075, 4.330127018922195425 ) ) ;
#8763 = CARTESIAN_POINT ( 'NONE',  ( 4.458734124999999437, -60.81249999863440081, -5.460374474430324690E-16 ) ) ;
#8764 = CARTESIAN_POINT ( 'NONE',  ( -2.499999999999996447, 15.29166666939785202, 4.330127018922195425 ) ) ;
#8765 = CARTESIAN_POINT ( 'NONE',  ( -5.000000000000000000, 2.125000002731185056, 0.000000000000000000 ) ) ;
#8766 = CARTESIAN_POINT ( 'NONE',  ( -4.458734124999999437, -27.39583333196773651, -2.574251347313719407 ) ) ;
#8767 = CARTESIAN_POINT ( 'NONE',  ( -58.24261429053147765, -144.3750000027312126, -3.805975901505573855 ) ) ;
#8768 = CARTESIAN_POINT ( 'NONE',  ( 5.000000000000000888, -63.58333333333332860, 2.886751345948126879 ) ) ;
#8769 = DIRECTION ( 'NONE',  ( -0.000000000000000000, 1.000000000000000000, -0.000000000000000000 ) ) ;
#8770 = CARTESIAN_POINT ( 'NONE',  ( 5.000000000000000888, -43.58333333333333570, 2.886751345948126879 ) ) ;
#8772 = CARTESIAN_POINT ( 'NONE',  ( -4.458734124999998549, -20.47916666530107577, 2.574251347313722516 ) ) ;
#8771 = CARTESIAN_POINT ( 'NONE',  ( 1.464175926609780648E-14, 23.87500000273118417, -5.000000000000000000 ) ) ;
#8773 = CARTESIAN_POINT ( 'NONE',  ( -6.972266317189433020E-16, -64.24999999999998579, -5.000000000000000000 ) ) ;
#8774 = CARTESIAN_POINT ( 'NONE',  ( -2.229367062500000163, -66.47916666530106511, -3.861377020970580443 ) ) ;
#8775 = CARTESIAN_POINT ( 'NONE',  ( -4.458734124999999437, -146.1875000013656063, -5.460374474430324690E-16 ) ) ;
#8776 = CARTESIAN_POINT ( 'NONE',  ( -4.458734124999998549, -78.22916666530106511, 2.574251347313722516 ) ) ;
#8777 = CARTESIAN_POINT ( 'NONE',  ( -50.40829686548195099, -143.2500000013656063, -1.485763867205728284 ) ) ;
#8778 = CARTESIAN_POINT ( 'NONE',  ( 9.457646018065525792E-16, -27.31249999863440436, 5.148502694627439702 ) ) ;
#8779 = CARTESIAN_POINT ( 'NONE',  ( 5.000000000000000888, -65.45833333060214443, 2.886751345948126879 ) ) ;
#8780 = ORIENTED_EDGE ( 'NONE', *, *, #35360, .F. ) ;
#8781 = CARTESIAN_POINT ( 'NONE',  ( 1.339745962155612702, -1.294658198738520172, -5.000000000000000000 ) ) ;
#8782 = ORIENTED_EDGE ( 'NONE', *, *, #37063, .T. ) ;
#8783 = CARTESIAN_POINT ( 'NONE',  ( 4.458734124999998549, -68.97916666530106511, -2.574251347313721627 ) ) ;
#8784 = LINE ( 'NONE', #13614, #58446 ) ;
#8785 = CARTESIAN_POINT ( 'NONE',  ( -4.999999999999998224, -5.791666663935480130, 2.886751345948131764 ) ) ;
#8786 = VERTEX_POINT ( 'NONE', #25572 ) ;
#8787 = FACE_OUTER_BOUND ( 'NONE', #46513, .T. ) ;
#8788 = CARTESIAN_POINT ( 'NONE',  ( 2.229367062499998831, -52.89583333196773651, -3.861377020970580887 ) ) ;
#8789 = CARTESIAN_POINT ( 'NONE',  ( -4.458734124999999437, 1.437500001365592972, 0.000000000000000000 ) ) ;
#8790 = ORIENTED_EDGE ( 'NONE', *, *, #27471, .F. ) ;
#8791 =( BOUNDED_CURVE ( )  B_SPLINE_CURVE ( 2, ( #40810, #12500, #22162, #21531, #60775, #51116, #61092, #7053, #21204 ),
 .UNSPECIFIED., .F., .F. ) 
 B_SPLINE_CURVE_WITH_KNOTS ( ( 3, 2, 2, 2, 3 ),
 ( 0.3624999999999999889, 0.3630952380952380820, 0.3642857142857142683, 0.3654761904761904545, 0.3660714285714285476 ),
 .UNSPECIFIED. ) 
 CURVE ( )  GEOMETRIC_REPRESENTATION_ITEM ( )  RATIONAL_B_SPLINE_CURVE ( ( 0.9330127018922194093, 0.9330127018922194093, 1.000000000000000000, 0.8660254037844387076, 1.000000000000000000, 0.8660254037844387076, 1.000000000000000000, 0.9330127018922194093, 0.9330127018922194093 ) ) 
 REPRESENTATION_ITEM ( '' )  );
#8792 = FACE_OUTER_BOUND ( 'NONE', #44632, .T. ) ;
#8793 = CARTESIAN_POINT ( 'NONE',  ( 4.458734124999998549, 1.270833334698927342, -2.574251347313721627 ) ) ;
#8794 = CARTESIAN_POINT ( 'NONE',  ( 4.458734124999998549, 16.27083333469892779, -2.574251347313721627 ) ) ;
#8795 = CARTESIAN_POINT ( 'NONE',  ( -51.60603307380591787, -145.9375000013656063, -2.891590998281053704 ) ) ;
#8796 = CARTESIAN_POINT ( 'NONE',  ( 2.500000000000002220, 16.33333333333333215, 4.330127018922192761 ) ) ;
#8797 = CARTESIAN_POINT ( 'NONE',  ( 1.846868145590736310, -166.6250000013656063, 4.458734124999997661 ) ) ;
#8798 = ORIENTED_EDGE ( 'NONE', *, *, #4031, .T. ) ;
#8799 = CARTESIAN_POINT ( 'NONE',  ( -2.229367062499996610, -78.14583333196773651, 3.861377020970582219 ) ) ;
#8800 = DIRECTION ( 'NONE',  ( -0.000000000000000000, 1.000000000000000000, -0.000000000000000000 ) ) ;
#8801 = CARTESIAN_POINT ( 'NONE',  ( 2.229367062499998831, 9.354166668032261711, -3.861377020970580887 ) ) ;
#8802 =( BOUNDED_CURVE ( )  B_SPLINE_CURVE ( 2, ( #22383, #9768, #23947, #49336, #34524, #465, #30345, #44501, #4327 ),
 .UNSPECIFIED., .F., .F. ) 
 B_SPLINE_CURVE_WITH_KNOTS ( ( 3, 2, 2, 2, 3 ),
 ( 0.2062499999999999889, 0.2069444444444444309, 0.2083333333333333426, 0.2097222222222222265, 0.2104166666666666685 ),
 .UNSPECIFIED. ) 
 CURVE ( )  GEOMETRIC_REPRESENTATION_ITEM ( )  RATIONAL_B_SPLINE_CURVE ( ( 0.9330127018922194093, 0.9330127018922194093, 1.000000000000000000, 0.8660254037844387076, 1.000000000000000000, 0.8660254037844387076, 1.000000000000000000, 0.9330127018922194093, 0.9330127018922194093 ) ) 
 REPRESENTATION_ITEM ( '' )  );
#8803 = CARTESIAN_POINT ( 'NONE',  ( -5.000000000000000000, -162.6250000027311842, -6.123233995736766282E-16 ) ) ;
#8804 = CARTESIAN_POINT ( 'NONE',  ( 9.457646018065525792E-16, -58.31249999863440792, 5.148502694627439702 ) ) ;
#8805 = CARTESIAN_POINT ( 'NONE',  ( 5.000000000000000000, -20.29166666393548368, -2.886751345948129988 ) ) ;
#8806 = CARTESIAN_POINT ( 'NONE',  ( 1.975475456537005874E-15, 1.375000002731185500, 5.000000000000000000 ) ) ;
#8807 = FACE_OUTER_BOUND ( 'NONE', #59150, .T. ) ;
#8808 = LINE ( 'NONE', #37769, #20258 ) ;
#8809 = CARTESIAN_POINT ( 'NONE',  ( 1.975475456537005874E-15, -105.6249999972688016, 5.000000000000000000 ) ) ;
#8810 = DIRECTION ( 'NONE',  ( -0.000000000000000000, 1.000000000000000000, -0.000000000000000000 ) ) ;
#8811 = EDGE_CURVE ( 'NONE', #13416, #59564, #409, .T. ) ;
#8812 = CARTESIAN_POINT ( 'NONE',  ( 2.229367062500001939, -40.97916666530107221, 3.861377020970579999 ) ) ;
#8813 = CARTESIAN_POINT ( 'NONE',  ( 4.458734125000000326, -29.14583333196774007, 2.574251347313718519 ) ) ;
#8814 = CARTESIAN_POINT ( 'NONE',  ( -58.24261429053147765, -152.2500000000000284, -3.805975901505573855 ) ) ;
#8815 = CARTESIAN_POINT ( 'NONE',  ( 5.000000000000000888, 24.41666666666666785, 2.886751345948126879 ) ) ;
#8816 = CARTESIAN_POINT ( 'NONE',  ( -2.071067811865475061, -153.8125000027311842, -5.000000000000000888 ) ) ;
#8817 = ORIENTED_EDGE ( 'NONE', *, *, #18172, .T. ) ;
#8818 = CARTESIAN_POINT ( 'NONE',  ( -4.458734124999999437, -105.6458333319677507, -2.574251347313719407 ) ) ;
#8819 = CARTESIAN_POINT ( 'NONE',  ( -2.229367062499996610, -32.14583333196773651, 3.861377020970582219 ) ) ;
#8820 = CARTESIAN_POINT ( 'NONE',  ( 5.000000000000000888, -66.45833333060214443, 2.886751345948126879 ) ) ;
#8821 = AXIS2_PLACEMENT_3D ( 'NONE', #32656, #12407, #7593 ) ;
#8822 = CARTESIAN_POINT ( 'NONE',  ( -56.48576386720575471, -150.0000000013655779, -4.591703134518078322 ) ) ;
#8823 = CARTESIAN_POINT ( 'NONE',  ( 5.000000000000000000, -141.0625000000000000, 2.071067811865478614 ) ) ;
#8824 = EDGE_CURVE ( 'NONE', #46916, #53830, #13555, .T. ) ;
#8825 = CARTESIAN_POINT ( 'NONE',  ( -4.458734124999999437, -29.31249999863440436, 0.000000000000000000 ) ) ;
#8826 = CARTESIAN_POINT ( 'NONE',  ( -2.229367062500000163, -76.72916666530106511, -3.861377020970580443 ) ) ;
#8827 = CARTESIAN_POINT ( 'NONE',  ( 5.000000000000000888, 22.54166666939785202, 2.886751345948126879 ) ) ;
#8828 = CARTESIAN_POINT ( 'NONE',  ( -2.229367062500000163, -30.47916666530107221, -3.861377020970580443 ) ) ;
#8829 = CARTESIAN_POINT ( 'NONE',  ( -51.75738570946856498, -147.7500000000000284, 3.805975901505576964 ) ) ;
#8830 = DIRECTION ( 'NONE',  ( -0.000000000000000000, 1.000000000000000000, -0.000000000000000000 ) ) ;
#8831 = CARTESIAN_POINT ( 'NONE',  ( -4.999999999999999112, -19.91666666666666785, 2.886751345948131764 ) ) ;
#8832 = CARTESIAN_POINT ( 'NONE',  ( -3.152801135295367096, -146.0625000013655779, -3.152801135295367541 ) ) ;
#8833 = ORIENTED_EDGE ( 'NONE', *, *, #9370, .T. ) ;
#8834 = CARTESIAN_POINT ( 'NONE',  ( -6.972266317189433020E-16, 1.750000000000000444, -5.000000000000000000 ) ) ;
#8835 = CARTESIAN_POINT ( 'NONE',  ( 9.457646018065525792E-16, -59.31249999863440081, 5.148502694627439702 ) ) ;
#8836 = CARTESIAN_POINT ( 'NONE',  ( -5.000000000000000000, 26.04166666939784847, -2.886751345948128211 ) ) ;
#8837 = CARTESIAN_POINT ( 'NONE',  ( -5.000000000000000000, -162.5000000000000000, -6.123233995736766282E-16 ) ) ;
#8838 = CARTESIAN_POINT ( 'NONE',  ( 5.000000000000000888, 20.41666666666666430, 2.886751345948126879 ) ) ;
#8839 = LINE ( 'NONE', #57739, #34495 ) ;
#8840 = CARTESIAN_POINT ( 'NONE',  ( -3.152548672688508926E-16, -2.562499998634407028, -5.148502694627439702 ) ) ;
#8841 = CARTESIAN_POINT ( 'NONE',  ( 3.253724281355068545E-15, 28.75000000000000000, -5.000000000000000000 ) ) ;
#8842 = CARTESIAN_POINT ( 'NONE',  ( 6.123233995736766282E-16, -120.0000000000000000, -5.000000000000000000 ) ) ;
#8843 = CARTESIAN_POINT ( 'NONE',  ( 9.457646018065525792E-16, 12.68750000136559208, 5.148502694627439702 ) ) ;
#8844 = CARTESIAN_POINT ( 'NONE',  ( -55.00000000000002132, -155.0000000000000284, 1.734723475976807094E-15 ) ) ;
#8845 = ORIENTED_EDGE ( 'NONE', *, *, #2516, .T. ) ;
#8846 = CARTESIAN_POINT ( 'NONE',  ( -51.19402409849444524, -135.5000000000000284, -3.242614290531456334 ) ) ;
#8847 = CARTESIAN_POINT ( 'NONE',  ( -2.229367062500000163, -51.47916666530107221, -3.861377020970580443 ) ) ;
#8848 = CARTESIAN_POINT ( 'NONE',  ( 3.152801135295367541, -161.5625000013656063, -3.152801135295367541 ) ) ;
#8849 = CARTESIAN_POINT ( 'NONE',  ( -2.499999999999996447, -47.70833333060215153, 4.330127018922195425 ) ) ;
#8850 = ORIENTED_EDGE ( 'NONE', *, *, #51213, .F. ) ;
#8851 = CARTESIAN_POINT ( 'NONE',  ( -4.458734124999999437, -23.31249999863440436, 0.000000000000000000 ) ) ;
#8852 = ORIENTED_EDGE ( 'NONE', *, *, #52242, .T. ) ;
#8853 = FACE_OUTER_BOUND ( 'NONE', #34956, .T. ) ;
#8854 = CARTESIAN_POINT ( 'NONE',  ( -4.458734125000000326, -162.0000000013655779, -1.846868145590735644 ) ) ;
#8855 = VERTEX_POINT ( 'NONE', #55493 ) ;
#8856 =( BOUNDED_CURVE ( )  B_SPLINE_CURVE ( 2, ( #18237, #13721, #62938, #37861, #9211, #57494, #33034, #52650, #8585 ),
 .UNSPECIFIED., .F., .F. ) 
 B_SPLINE_CURVE_WITH_KNOTS ( ( 3, 2, 2, 2, 3 ),
 ( 0.9604166666666666963, 0.9611111111111111382, 0.9625000000000000222, 0.9638888888888889062, 0.9645833333333333481 ),
 .UNSPECIFIED. ) 
 CURVE ( )  GEOMETRIC_REPRESENTATION_ITEM ( )  RATIONAL_B_SPLINE_CURVE ( ( 0.9330127018922194093, 0.9330127018922194093, 1.000000000000000000, 0.8660254037844387076, 1.000000000000000000, 0.8660254037844387076, 1.000000000000000000, 0.9330127018922194093, 0.9330127018922194093 ) ) 
 REPRESENTATION_ITEM ( '' )  );
#8857 = VECTOR ( 'NONE', #46815, 1000.000000000000000 ) ;
#8858 = CARTESIAN_POINT ( 'NONE',  ( 1.975475456537005874E-15, -39.62499999726880162, 5.000000000000000000 ) ) ;
#8859 = CARTESIAN_POINT ( 'NONE',  ( -58.24261429053147765, -135.2500000000000284, -3.805975901505573855 ) ) ;
#8860 = CARTESIAN_POINT ( 'NONE',  ( -4.458734124999998549, -36.47916666530107221, 2.574251347313722516 ) ) ;
#8861 = VECTOR ( 'NONE', #26646, 1000.000000000000000 ) ;
#8862 = VERTEX_POINT ( 'NONE', #55170 ) ;
#8863 = CARTESIAN_POINT ( 'NONE',  ( -4.458734124999999437, -83.31249999863439371, 0.000000000000000000 ) ) ;
#8864 = CARTESIAN_POINT ( 'NONE',  ( -4.458734124999999437, 19.60416666803225993, -2.574251347313719407 ) ) ;
#8865 = LINE ( 'NONE', #4660, #61546 ) ;
#8866 = VERTEX_POINT ( 'NONE', #21070 ) ;
#8867 = CARTESIAN_POINT ( 'NONE',  ( -59.59170313451810586, -137.7500000013656063, 1.485763867205729394 ) ) ;
#8868 = CARTESIAN_POINT ( 'NONE',  ( 2.229367062499998831, -86.89583333196773651, -3.861377020970580887 ) ) ;
#8869 = CARTESIAN_POINT ( 'NONE',  ( -52.53715891517739323, -128.5625000027311842, -4.819101127000233298 ) ) ;
#8870 = CARTESIAN_POINT ( 'NONE',  ( 1.975475456537005874E-15, -88.74999999999998579, 5.000000000000000000 ) ) ;
#8871 = CARTESIAN_POINT ( 'NONE',  ( -1.339745962155613812, -7.205341801261479162, -5.000000000000000000 ) ) ;
#8872 = CARTESIAN_POINT ( 'NONE',  ( 1.975475456537005874E-15, -46.62499999726880873, 5.000000000000000000 ) ) ;
#8873 = CARTESIAN_POINT ( 'NONE',  ( 2.229367062500001939, -61.97916666530106511, 3.861377020970579999 ) ) ;
#8874 = CARTESIAN_POINT ( 'NONE',  ( 2.499999999999998668, -37.33333333333332860, -4.330127018922193649 ) ) ;
#8875 = CARTESIAN_POINT ( 'NONE',  ( -3.152548672688508926E-16, 24.43750000136559564, -5.148502694627439702 ) ) ;
#8876 = CARTESIAN_POINT ( 'NONE',  ( 5.000000000000000000, -97.41666666666665719, -2.886751345948130876 ) ) ;
#8877 = CARTESIAN_POINT ( 'NONE',  ( -58.24261429053147765, -155.0000000000000284, -3.805975901505573411 ) ) ;
#8878 = CARTESIAN_POINT ( 'NONE',  ( 2.229367062500001939, -44.22916666530106511, 3.861377020970579999 ) ) ;
#8879 = CARTESIAN_POINT ( 'NONE',  ( 1.060575238724906964E-15, -4.624999997268816720, 5.773502691896257311 ) ) ;
#8880 = DIRECTION ( 'NONE',  ( -0.000000000000000000, 1.000000000000000000, -0.000000000000000000 ) ) ;
#8881 = CARTESIAN_POINT ( 'NONE',  ( -5.000000000000000000, -61.08333333333333570, -2.886751345948128211 ) ) ;
#8882 = CARTESIAN_POINT ( 'NONE',  ( 4.458734124999998549, -84.97916666530106511, -2.574251347313721627 ) ) ;
#8883 = CARTESIAN_POINT ( 'NONE',  ( 4.458734124999998549, -109.7291666653010651, -2.574251347313721627 ) ) ;
#8884 =( BOUNDED_CURVE ( )  B_SPLINE_CURVE ( 2, ( #44580, #5032, #48461, #9538, #38795, #40071, #54234, #14671, #5355 ),
 .UNSPECIFIED., .F., .F. ) 
 B_SPLINE_CURVE_WITH_KNOTS ( ( 3, 2, 2, 2, 3 ),
 ( 0.1083333333333334203, 0.1125000000000000999, 0.1166666666666667657, 0.1208333333333334314, 0.1250000000000001110 ),
 .UNSPECIFIED. ) 
 CURVE ( )  GEOMETRIC_REPRESENTATION_ITEM ( )  RATIONAL_B_SPLINE_CURVE ( ( 0.9999999999999984457, 0.9238795325112882928, 1.000000000000000000, 0.9238795325112867385, 1.000000000000000000, 0.9238795325112867385, 1.000000000000000000, 0.9238795325112847401, 1.000000000000001998 ) ) 
 REPRESENTATION_ITEM ( '' )  );
#8885 = CARTESIAN_POINT ( 'NONE',  ( -4.458734124999997661, -11.47916666530107044, 2.574251347313722516 ) ) ;
#8886 = VERTEX_POINT ( 'NONE', #45505 ) ;
#8887 = CARTESIAN_POINT ( 'NONE',  ( 5.000000000000000000, -52.50000000000000711, -6.123233995736766282E-16 ) ) ;
#8888 = CARTESIAN_POINT ( 'NONE',  ( -4.458734124999999437, -100.3958333319677365, -2.574251347313719407 ) ) ;
#8889 = CARTESIAN_POINT ( 'NONE',  ( 3.061616997868383141E-16, -164.8750000027311842, -5.000000000000000000 ) ) ;
#8890 = CARTESIAN_POINT ( 'NONE',  ( 2.229367062499998831, -92.89583333196773651, -3.861377020970580887 ) ) ;
#8891 = CARTESIAN_POINT ( 'NONE',  ( -3.535250795749689387E-16, -54.12499999726880162, -5.773502691896257311 ) ) ;
#8892 = CARTESIAN_POINT ( 'NONE',  ( -6.972266317189433020E-16, -30.25000000000000000, -5.000000000000000000 ) ) ;
#8893 = CARTESIAN_POINT ( 'NONE',  ( -55.35523342533222291, -130.3125000013656063, 4.444560631937231499 ) ) ;
#8894 = CARTESIAN_POINT ( 'NONE',  ( -59.44456063193725015, -148.5625000013656063, -0.3552334253322034230 ) ) ;
#8895 = CARTESIAN_POINT ( 'NONE',  ( -4.458734124999997661, -12.22916666530106866, 2.574251347313722516 ) ) ;
#8896 = CARTESIAN_POINT ( 'NONE',  ( 9.457646018065525792E-16, 10.68750000136559386, 5.148502694627439702 ) ) ;
#8897 = CARTESIAN_POINT ( 'NONE',  ( -4.458734124999999437, -57.56249999863440081, 0.000000000000000000 ) ) ;
#8898 = CARTESIAN_POINT ( 'NONE',  ( -4.999999999999998224, -19.91666666666666430, 2.886751345948131764 ) ) ;
#8899 = CARTESIAN_POINT ( 'NONE',  ( 4.458734124999999437, -12.81249999863440259, -5.460374474430324690E-16 ) ) ;
#8900 = CYLINDRICAL_SURFACE ( 'NONE', #6415, 5.000000000000000000 ) ;
#8901 = ORIENTED_EDGE ( 'NONE', *, *, #24677, .F. ) ;
#8902 = CARTESIAN_POINT ( 'NONE',  ( 4.458734124999999437, -43.06249999863440081, -5.460374474430324690E-16 ) ) ;
#8903 = VECTOR ( 'NONE', #6289, 1000.000000000000000 ) ;
#8904 = CARTESIAN_POINT ( 'NONE',  ( 5.000000000000000000, -83.29166666393547303, -2.886751345948130876 ) ) ;
#8905 = DIRECTION ( 'NONE',  ( 0.000000000000000000, 0.000000000000000000, 1.000000000000000000 ) ) ;
#8906 = CARTESIAN_POINT ( 'NONE',  ( -2.623433461001184686, 7.604994000793856124, -7.633824513837113912 ) ) ;
#8907 = CARTESIAN_POINT ( 'NONE',  ( 4.458734124999999437, -84.81249999863439371, -5.460374474430324690E-16 ) ) ;
#8908 = CARTESIAN_POINT ( 'NONE',  ( -2.229367062500000163, 20.27083333469892779, -3.861377020970580443 ) ) ;
#8909 = AXIS2_PLACEMENT_3D ( 'NONE', #41908, #17487, #12958 ) ;
#8910 = VECTOR ( 'NONE', #19243, 1000.000000000000000 ) ;
#8911 = CARTESIAN_POINT ( 'NONE',  ( -4.458734124999998549, 13.77083333469892779, 2.574251347313722516 ) ) ;
#8912 = CARTESIAN_POINT ( 'NONE',  ( -4.999999999999998224, -47.91666666666667140, 2.886751345948131764 ) ) ;
#8913 = CIRCLE ( 'NONE', #58273, 4.999999999999999112 ) ;
#8914 = CARTESIAN_POINT ( 'NONE',  ( 1.975475456537005874E-15, -64.62499999726880162, 5.000000000000000000 ) ) ;
#8915 = CARTESIAN_POINT ( 'NONE',  ( 4.458734124999999437, -88.06249999863439371, -5.460374474430324690E-16 ) ) ;
#8916 = CARTESIAN_POINT ( 'NONE',  ( 5.000000000000000000, -72.50000000000000000, -6.123233995736766282E-16 ) ) ;
#8917 = CARTESIAN_POINT ( 'NONE',  ( -2.500000000000000444, 11.95833333606451809, -4.330127018922193649 ) ) ;
#8918 = VERTEX_POINT ( 'NONE', #1468 ) ;
#8919 = CARTESIAN_POINT ( 'NONE',  ( -6.972266317189433020E-16, -28.12499999726880873, -5.000000000000000000 ) ) ;
#8920 = CYLINDRICAL_SURFACE ( 'NONE', #11423, 5.000000000000000000 ) ;
#8921 = CARTESIAN_POINT ( 'NONE',  ( 5.000000000000000000, -29.50000000000000000, -6.123233995736766282E-16 ) ) ;
#8922 = CARTESIAN_POINT ( 'NONE',  ( 4.458734124999999437, -30.81249999863440436, -5.460374474430324690E-16 ) ) ;
#8923 = EDGE_CURVE ( 'NONE', #9785, #55783, #9034, .T. ) ;
#8924 = CARTESIAN_POINT ( 'NONE',  ( -2.499999999999996447, -35.70833333060213732, 4.330127018922195425 ) ) ;
#8926 = ORIENTED_EDGE ( 'NONE', *, *, #10765, .F. ) ;
#8925 = CARTESIAN_POINT ( 'NONE',  ( 4.458734125000001214, -62.89583333196775072, 2.574251347313718519 ) ) ;
#8927 = CARTESIAN_POINT ( 'NONE',  ( -50.40829686548195099, -152.2500000013656347, -1.485763867205728284 ) ) ;
#8929 = ORIENTED_EDGE ( 'NONE', *, *, #12668, .T. ) ;
#8928 = CARTESIAN_POINT ( 'NONE',  ( -2.229367062500000163, -11.72916666530107044, -3.861377020970580443 ) ) ;
#8930 = CARTESIAN_POINT ( 'NONE',  ( 5.000000000000000888, -74.58333333333332860, 2.886751345948126879 ) ) ;
#8931 = CARTESIAN_POINT ( 'NONE',  ( -57.89159099828107458, -135.6875000013656063, -3.393966926194107447 ) ) ;
#8932 = CARTESIAN_POINT ( 'NONE',  ( -2.229367062499996610, -56.39583333196773651, 3.861377020970582219 ) ) ;
#8933 = CARTESIAN_POINT ( 'NONE',  ( -5.000000000000000000, -80.87499999726881583, 0.000000000000000000 ) ) ;
#8935 = EDGE_LOOP ( 'NONE', ( #43647, #49100, #63636, #10125 ) ) ;
#8934 = CARTESIAN_POINT ( 'NONE',  ( -2.499999999999996447, 10.29166666939785024, 4.330127018922195425 ) ) ;
#8936 = CARTESIAN_POINT ( 'NONE',  ( -56.66612745406270335, -145.3125000000000284, -5.149110718188516067 ) ) ;
#8937 = CARTESIAN_POINT ( 'NONE',  ( 4.458734124999999437, -21.06249999863440436, -5.460374474430324690E-16 ) ) ;
#8939 = EDGE_LOOP ( 'NONE', ( #25843, #807, #15291, #7817 ) ) ;
#8938 = CARTESIAN_POINT ( 'NONE',  ( 4.458734125000001214, -57.14583333196773651, 2.574251347313718519 ) ) ;
#8940 = CARTESIAN_POINT ( 'NONE',  ( 4.458734124999999437, -168.6875000013656063, 0.000000000000000000 ) ) ;
#8941 = CARTESIAN_POINT ( 'NONE',  ( -2.229367062500000163, -104.7291666653010651, -3.861377020970580443 ) ) ;
#8942 = CARTESIAN_POINT ( 'NONE',  ( -2.071067811865491493, -167.8125000027311842, -4.999999999999985789 ) ) ;
#8943 = ORIENTED_EDGE ( 'NONE', *, *, #1200, .F. ) ;
#8944 = CARTESIAN_POINT ( 'NONE',  ( -52.80376928212989185, -151.1250000013656347, -4.297418129356378458 ) ) ;
#8945 = CARTESIAN_POINT ( 'NONE',  ( -53.33387254593733928, -138.9375000027312126, 5.149110718188519620 ) ) ;
#8946 = CARTESIAN_POINT ( 'NONE',  ( 2.229367062500001939, -37.97916666530107221, 3.861377020970579999 ) ) ;
#8947 = AXIS2_PLACEMENT_3D ( 'NONE', #27536, #2793, #61651 ) ;
#8948 = CARTESIAN_POINT ( 'NONE',  ( -62.00000000000001421, -155.0000000000000284, 4.041451884327384114 ) ) ;
#8949 = AXIS2_PLACEMENT_3D ( 'NONE', #56709, #3311, #37706 ) ;
#8950 = CARTESIAN_POINT ( 'NONE',  ( 4.458734125000001214, -7.895833331967735624, 2.574251347313718519 ) ) ;
#8951 = CIRCLE ( 'NONE', #44907, 10.39117206796836079 ) ;
#8952 = CARTESIAN_POINT ( 'NONE',  ( -4.458734124999999437, -101.6458333319677365, -2.574251347313719407 ) ) ;
#8953 = CARTESIAN_POINT ( 'NONE',  ( 4.458734124999999437, -143.7500000013655779, 1.846868145590737864 ) ) ;
#8954 = CARTESIAN_POINT ( 'NONE',  ( 2.229367062500001939, -26.22916666530106866, 3.861377020970579999 ) ) ;
#8955 = AXIS2_PLACEMENT_3D ( 'NONE', #57466, #61340, #28169 ) ;
#8956 = DIRECTION ( 'NONE',  ( 0.000000000000000000, 0.000000000000000000, 1.000000000000000000 ) ) ;
#8957 = CARTESIAN_POINT ( 'NONE',  ( -59.29741812935640155, -131.6250000013655779, -2.196230717870135685 ) ) ;
#8958 = CARTESIAN_POINT ( 'NONE',  ( -4.458734124999999437, -66.64583333196773651, -2.574251347313719407 ) ) ;
#8959 = CARTESIAN_POINT ( 'NONE',  ( -5.000000000000000000, -16.08333333333333215, -2.886751345948128211 ) ) ;
#8960 = CARTESIAN_POINT ( 'NONE',  ( -1.339745962155613812, -34.20534180126147561, -5.000000000000000000 ) ) ;
#8961 = CARTESIAN_POINT ( 'NONE',  ( 3.152801135295366208, -141.5625000013655779, 3.152801135295367985 ) ) ;
#8962 = CARTESIAN_POINT ( 'NONE',  ( 2.229367062500001939, 3.770833334698926009, 3.861377020970579999 ) ) ;
#8963 = VERTEX_POINT ( 'NONE', #26530 ) ;
#8964 = DIRECTION ( 'NONE',  ( 1.000000000000000000, 0.000000000000000000, 0.000000000000000000 ) ) ;
#8965 = CARTESIAN_POINT ( 'NONE',  ( 1.339745962155641346, 9.705341801261479162, -4.999999999999983125 ) ) ;
#8967 = CARTESIAN_POINT ( 'NONE',  ( 2.229367062500001939, -30.97916666530107221, 3.861377020970579999 ) ) ;
#8966 = CARTESIAN_POINT ( 'NONE',  ( -2.499999999999996447, -93.83333333333332860, 4.330127018922195425 ) ) ;
#8968 = CARTESIAN_POINT ( 'NONE',  ( 1.339745962155615144, -14.58034179853029322, 4.999999999999999112 ) ) ;
#8969 = CARTESIAN_POINT ( 'NONE',  ( 2.229367062500001939, -76.22916666530106511, 3.861377020970579999 ) ) ;
#8970 = CARTESIAN_POINT ( 'NONE',  ( -4.458734124999997661, 21.52083333469893134, 2.574251347313722516 ) ) ;
#8971 = DIRECTION ( 'NONE',  ( -0.000000000000000000, 1.000000000000000000, -0.000000000000000000 ) ) ;
#8972 =( BOUNDED_CURVE ( )  B_SPLINE_CURVE ( 2, ( #55977, #31507, #21878, #20922, #41473, #51153, #21236, #16090, #40214 ),
 .UNSPECIFIED., .F., .F. ) 
 B_SPLINE_CURVE_WITH_KNOTS ( ( 3, 2, 2, 2, 3 ),
 ( 0.2979166666666666630, 0.2986111111111111049, 0.2999999999999999889, 0.3013888888888888729, 0.3020833333333333148 ),
 .UNSPECIFIED. ) 
 CURVE ( )  GEOMETRIC_REPRESENTATION_ITEM ( )  RATIONAL_B_SPLINE_CURVE ( ( 0.9330127018922194093, 0.9330127018922194093, 1.000000000000000000, 0.8660254037844387076, 1.000000000000000000, 0.8660254037844387076, 1.000000000000000000, 0.9330127018922194093, 0.9330127018922194093 ) ) 
 REPRESENTATION_ITEM ( '' )  );
#8973 = CARTESIAN_POINT ( 'NONE',  ( -51.60603307380591787, -142.9375000013656063, -2.891590998281053704 ) ) ;
#8974 = CARTESIAN_POINT ( 'NONE',  ( 4.458734125000000326, 5.104166668032261711, 2.574251347313718519 ) ) ;
#8975 = CARTESIAN_POINT ( 'NONE',  ( 4.458734124999999437, 28.93750000136559208, -5.460374474430324690E-16 ) ) ;
#8976 = CARTESIAN_POINT ( 'NONE',  ( -4.458734124999997661, -43.47916666530106511, 2.574251347313722516 ) ) ;
#8977 = CARTESIAN_POINT ( 'NONE',  ( -2.499999999999996447, -3.708333330602147537, 4.330127018922195425 ) ) ;
#8978 = CARTESIAN_POINT ( 'NONE',  ( -2.229367062499996610, -0.1458333319677394824, 3.861377020970582219 ) ) ;
#8979 = CARTESIAN_POINT ( 'NONE',  ( -2.229367062500000163, -26.72916666530106866, -3.861377020970580443 ) ) ;
#8980 = CARTESIAN_POINT ( 'NONE',  ( -1.846868145590734756, -156.1250000013655779, -4.458734125000000326 ) ) ;
#8981 = CARTESIAN_POINT ( 'NONE',  ( 2.229367062500001939, -70.97916666530107932, 3.861377020970579999 ) ) ;
#8982 = CARTESIAN_POINT ( 'NONE',  ( -3.535250795749689387E-16, -102.1249999972688158, -5.773502691896257311 ) ) ;
#8983 =( BOUNDED_CURVE ( )  B_SPLINE_CURVE ( 2, ( #48659, #38082, #23293, #9118, #28106, #28726, #58954, #58013, #43830 ),
 .UNSPECIFIED., .F., .F. ) 
 B_SPLINE_CURVE_WITH_KNOTS ( ( 3, 2, 2, 2, 3 ),
 ( 0.4187500000000000111, 0.4194444444444444531, 0.4208333333333333370, 0.4222222222222222210, 0.4229166666666666630 ),
 .UNSPECIFIED. ) 
 CURVE ( )  GEOMETRIC_REPRESENTATION_ITEM ( )  RATIONAL_B_SPLINE_CURVE ( ( 0.9330127018922194093, 0.9330127018922194093, 1.000000000000000000, 0.8660254037844387076, 1.000000000000000000, 0.8660254037844387076, 1.000000000000000000, 0.9330127018922194093, 0.9330127018922194093 ) ) 
 REPRESENTATION_ITEM ( '' )  );
#8984 = CARTESIAN_POINT ( 'NONE',  ( -3.152548672688508926E-16, 29.43750000136559564, -5.148502694627439702 ) ) ;
#8985 = CARTESIAN_POINT ( 'NONE',  ( -4.999999999999998224, -63.91666666666666430, 2.886751345948131764 ) ) ;
#8986 = CARTESIAN_POINT ( 'NONE',  ( -4.458734124999997661, -104.4791666653010651, 2.574251347313722516 ) ) ;
#8987 = CARTESIAN_POINT ( 'NONE',  ( -4.458734124999999437, -75.56249999863440792, 0.000000000000000000 ) ) ;
#8988 = CARTESIAN_POINT ( 'NONE',  ( 5.000000000000000000, -53.49999999999999289, -6.123233995736766282E-16 ) ) ;
#8989 = CARTESIAN_POINT ( 'NONE',  ( -6.972266317189433020E-16, -73.25000000000000000, -5.000000000000000000 ) ) ;
#8990 = CARTESIAN_POINT ( 'NONE',  ( -4.999999999999999112, 27.20833333606451987, 2.886751345948131764 ) ) ;
#8991 = VERTEX_POINT ( 'NONE', #46151 ) ;
#8992 = FACE_OUTER_BOUND ( 'NONE', #46904, .T. ) ;
#8993 = CARTESIAN_POINT ( 'NONE',  ( 2.500000000000002220, -6.541666663935481019, 4.330127018922192761 ) ) ;
#8994 = CARTESIAN_POINT ( 'NONE',  ( -4.999999999999999112, -10.91666666666666607, 2.886751345948131764 ) ) ;
#8995 = CARTESIAN_POINT ( 'NONE',  ( -4.458734124999999437, -19.39583333196774007, -2.574251347313719407 ) ) ;
#8996 = ADVANCED_FACE ( 'NONE', ( #21714 ), #41307, .T. ) ;
#8997 = CARTESIAN_POINT ( 'NONE',  ( 9.457646018065525792E-16, -76.06249999863440792, 5.148502694627439702 ) ) ;
#8998 = AXIS2_PLACEMENT_3D ( 'NONE', #63163, #44793, #44150 ) ;
#8999 = CARTESIAN_POINT ( 'NONE',  ( -1.846868145590737420, -167.0000000013655779, 4.458734124999999437 ) ) ;
#9000 = CARTESIAN_POINT ( 'NONE',  ( 1.060575238724906964E-15, -20.62499999726880873, 5.773502691896257311 ) ) ;
#9002 = ORIENTED_EDGE ( 'NONE', *, *, #29089, .T. ) ;
#9001 = CARTESIAN_POINT ( 'NONE',  ( 4.458734124999999437, -45.81249999863440081, -5.460374474430324690E-16 ) ) ;
#9003 = CARTESIAN_POINT ( 'NONE',  ( -51.75738570946856498, -155.0000000000000284, 3.805975901505577408 ) ) ;
#9005 = ORIENTED_EDGE ( 'NONE', *, *, #23458, .T. ) ;
#9004 = CARTESIAN_POINT ( 'NONE',  ( 9.457646018065525792E-16, 6.687500001365594748, 5.148502694627439702 ) ) ;
#9006 = CARTESIAN_POINT ( 'NONE',  ( -57.89159099828107458, -153.6875000013656063, -3.393966926194107447 ) ) ;
#9007 = CARTESIAN_POINT ( 'NONE',  ( -2.500000000000000444, -60.16666666666665719, -4.330127018922193649 ) ) ;
#9008 = CARTESIAN_POINT ( 'NONE',  ( 3.152801135295367541, -157.5625000013656063, -3.152801135295367541 ) ) ;
#9009 = CARTESIAN_POINT ( 'NONE',  ( 2.229367062500001939, -42.22916666530107932, 3.861377020970579999 ) ) ;
#9010 = CARTESIAN_POINT ( 'NONE',  ( -5.000000000000000000, -56.08333333333332860, -2.886751345948128211 ) ) ;
#9011 = CARTESIAN_POINT ( 'NONE',  ( -3.535533905932738641, -164.3750000000000284, 3.535533905932737309 ) ) ;
#9012 = ADVANCED_FACE ( 'NONE', ( #18457 ), #31985, .T. ) ;
#9013 = LINE ( 'NONE', #53388, #4586 ) ;
#9014 = CARTESIAN_POINT ( 'NONE',  ( -55.35523342533222291, -131.5625000013656063, 4.444560631937231499 ) ) ;
#9015 = CARTESIAN_POINT ( 'NONE',  ( 2.229367062500001939, -7.229166665301073103, 3.861377020970579999 ) ) ;
#9016 = CARTESIAN_POINT ( 'NONE',  ( 4.458734125000001214, -39.14583333196773651, 2.574251347313718519 ) ) ;
#9017 = CARTESIAN_POINT ( 'NONE',  ( -6.972266317189433020E-16, -25.12499999726881228, -5.000000000000000000 ) ) ;
#9018 = CARTESIAN_POINT ( 'NONE',  ( 4.458734124999999437, -147.5000000013656063, 1.846868145590737864 ) ) ;
#9019 = ADVANCED_FACE ( 'NONE', ( #52243 ), #28103, .T. ) ;
#9020 = CARTESIAN_POINT ( 'NONE',  ( 4.458734125000001214, -86.14583333196775072, 2.574251347313718519 ) ) ;
#9021 = CARTESIAN_POINT ( 'NONE',  ( -4.458734124999999437, 29.43750000136559208, 0.000000000000000000 ) ) ;
#9022 = ORIENTED_EDGE ( 'NONE', *, *, #59246, .T. ) ;
#9023 = CARTESIAN_POINT ( 'NONE',  ( 1.975475456537005874E-15, -99.74999999999998579, 5.000000000000000000 ) ) ;
#9024 = CARTESIAN_POINT ( 'NONE',  ( -55.39835681537999790, -151.0000000027312410, 4.984105922594378235 ) ) ;
#9025 = CARTESIAN_POINT ( 'NONE',  ( -7.897850199329715437, 1.533397866934075759, -7.634054012537968781 ) ) ;
#9026 = CARTESIAN_POINT ( 'NONE',  ( -4.458734124999998549, -77.47916666530106511, 2.574251347313722516 ) ) ;
#9027 = EDGE_LOOP ( 'NONE', ( #40370, #50237, #29498, #4465 ) ) ;
#9028 = FACE_OUTER_BOUND ( 'NONE', #28391, .T. ) ;
#9029 = CARTESIAN_POINT ( 'NONE',  ( 2.229367062499998831, -10.89583333196773829, -3.861377020970580887 ) ) ;
#9030 = CARTESIAN_POINT ( 'NONE',  ( 1.339745962155615144, -79.58034179853028434, 4.999999999999999112 ) ) ;
#9031 = CARTESIAN_POINT ( 'NONE',  ( 4.458734124999999437, 3.187500001365594304, -5.460374474430324690E-16 ) ) ;
#9032 = DIRECTION ( 'NONE',  ( 0.000000000000000000, 0.000000000000000000, 1.000000000000000000 ) ) ;
#9033 = CARTESIAN_POINT ( 'NONE',  ( 3.152801135295367541, -152.3125000013655779, -3.152801135295367541 ) ) ;
#9034 =( BOUNDED_CURVE ( )  B_SPLINE_CURVE ( 2, ( #11722, #16246, #45828, #40996, #60640, #2112, #31339, #5961, #6919 ),
 .UNSPECIFIED., .F., .F. ) 
 B_SPLINE_CURVE_WITH_KNOTS ( ( 3, 2, 2, 2, 3 ),
 ( 0.04166666666666670599, 0.04583333333333337173, 0.05000000000000004441, 0.05416666666666671709, 0.05833333333333338283 ),
 .UNSPECIFIED. ) 
 CURVE ( )  GEOMETRIC_REPRESENTATION_ITEM ( )  RATIONAL_B_SPLINE_CURVE ( ( 0.9999999999999992228, 0.9238795325112875156, 1.000000000000000000, 0.9238795325112867385, 1.000000000000000000, 0.9238795325112867385, 1.000000000000000000, 0.9238795325112858503, 1.000000000000000888 ) ) 
 REPRESENTATION_ITEM ( '' )  );
#9035 = CARTESIAN_POINT ( 'NONE',  ( -4.458734124999999437, 22.43750000136559564, 0.000000000000000000 ) ) ;
#9036 = VERTEX_POINT ( 'NONE', #57079 ) ;
#9037 = CARTESIAN_POINT ( 'NONE',  ( -2.229367062500000163, -92.47916666530106511, -3.861377020970580443 ) ) ;
#9038 = CARTESIAN_POINT ( 'NONE',  ( 6.123233995736766282E-16, -170.0000000000000000, -5.000000000000000000 ) ) ;
#9039 = CARTESIAN_POINT ( 'NONE',  ( 0.000000000000000000, -120.0000000000000000, 5.000000000000000000 ) ) ;
#9040 = CARTESIAN_POINT ( 'NONE',  ( 4.458734124999999437, -15.81249999863440436, -5.460374474430324690E-16 ) ) ;
#9041 = VECTOR ( 'NONE', #59064, 1000.000000000000000 ) ;
#9042 = CARTESIAN_POINT ( 'NONE',  ( 0.000000000000000000, -170.0000000000000000, 5.000000000000000000 ) ) ;
#9043 = FACE_OUTER_BOUND ( 'NONE', #19641, .T. ) ;
#9044 = DIRECTION ( 'NONE',  ( -0.000000000000000000, 1.000000000000000000, -0.000000000000000000 ) ) ;
#9045 = ADVANCED_FACE ( 'NONE', ( #32937 ), #41618, .T. ) ;
#9046 = CARTESIAN_POINT ( 'NONE',  ( 1.060575238724906964E-15, -36.62499999726880873, 5.773502691896257311 ) ) ;
#9047 = CARTESIAN_POINT ( 'NONE',  ( 2.499999999999998668, -49.20833333060213732, -4.330127018922193649 ) ) ;
#9048 = CARTESIAN_POINT ( 'NONE',  ( 4.458734125000000326, 21.10416666803226704, 2.574251347313718519 ) ) ;
#9049 = CARTESIAN_POINT ( 'NONE',  ( 4.458734124999998549, 20.27083333469892779, -2.574251347313721627 ) ) ;
#9050 = CARTESIAN_POINT ( 'NONE',  ( 4.458734124999999437, -56.81249999863440081, -5.460374474430324690E-16 ) ) ;
#9051 = CARTESIAN_POINT ( 'NONE',  ( -4.458734124999999437, -11.56249999863440792, 0.000000000000000000 ) ) ;
#9052 = DIRECTION ( 'NONE',  ( -0.000000000000000000, 1.000000000000000000, -0.000000000000000000 ) ) ;
#9053 = CARTESIAN_POINT ( 'NONE',  ( -5.000000000000000000, 9.999999999999998224, 0.000000000000000000 ) ) ;
#9054 = CARTESIAN_POINT ( 'NONE',  ( -4.458734125000000326, -168.0000000013655779, -1.846868145590735644 ) ) ;
#9055 = CARTESIAN_POINT ( 'NONE',  ( 4.458734125000001214, -55.89583333196773651, 2.574251347313718519 ) ) ;
#9056 = CARTESIAN_POINT ( 'NONE',  ( -5.000000000000000000, -81.87499999726881583, 0.000000000000000000 ) ) ;
#9057 = VECTOR ( 'NONE', #51541, 1000.000000000000000 ) ;
#9058 = CARTESIAN_POINT ( 'NONE',  ( -50.55543936806279248, -134.3125000013656063, 0.3552334253322060320 ) ) ;
#9059 = CARTESIAN_POINT ( 'NONE',  ( -58.24261429053147765, -140.3750000027312126, -3.805975901505573855 ) ) ;
#9060 = CARTESIAN_POINT ( 'NONE',  ( -4.999999999999998224, -104.7916666639354730, 2.886751345948131764 ) ) ;
#9061 = CARTESIAN_POINT ( 'NONE',  ( -4.458734124999999437, -90.64583333196773651, -2.574251347313719407 ) ) ;
#9062 = CARTESIAN_POINT ( 'NONE',  ( -4.458734124999999437, -159.2500000013656063, -1.846868145590735644 ) ) ;
#9063 = CARTESIAN_POINT ( 'NONE',  ( -5.000000000000000000, -36.08333333333332860, -2.886751345948128211 ) ) ;
#9064 = CARTESIAN_POINT ( 'NONE',  ( 1.243387493232115550E-13, -20.12499999726881228, -5.000000000000000000 ) ) ;
#9065 = CARTESIAN_POINT ( 'NONE',  ( -57.78304654714001742, -135.0000000000000853, -3.610108303323515511 ) ) ;
#9066 = VERTEX_POINT ( 'NONE', #13316 ) ;
#9067 = CARTESIAN_POINT ( 'NONE',  ( 2.229367062500001939, -96.97916666530105090, 3.861377020970579999 ) ) ;
#9068 = CARTESIAN_POINT ( 'NONE',  ( -2.229367062500000163, 7.270833334698929562, -3.861377020970580443 ) ) ;
#9069 = CARTESIAN_POINT ( 'NONE',  ( -2.499999999999996447, 11.29166666939785202, 4.330127018922195425 ) ) ;
#9070 = DIRECTION ( 'NONE',  ( -0.000000000000000000, 1.000000000000000000, -0.000000000000000000 ) ) ;
#9071 = CARTESIAN_POINT ( 'NONE',  ( 5.000000000000000888, 2.416666666666667851, 2.886751345948126879 ) ) ;
#9072 = CARTESIAN_POINT ( 'NONE',  ( -4.458734124999999437, -59.39583333196773651, -2.574251347313719407 ) ) ;
#9073 = CARTESIAN_POINT ( 'NONE',  ( -2.499999999999996447, 3.166666666666664742, 4.330127018922195425 ) ) ;
#9074 = EDGE_CURVE ( 'NONE', #44817, #43815, #20115, .T. ) ;
#9075 = EDGE_CURVE ( 'NONE', #21118, #47300, #62218, .T. ) ;
#9076 = CARTESIAN_POINT ( 'NONE',  ( 2.500000000000002220, -0.5416666639354792423, 4.330127018922192761 ) ) ;
#9077 = CARTESIAN_POINT ( 'NONE',  ( 4.458734124999998549, -30.72916666530107221, -2.574251347313721627 ) ) ;
#9078 = CARTESIAN_POINT ( 'NONE',  ( -59.98410592259440222, -144.2500000027312126, -0.3983568153799752487 ) ) ;
#9079 = CARTESIAN_POINT ( 'NONE',  ( -6.972266317189433020E-16, -23.12499999726880873, -5.000000000000000000 ) ) ;
#9080 = CARTESIAN_POINT ( 'NONE',  ( -9.184850993605147944E-16, -151.2500000000000284, 5.000000000000000000 ) ) ;
#9081 = CARTESIAN_POINT ( 'NONE',  ( -2.499999999999996447, -46.83333333333333570, 4.330127018922195425 ) ) ;
#9083 = CARTESIAN_POINT ( 'NONE',  ( -4.458734124999998549, -25.47916666530106866, 2.574251347313722516 ) ) ;
#9082 = CARTESIAN_POINT ( 'NONE',  ( 1.975475456537005874E-15, -39.62499999726880162, 5.000000000000000000 ) ) ;
#9084 = CARTESIAN_POINT ( 'NONE',  ( 1.339745962155612702, -64.29465819873851729, -5.000000000000000000 ) ) ;
#9085 = CARTESIAN_POINT ( 'NONE',  ( -4.458734124999998549, -69.22916666530107932, 2.574251347313722516 ) ) ;
#9086 =( BOUNDED_CURVE ( )  B_SPLINE_CURVE ( 2, ( #54040, #345, #43126, #62766, #57940, #13858, #33482, #53103, #43439 ),
 .UNSPECIFIED., .F., .F. ) 
 B_SPLINE_CURVE_WITH_KNOTS ( ( 3, 2, 2, 2, 3 ),
 ( 0.5517857142857143238, 0.5523809523809524169, 0.5535714285714286031, 0.5547619047619047894, 0.5553571428571428825 ),
 .UNSPECIFIED. ) 
 CURVE ( )  GEOMETRIC_REPRESENTATION_ITEM ( )  RATIONAL_B_SPLINE_CURVE ( ( 0.9330127018922194093, 0.9330127018922194093, 1.000000000000000000, 0.8660254037844387076, 1.000000000000000000, 0.8660254037844387076, 1.000000000000000000, 0.9330127018922194093, 0.9330127018922194093 ) ) 
 REPRESENTATION_ITEM ( '' )  );
#9087 = CARTESIAN_POINT ( 'NONE',  ( 3.152801135295366208, -148.8125000013655779, 3.152801135295367985 ) ) ;
#9088 = CARTESIAN_POINT ( 'NONE',  ( 9.457646018065525792E-16, -78.06249999863440792, 5.148502694627439702 ) ) ;
#9089 = VECTOR ( 'NONE', #16697, 1000.000000000000000 ) ;
#9090 = CARTESIAN_POINT ( 'NONE',  ( -52.80376928212989185, -143.1250000013656063, -4.297418129356379346 ) ) ;
#9091 = EDGE_CURVE ( 'NONE', #3482, #31783, #47187, .T. ) ;
#9092 = CARTESIAN_POINT ( 'NONE',  ( 2.229367062499998831, -22.89583333196773651, -3.861377020970580887 ) ) ;
#9093 = CARTESIAN_POINT ( 'NONE',  ( 5.000000000000000000, -66.29166666393547303, -2.886751345948129988 ) ) ;
#9094 = ORIENTED_EDGE ( 'NONE', *, *, #31450, .T. ) ;
#9095 = CARTESIAN_POINT ( 'NONE',  ( 4.769696007084728073, -120.0000000000000000, -1.500000000000000444 ) ) ;
#9097 = EDGE_LOOP ( 'NONE', ( #37180, #52059, #27354, #36577 ) ) ;
#9096 = EDGE_CURVE ( 'NONE', #49104, #1040, #9773, .T. ) ;
#9098 = CARTESIAN_POINT ( 'NONE',  ( 9.457646018065525792E-16, -69.31249999863440792, 5.148502694627439702 ) ) ;
#9099 = ORIENTED_EDGE ( 'NONE', *, *, #29978, .T. ) ;
#9100 = EDGE_CURVE ( 'NONE', #6898, #3623, #16382, .T. ) ;
#9101 = LINE ( 'NONE', #43812, #21965 ) ;
#9102 = CARTESIAN_POINT ( 'NONE',  ( 9.457646018065525792E-16, -60.31249999863440792, 5.148502694627439702 ) ) ;
#9103 = CARTESIAN_POINT ( 'NONE',  ( -2.229367062500000163, -0.7291666653010709931, -3.861377020970580443 ) ) ;
#9104 = EDGE_LOOP ( 'NONE', ( #3981, #60628, #887, #6580 ) ) ;
#9105 = VECTOR ( 'NONE', #26533, 1000.000000000000000 ) ;
#9106 = CARTESIAN_POINT ( 'NONE',  ( 0.000000000000000000, -170.0000000000000000, 0.000000000000000000 ) ) ;
#9107 = CARTESIAN_POINT ( 'NONE',  ( 9.457646018065525792E-16, 20.93750000136558853, 5.148502694627439702 ) ) ;
#9108 = CARTESIAN_POINT ( 'NONE',  ( -58.39396692619412477, -146.4375000013656063, 2.891590998281057701 ) ) ;
#9109 = CARTESIAN_POINT ( 'NONE',  ( 5.000000000000000000, 20.62500000273118772, -6.123233995736766282E-16 ) ) ;
#9110 = CARTESIAN_POINT ( 'NONE',  ( 3.152801135295366208, -166.5625000013656063, 3.152801135295367985 ) ) ;
#9111 = ORIENTED_EDGE ( 'NONE', *, *, #53943, .F. ) ;
#9112 = CARTESIAN_POINT ( 'NONE',  ( 2.229367062499998831, -76.64583333196773651, -3.861377020970580887 ) ) ;
#9113 = CARTESIAN_POINT ( 'NONE',  ( 1.975475456537005874E-15, -39.75000000000000000, 5.000000000000000000 ) ) ;
#9114 = CARTESIAN_POINT ( 'NONE',  ( -2.229367062500000163, 6.520833334698928674, -3.861377020970580443 ) ) ;
#9115 = CARTESIAN_POINT ( 'NONE',  ( 2.499999999999998668, -40.20833333060214443, -4.330127018922193649 ) ) ;
#9116 = CARTESIAN_POINT ( 'NONE',  ( 4.458734124999998549, -59.97916666530107221, -2.574251347313721627 ) ) ;
#9117 = CARTESIAN_POINT ( 'NONE',  ( -5.000000000000000000, -20.95833333060214798, -2.886751345948128211 ) ) ;
#9118 = CARTESIAN_POINT ( 'NONE',  ( 5.000000000000000000, -20.41666666666666785, -2.886751345948130876 ) ) ;
#9119 = CARTESIAN_POINT ( 'NONE',  ( 5.000000000000000000, -44.37499999726880873, -6.123233995736766282E-16 ) ) ;
#9120 = CARTESIAN_POINT ( 'NONE',  ( 1.339745962155612702, -49.29465819873851018, -5.000000000000000000 ) ) ;
#9121 = CARTESIAN_POINT ( 'NONE',  ( 1.339745962155565406, -18.58034179853029855, 5.000000000000028422 ) ) ;
#9122 = CARTESIAN_POINT ( 'NONE',  ( -2.071067811865372921, -159.3125000000000000, 5.000000000000104805 ) ) ;
#9123 = CARTESIAN_POINT ( 'NONE',  ( -4.458734124999999437, -42.39583333196773651, -2.574251347313719407 ) ) ;
#9124 = CARTESIAN_POINT ( 'NONE',  ( 9.457646018065525792E-16, -29.31249999863440436, 5.148502694627439702 ) ) ;
#9125 = VECTOR ( 'NONE', #41654, 1000.000000000000000 ) ;
#9126 = CARTESIAN_POINT ( 'NONE',  ( 1.339745962155615144, 11.29465819873851906, 4.999999999999999112 ) ) ;
#9127 = CARTESIAN_POINT ( 'NONE',  ( 5.000000000000000000, 23.58333333333333215, -2.886751345948129988 ) ) ;
#9128 = CARTESIAN_POINT ( 'NONE',  ( -2.071067811865478170, -149.4375000027312410, 5.000000000000000000 ) ) ;
#9129 = CARTESIAN_POINT ( 'NONE',  ( -2.229367062499996610, -107.3958333319677365, 3.861377020970582219 ) ) ;
#9130 = AXIS2_PLACEMENT_3D ( 'NONE', #15902, #21368, #26510 ) ;
#9131 = CARTESIAN_POINT ( 'NONE',  ( -3.152548672688508926E-16, -30.56249999863440436, -5.148502694627439702 ) ) ;
#9132 = CARTESIAN_POINT ( 'NONE',  ( 2.499999999999998668, -69.20833333060214443, -4.330127018922193649 ) ) ;
#9133 = CARTESIAN_POINT ( 'NONE',  ( -58.39396692619412477, -149.6875000013656063, 2.891590998281057701 ) ) ;
#9134 = CARTESIAN_POINT ( 'NONE',  ( -5.000000000000000888, -142.4375000000000000, 2.071067811865474617 ) ) ;
#9135 = CARTESIAN_POINT ( 'NONE',  ( -2.229367062500000163, -73.72916666530106511, -3.861377020970580443 ) ) ;
#9136 = CARTESIAN_POINT ( 'NONE',  ( -4.458734124999999437, -168.2500000013656063, -1.846868145590735644 ) ) ;
#9137 = CARTESIAN_POINT ( 'NONE',  ( 9.457646018065525792E-16, -29.06249999863440436, 5.148502694627439702 ) ) ;
#9138 = DIRECTION ( 'NONE',  ( -0.000000000000000000, 1.000000000000000000, -0.000000000000000000 ) ) ;
#9139 = CYLINDRICAL_SURFACE ( 'NONE', #14309, 5.000000000000000000 ) ;
#9140 = CARTESIAN_POINT ( 'NONE',  ( 1.060575238724906964E-15, -24.75000000000000355, 5.773502691896257311 ) ) ;
#9141 = CARTESIAN_POINT ( 'NONE',  ( -4.458734125000000326, -148.0000000013655779, -1.846868145590735644 ) ) ;
#9142 = ORIENTED_EDGE ( 'NONE', *, *, #25492, .F. ) ;
#9143 = CARTESIAN_POINT ( 'NONE',  ( -2.500000000000000444, -90.04166666393547303, -4.330127018922193649 ) ) ;
#9144 = CARTESIAN_POINT ( 'NONE',  ( -1.339745962155613812, -49.20534180126148271, -5.000000000000000000 ) ) ;
#9145 = CARTESIAN_POINT ( 'NONE',  ( 4.458734124999999437, -58.06249999863440081, -5.460374474430324690E-16 ) ) ;
#9146 = CARTESIAN_POINT ( 'NONE',  ( 5.000000000000000888, 24.54166666939784847, 2.886751345948126879 ) ) ;
#9147 = CARTESIAN_POINT ( 'NONE',  ( 5.000000000000000888, -48.45833333060215153, 2.886751345948126879 ) ) ;
#9148 = CARTESIAN_POINT ( 'NONE',  ( 2.500000000000002220, 20.33333333333333215, 4.330127018922192761 ) ) ;
#9149 = DIRECTION ( 'NONE',  ( 0.000000000000000000, 0.000000000000000000, 1.000000000000000000 ) ) ;
#9150 = CARTESIAN_POINT ( 'NONE',  ( 4.458734124999999437, -6.812499998634404363, -5.460374474430324690E-16 ) ) ;
#9151 = CARTESIAN_POINT ( 'NONE',  ( -2.071067811865308972, -154.3125000000000000, 5.000000000000169642 ) ) ;
#9152 = EDGE_CURVE ( 'NONE', #59111, #38517, #22025, .T. ) ;
#9153 = CARTESIAN_POINT ( 'NONE',  ( 2.229367062500001939, 8.770833334698927786, 3.861377020970579999 ) ) ;
#9154 = LINE ( 'NONE', #13669, #37696 ) ;
#9155 = ORIENTED_EDGE ( 'NONE', *, *, #14240, .F. ) ;
#9156 = DIRECTION ( 'NONE',  ( 0.000000000000000000, 1.000000000000000000, 0.000000000000000000 ) ) ;
#9157 = CARTESIAN_POINT ( 'NONE',  ( 4.458734124999999437, -56.81249999863440081, -5.460374474430324690E-16 ) ) ;
#9158 = CARTESIAN_POINT ( 'NONE',  ( 1.846868145590736310, -160.8750000013655779, 4.458734124999999437 ) ) ;
#9159 =( BOUNDED_CURVE ( )  B_SPLINE_CURVE ( 2, ( #41074, #36574, #7325, #32061, #35951, #7003, #25976, #12128, #46552 ),
 .UNSPECIFIED., .F., .F. ) 
 B_SPLINE_CURVE_WITH_KNOTS ( ( 3, 2, 2, 2, 3 ),
 ( 0.1696428571428571508, 0.1702380952380952439, 0.1714285714285714302, 0.1726190476190476164, 0.1732142857142857095 ),
 .UNSPECIFIED. ) 
 CURVE ( )  GEOMETRIC_REPRESENTATION_ITEM ( )  RATIONAL_B_SPLINE_CURVE ( ( 0.9330127018922194093, 0.9330127018922194093, 1.000000000000000000, 0.8660254037844387076, 1.000000000000000000, 0.8660254037844387076, 1.000000000000000000, 0.9330127018922194093, 0.9330127018922194093 ) ) 
 REPRESENTATION_ITEM ( '' )  );
#9160 = CARTESIAN_POINT ( 'NONE',  ( -4.999999999999999112, -52.79166666393547303, 2.886751345948131764 ) ) ;
#9161 = EDGE_LOOP ( 'NONE', ( #6803, #44772, #40941, #25872 ) ) ;
#9162 = CARTESIAN_POINT ( 'NONE',  ( -2.229367062500000163, 6.270833334698928674, -3.861377020970580443 ) ) ;
#9163 = ORIENTED_EDGE ( 'NONE', *, *, #62993, .F. ) ;
#9165 = CARTESIAN_POINT ( 'NONE',  ( -5.000000000000000000, -102.9583333306021586, -2.886751345948128211 ) ) ;
#9164 = CARTESIAN_POINT ( 'NONE',  ( -6.972266317189433020E-16, 13.74999999999999822, -5.000000000000000000 ) ) ;
#9166 = CARTESIAN_POINT ( 'NONE',  ( -3.152801135295367985, -160.8125000013656063, 3.152801135295367096 ) ) ;
#9167 = EDGE_CURVE ( 'NONE', #9668, #19705, #12371, .T. ) ;
#9168 = EDGE_LOOP ( 'NONE', ( #46129, #6031, #52218, #5845 ) ) ;
#9169 =( GEOMETRIC_REPRESENTATION_CONTEXT ( 3 ) GLOBAL_UNCERTAINTY_ASSIGNED_CONTEXT ( ( #63524 ) ) GLOBAL_UNIT_ASSIGNED_CONTEXT ( ( #59255, #44448, #54100 ) ) REPRESENTATION_CONTEXT ( 'NONE', 'WORKASPACE' ) );
#9170 = EDGE_CURVE ( 'NONE', #60689, #13643, #29490, .T. ) ;
#9171 = CARTESIAN_POINT ( 'NONE',  ( 2.499999999999998668, -87.20833333060214443, -4.330127018922193649 ) ) ;
#9172 = CARTESIAN_POINT ( 'NONE',  ( -52.53715891517739323, -132.4375000000000284, -4.819101127000233298 ) ) ;
#9174 = CIRCLE ( 'NONE', #6116, 5.000000000000000000 ) ;
#9173 = CARTESIAN_POINT ( 'NONE',  ( -6.972266317189433020E-16, -82.24999999999998579, -5.000000000000000000 ) ) ;
#9175 = CARTESIAN_POINT ( 'NONE',  ( 4.458734124999998549, -36.97916666530107221, -2.574251347313721627 ) ) ;
#9176 = EDGE_LOOP ( 'NONE', ( #2541, #52857, #17906, #7268 ) ) ;
#9177 = EDGE_CURVE ( 'NONE', #62942, #37665, #36098, .T. ) ;
#9178 = CARTESIAN_POINT ( 'NONE',  ( -2.229367062499996610, -80.14583333196773651, 3.861377020970582219 ) ) ;
#9179 = CARTESIAN_POINT ( 'NONE',  ( 4.458734125000001214, 21.10416666803226349, 2.574251347313718519 ) ) ;
#9180 = CARTESIAN_POINT ( 'NONE',  ( -2.071067811865602071, -156.8125000027311842, -4.999999999999874767 ) ) ;
#9181 = ORIENTED_EDGE ( 'NONE', *, *, #21310, .T. ) ;
#9182 = CARTESIAN_POINT ( 'NONE',  ( -4.458734124999998549, -83.47916666530107932, 2.574251347313722516 ) ) ;
#9183 = CARTESIAN_POINT ( 'NONE',  ( -55.39835681537999790, -125.0000000027311984, 4.984105922594378235 ) ) ;
#9184 = CARTESIAN_POINT ( 'NONE',  ( -4.999999999999998224, 25.20833333606451987, 2.886751345948131764 ) ) ;
#9185 = CARTESIAN_POINT ( 'NONE',  ( -50.46537964183328029, -135.0000000000000284, 0.7220904342385146002 ) ) ;
#9186 = CARTESIAN_POINT ( 'NONE',  ( -6.972266317189433020E-16, -13.12499999726881050, -5.000000000000000000 ) ) ;
#9187 = CARTESIAN_POINT ( 'NONE',  ( -4.458734124999997661, -60.22916666530105800, 2.574251347313722516 ) ) ;
#9188 = CARTESIAN_POINT ( 'NONE',  ( 3.061616997868383141E-16, -143.8750000027312126, -5.000000000000000000 ) ) ;
#9189 = CARTESIAN_POINT ( 'NONE',  ( -2.229367062499996610, 23.85416666803225993, 3.861377020970582219 ) ) ;
#9190 = CYLINDRICAL_SURFACE ( 'NONE', #1906, 5.000000000000000000 ) ;
#9191 = CARTESIAN_POINT ( 'NONE',  ( -6.972266317189433020E-16, -40.24999999999999289, -5.000000000000000000 ) ) ;
#9192 = CARTESIAN_POINT ( 'NONE',  ( 2.229367062499998831, -44.89583333196774362, -3.861377020970580887 ) ) ;
#9193 = CARTESIAN_POINT ( 'NONE',  ( 2.499999999999998668, -3.208333330602147093, -4.330127018922193649 ) ) ;
#9194 = CARTESIAN_POINT ( 'NONE',  ( 0.000000000000000000, -170.0000000000000000, 5.000000000000000000 ) ) ;
#9195 = DIRECTION ( 'NONE',  ( -0.000000000000000000, 1.000000000000000000, -0.000000000000000000 ) ) ;
#9196 = CARTESIAN_POINT ( 'NONE',  ( 4.458734125000001214, -85.14583333196773651, 2.574251347313718519 ) ) ;
#9197 = DIRECTION ( 'NONE',  ( -0.000000000000000000, 1.000000000000000000, -0.000000000000000000 ) ) ;
#9198 = CARTESIAN_POINT ( 'NONE',  ( -3.152548672688508926E-16, -8.812499998634406140, -5.148502694627439702 ) ) ;
#9199 = ORIENTED_EDGE ( 'NONE', *, *, #40356, .T. ) ;
#9200 = CARTESIAN_POINT ( 'NONE',  ( -4.458734124999999437, 29.56250000136559208, 0.000000000000000000 ) ) ;
#9201 = CARTESIAN_POINT ( 'NONE',  ( -3.152548672688508926E-16, -96.56249999863439371, -5.148502694627439702 ) ) ;
#9202 = CARTESIAN_POINT ( 'NONE',  ( -3.535533905932737309, -166.7500000027312126, -3.535533905932738197 ) ) ;
#9203 = CARTESIAN_POINT ( 'NONE',  ( -2.229367062500000163, -90.72916666530106511, -3.861377020970580443 ) ) ;
#9204 = CARTESIAN_POINT ( 'NONE',  ( -5.000000000000000000, -51.95833333060213732, -2.886751345948128211 ) ) ;
#9205 = CARTESIAN_POINT ( 'NONE',  ( -7.500000000000000000, 4.330127018922191873, -0.9999999999999970024 ) ) ;
#9206 = CARTESIAN_POINT ( 'NONE',  ( -59.44456063193725015, -130.5625000013656063, -0.3552334253322034230 ) ) ;
#9207 = CARTESIAN_POINT ( 'NONE',  ( -51.60603307380591787, -145.9375000013656063, -2.891590998281053704 ) ) ;
#9208 = CARTESIAN_POINT ( 'NONE',  ( 4.458734124999999437, -19.81249999863440081, -5.460374474430324690E-16 ) ) ;
#9209 = CARTESIAN_POINT ( 'NONE',  ( -4.458734124999999437, 10.35416666803225816, -2.574251347313719407 ) ) ;
#9210 = CARTESIAN_POINT ( 'NONE',  ( 2.229367062499998831, -60.89583333196774362, -3.861377020970580887 ) ) ;
#9211 = CARTESIAN_POINT ( 'NONE',  ( 5.000000000000000000, -86.37499999726880162, -6.123233995736766282E-16 ) ) ;
#9212 = CARTESIAN_POINT ( 'NONE',  ( -2.229367062499996610, -12.14583333196774007, 3.861377020970582219 ) ) ;
#9213 = LINE ( 'NONE', #24316, #34113 ) ;
#9214 = ORIENTED_EDGE ( 'NONE', *, *, #4211, .T. ) ;
#9215 = CARTESIAN_POINT ( 'NONE',  ( 2.229367062499998831, -38.89583333196773651, -3.861377020970580887 ) ) ;
#9216 = CARTESIAN_POINT ( 'NONE',  ( -8.190561711645485556E-16, -154.9375000013655779, 4.458734124999999437 ) ) ;
#9217 = FACE_OUTER_BOUND ( 'NONE', #5611, .T. ) ;
#9218 = CARTESIAN_POINT ( 'NONE',  ( 1.975475456537005874E-15, -46.74999999999999289, 5.000000000000000000 ) ) ;
#9219 = CARTESIAN_POINT ( 'NONE',  ( -5.000000000000000000, -25.08333333333333215, -2.886751345948128211 ) ) ;
#9220 = CARTESIAN_POINT ( 'NONE',  ( -4.458734124999999437, -86.31249999863439371, 0.000000000000000000 ) ) ;
#9221 = CARTESIAN_POINT ( 'NONE',  ( 9.457646018065525792E-16, 20.68750000136559564, 5.148502694627439702 ) ) ;
#9223 = EDGE_CURVE ( 'NONE', #7560, #27699, #38178, .T. ) ;
#9222 = CARTESIAN_POINT ( 'NONE',  ( 4.458734124999998549, 12.27083333469892423, -2.574251347313721627 ) ) ;
#9224 = CARTESIAN_POINT ( 'NONE',  ( -5.000000000000000000, -6.999999999999999112, 0.000000000000000000 ) ) ;
#9225 = CARTESIAN_POINT ( 'NONE',  ( 4.458734124999999437, -90.06249999863440792, -5.460374474430324690E-16 ) ) ;
#9226 = CARTESIAN_POINT ( 'NONE',  ( -4.999999999999999112, -67.91666666666667140, 2.886751345948131764 ) ) ;
#9227 = CARTESIAN_POINT ( 'NONE',  ( 2.499999999999998668, 12.79166666939785379, -4.330127018922193649 ) ) ;
#9228 = ORIENTED_EDGE ( 'NONE', *, *, #63627, .F. ) ;
#9229 = FACE_OUTER_BOUND ( 'NONE', #26917, .T. ) ;
#9230 = ORIENTED_EDGE ( 'NONE', *, *, #48437, .F. ) ;
#9231 = CARTESIAN_POINT ( 'NONE',  ( 3.061616997868383141E-16, -166.7500000000000000, -5.000000000000000000 ) ) ;
#9232 =( BOUNDED_CURVE ( )  B_SPLINE_CURVE ( 2, ( #6614, #26227, #45847, #31358, #50999, #6939, #43533, #18480, #3385 ),
 .UNSPECIFIED., .F., .F. ) 
 B_SPLINE_CURVE_WITH_KNOTS ( ( 3, 2, 2, 2, 3 ),
 ( 0.5916666666666671182, 0.5958333333333335480, 0.6000000000000000888, 0.6041666666666665186, 0.6083333333333329485 ),
 .UNSPECIFIED. ) 
 CURVE ( )  GEOMETRIC_REPRESENTATION_ITEM ( )  RATIONAL_B_SPLINE_CURVE ( ( 0.9999999999999918954, 0.9238795325112948431, 1.000000000000000000, 0.9238795325112867385, 1.000000000000000000, 0.9238795325112867385, 1.000000000000000000, 0.9238795325112928447, 0.9999999999999938938 ) ) 
 REPRESENTATION_ITEM ( '' )  );
#9234 = CARTESIAN_POINT ( 'NONE',  ( 2.499999999999998668, -29.33333333333332860, -4.330127018922193649 ) ) ;
#9233 = CARTESIAN_POINT ( 'NONE',  ( 5.000000000000000888, -85.58333333333332860, 2.886751345948126879 ) ) ;
#9235 = CARTESIAN_POINT ( 'NONE',  ( 4.458734124999998549, -33.72916666530106511, -2.574251347313721627 ) ) ;
#9236 = CARTESIAN_POINT ( 'NONE',  ( -2.500000000000000444, -35.04166666393547303, -4.330127018922193649 ) ) ;
#9238 = ORIENTED_EDGE ( 'NONE', *, *, #42910, .T. ) ;
#9237 = CARTESIAN_POINT ( 'NONE',  ( -2.229367062499996610, -64.14583333196773651, 3.861377020970582219 ) ) ;
#9239 = CARTESIAN_POINT ( 'NONE',  ( -56.48576386720575471, -152.0000000013655779, -4.591703134518078322 ) ) ;
#9241 = ORIENTED_EDGE ( 'NONE', *, *, #787, .F. ) ;
#9240 = CARTESIAN_POINT ( 'NONE',  ( 2.229367062499998831, -14.89583333196773474, -3.861377020970580887 ) ) ;
#9242 = CARTESIAN_POINT ( 'NONE',  ( 2.499999999999998668, -77.33333333333334281, -4.330127018922193649 ) ) ;
#9243 = LINE ( 'NONE', #18890, #15569 ) ;
#9244 = CARTESIAN_POINT ( 'NONE',  ( -2.229367062500000163, -54.72916666530107221, -3.861377020970580443 ) ) ;
#9245 = CARTESIAN_POINT ( 'NONE',  ( -4.999999999999999112, -80.79166666393547303, 2.886751345948131764 ) ) ;
#9247 = EDGE_LOOP ( 'NONE', ( #39630, #8506, #12086, #29650 ) ) ;
#9246 = CARTESIAN_POINT ( 'NONE',  ( -1.339745962155610925, -31.79465819873851373, 5.000000000000000000 ) ) ;
#9248 = CARTESIAN_POINT ( 'NONE',  ( -51.75738570946856498, -144.7500000000000284, 3.805975901505576964 ) ) ;
#9249 = CARTESIAN_POINT ( 'NONE',  ( -3.152548672688508926E-16, -23.81249999863440792, -5.148502694627439702 ) ) ;
#9251 = ORIENTED_EDGE ( 'NONE', *, *, #57044, .T. ) ;
#9250 = CARTESIAN_POINT ( 'NONE',  ( -2.229367062500000163, -59.72916666530106511, -3.861377020970580443 ) ) ;
#9252 = CARTESIAN_POINT ( 'NONE',  ( -55.00000000000002842, 24.99999999999999645, 0.000000000000000000 ) ) ;
#9253 = CARTESIAN_POINT ( 'NONE',  ( 3.152801135295366208, -167.8125000013656063, 3.152801135295367985 ) ) ;
#9254 = CARTESIAN_POINT ( 'NONE',  ( -4.458734124999998549, -106.4791666653010651, 2.574251347313722516 ) ) ;
#9255 = CARTESIAN_POINT ( 'NONE',  ( -5.000000000000000000, -26.95833333060214798, -2.886751345948128211 ) ) ;
#9256 = ORIENTED_EDGE ( 'NONE', *, *, #24032, .T. ) ;
#9257 = CARTESIAN_POINT ( 'NONE',  ( -51.60603307380591787, -152.1875000013656063, -2.891590998281053704 ) ) ;
#9258 = CARTESIAN_POINT ( 'NONE',  ( -52.53715891517739323, -137.5625000027312126, -4.819101127000233298 ) ) ;
#9259 = CARTESIAN_POINT ( 'NONE',  ( -4.458734124999999437, -40.31249999863440081, 0.000000000000000000 ) ) ;
#9260 =( BOUNDED_CURVE ( )  B_SPLINE_CURVE ( 2, ( #31188, #51143, #46308, #26366, #2569, #17039, #50502, #55654, #2265 ),
 .UNSPECIFIED., .F., .F. ) 
 B_SPLINE_CURVE_WITH_KNOTS ( ( 3, 2, 2, 2, 3 ),
 ( 0.03750000000000000555, 0.03809523809523809867, 0.03928571428571428492, 0.04047619047619047811, 0.04107142857142857123 ),
 .UNSPECIFIED. ) 
 CURVE ( )  GEOMETRIC_REPRESENTATION_ITEM ( )  RATIONAL_B_SPLINE_CURVE ( ( 0.9330127018922194093, 0.9330127018922197424, 1.000000000000000000, 0.8660254037844387076, 1.000000000000000000, 0.8660254037844387076, 1.000000000000000000, 0.9330127018922194093, 0.9330127018922194093 ) ) 
 REPRESENTATION_ITEM ( '' )  );
#9261 = CARTESIAN_POINT ( 'NONE',  ( 0.000000000000000000, -120.0000000000000000, 0.000000000000000000 ) ) ;
#9262 = CARTESIAN_POINT ( 'NONE',  ( -4.458734124999998549, -10.22916666530106866, 2.574251347313722516 ) ) ;
#9263 = CARTESIAN_POINT ( 'NONE',  ( -3.152548672688508926E-16, -101.8124999986344079, -5.148502694627439702 ) ) ;
#9264 = CARTESIAN_POINT ( 'NONE',  ( -8.190561711645485556E-16, -144.9375000013656063, 4.458734124999999437 ) ) ;
#9265 = CARTESIAN_POINT ( 'NONE',  ( 9.457646018065525792E-16, -29.31249999863440436, 5.148502694627439702 ) ) ;
#9266 = CARTESIAN_POINT ( 'NONE',  ( -51.19402409849444524, -139.6250000027312126, -3.242614290531456334 ) ) ;
#9267 = CARTESIAN_POINT ( 'NONE',  ( -53.51423613279429503, -131.2500000013656347, 4.591703134518082763 ) ) ;
#9268 = CARTESIAN_POINT ( 'NONE',  ( -4.458734124999999437, -68.56249999863439371, 0.000000000000000000 ) ) ;
#9269 = CARTESIAN_POINT ( 'NONE',  ( -5.000000000000000000, -91.00000000000000000, 0.000000000000000000 ) ) ;
#9270 = CARTESIAN_POINT ( 'NONE',  ( -4.458734125000000326, -140.8750000013656063, 1.846868145590734089 ) ) ;
#9271 = CARTESIAN_POINT ( 'NONE',  ( -4.458734124999999437, 7.354166668032259047, -2.574251347313719407 ) ) ;
#9272 = ORIENTED_EDGE ( 'NONE', *, *, #62021, .F. ) ;
#9273 =( LENGTH_UNIT ( ) NAMED_UNIT ( * ) SI_UNIT ( .MILLI., .METRE. ) );
#9274 = CARTESIAN_POINT ( 'NONE',  ( 1.975475456537005874E-15, 9.250000000000000000, 5.000000000000000000 ) ) ;
#9276 = CARTESIAN_POINT ( 'NONE',  ( -4.458734124999999437, -27.39583333196773651, -2.574251347313719407 ) ) ;
#9275 = CARTESIAN_POINT ( 'NONE',  ( 2.500000000000002220, -94.66666666666665719, 4.330127018922192761 ) ) ;
#9277 = DIRECTION ( 'NONE',  ( 0.000000000000000000, 0.000000000000000000, 1.000000000000000000 ) ) ;
#9278 = CARTESIAN_POINT ( 'NONE',  ( -4.458734124999999437, -74.56249999863440792, 0.000000000000000000 ) ) ;
#9279 = ADVANCED_FACE ( 'NONE', ( #2509 ), #27567, .T. ) ;
#9280 = CARTESIAN_POINT ( 'NONE',  ( 4.458734124999999437, 20.93750000136559208, -5.460374474430324690E-16 ) ) ;
#9281 = CARTESIAN_POINT ( 'NONE',  ( 1.339745962155615144, -18.70534180126147916, 4.999999999999999112 ) ) ;
#9282 = CARTESIAN_POINT ( 'NONE',  ( -57.19623071787017210, -142.3750000013656063, 4.297418129356382899 ) ) ;
#9283 = CARTESIAN_POINT ( 'NONE',  ( 2.229367062499998831, 5.354166668032261711, -3.861377020970580887 ) ) ;
#9284 = CARTESIAN_POINT ( 'NONE',  ( 2.229367062500001939, 25.77083333469892779, 3.861377020970579999 ) ) ;
#9285 = CARTESIAN_POINT ( 'NONE',  ( 4.458734125000000326, -41.14583333196773651, 2.574251347313718519 ) ) ;
#9286 = CARTESIAN_POINT ( 'NONE',  ( 1.339745962155615144, -80.70534180126146850, 4.999999999999999112 ) ) ;
#9287 = CARTESIAN_POINT ( 'NONE',  ( -4.458734124999999437, 1.604166668032262155, -2.574251347313719407 ) ) ;
#9288 = CARTESIAN_POINT ( 'NONE',  ( 9.457646018065525792E-16, -23.31249999863440436, 5.148502694627439702 ) ) ;
#9289 = CARTESIAN_POINT ( 'NONE',  ( 4.458734125000000326, -157.3750000013656347, -1.846868145590734978 ) ) ;
#9290 = CARTESIAN_POINT ( 'NONE',  ( -4.458734124999999437, -70.39583333196773651, -2.574251347313719407 ) ) ;
#9291 = CARTESIAN_POINT ( 'NONE',  ( 5.000000000000000000, -106.3749999972688158, -6.123233995736766282E-16 ) ) ;
#9292 = LINE ( 'NONE', #47284, #33696 ) ;
#9293 = CARTESIAN_POINT ( 'NONE',  ( 0.000000000000000000, -120.0000000000000000, 5.000000000000000000 ) ) ;
#9294 = CARTESIAN_POINT ( 'NONE',  ( -4.458734124999999437, -105.6458333319677365, -2.574251347313719407 ) ) ;
#9295 = CARTESIAN_POINT ( 'NONE',  ( -4.458734124999999437, -70.56249999863439371, 0.000000000000000000 ) ) ;
#9296 = CARTESIAN_POINT ( 'NONE',  ( 2.500000000000002220, -52.66666666666666430, 4.330127018922192761 ) ) ;
#9297 = CARTESIAN_POINT ( 'NONE',  ( 0.000000000000000000, -170.0000000000000000, 0.000000000000000000 ) ) ;
#9298 = FACE_OUTER_BOUND ( 'NONE', #41505, .T. ) ;
#9299 = VERTEX_POINT ( 'NONE', #8279 ) ;
#9300 = LINE ( 'NONE', #24105, #50976 ) ;
#9301 = AXIS2_PLACEMENT_3D ( 'NONE', #62150, #58260, #33810 ) ;
#9302 = LINE ( 'NONE', #28917, #61724 ) ;
#9303 = CARTESIAN_POINT ( 'NONE',  ( 5.000000000000000000, -12.41666666666666607, -2.886751345948129988 ) ) ;
#9304 = CARTESIAN_POINT ( 'NONE',  ( -3.152548672688508926E-16, -14.56249999863440436, -5.148502694627439702 ) ) ;
#9305 = VECTOR ( 'NONE', #55369, 1000.000000000000000 ) ;
#9306 = CARTESIAN_POINT ( 'NONE',  ( 2.229367062499998831, -77.64583333196773651, -3.861377020970580887 ) ) ;
#9307 = CARTESIAN_POINT ( 'NONE',  ( 2.730187237215162345E-16, -168.4375000013656063, -4.458734124999999437 ) ) ;
#9308 = CARTESIAN_POINT ( 'NONE',  ( -3.535250795749689387E-16, -18.12499999726881228, -5.773502691896257311 ) ) ;
#9310 = ORIENTED_EDGE ( 'NONE', *, *, #15253, .T. ) ;
#9309 = CARTESIAN_POINT ( 'NONE',  ( 4.458734124999998549, -46.72916666530106511, -2.574251347313721627 ) ) ;
#9311 = LINE ( 'NONE', #59161, #16908 ) ;
#9313 = ORIENTED_EDGE ( 'NONE', *, *, #14581, .F. ) ;
#9312 = CARTESIAN_POINT ( 'NONE',  ( -4.458734124999999437, 0.3541666680322609340, -2.574251347313719407 ) ) ;
#9314 = CARTESIAN_POINT ( 'NONE',  ( -57.19623071787016499, -153.3750000013656063, 4.297418129356382899 ) ) ;
#9315 = CARTESIAN_POINT ( 'NONE',  ( -2.500000000000000444, -62.16666666666666430, -4.330127018922193649 ) ) ;
#9316 = CARTESIAN_POINT ( 'NONE',  ( -1.846868145590734756, -157.3750000013656347, -4.458734125000000326 ) ) ;
#9317 = CARTESIAN_POINT ( 'NONE',  ( 4.458734124999999437, -40.06249999863440081, -5.460374474430324690E-16 ) ) ;
#9318 = CARTESIAN_POINT ( 'NONE',  ( -1.339745962155613812, -65.20534180126146850, -5.000000000000000000 ) ) ;
#9319 = CARTESIAN_POINT ( 'NONE',  ( 2.071067811865475505, -161.8125000000000284, -5.000000000000000888 ) ) ;
#9320 = CARTESIAN_POINT ( 'NONE',  ( 2.071067811865455077, -167.8124999999999716, -5.000000000000022204 ) ) ;
#9321 = CARTESIAN_POINT ( 'NONE',  ( -50.70258187064364108, -125.3750000013656205, 2.196230717870141014 ) ) ;
#9322 = CARTESIAN_POINT ( 'NONE',  ( 9.457646018065525792E-16, -5.312499998634402587, 5.148502694627439702 ) ) ;
#9323 = CARTESIAN_POINT ( 'NONE',  ( 2.229367062500001939, -47.22916666530106511, 3.861377020970579999 ) ) ;
#9324 = CARTESIAN_POINT ( 'NONE',  ( 1.339745962155615144, -67.58034179853029855, 4.999999999999999112 ) ) ;
#9325 = CARTESIAN_POINT ( 'NONE',  ( -3.152801135295367096, -149.0625000013655779, -3.152801135295367541 ) ) ;
#9326 = CARTESIAN_POINT ( 'NONE',  ( -2.229367062500000163, -91.72916666530106511, -3.861377020970580443 ) ) ;
#9327 = CARTESIAN_POINT ( 'NONE',  ( 1.975475456537005874E-15, -34.62499999726880873, 5.000000000000000000 ) ) ;
#9328 = ORIENTED_EDGE ( 'NONE', *, *, #21593, .T. ) ;
#9329 = CARTESIAN_POINT ( 'NONE',  ( 5.000000000000000888, -155.0625000027311842, -2.071067811865475505 ) ) ;
#9330 = CARTESIAN_POINT ( 'NONE',  ( -1.339745962155610925, -68.66965819600733312, 5.000000000000000000 ) ) ;
#9331 = CARTESIAN_POINT ( 'NONE',  ( -55.39835681537999790, -152.0000000027312410, 4.984105922594378235 ) ) ;
#9332 = CARTESIAN_POINT ( 'NONE',  ( 0.000000000000000000, -120.0000000000000000, 0.000000000000000000 ) ) ;
#9333 = EDGE_LOOP ( 'NONE', ( #37046, #50243, #37709, #22033 ) ) ;
#9334 =( BOUNDED_CURVE ( )  B_SPLINE_CURVE ( 2, ( #32698, #60717, #16640, #17272, #61036, #12759, #36262, #12446, #32382 ),
 .UNSPECIFIED., .F., .F. ) 
 B_SPLINE_CURVE_WITH_KNOTS ( ( 3, 2, 2, 2, 3 ),
 ( 0.1020833333333333315, 0.1027777777777777735, 0.1041666666666666713, 0.1055555555555555552, 0.1062499999999999972 ),
 .UNSPECIFIED. ) 
 CURVE ( )  GEOMETRIC_REPRESENTATION_ITEM ( )  RATIONAL_B_SPLINE_CURVE ( ( 0.9330127018922194093, 0.9330127018922194093, 1.000000000000000000, 0.8660254037844387076, 1.000000000000000000, 0.8660254037844387076, 1.000000000000000000, 0.9330127018922194093, 0.9330127018922194093 ) ) 
 REPRESENTATION_ITEM ( '' )  );
#9335 = DIRECTION ( 'NONE',  ( -0.000000000000000000, 1.000000000000000000, -0.000000000000000000 ) ) ;
#9336 = CARTESIAN_POINT ( 'NONE',  ( -4.458734124999998549, -10.47916666530107044, 2.574251347313722516 ) ) ;
#9337 = CARTESIAN_POINT ( 'NONE',  ( -54.60164318462004474, -150.5000000027312126, -4.984105922594373794 ) ) ;
#9338 = CARTESIAN_POINT ( 'NONE',  ( -4.458734124999999437, -3.312499998634407916, 0.000000000000000000 ) ) ;
#9339 = CARTESIAN_POINT ( 'NONE',  ( -5.000000000000000000, -11.95833333060214798, -2.886751345948128211 ) ) ;
#9340 = CARTESIAN_POINT ( 'NONE',  ( 1.846868145590735200, -154.2500000013656063, -4.458734124999999437 ) ) ;
#9341 = CARTESIAN_POINT ( 'NONE',  ( -4.458734124999997661, 19.52083333469893134, 2.574251347313722516 ) ) ;
#9342 = VERTEX_POINT ( 'NONE', #42992 ) ;
#9343 = CARTESIAN_POINT ( 'NONE',  ( -4.458734124999997661, -94.22916666530106511, 2.574251347313722516 ) ) ;
#9344 = CARTESIAN_POINT ( 'NONE',  ( -6.972266317189433020E-16, -104.1249999972688016, -5.000000000000000000 ) ) ;
#9345 = CARTESIAN_POINT ( 'NONE',  ( -4.458734124999999437, -14.39583333196773474, -2.574251347313719407 ) ) ;
#9346 = AXIS2_PLACEMENT_3D ( 'NONE', #37251, #52049, #31785 ) ;
#9347 = EDGE_CURVE ( 'NONE', #47748, #8541, #11856, .T. ) ;
#9348 = DIRECTION ( 'NONE',  ( -0.000000000000000000, 1.000000000000000000, -0.000000000000000000 ) ) ;
#9349 = CARTESIAN_POINT ( 'NONE',  ( 1.975475456537005874E-15, 8.375000002731187720, 5.000000000000000000 ) ) ;
#9350 =( BOUNDED_CURVE ( )  B_SPLINE_CURVE ( 2, ( #57319, #35866, #13236, #55491, #42816, #32859, #26529, #52488, #46149 ),
 .UNSPECIFIED., .F., .F. ) 
 B_SPLINE_CURVE_WITH_KNOTS ( ( 3, 2, 2, 2, 3 ),
 ( 0.6624999999999999778, 0.6630952380952380709, 0.6642857142857142572, 0.6654761904761904434, 0.6660714285714285365 ),
 .UNSPECIFIED. ) 
 CURVE ( )  GEOMETRIC_REPRESENTATION_ITEM ( )  RATIONAL_B_SPLINE_CURVE ( ( 0.9330127018922194093, 0.9330127018922194093, 1.000000000000000000, 0.8660254037844387076, 1.000000000000000000, 0.8660254037844387076, 1.000000000000000000, 0.9330127018922194093, 0.9330127018922194093 ) ) 
 REPRESENTATION_ITEM ( '' )  );
#9351 = CARTESIAN_POINT ( 'NONE',  ( -52.10840900171896806, -152.1875000013656063, 3.393966926194110556 ) ) ;
#9352 = CARTESIAN_POINT ( 'NONE',  ( 1.060575238724906964E-15, -41.62499999726880162, 5.773502691896257311 ) ) ;
#9353 = CARTESIAN_POINT ( 'NONE',  ( 0.000000000000000000, -135.0000000000000284, 0.000000000000000000 ) ) ;
#9354 = CARTESIAN_POINT ( 'NONE',  ( -4.458734124999999437, 21.68750000136559208, 0.000000000000000000 ) ) ;
#9355 = CARTESIAN_POINT ( 'NONE',  ( -5.000000000000000000, 12.12500000273118772, 0.000000000000000000 ) ) ;
#9356 = ORIENTED_EDGE ( 'NONE', *, *, #36609, .F. ) ;
#9357 = CARTESIAN_POINT ( 'NONE',  ( -3.152548672688508926E-16, 15.43750000136559564, -5.148502694627439702 ) ) ;
#9358 = CARTESIAN_POINT ( 'NONE',  ( 2.229367062499998831, -62.64583333196774362, -3.861377020970580887 ) ) ;
#9359 = CARTESIAN_POINT ( 'NONE',  ( -2.229367062499996610, -7.395833331967735624, 3.861377020970582219 ) ) ;
#9360 = CARTESIAN_POINT ( 'NONE',  ( -1.339745962155613812, -63.20534180126146850, -5.000000000000000000 ) ) ;
#9361 = CARTESIAN_POINT ( 'NONE',  ( -2.499999999999996447, 12.16666666666666607, 4.330127018922195425 ) ) ;
#9362 = CARTESIAN_POINT ( 'NONE',  ( -3.152801135295367096, -169.0625000013656063, -3.152801135295367541 ) ) ;
#9363 = CARTESIAN_POINT ( 'NONE',  ( 5.000000000000000000, -88.50000000000000000, -6.123233995736766282E-16 ) ) ;
#9364 = CARTESIAN_POINT ( 'NONE',  ( -2.229367062499996610, -52.14583333196773651, 3.861377020970582219 ) ) ;
#9365 = CARTESIAN_POINT ( 'NONE',  ( 5.000000000000000000, -89.29166666393545881, -2.886751345948129988 ) ) ;
#9366 = CARTESIAN_POINT ( 'NONE',  ( -58.39396692619412477, -130.6875000013656063, 2.891590998281057701 ) ) ;
#9367 = LINE ( 'NONE', #19652, #56537 ) ;
#9368 = EDGE_CURVE ( 'NONE', #45662, #49599, #22208, .T. ) ;
#9369 = LINE ( 'NONE', #33198, #8006 ) ;
#9370 = EDGE_CURVE ( 'NONE', #3859, #27694, #24251, .T. ) ;
#9371 = CARTESIAN_POINT ( 'NONE',  ( 9.457646018065525792E-16, -89.31249999863440792, 5.148502694627439702 ) ) ;
#9372 = CARTESIAN_POINT ( 'NONE',  ( -4.458734124999999437, -153.1875000013656063, -5.460374474430324690E-16 ) ) ;
#9373 = CARTESIAN_POINT ( 'NONE',  ( -2.499999999999996447, -38.83333333333332860, 4.330127018922195425 ) ) ;
#9374 = CARTESIAN_POINT ( 'NONE',  ( -57.46284108482265651, -139.9375000000000284, 4.819101127000238627 ) ) ;
#9375 = VERTEX_POINT ( 'NONE', #17919 ) ;
#9376 = CARTESIAN_POINT ( 'NONE',  ( -4.458734124999998549, -101.2291666653010651, 2.574251347313722516 ) ) ;
#9377 = CARTESIAN_POINT ( 'NONE',  ( -4.458734124999998549, 8.520833334698926009, 2.574251347313722516 ) ) ;
#9378 = CARTESIAN_POINT ( 'NONE',  ( 5.000000000000000000, -162.0625000000000000, 2.071067811865478614 ) ) ;
#9379 = CARTESIAN_POINT ( 'NONE',  ( 5.000000000000000000, 1.583333333333332593, -2.886751345948129988 ) ) ;
#9380 = EDGE_CURVE ( 'NONE', #21022, #45244, #45670, .T. ) ;
#9381 = CARTESIAN_POINT ( 'NONE',  ( 2.229367062500001939, -61.97916666530106511, 3.861377020970579999 ) ) ;
#9382 = DIRECTION ( 'NONE',  ( -0.000000000000000000, 1.000000000000000000, -0.000000000000000000 ) ) ;
#9383 = CARTESIAN_POINT ( 'NONE',  ( -5.000000000000000000, -4.874999997268810503, 0.000000000000000000 ) ) ;
#9384 = CARTESIAN_POINT ( 'NONE',  ( 9.457646018065525792E-16, -29.06249999863440081, 5.148502694627439702 ) ) ;
#9385 = DIRECTION ( 'NONE',  ( -0.000000000000000000, 1.000000000000000000, -0.000000000000000000 ) ) ;
#9386 = CYLINDRICAL_SURFACE ( 'NONE', #46702, 5.000000000000000000 ) ;
#9387 = CARTESIAN_POINT ( 'NONE',  ( 6.324555320336760822, 15.00000000000000000, 8.999999999999998224 ) ) ;
#9388 = CARTESIAN_POINT ( 'NONE',  ( -5.000000000000000000, -43.08333333333332860, -2.886751345948128211 ) ) ;
#9390 = CARTESIAN_POINT ( 'NONE',  ( 4.458734124999999437, -23.06249999863440436, -5.460374474430324690E-16 ) ) ;
#9389 = CARTESIAN_POINT ( 'NONE',  ( -5.000000000000000000, -89.87499999726880162, 0.000000000000000000 ) ) ;
#9391 = CARTESIAN_POINT ( 'NONE',  ( 4.458734124999999437, -71.81249999863439371, -5.460374474430324690E-16 ) ) ;
#9392 = CARTESIAN_POINT ( 'NONE',  ( 1.846868145590735200, -145.5000000013655779, -4.458734125000000326 ) ) ;
#9393 = AXIS2_PLACEMENT_3D ( 'NONE', #17679, #47569, #37602 ) ;
#9394 = CARTESIAN_POINT ( 'NONE',  ( 4.458734124999998549, -78.72916666530106511, -2.574251347313721627 ) ) ;
#9395 = CARTESIAN_POINT ( 'NONE',  ( -50.70258187064364108, -138.3750000013656063, 2.196230717870141014 ) ) ;
#9396 = CARTESIAN_POINT ( 'NONE',  ( 2.229367062500001939, -25.22916666530106866, 3.861377020970579999 ) ) ;
#9397 = CARTESIAN_POINT ( 'NONE',  ( 5.000000000000000000, -67.37499999726881583, -6.123233995736766282E-16 ) ) ;
#9398 = EDGE_LOOP ( 'NONE', ( #48431, #16615, #47457, #33617 ) ) ;
#9399 = EDGE_CURVE ( 'NONE', #38994, #13010, #28775, .T. ) ;
#9400 = CARTESIAN_POINT ( 'NONE',  ( -58.24261429053147765, -148.3750000027312126, -3.805975901505573855 ) ) ;
#9401 = ORIENTED_EDGE ( 'NONE', *, *, #62908, .F. ) ;
#9402 = CARTESIAN_POINT ( 'NONE',  ( 4.458734124999999437, -72.06249999863439371, -5.460374474430324690E-16 ) ) ;
#9403 = CARTESIAN_POINT ( 'NONE',  ( 2.071067811865433317, -165.8125000000000000, -5.000000000000041744 ) ) ;
#9404 = EDGE_LOOP ( 'NONE', ( #48405, #52607, #40576, #25148 ) ) ;
#9405 = CARTESIAN_POINT ( 'NONE',  ( 1.062108568985190270E-13, -25.25000000000000355, -4.999999999999999112 ) ) ;
#9406 =( BOUNDED_CURVE ( )  B_SPLINE_CURVE ( 2, ( #54771, #25172, #50257, #46955, #29990, #45113, #10703, #17682, #10381 ),
 .UNSPECIFIED., .F., .F. ) 
 B_SPLINE_CURVE_WITH_KNOTS ( ( 3, 2, 2, 2, 3 ),
 ( 0.5520833333333333703, 0.5527777777777778123, 0.5541666666666666963, 0.5555555555555555802, 0.5562500000000000222 ),
 .UNSPECIFIED. ) 
 CURVE ( )  GEOMETRIC_REPRESENTATION_ITEM ( )  RATIONAL_B_SPLINE_CURVE ( ( 0.9330127018922194093, 0.9330127018922194093, 1.000000000000000000, 0.8660254037844387076, 1.000000000000000000, 0.8660254037844387076, 1.000000000000000000, 0.9330127018922194093, 0.9330127018922194093 ) ) 
 REPRESENTATION_ITEM ( '' )  );
#9407 = CARTESIAN_POINT ( 'NONE',  ( -4.999999999999998224, -2.916666666666664742, 2.886751345948131764 ) ) ;
#9408 = CARTESIAN_POINT ( 'NONE',  ( 2.229367062500001939, -60.22916666530106511, 3.861377020970579999 ) ) ;
#9409 = CARTESIAN_POINT ( 'NONE',  ( 9.457646018065525792E-16, -0.3124999986344051961, 5.148502694627439702 ) ) ;
#9410 = ORIENTED_EDGE ( 'NONE', *, *, #51133, .F. ) ;
#9411 = CARTESIAN_POINT ( 'NONE',  ( 5.000000000000000000, -69.29166666393547303, -2.886751345948130876 ) ) ;
#9412 = CARTESIAN_POINT ( 'NONE',  ( 4.458734124999998549, 12.27083333469892423, -2.574251347313721627 ) ) ;
#9413 = CARTESIAN_POINT ( 'NONE',  ( -59.59170313451811296, -145.5000000013656063, 1.485763867205729394 ) ) ;
#9414 = CARTESIAN_POINT ( 'NONE',  ( 5.000000000000000000, 16.50000000000000000, -6.123233995736766282E-16 ) ) ;
#9415 = CARTESIAN_POINT ( 'NONE',  ( 3.152801135295367541, -166.3125000013656063, -3.152801135295367541 ) ) ;
#9416 = ORIENTED_EDGE ( 'NONE', *, *, #51226, .F. ) ;
#9417 = CARTESIAN_POINT ( 'NONE',  ( -4.458734124999999437, -75.31249999863440792, 0.000000000000000000 ) ) ;
#9418 = CARTESIAN_POINT ( 'NONE',  ( -2.500000000000000444, -70.04166666393547303, -4.330127018922193649 ) ) ;
#9419 = CARTESIAN_POINT ( 'NONE',  ( -4.458734124999998549, 0.7708333346989267865, 2.574251347313722516 ) ) ;
#9420 = EDGE_CURVE ( 'NONE', #12555, #42937, #58970, .T. ) ;
#9421 = EDGE_CURVE ( 'NONE', #29717, #61181, #34507, .T. ) ;
#9422 = CARTESIAN_POINT ( 'NONE',  ( 5.000000000000000888, -40.45833333060214443, 2.886751345948126879 ) ) ;
#9423 = EDGE_CURVE ( 'NONE', #49599, #10376, #61657, .T. ) ;
#9424 = CARTESIAN_POINT ( 'NONE',  ( 9.457646018065525792E-16, -65.31249999863440792, 5.148502694627439702 ) ) ;
#9425 = CARTESIAN_POINT ( 'NONE',  ( -2.499999999999996447, -26.70833333060214798, 4.330127018922195425 ) ) ;
#9426 = CARTESIAN_POINT ( 'NONE',  ( 5.000000000000000888, -96.45833333060213022, 2.886751345948126879 ) ) ;
#9427 = CARTESIAN_POINT ( 'NONE',  ( -6.972266317189433020E-16, -59.25000000000000000, -5.000000000000000000 ) ) ;
#9428 = LINE ( 'NONE', #57711, #30616 ) ;
#9429 = FACE_OUTER_BOUND ( 'NONE', #59719, .T. ) ;
#9430 = CARTESIAN_POINT ( 'NONE',  ( 4.458734125000001214, -43.89583333196775072, 2.574251347313718519 ) ) ;
#9431 = CARTESIAN_POINT ( 'NONE',  ( 4.458734125000000326, -27.14583333196774717, 2.574251347313718519 ) ) ;
#9432 = CARTESIAN_POINT ( 'NONE',  ( -3.152548672688508926E-16, 8.187500001365595637, -5.148502694627439702 ) ) ;
#9433 = DIRECTION ( 'NONE',  ( 0.000000000000000000, 0.000000000000000000, 1.000000000000000000 ) ) ;
#9434 = CARTESIAN_POINT ( 'NONE',  ( 5.000000000000000000, 27.50000000000000000, -6.123233995736766282E-16 ) ) ;
#9435 = CARTESIAN_POINT ( 'NONE',  ( 5.000000000000000888, -151.0625000027312126, -2.071067811865475505 ) ) ;
#9436 = CARTESIAN_POINT ( 'NONE',  ( 3.061616997868383141E-16, -156.8750000027311842, -5.000000000000000000 ) ) ;
#9437 = CARTESIAN_POINT ( 'NONE',  ( -2.229367062499996610, -39.14583333196773651, 3.861377020970582219 ) ) ;
#9438 = CARTESIAN_POINT ( 'NONE',  ( 5.000000000000000000, -67.29166666393547303, -2.886751345948129988 ) ) ;
#9439 = CARTESIAN_POINT ( 'NONE',  ( -53.51423613279429503, -148.5000000013655779, 4.591703134518082763 ) ) ;
#9440 = CARTESIAN_POINT ( 'NONE',  ( 2.071067811865476394, -141.1875000000000284, 5.000000000000000000 ) ) ;
#9441 = EDGE_CURVE ( 'NONE', #48710, #49422, #43425, .T. ) ;
#9442 = CARTESIAN_POINT ( 'NONE',  ( 9.457646018065525792E-16, -76.31249999863440792, 5.148502694627439702 ) ) ;
#9443 = CARTESIAN_POINT ( 'NONE',  ( 4.458734124999999437, -165.6875000013655779, 0.000000000000000000 ) ) ;
#9444 = CARTESIAN_POINT ( 'NONE',  ( -2.229367062499996610, -28.14583333196774007, 3.861377020970582219 ) ) ;
#9445 = CARTESIAN_POINT ( 'NONE',  ( -59.98410592259440222, -136.2500000027312126, -0.3983568153799752487 ) ) ;
#9446 = CARTESIAN_POINT ( 'NONE',  ( 2.500000000000002220, 22.45833333606451987, 4.330127018922192761 ) ) ;
#9447 = CARTESIAN_POINT ( 'NONE',  ( -2.499999999999996447, -20.83333333333333570, 4.330127018922195425 ) ) ;
#9448 = CARTESIAN_POINT ( 'NONE',  ( -3.152801135295367985, -142.8125000013655779, 3.152801135295367096 ) ) ;
#9449 = ORIENTED_EDGE ( 'NONE', *, *, #28771, .T. ) ;
#9450 = CARTESIAN_POINT ( 'NONE',  ( -2.229367062500000163, 26.27083333469892779, -3.861377020970580443 ) ) ;
#9451 = CARTESIAN_POINT ( 'NONE',  ( 1.339745962155612702, 1.705341801261480272, -5.000000000000000000 ) ) ;
#9452 = CARTESIAN_POINT ( 'NONE',  ( -4.458734124999999437, -55.64583333196773651, -2.574251347313719407 ) ) ;
#9453 = CARTESIAN_POINT ( 'NONE',  ( -4.999999999999999112, 28.20833333606451632, 2.886751345948131764 ) ) ;
#9454 =( BOUNDED_CURVE ( )  B_SPLINE_CURVE ( 2, ( #50333, #1149, #40354, #41303, #11086, #22022, #20749, #30708, #55167 ),
 .UNSPECIFIED., .F., .F. ) 
 B_SPLINE_CURVE_WITH_KNOTS ( ( 3, 2, 2, 2, 3 ),
 ( 0.2395833333333333426, 0.2402777777777777846, 0.2416666666666666685, 0.2430555555555555525, 0.2437499999999999944 ),
 .UNSPECIFIED. ) 
 CURVE ( )  GEOMETRIC_REPRESENTATION_ITEM ( )  RATIONAL_B_SPLINE_CURVE ( ( 0.9330127018922194093, 0.9330127018922194093, 1.000000000000000000, 0.8660254037844387076, 1.000000000000000000, 0.8660254037844387076, 1.000000000000000000, 0.9330127018922194093, 0.9330127018922194093 ) ) 
 REPRESENTATION_ITEM ( '' )  );
#9455 = CARTESIAN_POINT ( 'NONE',  ( 1.339745962155612702, 13.83034180399266333, -5.000000000000000000 ) ) ;
#9456 = CARTESIAN_POINT ( 'NONE',  ( 5.000000000000000000, 20.58333333333333570, -2.886751345948129988 ) ) ;
#9457 = CARTESIAN_POINT ( 'NONE',  ( -4.999999999999998224, -36.79166666393548013, 2.886751345948131764 ) ) ;
#9458 = CARTESIAN_POINT ( 'NONE',  ( 2.229367062499998831, -8.645833331967736513, -3.861377020970580887 ) ) ;
#9459 = CARTESIAN_POINT ( 'NONE',  ( -2.499999999999996447, -22.83333333333333215, 4.330127018922195425 ) ) ;
#9460 = CARTESIAN_POINT ( 'NONE',  ( 1.975475456537005874E-15, -40.62499999726879452, 5.000000000000000000 ) ) ;
#9461 = CARTESIAN_POINT ( 'NONE',  ( -6.972266317189433020E-16, -89.12499999726880162, -5.000000000000000000 ) ) ;
#9462 = CARTESIAN_POINT ( 'NONE',  ( -4.999999999999998224, -87.79166666393547303, 2.886751345948131764 ) ) ;
#9463 = CARTESIAN_POINT ( 'NONE',  ( -2.229367062500000163, -22.47916666530107221, -3.861377020970580443 ) ) ;
#9464 = CARTESIAN_POINT ( 'NONE',  ( 1.339745962155615144, 0.2946581987385212820, 4.999999999999999112 ) ) ;
#9465 = CARTESIAN_POINT ( 'NONE',  ( 9.457646018065525792E-16, -54.06249999863440081, 5.148502694627439702 ) ) ;
#9466 = CARTESIAN_POINT ( 'NONE',  ( -1.846868145590737420, -155.0000000013656063, 4.458734124999999437 ) ) ;
#9467 = CARTESIAN_POINT ( 'NONE',  ( -2.499999999999996447, -50.70833333060213732, 4.330127018922195425 ) ) ;
#9468 = ORIENTED_EDGE ( 'NONE', *, *, #23681, .T. ) ;
#9469 = CARTESIAN_POINT ( 'NONE',  ( 2.229367062499998831, 7.104166668032259935, -3.861377020970580887 ) ) ;
#9470 = VERTEX_POINT ( 'NONE', #48132 ) ;
#9472 = CARTESIAN_POINT ( 'NONE',  ( -5.000000000000000000, -67.87499999726881583, 0.000000000000000000 ) ) ;
#9471 = CARTESIAN_POINT ( 'NONE',  ( 2.500000000000002220, -87.66666666666667140, 4.330127018922192761 ) ) ;
#9473 = CARTESIAN_POINT ( 'NONE',  ( -8.190561711645485556E-16, -161.6875000013655779, 4.458734124999999437 ) ) ;
#9474 = ORIENTED_EDGE ( 'NONE', *, *, #17743, .T. ) ;
#9475 = CARTESIAN_POINT ( 'NONE',  ( 0.000000000000000000, -120.0000000000000000, 5.000000000000000000 ) ) ;
#9476 = CARTESIAN_POINT ( 'NONE',  ( -50.18089887299979068, -131.6875000000000568, 2.462841084822635640 ) ) ;
#9477 = CARTESIAN_POINT ( 'NONE',  ( 5.000000000000000000, -47.29166666393547303, -2.886751345948130876 ) ) ;
#9478 = CARTESIAN_POINT ( 'NONE',  ( -3.152548672688508926E-16, -44.81249999863440792, -5.148502694627439702 ) ) ;
#9479 = ORIENTED_EDGE ( 'NONE', *, *, #12296, .T. ) ;
#9480 = CARTESIAN_POINT ( 'NONE',  ( 5.000000000000000000, 9.708333336064519870, -2.886751345948130876 ) ) ;
#9481 = CARTESIAN_POINT ( 'NONE',  ( -4.458734124999998549, 18.77083333469893134, 2.574251347313722516 ) ) ;
#9482 = CARTESIAN_POINT ( 'NONE',  ( 5.000000000000000000, -12.29166666393547835, -2.886751345948130876 ) ) ;
#9483 = VERTEX_POINT ( 'NONE', #21016 ) ;
#9484 = CARTESIAN_POINT ( 'NONE',  ( 2.229367062500001939, 28.02083333469892779, 3.861377020970579999 ) ) ;
#9485 = CARTESIAN_POINT ( 'NONE',  ( -50.18089887299979068, -126.8125000027312126, 2.462841084822635640 ) ) ;
#9486 = CARTESIAN_POINT ( 'NONE',  ( 1.339745962155612702, -88.29465819873851729, -5.000000000000000000 ) ) ;
#9487 = CARTESIAN_POINT ( 'NONE',  ( 0.000000000000000000, -120.0000000000000000, 5.000000000000000000 ) ) ;
#9488 = CARTESIAN_POINT ( 'NONE',  ( -5.000000000000000000, -103.0833333333333286, -2.886751345948128211 ) ) ;
#9489 = CARTESIAN_POINT ( 'NONE',  ( 4.458734124999999437, -61.81249999863440081, -5.460374474430324690E-16 ) ) ;
#9490 = CARTESIAN_POINT ( 'NONE',  ( 5.335963852943280017, 6.035591050531201596, -7.593821156097048330 ) ) ;
#9491 = CARTESIAN_POINT ( 'NONE',  ( 9.457646018065525792E-16, 16.93750000136559564, 5.148502694627439702 ) ) ;
#9492 = FACE_OUTER_BOUND ( 'NONE', #59076, .T. ) ;
#9493 = LINE ( 'NONE', #48110, #38152 ) ;
#9494 = EDGE_CURVE ( 'NONE', #2754, #6651, #48481, .T. ) ;
#9495 = EDGE_CURVE ( 'NONE', #45662, #29252, #49640, .T. ) ;
#9496 = CARTESIAN_POINT ( 'NONE',  ( 4.458734125000001214, -48.14583333196773651, 2.574251347313718519 ) ) ;
#9497 = CARTESIAN_POINT ( 'NONE',  ( -3.535250795749689387E-16, -3.124999997268815832, -5.773502691896257311 ) ) ;
#9498 = LINE ( 'NONE', #58402, #49949 ) ;
#9499 = CARTESIAN_POINT ( 'NONE',  ( -2.499999999999996447, -60.83333333333333570, 4.330127018922195425 ) ) ;
#9500 = CARTESIAN_POINT ( 'NONE',  ( -4.458734124999999437, -83.64583333196773651, -2.574251347313719407 ) ) ;
#9501 = EDGE_CURVE ( 'NONE', #34999, #36723, #10721, .T. ) ;
#9502 = CARTESIAN_POINT ( 'NONE',  ( 9.457646018065525792E-16, -107.0624999986343937, 5.148502694627439702 ) ) ;
#9503 = CARTESIAN_POINT ( 'NONE',  ( 2.229367062499998831, -11.89583333196774007, -3.861377020970580887 ) ) ;
#9505 = ORIENTED_EDGE ( 'NONE', *, *, #10671, .F. ) ;
#9504 = EDGE_CURVE ( 'NONE', #30240, #24529, #34561, .T. ) ;
#9506 = CARTESIAN_POINT ( 'NONE',  ( 1.339745962155612702, -52.29465819873851729, -5.000000000000000000 ) ) ;
#9507 = CARTESIAN_POINT ( 'NONE',  ( 2.229367062500001939, -99.97916666530106511, 3.861377020970579999 ) ) ;
#9508 = CARTESIAN_POINT ( 'NONE',  ( 3.061616997868383141E-16, -162.8750000027311842, -5.000000000000000000 ) ) ;
#9509 = CARTESIAN_POINT ( 'NONE',  ( 4.458734124999999437, -91.06249999863440792, -5.460374474430324690E-16 ) ) ;
#9510 = CYLINDRICAL_SURFACE ( 'NONE', #51023, 5.000000000000000000 ) ;
#9512 = EDGE_CURVE ( 'NONE', #25897, #32533, #11097, .T. ) ;
#9511 = CARTESIAN_POINT ( 'NONE',  ( -2.500000000000000444, -50.04166666393547303, -4.330127018922193649 ) ) ;
#9513 = CARTESIAN_POINT ( 'NONE',  ( 1.339745962155615144, -5.705341801261479162, 4.999999999999999112 ) ) ;
#9514 = EDGE_CURVE ( 'NONE', #50188, #30770, #28755, .T. ) ;
#9515 = CARTESIAN_POINT ( 'NONE',  ( -57.89159099828107458, -128.6875000013656063, -3.393966926194107447 ) ) ;
#9516 = CARTESIAN_POINT ( 'NONE',  ( -57.19623071787016499, -148.3750000013656063, 4.297418129356382899 ) ) ;
#9517 = CARTESIAN_POINT ( 'NONE',  ( 2.229367062500001939, -19.97916666530107221, 3.861377020970579999 ) ) ;
#9518 = CARTESIAN_POINT ( 'NONE',  ( 9.457646018065525792E-16, 12.68750000136559208, 5.148502694627439702 ) ) ;
#9519 = CARTESIAN_POINT ( 'NONE',  ( 9.457646018065525792E-16, -60.31249999863441502, 5.148502694627439702 ) ) ;
#9520 = CYLINDRICAL_SURFACE ( 'NONE', #32561, 5.000000000000000000 ) ;
#9521 = CARTESIAN_POINT ( 'NONE',  ( 4.458734125000000326, -12.89583333196774362, 2.574251347313718519 ) ) ;
#9522 = DIRECTION ( 'NONE',  ( -0.000000000000000000, 1.000000000000000000, -0.000000000000000000 ) ) ;
#9523 = CARTESIAN_POINT ( 'NONE',  ( 3.061616997868383141E-16, -153.7500000000000000, -5.000000000000000000 ) ) ;
#9524 = CARTESIAN_POINT ( 'NONE',  ( -2.500000000000000444, -7.166666666666668739, -4.330127018922193649 ) ) ;
#9525 = EDGE_CURVE ( 'NONE', #61372, #29467, #52624, .T. ) ;
#9526 = ORIENTED_EDGE ( 'NONE', *, *, #14600, .F. ) ;
#9527 = CARTESIAN_POINT ( 'NONE',  ( -4.458734124999999437, -39.56249999863440081, 0.000000000000000000 ) ) ;
#9528 = CARTESIAN_POINT ( 'NONE',  ( -6.972266317189433020E-16, -103.1249999972688158, -5.000000000000000000 ) ) ;
#9529 = EDGE_CURVE ( 'NONE', #859, #29294, #11663, .T. ) ;
#9530 = CARTESIAN_POINT ( 'NONE',  ( -2.500000000000000444, -9.166666666666662522, -4.330127018922193649 ) ) ;
#9531 = CARTESIAN_POINT ( 'NONE',  ( -6.601567268551443490, 5.319966374295965750, -7.792327460285856766 ) ) ;
#9532 = CARTESIAN_POINT ( 'NONE',  ( 2.229367062500001939, -86.97916666530107932, 3.861377020970579999 ) ) ;
#9533 = CARTESIAN_POINT ( 'NONE',  ( 2.229367062500001939, 17.77083333469892779, 3.861377020970579999 ) ) ;
#9534 =( BOUNDED_CURVE ( )  B_SPLINE_CURVE ( 2, ( #34095, #53720, #9651, #24452, #23, #44059, #19624, #29582, #58860 ),
 .UNSPECIFIED., .F., .F. ) 
 B_SPLINE_CURVE_WITH_KNOTS ( ( 3, 2, 2, 2, 3 ),
 ( 0.6729166666666667185, 0.6736111111111111605, 0.6750000000000000444, 0.6763888888888889284, 0.6770833333333333703 ),
 .UNSPECIFIED. ) 
 CURVE ( )  GEOMETRIC_REPRESENTATION_ITEM ( )  RATIONAL_B_SPLINE_CURVE ( ( 0.9330127018922194093, 0.9330127018922194093, 1.000000000000000000, 0.8660254037844387076, 1.000000000000000000, 0.8660254037844387076, 1.000000000000000000, 0.9330127018922194093, 0.9330127018922194093 ) ) 
 REPRESENTATION_ITEM ( '' )  );
#9535 = CARTESIAN_POINT ( 'NONE',  ( 4.458734124999999437, 10.18750000136559386, -5.460374474430324690E-16 ) ) ;
#9536 = EDGE_CURVE ( 'NONE', #29985, #3756, #14262, .T. ) ;
#9537 = CARTESIAN_POINT ( 'NONE',  ( 1.975475456537005874E-15, -43.75000000000000000, 5.000000000000000000 ) ) ;
#9538 = CARTESIAN_POINT ( 'NONE',  ( -5.000000000000000888, -165.6875000027311842, -2.071067811865475949 ) ) ;
#9539 = CARTESIAN_POINT ( 'NONE',  ( 4.458734124999999437, -87.06249999863439371, -5.460374474430324690E-16 ) ) ;
#9540 = CARTESIAN_POINT ( 'NONE',  ( -4.458734124999999437, 21.43750000136559208, 0.000000000000000000 ) ) ;
#9541 = CARTESIAN_POINT ( 'NONE',  ( 1.060575238724906964E-15, -72.74999999999998579, 5.773502691896257311 ) ) ;
#9542 = CARTESIAN_POINT ( 'NONE',  ( 1.060575238724906964E-15, 15.37500000273118417, 5.773502691896257311 ) ) ;
#9543 = ORIENTED_EDGE ( 'NONE', *, *, #33801, .F. ) ;
#9544 = CARTESIAN_POINT ( 'NONE',  ( 1.339745962155615144, -79.70534180126146850, 4.999999999999999112 ) ) ;
#9545 = VERTEX_POINT ( 'NONE', #21333 ) ;
#9547 = CARTESIAN_POINT ( 'NONE',  ( -2.500000000000000444, -33.16666666666666430, -4.330127018922193649 ) ) ;
#9546 = CARTESIAN_POINT ( 'NONE',  ( 0.000000000000000000, -170.0000000000000000, 0.000000000000000000 ) ) ;
#9548 = CARTESIAN_POINT ( 'NONE',  ( 4.458734124999999437, -38.81249999863440081, -5.460374474430324690E-16 ) ) ;
#9549 = CARTESIAN_POINT ( 'NONE',  ( 2.499999999999998668, -32.20833333060215153, -4.330127018922193649 ) ) ;
#9551 = ORIENTED_EDGE ( 'NONE', *, *, #39672, .T. ) ;
#9550 = CARTESIAN_POINT ( 'NONE',  ( -3.152548672688508926E-16, -67.56249999863440792, -5.148502694627439702 ) ) ;
#9552 = CARTESIAN_POINT ( 'NONE',  ( -59.29741812935640155, -151.8750000013655779, -2.196230717870135685 ) ) ;
#9553 = CARTESIAN_POINT ( 'NONE',  ( -2.229367062499996610, -10.14583333196773829, 3.861377020970582219 ) ) ;
#9555 = ORIENTED_EDGE ( 'NONE', *, *, #3544, .T. ) ;
#9554 = CARTESIAN_POINT ( 'NONE',  ( -4.458734124999999437, -16.64583333196773651, -2.574251347313719407 ) ) ;
#9556 = CARTESIAN_POINT ( 'NONE',  ( -3.535250795749689387E-16, -83.25000000000000000, -5.773502691896257311 ) ) ;
#9557 = CARTESIAN_POINT ( 'NONE',  ( -58.39396692619412477, -135.4375000013656063, 2.891590998281057701 ) ) ;
#9558 = CARTESIAN_POINT ( 'NONE',  ( 4.458734124999999437, -56.06249999863440081, -5.460374474430324690E-16 ) ) ;
#9559 = CARTESIAN_POINT ( 'NONE',  ( -2.499999999999996447, -80.70833333060213022, 4.330127018922195425 ) ) ;
#9561 = VERTEX_POINT ( 'NONE', #41886 ) ;
#9560 = CARTESIAN_POINT ( 'NONE',  ( 5.000000000000000000, 3.625000002731186388, -6.123233995736766282E-16 ) ) ;
#9562 = CARTESIAN_POINT ( 'NONE',  ( -58.80597590150559739, -145.0000000000000284, 3.242614290531460330 ) ) ;
#9563 = CARTESIAN_POINT ( 'NONE',  ( 2.229367062500001939, -25.22916666530106866, 3.861377020970579999 ) ) ;
#9564 = VERTEX_POINT ( 'NONE', #17138 ) ;
#9565 = DIRECTION ( 'NONE',  ( -0.7611951803011149931, 0.000000000000000000, 0.6485228581062917330 ) ) ;
#9566 = CARTESIAN_POINT ( 'NONE',  ( -1.846868145590734756, -167.3750000013656347, -4.458734125000000326 ) ) ;
#9567 = CARTESIAN_POINT ( 'NONE',  ( -2.229367062499996610, -107.3958333319677365, 3.861377020970582219 ) ) ;
#9568 = CARTESIAN_POINT ( 'NONE',  ( 1.975475456537005874E-15, 18.24999999999999645, 5.000000000000000000 ) ) ;
#9569 = ORIENTED_EDGE ( 'NONE', *, *, #13449, .F. ) ;
#9570 = CARTESIAN_POINT ( 'NONE',  ( -55.35523342533222291, -144.5625000013656063, 4.444560631937231499 ) ) ;
#9571 = CARTESIAN_POINT ( 'NONE',  ( -50.01589407740564042, -139.7500000027312126, 0.3983568153799778022 ) ) ;
#9572 = CARTESIAN_POINT ( 'NONE',  ( -4.458734124999999437, -36.39583333196773651, -2.574251347313719407 ) ) ;
#9573 = CARTESIAN_POINT ( 'NONE',  ( -7.915341292092594294, -3.857523022641989652, -7.913710289178173873 ) ) ;
#9574 = CARTESIAN_POINT ( 'NONE',  ( 2.499999999999998668, -3.208333330602147093, -4.330127018922193649 ) ) ;
#9575 = CARTESIAN_POINT ( 'NONE',  ( 2.229367062500001939, -10.97916666530107044, 3.861377020970579999 ) ) ;
#9576 = CARTESIAN_POINT ( 'NONE',  ( 2.229367062500001939, -98.22916666530105090, 3.861377020970579999 ) ) ;
#9577 = B_SPLINE_CURVE_WITH_KNOTS ( 'NONE', 3,
 ( #27460, #27776, #61576, #61895, #37438, #17511 ),
 .UNSPECIFIED., .F., .F.,
 ( 4, 2, 4 ),
 ( 2.475503369212747145E-07, 0.002222330217055634109, 0.004444412883774346255 ),
 .UNSPECIFIED. ) ;
#9578 = VERTEX_POINT ( 'NONE', #45771 ) ;
#9579 = CARTESIAN_POINT ( 'NONE',  ( -3.152801135295367985, -145.0625000013655779, 3.152801135295367096 ) ) ;
#9580 = CARTESIAN_POINT ( 'NONE',  ( 4.458734124999999437, -35.06249999863440792, -5.460374474430324690E-16 ) ) ;
#9581 = CARTESIAN_POINT ( 'NONE',  ( -6.972266317189433020E-16, 11.74999999999999645, -5.000000000000000000 ) ) ;
#9582 = CARTESIAN_POINT ( 'NONE',  ( -57.19623071787017210, -132.3750000013656347, 4.297418129356382899 ) ) ;
#9583 =( BOUNDED_CURVE ( )  B_SPLINE_CURVE ( 2, ( #26015, #31147, #50131, #11840, #1276, #31459, #51099, #2226, #25698 ),
 .UNSPECIFIED., .F., .F. ) 
 B_SPLINE_CURVE_WITH_KNOTS ( ( 3, 2, 2, 2, 3 ),
 ( 0.6749999999999996003, 0.6791666666666662522, 0.6833333333333329040, 0.6874999999999996669, 0.6916666666666663188 ),
 .UNSPECIFIED. ) 
 CURVE ( )  GEOMETRIC_REPRESENTATION_ITEM ( )  RATIONAL_B_SPLINE_CURVE ( ( 1.000000000000008216, 0.9238795325112786339, 1.000000000000000000, 0.9238795325112867385, 1.000000000000000000, 0.9238795325112867385, 1.000000000000000000, 0.9238795325112928447, 0.9999999999999938938 ) ) 
 REPRESENTATION_ITEM ( '' )  );
#9584 = CARTESIAN_POINT ( 'NONE',  ( 2.229367062499998831, -68.89583333196773651, -3.861377020970580887 ) ) ;
#9585 = CARTESIAN_POINT ( 'NONE',  ( 5.000000000000000888, -17.58333333333333215, 2.886751345948126879 ) ) ;
#9586 = CARTESIAN_POINT ( 'NONE',  ( -1.339745962155613812, -1.080341798530293218, -5.000000000000000000 ) ) ;
#9587 = CARTESIAN_POINT ( 'NONE',  ( -4.458734124999999437, -143.0000000013655779, -1.846868145590735644 ) ) ;
#9588 = CARTESIAN_POINT ( 'NONE',  ( 9.457646018065525792E-16, 4.687500001365595637, 5.148502694627439702 ) ) ;
#9589 = VERTEX_POINT ( 'NONE', #2048 ) ;
#9590 = CARTESIAN_POINT ( 'NONE',  ( -1.339745962155613812, -50.08034179853029855, -5.000000000000000000 ) ) ;
#9592 = CARTESIAN_POINT ( 'NONE',  ( -4.458734124999999437, -32.39583333196773651, -2.574251347313719407 ) ) ;
#9591 = CARTESIAN_POINT ( 'NONE',  ( -2.500000000000000444, -94.16666666666665719, -4.330127018922193649 ) ) ;
#9593 = CARTESIAN_POINT ( 'NONE',  ( -50.01589407740564042, -143.7500000027312126, 0.3983568153799778022 ) ) ;
#9594 = CARTESIAN_POINT ( 'NONE',  ( -2.229367062500000163, -77.72916666530106511, -3.861377020970580443 ) ) ;
#9595 = CARTESIAN_POINT ( 'NONE',  ( -3.152548672688508926E-16, 24.18750000136559564, -5.148502694627439702 ) ) ;
#9596 = CARTESIAN_POINT ( 'NONE',  ( -1.339745962155613812, -102.0803417985302843, -5.000000000000000000 ) ) ;
#9597 = CARTESIAN_POINT ( 'NONE',  ( -54.64476657466781973, -142.8125000013656063, -4.444560631937228834 ) ) ;
#9598 = CARTESIAN_POINT ( 'NONE',  ( -3.152548672688508926E-16, -4.562499998634401699, -5.148502694627439702 ) ) ;
#9599 = CARTESIAN_POINT ( 'NONE',  ( -3.152548672688508926E-16, 27.18750000136559564, -5.148502694627439702 ) ) ;
#9600 = CARTESIAN_POINT ( 'NONE',  ( -3.152548672688508926E-16, -43.81249999863440081, -5.148502694627439702 ) ) ;
#9601 = CARTESIAN_POINT ( 'NONE',  ( -51.75738570946856498, -144.7500000000000284, 3.805975901505576964 ) ) ;
#9602 = CARTESIAN_POINT ( 'NONE',  ( 9.457646018065525792E-16, 1.937500001365593416, 5.148502694627439702 ) ) ;
#9603 = ORIENTED_EDGE ( 'NONE', *, *, #1931, .F. ) ;
#9604 = CARTESIAN_POINT ( 'NONE',  ( -4.458734124999999437, -27.56249999863440081, 0.000000000000000000 ) ) ;
#9605 = CARTESIAN_POINT ( 'NONE',  ( 4.458734125000001214, -69.89583333196773651, 2.574251347313718519 ) ) ;
#9606 = CARTESIAN_POINT ( 'NONE',  ( 2.500000000000002220, -104.5416666639354730, 4.330127018922192761 ) ) ;
#9607 = CARTESIAN_POINT ( 'NONE',  ( -4.458734124999999437, 27.68750000136559208, 0.000000000000000000 ) ) ;
#9608 = EDGE_CURVE ( 'NONE', #14094, #50477, #21655, .T. ) ;
#9609 = CARTESIAN_POINT ( 'NONE',  ( -2.500000000000000444, -64.16666666666665719, -4.330127018922193649 ) ) ;
#9610 = LINE ( 'NONE', #10562, #31677 ) ;
#9611 = CARTESIAN_POINT ( 'NONE',  ( -2.229367062500000163, -71.72916666530107932, -3.861377020970580443 ) ) ;
#9612 = CARTESIAN_POINT ( 'NONE',  ( 2.500000000000002220, -54.66666666666667140, 4.330127018922192761 ) ) ;
#9613 = CARTESIAN_POINT ( 'NONE',  ( -4.330127018922101279, 45.00000000000000000, 7.500000000000002665 ) ) ;
#9614 = CYLINDRICAL_SURFACE ( 'NONE', #17127, 5.000000000000000000 ) ;
#9615 = ORIENTED_EDGE ( 'NONE', *, *, #22108, .F. ) ;
#9616 = CARTESIAN_POINT ( 'NONE',  ( 2.499999999999998668, 6.666666666666667851, -4.330127018922193649 ) ) ;
#9617 = CARTESIAN_POINT ( 'NONE',  ( 2.500000000000002220, -89.54166666393547303, 4.330127018922192761 ) ) ;
#9618 = CARTESIAN_POINT ( 'NONE',  ( 5.000000000000000000, -18.41666666666666430, -2.886751345948129988 ) ) ;
#9619 = CARTESIAN_POINT ( 'NONE',  ( 4.458734125000001214, -24.89583333196773651, 2.574251347313718519 ) ) ;
#9620 = CARTESIAN_POINT ( 'NONE',  ( -3.152548672688508926E-16, -80.56249999863440792, -5.148502694627439702 ) ) ;
#9621 = CARTESIAN_POINT ( 'NONE',  ( 3.152801135295367541, -169.5625000013656063, -3.152801135295367541 ) ) ;
#9622 = CARTESIAN_POINT ( 'NONE',  ( 2.500000000000002220, -17.54166666393547658, 4.330127018922192761 ) ) ;
#9624 = ORIENTED_EDGE ( 'NONE', *, *, #23606, .T. ) ;
#9623 = CARTESIAN_POINT ( 'NONE',  ( 2.229367062499998831, -52.64583333196773651, -3.861377020970580887 ) ) ;
#9625 = CARTESIAN_POINT ( 'NONE',  ( -1.339745962155610925, -23.79465819873851729, 5.000000000000000000 ) ) ;
#9626 = LINE ( 'NONE', #43714, #58997 ) ;
#9628 = ORIENTED_EDGE ( 'NONE', *, *, #24758, .T. ) ;
#9627 = CARTESIAN_POINT ( 'NONE',  ( -4.458734124999998549, 1.520833334698927342, 2.574251347313722516 ) ) ;
#9629 = CARTESIAN_POINT ( 'NONE',  ( -57.19623071787016499, -152.3750000013656063, 4.297418129356382899 ) ) ;
#9630 = CARTESIAN_POINT ( 'NONE',  ( 5.000000000000000000, -59.41666666666665719, -2.886751345948129988 ) ) ;
#9631 = CARTESIAN_POINT ( 'NONE',  ( -8.190561711645485556E-16, -155.9375000013655779, 4.458734124999999437 ) ) ;
#9632 = CARTESIAN_POINT ( 'NONE',  ( 2.229367062499998831, -40.89583333196773651, -3.861377020970580887 ) ) ;
#9633 =( BOUNDED_CURVE ( )  B_SPLINE_CURVE ( 2, ( #8102, #18681, #48259, #14163, #4217, #17746, #63078, #3283, #47947 ),
 .UNSPECIFIED., .F., .F. ) 
 B_SPLINE_CURVE_WITH_KNOTS ( ( 3, 2, 2, 2, 3 ),
 ( 0.6062499999999999556, 0.6069444444444443976, 0.6083333333333332815, 0.6097222222222222765, 0.6104166666666667185 ),
 .UNSPECIFIED. ) 
 CURVE ( )  GEOMETRIC_REPRESENTATION_ITEM ( )  RATIONAL_B_SPLINE_CURVE ( ( 0.9330127018922194093, 0.9330127018922194093, 1.000000000000000000, 0.8660254037844387076, 1.000000000000000000, 0.8660254037844387076, 1.000000000000000000, 0.9330127018922194093, 0.9330127018922194093 ) ) 
 REPRESENTATION_ITEM ( '' )  );
#9634 = CARTESIAN_POINT ( 'NONE',  ( -2.071067811865475061, -163.6875000000000000, -5.000000000000000888 ) ) ;
#9635 = CARTESIAN_POINT ( 'NONE',  ( -1.339745962155589165, 10.79465819873851729, -5.000000000000014211 ) ) ;
#9636 = CARTESIAN_POINT ( 'NONE',  ( -59.29741812935640155, -127.8750000013656063, -2.196230717870135685 ) ) ;
#9637 = CARTESIAN_POINT ( 'NONE',  ( 4.458734124999999437, -8.062499998634404363, -5.460374474430324690E-16 ) ) ;
#9638 = CARTESIAN_POINT ( 'NONE',  ( -4.458734124999998549, -48.47916666530106511, 2.574251347313722516 ) ) ;
#9639 = VECTOR ( 'NONE', #40028, 1000.000000000000000 ) ;
#9640 = CARTESIAN_POINT ( 'NONE',  ( -9.184850993605147944E-16, -162.3750000027311842, 5.000000000000000000 ) ) ;
#9641 = CARTESIAN_POINT ( 'NONE',  ( -1.846868145590734756, -147.1250000013656063, -4.458734125000000326 ) ) ;
#9642 = CARTESIAN_POINT ( 'NONE',  ( 2.229367062500001939, -89.22916666530106511, 3.861377020970579999 ) ) ;
#9643 = CARTESIAN_POINT ( 'NONE',  ( 5.000000000000000888, 8.416666666666666075, 2.886751345948126879 ) ) ;
#9644 = ORIENTED_EDGE ( 'NONE', *, *, #23528, .F. ) ;
#9645 = CARTESIAN_POINT ( 'NONE',  ( -1.339745962155610925, -46.79465819873852439, 5.000000000000000000 ) ) ;
#9646 = CARTESIAN_POINT ( 'NONE',  ( -60.14911071818854538, -149.1875000027312410, 1.666127454062681368 ) ) ;
#9647 = CARTESIAN_POINT ( 'NONE',  ( 5.000000000000000000, -2.291666663935477466, -2.886751345948130876 ) ) ;
#9648 = ORIENTED_EDGE ( 'NONE', *, *, #57116, .F. ) ;
#9649 = DIRECTION ( 'NONE',  ( 0.8660254037844387076, 0.000000000000000000, -0.4999999999999998890 ) ) ;
#9650 = CARTESIAN_POINT ( 'NONE',  ( 4.458734124999999437, -14.06249999863440436, -5.460374474430324690E-16 ) ) ;
#9651 = CARTESIAN_POINT ( 'NONE',  ( -2.499999999999996447, -50.83333333333332860, 4.330127018922195425 ) ) ;
#9652 = CARTESIAN_POINT ( 'NONE',  ( 2.229367062499998831, -0.6458333319677399542, -3.861377020970580887 ) ) ;
#9653 = CYLINDRICAL_SURFACE ( 'NONE', #6947, 5.000000000000000000 ) ;
#9654 = CARTESIAN_POINT ( 'NONE',  ( 3.152801135295367541, -154.3125000013656063, -3.152801135295367541 ) ) ;
#9655 = CARTESIAN_POINT ( 'NONE',  ( 4.458734125000000326, 19.85416666803226349, 2.574251347313718519 ) ) ;
#9656 = ORIENTED_EDGE ( 'NONE', *, *, #10148, .F. ) ;
#9657 = CARTESIAN_POINT ( 'NONE',  ( 4.458734124999998549, -98.72916666530105090, -2.574251347313721627 ) ) ;
#9658 = CARTESIAN_POINT ( 'NONE',  ( -1.339745962155610925, -33.66965819600732601, 5.000000000000000000 ) ) ;
#9659 = CARTESIAN_POINT ( 'NONE',  ( 1.339745962155615144, -40.70534180126147561, 4.999999999999999112 ) ) ;
#9660 = CARTESIAN_POINT ( 'NONE',  ( 2.229367062500001939, -11.97916666530107044, 3.861377020970579999 ) ) ;
#9661 = CARTESIAN_POINT ( 'NONE',  ( 2.499999999999998668, -39.20833333060214443, -4.330127018922193649 ) ) ;
#9662 = CARTESIAN_POINT ( 'NONE',  ( 1.339745962155613146, 29.70534180126147561, -4.999999999999999112 ) ) ;
#9663 = CARTESIAN_POINT ( 'NONE',  ( 1.975475456537005874E-15, -90.74999999999998579, 5.000000000000000000 ) ) ;
#9664 = CARTESIAN_POINT ( 'NONE',  ( 2.499999999999998668, -42.20833333060214443, -4.330127018922193649 ) ) ;
#9665 = CARTESIAN_POINT ( 'NONE',  ( 5.000000000000000888, -29.58333333333332860, 2.886751345948126879 ) ) ;
#9666 = CARTESIAN_POINT ( 'NONE',  ( -4.458734124999999437, 15.60416666803225993, -2.574251347313719407 ) ) ;
#9667 = CARTESIAN_POINT ( 'NONE',  ( 5.000000000000000000, -46.37499999726880873, -6.123233995736766282E-16 ) ) ;
#9668 = VERTEX_POINT ( 'NONE', #61533 ) ;
#9669 = CARTESIAN_POINT ( 'NONE',  ( -4.458734124999997661, 16.77083333469892779, 2.574251347313722516 ) ) ;
#9670 = CARTESIAN_POINT ( 'NONE',  ( -2.229367062500000163, -61.47916666530106511, -3.861377020970580443 ) ) ;
#9671 = CARTESIAN_POINT ( 'NONE',  ( -4.458734124999999437, -7.562499998634404363, 0.000000000000000000 ) ) ;
#9672 = CARTESIAN_POINT ( 'NONE',  ( -6.972266317189433020E-16, -109.1249999972688016, -5.000000000000000000 ) ) ;
#9673 = CARTESIAN_POINT ( 'NONE',  ( -5.000000000000000000, 7.916666666666665186, -2.886751345948128211 ) ) ;
#9674 = CARTESIAN_POINT ( 'NONE',  ( -4.458734124999999437, -168.9375000013656063, -5.460374474430324690E-16 ) ) ;
#9675 = CARTESIAN_POINT ( 'NONE',  ( 1.975475456537005874E-15, -98.62499999726880162, 5.000000000000000000 ) ) ;
#9676 = CARTESIAN_POINT ( 'NONE',  ( 4.458734124999999437, -50.81249999863440792, -5.460374474430324690E-16 ) ) ;
#9677 = CARTESIAN_POINT ( 'NONE',  ( -2.499999999999996447, -91.70833333060214443, 4.330127018922195425 ) ) ;
#9678 = AXIS2_PLACEMENT_3D ( 'NONE', #4259, #14209, #59566 ) ;
#9679 = LINE ( 'NONE', #3617, #30854 ) ;
#9680 = CARTESIAN_POINT ( 'NONE',  ( 1.975475456537005874E-15, -54.62499999726880873, 5.000000000000000000 ) ) ;
#9681 = CARTESIAN_POINT ( 'NONE',  ( 1.339745962155612702, -69.29465819873850307, -5.000000000000000000 ) ) ;
#9682 = CARTESIAN_POINT ( 'NONE',  ( -4.458734125000000326, -152.1250000013655779, 1.846868145590734089 ) ) ;
#9683 = CARTESIAN_POINT ( 'NONE',  ( -2.499999999999996447, -37.83333333333332860, 4.330127018922195425 ) ) ;
#9684 = CARTESIAN_POINT ( 'NONE',  ( -6.972266317189433020E-16, -46.24999999999999289, -5.000000000000000000 ) ) ;
#9685 = CARTESIAN_POINT ( 'NONE',  ( 2.499999999999998668, -22.33333333333332860, -4.330127018922193649 ) ) ;
#9686 = ORIENTED_EDGE ( 'NONE', *, *, #37074, .T. ) ;
#9687 = CARTESIAN_POINT ( 'NONE',  ( -4.458734124999999437, -100.3124999986344079, 0.000000000000000000 ) ) ;
#9688 = CARTESIAN_POINT ( 'NONE',  ( 2.229367062499998831, 5.104166668032261711, -3.861377020970580887 ) ) ;
#9689 = CARTESIAN_POINT ( 'NONE',  ( -5.000000000000000000, -87.95833333060213022, -2.886751345948128211 ) ) ;
#9690 = CARTESIAN_POINT ( 'NONE',  ( -4.999999999999999112, 5.083333333333332149, 2.886751345948131764 ) ) ;
#9691 = B_SPLINE_CURVE_WITH_KNOTS ( 'NONE', 3,
 ( #9205, #201, #23698, #4076, #19481, #43296 ),
 .UNSPECIFIED., .F., .F.,
 ( 4, 2, 4 ),
 ( 2.475503369207376426E-07, 0.002222330217055627170, 0.004444412883774334112 ),
 .UNSPECIFIED. ) ;
#9692 = CARTESIAN_POINT ( 'NONE',  ( 9.457646018065525792E-16, -66.06249999863440792, 5.148502694627439702 ) ) ;
#9693 = CARTESIAN_POINT ( 'NONE',  ( -6.972266317189433020E-16, 2.750000000000000000, -5.000000000000000000 ) ) ;
#9694 = CARTESIAN_POINT ( 'NONE',  ( -5.000000000000000000, -0.8749999972688139449, 0.000000000000000000 ) ) ;
#9696 = ORIENTED_EDGE ( 'NONE', *, *, #42941, .F. ) ;
#9695 = CARTESIAN_POINT ( 'NONE',  ( 4.458734124999999437, -35.81249999863440792, -5.460374474430324690E-16 ) ) ;
#9697 = CARTESIAN_POINT ( 'NONE',  ( 5.000000000000000888, 17.54166666939785557, 2.886751345948126879 ) ) ;
#9698 = CARTESIAN_POINT ( 'NONE',  ( 0.000000000000000000, -170.0000000000000000, 0.000000000000000000 ) ) ;
#9699 = CARTESIAN_POINT ( 'NONE',  ( -58.24261429053147765, -136.2500000000000284, -3.805975901505573855 ) ) ;
#9700 = CARTESIAN_POINT ( 'NONE',  ( 5.000000000000000888, -47.58333333333333570, 2.886751345948126879 ) ) ;
#9702 = CARTESIAN_POINT ( 'NONE',  ( 2.229367062500001939, -24.22916666530107577, 3.861377020970579999 ) ) ;
#9701 = DIRECTION ( 'NONE',  ( -0.000000000000000000, 1.000000000000000000, -0.000000000000000000 ) ) ;
#9703 = CARTESIAN_POINT ( 'NONE',  ( 5.000000000000000000, -64.50000000000000000, -6.123233995736766282E-16 ) ) ;
#9704 = CARTESIAN_POINT ( 'NONE',  ( 4.458734124999999437, -68.81249999863439371, -5.460374474430324690E-16 ) ) ;
#9705 = CARTESIAN_POINT ( 'NONE',  ( -4.458734125000001214, -145.1250000013655779, 1.846868145590734089 ) ) ;
#9707 = EDGE_CURVE ( 'NONE', #36379, #32107, #60893, .T. ) ;
#9706 = CARTESIAN_POINT ( 'NONE',  ( -4.458734124999999437, -79.31249999863440792, 0.000000000000000000 ) ) ;
#9708 = CARTESIAN_POINT ( 'NONE',  ( -52.80376928212989185, -141.1250000013655779, -4.297418129356379346 ) ) ;
#9709 =( BOUNDED_CURVE ( )  B_SPLINE_CURVE ( 2, ( #348, #48899, #52795, #39560, #58564, #38315, #24463, #19950, #59202 ),
 .UNSPECIFIED., .F., .F. ) 
 B_SPLINE_CURVE_WITH_KNOTS ( ( 3, 2, 2, 2, 3 ),
 ( 0.006250000000000000347, 0.006944444444444444059, 0.008333333333333333218, 0.009722222222222222376, 0.01041666666666666782 ),
 .UNSPECIFIED. ) 
 CURVE ( )  GEOMETRIC_REPRESENTATION_ITEM ( )  RATIONAL_B_SPLINE_CURVE ( ( 0.9330127018922194093, 0.9330127018922194093, 1.000000000000000000, 0.8660254037844387076, 1.000000000000000000, 0.8660254037844387076, 1.000000000000000000, 0.9330127018922191873, 0.9330127018922192983 ) ) 
 REPRESENTATION_ITEM ( '' )  );
#9710 = CARTESIAN_POINT ( 'NONE',  ( -2.229367062500000163, -30.72916666530107221, -3.861377020970580443 ) ) ;
#9711 = CARTESIAN_POINT ( 'NONE',  ( -2.500000000000000444, -69.04166666393547303, -4.330127018922193649 ) ) ;
#9712 = ORIENTED_EDGE ( 'NONE', *, *, #16715, .F. ) ;
#9713 = CARTESIAN_POINT ( 'NONE',  ( 0.000000000000000000, -120.0000000000000000, 0.000000000000000000 ) ) ;
#9714 = VERTEX_POINT ( 'NONE', #16817 ) ;
#9715 = CARTESIAN_POINT ( 'NONE',  ( -2.229367062500000163, -74.72916666530106511, -3.861377020970580443 ) ) ;
#9716 = CARTESIAN_POINT ( 'NONE',  ( -4.999999999999998224, 29.08333333333333215, 2.886751345948131764 ) ) ;
#9717 = ORIENTED_EDGE ( 'NONE', *, *, #30182, .T. ) ;
#9718 = CARTESIAN_POINT ( 'NONE',  ( 2.499999999999998668, -20.20833333060214798, -4.330127018922193649 ) ) ;
#9719 = CARTESIAN_POINT ( 'NONE',  ( -2.500000000000000444, -3.166666666666664742, -4.330127018922193649 ) ) ;
#9720 = CARTESIAN_POINT ( 'NONE',  ( -3.152548672688508926E-16, -61.81249999863440081, -5.148502694627439702 ) ) ;
#9721 = CARTESIAN_POINT ( 'NONE',  ( -4.458734124999999437, 0.4375000013655955255, 0.000000000000000000 ) ) ;
#9722 = ORIENTED_EDGE ( 'NONE', *, *, #55429, .F. ) ;
#9723 =( BOUNDED_CURVE ( )  B_SPLINE_CURVE ( 2, ( #12133, #46234, #51388, #56533, #7008, #47491, #21482, #61046, #36272 ),
 .UNSPECIFIED., .F., .F. ) 
 B_SPLINE_CURVE_WITH_KNOTS ( ( 3, 2, 2, 2, 3 ),
 ( 0.6437500000000000444, 0.6444444444444444864, 0.6458333333333333703, 0.6472222222222222543, 0.6479166666666666963 ),
 .UNSPECIFIED. ) 
 CURVE ( )  GEOMETRIC_REPRESENTATION_ITEM ( )  RATIONAL_B_SPLINE_CURVE ( ( 0.9330127018922194093, 0.9330127018922194093, 1.000000000000000000, 0.8660254037844387076, 1.000000000000000000, 0.8660254037844387076, 1.000000000000000000, 0.9330127018922194093, 0.9330127018922194093 ) ) 
 REPRESENTATION_ITEM ( '' )  );
#9724 = EDGE_CURVE ( 'NONE', #27676, #45662, #58811, .T. ) ;
#9725 = CARTESIAN_POINT ( 'NONE',  ( 6.123233995736766282E-16, -170.0000000000000000, -5.000000000000000000 ) ) ;
#9726 = CARTESIAN_POINT ( 'NONE',  ( 1.975475456537005874E-15, -59.62499999726880873, 5.000000000000000000 ) ) ;
#9727 = CARTESIAN_POINT ( 'NONE',  ( -2.229367062499996610, 13.85416666803226171, 3.861377020970582219 ) ) ;
#9728 = CARTESIAN_POINT ( 'NONE',  ( -57.89159099828107458, -143.6875000013656063, -3.393966926194107447 ) ) ;
#9729 = CARTESIAN_POINT ( 'NONE',  ( 5.000000000000000000, -32.41666666666666430, -2.886751345948130876 ) ) ;
#9730 = CARTESIAN_POINT ( 'NONE',  ( -4.458734124999999437, -167.0000000013655779, -1.846868145590735644 ) ) ;
#9731 = ORIENTED_EDGE ( 'NONE', *, *, #8580, .F. ) ;
#9732 = CARTESIAN_POINT ( 'NONE',  ( 4.458734125000000326, -76.89583333196773651, 2.574251347313718519 ) ) ;
#9733 = CARTESIAN_POINT ( 'NONE',  ( -4.999999999999998224, -51.79166666393547303, 2.886751345948131764 ) ) ;
#9734 = CARTESIAN_POINT ( 'NONE',  ( 2.229367062499998831, 4.354166668032260823, -3.861377020970580887 ) ) ;
#9735 = CARTESIAN_POINT ( 'NONE',  ( 0.000000000000000000, -114.9999999999999858, 0.000000000000000000 ) ) ;
#9736 = CARTESIAN_POINT ( 'NONE',  ( -3.152548672688508926E-16, -64.81249999863440792, -5.148502694627439702 ) ) ;
#9737 = CARTESIAN_POINT ( 'NONE',  ( 2.500000000000002220, -24.54166666393548368, 4.330127018922192761 ) ) ;
#9738 = CARTESIAN_POINT ( 'NONE',  ( 0.000000000000000000, -120.0000000000000000, 0.000000000000000000 ) ) ;
#9739 = CARTESIAN_POINT ( 'NONE',  ( 5.000000000000000000, -28.37499999726881228, -6.123233995736766282E-16 ) ) ;
#9740 = CARTESIAN_POINT ( 'NONE',  ( 0.000000000000000000, -120.0000000000000000, 5.000000000000000000 ) ) ;
#9741 = CARTESIAN_POINT ( 'NONE',  ( 2.229367062499998831, -45.64583333196774362, -3.861377020970580887 ) ) ;
#9742 = CARTESIAN_POINT ( 'NONE',  ( -2.229367062500000163, -24.72916666530106866, -3.861377020970580443 ) ) ;
#9743 = CARTESIAN_POINT ( 'NONE',  ( 2.229367062499998831, 9.104166668032261711, -3.861377020970580887 ) ) ;
#9744 = CARTESIAN_POINT ( 'NONE',  ( 1.975475456537005874E-15, -9.624999997268814056, 5.000000000000000000 ) ) ;
#9745 = CARTESIAN_POINT ( 'NONE',  ( 2.500000000000002220, 27.33333333333333215, 4.330127018922192761 ) ) ;
#9746 = CARTESIAN_POINT ( 'NONE',  ( -3.535533905932738641, -147.5000000027311842, 3.535533905932737309 ) ) ;
#9747 = CARTESIAN_POINT ( 'NONE',  ( -51.75738570946856498, -154.7500000000000284, 3.805975901505576964 ) ) ;
#9748 = CARTESIAN_POINT ( 'NONE',  ( 4.458734124999998549, -38.72916666530106511, -2.574251347313721627 ) ) ;
#9749 = CARTESIAN_POINT ( 'NONE',  ( -4.999999999999999112, -70.79166666393548724, 2.886751345948131764 ) ) ;
#9750 = CARTESIAN_POINT ( 'NONE',  ( -55.35523342533222291, -145.5625000013656063, 4.444560631937231499 ) ) ;
#9751 = CARTESIAN_POINT ( 'NONE',  ( 5.000000000000000000, -143.0625000000000000, 2.071067811865478614 ) ) ;
#9752 = CARTESIAN_POINT ( 'NONE',  ( 2.229367062500001939, -77.22916666530106511, 3.861377020970579999 ) ) ;
#9753 = CARTESIAN_POINT ( 'NONE',  ( 4.458734124999999437, -166.6875000013655779, 0.000000000000000000 ) ) ;
#9754 = CARTESIAN_POINT ( 'NONE',  ( -2.229367062500000163, -32.47916666530106511, -3.861377020970580443 ) ) ;
#9755 = CARTESIAN_POINT ( 'NONE',  ( 0.000000000000000000, -120.0000000000000000, 0.000000000000000000 ) ) ;
#9756 = CYLINDRICAL_SURFACE ( 'NONE', #5093, 5.000000000000000000 ) ;
#9757 = CARTESIAN_POINT ( 'NONE',  ( -2.500000000000000444, -23.16666666666666785, -4.330127018922193649 ) ) ;
#9758 = CARTESIAN_POINT ( 'NONE',  ( 2.730187237215162345E-16, -143.1875000013656063, -4.458734124999999437 ) ) ;
#9759 = ORIENTED_EDGE ( 'NONE', *, *, #33908, .T. ) ;
#9760 = CARTESIAN_POINT ( 'NONE',  ( 2.229367062499998831, 27.10416666803225993, -3.861377020970580887 ) ) ;
#9761 = EDGE_LOOP ( 'NONE', ( #2779, #52298, #17042, #23263 ) ) ;
#9762 = CARTESIAN_POINT ( 'NONE',  ( 2.229367062499998831, -61.89583333196774362, -3.861377020970580887 ) ) ;
#9763 = CARTESIAN_POINT ( 'NONE',  ( 5.000000000000000000, 26.62500000273118772, -6.123233995736766282E-16 ) ) ;
#9764 = CARTESIAN_POINT ( 'NONE',  ( -2.499999999999996447, 21.16666666666666785, 4.330127018922195425 ) ) ;
#9765 = CARTESIAN_POINT ( 'NONE',  ( -5.000000000000000000, 8.125000002731187720, 0.000000000000000000 ) ) ;
#9766 = VECTOR ( 'NONE', #29395, 1000.000000000000000 ) ;
#9767 = CARTESIAN_POINT ( 'NONE',  ( 4.458734125000001214, -8.895833331967736513, 2.574251347313718519 ) ) ;
#9768 = CARTESIAN_POINT ( 'NONE',  ( -1.339745962155610925, 4.330341803992665106, 5.000000000000000000 ) ) ;
#9769 = FACE_OUTER_BOUND ( 'NONE', #32489, .T. ) ;
#9770 = CARTESIAN_POINT ( 'NONE',  ( 2.493747252781420335E-13, -91.12499999726880162, -5.000000000000000000 ) ) ;
#9771 = CYLINDRICAL_SURFACE ( 'NONE', #49995, 5.000000000000000000 ) ;
#9774 = CARTESIAN_POINT ( 'NONE',  ( 4.458734124999998549, -21.72916666530107221, -2.574251347313721627 ) ) ;
#9773 =( BOUNDED_CURVE ( )  B_SPLINE_CURVE ( 2, ( #27786, #37763, #42265, #3676, #57394, #52560, #47411, #56763, #12684 ),
 .UNSPECIFIED., .F., .F. ) 
 B_SPLINE_CURVE_WITH_KNOTS ( ( 3, 2, 2, 2, 3 ),
 ( 0.9583333333333331483, 0.9624999999999998002, 0.9666666666666665630, 0.9708333333333332149, 0.9749999999999998668 ),
 .UNSPECIFIED. ) 
 CURVE ( )  GEOMETRIC_REPRESENTATION_ITEM ( )  RATIONAL_B_SPLINE_CURVE ( ( 1.000000000000003997, 0.9238795325112826307, 1.000000000000000000, 0.9238795325112867385, 1.000000000000000000, 0.9238795325112867385, 1.000000000000000000, 0.9238795325112887369, 0.9999999999999980016 ) ) 
 REPRESENTATION_ITEM ( '' )  );
#9772 = CARTESIAN_POINT ( 'NONE',  ( 5.000000000000000000, 18.58333333333333215, -2.886751345948130876 ) ) ;
#9775 = CARTESIAN_POINT ( 'NONE',  ( 2.499999999999998668, -97.20833333060213022, -4.330127018922193649 ) ) ;
#9776 = CARTESIAN_POINT ( 'NONE',  ( 2.229367062499998831, -56.64583333196773651, -3.861377020970580887 ) ) ;
#9777 = CARTESIAN_POINT ( 'NONE',  ( 1.846868145590736310, -157.8750000013656063, 4.458734124999999437 ) ) ;
#9778 = EDGE_CURVE ( 'NONE', #24820, #7044, #22928, .T. ) ;
#9779 = CARTESIAN_POINT ( 'NONE',  ( 2.499999999999998668, -51.20833333060213732, -4.330127018922193649 ) ) ;
#9780 = ORIENTED_EDGE ( 'NONE', *, *, #22199, .T. ) ;
#9781 = CARTESIAN_POINT ( 'NONE',  ( 4.458734124999998549, 7.020833334698929562, -2.574251347313721627 ) ) ;
#9782 = ORIENTED_EDGE ( 'NONE', *, *, #28330, .T. ) ;
#9783 = CARTESIAN_POINT ( 'NONE',  ( 2.500000000000002220, -56.66666666666667140, 4.330127018922192761 ) ) ;
#9784 = CARTESIAN_POINT ( 'NONE',  ( -1.846868145590734756, -156.1250000013655779, -4.458734125000000326 ) ) ;
#9785 = VERTEX_POINT ( 'NONE', #48604 ) ;
#9786 = EDGE_CURVE ( 'NONE', #54905, #6256, #41150, .T. ) ;
#9787 = CARTESIAN_POINT ( 'NONE',  ( -1.339745962155610925, 11.20534180126147739, 5.000000000000000000 ) ) ;
#9788 = CARTESIAN_POINT ( 'NONE',  ( -56.66612745406270335, -135.3125000000000000, -5.149110718188516067 ) ) ;
#9789 = DIRECTION ( 'NONE',  ( -0.000000000000000000, 1.000000000000000000, -0.000000000000000000 ) ) ;
#9790 = CARTESIAN_POINT ( 'NONE',  ( 9.457646018065525792E-16, -41.31249999863440081, 5.148502694627439702 ) ) ;
#9791 = ORIENTED_EDGE ( 'NONE', *, *, #45389, .F. ) ;
#9792 = CARTESIAN_POINT ( 'NONE',  ( 6.123233995736766282E-16, -170.0000000000000000, -5.000000000000000000 ) ) ;
#9793 = ADVANCED_FACE ( 'NONE', ( #62159 ), #57961, .T. ) ;
#9794 = CARTESIAN_POINT ( 'NONE',  ( 4.458734124999998549, 18.27083333469893134, -2.574251347313721627 ) ) ;
#9795 = CARTESIAN_POINT ( 'NONE',  ( 55.00000000000002132, 15.00000000000000000, 0.000000000000000000 ) ) ;
#9796 = VERTEX_POINT ( 'NONE', #57022 ) ;
#9797 = CARTESIAN_POINT ( 'NONE',  ( -4.458734124999999437, 27.60416666803226349, -2.574251347313719407 ) ) ;
#9798 = CARTESIAN_POINT ( 'NONE',  ( -57.46284108482265651, -128.0625000027312410, 4.819101127000239515 ) ) ;
#9799 = DIRECTION ( 'NONE',  ( 0.000000000000000000, 0.000000000000000000, 1.000000000000000000 ) ) ;
#9800 = CARTESIAN_POINT ( 'NONE',  ( 5.275681513340003914E-14, 10.87500000273118239, -5.000000000000000000 ) ) ;
#9801 = CARTESIAN_POINT ( 'NONE',  ( 2.499999999999998668, -52.20833333060213732, -4.330127018922193649 ) ) ;
#9802 = CARTESIAN_POINT ( 'NONE',  ( -2.229367062499996610, -62.14583333196774362, 3.861377020970582219 ) ) ;
#9803 = CARTESIAN_POINT ( 'NONE',  ( -4.458734124999999437, 15.68750000136559564, 0.000000000000000000 ) ) ;
#9804 = VECTOR ( 'NONE', #25286, 1000.000000000000000 ) ;
#9805 = CARTESIAN_POINT ( 'NONE',  ( 0.000000000000000000, -120.0000000000000000, 0.000000000000000000 ) ) ;
#9806 = CARTESIAN_POINT ( 'NONE',  ( -4.458734124999999437, -51.64583333196773651, -2.574251347313719407 ) ) ;
#9807 = CARTESIAN_POINT ( 'NONE',  ( -5.000000000000000000, -10.87499999726881583, 0.000000000000000000 ) ) ;
#9808 = CARTESIAN_POINT ( 'NONE',  ( 1.975475456537005874E-15, -92.74999999999998579, 5.000000000000000000 ) ) ;
#9809 = CARTESIAN_POINT ( 'NONE',  ( -2.500000000000000444, -61.16666666666666430, -4.330127018922193649 ) ) ;
#9810 = CARTESIAN_POINT ( 'NONE',  ( -4.458734124999999437, -89.64583333196773651, -2.574251347313719407 ) ) ;
#9811 = CARTESIAN_POINT ( 'NONE',  ( -2.229367062500000163, -107.4791666653010651, -3.861377020970580443 ) ) ;
#9812 = CARTESIAN_POINT ( 'NONE',  ( -4.458734124999999437, -8.645833331967736513, -2.574251347313719407 ) ) ;
#9813 = ORIENTED_EDGE ( 'NONE', *, *, #44502, .T. ) ;
#9814 = CARTESIAN_POINT ( 'NONE',  ( 9.457646018065525792E-16, -96.06249999863440792, 5.148502694627439702 ) ) ;
#9815 = CARTESIAN_POINT ( 'NONE',  ( 5.000000000000000000, -163.1250000027311842, 0.000000000000000000 ) ) ;
#9816 = CARTESIAN_POINT ( 'NONE',  ( 4.458734124999999437, -98.06249999863440792, -5.460374474430324690E-16 ) ) ;
#9817 = EDGE_CURVE ( 'NONE', #37570, #60372, #37700, .T. ) ;
#9818 = CARTESIAN_POINT ( 'NONE',  ( 1.975475456537005874E-15, -7.750000000000000000, 5.000000000000000000 ) ) ;
#9819 = CARTESIAN_POINT ( 'NONE',  ( 2.500000000000002220, -55.54166666393548013, 4.330127018922192761 ) ) ;
#9820 = CARTESIAN_POINT ( 'NONE',  ( 5.000000000000000000, -5.499999999999998224, -6.123233995736766282E-16 ) ) ;
#9821 = CARTESIAN_POINT ( 'NONE',  ( -51.60603307380591787, -126.9375000013656063, -2.891590998281053704 ) ) ;
#9822 = CARTESIAN_POINT ( 'NONE',  ( -58.39396692619412477, -146.4375000013656063, 2.891590998281057701 ) ) ;
#9823 = CARTESIAN_POINT ( 'NONE',  ( 4.458734124999998549, -19.72916666530107221, -2.574251347313721627 ) ) ;
#9824 = CARTESIAN_POINT ( 'NONE',  ( -4.458734124999999437, 4.437500001365595637, 0.000000000000000000 ) ) ;
#9825 = CARTESIAN_POINT ( 'NONE',  ( 4.458734124999999437, -58.06249999863440081, -5.460374474430324690E-16 ) ) ;
#9826 = CARTESIAN_POINT ( 'NONE',  ( 1.975475456537005874E-15, -94.62499999726880162, 5.000000000000000000 ) ) ;
#9827 = CARTESIAN_POINT ( 'NONE',  ( 4.458734124999999437, -11.81249999863440081, -5.460374474430324690E-16 ) ) ;
#9828 = CARTESIAN_POINT ( 'NONE',  ( -4.250000000000000000, 5.204748896376250699E-16, -0.5251556536572846712 ) ) ;
#9829 = CARTESIAN_POINT ( 'NONE',  ( -5.000000000000000888, -156.5625000000000284, -2.071067811865475949 ) ) ;
#9830 = CARTESIAN_POINT ( 'NONE',  ( -2.500000000000000444, -6.166666666666667851, -4.330127018922193649 ) ) ;
#9831 = ORIENTED_EDGE ( 'NONE', *, *, #13105, .F. ) ;
#9832 = CARTESIAN_POINT ( 'NONE',  ( -2.229367062499996610, -41.39583333196773651, 3.861377020970582219 ) ) ;
#9833 = CARTESIAN_POINT ( 'NONE',  ( -59.44456063193725015, -125.8125000013655921, -0.3552334253322034230 ) ) ;
#9834 = CARTESIAN_POINT ( 'NONE',  ( -4.599534470795546781, 6.460478697738500031, -7.590212325761530821 ) ) ;
#9835 = DIRECTION ( 'NONE',  ( 0.000000000000000000, 0.000000000000000000, 1.000000000000000000 ) ) ;
#9836 = CARTESIAN_POINT ( 'NONE',  ( 2.229367062500001939, -85.97916666530107932, 3.861377020970579999 ) ) ;
#9837 = CARTESIAN_POINT ( 'NONE',  ( 4.458734125000001214, 18.85416666803226349, 2.574251347313718519 ) ) ;
#9838 = CARTESIAN_POINT ( 'NONE',  ( -2.229367062499996610, 7.854166668032260823, 3.861377020970582219 ) ) ;
#9839 = CARTESIAN_POINT ( 'NONE',  ( 5.000000000000000000, -0.4166666666666659080, -2.886751345948130876 ) ) ;
#9840 = CARTESIAN_POINT ( 'NONE',  ( 5.000000000000000000, -37.29166666393548724, -2.886751345948130876 ) ) ;
#9841 = CARTESIAN_POINT ( 'NONE',  ( 4.458734124999998549, -89.97916666530106511, -2.574251347313721627 ) ) ;
#9842 = CARTESIAN_POINT ( 'NONE',  ( 4.458734124999998549, 21.02083333469892779, -2.574251347313721627 ) ) ;
#9843 = CARTESIAN_POINT ( 'NONE',  ( -2.499999999999996447, -77.83333333333334281, 4.330127018922195425 ) ) ;
#9844 = CARTESIAN_POINT ( 'NONE',  ( -5.000000000000000000, 12.12500000273118772, 0.000000000000000000 ) ) ;
#9845 = ORIENTED_EDGE ( 'NONE', *, *, #27519, .T. ) ;
#9846 = CARTESIAN_POINT ( 'NONE',  ( -1.339745962155613812, -7.080341798530293218, -5.000000000000000000 ) ) ;
#9847 = ORIENTED_EDGE ( 'NONE', *, *, #23689, .T. ) ;
#9849 = CARTESIAN_POINT ( 'NONE',  ( -5.000000000000000000, -35.08333333333332149, -2.886751345948128211 ) ) ;
#9848 = CARTESIAN_POINT ( 'NONE',  ( -2.500000000000000444, -104.1666666666666572, -4.330127018922193649 ) ) ;
#9850 = CARTESIAN_POINT ( 'NONE',  ( -2.229367062499996610, -40.14583333196773651, 3.861377020970582219 ) ) ;
#9851 = AXIS2_PLACEMENT_3D ( 'NONE', #45942, #21512, #54644 ) ;
#9852 = AXIS2_PLACEMENT_3D ( 'NONE', #2976, #3291, #62140 ) ;
#9853 = EDGE_CURVE ( 'NONE', #24525, #28986, #23225, .T. ) ;
#9854 = CARTESIAN_POINT ( 'NONE',  ( -2.500000000000000444, -33.04166666393547303, -4.330127018922193649 ) ) ;
#9855 = EDGE_CURVE ( 'NONE', #4086, #44176, #59195, .T. ) ;
#9857 = ORIENTED_EDGE ( 'NONE', *, *, #58262, .T. ) ;
#9856 = CARTESIAN_POINT ( 'NONE',  ( -4.458734124999998549, -67.22916666530106511, 2.574251347313722516 ) ) ;
#9858 = CARTESIAN_POINT ( 'NONE',  ( -56.48576386720575471, -151.0000000013656063, -4.591703134518078322 ) ) ;
#9859 = CARTESIAN_POINT ( 'NONE',  ( -4.458734124999999437, -13.39583333196774184, -2.574251347313719407 ) ) ;
#9861 = ORIENTED_EDGE ( 'NONE', *, *, #27594, .F. ) ;
#9860 = CARTESIAN_POINT ( 'NONE',  ( -2.229367062499996610, -13.39583333196774007, 3.861377020970582219 ) ) ;
#9862 = EDGE_CURVE ( 'NONE', #20081, #44647, #23857, .T. ) ;
#9863 = CARTESIAN_POINT ( 'NONE',  ( -2.500000000000000444, -81.16666666666667140, -4.330127018922193649 ) ) ;
#9864 = CARTESIAN_POINT ( 'NONE',  ( 4.458734124999999437, -167.4375000013655779, 0.000000000000000000 ) ) ;
#9865 = CARTESIAN_POINT ( 'NONE',  ( -2.229367062500000163, -58.72916666530106511, -3.861377020970580443 ) ) ;
#9866 = CARTESIAN_POINT ( 'NONE',  ( -2.499999999999996447, -81.70833333060213022, 4.330127018922195425 ) ) ;
#9868 = ORIENTED_EDGE ( 'NONE', *, *, #20699, .F. ) ;
#9867 = CARTESIAN_POINT ( 'NONE',  ( -2.500000000000000444, -18.16666666666666430, -4.330127018922193649 ) ) ;
#9869 = CARTESIAN_POINT ( 'NONE',  ( -56.66612745406270335, -144.3125000000000284, -5.149110718188516067 ) ) ;
#9870 = CARTESIAN_POINT ( 'NONE',  ( -4.458734124999999437, -24.64583333196773651, -2.574251347313719407 ) ) ;
#9871 = ADVANCED_FACE ( 'NONE', ( #28046 ), #33817, .T. ) ;
#9872 = ORIENTED_EDGE ( 'NONE', *, *, #25196, .F. ) ;
#9873 = SHAPE_DEFINITION_REPRESENTATION ( #43520, #14320 ) ;
#9874 = CARTESIAN_POINT ( 'NONE',  ( -8.190561711645485556E-16, -165.9375000013655779, 4.458734124999999437 ) ) ;
#9875 = EDGE_CURVE ( 'NONE', #7933, #44977, #9369, .T. ) ;
#9876 = CARTESIAN_POINT ( 'NONE',  ( 4.458734125000001214, -103.1458333319677365, 2.574251347313718519 ) ) ;
#9877 = CARTESIAN_POINT ( 'NONE',  ( 5.000000000000000888, -55.45833333060214443, 2.886751345948126879 ) ) ;
#9878 = ORIENTED_EDGE ( 'NONE', *, *, #37254, .T. ) ;
#9879 = EDGE_CURVE ( 'NONE', #35341, #36804, #8751, .T. ) ;
#9880 = CARTESIAN_POINT ( 'NONE',  ( -52.80376928212989185, -147.1250000013656063, -4.297418129356378458 ) ) ;
#9881 = CARTESIAN_POINT ( 'NONE',  ( -51.75738570946856498, -139.8750000027312126, 3.805975901505576964 ) ) ;
#9882 = CARTESIAN_POINT ( 'NONE',  ( -4.458734124999999437, -39.31249999863440081, 0.000000000000000000 ) ) ;
#9883 = CARTESIAN_POINT ( 'NONE',  ( -1.846868145590734756, -145.3750000013656063, -4.458734124999999437 ) ) ;
#9884 = EDGE_CURVE ( 'NONE', #6339, #38436, #37414, .T. ) ;
#9885 = LINE ( 'NONE', #59752, #61052 ) ;
#9886 = CARTESIAN_POINT ( 'NONE',  ( 1.339745962155586056, 2.419658201469705894, 5.000000000000015987 ) ) ;
#9887 = CARTESIAN_POINT ( 'NONE',  ( -3.152548672688508926E-16, -12.56249999863440081, -5.148502694627439702 ) ) ;
#9888 = CARTESIAN_POINT ( 'NONE',  ( 4.458734124999999437, -102.0624999986344079, -5.460374474430324690E-16 ) ) ;
#9889 = ORIENTED_EDGE ( 'NONE', *, *, #16937, .T. ) ;
#9890 = CARTESIAN_POINT ( 'NONE',  ( 4.458734124999999437, -140.6875000013656063, 0.000000000000000000 ) ) ;
#9891 = CARTESIAN_POINT ( 'NONE',  ( -4.458734124999999437, -32.56249999863440792, 0.000000000000000000 ) ) ;
#9892 = CARTESIAN_POINT ( 'NONE',  ( 2.499999999999998668, 5.791666669397853795, -4.330127018922193649 ) ) ;
#9893 = CARTESIAN_POINT ( 'NONE',  ( -54.60164318462004474, -153.3750000000000284, -4.984105922594373794 ) ) ;
#9894 = CARTESIAN_POINT ( 'NONE',  ( -51.60603307380591787, -132.9375000013656063, -2.891590998281053704 ) ) ;
#9895 = CARTESIAN_POINT ( 'NONE',  ( 4.458734124999999437, -73.06249999863439371, -5.460374474430324690E-16 ) ) ;
#9896 = CARTESIAN_POINT ( 'NONE',  ( -5.000000000000000000, -144.6250000027312126, -6.123233995736766282E-16 ) ) ;
#9897 = CARTESIAN_POINT ( 'NONE',  ( 2.500000000000002220, -54.54166666393548013, 4.330127018922192761 ) ) ;
#9898 = CARTESIAN_POINT ( 'NONE',  ( -0.6508621380849236582, -8.763657152406455708, -7.907633014911225722 ) ) ;
#9899 = CARTESIAN_POINT ( 'NONE',  ( 2.229367062500001939, 4.770833334698926897, 3.861377020970579999 ) ) ;
#9900 = ORIENTED_EDGE ( 'NONE', *, *, #58890, .F. ) ;
#9901 = CARTESIAN_POINT ( 'NONE',  ( 2.500000000000002220, 9.333333333333332149, 4.330127018922192761 ) ) ;
#9903 = CARTESIAN_POINT ( 'NONE',  ( 4.458734124999998549, -28.72916666530107221, -2.574251347313721627 ) ) ;
#9902 = CARTESIAN_POINT ( 'NONE',  ( -5.000000000000000000, -98.00000000000000000, 0.000000000000000000 ) ) ;
#9904 = CARTESIAN_POINT ( 'NONE',  ( -49.85088928181150436, -143.6875000027312126, -1.666127454062680480 ) ) ;
#9905 = CARTESIAN_POINT ( 'NONE',  ( -2.229367062499996610, -82.39583333196773651, 3.861377020970582219 ) ) ;
#9906 = CARTESIAN_POINT ( 'NONE',  ( -4.458734124999999437, 21.35416666803225993, -2.574251347313719407 ) ) ;
#9907 = CARTESIAN_POINT ( 'NONE',  ( -2.500000000000000444, 22.95833333606451632, -4.330127018922193649 ) ) ;
#9908 = AXIS2_PLACEMENT_3D ( 'NONE', #54860, #5335, #29757 ) ;
#9909 =( BOUNDED_CURVE ( )  B_SPLINE_CURVE ( 2, ( #47161, #60698, #26589, #21773, #61010, #4581, #20012, #5542, #54102 ),
 .UNSPECIFIED., .F., .F. ) 
 B_SPLINE_CURVE_WITH_KNOTS ( ( 3, 2, 2, 2, 3 ),
 ( 0.5729166666666666297, 0.5736111111111110716, 0.5749999999999999556, 0.5763888888888888395, 0.5770833333333332815 ),
 .UNSPECIFIED. ) 
 CURVE ( )  GEOMETRIC_REPRESENTATION_ITEM ( )  RATIONAL_B_SPLINE_CURVE ( ( 0.9330127018922194093, 0.9330127018922194093, 1.000000000000000000, 0.8660254037844387076, 1.000000000000000000, 0.8660254037844387076, 1.000000000000000000, 0.9330127018922194093, 0.9330127018922194093 ) ) 
 REPRESENTATION_ITEM ( '' )  );
#9910 = CARTESIAN_POINT ( 'NONE',  ( -58.39396692619412477, -142.4375000013656063, 2.891590998281057701 ) ) ;
#9911 = CARTESIAN_POINT ( 'NONE',  ( -3.152548672688508926E-16, -2.562499998634407028, -5.148502694627439702 ) ) ;
#9912 = CARTESIAN_POINT ( 'NONE',  ( -4.458734124999999437, 29.35416666803225993, -2.574251347313719407 ) ) ;
#9913 = CARTESIAN_POINT ( 'NONE',  ( -3.152548672688508926E-16, -44.81249999863439371, -5.148502694627439702 ) ) ;
#9914 = CARTESIAN_POINT ( 'NONE',  ( 2.229367062499998831, 2.354166668032262599, -3.861377020970580887 ) ) ;
#9915 = CARTESIAN_POINT ( 'NONE',  ( -3.152548672688508926E-16, -24.81249999863440436, -5.148502694627439702 ) ) ;
#9916 = CARTESIAN_POINT ( 'NONE',  ( -3.152548672688508926E-16, -70.56249999863439371, -5.148502694627439702 ) ) ;
#9917 = CARTESIAN_POINT ( 'NONE',  ( -5.000000000000000000, -103.9583333306021444, -2.886751345948128211 ) ) ;
#9918 = CARTESIAN_POINT ( 'NONE',  ( 4.458734124999999437, 28.18750000136559208, -5.460374474430324690E-16 ) ) ;
#9919 = DIRECTION ( 'NONE',  ( -0.6485228581062915110, 0.000000000000000000, -0.7611951803011149931 ) ) ;
#9920 = CARTESIAN_POINT ( 'NONE',  ( -6.972266317189433020E-16, -80.12499999726881583, -5.000000000000000000 ) ) ;
#9921 = CARTESIAN_POINT ( 'NONE',  ( 2.229367062499998831, -74.89583333196773651, -3.861377020970580887 ) ) ;
#9922 = CARTESIAN_POINT ( 'NONE',  ( -3.535250795749689387E-16, -59.25000000000000000, -5.773502691896257311 ) ) ;
#9923 = PRODUCT_RELATED_PRODUCT_CATEGORY ( 'part', '', ( #5039 ) ) ;
#9924 = CARTESIAN_POINT ( 'NONE',  ( 0.000000000000000000, 15.00000000000000000, 5.000000000000000000 ) ) ;
#9925 = DIRECTION ( 'NONE',  ( 0.000000000000000000, 0.000000000000000000, 1.000000000000000000 ) ) ;
#9926 = ORIENTED_EDGE ( 'NONE', *, *, #9504, .T. ) ;
#9927 = CARTESIAN_POINT ( 'NONE',  ( -5.000000000000000000, -26.99999999999999645, 0.000000000000000000 ) ) ;
#9928 = CARTESIAN_POINT ( 'NONE',  ( 1.975475456537005874E-15, -67.74999999999998579, 5.000000000000000000 ) ) ;
#9929 = CARTESIAN_POINT ( 'NONE',  ( -5.000000000000000000, -18.00000000000000355, 0.000000000000000000 ) ) ;
#9930 = CARTESIAN_POINT ( 'NONE',  ( 9.457646018065525792E-16, -23.06249999863440792, 5.148502694627439702 ) ) ;
#9931 = CARTESIAN_POINT ( 'NONE',  ( -4.458734124999997661, -85.22916666530107932, 2.574251347313722516 ) ) ;
#9932 = CARTESIAN_POINT ( 'NONE',  ( -4.458734125000001214, -166.1250000013655779, 1.846868145590734089 ) ) ;
#9933 = ADVANCED_FACE ( 'NONE', ( #19336 ), #52183, .T. ) ;
#9934 = CARTESIAN_POINT ( 'NONE',  ( -4.999999999999999112, -18.79166666393547658, 2.886751345948131764 ) ) ;
#9936 = ORIENTED_EDGE ( 'NONE', *, *, #35825, .T. ) ;
#9935 = CARTESIAN_POINT ( 'NONE',  ( -4.458734124999999437, -50.39583333196773651, -2.574251347313719407 ) ) ;
#9937 = CARTESIAN_POINT ( 'NONE',  ( 6.123233995736766282E-16, -120.0000000000000000, -5.000000000000000000 ) ) ;
#9938 = CARTESIAN_POINT ( 'NONE',  ( 5.000000000000000000, -15.29166666393548191, -2.886751345948130876 ) ) ;
#9940 = ORIENTED_EDGE ( 'NONE', *, *, #22922, .T. ) ;
#9939 = CARTESIAN_POINT ( 'NONE',  ( -2.229367062499996610, 1.604166668032262155, 3.861377020970582219 ) ) ;
#9941 = CARTESIAN_POINT ( 'NONE',  ( -52.80376928212989185, -153.8750000013655779, -4.297418129356378458 ) ) ;
#9942 = CARTESIAN_POINT ( 'NONE',  ( -2.499999999999996447, -65.83333333333332860, 4.330127018922195425 ) ) ;
#9943 = CARTESIAN_POINT ( 'NONE',  ( 4.458734124999999437, -155.7500000013655779, 1.846868145590737864 ) ) ;
#9944 = CARTESIAN_POINT ( 'NONE',  ( 4.458734124999999437, -43.06249999863440081, -5.460374474430324690E-16 ) ) ;
#9945 = CARTESIAN_POINT ( 'NONE',  ( 1.975475456537005874E-15, -80.62499999726881583, 5.000000000000000000 ) ) ;
#9946 = VECTOR ( 'NONE', #8050, 1000.000000000000000 ) ;
#9947 = CARTESIAN_POINT ( 'NONE',  ( -5.000000000000000888, -162.4375000000000568, 2.071067811865474617 ) ) ;
#9948 = DIRECTION ( 'NONE',  ( 0.000000000000000000, 0.000000000000000000, 1.000000000000000000 ) ) ;
#9949 = CARTESIAN_POINT ( 'NONE',  ( -52.80376928212989185, -127.1250000013656205, -4.297418129356379346 ) ) ;
#9950 = VECTOR ( 'NONE', #1830, 1000.000000000000000 ) ;
#9951 = CARTESIAN_POINT ( 'NONE',  ( 4.458734124999999437, -12.06249999863440081, -5.460374474430324690E-16 ) ) ;
#9952 = AXIS2_PLACEMENT_3D ( 'NONE', #26448, #46069, #35153 ) ;
#9953 = CARTESIAN_POINT ( 'NONE',  ( -4.458734124999998549, -44.47916666530106511, 2.574251347313722516 ) ) ;
#9954 = CARTESIAN_POINT ( 'NONE',  ( 0.000000000000000000, -120.0000000000000000, 5.000000000000000000 ) ) ;
#9955 = CARTESIAN_POINT ( 'NONE',  ( 3.152801135295366208, -146.5625000013655779, 3.152801135295367985 ) ) ;
#9956 = CARTESIAN_POINT ( 'NONE',  ( 4.458734124999999437, -88.06249999863439371, -5.460374474430324690E-16 ) ) ;
#9957 = CYLINDRICAL_SURFACE ( 'NONE', #23514, 5.000000000000000000 ) ;
#9958 =( BOUNDED_CURVE ( )  B_SPLINE_CURVE ( 2, ( #39115, #10173, #44579, #54879, #34942, #54562, #39744, #30421, #43934 ),
 .UNSPECIFIED., .F., .F. ) 
 B_SPLINE_CURVE_WITH_KNOTS ( ( 3, 2, 2, 2, 3 ),
 ( 0.8017857142857143238, 0.8023809523809524169, 0.8035714285714286031, 0.8047619047619047894, 0.8053571428571428825 ),
 .UNSPECIFIED. ) 
 CURVE ( )  GEOMETRIC_REPRESENTATION_ITEM ( )  RATIONAL_B_SPLINE_CURVE ( ( 0.9330127018922194093, 0.9330127018922194093, 1.000000000000000000, 0.8660254037844387076, 1.000000000000000000, 0.8660254037844387076, 1.000000000000000000, 0.9330127018922194093, 0.9330127018922194093 ) ) 
 REPRESENTATION_ITEM ( '' )  );
#9959 = ORIENTED_EDGE ( 'NONE', *, *, #27519, .F. ) ;
#9960 = EDGE_CURVE ( 'NONE', #17569, #16469, #4518, .T. ) ;
#9961 = CARTESIAN_POINT ( 'NONE',  ( 0.000000000000000000, 15.00000000000000000, 0.000000000000000000 ) ) ;
#9962 = CARTESIAN_POINT ( 'NONE',  ( 4.330127018922258486, 45.00000000000000000, 7.499999999999910294 ) ) ;
#9963 = CARTESIAN_POINT ( 'NONE',  ( -50.18089887299979068, -148.8125000027312126, 2.462841084822635640 ) ) ;
#9964 = EDGE_CURVE ( 'NONE', #6403, #57220, #30571, .T. ) ;
#9965 = DIRECTION ( 'NONE',  ( 0.000000000000000000, 0.000000000000000000, 1.000000000000000000 ) ) ;
#9966 = ORIENTED_EDGE ( 'NONE', *, *, #23259, .T. ) ;
#9967 = CARTESIAN_POINT ( 'NONE',  ( -2.229367062500000163, 2.520833334698928230, -3.861377020970580443 ) ) ;
#9968 = EDGE_CURVE ( 'NONE', #24283, #19422, #35343, .T. ) ;
#9969 = CARTESIAN_POINT ( 'NONE',  ( 0.000000000000000000, -170.0000000000000000, 0.000000000000000000 ) ) ;
#9970 = CARTESIAN_POINT ( 'NONE',  ( 4.458734125000001214, -15.14583333196773651, 2.574251347313718519 ) ) ;
#9971 = CARTESIAN_POINT ( 'NONE',  ( 0.000000000000000000, -120.0000000000000000, 0.000000000000000000 ) ) ;
#9972 = CARTESIAN_POINT ( 'NONE',  ( 4.458734124999999437, -2.812499998634407472, -5.460374474430324690E-16 ) ) ;
#9973 = CARTESIAN_POINT ( 'NONE',  ( 1.339745962155612702, -73.16965819600734733, -5.000000000000000000 ) ) ;
#9974 = CARTESIAN_POINT ( 'NONE',  ( -3.152801135295367096, -149.0625000013655779, -3.152801135295367541 ) ) ;
#9975 = CARTESIAN_POINT ( 'NONE',  ( -3.152548672688508926E-16, 22.18750000136559564, -5.148502694627439702 ) ) ;
#9976 = ORIENTED_EDGE ( 'NONE', *, *, #20106, .T. ) ;
#9977 = CARTESIAN_POINT ( 'NONE',  ( 2.229367062499998831, -95.64583333196773651, -3.861377020970580887 ) ) ;
#9978 = CARTESIAN_POINT ( 'NONE',  ( -6.972266317189433020E-16, -47.24999999999999289, -5.000000000000000000 ) ) ;
#9979 = CARTESIAN_POINT ( 'NONE',  ( -5.000000000000000000, -103.8749999972688158, 0.000000000000000000 ) ) ;
#9980 = CARTESIAN_POINT ( 'NONE',  ( 4.458734125000001214, -12.89583333196774184, 2.574251347313718519 ) ) ;
#9981 = CARTESIAN_POINT ( 'NONE',  ( -1.339745962155613812, -85.08034179853028434, -5.000000000000000000 ) ) ;
#9982 = CARTESIAN_POINT ( 'NONE',  ( -2.500000000000000444, -13.16666666666666607, -4.330127018922193649 ) ) ;
#9983 = CARTESIAN_POINT ( 'NONE',  ( -54.64476657466781973, -152.8125000013656063, -4.444560631937228834 ) ) ;
#9984 = CARTESIAN_POINT ( 'NONE',  ( -4.999999999999999112, -39.79166666393547303, 2.886751345948131764 ) ) ;
#9985 = CARTESIAN_POINT ( 'NONE',  ( -7.703920929261744099, 4.447860822324859242, -7.917989418073275942 ) ) ;
#9986 = CARTESIAN_POINT ( 'NONE',  ( 4.458734125000000326, 12.10416666803226171, 2.574251347313718519 ) ) ;
#9987 = CARTESIAN_POINT ( 'NONE',  ( -2.500000000000000444, -72.16666666666667140, -4.330127018922193649 ) ) ;
#9988 = EDGE_LOOP ( 'NONE', ( #43197, #26517, #28393, #52012 ) ) ;
#9989 = CARTESIAN_POINT ( 'NONE',  ( 4.458734125000000326, 17.10416666803225993, 2.574251347313718519 ) ) ;
#9990 = CARTESIAN_POINT ( 'NONE',  ( 2.229367062500001939, -61.97916666530106511, 3.861377020970579999 ) ) ;
#9991 = ORIENTED_EDGE ( 'NONE', *, *, #26810, .F. ) ;
#9992 = CARTESIAN_POINT ( 'NONE',  ( 4.458734124999998549, -7.979166665301073991, -2.574251347313721627 ) ) ;
#9993 = CARTESIAN_POINT ( 'NONE',  ( 5.000000000000000000, -109.2916666639354730, -2.886751345948130876 ) ) ;
#9994 = CARTESIAN_POINT ( 'NONE',  ( -4.999999999999999112, 4.083333333333334814, 2.886751345948131764 ) ) ;
#9995 = CARTESIAN_POINT ( 'NONE',  ( 1.846868145590735200, -167.2500000013655779, -4.458734125000000326 ) ) ;
#9996 = CARTESIAN_POINT ( 'NONE',  ( -6.972266317189433020E-16, -21.12499999726881228, -5.000000000000000000 ) ) ;
#9997 = CARTESIAN_POINT ( 'NONE',  ( -4.458734124999999437, -51.39583333196772941, -2.574251347313719407 ) ) ;
#9998 = CARTESIAN_POINT ( 'NONE',  ( 5.000000000000000000, -90.37499999726880162, -6.123233995736766282E-16 ) ) ;
#9999 = AXIS2_PLACEMENT_3D ( 'NONE', #49623, #16165, #40290 ) ;
#10000 = CARTESIAN_POINT ( 'NONE',  ( -3.152548672688508926E-16, -32.56249999863440792, -5.148502694627439702 ) ) ;
#10001 = CARTESIAN_POINT ( 'NONE',  ( -2.499999999999996447, -76.83333333333334281, 4.330127018922195425 ) ) ;
#10002 = CARTESIAN_POINT ( 'NONE',  ( 1.975475456537005874E-15, 11.24999999999999822, 5.000000000000000000 ) ) ;
#10003 = DIRECTION ( 'NONE',  ( 0.5000000000000069944, 0.000000000000000000, 0.8660254037844345998 ) ) ;
#10004 = AXIS2_PLACEMENT_3D ( 'NONE', #5632, #44858, #821 ) ;
#10005 = CARTESIAN_POINT ( 'NONE',  ( 4.458734124999997661, -151.7500000013656063, 1.846868145590737864 ) ) ;
#10006 = CARTESIAN_POINT ( 'NONE',  ( -2.499999999999996447, -44.83333333333333570, 4.330127018922195425 ) ) ;
#10007 = CARTESIAN_POINT ( 'NONE',  ( -6.972266317189433020E-16, -6.124999997268813168, -5.000000000000000000 ) ) ;
#10008 = CARTESIAN_POINT ( 'NONE',  ( -59.65692920852630010, -135.0000000000000284, 1.510532900655110256 ) ) ;
#10009 = VERTEX_POINT ( 'NONE', #30251 ) ;
#10010 = CARTESIAN_POINT ( 'NONE',  ( 4.458734125000001214, -100.8958333319677365, 2.574251347313718519 ) ) ;
#10011 = CARTESIAN_POINT ( 'NONE',  ( -2.229367062500000163, 5.270833334698927786, -3.861377020970580443 ) ) ;
#10012 =( BOUNDED_CURVE ( )  B_SPLINE_CURVE ( 2, ( #27715, #47343, #22911, #18060, #62141, #8426, #3292, #25894, #42819 ),
 .UNSPECIFIED., .F., .F. ) 
 B_SPLINE_CURVE_WITH_KNOTS ( ( 3, 2, 2, 2, 3 ),
 ( 0.1053571428571428575, 0.1059523809523809507, 0.1071428571428571369, 0.1083333333333333370, 0.1089285714285714302 ),
 .UNSPECIFIED. ) 
 CURVE ( )  GEOMETRIC_REPRESENTATION_ITEM ( )  RATIONAL_B_SPLINE_CURVE ( ( 0.9330127018922194093, 0.9330127018922194093, 1.000000000000000000, 0.8660254037844387076, 1.000000000000000000, 0.8660254037844387076, 1.000000000000000000, 0.9330127018922194093, 0.9330127018922194093 ) ) 
 REPRESENTATION_ITEM ( '' )  );
#10013 = LINE ( 'NONE', #53446, #57633 ) ;
#10014 = CARTESIAN_POINT ( 'NONE',  ( -2.500000000000000444, -0.1666666666666656582, -4.330127018922193649 ) ) ;
#10015 = CARTESIAN_POINT ( 'NONE',  ( 2.229367062500001939, -67.97916666530106511, 3.861377020970579999 ) ) ;
#10016 = ADVANCED_FACE ( 'NONE', ( #19653 ), #55032, .F. ) ;
#10017 = DIRECTION ( 'NONE',  ( 1.000000000000000000, 0.000000000000000000, 0.000000000000000000 ) ) ;
#10018 = CARTESIAN_POINT ( 'NONE',  ( -5.000000000000000000, 0.1250000027311869155, 0.000000000000000000 ) ) ;
#10020 = ORIENTED_EDGE ( 'NONE', *, *, #22761, .F. ) ;
#10019 = CARTESIAN_POINT ( 'NONE',  ( -4.458734124999999437, -32.39583333196773651, -2.574251347313719407 ) ) ;
#10021 = FACE_OUTER_BOUND ( 'NONE', #20874, .T. ) ;
#10022 = CARTESIAN_POINT ( 'NONE',  ( -5.000000000000000000, -47.87499999726880873, 0.000000000000000000 ) ) ;
#10023 = CARTESIAN_POINT ( 'NONE',  ( 1.975475456537005874E-15, -50.62499999726881583, 5.000000000000000000 ) ) ;
#10024 = CARTESIAN_POINT ( 'NONE',  ( 5.000000000000000000, -51.41666666666666430, -2.886751345948129988 ) ) ;
#10026 = CARTESIAN_POINT ( 'NONE',  ( -4.458734124999998549, -27.47916666530106866, 2.574251347313722516 ) ) ;
#10025 = CARTESIAN_POINT ( 'NONE',  ( -6.972266317189433020E-16, -17.12499999726881583, -5.000000000000000000 ) ) ;
#10027 = CARTESIAN_POINT ( 'NONE',  ( -6.972266317189433020E-16, -64.12499999726880162, -5.000000000000000000 ) ) ;
#10028 = CARTESIAN_POINT ( 'NONE',  ( 4.458734124999998549, -70.72916666530107932, -2.574251347313721627 ) ) ;
#10029 = CARTESIAN_POINT ( 'NONE',  ( 1.846868145590736310, -142.8750000013656063, 4.458734124999999437 ) ) ;
#10030 = CARTESIAN_POINT ( 'NONE',  ( -2.229367062500000163, -83.47916666530106511, -3.861377020970580443 ) ) ;
#10031 = CARTESIAN_POINT ( 'NONE',  ( -55.35523342533222291, -140.5625000013656063, 4.444560631937231499 ) ) ;
#10032 = CARTESIAN_POINT ( 'NONE',  ( 4.458734125000001214, -28.14583333196774007, 2.574251347313718519 ) ) ;
#10033 = CARTESIAN_POINT ( 'NONE',  ( 2.500000000000002220, -70.54166666393547303, 4.330127018922192761 ) ) ;
#10034 = ORIENTED_EDGE ( 'NONE', *, *, #4425, .F. ) ;
#10035 = FACE_OUTER_BOUND ( 'NONE', #31440, .T. ) ;
#10036 = ORIENTED_EDGE ( 'NONE', *, *, #25554, .T. ) ;
#10037 = CARTESIAN_POINT ( 'NONE',  ( -4.458734124999999437, -71.56249999863439371, 0.000000000000000000 ) ) ;
#10038 = CARTESIAN_POINT ( 'NONE',  ( -1.339745962155613146, 29.20534180126147916, 5.000000000000000000 ) ) ;
#10039 = ORIENTED_EDGE ( 'NONE', *, *, #7515, .T. ) ;
#10040 = CARTESIAN_POINT ( 'NONE',  ( -6.972266317189433020E-16, -32.12499999726880873, -5.000000000000000000 ) ) ;
#10041 = AXIS2_PLACEMENT_3D ( 'NONE', #28727, #18140, #62848 ) ;
#10042 = CARTESIAN_POINT ( 'NONE',  ( 1.975475456537005874E-15, -75.62499999726880162, 5.000000000000000000 ) ) ;
#10043 = CARTESIAN_POINT ( 'NONE',  ( 4.458734124999998549, -56.97916666530107932, -2.574251347313721627 ) ) ;
#10044 = VECTOR ( 'NONE', #38949, 1000.000000000000000 ) ;
#10045 = CARTESIAN_POINT ( 'NONE',  ( 4.458734124999999437, -2.062499998634406584, -5.460374474430324690E-16 ) ) ;
#10046 = ORIENTED_EDGE ( 'NONE', *, *, #17824, .F. ) ;
#10047 = DIRECTION ( 'NONE',  ( -0.000000000000000000, 1.000000000000000000, -0.000000000000000000 ) ) ;
#10048 = CARTESIAN_POINT ( 'NONE',  ( -5.000000000000000000, -45.00000000000000000, 0.000000000000000000 ) ) ;
#10049 = CARTESIAN_POINT ( 'NONE',  ( 2.229367062500001939, 14.02083333469892779, 3.861377020970579999 ) ) ;
#10050 = CARTESIAN_POINT ( 'NONE',  ( -51.60603307380591787, -141.9375000013656063, -2.891590998281053704 ) ) ;
#10051 = CARTESIAN_POINT ( 'NONE',  ( 1.339745962155612702, -32.29465819873852439, -5.000000000000000000 ) ) ;
#10052 = CARTESIAN_POINT ( 'NONE',  ( -4.458734125000000326, -163.8750000013656063, 1.846868145590734089 ) ) ;
#10053 = ORIENTED_EDGE ( 'NONE', *, *, #20126, .F. ) ;
#10054 = CARTESIAN_POINT ( 'NONE',  ( -2.229367062499996610, -80.14583333196773651, 3.861377020970582219 ) ) ;
#10055 = CARTESIAN_POINT ( 'NONE',  ( 1.975475456537005874E-15, -69.62499999726880162, 5.000000000000000000 ) ) ;
#10056 = CARTESIAN_POINT ( 'NONE',  ( 2.229367062500001939, 0.02083333469892964529, 3.861377020970579999 ) ) ;
#10057 = CARTESIAN_POINT ( 'NONE',  ( -2.500000000000000444, -83.16666666666667140, -4.330127018922193649 ) ) ;
#10058 = CARTESIAN_POINT ( 'NONE',  ( -5.000000000000000000, -42.95833333060214443, -2.886751345948128211 ) ) ;
#10059 = CARTESIAN_POINT ( 'NONE',  ( 4.458734124999999437, -66.06249999863440792, -5.460374474430324690E-16 ) ) ;
#10060 = CARTESIAN_POINT ( 'NONE',  ( 1.060575238724906964E-15, -24.62499999726881228, 5.773502691896257311 ) ) ;
#10061 = CARTESIAN_POINT ( 'NONE',  ( -6.972266317189433020E-16, -21.24999999999999289, -5.000000000000000000 ) ) ;
#10062 = CARTESIAN_POINT ( 'NONE',  ( -4.458734124999999437, 27.60416666803226349, -2.574251347313719407 ) ) ;
#10063 = CARTESIAN_POINT ( 'NONE',  ( 1.339745962155615144, -49.70534180126148271, 4.999999999999999112 ) ) ;
#10064 = CARTESIAN_POINT ( 'NONE',  ( 5.000000000000000888, -43.45833333060214443, 2.886751345948126879 ) ) ;
#10065 = CARTESIAN_POINT ( 'NONE',  ( -3.152548672688508926E-16, -44.56249999863440081, -5.148502694627439702 ) ) ;
#10066 = CARTESIAN_POINT ( 'NONE',  ( 2.229367062500001939, -32.22916666530106511, 3.861377020970579999 ) ) ;
#10067 = CARTESIAN_POINT ( 'NONE',  ( 4.458734124999998549, 6.020833334698928674, -2.574251347313721627 ) ) ;
#10068 = CARTESIAN_POINT ( 'NONE',  ( -58.24261429053147765, -150.2500000000000284, -3.805975901505573855 ) ) ;
#10069 = CARTESIAN_POINT ( 'NONE',  ( -5.000000000000000000, 19.99999999999999645, 0.000000000000000000 ) ) ;
#10070 = CARTESIAN_POINT ( 'NONE',  ( -5.000000000000000888, -149.5625000027311842, 2.071067811865474617 ) ) ;
#10071 = CARTESIAN_POINT ( 'NONE',  ( -50.18089887299979068, -154.6874999999999716, 2.462841084822631199 ) ) ;
#10072 = EDGE_CURVE ( 'NONE', #31090, #45744, #17693, .T. ) ;
#10073 = CARTESIAN_POINT ( 'NONE',  ( -4.458734124999999437, -37.31249999863440792, 0.000000000000000000 ) ) ;
#10074 = CARTESIAN_POINT ( 'NONE',  ( 5.000000000000000000, -75.37499999726880162, -6.123233995736766282E-16 ) ) ;
#10075 = CARTESIAN_POINT ( 'NONE',  ( -50.40829686548195099, -144.2500000013656063, -1.485763867205728284 ) ) ;
#10076 = CARTESIAN_POINT ( 'NONE',  ( 2.071067811865475505, -143.8125000000000000, -5.000000000000000888 ) ) ;
#10077 = CARTESIAN_POINT ( 'NONE',  ( -5.007715329123872641E-16, -8.660254037844399733, -7.422398894150038728 ) ) ;
#10078 = CARTESIAN_POINT ( 'NONE',  ( 2.229367062500001939, -80.22916666530106511, 3.861377020970579999 ) ) ;
#10079 = CARTESIAN_POINT ( 'NONE',  ( 4.458734124999997661, -163.7500000013655779, 1.846868145590737864 ) ) ;
#10080 = CARTESIAN_POINT ( 'NONE',  ( -4.458734124999999437, -37.39583333196773651, -2.574251347313719407 ) ) ;
#10081 = DIRECTION ( 'NONE',  ( 0.000000000000000000, 0.000000000000000000, 1.000000000000000000 ) ) ;
#10082 = CARTESIAN_POINT ( 'NONE',  ( -6.972266317189433020E-16, -18.25000000000000000, -5.000000000000000000 ) ) ;
#10083 = CARTESIAN_POINT ( 'NONE',  ( -4.999999999999999112, -22.91666666666666785, 2.886751345948131764 ) ) ;
#10084 = CARTESIAN_POINT ( 'NONE',  ( -3.152801135295367096, -142.0625000013655779, -3.152801135295367541 ) ) ;
#10085 = VERTEX_POINT ( 'NONE', #50199 ) ;
#10086 = CARTESIAN_POINT ( 'NONE',  ( -4.458734124999999437, 29.43750000136559208, 0.000000000000000000 ) ) ;
#10087 = ORIENTED_EDGE ( 'NONE', *, *, #24861, .T. ) ;
#10088 = CARTESIAN_POINT ( 'NONE',  ( 9.457646018065525792E-16, -63.31249999863440792, 5.148502694627439702 ) ) ;
#10089 = VECTOR ( 'NONE', #11206, 1000.000000000000000 ) ;
#10090 = CARTESIAN_POINT ( 'NONE',  ( -4.999999999999999112, 20.20833333606451987, 2.886751345948131764 ) ) ;
#10091 = DIRECTION ( 'NONE',  ( -0.000000000000000000, 1.000000000000000000, -0.000000000000000000 ) ) ;
#10092 = CARTESIAN_POINT ( 'NONE',  ( 1.060575238724906964E-15, 11.25000000000000000, 5.773502691896257311 ) ) ;
#10093 = CONICAL_SURFACE ( 'NONE', #3909, 10.39117206796836079, 1.221730476396047926 ) ;
#10094 =( BOUNDED_CURVE ( )  B_SPLINE_CURVE ( 2, ( #11173, #50095, #21150, #11494, #25972, #60403, #54607, #40438, #45588 ),
 .UNSPECIFIED., .F., .F. ) 
 B_SPLINE_CURVE_WITH_KNOTS ( ( 3, 2, 2, 2, 3 ),
 ( 0.2553571428571428381, 0.2559523809523809312, 0.2571428571428571175, 0.2583333333333333592, 0.2589285714285714524 ),
 .UNSPECIFIED. ) 
 CURVE ( )  GEOMETRIC_REPRESENTATION_ITEM ( )  RATIONAL_B_SPLINE_CURVE ( ( 0.9330127018922194093, 0.9330127018922194093, 1.000000000000000000, 0.8660254037844387076, 1.000000000000000000, 0.8660254037844387076, 1.000000000000000000, 0.9330127018922194093, 0.9330127018922194093 ) ) 
 REPRESENTATION_ITEM ( '' )  );
#10095 = CARTESIAN_POINT ( 'NONE',  ( -2.229367062500000163, -48.47916666530106511, -3.861377020970580443 ) ) ;
#10096 = CARTESIAN_POINT ( 'NONE',  ( -4.458734124999999437, -6.395833331967740953, -2.574251347313719407 ) ) ;
#10097 = DIRECTION ( 'NONE',  ( 0.000000000000000000, 0.000000000000000000, 1.000000000000000000 ) ) ;
#10098 = CARTESIAN_POINT ( 'NONE',  ( -2.499999999999996447, -40.70833333060214443, 4.330127018922195425 ) ) ;
#10099 = CARTESIAN_POINT ( 'NONE',  ( 5.000000000000000888, -91.45833333060214443, 2.886751345948126879 ) ) ;
#10100 = CARTESIAN_POINT ( 'NONE',  ( 5.000000000000000000, -74.50000000000000000, -6.123233995736766282E-16 ) ) ;
#10102 = CARTESIAN_POINT ( 'NONE',  ( -2.229367062500000163, -20.47916666530107221, -3.861377020970580443 ) ) ;
#10101 = CARTESIAN_POINT ( 'NONE',  ( 5.000000000000000000, 21.70833333606451987, -2.886751345948130876 ) ) ;
#10103 = CARTESIAN_POINT ( 'NONE',  ( -2.500000000000000444, -72.04166666393548724, -4.330127018922193649 ) ) ;
#10104 = CARTESIAN_POINT ( 'NONE',  ( 4.458734124999998549, -53.72916666530106511, -2.574251347313721627 ) ) ;
#10105 = CARTESIAN_POINT ( 'NONE',  ( -8.190561711645485556E-16, -155.9375000013655779, 4.458734124999999437 ) ) ;
#10106 = AXIS2_PLACEMENT_3D ( 'NONE', #14962, #9195, #38764 ) ;
#10107 =( BOUNDED_CURVE ( )  B_SPLINE_CURVE ( 2, ( #20319, #1996, #50220, #25457, #5847, #30274, #35754, #31233, #35122 ),
 .UNSPECIFIED., .F., .F. ) 
 B_SPLINE_CURVE_WITH_KNOTS ( ( 3, 2, 2, 2, 3 ),
 ( 0.5553571428571428825, 0.5559523809523809756, 0.5571428571428571619, 0.5583333333333333481, 0.5589285714285714413 ),
 .UNSPECIFIED. ) 
 CURVE ( )  GEOMETRIC_REPRESENTATION_ITEM ( )  RATIONAL_B_SPLINE_CURVE ( ( 0.9330127018922194093, 0.9330127018922194093, 1.000000000000000000, 0.8660254037844387076, 1.000000000000000000, 0.8660254037844387076, 1.000000000000000000, 0.9330127018922194093, 0.9330127018922194093 ) ) 
 REPRESENTATION_ITEM ( '' )  );
#10108 = CARTESIAN_POINT ( 'NONE',  ( -2.500000000000000444, -58.04166666393548013, -4.330127018922193649 ) ) ;
#10109 = ORIENTED_EDGE ( 'NONE', *, *, #46867, .F. ) ;
#10110 = CARTESIAN_POINT ( 'NONE',  ( 0.000000000000000000, 0.000000000000000000, -0.5776712190230133270 ) ) ;
#10111 = CARTESIAN_POINT ( 'NONE',  ( -4.458734124999998549, 5.520833334698927786, 2.574251347313722516 ) ) ;
#10112 = ORIENTED_EDGE ( 'NONE', *, *, #9421, .T. ) ;
#10114 = CARTESIAN_POINT ( 'NONE',  ( -9.184850993605147944E-16, -160.3750000027311842, 5.000000000000000000 ) ) ;
#10113 = DIRECTION ( 'NONE',  ( 0.000000000000000000, 0.000000000000000000, 1.000000000000000000 ) ) ;
#10115 = CARTESIAN_POINT ( 'NONE',  ( -4.458734124999999437, -157.9375000013655779, -5.460374474430324690E-16 ) ) ;
#10116 = ORIENTED_EDGE ( 'NONE', *, *, #16497, .T. ) ;
#10117 = DIRECTION ( 'NONE',  ( 0.000000000000000000, 0.000000000000000000, 1.000000000000000000 ) ) ;
#10118 = CARTESIAN_POINT ( 'NONE',  ( -56.66612745406270335, -134.3125000000000284, -5.149110718188516067 ) ) ;
#10119 = CARTESIAN_POINT ( 'NONE',  ( 3.535533905932738197, -161.0000000027312126, -3.535533905932738197 ) ) ;
#10120 = CARTESIAN_POINT ( 'NONE',  ( 2.229367062500001939, -44.22916666530106511, 3.861377020970579999 ) ) ;
#10121 = ORIENTED_EDGE ( 'NONE', *, *, #20868, .T. ) ;
#10122 = CARTESIAN_POINT ( 'NONE',  ( 5.000000000000000888, -103.4583333306021444, 2.886751345948126879 ) ) ;
#10123 = CARTESIAN_POINT ( 'NONE',  ( -4.458734124999999437, 17.68750000136559208, 0.000000000000000000 ) ) ;
#10124 = FACE_OUTER_BOUND ( 'NONE', #16131, .T. ) ;
#10125 = ORIENTED_EDGE ( 'NONE', *, *, #7139, .T. ) ;
#10126 = CARTESIAN_POINT ( 'NONE',  ( 2.229367062499998831, -89.89583333196773651, -3.861377020970580887 ) ) ;
#10127 = CARTESIAN_POINT ( 'NONE',  ( -54.64476657466781973, -151.8125000013656063, -4.444560631937228834 ) ) ;
#10128 = CARTESIAN_POINT ( 'NONE',  ( 5.000000000000000000, 12.62500000273118417, -6.123233995736766282E-16 ) ) ;
#10129 = LINE ( 'NONE', #180, #26454 ) ;
#10130 = VECTOR ( 'NONE', #30271, 1000.000000000000000 ) ;
#10131 = CARTESIAN_POINT ( 'NONE',  ( -2.500000000000000444, -103.1666666666666572, -4.330127018922193649 ) ) ;
#10132 = CARTESIAN_POINT ( 'NONE',  ( -2.229367062499996610, -65.14583333196773651, 3.861377020970582219 ) ) ;
#10133 = DIRECTION ( 'NONE',  ( -0.000000000000000000, 1.000000000000000000, -0.000000000000000000 ) ) ;
#10134 = CARTESIAN_POINT ( 'NONE',  ( -2.229367062499996610, 17.85416666803225993, 3.861377020970582219 ) ) ;
#10135 = VECTOR ( 'NONE', #44199, 1000.000000000000000 ) ;
#10136 = CARTESIAN_POINT ( 'NONE',  ( -6.972266317189433020E-16, -79.12499999726881583, -5.000000000000000000 ) ) ;
#10137 = CARTESIAN_POINT ( 'NONE',  ( -4.458734124999999437, -47.64583333196775072, -2.574251347313719407 ) ) ;
#10138 = CARTESIAN_POINT ( 'NONE',  ( -5.000000000000000000, -11.95833333060214976, -2.886751345948128211 ) ) ;
#10139 = CARTESIAN_POINT ( 'NONE',  ( 5.000000000000000000, -25.29166666393547658, -2.886751345948130876 ) ) ;
#10140 = FACE_OUTER_BOUND ( 'NONE', #36728, .T. ) ;
#10141 = CARTESIAN_POINT ( 'NONE',  ( 2.229367062499998831, -107.6458333319677365, -3.861377020970580887 ) ) ;
#10142 = CARTESIAN_POINT ( 'NONE',  ( -4.458734124999999437, -16.64583333196773651, -2.574251347313719407 ) ) ;
#10143 = ORIENTED_EDGE ( 'NONE', *, *, #5626, .T. ) ;
#10144 = CARTESIAN_POINT ( 'NONE',  ( -5.000000000000000888, -143.6875000027312126, -2.071067811865475949 ) ) ;
#10145 = CARTESIAN_POINT ( 'NONE',  ( 9.457646018065525792E-16, -100.0624999986344221, 5.148502694627439702 ) ) ;
#10146 = CARTESIAN_POINT ( 'NONE',  ( -9.184850993605147944E-16, -162.3750000027311842, 5.000000000000000000 ) ) ;
#10147 = CARTESIAN_POINT ( 'NONE',  ( -2.229367062500000163, -95.72916666530107932, -3.861377020970580443 ) ) ;
#10148 = EDGE_CURVE ( 'NONE', #8617, #45777, #59220, .T. ) ;
#10149 = CARTESIAN_POINT ( 'NONE',  ( 3.061616997868383141E-16, -158.7500000000000000, -5.000000000000000000 ) ) ;
#10150 = CARTESIAN_POINT ( 'NONE',  ( 5.000000000000000888, -58.45833333060214443, 2.886751345948126879 ) ) ;
#10151 = CARTESIAN_POINT ( 'NONE',  ( -6.972266317189433020E-16, -15.12499999726881050, -5.000000000000000000 ) ) ;
#10152 = AXIS2_PLACEMENT_3D ( 'NONE', #14982, #10160, #45849 ) ;
#10153 = CARTESIAN_POINT ( 'NONE',  ( -58.39396692619412477, -127.4375000013656063, 2.891590998281057701 ) ) ;
#10154 = CARTESIAN_POINT ( 'NONE',  ( -50.40829686548195099, -146.0000000013656347, -1.485763867205728284 ) ) ;
#10155 = CARTESIAN_POINT ( 'NONE',  ( 4.458734124999999437, -18.81249999863440792, -5.460374474430324690E-16 ) ) ;
#10156 = CARTESIAN_POINT ( 'NONE',  ( 4.458734124999999437, 6.937500001365594748, -5.460374474430324690E-16 ) ) ;
#10157 = CARTESIAN_POINT ( 'NONE',  ( -3.152548672688508926E-16, -56.81249999863440792, -5.148502694627439702 ) ) ;
#10158 = CARTESIAN_POINT ( 'NONE',  ( -6.972266317189433020E-16, -54.24999999999999289, -5.000000000000000000 ) ) ;
#10159 = CARTESIAN_POINT ( 'NONE',  ( -4.458734124999999437, -20.39583333196774362, -2.574251347313719407 ) ) ;
#10160 = DIRECTION ( 'NONE',  ( -0.000000000000000000, 1.000000000000000000, -0.000000000000000000 ) ) ;
#10161 = CARTESIAN_POINT ( 'NONE',  ( 3.061616997868383141E-16, -155.7500000000000000, -5.000000000000000000 ) ) ;
#10162 = CARTESIAN_POINT ( 'NONE',  ( 1.060575238724906964E-15, -4.749999999999997335, 5.773502691896257311 ) ) ;
#10163 = EDGE_LOOP ( 'NONE', ( #45809, #7119, #61825, #20977 ) ) ;
#10164 = CARTESIAN_POINT ( 'NONE',  ( 2.229367062500001939, -45.22916666530106511, 3.861377020970579999 ) ) ;
#10165 =( BOUNDED_CURVE ( )  B_SPLINE_CURVE ( 2, ( #28658, #44075, #53421, #48274, #9667, #4230, #23845, #24156, #53734 ),
 .UNSPECIFIED., .F., .F. ) 
 B_SPLINE_CURVE_WITH_KNOTS ( ( 3, 2, 2, 2, 3 ),
 ( 0.5374999999999999778, 0.5380952380952380709, 0.5392857142857142572, 0.5404761904761904434, 0.5410714285714285365 ),
 .UNSPECIFIED. ) 
 CURVE ( )  GEOMETRIC_REPRESENTATION_ITEM ( )  RATIONAL_B_SPLINE_CURVE ( ( 0.9330127018922194093, 0.9330127018922194093, 1.000000000000000000, 0.8660254037844387076, 1.000000000000000000, 0.8660254037844387076, 1.000000000000000000, 0.9330127018922194093, 0.9330127018922194093 ) ) 
 REPRESENTATION_ITEM ( '' )  );
#10166 = FACE_OUTER_BOUND ( 'NONE', #48771, .T. ) ;
#10167 = CARTESIAN_POINT ( 'NONE',  ( -6.972266317189433020E-16, -92.12499999726878741, -5.000000000000000000 ) ) ;
#10168 = CARTESIAN_POINT ( 'NONE',  ( -1.339745962155613146, 27.33034180399266333, 5.000000000000000000 ) ) ;
#10169 = CARTESIAN_POINT ( 'NONE',  ( -3.152548672688508926E-16, -92.56249999863439371, -5.148502694627439702 ) ) ;
#10170 = CARTESIAN_POINT ( 'NONE',  ( 4.458734124999998549, 18.02083333469892779, -2.574251347313721627 ) ) ;
#10171 = CARTESIAN_POINT ( 'NONE',  ( 2.229367062500001939, 11.02083333469892956, 3.861377020970579999 ) ) ;
#10172 = EDGE_CURVE ( 'NONE', #23665, #57819, #14822, .T. ) ;
#10173 = CARTESIAN_POINT ( 'NONE',  ( 1.339745962155612702, -82.29465819873851729, -5.000000000000000000 ) ) ;
#10174 = EDGE_CURVE ( 'NONE', #483, #44925, #29288, .T. ) ;
#10175 = CARTESIAN_POINT ( 'NONE',  ( 1.975475456537005874E-15, -29.62499999726881228, 5.000000000000000000 ) ) ;
#10176 = CARTESIAN_POINT ( 'NONE',  ( -4.458734124999999437, -89.64583333196773651, -2.574251347313719407 ) ) ;
#10177 = CARTESIAN_POINT ( 'NONE',  ( 9.457646018065525792E-16, 20.68750000136559564, 5.148502694627439702 ) ) ;
#10178 = CARTESIAN_POINT ( 'NONE',  ( -2.500000000000000444, -76.16666666666665719, -4.330127018922193649 ) ) ;
#10179 = CARTESIAN_POINT ( 'NONE',  ( -3.535250795749689387E-16, 8.875000002731184168, -5.773502691896257311 ) ) ;
#10180 = ORIENTED_EDGE ( 'NONE', *, *, #47925, .T. ) ;
#10181 = CARTESIAN_POINT ( 'NONE',  ( -5.000000000000000000, -6.958333330602150646, -2.886751345948128211 ) ) ;
#10182 = EDGE_LOOP ( 'NONE', ( #25107, #46829, #33374, #28603 ) ) ;
#10184 = CARTESIAN_POINT ( 'NONE',  ( -2.499999999999996447, -31.83333333333333215, 4.330127018922195425 ) ) ;
#10183 = CARTESIAN_POINT ( 'NONE',  ( 1.975475456537005874E-15, -54.62499999726880873, 5.000000000000000000 ) ) ;
#10185 = CARTESIAN_POINT ( 'NONE',  ( 2.229367062500001939, -35.97916666530107221, 3.861377020970579999 ) ) ;
#10186 = VECTOR ( 'NONE', #23588, 1000.000000000000000 ) ;
#10187 = EDGE_CURVE ( 'NONE', #42151, #45889, #53748, .T. ) ;
#10188 = CARTESIAN_POINT ( 'NONE',  ( 2.499999999999998668, -37.20833333060213732, -4.330127018922193649 ) ) ;
#10189 = VERTEX_POINT ( 'NONE', #15152 ) ;
#10190 = CARTESIAN_POINT ( 'NONE',  ( -55.35523342533222291, -147.5625000013656063, 4.444560631937231499 ) ) ;
#10191 = CARTESIAN_POINT ( 'NONE',  ( -2.229367062499996610, -14.14583333196774184, 3.861377020970582219 ) ) ;
#10193 = ORIENTED_EDGE ( 'NONE', *, *, #3416, .T. ) ;
#10192 = CARTESIAN_POINT ( 'NONE',  ( 2.229367062500001939, -12.22916666530107044, 3.861377020970579999 ) ) ;
#10194 = CARTESIAN_POINT ( 'NONE',  ( 5.000000000000000000, -84.41666666666667140, -2.886751345948129988 ) ) ;
#10195 = CARTESIAN_POINT ( 'NONE',  ( -3.152801135295367096, -167.0625000013656063, -3.152801135295367541 ) ) ;
#10196 = CARTESIAN_POINT ( 'NONE',  ( -4.458734124999999437, -63.56249999863440792, 0.000000000000000000 ) ) ;
#10197 = CARTESIAN_POINT ( 'NONE',  ( -3.535250795749689387E-16, -83.12499999726880162, -5.773502691896257311 ) ) ;
#10199 = ORIENTED_EDGE ( 'NONE', *, *, #22100, .T. ) ;
#10198 = CYLINDRICAL_SURFACE ( 'NONE', #54968, 5.000000000000000000 ) ;
#10200 = CARTESIAN_POINT ( 'NONE',  ( -59.81910112700025905, -147.1875000000000000, -2.462841084822630311 ) ) ;
#10201 = CARTESIAN_POINT ( 'NONE',  ( -2.229367062500000163, -26.72916666530106866, -3.861377020970580443 ) ) ;
#10202 = CARTESIAN_POINT ( 'NONE',  ( 1.975475456537005874E-15, -52.62499999726880873, 5.000000000000000000 ) ) ;
#10203 = ORIENTED_EDGE ( 'NONE', *, *, #39652, .T. ) ;
#10204 = CARTESIAN_POINT ( 'NONE',  ( 4.458734124999999437, -162.6875000013655779, 0.000000000000000000 ) ) ;
#10205 = EDGE_CURVE ( 'NONE', #16047, #41941, #29616, .T. ) ;
#10206 = CARTESIAN_POINT ( 'NONE',  ( -4.458734124999999437, -103.5624999986344079, 0.000000000000000000 ) ) ;
#10207 = CARTESIAN_POINT ( 'NONE',  ( 5.000000000000000888, -147.9375000000000000, -2.071067811865475505 ) ) ;
#10208 = VERTEX_POINT ( 'NONE', #34773 ) ;
#10209 = CARTESIAN_POINT ( 'NONE',  ( -59.59170313451810586, -145.7500000013656063, 1.485763867205729394 ) ) ;
#10210 = CARTESIAN_POINT ( 'NONE',  ( 2.229367062499998831, -72.89583333196773651, -3.861377020970580887 ) ) ;
#10211 = CARTESIAN_POINT ( 'NONE',  ( -49.85088928181150436, -139.6875000027312126, -1.666127454062680702 ) ) ;
#10212 = CARTESIAN_POINT ( 'NONE',  ( 2.229367062500001939, -45.97916666530106511, 3.861377020970579999 ) ) ;
#10213 = CARTESIAN_POINT ( 'NONE',  ( 1.846868145590735200, -146.5000000013656347, -4.458734124999999437 ) ) ;
#10214 = CYLINDRICAL_SURFACE ( 'NONE', #45604, 5.000000000000000000 ) ;
#10215 = CARTESIAN_POINT ( 'NONE',  ( -2.229367062500000163, -15.47916666530107399, -3.861377020970580443 ) ) ;
#10216 = CARTESIAN_POINT ( 'NONE',  ( -2.499999999999996447, -100.8333333333333286, 4.330127018922195425 ) ) ;
#10217 = ORIENTED_EDGE ( 'NONE', *, *, #24410, .T. ) ;
#10218 = CARTESIAN_POINT ( 'NONE',  ( 4.458734124999999437, -34.06249999863440792, -5.460374474430324690E-16 ) ) ;
#10219 = CARTESIAN_POINT ( 'NONE',  ( 5.000000000000000888, 5.541666669397854683, 2.886751345948126879 ) ) ;
#10220 = FACE_OUTER_BOUND ( 'NONE', #21430, .T. ) ;
#10221 = CARTESIAN_POINT ( 'NONE',  ( -51.60603307380591787, -131.9375000013656063, -2.891590998281053704 ) ) ;
#10222 = CARTESIAN_POINT ( 'NONE',  ( -2.229367062499996610, -72.39583333196773651, 3.861377020970582219 ) ) ;
#10223 = CARTESIAN_POINT ( 'NONE',  ( -6.972266317189433020E-16, -92.24999999999998579, -5.000000000000000000 ) ) ;
#10224 = CARTESIAN_POINT ( 'NONE',  ( 0.000000000000000000, -120.0000000000000000, 0.000000000000000000 ) ) ;
#10225 = FACE_OUTER_BOUND ( 'NONE', #39134, .T. ) ;
#10226 = CARTESIAN_POINT ( 'NONE',  ( 1.060575238724906964E-15, -68.74999999999998579, 5.773502691896257311 ) ) ;
#10227 = CARTESIAN_POINT ( 'NONE',  ( 4.458734124999998549, 4.020833334698926009, -2.574251347313721627 ) ) ;
#10228 = ORIENTED_EDGE ( 'NONE', *, *, #21593, .F. ) ;
#10229 = CARTESIAN_POINT ( 'NONE',  ( -6.972266317189433020E-16, -30.25000000000000000, -5.000000000000000000 ) ) ;
#10230 = CARTESIAN_POINT ( 'NONE',  ( 6.123233995736766282E-16, -120.0000000000000000, -5.000000000000000000 ) ) ;
#10232 = CARTESIAN_POINT ( 'NONE',  ( -3.152548672688508926E-16, -31.56249999863440436, -5.148502694627439702 ) ) ;
#10231 = CARTESIAN_POINT ( 'NONE',  ( 5.000000000000000000, -98.41666666666667140, -2.886751345948129988 ) ) ;
#10233 = CARTESIAN_POINT ( 'NONE',  ( -6.972266317189433020E-16, -16.12499999726881228, -5.000000000000000000 ) ) ;
#10234 = CARTESIAN_POINT ( 'NONE',  ( 9.457646018065525792E-16, -83.31249999863440792, 5.148502694627439702 ) ) ;
#10235 = EDGE_CURVE ( 'NONE', #45336, #50575, #6600, .T. ) ;
#10236 = CARTESIAN_POINT ( 'NONE',  ( -3.152548672688508926E-16, 17.18750000136559564, -5.148502694627439702 ) ) ;
#10237 = CARTESIAN_POINT ( 'NONE',  ( -5.000000000000000000, 27.00000000000000000, 0.000000000000000000 ) ) ;
#10238 = CARTESIAN_POINT ( 'NONE',  ( -53.51423613279429503, -136.2500000013656063, 4.591703134518082763 ) ) ;
#10239 = EDGE_CURVE ( 'NONE', #143, #55022, #30835, .T. ) ;
#10240 = EDGE_CURVE ( 'NONE', #39571, #57126, #60504, .T. ) ;
#10241 = CARTESIAN_POINT ( 'NONE',  ( -3.152548672688508926E-16, -1.562499998634406140, -5.148502694627439702 ) ) ;
#10242 = CARTESIAN_POINT ( 'NONE',  ( 4.458734125000001214, 19.85416666803226349, 2.574251347313718519 ) ) ;
#10243 = CARTESIAN_POINT ( 'NONE',  ( 4.458734124999998549, -41.97916666530107932, -2.574251347313721627 ) ) ;
#10244 = CARTESIAN_POINT ( 'NONE',  ( 2.500000000000002220, -15.66666666666666963, 4.330127018922192761 ) ) ;
#10245 = CARTESIAN_POINT ( 'NONE',  ( -2.229367062500000163, 2.520833334698928230, -3.861377020970580443 ) ) ;
#10246 = ORIENTED_EDGE ( 'NONE', *, *, #43342, .F. ) ;
#10247 = CARTESIAN_POINT ( 'NONE',  ( 4.458734125000000326, -31.14583333196773651, 2.574251347313718519 ) ) ;
#10248 = CARTESIAN_POINT ( 'NONE',  ( 4.458734124999998549, -67.72916666530107932, -2.574251347313721627 ) ) ;
#10249 = CARTESIAN_POINT ( 'NONE',  ( -2.499999999999996447, -106.7083333306021444, 4.330127018922195425 ) ) ;
#10250 = EDGE_CURVE ( 'NONE', #4248, #36690, #1741, .T. ) ;
#10251 = CARTESIAN_POINT ( 'NONE',  ( 4.458734124999999437, 26.18750000136559564, -5.460374474430324690E-16 ) ) ;
#10252 = CARTESIAN_POINT ( 'NONE',  ( 1.975475456537005874E-15, -101.7499999999999858, 5.000000000000000000 ) ) ;
#10253 = EDGE_CURVE ( 'NONE', #7188, #37182, #50171, .T. ) ;
#10254 = CARTESIAN_POINT ( 'NONE',  ( -58.80597590150559739, -153.1250000027312126, 3.242614290531460330 ) ) ;
#10255 = CARTESIAN_POINT ( 'NONE',  ( -2.229367062499996610, -71.39583333196773651, 3.861377020970582219 ) ) ;
#10256 = CARTESIAN_POINT ( 'NONE',  ( 1.060575238724906964E-15, -57.75000000000000000, 5.773502691896257311 ) ) ;
#10257 = CARTESIAN_POINT ( 'NONE',  ( -2.500000000000000444, -66.04166666393547303, -4.330127018922193649 ) ) ;
#10258 = CARTESIAN_POINT ( 'NONE',  ( 2.499999999999998668, 26.79166666939785202, -4.330127018922193649 ) ) ;
#10259 = ORIENTED_EDGE ( 'NONE', *, *, #26003, .T. ) ;
#10260 = CARTESIAN_POINT ( 'NONE',  ( 1.339745962155615144, 6.294658198738519062, 4.999999999999999112 ) ) ;
#10261 = CARTESIAN_POINT ( 'NONE',  ( -4.999999999999998224, -98.91666666666667140, 2.886751345948131764 ) ) ;
#10262 = CARTESIAN_POINT ( 'NONE',  ( 5.000000000000000000, -19.41666666666666075, -2.886751345948129988 ) ) ;
#10263 = CARTESIAN_POINT ( 'NONE',  ( 2.229367062499998831, -19.64583333196774007, -3.861377020970580887 ) ) ;
#10264 = CARTESIAN_POINT ( 'NONE',  ( 2.229367062499998831, -81.64583333196773651, -3.861377020970580887 ) ) ;
#10265 = CARTESIAN_POINT ( 'NONE',  ( -3.535250795749689387E-16, -20.12499999726881228, -5.773502691896257311 ) ) ;
#10267 = VERTEX_POINT ( 'NONE', #61142 ) ;
#10266 = CARTESIAN_POINT ( 'NONE',  ( -4.458734124999998549, -51.22916666530107221, 2.574251347313722516 ) ) ;
#10268 = CARTESIAN_POINT ( 'NONE',  ( 5.000000000000000000, -35.37499999726881583, -6.123233995736766282E-16 ) ) ;
#10269 = CARTESIAN_POINT ( 'NONE',  ( 5.000000000000000000, -98.41666666666668561, -2.886751345948130876 ) ) ;
#10271 = VERTEX_POINT ( 'NONE', #46334 ) ;
#10270 = CARTESIAN_POINT ( 'NONE',  ( 2.229367062499998831, 2.104166668032262599, -3.861377020970580887 ) ) ;
#10272 = CARTESIAN_POINT ( 'NONE',  ( -59.59170313451810586, -149.5000000013656063, 1.485763867205729394 ) ) ;
#10273 = CARTESIAN_POINT ( 'NONE',  ( -5.000000000000000000, -66.00000000000000000, 0.000000000000000000 ) ) ;
#10274 = CARTESIAN_POINT ( 'NONE',  ( -4.458734125000000326, -152.2500000013656347, -1.846868145590735644 ) ) ;
#10275 = CARTESIAN_POINT ( 'NONE',  ( -4.458734124999998549, -41.47916666530107221, 2.574251347313722516 ) ) ;
#10276 = CARTESIAN_POINT ( 'NONE',  ( -5.000000000000000888, -162.5625000000000000, -2.071067811865475949 ) ) ;
#10277 = CARTESIAN_POINT ( 'NONE',  ( 3.061616997868383141E-16, -158.8750000027311842, -5.000000000000000000 ) ) ;
#10278 = AXIS2_PLACEMENT_3D ( 'NONE', #27578, #43622, #47517 ) ;
#10279 = CARTESIAN_POINT ( 'NONE',  ( -59.59170313451811296, -125.7500000013656347, 1.485763867205729394 ) ) ;
#10280 = CARTESIAN_POINT ( 'NONE',  ( -2.229367062499996610, -9.395833331967736513, 3.861377020970582219 ) ) ;
#10281 = CARTESIAN_POINT ( 'NONE',  ( 2.229367062500001939, -44.22916666530106511, 3.861377020970579999 ) ) ;
#10282 = CYLINDRICAL_SURFACE ( 'NONE', #22182, 5.000000000000000000 ) ;
#10283 = CARTESIAN_POINT ( 'NONE',  ( -4.458734125000001214, -147.8750000013656063, 1.846868145590734089 ) ) ;
#10284 = CARTESIAN_POINT ( 'NONE',  ( 4.458734124999998549, -89.97916666530105090, -2.574251347313721627 ) ) ;
#10285 = CARTESIAN_POINT ( 'NONE',  ( -4.999999999999998224, 21.20833333606451987, 2.886751345948131764 ) ) ;
#10286 = ORIENTED_EDGE ( 'NONE', *, *, #35111, .T. ) ;
#10287 = CARTESIAN_POINT ( 'NONE',  ( -1.339745962155613812, -32.20534180126148271, -5.000000000000000000 ) ) ;
#10288 = CARTESIAN_POINT ( 'NONE',  ( -5.000000000000000000, -5.958333330602149758, -2.886751345948128211 ) ) ;
#10289 = CARTESIAN_POINT ( 'NONE',  ( -54.60164318462004474, -152.5000000027312410, -4.984105922594373794 ) ) ;
#10290 = CARTESIAN_POINT ( 'NONE',  ( 5.000000000000000000, -82.37499999726881583, -6.123233995736766282E-16 ) ) ;
#10291 = EDGE_LOOP ( 'NONE', ( #45407, #36195, #16851, #4288 ) ) ;
#10292 = CARTESIAN_POINT ( 'NONE',  ( -2.229367062499996610, 3.854166668032260823, 3.861377020970582219 ) ) ;
#10293 =( BOUNDED_CURVE ( )  B_SPLINE_CURVE ( 2, ( #2552, #50487, #45653, #61414, #6426, #41132, #55319, #41764, #46290 ),
 .UNSPECIFIED., .F., .F. ) 
 B_SPLINE_CURVE_WITH_KNOTS ( ( 3, 2, 2, 2, 3 ),
 ( 0.2053571428571428492, 0.2059523809523809423, 0.2071428571428571563, 0.2083333333333333426, 0.2089285714285714357 ),
 .UNSPECIFIED. ) 
 CURVE ( )  GEOMETRIC_REPRESENTATION_ITEM ( )  RATIONAL_B_SPLINE_CURVE ( ( 0.9330127018922194093, 0.9330127018922194093, 1.000000000000000000, 0.8660254037844387076, 1.000000000000000000, 0.8660254037844387076, 1.000000000000000000, 0.9330127018922194093, 0.9330127018922194093 ) ) 
 REPRESENTATION_ITEM ( '' )  );
#10294 = CARTESIAN_POINT ( 'NONE',  ( 5.000000000000000000, -19.49999999999999645, -6.123233995736766282E-16 ) ) ;
#10295 = CARTESIAN_POINT ( 'NONE',  ( 4.458734125000001214, -17.14583333196773651, 2.574251347313718519 ) ) ;
#10296 = CARTESIAN_POINT ( 'NONE',  ( 4.458734125000001214, -4.895833331967740065, 2.574251347313718519 ) ) ;
#10297 = CARTESIAN_POINT ( 'NONE',  ( 1.975475456537005874E-15, -44.62499999726880162, 5.000000000000000000 ) ) ;
#10298 = CARTESIAN_POINT ( 'NONE',  ( 4.458734124999999437, -150.3750000013655779, -1.846868145590734978 ) ) ;
#10299 = CARTESIAN_POINT ( 'NONE',  ( -2.229367062499996610, 19.60416666803225993, 3.861377020970582219 ) ) ;
#10300 = ORIENTED_EDGE ( 'NONE', *, *, #9707, .F. ) ;
#10301 = CARTESIAN_POINT ( 'NONE',  ( 2.229367062500001939, -99.97916666530106511, 3.861377020970579999 ) ) ;
#10302 = CARTESIAN_POINT ( 'NONE',  ( 4.458734125000001214, -13.89583333196774007, 2.574251347313718519 ) ) ;
#10303 = CARTESIAN_POINT ( 'NONE',  ( 0.000000000000000000, -120.0000000000000000, 0.000000000000000000 ) ) ;
#10304 = CYLINDRICAL_SURFACE ( 'NONE', #52037, 5.000000000000000000 ) ;
#10305 = CARTESIAN_POINT ( 'NONE',  ( -59.59170313451811296, -148.5000000013655779, 1.485763867205729394 ) ) ;
#10306 = ADVANCED_FACE ( 'NONE', ( #46972 ), #6785, .T. ) ;
#10307 = CARTESIAN_POINT ( 'NONE',  ( -5.000000000000000000, -39.95833333060213732, -2.886751345948128211 ) ) ;
#10308 = CARTESIAN_POINT ( 'NONE',  ( 1.975475456537005874E-15, -74.75000000000000000, 5.000000000000000000 ) ) ;
#10309 = CARTESIAN_POINT ( 'NONE',  ( -3.152548672688508926E-16, 14.43750000136559386, -5.148502694627439702 ) ) ;
#10310 = CARTESIAN_POINT ( 'NONE',  ( 0.000000000000000000, -170.0000000000000000, 0.000000000000000000 ) ) ;
#10311 = CARTESIAN_POINT ( 'NONE',  ( -3.152548672688508926E-16, 16.43750000136559564, -5.148502694627439702 ) ) ;
#10312 = CARTESIAN_POINT ( 'NONE',  ( 4.458734124999999437, -60.81249999863440081, -5.460374474430324690E-16 ) ) ;
#10313 = ORIENTED_EDGE ( 'NONE', *, *, #14877, .F. ) ;
#10314 = AXIS2_PLACEMENT_3D ( 'NONE', #61842, #43139, #3299 ) ;
#10315 = CARTESIAN_POINT ( 'NONE',  ( 2.229367062499998831, -9.895833331967738289, -3.861377020970580887 ) ) ;
#10316 = EDGE_CURVE ( 'NONE', #22477, #12901, #32520, .T. ) ;
#10317 = CARTESIAN_POINT ( 'NONE',  ( -3.535250795749689387E-16, 5.749999999999998224, -5.773502691896257311 ) ) ;
#10318 = CARTESIAN_POINT ( 'NONE',  ( 4.458734124999999437, -168.4375000013656063, 0.000000000000000000 ) ) ;
#10319 = CARTESIAN_POINT ( 'NONE',  ( -1.339745962155610925, -98.66965819600734733, 5.000000000000000000 ) ) ;
#10320 = CARTESIAN_POINT ( 'NONE',  ( -2.229367062499996610, -53.14583333196773651, 3.861377020970582219 ) ) ;
#10321 = CARTESIAN_POINT ( 'NONE',  ( 5.000000000000000000, -89.37499999726880162, -6.123233995736766282E-16 ) ) ;
#10322 = CARTESIAN_POINT ( 'NONE',  ( -2.229367062500000163, -32.47916666530106511, -3.861377020970580443 ) ) ;
#10323 = EDGE_CURVE ( 'NONE', #45276, #58623, #12239, .T. ) ;
#10324 = CARTESIAN_POINT ( 'NONE',  ( 2.499999999999998668, -38.33333333333332860, -4.330127018922193649 ) ) ;
#10325 = FACE_OUTER_BOUND ( 'NONE', #24768, .T. ) ;
#10326 = CARTESIAN_POINT ( 'NONE',  ( -6.972266317189433020E-16, -108.1249999972688158, -5.000000000000000000 ) ) ;
#10327 = CARTESIAN_POINT ( 'NONE',  ( 1.846868145590735200, -154.5000000013656347, -4.458734124999999437 ) ) ;
#10328 = CARTESIAN_POINT ( 'NONE',  ( 5.000000000000000888, -41.58333333333332860, 2.886751345948126879 ) ) ;
#10329 = FACE_OUTER_BOUND ( 'NONE', #24922, .T. ) ;
#10330 = EDGE_CURVE ( 'NONE', #55783, #24283, #26325, .T. ) ;
#10331 = CARTESIAN_POINT ( 'NONE',  ( -58.24086726761811406, -135.0000000000000000, -3.252698689335780102 ) ) ;
#10332 = VERTEX_POINT ( 'NONE', #37313 ) ;
#10333 = CARTESIAN_POINT ( 'NONE',  ( 9.457646018065525792E-16, -99.06249999863440792, 5.148502694627439702 ) ) ;
#10334 = CARTESIAN_POINT ( 'NONE',  ( -4.458734124999998549, 3.520833334698929118, 2.574251347313722516 ) ) ;
#10335 = EDGE_CURVE ( 'NONE', #40878, #41738, #43956, .T. ) ;
#10336 = CARTESIAN_POINT ( 'NONE',  ( 5.000000000000000000, -4.416666666666666075, -2.886751345948129988 ) ) ;
#10337 = CARTESIAN_POINT ( 'NONE',  ( -4.458734124999999437, -66.39583333196773651, -2.574251347313719407 ) ) ;
#10338 = CARTESIAN_POINT ( 'NONE',  ( -5.000000000000000000, 2.916666666666668739, -2.886751345948128211 ) ) ;
#10339 = EDGE_CURVE ( 'NONE', #7464, #23303, #32482, .T. ) ;
#10340 = CARTESIAN_POINT ( 'NONE',  ( -2.499999999999996447, -3.708333330602147537, 4.330127018922195425 ) ) ;
#10342 = ORIENTED_EDGE ( 'NONE', *, *, #19755, .F. ) ;
#10341 = CARTESIAN_POINT ( 'NONE',  ( -2.229367062500000163, -34.47916666530107221, -3.861377020970580443 ) ) ;
#10343 = CARTESIAN_POINT ( 'NONE',  ( -5.000000000000000000, -78.08333333333332860, -2.886751345948128211 ) ) ;
#10344 = ORIENTED_EDGE ( 'NONE', *, *, #53805, .T. ) ;
#10345 =( BOUNDED_CURVE ( )  B_SPLINE_CURVE ( 2, ( #44434, #44752, #55381, #55058, #59241, #395, #19997, #39925, #39605 ),
 .UNSPECIFIED., .F., .F. ) 
 B_SPLINE_CURVE_WITH_KNOTS ( ( 3, 2, 2, 2, 3 ),
 ( 0.2812500000000000000, 0.2819444444444444420, 0.2833333333333333259, 0.2847222222222222099, 0.2854166666666666519 ),
 .UNSPECIFIED. ) 
 CURVE ( )  GEOMETRIC_REPRESENTATION_ITEM ( )  RATIONAL_B_SPLINE_CURVE ( ( 0.9330127018922194093, 0.9330127018922194093, 1.000000000000000000, 0.8660254037844387076, 1.000000000000000000, 0.8660254037844387076, 1.000000000000000000, 0.9330127018922194093, 0.9330127018922194093 ) ) 
 REPRESENTATION_ITEM ( '' )  );
#10346 = CARTESIAN_POINT ( 'NONE',  ( -5.000000000000000000, -52.08333333333332860, -2.886751345948128211 ) ) ;
#10349 = CARTESIAN_POINT ( 'NONE',  ( 9.457646018065525792E-16, -26.31249999863440792, 5.148502694627439702 ) ) ;
#10348 =( BOUNDED_CURVE ( )  B_SPLINE_CURVE ( 2, ( #22391, #56167, #12090, #51346, #7285, #41992, #52289, #46514, #37488 ),
 .UNSPECIFIED., .F., .F. ) 
 B_SPLINE_CURVE_WITH_KNOTS ( ( 3, 2, 2, 2, 3 ),
 ( 0.8395833333333333481, 0.8402777777777777901, 0.8416666666666666741, 0.8430555555555555580, 0.8437500000000000000 ),
 .UNSPECIFIED. ) 
 CURVE ( )  GEOMETRIC_REPRESENTATION_ITEM ( )  RATIONAL_B_SPLINE_CURVE ( ( 0.9330127018922194093, 0.9330127018922194093, 1.000000000000000000, 0.8660254037844387076, 1.000000000000000000, 0.8660254037844387076, 1.000000000000000000, 0.9330127018922194093, 0.9330127018922194093 ) ) 
 REPRESENTATION_ITEM ( '' )  );
#10347 = CYLINDRICAL_SURFACE ( 'NONE', #62418, 5.000000000000000000 ) ;
#10350 = CARTESIAN_POINT ( 'NONE',  ( -5.000000000000000000, -41.87499999726880873, 0.000000000000000000 ) ) ;
#10351 = CARTESIAN_POINT ( 'NONE',  ( -2.229367062499996610, -70.14583333196773651, 3.861377020970582219 ) ) ;
#10352 = CARTESIAN_POINT ( 'NONE',  ( 2.730187237215162345E-16, -142.4375000013656063, -4.458734124999999437 ) ) ;
#10353 = CARTESIAN_POINT ( 'NONE',  ( -4.458734124999998549, -84.22916666530107932, 2.574251347313722516 ) ) ;
#10354 = CARTESIAN_POINT ( 'NONE',  ( -50.55543936806279248, -138.3125000013656063, 0.3552334253322060320 ) ) ;
#10355 = CARTESIAN_POINT ( 'NONE',  ( -3.152548672688508926E-16, -28.81249999863440436, -5.148502694627439702 ) ) ;
#10356 = CARTESIAN_POINT ( 'NONE',  ( 1.060575238724906964E-15, -70.62499999726881583, 5.773502691896257311 ) ) ;
#10357 = VERTEX_POINT ( 'NONE', #52111 ) ;
#10358 = DIRECTION ( 'NONE',  ( -0.000000000000000000, 1.000000000000000000, -0.000000000000000000 ) ) ;
#10359 = ORIENTED_EDGE ( 'NONE', *, *, #55866, .T. ) ;
#10360 = CARTESIAN_POINT ( 'NONE',  ( -4.458734124999999437, -72.64583333196773651, -2.574251347313719407 ) ) ;
#10361 = DIRECTION ( 'NONE',  ( -0.6485228581062915110, 0.000000000000000000, -0.7611951803011149931 ) ) ;
#10362 = ORIENTED_EDGE ( 'NONE', *, *, #6436, .T. ) ;
#10363 = DIRECTION ( 'NONE',  ( -0.6485228581062915110, 0.000000000000000000, -0.7611951803011149931 ) ) ;
#10365 = VECTOR ( 'NONE', #45144, 1000.000000000000000 ) ;
#10364 = CARTESIAN_POINT ( 'NONE',  ( 1.339745962155615144, -12.70534180126147739, 4.999999999999999112 ) ) ;
#10366 = CARTESIAN_POINT ( 'NONE',  ( -4.458734124999999437, -57.64583333196773651, -2.574251347313719407 ) ) ;
#10367 = CARTESIAN_POINT ( 'NONE',  ( -3.152548672688508926E-16, -5.812499998634404363, -5.148502694627439702 ) ) ;
#10368 = EDGE_LOOP ( 'NONE', ( #48610, #7682, #55698, #21779 ) ) ;
#10369 = LINE ( 'NONE', #19699, #21400 ) ;
#10370 = CYLINDRICAL_SURFACE ( 'NONE', #29444, 5.000000000000000000 ) ;
#10371 =( BOUNDED_CURVE ( )  B_SPLINE_CURVE ( 2, ( #14205, #19986, #29300, #4878, #39913, #43786, #24499, #54079, #702 ),
 .UNSPECIFIED., .F., .F. ) 
 B_SPLINE_CURVE_WITH_KNOTS ( ( 3, 2, 2, 2, 3 ),
 ( 0.4979166666666666741, 0.4986111111111111160, 0.5000000000000000000, 0.5013888888888888840, 0.5020833333333333259 ),
 .UNSPECIFIED. ) 
 CURVE ( )  GEOMETRIC_REPRESENTATION_ITEM ( )  RATIONAL_B_SPLINE_CURVE ( ( 0.9330127018922194093, 0.9330127018922194093, 1.000000000000000000, 0.8660254037844387076, 1.000000000000000000, 0.8660254037844387076, 1.000000000000000000, 0.9330127018922194093, 0.9330127018922194093 ) ) 
 REPRESENTATION_ITEM ( '' )  );
#10372 = CARTESIAN_POINT ( 'NONE',  ( -2.229367062500000163, 11.52083333469892601, -3.861377020970580443 ) ) ;
#10373 = CARTESIAN_POINT ( 'NONE',  ( -57.19623071787017210, -139.3750000013656063, 4.297418129356382899 ) ) ;
#10374 = CARTESIAN_POINT ( 'NONE',  ( -48.00000000000002132, -135.0000000000000284, -4.041451884327376121 ) ) ;
#10375 = CARTESIAN_POINT ( 'NONE',  ( 1.846868145590735200, -160.2500000013656063, -4.458734124999999437 ) ) ;
#10376 = VERTEX_POINT ( 'NONE', #2920 ) ;
#10377 = CARTESIAN_POINT ( 'NONE',  ( -4.458734124999999437, -82.39583333196773651, -2.574251347313719407 ) ) ;
#10378 = CARTESIAN_POINT ( 'NONE',  ( 6.123233995736766282E-16, -170.0000000000000000, -5.000000000000000000 ) ) ;
#10379 = CARTESIAN_POINT ( 'NONE',  ( -4.458734124999999437, 3.687500001365594748, 0.000000000000000000 ) ) ;
#10380 = CARTESIAN_POINT ( 'NONE',  ( 2.500000000000002220, -83.66666666666667140, 4.330127018922192761 ) ) ;
#10381 = CARTESIAN_POINT ( 'NONE',  ( 1.975475456537005874E-15, -36.75000000000000000, 5.000000000000000000 ) ) ;
#10382 = CARTESIAN_POINT ( 'NONE',  ( 4.458734124999999437, -65.06249999863440792, -5.460374474430324690E-16 ) ) ;
#10383 = CARTESIAN_POINT ( 'NONE',  ( -5.000000000000000000, -22.95833333060214798, -2.886751345948128211 ) ) ;
#10384 = CARTESIAN_POINT ( 'NONE',  ( -1.339745962155610925, -72.66965819600733312, 5.000000000000000000 ) ) ;
#10385 = CARTESIAN_POINT ( 'NONE',  ( 4.458734124999998549, 27.27083333469892779, -2.574251347313721627 ) ) ;
#10386 = CARTESIAN_POINT ( 'NONE',  ( -2.500000000000000444, -38.04166666393548013, -4.330127018922193649 ) ) ;
#10387 = CARTESIAN_POINT ( 'NONE',  ( 5.000000000000000888, -3.458333330602147093, 2.886751345948126879 ) ) ;
#10388 = CARTESIAN_POINT ( 'NONE',  ( 2.229367062500001939, -44.97916666530106511, 3.861377020970579999 ) ) ;
#10389 = CARTESIAN_POINT ( 'NONE',  ( 4.458734124999999437, -30.06249999863440436, -5.460374474430324690E-16 ) ) ;
#10390 = CARTESIAN_POINT ( 'NONE',  ( -2.229367062499996610, 5.604166668032261711, 3.861377020970582219 ) ) ;
#10391 =( BOUNDED_CURVE ( )  B_SPLINE_CURVE ( 2, ( #27964, #27028, #62398, #56630, #27654, #47587, #3538, #23147, #2917 ),
 .UNSPECIFIED., .F., .F. ) 
 B_SPLINE_CURVE_WITH_KNOTS ( ( 3, 2, 2, 2, 3 ),
 ( 0.3750000000000002776, 0.3791666666666669294, 0.3833333333333336368, 0.3875000000000003442, 0.3916666666666669960 ),
 .UNSPECIFIED. ) 
 CURVE ( )  GEOMETRIC_REPRESENTATION_ITEM ( )  RATIONAL_B_SPLINE_CURVE ( ( 0.9999999999999948930, 0.9238795325112918455, 1.000000000000000000, 0.9238795325112867385, 1.000000000000000000, 0.9238795325112867385, 1.000000000000000000, 0.9238795325112806323, 1.000000000000005995 ) ) 
 REPRESENTATION_ITEM ( '' )  );
#10392 = DIRECTION ( 'NONE',  ( -0.000000000000000000, 1.000000000000000000, -0.000000000000000000 ) ) ;
#10393 = CARTESIAN_POINT ( 'NONE',  ( 5.000000000000000000, 18.50000000000000000, -6.123233995736766282E-16 ) ) ;
#10394 = CARTESIAN_POINT ( 'NONE',  ( 3.535533905932738197, -151.0000000027312126, -3.535533905932738197 ) ) ;
#10395 = CARTESIAN_POINT ( 'NONE',  ( -5.000000000000000000, -50.00000000000000000, 0.000000000000000000 ) ) ;
#10396 = CARTESIAN_POINT ( 'NONE',  ( 2.229367062500001939, -37.97916666530107221, 3.861377020970579999 ) ) ;
#10397 = CARTESIAN_POINT ( 'NONE',  ( -3.535250795749689387E-16, -72.12499999726881583, -5.773502691896257311 ) ) ;
#10398 = CARTESIAN_POINT ( 'NONE',  ( -57.19623071787017210, -142.6250000013655779, 4.297418129356382899 ) ) ;
#10399 = DIRECTION ( 'NONE',  ( 0.000000000000000000, 0.000000000000000000, 1.000000000000000000 ) ) ;
#10400 = CARTESIAN_POINT ( 'NONE',  ( 5.000000000000000000, -15.37499999726881228, -6.123233995736766282E-16 ) ) ;
#10401 = CARTESIAN_POINT ( 'NONE',  ( -2.229367062500000163, -79.72916666530106511, -3.861377020970580443 ) ) ;
#10402 = CARTESIAN_POINT ( 'NONE',  ( -4.458734124999999437, -165.1875000013655779, -5.460374474430324690E-16 ) ) ;
#10403 = CARTESIAN_POINT ( 'NONE',  ( 1.339745962155612702, 18.83034180399265978, -5.000000000000000000 ) ) ;
#10404 = CARTESIAN_POINT ( 'NONE',  ( 0.000000000000000000, -120.0000000000000000, 0.000000000000000000 ) ) ;
#10405 = CARTESIAN_POINT ( 'NONE',  ( -2.500000000000000444, -26.16666666666666430, -4.330127018922193649 ) ) ;
#10406 = CARTESIAN_POINT ( 'NONE',  ( -4.458734124999999437, -142.9375000013656063, -5.460374474430324690E-16 ) ) ;
#10407 = EDGE_LOOP ( 'NONE', ( #50431, #38786, #27522, #52949 ) ) ;
#10408 = CARTESIAN_POINT ( 'NONE',  ( 2.500000000000002220, -90.54166666393547303, 4.330127018922192761 ) ) ;
#10409 = ORIENTED_EDGE ( 'NONE', *, *, #18156, .F. ) ;
#10410 = CARTESIAN_POINT ( 'NONE',  ( -2.229367062500000163, -63.72916666530106511, -3.861377020970580443 ) ) ;
#10411 = CARTESIAN_POINT ( 'NONE',  ( -5.000000000000000000, 23.04166666939785557, -2.886751345948128211 ) ) ;
#10412 = DIRECTION ( 'NONE',  ( -0.000000000000000000, -1.000000000000000000, -0.000000000000000000 ) ) ;
#10413 = CARTESIAN_POINT ( 'NONE',  ( -2.500000000000000444, 12.83333333333333215, -4.330127018922193649 ) ) ;
#10414 = VECTOR ( 'NONE', #4729, 1000.000000000000000 ) ;
#10415 = CARTESIAN_POINT ( 'NONE',  ( 4.458734124999999437, -49.81249999863440792, -5.460374474430324690E-16 ) ) ;
#10416 = CARTESIAN_POINT ( 'NONE',  ( 4.458734124999998549, -7.729166665301073103, -2.574251347313721627 ) ) ;
#10417 = CARTESIAN_POINT ( 'NONE',  ( 3.535533905932736864, -166.2500000027312126, 3.535533905932738641 ) ) ;
#10418 = CARTESIAN_POINT ( 'NONE',  ( -52.53715891517739323, -145.5625000027312126, -4.819101127000233298 ) ) ;
#10419 = CARTESIAN_POINT ( 'NONE',  ( 1.339745962155615144, -91.58034179853028434, 4.999999999999999112 ) ) ;
#10420 = CARTESIAN_POINT ( 'NONE',  ( -75.00000000000001421, 15.00000000000000000, -9.000000000000001776 ) ) ;
#10422 = CARTESIAN_POINT ( 'NONE',  ( -4.458734124999999437, -21.39583333196774007, -2.574251347313719407 ) ) ;
#10421 = CARTESIAN_POINT ( 'NONE',  ( -5.000000000000000000, -59.08333333333332860, -2.886751345948128211 ) ) ;
#10423 = CARTESIAN_POINT ( 'NONE',  ( 2.229367062499998831, -53.64583333196773651, -3.861377020970580887 ) ) ;
#10424 = CARTESIAN_POINT ( 'NONE',  ( -1.846868145590734756, -154.3750000013655779, -4.458734125000000326 ) ) ;
#10425 = CARTESIAN_POINT ( 'NONE',  ( 2.500000000000002220, -55.54166666393548013, 4.330127018922192761 ) ) ;
#10426 = ORIENTED_EDGE ( 'NONE', *, *, #41745, .F. ) ;
#10427 = CARTESIAN_POINT ( 'NONE',  ( -52.53715891517739323, -137.4375000000000284, -4.819101127000233298 ) ) ;
#10428 = CARTESIAN_POINT ( 'NONE',  ( 4.458734124999998549, 3.020833334698928674, -2.574251347313721627 ) ) ;
#10429 = ORIENTED_EDGE ( 'NONE', *, *, #29547, .T. ) ;
#10431 = CARTESIAN_POINT ( 'NONE',  ( -2.500000000000000444, -29.16666666666666785, -4.330127018922193649 ) ) ;
#10430 = CARTESIAN_POINT ( 'NONE',  ( 1.975475456537005874E-15, -56.75000000000000000, 5.000000000000000000 ) ) ;
#10432 = CARTESIAN_POINT ( 'NONE',  ( -1.846868145590737420, -157.7500000013656063, 4.458734124999999437 ) ) ;
#10433 = VERTEX_POINT ( 'NONE', #27657 ) ;
#10434 = CARTESIAN_POINT ( 'NONE',  ( -4.999999999999998224, 11.08333333333333393, 2.886751345948131764 ) ) ;
#10435 = CARTESIAN_POINT ( 'NONE',  ( -50.01589407740564042, -127.6250000000000142, 0.3983568153799778022 ) ) ;
#10436 = CARTESIAN_POINT ( 'NONE',  ( -6.972266317189433020E-16, -86.25000000000001421, -5.000000000000000000 ) ) ;
#10437 = CARTESIAN_POINT ( 'NONE',  ( -2.229367062499996610, -41.39583333196773651, 3.861377020970582219 ) ) ;
#10438 = ORIENTED_EDGE ( 'NONE', *, *, #53617, .F. ) ;
#10439 = CARTESIAN_POINT ( 'NONE',  ( 1.339745962155637349, 9.830341803992661553, -4.999999999999985789 ) ) ;
#10440 = CARTESIAN_POINT ( 'NONE',  ( -4.458734124999999437, 14.68750000136559386, 0.000000000000000000 ) ) ;
#10441 = CARTESIAN_POINT ( 'NONE',  ( -4.458734124999999437, 29.68750000136559208, 0.000000000000000000 ) ) ;
#10442 = CARTESIAN_POINT ( 'NONE',  ( -50.70258187064364108, -152.1250000013656063, 2.196230717870141014 ) ) ;
#10443 = LINE ( 'NONE', #59992, #53164 ) ;
#10444 = CARTESIAN_POINT ( 'NONE',  ( 7.500000000000000000, -3.608439182435168036, -7.298562697733107285 ) ) ;
#10445 = CARTESIAN_POINT ( 'NONE',  ( -5.000000000000000000, 24.00000000000000000, 0.000000000000000000 ) ) ;
#10446 = CARTESIAN_POINT ( 'NONE',  ( 4.458734124999999437, -65.81249999863440792, -5.460374474430324690E-16 ) ) ;
#10447 = CYLINDRICAL_SURFACE ( 'NONE', #16120, 5.000000000000000000 ) ;
#10448 = CARTESIAN_POINT ( 'NONE',  ( -2.229367062499996610, 18.85416666803225993, 3.861377020970582219 ) ) ;
#10449 = CARTESIAN_POINT ( 'NONE',  ( 4.458734124999998549, -50.97916666530107221, -2.574251347313721627 ) ) ;
#10450 = CARTESIAN_POINT ( 'NONE',  ( -3.535250795749689387E-16, -10.12499999726881583, -5.773502691896257311 ) ) ;
#10451 = CARTESIAN_POINT ( 'NONE',  ( -4.999999999999998224, 5.083333333333332149, 2.886751345948131764 ) ) ;
#10452 = FACE_OUTER_BOUND ( 'NONE', #1736, .T. ) ;
#10453 = CARTESIAN_POINT ( 'NONE',  ( 2.229367062499998831, -87.89583333196773651, -3.861377020970580887 ) ) ;
#10454 = CARTESIAN_POINT ( 'NONE',  ( -2.500000000000000444, 10.95833333606451632, -4.330127018922193649 ) ) ;
#10455 = CARTESIAN_POINT ( 'NONE',  ( 4.458734124999999437, -18.06249999863440792, -5.460374474430324690E-16 ) ) ;
#10456 = ORIENTED_EDGE ( 'NONE', *, *, #35457, .T. ) ;
#10457 = CARTESIAN_POINT ( 'NONE',  ( -5.000000000000000000, -46.95833333060214443, -2.886751345948128211 ) ) ;
#10458 = CARTESIAN_POINT ( 'NONE',  ( -4.458734124999998549, -105.2291666653010651, 2.574251347313722516 ) ) ;
#10459 = CARTESIAN_POINT ( 'NONE',  ( 3.535533905932738197, -161.0000000027312126, -3.535533905932738197 ) ) ;
#10460 = EDGE_LOOP ( 'NONE', ( #44461, #9847, #1211, #1520 ) ) ;
#10461 = CARTESIAN_POINT ( 'NONE',  ( -4.458734124999999437, -95.64583333196772230, -2.574251347313719407 ) ) ;
#10462 = CARTESIAN_POINT ( 'NONE',  ( 5.000000000000000000, -49.29166666393547303, -2.886751345948130876 ) ) ;
#10463 = CARTESIAN_POINT ( 'NONE',  ( -4.999999999999999112, -57.79166666393548013, 2.886751345948131764 ) ) ;
#10464 = CARTESIAN_POINT ( 'NONE',  ( 1.975475456537005874E-15, -71.62499999726878741, 5.000000000000000000 ) ) ;
#10465 =( BOUNDED_CURVE ( )  B_SPLINE_CURVE ( 2, ( #52057, #2235, #32105, #21839, #26976, #27911, #23097, #56571, #61084 ),
 .UNSPECIFIED., .F., .F. ) 
 B_SPLINE_CURVE_WITH_KNOTS ( ( 3, 2, 2, 2, 3 ),
 ( 0.4160714285714285920, 0.4166666666666666852, 0.4178571428571428714, 0.4190476190476190577, 0.4196428571428571508 ),
 .UNSPECIFIED. ) 
 CURVE ( )  GEOMETRIC_REPRESENTATION_ITEM ( )  RATIONAL_B_SPLINE_CURVE ( ( 0.9330127018922194093, 0.9330127018922194093, 1.000000000000000000, 0.8660254037844387076, 1.000000000000000000, 0.8660254037844387076, 1.000000000000000000, 0.9330127018922194093, 0.9330127018922194093 ) ) 
 REPRESENTATION_ITEM ( '' )  );
#10466 = CARTESIAN_POINT ( 'NONE',  ( -53.51423613279429503, -125.2500000013656347, 4.591703134518082763 ) ) ;
#10467 = CARTESIAN_POINT ( 'NONE',  ( -58.39396692619412477, -144.4375000013656063, 2.891590998281057701 ) ) ;
#10468 = CARTESIAN_POINT ( 'NONE',  ( 4.458734124999999437, -17.81249999863440792, -5.460374474430324690E-16 ) ) ;
#10469 = CARTESIAN_POINT ( 'NONE',  ( 2.229367062500001939, 6.770833334698928674, 3.861377020970579999 ) ) ;
#10470 = CARTESIAN_POINT ( 'NONE',  ( 2.229367062500001939, -63.22916666530106511, 3.861377020970579999 ) ) ;
#10471 = DIRECTION ( 'NONE',  ( -0.000000000000000000, 1.000000000000000000, -0.000000000000000000 ) ) ;
#10472 = CARTESIAN_POINT ( 'NONE',  ( 4.458734124999999437, -18.81249999863440792, -5.460374474430324690E-16 ) ) ;
#10473 = CARTESIAN_POINT ( 'NONE',  ( 1.975475456537005874E-15, -75.74999999999998579, 5.000000000000000000 ) ) ;
#10474 = CARTESIAN_POINT ( 'NONE',  ( -2.071067811865475061, -154.6875000000000568, -5.000000000000000888 ) ) ;
#10475 = CARTESIAN_POINT ( 'NONE',  ( -5.000000000000000000, -13.08333333333333570, -2.886751345948128211 ) ) ;
#10476 = CARTESIAN_POINT ( 'NONE',  ( -4.458734124999999437, -155.9375000013655779, -5.460374474430324690E-16 ) ) ;
#10477 = ORIENTED_EDGE ( 'NONE', *, *, #14502, .F. ) ;
#10478 = CARTESIAN_POINT ( 'NONE',  ( 9.457646018065525792E-16, -45.31249999863440081, 5.148502694627439702 ) ) ;
#10479 = CARTESIAN_POINT ( 'NONE',  ( 5.000000000000000888, -44.45833333060214443, 2.886751345948126879 ) ) ;
#10480 = CARTESIAN_POINT ( 'NONE',  ( -2.500000000000000444, -92.04166666393547303, -4.330127018922193649 ) ) ;
#10481 = CARTESIAN_POINT ( 'NONE',  ( 2.229367062499998831, -89.64583333196773651, -3.861377020970580887 ) ) ;
#10482 = CARTESIAN_POINT ( 'NONE',  ( 4.458734124999998549, -91.72916666530106511, -2.574251347313721627 ) ) ;
#10483 = CARTESIAN_POINT ( 'NONE',  ( -4.458734124999999437, 13.35416666803225993, -2.574251347313719407 ) ) ;
#10484 = CARTESIAN_POINT ( 'NONE',  ( -4.458734124999999437, 10.60416666803225993, -2.574251347313719407 ) ) ;
#10485 =( BOUNDED_CURVE ( )  B_SPLINE_CURVE ( 2, ( #57672, #32260, #62180, #51889, #57045, #22946, #31947, #18419, #41581 ),
 .UNSPECIFIED., .F., .F. ) 
 B_SPLINE_CURVE_WITH_KNOTS ( ( 3, 2, 2, 2, 3 ),
 ( 0.5750000000000005107, 0.5791666666666672736, 0.5833333333333339255, 0.5875000000000004663, 0.5916666666666671182 ),
 .UNSPECIFIED. ) 
 CURVE ( )  GEOMETRIC_REPRESENTATION_ITEM ( )  RATIONAL_B_SPLINE_CURVE ( ( 0.9999999999999898970, 0.9238795325112968415, 1.000000000000000000, 0.9238795325112867385, 1.000000000000000000, 0.9238795325112867385, 1.000000000000000000, 0.9238795325112786339, 1.000000000000008216 ) ) 
 REPRESENTATION_ITEM ( '' )  );
#10486 = FACE_OUTER_BOUND ( 'NONE', #6270, .T. ) ;
#10487 = CARTESIAN_POINT ( 'NONE',  ( -2.229367062499996610, 18.60416666803225993, 3.861377020970582219 ) ) ;
#10488 = CARTESIAN_POINT ( 'NONE',  ( -2.499999999999996447, -73.83333333333332860, 4.330127018922195425 ) ) ;
#10489 = CARTESIAN_POINT ( 'NONE',  ( -4.999999999999999112, 9.208333336064519870, 2.886751345948131764 ) ) ;
#10490 = ORIENTED_EDGE ( 'NONE', *, *, #28417, .T. ) ;
#10491 = CARTESIAN_POINT ( 'NONE',  ( 1.975475456537005874E-15, 8.249999999999998224, 5.000000000000000000 ) ) ;
#10492 = ORIENTED_EDGE ( 'NONE', *, *, #43620, .T. ) ;
#10493 = CARTESIAN_POINT ( 'NONE',  ( -4.999999999999998224, -50.91666666666666430, 2.886751345948131764 ) ) ;
#10494 = CARTESIAN_POINT ( 'NONE',  ( 4.458734125000001214, -38.89583333196773651, 2.574251347313718519 ) ) ;
#10495 = CARTESIAN_POINT ( 'NONE',  ( -2.499999999999996447, -39.70833333060214443, 4.330127018922195425 ) ) ;
#10496 = ORIENTED_EDGE ( 'NONE', *, *, #38212, .F. ) ;
#10497 = CARTESIAN_POINT ( 'NONE',  ( -3.152548672688508926E-16, -10.56249999863440792, -5.148502694627439702 ) ) ;
#10499 = ORIENTED_EDGE ( 'NONE', *, *, #13111, .F. ) ;
#10498 = CARTESIAN_POINT ( 'NONE',  ( 2.229367062500001939, -21.22916666530107221, 3.861377020970579999 ) ) ;
#10500 = CARTESIAN_POINT ( 'NONE',  ( -5.000000000000000000, -80.08333333333332860, -2.886751345948128211 ) ) ;
#10501 = CARTESIAN_POINT ( 'NONE',  ( -4.458734125000000326, -169.0000000013655779, -1.846868145590735644 ) ) ;
#10502 = CARTESIAN_POINT ( 'NONE',  ( 4.458734125000001214, -65.14583333196773651, 2.574251347313718519 ) ) ;
#10503 = CARTESIAN_POINT ( 'NONE',  ( -5.000000000000000000, -87.95833333060213022, -2.886751345948128211 ) ) ;
#10505 = ORIENTED_EDGE ( 'NONE', *, *, #9091, .F. ) ;
#10504 = CARTESIAN_POINT ( 'NONE',  ( 0.000000000000000000, -170.0000000000000000, 5.000000000000000000 ) ) ;
#10506 = CARTESIAN_POINT ( 'NONE',  ( -57.46284108482265651, -140.9375000000000000, 4.819101127000239515 ) ) ;
#10507 = EDGE_CURVE ( 'NONE', #54676, #18754, #9292, .T. ) ;
#10508 = CARTESIAN_POINT ( 'NONE',  ( 2.229367062499998831, -25.89583333196773651, -3.861377020970580887 ) ) ;
#10509 = CARTESIAN_POINT ( 'NONE',  ( 5.000000000000000000, -5.291666663935480130, -2.886751345948130876 ) ) ;
#10510 = ORIENTED_EDGE ( 'NONE', *, *, #38873, .T. ) ;
#10511 = SHAPE_DEFINITION_REPRESENTATION ( #34838, #49651 ) ;
#10512 = CARTESIAN_POINT ( 'NONE',  ( -3.152801135295367985, -164.0625000013656063, 3.152801135295367096 ) ) ;
#10513 = CARTESIAN_POINT ( 'NONE',  ( 2.229367062499998831, -108.8958333319677365, -3.861377020970580887 ) ) ;
#10514 = FACE_OUTER_BOUND ( 'NONE', #34226, .T. ) ;
#10515 = ORIENTED_EDGE ( 'NONE', *, *, #9347, .F. ) ;
#10516 = CARTESIAN_POINT ( 'NONE',  ( -51.60603307380591787, -146.1875000013656063, -2.891590998281053704 ) ) ;
#10517 = CARTESIAN_POINT ( 'NONE',  ( 2.229367062499998831, -73.89583333196773651, -3.861377020970580887 ) ) ;
#10518 = CARTESIAN_POINT ( 'NONE',  ( -58.24261429053147765, -134.3750000027312126, -3.805975901505573855 ) ) ;
#10519 = CARTESIAN_POINT ( 'NONE',  ( 4.458734124999998549, -45.72916666530106511, -2.574251347313721627 ) ) ;
#10520 = CARTESIAN_POINT ( 'NONE',  ( 1.846868145590736310, -146.8750000013656063, 4.458734124999997661 ) ) ;
#10521 = CARTESIAN_POINT ( 'NONE',  ( -5.000000000000000000, 22.91666666666666430, -2.886751345948128211 ) ) ;
#10522 = CARTESIAN_POINT ( 'NONE',  ( 2.229367062500001939, -49.97916666530107221, 3.861377020970579999 ) ) ;
#10523 = CARTESIAN_POINT ( 'NONE',  ( -6.972266317189433020E-16, -71.25000000000000000, -5.000000000000000000 ) ) ;
#10524 = CARTESIAN_POINT ( 'NONE',  ( -2.229367062499996610, -11.14583333196773829, 3.861377020970582219 ) ) ;
#10525 = CARTESIAN_POINT ( 'NONE',  ( 2.499999999999998668, -99.33333333333332860, -4.330127018922193649 ) ) ;
#10526 = ADVANCED_FACE ( 'NONE', ( #4169 ), #42441, .T. ) ;
#10527 = CARTESIAN_POINT ( 'NONE',  ( -4.458734125000000326, -141.2500000013656063, -1.846868145590735644 ) ) ;
#10528 = CARTESIAN_POINT ( 'NONE',  ( -2.229367062500000163, -34.72916666530107221, -3.861377020970580443 ) ) ;
#10529 = EDGE_CURVE ( 'NONE', #33480, #3482, #6235, .T. ) ;
#10530 = CARTESIAN_POINT ( 'NONE',  ( -5.000000000000000000, 9.041666669397852019, -2.886751345948128211 ) ) ;
#10531 = CARTESIAN_POINT ( 'NONE',  ( 1.975475456537005874E-15, -52.75000000000000000, 5.000000000000000000 ) ) ;
#10532 = CARTESIAN_POINT ( 'NONE',  ( -52.10840900171896806, -128.1875000013656063, 3.393966926194110556 ) ) ;
#10533 = CARTESIAN_POINT ( 'NONE',  ( 9.457646018065525792E-16, -73.31249999863440792, 5.148502694627439702 ) ) ;
#10534 = CARTESIAN_POINT ( 'NONE',  ( -58.24261429053147765, -141.2500000000000284, -3.805975901505573855 ) ) ;
#10535 = CYLINDRICAL_SURFACE ( 'NONE', #45959, 5.000000000000000000 ) ;
#10536 = CARTESIAN_POINT ( 'NONE',  ( -3.280815508853482498, -7.221948645665452915, -7.591546097228404122 ) ) ;
#10537 = CARTESIAN_POINT ( 'NONE',  ( 4.458734124999998549, -1.979166665301068662, -2.574251347313721627 ) ) ;
#10538 =( BOUNDED_CURVE ( )  B_SPLINE_CURVE ( 2, ( #15854, #20689, #12923, #32224, #51855, #47651, #3605, #18064, #37686 ),
 .UNSPECIFIED., .F., .F. ) 
 B_SPLINE_CURVE_WITH_KNOTS ( ( 3, 2, 2, 2, 3 ),
 ( 0.2410714285714285754, 0.2416666666666666685, 0.2428571428571428548, 0.2440476190476190410, 0.2446428571428571341 ),
 .UNSPECIFIED. ) 
 CURVE ( )  GEOMETRIC_REPRESENTATION_ITEM ( )  RATIONAL_B_SPLINE_CURVE ( ( 0.9330127018922194093, 0.9330127018922194093, 1.000000000000000000, 0.8660254037844387076, 1.000000000000000000, 0.8660254037844387076, 1.000000000000000000, 0.9330127018922194093, 0.9330127018922194093 ) ) 
 REPRESENTATION_ITEM ( '' )  );
#10539 = ORIENTED_EDGE ( 'NONE', *, *, #27184, .T. ) ;
#10540 = CARTESIAN_POINT ( 'NONE',  ( 3.061616997868383141E-16, -145.7500000000000284, -5.000000000000000000 ) ) ;
#10541 = CARTESIAN_POINT ( 'NONE',  ( -1.339745962155610925, -14.66965819600733667, 5.000000000000000000 ) ) ;
#10543 = CARTESIAN_POINT ( 'NONE',  ( 2.229367062499998831, -37.64583333196773651, -3.861377020970580887 ) ) ;
#10542 = CARTESIAN_POINT ( 'NONE',  ( 4.458734124999999437, -86.81249999863439371, -5.460374474430324690E-16 ) ) ;
#10544 = CARTESIAN_POINT ( 'NONE',  ( -51.75738570946856498, -143.8750000027312126, 3.805975901505576964 ) ) ;
#10545 = CARTESIAN_POINT ( 'NONE',  ( 2.229367062499998831, -78.89583333196773651, -3.861377020970580887 ) ) ;
#10546 = CARTESIAN_POINT ( 'NONE',  ( 4.458734125000000326, 17.85416666803225993, 2.574251347313718519 ) ) ;
#10547 = CARTESIAN_POINT ( 'NONE',  ( -1.339745962155613812, -53.20534180126147561, -5.000000000000000000 ) ) ;
#10548 = EDGE_CURVE ( 'NONE', #59225, #44836, #54306, .T. ) ;
#10549 = CARTESIAN_POINT ( 'NONE',  ( -55.35523342533222291, -138.3125000013656063, 4.444560631937231499 ) ) ;
#10550 = CARTESIAN_POINT ( 'NONE',  ( -2.229367062500000163, -2.479166665301069106, -3.861377020970580443 ) ) ;
#10551 = CARTESIAN_POINT ( 'NONE',  ( -2.229367062500000163, 21.27083333469892779, -3.861377020970580443 ) ) ;
#10552 = CARTESIAN_POINT ( 'NONE',  ( -3.152548672688508926E-16, -48.81249999863440792, -5.148502694627439702 ) ) ;
#10553 = CARTESIAN_POINT ( 'NONE',  ( -1.339745962155613812, -46.08034179853028434, -5.000000000000000000 ) ) ;
#10554 = CARTESIAN_POINT ( 'NONE',  ( 4.458734125000000326, -3.895833331967739177, 2.574251347313718519 ) ) ;
#10555 = CARTESIAN_POINT ( 'NONE',  ( 2.229367062500001939, -29.22916666530107221, 3.861377020970579999 ) ) ;
#10556 = CARTESIAN_POINT ( 'NONE',  ( -50.70258187064364108, -132.3750000013656347, 2.196230717870141014 ) ) ;
#10557 = CARTESIAN_POINT ( 'NONE',  ( -2.229367062499996610, -75.14583333196773651, 3.861377020970582219 ) ) ;
#10558 = CARTESIAN_POINT ( 'NONE',  ( -3.535250795749689387E-16, -105.1249999972688158, -5.773502691896257311 ) ) ;
#10559 = CARTESIAN_POINT ( 'NONE',  ( 4.458734124999998549, 26.27083333469893134, -2.574251347313721627 ) ) ;
#10560 = CARTESIAN_POINT ( 'NONE',  ( 5.000000000000000000, 26.62500000273118772, -6.123233995736766282E-16 ) ) ;
#10561 = ADVANCED_FACE ( 'NONE', ( #57264 ), #50562, .T. ) ;
#10562 = CARTESIAN_POINT ( 'NONE',  ( 6.123233995736766282E-16, -120.0000000000000000, -5.000000000000000000 ) ) ;
#10563 = CARTESIAN_POINT ( 'NONE',  ( -4.458734124999999437, -75.64583333196773651, -2.574251347313719407 ) ) ;
#10564 = CARTESIAN_POINT ( 'NONE',  ( -2.500000000000000444, -57.16666666666667140, -4.330127018922193649 ) ) ;
#10565 = CARTESIAN_POINT ( 'NONE',  ( -6.972266317189433020E-16, -75.25000000000000000, -5.000000000000000000 ) ) ;
#10566 = CARTESIAN_POINT ( 'NONE',  ( -5.000000000000000000, 22.12500000273118417, 0.000000000000000000 ) ) ;
#10567 = ORIENTED_EDGE ( 'NONE', *, *, #10240, .F. ) ;
#10568 = FACE_OUTER_BOUND ( 'NONE', #9404, .T. ) ;
#10569 =( BOUNDED_CURVE ( )  B_SPLINE_CURVE ( 2, ( #55480, #6271, #16863, #40985, #56109, #12031, #25878, #35855, #11397 ),
 .UNSPECIFIED., .F., .F. ) 
 B_SPLINE_CURVE_WITH_KNOTS ( ( 3, 2, 2, 2, 3 ),
 ( 0.09791666666666666574, 0.09861111111111110772, 0.1000000000000000056, 0.1013888888888888895, 0.1020833333333333315 ),
 .UNSPECIFIED. ) 
 CURVE ( )  GEOMETRIC_REPRESENTATION_ITEM ( )  RATIONAL_B_SPLINE_CURVE ( ( 0.9330127018922194093, 0.9330127018922194093, 1.000000000000000000, 0.8660254037844387076, 1.000000000000000000, 0.8660254037844387076, 1.000000000000000000, 0.9330127018922194093, 0.9330127018922194093 ) ) 
 REPRESENTATION_ITEM ( '' )  );
#10570 = CARTESIAN_POINT ( 'NONE',  ( 1.975475456537005874E-15, -56.62499999726880162, 5.000000000000000000 ) ) ;
#10571 = CARTESIAN_POINT ( 'NONE',  ( 2.500000000000002220, -20.66666666666666785, 4.330127018922192761 ) ) ;
#10572 = CARTESIAN_POINT ( 'NONE',  ( -3.152548672688508926E-16, -22.56249999863440081, -5.148502694627439702 ) ) ;
#10573 = CARTESIAN_POINT ( 'NONE',  ( 2.229367062500001939, -82.97916666530106511, 3.861377020970579999 ) ) ;
#10574 = CARTESIAN_POINT ( 'NONE',  ( -5.000000000000000000, -24.95833333060214798, -2.886751345948128211 ) ) ;
#10576 = ORIENTED_EDGE ( 'NONE', *, *, #10882, .T. ) ;
#10575 = CARTESIAN_POINT ( 'NONE',  ( -4.458734124999998549, -49.22916666530106511, 2.574251347313722516 ) ) ;
#10577 = DIRECTION ( 'NONE',  ( -0.000000000000000000, 1.000000000000000000, -0.000000000000000000 ) ) ;
#10579 = VERTEX_POINT ( 'NONE', #1839 ) ;
#10578 = CARTESIAN_POINT ( 'NONE',  ( -4.458734124999999437, 2.354166668032262599, -2.574251347313719407 ) ) ;
#10580 = CARTESIAN_POINT ( 'NONE',  ( -57.89159099828107458, -150.6875000013656063, -3.393966926194107447 ) ) ;
#10581 = CARTESIAN_POINT ( 'NONE',  ( -3.535250795749689387E-16, -66.25000000000000000, -5.773502691896257311 ) ) ;
#10582 = CARTESIAN_POINT ( 'NONE',  ( -4.458734125000000326, -153.2500000013655779, -1.846868145590735644 ) ) ;
#10583 = CARTESIAN_POINT ( 'NONE',  ( -4.458734124999999437, -47.56249999863440792, 0.000000000000000000 ) ) ;
#10584 = CARTESIAN_POINT ( 'NONE',  ( 1.062108568985190270E-13, -27.25000000000000000, -4.999999999999999112 ) ) ;
#10585 = CARTESIAN_POINT ( 'NONE',  ( -9.184850993605147944E-16, -159.2500000000000000, 5.000000000000000000 ) ) ;
#10586 = CARTESIAN_POINT ( 'NONE',  ( 1.975475456537005874E-15, 7.375000002731186832, 5.000000000000000000 ) ) ;
#10587 = CARTESIAN_POINT ( 'NONE',  ( -60.14911071818854538, -152.0625000000000000, 1.666127454062681368 ) ) ;
#10588 = ADVANCED_FACE ( 'NONE', ( #25941 ), #21442, .T. ) ;
#10589 = CARTESIAN_POINT ( 'NONE',  ( 9.457646018065525792E-16, -9.312499998634406140, 5.148502694627439702 ) ) ;
#10590 = CARTESIAN_POINT ( 'NONE',  ( 4.458734124999999437, -47.06249999863440792, -5.460374474430324690E-16 ) ) ;
#10591 = CARTESIAN_POINT ( 'NONE',  ( 1.975475456537005874E-15, -89.74999999999998579, 5.000000000000000000 ) ) ;
#10592 = CARTESIAN_POINT ( 'NONE',  ( -3.152801135295367985, -145.8125000013655779, 3.152801135295367096 ) ) ;
#10593 = CARTESIAN_POINT ( 'NONE',  ( 2.229367062499998831, -95.89583333196773651, -3.861377020970580887 ) ) ;
#10594 = CARTESIAN_POINT ( 'NONE',  ( -1.339745962155610925, -106.7946581987385173, 5.000000000000000000 ) ) ;
#10595 = ORIENTED_EDGE ( 'NONE', *, *, #3493, .F. ) ;
#10596 = CARTESIAN_POINT ( 'NONE',  ( -2.500000000000000444, -32.16666666666666430, -4.330127018922193649 ) ) ;
#10597 = CARTESIAN_POINT ( 'NONE',  ( -4.458734124999999437, 28.35416666803226349, -2.574251347313719407 ) ) ;
#10598 = CARTESIAN_POINT ( 'NONE',  ( -56.66612745406270335, -148.4375000027312126, -5.149110718188516067 ) ) ;
#10599 = CARTESIAN_POINT ( 'NONE',  ( 1.339745962155615144, -29.58034179853029499, 4.999999999999999112 ) ) ;
#10600 = ORIENTED_EDGE ( 'NONE', *, *, #51497, .T. ) ;
#10601 = CARTESIAN_POINT ( 'NONE',  ( -4.458734124999999437, 2.604166668032263043, -2.574251347313719407 ) ) ;
#10602 = VECTOR ( 'NONE', #15116, 1000.000000000000000 ) ;
#10603 = CARTESIAN_POINT ( 'NONE',  ( 2.500000000000002220, -106.6666666666666572, 4.330127018922192761 ) ) ;
#10604 = CARTESIAN_POINT ( 'NONE',  ( -4.458734124999998549, -16.47916666530107577, 2.574251347313722516 ) ) ;
#10605 = EDGE_CURVE ( 'NONE', #62971, #53159, #25944, .T. ) ;
#10606 = CARTESIAN_POINT ( 'NONE',  ( -2.499999999999996447, -100.8333333333333286, 4.330127018922195425 ) ) ;
#10608 = EDGE_CURVE ( 'NONE', #3031, #6430, #56773, .T. ) ;
#10607 = CARTESIAN_POINT ( 'NONE',  ( 4.458734124999998549, -9.729166665301068662, -2.574251347313721627 ) ) ;
#10609 = CARTESIAN_POINT ( 'NONE',  ( -4.458734124999999437, -90.43749999863440792, 0.000000000000000000 ) ) ;
#10610 = CARTESIAN_POINT ( 'NONE',  ( 4.458734124999999437, -147.3750000013656063, -1.846868145590734978 ) ) ;
#10611 = CARTESIAN_POINT ( 'NONE',  ( 4.458734125000000326, 17.85416666803225993, 2.574251347313718519 ) ) ;
#10612 = ORIENTED_EDGE ( 'NONE', *, *, #33487, .F. ) ;
#10613 = CARTESIAN_POINT ( 'NONE',  ( -4.458734124999997661, -96.22916666530105090, 2.574251347313722516 ) ) ;
#10614 = CARTESIAN_POINT ( 'NONE',  ( -2.500000000000000444, -19.04166666393547658, -4.330127018922193649 ) ) ;
#10615 = CARTESIAN_POINT ( 'NONE',  ( 0.000000000000000000, -120.0000000000000000, 0.000000000000000000 ) ) ;
#10616 = CARTESIAN_POINT ( 'NONE',  ( 4.458734124999999437, -16.81249999863440436, -5.460374474430324690E-16 ) ) ;
#10617 = CARTESIAN_POINT ( 'NONE',  ( 5.000000000000000000, -85.37499999726880162, -6.123233995736766282E-16 ) ) ;
#10618 = CARTESIAN_POINT ( 'NONE',  ( 2.500000000000002220, -3.666666666666665186, 4.330127018922192761 ) ) ;
#10619 = CARTESIAN_POINT ( 'NONE',  ( -50.40829686548195099, -148.0000000013655779, -1.485763867205728284 ) ) ;
#10620 = CARTESIAN_POINT ( 'NONE',  ( -2.500000000000000444, -44.04166666393546592, -4.330127018922193649 ) ) ;
#10621 = CARTESIAN_POINT ( 'NONE',  ( -55.00000000000002132, -155.0000000000000284, 1.734723475976807094E-15 ) ) ;
#10622 = CARTESIAN_POINT ( 'NONE',  ( -4.458734124999999437, 12.68750000136559564, 0.000000000000000000 ) ) ;
#10623 = CARTESIAN_POINT ( 'NONE',  ( -4.999999999999998224, -89.79166666393547303, 2.886751345948131764 ) ) ;
#10624 = PLANE ( 'NONE',  #38688 ) ;
#10625 = CARTESIAN_POINT ( 'NONE',  ( 4.458734124999998549, 12.27083333469892423, -2.574251347313721627 ) ) ;
#10626 = CARTESIAN_POINT ( 'NONE',  ( -3.152548672688508926E-16, -62.56249999863440792, -5.148502694627439702 ) ) ;
#10627 = ORIENTED_EDGE ( 'NONE', *, *, #46144, .T. ) ;
#10628 = CARTESIAN_POINT ( 'NONE',  ( 2.229367062500001939, -14.22916666530107221, 3.861377020970579999 ) ) ;
#10629 = CARTESIAN_POINT ( 'NONE',  ( -2.499999999999996447, 7.166666666666665186, 4.330127018922195425 ) ) ;
#10630 = CARTESIAN_POINT ( 'NONE',  ( 4.458734125000000326, -163.3750000013656347, -1.846868145590734978 ) ) ;
#10631 = CARTESIAN_POINT ( 'NONE',  ( -4.999999999999998224, -98.79166666393544460, 2.886751345948131764 ) ) ;
#10632 = CARTESIAN_POINT ( 'NONE',  ( -4.458734124999999437, -57.31249999863440081, 0.000000000000000000 ) ) ;
#10633 = CARTESIAN_POINT ( 'NONE',  ( 5.000000000000000000, -88.37499999726880162, -6.123233995736766282E-16 ) ) ;
#10634 = EDGE_CURVE ( 'NONE', #50889, #46232, #13176, .T. ) ;
#10635 = CARTESIAN_POINT ( 'NONE',  ( -4.458734124999999437, -32.31249999863440792, 0.000000000000000000 ) ) ;
#10636 = DIRECTION ( 'NONE',  ( -0.000000000000000000, 1.000000000000000000, -0.000000000000000000 ) ) ;
#10637 = CARTESIAN_POINT ( 'NONE',  ( -6.972266317189433020E-16, -55.12499999726880873, -5.000000000000000000 ) ) ;
#10638 = CARTESIAN_POINT ( 'NONE',  ( -4.999999999999998224, -107.7916666639354730, 2.886751345948131764 ) ) ;
#10639 = CYLINDRICAL_SURFACE ( 'NONE', #50267, 5.000000000000000000 ) ;
#10640 = CARTESIAN_POINT ( 'NONE',  ( -4.458734124999999437, -154.1875000013656063, -5.460374474430324690E-16 ) ) ;
#10641 = CARTESIAN_POINT ( 'NONE',  ( 5.000000000000000000, -43.41666666666666430, -2.886751345948129988 ) ) ;
#10642 = CARTESIAN_POINT ( 'NONE',  ( -5.000000000000000000, 18.91666666666666430, -2.886751345948128211 ) ) ;
#10643 = CARTESIAN_POINT ( 'NONE',  ( -6.972266317189433020E-16, -68.12499999726881583, -5.000000000000000000 ) ) ;
#10644 = ORIENTED_EDGE ( 'NONE', *, *, #42935, .F. ) ;
#10645 = CARTESIAN_POINT ( 'NONE',  ( 2.229367062500001939, -101.9791666653010651, 3.861377020970579999 ) ) ;
#10646 = CARTESIAN_POINT ( 'NONE',  ( 2.229367062500001939, 4.770833334698926897, 3.861377020970579999 ) ) ;
#10647 = FACE_OUTER_BOUND ( 'NONE', #61401, .T. ) ;
#10648 = CARTESIAN_POINT ( 'NONE',  ( -5.000000000000000000, -4.083333333333334814, -2.886751345948128211 ) ) ;
#10649 = CARTESIAN_POINT ( 'NONE',  ( -4.458734124999999437, -65.39583333196773651, -2.574251347313719407 ) ) ;
#10650 = VECTOR ( 'NONE', #28561, 1000.000000000000000 ) ;
#10651 = CARTESIAN_POINT ( 'NONE',  ( -54.60164318462004474, -147.5000000027312126, -4.984105922594373794 ) ) ;
#10652 = CARTESIAN_POINT ( 'NONE',  ( -5.000000000000000000, -6.874999997268812280, 0.000000000000000000 ) ) ;
#10654 = ORIENTED_EDGE ( 'NONE', *, *, #38067, .T. ) ;
#10653 = CARTESIAN_POINT ( 'NONE',  ( -3.152548672688508926E-16, -32.56249999863440792, -5.148502694627439702 ) ) ;
#10655 = CARTESIAN_POINT ( 'NONE',  ( 1.975475456537005874E-15, -76.75000000000000000, 5.000000000000000000 ) ) ;
#10656 = CARTESIAN_POINT ( 'NONE',  ( -1.339745962155610925, -16.66965819600733312, 5.000000000000000000 ) ) ;
#10657 = VERTEX_POINT ( 'NONE', #22718 ) ;
#10658 = LINE ( 'NONE', #60840, #50469 ) ;
#10659 = CARTESIAN_POINT ( 'NONE',  ( -2.500000000000000444, -51.16666666666666430, -4.330127018922193649 ) ) ;
#10661 = CARTESIAN_POINT ( 'NONE',  ( -2.229367062499996610, -28.39583333196774007, 3.861377020970582219 ) ) ;
#10660 = CARTESIAN_POINT ( 'NONE',  ( 1.339745962155612702, -46.16965819600732601, -5.000000000000000000 ) ) ;
#10662 = CARTESIAN_POINT ( 'NONE',  ( 5.000000000000000000, -32.37499999726880873, -6.123233995736766282E-16 ) ) ;
#10663 = CARTESIAN_POINT ( 'NONE',  ( -2.229367062500000163, -74.47916666530106511, -3.861377020970580443 ) ) ;
#10664 = CARTESIAN_POINT ( 'NONE',  ( 1.846868145590736310, -145.8750000013656063, 4.458734124999999437 ) ) ;
#10665 = CARTESIAN_POINT ( 'NONE',  ( -4.458734124999999437, -84.31249999863439371, 0.000000000000000000 ) ) ;
#10666 = CARTESIAN_POINT ( 'NONE',  ( -56.48576386720575471, -138.0000000013656063, -4.591703134518078322 ) ) ;
#10667 = CARTESIAN_POINT ( 'NONE',  ( -4.458734124999999437, -29.64583333196773651, -2.574251347313719407 ) ) ;
#10668 =( BOUNDED_CURVE ( )  B_SPLINE_CURVE ( 2, ( #20054, #10403, #49323, #39980, #35178, #39658, #44170, #30331, #49957 ),
 .UNSPECIFIED., .F., .F. ) 
 B_SPLINE_CURVE_WITH_KNOTS ( ( 3, 2, 2, 2, 3 ),
 ( 0.07321428571428571785, 0.07380952380952381098, 0.07499999999999999722, 0.07619047619047619735, 0.07678571428571429047 ),
 .UNSPECIFIED. ) 
 CURVE ( )  GEOMETRIC_REPRESENTATION_ITEM ( )  RATIONAL_B_SPLINE_CURVE ( ( 0.9330127018922194093, 0.9330127018922194093, 1.000000000000000000, 0.8660254037844387076, 1.000000000000000000, 0.8660254037844387076, 1.000000000000000000, 0.9330127018922194093, 0.9330127018922194093 ) ) 
 REPRESENTATION_ITEM ( '' )  );
#10670 = ORIENTED_EDGE ( 'NONE', *, *, #9855, .F. ) ;
#10669 = EDGE_CURVE ( 'NONE', #31572, #51345, #52299, .T. ) ;
#10671 = EDGE_CURVE ( 'NONE', #14391, #7881, #41910, .T. ) ;
#10672 = DIRECTION ( 'NONE',  ( -0.000000000000000000, 1.000000000000000000, -0.000000000000000000 ) ) ;
#10673 = ORIENTED_EDGE ( 'NONE', *, *, #49606, .T. ) ;
#10674 = CARTESIAN_POINT ( 'NONE',  ( 4.458734124999998549, -74.97916666530106511, -2.574251347313721627 ) ) ;
#10675 = CARTESIAN_POINT ( 'NONE',  ( 1.339745962155615144, -21.70534180126147916, 4.999999999999999112 ) ) ;
#10676 = EDGE_CURVE ( 'NONE', #17081, #48474, #21444, .T. ) ;
#10677 = ORIENTED_EDGE ( 'NONE', *, *, #23458, .F. ) ;
#10678 = CARTESIAN_POINT ( 'NONE',  ( -50.18089887299976937, -140.6875000000000284, 2.462841084822397164 ) ) ;
#10679 = EDGE_CURVE ( 'NONE', #57284, #54893, #23658, .T. ) ;
#10680 = CARTESIAN_POINT ( 'NONE',  ( -2.500000000000000444, 7.833333333333334814, -4.330127018922193649 ) ) ;
#10681 = CARTESIAN_POINT ( 'NONE',  ( 4.458734125000001214, -62.14583333196774362, 2.574251347313718519 ) ) ;
#10682 = ADVANCED_FACE ( 'NONE', ( #56815 ), #10093, .T. ) ;
#10683 = CARTESIAN_POINT ( 'NONE',  ( 2.229367062499998831, -2.895833331967738289, -3.861377020970580887 ) ) ;
#10684 = ORIENTED_EDGE ( 'NONE', *, *, #893, .T. ) ;
#10685 = ADVANCED_FACE ( 'NONE', ( #33299 ), #62271, .F. ) ;
#10686 = CARTESIAN_POINT ( 'NONE',  ( -2.499999999999996447, 3.291666669397851575, 4.330127018922195425 ) ) ;
#10687 = CARTESIAN_POINT ( 'NONE',  ( -2.500000000000000444, -45.16666666666665719, -4.330127018922193649 ) ) ;
#10688 = EDGE_CURVE ( 'NONE', #45629, #43365, #12798, .T. ) ;
#10689 = ADVANCED_FACE ( 'NONE', ( #14615 ), #15261, .T. ) ;
#10690 = CARTESIAN_POINT ( 'NONE',  ( -3.152548672688508926E-16, 12.43750000136559564, -5.148502694627439702 ) ) ;
#10691 = CARTESIAN_POINT ( 'NONE',  ( -54.64476657466781973, -141.8125000013656063, -4.444560631937228834 ) ) ;
#10692 = CARTESIAN_POINT ( 'NONE',  ( -58.80597590150559739, -155.0000000000000284, 3.242614290531457666 ) ) ;
#10693 = CARTESIAN_POINT ( 'NONE',  ( 3.152801135295366208, -161.5625000013656063, 3.152801135295367985 ) ) ;
#10694 = CARTESIAN_POINT ( 'NONE',  ( -6.972266317189433020E-16, -102.1249999972688158, -5.000000000000000000 ) ) ;
#10696 = EDGE_CURVE ( 'NONE', #54583, #15515, #27, .T. ) ;
#10695 = ORIENTED_EDGE ( 'NONE', *, *, #37272, .T. ) ;
#10697 = CARTESIAN_POINT ( 'NONE',  ( 9.457646018065525792E-16, -81.06249999863440792, 5.148502694627439702 ) ) ;
#10698 = EDGE_CURVE ( 'NONE', #2721, #18523, #55299, .T. ) ;
#10699 = CARTESIAN_POINT ( 'NONE',  ( 2.499999999999998668, -75.33333333333332860, -4.330127018922193649 ) ) ;
#10700 = CARTESIAN_POINT ( 'NONE',  ( -3.152548672688508926E-16, -0.5624999986344053626, -5.148502694627439702 ) ) ;
#10701 = CARTESIAN_POINT ( 'NONE',  ( -58.24261429053147765, -147.2500000000000284, -3.805975901505573855 ) ) ;
#10702 = VECTOR ( 'NONE', #21226, 1000.000000000000000 ) ;
#10703 = CARTESIAN_POINT ( 'NONE',  ( 2.500000000000002220, -36.66666666666666430, 4.330127018922192761 ) ) ;
#10704 = CARTESIAN_POINT ( 'NONE',  ( -4.458734124999999437, -71.64583333196773651, -2.574251347313719407 ) ) ;
#10705 = CARTESIAN_POINT ( 'NONE',  ( 2.499999999999998668, -27.20833333060214798, -4.330127018922193649 ) ) ;
#10706 = CARTESIAN_POINT ( 'NONE',  ( -2.500000000000000444, -73.04166666393548724, -4.330127018922193649 ) ) ;
#10707 = CARTESIAN_POINT ( 'NONE',  ( 2.499999999999998668, -78.20833333060214443, -4.330127018922193649 ) ) ;
#10708 = CARTESIAN_POINT ( 'NONE',  ( 1.975475456537005874E-15, -110.6249999972688158, 5.000000000000000000 ) ) ;
#10709 = PLANE ( 'NONE',  #8998 ) ;
#10710 = CARTESIAN_POINT ( 'NONE',  ( 2.229367062499998831, -44.64583333196774362, -3.861377020970580887 ) ) ;
#10711 = CARTESIAN_POINT ( 'NONE',  ( -2.229367062499996610, -34.39583333196772941, 3.861377020970582219 ) ) ;
#10712 = CARTESIAN_POINT ( 'NONE',  ( -4.458734124999999437, 0.4375000013655955255, 0.000000000000000000 ) ) ;
#10713 = CARTESIAN_POINT ( 'NONE',  ( -5.000000000000000000, -161.6250000027311842, -6.123233995736766282E-16 ) ) ;
#10714 = CARTESIAN_POINT ( 'NONE',  ( -5.000000000000000000, 23.00000000000000000, 0.000000000000000000 ) ) ;
#10715 = CARTESIAN_POINT ( 'NONE',  ( -2.071067811865478170, -147.4375000027312410, 5.000000000000000000 ) ) ;
#10716 = LINE ( 'NONE', #438, #33604 ) ;
#10717 = CARTESIAN_POINT ( 'NONE',  ( -4.458734124999998549, -38.22916666530107932, 2.574251347313722516 ) ) ;
#10718 = CARTESIAN_POINT ( 'NONE',  ( -4.999999999999999112, -74.79166666393547303, 2.886751345948131764 ) ) ;
#10719 = CARTESIAN_POINT ( 'NONE',  ( -57.89159099828107458, -144.9375000013656063, -3.393966926194107447 ) ) ;
#10720 = CARTESIAN_POINT ( 'NONE',  ( 2.500000000000002220, -24.54166666393548368, 4.330127018922192761 ) ) ;
#10721 = LINE ( 'NONE', #25513, #27505 ) ;
#10722 = CARTESIAN_POINT ( 'NONE',  ( -3.152548672688508926E-16, -81.81249999863440792, -5.148502694627439702 ) ) ;
#10723 = CARTESIAN_POINT ( 'NONE',  ( -4.458734124999999437, -164.2500000013656063, -1.846868145590735644 ) ) ;
#10724 =( BOUNDED_CURVE ( )  B_SPLINE_CURVE ( 2, ( #46674, #46036, #8080, #60843, #61795, #51511, #32506, #37649, #52138 ),
 .UNSPECIFIED., .F., .F. ) 
 B_SPLINE_CURVE_WITH_KNOTS ( ( 3, 2, 2, 2, 3 ),
 ( 0.2839285714285714191, 0.2845238095238095122, 0.2857142857142856984, 0.2869047619047618847, 0.2874999999999999778 ),
 .UNSPECIFIED. ) 
 CURVE ( )  GEOMETRIC_REPRESENTATION_ITEM ( )  RATIONAL_B_SPLINE_CURVE ( ( 0.9330127018922194093, 0.9330127018922194093, 1.000000000000000000, 0.8660254037844387076, 1.000000000000000000, 0.8660254037844387076, 1.000000000000000000, 0.9330127018922194093, 0.9330127018922194093 ) ) 
 REPRESENTATION_ITEM ( '' )  );
#10725 = CARTESIAN_POINT ( 'NONE',  ( -2.071067811865580754, -159.8125000027311842, -4.999999999999894307 ) ) ;
#10726 = CARTESIAN_POINT ( 'NONE',  ( -5.000000000000000000, -26.00000000000000355, 0.000000000000000000 ) ) ;
#10727 = CARTESIAN_POINT ( 'NONE',  ( -4.458734125000001214, -144.8750000013655779, 1.846868145590734089 ) ) ;
#10728 = ORIENTED_EDGE ( 'NONE', *, *, #61829, .F. ) ;
#10729 = CARTESIAN_POINT ( 'NONE',  ( 9.457646018065525792E-16, 21.68750000136559208, 5.148502694627439702 ) ) ;
#10730 = ORIENTED_EDGE ( 'NONE', *, *, #58870, .T. ) ;
#10731 = CARTESIAN_POINT ( 'NONE',  ( -4.458734124999999437, -64.56249999863440792, 0.000000000000000000 ) ) ;
#10732 =( BOUNDED_CURVE ( )  B_SPLINE_CURVE ( 2, ( #31006, #12021, #56101, #41285, #31651, #7219, #34772, #25437, #54397 ),
 .UNSPECIFIED., .F., .F. ) 
 B_SPLINE_CURVE_WITH_KNOTS ( ( 3, 2, 2, 2, 3 ),
 ( 0.2732142857142857428, 0.2738095238095238360, 0.2750000000000000222, 0.2761904761904762085, 0.2767857142857143016 ),
 .UNSPECIFIED. ) 
 CURVE ( )  GEOMETRIC_REPRESENTATION_ITEM ( )  RATIONAL_B_SPLINE_CURVE ( ( 0.9330127018922194093, 0.9330127018922225179, 1.000000000000000000, 0.8660254037844387076, 1.000000000000000000, 0.8660254037844387076, 1.000000000000000000, 0.9330127018922194093, 0.9330127018922194093 ) ) 
 REPRESENTATION_ITEM ( '' )  );
#10733 = CARTESIAN_POINT ( 'NONE',  ( -5.000000000000000000, 19.12500000273118772, 0.000000000000000000 ) ) ;
#10734 = DIRECTION ( 'NONE',  ( 0.000000000000000000, 0.000000000000000000, 1.000000000000000000 ) ) ;
#10735 = CARTESIAN_POINT ( 'NONE',  ( 5.000000000000000000, 12.50000000000000000, -6.123233995736766282E-16 ) ) ;
#10736 = CARTESIAN_POINT ( 'NONE',  ( -4.458734124999997661, -51.22916666530107932, 2.574251347313722516 ) ) ;
#10737 = CARTESIAN_POINT ( 'NONE',  ( -3.152548672688508926E-16, -9.562499998634406140, -5.148502694627439702 ) ) ;
#10738 = CARTESIAN_POINT ( 'NONE',  ( 3.535533905932738197, -166.0000000027312126, -3.535533905932738197 ) ) ;
#10739 = CARTESIAN_POINT ( 'NONE',  ( 1.339745962155615144, 15.41965820146970678, 4.999999999999999112 ) ) ;
#10740 = CARTESIAN_POINT ( 'NONE',  ( -5.000000000000000000, 0.000000000000000000, 0.000000000000000000 ) ) ;
#10741 = CARTESIAN_POINT ( 'NONE',  ( 2.500000000000002220, 28.45833333606451987, 4.330127018922192761 ) ) ;
#10742 = CARTESIAN_POINT ( 'NONE',  ( 0.000000000000000000, -120.0000000000000000, 5.000000000000000000 ) ) ;
#10744 = CARTESIAN_POINT ( 'NONE',  ( 2.229367062500001939, -20.97916666530107221, 3.861377020970579999 ) ) ;
#10743 = CARTESIAN_POINT ( 'NONE',  ( 6.123233995736766282E-16, -170.0000000000000000, -5.000000000000000000 ) ) ;
#10745 = CARTESIAN_POINT ( 'NONE',  ( 1.975475456537005874E-15, -77.62499999726881583, 5.000000000000000000 ) ) ;
#10746 = CARTESIAN_POINT ( 'NONE',  ( 4.458734125000001214, -58.89583333196773651, 2.574251347313718519 ) ) ;
#10747 = CARTESIAN_POINT ( 'NONE',  ( 1.846868145590735200, -156.5000000013656347, -4.458734125000000326 ) ) ;
#10748 = AXIS2_PLACEMENT_3D ( 'NONE', #23572, #28067, #32258 ) ;
#10749 = CARTESIAN_POINT ( 'NONE',  ( -5.000000000000000000, -56.95833333060214443, -2.886751345948128211 ) ) ;
#10750 = ORIENTED_EDGE ( 'NONE', *, *, #24396, .T. ) ;
#10751 = CARTESIAN_POINT ( 'NONE',  ( 5.000000000000000000, 13.49999999999999822, -6.123233995736766282E-16 ) ) ;
#10752 = CARTESIAN_POINT ( 'NONE',  ( 4.458734124999998549, 2.020833334698927786, -2.574251347313721627 ) ) ;
#10753 = ORIENTED_EDGE ( 'NONE', *, *, #34641, .T. ) ;
#10754 =( BOUNDED_CURVE ( )  B_SPLINE_CURVE ( 2, ( #37870, #36922, #62643, #18562, #13106, #12472, #42998, #42366, #38185 ),
 .UNSPECIFIED., .F., .F. ) 
 B_SPLINE_CURVE_WITH_KNOTS ( ( 3, 2, 2, 2, 3 ),
 ( 0.2354166666666666630, 0.2361111111111111049, 0.2374999999999999889, 0.2388888888888889006, 0.2395833333333333426 ),
 .UNSPECIFIED. ) 
 CURVE ( )  GEOMETRIC_REPRESENTATION_ITEM ( )  RATIONAL_B_SPLINE_CURVE ( ( 0.9330127018922194093, 0.9330127018922194093, 1.000000000000000000, 0.8660254037844387076, 1.000000000000000000, 0.8660254037844387076, 1.000000000000000000, 0.9330127018922194093, 0.9330127018922194093 ) ) 
 REPRESENTATION_ITEM ( '' )  );
#10756 = CARTESIAN_POINT ( 'NONE',  ( -6.972266317189433020E-16, -3.250000000000001332, -5.000000000000000000 ) ) ;
#10755 = FACE_OUTER_BOUND ( 'NONE', #1056, .T. ) ;
#10757 = CARTESIAN_POINT ( 'NONE',  ( 4.458734124999999437, -156.4375000013655779, 0.000000000000000000 ) ) ;
#10758 = ORIENTED_EDGE ( 'NONE', *, *, #63339, .F. ) ;
#10759 = CARTESIAN_POINT ( 'NONE',  ( -54.60164318462004474, -131.3750000000000284, -4.984105922594373794 ) ) ;
#10760 = CARTESIAN_POINT ( 'NONE',  ( -4.458734124999999437, -90.31249999863440792, 0.000000000000000000 ) ) ;
#10761 = CARTESIAN_POINT ( 'NONE',  ( -4.458734124999999437, -43.56249999863440081, 0.000000000000000000 ) ) ;
#10762 = EDGE_LOOP ( 'NONE', ( #61650, #42630, #333, #803 ) ) ;
#10763 = CARTESIAN_POINT ( 'NONE',  ( -1.339745962155613812, -46.20534180126146850, -5.000000000000000000 ) ) ;
#10764 = CARTESIAN_POINT ( 'NONE',  ( 2.229367062499998831, 15.35416666803225993, -3.861377020970580887 ) ) ;
#10765 = EDGE_CURVE ( 'NONE', #17081, #60982, #56311, .T. ) ;
#10766 = CARTESIAN_POINT ( 'NONE',  ( -2.229367062500000163, 29.52083333469892779, -3.861377020970580443 ) ) ;
#10767 = CARTESIAN_POINT ( 'NONE',  ( -57.89159099828107458, -151.6875000013656063, -3.393966926194107447 ) ) ;
#10768 = CYLINDRICAL_SURFACE ( 'NONE', #21306, 5.000000000000000000 ) ;
#10769 = CARTESIAN_POINT ( 'NONE',  ( 7.500000000000000000, 2.886751345948125547, -7.198902722707427593 ) ) ;
#10770 =( BOUNDED_CURVE ( )  B_SPLINE_CURVE ( 2, ( #22530, #56939, #42126, #17696, #37310 ),
 .UNSPECIFIED., .F., .F. ) 
 B_SPLINE_CURVE_WITH_KNOTS ( ( 3, 2, 3 ),
 ( 0.000000000000000000, 0.001388888888888888942, 0.002083333333333333738 ),
 .UNSPECIFIED. ) 
 CURVE ( )  GEOMETRIC_REPRESENTATION_ITEM ( )  RATIONAL_B_SPLINE_CURVE ( ( 1.000000000000000000, 0.8660254037844387076, 1.000000000000000000, 0.9330127018922192983, 0.9330127018922194093 ) ) 
 REPRESENTATION_ITEM ( '' )  );
#10771 = CARTESIAN_POINT ( 'NONE',  ( 6.123233995736766282E-16, -170.0000000000000000, -5.000000000000000000 ) ) ;
#10772 = CARTESIAN_POINT ( 'NONE',  ( 9.457646018065525792E-16, -63.06249999863440792, 5.148502694627439702 ) ) ;
#10773 = CARTESIAN_POINT ( 'NONE',  ( 6.484173630542770184, 4.916614646782027087, -7.642786413619098163 ) ) ;
#10774 = CARTESIAN_POINT ( 'NONE',  ( 4.458734124999999437, 16.18750000136559564, -5.460374474430324690E-16 ) ) ;
#10775 = DIRECTION ( 'NONE',  ( -0.000000000000000000, 1.000000000000000000, -0.000000000000000000 ) ) ;
#10776 = ADVANCED_FACE ( 'NONE', ( #165 ), #44841, .T. ) ;
#10777 = CARTESIAN_POINT ( 'NONE',  ( -2.071067811865602071, -157.6874999999999716, -4.999999999999874767 ) ) ;
#10778 = CARTESIAN_POINT ( 'NONE',  ( 4.458734125000001214, -47.14583333196774362, 2.574251347313718519 ) ) ;
#10779 = CARTESIAN_POINT ( 'NONE',  ( 2.499999999999998668, -10.20833333060214621, -4.330127018922193649 ) ) ;
#10780 = CARTESIAN_POINT ( 'NONE',  ( 1.339745962155615144, -42.58034179853029144, 4.999999999999999112 ) ) ;
#10781 = CARTESIAN_POINT ( 'NONE',  ( -60.14911071818854538, -147.0625000000000000, 1.666127454062681146 ) ) ;
#10782 = CARTESIAN_POINT ( 'NONE',  ( 2.229367062499998831, -89.89583333196773651, -3.861377020970580887 ) ) ;
#10783 = DIRECTION ( 'NONE',  ( -0.000000000000000000, 1.000000000000000000, -0.000000000000000000 ) ) ;
#10784 = CARTESIAN_POINT ( 'NONE',  ( -3.152548672688508926E-16, -16.81249999863440436, -5.148502694627439702 ) ) ;
#10785 = ORIENTED_EDGE ( 'NONE', *, *, #43292, .T. ) ;
#10786 = CARTESIAN_POINT ( 'NONE',  ( -58.24261429053147765, -146.2500000000000284, -3.805975901505573855 ) ) ;
#10787 = CARTESIAN_POINT ( 'NONE',  ( 2.229367062500001939, -102.9791666653010651, 3.861377020970579999 ) ) ;
#10788 = CARTESIAN_POINT ( 'NONE',  ( -5.000000000000000888, -156.6875000027312126, -2.071067811865475949 ) ) ;
#10789 = ORIENTED_EDGE ( 'NONE', *, *, #51676, .F. ) ;
#10790 = CARTESIAN_POINT ( 'NONE',  ( 4.458734125000001214, -99.14583333196773651, 2.574251347313718519 ) ) ;
#10791 = CARTESIAN_POINT ( 'NONE',  ( -4.999999999999999112, -58.79166666393546592, 2.886751345948131764 ) ) ;
#10792 = CARTESIAN_POINT ( 'NONE',  ( -59.29741812935640155, -124.6250000013656347, -2.196230717870135685 ) ) ;
#10793 = CARTESIAN_POINT ( 'NONE',  ( -52.80376928212989185, -143.8750000013655779, -4.297418129356378458 ) ) ;
#10794 = CARTESIAN_POINT ( 'NONE',  ( -2.229367062500000163, -22.47916666530107221, -3.861377020970580443 ) ) ;
#10795 = CARTESIAN_POINT ( 'NONE',  ( 9.457646018065525792E-16, 6.687500001365594748, 5.148502694627439702 ) ) ;
#10796 = CARTESIAN_POINT ( 'NONE',  ( -2.229367062499996610, -66.39583333196773651, 3.861377020970582219 ) ) ;
#10797 = CARTESIAN_POINT ( 'NONE',  ( 5.000000000000000888, -48.45833333060215153, 2.886751345948126879 ) ) ;
#10798 = CARTESIAN_POINT ( 'NONE',  ( 2.229367062500001939, -18.97916666530106866, 3.861377020970579999 ) ) ;
#10799 = CARTESIAN_POINT ( 'NONE',  ( -6.972266317189433020E-16, -75.25000000000000000, -5.000000000000000000 ) ) ;
#10800 = CARTESIAN_POINT ( 'NONE',  ( 5.000000000000000000, -150.0625000000000000, 2.071067811865478614 ) ) ;
#10801 = CARTESIAN_POINT ( 'NONE',  ( -4.999999999999999112, -10.91666666666666607, 2.886751345948131764 ) ) ;
#10802 = CARTESIAN_POINT ( 'NONE',  ( 1.846868145590735200, -154.2500000013656063, -4.458734125000000326 ) ) ;
#10803 = ORIENTED_EDGE ( 'NONE', *, *, #23930, .T. ) ;
#10804 = CARTESIAN_POINT ( 'NONE',  ( 4.458734124999998549, -45.97916666530106511, -2.574251347313721627 ) ) ;
#10805 = CARTESIAN_POINT ( 'NONE',  ( 0.000000000000000000, -170.0000000000000000, 0.000000000000000000 ) ) ;
#10806 = FACE_OUTER_BOUND ( 'NONE', #8324, .T. ) ;
#10807 = CARTESIAN_POINT ( 'NONE',  ( 5.000000000000000000, 28.49999999999999645, -6.123233995736766282E-16 ) ) ;
#10808 = CARTESIAN_POINT ( 'NONE',  ( -2.229367062499996610, 2.854166668032259935, 3.861377020970582219 ) ) ;
#10809 = CARTESIAN_POINT ( 'NONE',  ( -4.999999999999998224, -43.91666666666665719, 2.886751345948131764 ) ) ;
#10810 = CARTESIAN_POINT ( 'NONE',  ( 0.000000000000000000, -170.0000000000000000, 5.000000000000000000 ) ) ;
#10811 = CARTESIAN_POINT ( 'NONE',  ( 5.000000000000000000, -17.41666666666666430, -2.886751345948130876 ) ) ;
#10812 = CARTESIAN_POINT ( 'NONE',  ( -4.458734124999999437, 22.35416666803225638, -2.574251347313719407 ) ) ;
#10813 = CARTESIAN_POINT ( 'NONE',  ( 5.000000000000000000, -77.41666666666665719, -2.886751345948129988 ) ) ;
#10814 = CARTESIAN_POINT ( 'NONE',  ( -2.500000000000000444, 5.958333336064519870, -4.330127018922193649 ) ) ;
#10815 = ORIENTED_EDGE ( 'NONE', *, *, #62275, .T. ) ;
#10816 = CARTESIAN_POINT ( 'NONE',  ( 5.000000000000000888, -80.45833333060213022, 2.886751345948126879 ) ) ;
#10817 = EDGE_LOOP ( 'NONE', ( #59567, #39206, #60006, #51564 ) ) ;
#10818 = CARTESIAN_POINT ( 'NONE',  ( -6.972266317189433020E-16, -85.25000000000000000, -5.000000000000000000 ) ) ;
#10819 = CARTESIAN_POINT ( 'NONE',  ( -4.458734124999998549, -37.22916666530107221, 2.574251347313722516 ) ) ;
#10820 = EDGE_CURVE ( 'NONE', #31465, #14946, #39076, .T. ) ;
#10821 = CARTESIAN_POINT ( 'NONE',  ( 5.000000000000000888, -41.45833333060213732, 2.886751345948126879 ) ) ;
#10822 = EDGE_LOOP ( 'NONE', ( #62279, #10677, #1242, #56827 ) ) ;
#10823 = CARTESIAN_POINT ( 'NONE',  ( -4.458734124999998549, -13.22916666530107221, 2.574251347313722516 ) ) ;
#10824 = VERTEX_POINT ( 'NONE', #63207 ) ;
#10825 = CARTESIAN_POINT ( 'NONE',  ( -4.999999999999999112, -84.91666666666667140, 2.886751345948131764 ) ) ;
#10826 = CARTESIAN_POINT ( 'NONE',  ( -1.846868145590737420, -168.7500000013656063, 4.458734124999999437 ) ) ;
#10827 = CARTESIAN_POINT ( 'NONE',  ( 2.499999999999998668, -89.20833333060214443, -4.330127018922193649 ) ) ;
#10829 = ORIENTED_EDGE ( 'NONE', *, *, #29564, .T. ) ;
#10828 = CARTESIAN_POINT ( 'NONE',  ( -5.000000000000000000, -32.00000000000000000, 0.000000000000000000 ) ) ;
#10830 = CARTESIAN_POINT ( 'NONE',  ( -60.14911071818854538, -143.0625000000000284, 1.666127454062681368 ) ) ;
#10831 = CARTESIAN_POINT ( 'NONE',  ( -4.458734124999999437, -26.56249999863440792, 0.000000000000000000 ) ) ;
#10832 = FACE_OUTER_BOUND ( 'NONE', #59269, .T. ) ;
#10833 = ORIENTED_EDGE ( 'NONE', *, *, #29647, .T. ) ;
#10834 = VECTOR ( 'NONE', #32218, 1000.000000000000000 ) ;
#10835 = CARTESIAN_POINT ( 'NONE',  ( -3.152801135295367096, -162.3125000013656063, -3.152801135295367541 ) ) ;
#10836 = CARTESIAN_POINT ( 'NONE',  ( -4.458734124999999437, 27.68750000136559208, 0.000000000000000000 ) ) ;
#10837 = ORIENTED_EDGE ( 'NONE', *, *, #50029, .T. ) ;
#10838 = CARTESIAN_POINT ( 'NONE',  ( -52.10840900171896806, -147.4375000013656063, 3.393966926194110556 ) ) ;
#10839 = CARTESIAN_POINT ( 'NONE',  ( -4.458734124999999437, -72.64583333196773651, -2.574251347313719407 ) ) ;
#10840 = CARTESIAN_POINT ( 'NONE',  ( -54.60164318462004474, -133.5000000027312126, -4.984105922594373794 ) ) ;
#10841 = CARTESIAN_POINT ( 'NONE',  ( -2.229367062499996610, -42.14583333196773651, 3.861377020970582219 ) ) ;
#10842 = CARTESIAN_POINT ( 'NONE',  ( -1.846868145590737420, -142.0000000013655495, 4.458734124999997661 ) ) ;
#10843 = CARTESIAN_POINT ( 'NONE',  ( -7.500000000000000000, -3.948305025207388130, -7.349903712356284480 ) ) ;
#10844 = CARTESIAN_POINT ( 'NONE',  ( 4.458734124999999437, -50.81249999863440792, -5.460374474430324690E-16 ) ) ;
#10845 = CARTESIAN_POINT ( 'NONE',  ( -5.000000000000000000, -71.08333333333332860, -2.886751345948128211 ) ) ;
#10846 = CARTESIAN_POINT ( 'NONE',  ( 2.229367062500001939, -17.97916666530106866, 3.861377020970579999 ) ) ;
#10847 =( BOUNDED_CURVE ( )  B_SPLINE_CURVE ( 2, ( #59235, #29633, #5521, #29953, #10022, #14838, #33837, #38967, #38652 ),
 .UNSPECIFIED., .F., .F. ) 
 B_SPLINE_CURVE_WITH_KNOTS ( ( 3, 2, 2, 2, 3 ),
 ( 0.6395833333333332815, 0.6402777777777777235, 0.6416666666666667185, 0.6430555555555556024, 0.6437500000000000444 ),
 .UNSPECIFIED. ) 
 CURVE ( )  GEOMETRIC_REPRESENTATION_ITEM ( )  RATIONAL_B_SPLINE_CURVE ( ( 0.9330127018922194093, 0.9330127018922194093, 1.000000000000000000, 0.8660254037844387076, 1.000000000000000000, 0.8660254037844387076, 1.000000000000000000, 0.9330127018922194093, 0.9330127018922194093 ) ) 
 REPRESENTATION_ITEM ( '' )  );
#10848 = CARTESIAN_POINT ( 'NONE',  ( 1.060575238724906964E-15, -100.7500000000000000, 5.773502691896257311 ) ) ;
#10849 = CARTESIAN_POINT ( 'NONE',  ( -3.535533905932738641, -167.3750000000000284, 3.535533905932737309 ) ) ;
#10850 = CARTESIAN_POINT ( 'NONE',  ( -2.229367062499996610, -32.39583333196773651, 3.861377020970582219 ) ) ;
#10851 = CARTESIAN_POINT ( 'NONE',  ( -4.999999999999999112, 9.208333336064519870, 2.886751345948131764 ) ) ;
#10852 = CYLINDRICAL_SURFACE ( 'NONE', #25298, 5.000000000000000000 ) ;
#10853 = CARTESIAN_POINT ( 'NONE',  ( -53.51423613279429503, -129.2500000013656347, 4.591703134518082763 ) ) ;
#10854 = CARTESIAN_POINT ( 'NONE',  ( 4.458734124999998549, -74.97916666530106511, -2.574251347313721627 ) ) ;
#10855 = CARTESIAN_POINT ( 'NONE',  ( -9.184850993605147944E-16, -166.2500000000000000, 5.000000000000000000 ) ) ;
#10856 = CARTESIAN_POINT ( 'NONE',  ( -3.535533905932737309, -139.7500000027311842, -3.535533905932738197 ) ) ;
#10857 = CARTESIAN_POINT ( 'NONE',  ( 5.000000000000000888, -68.58333333333332860, 2.886751345948126879 ) ) ;
#10858 = CARTESIAN_POINT ( 'NONE',  ( -4.458734124999999437, 0.4375000013655955255, 0.000000000000000000 ) ) ;
#10859 = ORIENTED_EDGE ( 'NONE', *, *, #30730, .T. ) ;
#10860 = CARTESIAN_POINT ( 'NONE',  ( -6.972266317189433020E-16, -54.12499999726880162, -5.000000000000000000 ) ) ;
#10861 = CARTESIAN_POINT ( 'NONE',  ( 1.339745962155615144, -15.70534180126148271, 4.999999999999999112 ) ) ;
#10863 = CARTESIAN_POINT ( 'NONE',  ( 4.458734124999998549, -37.72916666530107221, -2.574251347313721627 ) ) ;
#10862 = CARTESIAN_POINT ( 'NONE',  ( -4.458734124999999437, -86.39583333196772230, -2.574251347313719407 ) ) ;
#10864 = DIRECTION ( 'NONE',  ( -0.000000000000000000, 1.000000000000000000, -0.000000000000000000 ) ) ;
#10865 = CARTESIAN_POINT ( 'NONE',  ( 2.229367062499998831, -82.89583333196773651, -3.861377020970580887 ) ) ;
#10866 = CARTESIAN_POINT ( 'NONE',  ( 4.458734124999999437, 17.93750000136559208, -5.460374474430324690E-16 ) ) ;
#10867 = CARTESIAN_POINT ( 'NONE',  ( 0.000000000000000000, -120.0000000000000000, 0.000000000000000000 ) ) ;
#10868 = CARTESIAN_POINT ( 'NONE',  ( -56.48576386720575471, -138.7500000013656063, -4.591703134518078322 ) ) ;
#10869 =( BOUNDED_CURVE ( )  B_SPLINE_CURVE ( 2, ( #43860, #20394, #39358, #33907, #24579, #35191, #53531, #5280, #34214 ),
 .UNSPECIFIED., .F., .F. ) 
 B_SPLINE_CURVE_WITH_KNOTS ( ( 3, 2, 2, 2, 3 ),
 ( 0.1839285714285714413, 0.1845238095238095344, 0.1857142857142857206, 0.1869047619047619069, 0.1875000000000000000 ),
 .UNSPECIFIED. ) 
 CURVE ( )  GEOMETRIC_REPRESENTATION_ITEM ( )  RATIONAL_B_SPLINE_CURVE ( ( 0.9330127018922194093, 0.9330127018922209636, 1.000000000000000000, 0.8660254037844387076, 1.000000000000000000, 0.8660254037844387076, 1.000000000000000000, 0.9330127018922194093, 0.9330127018922194093 ) ) 
 REPRESENTATION_ITEM ( '' )  );
#10870 = CARTESIAN_POINT ( 'NONE',  ( -2.229367062499996610, -3.145833331967738733, 3.861377020970582219 ) ) ;
#10871 = CARTESIAN_POINT ( 'NONE',  ( -4.458734124999999437, 22.43750000136559564, 0.000000000000000000 ) ) ;
#10872 = CARTESIAN_POINT ( 'NONE',  ( -2.229367062500000163, -47.72916666530106511, -3.861377020970580443 ) ) ;
#10873 = CARTESIAN_POINT ( 'NONE',  ( 0.000000000000000000, -170.0000000000000000, 5.000000000000000000 ) ) ;
#10874 = CARTESIAN_POINT ( 'NONE',  ( -3.152548672688508926E-16, -84.56249999863439371, -5.148502694627439702 ) ) ;
#10875 = CARTESIAN_POINT ( 'NONE',  ( -3.152548672688508926E-16, -3.562499998634408360, -5.148502694627439702 ) ) ;
#10876 = AXIS2_PLACEMENT_3D ( 'NONE', #40501, #11553, #45969 ) ;
#10877 = EDGE_LOOP ( 'NONE', ( #9449, #11141, #62579, #56399, #8926, #52924 ) ) ;
#10878 = CARTESIAN_POINT ( 'NONE',  ( -3.152548672688508926E-16, -29.81249999863440436, -5.148502694627439702 ) ) ;
#10879 = CARTESIAN_POINT ( 'NONE',  ( -57.19623071787017210, -133.6250000013655779, 4.297418129356382899 ) ) ;
#10880 = CARTESIAN_POINT ( 'NONE',  ( 4.458734125000001214, -75.89583333196775072, 2.574251347313718519 ) ) ;
#10881 = CARTESIAN_POINT ( 'NONE',  ( -4.458734124999999437, 29.43750000136559208, 0.000000000000000000 ) ) ;
#10882 = EDGE_CURVE ( 'NONE', #44517, #50477, #19739, .T. ) ;
#10883 = CARTESIAN_POINT ( 'NONE',  ( -2.229367062500000163, 24.52083333469892779, -3.861377020970580443 ) ) ;
#10884 = CARTESIAN_POINT ( 'NONE',  ( 6.123233995736766282E-16, -120.0000000000000000, -5.000000000000000000 ) ) ;
#10885 = CARTESIAN_POINT ( 'NONE',  ( -5.000000000000000888, -145.6875000027312126, -2.071067811865475949 ) ) ;
#10886 = CARTESIAN_POINT ( 'NONE',  ( 2.229367062499998831, -78.89583333196773651, -3.861377020970580887 ) ) ;
#10887 = CARTESIAN_POINT ( 'NONE',  ( -3.535250795749689387E-16, -57.25000000000000000, -5.773502691896257311 ) ) ;
#10888 = CARTESIAN_POINT ( 'NONE',  ( 1.339745962155615144, -90.58034179853029855, 4.999999999999999112 ) ) ;
#10889 = CARTESIAN_POINT ( 'NONE',  ( -2.499999999999996447, 23.29166666939785202, 4.330127018922195425 ) ) ;
#10890 = ORIENTED_EDGE ( 'NONE', *, *, #11000, .T. ) ;
#10891 = CARTESIAN_POINT ( 'NONE',  ( -55.00000000000002132, -155.0000000000000284, 1.734723475976807094E-15 ) ) ;
#10892 = CARTESIAN_POINT ( 'NONE',  ( -6.972266317189433020E-16, -99.24999999999998579, -5.000000000000000000 ) ) ;
#10894 = CARTESIAN_POINT ( 'NONE',  ( 5.000000000000000000, -16.41666666666667140, -2.886751345948129988 ) ) ;
#10893 = CARTESIAN_POINT ( 'NONE',  ( 1.975475456537005874E-15, -57.74999999999999289, 5.000000000000000000 ) ) ;
#10895 = CARTESIAN_POINT ( 'NONE',  ( -4.458734124999999437, -20.39583333196774362, -2.574251347313719407 ) ) ;
#10896 = CARTESIAN_POINT ( 'NONE',  ( 2.229367062499998831, -84.64583333196773651, -3.861377020970580887 ) ) ;
#10897 = CARTESIAN_POINT ( 'NONE',  ( -4.999999999999999112, -24.79166666393548368, 2.886751345948131764 ) ) ;
#10899 = ORIENTED_EDGE ( 'NONE', *, *, #52386, .T. ) ;
#10898 = CARTESIAN_POINT ( 'NONE',  ( 4.458734124999998549, -54.72916666530107932, -2.574251347313721627 ) ) ;
#10900 = CYLINDRICAL_SURFACE ( 'NONE', #13046, 5.000000000000000000 ) ;
#10901 = CARTESIAN_POINT ( 'NONE',  ( 6.158835246850666199E-14, -1.250000000000002442, -4.999999999999999112 ) ) ;
#10903 = ORIENTED_EDGE ( 'NONE', *, *, #32893, .F. ) ;
#10902 = CARTESIAN_POINT ( 'NONE',  ( -4.458734124999999437, -5.645833331967740953, -2.574251347313719407 ) ) ;
#10904 = CARTESIAN_POINT ( 'NONE',  ( -58.39396692619412477, -149.4375000013656063, 2.891590998281057701 ) ) ;
#10905 = CARTESIAN_POINT ( 'NONE',  ( 1.060575238724906964E-15, -63.75000000000000000, 5.773502691896257311 ) ) ;
#10906 = CARTESIAN_POINT ( 'NONE',  ( -4.458734125000000326, -154.2500000013656063, -1.846868145590735644 ) ) ;
#10907 = CARTESIAN_POINT ( 'NONE',  ( -4.458734124999999437, -46.56249999863440792, 0.000000000000000000 ) ) ;
#10908 = CARTESIAN_POINT ( 'NONE',  ( -6.972266317189433020E-16, -81.12499999726881583, -5.000000000000000000 ) ) ;
#10909 = CARTESIAN_POINT ( 'NONE',  ( 3.535533905932738197, -159.8750000000000284, -3.535533905932738197 ) ) ;
#10910 = CARTESIAN_POINT ( 'NONE',  ( -1.339745962155610925, -81.66965819600736154, 5.000000000000000000 ) ) ;
#10911 = CARTESIAN_POINT ( 'NONE',  ( -53.33387254593733928, -151.8125000000000000, 5.149110718188519620 ) ) ;
#10912 = CARTESIAN_POINT ( 'NONE',  ( 9.457646018065525792E-16, -13.31249999863440259, 5.148502694627439702 ) ) ;
#10913 = CARTESIAN_POINT ( 'NONE',  ( -2.229367062500000163, -50.72916666530107221, -3.861377020970580443 ) ) ;
#10914 = CARTESIAN_POINT ( 'NONE',  ( -58.24261429053147765, -144.2500000000000284, -3.805975901505573855 ) ) ;
#10915 = CARTESIAN_POINT ( 'NONE',  ( 1.846868145590736310, -145.6250000013655779, 4.458734124999999437 ) ) ;
#10916 = CARTESIAN_POINT ( 'NONE',  ( 2.229367062500001939, -94.22916666530106511, 3.861377020970579999 ) ) ;
#10917 = ORIENTED_EDGE ( 'NONE', *, *, #34941, .F. ) ;
#10918 = CARTESIAN_POINT ( 'NONE',  ( -5.000000000000000000, -32.00000000000000000, 0.000000000000000000 ) ) ;
#10919 = CARTESIAN_POINT ( 'NONE',  ( 4.458734124999999437, 27.93750000136559208, -5.460374474430324690E-16 ) ) ;
#10920 = CARTESIAN_POINT ( 'NONE',  ( -60.14911071818854538, -147.1875000027312126, 1.666127454062681368 ) ) ;
#10921 =( BOUNDED_CURVE ( )  B_SPLINE_CURVE ( 2, ( #60564, #25177, #50903, #60252, #49936, #21002, #30315, #2034, #21639 ),
 .UNSPECIFIED., .F., .F. ) 
 B_SPLINE_CURVE_WITH_KNOTS ( ( 3, 2, 2, 2, 3 ),
 ( 0.6125000000000000444, 0.6130952380952381375, 0.6142857142857143238, 0.6154761904761905100, 0.6160714285714286031 ),
 .UNSPECIFIED. ) 
 CURVE ( )  GEOMETRIC_REPRESENTATION_ITEM ( )  RATIONAL_B_SPLINE_CURVE ( ( 0.9330127018922194093, 0.9330127018922194093, 1.000000000000000000, 0.8660254037844387076, 1.000000000000000000, 0.8660254037844387076, 1.000000000000000000, 0.9330127018922194093, 0.9330127018922194093 ) ) 
 REPRESENTATION_ITEM ( '' )  );
#10922 = CARTESIAN_POINT ( 'NONE',  ( 1.975475456537005874E-15, -100.6249999972688016, 5.000000000000000000 ) ) ;
#10923 = ORIENTED_EDGE ( 'NONE', *, *, #43376, .T. ) ;
#10924 = CARTESIAN_POINT ( 'NONE',  ( -2.229367062499996610, -4.145833331967739177, 3.861377020970582219 ) ) ;
#10925 = VECTOR ( 'NONE', #56690, 1000.000000000000000 ) ;
#10926 = CARTESIAN_POINT ( 'NONE',  ( -6.972266317189433020E-16, 7.875000002731185056, -5.000000000000000000 ) ) ;
#10927 = CARTESIAN_POINT ( 'NONE',  ( -2.229367062499996610, -16.39583333196773651, 3.861377020970582219 ) ) ;
#10928 = CARTESIAN_POINT ( 'NONE',  ( -5.000000000000000000, 2.125000002731185056, 0.000000000000000000 ) ) ;
#10929 = CARTESIAN_POINT ( 'NONE',  ( 2.229367062500001939, -6.979166665301073103, 3.861377020970579999 ) ) ;
#10930 = CARTESIAN_POINT ( 'NONE',  ( 1.339745962155612702, -55.16965819600732601, -5.000000000000000000 ) ) ;
#10931 = CARTESIAN_POINT ( 'NONE',  ( 3.152801135295367541, -147.3125000013655779, -3.152801135295367541 ) ) ;
#10932 = CARTESIAN_POINT ( 'NONE',  ( 2.229367062499998831, 18.10416666803225993, -3.861377020970580887 ) ) ;
#10933 = VERTEX_POINT ( 'NONE', #54175 ) ;
#10934 = CARTESIAN_POINT ( 'NONE',  ( -4.458734124999999437, -20.31249999863440081, 0.000000000000000000 ) ) ;
#10935 = CARTESIAN_POINT ( 'NONE',  ( -50.01589407740564042, -143.6250000000000284, 0.3983568153799778022 ) ) ;
#10936 = CARTESIAN_POINT ( 'NONE',  ( 1.339745962155615144, 1.419658201469705672, 4.999999999999999112 ) ) ;
#10937 = CARTESIAN_POINT ( 'NONE',  ( -56.48576386720575471, -150.7500000013655495, -4.591703134518078322 ) ) ;
#10938 = CARTESIAN_POINT ( 'NONE',  ( -2.500000000000000444, -46.04166666393547303, -4.330127018922193649 ) ) ;
#10939 = CARTESIAN_POINT ( 'NONE',  ( -4.458734124999997661, 14.77083333469892779, 2.574251347313722516 ) ) ;
#10940 = CARTESIAN_POINT ( 'NONE',  ( 0.000000000000000000, 30.00000000000000000, 0.000000000000000000 ) ) ;
#10941 = CARTESIAN_POINT ( 'NONE',  ( -2.499999999999996447, -47.70833333060215153, 4.330127018922195425 ) ) ;
#10942 = CARTESIAN_POINT ( 'NONE',  ( 4.458734124999998549, 10.27083333469892779, -2.574251347313721627 ) ) ;
#10943 = CARTESIAN_POINT ( 'NONE',  ( 2.229367062499998831, -68.64583333196773651, -3.861377020970580887 ) ) ;
#10944 = VERTEX_POINT ( 'NONE', #10114 ) ;
#10945 = CARTESIAN_POINT ( 'NONE',  ( -4.458734124999999437, -15.56249999863440436, 0.000000000000000000 ) ) ;
#10946 =( BOUNDED_CURVE ( )  B_SPLINE_CURVE ( 2, ( #5712, #54919, #578, #15996, #53954, #10845, #39471, #15679, #10523 ),
 .UNSPECIFIED., .F., .F. ) 
 B_SPLINE_CURVE_WITH_KNOTS ( ( 3, 2, 2, 2, 3 ),
 ( 0.7196428571428571397, 0.7202380952380952328, 0.7214285714285714191, 0.7226190476190476053, 0.7232142857142856984 ),
 .UNSPECIFIED. ) 
 CURVE ( )  GEOMETRIC_REPRESENTATION_ITEM ( )  RATIONAL_B_SPLINE_CURVE ( ( 0.9330127018922194093, 0.9330127018922194093, 1.000000000000000000, 0.8660254037844387076, 1.000000000000000000, 0.8660254037844387076, 1.000000000000000000, 0.9330127018922194093, 0.9330127018922194093 ) ) 
 REPRESENTATION_ITEM ( '' )  );
#10947 = CARTESIAN_POINT ( 'NONE',  ( 2.499999999999998668, 2.666666666666667851, -4.330127018922193649 ) ) ;
#10948 = CARTESIAN_POINT ( 'NONE',  ( -4.458734125000001214, -163.8750000013655779, 1.846868145590734089 ) ) ;
#10949 = CARTESIAN_POINT ( 'NONE',  ( -2.500000000000000444, 25.95833333606451632, -4.330127018922193649 ) ) ;
#10950 = CARTESIAN_POINT ( 'NONE',  ( 9.457646018065525792E-16, -60.06249999863440792, 5.148502694627439702 ) ) ;
#10951 = CARTESIAN_POINT ( 'NONE',  ( -3.535250795749689387E-16, -95.12499999726881583, -5.773502691896257311 ) ) ;
#10952 = EDGE_CURVE ( 'NONE', #21555, #55752, #55073, .T. ) ;
#10953 = CARTESIAN_POINT ( 'NONE',  ( -3.152548672688508926E-16, -35.56249999863440792, -5.148502694627439702 ) ) ;
#10954 = DIRECTION ( 'NONE',  ( -0.000000000000000000, 1.000000000000000000, -0.000000000000000000 ) ) ;
#10955 = CARTESIAN_POINT ( 'NONE',  ( -6.972266317189433020E-16, -38.25000000000000000, -5.000000000000000000 ) ) ;
#10956 = CARTESIAN_POINT ( 'NONE',  ( -5.000000000000000000, -107.8749999972687874, 0.000000000000000000 ) ) ;
#10957 = CARTESIAN_POINT ( 'NONE',  ( -5.000000000000000000, -78.95833333060213022, -2.886751345948128211 ) ) ;
#10958 = CARTESIAN_POINT ( 'NONE',  ( 3.152801135295367541, -151.5625000013655779, -3.152801135295367541 ) ) ;
#10959 = CARTESIAN_POINT ( 'NONE',  ( -4.999999999999999112, -44.91666666666666430, 2.886751345948131764 ) ) ;
#10960 = CARTESIAN_POINT ( 'NONE',  ( -2.500000000000000444, -58.04166666393548013, -4.330127018922193649 ) ) ;
#10961 = CARTESIAN_POINT ( 'NONE',  ( 5.000000000000000888, -17.45833333060214443, 2.886751345948126879 ) ) ;
#10962 = VERTEX_POINT ( 'NONE', #26188 ) ;
#10963 = CARTESIAN_POINT ( 'NONE',  ( -4.458734124999999437, -104.3124999986344079, 0.000000000000000000 ) ) ;
#10964 = CARTESIAN_POINT ( 'NONE',  ( 2.229367062499998831, 3.104166668032259935, -3.861377020970580887 ) ) ;
#10965 = AXIS2_PLACEMENT_3D ( 'NONE', #34120, #53743, #24799 ) ;
#10966 = CARTESIAN_POINT ( 'NONE',  ( -5.000000000000000000, -96.87499999726881583, 0.000000000000000000 ) ) ;
#10967 = CARTESIAN_POINT ( 'NONE',  ( 2.499999999999998668, -0.3333333333333348136, -4.330127018922193649 ) ) ;
#10968 = EDGE_CURVE ( 'NONE', #55556, #36504, #52253, .T. ) ;
#10969 = AXIS2_PLACEMENT_3D ( 'NONE', #57820, #43941, #24979 ) ;
#10970 = CARTESIAN_POINT ( 'NONE',  ( -4.458734124999999437, -66.31249999863440792, 0.000000000000000000 ) ) ;
#10971 = CARTESIAN_POINT ( 'NONE',  ( -3.535250795749689387E-16, -9.124999997268815832, -5.773502691896257311 ) ) ;
#10973 = VERTEX_POINT ( 'NONE', #6262 ) ;
#10972 = CARTESIAN_POINT ( 'NONE',  ( -2.229367062500000163, -32.47916666530106511, -3.861377020970580443 ) ) ;
#10974 = CARTESIAN_POINT ( 'NONE',  ( -2.500000000000000444, -78.16666666666665719, -4.330127018922193649 ) ) ;
#10975 = CARTESIAN_POINT ( 'NONE',  ( 2.499999999999998668, -22.20833333060215153, -4.330127018922193649 ) ) ;
#10976 = EDGE_CURVE ( 'NONE', #24051, #57423, #35522, .T. ) ;
#10978 = ORIENTED_EDGE ( 'NONE', *, *, #62040, .F. ) ;
#10977 = CARTESIAN_POINT ( 'NONE',  ( 4.458734125000001214, 13.85416666803226171, 2.574251347313718519 ) ) ;
#10979 = CARTESIAN_POINT ( 'NONE',  ( -59.81910112700026616, -141.3125000027312126, -2.462841084822451343 ) ) ;
#10980 = CARTESIAN_POINT ( 'NONE',  ( 1.060575238724906964E-15, -51.75000000000000711, 5.773502691896257311 ) ) ;
#10981 = CARTESIAN_POINT ( 'NONE',  ( 2.229367062500001939, -32.22916666530106511, 3.861377020970579999 ) ) ;
#10982 = CARTESIAN_POINT ( 'NONE',  ( -1.339745962155613812, 13.91965820146970678, -5.000000000000000000 ) ) ;
#10983 = CARTESIAN_POINT ( 'NONE',  ( 4.458734124999999437, -74.81249999863440792, -5.460374474430324690E-16 ) ) ;
#10984 = CARTESIAN_POINT ( 'NONE',  ( 4.458734124999999437, -141.7500000013655779, 1.846868145590737864 ) ) ;
#10985 = CARTESIAN_POINT ( 'NONE',  ( -2.229367062500000163, -81.47916666530106511, -3.861377020970580443 ) ) ;
#10986 = CARTESIAN_POINT ( 'NONE',  ( -59.59170313451811296, -133.7500000013656063, 1.485763867205729394 ) ) ;
#10987 = CARTESIAN_POINT ( 'NONE',  ( -4.458734124999998549, -31.47916666530107221, 2.574251347313722516 ) ) ;
#10988 = ORIENTED_EDGE ( 'NONE', *, *, #22101, .T. ) ;
#10989 = CARTESIAN_POINT ( 'NONE',  ( -1.339745962155610925, -82.66965819600731891, 5.000000000000000000 ) ) ;
#10990 = ORIENTED_EDGE ( 'NONE', *, *, #16578, .T. ) ;
#10991 = CARTESIAN_POINT ( 'NONE',  ( -4.458734124999999437, -80.64583333196773651, -2.574251347313719407 ) ) ;
#10992 = CARTESIAN_POINT ( 'NONE',  ( -1.339745962155610925, 13.33034180399266688, 5.000000000000000000 ) ) ;
#10993 = ORIENTED_EDGE ( 'NONE', *, *, #16118, .F. ) ;
#10994 = CARTESIAN_POINT ( 'NONE',  ( 0.000000000000000000, -120.0000000000000000, 0.000000000000000000 ) ) ;
#10995 = CARTESIAN_POINT ( 'NONE',  ( 5.000000000000000888, -12.58333333333333570, 2.886751345948126879 ) ) ;
#10996 = CARTESIAN_POINT ( 'NONE',  ( 4.458734125000001214, -63.14583333196774362, 2.574251347313718519 ) ) ;
#10997 = CARTESIAN_POINT ( 'NONE',  ( -4.458734124999999437, -3.645833331967739621, -2.574251347313719407 ) ) ;
#10998 = ORIENTED_EDGE ( 'NONE', *, *, #18539, .T. ) ;
#10999 = CARTESIAN_POINT ( 'NONE',  ( 4.769696007084727185, -120.0000000000000000, -1.500000000000000444 ) ) ;
#11000 = EDGE_CURVE ( 'NONE', #15736, #24591, #55145, .T. ) ;
#11001 = CARTESIAN_POINT ( 'NONE',  ( 0.000000000000000000, -120.0000000000000000, 0.000000000000000000 ) ) ;
#11002 = CARTESIAN_POINT ( 'NONE',  ( -3.152548672688508926E-16, 6.437500001365592972, -5.148502694627439702 ) ) ;
#11003 = CARTESIAN_POINT ( 'NONE',  ( -59.59170313451811296, -141.5000000013656063, 1.485763867205729394 ) ) ;
#11004 = CARTESIAN_POINT ( 'NONE',  ( -1.339745962155610925, -0.7946581987385198387, 5.000000000000000000 ) ) ;
#11005 = CARTESIAN_POINT ( 'NONE',  ( -3.152801135295367985, -159.8125000013656063, 3.152801135295367096 ) ) ;
#11006 = AXIS2_PLACEMENT_3D ( 'NONE', #29329, #4911, #34476 ) ;
#11007 = EDGE_LOOP ( 'NONE', ( #31175, #49595, #53543, #9615 ) ) ;
#11008 = CARTESIAN_POINT ( 'NONE',  ( -2.229367062500000163, -80.47916666530106511, -3.861377020970580443 ) ) ;
#11009 = CARTESIAN_POINT ( 'NONE',  ( 1.975475456537005874E-15, -96.75000000000000000, 5.000000000000000000 ) ) ;
#11010 = CARTESIAN_POINT ( 'NONE',  ( 4.458734124999999437, -4.812499998634402587, -5.460374474430324690E-16 ) ) ;
#11011 = AXIS2_PLACEMENT_3D ( 'NONE', #2670, #42526, #33202 ) ;
#11012 = DIRECTION ( 'NONE',  ( 0.000000000000000000, 0.000000000000000000, 1.000000000000000000 ) ) ;
#11013 = VECTOR ( 'NONE', #14799, 1000.000000000000000 ) ;
#11014 = CARTESIAN_POINT ( 'NONE',  ( 2.229367062500001939, -68.22916666530106511, 3.861377020970579999 ) ) ;
#11015 = AXIS2_PLACEMENT_3D ( 'NONE', #63633, #54612, #40124 ) ;
#11016 = CARTESIAN_POINT ( 'NONE',  ( -3.535250795749689387E-16, -33.12499999726881583, -5.773502691896257311 ) ) ;
#11017 = CARTESIAN_POINT ( 'NONE',  ( -2.499999999999996447, -14.83333333333333037, 4.330127018922195425 ) ) ;
#11018 = CARTESIAN_POINT ( 'NONE',  ( -2.229367062499996610, 27.85416666803225993, 3.861377020970582219 ) ) ;
#11019 = CARTESIAN_POINT ( 'NONE',  ( 5.000000000000000000, -110.3749999972688016, -6.123233995736766282E-16 ) ) ;
#11020 = CARTESIAN_POINT ( 'NONE',  ( 5.000000000000000000, -82.29166666393547303, -2.886751345948130876 ) ) ;
#11021 = CARTESIAN_POINT ( 'NONE',  ( -2.229367062500000163, -53.47916666530107221, -3.861377020970580443 ) ) ;
#11022 = CARTESIAN_POINT ( 'NONE',  ( 2.229367062499998831, -34.89583333196772941, -3.861377020970580887 ) ) ;
#11023 = CARTESIAN_POINT ( 'NONE',  ( -4.458734124999999437, 4.354166668032260823, -2.574251347313719407 ) ) ;
#11024 = CARTESIAN_POINT ( 'NONE',  ( 2.071067811865560326, -145.9375000027311842, -4.999999999999914735 ) ) ;
#11025 = CARTESIAN_POINT ( 'NONE',  ( -3.535250795749689387E-16, 22.75000000000000000, -5.773502691896257311 ) ) ;
#11026 = CARTESIAN_POINT ( 'NONE',  ( -5.000000000000000000, -145.6250000027312126, -6.123233995736766282E-16 ) ) ;
#11027 = CARTESIAN_POINT ( 'NONE',  ( -2.229367062500000163, -41.47916666530107932, -3.861377020970580443 ) ) ;
#11028 = CARTESIAN_POINT ( 'NONE',  ( -2.499999999999996447, -73.70833333060214443, 4.330127018922195425 ) ) ;
#11029 = CARTESIAN_POINT ( 'NONE',  ( -53.51423613279429503, -142.5000000013656347, 4.591703134518082763 ) ) ;
#11030 = CARTESIAN_POINT ( 'NONE',  ( -6.972266317189433020E-16, 5.749999999999999112, -5.000000000000000000 ) ) ;
#11031 = EDGE_CURVE ( 'NONE', #14930, #25261, #32906, .T. ) ;
#11032 = CARTESIAN_POINT ( 'NONE',  ( 6.123233995736766282E-16, -120.0000000000000000, -5.000000000000000000 ) ) ;
#11033 = EDGE_CURVE ( 'NONE', #10332, #40250, #11386, .T. ) ;
#11034 = CARTESIAN_POINT ( 'NONE',  ( 2.229367062500001939, -78.22916666530106511, 3.861377020970579999 ) ) ;
#11035 = CARTESIAN_POINT ( 'NONE',  ( -1.846868145590734756, -162.3750000013656063, -4.458734124999999437 ) ) ;
#11036 = DIRECTION ( 'NONE',  ( -0.000000000000000000, 1.000000000000000000, -0.000000000000000000 ) ) ;
#11037 = FACE_OUTER_BOUND ( 'NONE', #26186, .T. ) ;
#11038 = CARTESIAN_POINT ( 'NONE',  ( 2.499999999999998668, -27.33333333333333570, -4.330127018922193649 ) ) ;
#11039 = CARTESIAN_POINT ( 'NONE',  ( -1.846868145590737420, -140.7500000013655779, 4.458734124999999437 ) ) ;
#11040 = ORIENTED_EDGE ( 'NONE', *, *, #8031, .F. ) ;
#11041 = CARTESIAN_POINT ( 'NONE',  ( -3.152548672688508926E-16, 25.18750000136558853, -5.148502694627439702 ) ) ;
#11042 = ORIENTED_EDGE ( 'NONE', *, *, #37761, .T. ) ;
#11043 = CARTESIAN_POINT ( 'NONE',  ( 2.229367062499998831, -62.89583333196774362, -3.861377020970580887 ) ) ;
#11044 = CARTESIAN_POINT ( 'NONE',  ( 2.499999999999998668, 21.79166666939785202, -4.330127018922193649 ) ) ;
#11045 = CARTESIAN_POINT ( 'NONE',  ( -1.339745962155610925, -2.669658196007334450, 5.000000000000000000 ) ) ;
#11046 = CARTESIAN_POINT ( 'NONE',  ( 2.499999999999998668, 15.66666666666666607, -4.330127018922193649 ) ) ;
#11047 = EDGE_CURVE ( 'NONE', #27288, #63081, #61277, .T. ) ;
#11048 = CARTESIAN_POINT ( 'NONE',  ( -4.458734124999997661, -49.22916666530106511, 2.574251347313722516 ) ) ;
#11049 = CARTESIAN_POINT ( 'NONE',  ( 9.457646018065525792E-16, -9.062499998634406140, 5.148502694627439702 ) ) ;
#11050 =( BOUNDED_CURVE ( )  B_SPLINE_CURVE ( 2, ( #17828, #13000, #60960, #52246, #18139, #3365, #8187, #57398, #26858 ),
 .UNSPECIFIED., .F., .F. ) 
 B_SPLINE_CURVE_WITH_KNOTS ( ( 3, 2, 2, 2, 3 ),
 ( 0.2104166666666666685, 0.2111111111111111105, 0.2124999999999999944, 0.2138888888888888784, 0.2145833333333333481 ),
 .UNSPECIFIED. ) 
 CURVE ( )  GEOMETRIC_REPRESENTATION_ITEM ( )  RATIONAL_B_SPLINE_CURVE ( ( 0.9330127018922194093, 0.9330127018922194093, 1.000000000000000000, 0.8660254037844387076, 1.000000000000000000, 0.8660254037844387076, 1.000000000000000000, 0.9330127018922180770, 0.9330127018922194093 ) ) 
 REPRESENTATION_ITEM ( '' )  );
#11051 = DIRECTION ( 'NONE',  ( -0.6485228581062915110, 0.000000000000000000, -0.7611951803011149931 ) ) ;
#11052 = CARTESIAN_POINT ( 'NONE',  ( 5.000000000000000000, -99.37499999726881583, -6.123233995736766282E-16 ) ) ;
#11053 = CARTESIAN_POINT ( 'NONE',  ( -6.972266317189433020E-16, -37.25000000000000000, -5.000000000000000000 ) ) ;
#11054 = EDGE_CURVE ( 'NONE', #12980, #50712, #10732, .T. ) ;
#11055 = CARTESIAN_POINT ( 'NONE',  ( 5.000000000000000888, 28.54166666939784847, 2.886751345948126879 ) ) ;
#11056 = CARTESIAN_POINT ( 'NONE',  ( -55.00000000000002132, 15.00000000000000000, -5.000000000000000000 ) ) ;
#11058 = CARTESIAN_POINT ( 'NONE',  ( 4.458734124999998549, -14.97916666530107221, -2.574251347313721627 ) ) ;
#11057 = CARTESIAN_POINT ( 'NONE',  ( -5.000000000000000000, -34.00000000000000000, 0.000000000000000000 ) ) ;
#11059 = AXIS2_PLACEMENT_3D ( 'NONE', #5953, #21063, #4985 ) ;
#11060 = CARTESIAN_POINT ( 'NONE',  ( -1.339745962155613812, -32.08034179853029855, -5.000000000000000000 ) ) ;
#11061 = CARTESIAN_POINT ( 'NONE',  ( -4.458734124999999437, -59.31249999863440081, 0.000000000000000000 ) ) ;
#11062 = CARTESIAN_POINT ( 'NONE',  ( 1.846868145590735200, -152.5000000013656347, -4.458734125000000326 ) ) ;
#11063 = CARTESIAN_POINT ( 'NONE',  ( -4.458734124999999437, -68.39583333196773651, -2.574251347313719407 ) ) ;
#11064 = VECTOR ( 'NONE', #54138, 1000.000000000000000 ) ;
#11065 = CARTESIAN_POINT ( 'NONE',  ( -5.000000000000000000, -53.87499999726880162, 0.000000000000000000 ) ) ;
#11066 = ORIENTED_EDGE ( 'NONE', *, *, #15869, .F. ) ;
#11067 = CARTESIAN_POINT ( 'NONE',  ( 0.000000000000000000, -120.0000000000000000, 0.000000000000000000 ) ) ;
#11068 = CARTESIAN_POINT ( 'NONE',  ( 2.229367062499998831, 0.1041666680322607397, -3.861377020970580887 ) ) ;
#11069 = VERTEX_POINT ( 'NONE', #15480 ) ;
#11071 = CARTESIAN_POINT ( 'NONE',  ( 0.000000000000000000, -170.0000000000000000, 5.000000000000000000 ) ) ;
#11070 = CARTESIAN_POINT ( 'NONE',  ( -60.14911071818854538, -149.1875000027312410, 1.666127454062681146 ) ) ;
#11072 = CARTESIAN_POINT ( 'NONE',  ( 4.458734124999999437, -155.5000000013655779, 1.846868145590737864 ) ) ;
#11073 = ORIENTED_EDGE ( 'NONE', *, *, #36719, .T. ) ;
#11074 = DIRECTION ( 'NONE',  ( 0.000000000000000000, 0.000000000000000000, 1.000000000000000000 ) ) ;
#11075 = CARTESIAN_POINT ( 'NONE',  ( -53.33387254593733928, -129.8125000000000284, 5.149110718188519620 ) ) ;
#11076 = CARTESIAN_POINT ( 'NONE',  ( 2.499999999999998668, 15.66666666666666607, -4.330127018922193649 ) ) ;
#11077 = CARTESIAN_POINT ( 'NONE',  ( 2.229367062499998831, -48.89583333196772941, -3.861377020970580887 ) ) ;
#11078 = VERTEX_POINT ( 'NONE', #10955 ) ;
#11079 = CARTESIAN_POINT ( 'NONE',  ( -6.972266317189433020E-16, -110.1249999972688158, -5.000000000000000000 ) ) ;
#11080 = CARTESIAN_POINT ( 'NONE',  ( 4.458734124999999437, 12.18750000136559564, -5.460374474430324690E-16 ) ) ;
#11081 = CARTESIAN_POINT ( 'NONE',  ( 2.229367062499998831, 23.35416666803225993, -3.861377020970580887 ) ) ;
#11082 = CARTESIAN_POINT ( 'NONE',  ( -57.19623071787017210, -151.3750000013656063, 4.297418129356382899 ) ) ;
#11083 = CARTESIAN_POINT ( 'NONE',  ( -6.972266317189433020E-16, 12.87500000273118417, -5.000000000000000000 ) ) ;
#11084 = CARTESIAN_POINT ( 'NONE',  ( 6.123233995736766282E-16, -120.0000000000000000, -5.000000000000000000 ) ) ;
#11085 = CARTESIAN_POINT ( 'NONE',  ( 4.458734124999999437, -64.81249999863440792, -5.460374474430324690E-16 ) ) ;
#11086 = CARTESIAN_POINT ( 'NONE',  ( -5.000000000000000000, 1.000000000000000888, 0.000000000000000000 ) ) ;
#11087 = CARTESIAN_POINT ( 'NONE',  ( -3.152548672688508926E-16, 12.43750000136559564, -5.148502694627439702 ) ) ;
#11088 = CARTESIAN_POINT ( 'NONE',  ( -5.000000000000000000, -78.87499999726881583, 0.000000000000000000 ) ) ;
#11089 = CARTESIAN_POINT ( 'NONE',  ( -5.000000000000000000, -1.958333330602145983, -2.886751345948128211 ) ) ;
#11090 = CARTESIAN_POINT ( 'NONE',  ( 2.229367062500001939, -53.22916666530107221, 3.861377020970579999 ) ) ;
#11091 = CARTESIAN_POINT ( 'NONE',  ( -2.499999999999996447, -7.708333330602144429, 4.330127018922195425 ) ) ;
#11092 = CARTESIAN_POINT ( 'NONE',  ( 1.339745962155612702, -25.16965819600734022, -5.000000000000000000 ) ) ;
#11093 = CARTESIAN_POINT ( 'NONE',  ( -55.39835681537999790, -146.8750000000000284, 4.984105922594378235 ) ) ;
#11094 = CARTESIAN_POINT ( 'NONE',  ( -4.458734124999999437, -90.56249999863440792, 0.000000000000000000 ) ) ;
#11095 = CARTESIAN_POINT ( 'NONE',  ( 1.975475456537005874E-15, 8.375000002731187720, 5.000000000000000000 ) ) ;
#11096 = CARTESIAN_POINT ( 'NONE',  ( 2.229367062499998831, -16.89583333196773651, -3.861377020970580887 ) ) ;
#11097 =( BOUNDED_CURVE ( )  B_SPLINE_CURVE ( 2, ( #27413, #12624, #36436, #16502, #56066, #22287, #31929, #51557, #36124 ),
 .UNSPECIFIED., .F., .F. ) 
 B_SPLINE_CURVE_WITH_KNOTS ( ( 3, 2, 2, 2, 3 ),
 ( 0.4354166666666666741, 0.4361111111111111160, 0.4375000000000000000, 0.4388888888888888840, 0.4395833333333333259 ),
 .UNSPECIFIED. ) 
 CURVE ( )  GEOMETRIC_REPRESENTATION_ITEM ( )  RATIONAL_B_SPLINE_CURVE ( ( 0.9330127018922194093, 0.9330127018922194093, 1.000000000000000000, 0.8660254037844387076, 1.000000000000000000, 0.8660254037844387076, 1.000000000000000000, 0.9330127018922194093, 0.9330127018922194093 ) ) 
 REPRESENTATION_ITEM ( '' )  );
#11098 = ORIENTED_EDGE ( 'NONE', *, *, #34361, .T. ) ;
#11099 = AXIS2_PLACEMENT_3D ( 'NONE', #47709, #23277, #47400 ) ;
#11100 = CARTESIAN_POINT ( 'NONE',  ( -2.229367062499996610, -104.1458333319677365, 3.861377020970582219 ) ) ;
#11101 = CARTESIAN_POINT ( 'NONE',  ( -3.535533905932738641, -158.5000000027312126, 3.535533905932737309 ) ) ;
#11102 = VERTEX_POINT ( 'NONE', #15151 ) ;
#11103 = CARTESIAN_POINT ( 'NONE',  ( -4.458734124999998549, -95.47916666530106511, 2.574251347313722516 ) ) ;
#11104 = CARTESIAN_POINT ( 'NONE',  ( -2.229367062499996610, -25.14583333196773651, 3.861377020970582219 ) ) ;
#11105 = CARTESIAN_POINT ( 'NONE',  ( 1.060575238724906964E-15, -57.62499999726880873, 5.773502691896257311 ) ) ;
#11106 = CARTESIAN_POINT ( 'NONE',  ( -50.40829686548195099, -126.0000000013656063, -1.485763867205728284 ) ) ;
#11107 = CARTESIAN_POINT ( 'NONE',  ( -50.40829686548195099, -142.0000000013656063, -1.485763867205728284 ) ) ;
#11108 = EDGE_CURVE ( 'NONE', #15348, #20078, #57154, .T. ) ;
#11109 = CARTESIAN_POINT ( 'NONE',  ( 2.229367062499998831, -23.64583333196773651, -3.861377020970580887 ) ) ;
#11110 = CARTESIAN_POINT ( 'NONE',  ( 4.458734125000000326, -65.14583333196773651, 2.574251347313718519 ) ) ;
#11111 = CARTESIAN_POINT ( 'NONE',  ( 4.330127018922154569, 45.00000000000000000, -7.499999999999971578 ) ) ;
#11112 = CARTESIAN_POINT ( 'NONE',  ( 4.458734124999998549, -20.72916666530107221, -2.574251347313721627 ) ) ;
#11113 = CARTESIAN_POINT ( 'NONE',  ( -2.071067811865478170, -149.3125000000000000, 5.000000000000000000 ) ) ;
#11114 = CARTESIAN_POINT ( 'NONE',  ( -2.500000000000000444, -13.16666666666666607, -4.330127018922193649 ) ) ;
#11115 = CARTESIAN_POINT ( 'NONE',  ( 1.846868145590736310, -152.6250000013655495, 4.458734124999999437 ) ) ;
#11116 = ORIENTED_EDGE ( 'NONE', *, *, #4211, .F. ) ;
#11117 = CARTESIAN_POINT ( 'NONE',  ( 4.458734124999998549, -43.97916666530106511, -2.574251347313721627 ) ) ;
#11118 = CARTESIAN_POINT ( 'NONE',  ( -5.000000000000000000, -38.08333333333333570, -2.886751345948128211 ) ) ;
#11119 = CARTESIAN_POINT ( 'NONE',  ( 1.975475456537005874E-15, -41.62499999726880162, 5.000000000000000000 ) ) ;
#11120 = CARTESIAN_POINT ( 'NONE',  ( -4.458734124999999437, -89.39583333196773651, -2.574251347313719407 ) ) ;
#11121 = AXIS2_PLACEMENT_3D ( 'NONE', #1157, #34909, #15926 ) ;
#11122 = CARTESIAN_POINT ( 'NONE',  ( 4.458734124999999437, 6.187500001365593860, -5.460374474430324690E-16 ) ) ;
#11123 = CARTESIAN_POINT ( 'NONE',  ( -4.999999999999998224, -73.79166666393547303, 2.886751345948131764 ) ) ;
#11124 = FACE_OUTER_BOUND ( 'NONE', #12824, .T. ) ;
#11125 = CARTESIAN_POINT ( 'NONE',  ( -6.902527771671634227, -4.675077770780906583, -0.7026937717022867513 ) ) ;
#11126 = CARTESIAN_POINT ( 'NONE',  ( 4.458734125000001214, 13.85416666803226171, 2.574251347313718519 ) ) ;
#11127 = CARTESIAN_POINT ( 'NONE',  ( -2.500000000000000444, -79.16666666666665719, -4.330127018922193649 ) ) ;
#11128 = CARTESIAN_POINT ( 'NONE',  ( -5.000000000000000000, 9.125000002731184168, 0.000000000000000000 ) ) ;
#11130 = ORIENTED_EDGE ( 'NONE', *, *, #45236, .T. ) ;
#11129 = EDGE_CURVE ( 'NONE', #1258, #8991, #49113, .T. ) ;
#11131 = CARTESIAN_POINT ( 'NONE',  ( -1.339745962155610925, 8.205341801261479162, 5.000000000000000000 ) ) ;
#11132 = VERTEX_POINT ( 'NONE', #10002 ) ;
#11133 = CARTESIAN_POINT ( 'NONE',  ( -2.480964764533239819E-13, -108.6249999972688016, 5.000000000000000000 ) ) ;
#11134 = CARTESIAN_POINT ( 'NONE',  ( -4.458734124999999437, -42.39583333196773651, -2.574251347313719407 ) ) ;
#11135 = EDGE_CURVE ( 'NONE', #2325, #1738, #29936, .T. ) ;
#11136 = CARTESIAN_POINT ( 'NONE',  ( 2.500000000000002220, -59.54166666393546592, 4.330127018922192761 ) ) ;
#11137 = ADVANCED_FACE ( 'NONE', ( #10325 ), #45377, .F. ) ;
#11138 = CARTESIAN_POINT ( 'NONE',  ( 5.000000000000000888, -40.45833333060214443, 2.886751345948126879 ) ) ;
#11139 = VERTEX_POINT ( 'NONE', #20300 ) ;
#11140 = CARTESIAN_POINT ( 'NONE',  ( -3.152548672688508926E-16, -20.56249999863440081, -5.148502694627439702 ) ) ;
#11141 = ORIENTED_EDGE ( 'NONE', *, *, #28767, .T. ) ;
#11142 = CARTESIAN_POINT ( 'NONE',  ( -5.000000000000000000, -85.08333333333332860, -2.886751345948128211 ) ) ;
#11143 = CARTESIAN_POINT ( 'NONE',  ( -1.846868145590734756, -169.1250000013656347, -4.458734125000000326 ) ) ;
#11144 = AXIS2_PLACEMENT_3D ( 'NONE', #61503, #38835, #62127 ) ;
#11145 =( BOUNDED_CURVE ( )  B_SPLINE_CURVE ( 2, ( #23415, #19435, #39047, #9772, #28219, #27284, #44189, #43017, #29379 ),
 .UNSPECIFIED., .F., .F. ) 
 B_SPLINE_CURVE_WITH_KNOTS ( ( 3, 2, 2, 2, 3 ),
 ( 0.08035714285714286309, 0.08095238095238095621, 0.08214285714285714246, 0.08333333333333332871, 0.08392857142857143571 ),
 .UNSPECIFIED. ) 
 CURVE ( )  GEOMETRIC_REPRESENTATION_ITEM ( )  RATIONAL_B_SPLINE_CURVE ( ( 0.9330127018922192983, 0.9330127018922200755, 1.000000000000000000, 0.8660254037844387076, 1.000000000000000000, 0.8660254037844387076, 1.000000000000000000, 0.9330127018922185211, 0.9330127018922192983 ) ) 
 REPRESENTATION_ITEM ( '' )  );
#11146 = CARTESIAN_POINT ( 'NONE',  ( -2.500000000000000444, -89.04166666393547303, -4.330127018922193649 ) ) ;
#11148 = ORIENTED_EDGE ( 'NONE', *, *, #57913, .F. ) ;
#11147 = CARTESIAN_POINT ( 'NONE',  ( -4.999999999999998224, -34.79166666393547303, 2.886751345948131764 ) ) ;
#11149 = CARTESIAN_POINT ( 'NONE',  ( -54.60164318462004474, -143.3750000000000284, -4.984105922594373794 ) ) ;
#11150 = CIRCLE ( 'NONE', #25528, 5.000000000000000000 ) ;
#11151 = CARTESIAN_POINT ( 'NONE',  ( 9.457646018065525792E-16, -32.31249999863440792, 5.148502694627439702 ) ) ;
#11152 = CARTESIAN_POINT ( 'NONE',  ( 5.000000000000000888, -5.458333330602148870, 2.886751345948126879 ) ) ;
#11153 = VERTEX_POINT ( 'NONE', #44091 ) ;
#11154 = CONTEXT_DEPENDENT_SHAPE_REPRESENTATION ( #33119, #33259 ) ;
#11155 = CARTESIAN_POINT ( 'NONE',  ( 2.229367062499998831, -78.64583333196773651, -3.861377020970580887 ) ) ;
#11156 = CARTESIAN_POINT ( 'NONE',  ( -4.458734124999999437, -109.6458333319677365, -2.574251347313719407 ) ) ;
#11157 = CARTESIAN_POINT ( 'NONE',  ( 1.975475456537005874E-15, -44.74999999999999289, 5.000000000000000000 ) ) ;
#11158 = ORIENTED_EDGE ( 'NONE', *, *, #39188, .T. ) ;
#11159 = CARTESIAN_POINT ( 'NONE',  ( 1.975475456537005874E-15, -25.75000000000000355, 5.000000000000000000 ) ) ;
#11160 = CARTESIAN_POINT ( 'NONE',  ( -59.29741812935640155, -142.8750000013656063, -2.196230717870135685 ) ) ;
#11161 = CARTESIAN_POINT ( 'NONE',  ( 4.458734125000001214, -77.14583333196775072, 2.574251347313718519 ) ) ;
#11162 = CARTESIAN_POINT ( 'NONE',  ( -55.39835681537999790, -135.0000000027312126, 4.984105922594378235 ) ) ;
#11163 = CARTESIAN_POINT ( 'NONE',  ( 4.458734124999998549, -43.72916666530106511, -2.574251347313721627 ) ) ;
#11164 = CARTESIAN_POINT ( 'NONE',  ( -8.190561711645485556E-16, -142.9375000013656063, 4.458734124999999437 ) ) ;
#11165 = CARTESIAN_POINT ( 'NONE',  ( -3.152548672688508926E-16, -51.56249999863440792, -5.148502694627439702 ) ) ;
#11166 = CARTESIAN_POINT ( 'NONE',  ( -4.458734124999999437, -47.31249999863440792, 0.000000000000000000 ) ) ;
#11167 = CARTESIAN_POINT ( 'NONE',  ( -60.14911071818853827, -135.0625000000000284, 1.666127454062502622 ) ) ;
#11168 = CARTESIAN_POINT ( 'NONE',  ( 9.457646018065525792E-16, -17.06249999863440792, 5.148502694627439702 ) ) ;
#11169 = CARTESIAN_POINT ( 'NONE',  ( 5.000000000000000888, -99.58333333333334281, 2.886751345948126879 ) ) ;
#11170 = CARTESIAN_POINT ( 'NONE',  ( -1.846868145590737420, -141.0000000013656063, 4.458734124999999437 ) ) ;
#11171 = CARTESIAN_POINT ( 'NONE',  ( 2.229367062499998831, -37.89583333196773651, -3.861377020970580887 ) ) ;
#11172 = CARTESIAN_POINT ( 'NONE',  ( 2.499999999999998668, 8.791666669397853795, -4.330127018922193649 ) ) ;
#11173 = CARTESIAN_POINT ( 'NONE',  ( 1.975475456537005874E-15, -6.624999997268813168, 5.000000000000000000 ) ) ;
#11174 = CARTESIAN_POINT ( 'NONE',  ( -59.59170313451811296, -127.5000000013656347, 1.485763867205729394 ) ) ;
#11175 = CARTESIAN_POINT ( 'NONE',  ( 2.229367062499998831, -71.89583333196773651, -3.861377020970580887 ) ) ;
#11176 = DIRECTION ( 'NONE',  ( -0.000000000000000000, 1.000000000000000000, -0.000000000000000000 ) ) ;
#11177 = FACE_OUTER_BOUND ( 'NONE', #24271, .T. ) ;
#11178 = CARTESIAN_POINT ( 'NONE',  ( 4.458734124999998549, 0.02083333469892617584, -2.574251347313721627 ) ) ;
#11179 = ORIENTED_EDGE ( 'NONE', *, *, #3236, .F. ) ;
#11180 = CARTESIAN_POINT ( 'NONE',  ( 1.339745962155612702, -30.29465819873851729, -5.000000000000000000 ) ) ;
#11181 = DIRECTION ( 'NONE',  ( -0.000000000000000000, 1.000000000000000000, -0.000000000000000000 ) ) ;
#11183 = CARTESIAN_POINT ( 'NONE',  ( 4.458734124999999437, -36.81249999863440792, -5.460374474430324690E-16 ) ) ;
#11182 = CARTESIAN_POINT ( 'NONE',  ( 4.458734124999998549, -85.72916666530106511, -2.574251347313721627 ) ) ;
#11184 = DIRECTION ( 'NONE',  ( -0.000000000000000000, 1.000000000000000000, -0.000000000000000000 ) ) ;
#11185 = CARTESIAN_POINT ( 'NONE',  ( 2.229367062500001939, -80.22916666530106511, 3.861377020970579999 ) ) ;
#11186 = CARTESIAN_POINT ( 'NONE',  ( 2.229367062499998831, 18.10416666803225993, -3.861377020970580887 ) ) ;
#11187 = DIRECTION ( 'NONE',  ( 0.000000000000000000, -1.000000000000000000, 0.000000000000000000 ) ) ;
#11189 = EDGE_CURVE ( 'NONE', #57597, #15422, #49562, .T. ) ;
#11188 = CARTESIAN_POINT ( 'NONE',  ( -59.29741812935640155, -136.6250000013655779, -2.196230717870135685 ) ) ;
#11190 = CARTESIAN_POINT ( 'NONE',  ( -2.229367062499996610, -6.145833331967740953, 3.861377020970582219 ) ) ;
#11191 = CARTESIAN_POINT ( 'NONE',  ( -4.458734124999998549, 20.52083333469892423, 2.574251347313722516 ) ) ;
#11192 = CARTESIAN_POINT ( 'NONE',  ( 2.229367062499998831, -45.89583333196774362, -3.861377020970580887 ) ) ;
#11193 = CARTESIAN_POINT ( 'NONE',  ( 1.975475456537005874E-15, -105.7500000000000000, 5.000000000000000000 ) ) ;
#11194 = CARTESIAN_POINT ( 'NONE',  ( -4.458734124999999437, -83.31249999863439371, 0.000000000000000000 ) ) ;
#11195 = CARTESIAN_POINT ( 'NONE',  ( 2.229367062499998831, -1.645833331967737401, -3.861377020970580887 ) ) ;
#11196 = CARTESIAN_POINT ( 'NONE',  ( 6.123233995736766282E-16, -170.0000000000000000, -5.000000000000000000 ) ) ;
#11197 = ORIENTED_EDGE ( 'NONE', *, *, #56215, .F. ) ;
#11198 = CARTESIAN_POINT ( 'NONE',  ( 9.457646018065525792E-16, -28.31249999863440081, 5.148502694627439702 ) ) ;
#11199 = AXIS2_PLACEMENT_3D ( 'NONE', #28140, #18497, #47757 ) ;
#11200 = CARTESIAN_POINT ( 'NONE',  ( -54.64476657466781973, -130.0625000013656063, -4.444560631937228834 ) ) ;
#11201 = CARTESIAN_POINT ( 'NONE',  ( 4.458734124999998549, -76.72916666530106511, -2.574251347313721627 ) ) ;
#11202 = CARTESIAN_POINT ( 'NONE',  ( 2.229367062499998831, 28.10416666803225993, -3.861377020970580887 ) ) ;
#11203 = AXIS2_PLACEMENT_3D ( 'NONE', #7218, #26831, #41598 ) ;
#11204 = CARTESIAN_POINT ( 'NONE',  ( 2.229367062499998831, 18.35416666803225993, -3.861377020970580887 ) ) ;
#11205 = LINE ( 'NONE', #54954, #35913 ) ;
#11206 = DIRECTION ( 'NONE',  ( -0.000000000000000000, 1.000000000000000000, -0.000000000000000000 ) ) ;
#11207 = CARTESIAN_POINT ( 'NONE',  ( -2.229367062500000163, -76.72916666530106511, -3.861377020970580443 ) ) ;
#11208 = CARTESIAN_POINT ( 'NONE',  ( 2.500000000000002220, -60.66666666666665719, 4.330127018922192761 ) ) ;
#11209 = CARTESIAN_POINT ( 'NONE',  ( 2.500000000000002220, 23.45833333606451632, 4.330127018922192761 ) ) ;
#11210 = EDGE_LOOP ( 'NONE', ( #27929, #11417, #62261, #63600 ) ) ;
#11211 = CARTESIAN_POINT ( 'NONE',  ( 3.044556291839386294E-14, 18.75000000000000355, -5.000000000000000000 ) ) ;
#11212 = CARTESIAN_POINT ( 'NONE',  ( 6.123233995736766282E-16, -170.0000000000000000, -5.000000000000000000 ) ) ;
#11214 = CARTESIAN_POINT ( 'NONE',  ( 1.060575238724906964E-15, -25.75000000000000000, 5.773502691896257311 ) ) ;
#11213 = CARTESIAN_POINT ( 'NONE',  ( -9.184850993605147944E-16, -140.2500000000000000, 5.000000000000000000 ) ) ;
#11215 = CARTESIAN_POINT ( 'NONE',  ( -2.229367062500000163, -25.47916666530106866, -3.861377020970580443 ) ) ;
#11216 = CARTESIAN_POINT ( 'NONE',  ( -2.229367062500000163, -87.47916666530107932, -3.861377020970580443 ) ) ;
#11217 = CARTESIAN_POINT ( 'NONE',  ( 5.000000000000000888, -22.45833333060214088, 2.886751345948126879 ) ) ;
#11219 = ORIENTED_EDGE ( 'NONE', *, *, #17824, .T. ) ;
#11218 = CARTESIAN_POINT ( 'NONE',  ( 2.229367062500001939, -53.97916666530107221, 3.861377020970579999 ) ) ;
#11220 = CARTESIAN_POINT ( 'NONE',  ( 5.000000000000000000, -49.50000000000000000, -6.123233995736766282E-16 ) ) ;
#11221 = CARTESIAN_POINT ( 'NONE',  ( 2.500000000000002220, -59.54166666393546592, 4.330127018922192761 ) ) ;
#11223 = ORIENTED_EDGE ( 'NONE', *, *, #9608, .T. ) ;
#11222 = CARTESIAN_POINT ( 'NONE',  ( -2.229367062499996610, -2.395833331967737845, 3.861377020970582219 ) ) ;
#11224 = CARTESIAN_POINT ( 'NONE',  ( -4.999999999999999112, -63.91666666666666430, 2.886751345948131764 ) ) ;
#11225 = CARTESIAN_POINT ( 'NONE',  ( -3.152801135295367096, -150.3125000013655779, -3.152801135295367541 ) ) ;
#11226 = CARTESIAN_POINT ( 'NONE',  ( 2.229367062499998831, -45.89583333196774362, -3.861377020970580887 ) ) ;
#11227 = CARTESIAN_POINT ( 'NONE',  ( 2.499999999999998668, -23.33333333333333215, -4.330127018922193649 ) ) ;
#11228 = CARTESIAN_POINT ( 'NONE',  ( -2.071067811865478170, -157.3125000000000000, 5.000000000000000000 ) ) ;
#11229 = CARTESIAN_POINT ( 'NONE',  ( -6.972266317189433020E-16, -10.12499999726881406, -5.000000000000000000 ) ) ;
#11230 = CARTESIAN_POINT ( 'NONE',  ( -53.33387254593733928, -153.8125000000000000, 5.149110718188519620 ) ) ;
#11231 = CARTESIAN_POINT ( 'NONE',  ( -2.229367062500000163, -13.72916666530107221, -3.861377020970580443 ) ) ;
#11232 = CARTESIAN_POINT ( 'NONE',  ( -2.229367062500000163, -52.72916666530107221, -3.861377020970580443 ) ) ;
#11233 =( BOUNDED_CURVE ( )  B_SPLINE_CURVE ( 2, ( #15450, #15764, #49531, #26052, #45666, #30543, #50167, #6443, #6122 ),
 .UNSPECIFIED., .F., .F. ) 
 B_SPLINE_CURVE_WITH_KNOTS ( ( 3, 2, 2, 2, 3 ),
 ( 0.1437499999999999889, 0.1444444444444444309, 0.1458333333333333426, 0.1472222222222222265, 0.1479166666666666685 ),
 .UNSPECIFIED. ) 
 CURVE ( )  GEOMETRIC_REPRESENTATION_ITEM ( )  RATIONAL_B_SPLINE_CURVE ( ( 0.9330127018922194093, 0.9330127018922194093, 1.000000000000000000, 0.8660254037844387076, 1.000000000000000000, 0.8660254037844387076, 1.000000000000000000, 0.9330127018922194093, 0.9330127018922194093 ) ) 
 REPRESENTATION_ITEM ( '' )  );
#11234 = CARTESIAN_POINT ( 'NONE',  ( 5.275681513340003914E-14, 10.74999999999999645, -5.000000000000000000 ) ) ;
#11235 = CARTESIAN_POINT ( 'NONE',  ( 4.458734125000000326, -144.3750000013656063, -1.846868145590734978 ) ) ;
#11236 = CARTESIAN_POINT ( 'NONE',  ( 4.458734124999999437, -97.06249999863440792, -5.460374474430324690E-16 ) ) ;
#11237 = CARTESIAN_POINT ( 'NONE',  ( -2.499999999999996447, -106.8333333333333428, 4.330127018922195425 ) ) ;
#11238 = ORIENTED_EDGE ( 'NONE', *, *, #5883, .F. ) ;
#11239 = CARTESIAN_POINT ( 'NONE',  ( -4.999999999999998224, 14.20833333606451987, 2.886751345948131764 ) ) ;
#11240 = CARTESIAN_POINT ( 'NONE',  ( -3.152548672688508926E-16, 27.18750000136559564, -5.148502694627439702 ) ) ;
#11241 = CARTESIAN_POINT ( 'NONE',  ( -49.85088928181150436, -145.6875000027311842, -1.666127454062680702 ) ) ;
#11242 = COLOUR_RGB ( '',0.8941176470588234615, 0.8941176470588234615, 0.8941176470588234615 ) ;
#11243 = CARTESIAN_POINT ( 'NONE',  ( -6.972266317189433020E-16, -50.24999999999999289, -5.000000000000000000 ) ) ;
#11244 = ORIENTED_EDGE ( 'NONE', *, *, #54759, .F. ) ;
#11245 = CARTESIAN_POINT ( 'NONE',  ( -4.458734124999999437, -1.312499998634406140, 0.000000000000000000 ) ) ;
#11246 = CARTESIAN_POINT ( 'NONE',  ( 2.499999999999998668, -19.33333333333333570, -4.330127018922193649 ) ) ;
#11247 = CARTESIAN_POINT ( 'NONE',  ( -4.458734124999999437, -15.56249999863440436, 0.000000000000000000 ) ) ;
#11248 = CARTESIAN_POINT ( 'NONE',  ( -2.500000000000000444, 8.833333333333332149, -4.330127018922193649 ) ) ;
#11249 = CARTESIAN_POINT ( 'NONE',  ( 2.229367062500001939, -5.979166665301072214, 3.861377020970579999 ) ) ;
#11250 = FACE_OUTER_BOUND ( 'NONE', #7122, .T. ) ;
#11251 = CARTESIAN_POINT ( 'NONE',  ( -1.846868145590737420, -148.7500000013656063, 4.458734124999997661 ) ) ;
#11252 = CARTESIAN_POINT ( 'NONE',  ( 4.458734124999998549, 17.02083333469892779, -2.574251347313721627 ) ) ;
#11253 = ORIENTED_EDGE ( 'NONE', *, *, #33502, .T. ) ;
#11254 = CARTESIAN_POINT ( 'NONE',  ( -5.000000000000000000, -26.87499999726881583, 0.000000000000000000 ) ) ;
#11255 = CARTESIAN_POINT ( 'NONE',  ( -1.339745962155613812, -13.20534180126147916, -5.000000000000000000 ) ) ;
#11256 = CARTESIAN_POINT ( 'NONE',  ( -2.229367062500000163, -18.47916666530106866, -3.861377020970580443 ) ) ;
#11257 = CARTESIAN_POINT ( 'NONE',  ( 1.339745962155612702, -25.16965819600734022, -5.000000000000000000 ) ) ;
#11258 = CARTESIAN_POINT ( 'NONE',  ( 5.000000000000000000, 1.625000002731184834, -6.123233995736766282E-16 ) ) ;
#11259 = CARTESIAN_POINT ( 'NONE',  ( -52.10840900171896806, -150.1875000013656063, 3.393966926194110556 ) ) ;
#11260 = CARTESIAN_POINT ( 'NONE',  ( 5.000000000000000000, -49.37499999726880873, -6.123233995736766282E-16 ) ) ;
#11261 = DIRECTION ( 'NONE',  ( -0.000000000000000000, 1.000000000000000000, -0.000000000000000000 ) ) ;
#11262 = CARTESIAN_POINT ( 'NONE',  ( -4.458734124999997661, 8.770833334698927786, 2.574251347313722516 ) ) ;
#11263 = CARTESIAN_POINT ( 'NONE',  ( 1.243387493232115550E-13, -9.124999997268817609, -5.000000000000000000 ) ) ;
#11264 = CARTESIAN_POINT ( 'NONE',  ( 0.000000000000000000, -120.0000000000000000, 5.000000000000000000 ) ) ;
#11265 = CARTESIAN_POINT ( 'NONE',  ( 2.229367062499998831, 10.35416666803225993, -3.861377020970580887 ) ) ;
#11266 = CARTESIAN_POINT ( 'NONE',  ( 2.229367062499998831, -65.64583333196773651, -3.861377020970580887 ) ) ;
#11267 = CARTESIAN_POINT ( 'NONE',  ( 2.229367062499998831, -14.89583333196773474, -3.861377020970580887 ) ) ;
#11268 = CARTESIAN_POINT ( 'NONE',  ( -2.499999999999996447, 3.166666666666664742, 4.330127018922195425 ) ) ;
#11269 = CARTESIAN_POINT ( 'NONE',  ( -8.190561711645485556E-16, -165.6875000013655779, 4.458734124999999437 ) ) ;
#11270 = CARTESIAN_POINT ( 'NONE',  ( 2.499999999999998668, 23.66666666666666430, -4.330127018922193649 ) ) ;
#11271 = CARTESIAN_POINT ( 'NONE',  ( -3.152548672688508926E-16, -60.56249999863440792, -5.148502694627439702 ) ) ;
#11272 = CARTESIAN_POINT ( 'NONE',  ( 2.499999999999998668, -96.20833333060213022, -4.330127018922193649 ) ) ;
#11273 = CARTESIAN_POINT ( 'NONE',  ( -4.330127018922101279, 30.00000000000000000, 7.500000000000002665 ) ) ;
#11274 = CARTESIAN_POINT ( 'NONE',  ( -4.999999999999998224, -69.91666666666667140, 2.886751345948131764 ) ) ;
#11275 = CARTESIAN_POINT ( 'NONE',  ( 1.975475456537005874E-15, -56.75000000000000000, 5.000000000000000000 ) ) ;
#11276 = CARTESIAN_POINT ( 'NONE',  ( -4.458734124999997661, -35.22916666530107221, 2.574251347313722516 ) ) ;
#11277 = DIRECTION ( 'NONE',  ( 0.6485228581062915110, 0.000000000000000000, 0.7611951803011149931 ) ) ;
#11278 = CARTESIAN_POINT ( 'NONE',  ( -3.535250795749689387E-16, -41.25000000000000000, -5.773502691896257311 ) ) ;
#11279 = CARTESIAN_POINT ( 'NONE',  ( -1.339745962155610925, -57.66965819600732601, 5.000000000000000000 ) ) ;
#11280 = CARTESIAN_POINT ( 'NONE',  ( -5.000000000000000000, -107.9999999999999858, 0.000000000000000000 ) ) ;
#11281 = ORIENTED_EDGE ( 'NONE', *, *, #61532, .F. ) ;
#11282 = CARTESIAN_POINT ( 'NONE',  ( 9.457646018065525792E-16, -107.0624999986343937, 5.148502694627439702 ) ) ;
#11283 = CARTESIAN_POINT ( 'NONE',  ( -2.229367062500000163, -3.729166665301070438, -3.861377020970580443 ) ) ;
#11284 =( GEOMETRIC_REPRESENTATION_CONTEXT ( 3 ) GLOBAL_UNCERTAINTY_ASSIGNED_CONTEXT ( ( #33926 ) ) GLOBAL_UNIT_ASSIGNED_CONTEXT ( ( #27925, #13141, #57845 ) ) REPRESENTATION_CONTEXT ( 'NONE', 'WORKASPACE' ) );
#11285 = CARTESIAN_POINT ( 'NONE',  ( -3.535250795749689387E-16, -0.2500000000000002220, -5.773502691896257311 ) ) ;
#11286 = CARTESIAN_POINT ( 'NONE',  ( 4.458734124999999437, -72.81249999863439371, -5.460374474430324690E-16 ) ) ;
#11287 = CARTESIAN_POINT ( 'NONE',  ( 1.339745962155612702, -22.16965819600733312, -5.000000000000000000 ) ) ;
#11288 = CARTESIAN_POINT ( 'NONE',  ( -2.500000000000000444, -7.041666663935481907, -4.330127018922193649 ) ) ;
#11290 = ORIENTED_EDGE ( 'NONE', *, *, #5800, .T. ) ;
#11289 = CARTESIAN_POINT ( 'NONE',  ( -2.229367062499996610, -41.14583333196773651, 3.861377020970582219 ) ) ;
#11291 = CARTESIAN_POINT ( 'NONE',  ( 2.499999999999998668, -6.333333333333336590, -4.330127018922193649 ) ) ;
#11293 = VERTEX_POINT ( 'NONE', #50198 ) ;
#11292 = CARTESIAN_POINT ( 'NONE',  ( -3.152548672688508926E-16, 11.18750000136559564, -5.148502694627439702 ) ) ;
#11294 = CARTESIAN_POINT ( 'NONE',  ( 2.499999999999998668, -101.3333333333333286, -4.330127018922193649 ) ) ;
#11295 = CARTESIAN_POINT ( 'NONE',  ( -5.000000000000000000, -52.99999999999999289, 0.000000000000000000 ) ) ;
#11296 = CARTESIAN_POINT ( 'NONE',  ( -4.458734124999998549, -29.47916666530106866, 2.574251347313722516 ) ) ;
#11297 = DIRECTION ( 'NONE',  ( -0.000000000000000000, 1.000000000000000000, -0.000000000000000000 ) ) ;
#11298 = CARTESIAN_POINT ( 'NONE',  ( 9.457646018065525792E-16, -76.06249999863440792, 5.148502694627439702 ) ) ;
#11299 =( BOUNDED_CURVE ( )  B_SPLINE_CURVE ( 2, ( #43069, #62707, #13800, #33421, #18932, #33733, #53351, #9286, #44323 ),
 .UNSPECIFIED., .F., .F. ) 
 B_SPLINE_CURVE_WITH_KNOTS ( ( 3, 2, 2, 2, 3 ),
 ( 0.9187499999999999556, 0.9194444444444443976, 0.9208333333333332815, 0.9222222222222222765, 0.9229166666666667185 ),
 .UNSPECIFIED. ) 
 CURVE ( )  GEOMETRIC_REPRESENTATION_ITEM ( )  RATIONAL_B_SPLINE_CURVE ( ( 0.9330127018922194093, 0.9330127018922194093, 1.000000000000000000, 0.8660254037844387076, 1.000000000000000000, 0.8660254037844387076, 1.000000000000000000, 0.9330127018922194093, 0.9330127018922194093 ) ) 
 REPRESENTATION_ITEM ( '' )  );
#11300 = CARTESIAN_POINT ( 'NONE',  ( -4.458734125000000326, -141.2500000013656063, -1.846868145590735644 ) ) ;
#11301 = CARTESIAN_POINT ( 'NONE',  ( 9.457646018065525792E-16, -80.06249999863439371, 5.148502694627439702 ) ) ;
#11302 = CARTESIAN_POINT ( 'NONE',  ( -51.60603307380591787, -136.1875000013656063, -2.891590998281053704 ) ) ;
#11303 = CARTESIAN_POINT ( 'NONE',  ( -4.458734124999999437, -35.56249999863440792, 0.000000000000000000 ) ) ;
#11304 = VERTEX_POINT ( 'NONE', #29287 ) ;
#11305 = CARTESIAN_POINT ( 'NONE',  ( 1.975475456537005874E-15, -16.62499999726881583, 5.000000000000000000 ) ) ;
#11306 = ORIENTED_EDGE ( 'NONE', *, *, #48449, .T. ) ;
#11307 = CARTESIAN_POINT ( 'NONE',  ( -2.229367062500000163, -78.72916666530106511, -3.861377020970580443 ) ) ;
#11308 = CYLINDRICAL_SURFACE ( 'NONE', #30710, 5.000000000000000000 ) ;
#11309 = EDGE_LOOP ( 'NONE', ( #34515, #37261, #46350, #54536 ) ) ;
#11310 = LINE ( 'NONE', #30292, #43932 ) ;
#11311 = CARTESIAN_POINT ( 'NONE',  ( -1.339745962155613812, 7.794658198738521726, -5.000000000000000000 ) ) ;
#11313 = EDGE_CURVE ( 'NONE', #52441, #1445, #47729, .T. ) ;
#11312 = CARTESIAN_POINT ( 'NONE',  ( -4.458734124999998549, -63.47916666530106511, 2.574251347313722516 ) ) ;
#11314 = CARTESIAN_POINT ( 'NONE',  ( 4.458734124999998549, -4.979166665301072214, -2.574251347313721627 ) ) ;
#11315 = VERTEX_POINT ( 'NONE', #1023 ) ;
#11316 = CARTESIAN_POINT ( 'NONE',  ( 1.339745962155590275, 3.419658201469704562, 5.000000000000013323 ) ) ;
#11317 = CARTESIAN_POINT ( 'NONE',  ( 0.000000000000000000, -120.0000000000000000, 0.000000000000000000 ) ) ;
#11318 = ORIENTED_EDGE ( 'NONE', *, *, #10316, .F. ) ;
#11319 = CARTESIAN_POINT ( 'NONE',  ( 5.000000000000000888, -91.58333333333334281, 2.886751345948126879 ) ) ;
#11320 = CARTESIAN_POINT ( 'NONE',  ( -2.229367062499996610, 5.854166668032262599, 3.861377020970582219 ) ) ;
#11321 = AXIS2_PLACEMENT_3D ( 'NONE', #62064, #26696, #17977 ) ;
#11322 = CARTESIAN_POINT ( 'NONE',  ( 4.458734124999999437, -160.3750000013655779, -1.846868145590734978 ) ) ;
#11323 =( BOUNDED_CURVE ( )  B_SPLINE_CURVE ( 2, ( #12746, #53483, #43817, #58630, #18206 ),
 .UNSPECIFIED., .F., .F. ) 
 B_SPLINE_CURVE_WITH_KNOTS ( ( 3, 2, 3 ),
 ( 0.000000000000000000, 0.001190476190476190584, 0.001785714285714286092 ),
 .UNSPECIFIED. ) 
 CURVE ( )  GEOMETRIC_REPRESENTATION_ITEM ( )  RATIONAL_B_SPLINE_CURVE ( ( 1.000000000000000000, 0.8660254037844387076, 1.000000000000000000, 0.9330127018922192983, 0.9330127018922194093 ) ) 
 REPRESENTATION_ITEM ( '' )  );
#11324 = FACE_OUTER_BOUND ( 'NONE', #55623, .T. ) ;
#11325 = VERTEX_POINT ( 'NONE', #24804 ) ;
#11326 = CARTESIAN_POINT ( 'NONE',  ( -4.458734124999999437, -79.39583333196773651, -2.574251347313719407 ) ) ;
#11327 = CARTESIAN_POINT ( 'NONE',  ( 5.000000000000000000, -75.50000000000000000, -6.123233995736766282E-16 ) ) ;
#11328 = CARTESIAN_POINT ( 'NONE',  ( 2.229367062500001939, -1.979166665301068662, 3.861377020970579999 ) ) ;
#11329 = CARTESIAN_POINT ( 'NONE',  ( -2.498395430326213474E-14, 15.25000000000000000, 5.000000000000000000 ) ) ;
#11330 = EDGE_CURVE ( 'NONE', #46232, #51312, #23879, .T. ) ;
#11331 = CARTESIAN_POINT ( 'NONE',  ( 5.000000000000000888, 4.541666669397852019, 2.886751345948126879 ) ) ;
#11332 = CARTESIAN_POINT ( 'NONE',  ( -4.458734124999999437, -69.64583333196773651, -2.574251347313719407 ) ) ;
#11333 = CARTESIAN_POINT ( 'NONE',  ( -3.535250795749689387E-16, -31.12499999726881228, -5.773502691896257311 ) ) ;
#11334 = ADVANCED_FACE ( 'NONE', ( #59219 ), #20628, .T. ) ;
#11335 = CARTESIAN_POINT ( 'NONE',  ( -5.000000000000000000, -15.00000000000000000, 0.000000000000000000 ) ) ;
#11336 = CARTESIAN_POINT ( 'NONE',  ( -2.229367062499996610, 28.85416666803226349, 3.861377020970582219 ) ) ;
#11337 = CARTESIAN_POINT ( 'NONE',  ( 5.000000000000000888, -104.5833333333333286, 2.886751345948126879 ) ) ;
#11338 = CARTESIAN_POINT ( 'NONE',  ( -3.152548672688508926E-16, 26.43750000136559564, -5.148502694627439702 ) ) ;
#11339 = CARTESIAN_POINT ( 'NONE',  ( -4.458734124999999437, -53.39583333196773651, -2.574251347313719407 ) ) ;
#11340 = CARTESIAN_POINT ( 'NONE',  ( 9.457646018065525792E-16, -34.31249999863440792, 5.148502694627439702 ) ) ;
#11341 = CARTESIAN_POINT ( 'NONE',  ( -4.458734124999997661, 1.520833334698927564, 2.574251347313722516 ) ) ;
#11342 = CARTESIAN_POINT ( 'NONE',  ( -5.000000000000000888, -149.5625000027311842, 2.071067811865474617 ) ) ;
#11343 = CARTESIAN_POINT ( 'NONE',  ( 2.499999999999998668, 20.66666666666666785, -4.330127018922193649 ) ) ;
#11344 = CARTESIAN_POINT ( 'NONE',  ( -2.071067811865478170, -146.4375000027311842, 5.000000000000000000 ) ) ;
#11345 = CARTESIAN_POINT ( 'NONE',  ( 5.000000000000000000, -26.29166666393547658, -2.886751345948130876 ) ) ;
#11346 = CARTESIAN_POINT ( 'NONE',  ( -3.152548672688508926E-16, -41.56249999863439371, -5.148502694627439702 ) ) ;
#11347 = CARTESIAN_POINT ( 'NONE',  ( 5.000000000000000000, -77.29166666393545881, -2.886751345948129988 ) ) ;
#11348 = EDGE_CURVE ( 'NONE', #897, #42031, #19358, .T. ) ;
#11349 = CARTESIAN_POINT ( 'NONE',  ( -50.40829686548195099, -140.2500000013656063, -1.485763867205728284 ) ) ;
#11350 = DIRECTION ( 'NONE',  ( 0.000000000000000000, 0.000000000000000000, 1.000000000000000000 ) ) ;
#11351 = DIRECTION ( 'NONE',  ( -0.000000000000000000, 1.000000000000000000, -0.000000000000000000 ) ) ;
#11352 = CARTESIAN_POINT ( 'NONE',  ( -3.152548672688508926E-16, -78.81249999863442213, -5.148502694627439702 ) ) ;
#11353 = CARTESIAN_POINT ( 'NONE',  ( -4.458734124999999437, -161.2500000013655779, -1.846868145590735644 ) ) ;
#11354 = CARTESIAN_POINT ( 'NONE',  ( -2.499999999999996447, -24.83333333333333215, 4.330127018922195425 ) ) ;
#11355 = CARTESIAN_POINT ( 'NONE',  ( -1.846868145590734756, -141.1250000013655779, -4.458734125000000326 ) ) ;
#11356 = ORIENTED_EDGE ( 'NONE', *, *, #23548, .T. ) ;
#11357 = CARTESIAN_POINT ( 'NONE',  ( 4.458734125000001214, 23.85416666803225993, 2.574251347313718519 ) ) ;
#11358 = VERTEX_POINT ( 'NONE', #26717 ) ;
#11359 = CARTESIAN_POINT ( 'NONE',  ( 5.000000000000000000, 18.62500000273118772, -6.123233995736766282E-16 ) ) ;
#11360 = CARTESIAN_POINT ( 'NONE',  ( 1.339745962155615144, 2.294658198738519950, 4.999999999999999112 ) ) ;
#11361 = CARTESIAN_POINT ( 'NONE',  ( 5.000000000000000000, 11.58333333333333570, -2.886751345948129988 ) ) ;
#11362 = CARTESIAN_POINT ( 'NONE',  ( -4.458734124999997661, -52.22916666530107932, 2.574251347313722516 ) ) ;
#11363 = CARTESIAN_POINT ( 'NONE',  ( 4.458734124999998549, -13.72916666530107399, -2.574251347313721627 ) ) ;
#11364 = CARTESIAN_POINT ( 'NONE',  ( 7.499999999999999112, 0.7577384720672989404, -7.446470314338469620 ) ) ;
#11365 = EDGE_CURVE ( 'NONE', #46520, #56134, #51170, .T. ) ;
#11366 = CARTESIAN_POINT ( 'NONE',  ( -53.51423613279429503, -136.5000000013656063, 4.591703134518083651 ) ) ;
#11367 = CARTESIAN_POINT ( 'NONE',  ( 0.000000000000000000, -170.0000000000000000, 5.000000000000000000 ) ) ;
#11368 = CARTESIAN_POINT ( 'NONE',  ( -1.339745962155613812, -37.20534180126147561, -5.000000000000000000 ) ) ;
#11369 = CARTESIAN_POINT ( 'NONE',  ( 5.000000000000000888, -11.45833333060214976, 2.886751345948126879 ) ) ;
#11370 = CARTESIAN_POINT ( 'NONE',  ( 5.000000000000000000, -35.50000000000000711, -6.123233995736766282E-16 ) ) ;
#11371 = CARTESIAN_POINT ( 'NONE',  ( 2.500000000000002220, -56.54166666393548013, 4.330127018922192761 ) ) ;
#11372 = PRESENTATION_LAYER_ASSIGNMENT (  '', '', ( #59644 ) ) ;
#11374 = CARTESIAN_POINT ( 'NONE',  ( -3.152548672688508926E-16, -14.81249999863440436, -5.148502694627439702 ) ) ;
#11373 = CARTESIAN_POINT ( 'NONE',  ( 5.000000000000000000, 21.62500000273118417, -6.123233995736766282E-16 ) ) ;
#11375 = DIRECTION ( 'NONE',  ( -0.000000000000000000, 1.000000000000000000, -0.000000000000000000 ) ) ;
#11376 = CARTESIAN_POINT ( 'NONE',  ( 2.229367062500001939, -56.97916666530107932, 3.861377020970579999 ) ) ;
#11377 = CARTESIAN_POINT ( 'NONE',  ( 4.458734125000000326, -153.6250000013655779, -1.846868145590734978 ) ) ;
#11378 = VECTOR ( 'NONE', #24735, 1000.000000000000000 ) ;
#11379 = CARTESIAN_POINT ( 'NONE',  ( -4.458734124999999437, -65.31249999863440792, 0.000000000000000000 ) ) ;
#11380 = CARTESIAN_POINT ( 'NONE',  ( -59.59170313451811296, -145.7500000013655779, 1.485763867205729394 ) ) ;
#11381 = CARTESIAN_POINT ( 'NONE',  ( 2.500000000000002220, -57.54166666393548013, 4.330127018922192761 ) ) ;
#11382 = ORIENTED_EDGE ( 'NONE', *, *, #22011, .F. ) ;
#11383 = FACE_OUTER_BOUND ( 'NONE', #19629, .T. ) ;
#11384 = ORIENTED_EDGE ( 'NONE', *, *, #37762, .F. ) ;
#11386 = LINE ( 'NONE', #21369, #16261 ) ;
#11385 = CARTESIAN_POINT ( 'NONE',  ( 0.000000000000000000, -170.0000000000000000, 0.000000000000000000 ) ) ;
#11387 = CARTESIAN_POINT ( 'NONE',  ( 1.846868145590735200, -154.2500000013656063, -4.458734125000000326 ) ) ;
#11388 = ORIENTED_EDGE ( 'NONE', *, *, #38099, .F. ) ;
#11389 = CARTESIAN_POINT ( 'NONE',  ( -6.972266317189433020E-16, -54.24999999999999289, -5.000000000000000000 ) ) ;
#11390 = CARTESIAN_POINT ( 'NONE',  ( -57.46284108482265651, -128.9375000000000284, 4.819101127000239515 ) ) ;
#11391 = CARTESIAN_POINT ( 'NONE',  ( -6.972266317189433020E-16, 15.75000000000000000, -5.000000000000000000 ) ) ;
#11393 = ADVANCED_FACE ( 'NONE', ( #13420 ), #55361, .T. ) ;
#11392 = CARTESIAN_POINT ( 'NONE',  ( 4.458734125000001214, -48.14583333196773651, 2.574251347313718519 ) ) ;
#11394 = VERTEX_POINT ( 'NONE', #21253 ) ;
#11395 = EDGE_CURVE ( 'NONE', #1059, #20760, #35733, .T. ) ;
#11396 = ADVANCED_FACE ( 'NONE', ( #55678 ), #52351, .T. ) ;
#11397 = CARTESIAN_POINT ( 'NONE',  ( -6.972266317189433020E-16, 16.87500000273118417, -5.000000000000000000 ) ) ;
#11398 = CARTESIAN_POINT ( 'NONE',  ( -4.458734124999998549, 11.77083333469892601, 2.574251347313722516 ) ) ;
#11399 = CARTESIAN_POINT ( 'NONE',  ( -3.152548672688508926E-16, 25.43750000136559208, -5.148502694627439702 ) ) ;
#11400 = CARTESIAN_POINT ( 'NONE',  ( -50.70258187064364108, -154.1250000013656347, 2.196230717870141014 ) ) ;
#11401 = CARTESIAN_POINT ( 'NONE',  ( 4.330127018922258486, 30.00000000000000000, 7.499999999999910294 ) ) ;
#11402 = CARTESIAN_POINT ( 'NONE',  ( 0.000000000000000000, -170.0000000000000000, 5.000000000000000000 ) ) ;
#11403 = VERTEX_POINT ( 'NONE', #60186 ) ;
#11404 = CARTESIAN_POINT ( 'NONE',  ( 2.229367062500001939, -65.97916666530106511, 3.861377020970579999 ) ) ;
#11405 = CARTESIAN_POINT ( 'NONE',  ( 9.457646018065525792E-16, 12.93750000136559386, 5.148502694627439702 ) ) ;
#11406 =( BOUNDED_CURVE ( )  B_SPLINE_CURVE ( 2, ( #55901, #16341, #40134, #1882, #21487, #1250, #50440, #51070, #20208 ),
 .UNSPECIFIED., .F., .F. ) 
 B_SPLINE_CURVE_WITH_KNOTS ( ( 3, 2, 2, 2, 3 ),
 ( 0.8854166666666666297, 0.8861111111111110716, 0.8874999999999999556, 0.8888888888888888395, 0.8895833333333332815 ),
 .UNSPECIFIED. ) 
 CURVE ( )  GEOMETRIC_REPRESENTATION_ITEM ( )  RATIONAL_B_SPLINE_CURVE ( ( 0.9330127018922194093, 0.9330127018922194093, 1.000000000000000000, 0.8660254037844387076, 1.000000000000000000, 0.8660254037844387076, 1.000000000000000000, 0.9330127018922194093, 0.9330127018922194093 ) ) 
 REPRESENTATION_ITEM ( '' )  );
#11407 = CARTESIAN_POINT ( 'NONE',  ( 1.975475456537005874E-15, -63.74999999999998579, 5.000000000000000000 ) ) ;
#11408 = CARTESIAN_POINT ( 'NONE',  ( -6.972266317189433020E-16, -2.124999997268814056, -5.000000000000000000 ) ) ;
#11409 = CARTESIAN_POINT ( 'NONE',  ( 4.458734124999999437, -53.06249999863440792, -5.460374474430324690E-16 ) ) ;
#11410 = CARTESIAN_POINT ( 'NONE',  ( -4.999999999999999112, -12.79166666393547835, 2.886751345948131764 ) ) ;
#11411 = FACE_OUTER_BOUND ( 'NONE', #33468, .T. ) ;
#11412 = EDGE_CURVE ( 'NONE', #8866, #61326, #32724, .T. ) ;
#11413 = CYLINDRICAL_SURFACE ( 'NONE', #11121, 5.000000000000000000 ) ;
#11414 = CARTESIAN_POINT ( 'NONE',  ( 8.660254037844342889, 30.00000000000000000, 0.000000000000000000 ) ) ;
#11415 = CARTESIAN_POINT ( 'NONE',  ( 5.000000000000000000, -104.2916666639354730, -2.886751345948130876 ) ) ;
#11416 = CARTESIAN_POINT ( 'NONE',  ( 2.229367062499998831, -14.89583333196773474, -3.861377020970580887 ) ) ;
#11417 = ORIENTED_EDGE ( 'NONE', *, *, #49475, .T. ) ;
#11418 = CARTESIAN_POINT ( 'NONE',  ( -9.184850993605147944E-16, -143.3750000027312126, 5.000000000000000000 ) ) ;
#11419 = CARTESIAN_POINT ( 'NONE',  ( 2.229367062499998831, -103.6458333319677365, -3.861377020970580887 ) ) ;
#11420 = CARTESIAN_POINT ( 'NONE',  ( -5.000000000000000888, -155.6875000027312126, -2.071067811865475949 ) ) ;
#11421 = ORIENTED_EDGE ( 'NONE', *, *, #49870, .T. ) ;
#11422 = CARTESIAN_POINT ( 'NONE',  ( -4.458734124999999437, -101.6458333319677365, -2.574251347313719407 ) ) ;
#11423 = AXIS2_PLACEMENT_3D ( 'NONE', #58441, #15246, #57199 ) ;
#11424 = CARTESIAN_POINT ( 'NONE',  ( 4.458734124999999437, -28.81249999863440436, -5.460374474430324690E-16 ) ) ;
#11425 = CARTESIAN_POINT ( 'NONE',  ( 5.000000000000000000, -61.29166666393548013, -2.886751345948129988 ) ) ;
#11426 = CARTESIAN_POINT ( 'NONE',  ( -51.60603307380591787, -152.1875000013656063, -2.891590998281053704 ) ) ;
#11427 =( BOUNDED_CURVE ( )  B_SPLINE_CURVE ( 2, ( #23380, #9506, #47800, #52950, #8887, #48432, #23691, #43290, #28812 ),
 .UNSPECIFIED., .F., .F. ) 
 B_SPLINE_CURVE_WITH_KNOTS ( ( 3, 2, 2, 2, 3 ),
 ( 0.5875000000000000222, 0.5880952380952381153, 0.5892857142857143016, 0.5904761904761904878, 0.5910714285714285809 ),
 .UNSPECIFIED. ) 
 CURVE ( )  GEOMETRIC_REPRESENTATION_ITEM ( )  RATIONAL_B_SPLINE_CURVE ( ( 0.9330127018922194093, 0.9330127018922194093, 1.000000000000000000, 0.8660254037844387076, 1.000000000000000000, 0.8660254037844387076, 1.000000000000000000, 0.9330127018922194093, 0.9330127018922194093 ) ) 
 REPRESENTATION_ITEM ( '' )  );
#11428 = CARTESIAN_POINT ( 'NONE',  ( -53.51423613279429503, -142.2500000013656063, 4.591703134518083651 ) ) ;
#11429 = CARTESIAN_POINT ( 'NONE',  ( 4.458734125000000326, -23.89583333196773651, 2.574251347313718519 ) ) ;
#11430 = CARTESIAN_POINT ( 'NONE',  ( -2.229367062500000163, -61.72916666530106511, -3.861377020970580443 ) ) ;
#11431 = CARTESIAN_POINT ( 'NONE',  ( 1.975475456537005874E-15, -89.74999999999998579, 5.000000000000000000 ) ) ;
#11432 = CARTESIAN_POINT ( 'NONE',  ( -2.229367062499996610, -21.14583333196774007, 3.861377020970582219 ) ) ;
#11433 = CARTESIAN_POINT ( 'NONE',  ( -6.031010364368858512E-14, 4.249999999999995559, 5.000000000000000000 ) ) ;
#11434 = CARTESIAN_POINT ( 'NONE',  ( 2.071067811865476394, -151.1875000000000000, 5.000000000000000000 ) ) ;
#11435 = CARTESIAN_POINT ( 'NONE',  ( -5.000000000000000000, -13.99999999999999822, 0.000000000000000000 ) ) ;
#11436 = CARTESIAN_POINT ( 'NONE',  ( 1.846868145590736310, -151.6250000013656063, 4.458734124999999437 ) ) ;
#11437 = ORIENTED_EDGE ( 'NONE', *, *, #16894, .F. ) ;
#11438 = CARTESIAN_POINT ( 'NONE',  ( -4.458734124999999437, -43.64583333196773651, -2.574251347313719407 ) ) ;
#11439 = CARTESIAN_POINT ( 'NONE',  ( 1.975475456537005874E-15, -12.62499999726881050, 5.000000000000000000 ) ) ;
#11440 = FACE_OUTER_BOUND ( 'NONE', #51205, .T. ) ;
#11441 = CARTESIAN_POINT ( 'NONE',  ( 1.060575238724906964E-15, 29.25000000000000000, 5.773502691896257311 ) ) ;
#11442 = CARTESIAN_POINT ( 'NONE',  ( 4.458734124999998549, 3.270833334698929118, -2.574251347313721627 ) ) ;
#11443 = CARTESIAN_POINT ( 'NONE',  ( -9.184850993605147944E-16, -160.3750000027311842, 5.000000000000000000 ) ) ;
#11444 = CARTESIAN_POINT ( 'NONE',  ( 2.499999999999998668, -11.20833333060214798, -4.330127018922193649 ) ) ;
#11445 = CARTESIAN_POINT ( 'NONE',  ( -1.339745962155614700, 26.20534180126147561, 4.999999999999999112 ) ) ;
#11446 = CARTESIAN_POINT ( 'NONE',  ( 4.458734124999999437, 15.93750000136559564, -5.460374474430324690E-16 ) ) ;
#11447 = CARTESIAN_POINT ( 'NONE',  ( -4.999999999999999112, -81.91666666666665719, 2.886751345948131764 ) ) ;
#11448 = CARTESIAN_POINT ( 'NONE',  ( 5.000000000000000000, 7.625000002731186832, -6.123233995736766282E-16 ) ) ;
#11449 = ORIENTED_EDGE ( 'NONE', *, *, #57018, .F. ) ;
#11450 = CARTESIAN_POINT ( 'NONE',  ( 1.975475456537005874E-15, 4.375000002731185056, 5.000000000000000000 ) ) ;
#11451 = ORIENTED_EDGE ( 'NONE', *, *, #7605, .T. ) ;
#11452 = DIRECTION ( 'NONE',  ( -0.000000000000000000, 1.000000000000000000, -0.000000000000000000 ) ) ;
#11453 = CARTESIAN_POINT ( 'NONE',  ( 4.458734124999999437, -45.81249999863440081, -5.460374474430324690E-16 ) ) ;
#11454 = CARTESIAN_POINT ( 'NONE',  ( 4.458734125000000326, -164.6250000013655779, -1.846868145590734978 ) ) ;
#11455 = CARTESIAN_POINT ( 'NONE',  ( 2.499999999999998668, -42.20833333060214443, -4.330127018922193649 ) ) ;
#11456 = ORIENTED_EDGE ( 'NONE', *, *, #27532, .T. ) ;
#11457 = CARTESIAN_POINT ( 'NONE',  ( 4.458734124999999437, -16.81249999863440436, -5.460374474430324690E-16 ) ) ;
#11458 = VERTEX_POINT ( 'NONE', #20943 ) ;
#11459 = CARTESIAN_POINT ( 'NONE',  ( 2.500000000000002220, -87.66666666666667140, 4.330127018922192761 ) ) ;
#11460 = CARTESIAN_POINT ( 'NONE',  ( -4.458734124999999437, -162.9375000013655779, -5.460374474430324690E-16 ) ) ;
#11461 = CARTESIAN_POINT ( 'NONE',  ( 2.500000000000002220, -87.54166666393547303, 4.330127018922192761 ) ) ;
#11463 = ORIENTED_EDGE ( 'NONE', *, *, #2093, .F. ) ;
#11462 = CARTESIAN_POINT ( 'NONE',  ( -1.049326080737009628E-13, -20.62499999726881583, 5.000000000000000000 ) ) ;
#11464 = AXIS2_PLACEMENT_3D ( 'NONE', #45836, #41625, #50662 ) ;
#11465 = CARTESIAN_POINT ( 'NONE',  ( -56.66612745406270335, -140.3125000000000284, -5.149110718188516067 ) ) ;
#11466 = CARTESIAN_POINT ( 'NONE',  ( -4.458734124999998549, -32.47916666530107221, 2.574251347313722516 ) ) ;
#11467 = CARTESIAN_POINT ( 'NONE',  ( -5.000000000000000000, -84.08333333333332860, -2.886751345948128211 ) ) ;
#11468 = EDGE_LOOP ( 'NONE', ( #24641, #38954, #55862, #10859 ) ) ;
#11469 = EDGE_CURVE ( 'NONE', #19054, #24216, #8286, .T. ) ;
#11470 = EDGE_CURVE ( 'NONE', #23690, #37137, #39454, .T. ) ;
#11471 = CARTESIAN_POINT ( 'NONE',  ( -3.152548672688508926E-16, -79.56249999863440792, -5.148502694627439702 ) ) ;
#11472 = CARTESIAN_POINT ( 'NONE',  ( -2.229367062500000163, -109.7291666653010651, -3.861377020970580443 ) ) ;
#11473 = CARTESIAN_POINT ( 'NONE',  ( -51.75738570946856498, -136.8750000027312126, 3.805975901505576964 ) ) ;
#11474 = EDGE_CURVE ( 'NONE', #23099, #45276, #30440, .T. ) ;
#11475 = EDGE_LOOP ( 'NONE', ( #22229, #12396, #41921, #56033 ) ) ;
#11476 = CARTESIAN_POINT ( 'NONE',  ( -1.339745962155613812, -26.20534180126147916, -5.000000000000000000 ) ) ;
#11477 = CARTESIAN_POINT ( 'NONE',  ( -50.70258187064364108, -142.3750000013656063, 2.196230717870141014 ) ) ;
#11478 = CARTESIAN_POINT ( 'NONE',  ( -2.229367062499996610, -79.39583333196773651, 3.861377020970582219 ) ) ;
#11479 = CARTESIAN_POINT ( 'NONE',  ( -50.01589407740564042, -134.7500000027312126, 0.3983568153799778022 ) ) ;
#11480 = CARTESIAN_POINT ( 'NONE',  ( -4.458734124999999437, -42.39583333196773651, -2.574251347313719407 ) ) ;
#11481 = CARTESIAN_POINT ( 'NONE',  ( 1.846868145590736310, -141.8750000013656063, 4.458734124999997661 ) ) ;
#11482 =( BOUNDED_CURVE ( )  B_SPLINE_CURVE ( 2, ( #425, #29670, #9115, #24865, #28723, #9422, #19391, #20030, #18758 ),
 .UNSPECIFIED., .F., .F. ) 
 B_SPLINE_CURVE_WITH_KNOTS ( ( 3, 2, 2, 2, 3 ),
 ( 0.5770833333333332815, 0.5777777777777777235, 0.5791666666666667185, 0.5805555555555556024, 0.5812500000000000444 ),
 .UNSPECIFIED. ) 
 CURVE ( )  GEOMETRIC_REPRESENTATION_ITEM ( )  RATIONAL_B_SPLINE_CURVE ( ( 0.9330127018922194093, 0.9330127018922194093, 1.000000000000000000, 0.8660254037844387076, 1.000000000000000000, 0.8660254037844387076, 1.000000000000000000, 0.9330127018922194093, 0.9330127018922194093 ) ) 
 REPRESENTATION_ITEM ( '' )  );
#11483 = CARTESIAN_POINT ( 'NONE',  ( 1.339745962155612702, 20.70534180126147916, -5.000000000000000000 ) ) ;
#11484 = CARTESIAN_POINT ( 'NONE',  ( -2.229367062500000163, -50.47916666530107221, -3.861377020970580443 ) ) ;
#11485 = CARTESIAN_POINT ( 'NONE',  ( 4.458734125000000326, -45.89583333196774362, 2.574251347313718519 ) ) ;
#11486 = CARTESIAN_POINT ( 'NONE',  ( -2.500000000000000444, 27.83333333333333215, -4.330127018922193649 ) ) ;
#11487 = EDGE_CURVE ( 'NONE', #16047, #8105, #21829, .T. ) ;
#11488 = CARTESIAN_POINT ( 'NONE',  ( 2.229367062500001939, -15.97916666530107399, 3.861377020970579999 ) ) ;
#11489 = EDGE_CURVE ( 'NONE', #2897, #19298, #63258, .T. ) ;
#11490 = CARTESIAN_POINT ( 'NONE',  ( 2.499999999999998668, -102.3333333333333286, -4.330127018922193649 ) ) ;
#11491 = CYLINDRICAL_SURFACE ( 'NONE', #37114, 5.000000000000000000 ) ;
#11492 = CARTESIAN_POINT ( 'NONE',  ( -3.152548672688508926E-16, -37.81249999863440792, -5.148502694627439702 ) ) ;
#11493 = CARTESIAN_POINT ( 'NONE',  ( -2.499999999999996447, 1.291666669397853351, 4.330127018922195425 ) ) ;
#11494 = CARTESIAN_POINT ( 'NONE',  ( -4.999999999999998224, -6.791666663935481019, 2.886751345948131764 ) ) ;
#11495 = CARTESIAN_POINT ( 'NONE',  ( -57.19623071787017210, -127.3750000013656205, 4.297418129356382899 ) ) ;
#11496 = CARTESIAN_POINT ( 'NONE',  ( -2.229367062500000163, -79.72916666530106511, -3.861377020970580443 ) ) ;
#11497 = EDGE_CURVE ( 'NONE', #45023, #23818, #8301, .T. ) ;
#11498 = CARTESIAN_POINT ( 'NONE',  ( 1.975475456537005874E-15, -71.75000000000000000, 5.000000000000000000 ) ) ;
#11499 = CARTESIAN_POINT ( 'NONE',  ( -6.972266317189433020E-16, 19.87500000273118417, -5.000000000000000000 ) ) ;
#11500 = CARTESIAN_POINT ( 'NONE',  ( 2.229367062500001939, -1.229166665301071548, 3.861377020970579999 ) ) ;
#11501 = EDGE_LOOP ( 'NONE', ( #13916, #15968, #13102, #17732 ) ) ;
#11502 = CARTESIAN_POINT ( 'NONE',  ( 5.000000000000000000, 16.70833333606451987, -2.886751345948130876 ) ) ;
#11503 = ADVANCED_FACE ( 'NONE', ( #63577 ), #28832, .T. ) ;
#11504 = CARTESIAN_POINT ( 'NONE',  ( 4.458734124999998549, -86.72916666530107932, -2.574251347313721627 ) ) ;
#11505 = DIRECTION ( 'NONE',  ( -0.000000000000000000, 1.000000000000000000, -0.000000000000000000 ) ) ;
#11506 = CARTESIAN_POINT ( 'NONE',  ( 4.458734124999998549, -86.97916666530106511, -2.574251347313721627 ) ) ;
#11507 = CARTESIAN_POINT ( 'NONE',  ( 2.229367062499998831, 20.10416666803225993, -3.861377020970580887 ) ) ;
#11508 = DIRECTION ( 'NONE',  ( -0.000000000000000000, 1.000000000000000000, -0.000000000000000000 ) ) ;
#11509 = CARTESIAN_POINT ( 'NONE',  ( -52.80376928212989185, -137.8750000013655779, -4.297418129356379346 ) ) ;
#11510 = CARTESIAN_POINT ( 'NONE',  ( -3.152548672688508926E-16, -5.562499998634400811, -5.148502694627439702 ) ) ;
#11511 = CARTESIAN_POINT ( 'NONE',  ( -2.229367062499996610, 16.60416666803225638, 3.861377020970582219 ) ) ;
#11512 = CARTESIAN_POINT ( 'NONE',  ( 9.457646018065525792E-16, -49.31249999863440792, 5.148502694627439702 ) ) ;
#11513 = CARTESIAN_POINT ( 'NONE',  ( -5.000000000000000000, 17.12500000273118417, 0.000000000000000000 ) ) ;
#11514 = CARTESIAN_POINT ( 'NONE',  ( -4.458734124999999437, -84.31249999863439371, 0.000000000000000000 ) ) ;
#11515 = CARTESIAN_POINT ( 'NONE',  ( 2.229367062500001939, -2.979166665301069550, 3.861377020970579999 ) ) ;
#11516 = SURFACE_STYLE_FILL_AREA ( #19963 ) ;
#11517 = ORIENTED_EDGE ( 'NONE', *, *, #28268, .T. ) ;
#11518 = CARTESIAN_POINT ( 'NONE',  ( 2.229367062500001939, -32.22916666530106511, 3.861377020970579999 ) ) ;
#11519 = CARTESIAN_POINT ( 'NONE',  ( -52.10840900171896806, -133.4375000013656063, 3.393966926194110556 ) ) ;
#11520 = CARTESIAN_POINT ( 'NONE',  ( 2.229367062499998831, -73.64583333196773651, -3.861377020970580887 ) ) ;
#11521 = CARTESIAN_POINT ( 'NONE',  ( 4.458734124999999437, 27.93750000136559208, -5.460374474430324690E-16 ) ) ;
#11522 = CARTESIAN_POINT ( 'NONE',  ( 4.458734125000001214, 20.10416666803225993, 2.574251347313718519 ) ) ;
#11523 = CARTESIAN_POINT ( 'NONE',  ( 1.975475456537005874E-15, -57.62499999726880873, 5.000000000000000000 ) ) ;
#11524 = CARTESIAN_POINT ( 'NONE',  ( 5.000000000000000888, -28.58333333333333570, 2.886751345948126879 ) ) ;
#11525 = CARTESIAN_POINT ( 'NONE',  ( -4.458734124999999437, -79.56249999863440792, 0.000000000000000000 ) ) ;
#11526 = CARTESIAN_POINT ( 'NONE',  ( -2.499999999999996447, -65.83333333333332860, 4.330127018922195425 ) ) ;
#11527 = CARTESIAN_POINT ( 'NONE',  ( -2.499999999999996447, -31.70833333060214798, 4.330127018922195425 ) ) ;
#11528 = CARTESIAN_POINT ( 'NONE',  ( -2.499999999999996447, 24.29166666939785202, 4.330127018922195425 ) ) ;
#11529 = ORIENTED_EDGE ( 'NONE', *, *, #40068, .T. ) ;
#11530 = CARTESIAN_POINT ( 'NONE',  ( -1.339745962155610925, -56.79465819873851729, 5.000000000000000000 ) ) ;
#11531 =( BOUNDED_CURVE ( )  B_SPLINE_CURVE ( 2, ( #122, #39325, #4603, #43832, #63478, #45118, #31270, #26459, #5892 ),
 .UNSPECIFIED., .F., .F. ) 
 B_SPLINE_CURVE_WITH_KNOTS ( ( 3, 2, 2, 2, 3 ),
 ( 0.7354166666666667185, 0.7361111111111111605, 0.7375000000000000444, 0.7388888888888889284, 0.7395833333333333703 ),
 .UNSPECIFIED. ) 
 CURVE ( )  GEOMETRIC_REPRESENTATION_ITEM ( )  RATIONAL_B_SPLINE_CURVE ( ( 0.9330127018922194093, 0.9330127018922194093, 1.000000000000000000, 0.8660254037844387076, 1.000000000000000000, 0.8660254037844387076, 1.000000000000000000, 0.9330127018922194093, 0.9330127018922194093 ) ) 
 REPRESENTATION_ITEM ( '' )  );
#11533 = CARTESIAN_POINT ( 'NONE',  ( -2.499999999999996447, -24.83333333333333215, 4.330127018922195425 ) ) ;
#11532 = CARTESIAN_POINT ( 'NONE',  ( 5.000000000000000000, -139.5625000013656063, 0.000000000000000000 ) ) ;
#11534 = CARTESIAN_POINT ( 'NONE',  ( -3.152548672688508926E-16, -26.56249999863440792, -5.148502694627439702 ) ) ;
#11535 = CARTESIAN_POINT ( 'NONE',  ( -4.458734124999999437, -88.39583333196773651, -2.574251347313719407 ) ) ;
#11536 = CARTESIAN_POINT ( 'NONE',  ( 2.499999999999998668, -21.20833333060214798, -4.330127018922193649 ) ) ;
#11538 = VERTEX_POINT ( 'NONE', #52968 ) ;
#11537 = CARTESIAN_POINT ( 'NONE',  ( -4.458734124999999437, -54.31249999863440081, 0.000000000000000000 ) ) ;
#11539 = DIRECTION ( 'NONE',  ( 0.000000000000000000, 0.000000000000000000, 1.000000000000000000 ) ) ;
#11540 = CARTESIAN_POINT ( 'NONE',  ( 0.000000000000000000, -170.0000000000000000, 5.000000000000000000 ) ) ;
#11542 = VERTEX_POINT ( 'NONE', #58739 ) ;
#11541 = CARTESIAN_POINT ( 'NONE',  ( 9.457646018065525792E-16, -5.312499998634402587, 5.148502694627439702 ) ) ;
#11543 = CARTESIAN_POINT ( 'NONE',  ( -4.999999999999999112, -69.91666666666667140, 2.886751345948131764 ) ) ;
#11544 = CARTESIAN_POINT ( 'NONE',  ( 4.458734124999999437, -152.7500000013656063, 1.846868145590737864 ) ) ;
#11545 = CARTESIAN_POINT ( 'NONE',  ( -2.229367062500000163, -44.72916666530106511, -3.861377020970580443 ) ) ;
#11546 = DIRECTION ( 'NONE',  ( 0.000000000000000000, 1.000000000000000000, 0.000000000000000000 ) ) ;
#11547 = CARTESIAN_POINT ( 'NONE',  ( -9.184850993605147944E-16, -157.2500000000000000, 5.000000000000000000 ) ) ;
#11548 = CARTESIAN_POINT ( 'NONE',  ( -2.500000000000000444, -71.04166666393547303, -4.330127018922193649 ) ) ;
#11549 = FACE_OUTER_BOUND ( 'NONE', #12029, .T. ) ;
#11550 = CARTESIAN_POINT ( 'NONE',  ( -51.19402409849444524, -154.5000000000000284, -3.242614290531456334 ) ) ;
#11551 = CARTESIAN_POINT ( 'NONE',  ( 2.229367062500001939, -16.22916666530107577, 3.861377020970579999 ) ) ;
#11552 = CARTESIAN_POINT ( 'NONE',  ( -3.152548672688508926E-16, -49.81249999863440081, -5.148502694627439702 ) ) ;
#11553 = DIRECTION ( 'NONE',  ( -0.000000000000000000, 1.000000000000000000, -0.000000000000000000 ) ) ;
#11554 = CARTESIAN_POINT ( 'NONE',  ( -8.190561711645485556E-16, -145.6875000013656063, 4.458734124999999437 ) ) ;
#11555 = CARTESIAN_POINT ( 'NONE',  ( -4.458734124999998549, -93.47916666530106511, 2.574251347313722516 ) ) ;
#11556 = CARTESIAN_POINT ( 'NONE',  ( -4.999999999999998224, -106.9166666666666572, 2.886751345948131764 ) ) ;
#11557 = VERTEX_POINT ( 'NONE', #14666 ) ;
#11558 = CARTESIAN_POINT ( 'NONE',  ( -55.35523342533222291, -152.5625000013656063, 4.444560631937231499 ) ) ;
#11559 = CARTESIAN_POINT ( 'NONE',  ( 4.458734125000001214, 24.85416666803225993, 2.574251347313718519 ) ) ;
#11560 = CARTESIAN_POINT ( 'NONE',  ( -57.46284108482265651, -148.0625000027312126, 4.819101127000239515 ) ) ;
#11561 = LINE ( 'NONE', #55647, #57918 ) ;
#11562 = ORIENTED_EDGE ( 'NONE', *, *, #35751, .F. ) ;
#11563 = CARTESIAN_POINT ( 'NONE',  ( -2.229367062499996610, -0.1458333319677394824, 3.861377020970582219 ) ) ;
#11564 = CARTESIAN_POINT ( 'NONE',  ( 5.000000000000000888, 6.416666666666667851, 2.886751345948126879 ) ) ;
#11565 = CARTESIAN_POINT ( 'NONE',  ( 4.458734125000001214, -21.14583333196774362, 2.574251347313718519 ) ) ;
#11566 = CARTESIAN_POINT ( 'NONE',  ( 1.339745962155612702, -72.29465819873850307, -5.000000000000000000 ) ) ;
#11567 = CARTESIAN_POINT ( 'NONE',  ( 4.458734125000001214, -8.895833331967736513, 2.574251347313718519 ) ) ;
#11568 = CARTESIAN_POINT ( 'NONE',  ( 1.975475456537005874E-15, 6.375000002731185944, 5.000000000000000000 ) ) ;
#11569 = CARTESIAN_POINT ( 'NONE',  ( -4.458734125000000326, -143.8750000013656063, 1.846868145590734089 ) ) ;
#11570 = CARTESIAN_POINT ( 'NONE',  ( -4.458734124999997661, 17.52083333469892779, 2.574251347313722516 ) ) ;
#11571 = VERTEX_POINT ( 'NONE', #38480 ) ;
#11572 = CARTESIAN_POINT ( 'NONE',  ( -1.339745962155613812, -14.08034179853029144, -5.000000000000000000 ) ) ;
#11573 = CARTESIAN_POINT ( 'NONE',  ( -1.339745962155610925, -12.79465819873851906, 5.000000000000000000 ) ) ;
#11575 = CARTESIAN_POINT ( 'NONE',  ( -4.458734124999999437, -18.39583333196774007, -2.574251347313719407 ) ) ;
#11574 = CARTESIAN_POINT ( 'NONE',  ( 5.000000000000000000, -86.41666666666667140, -2.886751345948129988 ) ) ;
#11576 = CARTESIAN_POINT ( 'NONE',  ( 1.339745962155612702, -85.16965819600733312, -5.000000000000000000 ) ) ;
#11577 = CARTESIAN_POINT ( 'NONE',  ( 5.000000000000000000, -88.37499999726880162, -6.123233995736766282E-16 ) ) ;
#11578 = CARTESIAN_POINT ( 'NONE',  ( -54.64476657466781973, -149.8125000013656063, -4.444560631937228834 ) ) ;
#11579 = ADVANCED_FACE ( 'NONE', ( #14356 ), #14036, .T. ) ;
#11580 = CARTESIAN_POINT ( 'NONE',  ( -3.535250795749689387E-16, -44.12499999726880873, -5.773502691896257311 ) ) ;
#11581 = CARTESIAN_POINT ( 'NONE',  ( 0.000000000000000000, -120.0000000000000000, 0.000000000000000000 ) ) ;
#11582 = CARTESIAN_POINT ( 'NONE',  ( 2.229367062499998831, 7.354166668032259935, -3.861377020970580887 ) ) ;
#11583 = DIRECTION ( 'NONE',  ( 0.000000000000000000, 1.000000000000000000, 0.000000000000000000 ) ) ;
#11584 = FACE_OUTER_BOUND ( 'NONE', #24117, .T. ) ;
#11585 = CARTESIAN_POINT ( 'NONE',  ( -4.458734124999999437, 12.68750000136559564, 0.000000000000000000 ) ) ;
#11586 = CARTESIAN_POINT ( 'NONE',  ( 4.458734125000001214, -68.89583333196773651, 2.574251347313718519 ) ) ;
#11587 = CARTESIAN_POINT ( 'NONE',  ( 4.458734124999999437, -12.06249999863440081, -5.460374474430324690E-16 ) ) ;
#11588 = CARTESIAN_POINT ( 'NONE',  ( -3.535250795749689387E-16, -1.250000000000001110, -5.773502691896257311 ) ) ;
#11589 = CARTESIAN_POINT ( 'NONE',  ( 2.730187237215162345E-16, -162.1875000013655779, -4.458734124999999437 ) ) ;
#11590 = DIRECTION ( 'NONE',  ( -1.000000000000000000, 0.000000000000000000, 0.000000000000000000 ) ) ;
#11591 = CARTESIAN_POINT ( 'NONE',  ( -4.458734124999999437, -56.39583333196773651, -2.574251347313719407 ) ) ;
#11592 = CARTESIAN_POINT ( 'NONE',  ( -2.499999999999996447, -96.70833333060213022, 4.330127018922195425 ) ) ;
#11593 = CARTESIAN_POINT ( 'NONE',  ( -58.24261429053147765, -152.3750000027312126, -3.805975901505573855 ) ) ;
#11594 = CARTESIAN_POINT ( 'NONE',  ( 4.458734125000000326, -34.89583333196772941, 2.574251347313718519 ) ) ;
#11595 = CARTESIAN_POINT ( 'NONE',  ( -5.000000000000000000, -90.95833333060213022, -2.886751345948128211 ) ) ;
#11596 = CARTESIAN_POINT ( 'NONE',  ( 1.060575238724906964E-15, -48.75000000000000000, 5.773502691896257311 ) ) ;
#11597 = CARTESIAN_POINT ( 'NONE',  ( 5.000000000000000000, -13.41666666666666785, -2.886751345948130876 ) ) ;
#11598 = CARTESIAN_POINT ( 'NONE',  ( 1.339745962155615144, -17.58034179853029499, 4.999999999999999112 ) ) ;
#11599 = VERTEX_POINT ( 'NONE', #24325 ) ;
#11600 = CARTESIAN_POINT ( 'NONE',  ( -2.229367062499996610, -108.1458333319677365, 3.861377020970582219 ) ) ;
#11601 = CARTESIAN_POINT ( 'NONE',  ( 4.458734124999999437, -0.06249999863440491854, -5.460374474430324690E-16 ) ) ;
#11602 = CARTESIAN_POINT ( 'NONE',  ( -1.339745962155613812, -97.08034179853028434, -5.000000000000000000 ) ) ;
#11603 = CARTESIAN_POINT ( 'NONE',  ( 5.000000000000000000, -7.416666666666667851, -2.886751345948129988 ) ) ;
#11604 = CARTESIAN_POINT ( 'NONE',  ( -4.458734124999999437, -71.39583333196773651, -2.574251347313719407 ) ) ;
#11605 =( BOUNDED_CURVE ( )  B_SPLINE_CURVE ( 2, ( #16719, #27632, #45984, #31827, #36020, #32134, #46946, #40832, #7076 ),
 .UNSPECIFIED., .F., .F. ) 
 B_SPLINE_CURVE_WITH_KNOTS ( ( 3, 2, 2, 2, 3 ),
 ( 0.7160714285714285809, 0.7166666666666666741, 0.7178571428571428603, 0.7190476190476190466, 0.7196428571428571397 ),
 .UNSPECIFIED. ) 
 CURVE ( )  GEOMETRIC_REPRESENTATION_ITEM ( )  RATIONAL_B_SPLINE_CURVE ( ( 0.9330127018922194093, 0.9330127018922194093, 1.000000000000000000, 0.8660254037844387076, 1.000000000000000000, 0.8660254037844387076, 1.000000000000000000, 0.9330127018922194093, 0.9330127018922194093 ) ) 
 REPRESENTATION_ITEM ( '' )  );
#11606 = DIRECTION ( 'NONE',  ( 0.000000000000000000, -0.000000000000000000, 1.000000000000000000 ) ) ;
#11607 = CARTESIAN_POINT ( 'NONE',  ( 5.000000000000000000, -8.374999997268814056, -6.123233995736766282E-16 ) ) ;
#11609 = ORIENTED_EDGE ( 'NONE', *, *, #17395, .F. ) ;
#11608 = CARTESIAN_POINT ( 'NONE',  ( -4.458734124999998549, -39.22916666530107221, 2.574251347313722516 ) ) ;
#11610 = FACE_OUTER_BOUND ( 'NONE', #49438, .T. ) ;
#11612 = ORIENTED_EDGE ( 'NONE', *, *, #50396, .F. ) ;
#11611 = CARTESIAN_POINT ( 'NONE',  ( 2.229367062499998831, 11.10416666803225993, -3.861377020970580887 ) ) ;
#11613 = CARTESIAN_POINT ( 'NONE',  ( -1.339745962155606929, 24.79465819873852439, -5.000000000000004441 ) ) ;
#11614 = CARTESIAN_POINT ( 'NONE',  ( 2.499999999999998668, -57.33333333333333570, -4.330127018922193649 ) ) ;
#11615 = CARTESIAN_POINT ( 'NONE',  ( 2.229367062499998831, -27.89583333196774007, -3.861377020970580887 ) ) ;
#11616 = CARTESIAN_POINT ( 'NONE',  ( 5.000000000000000000, -145.0624999999999716, 2.071067811865478614 ) ) ;
#11617 = CARTESIAN_POINT ( 'NONE',  ( -4.458734124999998549, -76.22916666530107932, 2.574251347313722516 ) ) ;
#11618 = CARTESIAN_POINT ( 'NONE',  ( 5.000000000000000000, -169.0000000000000000, 0.000000000000000000 ) ) ;
#11619 = CARTESIAN_POINT ( 'NONE',  ( -3.152548672688508926E-16, -86.56249999863440792, -5.148502694627439702 ) ) ;
#11620 = CARTESIAN_POINT ( 'NONE',  ( -52.10840900171896806, -136.4375000013656063, 3.393966926194110556 ) ) ;
#11621 = CARTESIAN_POINT ( 'NONE',  ( 4.458734124999998549, -33.97916666530107221, -2.574251347313721627 ) ) ;
#11622 = CARTESIAN_POINT ( 'NONE',  ( -5.000000000000000000, -93.87499999726881583, 0.000000000000000000 ) ) ;
#11623 = ORIENTED_EDGE ( 'NONE', *, *, #36274, .F. ) ;
#11624 = CARTESIAN_POINT ( 'NONE',  ( 2.229367062499998831, -75.89583333196773651, -3.861377020970580887 ) ) ;
#11625 = CARTESIAN_POINT ( 'NONE',  ( -54.93493926172311603, -135.0000000000000000, -4.467806258561277666 ) ) ;
#11626 = ORIENTED_EDGE ( 'NONE', *, *, #5172, .T. ) ;
#11627 = PLANE ( 'NONE',  #48078 ) ;
#11628 = CARTESIAN_POINT ( 'NONE',  ( 0.000000000000000000, -120.0000000000000000, 5.000000000000000000 ) ) ;
#11629 = CARTESIAN_POINT ( 'NONE',  ( 4.458734124999998549, -65.97916666530106511, -2.574251347313721627 ) ) ;
#11630 = CARTESIAN_POINT ( 'NONE',  ( 4.458734124999999437, -11.06249999863440792, -5.460374474430324690E-16 ) ) ;
#11631 = ORIENTED_EDGE ( 'NONE', *, *, #20143, .T. ) ;
#11632 = CARTESIAN_POINT ( 'NONE',  ( -5.000000000000000888, -156.6875000027312126, -2.071067811865475949 ) ) ;
#11633 = CARTESIAN_POINT ( 'NONE',  ( -1.339745962155610925, -92.66965819600731891, 5.000000000000000000 ) ) ;
#11634 = EDGE_LOOP ( 'NONE', ( #41044, #6126, #29481, #54802 ) ) ;
#11635 = CARTESIAN_POINT ( 'NONE',  ( 4.458734125000001214, -7.145833331967734736, 2.574251347313718519 ) ) ;
#11636 = CARTESIAN_POINT ( 'NONE',  ( 2.229367062499998831, 8.354166668032261711, -3.861377020970580887 ) ) ;
#11637 = CARTESIAN_POINT ( 'NONE',  ( -1.339745962155610925, -11.66965819600733667, 5.000000000000000000 ) ) ;
#11638 = CARTESIAN_POINT ( 'NONE',  ( 1.846868145590735200, -161.2500000013655779, -4.458734124999999437 ) ) ;
#11639 = CARTESIAN_POINT ( 'NONE',  ( -4.458734124999999437, 29.43750000136559208, 0.000000000000000000 ) ) ;
#11640 = ORIENTED_EDGE ( 'NONE', *, *, #11474, .F. ) ;
#11641 = CARTESIAN_POINT ( 'NONE',  ( 4.458734124999999437, -85.81249999863439371, -5.460374474430324690E-16 ) ) ;
#11642 = CARTESIAN_POINT ( 'NONE',  ( 2.499999999999998668, -29.20833333060214798, -4.330127018922193649 ) ) ;
#11643 = CARTESIAN_POINT ( 'NONE',  ( -2.229367062500000163, -1.479166665301071770, -3.861377020970580443 ) ) ;
#11644 = CARTESIAN_POINT ( 'NONE',  ( 5.000000000000000000, 25.62500000273118417, -6.123233995736766282E-16 ) ) ;
#11645 = CARTESIAN_POINT ( 'NONE',  ( 5.000000000000000000, -31.29166666393548368, -2.886751345948129988 ) ) ;
#11646 = CARTESIAN_POINT ( 'NONE',  ( 5.000000000000000000, -78.41666666666667140, -2.886751345948130876 ) ) ;
#11647 = CARTESIAN_POINT ( 'NONE',  ( 9.457646018065525792E-16, 25.93750000136559564, 5.148502694627439702 ) ) ;
#11648 = CARTESIAN_POINT ( 'NONE',  ( -6.972266317189433020E-16, -79.24999999999998579, -5.000000000000000000 ) ) ;
#11649 =( BOUNDED_CURVE ( )  B_SPLINE_CURVE ( 2, ( #50122, #24409, #295, #63658, #19576, #24726, #1266, #20224, #58815 ),
 .UNSPECIFIED., .F., .F. ) 
 B_SPLINE_CURVE_WITH_KNOTS ( ( 3, 2, 2, 2, 3 ),
 ( 0.1410714285714285698, 0.1416666666666666630, 0.1428571428571428492, 0.1440476190476190355, 0.1446428571428571563 ),
 .UNSPECIFIED. ) 
 CURVE ( )  GEOMETRIC_REPRESENTATION_ITEM ( )  RATIONAL_B_SPLINE_CURVE ( ( 0.9330127018922194093, 0.9330127018922194093, 1.000000000000000000, 0.8660254037844387076, 1.000000000000000000, 0.8660254037844387076, 1.000000000000000000, 0.9330127018922178550, 0.9330127018922194093 ) ) 
 REPRESENTATION_ITEM ( '' )  );
#11650 = CARTESIAN_POINT ( 'NONE',  ( -4.458734124999997661, 25.77083333469893134, 2.574251347313722516 ) ) ;
#11651 = CARTESIAN_POINT ( 'NONE',  ( 4.458734124999999437, -48.81249999863440792, -5.460374474430324690E-16 ) ) ;
#11652 = CARTESIAN_POINT ( 'NONE',  ( 4.458734125000000326, -37.14583333196773651, 2.574251347313718519 ) ) ;
#11653 = CARTESIAN_POINT ( 'NONE',  ( 4.458734125000000326, 1.854166668032262599, 2.574251347313718519 ) ) ;
#11654 = CARTESIAN_POINT ( 'NONE',  ( -5.000000000000000888, -149.6875000027312126, -2.071067811865475949 ) ) ;
#11655 = CARTESIAN_POINT ( 'NONE',  ( 5.000000000000000888, 13.41666666666666607, 2.886751345948126879 ) ) ;
#11656 = CARTESIAN_POINT ( 'NONE',  ( -2.071067811865478170, -144.4375000027312126, 5.000000000000000000 ) ) ;
#11657 = CARTESIAN_POINT ( 'NONE',  ( -1.230605004983934782E-13, -26.62499999726881583, 5.000000000000000000 ) ) ;
#11658 = CARTESIAN_POINT ( 'NONE',  ( -2.229367062500000163, -44.47916666530106511, -3.861377020970580443 ) ) ;
#11659 = CARTESIAN_POINT ( 'NONE',  ( -5.000000000000000000, -77.87499999726881583, 0.000000000000000000 ) ) ;
#11660 = CARTESIAN_POINT ( 'NONE',  ( -56.48576386720575471, -141.0000000013656063, -4.591703134518078322 ) ) ;
#11661 = VECTOR ( 'NONE', #52854, 1000.000000000000000 ) ;
#11662 = CARTESIAN_POINT ( 'NONE',  ( 5.000000000000000000, -24.29166666393548368, -2.886751345948130876 ) ) ;
#11663 = LINE ( 'NONE', #56705, #19268 ) ;
#11664 = CARTESIAN_POINT ( 'NONE',  ( 2.229367062500001939, -86.22916666530107932, 3.861377020970579999 ) ) ;
#11665 = CARTESIAN_POINT ( 'NONE',  ( 3.152801135295367541, -160.5625000013656063, -3.152801135295367541 ) ) ;
#11666 = CARTESIAN_POINT ( 'NONE',  ( -1.282512619719133662, -8.391164935524759727, -7.795653906409117262 ) ) ;
#11667 = CARTESIAN_POINT ( 'NONE',  ( 1.060575238724906964E-15, -29.74999999999999645, 5.773502691896257311 ) ) ;
#11668 = CARTESIAN_POINT ( 'NONE',  ( -1.846868145590734756, -140.1250000013655779, -4.458734125000000326 ) ) ;
#11669 = ORIENTED_EDGE ( 'NONE', *, *, #46497, .F. ) ;
#11670 = CARTESIAN_POINT ( 'NONE',  ( 4.458734124999998549, 23.02083333469892423, -2.574251347313721627 ) ) ;
#11671 = VERTEX_POINT ( 'NONE', #34286 ) ;
#11672 = CARTESIAN_POINT ( 'NONE',  ( -2.229367062500000163, -91.47916666530106511, -3.861377020970580443 ) ) ;
#11673 = CARTESIAN_POINT ( 'NONE',  ( -2.229367062499996610, 12.60416666803226171, 3.861377020970582219 ) ) ;
#11674 = CARTESIAN_POINT ( 'NONE',  ( 1.060575238724906964E-15, 15.37500000273118417, 5.773502691896257311 ) ) ;
#11675 = LINE ( 'NONE', #39989, #46329 ) ;
#11676 = CARTESIAN_POINT ( 'NONE',  ( -5.000000000000000000, 9.999999999999998224, 0.000000000000000000 ) ) ;
#11677 = EDGE_CURVE ( 'NONE', #16288, #17633, #58428, .T. ) ;
#11678 = CARTESIAN_POINT ( 'NONE',  ( -4.458734124999999437, -56.39583333196773651, -2.574251347313719407 ) ) ;
#11679 = CARTESIAN_POINT ( 'NONE',  ( -4.458734124999998549, -11.22916666530106866, 2.574251347313722516 ) ) ;
#11680 = CARTESIAN_POINT ( 'NONE',  ( 1.975475456537005874E-15, 0.2500000000000001665, 5.000000000000000000 ) ) ;
#11681 = CARTESIAN_POINT ( 'NONE',  ( -2.499999999999996447, -51.83333333333332860, 4.330127018922195425 ) ) ;
#11682 = CARTESIAN_POINT ( 'NONE',  ( -5.000000000000000000, -109.9999999999999858, 0.000000000000000000 ) ) ;
#11683 = CARTESIAN_POINT ( 'NONE',  ( 1.975475456537005874E-15, 2.249999999999999556, 5.000000000000000000 ) ) ;
#11684 = CARTESIAN_POINT ( 'NONE',  ( -5.000000000000000000, -62.00000000000000000, 0.000000000000000000 ) ) ;
#11685 = CARTESIAN_POINT ( 'NONE',  ( 2.499999999999998668, -33.33333333333332860, -4.330127018922193649 ) ) ;
#11686 = CARTESIAN_POINT ( 'NONE',  ( 6.123233995736766282E-16, -120.0000000000000000, -5.000000000000000000 ) ) ;
#11688 = CARTESIAN_POINT ( 'NONE',  ( -4.458734124999999437, -16.56249999863440436, 0.000000000000000000 ) ) ;
#11687 = DIRECTION ( 'NONE',  ( -0.000000000000000000, 1.000000000000000000, -0.000000000000000000 ) ) ;
#11689 = CARTESIAN_POINT ( 'NONE',  ( -58.24261429053147765, -135.3750000027312410, -3.805975901505573855 ) ) ;
#11690 = CARTESIAN_POINT ( 'NONE',  ( -4.458734124999998549, -60.22916666530106511, 2.574251347313722516 ) ) ;
#11691 = CARTESIAN_POINT ( 'NONE',  ( -8.190561711645485556E-16, -150.9375000013656063, 4.458734124999999437 ) ) ;
#11692 = CARTESIAN_POINT ( 'NONE',  ( 9.457646018065525792E-16, -70.06249999863439371, 5.148502694627439702 ) ) ;
#11693 = CARTESIAN_POINT ( 'NONE',  ( -58.39396692619412477, -145.6875000013656063, 2.891590998281057701 ) ) ;
#11694 = CARTESIAN_POINT ( 'NONE',  ( -3.152548672688508926E-16, -21.81249999863440436, -5.148502694627439702 ) ) ;
#11695 = CARTESIAN_POINT ( 'NONE',  ( -2.499999999999996447, -58.70833333060214443, 4.330127018922195425 ) ) ;
#11696 = ORIENTED_EDGE ( 'NONE', *, *, #40815, .T. ) ;
#11697 = CARTESIAN_POINT ( 'NONE',  ( 5.000000000000000000, -31.29166666393548724, -2.886751345948130876 ) ) ;
#11698 = ORIENTED_EDGE ( 'NONE', *, *, #35825, .F. ) ;
#11699 = CARTESIAN_POINT ( 'NONE',  ( -4.458734124999999437, -63.64583333196773651, -2.574251347313719407 ) ) ;
#11701 = CARTESIAN_POINT ( 'NONE',  ( 5.000000000000000000, -58.50000000000000000, -6.123233995736766282E-16 ) ) ;
#11700 = CARTESIAN_POINT ( 'NONE',  ( -5.000000000000000000, -157.6250000027311842, -6.123233995736766282E-16 ) ) ;
#11702 = CARTESIAN_POINT ( 'NONE',  ( -3.152801135295367096, -154.0625000013656063, -3.152801135295367541 ) ) ;
#11703 = EDGE_LOOP ( 'NONE', ( #45885, #21974, #54800, #32668 ) ) ;
#11704 =( BOUNDED_CURVE ( )  B_SPLINE_CURVE ( 2, ( #57387, #39001, #62212, #48028, #37755, #43195, #38679, #53175, #38376 ),
 .UNSPECIFIED., .F., .F. ) 
 B_SPLINE_CURVE_WITH_KNOTS ( ( 3, 2, 2, 2, 3 ),
 ( 0.2645833333333333370, 0.2652777777777777790, 0.2666666666666666630, 0.2680555555555555469, 0.2687499999999999889 ),
 .UNSPECIFIED. ) 
 CURVE ( )  GEOMETRIC_REPRESENTATION_ITEM ( )  RATIONAL_B_SPLINE_CURVE ( ( 0.9330127018922194093, 0.9330127018922194093, 1.000000000000000000, 0.8660254037844387076, 1.000000000000000000, 0.8660254037844387076, 1.000000000000000000, 0.9330127018922194093, 0.9330127018922194093 ) ) 
 REPRESENTATION_ITEM ( '' )  );
#11705 = CARTESIAN_POINT ( 'NONE',  ( -5.000000000000000000, -7.874999997268813168, 0.000000000000000000 ) ) ;
#11706 = CARTESIAN_POINT ( 'NONE',  ( -58.24261429053147765, -127.2500000000000284, -3.805975901505573855 ) ) ;
#11707 = CARTESIAN_POINT ( 'NONE',  ( -2.499999999999996447, -74.70833333060214443, 4.330127018922195425 ) ) ;
#11708 = CARTESIAN_POINT ( 'NONE',  ( 2.229367062499998831, -45.89583333196774362, -3.861377020970580887 ) ) ;
#11709 = ORIENTED_EDGE ( 'NONE', *, *, #12848, .F. ) ;
#11710 = VECTOR ( 'NONE', #43361, 1000.000000000000000 ) ;
#11711 = CARTESIAN_POINT ( 'NONE',  ( 5.000000000000000000, 10.70833333606451987, -2.886751345948130876 ) ) ;
#11712 = CARTESIAN_POINT ( 'NONE',  ( -2.229367062499996610, 7.854166668032260823, 3.861377020970582219 ) ) ;
#11713 = CARTESIAN_POINT ( 'NONE',  ( 4.458734124999999437, 23.18750000136559564, -5.460374474430324690E-16 ) ) ;
#11714 = CARTESIAN_POINT ( 'NONE',  ( -59.44456063193725015, -149.5625000013656063, -0.3552334253322034230 ) ) ;
#11715 = CARTESIAN_POINT ( 'NONE',  ( 1.339745962155499015, -108.5803417985302843, 5.000000000000065725 ) ) ;
#11716 = CARTESIAN_POINT ( 'NONE',  ( 2.500000000000002220, -61.54166666393547303, 4.330127018922192761 ) ) ;
#11717 = EDGE_LOOP ( 'NONE', ( #45483, #49505, #55539, #22066 ) ) ;
#11718 = CARTESIAN_POINT ( 'NONE',  ( -4.458734124999999437, -70.31249999863439371, 0.000000000000000000 ) ) ;
#11719 = DIRECTION ( 'NONE',  ( -0.000000000000000000, 1.000000000000000000, -0.000000000000000000 ) ) ;
#11720 = CARTESIAN_POINT ( 'NONE',  ( -3.152548672688508926E-16, 10.43750000136559386, -5.148502694627439702 ) ) ;
#11721 = CARTESIAN_POINT ( 'NONE',  ( 2.499999999999998668, 7.791666669397852019, -4.330127018922193649 ) ) ;
#11722 = CARTESIAN_POINT ( 'NONE',  ( -51.75738570946856498, -152.8750000027312126, 3.805975901505576964 ) ) ;
#11723 = CARTESIAN_POINT ( 'NONE',  ( -3.152548672688508926E-16, -54.81249999863440081, -5.148502694627439702 ) ) ;
#11724 = CARTESIAN_POINT ( 'NONE',  ( 5.000000000000000000, -12.29166666393547835, -2.886751345948129988 ) ) ;
#11725 = CARTESIAN_POINT ( 'NONE',  ( 7.500000000000000888, -0.7512838658081439913, 1.423015351387224570E-15 ) ) ;
#11726 = CYLINDRICAL_SURFACE ( 'NONE', #32646, 5.000000000000000000 ) ;
#11727 = CARTESIAN_POINT ( 'NONE',  ( -4.458734124999999437, -21.56249999863440436, 0.000000000000000000 ) ) ;
#11728 = ORIENTED_EDGE ( 'NONE', *, *, #2774, .F. ) ;
#11729 = CARTESIAN_POINT ( 'NONE',  ( -1.049326080737009628E-13, -18.62499999726881583, 5.000000000000000000 ) ) ;
#11730 = CARTESIAN_POINT ( 'NONE',  ( -4.458734124999998549, -106.2291666653010793, 2.574251347313722516 ) ) ;
#11731 = CARTESIAN_POINT ( 'NONE',  ( 5.000000000000000000, -157.1250000027311842, 0.000000000000000000 ) ) ;
#11732 = EDGE_LOOP ( 'NONE', ( #24675, #13816, #20138, #18472 ) ) ;
#11733 = CARTESIAN_POINT ( 'NONE',  ( 2.229367062500001939, -104.2291666653010651, 3.861377020970579999 ) ) ;
#11734 = CARTESIAN_POINT ( 'NONE',  ( 4.458734124999999437, -27.81249999863440081, -5.460374474430324690E-16 ) ) ;
#11735 = CARTESIAN_POINT ( 'NONE',  ( -3.535250795749689387E-16, -61.12499999726880873, -5.773502691896257311 ) ) ;
#11736 = CARTESIAN_POINT ( 'NONE',  ( -54.64476657466781973, -150.0625000013656063, -4.444560631937228834 ) ) ;
#11737 = CARTESIAN_POINT ( 'NONE',  ( -59.29741812935640155, -143.6250000013655779, -2.196230717870135685 ) ) ;
#11738 = CARTESIAN_POINT ( 'NONE',  ( -4.458734124999999437, -25.39583333196773651, -2.574251347313719407 ) ) ;
#11739 = CARTESIAN_POINT ( 'NONE',  ( -4.458734124999999437, -62.56249999863440792, 0.000000000000000000 ) ) ;
#11740 = CARTESIAN_POINT ( 'NONE',  ( -54.60164318462004474, -153.5000000027312410, -4.984105922594373794 ) ) ;
#11741 = CARTESIAN_POINT ( 'NONE',  ( -2.229367062500000163, -25.47916666530106866, -3.861377020970580443 ) ) ;
#11742 = CARTESIAN_POINT ( 'NONE',  ( 5.000000000000000000, -32.41666666666666430, -2.886751345948130876 ) ) ;
#11743 = CARTESIAN_POINT ( 'NONE',  ( -2.071067811865475061, -151.6875000000000000, -5.000000000000000888 ) ) ;
#11744 = CARTESIAN_POINT ( 'NONE',  ( 5.000000000000000000, -12.49999999999999645, -6.123233995736766282E-16 ) ) ;
#11745 = CARTESIAN_POINT ( 'NONE',  ( -4.458734125000001214, -149.8750000013655779, 1.846868145590734089 ) ) ;
#11746 = ORIENTED_EDGE ( 'NONE', *, *, #56301, .F. ) ;
#11747 = CARTESIAN_POINT ( 'NONE',  ( 2.229367062500001939, -50.22916666530107221, 3.861377020970579999 ) ) ;
#11748 = CARTESIAN_POINT ( 'NONE',  ( 2.499999999999998668, -2.333333333333333037, -4.330127018922193649 ) ) ;
#11749 = CARTESIAN_POINT ( 'NONE',  ( -58.80597590150559739, -136.0000000000000284, 3.242614290531460330 ) ) ;
#11750 = CARTESIAN_POINT ( 'NONE',  ( 5.000000000000000888, 28.41666666666666430, 2.886751345948126879 ) ) ;
#11751 = EDGE_CURVE ( 'NONE', #35203, #53762, #15955, .T. ) ;
#11752 = FACE_OUTER_BOUND ( 'NONE', #24204, .T. ) ;
#11753 = AXIS2_PLACEMENT_3D ( 'NONE', #59966, #26492, #21035 ) ;
#11754 = CARTESIAN_POINT ( 'NONE',  ( -4.458734124999999437, 4.604166668032261711, -2.574251347313719407 ) ) ;
#11755 = CARTESIAN_POINT ( 'NONE',  ( -5.000000000000000000, -73.95833333060214443, -2.886751345948128211 ) ) ;
#11756 = CARTESIAN_POINT ( 'NONE',  ( 5.000000000000000000, -95.29166666393547303, -2.886751345948130876 ) ) ;
#11757 = CARTESIAN_POINT ( 'NONE',  ( 0.000000000000000000, -170.0000000000000000, 0.000000000000000000 ) ) ;
#11758 = CARTESIAN_POINT ( 'NONE',  ( 9.457646018065525792E-16, 15.68750000136559386, 5.148502694627439702 ) ) ;
#11759 = CARTESIAN_POINT ( 'NONE',  ( -2.500000000000000444, 0.9583333360645186483, -4.330127018922193649 ) ) ;
#11760 = VERTEX_POINT ( 'NONE', #44252 ) ;
#11761 = CYLINDRICAL_SURFACE ( 'NONE', #55154, 5.000000000000000000 ) ;
#11762 = ORIENTED_EDGE ( 'NONE', *, *, #2521, .F. ) ;
#11763 = CARTESIAN_POINT ( 'NONE',  ( -6.972266317189433020E-16, -51.25000000000000000, -5.000000000000000000 ) ) ;
#11764 = CARTESIAN_POINT ( 'NONE',  ( 2.229367062499998831, -45.64583333196774362, -3.861377020970580887 ) ) ;
#11765 = CARTESIAN_POINT ( 'NONE',  ( -1.846868145590737420, -166.0000000013656063, 4.458734124999999437 ) ) ;
#11766 = EDGE_CURVE ( 'NONE', #24077, #26556, #14843, .T. ) ;
#11767 = CARTESIAN_POINT ( 'NONE',  ( -3.535250795749689387E-16, -43.12499999726880162, -5.773502691896257311 ) ) ;
#11768 = EDGE_LOOP ( 'NONE', ( #13261, #22399, #49158, #46990 ) ) ;
#11770 = EDGE_CURVE ( 'NONE', #33683, #14691, #46051, .T. ) ;
#11769 = CARTESIAN_POINT ( 'NONE',  ( 4.458734125000001214, -18.89583333196773651, 2.574251347313718519 ) ) ;
#11771 = ORIENTED_EDGE ( 'NONE', *, *, #57099, .F. ) ;
#11772 = CARTESIAN_POINT ( 'NONE',  ( -2.500000000000000444, -88.16666666666665719, -4.330127018922193649 ) ) ;
#11773 = CARTESIAN_POINT ( 'NONE',  ( -3.152801135295367985, -163.8125000013656063, 3.152801135295367096 ) ) ;
#11775 = ORIENTED_EDGE ( 'NONE', *, *, #1126, .F. ) ;
#11774 = CARTESIAN_POINT ( 'NONE',  ( 1.339745962155615144, -55.70534180126148271, 4.999999999999999112 ) ) ;
#11776 = CARTESIAN_POINT ( 'NONE',  ( -55.39835681537999790, -140.8750000000000284, 4.984105922594378235 ) ) ;
#11777 = CARTESIAN_POINT ( 'NONE',  ( -2.229367062499996610, -32.39583333196773651, 3.861377020970582219 ) ) ;
#11778 = CARTESIAN_POINT ( 'NONE',  ( 1.975475456537005874E-15, 21.24999999999999289, 5.000000000000000000 ) ) ;
#11779 = ORIENTED_EDGE ( 'NONE', *, *, #57738, .T. ) ;
#11780 =( BOUNDED_CURVE ( )  B_SPLINE_CURVE ( 2, ( #39139, #53629, #44600, #20493, #34967, #14696, #9867, #560, #54582 ),
 .UNSPECIFIED., .F., .F. ) 
 B_SPLINE_CURVE_WITH_KNOTS ( ( 3, 2, 2, 2, 3 ),
 ( 0.3979166666666666963, 0.3986111111111111382, 0.4000000000000000222, 0.4013888888888889062, 0.4020833333333333481 ),
 .UNSPECIFIED. ) 
 CURVE ( )  GEOMETRIC_REPRESENTATION_ITEM ( )  RATIONAL_B_SPLINE_CURVE ( ( 0.9330127018922194093, 0.9330127018922220739, 1.000000000000000000, 0.8660254037844387076, 1.000000000000000000, 0.8660254037844387076, 1.000000000000000000, 0.9330127018922194093, 0.9330127018922194093 ) ) 
 REPRESENTATION_ITEM ( '' )  );
#11781 = CARTESIAN_POINT ( 'NONE',  ( -3.152548672688508926E-16, -75.56249999863439371, -5.148502694627439702 ) ) ;
#11782 = CARTESIAN_POINT ( 'NONE',  ( 2.229367062499998831, 28.35416666803225993, -3.861377020970580887 ) ) ;
#11783 = CARTESIAN_POINT ( 'NONE',  ( 6.123233995736766282E-16, -120.0000000000000000, -5.000000000000000000 ) ) ;
#11784 = ORIENTED_EDGE ( 'NONE', *, *, #21385, .F. ) ;
#11785 = LINE ( 'NONE', #40739, #52077 ) ;
#11786 = CARTESIAN_POINT ( 'NONE',  ( -50.40829686548195099, -143.2500000013656063, -1.485763867205728284 ) ) ;
#11787 = CARTESIAN_POINT ( 'NONE',  ( 2.229367062499998831, -81.89583333196773651, -3.861377020970580887 ) ) ;
#11788 = CARTESIAN_POINT ( 'NONE',  ( -51.19402409849444524, -133.6250000027312126, -3.242614290531456334 ) ) ;
#11789 = CARTESIAN_POINT ( 'NONE',  ( 2.499999999999998668, 22.66666666666666430, -4.330127018922193649 ) ) ;
#11790 = CARTESIAN_POINT ( 'NONE',  ( -4.458734124999999437, -143.2500000013655779, -1.846868145590735644 ) ) ;
#11791 = CARTESIAN_POINT ( 'NONE',  ( 5.000000000000000888, -84.45833333060214443, 2.886751345948126879 ) ) ;
#11792 = CARTESIAN_POINT ( 'NONE',  ( 4.458734124999998549, -47.72916666530106511, -2.574251347313721627 ) ) ;
#11793 = CARTESIAN_POINT ( 'NONE',  ( -4.458734124999999437, -45.39583333196773651, -2.574251347313719407 ) ) ;
#11794 = CARTESIAN_POINT ( 'NONE',  ( 9.457646018065525792E-16, 27.93750000136559208, 5.148502694627439702 ) ) ;
#11795 = EDGE_CURVE ( 'NONE', #6430, #42800, #29136, .T. ) ;
#11796 = CARTESIAN_POINT ( 'NONE',  ( -2.500000000000000444, -105.1666666666666572, -4.330127018922193649 ) ) ;
#11797 = VECTOR ( 'NONE', #10577, 1000.000000000000000 ) ;
#11798 =( BOUNDED_CURVE ( )  B_SPLINE_CURVE ( 2, ( #57406, #62854, #58018, #23300, #47421, #13946, #43214, #9126, #43523 ),
 .UNSPECIFIED., .F., .F. ) 
 B_SPLINE_CURVE_WITH_KNOTS ( ( 3, 2, 2, 2, 3 ),
 ( 0.1520833333333333481, 0.1527777777777777901, 0.1541666666666666741, 0.1555555555555555580, 0.1562500000000000000 ),
 .UNSPECIFIED. ) 
 CURVE ( )  GEOMETRIC_REPRESENTATION_ITEM ( )  RATIONAL_B_SPLINE_CURVE ( ( 0.9330127018922194093, 0.9330127018922207416, 1.000000000000000000, 0.8660254037844387076, 1.000000000000000000, 0.8660254037844387076, 1.000000000000000000, 0.9330127018922194093, 0.9330127018922194093 ) ) 
 REPRESENTATION_ITEM ( '' )  );
#11799 = CARTESIAN_POINT ( 'NONE',  ( 5.000000000000000000, -159.1875000027312126, 2.071067811865478614 ) ) ;
#11800 = CARTESIAN_POINT ( 'NONE',  ( -2.229367062499996610, -37.39583333196773651, 3.861377020970582219 ) ) ;
#11801 = CARTESIAN_POINT ( 'NONE',  ( 2.499999999999998668, -0.2083333306021478704, -4.330127018922193649 ) ) ;
#11802 = LINE ( 'NONE', #3438, #5787 ) ;
#11803 = CARTESIAN_POINT ( 'NONE',  ( -53.51423613279429503, -130.2500000013656063, 4.591703134518082763 ) ) ;
#11804 = CARTESIAN_POINT ( 'NONE',  ( 9.457646018065525792E-16, -77.31249999863440792, 5.148502694627439702 ) ) ;
#11805 = CARTESIAN_POINT ( 'NONE',  ( -4.458734124999997661, -95.22916666530106511, 2.574251347313722516 ) ) ;
#11806 = CARTESIAN_POINT ( 'NONE',  ( -3.152548672688508926E-16, 0.1875000013655953035, -5.148502694627439702 ) ) ;
#11807 = VERTEX_POINT ( 'NONE', #32737 ) ;
#11808 = CARTESIAN_POINT ( 'NONE',  ( 0.000000000000000000, -120.0000000000000000, 5.000000000000000000 ) ) ;
#11809 = DIRECTION ( 'NONE',  ( -0.000000000000000000, 1.000000000000000000, -0.000000000000000000 ) ) ;
#11810 = CARTESIAN_POINT ( 'NONE',  ( -3.152548672688508926E-16, -85.56249999863439371, -5.148502694627439702 ) ) ;
#11811 = CARTESIAN_POINT ( 'NONE',  ( 2.229367062499998831, -84.89583333196773651, -3.861377020970580887 ) ) ;
#11812 = CARTESIAN_POINT ( 'NONE',  ( -4.458734124999999437, 12.43750000136559564, 0.000000000000000000 ) ) ;
#11813 = LINE ( 'NONE', #20851, #30484 ) ;
#11814 = CARTESIAN_POINT ( 'NONE',  ( -52.80376928212989185, -132.8750000013656063, -4.297418129356379346 ) ) ;
#11815 = CARTESIAN_POINT ( 'NONE',  ( 2.229367062499998831, -5.645833331967740953, -3.861377020970580887 ) ) ;
#11816 = CARTESIAN_POINT ( 'NONE',  ( -3.152548672688508926E-16, 16.18750000136559564, -5.148502694627439702 ) ) ;
#11817 = CARTESIAN_POINT ( 'NONE',  ( 2.229367062500001939, -50.22916666530107221, 3.861377020970579999 ) ) ;
#11818 = CARTESIAN_POINT ( 'NONE',  ( 1.975475456537005874E-15, -27.74999999999999645, 5.000000000000000000 ) ) ;
#11819 = CARTESIAN_POINT ( 'NONE',  ( 4.458734125000001214, -83.89583333196773651, 2.574251347313718519 ) ) ;
#11820 = CARTESIAN_POINT ( 'NONE',  ( -2.229367062500000163, -5.479166665301072214, -3.861377020970580443 ) ) ;
#11821 = LINE ( 'NONE', #55277, #60706 ) ;
#11822 = ORIENTED_EDGE ( 'NONE', *, *, #48201, .T. ) ;
#11823 = CARTESIAN_POINT ( 'NONE',  ( -4.458734124999999437, -36.64583333196773651, -2.574251347313719407 ) ) ;
#11824 = CARTESIAN_POINT ( 'NONE',  ( -53.51423613279429503, -128.5000000013656063, 4.591703134518082763 ) ) ;
#11825 = CARTESIAN_POINT ( 'NONE',  ( -3.152548672688508926E-16, -75.56249999863439371, -5.148502694627439702 ) ) ;
#11826 = CARTESIAN_POINT ( 'NONE',  ( -2.499999999999996447, -110.7083333306021444, 4.330127018922195425 ) ) ;
#11827 = CARTESIAN_POINT ( 'NONE',  ( -4.458734124999999437, 21.68750000136559208, 0.000000000000000000 ) ) ;
#11828 = EDGE_CURVE ( 'NONE', #17309, #42628, #2120, .T. ) ;
#11829 = EDGE_CURVE ( 'NONE', #12275, #10579, #8665, .T. ) ;
#11830 = CARTESIAN_POINT ( 'NONE',  ( -2.499999999999996447, -93.83333333333332860, 4.330127018922195425 ) ) ;
#11831 = CARTESIAN_POINT ( 'NONE',  ( -9.184850993605147944E-16, -145.3750000027312126, 5.000000000000000000 ) ) ;
#11832 = CARTESIAN_POINT ( 'NONE',  ( -2.229367062499996610, -78.39583333196773651, 3.861377020970582219 ) ) ;
#11833 = CARTESIAN_POINT ( 'NONE',  ( 5.000000000000000000, -63.41666666666665719, -2.886751345948129988 ) ) ;
#11834 = ADVANCED_FACE ( 'NONE', ( #56564 ), #42066, .T. ) ;
#11835 = CARTESIAN_POINT ( 'NONE',  ( 5.000000000000000000, -36.37499999726881583, -6.123233995736766282E-16 ) ) ;
#11836 = CARTESIAN_POINT ( 'NONE',  ( -2.499999999999996447, 20.29166666939784847, 4.330127018922195425 ) ) ;
#11837 = ORIENTED_EDGE ( 'NONE', *, *, #62117, .F. ) ;
#11838 = CARTESIAN_POINT ( 'NONE',  ( -1.339745962155613812, -57.20534180126148271, -5.000000000000000000 ) ) ;
#11839 = CARTESIAN_POINT ( 'NONE',  ( -51.75738570946856498, -138.8750000027312126, 3.805975901505576964 ) ) ;
#11841 = CARTESIAN_POINT ( 'NONE',  ( 5.000000000000000000, -24.50000000000000000, -6.123233995736766282E-16 ) ) ;
#11840 = CARTESIAN_POINT ( 'NONE',  ( -5.000000000000000888, -149.5625000000000568, -2.071067811865475949 ) ) ;
#11842 = CARTESIAN_POINT ( 'NONE',  ( -4.458734124999998549, -25.22916666530106866, 2.574251347313722516 ) ) ;
#11843 = CARTESIAN_POINT ( 'NONE',  ( 4.458734124999998549, -88.72916666530106511, -2.574251347313721627 ) ) ;
#11844 = ADVANCED_FACE ( 'NONE', ( #17635 ), #46907, .T. ) ;
#11845 = CARTESIAN_POINT ( 'NONE',  ( -5.000000000000000000, -25.95833333060214798, -2.886751345948128211 ) ) ;
#11847 = VERTEX_POINT ( 'NONE', #13120 ) ;
#11846 = CARTESIAN_POINT ( 'NONE',  ( -2.229367062500000163, -54.47916666530107221, -3.861377020970580443 ) ) ;
#11848 = CARTESIAN_POINT ( 'NONE',  ( 5.000000000000000000, -59.29166666393547303, -2.886751345948130876 ) ) ;
#11849 = EDGE_CURVE ( 'NONE', #62091, #33038, #37043, .T. ) ;
#11851 = ORIENTED_EDGE ( 'NONE', *, *, #31628, .F. ) ;
#11850 = CARTESIAN_POINT ( 'NONE',  ( -2.229367062500000163, -3.729166665301070438, -3.861377020970580443 ) ) ;
#11852 = CARTESIAN_POINT ( 'NONE',  ( -2.499999999999996447, -72.83333333333332860, 4.330127018922195425 ) ) ;
#11853 = CARTESIAN_POINT ( 'NONE',  ( -54.64476657466781973, -137.8125000013656063, -4.444560631937228834 ) ) ;
#11854 = CARTESIAN_POINT ( 'NONE',  ( 2.229367062499998831, -44.89583333196774362, -3.861377020970580887 ) ) ;
#11855 = CARTESIAN_POINT ( 'NONE',  ( -6.972266317189433020E-16, -68.24999999999998579, -5.000000000000000000 ) ) ;
#11856 =( BOUNDED_CURVE ( )  B_SPLINE_CURVE ( 2, ( #3768, #47200, #51713, #3144, #33035, #23069, #52651, #46884, #8586 ),
 .UNSPECIFIED., .F., .F. ) 
 B_SPLINE_CURVE_WITH_KNOTS ( ( 3, 2, 2, 2, 3 ),
 ( 0.5750000000000005107, 0.5791666666666672736, 0.5833333333333339255, 0.5875000000000004663, 0.5916666666666671182 ),
 .UNSPECIFIED. ) 
 CURVE ( )  GEOMETRIC_REPRESENTATION_ITEM ( )  RATIONAL_B_SPLINE_CURVE ( ( 0.9999999999999898970, 0.9238795325112968415, 1.000000000000000000, 0.9238795325112867385, 1.000000000000000000, 0.9238795325112867385, 1.000000000000000000, 0.9238795325112786339, 1.000000000000008216 ) ) 
 REPRESENTATION_ITEM ( '' )  );
#11857 = EDGE_CURVE ( 'NONE', #57389, #51032, #43580, .T. ) ;
#11858 = CARTESIAN_POINT ( 'NONE',  ( -3.535250795749689387E-16, -69.12499999726880162, -5.773502691896257311 ) ) ;
#11859 = CARTESIAN_POINT ( 'NONE',  ( -5.000000000000000000, -81.95833333060213022, -2.886751345948128211 ) ) ;
#11860 = CARTESIAN_POINT ( 'NONE',  ( -51.75738570946856498, -154.7500000000000284, 3.805975901505576964 ) ) ;
#11861 = CARTESIAN_POINT ( 'NONE',  ( 2.229367062499998831, -15.89583333196773651, -3.861377020970580887 ) ) ;
#11862 = CARTESIAN_POINT ( 'NONE',  ( 2.229367062500001939, -51.22916666530107221, 3.861377020970579999 ) ) ;
#11863 = CARTESIAN_POINT ( 'NONE',  ( 2.500000000000002220, 22.33333333333333215, 4.330127018922192761 ) ) ;
#11864 = CARTESIAN_POINT ( 'NONE',  ( 3.152801135295367541, -142.3125000013655779, -3.152801135295367541 ) ) ;
#11865 = CARTESIAN_POINT ( 'NONE',  ( 4.458734124999998549, -95.97916666530107932, -2.574251347313721627 ) ) ;
#11866 = CARTESIAN_POINT ( 'NONE',  ( 5.000000000000000000, -8.291666663935481907, -2.886751345948130876 ) ) ;
#11867 = VERTEX_POINT ( 'NONE', #3791 ) ;
#11868 = DIRECTION ( 'NONE',  ( -0.000000000000000000, 1.000000000000000000, -0.000000000000000000 ) ) ;
#11869 = CARTESIAN_POINT ( 'NONE',  ( 2.229367062499998831, 24.10416666803225993, -3.861377020970580887 ) ) ;
#11870 = CARTESIAN_POINT ( 'NONE',  ( -49.85088928181150436, -147.6875000027311557, -1.666127454062680702 ) ) ;
#11871 = LINE ( 'NONE', #56596, #27063 ) ;
#11872 = CARTESIAN_POINT ( 'NONE',  ( 2.229367062500001939, 0.02083333469892964529, 3.861377020970579999 ) ) ;
#11873 = CARTESIAN_POINT ( 'NONE',  ( -3.152548672688508926E-16, -97.81249999863439371, -5.148502694627439702 ) ) ;
#11874 = CARTESIAN_POINT ( 'NONE',  ( 4.458734124999999437, -148.6875000013656063, 0.000000000000000000 ) ) ;
#11875 = CARTESIAN_POINT ( 'NONE',  ( -4.458734124999999437, -24.64583333196773651, -2.574251347313719407 ) ) ;
#11876 = CARTESIAN_POINT ( 'NONE',  ( 2.229367062500001939, -63.22916666530106511, 3.861377020970579999 ) ) ;
#11877 = CARTESIAN_POINT ( 'NONE',  ( -1.339745962155610925, -83.66965819600733312, 5.000000000000000000 ) ) ;
#11878 = CARTESIAN_POINT ( 'NONE',  ( -2.229367062500000163, -9.479166665301068662, -3.861377020970580443 ) ) ;
#11879 = CARTESIAN_POINT ( 'NONE',  ( -6.972266317189433020E-16, -93.12499999726881583, -5.000000000000000000 ) ) ;
#11880 = CARTESIAN_POINT ( 'NONE',  ( -4.458734125000000326, -146.8750000013656063, 1.846868145590734089 ) ) ;
#11881 =( BOUNDED_CURVE ( )  B_SPLINE_CURVE ( 2, ( #4320, #49875, #25439, #43853, #30579, #52898, #58034, #35101, #30252 ),
 .UNSPECIFIED., .F., .F. ) 
 B_SPLINE_CURVE_WITH_KNOTS ( ( 3, 2, 2, 2, 3 ),
 ( 0.3232142857142857317, 0.3238095238095238249, 0.3250000000000000111, 0.3261904761904761973, 0.3267857142857142905 ),
 .UNSPECIFIED. ) 
 CURVE ( )  GEOMETRIC_REPRESENTATION_ITEM ( )  RATIONAL_B_SPLINE_CURVE ( ( 0.9330127018922194093, 0.9330127018922194093, 1.000000000000000000, 0.8660254037844387076, 1.000000000000000000, 0.8660254037844387076, 1.000000000000000000, 0.9330127018922194093, 0.9330127018922194093 ) ) 
 REPRESENTATION_ITEM ( '' )  );
#11882 = CARTESIAN_POINT ( 'NONE',  ( -4.458734124999997661, 14.52083333469892779, 2.574251347313722516 ) ) ;
#11883 = ORIENTED_EDGE ( 'NONE', *, *, #17664, .T. ) ;
#11884 = CARTESIAN_POINT ( 'NONE',  ( -4.999999999999998224, -13.79166666393548191, 2.886751345948131764 ) ) ;
#11885 = CARTESIAN_POINT ( 'NONE',  ( 1.339745962155612702, -66.16965819600733312, -5.000000000000000000 ) ) ;
#11887 = CARTESIAN_POINT ( 'NONE',  ( -4.458734124999999437, -19.39583333196774007, -2.574251347313719407 ) ) ;
#11886 = CARTESIAN_POINT ( 'NONE',  ( -4.999999999999999112, -83.91666666666667140, 2.886751345948131764 ) ) ;
#11888 = CARTESIAN_POINT ( 'NONE',  ( 2.229367062500001939, 25.77083333469892779, 3.861377020970579999 ) ) ;
#11889 = CARTESIAN_POINT ( 'NONE',  ( -6.972266317189433020E-16, 1.875000002731185722, -5.000000000000000000 ) ) ;
#11890 = AXIS2_PLACEMENT_3D ( 'NONE', #18294, #37917, #46305 ) ;
#11891 = CARTESIAN_POINT ( 'NONE',  ( -57.89159099828107458, -147.6875000013656063, -3.393966926194107447 ) ) ;
#11892 = CARTESIAN_POINT ( 'NONE',  ( -3.535250795749689387E-16, -48.12499999726880873, -5.773502691896257311 ) ) ;
#11893 = CARTESIAN_POINT ( 'NONE',  ( 2.499999999999998668, -41.20833333060214443, -4.330127018922193649 ) ) ;
#11894 = CARTESIAN_POINT ( 'NONE',  ( 4.458734124999998549, 10.27083333469892779, -2.574251347313721627 ) ) ;
#11895 = FACE_OUTER_BOUND ( 'NONE', #21259, .T. ) ;
#11896 = PRODUCT_DEFINITION_CONTEXT ( 'detailed design', #12544, 'design' ) ;
#11897 = CYLINDRICAL_SURFACE ( 'NONE', #11985, 5.000000000000000000 ) ;
#11898 = CARTESIAN_POINT ( 'NONE',  ( -2.229367062500000163, 11.52083333469892601, -3.861377020970580443 ) ) ;
#11899 = CARTESIAN_POINT ( 'NONE',  ( -4.458734124999999437, -65.39583333196773651, -2.574251347313719407 ) ) ;
#11900 = CARTESIAN_POINT ( 'NONE',  ( 4.458734125000000326, -16.14583333196773651, 2.574251347313718519 ) ) ;
#11901 =( BOUNDED_CURVE ( )  B_SPLINE_CURVE ( 2, ( #28896, #34678, #19880, #14102, #28582, #58801, #39176, #9281, #14732 ),
 .UNSPECIFIED., .F., .F. ) 
 B_SPLINE_CURVE_WITH_KNOTS ( ( 3, 2, 2, 2, 3 ),
 ( 0.4020833333333333481, 0.4027777777777777901, 0.4041666666666666741, 0.4055555555555555580, 0.4062500000000000000 ),
 .UNSPECIFIED. ) 
 CURVE ( )  GEOMETRIC_REPRESENTATION_ITEM ( )  RATIONAL_B_SPLINE_CURVE ( ( 0.9330127018922194093, 0.9330127018922194093, 1.000000000000000000, 0.8660254037844387076, 1.000000000000000000, 0.8660254037844387076, 1.000000000000000000, 0.9330127018922194093, 0.9330127018922194093 ) ) 
 REPRESENTATION_ITEM ( '' )  );
#11902 = CARTESIAN_POINT ( 'NONE',  ( -5.000000000000000000, 1.000000000000000888, 0.000000000000000000 ) ) ;
#11903 = CARTESIAN_POINT ( 'NONE',  ( -8.190561711645485556E-16, -159.6875000013655779, 4.458734124999999437 ) ) ;
#11904 = DIRECTION ( 'NONE',  ( -0.000000000000000000, -1.000000000000000000, -0.000000000000000000 ) ) ;
#11905 = CARTESIAN_POINT ( 'NONE',  ( -4.458734124999998549, -60.22916666530106511, 2.574251347313722516 ) ) ;
#11906 = CARTESIAN_POINT ( 'NONE',  ( -4.999999999999999112, -92.79166666393547303, 2.886751345948131764 ) ) ;
#11907 = CARTESIAN_POINT ( 'NONE',  ( -5.000000000000000000, 9.999999999999998224, 0.000000000000000000 ) ) ;
#11908 = CARTESIAN_POINT ( 'NONE',  ( -57.46284108482265651, -152.0625000027312410, 4.819101127000238627 ) ) ;
#11909 = CARTESIAN_POINT ( 'NONE',  ( 4.458734125000000326, -37.89583333196773651, 2.574251347313718519 ) ) ;
#11910 = ADVANCED_FACE ( 'NONE', ( #42379 ), #17315, .T. ) ;
#11911 = DIRECTION ( 'NONE',  ( -0.000000000000000000, 1.000000000000000000, -0.000000000000000000 ) ) ;
#11912 = CARTESIAN_POINT ( 'NONE',  ( 5.000000000000000000, -50.50000000000000000, -6.123233995736766282E-16 ) ) ;
#11913 = CARTESIAN_POINT ( 'NONE',  ( 1.975475456537005874E-15, -13.75000000000000000, 5.000000000000000000 ) ) ;
#11914 = DIRECTION ( 'NONE',  ( -0.000000000000000000, 1.000000000000000000, -0.000000000000000000 ) ) ;
#11915 = VERTEX_POINT ( 'NONE', #18576 ) ;
#11916 = CARTESIAN_POINT ( 'NONE',  ( -4.458734124999999437, -108.3124999986343937, 0.000000000000000000 ) ) ;
#11917 = CARTESIAN_POINT ( 'NONE',  ( 2.229367062499998831, -0.8958333319677401763, -3.861377020970580887 ) ) ;
#11918 = CARTESIAN_POINT ( 'NONE',  ( -2.499999999999996447, -6.833333333333330373, 4.330127018922195425 ) ) ;
#11919 = CARTESIAN_POINT ( 'NONE',  ( -4.458734124999999437, -74.39583333196775072, -2.574251347313719407 ) ) ;
#11920 = FACE_OUTER_BOUND ( 'NONE', #44522, .T. ) ;
#11921 = CARTESIAN_POINT ( 'NONE',  ( 5.000000000000000888, -9.458333330602144429, 2.886751345948126879 ) ) ;
#11923 = ORIENTED_EDGE ( 'NONE', *, *, #22427, .T. ) ;
#11922 = CARTESIAN_POINT ( 'NONE',  ( 2.229367062499998831, -37.64583333196773651, -3.861377020970580887 ) ) ;
#11925 = ORIENTED_EDGE ( 'NONE', *, *, #50417, .T. ) ;
#11924 = CARTESIAN_POINT ( 'NONE',  ( -4.458734124999999437, 13.35416666803225993, -2.574251347313719407 ) ) ;
#11926 = FACE_OUTER_BOUND ( 'NONE', #36238, .T. ) ;
#11927 = CARTESIAN_POINT ( 'NONE',  ( 1.060575238724906964E-15, -53.74999999999998579, 5.773502691896257311 ) ) ;
#11928 = ADVANCED_FACE ( 'NONE', ( #13744 ), #46588, .T. ) ;
#11929 = CARTESIAN_POINT ( 'NONE',  ( -1.846868145590737420, -162.0000000013655779, 4.458734124999999437 ) ) ;
#11930 = CARTESIAN_POINT ( 'NONE',  ( 2.229367062500001939, -30.22916666530107221, 3.861377020970579999 ) ) ;
#11931 = CARTESIAN_POINT ( 'NONE',  ( -1.339745962155613812, -87.20534180126148271, -5.000000000000000000 ) ) ;
#11932 = CARTESIAN_POINT ( 'NONE',  ( 9.457646018065525792E-16, -73.06249999863440792, 5.148502694627439702 ) ) ;
#11933 = VECTOR ( 'NONE', #46910, 1000.000000000000000 ) ;
#11934 = CARTESIAN_POINT ( 'NONE',  ( -5.000000000000000000, -168.5000000000000000, -6.123233995736766282E-16 ) ) ;
#11935 = ADVANCED_FACE ( 'NONE', ( #18878, #4105 ), #24981, .T. ) ;
#11936 = CARTESIAN_POINT ( 'NONE',  ( -4.458734124999999437, -88.39583333196773651, -2.574251347313719407 ) ) ;
#11937 = CARTESIAN_POINT ( 'NONE',  ( -59.29741812935640155, -133.8750000013656063, -2.196230717870135685 ) ) ;
#11938 = VECTOR ( 'NONE', #32795, 1000.000000000000000 ) ;
#11939 = CIRCLE ( 'NONE', #32512, 0.7733184030943203169 ) ;
#11940 = CARTESIAN_POINT ( 'NONE',  ( -4.458734124999999437, -33.56249999863440792, 0.000000000000000000 ) ) ;
#11941 = EDGE_CURVE ( 'NONE', #19205, #38280, #44265, .T. ) ;
#11942 = ORIENTED_EDGE ( 'NONE', *, *, #39284, .T. ) ;
#11943 = CARTESIAN_POINT ( 'NONE',  ( 2.229367062499998831, -78.89583333196773651, -3.861377020970580887 ) ) ;
#11944 = CARTESIAN_POINT ( 'NONE',  ( 5.000000000000000000, 3.583333333333333925, -2.886751345948130876 ) ) ;
#11945 = VERTEX_POINT ( 'NONE', #5041 ) ;
#11946 = CARTESIAN_POINT ( 'NONE',  ( 0.000000000000000000, -120.0000000000000000, 5.000000000000000000 ) ) ;
#11947 = DIRECTION ( 'NONE',  ( -0.000000000000000000, 1.000000000000000000, -0.000000000000000000 ) ) ;
#11948 = CARTESIAN_POINT ( 'NONE',  ( -2.229367062499996610, -66.39583333196773651, 3.861377020970582219 ) ) ;
#11949 = CARTESIAN_POINT ( 'NONE',  ( 4.458734124999998549, -7.979166665301073991, -2.574251347313721627 ) ) ;
#11950 = VERTEX_POINT ( 'NONE', #10183 ) ;
#11951 = CARTESIAN_POINT ( 'NONE',  ( -6.972266317189433020E-16, -85.25000000000000000, -5.000000000000000000 ) ) ;
#11952 = CARTESIAN_POINT ( 'NONE',  ( -4.999999999999998224, -92.79166666393545881, 2.886751345948131764 ) ) ;
#11953 = VERTEX_POINT ( 'NONE', #43322 ) ;
#11954 = CARTESIAN_POINT ( 'NONE',  ( -4.458734124999999437, -6.562499998634403475, 0.000000000000000000 ) ) ;
#11955 = CARTESIAN_POINT ( 'NONE',  ( -53.33387254593723981, -146.9375000027312126, 5.149110718188528502 ) ) ;
#11956 = CARTESIAN_POINT ( 'NONE',  ( 2.229367062499998831, 10.35416666803225993, -3.861377020970580887 ) ) ;
#11957 = CARTESIAN_POINT ( 'NONE',  ( 0.000000000000000000, -170.0000000000000000, 0.000000000000000000 ) ) ;
#11958 = CARTESIAN_POINT ( 'NONE',  ( -3.152801135295367985, -155.8125000013656063, 3.152801135295367096 ) ) ;
#11959 = LINE ( 'NONE', #25813, #35820 ) ;
#11960 = VERTEX_POINT ( 'NONE', #34300 ) ;
#11961 = CARTESIAN_POINT ( 'NONE',  ( -4.458734124999999437, -85.31249999863439371, 0.000000000000000000 ) ) ;
#11962 = CARTESIAN_POINT ( 'NONE',  ( 0.000000000000000000, -120.0000000000000000, 0.000000000000000000 ) ) ;
#11963 = CARTESIAN_POINT ( 'NONE',  ( -2.229367062500000163, -2.479166665301069106, -3.861377020970580443 ) ) ;
#11964 = FACE_OUTER_BOUND ( 'NONE', #58136, .T. ) ;
#11965 = CARTESIAN_POINT ( 'NONE',  ( -3.535250795749689387E-16, -28.12499999726880873, -5.773502691896257311 ) ) ;
#11966 = CARTESIAN_POINT ( 'NONE',  ( 1.339745962155615144, -78.70534180126148271, 4.999999999999999112 ) ) ;
#11967 = CARTESIAN_POINT ( 'NONE',  ( -2.229367062499996610, 22.85416666803225993, 3.861377020970582219 ) ) ;
#11968 = CARTESIAN_POINT ( 'NONE',  ( -55.00000000000002132, -155.0000000000000284, 1.734723475976807094E-15 ) ) ;
#11969 = CARTESIAN_POINT ( 'NONE',  ( 2.499999999999998668, -82.20833333060214443, -4.330127018922193649 ) ) ;
#11970 = CARTESIAN_POINT ( 'NONE',  ( 2.229367062499998831, -52.64583333196773651, -3.861377020970580887 ) ) ;
#11971 = CARTESIAN_POINT ( 'NONE',  ( 4.458734125000000326, -39.14583333196773651, 2.574251347313718519 ) ) ;
#11972 = CARTESIAN_POINT ( 'NONE',  ( 4.458734125000000326, 0.8541666680322613781, 2.574251347313718519 ) ) ;
#11973 = AXIS2_PLACEMENT_3D ( 'NONE', #52493, #33182, #61517 ) ;
#11974 = CARTESIAN_POINT ( 'NONE',  ( 1.975475456537005874E-15, -97.62499999726880162, 5.000000000000000000 ) ) ;
#11975 = CARTESIAN_POINT ( 'NONE',  ( -4.999999999999999112, 16.08333333333333215, 2.886751345948131764 ) ) ;
#11976 = CARTESIAN_POINT ( 'NONE',  ( 2.071067811865476394, -146.3125000027312410, 5.000000000000000000 ) ) ;
#11977 = CARTESIAN_POINT ( 'NONE',  ( -2.916731409357579869E-14, 12.37500000273118594, 5.000000000000000888 ) ) ;
#11978 = CARTESIAN_POINT ( 'NONE',  ( 4.458734124999999437, -41.81249999863440081, -5.460374474430324690E-16 ) ) ;
#11979 = CARTESIAN_POINT ( 'NONE',  ( 1.060575238724906964E-15, -79.62499999726881583, 5.773502691896257311 ) ) ;
#11980 = VECTOR ( 'NONE', #36781, 1000.000000000000000 ) ;
#11981 = CARTESIAN_POINT ( 'NONE',  ( -52.10840900171896806, -141.4375000013656063, 3.393966926194110556 ) ) ;
#11982 =( BOUNDED_CURVE ( )  B_SPLINE_CURVE ( 2, ( #40891, #26749, #6500, #2627, #21923, #16776, #27370, #61802, #56024 ),
 .UNSPECIFIED., .F., .F. ) 
 B_SPLINE_CURVE_WITH_KNOTS ( ( 3, 2, 2, 2, 3 ),
 ( 0.7089285714285714635, 0.7095238095238095566, 0.7107142857142857428, 0.7119047619047619291, 0.7125000000000000222 ),
 .UNSPECIFIED. ) 
 CURVE ( )  GEOMETRIC_REPRESENTATION_ITEM ( )  RATIONAL_B_SPLINE_CURVE ( ( 0.9330127018922194093, 0.9330127018922194093, 1.000000000000000000, 0.8660254037844387076, 1.000000000000000000, 0.8660254037844387076, 1.000000000000000000, 0.9330127018922194093, 0.9330127018922194093 ) ) 
 REPRESENTATION_ITEM ( '' )  );
#11983 = CARTESIAN_POINT ( 'NONE',  ( -6.972266317189433020E-16, -65.12499999726880162, -5.000000000000000000 ) ) ;
#11984 = EDGE_CURVE ( 'NONE', #39875, #56335, #39125, .T. ) ;
#11985 = AXIS2_PLACEMENT_3D ( 'NONE', #56623, #27022, #42432 ) ;
#11986 = CARTESIAN_POINT ( 'NONE',  ( -2.229367062500000163, -87.72916666530107932, -3.861377020970580443 ) ) ;
#11987 = CARTESIAN_POINT ( 'NONE',  ( 1.846868145590736310, -159.8750000013655779, 4.458734124999997661 ) ) ;
#11988 = DIRECTION ( 'NONE',  ( -0.000000000000000000, 1.000000000000000000, -0.000000000000000000 ) ) ;
#11989 = CARTESIAN_POINT ( 'NONE',  ( 2.499999999999998668, -33.33333333333332860, -4.330127018922193649 ) ) ;
#11990 = CARTESIAN_POINT ( 'NONE',  ( -2.499999999999996447, -90.70833333060214443, 4.330127018922195425 ) ) ;
#11991 = ORIENTED_EDGE ( 'NONE', *, *, #36714, .T. ) ;
#11992 = CARTESIAN_POINT ( 'NONE',  ( -2.229367062499996610, 23.60416666803225993, 3.861377020970582219 ) ) ;
#11993 = ORIENTED_EDGE ( 'NONE', *, *, #42855, .T. ) ;
#11994 = CARTESIAN_POINT ( 'NONE',  ( 4.458734124999998549, -88.72916666530106511, -2.574251347313721627 ) ) ;
#11995 = CARTESIAN_POINT ( 'NONE',  ( -4.458734124999999437, 14.43750000136559386, 0.000000000000000000 ) ) ;
#11996 = CARTESIAN_POINT ( 'NONE',  ( 2.499999999999998668, 14.79166666939785202, -4.330127018922193649 ) ) ;
#11997 = CARTESIAN_POINT ( 'NONE',  ( 0.000000000000000000, -120.0000000000000000, 5.000000000000000000 ) ) ;
#11998 = CARTESIAN_POINT ( 'NONE',  ( 5.000000000000000888, 9.416666666666666075, 2.886751345948126879 ) ) ;
#11999 = CARTESIAN_POINT ( 'NONE',  ( 9.457646018065525792E-16, -56.06249999863440792, 5.148502694627439702 ) ) ;
#12000 = CARTESIAN_POINT ( 'NONE',  ( 7.908217798048221781, 3.084840533507044125, -7.795645399445156443 ) ) ;
#12001 = CARTESIAN_POINT ( 'NONE',  ( -5.000000000000000000, -52.08333333333332860, -2.886751345948128211 ) ) ;
#12002 = DIRECTION ( 'NONE',  ( -0.000000000000000000, 1.000000000000000000, -0.000000000000000000 ) ) ;
#12003 = CARTESIAN_POINT ( 'NONE',  ( 5.000000000000000888, -1.583333333333332371, 2.886751345948126879 ) ) ;
#12004 = CARTESIAN_POINT ( 'NONE',  ( -4.999999999999998224, 18.20833333606451632, 2.886751345948131764 ) ) ;
#12005 = CARTESIAN_POINT ( 'NONE',  ( 2.500000000000002220, -41.66666666666667140, 4.330127018922192761 ) ) ;
#12006 = CARTESIAN_POINT ( 'NONE',  ( 2.499999999999998668, -96.33333333333332860, -4.330127018922193649 ) ) ;
#12008 = CARTESIAN_POINT ( 'NONE',  ( 2.229367062500001939, -15.22916666530107399, 3.861377020970579999 ) ) ;
#12007 = CARTESIAN_POINT ( 'NONE',  ( -1.339745962155610925, -44.79465819873851018, 5.000000000000000000 ) ) ;
#12009 = DIRECTION ( 'NONE',  ( 0.000000000000000000, 0.000000000000000000, 1.000000000000000000 ) ) ;
#12010 = CARTESIAN_POINT ( 'NONE',  ( -4.458734124999998549, -62.22916666530106511, 2.574251347313722516 ) ) ;
#12011 = CARTESIAN_POINT ( 'NONE',  ( 1.846868145590735200, -151.5000000013655779, -4.458734125000000326 ) ) ;
#12012 = CARTESIAN_POINT ( 'NONE',  ( 2.229367062499998831, -69.64583333196773651, -3.861377020970580887 ) ) ;
#12013 = CARTESIAN_POINT ( 'NONE',  ( -53.51423613279429503, -145.5000000013656063, 4.591703134518082763 ) ) ;
#12014 = CARTESIAN_POINT ( 'NONE',  ( 4.458734124999999437, -18.06249999863440792, -5.460374474430324690E-16 ) ) ;
#12015 = CARTESIAN_POINT ( 'NONE',  ( 5.000000000000000000, -63.37499999726880873, -6.123233995736766282E-16 ) ) ;
#12016 = VERTEX_POINT ( 'NONE', #43631 ) ;
#12017 = CARTESIAN_POINT ( 'NONE',  ( -5.000000000000000888, -150.5625000000000284, -2.071067811865475949 ) ) ;
#12018 = ORIENTED_EDGE ( 'NONE', *, *, #34127, .F. ) ;
#12019 = CARTESIAN_POINT ( 'NONE',  ( 4.458734124999999437, -60.06249999863440081, -5.460374474430324690E-16 ) ) ;
#12021 = CARTESIAN_POINT ( 'NONE',  ( 1.339745962155670655, -8.294658198738522614, -4.999999999999966249 ) ) ;
#12020 = CARTESIAN_POINT ( 'NONE',  ( 1.975475456537005874E-15, -27.74999999999999645, 5.000000000000000000 ) ) ;
#12022 = CARTESIAN_POINT ( 'NONE',  ( -3.152801135295367985, -153.8125000013656063, 3.152801135295367096 ) ) ;
#12023 = ORIENTED_EDGE ( 'NONE', *, *, #35372, .F. ) ;
#12024 = AXIS2_PLACEMENT_3D ( 'NONE', #52735, #17384, #32156 ) ;
#12025 = CARTESIAN_POINT ( 'NONE',  ( 5.000000000000000000, 25.58333333333333215, -2.886751345948130876 ) ) ;
#12026 = CARTESIAN_POINT ( 'NONE',  ( 4.606548227981508425, 6.456511556909250160, -7.591235721156633254 ) ) ;
#12027 = LINE ( 'NONE', #55789, #26784 ) ;
#12028 = CARTESIAN_POINT ( 'NONE',  ( -4.458734124999999437, -46.56249999863440792, 0.000000000000000000 ) ) ;
#12029 = EDGE_LOOP ( 'NONE', ( #36953, #53245, #6345, #5103 ) ) ;
#12030 = AXIS2_PLACEMENT_3D ( 'NONE', #21556, #15770, #55006 ) ;
#12031 = CARTESIAN_POINT ( 'NONE',  ( -5.000000000000000000, 17.04166666939785202, -2.886751345948128211 ) ) ;
#12032 = CLOSED_SHELL ( 'NONE', ( #32837, #57750, #31074, #60679, #4782, #34619, #63659, #2411, #54418, #4459, #8442, #13444, #34621, #46501, #47286, #6254, #47306, #50514, #34269, #26004, #30266, #62534, #21598, #4657, #3897, #41679, #14524, #46195, #51220, #27459, #731, #43895, #53883, #39772, #40186, #41617, #50611, #29923, #1231, #31980, #44886, #21303, #17700, #4819, #50763, #918, #41418, #28610, #28746, #26673, #13821, #52818, #29171, #25208, #37781, #52724, #18099, #2359, #55957, #49118, #12289, #30926, #44660, #30633, #18033, #35809, #44361, #44058, #21218, #60160, #6607, #37504, #14429, #61029, #4787, #44983, #34280, #17391, #40967, #31618, #38981, #29451, #54988, #50796, #10588, #11396, #22083, #44423, #34785, #12144, #8996, #16062, #3185, #10689, #30687, #935, #52310, #9871, #21503, #5620, #24047, #7, #30609, #60877, #16662, #55047, #7582, #84, #51572, #39410, #49487, #39436, #42396, #11393, #27982, #31823, #48007, #110, #45169, #2273, #293, #62559, #21033, #45346, #12309, #35335, #24859, #49800, #1291, #8712, #55962, #32240, #59406, #16864, #48794, #38140, #903, #35381, #31545, #36240, #7422, #60139, #33440, #62385, #20955, #38218, #21963, #41410, #20414, #21298, #18596, #24324, #42569, #55515, #38992, #47739, #59778, #42472, #12535, #43266, #7454, #18441, #61320, #21302, #1622, #5230, #23092, #48365, #4328, #44079, #6976, #57486, #39813, #57021, #53378, #17521, #56595, #59795, #42056, #36913, #47993, #18951, #27604, #34733, #58094, #61831, #3589, #57813, #8397, #10306, #47499, #61695, #11844, #42083, #55929, #51577, #17470, #42132, #37607, #52028, #15512, #186, #33753, #41227, #7465, #60315, #57919, #55360, #32334, #58076, #15047, #55606, #22087, #58098, #32333, #36271, #2447, #62964, #18669, #49147, #1154, #37405, #49151, #55854, #35450, #8746, #32972, #50865, #38302, #38905, #46352, #47148, #462, #46510, #53357, #61662, #26436, #54167, #925, #37497, #29452, #44022, #32701, #33046, #59792, #28760, #8721, #47555, #4449, #49617, #43706, #37426, #52752, #15067, #59418, #21670, #40003, #46365, #28249, #23354, #29416, #61381, #8716, #37369, #14327, #53048, #57535, #7773, #2096, #11334, #17814, #3650, #53170, #29902, #62966, #26278, #38558, #31075, #11503, #34181, #17369, #59713, #60959, #44422, #50702, #1297, #52643, #27625, #8311, #55650, #20105, #45568, #32179, #60501, #3950, #53616, #52395, #26670, #51589, #33320 ) ) ;
#12033 = CARTESIAN_POINT ( 'NONE',  ( -4.458734124999999437, 9.687500001365593860, 0.000000000000000000 ) ) ;
#12034 =( BOUNDED_CURVE ( )  B_SPLINE_CURVE ( 2, ( #21971, #27970, #63032, #8985, #58507, #18640, #9609, #3853, #2362 ),
 .UNSPECIFIED., .F., .F. ) 
 B_SPLINE_CURVE_WITH_KNOTS ( ( 3, 2, 2, 2, 3 ),
 ( 0.6696428571428570953, 0.6702380952380951884, 0.6714285714285713746, 0.6726190476190476719, 0.6732142857142857650 ),
 .UNSPECIFIED. ) 
 CURVE ( )  GEOMETRIC_REPRESENTATION_ITEM ( )  RATIONAL_B_SPLINE_CURVE ( ( 0.9330127018922194093, 0.9330127018922194093, 1.000000000000000000, 0.8660254037844387076, 1.000000000000000000, 0.8660254037844387076, 1.000000000000000000, 0.9330127018922194093, 0.9330127018922194093 ) ) 
 REPRESENTATION_ITEM ( '' )  );
#12035 = CARTESIAN_POINT ( 'NONE',  ( -4.458734124999998549, 25.77083333469892779, 2.574251347313722516 ) ) ;
#12036 = CARTESIAN_POINT ( 'NONE',  ( -50.70258187064364108, -148.1250000013656063, 2.196230717870141014 ) ) ;
#12037 = CARTESIAN_POINT ( 'NONE',  ( 5.000000000000000888, -108.4583333306021444, 2.886751345948126879 ) ) ;
#12038 = CARTESIAN_POINT ( 'NONE',  ( 1.846868145590735200, -167.2500000013655779, -4.458734124999999437 ) ) ;
#12039 = ORIENTED_EDGE ( 'NONE', *, *, #49514, .T. ) ;
#12040 = CARTESIAN_POINT ( 'NONE',  ( 2.229367062500001939, -70.97916666530107932, 3.861377020970579999 ) ) ;
#12041 = CARTESIAN_POINT ( 'NONE',  ( -1.339745962155610925, -49.66965819600732601, 5.000000000000000000 ) ) ;
#12042 = CARTESIAN_POINT ( 'NONE',  ( -4.458734124999998549, 14.77083333469892779, 2.574251347313722516 ) ) ;
#12043 = ADVANCED_FACE ( 'NONE', ( #58751 ), #14680, .T. ) ;
#12044 = CYLINDRICAL_SURFACE ( 'NONE', #61808, 5.000000000000000000 ) ;
#12045 = DIRECTION ( 'NONE',  ( 0.000000000000000000, 0.000000000000000000, 1.000000000000000000 ) ) ;
#12046 = CARTESIAN_POINT ( 'NONE',  ( -4.458734124999999437, -53.56249999863439371, 0.000000000000000000 ) ) ;
#12047 = CARTESIAN_POINT ( 'NONE',  ( -5.000000000000000000, -14.87499999726881228, 0.000000000000000000 ) ) ;
#12048 = CARTESIAN_POINT ( 'NONE',  ( 1.975475456537005874E-15, -18.74999999999999645, 5.000000000000000000 ) ) ;
#12049 = CARTESIAN_POINT ( 'NONE',  ( 3.061616997868383141E-16, -139.8750000027312126, -5.000000000000000000 ) ) ;
#12050 = CARTESIAN_POINT ( 'NONE',  ( -1.339745962155610925, -83.66965819600733312, 5.000000000000000000 ) ) ;
#12051 = CARTESIAN_POINT ( 'NONE',  ( 2.229367062500001939, -23.22916666530107221, 3.861377020970579999 ) ) ;
#12052 = VERTEX_POINT ( 'NONE', #15003 ) ;
#12053 = CARTESIAN_POINT ( 'NONE',  ( -1.339745962155610925, -101.7946581987385315, 5.000000000000000000 ) ) ;
#12054 = CARTESIAN_POINT ( 'NONE',  ( 2.229367062500001939, -106.9791666653010651, 3.861377020970579999 ) ) ;
#12055 = CARTESIAN_POINT ( 'NONE',  ( 5.000000000000000888, -159.0625000027312126, -2.071067811865475505 ) ) ;
#12056 = EDGE_LOOP ( 'NONE', ( #47420, #41394, #29236, #43507 ) ) ;
#12057 = CARTESIAN_POINT ( 'NONE',  ( 4.458734124999999437, -103.0624999986344079, -5.460374474430324690E-16 ) ) ;
#12058 = CARTESIAN_POINT ( 'NONE',  ( 9.457646018065525792E-16, -27.06249999863440081, 5.148502694627439702 ) ) ;
#12059 = CARTESIAN_POINT ( 'NONE',  ( 2.499999999999998668, -64.20833333060213022, -4.330127018922193649 ) ) ;
#12060 = CARTESIAN_POINT ( 'NONE',  ( -59.44456063193725015, -152.8125000013656063, -0.3552334253322034230 ) ) ;
#12061 = CARTESIAN_POINT ( 'NONE',  ( -5.000000000000000888, -147.4375000000000000, 2.071067811865474617 ) ) ;
#12062 = CARTESIAN_POINT ( 'NONE',  ( -4.458734124999997661, -25.22916666530106866, 2.574251347313722516 ) ) ;
#12063 = CARTESIAN_POINT ( 'NONE',  ( -4.458734124999999437, -67.56249999863440792, 0.000000000000000000 ) ) ;
#12064 = CARTESIAN_POINT ( 'NONE',  ( 4.330127018922154569, 45.00000000000000000, -7.499999999999971578 ) ) ;
#12065 = CARTESIAN_POINT ( 'NONE',  ( -3.152548672688508926E-16, -27.56249999863440081, -5.148502694627439702 ) ) ;
#12066 = CARTESIAN_POINT ( 'NONE',  ( -6.972266317189433020E-16, 14.74999999999999822, -5.000000000000000000 ) ) ;
#12067 = CARTESIAN_POINT ( 'NONE',  ( 5.000000000000000000, -151.0625000000000000, 2.071067811865478614 ) ) ;
#12068 = CARTESIAN_POINT ( 'NONE',  ( -2.500000000000000444, -16.16666666666666785, -4.330127018922193649 ) ) ;
#12069 = CARTESIAN_POINT ( 'NONE',  ( -4.458734125000001214, -150.8750000013655779, 1.846868145590734089 ) ) ;
#12070 = VERTEX_POINT ( 'NONE', #58121 ) ;
#12071 = CARTESIAN_POINT ( 'NONE',  ( 5.000000000000000888, -149.9375000000000000, -2.071067811865475505 ) ) ;
#12072 = CARTESIAN_POINT ( 'NONE',  ( 4.458734124999998549, -48.97916666530107221, -2.574251347313721627 ) ) ;
#12073 = AXIS2_PLACEMENT_3D ( 'NONE', #11957, #1701, #7155 ) ;
#12074 = CARTESIAN_POINT ( 'NONE',  ( -2.499999999999996447, -2.708333330602146649, 4.330127018922195425 ) ) ;
#12075 = CARTESIAN_POINT ( 'NONE',  ( 2.500000000000002220, -38.54166666393548013, 4.330127018922192761 ) ) ;
#12076 = CARTESIAN_POINT ( 'NONE',  ( -2.499999999999996447, 25.16666666666666430, 4.330127018922195425 ) ) ;
#12077 = AXIS2_PLACEMENT_3D ( 'NONE', #31454, #55289, #16361 ) ;
#12078 = VECTOR ( 'NONE', #2449, 1000.000000000000000 ) ;
#12079 = DIRECTION ( 'NONE',  ( -0.000000000000000000, 1.000000000000000000, -0.000000000000000000 ) ) ;
#12080 = CARTESIAN_POINT ( 'NONE',  ( -4.458734124999998549, 5.770833334698927786, 2.574251347313722516 ) ) ;
#12081 = CARTESIAN_POINT ( 'NONE',  ( 1.339745962155612702, 19.70534180126147561, -5.000000000000000000 ) ) ;
#12082 = CARTESIAN_POINT ( 'NONE',  ( 5.000000000000000000, -41.29166666393548013, -2.886751345948130876 ) ) ;
#12083 = CARTESIAN_POINT ( 'NONE',  ( 5.000000000000000000, -7.416666666666667851, -2.886751345948130876 ) ) ;
#12084 = CARTESIAN_POINT ( 'NONE',  ( -2.229367062500000163, 16.27083333469892779, -3.861377020970580443 ) ) ;
#12085 = CARTESIAN_POINT ( 'NONE',  ( 2.500000000000002220, 4.458333336064518093, 4.330127018922192761 ) ) ;
#12086 = ORIENTED_EDGE ( 'NONE', *, *, #26702, .T. ) ;
#12087 = CARTESIAN_POINT ( 'NONE',  ( -7.500000000000000000, -3.988190556646204588, -0.8526458641284329065 ) ) ;
#12088 = ORIENTED_EDGE ( 'NONE', *, *, #27163, .T. ) ;
#12089 =( BOUNDED_CURVE ( )  B_SPLINE_CURVE ( 2, ( #51622, #12688, #36496, #54930, #47415, #47103, #41948, #56126, #22982 ),
 .UNSPECIFIED., .F., .F. ) 
 B_SPLINE_CURVE_WITH_KNOTS ( ( 3, 2, 2, 2, 3 ),
 ( 0.5267857142857143016, 0.5273809523809523947, 0.5285714285714285809, 0.5297619047619047672, 0.5303571428571428603 ),
 .UNSPECIFIED. ) 
 CURVE ( )  GEOMETRIC_REPRESENTATION_ITEM ( )  RATIONAL_B_SPLINE_CURVE ( ( 0.9330127018922194093, 0.9330127018922194093, 1.000000000000000000, 0.8660254037844387076, 1.000000000000000000, 0.8660254037844387076, 1.000000000000000000, 0.9330127018922194093, 0.9330127018922194093 ) ) 
 REPRESENTATION_ITEM ( '' )  );
#12090 = CARTESIAN_POINT ( 'NONE',  ( -2.499999999999996447, -70.83333333333332860, 4.330127018922195425 ) ) ;
#12091 = CARTESIAN_POINT ( 'NONE',  ( 4.458734125000001214, -41.89583333196773651, 2.574251347313718519 ) ) ;
#12092 = CARTESIAN_POINT ( 'NONE',  ( 1.846868145590735200, -164.5000000013655779, -4.458734125000000326 ) ) ;
#12093 = CARTESIAN_POINT ( 'NONE',  ( 5.000000000000000888, -42.45833333060214443, 2.886751345948126879 ) ) ;
#12094 = ORIENTED_EDGE ( 'NONE', *, *, #33473, .F. ) ;
#12095 = CARTESIAN_POINT ( 'NONE',  ( -3.152548672688508926E-16, -19.56249999863440081, -5.148502694627439702 ) ) ;
#12096 = ORIENTED_EDGE ( 'NONE', *, *, #7288, .T. ) ;
#12097 = CARTESIAN_POINT ( 'NONE',  ( -5.000000000000000000, -90.00000000000000000, 0.000000000000000000 ) ) ;
#12098 = CARTESIAN_POINT ( 'NONE',  ( 1.846868145590735200, -163.2500000013655495, -4.458734125000000326 ) ) ;
#12100 = ORIENTED_EDGE ( 'NONE', *, *, #36538, .F. ) ;
#12099 = CARTESIAN_POINT ( 'NONE',  ( -5.000000000000000000, -60.87499999726880873, 0.000000000000000000 ) ) ;
#12101 = CARTESIAN_POINT ( 'NONE',  ( -51.75738570946856498, -137.7500000000000000, 3.805975901505576964 ) ) ;
#12102 = CARTESIAN_POINT ( 'NONE',  ( 2.229367062500001939, -30.22916666530107221, 3.861377020970579999 ) ) ;
#12103 = ORIENTED_EDGE ( 'NONE', *, *, #748, .F. ) ;
#12104 = CARTESIAN_POINT ( 'NONE',  ( 4.458734124999999437, -76.81249999863440792, -5.460374474430324690E-16 ) ) ;
#12105 = CARTESIAN_POINT ( 'NONE',  ( 4.458734124999998549, 24.27083333469892779, -2.574251347313721627 ) ) ;
#12106 = CARTESIAN_POINT ( 'NONE',  ( -4.999999999999998224, -28.79166666393548013, 2.886751345948131764 ) ) ;
#12107 = EDGE_LOOP ( 'NONE', ( #13612, #5695, #61672, #29094 ) ) ;
#12108 = FACE_OUTER_BOUND ( 'NONE', #52618, .T. ) ;
#12109 = CARTESIAN_POINT ( 'NONE',  ( -59.59170313451810586, -143.7500000013656063, 1.485763867205729394 ) ) ;
#12110 = CARTESIAN_POINT ( 'NONE',  ( -2.229367062500000163, -79.72916666530106511, -3.861377020970580443 ) ) ;
#12111 = CARTESIAN_POINT ( 'NONE',  ( -55.39835681537999790, -129.0000000027312126, 4.984105922594378235 ) ) ;
#12112 = CARTESIAN_POINT ( 'NONE',  ( -6.972266317189433020E-16, -84.12499999726880162, -5.000000000000000000 ) ) ;
#12113 = CARTESIAN_POINT ( 'NONE',  ( 3.152801135295366208, -143.8125000013655779, 3.152801135295367985 ) ) ;
#12114 = VECTOR ( 'NONE', #46785, 1000.000000000000000 ) ;
#12115 = CARTESIAN_POINT ( 'NONE',  ( 1.339745962155615144, 20.29465819873851729, 4.999999999999999112 ) ) ;
#12116 = CARTESIAN_POINT ( 'NONE',  ( 2.229367062499998831, -53.64583333196773651, -3.861377020970580887 ) ) ;
#12117 = CARTESIAN_POINT ( 'NONE',  ( -4.458734124999999437, -47.39583333196774362, -2.574251347313719407 ) ) ;
#12118 = CARTESIAN_POINT ( 'NONE',  ( 4.458734124999998549, 26.27083333469893134, -2.574251347313721627 ) ) ;
#12119 = EDGE_CURVE ( 'NONE', #25261, #59413, #15235, .T. ) ;
#12120 = AXIS2_PLACEMENT_3D ( 'NONE', #47818, #52659, #33043 ) ;
#12121 = CARTESIAN_POINT ( 'NONE',  ( -3.535250795749689387E-16, -104.2500000000000142, -5.773502691896257311 ) ) ;
#12122 = CARTESIAN_POINT ( 'NONE',  ( 5.000000000000000000, -3.416666666666665186, -2.886751345948130876 ) ) ;
#12123 = CARTESIAN_POINT ( 'NONE',  ( 2.229367062500001939, -38.22916666530107221, 3.861377020970579999 ) ) ;
#12124 = CARTESIAN_POINT ( 'NONE',  ( 1.060575238724906964E-15, 2.375000002731185500, 5.773502691896257311 ) ) ;
#12125 = CARTESIAN_POINT ( 'NONE',  ( -1.339745962155610925, -72.79465819873850307, 5.000000000000000000 ) ) ;
#12126 = CARTESIAN_POINT ( 'NONE',  ( -52.80376928212989185, -126.8750000013656205, -4.297418129356379346 ) ) ;
#12127 = CARTESIAN_POINT ( 'NONE',  ( -2.229367062499996610, -77.39583333196773651, 3.861377020970582219 ) ) ;
#12128 = CARTESIAN_POINT ( 'NONE',  ( -1.339745962155613812, 5.794658198738519950, -5.000000000000000000 ) ) ;
#12129 = CARTESIAN_POINT ( 'NONE',  ( 9.457646018065525792E-16, -103.0624999986343937, 5.148502694627439702 ) ) ;
#12130 = CARTESIAN_POINT ( 'NONE',  ( 9.457646018065525792E-16, -7.312499998634403475, 5.148502694627439702 ) ) ;
#12131 = ORIENTED_EDGE ( 'NONE', *, *, #52293, .T. ) ;
#12132 = CARTESIAN_POINT ( 'NONE',  ( 1.975475456537005874E-15, -77.62499999726881583, 5.000000000000000000 ) ) ;
#12133 = CARTESIAN_POINT ( 'NONE',  ( -6.972266317189433020E-16, -47.24999999999999289, -5.000000000000000000 ) ) ;
#12134 = CARTESIAN_POINT ( 'NONE',  ( -3.152548672688508926E-16, -91.56249999863440792, -5.148502694627439702 ) ) ;
#12135 = CARTESIAN_POINT ( 'NONE',  ( -9.184850993605147944E-16, -168.3750000027312126, 5.000000000000000000 ) ) ;
#12136 = CARTESIAN_POINT ( 'NONE',  ( -4.458734124999999437, -86.64583333196773651, -2.574251347313719407 ) ) ;
#12137 = CARTESIAN_POINT ( 'NONE',  ( 4.458734124999998549, 10.02083333469892779, -2.574251347313721627 ) ) ;
#12138 = CARTESIAN_POINT ( 'NONE',  ( 1.975475456537005874E-15, -15.75000000000000000, 5.000000000000000000 ) ) ;
#12139 = AXIS2_PLACEMENT_3D ( 'NONE', #10994, #21927, #60855 ) ;
#12140 = CARTESIAN_POINT ( 'NONE',  ( -57.19623071787017210, -132.3750000013656347, 4.297418129356382899 ) ) ;
#12141 = EDGE_CURVE ( 'NONE', #12417, #54676, #28381, .T. ) ;
#12142 = CARTESIAN_POINT ( 'NONE',  ( 4.458734124999999437, -8.812499998634406140, -5.460374474430324690E-16 ) ) ;
#12143 = CARTESIAN_POINT ( 'NONE',  ( -2.229367062500000163, 18.27083333469892779, -3.861377020970580443 ) ) ;
#12144 = ADVANCED_FACE ( 'NONE', ( #15329 ), #19190, .T. ) ;
#12145 = CARTESIAN_POINT ( 'NONE',  ( 4.458734125000000326, -53.14583333196773651, 2.574251347313718519 ) ) ;
#12146 = CARTESIAN_POINT ( 'NONE',  ( 3.044556291839386294E-14, 16.87500000273118417, -5.000000000000000000 ) ) ;
#12147 = CARTESIAN_POINT ( 'NONE',  ( -4.458734124999999437, -86.31249999863439371, 0.000000000000000000 ) ) ;
#12148 = CARTESIAN_POINT ( 'NONE',  ( -2.229367062500000163, -8.479166665301073991, -3.861377020970580443 ) ) ;
#12149 = CARTESIAN_POINT ( 'NONE',  ( 2.500000000000002220, -106.5416666639354730, 4.330127018922192761 ) ) ;
#12150 = ORIENTED_EDGE ( 'NONE', *, *, #6001, .T. ) ;
#12151 = CARTESIAN_POINT ( 'NONE',  ( 4.458734124999998549, -34.97916666530107221, -2.574251347313721627 ) ) ;
#12152 = CARTESIAN_POINT ( 'NONE',  ( -58.39396692619412477, -126.6875000013656063, 2.891590998281057701 ) ) ;
#12153 = CARTESIAN_POINT ( 'NONE',  ( 2.229367062499998831, -77.64583333196773651, -3.861377020970580887 ) ) ;
#12154 = CARTESIAN_POINT ( 'NONE',  ( -3.535250795749689387E-16, -110.1249999972687874, -5.773502691896257311 ) ) ;
#12155 = ADVANCED_FACE ( 'NONE', ( #38803 ), #58442, .T. ) ;
#12156 = CARTESIAN_POINT ( 'NONE',  ( 4.458734124999999437, -149.6250000013655779, -1.846868145590734978 ) ) ;
#12157 = CARTESIAN_POINT ( 'NONE',  ( 2.229367062499998831, 22.35416666803225993, -3.861377020970580887 ) ) ;
#12158 = CARTESIAN_POINT ( 'NONE',  ( 1.975475456537005874E-15, -53.74999999999999289, 5.000000000000000000 ) ) ;
#12159 = CARTESIAN_POINT ( 'NONE',  ( -3.535533905932738641, -145.5000000027311842, 3.535533905932737309 ) ) ;
#12160 = CARTESIAN_POINT ( 'NONE',  ( -3.152548672688508926E-16, -84.81249999863439371, -5.148502694627439702 ) ) ;
#12161 = CARTESIAN_POINT ( 'NONE',  ( 2.500000000000002220, -66.66666666666667140, 4.330127018922192761 ) ) ;
#12162 = CARTESIAN_POINT ( 'NONE',  ( 5.000000000000000888, -72.45833333060213022, 2.886751345948126879 ) ) ;
#12163 = CARTESIAN_POINT ( 'NONE',  ( -4.999999999999999112, 17.20833333606451987, 2.886751345948131764 ) ) ;
#12164 = VERTEX_POINT ( 'NONE', #48154 ) ;
#12165 = CARTESIAN_POINT ( 'NONE',  ( -4.999999999999998224, -61.79166666393547303, 2.886751345948131764 ) ) ;
#12166 = AXIS2_PLACEMENT_3D ( 'NONE', #9106, #54442, #53482 ) ;
#12167 = CARTESIAN_POINT ( 'NONE',  ( -1.339745962155613146, 28.20534180126148271, 5.000000000000000000 ) ) ;
#12169 = CARTESIAN_POINT ( 'NONE',  ( 2.499999999999998668, -21.33333333333333570, -4.330127018922193649 ) ) ;
#12168 = CARTESIAN_POINT ( 'NONE',  ( -4.999999999999998224, -106.7916666639354730, 2.886751345948131764 ) ) ;
#12170 = CARTESIAN_POINT ( 'NONE',  ( -3.152548672688508926E-16, -29.56249999863440436, -5.148502694627439702 ) ) ;
#12171 = VECTOR ( 'NONE', #40648, 1000.000000000000000 ) ;
#12172 = CARTESIAN_POINT ( 'NONE',  ( 2.229367062499998831, -85.64583333196773651, -3.861377020970580887 ) ) ;
#12173 =( BOUNDED_CURVE ( )  B_SPLINE_CURVE ( 2, ( #30370, #5944, #25550, #45170, #1137, #14468, #33463, #53087, #9023 ),
 .UNSPECIFIED., .F., .F. ) 
 B_SPLINE_CURVE_WITH_KNOTS ( ( 3, 2, 2, 2, 3 ),
 ( 0.9232142857142857650, 0.9238095238095238582, 0.9250000000000000444, 0.9261904761904762307, 0.9267857142857143238 ),
 .UNSPECIFIED. ) 
 CURVE ( )  GEOMETRIC_REPRESENTATION_ITEM ( )  RATIONAL_B_SPLINE_CURVE ( ( 0.9330127018922194093, 0.9330127018922194093, 1.000000000000000000, 0.8660254037844387076, 1.000000000000000000, 0.8660254037844387076, 1.000000000000000000, 0.9330127018922194093, 0.9330127018922194093 ) ) 
 REPRESENTATION_ITEM ( '' )  );
#12174 = CARTESIAN_POINT ( 'NONE',  ( -5.000000000000000000, -30.95833333060214443, -2.886751345948128211 ) ) ;
#12175 = ADVANCED_FACE ( 'NONE', ( #33992 ), #53613, .T. ) ;
#12177 = EDGE_LOOP ( 'NONE', ( #31316, #49850, #8534, #19262 ) ) ;
#12176 = CARTESIAN_POINT ( 'NONE',  ( -2.229367062499996610, -54.14583333196773651, 3.861377020970582219 ) ) ;
#12178 = DIRECTION ( 'NONE',  ( -0.000000000000000000, 1.000000000000000000, -0.000000000000000000 ) ) ;
#12179 = B_SPLINE_CURVE_WITH_KNOTS ( 'NONE', 3,
 ( #45509, #1472, #60324, #16250, #20110, #50658, #11725, #1794 ),
 .UNSPECIFIED., .F., .F.,
 ( 4, 2, 2, 4 ),
 ( 0.006061689441712453386, 0.007174127271521678166, 0.008286565101330902947, 0.01051144076094935251 ),
 .UNSPECIFIED. ) ;
#12181 = VERTEX_POINT ( 'NONE', #4717 ) ;
#12180 = CARTESIAN_POINT ( 'NONE',  ( -3.152548672688508926E-16, -5.812499998634404363, -5.148502694627439702 ) ) ;
#12182 = CARTESIAN_POINT ( 'NONE',  ( -2.499999999999996447, -73.83333333333332860, 4.330127018922195425 ) ) ;
#12183 = CARTESIAN_POINT ( 'NONE',  ( -52.10840900171896806, -139.1875000013656347, 3.393966926194110556 ) ) ;
#12184 = CARTESIAN_POINT ( 'NONE',  ( -2.229367062499996610, -52.39583333196773651, 3.861377020970582219 ) ) ;
#12185 = CARTESIAN_POINT ( 'NONE',  ( -2.500000000000000444, -0.04166666393548221214, -4.330127018922193649 ) ) ;
#12186 = CARTESIAN_POINT ( 'NONE',  ( -2.499999999999996447, -75.70833333060214443, 4.330127018922195425 ) ) ;
#12187 = CARTESIAN_POINT ( 'NONE',  ( 1.975475456537005874E-15, -53.62499999726880162, 5.000000000000000000 ) ) ;
#12188 = CARTESIAN_POINT ( 'NONE',  ( -49.85088928181150436, -149.5625000000000284, -1.666127454062680702 ) ) ;
#12189 = CARTESIAN_POINT ( 'NONE',  ( -2.229367062499996610, -18.39583333196774007, 3.861377020970582219 ) ) ;
#12190 = CARTESIAN_POINT ( 'NONE',  ( 4.458734124999999437, -50.06249999863440792, -5.460374474430324690E-16 ) ) ;
#12191 =( BOUNDED_CURVE ( )  B_SPLINE_CURVE ( 2, ( #2410, #13560, #40674, #42500, #21713, #31027, #18056, #60319, #50978 ),
 .UNSPECIFIED., .F., .F. ) 
 B_SPLINE_CURVE_WITH_KNOTS ( ( 3, 2, 2, 2, 3 ),
 ( 0.7053571428571429047, 0.7059523809523809978, 0.7071428571428571841, 0.7083333333333333703, 0.7089285714285714635 ),
 .UNSPECIFIED. ) 
 CURVE ( )  GEOMETRIC_REPRESENTATION_ITEM ( )  RATIONAL_B_SPLINE_CURVE ( ( 0.9330127018922194093, 0.9330127018922194093, 1.000000000000000000, 0.8660254037844387076, 1.000000000000000000, 0.8660254037844387076, 1.000000000000000000, 0.9330127018922194093, 0.9330127018922194093 ) ) 
 REPRESENTATION_ITEM ( '' )  );
#12192 = CARTESIAN_POINT ( 'NONE',  ( 5.000000000000000000, 22.58333333333333215, -2.886751345948130876 ) ) ;
#12193 = CARTESIAN_POINT ( 'NONE',  ( -3.152801135295367985, -140.8125000013655779, 3.152801135295367096 ) ) ;
#12194 = CARTESIAN_POINT ( 'NONE',  ( -4.458734124999998549, -101.4791666653010651, 2.574251347313722516 ) ) ;
#12195 = ORIENTED_EDGE ( 'NONE', *, *, #15269, .T. ) ;
#12196 = CARTESIAN_POINT ( 'NONE',  ( -50.70258187064364108, -154.3750000013656063, 2.196230717870141014 ) ) ;
#12197 = CARTESIAN_POINT ( 'NONE',  ( -55.39835681537999790, -142.0000000027312126, 4.984105922594378235 ) ) ;
#12198 = CARTESIAN_POINT ( 'NONE',  ( -6.972266317189433020E-16, 18.74999999999999645, -5.000000000000000000 ) ) ;
#12199 = EDGE_CURVE ( 'NONE', #19063, #50378, #34965, .T. ) ;
#12200 = CARTESIAN_POINT ( 'NONE',  ( -3.152548672688508926E-16, -3.562499998634408360, -5.148502694627439702 ) ) ;
#12201 = CARTESIAN_POINT ( 'NONE',  ( -3.152548672688508926E-16, -95.81249999863442213, -5.148502694627439702 ) ) ;
#12202 = EDGE_CURVE ( 'NONE', #34735, #55556, #28008, .T. ) ;
#12203 = EDGE_CURVE ( 'NONE', #44569, #58717, #40717, .T. ) ;
#12204 = CARTESIAN_POINT ( 'NONE',  ( -4.458734125000001214, -147.1250000013656063, 1.846868145590734089 ) ) ;
#12205 = CARTESIAN_POINT ( 'NONE',  ( -2.229367062500000163, -23.72916666530107577, -3.861377020970580443 ) ) ;
#12206 = CARTESIAN_POINT ( 'NONE',  ( 5.000000000000000888, -46.58333333333334991, 2.886751345948126879 ) ) ;
#12207 = CARTESIAN_POINT ( 'NONE',  ( -57.89159099828107458, -142.6875000013656063, -3.393966926194107447 ) ) ;
#12208 = CARTESIAN_POINT ( 'NONE',  ( 2.229367062499998831, -60.89583333196774362, -3.861377020970580887 ) ) ;
#12209 = CARTESIAN_POINT ( 'NONE',  ( 1.975475456537005874E-15, -83.62499999726878741, 5.000000000000000000 ) ) ;
#12210 = CARTESIAN_POINT ( 'NONE',  ( -10.12668159690567649, 1.256356190803088863E-15, -9.999999999999998224 ) ) ;
#12211 = CARTESIAN_POINT ( 'NONE',  ( 3.152801135295366208, -143.5625000013655779, 3.152801135295367985 ) ) ;
#12212 = AXIS2_PLACEMENT_3D ( 'NONE', #27509, #47139, #41985 ) ;
#12213 = CARTESIAN_POINT ( 'NONE',  ( 2.229367062500001939, 9.770833334698927786, 3.861377020970579999 ) ) ;
#12214 = ORIENTED_EDGE ( 'NONE', *, *, #49250, .T. ) ;
#12215 = CARTESIAN_POINT ( 'NONE',  ( -2.500000000000000444, -81.16666666666667140, -4.330127018922193649 ) ) ;
#12216 = CARTESIAN_POINT ( 'NONE',  ( -3.535533905932738641, -144.3750000000000000, 3.535533905932737309 ) ) ;
#12218 = CARTESIAN_POINT ( 'NONE',  ( -2.229367062499996610, -27.14583333196774007, 3.861377020970582219 ) ) ;
#12217 = CARTESIAN_POINT ( 'NONE',  ( -5.000000000000000000, -85.08333333333332860, -2.886751345948128211 ) ) ;
#12219 = AXIS2_PLACEMENT_3D ( 'NONE', #37660, #29251, #53085 ) ;
#12221 = ADVANCED_FACE ( 'NONE', ( #1198 ), #25619, .T. ) ;
#12220 = CYLINDRICAL_SURFACE ( 'NONE', #62235, 5.000000000000000000 ) ;
#12222 = CARTESIAN_POINT ( 'NONE',  ( 1.339745962155615144, -79.58034179853028434, 4.999999999999999112 ) ) ;
#12223 = CARTESIAN_POINT ( 'NONE',  ( -54.64476657466781973, -143.8125000013656063, -4.444560631937228834 ) ) ;
#12224 = CARTESIAN_POINT ( 'NONE',  ( -2.500000000000000444, -48.04166666393547303, -4.330127018922193649 ) ) ;
#12225 = CYLINDRICAL_SURFACE ( 'NONE', #12845, 5.000000000000000000 ) ;
#12226 = CARTESIAN_POINT ( 'NONE',  ( -2.229367062500000163, 7.520833334698929562, -3.861377020970580443 ) ) ;
#12227 = CARTESIAN_POINT ( 'NONE',  ( 2.500000000000002220, -56.54166666393548013, 4.330127018922192761 ) ) ;
#12228 = EDGE_CURVE ( 'NONE', #11847, #10332, #41527, .T. ) ;
#12229 = CARTESIAN_POINT ( 'NONE',  ( 1.339745962155602488, 21.29465819873852084, 5.000000000000007105 ) ) ;
#12230 = CARTESIAN_POINT ( 'NONE',  ( -4.458734124999999437, 7.687500001365594748, 0.000000000000000000 ) ) ;
#12231 = CARTESIAN_POINT ( 'NONE',  ( -4.458734124999999437, -68.39583333196773651, -2.574251347313719407 ) ) ;
#12232 = CARTESIAN_POINT ( 'NONE',  ( 2.229367062499998831, -20.89583333196774007, -3.861377020970580887 ) ) ;
#12233 = CARTESIAN_POINT ( 'NONE',  ( -2.500000000000000444, -3.166666666666664742, -4.330127018922193649 ) ) ;
#12234 = CARTESIAN_POINT ( 'NONE',  ( -1.846868145590734756, -161.1250000013656063, -4.458734125000000326 ) ) ;
#12235 = CARTESIAN_POINT ( 'NONE',  ( 1.975475456537005874E-15, -85.75000000000000000, 5.000000000000000000 ) ) ;
#12236 = CARTESIAN_POINT ( 'NONE',  ( 4.458734124999998549, -62.72916666530106511, -2.574251347313721627 ) ) ;
#12237 = CARTESIAN_POINT ( 'NONE',  ( 1.060575238724906964E-15, -94.62499999726881583, 5.773502691896257311 ) ) ;
#12238 = VECTOR ( 'NONE', #9138, 1000.000000000000000 ) ;
#12239 = LINE ( 'NONE', #7423, #42877 ) ;
#12240 = CARTESIAN_POINT ( 'NONE',  ( 4.458734124999998549, -35.72916666530107221, -2.574251347313721627 ) ) ;
#12241 = CARTESIAN_POINT ( 'NONE',  ( 5.000000000000000000, -51.29166666393547303, -2.886751345948130876 ) ) ;
#12242 = CARTESIAN_POINT ( 'NONE',  ( -3.152548672688508926E-16, -65.81249999863440792, -5.148502694627439702 ) ) ;
#12243 = CARTESIAN_POINT ( 'NONE',  ( 1.060575238724906964E-15, -46.75000000000000000, 5.773502691896257311 ) ) ;
#12244 = CARTESIAN_POINT ( 'NONE',  ( -6.972266317189433020E-16, -41.24999999999998579, -5.000000000000000000 ) ) ;
#12245 = CARTESIAN_POINT ( 'NONE',  ( -5.000000000000000000, 16.00000000000000000, 0.000000000000000000 ) ) ;
#12246 = VERTEX_POINT ( 'NONE', #31071 ) ;
#12247 = CARTESIAN_POINT ( 'NONE',  ( 4.458734124999998549, -105.7291666653010651, -2.574251347313721627 ) ) ;
#12248 = CARTESIAN_POINT ( 'NONE',  ( 9.457646018065525792E-16, -3.312499998634407472, 5.148502694627439702 ) ) ;
#12249 =( BOUNDED_CURVE ( )  B_SPLINE_CURVE ( 2, ( #27513, #47451, #22067, #51660, #46823, #41659, #2767, #61629, #17563 ),
 .UNSPECIFIED., .F., .F. ) 
 B_SPLINE_CURVE_WITH_KNOTS ( ( 3, 2, 2, 2, 3 ),
 ( 0.4196428571428571508, 0.4202380952380952439, 0.4214285714285714302, 0.4226190476190476164, 0.4232142857142857095 ),
 .UNSPECIFIED. ) 
 CURVE ( )  GEOMETRIC_REPRESENTATION_ITEM ( )  RATIONAL_B_SPLINE_CURVE ( ( 0.9330127018922194093, 0.9330127018922194093, 1.000000000000000000, 0.8660254037844387076, 1.000000000000000000, 0.8660254037844387076, 1.000000000000000000, 0.9330127018922194093, 0.9330127018922194093 ) ) 
 REPRESENTATION_ITEM ( '' )  );
#12250 = CARTESIAN_POINT ( 'NONE',  ( 1.060575238724906964E-15, -9.750000000000001776, 5.773502691896257311 ) ) ;
#12251 = CARTESIAN_POINT ( 'NONE',  ( 4.458734124999999437, -69.81249999863439371, -5.460374474430324690E-16 ) ) ;
#12252 = CARTESIAN_POINT ( 'NONE',  ( -1.339745962155613812, -6.205341801261478274, -5.000000000000000000 ) ) ;
#12253 = CARTESIAN_POINT ( 'NONE',  ( 1.060575238724906964E-15, -11.62499999726881761, 5.773502691896257311 ) ) ;
#12255 = ORIENTED_EDGE ( 'NONE', *, *, #49558, .F. ) ;
#12254 = CARTESIAN_POINT ( 'NONE',  ( 2.229367062500001939, -40.97916666530107221, 3.861377020970579999 ) ) ;
#12256 = CARTESIAN_POINT ( 'NONE',  ( -5.000000000000000000, 29.91666666666666430, -2.886751345948128211 ) ) ;
#12258 = EDGE_LOOP ( 'NONE', ( #32755, #24926, #5046, #37631, #62958, #34712 ) ) ;
#12257 = CARTESIAN_POINT ( 'NONE',  ( -2.229367062500000163, 11.27083333469892601, -3.861377020970580443 ) ) ;
#12259 = DIRECTION ( 'NONE',  ( -1.000000000000000000, 0.000000000000000000, 0.000000000000000000 ) ) ;
#12260 = CARTESIAN_POINT ( 'NONE',  ( -5.000000000000000000, -54.99999999999999289, 0.000000000000000000 ) ) ;
#12261 = CARTESIAN_POINT ( 'NONE',  ( 4.458734124999999437, -161.7500000013655495, 1.846868145590737864 ) ) ;
#12262 = CARTESIAN_POINT ( 'NONE',  ( 2.229367062500001939, -37.22916666530107221, 3.861377020970579999 ) ) ;
#12263 = MECHANICAL_DESIGN_GEOMETRIC_PRESENTATION_REPRESENTATION (  '', ( #24551 ), #49208 ) ;
#12264 = CARTESIAN_POINT ( 'NONE',  ( -5.000000000000000000, -35.00000000000000000, 0.000000000000000000 ) ) ;
#12265 = CARTESIAN_POINT ( 'NONE',  ( -2.229367062500000163, -78.47916666530106511, -3.861377020970580443 ) ) ;
#12266 = CARTESIAN_POINT ( 'NONE',  ( -5.000000000000000888, -169.4375000000000284, 2.071067811865474617 ) ) ;
#12267 = CARTESIAN_POINT ( 'NONE',  ( 9.457646018065525792E-16, -86.06249999863439371, 5.148502694627439702 ) ) ;
#12268 = VECTOR ( 'NONE', #2962, 1000.000000000000000 ) ;
#12269 = CARTESIAN_POINT ( 'NONE',  ( -59.44456063193725015, -133.8125000013656063, -0.3552334253322034230 ) ) ;
#12270 = CARTESIAN_POINT ( 'NONE',  ( 2.229367062500001939, -0.2291666653010705768, 3.861377020970579999 ) ) ;
#12271 = CARTESIAN_POINT ( 'NONE',  ( -4.458734124999998549, -36.47916666530107221, 2.574251347313722516 ) ) ;
#12272 = CARTESIAN_POINT ( 'NONE',  ( 1.339745962155615144, -16.58034179853029499, 4.999999999999999112 ) ) ;
#12273 = CARTESIAN_POINT ( 'NONE',  ( 9.457646018065525792E-16, -80.31249999863440792, 5.148502694627439702 ) ) ;
#12274 = CARTESIAN_POINT ( 'NONE',  ( -2.500000000000000000, 7.216878364870324525, -7.063244554130001518 ) ) ;
#12275 = VERTEX_POINT ( 'NONE', #11133 ) ;
#12276 = DIRECTION ( 'NONE',  ( -0.000000000000000000, 1.000000000000000000, -0.000000000000000000 ) ) ;
#12277 = CARTESIAN_POINT ( 'NONE',  ( 3.535533905932738197, -151.8750000000000000, -3.535533905932738197 ) ) ;
#12278 = CARTESIAN_POINT ( 'NONE',  ( -4.458734124999998549, -71.47916666530107932, 2.574251347313722516 ) ) ;
#12279 = CARTESIAN_POINT ( 'NONE',  ( 2.229367062499998831, -10.89583333196773829, -3.861377020970580887 ) ) ;
#12280 = ORIENTED_EDGE ( 'NONE', *, *, #54650, .F. ) ;
#12281 = LINE ( 'NONE', #62126, #16356 ) ;
#12282 = EDGE_CURVE ( 'NONE', #18224, #50232, #48103, .T. ) ;
#12283 = CARTESIAN_POINT ( 'NONE',  ( 1.975475456537005874E-15, -83.74999999999998579, 5.000000000000000000 ) ) ;
#12284 = CARTESIAN_POINT ( 'NONE',  ( -2.229367062500000163, -4.729166665301071326, -3.861377020970580443 ) ) ;
#12285 = CARTESIAN_POINT ( 'NONE',  ( -51.75738570946856498, -146.8750000027312126, 3.805975901505576964 ) ) ;
#12286 = CARTESIAN_POINT ( 'NONE',  ( -4.458734124999999437, 7.604166668032259935, -2.574251347313719407 ) ) ;
#12287 = CARTESIAN_POINT ( 'NONE',  ( 1.975475456537005874E-15, -75.74999999999998579, 5.000000000000000000 ) ) ;
#12288 = CARTESIAN_POINT ( 'NONE',  ( 1.846868145590736310, -156.6250000013655779, 4.458734124999997661 ) ) ;
#12289 = ADVANCED_FACE ( 'NONE', ( #50058 ), #44919, .T. ) ;
#12290 = CARTESIAN_POINT ( 'NONE',  ( 4.458734124999999437, 23.93750000136559564, -5.460374474430324690E-16 ) ) ;
#12291 = ORIENTED_EDGE ( 'NONE', *, *, #53534, .F. ) ;
#12292 = CARTESIAN_POINT ( 'NONE',  ( -4.458734124999997661, -88.22916666530107932, 2.574251347313722516 ) ) ;
#12293 = CARTESIAN_POINT ( 'NONE',  ( 4.458734124999999437, -1.812499998634406584, -5.460374474430324690E-16 ) ) ;
#12294 = EDGE_CURVE ( 'NONE', #58440, #6256, #35267, .T. ) ;
#12296 = EDGE_CURVE ( 'NONE', #36130, #47006, #30759, .T. ) ;
#12295 = DIRECTION ( 'NONE',  ( -0.000000000000000000, 1.000000000000000000, -0.000000000000000000 ) ) ;
#12297 = CARTESIAN_POINT ( 'NONE',  ( 5.000000000000000000, -32.37499999726880873, -6.123233995736766282E-16 ) ) ;
#12298 = CARTESIAN_POINT ( 'NONE',  ( -2.480964764533239819E-13, -59.75000000000000711, 5.000000000000000000 ) ) ;
#12299 = CARTESIAN_POINT ( 'NONE',  ( 4.458734124999999437, 25.18750000136559208, -5.460374474430324690E-16 ) ) ;
#12300 = CARTESIAN_POINT ( 'NONE',  ( -6.972266317189433020E-16, -7.249999999999998224, -5.000000000000000000 ) ) ;
#12301 = CARTESIAN_POINT ( 'NONE',  ( 2.500000000000002220, -82.54166666393547303, 4.330127018922192761 ) ) ;
#12302 = EDGE_CURVE ( 'NONE', #7607, #24077, #54688, .T. ) ;
#12303 = CARTESIAN_POINT ( 'NONE',  ( 2.229367062499998831, -50.64583333196772941, -3.861377020970580887 ) ) ;
#12304 = CARTESIAN_POINT ( 'NONE',  ( -4.458734124999999437, -39.64583333196773651, -2.574251347313719407 ) ) ;
#12305 = CARTESIAN_POINT ( 'NONE',  ( 4.458734124999998549, -0.9791666653010712151, -2.574251347313721627 ) ) ;
#12306 = CARTESIAN_POINT ( 'NONE',  ( -52.10840900171896806, -152.1875000013656063, 3.393966926194110556 ) ) ;
#12307 = CARTESIAN_POINT ( 'NONE',  ( 5.000000000000000888, -160.0625000027312410, -2.071067811865475505 ) ) ;
#12308 = CARTESIAN_POINT ( 'NONE',  ( 5.000000000000000000, 17.50000000000000000, -6.123233995736766282E-16 ) ) ;
#12309 = ADVANCED_FACE ( 'NONE', ( #31712 ), #3093, .T. ) ;
#12310 = CARTESIAN_POINT ( 'NONE',  ( -3.535533905932737309, -141.7500000027311842, -3.535533905932738197 ) ) ;
#12311 = LINE ( 'NONE', #16496, #38727 ) ;
#12312 = AXIS2_PLACEMENT_3D ( 'NONE', #31139, #17301, #41102 ) ;
#12313 = CARTESIAN_POINT ( 'NONE',  ( 9.457646018065525792E-16, -43.06249999863440081, 5.148502694627439702 ) ) ;
#12314 = CARTESIAN_POINT ( 'NONE',  ( -5.000000000000000000, -79.87499999726881583, 0.000000000000000000 ) ) ;
#12315 = CARTESIAN_POINT ( 'NONE',  ( -50.55543936806279248, -139.3125000013656063, 0.3552334253322060320 ) ) ;
#12316 = DIRECTION ( 'NONE',  ( 0.000000000000000000, 0.000000000000000000, 1.000000000000000000 ) ) ;
#12317 = EDGE_CURVE ( 'NONE', #40520, #49284, #4165, .T. ) ;
#12318 = CARTESIAN_POINT ( 'NONE',  ( -2.499999999999996447, -87.83333333333332860, 4.330127018922195425 ) ) ;
#12319 = CARTESIAN_POINT ( 'NONE',  ( 4.458734124999999437, -85.06249999863439371, -5.460374474430324690E-16 ) ) ;
#12320 = CARTESIAN_POINT ( 'NONE',  ( 3.152801135295366208, -159.8125000013656063, 3.152801135295367985 ) ) ;
#12321 = CARTESIAN_POINT ( 'NONE',  ( 2.500000000000002220, -33.66666666666666430, 4.330127018922192761 ) ) ;
#12322 = CARTESIAN_POINT ( 'NONE',  ( -3.152801135295367985, -141.8125000013655779, 3.152801135295367096 ) ) ;
#12323 = ORIENTED_EDGE ( 'NONE', *, *, #5099, .T. ) ;
#12324 = CARTESIAN_POINT ( 'NONE',  ( -4.458734124999998549, 19.52083333469893134, 2.574251347313722516 ) ) ;
#12325 = ORIENTED_EDGE ( 'NONE', *, *, #59513, .T. ) ;
#12326 = CARTESIAN_POINT ( 'NONE',  ( 4.458734124999999437, -92.81249999863440792, -5.460374474430324690E-16 ) ) ;
#12327 = CARTESIAN_POINT ( 'NONE',  ( -2.229367062499996610, 15.60416666803225993, 3.861377020970582219 ) ) ;
#12328 = CARTESIAN_POINT ( 'NONE',  ( 2.499999999999998668, 16.79166666939785202, -4.330127018922193649 ) ) ;
#12329 = CARTESIAN_POINT ( 'NONE',  ( 5.000000000000000000, -16.41666666666667140, -2.886751345948130876 ) ) ;
#12330 = CARTESIAN_POINT ( 'NONE',  ( 2.500000000000002220, 9.333333333333332149, 4.330127018922192761 ) ) ;
#12331 = CARTESIAN_POINT ( 'NONE',  ( -3.152548672688508926E-16, -54.56249999863439371, -5.148502694627439702 ) ) ;
#12332 = CARTESIAN_POINT ( 'NONE',  ( 7.908230272950877549, -3.123266379887881250, -7.776722524729575703 ) ) ;
#12333 = CARTESIAN_POINT ( 'NONE',  ( -52.80376928212989185, -136.1250000013656063, -4.297418129356378458 ) ) ;
#12334 = CARTESIAN_POINT ( 'NONE',  ( 0.000000000000000000, -120.0000000000000000, 5.000000000000000000 ) ) ;
#12335 = CARTESIAN_POINT ( 'NONE',  ( 2.500000000000002220, -1.666666666666663410, 4.330127018922192761 ) ) ;
#12336 = CARTESIAN_POINT ( 'NONE',  ( -4.999999999999998224, -24.79166666393548368, 2.886751345948131764 ) ) ;
#12337 = CARTESIAN_POINT ( 'NONE',  ( 2.499999999999998668, -38.33333333333332860, -4.330127018922193649 ) ) ;
#12338 = CARTESIAN_POINT ( 'NONE',  ( 1.975475456537005874E-15, -96.75000000000000000, 5.000000000000000000 ) ) ;
#12340 = CARTESIAN_POINT ( 'NONE',  ( 4.458734124999999437, -12.06249999863440081, -5.460374474430324690E-16 ) ) ;
#12339 = CARTESIAN_POINT ( 'NONE',  ( 1.975475456537005874E-15, 14.25000000000000000, 5.000000000000000000 ) ) ;
#12341 = CARTESIAN_POINT ( 'NONE',  ( 4.458734124999998549, -66.72916666530106511, -2.574251347313721627 ) ) ;
#12342 = CARTESIAN_POINT ( 'NONE',  ( -3.152801135295367096, -152.3125000013655779, -3.152801135295367541 ) ) ;
#12343 = CARTESIAN_POINT ( 'NONE',  ( -4.458734124999998549, -69.22916666530107932, 2.574251347313722516 ) ) ;
#12344 = CARTESIAN_POINT ( 'NONE',  ( -52.80376928212989185, -149.1250000013656063, -4.297418129356379346 ) ) ;
#12345 = CARTESIAN_POINT ( 'NONE',  ( -4.458734124999998549, -19.47916666530107221, 2.574251347313722516 ) ) ;
#12346 = CARTESIAN_POINT ( 'NONE',  ( -2.500000000000000444, -60.04166666393547303, -4.330127018922193649 ) ) ;
#12347 = ORIENTED_EDGE ( 'NONE', *, *, #26834, .F. ) ;
#12348 = CYLINDRICAL_SURFACE ( 'NONE', #22060, 5.000000000000000000 ) ;
#12349 = ORIENTED_EDGE ( 'NONE', *, *, #36892, .F. ) ;
#12350 = CARTESIAN_POINT ( 'NONE',  ( -2.229367062499996610, -63.39583333196774362, 3.861377020970582219 ) ) ;
#12351 = CARTESIAN_POINT ( 'NONE',  ( 2.071067811865349828, -149.3125000027311842, 5.000000000000126121 ) ) ;
#12352 = CARTESIAN_POINT ( 'NONE',  ( -3.152801135295367985, -151.8125000013655779, 3.152801135295367096 ) ) ;
#12353 = ORIENTED_EDGE ( 'NONE', *, *, #31046, .T. ) ;
#12354 = CARTESIAN_POINT ( 'NONE',  ( 1.975475456537005874E-15, -46.74999999999999289, 5.000000000000000000 ) ) ;
#12355 = CARTESIAN_POINT ( 'NONE',  ( -49.85088928181150436, -127.5625000000000284, -1.666127454062680702 ) ) ;
#12356 = VECTOR ( 'NONE', #2047, 1000.000000000000114 ) ;
#12357 = CARTESIAN_POINT ( 'NONE',  ( 2.229367062499998831, -50.89583333196772941, -3.861377020970580887 ) ) ;
#12358 = ORIENTED_EDGE ( 'NONE', *, *, #25126, .F. ) ;
#12359 = AXIS2_PLACEMENT_3D ( 'NONE', #38319, #13868, #33491 ) ;
#12360 = CARTESIAN_POINT ( 'NONE',  ( 2.229367062500001939, 8.020833334698926009, 3.861377020970579999 ) ) ;
#12361 = CARTESIAN_POINT ( 'NONE',  ( -4.458734124999999437, 25.60416666803225993, -2.574251347313719407 ) ) ;
#12362 = CARTESIAN_POINT ( 'NONE',  ( -59.59170313451811296, -149.5000000013655779, 1.485763867205729394 ) ) ;
#12363 = CARTESIAN_POINT ( 'NONE',  ( 2.493747252781420335E-13, -78.12499999726881583, -5.000000000000000000 ) ) ;
#12364 = CARTESIAN_POINT ( 'NONE',  ( 1.846868145590735200, -169.2500000013655779, -4.458734124999999437 ) ) ;
#12365 = ORIENTED_EDGE ( 'NONE', *, *, #4005, .T. ) ;
#12366 = CARTESIAN_POINT ( 'NONE',  ( 4.458734125000000326, -69.89583333196773651, 2.574251347313718519 ) ) ;
#12367 = CARTESIAN_POINT ( 'NONE',  ( 3.061616997868383141E-16, -148.8750000027312126, -5.000000000000000000 ) ) ;
#12368 = CARTESIAN_POINT ( 'NONE',  ( -4.458734124999998549, 12.77083333469892601, 2.574251347313722516 ) ) ;
#12369 = VECTOR ( 'NONE', #49528, 1000.000000000000000 ) ;
#12370 =( BOUNDED_CURVE ( )  B_SPLINE_CURVE ( 2, ( #60625, #15266, #1139, #24920, #1454, #35851, #10119, #40017, #15594 ),
 .UNSPECIFIED., .F., .F. ) 
 B_SPLINE_CURVE_WITH_KNOTS ( ( 3, 2, 2, 2, 3 ),
 ( 0.2583333333333335813, 0.2625000000000002331, 0.2666666666666668850, 0.2708333333333335369, 0.2750000000000002442 ),
 .UNSPECIFIED. ) 
 CURVE ( )  GEOMETRIC_REPRESENTATION_ITEM ( )  RATIONAL_B_SPLINE_CURVE ( ( 0.9999999999999958922, 0.9238795325112908463, 1.000000000000000000, 0.9238795325112867385, 1.000000000000000000, 0.9238795325112867385, 1.000000000000000000, 0.9238795325112826307, 1.000000000000003997 ) ) 
 REPRESENTATION_ITEM ( '' )  );
#12371 = LINE ( 'NONE', #28196, #17224 ) ;
#12372 = CARTESIAN_POINT ( 'NONE',  ( 2.229367062500001939, -55.22916666530107221, 3.861377020970579999 ) ) ;
#12373 = CARTESIAN_POINT ( 'NONE',  ( 2.500000000000002220, -12.54166666393548013, 4.330127018922192761 ) ) ;
#12374 = CARTESIAN_POINT ( 'NONE',  ( 1.243387493232115550E-13, -9.124999997268817609, -5.000000000000000000 ) ) ;
#12375 = CARTESIAN_POINT ( 'NONE',  ( 5.000000000000000888, -160.9375000000000000, -2.071067811865475505 ) ) ;
#12376 = CARTESIAN_POINT ( 'NONE',  ( 1.975475456537005874E-15, -38.75000000000000000, 5.000000000000000000 ) ) ;
#12377 = CARTESIAN_POINT ( 'NONE',  ( 4.458734125000001214, -32.89583333196774362, 2.574251347313718519 ) ) ;
#12378 = CARTESIAN_POINT ( 'NONE',  ( 9.457646018065525792E-16, -22.31249999863440792, 5.148502694627439702 ) ) ;
#12379 = ORIENTED_EDGE ( 'NONE', *, *, #24306, .T. ) ;
#12380 = CARTESIAN_POINT ( 'NONE',  ( -6.972266317189433020E-16, 17.87500000273118417, -5.000000000000000000 ) ) ;
#12381 = CARTESIAN_POINT ( 'NONE',  ( -4.458734124999999437, -109.3124999986343937, 0.000000000000000000 ) ) ;
#12382 = CARTESIAN_POINT ( 'NONE',  ( 2.071067811865476394, -155.3125000027311842, 5.000000000000000000 ) ) ;
#12383 = ORIENTED_EDGE ( 'NONE', *, *, #35116, .F. ) ;
#12384 = CARTESIAN_POINT ( 'NONE',  ( -4.458734124999998549, -103.4791666653010509, 2.574251347313722516 ) ) ;
#12385 = CARTESIAN_POINT ( 'NONE',  ( 4.458734125000001214, -27.89583333196774007, 2.574251347313718519 ) ) ;
#12386 = CARTESIAN_POINT ( 'NONE',  ( -2.499999999999996447, -62.70833333060214443, 4.330127018922195425 ) ) ;
#12387 = CARTESIAN_POINT ( 'NONE',  ( -55.35523342533222291, -153.5625000013656063, 4.444560631937231499 ) ) ;
#12388 = CARTESIAN_POINT ( 'NONE',  ( 5.000000000000000000, -146.0000000000000284, 0.000000000000000000 ) ) ;
#12389 = CARTESIAN_POINT ( 'NONE',  ( 4.458734124999999437, -30.81249999863440436, -5.460374474430324690E-16 ) ) ;
#12390 = CARTESIAN_POINT ( 'NONE',  ( 2.229367062499998831, -67.89583333196773651, -3.861377020970580887 ) ) ;
#12391 = CARTESIAN_POINT ( 'NONE',  ( 5.000000000000000000, 8.583333333333332149, -2.886751345948130876 ) ) ;
#12392 = CARTESIAN_POINT ( 'NONE',  ( -2.229367062500000163, -22.47916666530107221, -3.861377020970580443 ) ) ;
#12393 = CARTESIAN_POINT ( 'NONE',  ( 1.339745962155615144, -5.580341798530291442, 4.999999999999999112 ) ) ;
#12394 = CARTESIAN_POINT ( 'NONE',  ( -3.535250795749689387E-16, -16.25000000000000000, -5.773502691896257311 ) ) ;
#12395 = CARTESIAN_POINT ( 'NONE',  ( 4.458734124999999437, -153.5000000013656063, 1.846868145590737864 ) ) ;
#12396 = ORIENTED_EDGE ( 'NONE', *, *, #6693, .T. ) ;
#12397 = AXIS2_PLACEMENT_3D ( 'NONE', #34496, #49311, #34191 ) ;
#12398 = CARTESIAN_POINT ( 'NONE',  ( 2.071067811865349828, -150.1875000000000284, 5.000000000000126121 ) ) ;
#12399 = CARTESIAN_POINT ( 'NONE',  ( 9.457646018065525792E-16, -53.31249999863440792, 5.148502694627439702 ) ) ;
#12400 = CARTESIAN_POINT ( 'NONE',  ( 2.500000000000002220, -58.54166666393548013, 4.330127018922192761 ) ) ;
#12401 = CARTESIAN_POINT ( 'NONE',  ( -2.499999999999996447, -0.8333333333333317050, 4.330127018922195425 ) ) ;
#12402 = CARTESIAN_POINT ( 'NONE',  ( -3.535250795749689387E-16, 22.75000000000000000, -5.773502691896257311 ) ) ;
#12403 = AXIS2_PLACEMENT_3D ( 'NONE', #59218, #29935, #5501 ) ;
#12404 = CARTESIAN_POINT ( 'NONE',  ( 5.000000000000000888, -76.45833333060215864, 2.886751345948126879 ) ) ;
#12405 = CARTESIAN_POINT ( 'NONE',  ( -2.229367062499996610, -1.145833331967736957, 3.861377020970582219 ) ) ;
#12406 = CARTESIAN_POINT ( 'NONE',  ( -5.000000000000000888, -160.6875000027311842, -2.071067811865475949 ) ) ;
#12407 = DIRECTION ( 'NONE',  ( 0.000000000000000000, 1.000000000000000000, 0.000000000000000000 ) ) ;
#12408 = CARTESIAN_POINT ( 'NONE',  ( -2.229367062500000163, 15.27083333469892779, -3.861377020970580443 ) ) ;
#12409 = CARTESIAN_POINT ( 'NONE',  ( 2.500000000000002220, 0.4583333360645182042, 4.330127018922192761 ) ) ;
#12410 = ORIENTED_EDGE ( 'NONE', *, *, #56136, .T. ) ;
#12411 = CARTESIAN_POINT ( 'NONE',  ( 1.339745962155612702, -42.29465819873851729, -5.000000000000000000 ) ) ;
#12412 = ORIENTED_EDGE ( 'NONE', *, *, #31527, .F. ) ;
#12413 = CARTESIAN_POINT ( 'NONE',  ( -1.510657702057710340E-15, 27.37500000273118417, 5.000000000000000000 ) ) ;
#12414 = CARTESIAN_POINT ( 'NONE',  ( 4.458734124999999437, -41.81249999863440081, -5.460374474430324690E-16 ) ) ;
#12415 = CARTESIAN_POINT ( 'NONE',  ( -4.458734124999999437, -164.1875000013655779, -5.460374474430324690E-16 ) ) ;
#12416 = CARTESIAN_POINT ( 'NONE',  ( -3.535250795749689387E-16, -45.12499999726880162, -5.773502691896257311 ) ) ;
#12417 = VERTEX_POINT ( 'NONE', #57127 ) ;
#12418 = CARTESIAN_POINT ( 'NONE',  ( -4.458734124999998549, -20.22916666530107221, 2.574251347313722516 ) ) ;
#12419 = ORIENTED_EDGE ( 'NONE', *, *, #14240, .T. ) ;
#12420 =( BOUNDED_CURVE ( )  B_SPLINE_CURVE ( 2, ( #50634, #59979, #54823, #45484, #40656, #44840, #40973, #804, #59656 ),
 .UNSPECIFIED., .F., .F. ) 
 B_SPLINE_CURVE_WITH_KNOTS ( ( 3, 2, 2, 2, 3 ),
 ( 0.4416666666666670404, 0.4458333333333337478, 0.4500000000000003997, 0.4541666666666671071, 0.4583333333333337589 ),
 .UNSPECIFIED. ) 
 CURVE ( )  GEOMETRIC_REPRESENTATION_ITEM ( )  RATIONAL_B_SPLINE_CURVE ( ( 0.9999999999999928946, 0.9238795325112938439, 1.000000000000000000, 0.9238795325112867385, 1.000000000000000000, 0.9238795325112867385, 1.000000000000000000, 0.9238795325112786339, 1.000000000000008216 ) ) 
 REPRESENTATION_ITEM ( '' )  );
#12421 = CARTESIAN_POINT ( 'NONE',  ( 5.000000000000000000, -86.50000000000000000, -6.123233995736766282E-16 ) ) ;
#12422 = CARTESIAN_POINT ( 'NONE',  ( 3.152801135295367541, -166.3125000013656063, -3.152801135295367541 ) ) ;
#12423 =( BOUNDED_CURVE ( )  B_SPLINE_CURVE ( 2, ( #31951, #7835, #27436, #37728, #22950, #47070, #17792, #60922, #37416 ),
 .UNSPECIFIED., .F., .F. ) 
 B_SPLINE_CURVE_WITH_KNOTS ( ( 3, 2, 2, 2, 3 ),
 ( 0.9732142857142856984, 0.9738095238095237915, 0.9749999999999999778, 0.9761904761904761640, 0.9767857142857142572 ),
 .UNSPECIFIED. ) 
 CURVE ( )  GEOMETRIC_REPRESENTATION_ITEM ( )  RATIONAL_B_SPLINE_CURVE ( ( 0.9330127018922194093, 0.9330127018922194093, 1.000000000000000000, 0.8660254037844387076, 1.000000000000000000, 0.8660254037844387076, 1.000000000000000000, 0.9330127018922194093, 0.9330127018922194093 ) ) 
 REPRESENTATION_ITEM ( '' )  );
#12424 = DIRECTION ( 'NONE',  ( -0.000000000000000000, 1.000000000000000000, -0.000000000000000000 ) ) ;
#12425 = CARTESIAN_POINT ( 'NONE',  ( -54.60164318462004474, -136.3750000000000284, -4.984105922594373794 ) ) ;
#12426 = CARTESIAN_POINT ( 'NONE',  ( 4.458734125000001214, -34.14583333196772941, 2.574251347313718519 ) ) ;
#12427 = CARTESIAN_POINT ( 'NONE',  ( -2.071067811865604735, -147.4375000027312410, 4.999999999999872990 ) ) ;
#12428 = ORIENTED_EDGE ( 'NONE', *, *, #47647, .F. ) ;
#12429 = CARTESIAN_POINT ( 'NONE',  ( 2.229367062500001939, -76.97916666530106511, 3.861377020970579999 ) ) ;
#12430 = CARTESIAN_POINT ( 'NONE',  ( 2.229367062499998831, 22.35416666803225993, -3.861377020970580887 ) ) ;
#12431 = CARTESIAN_POINT ( 'NONE',  ( -1.339745962155613812, -54.20534180126147561, -5.000000000000000000 ) ) ;
#12432 = VERTEX_POINT ( 'NONE', #3717 ) ;
#12433 = CARTESIAN_POINT ( 'NONE',  ( -59.44456063193725015, -141.8125000013656063, -0.3552334253322034230 ) ) ;
#12434 = CARTESIAN_POINT ( 'NONE',  ( 4.458734124999999437, -79.06249999863440792, -5.460374474430324690E-16 ) ) ;
#12435 = CARTESIAN_POINT ( 'NONE',  ( -58.80597590150559739, -131.1250000027312126, 3.242614290531460330 ) ) ;
#12436 = CARTESIAN_POINT ( 'NONE',  ( -6.972266317189433020E-16, 22.74999999999999645, -5.000000000000000000 ) ) ;
#12437 = CARTESIAN_POINT ( 'NONE',  ( -5.000000000000000888, -158.5625000027312126, 2.071067811865474617 ) ) ;
#12438 = CARTESIAN_POINT ( 'NONE',  ( -1.127183054612291972E-14, 24.25000000000000000, 4.999999999999999112 ) ) ;
#12439 = CARTESIAN_POINT ( 'NONE',  ( -4.458734124999999437, -54.31249999863440081, 0.000000000000000000 ) ) ;
#12440 = CARTESIAN_POINT ( 'NONE',  ( -4.458734124999999437, -44.31249999863440081, 0.000000000000000000 ) ) ;
#12441 = CARTESIAN_POINT ( 'NONE',  ( -5.000000000000000000, 27.91666666666666430, -2.886751345948128211 ) ) ;
#12442 = CARTESIAN_POINT ( 'NONE',  ( -5.000000000000000000, -105.0000000000000142, 0.000000000000000000 ) ) ;
#12443 = CARTESIAN_POINT ( 'NONE',  ( 3.535533905932738197, -154.0000000027312126, -3.535533905932738197 ) ) ;
#12444 = CARTESIAN_POINT ( 'NONE',  ( -4.458734124999999437, -38.56249999863440081, 0.000000000000000000 ) ) ;
#12445 = CARTESIAN_POINT ( 'NONE',  ( -5.000000000000000000, -0.9583333306021485365, -2.886751345948128211 ) ) ;
#12446 = CARTESIAN_POINT ( 'NONE',  ( 1.339745962155615144, 16.41965820146970501, 4.999999999999999112 ) ) ;
#12447 = CARTESIAN_POINT ( 'NONE',  ( -56.48576386720575471, -126.7500000013655921, -4.591703134518078322 ) ) ;
#12448 =( BOUNDED_CURVE ( )  B_SPLINE_CURVE ( 2, ( #50212, #16122, #1666, #54730, #1037, #59886, #10651, #5838, #25450 ),
 .UNSPECIFIED., .F., .F. ) 
 B_SPLINE_CURVE_WITH_KNOTS ( ( 3, 2, 2, 2, 3 ),
 ( 0.2083333333333335091, 0.2125000000000001610, 0.2166666666666668406, 0.2208333333333335202, 0.2250000000000001998 ),
 .UNSPECIFIED. ) 
 CURVE ( )  GEOMETRIC_REPRESENTATION_ITEM ( )  RATIONAL_B_SPLINE_CURVE ( ( 0.9999999999999970024, 0.9238795325112897361, 1.000000000000000000, 0.9238795325112867385, 1.000000000000000000, 0.9238795325112867385, 1.000000000000000000, 0.9238795325112831858, 1.000000000000003553 ) ) 
 REPRESENTATION_ITEM ( '' )  );
#12449 = CARTESIAN_POINT ( 'NONE',  ( 2.229367062500001939, -78.22916666530106511, 3.861377020970579999 ) ) ;
#12450 = DIRECTION ( 'NONE',  ( 0.000000000000000000, 0.000000000000000000, 1.000000000000000000 ) ) ;
#12451 = CARTESIAN_POINT ( 'NONE',  ( -4.458734124999999437, -104.3958333319677365, -2.574251347313719407 ) ) ;
#12452 = CARTESIAN_POINT ( 'NONE',  ( -2.229367062499996610, -4.395833331967740065, 3.861377020970582219 ) ) ;
#12453 = ORIENTED_EDGE ( 'NONE', *, *, #57893, .F. ) ;
#12454 = CARTESIAN_POINT ( 'NONE',  ( -6.972266317189433020E-16, -58.24999999999999289, -5.000000000000000000 ) ) ;
#12455 = CARTESIAN_POINT ( 'NONE',  ( -2.229367062500000163, -92.47916666530106511, -3.861377020970580443 ) ) ;
#12456 = CARTESIAN_POINT ( 'NONE',  ( -3.535533905932737309, -168.7500000027312126, -3.535533905932738197 ) ) ;
#12457 = CARTESIAN_POINT ( 'NONE',  ( 2.229367062500001939, -87.22916666530107932, 3.861377020970579999 ) ) ;
#12458 = CARTESIAN_POINT ( 'NONE',  ( 4.458734125000000326, 10.85416666803225993, 2.574251347313718519 ) ) ;
#12459 = CARTESIAN_POINT ( 'NONE',  ( 5.000000000000000000, -2.374999997268815388, -6.123233995736766282E-16 ) ) ;
#12460 = CARTESIAN_POINT ( 'NONE',  ( -56.48576386720575471, -134.7500000013656063, -4.591703134518078322 ) ) ;
#12461 = CARTESIAN_POINT ( 'NONE',  ( 4.458734124999998549, -9.729166665301068662, -2.574251347313721627 ) ) ;
#12462 = CARTESIAN_POINT ( 'NONE',  ( 4.458734124999999437, 15.93750000136559564, -5.460374474430324690E-16 ) ) ;
#12463 = CARTESIAN_POINT ( 'NONE',  ( -4.458734124999997661, -55.47916666530106511, 2.574251347313722516 ) ) ;
#12464 = CARTESIAN_POINT ( 'NONE',  ( 2.499999999999998668, -38.20833333060213732, -4.330127018922193649 ) ) ;
#12465 = CARTESIAN_POINT ( 'NONE',  ( -4.999999999999998224, -36.91666666666667140, 2.886751345948131764 ) ) ;
#12466 = CARTESIAN_POINT ( 'NONE',  ( 2.229367062499998831, -11.64583333196774007, -3.861377020970580887 ) ) ;
#12467 = CARTESIAN_POINT ( 'NONE',  ( -4.999999999999998224, -38.91666666666667140, 2.886751345948131764 ) ) ;
#12468 = ORIENTED_EDGE ( 'NONE', *, *, #36971, .T. ) ;
#12469 = CARTESIAN_POINT ( 'NONE',  ( 2.229367062499998831, -36.89583333196773651, -3.861377020970580887 ) ) ;
#12470 =( BOUNDED_CURVE ( )  B_SPLINE_CURVE ( 2, ( #60826, #60509, #60193, #55365, #11280, #1981, #40552, #30256, #50849 ),
 .UNSPECIFIED., .F., .F. ) 
 B_SPLINE_CURVE_WITH_KNOTS ( ( 3, 2, 2, 2, 3 ),
 ( 0.9839285714285714857, 0.9845238095238095788, 0.9857142857142857650, 0.9869047619047619513, 0.9875000000000000444 ),
 .UNSPECIFIED. ) 
 CURVE ( )  GEOMETRIC_REPRESENTATION_ITEM ( )  RATIONAL_B_SPLINE_CURVE ( ( 0.9330127018922194093, 0.9330127018922256266, 1.000000000000000000, 0.8660254037844387076, 1.000000000000000000, 0.8660254037844387076, 1.000000000000000000, 0.9330127018922194093, 0.9330127018922194093 ) ) 
 REPRESENTATION_ITEM ( '' )  );
#12471 = CARTESIAN_POINT ( 'NONE',  ( -54.64476657466781973, -127.0625000013655921, -4.444560631937228834 ) ) ;
#12472 = CARTESIAN_POINT ( 'NONE',  ( 5.000000000000000888, 0.5416666693978527958, 2.886751345948126879 ) ) ;
#12473 = CARTESIAN_POINT ( 'NONE',  ( -2.229367062499996610, -82.14583333196773651, 3.861377020970582219 ) ) ;
#12474 = CARTESIAN_POINT ( 'NONE',  ( -4.458734124999999437, 26.35416666803226349, -2.574251347313719407 ) ) ;
#12475 = CARTESIAN_POINT ( 'NONE',  ( -1.846868145590737420, -149.0000000013656063, 4.458734124999997661 ) ) ;
#12476 = CARTESIAN_POINT ( 'NONE',  ( -4.458734124999999437, 12.68750000136559564, 0.000000000000000000 ) ) ;
#12477 = CARTESIAN_POINT ( 'NONE',  ( -6.972266317189433020E-16, -44.12499999726880162, -5.000000000000000000 ) ) ;
#12478 = CARTESIAN_POINT ( 'NONE',  ( -2.229367062499996610, -85.39583333196773651, 3.861377020970582219 ) ) ;
#12479 = CARTESIAN_POINT ( 'NONE',  ( 5.000000000000000000, -65.50000000000000000, -6.123233995736766282E-16 ) ) ;
#12480 = CARTESIAN_POINT ( 'NONE',  ( 3.061616997868383141E-16, -140.7500000000000000, -5.000000000000000000 ) ) ;
#12481 = CARTESIAN_POINT ( 'NONE',  ( 1.060575238724906964E-15, 20.37500000273119127, 5.773502691896257311 ) ) ;
#12482 = VERTEX_POINT ( 'NONE', #62263 ) ;
#12483 = CARTESIAN_POINT ( 'NONE',  ( 5.000000000000000888, -147.0625000027311842, -2.071067811865475505 ) ) ;
#12484 = CARTESIAN_POINT ( 'NONE',  ( 2.499999999999998668, 7.666666666666665186, -4.330127018922193649 ) ) ;
#12486 = CARTESIAN_POINT ( 'NONE',  ( 5.000000000000000000, -25.41666666666666430, -2.886751345948129988 ) ) ;
#12485 = CARTESIAN_POINT ( 'NONE',  ( -5.000000000000000000, -72.00000000000000000, 0.000000000000000000 ) ) ;
#12487 = CARTESIAN_POINT ( 'NONE',  ( -4.458734124999998549, -26.22916666530106866, 2.574251347313722516 ) ) ;
#12488 = EDGE_CURVE ( 'NONE', #1596, #42874, #17312, .T. ) ;
#12489 = CARTESIAN_POINT ( 'NONE',  ( 4.458734124999998549, -89.72916666530106511, -2.574251347313721627 ) ) ;
#12490 = CARTESIAN_POINT ( 'NONE',  ( 5.000000000000000000, -29.37499999726881228, -6.123233995736766282E-16 ) ) ;
#12492 = ORIENTED_EDGE ( 'NONE', *, *, #28311, .T. ) ;
#12491 = CARTESIAN_POINT ( 'NONE',  ( -4.458734124999999437, -58.39583333196774362, -2.574251347313719407 ) ) ;
#12493 = CARTESIAN_POINT ( 'NONE',  ( 0.000000000000000000, -170.0000000000000000, 0.000000000000000000 ) ) ;
#12495 = ORIENTED_EDGE ( 'NONE', *, *, #51869, .T. ) ;
#12494 = CARTESIAN_POINT ( 'NONE',  ( 9.457646018065525792E-16, -10.31249999863440614, 5.148502694627439702 ) ) ;
#12496 = CARTESIAN_POINT ( 'NONE',  ( -5.000000000000000000, -74.08333333333332860, -2.886751345948128211 ) ) ;
#12497 = CARTESIAN_POINT ( 'NONE',  ( -52.10840900171896806, -138.1875000013656347, 3.393966926194110556 ) ) ;
#12498 = CARTESIAN_POINT ( 'NONE',  ( -3.152548672688508926E-16, -49.81249999863440081, -5.148502694627439702 ) ) ;
#12499 = CARTESIAN_POINT ( 'NONE',  ( 2.499999999999998668, -78.20833333060214443, -4.330127018922193649 ) ) ;
#12501 = ORIENTED_EDGE ( 'NONE', *, *, #26313, .F. ) ;
#12500 = CARTESIAN_POINT ( 'NONE',  ( -1.339745962155610925, -21.66965819600733312, 5.000000000000000000 ) ) ;
#12502 = CARTESIAN_POINT ( 'NONE',  ( -50.01589407740564042, -149.6250000000000284, 0.3983568153799778022 ) ) ;
#12503 = CARTESIAN_POINT ( 'NONE',  ( -2.229367062500000163, -15.72916666530107399, -3.861377020970580443 ) ) ;
#12504 = CARTESIAN_POINT ( 'NONE',  ( 4.458734124999999437, -58.06249999863440081, -5.460374474430324690E-16 ) ) ;
#12505 = EDGE_CURVE ( 'NONE', #14472, #50070, #63335, .T. ) ;
#12506 = CARTESIAN_POINT ( 'NONE',  ( -51.75738570946856498, -150.7500000000000284, 3.805975901505576964 ) ) ;
#12507 = CARTESIAN_POINT ( 'NONE',  ( 3.152801135295367541, -169.5625000013656063, -3.152801135295367541 ) ) ;
#12508 = EDGE_CURVE ( 'NONE', #52130, #63378, #10348, .T. ) ;
#12509 = CARTESIAN_POINT ( 'NONE',  ( 2.229367062500001939, -97.22916666530105090, 3.861377020970579999 ) ) ;
#12510 = DIRECTION ( 'NONE',  ( -0.000000000000000000, 1.000000000000000000, -0.000000000000000000 ) ) ;
#12511 = ORIENTED_EDGE ( 'NONE', *, *, #12734, .T. ) ;
#12512 = CARTESIAN_POINT ( 'NONE',  ( -52.10840900171896806, -153.4375000013656063, 3.393966926194110556 ) ) ;
#12513 = CARTESIAN_POINT ( 'NONE',  ( -60.14911071818854538, -143.1875000027312126, 1.666127454062681368 ) ) ;
#12514 = CARTESIAN_POINT ( 'NONE',  ( -5.000000000000000000, -12.87499999726881050, 0.000000000000000000 ) ) ;
#12515 = CARTESIAN_POINT ( 'NONE',  ( -2.229367062500000163, -7.479166665301073991, -3.861377020970580443 ) ) ;
#12516 = CARTESIAN_POINT ( 'NONE',  ( 4.458734125000000326, -98.14583333196773651, 2.574251347313718519 ) ) ;
#12517 = CARTESIAN_POINT ( 'NONE',  ( -1.846868145590734756, -148.3750000013655779, -4.458734125000000326 ) ) ;
#12518 = CARTESIAN_POINT ( 'NONE',  ( -4.458734124999999437, -21.64583333196774362, -2.574251347313719407 ) ) ;
#12519 = DIRECTION ( 'NONE',  ( -0.000000000000000000, 1.000000000000000000, -0.000000000000000000 ) ) ;
#12520 = CARTESIAN_POINT ( 'NONE',  ( -59.44456063193725015, -136.5625000013656063, -0.3552334253322034230 ) ) ;
#12521 = CARTESIAN_POINT ( 'NONE',  ( -3.152548672688508926E-16, -60.81249999863440081, -5.148502694627439702 ) ) ;
#12522 = CARTESIAN_POINT ( 'NONE',  ( 7.549006887134058985, 4.358421158401185380, -7.700127545397291939 ) ) ;
#12523 = CARTESIAN_POINT ( 'NONE',  ( 2.352174619736673744, -7.302225387959338399, -7.450218641350605076 ) ) ;
#12524 = CARTESIAN_POINT ( 'NONE',  ( 1.846868145590736310, -145.6250000013655779, 4.458734124999997661 ) ) ;
#12525 = CARTESIAN_POINT ( 'NONE',  ( -3.152548672688508926E-16, 10.18750000136559208, -5.148502694627439702 ) ) ;
#12526 = VERTEX_POINT ( 'NONE', #2458 ) ;
#12527 = CARTESIAN_POINT ( 'NONE',  ( -1.339745962155613812, -53.08034179853029144, -5.000000000000000000 ) ) ;
#12528 = DIRECTION ( 'NONE',  ( -0.000000000000000000, 1.000000000000000000, -0.000000000000000000 ) ) ;
#12530 = CARTESIAN_POINT ( 'NONE',  ( -2.229367062500000163, -25.47916666530106866, -3.861377020970580443 ) ) ;
#12529 = CARTESIAN_POINT ( 'NONE',  ( 2.499999999999998668, -88.33333333333332860, -4.330127018922193649 ) ) ;
#12531 = CARTESIAN_POINT ( 'NONE',  ( 0.000000000000000000, -170.0000000000000000, 0.000000000000000000 ) ) ;
#12532 = CARTESIAN_POINT ( 'NONE',  ( 4.458734125000001214, -73.14583333196773651, 2.574251347313718519 ) ) ;
#12533 = DIRECTION ( 'NONE',  ( 0.000000000000000000, 0.000000000000000000, 1.000000000000000000 ) ) ;
#12534 = CARTESIAN_POINT ( 'NONE',  ( -50.70258187064364108, -146.1250000013656063, 2.196230717870141014 ) ) ;
#12535 = ADVANCED_FACE ( 'NONE', ( #61632 ), #51971, .T. ) ;
#12536 = CARTESIAN_POINT ( 'NONE',  ( 1.975475456537005874E-15, -24.74999999999999645, 5.000000000000000000 ) ) ;
#12537 = CARTESIAN_POINT ( 'NONE',  ( -3.152548672688508926E-16, 10.43750000136559386, -5.148502694627439702 ) ) ;
#12538 = CARTESIAN_POINT ( 'NONE',  ( -4.458734124999999437, 8.604166668032261711, -2.574251347313719407 ) ) ;
#12539 = CARTESIAN_POINT ( 'NONE',  ( -4.458734124999999437, -71.31249999863439371, 0.000000000000000000 ) ) ;
#12540 = CARTESIAN_POINT ( 'NONE',  ( 2.229367062500001939, -18.22916666530106866, 3.861377020970579999 ) ) ;
#12541 = CARTESIAN_POINT ( 'NONE',  ( 2.500000000000002220, 0.3333333333333348136, 4.330127018922192761 ) ) ;
#12542 = CARTESIAN_POINT ( 'NONE',  ( -4.458734124999999437, -158.9375000013655779, -5.460374474430324690E-16 ) ) ;
#12543 = CARTESIAN_POINT ( 'NONE',  ( 5.000000000000000000, 23.50000000000000000, -6.123233995736766282E-16 ) ) ;
#12544 = APPLICATION_CONTEXT ( 'automotive_design' ) ;
#12545 = CARTESIAN_POINT ( 'NONE',  ( -4.458734124999998549, -66.22916666530107932, 2.574251347313722516 ) ) ;
#12546 = CARTESIAN_POINT ( 'NONE',  ( 2.499999999999998668, -100.2083333306021444, -4.330127018922193649 ) ) ;
#12547 =( BOUNDED_CURVE ( )  B_SPLINE_CURVE ( 2, ( #45001, #45640, #15420, #16049, #59812, #20240, #40802, #50785, #55305 ),
 .UNSPECIFIED., .F., .F. ) 
 B_SPLINE_CURVE_WITH_KNOTS ( ( 3, 2, 2, 2, 3 ),
 ( 0.8604166666666667185, 0.8611111111111111605, 0.8625000000000000444, 0.8638888888888889284, 0.8645833333333333703 ),
 .UNSPECIFIED. ) 
 CURVE ( )  GEOMETRIC_REPRESENTATION_ITEM ( )  RATIONAL_B_SPLINE_CURVE ( ( 0.9330127018922194093, 0.9330127018922194093, 1.000000000000000000, 0.8660254037844387076, 1.000000000000000000, 0.8660254037844387076, 1.000000000000000000, 0.9330127018922194093, 0.9330127018922194093 ) ) 
 REPRESENTATION_ITEM ( '' )  );
#12548 = CARTESIAN_POINT ( 'NONE',  ( -1.339745962155610925, -35.79465819873851729, 5.000000000000000000 ) ) ;
#12549 = CARTESIAN_POINT ( 'NONE',  ( 4.458734124999998549, -39.72916666530107221, -2.574251347313721627 ) ) ;
#12550 = CARTESIAN_POINT ( 'NONE',  ( -6.972266317189433020E-16, 19.87500000273118417, -5.000000000000000000 ) ) ;
#12551 = CARTESIAN_POINT ( 'NONE',  ( 4.458734124999998549, -66.97916666530106511, -2.574251347313721627 ) ) ;
#12552 = CARTESIAN_POINT ( 'NONE',  ( -2.499999999999996447, -49.83333333333332860, 4.330127018922195425 ) ) ;
#12553 = CARTESIAN_POINT ( 'NONE',  ( -1.339745962155610259, 26.79465819873851729, -5.000000000000002665 ) ) ;
#12554 = CARTESIAN_POINT ( 'NONE',  ( -4.999999999999998224, 16.08333333333333215, 2.886751345948131764 ) ) ;
#12555 = VERTEX_POINT ( 'NONE', #42308 ) ;
#12556 = CARTESIAN_POINT ( 'NONE',  ( 2.499999999999998668, -94.33333333333332860, -4.330127018922193649 ) ) ;
#12557 = CARTESIAN_POINT ( 'NONE',  ( -4.999999999999998224, -67.79166666393547303, 2.886751345948131764 ) ) ;
#12558 = CARTESIAN_POINT ( 'NONE',  ( 5.000000000000000888, -8.583333333333330373, 2.886751345948126879 ) ) ;
#12559 = EDGE_CURVE ( 'NONE', #54893, #57064, #27831, .T. ) ;
#12560 = CARTESIAN_POINT ( 'NONE',  ( 2.229367062499998831, -71.64583333196773651, -3.861377020970580887 ) ) ;
#12562 = DIRECTION ( 'NONE',  ( -0.6592143633790360502, -0.5000000000000125455, 0.5616372700549346897 ) ) ;
#12561 =( BOUNDED_CURVE ( )  B_SPLINE_CURVE ( 2, ( #39211, #14452, #57601, #58836, #14765, #33762, #13528, #34383, #18961, #9941, #29556, #33147, #9006, #52762, #8691, #13830, #49190, #9314, #3875, #58208, #4191, #24430, #14135, #4806, #53381, #23494, #48551, #314, #23804, #58528, #63051, #43406, #62737, #9629, #19278, #5128, #12306, #28928, #4490, #44032, #37968, #24118, #18659, #57906, #34074, #48862, #633, #970, #15423, #44673, #5445, #25710, #15737, #39526, #54657, #39845, #20243, #59488, #35354, #35045, #10580, #60131, #30519, #19912, #30192, #16052, #45004, #54975, #49821, #45322, #5765, #59164, #25383, #54339, #1289, #20572, #15096, #40178, #59815, #10272, #10904, #50142, #55308, #6097, #34713, #29876, #20887, #35680, #40490, #49506, #25063, #14344, #23701, #19484, #8894, #24000, #20128, #9516, #52956, #24310, #19801, #5337, #29759, #48127, #39409, #49393, #63564, #28820, #34584, #4078, #48441, #58726, #24955, #39728, #29123, #33654, #203, #28509, #59048, #4381, #14652, #39097, #34271, #49066, #43298, #53897, #44560, #54216, #9822, #62934, #29433, #53272, #18848, #14976, #43917, #10154, #9207, #5013, #517, #38469, #14025, #13716, #58095, #33340, #24632, #43602, #63246, #44239, #19160, #38778, #4688, #58417, #33966, #53586, #48746, #49710, #45844, #15941, #26224, #40376, #10467, #16580, #55187, #15301, #41013, #60017, #36200, #60656, #34923, #10793, #30079, #5655, #35243, #11737, #30732, #25267, #35563, #6936, #59695, #31355, #25906, #55821, #16265, #55513, #40692, #26547, #15626, #50996, #21088, #46167, #44888, #54862, #50028, #54544, #849, #11428, #2129, #1806, #59367, #11107, #21730, #31045, #20452, #40051, #50354, #6301, #30405, #5986, #25591, #45204, #1171, #21410, #20771, #45524, #1485, #60337, #35883, #50670, #6611, #16695, #17327, #12811, #61088, #26980, #17947, #46599, #55938, #51745, #41122, #56258, #52378, #41753, #21526, #56575, #52061, #8315, #57212, #36626, #61718, #41439, #36949, #17010, #3177, #36314, #12183, #27293, #62030, #45956, #61403, #2239, #32432, #60770, #7999, #31797, #46918, #13131, #1921, #32109, #27602, #51429, #12497, #22797, #2860, #31471, #22482, #21843, #11853, #47235, #7687, #7372, #42077, #2543, #22159, #51112, #17647, #37263, #37572, #42390, #56891, #32750, #7049, #26662, #46280, #39136, #28227, #43954, #58132, #43026, #14063, #52990, #23423, #47843, #29162, #24041, #47537, #48164, #38210, #62666, #57835, #63284, #8931, #13754, #8619, #23101, #9557, #28544, #14379, #43643, #13446, #62348, #4117, #23737, #18269 ),
 .UNSPECIFIED., .F., .F. ) 
 B_SPLINE_CURVE_WITH_KNOTS ( ( 3, 2, 2, 2, 2, 2, 2, 2, 2, 2, 2, 2, 2, 2, 2, 2, 2, 2, 2, 2, 2, 2, 2, 2, 2, 2, 2, 2, 2, 2, 2, 2, 2, 2, 2, 2, 2, 2, 2, 2, 2, 2, 2, 2, 2, 2, 2, 2, 2, 2, 2, 2, 2, 2, 2, 2, 2, 2, 2, 2, 2, 2, 2, 2, 2, 2, 2, 2, 2, 2, 2, 2, 2, 2, 2, 2, 2, 2, 2, 2, 2, 2, 2, 2, 2, 2, 2, 2, 2, 2, 2, 2, 2, 2, 2, 2, 2, 2, 2, 2, 2, 2, 2, 2, 2, 2, 2, 2, 2, 2, 2, 2, 2, 2, 2, 2, 2, 2, 2, 2, 2, 2, 2, 2, 2, 2, 2, 2, 2, 2, 2, 2, 2, 2, 2, 2, 2, 2, 2, 2, 2, 2, 2, 2, 2, 2, 2, 2, 2, 2, 2, 2, 2, 2, 2, 2, 3 ),
 ( 0.000000000000000000, 0.004166666666666666609, 0.008333333333333333218, 0.01250000000000000243, 0.01666666666666666644, 0.02083333333333333218, 0.02500000000000000486, 0.02916666666666666713, 0.03333333333333333287, 0.03749999999999999861, 0.04166666666666666435, 0.04583333333333333010, 0.05000000000000000971, 0.05416666666666666852, 0.05833333333333333426, 0.06250000000000000000, 0.06666666666666666574, 0.07083333333333333148, 0.07499999999999999722, 0.07916666666666666297, 0.08333333333333332871, 0.08749999999999999445, 0.09166666666666666019, 0.09583333333333333981, 0.1000000000000000194, 0.1041666666666666713, 0.1083333333333333370, 0.1124999999999999889, 0.1166666666666666685, 0.1208333333333333204, 0.1250000000000000000, 0.1291666666666666796, 0.1333333333333333315, 0.1375000000000000111, 0.1416666666666666630, 0.1458333333333333426, 0.1499999999999999944, 0.1541666666666666741, 0.1583333333333333259, 0.1625000000000000056, 0.1666666666666666574, 0.1708333333333333370, 0.1749999999999999889, 0.1791666666666666685, 0.1833333333333333204, 0.1875000000000000000, 0.1916666666666666796, 0.1958333333333333315, 0.2000000000000000389, 0.2041666666666666907, 0.2083333333333333426, 0.2124999999999999944, 0.2166666666666666741, 0.2208333333333333259, 0.2249999999999999778, 0.2291666666666666574, 0.2333333333333333370, 0.2374999999999999889, 0.2416666666666666408, 0.2458333333333332926, 0.2500000000000000000, 0.2541666666666666519, 0.2583333333333333592, 0.2625000000000000111, 0.2666666666666666630, 0.2708333333333333148, 0.2750000000000000222, 0.2791666666666666741, 0.2833333333333333259, 0.2874999999999999778, 0.2916666666666666852, 0.2958333333333333370, 0.2999999999999999889, 0.3041666666666666408, 0.3083333333333333481, 0.3125000000000000000, 0.3166666666666666519, 0.3208333333333333592, 0.3250000000000000111, 0.3291666666666666630, 0.3333333333333333148, 0.3375000000000000222, 0.3416666666666666741, 0.3458333333333333259, 0.3499999999999999778, 0.3541666666666666852, 0.3583333333333333370, 0.3624999999999999889, 0.3666666666666666408, 0.3708333333333333481, 0.3750000000000000000, 0.3791666666666666519, 0.3833333333333333592, 0.3875000000000000111, 0.3916666666666666630, 0.3958333333333333148, 0.4000000000000000777, 0.4041666666666667296, 0.4083333333333333814, 0.4125000000000000333, 0.4166666666666666852, 0.4208333333333333370, 0.4249999999999999889, 0.4291666666666666408, 0.4333333333333333481, 0.4375000000000000000, 0.4416666666666666519, 0.4458333333333333037, 0.4499999999999999556, 0.4541666666666666630, 0.4583333333333333148, 0.4625000000000000222, 0.4666666666666666741, 0.4708333333333333259, 0.4749999999999999778, 0.4791666666666666297, 0.4833333333333332815, 0.4874999999999999334, 0.4916666666666665853, 0.4958333333333333481, 0.5000000000000000000, 0.5041666666666666519, 0.5083333333333333037, 0.5124999999999999556, 0.5166666666666667185, 0.5208333333333333703, 0.5250000000000000222, 0.5291666666666666741, 0.5333333333333333259, 0.5374999999999999778, 0.5416666666666666297, 0.5458333333333332815, 0.5500000000000000444, 0.5541666666666666963, 0.5583333333333333481, 0.5625000000000000000, 0.5666666666666666519, 0.5708333333333333037, 0.5749999999999999556, 0.5791666666666667185, 0.5833333333333333703, 0.5875000000000000222, 0.5916666666666666741, 0.5958333333333333259, 0.5999999999999999778, 0.6041666666666666297, 0.6083333333333332815, 0.6125000000000000444, 0.6166666666666666963, 0.6208333333333333481, 0.6250000000000000000, 0.6291666666666666519, 0.6333333333333333037, 0.6374999999999999556, 0.6416666666666667185, 0.6458333333333333703, 0.6479166667104350186 ),
 .UNSPECIFIED. ) 
 CURVE ( )  GEOMETRIC_REPRESENTATION_ITEM ( )  RATIONAL_B_SPLINE_CURVE ( ( 1.000000000000000000, 0.9238795325112867385, 1.000000000000000000, 0.9238795325112867385, 1.000000000000000000, 0.9238795325112867385, 1.000000000000000000, 0.9238795325112867385, 1.000000000000000000, 0.9238795325112867385, 1.000000000000000000, 0.9238795325112867385, 1.000000000000000000, 0.9238795325112867385, 1.000000000000000000, 0.9238795325112867385, 1.000000000000000000, 0.9238795325112867385, 1.000000000000000000, 0.9238795325112867385, 1.000000000000000000, 0.9238795325112867385, 1.000000000000000000, 0.9238795325112867385, 1.000000000000000000, 0.9238795325112867385, 1.000000000000000000, 0.9238795325112867385, 1.000000000000000000, 0.9238795325112867385, 1.000000000000000000, 0.9238795325112867385, 1.000000000000000000, 0.9238795325112867385, 1.000000000000000000, 0.9238795325112867385, 1.000000000000000000, 0.9238795325112867385, 1.000000000000000000, 0.9238795325112867385, 1.000000000000000000, 0.9238795325112867385, 1.000000000000000000, 0.9238795325112867385, 1.000000000000000000, 0.9238795325112867385, 1.000000000000000000, 0.9238795325112867385, 1.000000000000000000, 0.9238795325112867385, 1.000000000000000000, 0.9238795325112867385, 1.000000000000000000, 0.9238795325112867385, 1.000000000000000000, 0.9238795325112867385, 1.000000000000000000, 0.9238795325112867385, 1.000000000000000000, 0.9238795325112867385, 1.000000000000000000, 0.9238795325112867385, 1.000000000000000000, 0.9238795325112867385, 1.000000000000000000, 0.9238795325112867385, 1.000000000000000000, 0.9238795325112867385, 1.000000000000000000, 0.9238795325112867385, 1.000000000000000000, 0.9238795325112867385, 1.000000000000000000, 0.9238795325112867385, 1.000000000000000000, 0.9238795325112867385, 1.000000000000000000, 0.9238795325112867385, 1.000000000000000000, 0.9238795325112867385, 1.000000000000000000, 0.9238795325112867385, 1.000000000000000000, 0.9238795325112867385, 1.000000000000000000, 0.9238795325112867385, 1.000000000000000000, 0.9238795325112867385, 1.000000000000000000, 0.9238795325112867385, 1.000000000000000000, 0.9238795325112867385, 1.000000000000000000, 0.9238795325112867385, 1.000000000000000000, 0.9238795325112867385, 1.000000000000000000, 0.9238795325112867385, 1.000000000000000000, 0.9238795325112867385, 1.000000000000000000, 0.9238795325112867385, 1.000000000000000000, 0.9238795325112867385, 1.000000000000000000, 0.9238795325112867385, 1.000000000000000000, 0.9238795325112867385, 1.000000000000000000, 0.9238795325112867385, 1.000000000000000000, 0.9238795325112867385, 1.000000000000000000, 0.9238795325112867385, 1.000000000000000000, 0.9238795325112867385, 1.000000000000000000, 0.9238795325112867385, 1.000000000000000000, 0.9238795325112867385, 1.000000000000000000, 0.9238795325112867385, 1.000000000000000000, 0.9238795325112867385, 1.000000000000000000, 0.9238795325112867385, 1.000000000000000000, 0.9238795325112867385, 1.000000000000000000, 0.9238795325112867385, 1.000000000000000000, 0.9238795325112867385, 1.000000000000000000, 0.9238795325112867385, 1.000000000000000000, 0.9238795325112867385, 1.000000000000000000, 0.9238795325112867385, 1.000000000000000000, 0.9238795325112867385, 1.000000000000000000, 0.9238795325112867385, 1.000000000000000000, 0.9238795325112867385, 1.000000000000000000, 0.9238795325112867385, 1.000000000000000000, 0.9238795325112867385, 1.000000000000000000, 0.9238795325112867385, 1.000000000000000000, 0.9238795325112867385, 1.000000000000000000, 0.9238795325112867385, 1.000000000000000000, 0.9238795325112867385, 1.000000000000000000, 0.9238795325112867385, 1.000000000000000000, 0.9238795325112867385, 1.000000000000000000, 0.9238795325112867385, 1.000000000000000000, 0.9238795325112867385, 1.000000000000000000, 0.9238795325112867385, 1.000000000000000000, 0.9238795325112867385, 1.000000000000000000, 0.9238795325112867385, 1.000000000000000000, 0.9238795325112867385, 1.000000000000000000, 0.9238795325112867385, 1.000000000000000000, 0.9238795325112867385, 1.000000000000000000, 0.9238795325112867385, 1.000000000000000000, 0.9238795325112867385, 1.000000000000000000, 0.9238795325112867385, 1.000000000000000000, 0.9238795325112867385, 1.000000000000000000, 0.9238795325112867385, 1.000000000000000000, 0.9238795325112867385, 1.000000000000000000, 0.9238795325112867385, 1.000000000000000000, 0.9238795325112867385, 1.000000000000000000, 0.9238795325112867385, 1.000000000000000000, 0.9238795325112867385, 1.000000000000000000, 0.9238795325112867385, 1.000000000000000000, 0.9238795325112867385, 1.000000000000000000, 0.9238795325112867385, 1.000000000000000000, 0.9238795325112867385, 1.000000000000000000, 0.9238795325112867385, 1.000000000000000000, 0.9238795325112867385, 1.000000000000000000, 0.9238795325112867385, 1.000000000000000000, 0.9238795325112867385, 1.000000000000000000, 0.9238795325112867385, 1.000000000000000000, 0.9238795325112867385, 1.000000000000000000, 0.9238795325112867385, 1.000000000000000000, 0.9238795325112867385, 1.000000000000000000, 0.9238795325112867385, 1.000000000000000000, 0.9238795325112867385, 1.000000000000000000, 0.9238795325112867385, 1.000000000000000000, 0.9238795325112867385, 1.000000000000000000, 0.9238795325112867385, 1.000000000000000000, 0.9238795325112867385, 1.000000000000000000, 0.9238795325112867385, 1.000000000000000000, 0.9238795325112867385, 1.000000000000000000, 0.9238795325112867385, 1.000000000000000000, 0.9238795325112867385, 1.000000000000000000, 0.9238795325112867385, 1.000000000000000000, 0.9238795325112867385, 1.000000000000000000, 0.9238795325112867385, 1.000000000000000000, 0.9238795325112867385, 1.000000000000000000, 0.9238795325112867385, 1.000000000000000000, 0.9238795325112867385, 1.000000000000000000, 0.9238795325112867385, 1.000000000000000000, 0.9238795325112867385, 1.000000000000000000, 0.9238795325112867385, 1.000000000000000000, 0.9238795325112867385, 1.000000000000000000, 0.9238795325112867385, 1.000000000000000000, 0.9238795325112867385, 1.000000000000000000, 0.9238795325112867385, 1.000000000000000000, 0.9238795325112867385, 1.000000000000000000, 0.9238795325112867385, 1.000000000000000000, 0.9238795325112867385, 1.000000000000000000, 0.9238795325112867385, 1.000000000000000000, 0.9238795325112867385, 1.000000000000000000, 0.9238795325112867385, 1.000000000000000000, 0.9238795325112867385, 1.000000000000000000, 0.9238795325112867385, 1.000000000000000000, 0.9238795325112867385, 1.000000000000000000, 0.9238795325112867385, 1.000000000000000000, 0.9238795325112867385, 1.000000000000000000, 0.9238795325112867385, 1.000000000000000000, 0.9238795325112867385, 1.000000000000000000, 0.9238795325112867385, 1.000000000000000000, 0.9238795325112867385, 1.000000000000000000, 0.9238795325112867385, 1.000000000000000000, 0.9238795325112867385, 1.000000000000000000, 0.9238795325112867385, 1.000000000000000000, 0.9238795325112867385, 1.000000000000000000, 0.9238795325112867385, 1.000000000000000000, 0.9238795325112867385, 1.000000000000000000, 0.9238795325112867385, 1.000000000000000000, 0.9619397654560437605, 0.9619397662556433692 ) ) 
 REPRESENTATION_ITEM ( '' )  );
#12563 = CARTESIAN_POINT ( 'NONE',  ( 2.499999999999998668, -13.20833333060214976, -4.330127018922193649 ) ) ;
#12565 = ORIENTED_EDGE ( 'NONE', *, *, #13014, .F. ) ;
#12564 = CARTESIAN_POINT ( 'NONE',  ( 2.229367062499998831, -41.64583333196773651, -3.861377020970580887 ) ) ;
#12566 = DIRECTION ( 'NONE',  ( -0.000000000000000000, 1.000000000000000000, -0.000000000000000000 ) ) ;
#12568 = ORIENTED_EDGE ( 'NONE', *, *, #62179, .T. ) ;
#12567 = CARTESIAN_POINT ( 'NONE',  ( 2.229367062500001939, 8.770833334698927786, 3.861377020970579999 ) ) ;
#12569 = CARTESIAN_POINT ( 'NONE',  ( -6.972266317189433020E-16, -34.12499999726881583, -5.000000000000000000 ) ) ;
#12570 = CARTESIAN_POINT ( 'NONE',  ( -5.000000000000000000, -58.08333333333332860, -2.886751345948128211 ) ) ;
#12571 = CARTESIAN_POINT ( 'NONE',  ( 4.458734124999999437, -160.6875000013655779, 0.000000000000000000 ) ) ;
#12572 = CARTESIAN_POINT ( 'NONE',  ( -4.458734124999999437, -35.64583333196772941, -2.574251347313719407 ) ) ;
#12573 = DIRECTION ( 'NONE',  ( 0.000000000000000000, 0.000000000000000000, -1.000000000000000000 ) ) ;
#12574 = CARTESIAN_POINT ( 'NONE',  ( -4.458734124999999437, -82.39583333196773651, -2.574251347313719407 ) ) ;
#12575 = CARTESIAN_POINT ( 'NONE',  ( -2.071067811865475061, -164.6875000000000568, -5.000000000000000888 ) ) ;
#12576 = EDGE_CURVE ( 'NONE', #43124, #42363, #16931, .T. ) ;
#12577 = CARTESIAN_POINT ( 'NONE',  ( 2.229367062500001939, -88.97916666530106511, 3.861377020970579999 ) ) ;
#12578 = CARTESIAN_POINT ( 'NONE',  ( -59.59170313451811296, -129.7500000013656063, 1.485763867205729394 ) ) ;
#12579 = CARTESIAN_POINT ( 'NONE',  ( 2.229367062500001939, -1.229166665301071548, 3.861377020970579999 ) ) ;
#12580 = CARTESIAN_POINT ( 'NONE',  ( -4.458734124999999437, -36.64583333196773651, -2.574251347313719407 ) ) ;
#12581 = CARTESIAN_POINT ( 'NONE',  ( 5.000000000000000888, -72.58333333333332860, 2.886751345948126879 ) ) ;
#12582 = EDGE_CURVE ( 'NONE', #23583, #28403, #25565, .T. ) ;
#12583 = CARTESIAN_POINT ( 'NONE',  ( -4.458734124999999437, -82.64583333196772230, -2.574251347313719407 ) ) ;
#12584 = CARTESIAN_POINT ( 'NONE',  ( 2.500000000000002220, 3.333333333333333925, 4.330127018922192761 ) ) ;
#12585 = EDGE_LOOP ( 'NONE', ( #62120, #38181, #52148, #16112 ) ) ;
#12586 = EDGE_CURVE ( 'NONE', #14724, #47799, #62959, .T. ) ;
#12587 = CARTESIAN_POINT ( 'NONE',  ( -55.39835681537999790, -154.0000000027312410, 4.984105922594378235 ) ) ;
#12588 = CARTESIAN_POINT ( 'NONE',  ( -5.000000000000000000, -18.87499999726881583, 0.000000000000000000 ) ) ;
#12589 = CARTESIAN_POINT ( 'NONE',  ( -2.229367062499996610, -69.39583333196773651, 3.861377020970582219 ) ) ;
#12590 = CARTESIAN_POINT ( 'NONE',  ( -4.458734124999999437, -40.39583333196773651, -2.574251347313719407 ) ) ;
#12591 = CARTESIAN_POINT ( 'NONE',  ( -4.458734124999999437, -7.562499998634404363, 0.000000000000000000 ) ) ;
#12592 = ORIENTED_EDGE ( 'NONE', *, *, #5515, .F. ) ;
#12593 = DIRECTION ( 'NONE',  ( -0.000000000000000000, 1.000000000000000000, -0.000000000000000000 ) ) ;
#12594 = CARTESIAN_POINT ( 'NONE',  ( 6.123233995736766282E-16, -170.0000000000000000, -5.000000000000000000 ) ) ;
#12595 = CARTESIAN_POINT ( 'NONE',  ( -4.458734124999999437, -7.645833331967735624, -2.574251347313719407 ) ) ;
#12596 = LINE ( 'NONE', #1147, #44577 ) ;
#12597 = CARTESIAN_POINT ( 'NONE',  ( -4.458734124999998549, 4.770833334698926009, 2.574251347313722516 ) ) ;
#12598 = CARTESIAN_POINT ( 'NONE',  ( -1.339745962155610925, -75.79465819873853150, 5.000000000000000000 ) ) ;
#12599 = CARTESIAN_POINT ( 'NONE',  ( -1.846868145590737420, -156.7500000013656063, 4.458734124999997661 ) ) ;
#12600 = CARTESIAN_POINT ( 'NONE',  ( -2.229367062500000163, 28.27083333469892779, -3.861377020970580443 ) ) ;
#12601 = ORIENTED_EDGE ( 'NONE', *, *, #34737, .T. ) ;
#12602 = CARTESIAN_POINT ( 'NONE',  ( -4.458734124999999437, -88.39583333196773651, -2.574251347313719407 ) ) ;
#12603 = CARTESIAN_POINT ( 'NONE',  ( -2.499999999999996447, -24.83333333333333215, 4.330127018922195425 ) ) ;
#12604 = CARTESIAN_POINT ( 'NONE',  ( -4.458734124999999437, -8.395833331967736513, -2.574251347313719407 ) ) ;
#12605 = EDGE_CURVE ( 'NONE', #15422, #50505, #19437, .T. ) ;
#12606 = CARTESIAN_POINT ( 'NONE',  ( -9.184850993605147944E-16, -166.2500000000000000, 5.000000000000000000 ) ) ;
#12607 = CARTESIAN_POINT ( 'NONE',  ( 1.975475456537005874E-15, -48.74999999999999289, 5.000000000000000000 ) ) ;
#12608 = CARTESIAN_POINT ( 'NONE',  ( 5.000000000000000000, -37.29166666393548013, -2.886751345948129988 ) ) ;
#12609 = CARTESIAN_POINT ( 'NONE',  ( 1.975475456537005874E-15, 8.249999999999998224, 5.000000000000000000 ) ) ;
#12610 = CARTESIAN_POINT ( 'NONE',  ( -3.152548672688508926E-16, 26.43750000136559564, -5.148502694627439702 ) ) ;
#12611 = CARTESIAN_POINT ( 'NONE',  ( -6.972266317189433020E-16, -98.12499999726880162, -5.000000000000000000 ) ) ;
#12612 = CARTESIAN_POINT ( 'NONE',  ( 4.458734124999998549, 25.27083333469892779, -2.574251347313721627 ) ) ;
#12613 = CARTESIAN_POINT ( 'NONE',  ( 9.457646018065525792E-16, -55.06249999863439371, 5.148502694627439702 ) ) ;
#12614 = CARTESIAN_POINT ( 'NONE',  ( 4.458734124999998549, -1.979166665301068662, -2.574251347313721627 ) ) ;
#12615 =( BOUNDED_CURVE ( )  B_SPLINE_CURVE ( 2, ( #31069, #35907, #50693, #5680, #6636, #60039, #44917, #26244, #59393 ),
 .UNSPECIFIED., .F., .F. ) 
 B_SPLINE_CURVE_WITH_KNOTS ( ( 3, 2, 2, 2, 3 ),
 ( 0.2250000000000001998, 0.2291666666666668517, 0.2333333333333335313, 0.2375000000000001832, 0.2416666666666668628 ),
 .UNSPECIFIED. ) 
 CURVE ( )  GEOMETRIC_REPRESENTATION_ITEM ( )  RATIONAL_B_SPLINE_CURVE ( ( 0.9999999999999964473, 0.9238795325112902912, 1.000000000000000000, 0.9238795325112867385, 1.000000000000000000, 0.9238795325112867385, 1.000000000000000000, 0.9238795325112831858, 1.000000000000003553 ) ) 
 REPRESENTATION_ITEM ( '' )  );
#12616 = LINE ( 'NONE', #1718, #53474 ) ;
#12617 = CARTESIAN_POINT ( 'NONE',  ( -5.000000000000000000, 13.99999999999999822, 0.000000000000000000 ) ) ;
#12618 = CARTESIAN_POINT ( 'NONE',  ( -5.000000000000000888, -140.5625000027312410, 2.071067811865474617 ) ) ;
#12619 = CARTESIAN_POINT ( 'NONE',  ( -51.75738570946856498, -144.8750000027312126, 3.805975901505576964 ) ) ;
#12620 = CARTESIAN_POINT ( 'NONE',  ( 4.458734124999998549, -45.72916666530106511, -2.574251347313721627 ) ) ;
#12621 = CARTESIAN_POINT ( 'NONE',  ( 2.499999999999998668, -80.20833333060213022, -4.330127018922193649 ) ) ;
#12622 = CARTESIAN_POINT ( 'NONE',  ( -55.35523342533222291, -140.5625000013656063, 4.444560631937231499 ) ) ;
#12623 = CARTESIAN_POINT ( 'NONE',  ( -6.972266317189433020E-16, -37.12499999726881583, -5.000000000000000000 ) ) ;
#12624 = CARTESIAN_POINT ( 'NONE',  ( 1.339745962155612702, -22.29465819873851729, -5.000000000000000000 ) ) ;
#12625 = CARTESIAN_POINT ( 'NONE',  ( -4.458734124999999437, -86.64583333196773651, -2.574251347313719407 ) ) ;
#12626 = CARTESIAN_POINT ( 'NONE',  ( -1.846868145590737420, -158.0000000013656063, 4.458734124999997661 ) ) ;
#12627 = CARTESIAN_POINT ( 'NONE',  ( -2.500000000000000444, -30.16666666666666785, -4.330127018922193649 ) ) ;
#12628 = VERTEX_POINT ( 'NONE', #44509 ) ;
#12629 = CARTESIAN_POINT ( 'NONE',  ( 4.458734124999998549, 18.02083333469892779, -2.574251347313721627 ) ) ;
#12630 = ORIENTED_EDGE ( 'NONE', *, *, #54153, .T. ) ;
#12631 = CARTESIAN_POINT ( 'NONE',  ( -2.229367062500000163, -96.47916666530105090, -3.861377020970580443 ) ) ;
#12632 = CARTESIAN_POINT ( 'NONE',  ( 4.458734124999998549, 14.02083333469892779, -2.574251347313721627 ) ) ;
#12633 = CARTESIAN_POINT ( 'NONE',  ( -3.535250795749689387E-16, 16.87500000273118417, -5.773502691896257311 ) ) ;
#12634 = CARTESIAN_POINT ( 'NONE',  ( -2.500000000000000444, -60.16666666666665719, -4.330127018922193649 ) ) ;
#12635 = CARTESIAN_POINT ( 'NONE',  ( 5.000000000000000000, 7.500000000000000000, -6.123233995736766282E-16 ) ) ;
#12636 = CARTESIAN_POINT ( 'NONE',  ( 9.457646018065525792E-16, -57.06249999863440081, 5.148502694627439702 ) ) ;
#12637 = CARTESIAN_POINT ( 'NONE',  ( 5.000000000000000888, -61.45833333060214443, 2.886751345948126879 ) ) ;
#12638 = CARTESIAN_POINT ( 'NONE',  ( 2.499999999999998668, -82.33333333333332860, -4.330127018922193649 ) ) ;
#12639 = EDGE_CURVE ( 'NONE', #4656, #61181, #56402, .T. ) ;
#12640 = ADVANCED_FACE ( 'NONE', ( #63513 ), #58678, .T. ) ;
#12641 = DIRECTION ( 'NONE',  ( -0.000000000000000000, 1.000000000000000000, -0.000000000000000000 ) ) ;
#12642 = CARTESIAN_POINT ( 'NONE',  ( 2.499999999999998668, -40.20833333060214443, -4.330127018922193649 ) ) ;
#12643 = CARTESIAN_POINT ( 'NONE',  ( -1.339745962155610925, -12.66965819600733134, 5.000000000000000000 ) ) ;
#12644 = EDGE_CURVE ( 'NONE', #45741, #1619, #58994, .T. ) ;
#12645 = CARTESIAN_POINT ( 'NONE',  ( 2.500000000000002220, -109.6666666666666572, 4.330127018922192761 ) ) ;
#12646 = CARTESIAN_POINT ( 'NONE',  ( 5.000000000000000888, -37.58333333333332860, 2.886751345948126879 ) ) ;
#12647 = DIRECTION ( 'NONE',  ( 0.000000000000000000, 0.000000000000000000, 1.000000000000000000 ) ) ;
#12648 =( BOUNDED_CURVE ( )  B_SPLINE_CURVE ( 2, ( #48062, #43541, #23940, #45059, #29060, #10957, #35412, #23636, #57733 ),
 .UNSPECIFIED., .F., .F. ) 
 B_SPLINE_CURVE_WITH_KNOTS ( ( 3, 2, 2, 2, 3 ),
 ( 0.7696428571428571841, 0.7702380952380952772, 0.7714285714285714635, 0.7726190476190476497, 0.7732142857142857428 ),
 .UNSPECIFIED. ) 
 CURVE ( )  GEOMETRIC_REPRESENTATION_ITEM ( )  RATIONAL_B_SPLINE_CURVE ( ( 0.9330127018922194093, 0.9330127018922194093, 1.000000000000000000, 0.8660254037844387076, 1.000000000000000000, 0.8660254037844387076, 1.000000000000000000, 0.9330127018922194093, 0.9330127018922194093 ) ) 
 REPRESENTATION_ITEM ( '' )  );
#12649 = CARTESIAN_POINT ( 'NONE',  ( -4.458734124999999437, -18.56249999863440792, 0.000000000000000000 ) ) ;
#12650 = CYLINDRICAL_SURFACE ( 'NONE', #41960, 5.000000000000000000 ) ;
#12651 = CARTESIAN_POINT ( 'NONE',  ( 4.458734125000001214, -65.89583333196772230, 2.574251347313718519 ) ) ;
#12652 = CARTESIAN_POINT ( 'NONE',  ( -4.458734125000000326, -149.2500000013655779, -1.846868145590735644 ) ) ;
#12653 = CARTESIAN_POINT ( 'NONE',  ( -3.152548672688508926E-16, -73.56249999863440792, -5.148502694627439702 ) ) ;
#12654 = CARTESIAN_POINT ( 'NONE',  ( -52.10840900171896806, -142.4375000013656063, 3.393966926194110556 ) ) ;
#12655 = EDGE_CURVE ( 'NONE', #26835, #19510, #60905, .T. ) ;
#12656 = CARTESIAN_POINT ( 'NONE',  ( -4.458734124999998549, -20.47916666530107577, 2.574251347313722516 ) ) ;
#12657 = CARTESIAN_POINT ( 'NONE',  ( 1.060575238724906964E-15, -61.62499999726880873, 5.773502691896257311 ) ) ;
#12658 = EDGE_LOOP ( 'NONE', ( #36090, #24682, #30429, #52474 ) ) ;
#12659 = CARTESIAN_POINT ( 'NONE',  ( 3.061616997868383141E-16, -150.7500000000000284, -5.000000000000000000 ) ) ;
#12661 = ORIENTED_EDGE ( 'NONE', *, *, #5968, .T. ) ;
#12660 = EDGE_CURVE ( 'NONE', #3805, #29717, #23511, .T. ) ;
#12662 = CARTESIAN_POINT ( 'NONE',  ( -2.229367062499996610, -67.39583333196773651, 3.861377020970582219 ) ) ;
#12663 = CARTESIAN_POINT ( 'NONE',  ( -6.972266317189433020E-16, -100.2499999999999858, -5.000000000000000000 ) ) ;
#12664 =( NAMED_UNIT ( * ) SI_UNIT ( $, .STERADIAN. ) SOLID_ANGLE_UNIT ( ) );
#12665 = EDGE_CURVE ( 'NONE', #27072, #61565, #16211, .T. ) ;
#12666 = ORIENTED_EDGE ( 'NONE', *, *, #22108, .T. ) ;
#12667 = EDGE_CURVE ( 'NONE', #22959, #26195, #3789, .T. ) ;
#12668 = EDGE_CURVE ( 'NONE', #45244, #49104, #30059, .T. ) ;
#12669 = CARTESIAN_POINT ( 'NONE',  ( -58.24261429053147765, -152.2500000000000284, -3.805975901505573855 ) ) ;
#12670 = CARTESIAN_POINT ( 'NONE',  ( -52.53715891517739323, -127.4375000000000426, -4.819101127000233298 ) ) ;
#12671 = CARTESIAN_POINT ( 'NONE',  ( -6.972266317189433020E-16, -75.12499999726880162, -5.000000000000000000 ) ) ;
#12672 = CARTESIAN_POINT ( 'NONE',  ( -2.229367062499996610, -55.39583333196773651, 3.861377020970582219 ) ) ;
#12673 = VERTEX_POINT ( 'NONE', #15580 ) ;
#12674 = DIRECTION ( 'NONE',  ( -0.000000000000000000, 1.000000000000000000, -0.000000000000000000 ) ) ;
#12675 = CARTESIAN_POINT ( 'NONE',  ( 4.458734125000001214, 11.10416666803225993, 2.574251347313718519 ) ) ;
#12676 = CARTESIAN_POINT ( 'NONE',  ( -2.229367062500000163, 18.52083333469892779, -3.861377020970580443 ) ) ;
#12677 = CARTESIAN_POINT ( 'NONE',  ( -53.51423613279429503, -147.2500000013656063, 4.591703134518082763 ) ) ;
#12678 = CARTESIAN_POINT ( 'NONE',  ( -6.972266317189433020E-16, -108.1249999972688158, -5.000000000000000000 ) ) ;
#12679 = CARTESIAN_POINT ( 'NONE',  ( -1.846868145590737420, -168.7500000013656063, 4.458734124999997661 ) ) ;
#12680 = VERTEX_POINT ( 'NONE', #20725 ) ;
#12681 = CARTESIAN_POINT ( 'NONE',  ( -4.458734124999999437, -71.31249999863439371, 0.000000000000000000 ) ) ;
#12682 = CARTESIAN_POINT ( 'NONE',  ( 2.500000000000002220, -10.54166666393547835, 4.330127018922192761 ) ) ;
#12683 = CARTESIAN_POINT ( 'NONE',  ( -2.229367062499996610, 7.854166668032260823, 3.861377020970582219 ) ) ;
#12684 = CARTESIAN_POINT ( 'NONE',  ( 3.061616997868383141E-16, -139.8750000027312126, -5.000000000000000000 ) ) ;
#12685 = CARTESIAN_POINT ( 'NONE',  ( -2.229367062499996610, -58.39583333196773651, 3.861377020970582219 ) ) ;
#12686 = CARTESIAN_POINT ( 'NONE',  ( -5.000000000000000000, -19.87499999726880873, 0.000000000000000000 ) ) ;
#12687 = CARTESIAN_POINT ( 'NONE',  ( -5.000000000000000000, -100.0000000000000000, 0.000000000000000000 ) ) ;
#12688 = CARTESIAN_POINT ( 'NONE',  ( -1.339745962155610925, -44.66965819600733312, 5.000000000000000000 ) ) ;
#12689 = CARTESIAN_POINT ( 'NONE',  ( 1.339745962155615144, -30.58034179853029499, 4.999999999999999112 ) ) ;
#12690 = CARTESIAN_POINT ( 'NONE',  ( 0.000000000000000000, -120.0000000000000000, 5.000000000000000000 ) ) ;
#12691 = CARTESIAN_POINT ( 'NONE',  ( 4.458734125000001214, -35.89583333196773651, 2.574251347313718519 ) ) ;
#12692 = CARTESIAN_POINT ( 'NONE',  ( -4.458734124999999437, -23.56249999863440436, 0.000000000000000000 ) ) ;
#12693 = ORIENTED_EDGE ( 'NONE', *, *, #10323, .T. ) ;
#12694 = CARTESIAN_POINT ( 'NONE',  ( -6.972266317189433020E-16, -22.12499999726881228, -5.000000000000000000 ) ) ;
#12695 = CARTESIAN_POINT ( 'NONE',  ( 4.458734124999999437, -108.8124999986343937, -5.460374474430324690E-16 ) ) ;
#12696 = CARTESIAN_POINT ( 'NONE',  ( 3.535533905932738197, -153.0000000027312126, -3.535533905932738197 ) ) ;
#12697 = EDGE_LOOP ( 'NONE', ( #7916, #10036, #16589, #20170 ) ) ;
#12698 = CARTESIAN_POINT ( 'NONE',  ( -3.152548672688508926E-16, -107.8124999986343937, -5.148502694627439702 ) ) ;
#12699 = CARTESIAN_POINT ( 'NONE',  ( 2.229367062500001939, -33.97916666530107221, 3.861377020970579999 ) ) ;
#12700 = CARTESIAN_POINT ( 'NONE',  ( 5.000000000000000000, -64.29166666393547303, -2.886751345948129988 ) ) ;
#12701 = CARTESIAN_POINT ( 'NONE',  ( -52.80376928212989185, -151.1250000013655779, -4.297418129356379346 ) ) ;
#12702 = CARTESIAN_POINT ( 'NONE',  ( -5.000000000000000888, -146.4375000000000000, 2.071067811865474617 ) ) ;
#12703 = CARTESIAN_POINT ( 'NONE',  ( 2.229367062500001939, -29.97916666530107221, 3.861377020970579999 ) ) ;
#12704 = CARTESIAN_POINT ( 'NONE',  ( 9.457646018065525792E-16, -71.31249999863439371, 5.148502694627439702 ) ) ;
#12705 = CARTESIAN_POINT ( 'NONE',  ( -4.458734124999999437, -24.39583333196773651, -2.574251347313719407 ) ) ;
#12706 = CARTESIAN_POINT ( 'NONE',  ( 3.535533905932738197, -146.8750000000000000, -3.535533905932738197 ) ) ;
#12707 = CARTESIAN_POINT ( 'NONE',  ( 2.500000000000002220, 18.45833333606451632, 4.330127018922192761 ) ) ;
#12708 = CARTESIAN_POINT ( 'NONE',  ( 2.499999999999998668, -18.33333333333333215, -4.330127018922193649 ) ) ;
#12709 = CARTESIAN_POINT ( 'NONE',  ( 2.730187237215162345E-16, -148.1875000013656063, -4.458734124999999437 ) ) ;
#12710 = ORIENTED_EDGE ( 'NONE', *, *, #57324, .T. ) ;
#12711 = FACE_OUTER_BOUND ( 'NONE', #41933, .T. ) ;
#12712 = CARTESIAN_POINT ( 'NONE',  ( -4.458734124999997661, -49.47916666530107221, 2.574251347313722516 ) ) ;
#12713 = CARTESIAN_POINT ( 'NONE',  ( 2.500000000000002220, -2.666666666666664298, 4.330127018922192761 ) ) ;
#12714 = CARTESIAN_POINT ( 'NONE',  ( -55.00000000000002132, 0.000000000000000000, 0.000000000000000000 ) ) ;
#12715 = CARTESIAN_POINT ( 'NONE',  ( -2.500000000000000444, 23.83333333333333215, -4.330127018922193649 ) ) ;
#12716 = CARTESIAN_POINT ( 'NONE',  ( -52.53715891517739323, -152.4375000000000000, -4.819101127000233298 ) ) ;
#12717 = CARTESIAN_POINT ( 'NONE',  ( 4.458734125000001214, -1.895833331967737623, 2.574251347313718519 ) ) ;
#12718 = CARTESIAN_POINT ( 'NONE',  ( -58.24261429053147765, -155.0000000000000284, -3.805975901505573411 ) ) ;
#12719 = LINE ( 'NONE', #8842, #9125 ) ;
#12720 = CARTESIAN_POINT ( 'NONE',  ( -2.499999999999996447, -73.83333333333332860, 4.330127018922195425 ) ) ;
#12721 = CARTESIAN_POINT ( 'NONE',  ( -4.458734124999999437, 8.437500001365595637, 0.000000000000000000 ) ) ;
#12722 = VERTEX_POINT ( 'NONE', #40000 ) ;
#12723 = CARTESIAN_POINT ( 'NONE',  ( 0.000000000000000000, 0.000000000000000000, 0.000000000000000000 ) ) ;
#12724 = ORIENTED_EDGE ( 'NONE', *, *, #15037, .F. ) ;
#12725 = CARTESIAN_POINT ( 'NONE',  ( 2.499999999999998668, -7.208333330602150646, -4.330127018922193649 ) ) ;
#12726 = CARTESIAN_POINT ( 'NONE',  ( 4.458734124999998549, -48.72916666530107221, -2.574251347313721627 ) ) ;
#12727 = CARTESIAN_POINT ( 'NONE',  ( 4.458734124999999437, -162.7500000013655779, 1.846868145590737864 ) ) ;
#12728 = CARTESIAN_POINT ( 'NONE',  ( -4.999999999999999112, -42.79166666393548013, 2.886751345948131764 ) ) ;
#12729 = ORIENTED_EDGE ( 'NONE', *, *, #9096, .T. ) ;
#12730 = CARTESIAN_POINT ( 'NONE',  ( 2.229367062499998831, -25.64583333196773651, -3.861377020970580887 ) ) ;
#12731 = EDGE_LOOP ( 'NONE', ( #29648, #39121, #48947, #31792 ) ) ;
#12732 = CARTESIAN_POINT ( 'NONE',  ( -2.071067811865432873, -142.8125000027312410, -5.000000000000041744 ) ) ;
#12733 = CARTESIAN_POINT ( 'NONE',  ( -4.458734125000001214, -163.8750000013655779, 1.846868145590734089 ) ) ;
#12734 = EDGE_CURVE ( 'NONE', #49021, #33297, #49796, .T. ) ;
#12735 = FACE_OUTER_BOUND ( 'NONE', #4838, .T. ) ;
#12736 = CARTESIAN_POINT ( 'NONE',  ( -60.14911071818854538, -139.0625000000000284, 1.666127454062681368 ) ) ;
#12737 = CARTESIAN_POINT ( 'NONE',  ( -4.458734124999999437, -39.64583333196774362, -2.574251347313719407 ) ) ;
#12738 = CARTESIAN_POINT ( 'NONE',  ( 0.000000000000000000, -170.0000000000000000, 0.000000000000000000 ) ) ;
#12739 = ORIENTED_EDGE ( 'NONE', *, *, #24396, .F. ) ;
#12740 =( BOUNDED_CURVE ( )  B_SPLINE_CURVE ( 2, ( #22350, #16880, #2115, #47102, #42583, #47414, #27475, #32300, #51308 ),
 .UNSPECIFIED., .F., .F. ) 
 B_SPLINE_CURVE_WITH_KNOTS ( ( 3, 2, 2, 2, 3 ),
 ( 0.4410714285714285587, 0.4416666666666666519, 0.4428571428571428381, 0.4440476190476190244, 0.4446428571428571175 ),
 .UNSPECIFIED. ) 
 CURVE ( )  GEOMETRIC_REPRESENTATION_ITEM ( )  RATIONAL_B_SPLINE_CURVE ( ( 0.9330127018922194093, 0.9330127018922194093, 1.000000000000000000, 0.8660254037844387076, 1.000000000000000000, 0.8660254037844387076, 1.000000000000000000, 0.9330127018922194093, 0.9330127018922194093 ) ) 
 REPRESENTATION_ITEM ( '' )  );
#12741 = EDGE_CURVE ( 'NONE', #57389, #47780, #40962, .T. ) ;
#12742 = CARTESIAN_POINT ( 'NONE',  ( 2.229367062500001939, -80.97916666530106511, 3.861377020970579999 ) ) ;
#12743 = CARTESIAN_POINT ( 'NONE',  ( -2.229367062500000163, 26.52083333469892779, -3.861377020970580443 ) ) ;
#12744 = CARTESIAN_POINT ( 'NONE',  ( 1.339745962155612702, -59.29465819873853150, -5.000000000000000000 ) ) ;
#12745 = EDGE_LOOP ( 'NONE', ( #19810, #26250, #59340, #32658 ) ) ;
#12746 = CARTESIAN_POINT ( 'NONE',  ( -5.000000000000000000, 29.12500000273118417, 0.000000000000000000 ) ) ;
#12747 = CARTESIAN_POINT ( 'NONE',  ( -59.59170313451810586, -139.7500000013656347, 1.485763867205729394 ) ) ;
#12748 = CARTESIAN_POINT ( 'NONE',  ( 4.458734125000001214, -78.14583333196775072, 2.574251347313718519 ) ) ;
#12749 = CARTESIAN_POINT ( 'NONE',  ( -51.75738570946856498, -129.8750000027312126, 3.805975901505576964 ) ) ;
#12750 = FACE_OUTER_BOUND ( 'NONE', #50971, .T. ) ;
#12751 = CARTESIAN_POINT ( 'NONE',  ( 3.061616997868383141E-16, -144.8750000027312126, -5.000000000000000000 ) ) ;
#12752 = CARTESIAN_POINT ( 'NONE',  ( -2.229367062499996610, -53.14583333196773651, 3.861377020970582219 ) ) ;
#12753 = CARTESIAN_POINT ( 'NONE',  ( -5.000000000000000000, -71.95833333060214443, -2.886751345948128211 ) ) ;
#12754 = CARTESIAN_POINT ( 'NONE',  ( -4.458734124999999437, 29.68750000136559208, 0.000000000000000000 ) ) ;
#12755 = CARTESIAN_POINT ( 'NONE',  ( -2.500000000000000444, -106.1666666666666572, -4.330127018922193649 ) ) ;
#12756 = CARTESIAN_POINT ( 'NONE',  ( -6.972266317189433020E-16, 3.749999999999999556, -5.000000000000000000 ) ) ;
#12757 = CARTESIAN_POINT ( 'NONE',  ( 4.458734125000001214, -43.14583333196773651, 2.574251347313718519 ) ) ;
#12758 = CARTESIAN_POINT ( 'NONE',  ( 2.499999999999998668, 2.791666669397851130, -4.330127018922193649 ) ) ;
#12759 = CARTESIAN_POINT ( 'NONE',  ( 5.000000000000000888, 16.54166666939785202, 2.886751345948126879 ) ) ;
#12760 = CARTESIAN_POINT ( 'NONE',  ( -59.44456063193725015, -124.5625000013655921, -0.3552334253322034230 ) ) ;
#12761 = CARTESIAN_POINT ( 'NONE',  ( 2.229367062500001939, -81.22916666530106511, 3.861377020970579999 ) ) ;
#12762 = CARTESIAN_POINT ( 'NONE',  ( -2.229367062499996610, -103.1458333319677365, 3.861377020970582219 ) ) ;
#12763 = CARTESIAN_POINT ( 'NONE',  ( -2.229367062500000163, -5.729166665301072214, -3.861377020970580443 ) ) ;
#12764 = ORIENTED_EDGE ( 'NONE', *, *, #56675, .T. ) ;
#12765 = DIRECTION ( 'NONE',  ( -0.000000000000000000, 1.000000000000000000, -0.000000000000000000 ) ) ;
#12766 = CARTESIAN_POINT ( 'NONE',  ( -4.458734124999999437, -94.39583333196773651, -2.574251347313719407 ) ) ;
#12767 = CARTESIAN_POINT ( 'NONE',  ( -3.535533905932737309, -164.7500000027312126, -3.535533905932738197 ) ) ;
#12768 = CARTESIAN_POINT ( 'NONE',  ( -2.229367062499996610, -85.39583333196773651, 3.861377020970582219 ) ) ;
#12769 = CARTESIAN_POINT ( 'NONE',  ( 4.458734124999998549, 11.02083333469892956, -2.574251347313721627 ) ) ;
#12770 = DIRECTION ( 'NONE',  ( 0.000000000000000000, 0.000000000000000000, 1.000000000000000000 ) ) ;
#12771 = CIRCLE ( 'NONE', #9678, 5.000000000000001776 ) ;
#12772 = CARTESIAN_POINT ( 'NONE',  ( -59.29741812935640155, -135.6250000013655779, -2.196230717870135685 ) ) ;
#12773 = CARTESIAN_POINT ( 'NONE',  ( -4.458734124999999437, -14.39583333196773474, -2.574251347313719407 ) ) ;
#12774 = CARTESIAN_POINT ( 'NONE',  ( -4.458734124999999437, 16.35416666803225993, -2.574251347313719407 ) ) ;
#12775 = CARTESIAN_POINT ( 'NONE',  ( 2.229367062500001939, -54.22916666530107221, 3.861377020970579999 ) ) ;
#12776 = CARTESIAN_POINT ( 'NONE',  ( 5.000000000000000888, -38.45833333060213732, 2.886751345948126879 ) ) ;
#12777 = DIRECTION ( 'NONE',  ( -0.000000000000000000, 1.000000000000000000, -0.000000000000000000 ) ) ;
#12778 = CARTESIAN_POINT ( 'NONE',  ( 4.458734124999998549, -7.729166665301073991, -2.574251347313721627 ) ) ;
#12779 = CARTESIAN_POINT ( 'NONE',  ( -2.500000000000000444, -39.16666666666667140, -4.330127018922193649 ) ) ;
#12780 = EDGE_LOOP ( 'NONE', ( #30929, #37777, #5056, #47392 ) ) ;
#12781 = CARTESIAN_POINT ( 'NONE',  ( 9.457646018065525792E-16, -36.31249999863440792, 5.148502694627439702 ) ) ;
#12782 = CARTESIAN_POINT ( 'NONE',  ( -57.89159099828107458, -128.9375000013656063, -3.393966926194107447 ) ) ;
#12783 = CARTESIAN_POINT ( 'NONE',  ( 5.000000000000000000, -76.41666666666665719, -2.886751345948130876 ) ) ;
#12784 = CARTESIAN_POINT ( 'NONE',  ( -4.458734124999998549, -78.22916666530106511, 2.574251347313722516 ) ) ;
#12785 = CARTESIAN_POINT ( 'NONE',  ( -2.229367062500000163, 23.27083333469892779, -3.861377020970580443 ) ) ;
#12786 = CARTESIAN_POINT ( 'NONE',  ( 4.458734124999999437, -149.6875000013656063, 0.000000000000000000 ) ) ;
#12788 = EDGE_CURVE ( 'NONE', #34883, #26190, #36657, .T. ) ;
#12787 = CARTESIAN_POINT ( 'NONE',  ( 2.229367062499998831, 17.35416666803225993, -3.861377020970580887 ) ) ;
#12789 = CARTESIAN_POINT ( 'NONE',  ( 1.975475456537005874E-15, -47.74999999999999289, 5.000000000000000000 ) ) ;
#12790 = CYLINDRICAL_SURFACE ( 'NONE', #30706, 5.000000000000000000 ) ;
#12791 = CARTESIAN_POINT ( 'NONE',  ( 9.457646018065525792E-16, -84.31249999863440792, 5.148502694627439702 ) ) ;
#12792 = CARTESIAN_POINT ( 'NONE',  ( -2.500000000000000444, -62.16666666666666430, -4.330127018922193649 ) ) ;
#12793 =( BOUNDED_CURVE ( )  B_SPLINE_CURVE ( 2, ( #36073, #60530, #26104, #49584, #5526, #15818, #16454, #60211, #713 ),
 .UNSPECIFIED., .F., .F. ) 
 B_SPLINE_CURVE_WITH_KNOTS ( ( 3, 2, 2, 2, 3 ),
 ( 0.2854166666666666519, 0.2861111111111110938, 0.2874999999999999778, 0.2888888888888888618, 0.2895833333333333592 ),
 .UNSPECIFIED. ) 
 CURVE ( )  GEOMETRIC_REPRESENTATION_ITEM ( )  RATIONAL_B_SPLINE_CURVE ( ( 0.9330127018922194093, 0.9330127018922194093, 1.000000000000000000, 0.8660254037844387076, 1.000000000000000000, 0.8660254037844387076, 1.000000000000000000, 0.9330127018922167448, 0.9330127018922194093 ) ) 
 REPRESENTATION_ITEM ( '' )  );
#12794 = CARTESIAN_POINT ( 'NONE',  ( -1.339745962155610925, -1.669658196007333784, 5.000000000000000000 ) ) ;
#12795 = CARTESIAN_POINT ( 'NONE',  ( 2.500000000000002220, 18.45833333606451632, 4.330127018922192761 ) ) ;
#12796 = ORIENTED_EDGE ( 'NONE', *, *, #20959, .F. ) ;
#12797 = CARTESIAN_POINT ( 'NONE',  ( -6.972266317189433020E-16, -62.12499999726880162, -5.000000000000000000 ) ) ;
#12798 =( BOUNDED_CURVE ( )  B_SPLINE_CURVE ( 2, ( #39687, #59657, #805, #24593, #4649, #44200, #10431, #20083, #59327 ),
 .UNSPECIFIED., .F., .F. ) 
 B_SPLINE_CURVE_WITH_KNOTS ( ( 3, 2, 2, 2, 3 ),
 ( 0.4196428571428571508, 0.4202380952380952439, 0.4214285714285714302, 0.4226190476190476164, 0.4232142857142857095 ),
 .UNSPECIFIED. ) 
 CURVE ( )  GEOMETRIC_REPRESENTATION_ITEM ( )  RATIONAL_B_SPLINE_CURVE ( ( 0.9330127018922194093, 0.9330127018922194093, 1.000000000000000000, 0.8660254037844387076, 1.000000000000000000, 0.8660254037844387076, 1.000000000000000000, 0.9330127018922194093, 0.9330127018922194093 ) ) 
 REPRESENTATION_ITEM ( '' )  );
#12799 = FACE_OUTER_BOUND ( 'NONE', #2858, .T. ) ;
#12801 = CARTESIAN_POINT ( 'NONE',  ( 1.060575238724906964E-15, -28.74999999999999645, 5.773502691896257311 ) ) ;
#12800 = DIRECTION ( 'NONE',  ( 0.000000000000000000, 0.000000000000000000, 1.000000000000000000 ) ) ;
#12802 = CARTESIAN_POINT ( 'NONE',  ( 4.458734124999999437, -33.81249999863440792, -5.460374474430324690E-16 ) ) ;
#12803 = CARTESIAN_POINT ( 'NONE',  ( 6.123233995736766282E-16, -170.0000000000000000, -5.000000000000000000 ) ) ;
#12804 = CARTESIAN_POINT ( 'NONE',  ( 1.060575238724906964E-15, -26.62499999726881228, 5.773502691896257311 ) ) ;
#12806 = EDGE_LOOP ( 'NONE', ( #26411, #11306, #26573, #16300 ) ) ;
#12805 = CARTESIAN_POINT ( 'NONE',  ( -3.152548672688508926E-16, -59.56249999863440081, -5.148502694627439702 ) ) ;
#12807 = CARTESIAN_POINT ( 'NONE',  ( -58.39396692619412477, -153.6875000013656063, 2.891590998281057701 ) ) ;
#12809 = ORIENTED_EDGE ( 'NONE', *, *, #29089, .F. ) ;
#12808 = CARTESIAN_POINT ( 'NONE',  ( 4.458734125000001214, -11.14583333196774007, 2.574251347313718519 ) ) ;
#12810 = CARTESIAN_POINT ( 'NONE',  ( 2.499999999999998668, -69.33333333333332860, -4.330127018922193649 ) ) ;
#12811 = CARTESIAN_POINT ( 'NONE',  ( -59.29741812935640155, -140.6250000013656063, -2.196230717870135685 ) ) ;
#12812 = CARTESIAN_POINT ( 'NONE',  ( -2.229367062500000163, -51.72916666530107221, -3.861377020970580443 ) ) ;
#12813 = CARTESIAN_POINT ( 'NONE',  ( 5.000000000000000000, -79.37499999726881583, -6.123233995736766282E-16 ) ) ;
#12815 = ORIENTED_EDGE ( 'NONE', *, *, #24694, .T. ) ;
#12814 = CARTESIAN_POINT ( 'NONE',  ( -2.499999999999996447, -54.70833333060213732, 4.330127018922195425 ) ) ;
#12816 = CARTESIAN_POINT ( 'NONE',  ( -55.39835681537999790, -148.8750000000000284, 4.984105922594378235 ) ) ;
#12817 = CARTESIAN_POINT ( 'NONE',  ( 4.458734125000001214, -16.14583333196773651, 2.574251347313718519 ) ) ;
#12818 = CARTESIAN_POINT ( 'NONE',  ( -4.458734124999999437, -57.64583333196773651, -2.574251347313719407 ) ) ;
#12819 = CARTESIAN_POINT ( 'NONE',  ( -6.972266317189433020E-16, -24.24999999999999645, -5.000000000000000000 ) ) ;
#12820 = CARTESIAN_POINT ( 'NONE',  ( -3.152801135295367985, -139.8125000013655779, 3.152801135295367096 ) ) ;
#12821 = CARTESIAN_POINT ( 'NONE',  ( -2.229367062499996610, -98.39583333196773651, 3.861377020970582219 ) ) ;
#12822 = DIRECTION ( 'NONE',  ( 0.000000000000000000, 0.000000000000000000, 1.000000000000000000 ) ) ;
#12823 =( BOUNDED_CURVE ( )  B_SPLINE_CURVE ( 2, ( #29376, #44184, #39671, #786, #5595, #63194, #53839, #38721, #58362 ),
 .UNSPECIFIED., .F., .F. ) 
 B_SPLINE_CURVE_WITH_KNOTS ( ( 3, 2, 2, 2, 3 ),
 ( 0.04166666666666670599, 0.04583333333333337173, 0.05000000000000004441, 0.05416666666666671709, 0.05833333333333338283 ),
 .UNSPECIFIED. ) 
 CURVE ( )  GEOMETRIC_REPRESENTATION_ITEM ( )  RATIONAL_B_SPLINE_CURVE ( ( 0.9999999999999992228, 0.9238795325112875156, 1.000000000000000000, 0.9238795325112867385, 1.000000000000000000, 0.9238795325112867385, 1.000000000000000000, 0.9238795325112858503, 1.000000000000000888 ) ) 
 REPRESENTATION_ITEM ( '' )  );
#12824 = EDGE_LOOP ( 'NONE', ( #27159, #17469, #43886, #38216 ) ) ;
#12825 = CARTESIAN_POINT ( 'NONE',  ( -59.29741812935640155, -152.8750000013656063, -2.196230717870135685 ) ) ;
#12826 = CARTESIAN_POINT ( 'NONE',  ( -60.14911071818854538, -141.1875000027312126, 1.666127454062681368 ) ) ;
#12827 = FACE_OUTER_BOUND ( 'NONE', #5534, .T. ) ;
#12828 = CARTESIAN_POINT ( 'NONE',  ( -4.458734124999999437, -9.395833331967736513, -2.574251347313719407 ) ) ;
#12829 = CARTESIAN_POINT ( 'NONE',  ( -2.229367062499996610, -96.39583333196773651, 3.861377020970582219 ) ) ;
#12830 = CARTESIAN_POINT ( 'NONE',  ( 2.730187237215162345E-16, -146.4375000013656063, -4.458734124999999437 ) ) ;
#12831 = CARTESIAN_POINT ( 'NONE',  ( -3.152548672688508926E-16, -22.81249999863440436, -5.148502694627439702 ) ) ;
#12832 = CYLINDRICAL_SURFACE ( 'NONE', #20103, 5.000000000000000000 ) ;
#12833 = CARTESIAN_POINT ( 'NONE',  ( -56.48576386720575471, -135.7500000013656063, -4.591703134518078322 ) ) ;
#12834 = CARTESIAN_POINT ( 'NONE',  ( -2.229367062499996610, -64.39583333196773651, 3.861377020970582219 ) ) ;
#12835 = CARTESIAN_POINT ( 'NONE',  ( 0.000000000000000000, -120.0000000000000000, 5.000000000000000000 ) ) ;
#12836 = DIRECTION ( 'NONE',  ( -0.000000000000000000, 1.000000000000000000, -0.000000000000000000 ) ) ;
#12837 = CARTESIAN_POINT ( 'NONE',  ( 1.846868145590735200, -145.2500000013656347, -4.458734124999999437 ) ) ;
#12838 =( BOUNDED_CURVE ( )  B_SPLINE_CURVE ( 2, ( #4610, #20044, #24233, #5257, #43839, #39972, #15218, #59287, #49635 ),
 .UNSPECIFIED., .F., .F. ) 
 B_SPLINE_CURVE_WITH_KNOTS ( ( 3, 2, 2, 2, 3 ),
 ( 0.5946428571428571397, 0.5952380952380952328, 0.5964285714285714191, 0.5976190476190476053, 0.5982142857142856984 ),
 .UNSPECIFIED. ) 
 CURVE ( )  GEOMETRIC_REPRESENTATION_ITEM ( )  RATIONAL_B_SPLINE_CURVE ( ( 0.9330127018922194093, 0.9330127018922194093, 1.000000000000000000, 0.8660254037844387076, 1.000000000000000000, 0.8660254037844387076, 1.000000000000000000, 0.9330127018922194093, 0.9330127018922194093 ) ) 
 REPRESENTATION_ITEM ( '' )  );
#12839 = CARTESIAN_POINT ( 'NONE',  ( 4.458734125000000326, 9.854166668032261711, 2.574251347313718519 ) ) ;
#12840 = VERTEX_POINT ( 'NONE', #6249 ) ;
#12841 = CARTESIAN_POINT ( 'NONE',  ( -6.972266317189433020E-16, -5.249999999999998224, -5.000000000000000000 ) ) ;
#12842 = CARTESIAN_POINT ( 'NONE',  ( -9.184850993605147944E-16, -144.2500000000000284, 5.000000000000000000 ) ) ;
#12844 = CARTESIAN_POINT ( 'NONE',  ( -2.229367062500000163, -26.47916666530106866, -3.861377020970580443 ) ) ;
#12843 = CARTESIAN_POINT ( 'NONE',  ( 5.000000000000000000, -89.50000000000000000, -6.123233995736766282E-16 ) ) ;
#12845 = AXIS2_PLACEMENT_3D ( 'NONE', #11581, #26380, #45998 ) ;
#12846 = CARTESIAN_POINT ( 'NONE',  ( 1.975475456537005874E-15, -14.62499999726881228, 5.000000000000000000 ) ) ;
#12847 = CARTESIAN_POINT ( 'NONE',  ( -4.458734124999998549, -73.47916666530106511, 2.574251347313722516 ) ) ;
#12848 = EDGE_CURVE ( 'NONE', #23690, #14367, #16527, .T. ) ;
#12849 = CARTESIAN_POINT ( 'NONE',  ( -2.229367062500000163, 27.27083333469892779, -3.861377020970580443 ) ) ;
#12850 = CARTESIAN_POINT ( 'NONE',  ( 5.000000000000000000, -79.37499999726881583, -6.123233995736766282E-16 ) ) ;
#12851 = CARTESIAN_POINT ( 'NONE',  ( -58.39396692619412477, -147.4375000013656063, 2.891590998281057701 ) ) ;
#12852 = CARTESIAN_POINT ( 'NONE',  ( -4.458734124999999437, 4.604166668032261711, -2.574251347313719407 ) ) ;
#12853 = DIRECTION ( 'NONE',  ( 0.000000000000000000, 0.000000000000000000, 1.000000000000000000 ) ) ;
#12854 = CARTESIAN_POINT ( 'NONE',  ( -6.972266317189433020E-16, 5.875000002731185056, -5.000000000000000000 ) ) ;
#12855 = CARTESIAN_POINT ( 'NONE',  ( -2.229367062500000163, 8.520833334698926009, -3.861377020970580443 ) ) ;
#12856 = CARTESIAN_POINT ( 'NONE',  ( -3.152548672688508926E-16, -70.56249999863439371, -5.148502694627439702 ) ) ;
#12857 = CARTESIAN_POINT ( 'NONE',  ( 4.458734125000000326, -18.14583333196773651, 2.574251347313718519 ) ) ;
#12858 = CARTESIAN_POINT ( 'NONE',  ( -5.000000000000000000, -3.083333333333333925, -2.886751345948128211 ) ) ;
#12859 = CARTESIAN_POINT ( 'NONE',  ( -4.458734124999999437, -159.9375000013655779, -5.460374474430324690E-16 ) ) ;
#12860 = CARTESIAN_POINT ( 'NONE',  ( 1.339745962155612702, 15.83034180399266511, -5.000000000000000000 ) ) ;
#12861 = CARTESIAN_POINT ( 'NONE',  ( -4.458734124999998549, -62.22916666530106511, 2.574251347313722516 ) ) ;
#12862 = CARTESIAN_POINT ( 'NONE',  ( -2.499999999999996447, -100.7083333306021444, 4.330127018922195425 ) ) ;
#12863 = VECTOR ( 'NONE', #43753, 1000.000000000000000 ) ;
#12864 = CARTESIAN_POINT ( 'NONE',  ( -51.75738570946856498, -151.8750000027312126, 3.805975901505576964 ) ) ;
#12865 = CARTESIAN_POINT ( 'NONE',  ( -4.458734124999999437, -42.39583333196773651, -2.574251347313719407 ) ) ;
#12866 = CARTESIAN_POINT ( 'NONE',  ( -2.229367062499996610, -108.3958333319677365, 3.861377020970582219 ) ) ;
#12867 = CARTESIAN_POINT ( 'NONE',  ( 2.229367062499998831, -69.89583333196773651, -3.861377020970580887 ) ) ;
#12868 = CARTESIAN_POINT ( 'NONE',  ( 5.000000000000000000, -49.50000000000000000, -6.123233995736766282E-16 ) ) ;
#12869 = CARTESIAN_POINT ( 'NONE',  ( -5.926426369611017623E-15, 27.24999999999999645, 5.000000000000000000 ) ) ;
#12870 = CARTESIAN_POINT ( 'NONE',  ( 1.975475456537005874E-15, 19.25000000000000000, 5.000000000000000000 ) ) ;
#12871 = VERTEX_POINT ( 'NONE', #25538 ) ;
#12872 = CARTESIAN_POINT ( 'NONE',  ( -55.00000000000002132, 15.00000000000000000, 0.000000000000000000 ) ) ;
#12873 = LINE ( 'NONE', #2929, #53477 ) ;
#12874 = CARTESIAN_POINT ( 'NONE',  ( 5.000000000000000888, -7.583333333333330373, 2.886751345948126879 ) ) ;
#12875 = CARTESIAN_POINT ( 'NONE',  ( 2.229367062499998831, -13.64583333196774184, -3.861377020970580887 ) ) ;
#12876 = CARTESIAN_POINT ( 'NONE',  ( -4.458734124999999437, -76.31249999863440792, 0.000000000000000000 ) ) ;
#12877 = CARTESIAN_POINT ( 'NONE',  ( -2.499999999999996447, -4.708333330602147981, 4.330127018922195425 ) ) ;
#12878 = CARTESIAN_POINT ( 'NONE',  ( 5.000000000000000000, -14.37499999726881228, -6.123233995736766282E-16 ) ) ;
#12880 = ORIENTED_EDGE ( 'NONE', *, *, #53981, .F. ) ;
#12879 = CARTESIAN_POINT ( 'NONE',  ( -4.458734124999999437, -44.39583333196773651, -2.574251347313719407 ) ) ;
#12881 = CARTESIAN_POINT ( 'NONE',  ( -6.972266317189433020E-16, -51.12499999726880873, -5.000000000000000000 ) ) ;
#12883 = EDGE_LOOP ( 'NONE', ( #55054, #13920, #38222, #31232, #47827, #5477 ) ) ;
#12882 = CARTESIAN_POINT ( 'NONE',  ( -4.458734124999999437, 4.437500001365595637, 0.000000000000000000 ) ) ;
#12884 = CARTESIAN_POINT ( 'NONE',  ( 2.500000000000002220, -34.54166666393547303, 4.330127018922192761 ) ) ;
#12885 = CARTESIAN_POINT ( 'NONE',  ( -4.999999999999999112, -55.91666666666667140, 2.886751345948131764 ) ) ;
#12886 = CARTESIAN_POINT ( 'NONE',  ( 1.846868145590735200, -158.5000000013656631, -4.458734125000000326 ) ) ;
#12887 = CARTESIAN_POINT ( 'NONE',  ( -3.152548672688508926E-16, -37.81249999863440792, -5.148502694627439702 ) ) ;
#12888 = CARTESIAN_POINT ( 'NONE',  ( -3.152548672688508926E-16, -80.56249999863440792, -5.148502694627439702 ) ) ;
#12889 = CARTESIAN_POINT ( 'NONE',  ( -9.184850993605147944E-16, -166.2500000000000000, 5.000000000000000000 ) ) ;
#12890 = CARTESIAN_POINT ( 'NONE',  ( 5.000000000000000000, 5.625000002731185056, -6.123233995736766282E-16 ) ) ;
#12891 = CARTESIAN_POINT ( 'NONE',  ( -50.70258187064364108, -132.3750000013656347, 2.196230717870141014 ) ) ;
#12892 = CARTESIAN_POINT ( 'NONE',  ( 2.229367062500001939, 1.770833334698927786, 3.861377020970579999 ) ) ;
#12893 = CARTESIAN_POINT ( 'NONE',  ( 4.458734125000001214, -42.14583333196773651, 2.574251347313718519 ) ) ;
#12894 = CARTESIAN_POINT ( 'NONE',  ( 4.458734124999998549, -83.97916666530107932, -2.574251347313721627 ) ) ;
#12895 = CARTESIAN_POINT ( 'NONE',  ( 5.000000000000000000, -84.49999999999998579, -6.123233995736766282E-16 ) ) ;
#12896 = ORIENTED_EDGE ( 'NONE', *, *, #22819, .F. ) ;
#12897 = CARTESIAN_POINT ( 'NONE',  ( -54.60164318462004474, -153.5000000027312410, -4.984105922594373794 ) ) ;
#12898 = CARTESIAN_POINT ( 'NONE',  ( -9.184850993605147944E-16, -152.2500000000000000, 5.000000000000000000 ) ) ;
#12899 = CARTESIAN_POINT ( 'NONE',  ( -4.458734124999999437, -69.64583333196773651, -2.574251347313719407 ) ) ;
#12900 = CARTESIAN_POINT ( 'NONE',  ( 9.457646018065525792E-16, -9.312499998634406140, 5.148502694627439702 ) ) ;
#12901 = VERTEX_POINT ( 'NONE', #40329 ) ;
#12902 = VECTOR ( 'NONE', #45431, 1000.000000000000000 ) ;
#12903 = CARTESIAN_POINT ( 'NONE',  ( 3.535533905932736864, -164.1250000000000284, 3.535533905932738641 ) ) ;
#12904 = CARTESIAN_POINT ( 'NONE',  ( -1.049326080737009628E-13, -3.624999997268818053, 5.000000000000000000 ) ) ;
#12905 = CARTESIAN_POINT ( 'NONE',  ( -2.229367062500000163, -5.729166665301072214, -3.861377020970580443 ) ) ;
#12906 = CARTESIAN_POINT ( 'NONE',  ( 0.000000000000000000, -120.0000000000000000, 0.000000000000000000 ) ) ;
#12907 = CARTESIAN_POINT ( 'NONE',  ( -3.152548672688508926E-16, 0.4375000013655955255, -5.148502694627439702 ) ) ;
#12908 = FACE_OUTER_BOUND ( 'NONE', #25947, .T. ) ;
#12909 = CARTESIAN_POINT ( 'NONE',  ( 1.846868145590736310, -158.6250000013655779, 4.458734124999997661 ) ) ;
#12910 = CARTESIAN_POINT ( 'NONE',  ( 4.458734125000000326, 25.85416666803225993, 2.574251347313718519 ) ) ;
#12911 = ORIENTED_EDGE ( 'NONE', *, *, #57098, .F. ) ;
#12912 = CARTESIAN_POINT ( 'NONE',  ( 2.229367062500001939, -88.97916666530106511, 3.861377020970579999 ) ) ;
#12913 = CARTESIAN_POINT ( 'NONE',  ( -1.339745962155610925, -24.79465819873852439, 5.000000000000000000 ) ) ;
#12914 = CARTESIAN_POINT ( 'NONE',  ( -4.458734124999999437, -6.312499998634403475, 0.000000000000000000 ) ) ;
#12915 = ADVANCED_FACE ( 'NONE', ( #60287, #17490 ), #3019, .T. ) ;
#12916 = CARTESIAN_POINT ( 'NONE',  ( 6.123233995736766282E-16, -120.0000000000000000, -5.000000000000000000 ) ) ;
#12917 = CARTESIAN_POINT ( 'NONE',  ( -6.972266317189433020E-16, 0.7499999999999996669, -5.000000000000000000 ) ) ;
#12918 =( BOUNDED_CURVE ( )  B_SPLINE_CURVE ( 2, ( #41580, #55766, #16202, #50617, #21675, #12003, #12335, #30677, #36145 ),
 .UNSPECIFIED., .F., .F. ) 
 B_SPLINE_CURVE_WITH_KNOTS ( ( 3, 2, 2, 2, 3 ),
 ( 0.2232142857142857262, 0.2238095238095238193, 0.2250000000000000056, 0.2261904761904761918, 0.2267857142857142849 ),
 .UNSPECIFIED. ) 
 CURVE ( )  GEOMETRIC_REPRESENTATION_ITEM ( )  RATIONAL_B_SPLINE_CURVE ( ( 0.9330127018922194093, 0.9330127018922209636, 1.000000000000000000, 0.8660254037844387076, 1.000000000000000000, 0.8660254037844387076, 1.000000000000000000, 0.9330127018922194093, 0.9330127018922194093 ) ) 
 REPRESENTATION_ITEM ( '' )  );
#12919 = CARTESIAN_POINT ( 'NONE',  ( 1.975475456537005874E-15, -13.75000000000000000, 5.000000000000000000 ) ) ;
#12920 = CARTESIAN_POINT ( 'NONE',  ( -4.999999999999999112, -35.79166666393548013, 2.886751345948131764 ) ) ;
#12921 = CARTESIAN_POINT ( 'NONE',  ( 0.000000000000000000, -170.0000000000000000, 0.000000000000000000 ) ) ;
#12922 = CARTESIAN_POINT ( 'NONE',  ( -2.229367062500000163, 26.52083333469892779, -3.861377020970580443 ) ) ;
#12923 = CARTESIAN_POINT ( 'NONE',  ( -2.499999999999996447, -3.833333333333334370, 4.330127018922195425 ) ) ;
#12924 = CARTESIAN_POINT ( 'NONE',  ( 9.457646018065525792E-16, 20.93750000136558853, 5.148502694627439702 ) ) ;
#12925 = CARTESIAN_POINT ( 'NONE',  ( 2.229367062499998831, -54.64583333196773651, -3.861377020970580887 ) ) ;
#12926 = CARTESIAN_POINT ( 'NONE',  ( -2.229367062499996610, -1.395833331967737179, 3.861377020970582219 ) ) ;
#12927 = DIRECTION ( 'NONE',  ( 0.000000000000000000, 0.000000000000000000, 1.000000000000000000 ) ) ;
#12928 = CARTESIAN_POINT ( 'NONE',  ( 2.499999999999998668, 14.66666666666666607, -4.330127018922193649 ) ) ;
#12929 = CARTESIAN_POINT ( 'NONE',  ( 5.000000000000000888, -140.0625000027312126, -2.071067811865475505 ) ) ;
#12931 = EDGE_CURVE ( 'NONE', #13010, #23656, #25054, .T. ) ;
#12930 = CARTESIAN_POINT ( 'NONE',  ( 1.975475456537005874E-15, -75.62499999726880162, 5.000000000000000000 ) ) ;
#12932 = CARTESIAN_POINT ( 'NONE',  ( 4.458734124999999437, -49.81249999863440792, -5.460374474430324690E-16 ) ) ;
#12933 = CARTESIAN_POINT ( 'NONE',  ( 5.000000000000000000, -85.29166666393547303, -2.886751345948129988 ) ) ;
#12934 = CARTESIAN_POINT ( 'NONE',  ( -57.19623071787017210, -135.6250000013655779, 4.297418129356382899 ) ) ;
#12935 = DIRECTION ( 'NONE',  ( -0.000000000000000000, 1.000000000000000000, -0.000000000000000000 ) ) ;
#12936 =( BOUNDED_CURVE ( )  B_SPLINE_CURVE ( 2, ( #28378, #62807, #3951, #43168, #14525, #33838, #18726, #57977, #28997 ),
 .UNSPECIFIED., .F., .F. ) 
 B_SPLINE_CURVE_WITH_KNOTS ( ( 3, 2, 2, 2, 3 ),
 ( 0.3517857142857143127, 0.3523809523809524058, 0.3535714285714285920, 0.3547619047619047783, 0.3553571428571428714 ),
 .UNSPECIFIED. ) 
 CURVE ( )  GEOMETRIC_REPRESENTATION_ITEM ( )  RATIONAL_B_SPLINE_CURVE ( ( 0.9330127018922194093, 0.9330127018922225179, 1.000000000000000000, 0.8660254037844387076, 1.000000000000000000, 0.8660254037844387076, 1.000000000000000000, 0.9330127018922194093, 0.9330127018922194093 ) ) 
 REPRESENTATION_ITEM ( '' )  );
#12937 = CARTESIAN_POINT ( 'NONE',  ( -50.01589407740564042, -145.6250000000000284, 0.3983568153799778022 ) ) ;
#12938 = EDGE_CURVE ( 'NONE', #51592, #39751, #43213, .T. ) ;
#12939 = CARTESIAN_POINT ( 'NONE',  ( 4.458734124999998549, -84.97916666530107932, -2.574251347313721627 ) ) ;
#12940 = CARTESIAN_POINT ( 'NONE',  ( -3.152801135295367096, -159.3125000013656063, -3.152801135295367541 ) ) ;
#12941 = CARTESIAN_POINT ( 'NONE',  ( -3.535250795749689387E-16, -32.25000000000000000, -5.773502691896257311 ) ) ;
#12942 = ORIENTED_EDGE ( 'NONE', *, *, #60235, .T. ) ;
#12943 = CARTESIAN_POINT ( 'NONE',  ( 9.457646018065525792E-16, 19.68750000136559208, 5.148502694627439702 ) ) ;
#12944 = ORIENTED_EDGE ( 'NONE', *, *, #53033, .T. ) ;
#12945 = CARTESIAN_POINT ( 'NONE',  ( -4.458734124999999437, -98.31249999863440792, 0.000000000000000000 ) ) ;
#12946 = CARTESIAN_POINT ( 'NONE',  ( 2.229367062500001939, 7.770833334698926009, 3.861377020970579999 ) ) ;
#12947 = CARTESIAN_POINT ( 'NONE',  ( -4.999999999999999112, 13.20833333606451809, 2.886751345948131764 ) ) ;
#12948 = CARTESIAN_POINT ( 'NONE',  ( 2.500000000000002220, -16.66666666666666430, 4.330127018922192761 ) ) ;
#12949 = CARTESIAN_POINT ( 'NONE',  ( -2.499999999999996447, 8.166666666666666075, 4.330127018922195425 ) ) ;
#12950 = EDGE_CURVE ( 'NONE', #51146, #8450, #5850, .T. ) ;
#12951 = CARTESIAN_POINT ( 'NONE',  ( -4.458734124999997661, -58.22916666530106511, 2.574251347313722516 ) ) ;
#12952 = CARTESIAN_POINT ( 'NONE',  ( 1.975475456537005874E-15, -52.62499999726880873, 5.000000000000000000 ) ) ;
#12953 = CARTESIAN_POINT ( 'NONE',  ( 5.000000000000000888, -79.58333333333331439, 2.886751345948126879 ) ) ;
#12954 = CARTESIAN_POINT ( 'NONE',  ( -2.229367062500000163, -28.47916666530107221, -3.861377020970580443 ) ) ;
#12955 = CARTESIAN_POINT ( 'NONE',  ( -6.972266317189433020E-16, -55.12499999726880873, -5.000000000000000000 ) ) ;
#12956 = CARTESIAN_POINT ( 'NONE',  ( -1.339745962155613812, -25.08034179853028789, -5.000000000000000000 ) ) ;
#12957 = CARTESIAN_POINT ( 'NONE',  ( -5.000000000000000000, -39.99999999999999289, 0.000000000000000000 ) ) ;
#12958 = DIRECTION ( 'NONE',  ( 0.000000000000000000, 0.000000000000000000, 1.000000000000000000 ) ) ;
#12960 = CARTESIAN_POINT ( 'NONE',  ( 4.458734125000001214, -22.14583333196773296, 2.574251347313718519 ) ) ;
#12959 = CARTESIAN_POINT ( 'NONE',  ( -2.500000000000000444, 14.83333333333333215, -4.330127018922193649 ) ) ;
#12961 = CARTESIAN_POINT ( 'NONE',  ( -5.000000000000000000, -143.5000000000000284, -6.123233995736766282E-16 ) ) ;
#12962 = CARTESIAN_POINT ( 'NONE',  ( -4.458734124999998549, -67.22916666530106511, 2.574251347313722516 ) ) ;
#12963 = CARTESIAN_POINT ( 'NONE',  ( -3.152801135295367096, -149.3125000013655779, -3.152801135295367541 ) ) ;
#12964 = CARTESIAN_POINT ( 'NONE',  ( -2.229367062499996610, -73.14583333196773651, 3.861377020970582219 ) ) ;
#12965 = CARTESIAN_POINT ( 'NONE',  ( -57.89159099828107458, -143.9375000013656063, -3.393966926194107447 ) ) ;
#12966 = CARTESIAN_POINT ( 'NONE',  ( -2.229367062500000163, -25.72916666530106866, -3.861377020970580443 ) ) ;
#12967 = CARTESIAN_POINT ( 'NONE',  ( -5.000000000000000000, -62.95833333060214443, -2.886751345948128211 ) ) ;
#12968 = ORIENTED_EDGE ( 'NONE', *, *, #26823, .T. ) ;
#12969 = ADVANCED_FACE ( 'NONE', ( #2077 ), #52209, .T. ) ;
#12970 = DIRECTION ( 'NONE',  ( -0.000000000000000000, 1.000000000000000000, -0.000000000000000000 ) ) ;
#12971 = ORIENTED_EDGE ( 'NONE', *, *, #3927, .F. ) ;
#12972 = CARTESIAN_POINT ( 'NONE',  ( 2.229367062500001939, -65.22916666530106511, 3.861377020970579999 ) ) ;
#12973 = FACE_OUTER_BOUND ( 'NONE', #32744, .T. ) ;
#12974 = CARTESIAN_POINT ( 'NONE',  ( -2.499999999999996447, -5.708333330602148870, 4.330127018922195425 ) ) ;
#12975 = ORIENTED_EDGE ( 'NONE', *, *, #12559, .F. ) ;
#12976 = DIRECTION ( 'NONE',  ( 1.000000000000000000, 0.000000000000000000, 0.000000000000000000 ) ) ;
#12977 = CARTESIAN_POINT ( 'NONE',  ( -6.127431526422343306E-17, 9.147862274876549904, -8.047472243342932430 ) ) ;
#12978 = CARTESIAN_POINT ( 'NONE',  ( -1.339745962155613812, -56.08034179853028434, -5.000000000000000000 ) ) ;
#12979 = CARTESIAN_POINT ( 'NONE',  ( 4.458734124999998549, -55.97916666530107932, -2.574251347313721627 ) ) ;
#12980 = VERTEX_POINT ( 'NONE', #27755 ) ;
#12981 = CARTESIAN_POINT ( 'NONE',  ( 1.339745962155615144, -45.70534180126146850, 4.999999999999999112 ) ) ;
#12982 = CARTESIAN_POINT ( 'NONE',  ( -4.458734124999998549, 9.770833334698927786, 2.574251347313722516 ) ) ;
#12983 = CARTESIAN_POINT ( 'NONE',  ( 4.458734125000001214, 17.10416666803225993, 2.574251347313718519 ) ) ;
#12984 = CARTESIAN_POINT ( 'NONE',  ( -58.39396692619412477, -148.4375000013656063, 2.891590998281057701 ) ) ;
#12985 = CARTESIAN_POINT ( 'NONE',  ( 2.499999999999998668, 20.79166666939784847, -4.330127018922193649 ) ) ;
#12986 = DIRECTION ( 'NONE',  ( -0.000000000000000000, 1.000000000000000000, -0.000000000000000000 ) ) ;
#12987 =( BOUNDED_CURVE ( )  B_SPLINE_CURVE ( 2, ( #33096, #62692, #18616, #38242, #25977, #10857, #34668, #34342, #49463 ),
 .UNSPECIFIED., .F., .F. ) 
 B_SPLINE_CURVE_WITH_KNOTS ( ( 3, 2, 2, 2, 3 ),
 ( 0.8187499999999999778, 0.8194444444444444198, 0.8208333333333333037, 0.8222222222222221877, 0.8229166666666666297 ),
 .UNSPECIFIED. ) 
 CURVE ( )  GEOMETRIC_REPRESENTATION_ITEM ( )  RATIONAL_B_SPLINE_CURVE ( ( 0.9330127018922194093, 0.9330127018922194093, 1.000000000000000000, 0.8660254037844387076, 1.000000000000000000, 0.8660254037844387076, 1.000000000000000000, 0.9330127018922194093, 0.9330127018922194093 ) ) 
 REPRESENTATION_ITEM ( '' )  );
#12988 = AXIS2_PLACEMENT_3D ( 'NONE', #22055, #55834, #7271 ) ;
#12989 = ORIENTED_EDGE ( 'NONE', *, *, #44521, .T. ) ;
#12990 = CARTESIAN_POINT ( 'NONE',  ( 4.458734124999998549, -71.72916666530107932, -2.574251347313721627 ) ) ;
#12991 = CARTESIAN_POINT ( 'NONE',  ( -6.972266317189433020E-16, -10.12499999726881406, -5.000000000000000000 ) ) ;
#12992 = CARTESIAN_POINT ( 'NONE',  ( -2.229367062499996610, 5.854166668032262599, 3.861377020970582219 ) ) ;
#12993 = AXIS2_PLACEMENT_3D ( 'NONE', #61760, #31842, #62073 ) ;
#12994 = VECTOR ( 'NONE', #11719, 1000.000000000000000 ) ;
#12995 = EDGE_CURVE ( 'NONE', #27115, #30305, #22312, .T. ) ;
#12996 = DIRECTION ( 'NONE',  ( -0.000000000000000000, 1.000000000000000000, -0.000000000000000000 ) ) ;
#12997 = ADVANCED_FACE ( 'NONE', ( #41586 ), #12650, .T. ) ;
#12998 = CARTESIAN_POINT ( 'NONE',  ( 4.458734124999998549, -61.97916666530106511, -2.574251347313721627 ) ) ;
#12999 = CARTESIAN_POINT ( 'NONE',  ( 5.000000000000000000, -19.37499999726881583, -6.123233995736766282E-16 ) ) ;
#13000 = CARTESIAN_POINT ( 'NONE',  ( 1.339745962155612702, 4.705341801261479162, -5.000000000000000000 ) ) ;
#13001 = CARTESIAN_POINT ( 'NONE',  ( -2.459698528280933161, 7.240146430416066536, -0.09933465333851029810 ) ) ;
#13002 = CARTESIAN_POINT ( 'NONE',  ( -1.049326080737009628E-13, -20.62499999726881583, 5.000000000000000000 ) ) ;
#13003 = LINE ( 'NONE', #16882, #62452 ) ;
#13004 = CARTESIAN_POINT ( 'NONE',  ( -2.229367062499996610, -38.14583333196773651, 3.861377020970582219 ) ) ;
#13005 = CARTESIAN_POINT ( 'NONE',  ( -4.458734124999999437, -20.64583333196774007, -2.574251347313719407 ) ) ;
#13006 = ORIENTED_EDGE ( 'NONE', *, *, #18045, .F. ) ;
#13007 = CARTESIAN_POINT ( 'NONE',  ( 0.000000000000000000, -120.0000000000000000, 5.000000000000000000 ) ) ;
#13008 = CARTESIAN_POINT ( 'NONE',  ( -2.229367062500000163, -107.4791666653010651, -3.861377020970580443 ) ) ;
#13009 = CARTESIAN_POINT ( 'NONE',  ( -3.535533905932737309, -153.7500000027312126, -3.535533905932738197 ) ) ;
#13010 = VERTEX_POINT ( 'NONE', #28073 ) ;
#13011 = CARTESIAN_POINT ( 'NONE',  ( -4.458734124999999437, -106.6458333319677365, -2.574251347313719407 ) ) ;
#13012 = CARTESIAN_POINT ( 'NONE',  ( 4.458734125000001214, -31.89583333196773651, 2.574251347313718519 ) ) ;
#13013 = CARTESIAN_POINT ( 'NONE',  ( -2.499999999999996447, -67.70833333060214443, 4.330127018922195425 ) ) ;
#13014 = EDGE_CURVE ( 'NONE', #50926, #17569, #12423, .T. ) ;
#13015 = CARTESIAN_POINT ( 'NONE',  ( -58.39396692619412477, -146.6875000013656063, 2.891590998281057701 ) ) ;
#13016 = CARTESIAN_POINT ( 'NONE',  ( -3.535533905932738641, -145.3750000000000000, 3.535533905932737309 ) ) ;
#13017 = CARTESIAN_POINT ( 'NONE',  ( -4.458734124999999437, -28.39583333196773651, -2.574251347313719407 ) ) ;
#13018 = EDGE_CURVE ( 'NONE', #62985, #27288, #18981, .T. ) ;
#13019 = CARTESIAN_POINT ( 'NONE',  ( -2.229367062500000163, -70.72916666530107932, -3.861377020970580443 ) ) ;
#13020 = CARTESIAN_POINT ( 'NONE',  ( 4.458734124999997661, -168.7500000013656063, 1.846868145590737864 ) ) ;
#13021 = CARTESIAN_POINT ( 'NONE',  ( 2.229367062500001939, -22.97916666530107221, 3.861377020970579999 ) ) ;
#13022 = CARTESIAN_POINT ( 'NONE',  ( 5.000000000000000888, -32.58333333333333570, 2.886751345948126879 ) ) ;
#13023 = CYLINDRICAL_SURFACE ( 'NONE', #54407, 5.000000000000000000 ) ;
#13024 = CARTESIAN_POINT ( 'NONE',  ( -3.535250795749689387E-16, -15.25000000000000000, -5.773502691896257311 ) ) ;
#13025 = CARTESIAN_POINT ( 'NONE',  ( 4.458734124999999437, -148.4375000013656063, 0.000000000000000000 ) ) ;
#13026 = ORIENTED_EDGE ( 'NONE', *, *, #7928, .T. ) ;
#13027 = DIRECTION ( 'NONE',  ( -0.000000000000000000, 1.000000000000000000, -0.000000000000000000 ) ) ;
#13028 = CARTESIAN_POINT ( 'NONE',  ( 4.458734125000000326, -54.14583333196773651, 2.574251347313718519 ) ) ;
#13029 =( BOUNDED_CURVE ( )  B_SPLINE_CURVE ( 2, ( #34819, #23900, #29328, #48958, #102, #29979, #5547, #33862, #49291 ),
 .UNSPECIFIED., .F., .F. ) 
 B_SPLINE_CURVE_WITH_KNOTS ( ( 3, 2, 2, 2, 3 ),
 ( 0.3553571428571428714, 0.3559523809523809645, 0.3571428571428571508, 0.3583333333333333370, 0.3589285714285714302 ),
 .UNSPECIFIED. ) 
 CURVE ( )  GEOMETRIC_REPRESENTATION_ITEM ( )  RATIONAL_B_SPLINE_CURVE ( ( 0.9330127018922194093, 0.9330127018922194093, 1.000000000000000000, 0.8660254037844387076, 1.000000000000000000, 0.8660254037844387076, 1.000000000000000000, 0.9330127018922194093, 0.9330127018922194093 ) ) 
 REPRESENTATION_ITEM ( '' )  );
#13030 = CARTESIAN_POINT ( 'NONE',  ( 0.000000000000000000, -170.0000000000000000, 5.000000000000000000 ) ) ;
#13031 = CARTESIAN_POINT ( 'NONE',  ( -5.000000000000001776, 0.000000000000000000, -9.974600000000000577 ) ) ;
#13032 = CARTESIAN_POINT ( 'NONE',  ( 5.000000000000000000, 22.50000000000000000, -6.123233995736766282E-16 ) ) ;
#13033 = DIRECTION ( 'NONE',  ( 0.000000000000000000, 0.000000000000000000, 1.000000000000000000 ) ) ;
#13034 = CARTESIAN_POINT ( 'NONE',  ( 9.457646018065525792E-16, -3.062499998634407472, 5.148502694627439702 ) ) ;
#13035 = CARTESIAN_POINT ( 'NONE',  ( -1.339745962155610925, -51.66965819600733312, 5.000000000000000000 ) ) ;
#13036 = DIRECTION ( 'NONE',  ( -0.000000000000000000, 1.000000000000000000, -0.000000000000000000 ) ) ;
#13037 = CARTESIAN_POINT ( 'NONE',  ( 1.975475456537005874E-15, -61.62499999726880162, 5.000000000000000000 ) ) ;
#13038 = CARTESIAN_POINT ( 'NONE',  ( 4.458734124999998549, 12.02083333469892601, -2.574251347313721627 ) ) ;
#13039 = VERTEX_POINT ( 'NONE', #10027 ) ;
#13040 = DIRECTION ( 'NONE',  ( -0.000000000000000000, 1.000000000000000000, -0.000000000000000000 ) ) ;
#13041 = EDGE_LOOP ( 'NONE', ( #60524, #12428, #390, #62795 ) ) ;
#13042 = AXIS2_PLACEMENT_3D ( 'NONE', #24851, #5548, #15195 ) ;
#13043 = CARTESIAN_POINT ( 'NONE',  ( 2.500000000000002220, -7.541666663935481907, 4.330127018922192761 ) ) ;
#13044 = CARTESIAN_POINT ( 'NONE',  ( 9.457646018065525792E-16, -50.06249999863440792, 5.148502694627439702 ) ) ;
#13045 = CARTESIAN_POINT ( 'NONE',  ( -4.458734125000000326, -161.2500000013655779, -1.846868145590735644 ) ) ;
#13046 = AXIS2_PLACEMENT_3D ( 'NONE', #50784, #30515, #20568 ) ;
#13047 = VECTOR ( 'NONE', #51147, 1000.000000000000000 ) ;
#13048 = CARTESIAN_POINT ( 'NONE',  ( -2.499999999999996447, -46.70833333060214443, 4.330127018922195425 ) ) ;
#13049 = EDGE_LOOP ( 'NONE', ( #57588, #10803, #15964, #3098 ) ) ;
#13050 = CARTESIAN_POINT ( 'NONE',  ( -3.152548672688508926E-16, -23.56249999863440436, -5.148502694627439702 ) ) ;
#13051 = ORIENTED_EDGE ( 'NONE', *, *, #36926, .T. ) ;
#13052 = CARTESIAN_POINT ( 'NONE',  ( -2.500000000000000444, -103.0416666639354730, -4.330127018922193649 ) ) ;
#13053 = CARTESIAN_POINT ( 'NONE',  ( 4.458734125000000326, -162.3750000013655779, -1.846868145590734978 ) ) ;
#13054 = FACE_OUTER_BOUND ( 'NONE', #31653, .T. ) ;
#13055 = CARTESIAN_POINT ( 'NONE',  ( -51.19402409849444524, -138.5000000000000284, -3.242614290531456334 ) ) ;
#13056 = CARTESIAN_POINT ( 'NONE',  ( -4.458734124999999437, -35.56249999863440792, 0.000000000000000000 ) ) ;
#13057 = CARTESIAN_POINT ( 'NONE',  ( -5.000000000000000000, 23.12500000273118417, 0.000000000000000000 ) ) ;
#13058 = ORIENTED_EDGE ( 'NONE', *, *, #32793, .T. ) ;
#13059 = CARTESIAN_POINT ( 'NONE',  ( 4.458734124999999437, -80.81249999863440792, -5.460374474430324690E-16 ) ) ;
#13060 = CARTESIAN_POINT ( 'NONE',  ( 4.458734125000001214, 26.10416666803225993, 2.574251347313718519 ) ) ;
#13061 = CARTESIAN_POINT ( 'NONE',  ( 2.499999999999998668, -59.33333333333333570, -4.330127018922193649 ) ) ;
#13062 = EDGE_LOOP ( 'NONE', ( #13584, #24492, #53380, #7971 ) ) ;
#13063 = CARTESIAN_POINT ( 'NONE',  ( -1.339745962155613812, -60.08034179853027723, -5.000000000000000000 ) ) ;
#13064 = CARTESIAN_POINT ( 'NONE',  ( -50.55543936806279248, -139.3125000013656063, 0.3552334253322060320 ) ) ;
#13065 = CARTESIAN_POINT ( 'NONE',  ( 2.229367062500001939, -88.22916666530107932, 3.861377020970579999 ) ) ;
#13066 = CARTESIAN_POINT ( 'NONE',  ( -50.18089887299979068, -131.8125000027312126, 2.462841084822635640 ) ) ;
#13067 = CARTESIAN_POINT ( 'NONE',  ( -6.972266317189433020E-16, 0.8750000027311866102, -5.000000000000000000 ) ) ;
#13068 = CARTESIAN_POINT ( 'NONE',  ( -4.999999999999998224, -6.916666666666667851, 2.886751345948131764 ) ) ;
#13069 = CARTESIAN_POINT ( 'NONE',  ( 5.000000000000000000, -13.37499999726881050, -6.123233995736766282E-16 ) ) ;
#13070 = CARTESIAN_POINT ( 'NONE',  ( 2.229367062499998831, -55.64583333196773651, -3.861377020970580887 ) ) ;
#13071 = CARTESIAN_POINT ( 'NONE',  ( 5.000000000000000000, 21.50000000000000000, -6.123233995736766282E-16 ) ) ;
#13072 = CARTESIAN_POINT ( 'NONE',  ( 9.457646018065525792E-16, 21.93750000136559208, 5.148502694627439702 ) ) ;
#13073 = CARTESIAN_POINT ( 'NONE',  ( 5.000000000000000000, -105.5000000000000142, -6.123233995736766282E-16 ) ) ;
#13074 = CARTESIAN_POINT ( 'NONE',  ( -2.499999999999996447, -43.83333333333333570, 4.330127018922195425 ) ) ;
#13075 = EDGE_CURVE ( 'NONE', #40991, #14611, #45665, .T. ) ;
#13076 = CARTESIAN_POINT ( 'NONE',  ( 4.458734125000001214, -46.14583333196773651, 2.574251347313718519 ) ) ;
#13077 = CARTESIAN_POINT ( 'NONE',  ( 1.060575238724906964E-15, -5.624999997268811391, 5.773502691896257311 ) ) ;
#13078 = CYLINDRICAL_SURFACE ( 'NONE', #13995, 5.000000000000000000 ) ;
#13079 = CARTESIAN_POINT ( 'NONE',  ( -50.40829686548195099, -127.0000000013656063, -1.485763867205728284 ) ) ;
#13080 = CARTESIAN_POINT ( 'NONE',  ( 2.229367062499998831, -82.89583333196773651, -3.861377020970580887 ) ) ;
#13081 = CARTESIAN_POINT ( 'NONE',  ( 4.458734125000000326, -100.8958333319677365, 2.574251347313718519 ) ) ;
#13082 = CARTESIAN_POINT ( 'NONE',  ( 9.457646018065525792E-16, -6.312499998634403475, 5.148502694627439702 ) ) ;
#13083 = ORIENTED_EDGE ( 'NONE', *, *, #55852, .F. ) ;
#13084 = AXIS2_PLACEMENT_3D ( 'NONE', #47784, #29407, #52622 ) ;
#13085 = CARTESIAN_POINT ( 'NONE',  ( -5.000000000000000000, -85.87499999726880162, 0.000000000000000000 ) ) ;
#13086 = CARTESIAN_POINT ( 'NONE',  ( -2.229367062499996610, -93.14583333196773651, 3.861377020970582219 ) ) ;
#13087 = CARTESIAN_POINT ( 'NONE',  ( 3.535533905932736864, -166.2500000027312126, 3.535533905932738641 ) ) ;
#13088 = CARTESIAN_POINT ( 'NONE',  ( -2.229367062499996610, -91.39583333196773651, 3.861377020970582219 ) ) ;
#13089 = CARTESIAN_POINT ( 'NONE',  ( -4.458734124999997661, 12.52083333469892601, 2.574251347313722516 ) ) ;
#13090 = CARTESIAN_POINT ( 'NONE',  ( 0.000000000000000000, -170.0000000000000000, 0.000000000000000000 ) ) ;
#13091 = AXIS2_PLACEMENT_3D ( 'NONE', #11962, #51224, #7161 ) ;
#13092 = CARTESIAN_POINT ( 'NONE',  ( -52.80376928212989185, -131.8750000013656347, -4.297418129356379346 ) ) ;
#13093 = AXIS2_PLACEMENT_3D ( 'NONE', #33255, #45592, #52875 ) ;
#13094 = CARTESIAN_POINT ( 'NONE',  ( 9.457646018065525792E-16, -13.06249999863440259, 5.148502694627439702 ) ) ;
#13095 = CARTESIAN_POINT ( 'NONE',  ( -4.458734124999999437, 12.35416666803225993, -2.574251347313719407 ) ) ;
#13096 = CARTESIAN_POINT ( 'NONE',  ( -2.229367062500000163, -52.72916666530107221, -3.861377020970580443 ) ) ;
#13097 = DIRECTION ( 'NONE',  ( 0.000000000000000000, 0.000000000000000000, 1.000000000000000000 ) ) ;
#13098 = CARTESIAN_POINT ( 'NONE',  ( 1.975475456537005874E-15, -105.7500000000000000, 5.000000000000000000 ) ) ;
#13099 = CARTESIAN_POINT ( 'NONE',  ( -2.229367062499996610, -10.14583333196773829, 3.861377020970582219 ) ) ;
#13100 =( LENGTH_UNIT ( ) NAMED_UNIT ( * ) SI_UNIT ( .MILLI., .METRE. ) );
#13101 = EDGE_CURVE ( 'NONE', #11403, #47219, #24189, .T. ) ;
#13102 = ORIENTED_EDGE ( 'NONE', *, *, #2429, .T. ) ;
#13103 = CARTESIAN_POINT ( 'NONE',  ( 9.457646018065525792E-16, -37.31249999863440792, 5.148502694627439702 ) ) ;
#13104 = CARTESIAN_POINT ( 'NONE',  ( -50.55543936806279248, -128.3125000013656063, 0.3552334253322060320 ) ) ;
#13105 = EDGE_CURVE ( 'NONE', #23654, #22858, #13602, .T. ) ;
#13106 = CARTESIAN_POINT ( 'NONE',  ( 5.000000000000000000, 0.6250000027311873874, -6.123233995736766282E-16 ) ) ;
#13107 = CARTESIAN_POINT ( 'NONE',  ( -4.999999999999998224, 10.08333333333333393, 2.886751345948131764 ) ) ;
#13108 = CARTESIAN_POINT ( 'NONE',  ( -3.152548672688508926E-16, -80.56249999863440792, -5.148502694627439702 ) ) ;
#13109 = CARTESIAN_POINT ( 'NONE',  ( 2.229367062500001939, 21.77083333469892779, 3.861377020970579999 ) ) ;
#13110 = CARTESIAN_POINT ( 'NONE',  ( 2.229367062500001939, 13.02083333469892779, 3.861377020970579999 ) ) ;
#13111 = EDGE_CURVE ( 'NONE', #26645, #11325, #18423, .T. ) ;
#13112 = CARTESIAN_POINT ( 'NONE',  ( -6.972266317189433020E-16, 6.750000000000000000, -5.000000000000000000 ) ) ;
#13113 = CARTESIAN_POINT ( 'NONE',  ( -4.458734124999999437, -81.56249999863440792, 0.000000000000000000 ) ) ;
#13114 = CARTESIAN_POINT ( 'NONE',  ( -5.000000000000000000, -71.08333333333332860, -2.886751345948128211 ) ) ;
#13115 = CARTESIAN_POINT ( 'NONE',  ( 1.339745962155612702, -72.16965819600733312, -5.000000000000000000 ) ) ;
#13116 = CARTESIAN_POINT ( 'NONE',  ( -2.499999999999996447, 19.29166666939785202, 4.330127018922195425 ) ) ;
#13117 = ORIENTED_EDGE ( 'NONE', *, *, #23699, .F. ) ;
#13118 = CARTESIAN_POINT ( 'NONE',  ( -2.500000000000000444, -66.16666666666667140, -4.330127018922193649 ) ) ;
#13119 = CARTESIAN_POINT ( 'NONE',  ( -1.339745962155610925, -89.79465819873851729, 5.000000000000000000 ) ) ;
#13121 = CARTESIAN_POINT ( 'NONE',  ( -4.999999999999999112, -29.91666666666667140, 2.886751345948131764 ) ) ;
#13120 = CARTESIAN_POINT ( 'NONE',  ( 1.975475456537005874E-15, -50.75000000000000000, 5.000000000000000000 ) ) ;
#13122 = CARTESIAN_POINT ( 'NONE',  ( 9.457646018065525792E-16, -32.06249999863440792, 5.148502694627439702 ) ) ;
#13123 =( BOUNDED_CURVE ( )  B_SPLINE_CURVE ( 2, ( #58347, #48372, #14582, #4618, #4011, #43226, #29054, #23934, #13958 ),
 .UNSPECIFIED., .F., .F. ) 
 B_SPLINE_CURVE_WITH_KNOTS ( ( 3, 2, 2, 2, 3 ),
 ( 0.4053571428571428603, 0.4059523809523809534, 0.4071428571428571397, 0.4083333333333333259, 0.4089285714285714191 ),
 .UNSPECIFIED. ) 
 CURVE ( )  GEOMETRIC_REPRESENTATION_ITEM ( )  RATIONAL_B_SPLINE_CURVE ( ( 0.9330127018922194093, 0.9330127018922194093, 1.000000000000000000, 0.8660254037844387076, 1.000000000000000000, 0.8660254037844387076, 1.000000000000000000, 0.9330127018922194093, 0.9330127018922194093 ) ) 
 REPRESENTATION_ITEM ( '' )  );
#13124 = CARTESIAN_POINT ( 'NONE',  ( -5.000000000000000000, -29.87499999726881228, 0.000000000000000000 ) ) ;
#13126 = EDGE_LOOP ( 'NONE', ( #17933, #50162, #44198, #16350 ) ) ;
#13125 = CARTESIAN_POINT ( 'NONE',  ( 4.458734125000001214, -61.89583333196773651, 2.574251347313718519 ) ) ;
#13127 = CARTESIAN_POINT ( 'NONE',  ( 2.500000000000002220, -62.54166666393547303, 4.330127018922192761 ) ) ;
#13129 = VERTEX_POINT ( 'NONE', #33842 ) ;
#13128 = CARTESIAN_POINT ( 'NONE',  ( -4.458734124999999437, -11.56249999863440792, 0.000000000000000000 ) ) ;
#13130 = CARTESIAN_POINT ( 'NONE',  ( 1.060575238724906964E-15, -78.75000000000001421, 5.773502691896257311 ) ) ;
#13131 = CARTESIAN_POINT ( 'NONE',  ( -59.59170313451810586, -138.5000000013656063, 1.485763867205729394 ) ) ;
#13132 = CARTESIAN_POINT ( 'NONE',  ( 2.229367062499998831, -52.89583333196773651, -3.861377020970580887 ) ) ;
#13133 = VECTOR ( 'NONE', #40021, 1000.000000000000000 ) ;
#13134 = CARTESIAN_POINT ( 'NONE',  ( 5.000000000000000000, -75.29166666393547303, -2.886751345948129988 ) ) ;
#13136 = VERTEX_POINT ( 'NONE', #38657 ) ;
#13135 = CARTESIAN_POINT ( 'NONE',  ( 1.975475456537005874E-15, 10.37500000273118417, 5.000000000000000000 ) ) ;
#13137 = CARTESIAN_POINT ( 'NONE',  ( -52.53715891517739323, -149.4375000000000000, -4.819101127000233298 ) ) ;
#13138 = CARTESIAN_POINT ( 'NONE',  ( 4.458734125000001214, -20.14583333196774007, 2.574251347313718519 ) ) ;
#13140 = ORIENTED_EDGE ( 'NONE', *, *, #15362, .T. ) ;
#13139 = CARTESIAN_POINT ( 'NONE',  ( -4.458734124999998549, -56.47916666530107221, 2.574251347313722516 ) ) ;
#13141 =( NAMED_UNIT ( * ) PLANE_ANGLE_UNIT ( ) SI_UNIT ( $, .RADIAN. ) );
#13142 = CARTESIAN_POINT ( 'NONE',  ( 3.152801135295366208, -139.5625000013655779, 3.152801135295367985 ) ) ;
#13143 = CARTESIAN_POINT ( 'NONE',  ( -4.458734124999998549, -102.4791666653010509, 2.574251347313722516 ) ) ;
#13144 = VERTEX_POINT ( 'NONE', #14529 ) ;
#13145 = CARTESIAN_POINT ( 'NONE',  ( -58.39396692619412477, -151.6875000013656063, 2.891590998281057701 ) ) ;
#13146 = CARTESIAN_POINT ( 'NONE',  ( -53.33387254593733928, -140.9375000027312126, 5.149110718188519620 ) ) ;
#13147 = DIRECTION ( 'NONE',  ( 0.000000000000000000, 1.000000000000000000, 0.000000000000000000 ) ) ;
#13148 = CARTESIAN_POINT ( 'NONE',  ( 4.458734125000001214, -8.895833331967736513, 2.574251347313718519 ) ) ;
#13149 = CARTESIAN_POINT ( 'NONE',  ( 2.229367062499998831, -96.89583333196773651, -3.861377020970580887 ) ) ;
#13150 = CARTESIAN_POINT ( 'NONE',  ( 2.730187237215162345E-16, -148.4375000013656063, -4.458734124999999437 ) ) ;
#13151 = CARTESIAN_POINT ( 'NONE',  ( -4.458734124999998549, -29.47916666530106866, 2.574251347313722516 ) ) ;
#13152 = CARTESIAN_POINT ( 'NONE',  ( 1.975475456537005874E-15, -66.74999999999998579, 5.000000000000000000 ) ) ;
#13153 = CARTESIAN_POINT ( 'NONE',  ( -56.48576386720575471, -136.7500000013655779, -4.591703134518078322 ) ) ;
#13154 = CARTESIAN_POINT ( 'NONE',  ( -3.152548672688508926E-16, -64.81249999863440792, -5.148502694627439702 ) ) ;
#13155 = CARTESIAN_POINT ( 'NONE',  ( 2.500000000000002220, -21.54166666393548013, 4.330127018922192761 ) ) ;
#13156 = CARTESIAN_POINT ( 'NONE',  ( -2.500000000000000444, -34.16666666666666430, -4.330127018922193649 ) ) ;
#13157 = CARTESIAN_POINT ( 'NONE',  ( -3.152801135295367985, -140.8125000013655779, 3.152801135295367096 ) ) ;
#13158 = CARTESIAN_POINT ( 'NONE',  ( 4.458734124999998549, 11.02083333469892956, -2.574251347313721627 ) ) ;
#13159 = ORIENTED_EDGE ( 'NONE', *, *, #15760, .T. ) ;
#13160 = CARTESIAN_POINT ( 'NONE',  ( -2.071067811865415109, -164.4375000027311557, 5.000000000000062172 ) ) ;
#13161 = CARTESIAN_POINT ( 'NONE',  ( -6.972266317189433020E-16, 16.74999999999999645, -5.000000000000000000 ) ) ;
#13163 = CARTESIAN_POINT ( 'NONE',  ( 4.458734124999999437, -22.81249999863440436, -5.460374474430324690E-16 ) ) ;
#13162 = CARTESIAN_POINT ( 'NONE',  ( -3.535250795749689387E-16, -93.24999999999998579, -5.773502691896257311 ) ) ;
#13164 = CARTESIAN_POINT ( 'NONE',  ( -1.339745962155610925, 7.330341803992665994, 5.000000000000000000 ) ) ;
#13165 = CARTESIAN_POINT ( 'NONE',  ( 9.457646018065525792E-16, -77.31249999863440792, 5.148502694627439702 ) ) ;
#13166 = CARTESIAN_POINT ( 'NONE',  ( 4.458734124999999437, 25.93750000136559564, -5.460374474430324690E-16 ) ) ;
#13167 = DIRECTION ( 'NONE',  ( -0.000000000000000000, 1.000000000000000000, -0.000000000000000000 ) ) ;
#13168 = CARTESIAN_POINT ( 'NONE',  ( -57.19623071787017210, -144.3750000013656063, 4.297418129356382899 ) ) ;
#13169 = CARTESIAN_POINT ( 'NONE',  ( -4.458734124999997661, 4.770833334698926009, 2.574251347313722516 ) ) ;
#13170 = CARTESIAN_POINT ( 'NONE',  ( -1.339745962155610925, -62.66965819600734022, 5.000000000000000000 ) ) ;
#13171 =( BOUNDED_CURVE ( )  B_SPLINE_CURVE ( 2, ( #480, #53232, #59326, #43874, #19117, #38736, #9471, #19444, #43251 ),
 .UNSPECIFIED., .F., .F. ) 
 B_SPLINE_CURVE_WITH_KNOTS ( ( 3, 2, 2, 2, 3 ),
 ( 0.8375000000000000222, 0.8380952380952381153, 0.8392857142857143016, 0.8404761904761904878, 0.8410714285714285809 ),
 .UNSPECIFIED. ) 
 CURVE ( )  GEOMETRIC_REPRESENTATION_ITEM ( )  RATIONAL_B_SPLINE_CURVE ( ( 0.9330127018922194093, 0.9330127018922194093, 1.000000000000000000, 0.8660254037844387076, 1.000000000000000000, 0.8660254037844387076, 1.000000000000000000, 0.9330127018922194093, 0.9330127018922194093 ) ) 
 REPRESENTATION_ITEM ( '' )  );
#13172 = CARTESIAN_POINT ( 'NONE',  ( 1.975475456537005874E-15, -43.62499999726880873, 5.000000000000000000 ) ) ;
#13173 = CARTESIAN_POINT ( 'NONE',  ( 9.457646018065525792E-16, 6.937500001365595637, 5.148502694627439702 ) ) ;
#13174 = CARTESIAN_POINT ( 'NONE',  ( 2.229367062499998831, -72.64583333196773651, -3.861377020970580887 ) ) ;
#13175 = CARTESIAN_POINT ( 'NONE',  ( 4.458734124999998549, -17.97916666530106866, -2.574251347313721627 ) ) ;
#13176 =( BOUNDED_CURVE ( )  B_SPLINE_CURVE ( 2, ( #18196, #12732, #28471, #48398, #51978, #53233, #32669, #28155, #38132 ),
 .UNSPECIFIED., .F., .F. ) 
 B_SPLINE_CURVE_WITH_KNOTS ( ( 3, 2, 2, 2, 3 ),
 ( 0.8749999999999998890, 0.8791666666666665408, 0.8833333333333330817, 0.8874999999999997335, 0.8916666666666664964 ),
 .UNSPECIFIED. ) 
 CURVE ( )  GEOMETRIC_REPRESENTATION_ITEM ( )  RATIONAL_B_SPLINE_CURVE ( ( 1.000000000000001998, 0.9238795325112847401, 1.000000000000000000, 0.9238795325112867385, 1.000000000000000000, 0.9238795325112867385, 1.000000000000000000, 0.9238795325112908463, 0.9999999999999958922 ) ) 
 REPRESENTATION_ITEM ( '' )  );
#13177 = AXIS2_PLACEMENT_3D ( 'NONE', #19893, #951, #34363 ) ;
#13178 = CARTESIAN_POINT ( 'NONE',  ( 5.000000000000000888, -3.583333333333333925, 2.886751345948126879 ) ) ;
#13179 = CARTESIAN_POINT ( 'NONE',  ( -1.846868145590737420, -158.7500000013656063, 4.458734124999999437 ) ) ;
#13180 = CARTESIAN_POINT ( 'NONE',  ( -2.498395430326213474E-14, 15.37500000273118239, 5.000000000000000000 ) ) ;
#13181 = CARTESIAN_POINT ( 'NONE',  ( -2.229367062500000163, -61.47916666530106511, -3.861377020970580443 ) ) ;
#13182 = CARTESIAN_POINT ( 'NONE',  ( -4.999999999999999112, -100.7916666639354730, 2.886751345948131764 ) ) ;
#13183 = CARTESIAN_POINT ( 'NONE',  ( 4.458734124999998549, -38.72916666530106511, -2.574251347313721627 ) ) ;
#13184 = CYLINDRICAL_SURFACE ( 'NONE', #19450, 5.000000000000000000 ) ;
#13185 = CARTESIAN_POINT ( 'NONE',  ( 4.458734125000000326, -106.1458333319677365, 2.574251347313718519 ) ) ;
#13186 = CARTESIAN_POINT ( 'NONE',  ( -4.458734124999997661, -68.47916666530107932, 2.574251347313722516 ) ) ;
#13187 = CARTESIAN_POINT ( 'NONE',  ( 5.000000000000000000, -55.41666666666667140, -2.886751345948129988 ) ) ;
#13188 = DIRECTION ( 'NONE',  ( -0.000000000000000000, 1.000000000000000000, -0.000000000000000000 ) ) ;
#13189 = CARTESIAN_POINT ( 'NONE',  ( 2.500000000000002220, -36.54166666393547303, 4.330127018922192761 ) ) ;
#13190 = VERTEX_POINT ( 'NONE', #63443 ) ;
#13191 = CARTESIAN_POINT ( 'NONE',  ( -5.000000000000000000, 15.12500000273118417, 0.000000000000000000 ) ) ;
#13192 = CARTESIAN_POINT ( 'NONE',  ( -6.972266317189433020E-16, -68.12499999726881583, -5.000000000000000000 ) ) ;
#13193 = CARTESIAN_POINT ( 'NONE',  ( -2.500000000000000444, -11.16666666666666430, -4.330127018922193649 ) ) ;
#13194 = CARTESIAN_POINT ( 'NONE',  ( -2.229367062500000163, -14.47916666530107221, -3.861377020970580443 ) ) ;
#13195 = CARTESIAN_POINT ( 'NONE',  ( -4.458734124999997661, -75.22916666530106511, 2.574251347313722516 ) ) ;
#13196 = CIRCLE ( 'NONE', #52229, 5.000000000000000000 ) ;
#13197 = CARTESIAN_POINT ( 'NONE',  ( 2.499999999999998668, -59.20833333060214443, -4.330127018922193649 ) ) ;
#13198 = CARTESIAN_POINT ( 'NONE',  ( -2.500000000000000444, -12.04166666393547835, -4.330127018922193649 ) ) ;
#13200 = ORIENTED_EDGE ( 'NONE', *, *, #39783, .F. ) ;
#13199 = CARTESIAN_POINT ( 'NONE',  ( -3.152548672688508926E-16, -45.56249999863439371, -5.148502694627439702 ) ) ;
#13201 = CARTESIAN_POINT ( 'NONE',  ( 1.975475456537005874E-15, -81.74999999999998579, 5.000000000000000000 ) ) ;
#13203 = ORIENTED_EDGE ( 'NONE', *, *, #44444, .T. ) ;
#13202 = CARTESIAN_POINT ( 'NONE',  ( 2.229367062499998831, 6.104166668032262599, -3.861377020970580887 ) ) ;
#13204 = CARTESIAN_POINT ( 'NONE',  ( 5.000000000000000888, -81.58333333333332860, 2.886751345948126879 ) ) ;
#13205 = CARTESIAN_POINT ( 'NONE',  ( 5.000000000000000000, -62.50000000000000000, -6.123233995736766282E-16 ) ) ;
#13206 = CARTESIAN_POINT ( 'NONE',  ( -4.458734125000001214, -162.1250000013655779, 1.846868145590734089 ) ) ;
#13207 = CARTESIAN_POINT ( 'NONE',  ( 4.458734125000001214, -36.14583333196773651, 2.574251347313718519 ) ) ;
#13208 = CARTESIAN_POINT ( 'NONE',  ( 1.339745962155615144, -10.70534180126147916, 4.999999999999999112 ) ) ;
#13209 = CARTESIAN_POINT ( 'NONE',  ( -2.229367062499996610, -79.14583333196773651, 3.861377020970582219 ) ) ;
#13210 = CARTESIAN_POINT ( 'NONE',  ( -3.535533905932737309, -164.6250000000000284, -3.535533905932738197 ) ) ;
#13211 = CARTESIAN_POINT ( 'NONE',  ( -51.75738570946856498, -144.7500000000000284, 3.805975901505576964 ) ) ;
#13212 = CARTESIAN_POINT ( 'NONE',  ( -53.51423613279429503, -131.5000000013656347, 4.591703134518082763 ) ) ;
#13213 = CARTESIAN_POINT ( 'NONE',  ( 2.229367062500001939, -4.229166665301070438, 3.861377020970579999 ) ) ;
#13214 = CARTESIAN_POINT ( 'NONE',  ( -4.458734124999999437, -42.64583333196773651, -2.574251347313719407 ) ) ;
#13215 = CARTESIAN_POINT ( 'NONE',  ( -6.972266317189433020E-16, -26.25000000000000000, -5.000000000000000000 ) ) ;
#13216 = CARTESIAN_POINT ( 'NONE',  ( 2.229367062500001939, -81.22916666530106511, 3.861377020970579999 ) ) ;
#13217 = CARTESIAN_POINT ( 'NONE',  ( -2.499999999999996447, 16.29166666939785202, 4.330127018922195425 ) ) ;
#13218 = VERTEX_POINT ( 'NONE', #63129 ) ;
#13219 = AXIS2_PLACEMENT_3D ( 'NONE', #53763, #3948, #24184 ) ;
#13220 =( BOUNDED_CURVE ( )  B_SPLINE_CURVE ( 2, ( #6449, #26058, #50506, #20918, #21232, #55658, #16725, #30226, #40838 ),
 .UNSPECIFIED., .F., .F. ) 
 B_SPLINE_CURVE_WITH_KNOTS ( ( 3, 2, 2, 2, 3 ),
 ( 0.7645833333333332815, 0.7652777777777777235, 0.7666666666666667185, 0.7680555555555556024, 0.7687500000000000444 ),
 .UNSPECIFIED. ) 
 CURVE ( )  GEOMETRIC_REPRESENTATION_ITEM ( )  RATIONAL_B_SPLINE_CURVE ( ( 0.9330127018922194093, 0.9330127018922194093, 1.000000000000000000, 0.8660254037844387076, 1.000000000000000000, 0.8660254037844387076, 1.000000000000000000, 0.9330127018922194093, 0.9330127018922194093 ) ) 
 REPRESENTATION_ITEM ( '' )  );
#13221 = FACE_OUTER_BOUND ( 'NONE', #21755, .T. ) ;
#13222 = CARTESIAN_POINT ( 'NONE',  ( 4.458734124999999437, -69.06249999863439371, -5.460374474430324690E-16 ) ) ;
#13223 = AXIS2_PLACEMENT_3D ( 'NONE', #24592, #18806, #48707 ) ;
#13224 = CARTESIAN_POINT ( 'NONE',  ( -3.152801135295367096, -145.3125000013655779, -3.152801135295367541 ) ) ;
#13225 = ORIENTED_EDGE ( 'NONE', *, *, #3241, .F. ) ;
#13226 = DIRECTION ( 'NONE',  ( -0.000000000000000000, 1.000000000000000000, -0.000000000000000000 ) ) ;
#13227 = CARTESIAN_POINT ( 'NONE',  ( -2.229367062499996610, -11.39583333196773829, 3.861377020970582219 ) ) ;
#13228 = CARTESIAN_POINT ( 'NONE',  ( 0.000000000000000000, -120.0000000000000000, 0.000000000000000000 ) ) ;
#13229 = CARTESIAN_POINT ( 'NONE',  ( 4.458734124999999437, 1.187500001365596081, -5.460374474430324690E-16 ) ) ;
#13230 = CARTESIAN_POINT ( 'NONE',  ( 1.339745962155612702, -77.16965819600731891, -5.000000000000000000 ) ) ;
#13231 = CARTESIAN_POINT ( 'NONE',  ( -8.190561711645485556E-16, -158.6875000013655779, 4.458734124999999437 ) ) ;
#13232 = CARTESIAN_POINT ( 'NONE',  ( -4.458734124999997661, 27.52083333469892779, 2.574251347313722516 ) ) ;
#13233 = ORIENTED_EDGE ( 'NONE', *, *, #55161, .T. ) ;
#13234 = CARTESIAN_POINT ( 'NONE',  ( 2.229367062499998831, -91.64583333196773651, -3.861377020970580887 ) ) ;
#13235 = CARTESIAN_POINT ( 'NONE',  ( -75.00000000000000000, 0.000000000000000000, 8.999999999999998224 ) ) ;
#13236 = CARTESIAN_POINT ( 'NONE',  ( -2.499999999999996447, -62.83333333333333570, 4.330127018922195425 ) ) ;
#13237 = CARTESIAN_POINT ( 'NONE',  ( 4.458734124999998549, -6.729166665301073103, -2.574251347313721627 ) ) ;
#13238 = DIRECTION ( 'NONE',  ( -0.000000000000000000, 1.000000000000000000, -0.000000000000000000 ) ) ;
#13239 = CARTESIAN_POINT ( 'NONE',  ( 1.975475456537005874E-15, -23.62499999726880873, 5.000000000000000000 ) ) ;
#13240 = DIRECTION ( 'NONE',  ( 0.5000000000000069944, 0.000000000000000000, 0.8660254037844345998 ) ) ;
#13241 = CARTESIAN_POINT ( 'NONE',  ( 5.000000000000000888, -35.45833333060213732, 2.886751345948126879 ) ) ;
#13242 = CARTESIAN_POINT ( 'NONE',  ( 1.339745962155615144, -49.58034179853029144, 4.999999999999999112 ) ) ;
#13243 = CARTESIAN_POINT ( 'NONE',  ( 9.457646018065525792E-16, 16.93750000136559564, 5.148502694627439702 ) ) ;
#13244 = CARTESIAN_POINT ( 'NONE',  ( -1.339745962155610925, -20.66965819600733312, 5.000000000000000000 ) ) ;
#13245 = CARTESIAN_POINT ( 'NONE',  ( -4.458734124999999437, 21.68750000136559208, 0.000000000000000000 ) ) ;
#13246 = CARTESIAN_POINT ( 'NONE',  ( -3.152548672688508926E-16, -58.56249999863440081, -5.148502694627439702 ) ) ;
#13247 = CARTESIAN_POINT ( 'NONE',  ( 4.458734124999998549, -2.979166665301069106, -2.574251347313721627 ) ) ;
#13248 = FACE_OUTER_BOUND ( 'NONE', #16693, .T. ) ;
#13249 = CARTESIAN_POINT ( 'NONE',  ( -3.535250795749689387E-16, 9.749999999999998224, -5.773502691896257311 ) ) ;
#13250 = CARTESIAN_POINT ( 'NONE',  ( -2.071067811865478170, -140.4375000027312126, 5.000000000000000000 ) ) ;
#13251 = CARTESIAN_POINT ( 'NONE',  ( -4.999999999999998224, -45.91666666666665719, 2.886751345948131764 ) ) ;
#13252 = CARTESIAN_POINT ( 'NONE',  ( 2.229367062499998831, -48.64583333196772941, -3.861377020970580887 ) ) ;
#13253 = CARTESIAN_POINT ( 'NONE',  ( -5.000000000000000000, -85.95833333060213022, -2.886751345948128211 ) ) ;
#13254 = CARTESIAN_POINT ( 'NONE',  ( -50.55543936806279248, -135.3125000013656063, 0.3552334253322060320 ) ) ;
#13255 = CYLINDRICAL_SURFACE ( 'NONE', #50, 5.000000000000000000 ) ;
#13256 = DIRECTION ( 'NONE',  ( 0.000000000000000000, 0.000000000000000000, 1.000000000000000000 ) ) ;
#13257 = CARTESIAN_POINT ( 'NONE',  ( 4.458734124999998549, -91.97916666530106511, -2.574251347313721627 ) ) ;
#13258 = CARTESIAN_POINT ( 'NONE',  ( -4.458734124999999437, -158.2500000013656063, -1.846868145590735644 ) ) ;
#13259 = CARTESIAN_POINT ( 'NONE',  ( 2.500000000000002220, -32.66666666666666430, 4.330127018922192761 ) ) ;
#13260 = CARTESIAN_POINT ( 'NONE',  ( -9.184850993605147944E-16, -147.2500000000000284, 5.000000000000000000 ) ) ;
#13261 = ORIENTED_EDGE ( 'NONE', *, *, #55500, .F. ) ;
#13262 = CARTESIAN_POINT ( 'NONE',  ( 2.229367062499998831, 17.10416666803225993, -3.861377020970580887 ) ) ;
#13263 = ORIENTED_EDGE ( 'NONE', *, *, #11469, .T. ) ;
#13264 = CARTESIAN_POINT ( 'NONE',  ( 2.229367062499998831, -95.64583333196773651, -3.861377020970580887 ) ) ;
#13265 = CARTESIAN_POINT ( 'NONE',  ( 4.458734125000001214, 10.85416666803225993, 2.574251347313718519 ) ) ;
#13266 = PRESENTATION_LAYER_ASSIGNMENT (  '', '', ( #24551 ) ) ;
#13267 = CARTESIAN_POINT ( 'NONE',  ( 2.499999999999998668, 11.79166666939785202, -4.330127018922193649 ) ) ;
#13268 = CARTESIAN_POINT ( 'NONE',  ( -5.000000000000000000, -43.87499999726880873, 0.000000000000000000 ) ) ;
#13269 = CARTESIAN_POINT ( 'NONE',  ( 5.000000000000000888, 3.416666666666665186, 2.886751345948126879 ) ) ;
#13270 = VECTOR ( 'NONE', #52468, 1000.000000000000000 ) ;
#13271 = CARTESIAN_POINT ( 'NONE',  ( -4.458734124999999437, -61.39583333196774362, -2.574251347313719407 ) ) ;
#13272 = FACE_OUTER_BOUND ( 'NONE', #1938, .T. ) ;
#13273 = CARTESIAN_POINT ( 'NONE',  ( -4.999999999999999112, -80.91666666666667140, 2.886751345948131764 ) ) ;
#13274 = CARTESIAN_POINT ( 'NONE',  ( -2.229367062500000163, -29.47916666530107221, -3.861377020970580443 ) ) ;
#13275 = DIRECTION ( 'NONE',  ( -0.000000000000000000, 1.000000000000000000, -0.000000000000000000 ) ) ;
#13276 = CARTESIAN_POINT ( 'NONE',  ( -4.999999999999998224, 26.20833333606451632, 2.886751345948131764 ) ) ;
#13277 = DIRECTION ( 'NONE',  ( -0.000000000000000000, 1.000000000000000000, -0.000000000000000000 ) ) ;
#13278 = CARTESIAN_POINT ( 'NONE',  ( 5.000000000000000000, -39.49999999999999289, -6.123233995736766282E-16 ) ) ;
#13279 = CARTESIAN_POINT ( 'NONE',  ( 5.000000000000000000, -70.37499999726880162, -6.123233995736766282E-16 ) ) ;
#13281 = CARTESIAN_POINT ( 'NONE',  ( -4.458734124999998549, -21.47916666530107221, 2.574251347313722516 ) ) ;
#13280 = CARTESIAN_POINT ( 'NONE',  ( -6.972266317189433020E-16, -90.12499999726880162, -5.000000000000000000 ) ) ;
#13282 = CARTESIAN_POINT ( 'NONE',  ( 1.975475456537005874E-15, -57.74999999999999289, 5.000000000000000000 ) ) ;
#13283 = CARTESIAN_POINT ( 'NONE',  ( 4.458734124999998549, -62.72916666530106511, -2.574251347313721627 ) ) ;
#13284 = CARTESIAN_POINT ( 'NONE',  ( -1.846868145590734756, -147.3750000013656063, -4.458734125000000326 ) ) ;
#13286 = EDGE_CURVE ( 'NONE', #14049, #51281, #53461, .T. ) ;
#13285 = CARTESIAN_POINT ( 'NONE',  ( 4.458734124999998549, -75.72916666530106511, -2.574251347313721627 ) ) ;
#13287 = CARTESIAN_POINT ( 'NONE',  ( -50.55543936806279248, -142.3125000013656063, 0.3552334253322060320 ) ) ;
#13288 = CARTESIAN_POINT ( 'NONE',  ( -3.152548672688508926E-16, -26.81249999863440436, -5.148502694627439702 ) ) ;
#13289 = CARTESIAN_POINT ( 'NONE',  ( 2.499999999999998668, -64.20833333060213022, -4.330127018922193649 ) ) ;
#13290 = ORIENTED_EDGE ( 'NONE', *, *, #36629, .F. ) ;
#13291 = CARTESIAN_POINT ( 'NONE',  ( 1.975475456537005874E-15, -1.749999999999999334, 5.000000000000000000 ) ) ;
#13292 = ORIENTED_EDGE ( 'NONE', *, *, #36817, .F. ) ;
#13293 = CARTESIAN_POINT ( 'NONE',  ( -3.152548672688508926E-16, -67.81249999863440792, -5.148502694627439702 ) ) ;
#13294 = CARTESIAN_POINT ( 'NONE',  ( 3.535533905932736864, -149.2500000027311842, 3.535533905932738641 ) ) ;
#13295 = CARTESIAN_POINT ( 'NONE',  ( -6.972266317189433020E-16, -91.24999999999998579, -5.000000000000000000 ) ) ;
#13296 = ORIENTED_EDGE ( 'NONE', *, *, #45205, .T. ) ;
#13297 = CARTESIAN_POINT ( 'NONE',  ( 0.000000000000000000, -120.0000000000000000, 0.000000000000000000 ) ) ;
#13298 = CARTESIAN_POINT ( 'NONE',  ( -1.339745962155613812, -78.08034179853028434, -5.000000000000000000 ) ) ;
#13299 = CARTESIAN_POINT ( 'NONE',  ( -2.229367062500000163, -55.72916666530107221, -3.861377020970580443 ) ) ;
#13300 = ORIENTED_EDGE ( 'NONE', *, *, #7900, .T. ) ;
#13301 =( BOUNDED_CURVE ( )  B_SPLINE_CURVE ( 2, ( #8872, #27856, #13386, #32373, #38149, #62606, #61658, #57155, #61973 ),
 .UNSPECIFIED., .F., .F. ) 
 B_SPLINE_CURVE_WITH_KNOTS ( ( 3, 2, 2, 2, 3 ),
 ( 0.6312499999999999778, 0.6319444444444444198, 0.6333333333333333037, 0.6347222222222221877, 0.6354166666666666297 ),
 .UNSPECIFIED. ) 
 CURVE ( )  GEOMETRIC_REPRESENTATION_ITEM ( )  RATIONAL_B_SPLINE_CURVE ( ( 0.9330127018922194093, 0.9330127018922194093, 1.000000000000000000, 0.8660254037844387076, 1.000000000000000000, 0.8660254037844387076, 1.000000000000000000, 0.9330127018922194093, 0.9330127018922194093 ) ) 
 REPRESENTATION_ITEM ( '' )  );
#13302 = EDGE_CURVE ( 'NONE', #55786, #13440, #3785, .T. ) ;
#13303 = CARTESIAN_POINT ( 'NONE',  ( -5.000000000000000000, 2.125000002731185056, 0.000000000000000000 ) ) ;
#13304 = EDGE_CURVE ( 'NONE', #28142, #17776, #5846, .T. ) ;
#13305 = CARTESIAN_POINT ( 'NONE',  ( -4.458734124999998549, 4.770833334698926009, 2.574251347313722516 ) ) ;
#13306 = CARTESIAN_POINT ( 'NONE',  ( -3.152548672688508926E-16, 16.43750000136559564, -5.148502694627439702 ) ) ;
#13307 = CARTESIAN_POINT ( 'NONE',  ( -59.29741812935640155, -145.6250000013655779, -2.196230717870135685 ) ) ;
#13308 = CARTESIAN_POINT ( 'NONE',  ( -51.75738570946856498, -155.0000000000000284, 3.805975901505577408 ) ) ;
#13309 = CARTESIAN_POINT ( 'NONE',  ( 5.000000000000000000, -165.0625000000000000, 2.071067811865478614 ) ) ;
#13310 = PRODUCT_DEFINITION_FORMATION_WITH_SPECIFIED_SOURCE ( 'ANY', '', #5039, .NOT_KNOWN. ) ;
#13311 = ORIENTED_EDGE ( 'NONE', *, *, #19764, .T. ) ;
#13312 = CARTESIAN_POINT ( 'NONE',  ( 4.458734124999998549, -73.72916666530106511, -2.574251347313721627 ) ) ;
#13313 = DIRECTION ( 'NONE',  ( 0.000000000000000000, 1.000000000000000000, 0.000000000000000000 ) ) ;
#13314 = CARTESIAN_POINT ( 'NONE',  ( 9.457646018065525792E-16, 4.937500001365596525, 5.148502694627439702 ) ) ;
#13315 = EDGE_CURVE ( 'NONE', #61278, #15327, #15226, .T. ) ;
#13316 = CARTESIAN_POINT ( 'NONE',  ( 1.975475456537005874E-15, -59.74999999999999289, 5.000000000000000000 ) ) ;
#13317 = CARTESIAN_POINT ( 'NONE',  ( 4.458734124999998549, -60.97916666530106511, -2.574251347313721627 ) ) ;
#13318 = CARTESIAN_POINT ( 'NONE',  ( -5.000000000000000000, -17.87499999726881583, 0.000000000000000000 ) ) ;
#13319 = CARTESIAN_POINT ( 'NONE',  ( -6.972266317189433020E-16, -100.2499999999999858, -5.000000000000000000 ) ) ;
#13320 = CARTESIAN_POINT ( 'NONE',  ( 6.123233995736766282E-16, -170.0000000000000000, -5.000000000000000000 ) ) ;
#13321 = LINE ( 'NONE', #8498, #751 ) ;
#13322 = CARTESIAN_POINT ( 'NONE',  ( -6.972266317189433020E-16, -57.12499999726880162, -5.000000000000000000 ) ) ;
#13323 = DIRECTION ( 'NONE',  ( 1.000000000000000000, 0.000000000000000000, 0.000000000000000000 ) ) ;
#13324 = CARTESIAN_POINT ( 'NONE',  ( 2.229367062499998831, -38.64583333196773651, -3.861377020970580887 ) ) ;
#13325 = CARTESIAN_POINT ( 'NONE',  ( -2.229367062500000163, -25.72916666530106866, -3.861377020970580443 ) ) ;
#13326 = CARTESIAN_POINT ( 'NONE',  ( -55.39835681537999790, -143.8750000000000284, 4.984105922594378235 ) ) ;
#13327 = CARTESIAN_POINT ( 'NONE',  ( -2.229367062499996610, -109.1458333319677365, 3.861377020970582219 ) ) ;
#13328 = CARTESIAN_POINT ( 'NONE',  ( -2.071067811865478170, -152.4375000027311842, 5.000000000000000000 ) ) ;
#13329 = ORIENTED_EDGE ( 'NONE', *, *, #37350, .T. ) ;
#13330 = CARTESIAN_POINT ( 'NONE',  ( 2.229367062500001939, -107.2291666653010651, 3.861377020970579999 ) ) ;
#13331 = CARTESIAN_POINT ( 'NONE',  ( 4.458734124999998549, -30.72916666530107221, -2.574251347313721627 ) ) ;
#13332 = CARTESIAN_POINT ( 'NONE',  ( -2.500000000000000444, -70.04166666393547303, -4.330127018922193649 ) ) ;
#13333 = CARTESIAN_POINT ( 'NONE',  ( -59.59170313451811296, -146.7500000013655495, 1.485763867205729394 ) ) ;
#13334 = CARTESIAN_POINT ( 'NONE',  ( -5.000000000000000888, -148.4375000000000284, 2.071067811865474617 ) ) ;
#13335 = EDGE_CURVE ( 'NONE', #59584, #50115, #32132, .T. ) ;
#13336 = CARTESIAN_POINT ( 'NONE',  ( 9.457646018065525792E-16, -27.06249999863440081, 5.148502694627439702 ) ) ;
#13337 = CARTESIAN_POINT ( 'NONE',  ( -4.458734124999999437, -71.56249999863439371, 0.000000000000000000 ) ) ;
#13338 = CARTESIAN_POINT ( 'NONE',  ( -1.846868145590734756, -168.3750000013655779, -4.458734124999999437 ) ) ;
#13339 = CARTESIAN_POINT ( 'NONE',  ( 4.458734125000000326, -27.89583333196774007, 2.574251347313718519 ) ) ;
#13340 = PLANE ( 'NONE',  #59479 ) ;
#13341 = CARTESIAN_POINT ( 'NONE',  ( -5.000000000000000000, 9.041666669397853795, -2.886751345948128211 ) ) ;
#13342 = CARTESIAN_POINT ( 'NONE',  ( -5.000000000000000000, -18.00000000000000355, 0.000000000000000000 ) ) ;
#13343 = CARTESIAN_POINT ( 'NONE',  ( 1.846868145590736310, -149.6250000013655779, 4.458734124999999437 ) ) ;
#13344 = ORIENTED_EDGE ( 'NONE', *, *, #35407, .T. ) ;
#13345 = DIRECTION ( 'NONE',  ( -0.000000000000000000, 1.000000000000000000, -0.000000000000000000 ) ) ;
#13346 = CARTESIAN_POINT ( 'NONE',  ( -4.458734124999997661, -58.47916666530106511, 2.574251347313722516 ) ) ;
#13347 = CARTESIAN_POINT ( 'NONE',  ( 2.499999999999998668, 27.79166666939785202, -4.330127018922193649 ) ) ;
#13348 = DIRECTION ( 'NONE',  ( -0.000000000000000000, 1.000000000000000000, -0.000000000000000000 ) ) ;
#13349 = CARTESIAN_POINT ( 'NONE',  ( 2.500000000000002220, 16.33333333333333215, 4.330127018922192761 ) ) ;
#13350 = CARTESIAN_POINT ( 'NONE',  ( -4.999999999999998224, 8.208333336064518093, 2.886751345948131764 ) ) ;
#13351 = CARTESIAN_POINT ( 'NONE',  ( -4.458734124999999437, -1.312499998634406140, 0.000000000000000000 ) ) ;
#13352 = CARTESIAN_POINT ( 'NONE',  ( 0.000000000000000000, -170.0000000000000000, 5.000000000000000000 ) ) ;
#13353 = CARTESIAN_POINT ( 'NONE',  ( 6.123233995736766282E-16, -120.0000000000000000, -5.000000000000000000 ) ) ;
#13354 = CARTESIAN_POINT ( 'NONE',  ( 4.458734124999999437, 11.93750000136559564, -5.460374474430324690E-16 ) ) ;
#13355 = VERTEX_POINT ( 'NONE', #5209 ) ;
#13356 = CARTESIAN_POINT ( 'NONE',  ( -75.00000000000000000, 15.00000000000000000, 8.999999999999998224 ) ) ;
#13357 = ORIENTED_EDGE ( 'NONE', *, *, #14246, .F. ) ;
#13358 = CARTESIAN_POINT ( 'NONE',  ( -5.000000000000000000, -23.87499999726881228, 0.000000000000000000 ) ) ;
#13359 = CARTESIAN_POINT ( 'NONE',  ( -2.229367062500000163, -48.47916666530106511, -3.861377020970580443 ) ) ;
#13360 = CARTESIAN_POINT ( 'NONE',  ( 4.458734124999999437, -161.7500000013655495, 1.846868145590737864 ) ) ;
#13361 = AXIS2_PLACEMENT_3D ( 'NONE', #18249, #23081, #47213 ) ;
#13362 = EDGE_CURVE ( 'NONE', #60689, #28617, #45401, .T. ) ;
#13363 = CARTESIAN_POINT ( 'NONE',  ( -5.000000000000000000, -49.87499999726881583, 0.000000000000000000 ) ) ;
#13364 = EDGE_CURVE ( 'NONE', #57658, #38838, #12793, .T. ) ;
#13365 = ORIENTED_EDGE ( 'NONE', *, *, #12119, .T. ) ;
#13366 = CARTESIAN_POINT ( 'NONE',  ( 4.458734124999999437, -24.81249999863440436, -5.460374474430324690E-16 ) ) ;
#13367 = ORIENTED_EDGE ( 'NONE', *, *, #33924, .F. ) ;
#13369 = CARTESIAN_POINT ( 'NONE',  ( 3.535533905932738197, -169.8750000000000284, -3.535533905932738197 ) ) ;
#13368 = CARTESIAN_POINT ( 'NONE',  ( -6.972266317189433020E-16, -34.25000000000000000, -5.000000000000000000 ) ) ;
#13370 = CARTESIAN_POINT ( 'NONE',  ( -1.846868145590734756, -162.1250000013655779, -4.458734125000000326 ) ) ;
#13371 =( BOUNDED_CURVE ( )  B_SPLINE_CURVE ( 2, ( #48055, #42913, #18777, #42287, #32958, #62865, #61927, #17846, #58027, #13956, #37469, #52268, #62561, #32638, #4312, #13020, #8205, #27808, #47433, #23002, #42603, #13338, #53202, #9136, #62240, #18159, #37787, #28744, #28124, #57417, #48370, #47742, #23932, #19416, #34201, #44810, #54140, #25195, #39030, #44486, #24563, #59294, #4940, #34854, #29360, #45133, #58657, #44168, #9753, #43845, #14273, #33892, #49642, #53514, #49321, #15225, #20053, #5579, #25515, #447, #48993, #39979, #49956, #772, #9443, #135, #53824, #29052, #20706, #19729, #1097, #39657, #10402, #15557, #14579, #30014, #48676, #4616, #58345, #20379, #59625, #35177, #54795, #39342, #58973, #63491, #5265, #10723, #54475, #14900, #24241, #24885, #30330, #5908, #34509, #10079, #29690, #7184, #46723, #7498, #36764, #36126, #2668, #51249, #17140, #21335, #15872, #40935, #50919, #21018, #2050, #16186, #31613, #30658, #27110, #59949, #55110, #11035, #35813, #56392, #6861, #60268, #6225, #45453, #26792, #16505, #25837, #46412, #1419, #21658, #40625, #55437, #2361, #55748, #21970, #11353, #26476, #6541, #30975, #50599, #41249, #26154, #40311, #45773, #1731, #60585, #11665, #35492, #50280, #41563, #31284, #46090, #60895, #16819, #61214, #36438, #56068, #11987, #12320, #31931, #51559, #17467, #27733, #61854, #37089, #48292, #12940, #9062, #3620, #38023, #43150, #42208, #57655, #41889, #56707, #28672, #8753, #47979, #47361, #33200, #52815, #22613, #27415, #13258, #18709, #42841, #32563, #12626, #32882, #23552, #23227, #3309, #22930, #22290, #28358, #61535, #53130, #38334, #17771, #13884, #3933, #62790, #42524, #32242, #62161, #52510, #2996, #47668, #37390, #13581, #51871, #18402, #8445, #28048, #57963, #18081, #7813, #37704, #62484, #33512, #47046, #57025, #52185, #8130, #57342, #63108, #24487, #59221, #19019, #38632, #54398, #49247, #23859, #43774, #58894, #24170, #59548, #30253, #4868, #14823, #34437, #54720, #34774, #10327, #28983, #15483, #35102, #5502, #10640, #5190, #44410, #63420, #29938, #29289, #371, #24806, #4244, #15153, #19976, #14506, #39584, #58275, #14194, #49564, #9372, #48606, #39903, #20302, #33819, #25118, #19338, #48919, #44730, #54066, #44093, #43462, #53439, #57, #690, #4545, #38950, #9682, #58588, #34128, #53749, #19654, #39266, #10005, #29617, #22455, #10958, #56554, #5825, #1026, #52038, #27269, #46896, #40549, #32087, #51722, #42053, #15796, #7349, #17626, #61378, #1345, #20631, #26959, #61696, #17299, #60190, #16987, #7978, #7663, #49876, #25440, #56868, #25768, #32408, #37243, #12786, #12156, #40237, #31775, #2519, #50201, #36927, #45380, #2837, #45060, #59874, #12475, #35413, #55034, #30580, #6152, #20947, #36602, #56234, #51406, #46577, #22135, #41730, #8409, #23191, #14708, #42804, #20184, #28011, #44295, #15358, #62445, #34983, #59106, #18365, #37987, #57619, #257, #34327, #54598, #5390, #13546, #15033, #47628, #3584, #10520, #59429, #57307, #44615, #33167, #23515, #10213, #53952, #63618, #30134, #42485, #43972, #25005, #49763, #29816, #37664, #62124, #39469, #19539, #18041, #49448, #52781, #575, #5709, #9883, #13224, #5067, #8710, #39782, #32845, #52473, #28324, #47941, #3894, #39153, #58778, #29489, #49125, #24687, #19855, #34649, #54273, #40744, #25324, #6666, #46217, #51370, #21139, #15676, #12113, #60710, #60391, #16317, #31739, #36251, #2180, #56193, #55566, #11790, #30458, #6040, #35938, #51046, #11164, #21463, #35295, #36562, #16630, #40427, #35616, #55878, #902, #54915, #20826, #26273, #31408, #25645, #21785, #10842, #45261, #11481, #1227, #41377, #50083, #45895, #61023, #60067, #16949, #41063, #15991, #55242, #30786, #1857, #31101, #44944, #6989, #50409, #20509, #50722, #26601, #40108, #59751, #6357, #25961, #45578, #1534, #8557, #18528, #8254, #47475, #27230, #33006, #32371, #3429, #52319, #7311 ),
 .UNSPECIFIED., .F., .F. ) 
 B_SPLINE_CURVE_WITH_KNOTS ( ( 3, 2, 2, 2, 2, 2, 2, 2, 2, 2, 2, 2, 2, 2, 2, 2, 2, 2, 2, 2, 2, 2, 2, 2, 2, 2, 2, 2, 2, 2, 2, 2, 2, 2, 2, 2, 2, 2, 2, 2, 2, 2, 2, 2, 2, 2, 2, 2, 2, 2, 2, 2, 2, 2, 2, 2, 2, 2, 2, 2, 2, 2, 2, 2, 2, 2, 2, 2, 2, 2, 2, 2, 2, 2, 2, 2, 2, 2, 2, 2, 2, 2, 2, 2, 2, 2, 2, 2, 2, 2, 2, 2, 2, 2, 2, 2, 2, 2, 2, 2, 2, 2, 2, 2, 2, 2, 2, 2, 2, 2, 2, 2, 2, 2, 2, 2, 2, 2, 2, 2, 2, 2, 2, 2, 2, 2, 2, 2, 2, 2, 2, 2, 2, 2, 2, 2, 2, 2, 2, 2, 2, 2, 2, 2, 2, 2, 2, 2, 2, 2, 2, 2, 2, 2, 2, 2, 2, 2, 2, 2, 2, 2, 2, 2, 2, 2, 2, 2, 2, 2, 2, 2, 2, 2, 2, 2, 2, 2, 2, 2, 2, 2, 2, 2, 2, 2, 2, 2, 2, 2, 2, 2, 2, 2, 2, 2, 2, 2, 2, 2, 2, 2, 2, 2, 2, 2, 2, 2, 2, 2, 2, 2, 2, 2, 2, 2, 2, 2, 2, 2, 2, 2, 2, 2, 2, 2, 2, 2, 2, 2, 2, 2, 2, 2, 2, 2, 2, 2, 2, 2, 3 ),
 ( 0.000000000000000000, 0.004166666666666666609, 0.008333333333333333218, 0.01250000000000000069, 0.01666666666666666644, 0.02083333333333333218, 0.02500000000000000139, 0.02916666666666666713, 0.03333333333333333287, 0.03749999999999999861, 0.04166666666666666435, 0.04583333333333333010, 0.05000000000000000278, 0.05416666666666666852, 0.05833333333333333426, 0.06250000000000000000, 0.06666666666666666574, 0.07083333333333333148, 0.07499999999999999722, 0.07916666666666666297, 0.08333333333333332871, 0.08749999999999999445, 0.09166666666666666019, 0.09583333333333333981, 0.1000000000000000056, 0.1041666666666666713, 0.1083333333333333370, 0.1125000000000000028, 0.1166666666666666685, 0.1208333333333333343, 0.1250000000000000000, 0.1291666666666666796, 0.1333333333333333315, 0.1375000000000000111, 0.1416666666666666630, 0.1458333333333333426, 0.1499999999999999944, 0.1541666666666666741, 0.1583333333333333259, 0.1625000000000000056, 0.1666666666666666574, 0.1708333333333333370, 0.1749999999999999889, 0.1791666666666666685, 0.1833333333333333204, 0.1875000000000000000, 0.1916666666666666796, 0.1958333333333333315, 0.2000000000000000111, 0.2041666666666666630, 0.2083333333333333426, 0.2124999999999999944, 0.2166666666666666741, 0.2208333333333333259, 0.2250000000000000056, 0.2291666666666666574, 0.2333333333333333370, 0.2374999999999999889, 0.2416666666666666685, 0.2458333333333333204, 0.2500000000000000000, 0.2541666666666666519, 0.2583333333333333592, 0.2625000000000000111, 0.2666666666666666630, 0.2708333333333333148, 0.2750000000000000222, 0.2791666666666666741, 0.2833333333333333259, 0.2874999999999999778, 0.2916666666666666852, 0.2958333333333333370, 0.2999999999999999889, 0.3041666666666666408, 0.3083333333333333481, 0.3125000000000000000, 0.3166666666666666519, 0.3208333333333333592, 0.3250000000000000111, 0.3291666666666666630, 0.3333333333333333148, 0.3375000000000000222, 0.3416666666666666741, 0.3458333333333333259, 0.3499999999999999778, 0.3541666666666666852, 0.3583333333333333370, 0.3624999999999999889, 0.3666666666666666408, 0.3708333333333333481, 0.3750000000000000000, 0.3791666666666666519, 0.3833333333333333592, 0.3875000000000000111, 0.3916666666666666630, 0.3958333333333333148, 0.4000000000000000222, 0.4041666666666666741, 0.4083333333333333259, 0.4124999999999999778, 0.4166666666666666852, 0.4208333333333333370, 0.4249999999999999889, 0.4291666666666666408, 0.4333333333333333481, 0.4375000000000000000, 0.4416666666666666519, 0.4458333333333333592, 0.4500000000000000111, 0.4541666666666666630, 0.4583333333333333148, 0.4625000000000000222, 0.4666666666666666741, 0.4708333333333333259, 0.4749999999999999778, 0.4791666666666666852, 0.4833333333333333370, 0.4874999999999999889, 0.4916666666666666408, 0.4958333333333333481, 0.5000000000000000000, 0.5041666666666666519, 0.5083333333333333037, 0.5124999999999999556, 0.5166666666666667185, 0.5208333333333333703, 0.5250000000000000222, 0.5291666666666666741, 0.5333333333333333259, 0.5374999999999999778, 0.5416666666666666297, 0.5458333333333332815, 0.5500000000000000444, 0.5541666666666666963, 0.5583333333333333481, 0.5625000000000000000, 0.5666666666666666519, 0.5708333333333333037, 0.5749999999999999556, 0.5791666666666667185, 0.5833333333333333703, 0.5875000000000000222, 0.5916666666666666741, 0.5958333333333333259, 0.5999999999999999778, 0.6041666666666666297, 0.6083333333333332815, 0.6125000000000000444, 0.6166666666666666963, 0.6208333333333333481, 0.6250000000000000000, 0.6291666666666666519, 0.6333333333333333037, 0.6374999999999999556, 0.6416666666666667185, 0.6458333333333333703, 0.6500000000000000222, 0.6541666666666666741, 0.6583333333333333259, 0.6624999999999999778, 0.6666666666666666297, 0.6708333333333332815, 0.6750000000000000444, 0.6791666666666666963, 0.6833333333333333481, 0.6875000000000000000, 0.6916666666666666519, 0.6958333333333333037, 0.6999999999999999556, 0.7041666666666667185, 0.7083333333333333703, 0.7125000000000000222, 0.7166666666666666741, 0.7208333333333333259, 0.7249999999999999778, 0.7291666666666666297, 0.7333333333333332815, 0.7375000000000000444, 0.7416666666666666963, 0.7458333333333333481, 0.7500000000000000000, 0.7541666666666666519, 0.7583333333333333037, 0.7624999999999999556, 0.7666666666666667185, 0.7708333333333333703, 0.7750000000000000222, 0.7791666666666666741, 0.7833333333333333259, 0.7874999999999999778, 0.7916666666666666297, 0.7958333333333332815, 0.8000000000000000444, 0.8041666666666666963, 0.8083333333333333481, 0.8125000000000000000, 0.8166666666666666519, 0.8208333333333333037, 0.8249999999999999556, 0.8291666666666667185, 0.8333333333333333703, 0.8375000000000000222, 0.8416666666666666741, 0.8458333333333333259, 0.8499999999999999778, 0.8541666666666666297, 0.8583333333333332815, 0.8625000000000000444, 0.8666666666666666963, 0.8708333333333333481, 0.8750000000000000000, 0.8791666666666666519, 0.8833333333333333037, 0.8874999999999999556, 0.8916666666666667185, 0.8958333333333333703, 0.9000000000000000222, 0.9041666666666666741, 0.9083333333333333259, 0.9124999999999999778, 0.9166666666666666297, 0.9208333333333332815, 0.9250000000000000444, 0.9291666666666666963, 0.9333333333333333481, 0.9375000000000000000, 0.9416666666666666519, 0.9458333333333333037, 0.9499999999999999556, 0.9541666666666667185, 0.9583333333333333703, 0.9625000000000000222, 0.9666666666666666741, 0.9708333333333333259, 0.9749999999999999778, 0.9791666666666666297, 0.9833333333333332815, 0.9875000000000000444, 0.9916666666666666963, 0.9958333333333333481, 1.000000000000000000 ),
 .UNSPECIFIED. ) 
 CURVE ( )  GEOMETRIC_REPRESENTATION_ITEM ( )  RATIONAL_B_SPLINE_CURVE ( ( 1.000000000000000000, 0.9238795325112867385, 1.000000000000000000, 0.9238795325112867385, 1.000000000000000000, 0.9238795325112867385, 1.000000000000000000, 0.9238795325112867385, 1.000000000000000000, 0.9238795325112867385, 1.000000000000000000, 0.9238795325112867385, 1.000000000000000000, 0.9238795325112867385, 1.000000000000000000, 0.9238795325112867385, 1.000000000000000000, 0.9238795325112867385, 1.000000000000000000, 0.9238795325112867385, 1.000000000000000000, 0.9238795325112867385, 1.000000000000000000, 0.9238795325112867385, 1.000000000000000000, 0.9238795325112867385, 1.000000000000000000, 0.9238795325112867385, 1.000000000000000000, 0.9238795325112867385, 1.000000000000000000, 0.9238795325112867385, 1.000000000000000000, 0.9238795325112867385, 1.000000000000000000, 0.9238795325112867385, 1.000000000000000000, 0.9238795325112867385, 1.000000000000000000, 0.9238795325112867385, 1.000000000000000000, 0.9238795325112867385, 1.000000000000000000, 0.9238795325112867385, 1.000000000000000000, 0.9238795325112867385, 1.000000000000000000, 0.9238795325112867385, 1.000000000000000000, 0.9238795325112867385, 1.000000000000000000, 0.9238795325112867385, 1.000000000000000000, 0.9238795325112867385, 1.000000000000000000, 0.9238795325112867385, 1.000000000000000000, 0.9238795325112867385, 1.000000000000000000, 0.9238795325112867385, 1.000000000000000000, 0.9238795325112867385, 1.000000000000000000, 0.9238795325112867385, 1.000000000000000000, 0.9238795325112867385, 1.000000000000000000, 0.9238795325112867385, 1.000000000000000000, 0.9238795325112867385, 1.000000000000000000, 0.9238795325112867385, 1.000000000000000000, 0.9238795325112867385, 1.000000000000000000, 0.9238795325112867385, 1.000000000000000000, 0.9238795325112867385, 1.000000000000000000, 0.9238795325112867385, 1.000000000000000000, 0.9238795325112867385, 1.000000000000000000, 0.9238795325112867385, 1.000000000000000000, 0.9238795325112867385, 1.000000000000000000, 0.9238795325112867385, 1.000000000000000000, 0.9238795325112867385, 1.000000000000000000, 0.9238795325112867385, 1.000000000000000000, 0.9238795325112867385, 1.000000000000000000, 0.9238795325112867385, 1.000000000000000000, 0.9238795325112867385, 1.000000000000000000, 0.9238795325112867385, 1.000000000000000000, 0.9238795325112867385, 1.000000000000000000, 0.9238795325112867385, 1.000000000000000000, 0.9238795325112867385, 1.000000000000000000, 0.9238795325112867385, 1.000000000000000000, 0.9238795325112867385, 1.000000000000000000, 0.9238795325112867385, 1.000000000000000000, 0.9238795325112867385, 1.000000000000000000, 0.9238795325112867385, 1.000000000000000000, 0.9238795325112867385, 1.000000000000000000, 0.9238795325112867385, 1.000000000000000000, 0.9238795325112867385, 1.000000000000000000, 0.9238795325112867385, 1.000000000000000000, 0.9238795325112867385, 1.000000000000000000, 0.9238795325112867385, 1.000000000000000000, 0.9238795325112867385, 1.000000000000000000, 0.9238795325112867385, 1.000000000000000000, 0.9238795325112867385, 1.000000000000000000, 0.9238795325112867385, 1.000000000000000000, 0.9238795325112867385, 1.000000000000000000, 0.9238795325112867385, 1.000000000000000000, 0.9238795325112867385, 1.000000000000000000, 0.9238795325112867385, 1.000000000000000000, 0.9238795325112867385, 1.000000000000000000, 0.9238795325112867385, 1.000000000000000000, 0.9238795325112867385, 1.000000000000000000, 0.9238795325112867385, 1.000000000000000000, 0.9238795325112867385, 1.000000000000000000, 0.9238795325112867385, 1.000000000000000000, 0.9238795325112867385, 1.000000000000000000, 0.9238795325112867385, 1.000000000000000000, 0.9238795325112867385, 1.000000000000000000, 0.9238795325112867385, 1.000000000000000000, 0.9238795325112867385, 1.000000000000000000, 0.9238795325112867385, 1.000000000000000000, 0.9238795325112867385, 1.000000000000000000, 0.9238795325112867385, 1.000000000000000000, 0.9238795325112867385, 1.000000000000000000, 0.9238795325112867385, 1.000000000000000000, 0.9238795325112867385, 1.000000000000000000, 0.9238795325112867385, 1.000000000000000000, 0.9238795325112867385, 1.000000000000000000, 0.9238795325112867385, 1.000000000000000000, 0.9238795325112867385, 1.000000000000000000, 0.9238795325112867385, 1.000000000000000000, 0.9238795325112867385, 1.000000000000000000, 0.9238795325112867385, 1.000000000000000000, 0.9238795325112867385, 1.000000000000000000, 0.9238795325112867385, 1.000000000000000000, 0.9238795325112867385, 1.000000000000000000, 0.9238795325112867385, 1.000000000000000000, 0.9238795325112867385, 1.000000000000000000, 0.9238795325112867385, 1.000000000000000000, 0.9238795325112867385, 1.000000000000000000, 0.9238795325112867385, 1.000000000000000000, 0.9238795325112867385, 1.000000000000000000, 0.9238795325112867385, 1.000000000000000000, 0.9238795325112867385, 1.000000000000000000, 0.9238795325112867385, 1.000000000000000000, 0.9238795325112867385, 1.000000000000000000, 0.9238795325112867385, 1.000000000000000000, 0.9238795325112867385, 1.000000000000000000, 0.9238795325112867385, 1.000000000000000000, 0.9238795325112867385, 1.000000000000000000, 0.9238795325112867385, 1.000000000000000000, 0.9238795325112867385, 1.000000000000000000, 0.9238795325112867385, 1.000000000000000000, 0.9238795325112867385, 1.000000000000000000, 0.9238795325112867385, 1.000000000000000000, 0.9238795325112867385, 1.000000000000000000, 0.9238795325112867385, 1.000000000000000000, 0.9238795325112867385, 1.000000000000000000, 0.9238795325112867385, 1.000000000000000000, 0.9238795325112867385, 1.000000000000000000, 0.9238795325112867385, 1.000000000000000000, 0.9238795325112867385, 1.000000000000000000, 0.9238795325112867385, 1.000000000000000000, 0.9238795325112867385, 1.000000000000000000, 0.9238795325112867385, 1.000000000000000000, 0.9238795325112867385, 1.000000000000000000, 0.9238795325112867385, 1.000000000000000000, 0.9238795325112867385, 1.000000000000000000, 0.9238795325112867385, 1.000000000000000000, 0.9238795325112867385, 1.000000000000000000, 0.9238795325112867385, 1.000000000000000000, 0.9238795325112867385, 1.000000000000000000, 0.9238795325112867385, 1.000000000000000000, 0.9238795325112867385, 1.000000000000000000, 0.9238795325112867385, 1.000000000000000000, 0.9238795325112867385, 1.000000000000000000, 0.9238795325112867385, 1.000000000000000000, 0.9238795325112867385, 1.000000000000000000, 0.9238795325112867385, 1.000000000000000000, 0.9238795325112867385, 1.000000000000000000, 0.9238795325112867385, 1.000000000000000000, 0.9238795325112867385, 1.000000000000000000, 0.9238795325112867385, 1.000000000000000000, 0.9238795325112867385, 1.000000000000000000, 0.9238795325112867385, 1.000000000000000000, 0.9238795325112867385, 1.000000000000000000, 0.9238795325112867385, 1.000000000000000000, 0.9238795325112867385, 1.000000000000000000, 0.9238795325112867385, 1.000000000000000000, 0.9238795325112867385, 1.000000000000000000, 0.9238795325112867385, 1.000000000000000000, 0.9238795325112867385, 1.000000000000000000, 0.9238795325112867385, 1.000000000000000000, 0.9238795325112867385, 1.000000000000000000, 0.9238795325112867385, 1.000000000000000000, 0.9238795325112867385, 1.000000000000000000, 0.9238795325112867385, 1.000000000000000000, 0.9238795325112867385, 1.000000000000000000, 0.9238795325112867385, 1.000000000000000000, 0.9238795325112867385, 1.000000000000000000, 0.9238795325112867385, 1.000000000000000000, 0.9238795325112867385, 1.000000000000000000, 0.9238795325112867385, 1.000000000000000000, 0.9238795325112867385, 1.000000000000000000, 0.9238795325112867385, 1.000000000000000000, 0.9238795325112867385, 1.000000000000000000, 0.9238795325112867385, 1.000000000000000000, 0.9238795325112867385, 1.000000000000000000, 0.9238795325112867385, 1.000000000000000000, 0.9238795325112867385, 1.000000000000000000, 0.9238795325112867385, 1.000000000000000000, 0.9238795325112867385, 1.000000000000000000, 0.9238795325112867385, 1.000000000000000000, 0.9238795325112867385, 1.000000000000000000, 0.9238795325112867385, 1.000000000000000000, 0.9238795325112867385, 1.000000000000000000, 0.9238795325112867385, 1.000000000000000000, 0.9238795325112867385, 1.000000000000000000, 0.9238795325112867385, 1.000000000000000000, 0.9238795325112867385, 1.000000000000000000, 0.9238795325112867385, 1.000000000000000000, 0.9238795325112867385, 1.000000000000000000, 0.9238795325112867385, 1.000000000000000000, 0.9238795325112867385, 1.000000000000000000, 0.9238795325112867385, 1.000000000000000000, 0.9238795325112867385, 1.000000000000000000, 0.9238795325112867385, 1.000000000000000000, 0.9238795325112867385, 1.000000000000000000, 0.9238795325112867385, 1.000000000000000000, 0.9238795325112867385, 1.000000000000000000, 0.9238795325112867385, 1.000000000000000000, 0.9238795325112867385, 1.000000000000000000, 0.9238795325112867385, 1.000000000000000000, 0.9238795325112867385, 1.000000000000000000, 0.9238795325112867385, 1.000000000000000000, 0.9238795325112867385, 1.000000000000000000, 0.9238795325112867385, 1.000000000000000000, 0.9238795325112867385, 1.000000000000000000, 0.9238795325112867385, 1.000000000000000000, 0.9238795325112867385, 1.000000000000000000, 0.9238795325112867385, 1.000000000000000000, 0.9238795325112867385, 1.000000000000000000, 0.9238795325112867385, 1.000000000000000000, 0.9238795325112867385, 1.000000000000000000, 0.9238795325112867385, 1.000000000000000000, 0.9238795325112867385, 1.000000000000000000, 0.9238795325112867385, 1.000000000000000000, 0.9238795325112867385, 1.000000000000000000, 0.9238795325112867385, 1.000000000000000000, 0.9238795325112867385, 1.000000000000000000, 0.9238795325112867385, 1.000000000000000000, 0.9238795325112867385, 1.000000000000000000, 0.9238795325112867385, 1.000000000000000000, 0.9238795325112867385, 1.000000000000000000, 0.9238795325112867385, 1.000000000000000000, 0.9238795325112867385, 1.000000000000000000, 0.9238795325112867385, 1.000000000000000000, 0.9238795325112867385, 1.000000000000000000, 0.9238795325112867385, 1.000000000000000000, 0.9238795325112867385, 1.000000000000000000, 0.9238795325112867385, 1.000000000000000000, 0.9238795325112867385, 1.000000000000000000, 0.9238795325112867385, 1.000000000000000000, 0.9238795325112867385, 1.000000000000000000, 0.9238795325112867385, 1.000000000000000000, 0.9238795325112867385, 1.000000000000000000, 0.9238795325112867385, 1.000000000000000000, 0.9238795325112867385, 1.000000000000000000, 0.9238795325112867385, 1.000000000000000000, 0.9238795325112867385, 1.000000000000000000, 0.9238795325112867385, 1.000000000000000000, 0.9238795325112867385, 1.000000000000000000, 0.9238795325112867385, 1.000000000000000000, 0.9238795325112867385, 1.000000000000000000, 0.9238795325112867385, 1.000000000000000000, 0.9238795325112867385, 1.000000000000000000, 0.9238795325112867385, 1.000000000000000000 ) ) 
 REPRESENTATION_ITEM ( '' )  );
#13372 = DIRECTION ( 'NONE',  ( -0.000000000000000000, 1.000000000000000000, -0.000000000000000000 ) ) ;
#13373 = CARTESIAN_POINT ( 'NONE',  ( -50.18089887299979068, -138.6875000000000284, 2.462841084822635640 ) ) ;
#13374 = CARTESIAN_POINT ( 'NONE',  ( 4.458734124999999437, -40.06249999863440081, -5.460374474430324690E-16 ) ) ;
#13375 = ORIENTED_EDGE ( 'NONE', *, *, #10174, .T. ) ;
#13376 = CARTESIAN_POINT ( 'NONE',  ( -2.229367062499996610, -82.14583333196773651, 3.861377020970582219 ) ) ;
#13377 = EDGE_CURVE ( 'NONE', #33297, #36444, #48096, .T. ) ;
#13378 = CARTESIAN_POINT ( 'NONE',  ( -2.229367062499996610, 22.85416666803225993, 3.861377020970582219 ) ) ;
#13379 = CARTESIAN_POINT ( 'NONE',  ( 0.000000000000000000, -120.0000000000000000, 0.000000000000000000 ) ) ;
#13380 = ORIENTED_EDGE ( 'NONE', *, *, #63339, .T. ) ;
#13381 = CARTESIAN_POINT ( 'NONE',  ( -51.60603307380591787, -139.1875000013656347, -2.891590998281053704 ) ) ;
#13382 = CARTESIAN_POINT ( 'NONE',  ( 2.229367062499998831, -85.89583333196773651, -3.861377020970580887 ) ) ;
#13383 = CARTESIAN_POINT ( 'NONE',  ( -53.33387254593733928, -124.9375000027312268, 5.149110718188519620 ) ) ;
#13384 = CYLINDRICAL_SURFACE ( 'NONE', #60349, 5.000000000000000000 ) ;
#13385 = CARTESIAN_POINT ( 'NONE',  ( 1.975475456537005874E-15, -6.749999999999999112, 5.000000000000000000 ) ) ;
#13386 = CARTESIAN_POINT ( 'NONE',  ( -2.499999999999996447, -46.70833333060214443, 4.330127018922195425 ) ) ;
#13387 = CARTESIAN_POINT ( 'NONE',  ( -2.229367062500000163, -56.47916666530107221, -3.861377020970580443 ) ) ;
#13388 = CARTESIAN_POINT ( 'NONE',  ( -2.499999999999996447, -84.70833333060214443, 4.330127018922195425 ) ) ;
#13389 = CARTESIAN_POINT ( 'NONE',  ( 9.457646018065525792E-16, 23.93750000136559564, 5.148502694627439702 ) ) ;
#13390 = CARTESIAN_POINT ( 'NONE',  ( -55.00000000000001421, -135.0000000000000284, -8.082903768654752241 ) ) ;
#13391 = CARTESIAN_POINT ( 'NONE',  ( -2.500000000000000444, -44.16666666666665719, -4.330127018922193649 ) ) ;
#13392 = CARTESIAN_POINT ( 'NONE',  ( -4.458734124999998549, -43.47916666530106511, 2.574251347313722516 ) ) ;
#13393 = CARTESIAN_POINT ( 'NONE',  ( -5.000000000000000000, -1.958333330602145761, -2.886751345948128211 ) ) ;
#13394 = DIRECTION ( 'NONE',  ( -0.000000000000000000, 1.000000000000000000, -0.000000000000000000 ) ) ;
#13395 = CARTESIAN_POINT ( 'NONE',  ( -53.51423613279429503, -126.2500000013656063, 4.591703134518082763 ) ) ;
#13396 = CARTESIAN_POINT ( 'NONE',  ( 4.458734124999998549, -86.97916666530106511, -2.574251347313721627 ) ) ;
#13397 = CARTESIAN_POINT ( 'NONE',  ( -4.458734124999997661, -104.2291666653010651, 2.574251347313722516 ) ) ;
#13398 = AXIS2_PLACEMENT_3D ( 'NONE', #9805, #49046, #59024 ) ;
#13399 =( BOUNDED_CURVE ( )  B_SPLINE_CURVE ( 2, ( #33879, #4300, #33568, #47725, #23296, #13636, #28729, #42896, #18464 ),
 .UNSPECIFIED., .F., .F. ) 
 B_SPLINE_CURVE_WITH_KNOTS ( ( 3, 2, 2, 2, 3 ),
 ( 0.4416666666666670404, 0.4458333333333337478, 0.4500000000000003997, 0.4541666666666671071, 0.4583333333333337589 ),
 .UNSPECIFIED. ) 
 CURVE ( )  GEOMETRIC_REPRESENTATION_ITEM ( )  RATIONAL_B_SPLINE_CURVE ( ( 0.9999999999999928946, 0.9238795325112938439, 1.000000000000000000, 0.9238795325112867385, 1.000000000000000000, 0.9238795325112867385, 1.000000000000000000, 0.9238795325112786339, 1.000000000000008216 ) ) 
 REPRESENTATION_ITEM ( '' )  );
#13400 = CARTESIAN_POINT ( 'NONE',  ( -2.229367062500000163, -8.729166665301073991, -3.861377020970580443 ) ) ;
#13401 = ORIENTED_EDGE ( 'NONE', *, *, #51847, .T. ) ;
#13402 = CARTESIAN_POINT ( 'NONE',  ( -6.972266317189433020E-16, -81.24999999999998579, -5.000000000000000000 ) ) ;
#13403 = CARTESIAN_POINT ( 'NONE',  ( -2.229367062499996610, -94.14583333196772230, 3.861377020970582219 ) ) ;
#13404 = CARTESIAN_POINT ( 'NONE',  ( -2.071067811865475061, -165.8125000027311842, -5.000000000000000888 ) ) ;
#13405 = CARTESIAN_POINT ( 'NONE',  ( 4.458734125000001214, -91.14583333196773651, 2.574251347313718519 ) ) ;
#13406 = VECTOR ( 'NONE', #27670, 1000.000000000000000 ) ;
#13407 = CARTESIAN_POINT ( 'NONE',  ( -2.499999999999996447, -52.70833333060213732, 4.330127018922195425 ) ) ;
#13408 = CARTESIAN_POINT ( 'NONE',  ( 1.975475456537005874E-15, -29.74999999999999645, 5.000000000000000000 ) ) ;
#13409 = CARTESIAN_POINT ( 'NONE',  ( -51.60603307380591787, -127.9375000013656063, -2.891590998281053704 ) ) ;
#13410 = CARTESIAN_POINT ( 'NONE',  ( 4.458734124999999437, -14.81249999863440436, -5.460374474430324690E-16 ) ) ;
#13411 = CARTESIAN_POINT ( 'NONE',  ( -4.458734124999999437, 13.43750000136559386, 0.000000000000000000 ) ) ;
#13412 = CARTESIAN_POINT ( 'NONE',  ( -2.229367062500000163, -53.72916666530107221, -3.861377020970580443 ) ) ;
#13413 = CARTESIAN_POINT ( 'NONE',  ( 0.000000000000000000, -170.0000000000000000, 5.000000000000000000 ) ) ;
#13414 = CARTESIAN_POINT ( 'NONE',  ( -4.458734124999997661, -9.229166665301068662, 2.574251347313722516 ) ) ;
#13415 = CARTESIAN_POINT ( 'NONE',  ( 0.000000000000000000, -170.0000000000000000, 0.000000000000000000 ) ) ;
#13416 = VERTEX_POINT ( 'NONE', #1676 ) ;
#13417 = CARTESIAN_POINT ( 'NONE',  ( 9.457646018065525792E-16, -38.31249999863440792, 5.148502694627439702 ) ) ;
#13418 = CARTESIAN_POINT ( 'NONE',  ( -59.29741812935640155, -125.8750000013656063, -2.196230717870135685 ) ) ;
#13419 = CARTESIAN_POINT ( 'NONE',  ( -51.75738570946856498, -155.0000000000000284, 3.805975901505577408 ) ) ;
#13420 = FACE_OUTER_BOUND ( 'NONE', #37881, .T. ) ;
#13421 = CARTESIAN_POINT ( 'NONE',  ( -4.458734124999999437, -79.31249999863440792, 0.000000000000000000 ) ) ;
#13422 = CARTESIAN_POINT ( 'NONE',  ( -4.458734124999999437, 26.43750000136559564, 0.000000000000000000 ) ) ;
#13423 = CARTESIAN_POINT ( 'NONE',  ( -4.458734124999999437, 17.68750000136559208, 0.000000000000000000 ) ) ;
#13424 = CARTESIAN_POINT ( 'NONE',  ( -6.972266317189433020E-16, -34.12499999726881583, -5.000000000000000000 ) ) ;
#13425 = CARTESIAN_POINT ( 'NONE',  ( 1.339745962155615144, -55.70534180126148271, 4.999999999999999112 ) ) ;
#13426 = CARTESIAN_POINT ( 'NONE',  ( 2.229367062499998831, -81.89583333196773651, -3.861377020970580887 ) ) ;
#13427 = CARTESIAN_POINT ( 'NONE',  ( 1.060575238724906964E-15, -68.74999999999998579, 5.773502691896257311 ) ) ;
#13428 = CARTESIAN_POINT ( 'NONE',  ( 2.500000000000002220, 14.45833333606451809, 4.330127018922192761 ) ) ;
#13429 = ORIENTED_EDGE ( 'NONE', *, *, #42575, .F. ) ;
#13430 = CARTESIAN_POINT ( 'NONE',  ( -5.000000000000000000, -61.87499999726880873, 0.000000000000000000 ) ) ;
#13431 = CARTESIAN_POINT ( 'NONE',  ( -9.184850993605147944E-16, -149.3750000027312126, 5.000000000000000000 ) ) ;
#13433 = CARTESIAN_POINT ( 'NONE',  ( 2.499999999999998668, -31.33333333333333215, -4.330127018922193649 ) ) ;
#13432 = CARTESIAN_POINT ( 'NONE',  ( 6.123233995736766282E-16, -120.0000000000000000, -5.000000000000000000 ) ) ;
#13434 = CARTESIAN_POINT ( 'NONE',  ( -2.229367062500000163, -31.47916666530107577, -3.861377020970580443 ) ) ;
#13435 = CYLINDRICAL_SURFACE ( 'NONE', #61263, 5.000000000000000000 ) ;
#13436 = EDGE_CURVE ( 'NONE', #3491, #57658, #10345, .T. ) ;
#13437 = CARTESIAN_POINT ( 'NONE',  ( 5.000000000000000000, -30.37499999726881228, -6.123233995736766282E-16 ) ) ;
#13438 = EDGE_CURVE ( 'NONE', #21932, #56335, #1732, .T. ) ;
#13440 = VERTEX_POINT ( 'NONE', #54741 ) ;
#13439 = CARTESIAN_POINT ( 'NONE',  ( 2.229367062499998831, -60.64583333196774362, -3.861377020970580887 ) ) ;
#13441 = CARTESIAN_POINT ( 'NONE',  ( -52.80376928212989185, -154.1250000013656347, -4.297418129356379346 ) ) ;
#13443 = ORIENTED_EDGE ( 'NONE', *, *, #25296, .T. ) ;
#13442 = CARTESIAN_POINT ( 'NONE',  ( -3.152548672688508926E-16, -8.812499998634406140, -5.148502694627439702 ) ) ;
#13444 = ADVANCED_FACE ( 'NONE', ( #5852 ), #45082, .T. ) ;
#13445 = CARTESIAN_POINT ( 'NONE',  ( -2.499999999999996447, -74.83333333333332860, 4.330127018922195425 ) ) ;
#13446 = CARTESIAN_POINT ( 'NONE',  ( -52.10840900171896806, -135.1875000013656063, 3.393966926194110556 ) ) ;
#13447 = VECTOR ( 'NONE', #9052, 1000.000000000000000 ) ;
#13448 = CARTESIAN_POINT ( 'NONE',  ( 9.457646018065525792E-16, -54.31249999863440081, 5.148502694627439702 ) ) ;
#13449 = EDGE_CURVE ( 'NONE', #37904, #62889, #6173, .T. ) ;
#13450 = CARTESIAN_POINT ( 'NONE',  ( 2.500000000000002220, -74.54166666393547303, 4.330127018922192761 ) ) ;
#13452 = ORIENTED_EDGE ( 'NONE', *, *, #51863, .F. ) ;
#13451 = CARTESIAN_POINT ( 'NONE',  ( -1.339745962155613812, -55.08034179853029144, -5.000000000000000000 ) ) ;
#13453 = AXIS2_PLACEMENT_3D ( 'NONE', #49653, #54805, #10734 ) ;
#13454 = CARTESIAN_POINT ( 'NONE',  ( -51.75738570946856498, -150.7500000000000284, 3.805975901505576964 ) ) ;
#13455 = EDGE_CURVE ( 'NONE', #46822, #42419, #23507, .T. ) ;
#13456 = CARTESIAN_POINT ( 'NONE',  ( 2.229367062500001939, -19.22916666530106866, 3.861377020970579999 ) ) ;
#13457 = EDGE_CURVE ( 'NONE', #43823, #11304, #46359, .T. ) ;
#13459 = ORIENTED_EDGE ( 'NONE', *, *, #9786, .F. ) ;
#13458 = CARTESIAN_POINT ( 'NONE',  ( 2.229367062499998831, -54.89583333196773651, -3.861377020970580887 ) ) ;
#13460 = SURFACE_SIDE_STYLE ('',( #62357 ) ) ;
#13461 = CARTESIAN_POINT ( 'NONE',  ( 3.152801135295367541, -166.5625000013656063, -3.152801135295367541 ) ) ;
#13462 = CARTESIAN_POINT ( 'NONE',  ( 4.458734124999998549, -101.9791666653010651, -2.574251347313721627 ) ) ;
#13463 = CARTESIAN_POINT ( 'NONE',  ( -6.972266317189433020E-16, 17.75000000000000355, -5.000000000000000000 ) ) ;
#13464 = VERTEX_POINT ( 'NONE', #31236 ) ;
#13465 = EDGE_CURVE ( 'NONE', #15263, #61537, #45289, .T. ) ;
#13466 = CARTESIAN_POINT ( 'NONE',  ( -55.35523342533222291, -151.5625000013656063, 4.444560631937231499 ) ) ;
#13467 = CARTESIAN_POINT ( 'NONE',  ( -54.60164318462004474, -142.5000000027312126, -4.984105922594373794 ) ) ;
#13468 = ADVANCED_FACE ( 'NONE', ( #37030 ), #22874, .T. ) ;
#13469 = EDGE_CURVE ( 'NONE', #60305, #56096, #2944, .T. ) ;
#13470 = CARTESIAN_POINT ( 'NONE',  ( 5.000000000000000000, -83.49999999999998579, -6.123233995736766282E-16 ) ) ;
#13471 = CARTESIAN_POINT ( 'NONE',  ( 2.229367062500001939, -4.979166665301071326, 3.861377020970579999 ) ) ;
#13472 = CARTESIAN_POINT ( 'NONE',  ( -3.152548672688508926E-16, -98.81249999863440792, -5.148502694627439702 ) ) ;
#13473 = CARTESIAN_POINT ( 'NONE',  ( 2.730187237215162345E-16, -145.4375000013656063, -4.458734124999999437 ) ) ;
#13474 = CARTESIAN_POINT ( 'NONE',  ( -4.458734124999999437, -27.64583333196774007, -2.574251347313719407 ) ) ;
#13475 = CARTESIAN_POINT ( 'NONE',  ( -6.972266317189433020E-16, -70.25000000000000000, -5.000000000000000000 ) ) ;
#13476 = CARTESIAN_POINT ( 'NONE',  ( -55.35523342533222291, -137.3125000013656063, 4.444560631937231499 ) ) ;
#13477 = CARTESIAN_POINT ( 'NONE',  ( -2.229367062499996610, -70.39583333196773651, 3.861377020970582219 ) ) ;
#13478 = CYLINDRICAL_SURFACE ( 'NONE', #54877, 5.000000000000000000 ) ;
#13479 = LINE ( 'NONE', #27318, #22376 ) ;
#13480 = CARTESIAN_POINT ( 'NONE',  ( 4.458734124999999437, -139.4375000013656063, 0.000000000000000000 ) ) ;
#13481 = CARTESIAN_POINT ( 'NONE',  ( 4.458734124999999437, 7.937500001365595637, -5.460374474430324690E-16 ) ) ;
#13482 = ORIENTED_EDGE ( 'NONE', *, *, #9879, .T. ) ;
#13483 = CARTESIAN_POINT ( 'NONE',  ( -1.339745962155610925, 2.205341801261479606, 5.000000000000000000 ) ) ;
#13484 = FACE_BOUND ( 'NONE', #40670, .T. ) ;
#13486 = CARTESIAN_POINT ( 'NONE',  ( 9.457646018065525792E-16, -25.06249999863440792, 5.148502694627439702 ) ) ;
#13485 = CARTESIAN_POINT ( 'NONE',  ( -2.500000000000000444, -88.16666666666665719, -4.330127018922193649 ) ) ;
#13487 = LINE ( 'NONE', #33104, #44906 ) ;
#13488 = CARTESIAN_POINT ( 'NONE',  ( -4.458734124999998549, -74.47916666530106511, 2.574251347313722516 ) ) ;
#13489 = CARTESIAN_POINT ( 'NONE',  ( -4.458734124999999437, 25.35416666803225993, -2.574251347313719407 ) ) ;
#13490 = CARTESIAN_POINT ( 'NONE',  ( -9.184850993605147944E-16, -157.3750000027311842, 5.000000000000000000 ) ) ;
#13491 =( BOUNDED_CURVE ( )  B_SPLINE_CURVE ( 2, ( #29745, #45189, #831, #50012, #30717, #54200, #189, #10780, #31031 ),
 .UNSPECIFIED., .F., .F. ) 
 B_SPLINE_CURVE_WITH_KNOTS ( ( 3, 2, 2, 2, 3 ),
 ( 0.5937500000000000000, 0.5944444444444444420, 0.5958333333333333259, 0.5972222222222222099, 0.5979166666666666519 ),
 .UNSPECIFIED. ) 
 CURVE ( )  GEOMETRIC_REPRESENTATION_ITEM ( )  RATIONAL_B_SPLINE_CURVE ( ( 0.9330127018922194093, 0.9330127018922194093, 1.000000000000000000, 0.8660254037844387076, 1.000000000000000000, 0.8660254037844387076, 1.000000000000000000, 0.9330127018922194093, 0.9330127018922194093 ) ) 
 REPRESENTATION_ITEM ( '' )  );
#13492 = CARTESIAN_POINT ( 'NONE',  ( -57.19623071787017210, -141.3750000013656063, 4.297418129356382899 ) ) ;
#13493 = CARTESIAN_POINT ( 'NONE',  ( -4.458734124999997661, 0.7708333346989268975, 2.574251347313722516 ) ) ;
#13494 = CARTESIAN_POINT ( 'NONE',  ( -4.458734124999998549, 26.52083333469892779, 2.574251347313722516 ) ) ;
#13495 = CARTESIAN_POINT ( 'NONE',  ( 9.457646018065525792E-16, -37.31249999863440792, 5.148502694627439702 ) ) ;
#13496 = CARTESIAN_POINT ( 'NONE',  ( 5.000000000000000000, -43.29166666393548013, -2.886751345948130876 ) ) ;
#13497 = CARTESIAN_POINT ( 'NONE',  ( -4.458734124999999437, 4.687500001365595637, 0.000000000000000000 ) ) ;
#13498 = CARTESIAN_POINT ( 'NONE',  ( 4.458734124999999437, -71.81249999863439371, -5.460374474430324690E-16 ) ) ;
#13499 = CARTESIAN_POINT ( 'NONE',  ( 9.457646018065525792E-16, -21.31249999863440081, 5.148502694627439702 ) ) ;
#13500 = CARTESIAN_POINT ( 'NONE',  ( 2.499999999999998668, -5.333333333333335702, -4.330127018922193649 ) ) ;
#13501 = CARTESIAN_POINT ( 'NONE',  ( -4.458734125000000326, -157.0000000013655779, -1.846868145590735644 ) ) ;
#13502 = CARTESIAN_POINT ( 'NONE',  ( 5.000000000000000888, 23.41666666666666430, 2.886751345948126879 ) ) ;
#13503 = AXIS2_PLACEMENT_3D ( 'NONE', #27677, #46355, #32502 ) ;
#13504 = CARTESIAN_POINT ( 'NONE',  ( 4.458734124999999437, -65.81249999863440792, -5.460374474430324690E-16 ) ) ;
#13505 = CARTESIAN_POINT ( 'NONE',  ( 1.060575238724906964E-15, -97.62499999726881583, 5.773502691896257311 ) ) ;
#13506 =( BOUNDED_CURVE ( )  B_SPLINE_CURVE ( 2, ( #57497, #27260, #46886, #42362, #36592, #56228, #12149, #48134, #58102 ),
 .UNSPECIFIED., .F., .F. ) 
 B_SPLINE_CURVE_WITH_KNOTS ( ( 3, 2, 2, 2, 3 ),
 ( 0.9660714285714285809, 0.9666666666666666741, 0.9678571428571428603, 0.9690476190476190466, 0.9696428571428571397 ),
 .UNSPECIFIED. ) 
 CURVE ( )  GEOMETRIC_REPRESENTATION_ITEM ( )  RATIONAL_B_SPLINE_CURVE ( ( 0.9330127018922194093, 0.9330127018922194093, 1.000000000000000000, 0.8660254037844387076, 1.000000000000000000, 0.8660254037844387076, 1.000000000000000000, 0.9330127018922194093, 0.9330127018922194093 ) ) 
 REPRESENTATION_ITEM ( '' )  );
#13507 = CARTESIAN_POINT ( 'NONE',  ( 2.500000000000002220, -41.66666666666667140, 4.330127018922192761 ) ) ;
#13508 = CARTESIAN_POINT ( 'NONE',  ( -3.152548672688508926E-16, -40.56249999863440081, -5.148502694627439702 ) ) ;
#13509 = CARTESIAN_POINT ( 'NONE',  ( -6.972266317189433020E-16, 9.875000002731185944, -5.000000000000000000 ) ) ;
#13510 = CARTESIAN_POINT ( 'NONE',  ( 9.457646018065525792E-16, -104.3124999986344221, 5.148502694627439702 ) ) ;
#13511 = CARTESIAN_POINT ( 'NONE',  ( 4.458734124999998549, -68.97916666530107932, -2.574251347313721627 ) ) ;
#13512 = CARTESIAN_POINT ( 'NONE',  ( 5.000000000000000000, -52.50000000000000711, -6.123233995736766282E-16 ) ) ;
#13513 = CARTESIAN_POINT ( 'NONE',  ( 7.204675194429079505E-15, 26.74999999999999645, -5.000000000000000000 ) ) ;
#13514 = CARTESIAN_POINT ( 'NONE',  ( 0.000000000000000000, -120.0000000000000000, 0.000000000000000000 ) ) ;
#13515 = ORIENTED_EDGE ( 'NONE', *, *, #41414, .F. ) ;
#13516 = CARTESIAN_POINT ( 'NONE',  ( 5.000000000000000000, -94.41666666666664298, -2.886751345948130876 ) ) ;
#13517 = AXIS2_PLACEMENT_3D ( 'NONE', #39302, #29655, #49285 ) ;
#13518 = CARTESIAN_POINT ( 'NONE',  ( 1.339745962155590275, 2.419658201469706782, 5.000000000000013323 ) ) ;
#13519 = CARTESIAN_POINT ( 'NONE',  ( -3.535250795749689387E-16, -15.25000000000000000, -5.773502691896257311 ) ) ;
#13520 = CARTESIAN_POINT ( 'NONE',  ( -3.152548672688508926E-16, -15.56249999863440614, -5.148502694627439702 ) ) ;
#13521 = CARTESIAN_POINT ( 'NONE',  ( -4.458734124999999437, -75.31249999863440792, 0.000000000000000000 ) ) ;
#13522 = CYLINDRICAL_SURFACE ( 'NONE', #58581, 5.000000000000000000 ) ;
#13523 = CARTESIAN_POINT ( 'NONE',  ( -5.000000000000000000, -12.87499999726881050, 0.000000000000000000 ) ) ;
#13525 = ORIENTED_EDGE ( 'NONE', *, *, #58924, .T. ) ;
#13524 = CARTESIAN_POINT ( 'NONE',  ( 2.229367062499998831, -46.64583333196774362, -3.861377020970580887 ) ) ;
#13527 = ORIENTED_EDGE ( 'NONE', *, *, #14502, .T. ) ;
#13526 = CARTESIAN_POINT ( 'NONE',  ( -2.229367062499996610, 7.604166668032260823, 3.861377020970582219 ) ) ;
#13528 = CARTESIAN_POINT ( 'NONE',  ( -50.55543936806279248, -154.0625000013656347, 0.3552334253322060320 ) ) ;
#13529 = CARTESIAN_POINT ( 'NONE',  ( 2.500000000000002220, -58.66666666666665719, 4.330127018922192761 ) ) ;
#13530 = CARTESIAN_POINT ( 'NONE',  ( -4.458734125000001214, -158.1250000013656063, 1.846868145590734089 ) ) ;
#13531 = CARTESIAN_POINT ( 'NONE',  ( 9.457646018065525792E-16, -36.31249999863440792, 5.148502694627439702 ) ) ;
#13532 = CARTESIAN_POINT ( 'NONE',  ( -1.339745962155610925, -64.79465819873851729, 5.000000000000000000 ) ) ;
#13533 = CARTESIAN_POINT ( 'NONE',  ( -3.535533905932738641, -168.3750000000000284, 3.535533905932737309 ) ) ;
#13534 = DIRECTION ( 'NONE',  ( -0.000000000000000000, 1.000000000000000000, -0.000000000000000000 ) ) ;
#13535 = CARTESIAN_POINT ( 'NONE',  ( -52.80376928212989185, -133.1250000013656063, -4.297418129356379346 ) ) ;
#13536 = CARTESIAN_POINT ( 'NONE',  ( 9.457646018065525792E-16, -6.312499998634404363, 5.148502694627439702 ) ) ;
#13537 = CARTESIAN_POINT ( 'NONE',  ( 2.229367062500001939, -40.22916666530107221, 3.861377020970579999 ) ) ;
#13538 = CARTESIAN_POINT ( 'NONE',  ( 5.000000000000000888, -54.58333333333332860, 2.886751345948126879 ) ) ;
#13539 = CARTESIAN_POINT ( 'NONE',  ( 1.846868145590736310, -153.6250000013655779, 4.458734124999999437 ) ) ;
#13540 = CARTESIAN_POINT ( 'NONE',  ( -2.229367062500000163, -81.72916666530106511, -3.861377020970580443 ) ) ;
#13541 = CARTESIAN_POINT ( 'NONE',  ( 0.000000000000000000, -120.0000000000000000, 5.000000000000000000 ) ) ;
#13542 = EDGE_LOOP ( 'NONE', ( #5462, #22549, #24988, #10193 ) ) ;
#13543 = CARTESIAN_POINT ( 'NONE',  ( -2.071067811865562991, -141.3124999999999716, 4.999999999999913847 ) ) ;
#13544 = CARTESIAN_POINT ( 'NONE',  ( 1.339745962155615144, -2.580341798530292774, 4.999999999999999112 ) ) ;
#13545 = CARTESIAN_POINT ( 'NONE',  ( 4.458734124999999437, -70.06249999863439371, -5.460374474430324690E-16 ) ) ;
#13546 = CARTESIAN_POINT ( 'NONE',  ( -4.458734125000000326, -147.1250000013656063, 1.846868145590734089 ) ) ;
#13547 = VERTEX_POINT ( 'NONE', #42467 ) ;
#13548 = EDGE_CURVE ( 'NONE', #50783, #14315, #8297, .T. ) ;
#13549 = CARTESIAN_POINT ( 'NONE',  ( -5.000000000000000000, -13.99999999999999822, 0.000000000000000000 ) ) ;
#13550 = CARTESIAN_POINT ( 'NONE',  ( -2.229367062500000163, -10.72916666530106866, -3.861377020970580443 ) ) ;
#13551 = CARTESIAN_POINT ( 'NONE',  ( -2.499999999999996447, -34.83333333333332860, 4.330127018922195425 ) ) ;
#13552 = CARTESIAN_POINT ( 'NONE',  ( 4.458734125000001214, 3.104166668032260379, 2.574251347313718519 ) ) ;
#13553 = CARTESIAN_POINT ( 'NONE',  ( -6.972266317189433020E-16, -80.24999999999998579, -5.000000000000000000 ) ) ;
#13554 = CARTESIAN_POINT ( 'NONE',  ( 1.846868145590735200, -153.2500000013656063, -4.458734124999999437 ) ) ;
#13555 =( BOUNDED_CURVE ( )  B_SPLINE_CURVE ( 2, ( #35545, #44865, #26208, #6284, #50009, #51305, #7243, #31669, #828 ),
 .UNSPECIFIED., .F., .F. ) 
 B_SPLINE_CURVE_WITH_KNOTS ( ( 3, 2, 2, 2, 3 ),
 ( 0.3916666666666669960, 0.3958333333333336479, 0.4000000000000003553, 0.4041666666666670071, 0.4083333333333336590 ),
 .UNSPECIFIED. ) 
 CURVE ( )  GEOMETRIC_REPRESENTATION_ITEM ( )  RATIONAL_B_SPLINE_CURVE ( ( 0.9999999999999938938, 0.9238795325112928447, 1.000000000000000000, 0.9238795325112867385, 1.000000000000000000, 0.9238795325112867385, 1.000000000000000000, 0.9238795325112806323, 1.000000000000005995 ) ) 
 REPRESENTATION_ITEM ( '' )  );
#13556 = CARTESIAN_POINT ( 'NONE',  ( -4.458734124999999437, 24.35416666803225993, -2.574251347313719407 ) ) ;
#13557 = ORIENTED_EDGE ( 'NONE', *, *, #53664, .T. ) ;
#13558 = CARTESIAN_POINT ( 'NONE',  ( 4.458734125000000326, -93.89583333196772230, 2.574251347313718519 ) ) ;
#13559 = CARTESIAN_POINT ( 'NONE',  ( 1.975475456537005874E-15, -77.75000000000000000, 5.000000000000000000 ) ) ;
#13560 = CARTESIAN_POINT ( 'NONE',  ( -1.339745962155610925, -69.66965819600731891, 5.000000000000000000 ) ) ;
#13561 = CARTESIAN_POINT ( 'NONE',  ( 2.229367062499998831, -9.645833331967738289, -3.861377020970580887 ) ) ;
#13562 = CARTESIAN_POINT ( 'NONE',  ( 7.500000000000000000, 4.330127018922199866, -1.000000000000000888 ) ) ;
#13563 = DIRECTION ( 'NONE',  ( 0.000000000000000000, 0.000000000000000000, 1.000000000000000000 ) ) ;
#13564 = CARTESIAN_POINT ( 'NONE',  ( 1.339745962155615144, -87.70534180126146850, 4.999999999999999112 ) ) ;
#13565 = CARTESIAN_POINT ( 'NONE',  ( 2.499999999999998668, -38.20833333060213732, -4.330127018922193649 ) ) ;
#13566 = CARTESIAN_POINT ( 'NONE',  ( -6.972266317189433020E-16, -29.25000000000000000, -5.000000000000000000 ) ) ;
#13567 = CARTESIAN_POINT ( 'NONE',  ( 2.229367062499998831, 21.35416666803226349, -3.861377020970580887 ) ) ;
#13568 = CARTESIAN_POINT ( 'NONE',  ( 1.339745962155612702, -51.16965819600732601, -5.000000000000000000 ) ) ;
#13569 = CARTESIAN_POINT ( 'NONE',  ( -2.229367062500000163, 22.52083333469892423, -3.861377020970580443 ) ) ;
#13570 = CARTESIAN_POINT ( 'NONE',  ( 2.229367062500001939, -54.97916666530107221, 3.861377020970579999 ) ) ;
#13571 = CARTESIAN_POINT ( 'NONE',  ( -2.229367062500000163, -2.729166665301069550, -3.861377020970580443 ) ) ;
#13572 = DIRECTION ( 'NONE',  ( -0.000000000000000000, 1.000000000000000000, -0.000000000000000000 ) ) ;
#13573 = CARTESIAN_POINT ( 'NONE',  ( -4.999999999999999112, 8.083333333333330373, 2.886751345948131764 ) ) ;
#13574 = CARTESIAN_POINT ( 'NONE',  ( -3.535533905932738641, -139.5000000027311842, 3.535533905932737309 ) ) ;
#13575 = CARTESIAN_POINT ( 'NONE',  ( 2.500000000000002220, -75.54166666393547303, 4.330127018922192761 ) ) ;
#13576 = CARTESIAN_POINT ( 'NONE',  ( -2.229367062500000163, -50.47916666530107221, -3.861377020970580443 ) ) ;
#13577 = CARTESIAN_POINT ( 'NONE',  ( 1.060575238724906964E-15, -86.62499999726881583, 5.773502691896257311 ) ) ;
#13578 = CARTESIAN_POINT ( 'NONE',  ( -50.70258187064364108, -135.3750000013656063, 2.196230717870141014 ) ) ;
#13579 = DIRECTION ( 'NONE',  ( 0.000000000000000000, 0.000000000000000000, 1.000000000000000000 ) ) ;
#13580 = CARTESIAN_POINT ( 'NONE',  ( -2.229367062500000163, -88.72916666530106511, -3.861377020970580443 ) ) ;
#13581 = CARTESIAN_POINT ( 'NONE',  ( 4.458734124999999437, -156.6250000013655779, -1.846868145590734978 ) ) ;
#13582 = CARTESIAN_POINT ( 'NONE',  ( 2.499999999999998668, -39.33333333333332860, -4.330127018922193649 ) ) ;
#13583 = CARTESIAN_POINT ( 'NONE',  ( 1.975475456537005874E-15, 8.375000002731187720, 5.000000000000000000 ) ) ;
#13584 = ORIENTED_EDGE ( 'NONE', *, *, #49083, .T. ) ;
#13585 = CARTESIAN_POINT ( 'NONE',  ( -2.229367062500000163, 19.27083333469892779, -3.861377020970580443 ) ) ;
#13586 = ORIENTED_EDGE ( 'NONE', *, *, #23995, .T. ) ;
#13587 = CARTESIAN_POINT ( 'NONE',  ( -2.229367062499996610, -96.14583333196773651, 3.861377020970582219 ) ) ;
#13588 = CARTESIAN_POINT ( 'NONE',  ( 9.457646018065525792E-16, 6.687500001365594748, 5.148502694627439702 ) ) ;
#13589 = CARTESIAN_POINT ( 'NONE',  ( -5.000000000000000000, 12.04166666939785379, -2.886751345948128211 ) ) ;
#13590 = CARTESIAN_POINT ( 'NONE',  ( 3.535533905932736864, -162.1250000000000284, 3.535533905932738641 ) ) ;
#13591 = CARTESIAN_POINT ( 'NONE',  ( -2.500000000000000444, 4.833333333333332149, -4.330127018922193649 ) ) ;
#13592 = CARTESIAN_POINT ( 'NONE',  ( 9.457646018065525792E-16, -60.06249999863440081, 5.148502694627439702 ) ) ;
#13593 = CARTESIAN_POINT ( 'NONE',  ( 1.975475456537005874E-15, 15.37500000273118417, 5.000000000000000000 ) ) ;
#13594 = CARTESIAN_POINT ( 'NONE',  ( 2.500000000000002220, 3.458333336064517205, 4.330127018922192761 ) ) ;
#13595 = CARTESIAN_POINT ( 'NONE',  ( -4.458734124999999437, -27.31249999863440081, 0.000000000000000000 ) ) ;
#13596 = CARTESIAN_POINT ( 'NONE',  ( -6.972266317189433020E-16, 3.875000002731185500, -5.000000000000000000 ) ) ;
#13597 = CARTESIAN_POINT ( 'NONE',  ( 1.975475456537005874E-15, -44.74999999999999289, 5.000000000000000000 ) ) ;
#13598 = CARTESIAN_POINT ( 'NONE',  ( -2.500000000000000444, -25.04166666393547658, -4.330127018922193649 ) ) ;
#13599 = CARTESIAN_POINT ( 'NONE',  ( -5.000000000000000000, -45.00000000000000000, 0.000000000000000000 ) ) ;
#13601 = CARTESIAN_POINT ( 'NONE',  ( 4.458734124999999437, -18.06249999863440792, -5.460374474430324690E-16 ) ) ;
#13600 = CARTESIAN_POINT ( 'NONE',  ( -1.339745962155613812, -90.08034179853029855, -5.000000000000000000 ) ) ;
#13602 = LINE ( 'NONE', #62812, #60485 ) ;
#13603 = CARTESIAN_POINT ( 'NONE',  ( 2.229367062500001939, -64.97916666530106511, 3.861377020970579999 ) ) ;
#13604 =( BOUNDED_CURVE ( )  B_SPLINE_CURVE ( 2, ( #28958, #43750, #19312, #48896, #49538, #45355, #1631, #49851, #16086 ),
 .UNSPECIFIED., .F., .F. ) 
 B_SPLINE_CURVE_WITH_KNOTS ( ( 3, 2, 2, 2, 3 ),
 ( 0.7083333333333329263, 0.7124999999999995781, 0.7166666666666663410, 0.7208333333333329929, 0.7249999999999996447 ),
 .UNSPECIFIED. ) 
 CURVE ( )  GEOMETRIC_REPRESENTATION_ITEM ( )  RATIONAL_B_SPLINE_CURVE ( ( 1.000000000000008216, 0.9238795325112786339, 1.000000000000000000, 0.9238795325112867385, 1.000000000000000000, 0.9238795325112867385, 1.000000000000000000, 0.9238795325112928447, 0.9999999999999938938 ) ) 
 REPRESENTATION_ITEM ( '' )  );
#13605 = CARTESIAN_POINT ( 'NONE',  ( 2.730187237215162345E-16, -146.4375000013656063, -4.458734124999999437 ) ) ;
#13606 = CARTESIAN_POINT ( 'NONE',  ( 4.458734124999999437, -75.81249999863440792, -5.460374474430324690E-16 ) ) ;
#13607 = CARTESIAN_POINT ( 'NONE',  ( -54.64476657466781973, -144.0625000013656063, -4.444560631937228834 ) ) ;
#13608 = CARTESIAN_POINT ( 'NONE',  ( -3.152548672688508926E-16, -25.81249999863440792, -5.148502694627439702 ) ) ;
#13609 = CARTESIAN_POINT ( 'NONE',  ( -2.499999999999996447, -64.70833333060213022, 4.330127018922195425 ) ) ;
#13610 = ORIENTED_EDGE ( 'NONE', *, *, #28689, .F. ) ;
#13611 = CARTESIAN_POINT ( 'NONE',  ( 5.000000000000000888, -93.45833333060215864, 2.886751345948126879 ) ) ;
#13612 = ORIENTED_EDGE ( 'NONE', *, *, #9177, .F. ) ;
#13613 = CARTESIAN_POINT ( 'NONE',  ( -2.229367062499996610, -69.39583333196773651, 3.861377020970582219 ) ) ;
#13614 = CARTESIAN_POINT ( 'NONE',  ( 0.000000000000000000, -170.0000000000000000, 5.000000000000000000 ) ) ;
#13615 =( LENGTH_UNIT ( ) NAMED_UNIT ( * ) SI_UNIT ( .MILLI., .METRE. ) );
#13616 = VERTEX_POINT ( 'NONE', #56018 ) ;
#13617 = LINE ( 'NONE', #28399, #33249 ) ;
#13618 = CARTESIAN_POINT ( 'NONE',  ( 4.458734124999999437, -52.06249999863440792, -5.460374474430324690E-16 ) ) ;
#13619 = CARTESIAN_POINT ( 'NONE',  ( -4.458734124999998549, 2.520833334698928674, 2.574251347313722516 ) ) ;
#13620 = ORIENTED_EDGE ( 'NONE', *, *, #7436, .F. ) ;
#13621 = CARTESIAN_POINT ( 'NONE',  ( -1.339745962155613812, 1.919658201469706116, -5.000000000000000000 ) ) ;
#13622 = CARTESIAN_POINT ( 'NONE',  ( -4.458734124999999437, 2.687500001365593860, 0.000000000000000000 ) ) ;
#13623 = CARTESIAN_POINT ( 'NONE',  ( -2.229367062499996610, 16.85416666803225993, 3.861377020970582219 ) ) ;
#13624 = CARTESIAN_POINT ( 'NONE',  ( -55.35523342533222291, -146.3125000013656063, 4.444560631937231499 ) ) ;
#13625 = CARTESIAN_POINT ( 'NONE',  ( 2.626220312808019583E-14, 20.87500000273118062, -5.000000000000000000 ) ) ;
#13626 = CARTESIAN_POINT ( 'NONE',  ( -4.458734124999999437, -164.9375000013655779, -5.460374474430324690E-16 ) ) ;
#13627 = ORIENTED_EDGE ( 'NONE', *, *, #10235, .F. ) ;
#13628 = CARTESIAN_POINT ( 'NONE',  ( 4.458734124999999437, -77.81249999863440792, -5.460374474430324690E-16 ) ) ;
#13629 = CARTESIAN_POINT ( 'NONE',  ( -6.972266317189433020E-16, 14.87500000273118594, -5.000000000000000000 ) ) ;
#13630 = CARTESIAN_POINT ( 'NONE',  ( -4.458734124999998549, 4.770833334698926009, 2.574251347313722516 ) ) ;
#13631 = DIRECTION ( 'NONE',  ( 0.000000000000000000, 0.000000000000000000, 1.000000000000000000 ) ) ;
#13632 = CARTESIAN_POINT ( 'NONE',  ( 2.229367062499998831, -58.89583333196773651, -3.861377020970580887 ) ) ;
#13633 = CARTESIAN_POINT ( 'NONE',  ( -5.000000000000000000, -21.95833333060214798, -2.886751345948128211 ) ) ;
#13634 = CARTESIAN_POINT ( 'NONE',  ( 1.339745962155615144, -96.58034179853028434, 4.999999999999999112 ) ) ;
#13635 = CARTESIAN_POINT ( 'NONE',  ( -6.972266317189433020E-16, -73.25000000000000000, -5.000000000000000000 ) ) ;
#13636 = CARTESIAN_POINT ( 'NONE',  ( -5.000000000000000888, -156.4374999999999716, 2.071067811865474617 ) ) ;
#13637 = LINE ( 'NONE', #11808, #746 ) ;
#13638 = CARTESIAN_POINT ( 'NONE',  ( -4.458734124999998549, -40.22916666530107932, 2.574251347313722516 ) ) ;
#13639 = CARTESIAN_POINT ( 'NONE',  ( -3.152548672688508926E-16, -27.81249999863440436, -5.148502694627439702 ) ) ;
#13640 = DIRECTION ( 'NONE',  ( 0.000000000000000000, 0.000000000000000000, 1.000000000000000000 ) ) ;
#13641 = CARTESIAN_POINT ( 'NONE',  ( -3.535250795749689387E-16, 25.74999999999999645, -5.773502691896257311 ) ) ;
#13642 = CARTESIAN_POINT ( 'NONE',  ( 3.061616997868383141E-16, -151.8750000027311842, -5.000000000000000000 ) ) ;
#13643 = VERTEX_POINT ( 'NONE', #31562 ) ;
#13644 = CARTESIAN_POINT ( 'NONE',  ( 2.229367062500001939, -106.2291666653010651, 3.861377020970579999 ) ) ;
#13645 = EDGE_CURVE ( 'NONE', #59659, #54895, #56343, .T. ) ;
#13646 = CARTESIAN_POINT ( 'NONE',  ( 4.458734124999999437, -29.81249999863440436, -5.460374474430324690E-16 ) ) ;
#13647 = CARTESIAN_POINT ( 'NONE',  ( 5.000000000000000000, -69.37499999726880162, -6.123233995736766282E-16 ) ) ;
#13648 = CARTESIAN_POINT ( 'NONE',  ( -52.10840900171896806, -146.4375000013656063, 3.393966926194110556 ) ) ;
#13649 = CARTESIAN_POINT ( 'NONE',  ( 5.000000000000000000, -142.0000000000000284, 0.000000000000000000 ) ) ;
#13650 = CARTESIAN_POINT ( 'NONE',  ( 2.229367062499998831, -28.64583333196774007, -3.861377020970580887 ) ) ;
#13651 = CARTESIAN_POINT ( 'NONE',  ( 4.458734124999998549, -75.97916666530106511, -2.574251347313721627 ) ) ;
#13652 = CARTESIAN_POINT ( 'NONE',  ( -5.000000000000000000, -54.99999999999999289, 0.000000000000000000 ) ) ;
#13653 = CARTESIAN_POINT ( 'NONE',  ( 4.458734124999999437, -28.81249999863440436, -5.460374474430324690E-16 ) ) ;
#13654 = CARTESIAN_POINT ( 'NONE',  ( -53.33387254593751692, -135.9375000027312126, 5.149110718188503633 ) ) ;
#13655 = CARTESIAN_POINT ( 'NONE',  ( 5.000000000000000000, 22.62500000273118772, -6.123233995736766282E-16 ) ) ;
#13656 = CARTESIAN_POINT ( 'NONE',  ( -3.535250795749689387E-16, -20.24999999999999645, -5.773502691896257311 ) ) ;
#13657 = CARTESIAN_POINT ( 'NONE',  ( -4.458734125000001214, -148.8750000013655495, 1.846868145590734089 ) ) ;
#13658 = VERTEX_POINT ( 'NONE', #22559 ) ;
#13659 = CARTESIAN_POINT ( 'NONE',  ( -6.972266317189433020E-16, -49.24999999999999289, -5.000000000000000000 ) ) ;
#13660 = CARTESIAN_POINT ( 'NONE',  ( 2.229367062500001939, -59.22916666530106511, 3.861377020970579999 ) ) ;
#13661 = CARTESIAN_POINT ( 'NONE',  ( -5.000000000000000000, 28.04166666939785202, -2.886751345948128211 ) ) ;
#13662 = DIRECTION ( 'NONE',  ( -0.000000000000000000, 1.000000000000000000, -0.000000000000000000 ) ) ;
#13663 = CARTESIAN_POINT ( 'NONE',  ( 5.000000000000000000, 19.58333333333333215, -2.886751345948129988 ) ) ;
#13664 = CYLINDRICAL_SURFACE ( 'NONE', #45867, 5.000000000000000000 ) ;
#13665 = CARTESIAN_POINT ( 'NONE',  ( 2.229367062500001939, 1.020833334698927120, 3.861377020970579999 ) ) ;
#13666 = CARTESIAN_POINT ( 'NONE',  ( 2.499999999999998668, 28.66666666666666785, -4.330127018922193649 ) ) ;
#13667 = CARTESIAN_POINT ( 'NONE',  ( -5.147856630858197489E-14, 4.249999999999996447, 5.000000000000000000 ) ) ;
#13668 = CARTESIAN_POINT ( 'NONE',  ( 4.458734124999999437, 8.937500001365592084, -5.460374474430324690E-16 ) ) ;
#13669 = CARTESIAN_POINT ( 'NONE',  ( 6.123233995736766282E-16, -170.0000000000000000, -5.000000000000000000 ) ) ;
#13670 = ORIENTED_EDGE ( 'NONE', *, *, #34124, .F. ) ;
#13671 = CARTESIAN_POINT ( 'NONE',  ( -54.60164318462004474, -135.3750000000000284, -4.984105922594373794 ) ) ;
#13672 = CARTESIAN_POINT ( 'NONE',  ( 4.458734125000001214, -49.89583333196772941, 2.574251347313718519 ) ) ;
#13673 = CARTESIAN_POINT ( 'NONE',  ( -1.846868145590737420, -160.0000000013656063, 4.458734124999999437 ) ) ;
#13674 =( BOUNDED_CURVE ( )  B_SPLINE_CURVE ( 2, ( #37051, #41534, #62129, #18047, #51838, #27384, #42492, #22582, #2329 ),
 .UNSPECIFIED., .F., .F. ) 
 B_SPLINE_CURVE_WITH_KNOTS ( ( 3, 2, 2, 2, 3 ),
 ( 0.2229166666666666796, 0.2236111111111111216, 0.2250000000000000056, 0.2263888888888888895, 0.2270833333333333315 ),
 .UNSPECIFIED. ) 
 CURVE ( )  GEOMETRIC_REPRESENTATION_ITEM ( )  RATIONAL_B_SPLINE_CURVE ( ( 0.9330127018922194093, 0.9330127018922207416, 1.000000000000000000, 0.8660254037844387076, 1.000000000000000000, 0.8660254037844387076, 1.000000000000000000, 0.9330127018922194093, 0.9330127018922194093 ) ) 
 REPRESENTATION_ITEM ( '' )  );
#13675 = CARTESIAN_POINT ( 'NONE',  ( -3.535250795749689387E-16, -52.12499999726881583, -5.773502691896257311 ) ) ;
#13676 = ORIENTED_EDGE ( 'NONE', *, *, #59964, .T. ) ;
#13677 = CARTESIAN_POINT ( 'NONE',  ( -2.229367062500000163, -21.47916666530107221, -3.861377020970580443 ) ) ;
#13678 = VERTEX_POINT ( 'NONE', #6810 ) ;
#13680 = CARTESIAN_POINT ( 'NONE',  ( 5.000000000000000888, -169.9375000000000284, -2.071067811865475505 ) ) ;
#13679 = CARTESIAN_POINT ( 'NONE',  ( 1.975475456537005874E-15, -95.75000000000000000, 5.000000000000000000 ) ) ;
#13681 = CARTESIAN_POINT ( 'NONE',  ( -3.152801135295367096, -161.0625000013656063, -3.152801135295367541 ) ) ;
#13682 = ORIENTED_EDGE ( 'NONE', *, *, #20404, .T. ) ;
#13683 = CARTESIAN_POINT ( 'NONE',  ( -6.972266317189433020E-16, -35.25000000000000000, -5.000000000000000000 ) ) ;
#13684 = CARTESIAN_POINT ( 'NONE',  ( -51.19402409849444524, -135.5000000000000284, -3.242614290531456334 ) ) ;
#13685 = CARTESIAN_POINT ( 'NONE',  ( -2.229367062499996610, -38.39583333196773651, 3.861377020970582219 ) ) ;
#13686 = ORIENTED_EDGE ( 'NONE', *, *, #22790, .F. ) ;
#13687 = CARTESIAN_POINT ( 'NONE',  ( 2.229367062500001939, -79.97916666530106511, 3.861377020970579999 ) ) ;
#13688 = CARTESIAN_POINT ( 'NONE',  ( -4.458734124999999437, 20.68750000136559208, 0.000000000000000000 ) ) ;
#13689 = CARTESIAN_POINT ( 'NONE',  ( 5.000000000000000888, -24.45833333060214798, 2.886751345948126879 ) ) ;
#13690 = ORIENTED_EDGE ( 'NONE', *, *, #43570, .T. ) ;
#13691 = CARTESIAN_POINT ( 'NONE',  ( -52.80376928212989185, -139.1250000013656063, -4.297418129356378458 ) ) ;
#13692 = CARTESIAN_POINT ( 'NONE',  ( -2.229367062500000163, -86.72916666530107932, -3.861377020970580443 ) ) ;
#13693 = CARTESIAN_POINT ( 'NONE',  ( -57.46284108482265651, -125.0625000027312268, 4.819101127000239515 ) ) ;
#13694 = CARTESIAN_POINT ( 'NONE',  ( 1.975475456537005874E-15, -74.62499999726880162, 5.000000000000000000 ) ) ;
#13695 = CARTESIAN_POINT ( 'NONE',  ( 2.499999999999998668, 4.666666666666666075, -4.330127018922193649 ) ) ;
#13696 = CARTESIAN_POINT ( 'NONE',  ( 9.457646018065525792E-16, -60.06249999863440081, 5.148502694627439702 ) ) ;
#13697 = CARTESIAN_POINT ( 'NONE',  ( -60.14911071818854538, -151.1875000027312410, 1.666127454062681146 ) ) ;
#13698 = CARTESIAN_POINT ( 'NONE',  ( 4.458734125000001214, 25.10416666803225638, 2.574251347313718519 ) ) ;
#13699 = CARTESIAN_POINT ( 'NONE',  ( 2.499999999999998668, -97.33333333333332860, -4.330127018922193649 ) ) ;
#13700 = CARTESIAN_POINT ( 'NONE',  ( -7.499999999999998224, -4.330127018922197202, -7.564335161054478895 ) ) ;
#13701 = CARTESIAN_POINT ( 'NONE',  ( -2.229367062499996610, -45.39583333196774362, 3.861377020970582219 ) ) ;
#13702 = CARTESIAN_POINT ( 'NONE',  ( 2.499999999999998668, -5.208333330602148870, -4.330127018922193649 ) ) ;
#13703 = CARTESIAN_POINT ( 'NONE',  ( -1.339745962155610925, -92.79465819873851729, 5.000000000000000000 ) ) ;
#13704 = CARTESIAN_POINT ( 'NONE',  ( -4.999999999999998224, -60.91666666666666430, 2.886751345948131764 ) ) ;
#13705 = CARTESIAN_POINT ( 'NONE',  ( -4.458734124999998549, -85.47916666530106511, 2.574251347313722516 ) ) ;
#13706 = CARTESIAN_POINT ( 'NONE',  ( -2.229367062499996610, -108.1458333319677365, 3.861377020970582219 ) ) ;
#13707 = CARTESIAN_POINT ( 'NONE',  ( 2.229367062500001939, -10.22916666530106866, 3.861377020970579999 ) ) ;
#13708 = ORIENTED_EDGE ( 'NONE', *, *, #49085, .T. ) ;
#13709 = CARTESIAN_POINT ( 'NONE',  ( -4.458734124999999437, -98.31249999863440792, 0.000000000000000000 ) ) ;
#13710 = CARTESIAN_POINT ( 'NONE',  ( 5.000000000000000000, -167.1875000027312410, 2.071067811865478614 ) ) ;
#13711 = CARTESIAN_POINT ( 'NONE',  ( 2.229367062500001939, -91.22916666530106511, 3.861377020970579999 ) ) ;
#13712 = EDGE_CURVE ( 'NONE', #25378, #31719, #10724, .T. ) ;
#13713 = CARTESIAN_POINT ( 'NONE',  ( -2.500000000000000444, -54.04166666393548013, -4.330127018922193649 ) ) ;
#13714 = CARTESIAN_POINT ( 'NONE',  ( -4.999999999999998224, -29.91666666666667140, 2.886751345948131764 ) ) ;
#13715 = CARTESIAN_POINT ( 'NONE',  ( -56.48576386720575471, -127.7500000013655921, -4.591703134518078322 ) ) ;
#13716 = CARTESIAN_POINT ( 'NONE',  ( -59.29741812935640155, -145.6250000013655779, -2.196230717870135685 ) ) ;
#13717 = CARTESIAN_POINT ( 'NONE',  ( 4.458734124999998549, -14.72916666530107221, -2.574251347313721627 ) ) ;
#13718 = CARTESIAN_POINT ( 'NONE',  ( 4.458734125000001214, 10.85416666803225993, 2.574251347313718519 ) ) ;
#13719 = CARTESIAN_POINT ( 'NONE',  ( -4.458734124999997661, -59.47916666530106511, 2.574251347313722516 ) ) ;
#13720 =( BOUNDED_CURVE ( )  B_SPLINE_CURVE ( 2, ( #5425, #15716, #29854, #14745, #59467, #34362, #45299, #53992, #35660 ),
 .UNSPECIFIED., .F., .F. ) 
 B_SPLINE_CURVE_WITH_KNOTS ( ( 3, 2, 2, 2, 3 ),
 ( 0.6767857142857143238, 0.6773809523809524169, 0.6785714285714286031, 0.6797619047619047894, 0.6803571428571428825 ),
 .UNSPECIFIED. ) 
 CURVE ( )  GEOMETRIC_REPRESENTATION_ITEM ( )  RATIONAL_B_SPLINE_CURVE ( ( 0.9330127018922194093, 0.9330127018922194093, 1.000000000000000000, 0.8660254037844387076, 1.000000000000000000, 0.8660254037844387076, 1.000000000000000000, 0.9330127018922194093, 0.9330127018922194093 ) ) 
 REPRESENTATION_ITEM ( '' )  );
#13721 = CARTESIAN_POINT ( 'NONE',  ( 1.339745962155612702, -86.16965819600731891, -5.000000000000000000 ) ) ;
#13722 = CARTESIAN_POINT ( 'NONE',  ( -2.499999999999996447, -105.8333333333333286, 4.330127018922195425 ) ) ;
#13723 = CARTESIAN_POINT ( 'NONE',  ( -4.458734124999997661, -15.22916666530107754, 2.574251347313722516 ) ) ;
#13724 = FACE_OUTER_BOUND ( 'NONE', #19735, .T. ) ;
#13725 = EDGE_LOOP ( 'NONE', ( #8179, #9878, #1165, #60126 ) ) ;
#13726 = CARTESIAN_POINT ( 'NONE',  ( 2.229367062500001939, -42.22916666530107932, 3.861377020970579999 ) ) ;
#13727 = LINE ( 'NONE', #28830, #5832 ) ;
#13728 = CARTESIAN_POINT ( 'NONE',  ( 2.499999999999998668, -68.33333333333332860, -4.330127018922193649 ) ) ;
#13729 = EDGE_CURVE ( 'NONE', #53022, #41, #37040, .T. ) ;
#13730 = CARTESIAN_POINT ( 'NONE',  ( -7.264118654998712010, 4.945491722146218905, -7.907633014911216840 ) ) ;
#13731 = CARTESIAN_POINT ( 'NONE',  ( -2.229367062499996610, -83.14583333196773651, 3.861377020970582219 ) ) ;
#13732 = CARTESIAN_POINT ( 'NONE',  ( 2.229367062499998831, 26.10416666803225993, -3.861377020970580887 ) ) ;
#13733 = AXIS2_PLACEMENT_3D ( 'NONE', #47860, #27622, #3819 ) ;
#13734 = CARTESIAN_POINT ( 'NONE',  ( 2.229367062500001939, 16.02083333469892779, 3.861377020970579999 ) ) ;
#13735 = DIRECTION ( 'NONE',  ( 1.000000000000000000, 0.000000000000000000, 0.000000000000000000 ) ) ;
#13736 = EDGE_CURVE ( 'NONE', #14611, #38431, #54682, .T. ) ;
#13737 = CARTESIAN_POINT ( 'NONE',  ( -1.339745962155613812, -65.08034179853029855, -5.000000000000000000 ) ) ;
#13738 = CARTESIAN_POINT ( 'NONE',  ( 9.457646018065525792E-16, -90.31249999863439371, 5.148502694627439702 ) ) ;
#13739 = CARTESIAN_POINT ( 'NONE',  ( 2.500000000000002220, -68.66666666666667140, 4.330127018922192761 ) ) ;
#13740 = CARTESIAN_POINT ( 'NONE',  ( 2.499999999999998668, 11.79166666939785202, -4.330127018922193649 ) ) ;
#13741 = ORIENTED_EDGE ( 'NONE', *, *, #31183, .T. ) ;
#13742 = CARTESIAN_POINT ( 'NONE',  ( 5.000000000000000000, -79.50000000000000000, -6.123233995736766282E-16 ) ) ;
#13743 = CARTESIAN_POINT ( 'NONE',  ( -2.500000000000000444, -80.04166666393547303, -4.330127018922193649 ) ) ;
#13745 = CARTESIAN_POINT ( 'NONE',  ( -5.000000000000000000, -27.99999999999999645, 0.000000000000000000 ) ) ;
#13744 = FACE_OUTER_BOUND ( 'NONE', #54736, .T. ) ;
#13746 = CARTESIAN_POINT ( 'NONE',  ( -2.229367062500000163, -32.47916666530106511, -3.861377020970580443 ) ) ;
#13747 = CARTESIAN_POINT ( 'NONE',  ( 1.060575238724906964E-15, -35.62499999726881583, 5.773502691896257311 ) ) ;
#13749 = ORIENTED_EDGE ( 'NONE', *, *, #56664, .T. ) ;
#13748 = CARTESIAN_POINT ( 'NONE',  ( -3.152548672688508926E-16, -61.56249999863440792, -5.148502694627439702 ) ) ;
#13750 = CARTESIAN_POINT ( 'NONE',  ( -53.51423613279429503, -149.5000000013655779, 4.591703134518082763 ) ) ;
#13752 = ORIENTED_EDGE ( 'NONE', *, *, #49381, .F. ) ;
#13751 = CARTESIAN_POINT ( 'NONE',  ( 4.458734124999998549, -7.979166665301073991, -2.574251347313721627 ) ) ;
#13753 = CARTESIAN_POINT ( 'NONE',  ( 5.000000000000000888, -78.58333333333334281, 2.886751345948126879 ) ) ;
#13754 = CARTESIAN_POINT ( 'NONE',  ( -59.29741812935640155, -135.6250000013655779, -2.196230717870135685 ) ) ;
#13755 = CARTESIAN_POINT ( 'NONE',  ( -3.152548672688508926E-16, -54.81249999863440081, -5.148502694627439702 ) ) ;
#13756 = CARTESIAN_POINT ( 'NONE',  ( 5.000000000000000000, -83.29166666393547303, -2.886751345948129988 ) ) ;
#13758 = ORIENTED_EDGE ( 'NONE', *, *, #35905, .T. ) ;
#13757 = CARTESIAN_POINT ( 'NONE',  ( 0.000000000000000000, -170.0000000000000000, 0.000000000000000000 ) ) ;
#13759 = CARTESIAN_POINT ( 'NONE',  ( -58.24261429053147765, -145.2500000000000284, -3.805975901505573855 ) ) ;
#13760 = CARTESIAN_POINT ( 'NONE',  ( -2.229367062500000163, -20.72916666530107221, -3.861377020970580443 ) ) ;
#13762 = ORIENTED_EDGE ( 'NONE', *, *, #6329, .F. ) ;
#13761 = CARTESIAN_POINT ( 'NONE',  ( -4.458734124999999437, -56.56249999863440081, 0.000000000000000000 ) ) ;
#13763 = PRESENTATION_STYLE_ASSIGNMENT (( #23110 ) ) ;
#13764 = CARTESIAN_POINT ( 'NONE',  ( -3.152801135295367096, -165.3125000013656063, -3.152801135295367541 ) ) ;
#13765 = CARTESIAN_POINT ( 'NONE',  ( -4.458734124999999437, -106.5624999986343937, 0.000000000000000000 ) ) ;
#13766 = CARTESIAN_POINT ( 'NONE',  ( -6.972266317189433020E-16, -69.12499999726880162, -5.000000000000000000 ) ) ;
#13767 = ORIENTED_EDGE ( 'NONE', *, *, #60053, .F. ) ;
#13768 = CARTESIAN_POINT ( 'NONE',  ( -55.35523342533222291, -148.5625000013656063, 4.444560631937231499 ) ) ;
#13769 = CARTESIAN_POINT ( 'NONE',  ( -59.81910112700025905, -138.3125000027312410, -2.462841084822630311 ) ) ;
#13770 = CARTESIAN_POINT ( 'NONE',  ( -2.229367062500000163, -36.47916666530107221, -3.861377020970580443 ) ) ;
#13771 =( BOUNDED_CURVE ( )  B_SPLINE_CURVE ( 2, ( #24286, #9486, #62911, #8556, #57772, #43889, #33313, #62288, #8870 ),
 .UNSPECIFIED., .F., .F. ) 
 B_SPLINE_CURVE_WITH_KNOTS ( ( 3, 2, 2, 2, 3 ),
 ( 0.8446428571428571397, 0.8452380952380952328, 0.8464285714285714191, 0.8476190476190476053, 0.8482142857142856984 ),
 .UNSPECIFIED. ) 
 CURVE ( )  GEOMETRIC_REPRESENTATION_ITEM ( )  RATIONAL_B_SPLINE_CURVE ( ( 0.9330127018922194093, 0.9330127018922194093, 1.000000000000000000, 0.8660254037844387076, 1.000000000000000000, 0.8660254037844387076, 1.000000000000000000, 0.9330127018922194093, 0.9330127018922194093 ) ) 
 REPRESENTATION_ITEM ( '' )  );
#13772 = CARTESIAN_POINT ( 'NONE',  ( -9.184850993605147944E-16, -153.3750000027311842, 5.000000000000000000 ) ) ;
#13773 = CARTESIAN_POINT ( 'NONE',  ( -4.458734124999998549, -6.229166665301072214, 2.574251347313722516 ) ) ;
#13774 = CARTESIAN_POINT ( 'NONE',  ( 9.457646018065525792E-16, -98.31249999863440792, 5.148502694627439702 ) ) ;
#13775 = VECTOR ( 'NONE', #39470, 1000.000000000000000 ) ;
#13776 = CARTESIAN_POINT ( 'NONE',  ( -1.846868145590737420, -143.0000000013655779, 4.458734124999999437 ) ) ;
#13777 = CARTESIAN_POINT ( 'NONE',  ( -3.152548672688508926E-16, -27.81249999863440436, -5.148502694627439702 ) ) ;
#13778 = CARTESIAN_POINT ( 'NONE',  ( 2.499999999999998668, -70.33333333333332860, -4.330127018922193649 ) ) ;
#13779 = CARTESIAN_POINT ( 'NONE',  ( -57.89159099828107458, -137.6875000013656063, -3.393966926194107447 ) ) ;
#13780 = CARTESIAN_POINT ( 'NONE',  ( -2.229367062500000163, -66.72916666530106511, -3.861377020970580443 ) ) ;
#13781 = CARTESIAN_POINT ( 'NONE',  ( -6.972266317189433020E-16, -73.12499999726878741, -5.000000000000000000 ) ) ;
#13782 = CARTESIAN_POINT ( 'NONE',  ( 1.339745962155612702, -88.16965819600733312, -5.000000000000000000 ) ) ;
#13783 = CARTESIAN_POINT ( 'NONE',  ( -3.152801135295367096, -143.0625000013655779, -3.152801135295367541 ) ) ;
#13784 = CARTESIAN_POINT ( 'NONE',  ( -2.229367062500000163, 7.270833334698929562, -3.861377020970580443 ) ) ;
#13785 = VERTEX_POINT ( 'NONE', #29241 ) ;
#13786 = CARTESIAN_POINT ( 'NONE',  ( 5.000000000000000888, -159.9375000000000000, -2.071067811865475505 ) ) ;
#13788 = CARTESIAN_POINT ( 'NONE',  ( -4.458734124999999437, -28.39583333196774007, -2.574251347313719407 ) ) ;
#13787 = CARTESIAN_POINT ( 'NONE',  ( -5.000000000000000000, -93.00000000000000000, 0.000000000000000000 ) ) ;
#13789 = CARTESIAN_POINT ( 'NONE',  ( 2.499999999999998668, -14.20833333060214976, -4.330127018922193649 ) ) ;
#13790 = CARTESIAN_POINT ( 'NONE',  ( -2.229367062500000163, -76.72916666530106511, -3.861377020970580443 ) ) ;
#13791 = CARTESIAN_POINT ( 'NONE',  ( -3.152548672688508926E-16, 22.18750000136559564, -5.148502694627439702 ) ) ;
#13792 = B_SPLINE_CURVE_WITH_KNOTS ( 'NONE', 3,
 ( #36396, #27372, #7138, #12274, #26753, #31888, #42168, #61175, #61804 ),
 .UNSPECIFIED., .F., .F.,
 ( 4, 2, 1, 2, 4 ),
 ( 0.000000000000000000, 0.002165063509461098365, 0.004330127018922195863, 0.006495190528383293360, 0.008660254037844389990 ),
 .UNSPECIFIED. ) ;
#13793 = CARTESIAN_POINT ( 'NONE',  ( -1.339745962155617365, 23.33034180399266333, 4.999999999999998224 ) ) ;
#13794 = CARTESIAN_POINT ( 'NONE',  ( -52.10840900171896806, -141.1875000013656063, 3.393966926194110556 ) ) ;
#13795 = EDGE_CURVE ( 'NONE', #23803, #47078, #32901, .T. ) ;
#13796 = EDGE_CURVE ( 'NONE', #38436, #18131, #28932, .T. ) ;
#13797 = CARTESIAN_POINT ( 'NONE',  ( 2.229367062499998831, 1.354166668032261933, -3.861377020970580887 ) ) ;
#13798 = CARTESIAN_POINT ( 'NONE',  ( 4.458734124999999437, 26.93750000136559564, -5.460374474430324690E-16 ) ) ;
#13799 = CARTESIAN_POINT ( 'NONE',  ( -4.458734124999999437, -38.64583333196773651, -2.574251347313719407 ) ) ;
#13801 = EDGE_CURVE ( 'NONE', #592, #51356, #16928, .T. ) ;
#13800 = CARTESIAN_POINT ( 'NONE',  ( 2.499999999999998668, -80.33333333333332860, -4.330127018922193649 ) ) ;
#13802 = CARTESIAN_POINT ( 'NONE',  ( -2.229367062500000163, 3.520833334698929118, -3.861377020970580443 ) ) ;
#13803 = CARTESIAN_POINT ( 'NONE',  ( 9.457646018065525792E-16, -24.31249999863440436, 5.148502694627439702 ) ) ;
#13804 = CARTESIAN_POINT ( 'NONE',  ( -4.458734125000001214, -155.8750000013655779, 1.846868145590734089 ) ) ;
#13805 = CARTESIAN_POINT ( 'NONE',  ( -4.458734124999999437, -67.31249999863440792, 0.000000000000000000 ) ) ;
#13806 = CARTESIAN_POINT ( 'NONE',  ( -2.499999999999996447, -101.7083333306021444, 4.330127018922195425 ) ) ;
#13807 = EDGE_CURVE ( 'NONE', #1258, #57064, #57911, .T. ) ;
#13808 = CARTESIAN_POINT ( 'NONE',  ( 1.339745962155602488, 15.29465819873851729, 5.000000000000007105 ) ) ;
#13809 = CARTESIAN_POINT ( 'NONE',  ( 0.000000000000000000, -120.0000000000000000, 5.000000000000000000 ) ) ;
#13810 = EDGE_CURVE ( 'NONE', #62694, #15950, #21824, .T. ) ;
#13811 = CARTESIAN_POINT ( 'NONE',  ( -2.229367062499996610, -107.3958333319677365, 3.861377020970582219 ) ) ;
#13812 = CARTESIAN_POINT ( 'NONE',  ( -4.458734124999997661, -75.47916666530106511, 2.574251347313722516 ) ) ;
#13813 = CARTESIAN_POINT ( 'NONE',  ( 1.060575238724906964E-15, -55.74999999999999289, 5.773502691896257311 ) ) ;
#13814 = CARTESIAN_POINT ( 'NONE',  ( 1.339745962155612702, -73.29465819873851729, -5.000000000000000000 ) ) ;
#13815 = CARTESIAN_POINT ( 'NONE',  ( 3.535533905932738197, -156.0000000027312126, -3.535533905932738197 ) ) ;
#13816 = ORIENTED_EDGE ( 'NONE', *, *, #5149, .F. ) ;
#13817 = DIRECTION ( 'NONE',  ( 0.000000000000000000, 0.000000000000000000, 1.000000000000000000 ) ) ;
#13818 = CARTESIAN_POINT ( 'NONE',  ( -6.972266317189433020E-16, 11.87500000273118594, -5.000000000000000000 ) ) ;
#13819 = CARTESIAN_POINT ( 'NONE',  ( -5.000000000000000000, -13.08333333333333570, -2.886751345948128211 ) ) ;
#13820 = CARTESIAN_POINT ( 'NONE',  ( 4.458734124999999437, -17.81249999863440792, -5.460374474430324690E-16 ) ) ;
#13821 = ADVANCED_FACE ( 'NONE', ( #3879 ), #23498, .T. ) ;
#13822 = CARTESIAN_POINT ( 'NONE',  ( 4.458734125000000326, -76.89583333196773651, 2.574251347313718519 ) ) ;
#13823 = CARTESIAN_POINT ( 'NONE',  ( -3.152801135295367985, -167.0625000013656063, 3.152801135295367096 ) ) ;
#13824 = CARTESIAN_POINT ( 'NONE',  ( 5.000000000000000000, -19.37499999726881583, -6.123233995736766282E-16 ) ) ;
#13826 = ORIENTED_EDGE ( 'NONE', *, *, #30346, .F. ) ;
#13825 = CARTESIAN_POINT ( 'NONE',  ( -4.458734124999999437, -42.39583333196773651, -2.574251347313719407 ) ) ;
#13827 = CARTESIAN_POINT ( 'NONE',  ( 7.500000000000001776, 0.000000000000000000, 0.000000000000000000 ) ) ;
#13829 = VERTEX_POINT ( 'NONE', #62741 ) ;
#13828 = CARTESIAN_POINT ( 'NONE',  ( 2.229367062499998831, 7.104166668032259935, -3.861377020970580887 ) ) ;
#13830 = CARTESIAN_POINT ( 'NONE',  ( -59.59170313451810586, -153.5000000013656063, 1.485763867205729394 ) ) ;
#13831 = CARTESIAN_POINT ( 'NONE',  ( 5.000000000000000888, -61.58333333333334281, 2.886751345948126879 ) ) ;
#13832 = CARTESIAN_POINT ( 'NONE',  ( 2.730187237215162345E-16, -157.4375000013655779, -4.458734124999999437 ) ) ;
#13833 = CARTESIAN_POINT ( 'NONE',  ( -3.152548672688508926E-16, -39.81249999863440081, -5.148502694627439702 ) ) ;
#13834 = CARTESIAN_POINT ( 'NONE',  ( 2.071067811865476394, -167.1875000000000284, 5.000000000000000000 ) ) ;
#13835 = CARTESIAN_POINT ( 'NONE',  ( 1.339745962155612702, 5.830341803992665106, -5.000000000000000000 ) ) ;
#13836 = CARTESIAN_POINT ( 'NONE',  ( -54.64476657466781973, -132.0625000013656063, -4.444560631937228834 ) ) ;
#13837 = CARTESIAN_POINT ( 'NONE',  ( 9.457646018065525792E-16, -4.312499998634408804, 5.148502694627439702 ) ) ;
#13838 = CARTESIAN_POINT ( 'NONE',  ( -2.229367062499996610, -40.39583333196773651, 3.861377020970582219 ) ) ;
#13839 = CARTESIAN_POINT ( 'NONE',  ( 1.339745962155615144, -26.70534180126147561, 4.999999999999999112 ) ) ;
#13840 = CARTESIAN_POINT ( 'NONE',  ( -4.458734124999999437, -147.9375000013656063, -5.460374474430324690E-16 ) ) ;
#13841 = CARTESIAN_POINT ( 'NONE',  ( 2.229367062499998831, -85.89583333196773651, -3.861377020970580887 ) ) ;
#13842 = CARTESIAN_POINT ( 'NONE',  ( -6.972266317189433020E-16, 8.750000000000000000, -5.000000000000000000 ) ) ;
#13843 = ORIENTED_EDGE ( 'NONE', *, *, #15606, .T. ) ;
#13844 = CARTESIAN_POINT ( 'NONE',  ( -59.98410592259440222, -151.2500000027312410, -0.3983568153799752487 ) ) ;
#13845 = CARTESIAN_POINT ( 'NONE',  ( -7.894787914004607998, -1.230850257101226302E-13, -7.591390474663425536 ) ) ;
#13846 = CARTESIAN_POINT ( 'NONE',  ( 2.229367062500001939, -76.22916666530106511, 3.861377020970579999 ) ) ;
#13847 = ORIENTED_EDGE ( 'NONE', *, *, #58177, .T. ) ;
#13848 =( BOUNDED_CURVE ( )  B_SPLINE_CURVE ( 2, ( #42708, #37575, #62034, #27918, #43029, #52994, #3490, #47238, #22485 ),
 .UNSPECIFIED., .F., .F. ) 
 B_SPLINE_CURVE_WITH_KNOTS ( ( 3, 2, 2, 2, 3 ),
 ( 0.7854166666666666519, 0.7861111111111110938, 0.7874999999999999778, 0.7888888888888888618, 0.7895833333333333037 ),
 .UNSPECIFIED. ) 
 CURVE ( )  GEOMETRIC_REPRESENTATION_ITEM ( )  RATIONAL_B_SPLINE_CURVE ( ( 0.9330127018922194093, 0.9330127018922194093, 1.000000000000000000, 0.8660254037844387076, 1.000000000000000000, 0.8660254037844387076, 1.000000000000000000, 0.9330127018922194093, 0.9330127018922194093 ) ) 
 REPRESENTATION_ITEM ( '' )  );
#13849 = CARTESIAN_POINT ( 'NONE',  ( 0.000000000000000000, -170.0000000000000000, 0.000000000000000000 ) ) ;
#13850 = CARTESIAN_POINT ( 'NONE',  ( -4.458734124999999437, -10.56249999863440792, 0.000000000000000000 ) ) ;
#13851 = CARTESIAN_POINT ( 'NONE',  ( 5.000000000000000000, -79.37499999726881583, -6.123233995736766282E-16 ) ) ;
#13852 = CARTESIAN_POINT ( 'NONE',  ( 2.229367062499998831, 0.3541666680322609340, -3.861377020970580887 ) ) ;
#13853 = CARTESIAN_POINT ( 'NONE',  ( -4.999999999999998224, -79.91666666666667140, 2.886751345948131764 ) ) ;
#13854 = CARTESIAN_POINT ( 'NONE',  ( -4.458734124999999437, -155.0000000013656063, -1.846868145590735644 ) ) ;
#13855 = CARTESIAN_POINT ( 'NONE',  ( -3.152548672688508926E-16, 19.18750000136559208, -5.148502694627439702 ) ) ;
#13856 = ORIENTED_EDGE ( 'NONE', *, *, #42939, .F. ) ;
#13857 = CARTESIAN_POINT ( 'NONE',  ( -4.458734124999997661, -92.22916666530106511, 2.574251347313722516 ) ) ;
#13858 = CARTESIAN_POINT ( 'NONE',  ( 5.000000000000000888, -47.58333333333333570, 2.886751345948126879 ) ) ;
#13859 = CARTESIAN_POINT ( 'NONE',  ( -4.999999999999998224, -103.7916666639354730, 2.886751345948131764 ) ) ;
#13860 = CARTESIAN_POINT ( 'NONE',  ( -3.152548672688508926E-16, -6.562499998634404363, -5.148502694627439702 ) ) ;
#13861 = CARTESIAN_POINT ( 'NONE',  ( 1.975475456537005874E-15, -69.62499999726880162, 5.000000000000000000 ) ) ;
#13862 = CYLINDRICAL_SURFACE ( 'NONE', #55106, 5.000000000000000000 ) ;
#13863 = AXIS2_PLACEMENT_3D ( 'NONE', #5055, #19204, #19841 ) ;
#13864 =( BOUNDED_CURVE ( )  B_SPLINE_CURVE ( 2, ( #51691, #56523, #22742, #11799, #32379, #47178, #26280, #56839, #3121 ),
 .UNSPECIFIED., .F., .F. ) 
 B_SPLINE_CURVE_WITH_KNOTS ( ( 3, 2, 2, 2, 3 ),
 ( 0.3250000000000002887, 0.3291666666666669405, 0.3333333333333335924, 0.3375000000000002998, 0.3416666666666669516 ),
 .UNSPECIFIED. ) 
 CURVE ( )  GEOMETRIC_REPRESENTATION_ITEM ( )  RATIONAL_B_SPLINE_CURVE ( ( 0.9999999999999948930, 0.9238795325112918455, 1.000000000000000000, 0.9238795325112867385, 1.000000000000000000, 0.9238795325112867385, 1.000000000000000000, 0.9238795325112816315, 1.000000000000005107 ) ) 
 REPRESENTATION_ITEM ( '' )  );
#13865 = CARTESIAN_POINT ( 'NONE',  ( -52.80376928212989185, -151.8750000013655779, -4.297418129356379346 ) ) ;
#13866 = EDGE_CURVE ( 'NONE', #9036, #3130, #28377, .T. ) ;
#13867 = CARTESIAN_POINT ( 'NONE',  ( -5.000000000000000000, -34.95833333060213732, -2.886751345948128211 ) ) ;
#13868 = DIRECTION ( 'NONE',  ( -0.000000000000000000, 1.000000000000000000, -0.000000000000000000 ) ) ;
#13869 = CARTESIAN_POINT ( 'NONE',  ( -3.152548672688508926E-16, 21.43750000136559208, -5.148502694627439702 ) ) ;
#13870 = CARTESIAN_POINT ( 'NONE',  ( -5.000000000000000000, -72.08333333333332860, -2.886751345948128211 ) ) ;
#13871 = CARTESIAN_POINT ( 'NONE',  ( 4.458734124999999437, 25.18750000136559208, -5.460374474430324690E-16 ) ) ;
#13872 = CARTESIAN_POINT ( 'NONE',  ( -4.458734124999999437, -56.31249999863440081, 0.000000000000000000 ) ) ;
#13873 = CARTESIAN_POINT ( 'NONE',  ( 9.457646018065525792E-16, -11.31249999863440792, 5.148502694627439702 ) ) ;
#13874 = LINE ( 'NONE', #48278, #13447 ) ;
#13875 = CARTESIAN_POINT ( 'NONE',  ( -2.500000000000000444, 7.833333333333334814, -4.330127018922193649 ) ) ;
#13876 = CARTESIAN_POINT ( 'NONE',  ( -1.846868145590737420, -168.7500000013656063, 4.458734124999999437 ) ) ;
#13877 = CARTESIAN_POINT ( 'NONE',  ( 1.975475456537005874E-15, -69.74999999999998579, 5.000000000000000000 ) ) ;
#13878 = CARTESIAN_POINT ( 'NONE',  ( -2.229367062500000163, -55.47916666530107221, -3.861377020970580443 ) ) ;
#13879 = CARTESIAN_POINT ( 'NONE',  ( 1.060575238724906964E-15, -83.62499999726881583, 5.773502691896257311 ) ) ;
#13880 = CARTESIAN_POINT ( 'NONE',  ( -59.59170313451811296, -137.7500000013656063, 1.485763867205729394 ) ) ;
#13881 = CARTESIAN_POINT ( 'NONE',  ( 1.339745962155557191, -37.58034179853029855, 5.000000000000032863 ) ) ;
#13882 = CARTESIAN_POINT ( 'NONE',  ( -75.00000000000000000, 15.00000000000000000, 8.999999999999998224 ) ) ;
#13883 = CARTESIAN_POINT ( 'NONE',  ( -4.458734124999999437, -92.56249999863440792, 0.000000000000000000 ) ) ;
#13884 = CARTESIAN_POINT ( 'NONE',  ( -4.458734124999999437, -157.2500000013656063, -1.846868145590735644 ) ) ;
#13885 = CARTESIAN_POINT ( 'NONE',  ( 1.060575238724906964E-15, -38.74999999999998579, 5.773502691896257311 ) ) ;
#13886 = CARTESIAN_POINT ( 'NONE',  ( -2.500000000000000444, -20.04166666393548013, -4.330127018922193649 ) ) ;
#13887 = EDGE_CURVE ( 'NONE', #31992, #2252, #39070, .T. ) ;
#13888 = DIRECTION ( 'NONE',  ( -0.000000000000000000, 1.000000000000000000, -0.000000000000000000 ) ) ;
#13889 = ORIENTED_EDGE ( 'NONE', *, *, #53458, .F. ) ;
#13890 = CARTESIAN_POINT ( 'NONE',  ( -3.152548672688508926E-16, -97.56249999863440792, -5.148502694627439702 ) ) ;
#13891 = CARTESIAN_POINT ( 'NONE',  ( -4.458734124999999437, 10.35416666803225816, -2.574251347313719407 ) ) ;
#13892 = CARTESIAN_POINT ( 'NONE',  ( -3.535250795749689387E-16, 10.87500000273118417, -5.773502691896257311 ) ) ;
#13893 = CARTESIAN_POINT ( 'NONE',  ( -6.972266317189433020E-16, -80.24999999999998579, -5.000000000000000000 ) ) ;
#13894 = EDGE_CURVE ( 'NONE', #30039, #49750, #15741, .T. ) ;
#13895 = CARTESIAN_POINT ( 'NONE',  ( -2.499999999999996447, 5.166666666666666963, 4.330127018922195425 ) ) ;
#13896 = CARTESIAN_POINT ( 'NONE',  ( -3.152548672688508926E-16, -60.56249999863440792, -5.148502694627439702 ) ) ;
#13897 = CARTESIAN_POINT ( 'NONE',  ( 0.000000000000000000, 0.000000000000000000, 0.000000000000000000 ) ) ;
#13898 = EDGE_CURVE ( 'NONE', #44027, #57843, #56393, .T. ) ;
#13899 = CARTESIAN_POINT ( 'NONE',  ( 5.000000000000000000, 2.708333336064520314, -2.886751345948129988 ) ) ;
#13900 = CARTESIAN_POINT ( 'NONE',  ( -2.229367062499996610, -30.14583333196773651, 3.861377020970582219 ) ) ;
#13901 = CARTESIAN_POINT ( 'NONE',  ( -5.000000000000000000, -11.00000000000000355, 0.000000000000000000 ) ) ;
#13902 = CARTESIAN_POINT ( 'NONE',  ( 5.000000000000000000, 19.58333333333333215, -2.886751345948130876 ) ) ;
#13903 = CARTESIAN_POINT ( 'NONE',  ( -5.000000000000000000, -46.00000000000000000, 0.000000000000000000 ) ) ;
#13905 = CARTESIAN_POINT ( 'NONE',  ( 4.458734124999998549, -17.97916666530106866, -2.574251347313721627 ) ) ;
#13904 = CARTESIAN_POINT ( 'NONE',  ( -1.339745962155606929, 23.91965820146970145, -5.000000000000004441 ) ) ;
#13906 = CARTESIAN_POINT ( 'NONE',  ( 3.061616997868383141E-16, -154.7500000000000000, -5.000000000000000000 ) ) ;
#13907 = CARTESIAN_POINT ( 'NONE',  ( 2.229367062500001939, -68.97916666530107932, 3.861377020970579999 ) ) ;
#13908 = CARTESIAN_POINT ( 'NONE',  ( -3.152801135295367985, -149.0625000013655779, 3.152801135295367096 ) ) ;
#13909 = CARTESIAN_POINT ( 'NONE',  ( -2.229367062500000163, -77.47916666530106511, -3.861377020970580443 ) ) ;
#13910 = CARTESIAN_POINT ( 'NONE',  ( -52.10840900171896806, -141.4375000013656063, 3.393966926194110556 ) ) ;
#13911 = AXIS2_PLACEMENT_3D ( 'NONE', #37064, #8423, #61515 ) ;
#13912 = CARTESIAN_POINT ( 'NONE',  ( -3.152548672688508926E-16, -22.81249999863440436, -5.148502694627439702 ) ) ;
#13913 = CARTESIAN_POINT ( 'NONE',  ( -5.000000000000000000, -65.87499999726881583, 0.000000000000000000 ) ) ;
#13914 = EDGE_LOOP ( 'NONE', ( #10654, #47424, #58850, #7296 ) ) ;
#13915 = LINE ( 'NONE', #9095, #31265 ) ;
#13916 = ORIENTED_EDGE ( 'NONE', *, *, #29545, .F. ) ;
#13917 = CARTESIAN_POINT ( 'NONE',  ( -4.458734124999998549, -65.47916666530107932, 2.574251347313722516 ) ) ;
#13918 = CARTESIAN_POINT ( 'NONE',  ( -51.19402409849444524, -150.5000000000000284, -3.242614290531456334 ) ) ;
#13919 = DIRECTION ( 'NONE',  ( 1.000000000000000000, 0.000000000000000000, 0.000000000000000000 ) ) ;
#13920 = ORIENTED_EDGE ( 'NONE', *, *, #33494, .T. ) ;
#13921 =( BOUNDED_CURVE ( )  B_SPLINE_CURVE ( 2, ( #10544, #53659, #9593, #9904, #15380, #24391, #35004, #19877, #43994 ),
 .UNSPECIFIED., .F., .F. ) 
 B_SPLINE_CURVE_WITH_KNOTS ( ( 3, 2, 2, 2, 3 ),
 ( 0.3416666666666669516, 0.3458333333333336035, 0.3500000000000002554, 0.3541666666666669627, 0.3583333333333336146 ),
 .UNSPECIFIED. ) 
 CURVE ( )  GEOMETRIC_REPRESENTATION_ITEM ( )  RATIONAL_B_SPLINE_CURVE ( ( 0.9999999999999948930, 0.9238795325112918455, 1.000000000000000000, 0.9238795325112867385, 1.000000000000000000, 0.9238795325112867385, 1.000000000000000000, 0.9238795325112816315, 1.000000000000005107 ) ) 
 REPRESENTATION_ITEM ( '' )  );
#13922 = CYLINDRICAL_SURFACE ( 'NONE', #1414, 5.000000000000000000 ) ;
#13923 = CARTESIAN_POINT ( 'NONE',  ( -2.229367062500000163, -54.72916666530107221, -3.861377020970580443 ) ) ;
#13924 = CARTESIAN_POINT ( 'NONE',  ( -2.229367062499996610, 3.604166668032260379, 3.861377020970582219 ) ) ;
#13925 = VERTEX_POINT ( 'NONE', #14769 ) ;
#13926 = DIRECTION ( 'NONE',  ( -0.000000000000000000, 1.000000000000000000, -0.000000000000000000 ) ) ;
#13927 = CARTESIAN_POINT ( 'NONE',  ( -3.152548672688508926E-16, 19.43750000136559208, -5.148502694627439702 ) ) ;
#13928 = CARTESIAN_POINT ( 'NONE',  ( -50.40829686548195099, -144.0000000013656063, -1.485763867205728284 ) ) ;
#13929 = CARTESIAN_POINT ( 'NONE',  ( -2.498395430326213474E-14, 20.37500000273118062, 5.000000000000000000 ) ) ;
#13930 = CARTESIAN_POINT ( 'NONE',  ( 3.152801135295366208, -163.5625000013656063, 3.152801135295367985 ) ) ;
#13931 = ORIENTED_EDGE ( 'NONE', *, *, #28064, .T. ) ;
#13932 = CARTESIAN_POINT ( 'NONE',  ( 2.229367062500001939, -77.97916666530106511, 3.861377020970579999 ) ) ;
#13933 = CARTESIAN_POINT ( 'NONE',  ( -6.972266317189433020E-16, -52.12499999726880873, -5.000000000000000000 ) ) ;
#13934 = CARTESIAN_POINT ( 'NONE',  ( -3.152548672688508926E-16, 7.437500001365594748, -5.148502694627439702 ) ) ;
#13935 = EDGE_CURVE ( 'NONE', #6651, #25665, #17306, .T. ) ;
#13936 = CARTESIAN_POINT ( 'NONE',  ( 6.123233995736766282E-16, -170.0000000000000000, -5.000000000000000000 ) ) ;
#13937 = CARTESIAN_POINT ( 'NONE',  ( 9.457646018065525792E-16, -60.31249999863440792, 5.148502694627439702 ) ) ;
#13938 = CARTESIAN_POINT ( 'NONE',  ( 2.499999999999998668, -22.20833333060215153, -4.330127018922193649 ) ) ;
#13939 = CARTESIAN_POINT ( 'NONE',  ( 2.499999999999998668, -96.20833333060213022, -4.330127018922193649 ) ) ;
#13940 = CARTESIAN_POINT ( 'NONE',  ( -6.972266317189433020E-16, -44.12499999726880162, -5.000000000000000000 ) ) ;
#13941 = CARTESIAN_POINT ( 'NONE',  ( 5.000000000000000888, -49.58333333333332149, 2.886751345948126879 ) ) ;
#13942 = DIRECTION ( 'NONE',  ( -0.000000000000000000, 1.000000000000000000, -0.000000000000000000 ) ) ;
#13943 = CARTESIAN_POINT ( 'NONE',  ( -51.75738570946856498, -146.7500000000000284, 3.805975901505576964 ) ) ;
#13944 = CARTESIAN_POINT ( 'NONE',  ( -3.152548672688508926E-16, -41.56249999863439371, -5.148502694627439702 ) ) ;
#13945 = CARTESIAN_POINT ( 'NONE',  ( 4.458734124999999437, -27.06249999863440081, -5.460374474430324690E-16 ) ) ;
#13946 = CARTESIAN_POINT ( 'NONE',  ( 5.000000000000000888, 11.41666666666666607, 2.886751345948126879 ) ) ;
#13947 = CARTESIAN_POINT ( 'NONE',  ( 5.000000000000000000, 25.58333333333333215, -2.886751345948129988 ) ) ;
#13948 = CARTESIAN_POINT ( 'NONE',  ( 5.000000000000000000, -148.1875000027312126, 2.071067811865478614 ) ) ;
#13949 = CARTESIAN_POINT ( 'NONE',  ( 4.458734125000001214, -107.1458333319677507, 2.574251347313718519 ) ) ;
#13950 = CARTESIAN_POINT ( 'NONE',  ( -3.152548672688508926E-16, -33.56249999863440792, -5.148502694627439702 ) ) ;
#13951 = CARTESIAN_POINT ( 'NONE',  ( -3.535250795749689387E-16, -68.12499999726881583, -5.773502691896257311 ) ) ;
#13952 = AXIS2_PLACEMENT_3D ( 'NONE', #50688, #59388, #15644 ) ;
#13953 = CARTESIAN_POINT ( 'NONE',  ( -50.40829686548195099, -147.2500000013656063, -1.485763867205728284 ) ) ;
#13954 = CARTESIAN_POINT ( 'NONE',  ( 2.071067811865476394, -144.1875000000000000, 5.000000000000000000 ) ) ;
#13955 = CARTESIAN_POINT ( 'NONE',  ( -4.458734124999997661, -77.47916666530106511, 2.574251347313722516 ) ) ;
#13956 = CARTESIAN_POINT ( 'NONE',  ( -4.458734125000000326, -169.1250000013656063, 1.846868145590734089 ) ) ;
#13957 = CARTESIAN_POINT ( 'NONE',  ( 2.229367062500001939, -32.97916666530106511, 3.861377020970579999 ) ) ;
#13958 = CARTESIAN_POINT ( 'NONE',  ( -6.972266317189433020E-16, -28.12499999726880873, -5.000000000000000000 ) ) ;
#13959 = DIRECTION ( 'NONE',  ( -0.000000000000000000, 1.000000000000000000, -0.000000000000000000 ) ) ;
#13960 = CARTESIAN_POINT ( 'NONE',  ( 5.000000000000000888, -19.58333333333333215, 2.886751345948126879 ) ) ;
#13961 = CARTESIAN_POINT ( 'NONE',  ( 4.458734124999999437, -149.5000000013655779, 1.846868145590737864 ) ) ;
#13962 = ORIENTED_EDGE ( 'NONE', *, *, #14942, .F. ) ;
#13963 = CARTESIAN_POINT ( 'NONE',  ( 4.458734124999998549, 29.02083333469893134, -2.574251347313721627 ) ) ;
#13964 = CARTESIAN_POINT ( 'NONE',  ( -59.98410592259440222, -141.1250000000000284, -0.3983568153799752487 ) ) ;
#13965 = CARTESIAN_POINT ( 'NONE',  ( -4.458734124999999437, -55.56249999863440081, 0.000000000000000000 ) ) ;
#13966 = DIRECTION ( 'NONE',  ( 0.6485228581062915110, 0.000000000000000000, 0.7611951803011149931 ) ) ;
#13967 =( BOUNDED_CURVE ( )  B_SPLINE_CURVE ( 2, ( #32219, #37681, #18690, #26211, #61832, #57323, #23207, #17754, #13239 ),
 .UNSPECIFIED., .F., .F. ) 
 B_SPLINE_CURVE_WITH_KNOTS ( ( 3, 2, 2, 2, 3 ),
 ( 0.4354166666666666741, 0.4361111111111111160, 0.4375000000000000000, 0.4388888888888888840, 0.4395833333333333259 ),
 .UNSPECIFIED. ) 
 CURVE ( )  GEOMETRIC_REPRESENTATION_ITEM ( )  RATIONAL_B_SPLINE_CURVE ( ( 0.9330127018922194093, 0.9330127018922194093, 1.000000000000000000, 0.8660254037844387076, 1.000000000000000000, 0.8660254037844387076, 1.000000000000000000, 0.9330127018922194093, 0.9330127018922194093 ) ) 
 REPRESENTATION_ITEM ( '' )  );
#13968 = CARTESIAN_POINT ( 'NONE',  ( 2.500000000000002220, 4.458333336064518093, 4.330127018922192761 ) ) ;
#13969 = CARTESIAN_POINT ( 'NONE',  ( 1.060575238724906964E-15, 18.24999999999999645, 5.773502691896257311 ) ) ;
#13970 = CARTESIAN_POINT ( 'NONE',  ( 0.000000000000000000, -170.0000000000000000, 0.000000000000000000 ) ) ;
#13971 = CARTESIAN_POINT ( 'NONE',  ( -4.458734124999998549, -8.229166665301073991, 2.574251347313722516 ) ) ;
#13972 = CARTESIAN_POINT ( 'NONE',  ( -5.000000000000000000, -154.5000000000000284, -6.123233995736766282E-16 ) ) ;
#13973 = CARTESIAN_POINT ( 'NONE',  ( 5.000000000000000000, -165.1875000027312126, 2.071067811865478614 ) ) ;
#13974 = CARTESIAN_POINT ( 'NONE',  ( 4.458734124999999437, 10.93750000136559386, -5.460374474430324690E-16 ) ) ;
#13975 = CARTESIAN_POINT ( 'NONE',  ( -2.249002180491467900E-14, 9.016154170237591359, -7.999534413642735764 ) ) ;
#13976 = ORIENTED_EDGE ( 'NONE', *, *, #24062, .F. ) ;
#13977 = CARTESIAN_POINT ( 'NONE',  ( 5.000000000000000888, -97.45833333060213022, 2.886751345948126879 ) ) ;
#13978 = CARTESIAN_POINT ( 'NONE',  ( -4.458734124999999437, -50.39583333196773651, -2.574251347313719407 ) ) ;
#13979 = CARTESIAN_POINT ( 'NONE',  ( -4.458734125000001214, -161.1250000013656063, 1.846868145590734089 ) ) ;
#13980 = CARTESIAN_POINT ( 'NONE',  ( 1.060575238724906964E-15, -52.62499999726881583, 5.773502691896257311 ) ) ;
#13981 = ORIENTED_EDGE ( 'NONE', *, *, #45977, .F. ) ;
#13982 = CARTESIAN_POINT ( 'NONE',  ( -2.229367062499996610, 2.604166668032259491, 3.861377020970582219 ) ) ;
#13983 = ORIENTED_EDGE ( 'NONE', *, *, #28401, .T. ) ;
#13985 = CARTESIAN_POINT ( 'NONE',  ( -55.00000000000002132, -155.0000000000000284, 1.734723475976807094E-15 ) ) ;
#13984 = CARTESIAN_POINT ( 'NONE',  ( 5.000000000000000000, -4.416666666666666075, -2.886751345948130876 ) ) ;
#13986 = CARTESIAN_POINT ( 'NONE',  ( -3.152801135295367985, -158.8125000013656063, 3.152801135295367096 ) ) ;
#13987 = ORIENTED_EDGE ( 'NONE', *, *, #42115, .F. ) ;
#13988 = VECTOR ( 'NONE', #12079, 1000.000000000000000 ) ;
#13989 = CARTESIAN_POINT ( 'NONE',  ( 1.339745962155615144, -83.70534180126149693, 4.999999999999999112 ) ) ;
#13990 = CARTESIAN_POINT ( 'NONE',  ( -51.19402409849444524, -132.5000000000000284, -3.242614290531456334 ) ) ;
#13991 = EDGE_CURVE ( 'NONE', #35553, #60346, #45008, .T. ) ;
#13992 = CARTESIAN_POINT ( 'NONE',  ( 1.339745962155615144, -53.58034179853029144, 4.999999999999999112 ) ) ;
#13993 = CARTESIAN_POINT ( 'NONE',  ( -4.458734124999999437, -37.56249999863440792, 0.000000000000000000 ) ) ;
#13994 = ORIENTED_EDGE ( 'NONE', *, *, #7853, .T. ) ;
#13995 = AXIS2_PLACEMENT_3D ( 'NONE', #61667, #8263, #36571 ) ;
#13996 = CARTESIAN_POINT ( 'NONE',  ( 2.229367062499998831, -84.64583333196773651, -3.861377020970580887 ) ) ;
#13997 = CARTESIAN_POINT ( 'NONE',  ( -4.458734124999998549, 21.77083333469892779, 2.574251347313722516 ) ) ;
#13998 = CARTESIAN_POINT ( 'NONE',  ( 1.339745962155612702, -24.16965819600733312, -5.000000000000000000 ) ) ;
#13999 = ORIENTED_EDGE ( 'NONE', *, *, #46738, .T. ) ;
#14000 = CARTESIAN_POINT ( 'NONE',  ( -4.458734124999999437, -87.64583333196773651, -2.574251347313719407 ) ) ;
#14001 = CARTESIAN_POINT ( 'NONE',  ( -50.18089887299979068, -127.8125000027312268, 2.462841084822635640 ) ) ;
#14002 = CARTESIAN_POINT ( 'NONE',  ( -58.24261429053147765, -152.3750000027312126, -3.805975901505573855 ) ) ;
#14003 = CARTESIAN_POINT ( 'NONE',  ( -51.25318514546815862, -135.0000000000000853, 2.888716472484426312 ) ) ;
#14004 = CARTESIAN_POINT ( 'NONE',  ( 1.339745962155612702, 4.705341801261479162, -5.000000000000000000 ) ) ;
#14005 = CARTESIAN_POINT ( 'NONE',  ( -3.152548672688508926E-16, -62.56249999863440792, -5.148502694627439702 ) ) ;
#14006 = CARTESIAN_POINT ( 'NONE',  ( -5.000000000000000000, -84.95833333060213022, -2.886751345948128211 ) ) ;
#14007 = CARTESIAN_POINT ( 'NONE',  ( -2.229367062499996610, 22.85416666803225993, 3.861377020970582219 ) ) ;
#14008 = CARTESIAN_POINT ( 'NONE',  ( 1.339745962155612702, -97.29465819873851729, -5.000000000000000000 ) ) ;
#14009 = CARTESIAN_POINT ( 'NONE',  ( -2.499999999999996447, -81.83333333333332860, 4.330127018922195425 ) ) ;
#14010 = CARTESIAN_POINT ( 'NONE',  ( -2.229367062500000163, -45.72916666530106511, -3.861377020970580443 ) ) ;
#14011 = CARTESIAN_POINT ( 'NONE',  ( 5.000000000000000000, -4.291666663935479242, -2.886751345948129988 ) ) ;
#14012 = CARTESIAN_POINT ( 'NONE',  ( 2.499999999999998668, -31.33333333333333215, -4.330127018922193649 ) ) ;
#14013 = CARTESIAN_POINT ( 'NONE',  ( 1.975475456537005874E-15, -56.62499999726880162, 5.000000000000000000 ) ) ;
#14014 = CARTESIAN_POINT ( 'NONE',  ( -2.229367062499996610, -84.39583333196773651, 3.861377020970582219 ) ) ;
#14015 = CARTESIAN_POINT ( 'NONE',  ( 4.458734125000000326, -106.8958333319677649, 2.574251347313718519 ) ) ;
#14016 = CARTESIAN_POINT ( 'NONE',  ( -4.458734124999997661, -9.479166665301068662, 2.574251347313722516 ) ) ;
#14017 = ORIENTED_EDGE ( 'NONE', *, *, #14087, .F. ) ;
#14018 = CARTESIAN_POINT ( 'NONE',  ( -1.339745962155613812, -17.08034179853029144, -5.000000000000000000 ) ) ;
#14019 = CARTESIAN_POINT ( 'NONE',  ( 2.229367062500001939, -100.9791666653010651, 3.861377020970579999 ) ) ;
#14020 = CARTESIAN_POINT ( 'NONE',  ( -5.000000000000000000, -165.6250000027312126, -6.123233995736766282E-16 ) ) ;
#14021 = CARTESIAN_POINT ( 'NONE',  ( 4.458734125000001214, -92.14583333196775072, 2.574251347313718519 ) ) ;
#14022 = CARTESIAN_POINT ( 'NONE',  ( -4.999999999999999112, -53.79166666393548013, 2.886751345948131764 ) ) ;
#14023 = CARTESIAN_POINT ( 'NONE',  ( 3.061616997868383141E-16, -148.7500000000000284, -5.000000000000000000 ) ) ;
#14024 = CARTESIAN_POINT ( 'NONE',  ( -51.60603307380591787, -130.9375000013656063, -2.891590998281053704 ) ) ;
#14025 = CARTESIAN_POINT ( 'NONE',  ( -57.89159099828107458, -145.6875000013656063, -3.393966926194107447 ) ) ;
#14026 = CARTESIAN_POINT ( 'NONE',  ( -4.458734124999999437, -15.39583333196773651, -2.574251347313719407 ) ) ;
#14027 = CARTESIAN_POINT ( 'NONE',  ( -4.458734124999998549, 11.52083333469892779, 2.574251347313722516 ) ) ;
#14028 = CARTESIAN_POINT ( 'NONE',  ( -4.458734124999997661, -60.47916666530106511, 2.574251347313722516 ) ) ;
#14029 = CYLINDRICAL_SURFACE ( 'NONE', #51075, 5.000000000000000000 ) ;
#14030 = CARTESIAN_POINT ( 'NONE',  ( -2.229367062500000163, -15.47916666530107399, -3.861377020970580443 ) ) ;
#14031 = CARTESIAN_POINT ( 'NONE',  ( 2.500000000000002220, -8.541666663935483683, 4.330127018922192761 ) ) ;
#14032 = VERTEX_POINT ( 'NONE', #1604 ) ;
#14033 = CARTESIAN_POINT ( 'NONE',  ( -4.458734124999997661, -43.47916666530106511, 2.574251347313722516 ) ) ;
#14034 = CARTESIAN_POINT ( 'NONE',  ( 2.499999999999998668, -77.33333333333334281, -4.330127018922193649 ) ) ;
#14035 = CARTESIAN_POINT ( 'NONE',  ( -1.339745962155610925, -91.66965819600733312, 5.000000000000000000 ) ) ;
#14036 = CYLINDRICAL_SURFACE ( 'NONE', #18322, 5.000000000000000000 ) ;
#14037 = CARTESIAN_POINT ( 'NONE',  ( 2.229367062500001939, -83.97916666530106511, 3.861377020970579999 ) ) ;
#14038 = CARTESIAN_POINT ( 'NONE',  ( 2.229367062499998831, 17.10416666803225993, -3.861377020970580887 ) ) ;
#14039 = AXIS2_PLACEMENT_3D ( 'NONE', #41990, #51344, #17865 ) ;
#14040 = VECTOR ( 'NONE', #61993, 1000.000000000000000 ) ;
#14041 =( BOUNDED_CURVE ( )  B_SPLINE_CURVE ( 2, ( #62448, #47945, #43431, #58234, #13851, #62759, #4215, #9030, #18370 ),
 .UNSPECIFIED., .F., .F. ) 
 B_SPLINE_CURVE_WITH_KNOTS ( ( 3, 2, 2, 2, 3 ),
 ( 0.9020833333333333481, 0.9027777777777777901, 0.9041666666666666741, 0.9055555555555555580, 0.9062500000000000000 ),
 .UNSPECIFIED. ) 
 CURVE ( )  GEOMETRIC_REPRESENTATION_ITEM ( )  RATIONAL_B_SPLINE_CURVE ( ( 0.9330127018922194093, 0.9330127018922194093, 1.000000000000000000, 0.8660254037844387076, 1.000000000000000000, 0.8660254037844387076, 1.000000000000000000, 0.9330127018922194093, 0.9330127018922194093 ) ) 
 REPRESENTATION_ITEM ( '' )  );
#14042 = CARTESIAN_POINT ( 'NONE',  ( 9.457646018065525792E-16, 11.93750000136559386, 5.148502694627439702 ) ) ;
#14043 = CARTESIAN_POINT ( 'NONE',  ( 0.000000000000000000, -120.0000000000000000, 0.000000000000000000 ) ) ;
#14044 = AXIS2_PLACEMENT_3D ( 'NONE', #50519, #15781, #6459 ) ;
#14045 = CARTESIAN_POINT ( 'NONE',  ( 3.061616997868383141E-16, -144.7500000000000284, -5.000000000000000000 ) ) ;
#14046 = CARTESIAN_POINT ( 'NONE',  ( -51.75738570946856498, -142.8750000027312126, 3.805975901505576964 ) ) ;
#14047 = CARTESIAN_POINT ( 'NONE',  ( -5.000000000000000000, -70.08333333333332860, -2.886751345948128211 ) ) ;
#14048 = CARTESIAN_POINT ( 'NONE',  ( 5.000000000000000000, 15.70833333606451809, -2.886751345948129988 ) ) ;
#14049 = VERTEX_POINT ( 'NONE', #58840 ) ;
#14050 = CARTESIAN_POINT ( 'NONE',  ( 1.339745962155612702, -102.2946581987385173, -5.000000000000000000 ) ) ;
#14051 = VERTEX_POINT ( 'NONE', #26031 ) ;
#14052 = CARTESIAN_POINT ( 'NONE',  ( 2.071067811865443975, -166.8125000000000000, -5.000000000000031974 ) ) ;
#14054 = CARTESIAN_POINT ( 'NONE',  ( 5.000000000000000000, -28.49999999999999645, -6.123233995736766282E-16 ) ) ;
#14053 = DIRECTION ( 'NONE',  ( -0.000000000000000000, 1.000000000000000000, -0.000000000000000000 ) ) ;
#14055 = CARTESIAN_POINT ( 'NONE',  ( -3.152548672688508926E-16, -30.56249999863440436, -5.148502694627439702 ) ) ;
#14056 = CARTESIAN_POINT ( 'NONE',  ( 5.000000000000000888, -36.45833333060214443, 2.886751345948126879 ) ) ;
#14058 = ORIENTED_EDGE ( 'NONE', *, *, #26298, .T. ) ;
#14057 = CARTESIAN_POINT ( 'NONE',  ( 2.229367062499998831, -68.64583333196773651, -3.861377020970580887 ) ) ;
#14059 = CARTESIAN_POINT ( 'NONE',  ( -50.55543936806279248, -149.3125000013656063, 0.3552334253322060320 ) ) ;
#14061 = ORIENTED_EDGE ( 'NONE', *, *, #60875, .F. ) ;
#14060 = CARTESIAN_POINT ( 'NONE',  ( -4.458734124999999437, -15.64583333196773474, -2.574251347313719407 ) ) ;
#14062 = CARTESIAN_POINT ( 'NONE',  ( 5.000000000000000000, -76.50000000000000000, -6.123233995736766282E-16 ) ) ;
#14063 = CARTESIAN_POINT ( 'NONE',  ( -58.39396692619412477, -136.4375000013655779, 2.891590998281057701 ) ) ;
#14064 = CARTESIAN_POINT ( 'NONE',  ( 2.229367062499998831, -58.89583333196773651, -3.861377020970580887 ) ) ;
#14065 = CARTESIAN_POINT ( 'NONE',  ( 1.060575238724906964E-15, -82.62499999726880162, 5.773502691896257311 ) ) ;
#14066 = ORIENTED_EDGE ( 'NONE', *, *, #50786, .F. ) ;
#14067 = CARTESIAN_POINT ( 'NONE',  ( -54.60164318462004474, -147.3750000000000284, -4.984105922594373794 ) ) ;
#14068 = EDGE_CURVE ( 'NONE', #50477, #8862, #19354, .T. ) ;
#14069 = CARTESIAN_POINT ( 'NONE',  ( -4.458734124999999437, -23.64583333196773651, -2.574251347313719407 ) ) ;
#14071 = VERTEX_POINT ( 'NONE', #10584 ) ;
#14070 = CARTESIAN_POINT ( 'NONE',  ( 2.229367062499998831, -59.89583333196774362, -3.861377020970580887 ) ) ;
#14072 = CARTESIAN_POINT ( 'NONE',  ( -8.190561711645485556E-16, -164.9375000013655779, 4.458734124999999437 ) ) ;
#14073 = CARTESIAN_POINT ( 'NONE',  ( -4.458734124999999437, -104.6458333319677365, -2.574251347313719407 ) ) ;
#14074 = ORIENTED_EDGE ( 'NONE', *, *, #18539, .F. ) ;
#14075 = CARTESIAN_POINT ( 'NONE',  ( -58.39396692619412477, -149.6875000013656063, 2.891590998281057701 ) ) ;
#14076 = CARTESIAN_POINT ( 'NONE',  ( -55.39835681537999790, -139.0000000027312126, 4.984105922594378235 ) ) ;
#14077 = CARTESIAN_POINT ( 'NONE',  ( -2.229367062500000163, -40.47916666530107221, -3.861377020970580443 ) ) ;
#14078 = CARTESIAN_POINT ( 'NONE',  ( 5.000000000000000888, 18.41666666666666430, 2.886751345948126879 ) ) ;
#14079 = VECTOR ( 'NONE', #4293, 1000.000000000000000 ) ;
#14080 = CARTESIAN_POINT ( 'NONE',  ( -4.458734124999998549, -12.22916666530106866, 2.574251347313722516 ) ) ;
#14081 = VECTOR ( 'NONE', #593, 1000.000000000000000 ) ;
#14082 = CARTESIAN_POINT ( 'NONE',  ( 9.457646018065525792E-16, -101.3124999986344079, 5.148502694627439702 ) ) ;
#14083 = EDGE_CURVE ( 'NONE', #45777, #14700, #46047, .T. ) ;
#14084 = CARTESIAN_POINT ( 'NONE',  ( 4.458734124999999437, -142.6875000013656063, 0.000000000000000000 ) ) ;
#14085 = CARTESIAN_POINT ( 'NONE',  ( -2.229367062499996610, -27.39583333196774007, 3.861377020970582219 ) ) ;
#14086 = AXIS2_PLACEMENT_3D ( 'NONE', #29437, #44243, #5017 ) ;
#14087 = EDGE_CURVE ( 'NONE', #6727, #20337, #5769, .T. ) ;
#14088 = FACE_OUTER_BOUND ( 'NONE', #40344, .T. ) ;
#14089 = CARTESIAN_POINT ( 'NONE',  ( -59.29741812935640155, -134.6250000013656347, -2.196230717870135685 ) ) ;
#14090 =( BOUNDED_CURVE ( )  B_SPLINE_CURVE ( 2, ( #40905, #30941, #60861, #50886, #49363, #24925, #55719, #46057, #19775 ),
 .UNSPECIFIED., .F., .F. ) 
 B_SPLINE_CURVE_WITH_KNOTS ( ( 3, 2, 2, 2, 3 ),
 ( 0.2767857142857143016, 0.2773809523809523947, 0.2785714285714285809, 0.2797619047619047672, 0.2803571428571428603 ),
 .UNSPECIFIED. ) 
 CURVE ( )  GEOMETRIC_REPRESENTATION_ITEM ( )  RATIONAL_B_SPLINE_CURVE ( ( 0.9330127018922194093, 0.9330127018922194093, 1.000000000000000000, 0.8660254037844387076, 1.000000000000000000, 0.8660254037844387076, 1.000000000000000000, 0.9330127018922194093, 0.9330127018922194093 ) ) 
 REPRESENTATION_ITEM ( '' )  );
#14091 = CARTESIAN_POINT ( 'NONE',  ( 9.457646018065525792E-16, -71.31249999863439371, 5.148502694627439702 ) ) ;
#14092 = CARTESIAN_POINT ( 'NONE',  ( 1.846868145590736310, -140.6250000013656063, 4.458734124999997661 ) ) ;
#14093 = CARTESIAN_POINT ( 'NONE',  ( -4.458734124999999437, 7.437500001365594748, 0.000000000000000000 ) ) ;
#14094 = VERTEX_POINT ( 'NONE', #11855 ) ;
#14095 = CARTESIAN_POINT ( 'NONE',  ( 1.975475456537005874E-15, -63.62499999726880873, 5.000000000000000000 ) ) ;
#14096 = LINE ( 'NONE', #4450, #22649 ) ;
#14098 = CARTESIAN_POINT ( 'NONE',  ( -4.458734124999998549, -32.22916666530106511, 2.574251347313722516 ) ) ;
#14097 = CARTESIAN_POINT ( 'NONE',  ( 2.500000000000002220, -97.66666666666665719, 4.330127018922192761 ) ) ;
#14099 = CARTESIAN_POINT ( 'NONE',  ( -6.972266317189433020E-16, -73.25000000000000000, -5.000000000000000000 ) ) ;
#14100 = CARTESIAN_POINT ( 'NONE',  ( -4.458734124999999437, -77.56249999863440792, 0.000000000000000000 ) ) ;
#14101 = CARTESIAN_POINT ( 'NONE',  ( 2.229367062500001939, 21.77083333469892779, 3.861377020970579999 ) ) ;
#14102 = CARTESIAN_POINT ( 'NONE',  ( 5.000000000000000000, -18.41666666666666430, -2.886751345948130876 ) ) ;
#14103 = EDGE_CURVE ( 'NONE', #35597, #52286, #36316, .T. ) ;
#14104 = CARTESIAN_POINT ( 'NONE',  ( -50.70258187064364108, -141.1250000013655779, 2.196230717870141014 ) ) ;
#14105 = CARTESIAN_POINT ( 'NONE',  ( -4.458734124999999437, 1.687500001365593194, 0.000000000000000000 ) ) ;
#14106 = CARTESIAN_POINT ( 'NONE',  ( 6.123233995736766282E-16, -120.0000000000000000, -5.000000000000000000 ) ) ;
#14107 = CARTESIAN_POINT ( 'NONE',  ( 2.229367062499998831, -44.89583333196774362, -3.861377020970580887 ) ) ;
#14108 = CARTESIAN_POINT ( 'NONE',  ( -50.01589407740564042, -144.6250000000000284, 0.3983568153799778022 ) ) ;
#14109 = CARTESIAN_POINT ( 'NONE',  ( 4.458734124999998549, -0.7291666653010709931, -2.574251347313721627 ) ) ;
#14110 = CARTESIAN_POINT ( 'NONE',  ( -2.229367062499996610, -26.39583333196774007, 3.861377020970582219 ) ) ;
#14111 = CARTESIAN_POINT ( 'NONE',  ( -1.846868145590737420, -154.7500000013656063, 4.458734124999999437 ) ) ;
#14112 = CARTESIAN_POINT ( 'NONE',  ( -4.458734124999998549, -71.22916666530106511, 2.574251347313722516 ) ) ;
#14113 = CARTESIAN_POINT ( 'NONE',  ( 5.000000000000000000, -107.2916666639354588, -2.886751345948129988 ) ) ;
#14114 = CARTESIAN_POINT ( 'NONE',  ( -58.80597590150559739, -149.0000000000000284, 3.242614290531460330 ) ) ;
#14115 = LINE ( 'NONE', #39824, #7177 ) ;
#14116 = EDGE_CURVE ( 'NONE', #17975, #35597, #21441, .T. ) ;
#14117 = CARTESIAN_POINT ( 'NONE',  ( -2.229367062499996610, -105.3958333319677365, 3.861377020970582219 ) ) ;
#14118 = CARTESIAN_POINT ( 'NONE',  ( 4.458734125000000326, -73.14583333196772230, 2.574251347313718519 ) ) ;
#14119 = CARTESIAN_POINT ( 'NONE',  ( 5.000000000000000000, -51.50000000000000711, -6.123233995736766282E-16 ) ) ;
#14120 = CARTESIAN_POINT ( 'NONE',  ( -1.339745962155613812, -66.20534180126148271, -5.000000000000000000 ) ) ;
#14121 = CARTESIAN_POINT ( 'NONE',  ( -1.339745962155564296, -11.08034179853029677, -5.000000000000028422 ) ) ;
#14122 = ORIENTED_EDGE ( 'NONE', *, *, #25938, .T. ) ;
#14123 = CARTESIAN_POINT ( 'NONE',  ( 5.000000000000000000, 6.499999999999999112, -6.123233995736766282E-16 ) ) ;
#14124 = CARTESIAN_POINT ( 'NONE',  ( 2.500000000000002220, -27.54166666393548013, 4.330127018922192761 ) ) ;
#14125 = CARTESIAN_POINT ( 'NONE',  ( 2.499999999999998668, -14.33333333333333037, -4.330127018922193649 ) ) ;
#14126 = CARTESIAN_POINT ( 'NONE',  ( -2.229367062499996610, -17.14583333196773651, 3.861377020970582219 ) ) ;
#14127 = CARTESIAN_POINT ( 'NONE',  ( 4.458734124999999437, -77.81249999863440792, -5.460374474430324690E-16 ) ) ;
#14128 = CARTESIAN_POINT ( 'NONE',  ( -3.152801135295367985, -169.0625000013656063, 3.152801135295367096 ) ) ;
#14129 = CARTESIAN_POINT ( 'NONE',  ( -4.999999999999999112, -20.79166666393548013, 2.886751345948131764 ) ) ;
#14131 = ORIENTED_EDGE ( 'NONE', *, *, #31176, .T. ) ;
#14130 = CARTESIAN_POINT ( 'NONE',  ( -4.458734124999998549, -45.22916666530106511, 2.574251347313722516 ) ) ;
#14132 = CARTESIAN_POINT ( 'NONE',  ( 1.339745962155612702, -98.29465819873850307, -5.000000000000000000 ) ) ;
#14134 = VERTEX_POINT ( 'NONE', #36628 ) ;
#14133 = CARTESIAN_POINT ( 'NONE',  ( -4.458734124999998549, 0.5208333346989265644, 2.574251347313722516 ) ) ;
#14135 = CARTESIAN_POINT ( 'NONE',  ( -50.55543936806279248, -153.0625000013656063, 0.3552334253322060320 ) ) ;
#14136 = CARTESIAN_POINT ( 'NONE',  ( -4.999999999999999112, -59.91666666666665719, 2.886751345948131764 ) ) ;
#14137 = CARTESIAN_POINT ( 'NONE',  ( -8.190561711645485556E-16, -157.9375000013655779, 4.458734124999999437 ) ) ;
#14138 = CARTESIAN_POINT ( 'NONE',  ( -3.152548672688508926E-16, -42.81249999863440081, -5.148502694627439702 ) ) ;
#14139 = DIRECTION ( 'NONE',  ( -0.000000000000000000, 1.000000000000000000, -0.000000000000000000 ) ) ;
#14140 =( BOUNDED_CURVE ( )  B_SPLINE_CURVE ( 2, ( #26859, #2417, #33566, #42894, #58327, #29036, #39015, #42584, #38387 ),
 .UNSPECIFIED., .F., .F. ) 
 B_SPLINE_CURVE_WITH_KNOTS ( ( 3, 2, 2, 2, 3 ),
 ( 0.6270833333333333259, 0.6277777777777777679, 0.6291666666666666519, 0.6305555555555555358, 0.6312499999999999778 ),
 .UNSPECIFIED. ) 
 CURVE ( )  GEOMETRIC_REPRESENTATION_ITEM ( )  RATIONAL_B_SPLINE_CURVE ( ( 0.9330127018922194093, 0.9330127018922194093, 1.000000000000000000, 0.8660254037844387076, 1.000000000000000000, 0.8660254037844387076, 1.000000000000000000, 0.9330127018922194093, 0.9330127018922194093 ) ) 
 REPRESENTATION_ITEM ( '' )  );
#14141 = CARTESIAN_POINT ( 'NONE',  ( 5.000000000000000888, -160.9375000000000284, -2.071067811865475505 ) ) ;
#14142 = CYLINDRICAL_SURFACE ( 'NONE', #24111, 5.000000000000000000 ) ;
#14143 = CARTESIAN_POINT ( 'NONE',  ( -54.64476657466781973, -127.0625000013655921, -4.444560631937228834 ) ) ;
#14144 = EDGE_CURVE ( 'NONE', #8313, #16398, #11150, .T. ) ;
#14145 = CARTESIAN_POINT ( 'NONE',  ( 2.229367062499998831, -6.895833331967741842, -3.861377020970580887 ) ) ;
#14146 = CARTESIAN_POINT ( 'NONE',  ( 2.229367062500001939, -43.22916666530107932, 3.861377020970579999 ) ) ;
#14147 = EDGE_CURVE ( 'NONE', #29588, #21097, #57445, .T. ) ;
#14148 = ADVANCED_FACE ( 'NONE', ( #7051 ), #50793, .T. ) ;
#14149 = CARTESIAN_POINT ( 'NONE',  ( 2.500000000000002220, -83.54166666393547303, 4.330127018922192761 ) ) ;
#14150 = CARTESIAN_POINT ( 'NONE',  ( 3.152801135295366208, -147.5625000013655779, 3.152801135295367985 ) ) ;
#14151 = CARTESIAN_POINT ( 'NONE',  ( -4.458734124999998549, -91.47916666530106511, 2.574251347313722516 ) ) ;
#14152 = CARTESIAN_POINT ( 'NONE',  ( -59.81910112700026616, -143.1875000000000000, -2.462841084822451343 ) ) ;
#14153 = ORIENTED_EDGE ( 'NONE', *, *, #56327, .T. ) ;
#14154 = CARTESIAN_POINT ( 'NONE',  ( -59.98410592259440222, -152.1250000000000284, -0.3983568153799752487 ) ) ;
#14155 = CARTESIAN_POINT ( 'NONE',  ( -57.46284108482265651, -150.0625000027312126, 4.819101127000239515 ) ) ;
#14156 = CARTESIAN_POINT ( 'NONE',  ( 1.975475456537005874E-15, -43.75000000000000000, 5.000000000000000000 ) ) ;
#14157 = ORIENTED_EDGE ( 'NONE', *, *, #37324, .F. ) ;
#14158 = CARTESIAN_POINT ( 'NONE',  ( -1.339745962155613812, -14.20534180126148094, -5.000000000000000000 ) ) ;
#14159 = CARTESIAN_POINT ( 'NONE',  ( -4.458734124999999437, -9.645833331967738289, -2.574251347313719407 ) ) ;
#14160 = EDGE_CURVE ( 'NONE', #23800, #27142, #41524, .T. ) ;
#14161 = CARTESIAN_POINT ( 'NONE',  ( 2.499999999999998668, -105.2083333306021444, -4.330127018922193649 ) ) ;
#14162 = CARTESIAN_POINT ( 'NONE',  ( 4.458734124999998549, -3.729166665301070438, -2.574251347313721627 ) ) ;
#14163 = CARTESIAN_POINT ( 'NONE',  ( -4.999999999999998224, -42.91666666666665719, 2.886751345948131764 ) ) ;
#14164 = CARTESIAN_POINT ( 'NONE',  ( -3.152801135295367985, -152.8125000013656063, 3.152801135295367096 ) ) ;
#14165 = VECTOR ( 'NONE', #44853, 1000.000000000000114 ) ;
#14166 = CARTESIAN_POINT ( 'NONE',  ( -2.229367062499996610, 18.60416666803225993, 3.861377020970582219 ) ) ;
#14167 = VERTEX_POINT ( 'NONE', #16381 ) ;
#14168 = CARTESIAN_POINT ( 'NONE',  ( 2.229367062500001939, -93.97916666530106511, 3.861377020970579999 ) ) ;
#14169 = CARTESIAN_POINT ( 'NONE',  ( -1.339745962155613812, -75.20534180126148271, -5.000000000000000000 ) ) ;
#14170 = CARTESIAN_POINT ( 'NONE',  ( -6.972266317189433020E-16, 1.875000002731185722, -5.000000000000000000 ) ) ;
#14171 = CARTESIAN_POINT ( 'NONE',  ( 4.458734124999998549, -15.72916666530107399, -2.574251347313721627 ) ) ;
#14172 = CARTESIAN_POINT ( 'NONE',  ( -5.000000000000000000, -84.95833333060213022, -2.886751345948128211 ) ) ;
#14173 = CARTESIAN_POINT ( 'NONE',  ( 0.000000000000000000, -120.0000000000000000, 0.000000000000000000 ) ) ;
#14174 = CARTESIAN_POINT ( 'NONE',  ( -59.44456063193725015, -153.5625000013656063, -0.3552334253322034230 ) ) ;
#14175 = CARTESIAN_POINT ( 'NONE',  ( -3.535250795749689387E-16, -40.12499999726880162, -5.773502691896257311 ) ) ;
#14176 = CARTESIAN_POINT ( 'NONE',  ( 1.339745962155612702, -49.16965819600731891, -5.000000000000000000 ) ) ;
#14177 = CARTESIAN_POINT ( 'NONE',  ( 4.458734124999999437, 20.18750000136559208, -5.460374474430324690E-16 ) ) ;
#14178 = CARTESIAN_POINT ( 'NONE',  ( -1.339745962155625802, 12.33034180399266511, 4.999999999999991118 ) ) ;
#14179 = VERTEX_POINT ( 'NONE', #62588 ) ;
#14180 = CARTESIAN_POINT ( 'NONE',  ( -2.229367062500000163, 16.52083333469892779, -3.861377020970580443 ) ) ;
#14181 = CARTESIAN_POINT ( 'NONE',  ( 4.458734125000001214, -60.89583333196774362, 2.574251347313718519 ) ) ;
#14182 = CARTESIAN_POINT ( 'NONE',  ( -4.458734124999997661, -7.479166665301073991, 2.574251347313722516 ) ) ;
#14183 = CARTESIAN_POINT ( 'NONE',  ( 0.000000000000000000, -120.0000000000000000, 5.000000000000000000 ) ) ;
#14184 = CARTESIAN_POINT ( 'NONE',  ( 5.000000000000000888, 11.41666666666666607, 2.886751345948126879 ) ) ;
#14185 = CARTESIAN_POINT ( 'NONE',  ( -1.846868145590734756, -166.1250000013655779, -4.458734125000000326 ) ) ;
#14186 = CARTESIAN_POINT ( 'NONE',  ( -2.499999999999996447, -59.70833333060214443, 4.330127018922195425 ) ) ;
#14187 = CARTESIAN_POINT ( 'NONE',  ( -2.229367062499996610, -54.14583333196773651, 3.861377020970582219 ) ) ;
#14188 = CARTESIAN_POINT ( 'NONE',  ( 5.000000000000000000, -82.29166666393548724, -2.886751345948129988 ) ) ;
#14189 = VECTOR ( 'NONE', #3052, 1000.000000000000000 ) ;
#14190 = CARTESIAN_POINT ( 'NONE',  ( -51.60603307380591787, -136.1875000013656063, -2.891590998281053704 ) ) ;
#14191 = CARTESIAN_POINT ( 'NONE',  ( -55.00000000000002132, -155.0000000000000284, 1.734723475976807094E-15 ) ) ;
#14192 = CARTESIAN_POINT ( 'NONE',  ( -50.18089887299977647, -145.6875000000000284, 2.462841084822486426 ) ) ;
#14193 = CARTESIAN_POINT ( 'NONE',  ( -2.229367062500000163, -89.72916666530106511, -3.861377020970580443 ) ) ;
#14194 = CARTESIAN_POINT ( 'NONE',  ( -3.152801135295367096, -153.3125000013656063, -3.152801135295367541 ) ) ;
#14195 = CARTESIAN_POINT ( 'NONE',  ( 5.000000000000000000, -36.41666666666666430, -2.886751345948129988 ) ) ;
#14196 = CARTESIAN_POINT ( 'NONE',  ( -6.972266317189433020E-16, -98.12499999726880162, -5.000000000000000000 ) ) ;
#14197 = DIRECTION ( 'NONE',  ( 0.000000000000000000, 0.000000000000000000, 1.000000000000000000 ) ) ;
#14198 = VERTEX_POINT ( 'NONE', #56260 ) ;
#14199 = CARTESIAN_POINT ( 'NONE',  ( -4.458734124999999437, -102.3958333319677365, -2.574251347313719407 ) ) ;
#14200 = CARTESIAN_POINT ( 'NONE',  ( 9.457646018065525792E-16, 8.687500001365595637, 5.148502694627439702 ) ) ;
#14201 = CARTESIAN_POINT ( 'NONE',  ( 2.499999999999998668, 12.79166666939785379, -4.330127018922193649 ) ) ;
#14202 = CARTESIAN_POINT ( 'NONE',  ( 5.000000000000000888, -161.9374999999999716, -2.071067811865475505 ) ) ;
#14203 = CARTESIAN_POINT ( 'NONE',  ( 1.060575238724906964E-15, 3.249999999999999556, 5.773502691896257311 ) ) ;
#14204 = CARTESIAN_POINT ( 'NONE',  ( 9.457646018065525792E-16, -62.06249999863440792, 5.148502694627439702 ) ) ;
#14205 = CARTESIAN_POINT ( 'NONE',  ( 1.975475456537005874E-15, -30.62499999726881583, 5.000000000000000000 ) ) ;
#14206 = CARTESIAN_POINT ( 'NONE',  ( -4.999999999999999112, -4.791666663935479242, 2.886751345948131764 ) ) ;
#14207 = CARTESIAN_POINT ( 'NONE',  ( 2.229367062500001939, -26.97916666530106866, 3.861377020970579999 ) ) ;
#14208 = CARTESIAN_POINT ( 'NONE',  ( 2.788906526875773208E-15, 28.75000000000000000, -5.000000000000000000 ) ) ;
#14209 = DIRECTION ( 'NONE',  ( -0.000000000000000000, -0.000000000000000000, 1.000000000000000000 ) ) ;
#14210 = CARTESIAN_POINT ( 'NONE',  ( 5.000000000000000000, -20.41666666666666785, -2.886751345948130876 ) ) ;
#14211 = CARTESIAN_POINT ( 'NONE',  ( 5.000000000000000000, -44.50000000000000000, -6.123233995736766282E-16 ) ) ;
#14213 = CARTESIAN_POINT ( 'NONE',  ( 4.458734124999998549, -25.97916666530106866, -2.574251347313721627 ) ) ;
#14212 = CARTESIAN_POINT ( 'NONE',  ( 1.975475456537005874E-15, -89.62499999726880162, 5.000000000000000000 ) ) ;
#14214 = AXIS2_PLACEMENT_3D ( 'NONE', #41222, #21940, #26445 ) ;
#14215 = CARTESIAN_POINT ( 'NONE',  ( 6.123233995736766282E-16, -120.0000000000000000, -5.000000000000000000 ) ) ;
#14216 = CARTESIAN_POINT ( 'NONE',  ( 9.457646018065525792E-16, -69.06249999863439371, 5.148502694627439702 ) ) ;
#14217 = CARTESIAN_POINT ( 'NONE',  ( 4.458734124999999437, -143.6875000013656063, 0.000000000000000000 ) ) ;
#14218 = CARTESIAN_POINT ( 'NONE',  ( 2.229367062500001939, -76.97916666530106511, 3.861377020970579999 ) ) ;
#14219 = CARTESIAN_POINT ( 'NONE',  ( -56.48576386720575471, -141.0000000013656063, -4.591703134518078322 ) ) ;
#14220 =( BOUNDED_CURVE ( )  B_SPLINE_CURVE ( 2, ( #28474, #52303, #47462, #32671, #18810, #58059, #18513, #2782, #33302 ),
 .UNSPECIFIED., .F., .F. ) 
 B_SPLINE_CURVE_WITH_KNOTS ( ( 3, 2, 2, 2, 3 ),
 ( 0.4839285714285714302, 0.4845238095238095233, 0.4857142857142857095, 0.4869047619047618958, 0.4874999999999999889 ),
 .UNSPECIFIED. ) 
 CURVE ( )  GEOMETRIC_REPRESENTATION_ITEM ( )  RATIONAL_B_SPLINE_CURVE ( ( 0.9330127018922194093, 0.9330127018922194093, 1.000000000000000000, 0.8660254037844387076, 1.000000000000000000, 0.8660254037844387076, 1.000000000000000000, 0.9330127018922194093, 0.9330127018922194093 ) ) 
 REPRESENTATION_ITEM ( '' )  );
#14221 = CARTESIAN_POINT ( 'NONE',  ( -2.229367062499996610, -24.39583333196773651, 3.861377020970582219 ) ) ;
#14222 = CARTESIAN_POINT ( 'NONE',  ( -2.500000000000000444, -67.04166666393547303, -4.330127018922193649 ) ) ;
#14224 = ORIENTED_EDGE ( 'NONE', *, *, #52664, .T. ) ;
#14223 = EDGE_CURVE ( 'NONE', #42943, #50850, #19731, .T. ) ;
#14225 = CARTESIAN_POINT ( 'NONE',  ( 2.500000000000002220, -93.54166666393547303, 4.330127018922192761 ) ) ;
#14226 = VERTEX_POINT ( 'NONE', #51432 ) ;
#14227 = CARTESIAN_POINT ( 'NONE',  ( 4.458734125000001214, -71.14583333196773651, 2.574251347313718519 ) ) ;
#14228 = CARTESIAN_POINT ( 'NONE',  ( 5.000000000000000000, 28.49999999999999645, -6.123233995736766282E-16 ) ) ;
#14229 = VERTEX_POINT ( 'NONE', #28154 ) ;
#14230 = CARTESIAN_POINT ( 'NONE',  ( -6.972266317189433020E-16, -79.24999999999998579, -5.000000000000000000 ) ) ;
#14231 = EDGE_CURVE ( 'NONE', #25897, #27694, #31163, .T. ) ;
#14232 = CARTESIAN_POINT ( 'NONE',  ( -5.000000000000000000, -77.87499999726881583, 0.000000000000000000 ) ) ;
#14233 = CARTESIAN_POINT ( 'NONE',  ( -2.229367062500000163, -56.72916666530107221, -3.861377020970580443 ) ) ;
#14234 = ADVANCED_FACE ( 'NONE', ( #8853 ), #28470, .F. ) ;
#14235 = CARTESIAN_POINT ( 'NONE',  ( 4.458734125000001214, -1.145833331967740509, 2.574251347313718519 ) ) ;
#14236 = ORIENTED_EDGE ( 'NONE', *, *, #34954, .F. ) ;
#14237 = EDGE_CURVE ( 'NONE', #3805, #4656, #40808, .T. ) ;
#14238 =( BOUNDED_CURVE ( )  B_SPLINE_CURVE ( 2, ( #21079, #49701, #14967, #54853, #44230, #59357, #55504, #840, #24624 ),
 .UNSPECIFIED., .F., .F. ) 
 B_SPLINE_CURVE_WITH_KNOTS ( ( 3, 2, 2, 2, 3 ),
 ( 0.008333333333333340157, 0.01250000000000001110, 0.01666666666666668031, 0.02083333333333334952, 0.02500000000000002220 ),
 .UNSPECIFIED. ) 
 CURVE ( )  GEOMETRIC_REPRESENTATION_ITEM ( )  RATIONAL_B_SPLINE_CURVE ( ( 0.9999999999999998890, 0.9238795325112868495, 1.000000000000000000, 0.9238795325112867385, 1.000000000000000000, 0.9238795325112867385, 1.000000000000000000, 0.9238795325112864054, 1.000000000000000444 ) ) 
 REPRESENTATION_ITEM ( '' )  );
#14239 = CARTESIAN_POINT ( 'NONE',  ( -58.24261429053147765, -145.3750000027312126, -3.805975901505573855 ) ) ;
#14240 = EDGE_CURVE ( 'NONE', #39148, #39239, #6731, .T. ) ;
#14241 = CARTESIAN_POINT ( 'NONE',  ( -2.229367062500000163, 13.52083333469892779, -3.861377020970580443 ) ) ;
#14242 = CARTESIAN_POINT ( 'NONE',  ( -52.10840900171896806, -144.1875000013656063, 3.393966926194110556 ) ) ;
#14243 = LINE ( 'NONE', #18752, #31587 ) ;
#14244 = CARTESIAN_POINT ( 'NONE',  ( 4.458734124999999437, -165.3750000013656347, -1.846868145590734978 ) ) ;
#14246 = EDGE_CURVE ( 'NONE', #14537, #12052, #28005, .T. ) ;
#14245 = VERTEX_POINT ( 'NONE', #43562 ) ;
#14247 = CARTESIAN_POINT ( 'NONE',  ( -4.458734124999999437, -74.39583333196775072, -2.574251347313719407 ) ) ;
#14248 = DIRECTION ( 'NONE',  ( -0.000000000000000000, 1.000000000000000000, -0.000000000000000000 ) ) ;
#14249 = CARTESIAN_POINT ( 'NONE',  ( 4.458734125000001214, 2.104166668032262599, 2.574251347313718519 ) ) ;
#14250 = EDGE_CURVE ( 'NONE', #14315, #100, #13171, .T. ) ;
#14251 = CARTESIAN_POINT ( 'NONE',  ( 4.458734125000001214, -68.14583333196773651, 2.574251347313718519 ) ) ;
#14252 = CARTESIAN_POINT ( 'NONE',  ( -4.999999999999999112, -25.79166666393547658, 2.886751345948131764 ) ) ;
#14253 = CARTESIAN_POINT ( 'NONE',  ( -51.19402409849444524, -142.6250000027312126, -3.242614290531456334 ) ) ;
#14254 = DIRECTION ( 'NONE',  ( 0.000000000000000000, 0.000000000000000000, 1.000000000000000000 ) ) ;
#14255 = CARTESIAN_POINT ( 'NONE',  ( -2.500000000000000444, -59.16666666666665719, -4.330127018922193649 ) ) ;
#14256 = CARTESIAN_POINT ( 'NONE',  ( -2.500000000000000444, -106.0416666639354730, -4.330127018922193649 ) ) ;
#14257 =( NAMED_UNIT ( * ) PLANE_ANGLE_UNIT ( ) SI_UNIT ( $, .RADIAN. ) );
#14258 = CARTESIAN_POINT ( 'NONE',  ( 2.229367062499998831, -42.64583333196773651, -3.861377020970580887 ) ) ;
#14259 = CARTESIAN_POINT ( 'NONE',  ( -4.458734124999999437, -24.64583333196773651, -2.574251347313719407 ) ) ;
#14260 = CARTESIAN_POINT ( 'NONE',  ( -2.229367062499996610, 8.604166668032261711, 3.861377020970582219 ) ) ;
#14261 = AXIS2_PLACEMENT_3D ( 'NONE', #50937, #15887, #54809 ) ;
#14262 = B_SPLINE_CURVE_WITH_KNOTS ( 'NONE', 3,
 ( #26790, #1729, #17769, #46721, #6859, #6539 ),
 .UNSPECIFIED., .F., .F.,
 ( 4, 2, 4 ),
 ( 0.004615310220740742597, 0.006918661718823353700, 0.009222013216905964803 ),
 .UNSPECIFIED. ) ;
#14263 = CARTESIAN_POINT ( 'NONE',  ( -51.75738570946856498, -143.7500000000000284, 3.805975901505576964 ) ) ;
#14264 = CARTESIAN_POINT ( 'NONE',  ( 2.499999999999998668, 23.66666666666666430, -4.330127018922193649 ) ) ;
#14265 = CARTESIAN_POINT ( 'NONE',  ( 2.071067811865475505, -149.9375000027312126, -5.000000000000000888 ) ) ;
#14266 = CARTESIAN_POINT ( 'NONE',  ( -4.999999999999998224, 29.08333333333333215, 2.886751345948131764 ) ) ;
#14267 = AXIS2_PLACEMENT_3D ( 'NONE', #13379, #57146, #3422 ) ;
#14268 = CARTESIAN_POINT ( 'NONE',  ( 2.229367062499998831, -37.64583333196773651, -3.861377020970580887 ) ) ;
#14269 = CARTESIAN_POINT ( 'NONE',  ( 5.000000000000000000, -66.29166666393547303, -2.886751345948129988 ) ) ;
#14270 = CARTESIAN_POINT ( 'NONE',  ( -53.51423613279429503, -146.5000000013656347, 4.591703134518082763 ) ) ;
#14271 = CARTESIAN_POINT ( 'NONE',  ( -2.071067811865478170, -141.3125000000000000, 5.000000000000000000 ) ) ;
#14272 = CARTESIAN_POINT ( 'NONE',  ( -4.458734124999999437, -75.64583333196773651, -2.574251347313719407 ) ) ;
#14273 = CARTESIAN_POINT ( 'NONE',  ( 3.152801135295367541, -166.5625000013656063, -3.152801135295367541 ) ) ;
#14274 = CARTESIAN_POINT ( 'NONE',  ( -2.229367062500000163, -28.47916666530107221, -3.861377020970580443 ) ) ;
#14275 = CARTESIAN_POINT ( 'NONE',  ( -51.75738570946856498, -135.8750000027312410, 3.805975901505576964 ) ) ;
#14276 = FACE_OUTER_BOUND ( 'NONE', #22902, .T. ) ;
#14277 = CARTESIAN_POINT ( 'NONE',  ( 2.500000000000002220, -23.66666666666666785, 4.330127018922192761 ) ) ;
#14278 = CARTESIAN_POINT ( 'NONE',  ( -3.152801135295367985, -145.8125000013655779, 3.152801135295367096 ) ) ;
#14279 = ORIENTED_EDGE ( 'NONE', *, *, #27532, .F. ) ;
#14280 = CARTESIAN_POINT ( 'NONE',  ( 2.499999999999998668, -90.20833333060214443, -4.330127018922193649 ) ) ;
#14281 = CARTESIAN_POINT ( 'NONE',  ( -2.500000000000000444, -49.16666666666666430, -4.330127018922193649 ) ) ;
#14282 = CARTESIAN_POINT ( 'NONE',  ( -3.152548672688508926E-16, -57.81249999863440081, -5.148502694627439702 ) ) ;
#14283 = CARTESIAN_POINT ( 'NONE',  ( -3.535250795749689387E-16, 28.87500000273118417, -5.773502691896257311 ) ) ;
#14284 = CARTESIAN_POINT ( 'NONE',  ( -6.972266317189433020E-16, -90.12499999726880162, -5.000000000000000000 ) ) ;
#14285 = CARTESIAN_POINT ( 'NONE',  ( 5.000000000000000000, 17.50000000000000000, -6.123233995736766282E-16 ) ) ;
#14286 = CARTESIAN_POINT ( 'NONE',  ( -6.972266317189433020E-16, -37.12499999726881583, -5.000000000000000000 ) ) ;
#14287 = CARTESIAN_POINT ( 'NONE',  ( 9.457646018065525792E-16, -4.062499998634408804, 5.148502694627439702 ) ) ;
#14288 = FACE_OUTER_BOUND ( 'NONE', #12731, .T. ) ;
#14289 = CARTESIAN_POINT ( 'NONE',  ( -56.66612745406283125, -145.4375000027312126, -5.149110718188525837 ) ) ;
#14290 = CARTESIAN_POINT ( 'NONE',  ( 0.000000000000000000, -170.0000000000000000, 0.000000000000000000 ) ) ;
#14291 = CARTESIAN_POINT ( 'NONE',  ( 2.499999999999998668, -56.20833333060214443, -4.330127018922193649 ) ) ;
#14293 = CARTESIAN_POINT ( 'NONE',  ( -2.229367062499996610, -21.14583333196774007, 3.861377020970582219 ) ) ;
#14292 =( BOUNDED_CURVE ( )  B_SPLINE_CURVE ( 2, ( #28532, #58439, #54240, #48150, #33674, #58118, #4103, #23725, #43321 ),
 .UNSPECIFIED., .F., .F. ) 
 B_SPLINE_CURVE_WITH_KNOTS ( ( 3, 2, 2, 2, 3 ),
 ( 0.7803571428571428603, 0.7809523809523809534, 0.7821428571428571397, 0.7833333333333333259, 0.7839285714285714191 ),
 .UNSPECIFIED. ) 
 CURVE ( )  GEOMETRIC_REPRESENTATION_ITEM ( )  RATIONAL_B_SPLINE_CURVE ( ( 0.9330127018922194093, 0.9330127018922194093, 1.000000000000000000, 0.8660254037844387076, 1.000000000000000000, 0.8660254037844387076, 1.000000000000000000, 0.9330127018922194093, 0.9330127018922194093 ) ) 
 REPRESENTATION_ITEM ( '' )  );
#14294 = CARTESIAN_POINT ( 'NONE',  ( 2.499999999999998668, 0.6666666666666660745, -4.330127018922193649 ) ) ;
#14295 = CARTESIAN_POINT ( 'NONE',  ( 2.229367062500001939, -53.97916666530107221, 3.861377020970579999 ) ) ;
#14296 = CARTESIAN_POINT ( 'NONE',  ( 1.846868145590736310, -158.8750000013655779, 4.458734124999999437 ) ) ;
#14297 = CARTESIAN_POINT ( 'NONE',  ( 1.060575238724906964E-15, -48.62499999726881583, 5.773502691896257311 ) ) ;
#14298 = ORIENTED_EDGE ( 'NONE', *, *, #49083, .F. ) ;
#14299 = CARTESIAN_POINT ( 'NONE',  ( -4.458734124999999437, 5.354166668032262599, -2.574251347313719407 ) ) ;
#14300 = ORIENTED_EDGE ( 'NONE', *, *, #60309, .T. ) ;
#14302 = CARTESIAN_POINT ( 'NONE',  ( 1.975475456537005874E-15, -67.62499999726881583, 5.000000000000000000 ) ) ;
#14301 = FACE_OUTER_BOUND ( 'NONE', #527, .T. ) ;
#14303 = CARTESIAN_POINT ( 'NONE',  ( 4.458734124999999437, -162.5000000013655779, 1.846868145590737864 ) ) ;
#14304 = ORIENTED_EDGE ( 'NONE', *, *, #9380, .F. ) ;
#14305 = STYLED_ITEM ( 'NONE', ( #19692 ), #24770 ) ;
#14306 = FACE_OUTER_BOUND ( 'NONE', #48091, .T. ) ;
#14307 = CARTESIAN_POINT ( 'NONE',  ( -53.33387254593733928, -132.8125000000000568, 5.149110718188519620 ) ) ;
#14309 = AXIS2_PLACEMENT_3D ( 'NONE', #44171, #4943, #138 ) ;
#14308 = LINE ( 'NONE', #46926, #48016 ) ;
#14310 = CARTESIAN_POINT ( 'NONE',  ( 9.457646018065525792E-16, -42.31249999863440081, 5.148502694627439702 ) ) ;
#14311 = ORIENTED_EDGE ( 'NONE', *, *, #54183, .F. ) ;
#14312 = DIRECTION ( 'NONE',  ( -0.000000000000000000, 1.000000000000000000, -0.000000000000000000 ) ) ;
#14313 = CARTESIAN_POINT ( 'NONE',  ( 4.458734124999998549, 20.27083333469892779, -2.574251347313721627 ) ) ;
#14314 = CARTESIAN_POINT ( 'NONE',  ( 1.339745962155615144, -59.70534180126147561, 4.999999999999999112 ) ) ;
#14315 = VERTEX_POINT ( 'NONE', #4970 ) ;
#14316 = CARTESIAN_POINT ( 'NONE',  ( 4.458734124999999437, -88.06249999863439371, -5.460374474430324690E-16 ) ) ;
#14317 = CARTESIAN_POINT ( 'NONE',  ( -53.33387254593733928, -126.9375000027312126, 5.149110718188519620 ) ) ;
#14318 = CARTESIAN_POINT ( 'NONE',  ( 5.000000000000000000, -35.29166666393547303, -2.886751345948130876 ) ) ;
#14319 = CARTESIAN_POINT ( 'NONE',  ( -50.52035010823932737, -134.9999999999999147, -0.6337412764124265019 ) ) ;
#14320 = SHAPE_REPRESENTATION ( 'hex flange nut gradea_iso_ISO - 4161 - M10 - N', ( #43054 ), #24596 ) ;
#14321 = CARTESIAN_POINT ( 'NONE',  ( -2.499999999999996447, -102.8333333333333286, 4.330127018922195425 ) ) ;
#14322 = CARTESIAN_POINT ( 'NONE',  ( -4.458734124999999437, -60.39583333196774362, -2.574251347313719407 ) ) ;
#14323 = CARTESIAN_POINT ( 'NONE',  ( -1.339745962155613812, -62.08034179853028434, -5.000000000000000000 ) ) ;
#14324 = CARTESIAN_POINT ( 'NONE',  ( -3.152548672688508926E-16, 20.43750000136559208, -5.148502694627439702 ) ) ;
#14325 = FACE_OUTER_BOUND ( 'NONE', #29316, .T. ) ;
#14326 = CARTESIAN_POINT ( 'NONE',  ( 1.975475456537005874E-15, -43.75000000000000000, 5.000000000000000000 ) ) ;
#14327 = ADVANCED_FACE ( 'NONE', ( #58374 ), #4339, .T. ) ;
#14328 = CARTESIAN_POINT ( 'NONE',  ( -4.458734124999999437, -49.56249999863440792, 0.000000000000000000 ) ) ;
#14329 = CARTESIAN_POINT ( 'NONE',  ( 2.499999999999998668, -4.208333330602147981, -4.330127018922193649 ) ) ;
#14330 = DIRECTION ( 'NONE',  ( -0.000000000000000000, 1.000000000000000000, -0.000000000000000000 ) ) ;
#14331 = CARTESIAN_POINT ( 'NONE',  ( 6.123233995736766282E-16, -120.0000000000000000, -5.000000000000000000 ) ) ;
#14332 = CARTESIAN_POINT ( 'NONE',  ( 4.458734124999998549, -85.97916666530107932, -2.574251347313721627 ) ) ;
#14333 = CARTESIAN_POINT ( 'NONE',  ( -4.458734124999997661, -106.2291666653010793, 2.574251347313722516 ) ) ;
#14334 = CARTESIAN_POINT ( 'NONE',  ( -4.458734124999999437, -11.56249999863440792, 0.000000000000000000 ) ) ;
#14335 = ORIENTED_EDGE ( 'NONE', *, *, #54703, .F. ) ;
#14336 = CARTESIAN_POINT ( 'NONE',  ( -3.535533905932737309, -155.7500000027312126, -3.535533905932738197 ) ) ;
#14337 = CARTESIAN_POINT ( 'NONE',  ( 2.229367062499998831, -97.64583333196773651, -3.861377020970580887 ) ) ;
#14338 = CARTESIAN_POINT ( 'NONE',  ( 3.535533905932736864, -163.2500000027312126, 3.535533905932738641 ) ) ;
#14339 = CARTESIAN_POINT ( 'NONE',  ( 9.457646018065525792E-16, -90.31249999863439371, 5.148502694627439702 ) ) ;
#14340 = CARTESIAN_POINT ( 'NONE',  ( 2.626220312808019583E-14, 21.75000000000000000, -5.000000000000000000 ) ) ;
#14341 = CARTESIAN_POINT ( 'NONE',  ( 5.000000000000000000, -51.37499999726881583, -6.123233995736766282E-16 ) ) ;
#14342 = FACE_OUTER_BOUND ( 'NONE', #21274, .T. ) ;
#14343 = CARTESIAN_POINT ( 'NONE',  ( -50.40829686548195099, -129.0000000013656063, -1.485763867205728284 ) ) ;
#14344 = CARTESIAN_POINT ( 'NONE',  ( -56.48576386720575471, -148.7500000013655779, -4.591703134518078322 ) ) ;
#14345 = CARTESIAN_POINT ( 'NONE',  ( -4.458734124999999437, -20.39583333196774362, -2.574251347313719407 ) ) ;
#14346 = CARTESIAN_POINT ( 'NONE',  ( 2.229367062499998831, 11.10416666803225993, -3.861377020970580887 ) ) ;
#14347 = CARTESIAN_POINT ( 'NONE',  ( 2.229367062500001939, -58.22916666530107932, 3.861377020970579999 ) ) ;
#14348 = CARTESIAN_POINT ( 'NONE',  ( -5.000000000000000000, -20.08333333333333925, -2.886751345948128211 ) ) ;
#14349 = CARTESIAN_POINT ( 'NONE',  ( 2.229367062499998831, -14.64583333196773474, -3.861377020970580887 ) ) ;
#14350 = DIRECTION ( 'NONE',  ( -0.000000000000000000, 1.000000000000000000, -0.000000000000000000 ) ) ;
#14351 = CARTESIAN_POINT ( 'NONE',  ( -5.000000000000000888, -153.5625000000000568, -2.071067811865475949 ) ) ;
#14352 = ORIENTED_EDGE ( 'NONE', *, *, #37764, .T. ) ;
#14353 = CARTESIAN_POINT ( 'NONE',  ( 2.229367062500001939, -40.22916666530107221, 3.861377020970579999 ) ) ;
#14354 = CARTESIAN_POINT ( 'NONE',  ( -53.51423613279429503, -125.5000000013656205, 4.591703134518082763 ) ) ;
#14355 = CARTESIAN_POINT ( 'NONE',  ( 0.04606493828584144051, 9.175055303659556571, -8.057411785091790790 ) ) ;
#14356 = FACE_OUTER_BOUND ( 'NONE', #42846, .T. ) ;
#14357 = CARTESIAN_POINT ( 'NONE',  ( 2.229367062499998831, -86.64583333196773651, -3.861377020970580887 ) ) ;
#14358 = CARTESIAN_POINT ( 'NONE',  ( 4.458734124999998549, 20.02083333469892779, -2.574251347313721627 ) ) ;
#14359 = VECTOR ( 'NONE', #26490, 1000.000000000000000 ) ;
#14360 = CARTESIAN_POINT ( 'NONE',  ( 4.458734124999998549, 8.270833334698926009, -2.574251347313721627 ) ) ;
#14361 = FACE_OUTER_BOUND ( 'NONE', #30765, .T. ) ;
#14362 = CARTESIAN_POINT ( 'NONE',  ( -2.229367062499996610, -90.39583333196773651, 3.861377020970582219 ) ) ;
#14363 = CARTESIAN_POINT ( 'NONE',  ( 5.000000000000000000, -72.41666666666667140, -2.886751345948129988 ) ) ;
#14364 = CARTESIAN_POINT ( 'NONE',  ( 5.000000000000000000, 14.70833333606451987, -2.886751345948129988 ) ) ;
#14365 = VERTEX_POINT ( 'NONE', #62892 ) ;
#14366 = CARTESIAN_POINT ( 'NONE',  ( 1.339745962155615144, -102.7053418012614827, 4.999999999999999112 ) ) ;
#14367 = VERTEX_POINT ( 'NONE', #23657 ) ;
#14369 = CARTESIAN_POINT ( 'NONE',  ( 2.499999999999998668, -32.33333333333332860, -4.330127018922193649 ) ) ;
#14368 = CARTESIAN_POINT ( 'NONE',  ( 0.000000000000000000, -170.0000000000000000, 0.000000000000000000 ) ) ;
#14370 = CARTESIAN_POINT ( 'NONE',  ( 4.458734125000001214, -35.89583333196773651, 2.574251347313718519 ) ) ;
#14371 = CARTESIAN_POINT ( 'NONE',  ( -4.999999999999999112, -36.79166666393548013, 2.886751345948131764 ) ) ;
#14373 = VERTEX_POINT ( 'NONE', #9164 ) ;
#14372 = CARTESIAN_POINT ( 'NONE',  ( 4.458734124999998549, -64.72916666530106511, -2.574251347313721627 ) ) ;
#14374 = CARTESIAN_POINT ( 'NONE',  ( -58.39396692619412477, -149.6875000013656063, 2.891590998281057701 ) ) ;
#14375 = CARTESIAN_POINT ( 'NONE',  ( 2.229367062499998831, -14.64583333196773474, -3.861377020970580887 ) ) ;
#14377 = ORIENTED_EDGE ( 'NONE', *, *, #61491, .F. ) ;
#14376 = CARTESIAN_POINT ( 'NONE',  ( 4.458734124999999437, -16.06249999863440436, -5.460374474430324690E-16 ) ) ;
#14378 = CARTESIAN_POINT ( 'NONE',  ( -5.000000000000000000, -76.00000000000000000, 0.000000000000000000 ) ) ;
#14379 = CARTESIAN_POINT ( 'NONE',  ( -55.35523342533222291, -135.3125000013656063, 4.444560631937231499 ) ) ;
#14380 = CARTESIAN_POINT ( 'NONE',  ( 4.458734124999998549, -54.97916666530107221, -2.574251347313721627 ) ) ;
#14381 = CARTESIAN_POINT ( 'NONE',  ( -3.535250795749689387E-16, -81.12499999726881583, -5.773502691896257311 ) ) ;
#14383 = EDGE_LOOP ( 'NONE', ( #38130, #12693, #58046, #22781 ) ) ;
#14382 = DIRECTION ( 'NONE',  ( 0.000000000000000000, 0.000000000000000000, 1.000000000000000000 ) ) ;
#14384 = CARTESIAN_POINT ( 'NONE',  ( -50.01589407740564042, -144.6250000000000284, 0.3983568153799778022 ) ) ;
#14385 = CARTESIAN_POINT ( 'NONE',  ( -4.458734124999998549, -21.47916666530107221, 2.574251347313722516 ) ) ;
#14386 = ORIENTED_EDGE ( 'NONE', *, *, #52826, .T. ) ;
#14387 = DIRECTION ( 'NONE',  ( 0.000000000000000000, 1.000000000000000000, 0.000000000000000000 ) ) ;
#14388 = CARTESIAN_POINT ( 'NONE',  ( 4.458734125000000326, -166.6250000013656063, -1.846868145590734978 ) ) ;
#14389 = CARTESIAN_POINT ( 'NONE',  ( 4.458734125000001214, -107.1458333319677507, 2.574251347313718519 ) ) ;
#14390 = CARTESIAN_POINT ( 'NONE',  ( -5.000000000000000888, -167.5625000027312126, 2.071067811865474617 ) ) ;
#14391 = VERTEX_POINT ( 'NONE', #29080 ) ;
#14392 = CARTESIAN_POINT ( 'NONE',  ( -50.40829686548195099, -149.2500000013656063, -1.485763867205728284 ) ) ;
#14393 = VECTOR ( 'NONE', #11181, 1000.000000000000000 ) ;
#14394 = CARTESIAN_POINT ( 'NONE',  ( -59.81910112700025905, -139.3125000027312126, -2.462841084822630311 ) ) ;
#14395 = CARTESIAN_POINT ( 'NONE',  ( -3.152548672688508926E-16, -37.56249999863440792, -5.148502694627439702 ) ) ;
#14396 = CARTESIAN_POINT ( 'NONE',  ( -7.908228835406498902, 3.123118350879302341, -7.776694659841278501 ) ) ;
#14397 = VECTOR ( 'NONE', #50915, 1000.000000000000000 ) ;
#14398 = CYLINDRICAL_SURFACE ( 'NONE', #33736, 5.000000000000000000 ) ;
#14399 = CARTESIAN_POINT ( 'NONE',  ( -3.152548672688508926E-16, -10.56249999863440792, -5.148502694627439702 ) ) ;
#14400 = CARTESIAN_POINT ( 'NONE',  ( -4.458734124999997661, -102.4791666653010509, 2.574251347313722516 ) ) ;
#14401 = ORIENTED_EDGE ( 'NONE', *, *, #5916, .T. ) ;
#14402 = CARTESIAN_POINT ( 'NONE',  ( -1.846868145590734756, -142.3750000013656063, -4.458734125000000326 ) ) ;
#14403 = CARTESIAN_POINT ( 'NONE',  ( -4.458734124999999437, -29.56249999863440436, 0.000000000000000000 ) ) ;
#14404 = CARTESIAN_POINT ( 'NONE',  ( -1.339745962155613812, 11.79465819873851906, -5.000000000000000000 ) ) ;
#14405 = CARTESIAN_POINT ( 'NONE',  ( -59.44456063193725015, -133.5625000013656063, -0.3552334253322034230 ) ) ;
#14406 = CARTESIAN_POINT ( 'NONE',  ( 4.458734124999998549, -67.97916666530107932, -2.574251347313721627 ) ) ;
#14407 = CARTESIAN_POINT ( 'NONE',  ( 1.339745962155612702, -43.29465819873851729, -5.000000000000000000 ) ) ;
#14408 = CARTESIAN_POINT ( 'NONE',  ( -50.18089887299977647, -146.8125000027311842, 2.462841084822530835 ) ) ;
#14409 = CARTESIAN_POINT ( 'NONE',  ( 1.846868145590736310, -142.6250000013656063, 4.458734124999997661 ) ) ;
#14410 = CARTESIAN_POINT ( 'NONE',  ( -2.229367062499996610, 2.604166668032259491, 3.861377020970582219 ) ) ;
#14411 = ORIENTED_EDGE ( 'NONE', *, *, #1944, .T. ) ;
#14412 = DIRECTION ( 'NONE',  ( 0.000000000000000000, -1.000000000000000000, 0.000000000000000000 ) ) ;
#14414 = CARTESIAN_POINT ( 'NONE',  ( -4.458734124999999437, -30.31249999863440436, 0.000000000000000000 ) ) ;
#14413 = CARTESIAN_POINT ( 'NONE',  ( -3.535250795749689387E-16, -95.25000000000000000, -5.773502691896257311 ) ) ;
#14415 = CARTESIAN_POINT ( 'NONE',  ( -1.339745962155613812, -23.08034179853029144, -5.000000000000000000 ) ) ;
#14416 = CARTESIAN_POINT ( 'NONE',  ( 4.458734124999999437, -77.06249999863440792, -5.460374474430324690E-16 ) ) ;
#14417 = CARTESIAN_POINT ( 'NONE',  ( -4.458734124999999437, 24.43750000136559208, 0.000000000000000000 ) ) ;
#14418 = CYLINDRICAL_SURFACE ( 'NONE', #34550, 5.000000000000000000 ) ;
#14419 =( BOUNDED_CURVE ( )  B_SPLINE_CURVE ( 2, ( #39939, #29014, #48640, #43810, #59585, #35139, #14858, #63456, #19375 ),
 .UNSPECIFIED., .F., .F. ) 
 B_SPLINE_CURVE_WITH_KNOTS ( ( 3, 2, 2, 2, 3 ),
 ( 0.01874999999999999931, 0.01944444444444444475, 0.02083333333333333218, 0.02222222222222222307, 0.02291666666666666852 ),
 .UNSPECIFIED. ) 
 CURVE ( )  GEOMETRIC_REPRESENTATION_ITEM ( )  RATIONAL_B_SPLINE_CURVE ( ( 0.9330127018922194093, 0.9330127018922194093, 1.000000000000000000, 0.8660254037844387076, 1.000000000000000000, 0.8660254037844387076, 1.000000000000000000, 0.9330127018922191873, 0.9330127018922194093 ) ) 
 REPRESENTATION_ITEM ( '' )  );
#14420 = CARTESIAN_POINT ( 'NONE',  ( -55.35523342533222291, -142.3125000013656063, 4.444560631937231499 ) ) ;
#14421 = CARTESIAN_POINT ( 'NONE',  ( 4.458734125000000326, 0.1041666680322607674, 2.574251347313718519 ) ) ;
#14422 = CARTESIAN_POINT ( 'NONE',  ( -2.229367062499996610, 27.60416666803225993, 3.861377020970582219 ) ) ;
#14423 = CARTESIAN_POINT ( 'NONE',  ( -2.229367062499996610, -45.39583333196774362, 3.861377020970582219 ) ) ;
#14424 = CARTESIAN_POINT ( 'NONE',  ( -5.000000000000000000, -3.958333330602147537, -2.886751345948128211 ) ) ;
#14425 = CARTESIAN_POINT ( 'NONE',  ( 9.457646018065525792E-16, -0.06249999863440491854, 5.148502694627439702 ) ) ;
#14426 = CARTESIAN_POINT ( 'NONE',  ( -4.458734124999999437, -23.56249999863440436, 0.000000000000000000 ) ) ;
#14427 = CARTESIAN_POINT ( 'NONE',  ( 4.458734124999998549, -68.72916666530106511, -2.574251347313721627 ) ) ;
#14428 = CARTESIAN_POINT ( 'NONE',  ( -4.999999999999999112, -107.7916666639354730, 2.886751345948131764 ) ) ;
#14429 = ADVANCED_FACE ( 'NONE', ( #14301 ), #23957, .T. ) ;
#14430 = CARTESIAN_POINT ( 'NONE',  ( -3.152548672688508926E-16, 27.43750000136559564, -5.148502694627439702 ) ) ;
#14431 = DIRECTION ( 'NONE',  ( -0.000000000000000000, 1.000000000000000000, -0.000000000000000000 ) ) ;
#14432 = CARTESIAN_POINT ( 'NONE',  ( 2.229367062499998831, -108.8958333319677365, -3.861377020970580887 ) ) ;
#14433 = CARTESIAN_POINT ( 'NONE',  ( -2.229367062499996610, -73.39583333196773651, 3.861377020970582219 ) ) ;
#14434 = CARTESIAN_POINT ( 'NONE',  ( 1.060575238724906964E-15, -54.75000000000000000, 5.773502691896257311 ) ) ;
#14435 = CARTESIAN_POINT ( 'NONE',  ( 6.123233995736766282E-16, -170.0000000000000000, -5.000000000000000000 ) ) ;
#14436 = ORIENTED_EDGE ( 'NONE', *, *, #56313, .T. ) ;
#14437 = CARTESIAN_POINT ( 'NONE',  ( 1.975475456537005874E-15, -47.74999999999999289, 5.000000000000000000 ) ) ;
#14438 = AXIS2_PLACEMENT_3D ( 'NONE', #46400, #21645, #56699 ) ;
#14439 = CARTESIAN_POINT ( 'NONE',  ( 5.000000000000000000, -27.37499999726880873, -6.123233995736766282E-16 ) ) ;
#14440 = CARTESIAN_POINT ( 'NONE',  ( 5.000000000000000000, -17.50000000000000000, -6.123233995736766282E-16 ) ) ;
#14441 = CARTESIAN_POINT ( 'NONE',  ( 2.229367062500001939, -22.97916666530107221, 3.861377020970579999 ) ) ;
#14442 = AXIS2_PLACEMENT_3D ( 'NONE', #22699, #13348, #3708 ) ;
#14443 = CARTESIAN_POINT ( 'NONE',  ( -4.458734124999997661, -82.22916666530106511, 2.574251347313722516 ) ) ;
#14444 = CARTESIAN_POINT ( 'NONE',  ( -4.458734125000001214, -167.1250000013656063, 1.846868145590734089 ) ) ;
#14445 = ADVANCED_FACE ( 'NONE', ( #4648 ), #63520, .T. ) ;
#14446 = CARTESIAN_POINT ( 'NONE',  ( 5.000000000000000000, -16.29166666393548368, -2.886751345948129988 ) ) ;
#14448 = ORIENTED_EDGE ( 'NONE', *, *, #19984, .T. ) ;
#14447 = CARTESIAN_POINT ( 'NONE',  ( -4.458734124999999437, -52.39583333196773651, -2.574251347313719407 ) ) ;
#14449 = CARTESIAN_POINT ( 'NONE',  ( 2.499999999999998668, -98.33333333333332860, -4.330127018922193649 ) ) ;
#14451 = ORIENTED_EDGE ( 'NONE', *, *, #16209, .T. ) ;
#14450 = CARTESIAN_POINT ( 'NONE',  ( 2.229367062499998831, 4.104166668032260823, -3.861377020970580887 ) ) ;
#14452 = CARTESIAN_POINT ( 'NONE',  ( -57.19623071787016499, -154.3750000013656063, 4.297418129356382899 ) ) ;
#14453 = CARTESIAN_POINT ( 'NONE',  ( 5.000000000000000000, -60.50000000000000000, -6.123233995736766282E-16 ) ) ;
#14454 = CARTESIAN_POINT ( 'NONE',  ( -4.458734125000001214, -156.1250000013655779, 1.846868145590734089 ) ) ;
#14455 = CARTESIAN_POINT ( 'NONE',  ( 9.457646018065525792E-16, -43.31249999863440792, 5.148502694627439702 ) ) ;
#14456 = CARTESIAN_POINT ( 'NONE',  ( -5.000000000000000000, -55.99999999999999289, 0.000000000000000000 ) ) ;
#14457 = CARTESIAN_POINT ( 'NONE',  ( 2.071067811865476394, -163.1875000000000284, 5.000000000000000000 ) ) ;
#14458 = CARTESIAN_POINT ( 'NONE',  ( 0.000000000000000000, -120.0000000000000000, 0.000000000000000000 ) ) ;
#14459 = CARTESIAN_POINT ( 'NONE',  ( -55.35523342533222291, -125.5625000013655921, 4.444560631937231499 ) ) ;
#14460 = CARTESIAN_POINT ( 'NONE',  ( -4.458734124999999437, -6.562499998634403475, 0.000000000000000000 ) ) ;
#14461 = CARTESIAN_POINT ( 'NONE',  ( 2.229367062500001939, -48.22916666530106511, 3.861377020970579999 ) ) ;
#14462 = CARTESIAN_POINT ( 'NONE',  ( 1.975475456537005874E-15, -4.624999997268815832, 5.000000000000000000 ) ) ;
#14463 = CARTESIAN_POINT ( 'NONE',  ( 1.846868145590735200, -149.2500000013655779, -4.458734125000000326 ) ) ;
#14464 = CARTESIAN_POINT ( 'NONE',  ( -2.229367062500000163, -88.72916666530106511, -3.861377020970580443 ) ) ;
#14465 = CARTESIAN_POINT ( 'NONE',  ( 5.000000000000000000, 8.583333333333332149, -2.886751345948130876 ) ) ;
#14466 =( BOUNDED_CURVE ( )  B_SPLINE_CURVE ( 2, ( #39346, #39981, #21659, #41250, #45455, #1420, #25838, #40936, #60897 ),
 .UNSPECIFIED., .F., .F. ) 
 B_SPLINE_CURVE_WITH_KNOTS ( ( 3, 2, 2, 2, 3 ),
 ( 0.1854166666666666741, 0.1861111111111111160, 0.1875000000000000000, 0.1888888888888888840, 0.1895833333333333259 ),
 .UNSPECIFIED. ) 
 CURVE ( )  GEOMETRIC_REPRESENTATION_ITEM ( )  RATIONAL_B_SPLINE_CURVE ( ( 0.9330127018922194093, 0.9330127018922194093, 1.000000000000000000, 0.8660254037844387076, 1.000000000000000000, 0.8660254037844387076, 1.000000000000000000, 0.9330127018922194093, 0.9330127018922194093 ) ) 
 REPRESENTATION_ITEM ( '' )  );
#14467 = EDGE_LOOP ( 'NONE', ( #56921, #43491, #41508, #62164 ) ) ;
#14468 = CARTESIAN_POINT ( 'NONE',  ( 5.000000000000000888, -99.58333333333332860, 2.886751345948126879 ) ) ;
#14469 = CARTESIAN_POINT ( 'NONE',  ( -6.972266317189433020E-16, -6.124999997268813168, -5.000000000000000000 ) ) ;
#14470 = CARTESIAN_POINT ( 'NONE',  ( -56.66612745406270335, -149.4375000027311842, -5.149110718188516067 ) ) ;
#14471 = CARTESIAN_POINT ( 'NONE',  ( -6.972266317189433020E-16, -82.12499999726881583, -5.000000000000000000 ) ) ;
#14472 = VERTEX_POINT ( 'NONE', #19761 ) ;
#14473 = CARTESIAN_POINT ( 'NONE',  ( -4.458734124999999437, -13.64583333196774007, -2.574251347313719407 ) ) ;
#14474 = CARTESIAN_POINT ( 'NONE',  ( 1.339745962155615144, -105.5803417985302843, 4.999999999999999112 ) ) ;
#14475 = CARTESIAN_POINT ( 'NONE',  ( 2.229367062500001939, -0.9791666653010712151, 3.861377020970579999 ) ) ;
#14476 = CARTESIAN_POINT ( 'NONE',  ( -6.972266317189433020E-16, -55.12499999726880873, -5.000000000000000000 ) ) ;
#14477 = CARTESIAN_POINT ( 'NONE',  ( 3.152801135295367541, -153.3125000013656063, -3.152801135295367541 ) ) ;
#14478 = CARTESIAN_POINT ( 'NONE',  ( -4.458734124999997661, 18.52083333469892779, 2.574251347313722516 ) ) ;
#14479 = VERTEX_POINT ( 'NONE', #14614 ) ;
#14480 = CARTESIAN_POINT ( 'NONE',  ( -3.152548672688508926E-16, -93.56249999863440792, -5.148502694627439702 ) ) ;
#14481 = CARTESIAN_POINT ( 'NONE',  ( -4.999999999999998224, -33.79166666393547303, 2.886751345948131764 ) ) ;
#14482 = FACE_OUTER_BOUND ( 'NONE', #1221, .T. ) ;
#14483 = CARTESIAN_POINT ( 'NONE',  ( 4.458734124999999437, -13.81249999863440259, -5.460374474430324690E-16 ) ) ;
#14484 = VECTOR ( 'NONE', #13277, 1000.000000000000000 ) ;
#14485 = CARTESIAN_POINT ( 'NONE',  ( 0.000000000000000000, 0.000000000000000000, 0.000000000000000000 ) ) ;
#14486 = FACE_OUTER_BOUND ( 'NONE', #37739, .T. ) ;
#14487 = DIRECTION ( 'NONE',  ( 0.8660254037844387076, 0.000000000000000000, -0.4999999999999998890 ) ) ;
#14488 = CARTESIAN_POINT ( 'NONE',  ( -5.000000000000000000, -41.87499999726880873, 0.000000000000000000 ) ) ;
#14489 = CARTESIAN_POINT ( 'NONE',  ( 2.500000000000002220, -64.54166666393547303, 4.330127018922192761 ) ) ;
#14490 = CARTESIAN_POINT ( 'NONE',  ( -4.458734124999999437, 21.60416666803226349, -2.574251347313719407 ) ) ;
#14491 = CARTESIAN_POINT ( 'NONE',  ( -1.339745962155599601, 11.91965820146970145, -5.000000000000007994 ) ) ;
#14492 = EDGE_LOOP ( 'NONE', ( #38427, #22355, #44815, #61750 ) ) ;
#14493 = CARTESIAN_POINT ( 'NONE',  ( 4.458734124999998549, 19.27083333469893134, -2.574251347313721627 ) ) ;
#14494 = CARTESIAN_POINT ( 'NONE',  ( 4.458734124999999437, -61.81249999863440081, -5.460374474430324690E-16 ) ) ;
#14495 = CARTESIAN_POINT ( 'NONE',  ( 4.458734124999998549, -6.979166665301073103, -2.574251347313721627 ) ) ;
#14496 = CARTESIAN_POINT ( 'NONE',  ( 1.975475456537005874E-15, -8.624999997268812280, 5.000000000000000000 ) ) ;
#14497 = CARTESIAN_POINT ( 'NONE',  ( 1.060575238724906964E-15, 8.250000000000000000, 5.773502691896257311 ) ) ;
#14498 = CARTESIAN_POINT ( 'NONE',  ( 5.000000000000000000, -139.1250000027312126, 0.000000000000000000 ) ) ;
#14499 = CARTESIAN_POINT ( 'NONE',  ( -54.60164318462004474, -142.3750000000000284, -4.984105922594373794 ) ) ;
#14500 = CARTESIAN_POINT ( 'NONE',  ( -4.458734124999998549, -55.22916666530107932, 2.574251347313722516 ) ) ;
#14501 = CARTESIAN_POINT ( 'NONE',  ( 5.000000000000000888, -88.45833333060214443, 2.886751345948126879 ) ) ;
#14502 = EDGE_CURVE ( 'NONE', #47078, #39600, #26320, .T. ) ;
#14503 = CARTESIAN_POINT ( 'NONE',  ( 2.499999999999998668, -14.20833333060214976, -4.330127018922193649 ) ) ;
#14504 = CARTESIAN_POINT ( 'NONE',  ( -1.339745962155613812, -55.08034179853029144, -5.000000000000000000 ) ) ;
#14505 = DIRECTION ( 'NONE',  ( 0.000000000000000000, 0.000000000000000000, 1.000000000000000000 ) ) ;
#14506 = CARTESIAN_POINT ( 'NONE',  ( 1.846868145590735200, -153.5000000013656063, -4.458734124999999437 ) ) ;
#14507 = CARTESIAN_POINT ( 'NONE',  ( -4.999999999999999112, -39.91666666666667140, 2.886751345948131764 ) ) ;
#14508 = CARTESIAN_POINT ( 'NONE',  ( -48.00000000000002132, -135.0000000000000284, -4.041451884327376121 ) ) ;
#14509 = DIRECTION ( 'NONE',  ( -0.000000000000000000, 1.000000000000000000, -0.000000000000000000 ) ) ;
#14510 = ORIENTED_EDGE ( 'NONE', *, *, #50324, .T. ) ;
#14511 = CARTESIAN_POINT ( 'NONE',  ( -2.229367062499996610, -99.14583333196773651, 3.861377020970582219 ) ) ;
#14512 = CARTESIAN_POINT ( 'NONE',  ( 2.229367062500001939, 3.770833334698926009, 3.861377020970579999 ) ) ;
#14513 =( BOUNDED_SURFACE ( )  B_SPLINE_SURFACE ( 1, 2, ( 
 ( #52900, #57426, #43543, #14283, #58667, #58356, #42612, #43855, #28133, #38412, #53525, #9453, #29062, #13661, #23942, #63188, #13347, #19098, #14589, #32968, #53834, #23011, #63502, #34209, #43232, #62250, #58036, #47751, #38716, #48686, #9763, #47443, #62874, #4626, #3707, #33593, #33281, #8836, #28757, #3394, #42924, #57735, #28449, #52591, #18169, #37798, #8524, #23322, #62570, #18489, #38112, #53213, #4018, #23638, #18785, #9146, #48380, #45143, #39353, #1106, #49965, #5918, #20388, #30023, #19740, #34863, #30669, #21026, #55444, #49652, #40634, #49003, #44496, #10411, #44178, #35501, #34519, #145, #60275, #35821, #39666, #39988, #20062, #58983, #15566, #14911, #5588, #29370, #11044, #25525, #30339, #20715, #40320, #59958, #50288, #15881, #4950, #1427, #55119, #6236, #25845, #45462, #16193, #59303, #24573, #54150, #25205, #10090, #29700, #44819, #49331, #5274, #24895, #54484, #458, #15236, #781, #59633, #35186, #54804, #10733, #51880, #47054, #31293, #61862, #61543, #11359, #31623, #7820, #26163, #27423, #50929, #31939, #2060, #3004, #22621, #41572, #17475, #50607, #42217, #17779, #6870, #36136, #37398, #51567, #27118, #2676, #12633, #12328, #30983, #6548, #7506, #32250, #46731, #45782, #1742, #21667, #21344, #40944, #56076, #22298, #41897, #51259, #60594, #37096, #11674, #16828, #56715, #16514, #55757, #26485, #46099, #11996, #41258, #60906, #36447, #7193, #26801, #46421, #2370, #21979, #61224, #17148, #36772, #56403, #3941, #52518, #43469, #4251, #52823, #33519, #12947, #63115, #23866, #57349, #42532, #14201, #43158, #62798, #19026, #47370, #58282, #32571, #38640, #57033, #13589, #8139, #8760, #13267, #57969, #28679, #52193, #27741, #47987, #9069, #28057, #18717, #38031, #57663, #13892, #22938, #3628, #18411, #33208, #32890, #53137, #3318, #62169, #18089, #8453, #37712, #28366, #47676, #23235, #42849, #62492, #23561, #38342, #48298, #10851, #50094, #10530, #30142, #44954, #11172, #30466, #53960, #25332, #39478, #34662, #49771, #20519, #54281, #20192, #59439, #14716, #5717, #49133, #24698, #59114, #58786, #266, #50423, #5398, #59759, #39793, #30795, #34336, #60079, #15368, #6367, #25971, #6048, #15043, #15685, #29825, #45587, #16001, #914, #45269, #9892, #1545, #35625, #10219, #19864, #39161, #35305, #54925, #29502, #5076, #44302, #49458, #55253, #25014, #34991, #44624, #40118, #583, #25656, #1235, #54606, #20836, #40437, #36895, #21471, #51379, #51055, #26608, #2491, #40753, #16639, #31416, #46225, #31109, #17271, #51693, #12758, #32057, #16328, #61666, #1867, #12124, #7634, #27240, #46862, #6999, #41700, #7321, #22428, #35947, #21149, #61348, #31748, #21792, #11493, #2188, #42025, #32381, #47181, #41387, #52006, #60402, #36261, #61035, #55576, #2807, #26282, #50731, #7946, #27549, #16958, #26931, #11801, #6675, #46548, #45905, #36570, #41070, #17599, #56525, #22106, #12445, #37215, #56841, #60716, #55887, #56201, #38762, #62920, #23984, #18834, #4366, #33950, #13393, #29106, #32697, #47793, #4064, #38452, #42972, #19145, #33638, #3437, #8566, #58081, #53258, #53571, #9497, #9193, #3750, #28806, #43589, #58401, #23052, #3123, #48424, #22744, #23372, #63231, #17899, #14329, #14011, #42341, #38157, #57782, #8879, #61980, #37521, #57162, #52944, #42657, #62296, #13702, #48112, #18218, #62614, #18537, #13077, #33324, #52327, #8262, #37844, #27864, #47484, #57476, #33016, #23683, #28493, #52632, #28177, #43282, #49375, #60000, #40360, #59677, #59351, #34907, #54529, #1155, #39712, #29417, #30389, #11091, #39395, #29744, #49048, #19467, #4997, #5320, #5964, #59028, #48730, #15609, #5638, #39082, #15924, #25251, #44868, #35547, #15285, #830, #24616, #43899, #58711, #25574, #34253, #44222, #14637, #35227, #4673, #53881, #10450, #10779, #20437, #30065, #63547, #49694, #20108, #54847, #40035, #9807, #50011, #45188, #20754, #55172, #24939, #188, #19787, #24295, #14959, #34568, #54199, #44545, #10138, #501, #56451, #21716, #11724, #35869, #55496, #12373, #40998, #25891, #11410, #31341, #36186, #26857, #45830, #46153, #41310, #60642, #16564, #16879, #6286, #50981, #1792, #30716, #6921, #46469, #51620, #56765, #50338, #56124, #55808, #36495, #41620, #2415, #31030, #12047, #45507, #1470, #31671, #26532, #51307, #61271, #22027, #50656, #7245, #17193, #36820, #2114, #60958, #31987, #2730, #7554, #21072, #27167, #6594, #26210, #46781, #22349, #21394, #41946, #61590, #40677, #17524, #60322, #16248, #37143, #32299, #37450, #23912, #42582, #33252, #13318, #48351, #51928, #33564, #32939, #43513, #4295, #23610, #23292, #62540, #18459, #28725, #3678, #57081, #58012, #38689, #3364, #57396, #12999, #47101, #32618, #52562, #53185, #22980, #12686, #43203, #52872, #3051, #63159, #8805, #28421, #19069, #42892, #48036, #52245, #7869, #22668, #9117, #61907, #8186, #42267, #62846, #27474, #17827, #38081, #38385, #3987, #57707, #27788, #13633, #47720, #18760, #13938, #47413, #62220, #18138, #37766, #8495, #28105, #58642, #14561, #10383, #29992, #5562, #49625, #34488, #48975, #53804, #20361, #49304, #39321, #63475, #19393, #39959, #4924, #53494, #39013, #58953, #118, #54457, #9737, #10060, #5243, #24543, #44146, #44469, #33875, #14880, #29341, #58326, #54122, #25174, #15539, #35158, #19712, #14252, #44789, #15207, #29033, #25495, #34832, #752, #5888, #24867, #59607, #34183, #9425, #48658, #54773, #43829, #29672, #4599, #10705, #24222, #427, #20032, #30312, #49933, #39637, #59276, #45115, #1080, #20686, #11965, #50259, #36421, #6842, #26455, #41545, #16486, #40604, #60249, #56049, #31595, #51228, #7164, #36106, #30957, #35793, #2341, #31266, #21317, #45435, #1398, #21948, #50582, #35474, #20999, #40918, #45756, #26774, #55416, #55730, #50900, #6524, #26136, #46073, #15852, #60562, #11333, #40292, #11645, #46393, #61196, #2651, #59930, #2031, #1709, #21636, #17118, #36744, #16168, #41229, #56374, #12297, #60876, #16801, #31913, #51540, #7476, #55091, #27089, #46705, #11016, #30637, #6207, #25821, #3293, #42505, #61518, #52494, #32221, #7794, #42192, #41871, #47028, #33490, #52168, #42820, #22912, #57946, #17448, #43132, #62142, #53109, #13867, #33183, #32864, #8427, #28030, #38318, #13241, #2978, #3914, #48271, #12920, #18061, #22595, #56692, #61834, #37683, #52799, #47649, #3602, #23209, #9046, #62465, #17756, #23532, #22270, #32541, #57326, #37372, #12608, #57005, #18385, #62772, #8112, #37068, #8734, #38004, #51852, #28655, #57637, #13565, #27397, #28342, #47959, #27716, #47344, #18692, #44710, #53419, #48587, #58249, #54381, #23842, #38614, #34418, #29919, #44392, #29596, #19000, #9984, #39247, #10307, #39564, #14175, #351, #54047, #49228, #5486, #44072, #4528, #24153, #19953, #59205, #15133, #34755, #37, #58569, #63401, #49545, #58874, #48902, #9352, #28964, #25100, #14488, #63090, #43756, #4847, #9664, #673, #19317, #19637, #14804, #34109, #53731, #5168, #43445, #24467, #38933, #4228, #24786, #20282, #39884, #30233, #33802, #59529, #29272, #15462, #35080, #54699, #10620, #11580, #21563, #60805, #21238, #40845, #55666, #21880, #41160, #1007, #36034, #50181, #45361, #60488, #31199, #1326, #30884, #6455, #25421, #16416, #59852, #35393, #6133, #5804, #10938, #61127, #16093, #6768, #50515, #41476, #45040, #7089, #26064, #17051, #36667, #50828, #15776, #45681, #56296, #31512, #26379, #45997, #1963, #16732, #36349, #51155, #55979, #20611, #12224, #11892, #26703, #46319, #2276, #49856, #60171, #40216, #55015, #1638, #30556, #25747, #20925, #40529, #35716, #55346, #11260, #28817, #63243, #19480, #39094, #19156, #33335, #38775, #9511, #4685, #52644, #58723, #58413, #31839, #52954, #29120, #46636, #48742, #8577, #53269, #23385, #24308, #43913, #62931, #14341, #7409, #63561, #51471, #28188, #56619, #27018, #9204, #48436, #2582, #41799, #22200, #61443, #17371, #36992, #28504, #13407, #23696, #33027, #4378, #33962, #47804, #3761, #48123, #23996, #42983, #18845, #62626, #38171, #14022, #18549, #57793, #13713, #8891, #4075, #43599, #53583, #43295, #38464, #58091, #33651, #59042, #5651, #45201, #25588, #1168, #44557, #35240, #44883, #15937, #9819, #14649, #54859, #25264, #15297, #5009, #20123, #35560, #6299, #40690, #34920, #25904, #34266, #29756, #59364, #29429, #20768, #19798, #49063, #45522, #21085, #24951, #846, #5334, #24629, #11105, #53893, #10463, #30402, #14972, #20449, #513, #39725, #59692, #44236, #10150, #54542, #30076, #200, #10791, #40373, #1482, #60014, #39406, #55184, #34581, #40048, #30729, #50352, #54213, #49707, #50025, #15623, #49390, #5980, #60335, #36834, #51319, #60971, #50668, #2127, #61603, #51942, #22682, #16891, #7884, #16263, #11735, #41323, #11425, #2742, #1804, #31043, #27487, #3065, #6933, #7257, #50994, #6609, #46482, #26222, #36507, #35881, #41962, #17207, #61285, #12386, #7567, #51633, #17538, #56464, #55510, #32313, #32000, #37157, #27179, #56781, #47116, #26545, #45842, #21408, #56138, #46796, #22362, #12059, #12700, #41011, #60653, #21728, #16577, #36198, #55819, #31352, #46165, #31684, #26870, #2428, #22040, #41631, #29047, #28738, #42282, #62554, #38703, #57094, #19083, #62234, #62860, #32953, #14269, #58340, #8820, #48364, #17841, #33888, #53508, #37780, #3379, #4612, #18773, #58023, #9438, #52262, #48672, #37464, #61921, #13013, #38095, #32633, #33267, #42597, #13951, #4308, #38400, #63173, #8200, #27803, #4002, #3692, #28436, #53198, #33577, #47428, #23623, #9132, #23927, #13647, #52886, #48049, #22996, #43528, #18152, #43220, #57412, #13332, #52577, #8509, #28119, #23306, #18475, #47736, #42906, #57721, #9749, #44162, #43841, #48989, #35487, #54135, #44803, #24880, #59943, #63487, #45128, #44481, #55104, #15866, #35172, #34849, #10397, #30007, #40305, #15220, #4936, #5902, #50274, #14894, #5259, #24558, #58653, #131, #440, #1092, #34501, #24236, #54788, #766, #14573, #11028, #20374, #39975, #30652, #54470, #59620, #19725, #19411, #34196, #20701, #29354, #39334, #53819, #10718, #39025, #58967, #49637, #49947, #15551, #5574, #10074, #25188, #59289, #30325, #25508, #29686, #49316, #20046, #39651, #7489, #46085, #6535, #26149, #21962, #41558, #17133, #61209, #2045, #60577, #1724, #31926, #60889, #50913, #11347, #30970, #51554, #16499, #1412, #50595, #6855, #11659, #2355, #21330, #21650, #16813, #36120, #55743, #56063, #45448, #26470, #40930, #6220, #41243, #60262, #31279, #27103, #61529, #32233, #36433, #17461, #25832, #11979, #31608, #21012, #12314, #45768, #40619, #37083, #12621, #51243, #7179, #26787, #16181, #46405, #35806, #36757, #55431, #46718, #56387, #2663, #22283, #41883, #56703, #53122, #52810, #7808, #23854, #47971, #9056, #3926, #28666, #19014, #62155, #14188, #17767, #32877, #8748, #23545, #28043, #4239, #18704, #52180, #57337, #43145, #38329, #38627, #58267, #57958, #52505, #13879, #48284, #43457, #8125, #51865, #33507, #27409, #8439, #63102, #2990, #47041, #27728, #28353, #42518, #22608, #42204, #18397, #61848, #37384, #57017, #12933, #47355, #32555, #3304, #62785, #22926, #18074, #37695, #13253, #47663, #3615, #23222, #42833, #62477, #38018, #57649, #13577, #33195, #30246, #33814, #29611, #49557, #34122, #365, #52, #39261, #15147, #53433, #29285, #44087, #58887, #43769, #29933, #686, #25435, #44724, #28978, #10633, #14501, #24801, #20295, #39896, #59542, #19650, #54394, #19968, #35093, #48600, #9365, #10321, #44406, #34432, #4540, #5499, #39578, #54060, #24166, #14818, #54714, #45053, #59866, #9998, #1020, #63415, #48915, #49241, #19333, #15477, #38946, #58583, #20625, #40231, #5185, #59216, #24481, #53745, #34768, #9677, #25112, #4860, #49869, #5817, #16744, #31526, #26716, #7101, #17062, #36361, #35406, #51484, #11906, #36679, #51168, #56310, #46648, #26076, #41810, #45374, #60500, #55991, #46331, #55677, #31851, #2289, #16105, #21250, #21892, #41488, #2593, #22213, #61140, #16428, #12237, #7421, #27030, #35729, #15790, #55028, #10951, #36048, #30570, #50194, #6146, #55358, #25762, #6468, #1339, #20938, #46010, #40542, #60183, #11272, #30898, #50526, #45694, #1651, #40857, #11592, #31212, #50841, #6781, #26392, #1975, #21574, #41173, #60819, #52433, #61771, #13505, #47894, #57881, #61456, #57263, #33121, #17698, #27966, #27656, #3232, #42757, #17386, #56941, #8052, #22850, #7736, #57579, #28280, #53045, #8668, #56632, #38260, #42128, #8366, #3850, #23471, #43075, #47283, #18321, #47589, #62712, #12546, #32158, #2919, #42440, #62083, #52737, #12862, #13182, #3540, #17996, #37622, #23149, #37005, #32804, #32481, #51794, #62400, #18638, #13806, #23783, #27340, #37946, #33426, #8982, #28593, #48213, #22532, #4168, #46971, #37312, #52110, #14743, #49162, #15396, #34687, #58185, #29527, #43691, #38869, #34359, #24724, #58505, #24406, #63655, #18937, #9917, #53356, #28909, #63338, #63030, #4469, #54634, #9606, #292, #44009, #35021, #38553, #612, #19574, #10558, #30169, #54309, #53989, #5106, #44328, #59464, #19890, #24096, #25039, #5743, #34052, #39187, #39505, #49799, #9291, #58813, #59140, #15074, #10249, #43385, #29852, #19254, #48839, #49485, #5423, #14113, #33739, #44650, #20221, #39822, #48529, #14428, #53673, #29214, #4779, #25362, #45619, #21818, #40146, #2215, #45297, #45933, #16029, #61066, #41416, #55604, #31445, #947, #16986, #36598, #20865, #50119, #51405, #1896, #41098, #56233, #35332, #31773, #20549, #12154, #44981, #21175, #59791, #16355, #25688, #60745, #11826, #15714, #54952 ),
 ( #10881, #40468, #35656, #30825, #30498, #21502, #55914, #6075, #36291, #1262, #60108, #55283, #35976, #51088, #7026, #26635, #11202, #16669, #11521, #46255, #50455, #6395, #26001, #31136, #1575, #40783, #60429, #50761, #6705, #26311, #7977, #18565, #26958, #22454, #52035, #22133, #13422, #12474, #41728, #38188, #13732, #17625, #62007, #61694, #61377, #57188, #36924, #47209, #33354, #52661, #27893, #8288, #23078, #18247, #62323, #8595, #47514, #46576, #43001, #3465, #28206, #42682, #37873, #2836, #32726, #57809, #56553, #27575, #57506, #33045, #3153, #23401, #47820, #7662, #12785, #3777, #62646, #7347, #2518, #17298, #22772, #32084, #51721, #27268, #42052, #46893, #37242, #56867, #32407, #42368, #17926, #37548, #13109, #52353, #44576, #48761, #28524, #43931, #53285, #5028, #39424, #49408, #52970, #4703, #24647, #9221, #19498, #19177, #58430, #34288, #8908, #48457, #63260, #14358, #62948, #49081, #19816, #533, #218, #48141, #29774, #33666, #63579, #59066, #14991, #34601, #38792, #9837, #39113, #54231, #4093, #23716, #29447, #58741, #53601, #43313, #33980, #10170, #20146, #15317, #9533, #39742, #18862, #4395, #29138, #38482, #5352, #58110, #14038, #59383, #28834, #24327, #14668, #43617, #24014, #53911, #44254, #24970, #42216, #17474, #56401, #36771, #51566, #46730, #27117, #37095, #12327, #54560, #7819, #31938, #56714, #7505, #2675, #31292, #61223, #22620, #1740, #16827, #22297, #41896, #11995, #51879, #61541, #36134, #41257, #12632, #32249, #61861, #34939, #27422, #36446, #47053, #3003, #10483, #55756, #30982, #50606, #6547, #56075, #26162, #45781, #21343, #11673, #40943, #26484, #60593, #16513, #2369, #50928, #6869, #46098, #2058, #21666, #60904, #31622, #51257, #7192, #26800, #46420, #21978, #41571, #17147, #57968, #13265, #43157, #4551, #47369, #62491, #18716, #13891, #57662, #33826, #48297, #18088, #23234, #33518, #4250, #24176, #43780, #23865, #18409, #43468, #58281, #53445, #37711, #17778, #63114, #37397, #38030, #14200, #32570, #9377, #57348, #38341, #8452, #28988, #48612, #47986, #19025, #57032, #12946, #52192, #32889, #42531, #8137, #53136, #9068, #27740, #3317, #22937, #62168, #52517, #28056, #13588, #47675, #8759, #3627, #28678, #38639, #42848, #33207, #52822, #28365, #3940, #23559, #62797, #5195, #44736, #19344, #58900, #10011, #24813, #9688, #59554, #30259, #55039, #10646, #58594, #40243, #44099, #54404, #49882, #5831, #25446, #29623, #20309, #29944, #1032, #14512, #63427, #39909, #10334, #377, #53755, #44416, #20637, #10964, #25774, #19981, #30586, #38956, #14829, #39590, #34134, #45066, #4874, #29296, #50208, #6158, #49254, #49569, #54072, #48925, #5508, #24494, #59227, #63, #59881, #34443, #15159, #25123, #34780, #696, #15489, #19660, #35109, #54726, #39272, #15802, #35419, #17073, #2603, #45385, #36371, #11601, #16754, #2299, #7111, #30909, #56002, #26726, #21901, #1984, #21586, #11917, #51494, #46342, #60196, #31540, #26087, #1662, #41184, #51179, #21261, #31221, #6794, #40555, #60829, #35742, #50536, #45708, #20953, #6479, #7431, #36059, #41498, #50852, #27041, #16114, #56325, #26402, #46657, #1351, #12248, #61151, #36692, #31861, #55368, #11283, #46022, #40868, #60512, #16438, #55687, #42178, #61817, #2021, #17107, #37050, #32209, #12284, #52156, #2965, #36408, #41533, #51837, #22581, #22895, #42490, #17742, #36730, #37360, #12905, #8099, #56038, #62128, #56990, #36094, #56363, #32528, #50890, #27703, #11954, #56678, #26762, #47330, #3280, #2639, #55722, #11635, #31255, #6832, #31581, #60864, #26439, #12595, #7780, #46060, #21625, #41218, #16790, #51215, #7151, #31899, #46382, #27075, #2328, #27383, #21935, #61185, #51529, #7466, #47015, #46692, #22258, #41857, #61504, #17434, #28015, #14159, #48256, #4214, #19303, #57931, #18369, #37990, #33788, #53404, #28950, #9336, #13850, #8715, #13550, #43742, #9029, #62758, #23194, #42807, #63386, #28329, #13227, #62447, #18678, #23518, #48573, #33170, #33472, #28641, #47944, #3898, #23826, #57311, #38304, #52784, #18046, #53094, #4513, #38918, #44057, #37668, #43430, #43118, #63074, #24139, #58553, #57622, #18986, #14473, #34094, #38599, #58232, #53719, #9650, #29259, #32850, #48887, #4832, #24451, #52478, #8413, #47633, #3588, #20268, #39234, #30219, #9970, #49214, #19937, #19623, #24772, #11247, #29901, #20598, #659, #35703, #58859, #20910, #39867, #30871, #55330, #10927, #10604, #49843, #5790, #16079, #54681, #44376, #45348, #26051, #10295, #50499, #54032, #14791, #337, #59515, #40515, #49529, #21, #30542, #40202, #34403, #6442, #59838, #15763, #29581, #25408, #35377, #39549, #5152, #59189, #60156, #15120, #34739, #54367, #50165, #5471, #25086, #45027, #25734, #55000, #994, #44695, #6121, #1315, #15449, #35067, #46940, #46619, #1624, #17669, #41780, #2889, #61426, #51455, #32129, #51765, #7709, #11565, #26687, #2564, #17349, #21864, #61742, #12518, #45981, #51139, #36973, #27313, #32451, #52083, #22501, #46304, #42097, #37284, #56913, #1947, #8021, #12831, #45664, #2261, #21224, #60476, #40831, #21548, #22178, #36334, #16401, #36019, #12205, #55651, #31185, #50813, #6750, #41143, #26362, #60791, #56600, #16717, #55964, #11875, #31493, #7072, #41460, #61109, #17034, #36648, #56279, #31822, #7392, #26999, #24068, #27627, #23445, #43356, #27936, #57856, #57546, #33090, #8954, #47256, #23121, #37916, #52705, #37591, #23760, #58154, #19227, #38526, #22821, #4438, #8337, #18608, #14085, #33712, #53331, #13474, #48186, #13777, #28880, #42410, #3201, #4139, #38236, #28251, #17967, #8639, #48501, #38842, #53646, #47865, #58477, #62053, #42725, #3824, #57234, #9265, #32771, #13151, #14403, #34025, #43047, #33399, #18293, #52406, #53013, #47560, #62687, #3509, #43664, #63003, #28565, #62369, #63305, #18912, #53959, #63626, #59758, #29186, #43980, #39792, #35303, #49770, #34990, #24379, #15367, #44623, #15684, #44953, #19547, #5716, #59438, #54605, #10850, #49456, #9891, #29500, #25331, #913, #20518, #40117, #5397, #265, #5075, #54924, #582, #54280, #14715, #34335, #30465, #19863, #4751, #49132, #10218, #15042, #50093, #24696, #25013, #20191, #39477, #59113, #10528, #48813, #29824, #44301, #9580, #30141, #6047, #25655, #35624, #39160, #45268, #34660, #1234, #20835, #40436, #60077, #16000, #58785, #2490, #26607, #46224, #61034, #27239, #46547, #6366, #41386, #55575, #50730, #2187, #36569, #6674, #36260, #11800, #30794, #21791, #1544, #40752, #11492, #11171, #16327, #2806, #21470, #12123, #55886, #46861, #50422, #12444, #31415, #22426, #42024, #22105, #16957, #56200, #31747, #7633, #51378, #35946, #36894, #17598, #1866, #61665, #45586, #25970, #31108, #51054, #32056, #41069, #55252, #41699, #7320, #21148, #60401, #26930, #61346, #26281, #17270, #56524, #45904, #60715, #51692, #6998, #16638, #32696, #62919, #28176, #18217, #42340, #61979, #18832, #47483, #32380, #17898, #37843, #42656, #33323, #52326, #52631, #47792, #3436, #23051, #23371, #12757, #57475, #8260, #37214, #13392, #52943, #58080, #63230, #56840, #62613, #62295, #42971, #48111, #8878, #37520, #18536, #28492, #4063, #8565, #3749, #38156, #9192, #23682, #52005, #57780, #57161, #27863, #13701, #43281, #33014, #38451, #14010, #7945, #33637, #47179, #22743, #13076, #27548, #53257, #48423, #28805, #4365, #23983, #43587, #3122, #40033, #19786, #30388, #10778, #30064, #29743, #5319, #24938, #35226, #10137, #63546, #829, #45187, #29415, #5963, #9496, #38761, #19466, #39394, #59676, #49047, #19144, #49693, #39711, #53570, #50010, #59350, #15283, #25573, #49374, #34906, #39081, #14328, #29105, #15608, #4671, #58710, #48729, #5637, #58400, #24294, #44544, #44867, #54528, #500, #33949, #20107, #54197, #25250, #10449, #43898, #20436, #54846, #14636, #34252, #59027, #53880, #9806, #4996, #24615, #44221, #187, #14958, #34567, #1153, #60641, #16878, #1469, #31340, #31029, #6593, #46152, #20753, #60321, #11409, #26209, #11090, #60957, #31670, #56450, #12046, #59999, #41619, #45506, #55807, #51306, #7244, #26856, #50655, #21715, #50980, #2414, #15923, #40359, #41309, #11723, #1791, #55171, #45829, #22026, #12372, #27166, #21393, #31986, #35546, #16247, #40997, #30715, #46468, #6285, #50337, #51619, #7553, #16563, #6920, #55495, #25890, #26531, #21071, #36185, #40676, #61270, #36494, #2113, #56123, #17192, #36819, #35868, #47719, #2729, #18759, #42891, #3986, #62539, #52561, #33251, #52871, #8804, #12685, #27787, #3677, #18458, #22979, #62845, #13632, #47100, #52244, #38080, #28419, #33563, #53184, #48035, #47412, #23609, #43202, #38384, #3050, #9116, #58011, #46780, #3363, #13937, #61589, #22348, #22667, #23291, #37449, #41945, #17523, #13317, #37142, #56764, #32298, #51927, #42266, #7868, #27473, #57706, #61906, #17826, #57080, #12998, #32617, #8185, #42581, #62219, #18137, #37765, #57395, #32938, #8494, #28104, #54121, #43512, #34487, #117, #34831, #426, #38687, #24866, #58952, #14879, #29991, #4923, #29032, #48657, #44468, #20031, #39636, #59275, #24542, #19392, #24221, #54456, #19711, #9736, #33874, #53493, #10382, #39012, #23911, #9424, #29340, #34182, #15206, #43828, #44145, #39320, #58641, #14560, #10059, #4294, #48973, #63474, #28724, #29671, #49624, #5561, #54772, #48350, #49303, #53803, #5242, #25173, #44788, #4598, #750, #20360, #39958, #59606, #15538, #35157, #63158, #19068, #58325, #14251, #11014, #6206, #46632, #56615, #25820, #55415, #30956, #49932, #41795, #20685, #59929, #30636, #30311, #35473, #22835, #40603, #32144, #11332, #47269, #5887, #32465, #50581, #42425, #3215, #22516, #22194, #61439, #17365, #27641, #2578, #55090, #56927, #37606, #20998, #62068, #1079, #25494, #50258, #7405, #52097, #60248, #10704, #42111, #51778, #45114, #17981, #7722, #27326, #40291, #36987, #46956, #45434, #15851, #1397, #8036, #16166, #35792, #27012, #61756, #12532, #2903, #17683, #37298, #12847, #63018, #28580, #63320, #28894, #3524, #53344, #23771, #43372, #58492, #33413, #57563, #13488, #9278, #48515, #4454, #24083, #53029, #47879, #52719, #19241, #48200, #38248, #62384, #18306, #38856, #3839, #52419, #37930, #57869, #62700, #43678, #8653, #8969, #4154, #23457, #43062, #18925, #32788, #13790, #28266, #57249, #38539, #14416, #34039, #19562, #13165, #58169, #18625, #14100, #53660, #9594, #33105, #33726, #29202, #48827, #4765, #24392, #43995, #63641, #8351, #27950, #47573, #23134, #42740, #10545, #20534, #34676, #20205, #59451, #14730, #5731, #49146, #24711, #59128, #58799, #280, #50438, #5410, #59773, #39809, #11185, #34348, #60092, #15381, #6379, #30807, #50105, #49785, #25345, #44967, #55267, #30156, #19878, #20848, #1559, #49472, #25985, #29515, #53977, #39492, #35005, #16014, #25027, #39174, #6061, #15700, #9905, #45600, #35319, #54939, #5092, #930, #10865, #15061, #44316, #54295, #35639, #10234, #29840, #44638, #25672, #597, #54621, #40132, #1248, #30481, #45282, #40452, #7645, #21161, #41399, #17609, #35961, #61676, #41083, #41711, #11811, #56851, #37225, #51391, #27249, #60414, #12768, #32391, #16651, #45918, #47192, #61360, #36906, #52016, #31122, #27559, #16339, #7959, #40767, #16971, #55586, #12136, #21485, #56536, #46876, #11506, #50744, #36582, #12457, #60729, #7333, #51067, #26619, #2501, #6688, #36276, #31429, #46237, #26294, #17282, #51705, #1880, #32068, #55899, #7011, #2200, #31758, #2818, #22439, #42034, #21804, #61050, #26944, #56214, #46560, #22119, #43294, #57792, #3760, #57172, #8576, #4377, #58411, #29118, #23383, #14339, #22754, #18228, #47803, #17910, #9203, #8271, #37531, #33960, #9509, #13405, #13711, #57488, #13088, #52953, #32709, #42982, #3134, #48435, #23694, #4074, #18844, #14021, #58090, #23994, #62929, #42352, #38773, #38462, #43598, #33649, #8890, #53268, #28815, #63241, #52337, #62625, #19155, #53581, #18548, #61990, #27874, #3447, #28187, #47494, #23062, #42667, #62306, #37855, #38169, #33026, #52642, #33334, #28503, #48122, #24305, #49387, #19796, #48739, #29754, #44881, #5977, #11103, #4683, #10461, #10147, #34917, #59688, #844, #53892, #30075, #20447, #15621, #20121, #39723, #54540, #20765, #40046, #63559, #49705, #49059, #44233, #59360, #5649, #198, #5332, #24949, #43910, #15295, #58721, #34264, #5007, #19478, #9816, #60012, #14970, #25262, #44555, #40371, #39091, #25586, #511, #15935, #35558, #35238, #54857, #10790, #30400, #1166, #50023, #29427, #45199, #14647, #59040, #55182, #24627, #39404, #34578, #54210, #51631, #41009, #30727, #41629, #51317, #1480, #61601, #7255, #26867, #41958, #21726, #46480, #50666, #25902, #21083, #7565, #16260, #11422, #40688, #17204, #50350, #60333, #60969, #56462, #2426, #56135, #45519, #36505, #2125, #36832, #22038, #35879, #61283, #16889, #12057, #31997, #6931, #31041, #6606, #12384, #27177, #46794, #2740, #26542, #21405, #26220, #22360, #41321, #11733, #55508, #45840, #17536, #60651, #1802, #16574, #31349, #36196, #37154, #55817, #46163, #31681, #6297, #56779, #50992, #33575, #8818, #18473, #62858, #18771, #38397, #42279, #57410, #13644, #28434, #52574, #28736, #43218, #13011, #18150, #48047, #58021, #63170, #19081, #13949, #13330, #53196, #9129, #48362, #32631, #38701, #4306, #12698, #32951, #23925, #27485, #43526, #52259, #33265, #3377, #32311, #51940, #42904, #7882, #47114, #3062, #22680, #8198, #37462, #61919, #52883, #3999, #17839, #57092, #27800, #47425, #22994, #42595, #8507, #62232, #3690, #37778, #23621, #28117, #47734, #23304 ) ),
 .UNSPECIFIED., .F., .F., .F. ) 
 B_SPLINE_SURFACE_WITH_KNOTS ( ( 2, 2 ),
 ( 3, 2, 2, 2, 2, 2, 2, 2, 2, 2, 2, 2, 2, 2, 2, 2, 2, 2, 2, 2, 2, 2, 2, 2, 2, 2, 2, 2, 2, 2, 2, 2, 2, 2, 2, 2, 2, 2, 2, 2, 2, 2, 2, 2, 2, 2, 2, 2, 2, 2, 2, 2, 2, 2, 2, 2, 2, 2, 2, 2, 2, 2, 2, 2, 2, 2, 2, 2, 2, 2, 2, 2, 2, 2, 2, 2, 2, 2, 2, 2, 2, 2, 2, 2, 2, 2, 2, 2, 2, 2, 2, 2, 2, 2, 2, 2, 2, 2, 2, 2, 2, 2, 2, 2, 2, 2, 2, 2, 2, 2, 2, 2, 2, 2, 2, 2, 2, 2, 2, 2, 2, 2, 2, 2, 2, 2, 2, 2, 2, 2, 2, 2, 2, 2, 2, 2, 2, 2, 2, 2, 2, 2, 2, 2, 2, 2, 2, 2, 2, 2, 2, 2, 2, 2, 2, 2, 2, 2, 2, 2, 2, 2, 2, 2, 2, 2, 2, 2, 2, 2, 2, 2, 2, 2, 2, 2, 2, 2, 2, 2, 2, 2, 2, 2, 2, 2, 2, 2, 2, 2, 2, 2, 2, 2, 2, 2, 2, 2, 2, 2, 2, 2, 2, 2, 2, 2, 2, 2, 2, 2, 2, 2, 2, 2, 2, 2, 2, 2, 2, 2, 2, 2, 2, 2, 2, 2, 2, 2, 2, 2, 2, 2, 2, 2, 2, 2, 2, 2, 2, 2, 2, 2, 2, 2, 2, 2, 2, 2, 2, 2, 2, 2, 2, 2, 2, 2, 2, 2, 2, 2, 2, 2, 2, 2, 2, 2, 2, 2, 2, 2, 2, 2, 2, 2, 2, 2, 2, 2, 2, 2, 2, 2, 2, 2, 2, 2, 2, 2, 2, 2, 2, 2, 2, 2, 2, 2, 2, 2, 2, 2, 2, 2, 2, 2, 2, 2, 2, 2, 2, 2, 2, 2, 2, 2, 2, 2, 2, 2, 2, 2, 2, 2, 2, 2, 2, 2, 2, 2, 2, 2, 2, 2, 2, 2, 2, 2, 2, 2, 2, 2, 2, 2, 2, 2, 2, 2, 2, 2, 2, 2, 2, 2, 2, 2, 2, 2, 2, 2, 2, 2, 2, 2, 2, 2, 2, 2, 2, 2, 2, 2, 2, 2, 2, 2, 2, 2, 2, 2, 2, 2, 2, 2, 2, 2, 2, 2, 2, 2, 2, 2, 2, 2, 2, 2, 2, 2, 2, 2, 2, 2, 2, 2, 2, 2, 2, 2, 2, 2, 2, 2, 2, 2, 2, 2, 2, 2, 2, 2, 2, 2, 2, 2, 2, 2, 2, 2, 2, 2, 2, 2, 2, 2, 2, 2, 2, 2, 2, 2, 2, 2, 2, 2, 2, 2, 2, 2, 2, 2, 2, 2, 2, 2, 2, 2, 2, 2, 2, 2, 2, 2, 2, 2, 2, 2, 2, 2, 2, 2, 2, 2, 2, 2, 2, 2, 2, 2, 2, 2, 2, 2, 2, 2, 2, 2, 2, 2, 2, 2, 2, 2, 2, 2, 2, 2, 2, 2, 2, 2, 2, 2, 2, 2, 2, 2, 2, 2, 2, 2, 2, 2, 2, 2, 2, 2, 2, 2, 2, 2, 2, 2, 2, 2, 2, 2, 2, 2, 2, 2, 2, 2, 2, 2, 2, 2, 2, 2, 2, 2, 2, 2, 2, 2, 2, 2, 2, 2, 2, 2, 2, 2, 2, 2, 2, 2, 2, 2, 2, 2, 2, 2, 2, 2, 2, 2, 2, 2, 2, 2, 2, 2, 2, 2, 2, 2, 2, 2, 2, 2, 2, 2, 2, 2, 2, 2, 2, 2, 2, 2, 2, 2, 2, 2, 2, 2, 2, 2, 2, 2, 2, 2, 2, 2, 2, 2, 2, 2, 2, 2, 2, 2, 2, 2, 2, 2, 2, 2, 2, 2, 2, 2, 2, 2, 2, 2, 2, 2, 2, 2, 2, 2, 2, 2, 2, 2, 2, 2, 2, 2, 2, 2, 2, 2, 2, 2, 2, 2, 2, 2, 2, 2, 2, 2, 2, 2, 2, 2, 2, 2, 2, 2, 2, 2, 2, 2, 2, 2, 2, 2, 2, 2, 2, 2, 2, 2, 2, 2, 2, 2, 2, 2, 2, 2, 2, 2, 2, 2, 2, 2, 2, 2, 2, 2, 2, 2, 2, 2, 2, 2, 2, 2, 2, 2, 2, 2, 2, 2, 2, 2, 2, 2, 2, 2, 2, 2, 2, 2, 2, 2, 2, 2, 2, 2, 2, 2, 2, 2, 2, 2, 2, 2, 2, 2, 2, 2, 2, 2, 2, 2, 2, 2, 2, 2, 2, 2, 2, 2, 2, 2, 2, 2, 2, 2, 2, 2, 2, 2, 2, 2, 2, 2, 2, 2, 2, 2, 2, 2, 2, 2, 2, 2, 2, 2, 2, 2, 2, 2, 2, 2, 2, 2, 2, 2, 2, 2, 2, 2, 2, 2, 2, 2, 2, 2, 2, 2, 2, 2, 2, 2, 2, 2, 2, 2, 2, 2, 2, 2, 2, 2, 2, 2, 2, 2, 2, 2, 2, 2, 2, 2, 2, 2, 2, 2, 2, 2, 2, 2, 2, 2, 2, 2, 2, 2, 2, 2, 2, 2, 2, 2, 2, 2, 3 ),
 ( 0.000000000000000000, 1.000000000000000000 ),
 ( 0.000000000000000000, 0.001190476190476190584, 0.002380952380952381167, 0.003571428571428571317, 0.004761904761904762334, 0.005952380952380952051, 0.007142857142857142634, 0.008333333333333333218, 0.009523809523809524669, 0.01071428571428571438, 0.01190476190476190410, 0.01309523809523809555, 0.01428571428571428527, 0.01547619047619047672, 0.01666666666666666644, 0.01785714285714285615, 0.01904761904761904934, 0.02023809523809523905, 0.02142857142857142877, 0.02261904761904761849, 0.02380952380952380820, 0.02500000000000000139, 0.02619047619047619110, 0.02738095238095238082, 0.02857142857142857054, 0.02976190476190476025, 0.03095238095238095344, 0.03214285714285713969, 0.03333333333333333287, 0.03452380952380952606, 0.03571428571428571230, 0.03690476190476190549, 0.03809523809523809867, 0.03928571428571428492, 0.04047619047619047811, 0.04166666666666666435, 0.04285714285714285754, 0.04404761904761905073, 0.04523809523809523697, 0.04642857142857143016, 0.04761904761904761640, 0.04880952380952380959, 0.05000000000000000278, 0.05119047619047618902, 0.05238095238095238221, 0.05357142857142856845, 0.05476190476190476164, 0.05595238095238095483, 0.05714285714285714107, 0.05833333333333333426, 0.05952380952380952051, 0.06071428571428571369, 0.06190476190476190688, 0.06309523809523809312, 0.06428571428571427937, 0.06547619047619047949, 0.06666666666666666574, 0.06785714285714285199, 0.06904761904761905211, 0.07023809523809523836, 0.07142857142857142461, 0.07261904761904762473, 0.07380952380952381098, 0.07499999999999999722, 0.07619047619047619735, 0.07738095238095238360, 0.07857142857142856984, 0.07976190476190475609, 0.08095238095238095621, 0.08214285714285714246, 0.08333333333333332871, 0.08452380952380952883, 0.08571428571428571508, 0.08690476190476190133, 0.08809523809523810145, 0.08928571428571428770, 0.09047619047619047394, 0.09166666666666666019, 0.09285714285714286031, 0.09404761904761904656, 0.09523809523809523281, 0.09642857142857143293, 0.09761904761904761918, 0.09880952380952380543, 0.1000000000000000056, 0.1011904761904761918, 0.1023809523809523780, 0.1035714285714285782, 0.1047619047619047644, 0.1059523809523809507, 0.1071428571428571369, 0.1083333333333333370, 0.1095238095238095233, 0.1107142857142857095, 0.1119047619047619097, 0.1130952380952380959, 0.1142857142857142821, 0.1154761904761904823, 0.1166666666666666685, 0.1178571428571428548, 0.1190476190476190410, 0.1202380952380952411, 0.1214285714285714274, 0.1226190476190476136, 0.1238095238095238138, 0.1250000000000000000, 0.1261904761904761862, 0.1273809523809523725, 0.1285714285714285587, 0.1297619047619047727, 0.1309523809523809590, 0.1321428571428571452, 0.1333333333333333315, 0.1345238095238095177, 0.1357142857142857040, 0.1369047619047619180, 0.1380952380952381042, 0.1392857142857142905, 0.1404761904761904767, 0.1416666666666666630, 0.1428571428571428492, 0.1440476190476190355, 0.1452380952380952495, 0.1464285714285714357, 0.1476190476190476220, 0.1488095238095238082, 0.1499999999999999944, 0.1511904761904761807, 0.1523809523809523947, 0.1535714285714285809, 0.1547619047619047672, 0.1559523809523809534, 0.1571428571428571397, 0.1583333333333333259, 0.1595238095238095122, 0.1607142857142857262, 0.1619047619047619124, 0.1630952380952380987, 0.1642857142857142849, 0.1654761904761904712, 0.1666666666666666574, 0.1678571428571428437, 0.1690476190476190577, 0.1702380952380952439, 0.1714285714285714302, 0.1726190476190476164, 0.1738095238095238027, 0.1749999999999999889, 0.1761904761904762029, 0.1773809523809523891, 0.1785714285714285754, 0.1797619047619047616, 0.1809523809523809479, 0.1821428571428571341, 0.1833333333333333204, 0.1845238095238095344, 0.1857142857142857206, 0.1869047619047619069, 0.1880952380952380931, 0.1892857142857142794, 0.1904761904761904656, 0.1916666666666666796, 0.1928571428571428659, 0.1940476190476190521, 0.1952380952380952384, 0.1964285714285714246, 0.1976190476190476109, 0.1988095238095237971, 0.2000000000000000111, 0.2011904761904761973, 0.2023809523809523836, 0.2035714285714285698, 0.2047619047619047561, 0.2059523809523809423, 0.2071428571428571563, 0.2083333333333333426, 0.2095238095238095288, 0.2107142857142857151, 0.2119047619047619013, 0.2130952380952380876, 0.2142857142857142738, 0.2154761904761904878, 0.2166666666666666741, 0.2178571428571428603, 0.2190476190476190466, 0.2202380952380952328, 0.2214285714285714191, 0.2226190476190476053, 0.2238095238095238193, 0.2250000000000000056, 0.2261904761904761918, 0.2273809523809523780, 0.2285714285714285643, 0.2297619047619047505, 0.2309523809523809645, 0.2321428571428571508, 0.2333333333333333370, 0.2345238095238095233, 0.2357142857142857095, 0.2369047619047618958, 0.2380952380952380820, 0.2392857142857142960, 0.2404761904761904823, 0.2416666666666666685, 0.2428571428571428548, 0.2440476190476190410, 0.2452380952380952273, 0.2464285714285714413, 0.2476190476190476275, 0.2488095238095238138, 0.2500000000000000000, 0.2511904761904761862, 0.2523809523809523725, 0.2535714285714285587, 0.2547619047619047450, 0.2559523809523809312, 0.2571428571428571175, 0.2583333333333333592, 0.2595238095238095455, 0.2607142857142857317, 0.2619047619047619180, 0.2630952380952381042, 0.2642857142857142905, 0.2654761904761904767, 0.2666666666666666630, 0.2678571428571428492, 0.2690476190476190355, 0.2702380952380952217, 0.2714285714285714080, 0.2726190476190475942, 0.2738095238095238360, 0.2750000000000000222, 0.2761904761904762085, 0.2773809523809523947, 0.2785714285714285809, 0.2797619047619047672, 0.2809523809523809534, 0.2821428571428571397, 0.2833333333333333259, 0.2845238095238095122, 0.2857142857142856984, 0.2869047619047618847, 0.2880952380952380709, 0.2892857142857143127, 0.2904761904761904989, 0.2916666666666666852, 0.2928571428571428714, 0.2940476190476190577, 0.2952380952380952439, 0.2964285714285714302, 0.2976190476190476164, 0.2988095238095238027, 0.2999999999999999889, 0.3011904761904761751, 0.3023809523809523614, 0.3035714285714285476, 0.3047619047619047894, 0.3059523809523809756, 0.3071428571428571619, 0.3083333333333333481, 0.3095238095238095344, 0.3107142857142857206, 0.3119047619047619069, 0.3130952380952380931, 0.3142857142857142794, 0.3154761904761904656, 0.3166666666666666519, 0.3178571428571428381, 0.3190476190476190244, 0.3202380952380952106, 0.3214285714285714524, 0.3226190476190476386, 0.3238095238095238249, 0.3250000000000000111, 0.3261904761904761973, 0.3273809523809523836, 0.3285714285714285698, 0.3297619047619047561, 0.3309523809523809423, 0.3321428571428571286, 0.3333333333333333148, 0.3345238095238095011, 0.3357142857142856873, 0.3369047619047619291, 0.3380952380952381153, 0.3392857142857143016, 0.3404761904761904878, 0.3416666666666666741, 0.3428571428571428603, 0.3440476190476190466, 0.3452380952380952328, 0.3464285714285714191, 0.3476190476190476053, 0.3488095238095237915, 0.3499999999999999778, 0.3511904761904761640, 0.3523809523809524058, 0.3535714285714285920, 0.3547619047619047783, 0.3559523809523809645, 0.3571428571428571508, 0.3583333333333333370, 0.3595238095238095233, 0.3607142857142857095, 0.3619047619047618958, 0.3630952380952380820, 0.3642857142857142683, 0.3654761904761904545, 0.3666666666666666408, 0.3678571428571428825, 0.3690476190476190688, 0.3702380952380952550, 0.3714285714285714413, 0.3726190476190476275, 0.3738095238095238138, 0.3750000000000000000, 0.3761904761904761862, 0.3773809523809523725, 0.3785714285714285587, 0.3797619047619047450, 0.3809523809523809312, 0.3821428571428571175, 0.3833333333333333592, 0.3845238095238095455, 0.3857142857142857317, 0.3869047619047619180, 0.3880952380952381042, 0.3892857142857142905, 0.3904761904761904767, 0.3916666666666666630, 0.3928571428571428492, 0.3940476190476190355, 0.3952380952380952217, 0.3964285714285714080, 0.3976190476190475942, 0.3988095238095238360, 0.4000000000000000222, 0.4011904761904762085, 0.4023809523809523947, 0.4035714285714285809, 0.4047619047619047672, 0.4059523809523809534, 0.4071428571428571397, 0.4083333333333333259, 0.4095238095238095122, 0.4107142857142856984, 0.4119047619047618847, 0.4130952380952380709, 0.4142857142857143127, 0.4154761904761904989, 0.4166666666666666852, 0.4178571428571428714, 0.4190476190476190577, 0.4202380952380952439, 0.4214285714285714302, 0.4226190476190476164, 0.4238095238095238027, 0.4249999999999999889, 0.4261904761904761751, 0.4273809523809523614, 0.4285714285714285476, 0.4297619047619047894, 0.4309523809523809756, 0.4321428571428571619, 0.4333333333333333481, 0.4345238095238095344, 0.4357142857142857206, 0.4369047619047619069, 0.4380952380952380931, 0.4392857142857142794, 0.4404761904761904656, 0.4416666666666666519, 0.4428571428571428381, 0.4440476190476190244, 0.4452380952380952106, 0.4464285714285714524, 0.4476190476190476386, 0.4488095238095238249, 0.4500000000000000111, 0.4511904761904761973, 0.4523809523809523836, 0.4535714285714285698, 0.4547619047619047561, 0.4559523809523809423, 0.4571428571428571286, 0.4583333333333333148, 0.4595238095238095011, 0.4607142857142856873, 0.4619047619047619291, 0.4630952380952381153, 0.4642857142857143016, 0.4654761904761904878, 0.4666666666666666741, 0.4678571428571428603, 0.4690476190476190466, 0.4702380952380952328, 0.4714285714285714191, 0.4726190476190476053, 0.4738095238095237915, 0.4749999999999999778, 0.4761904761904761640, 0.4773809523809524058, 0.4785714285714285920, 0.4797619047619047783, 0.4809523809523809645, 0.4821428571428571508, 0.4833333333333333370, 0.4845238095238095233, 0.4857142857142857095, 0.4869047619047618958, 0.4880952380952380820, 0.4892857142857142683, 0.4904761904761904545, 0.4916666666666666408, 0.4928571428571428825, 0.4940476190476190688, 0.4952380952380952550, 0.4964285714285714413, 0.4976190476190476275, 0.4988095238095238138, 0.5000000000000000000, 0.5011904761904761862, 0.5023809523809523725, 0.5035714285714285587, 0.5047619047619047450, 0.5059523809523809312, 0.5071428571428571175, 0.5083333333333333037, 0.5095238095238094900, 0.5107142857142856762, 0.5119047619047618625, 0.5130952380952380487, 0.5142857142857142350, 0.5154761904761904212, 0.5166666666666667185, 0.5178571428571429047, 0.5190476190476190910, 0.5202380952380952772, 0.5214285714285714635, 0.5226190476190476497, 0.5238095238095238360, 0.5250000000000000222, 0.5261904761904762085, 0.5273809523809523947, 0.5285714285714285809, 0.5297619047619047672, 0.5309523809523809534, 0.5321428571428571397, 0.5333333333333333259, 0.5345238095238095122, 0.5357142857142856984, 0.5369047619047618847, 0.5380952380952380709, 0.5392857142857142572, 0.5404761904761904434, 0.5416666666666666297, 0.5428571428571428159, 0.5440476190476190022, 0.5452380952380951884, 0.5464285714285713746, 0.5476190476190476719, 0.5488095238095238582, 0.5500000000000000444, 0.5511904761904762307, 0.5523809523809524169, 0.5535714285714286031, 0.5547619047619047894, 0.5559523809523809756, 0.5571428571428571619, 0.5583333333333333481, 0.5595238095238095344, 0.5607142857142857206, 0.5619047619047619069, 0.5630952380952380931, 0.5642857142857142794, 0.5654761904761904656, 0.5666666666666666519, 0.5678571428571428381, 0.5690476190476190244, 0.5702380952380952106, 0.5714285714285713969, 0.5726190476190475831, 0.5738095238095237693, 0.5749999999999999556, 0.5761904761904761418, 0.5773809523809523281, 0.5785714285714286254, 0.5797619047619048116, 0.5809523809523809978, 0.5821428571428571841, 0.5833333333333333703, 0.5845238095238095566, 0.5857142857142857428, 0.5869047619047619291, 0.5880952380952381153, 0.5892857142857143016, 0.5904761904761904878, 0.5916666666666666741, 0.5928571428571428603, 0.5940476190476190466, 0.5952380952380952328, 0.5964285714285714191, 0.5976190476190476053, 0.5988095238095237915, 0.5999999999999999778, 0.6011904761904761640, 0.6023809523809523503, 0.6035714285714285365, 0.6047619047619047228, 0.6059523809523809090, 0.6071428571428570953, 0.6083333333333332815, 0.6095238095238095788, 0.6107142857142857650, 0.6119047619047619513, 0.6130952380952381375, 0.6142857142857143238, 0.6154761904761905100, 0.6166666666666666963, 0.6178571428571428825, 0.6190476190476190688, 0.6202380952380952550, 0.6214285714285714413, 0.6226190476190476275, 0.6238095238095238138, 0.6250000000000000000, 0.6261904761904761862, 0.6273809523809523725, 0.6285714285714285587, 0.6297619047619047450, 0.6309523809523809312, 0.6321428571428571175, 0.6333333333333333037, 0.6345238095238094900, 0.6357142857142856762, 0.6369047619047618625, 0.6380952380952380487, 0.6392857142857142350, 0.6404761904761904212, 0.6416666666666667185, 0.6428571428571429047, 0.6440476190476190910, 0.6452380952380952772, 0.6464285714285714635, 0.6476190476190476497, 0.6488095238095238360, 0.6500000000000000222, 0.6511904761904762085, 0.6523809523809523947, 0.6535714285714285809, 0.6547619047619047672, 0.6559523809523809534, 0.6571428571428571397, 0.6583333333333333259, 0.6595238095238095122, 0.6607142857142856984, 0.6619047619047618847, 0.6630952380952380709, 0.6642857142857142572, 0.6654761904761904434, 0.6666666666666666297, 0.6678571428571428159, 0.6690476190476190022, 0.6702380952380951884, 0.6714285714285713746, 0.6726190476190476719, 0.6738095238095238582, 0.6750000000000000444, 0.6761904761904762307, 0.6773809523809524169, 0.6785714285714286031, 0.6797619047619047894, 0.6809523809523809756, 0.6821428571428571619, 0.6833333333333333481, 0.6845238095238095344, 0.6857142857142857206, 0.6869047619047619069, 0.6880952380952380931, 0.6892857142857142794, 0.6904761904761904656, 0.6916666666666666519, 0.6928571428571428381, 0.6940476190476190244, 0.6952380952380952106, 0.6964285714285713969, 0.6976190476190475831, 0.6988095238095237693, 0.6999999999999999556, 0.7011904761904761418, 0.7023809523809523281, 0.7035714285714286254, 0.7047619047619048116, 0.7059523809523809978, 0.7071428571428571841, 0.7083333333333333703, 0.7095238095238095566, 0.7107142857142857428, 0.7119047619047619291, 0.7130952380952381153, 0.7142857142857143016, 0.7154761904761904878, 0.7166666666666666741, 0.7178571428571428603, 0.7190476190476190466, 0.7202380952380952328, 0.7214285714285714191, 0.7226190476190476053, 0.7238095238095237915, 0.7249999999999999778, 0.7261904761904761640, 0.7273809523809523503, 0.7285714285714285365, 0.7297619047619047228, 0.7309523809523809090, 0.7321428571428570953, 0.7333333333333332815, 0.7345238095238095788, 0.7357142857142857650, 0.7369047619047619513, 0.7380952380952381375, 0.7392857142857143238, 0.7404761904761905100, 0.7416666666666666963, 0.7428571428571428825, 0.7440476190476190688, 0.7452380952380952550, 0.7464285714285714413, 0.7476190476190476275, 0.7488095238095238138, 0.7500000000000000000, 0.7511904761904761862, 0.7523809523809523725, 0.7535714285714285587, 0.7547619047619047450, 0.7559523809523809312, 0.7571428571428571175, 0.7583333333333333037, 0.7595238095238094900, 0.7607142857142856762, 0.7619047619047618625, 0.7630952380952380487, 0.7642857142857142350, 0.7654761904761904212, 0.7666666666666667185, 0.7678571428571429047, 0.7690476190476190910, 0.7702380952380952772, 0.7714285714285714635, 0.7726190476190476497, 0.7738095238095238360, 0.7750000000000000222, 0.7761904761904762085, 0.7773809523809523947, 0.7785714285714285809, 0.7797619047619047672, 0.7809523809523809534, 0.7821428571428571397, 0.7833333333333333259, 0.7845238095238095122, 0.7857142857142856984, 0.7869047619047618847, 0.7880952380952380709, 0.7892857142857142572, 0.7904761904761904434, 0.7916666666666666297, 0.7928571428571428159, 0.7940476190476190022, 0.7952380952380951884, 0.7964285714285713746, 0.7976190476190476719, 0.7988095238095238582, 0.8000000000000000444, 0.8011904761904762307, 0.8023809523809524169, 0.8035714285714286031, 0.8047619047619047894, 0.8059523809523809756, 0.8071428571428571619, 0.8083333333333333481, 0.8095238095238095344, 0.8107142857142857206, 0.8119047619047619069, 0.8130952380952380931, 0.8142857142857142794, 0.8154761904761904656, 0.8166666666666666519, 0.8178571428571428381, 0.8190476190476190244, 0.8202380952380952106, 0.8214285714285713969, 0.8226190476190475831, 0.8238095238095237693, 0.8249999999999999556, 0.8261904761904761418, 0.8273809523809523281, 0.8285714285714286254, 0.8297619047619048116, 0.8309523809523809978, 0.8321428571428571841, 0.8333333333333333703, 0.8345238095238095566, 0.8357142857142857428, 0.8369047619047619291, 0.8380952380952381153, 0.8392857142857143016, 0.8404761904761904878, 0.8416666666666666741, 0.8428571428571428603, 0.8440476190476190466, 0.8452380952380952328, 0.8464285714285714191, 0.8476190476190476053, 0.8488095238095237915, 0.8499999999999999778, 0.8511904761904761640, 0.8523809523809523503, 0.8535714285714285365, 0.8547619047619047228, 0.8559523809523809090, 0.8571428571428570953, 0.8583333333333332815, 0.8595238095238095788, 0.8607142857142857650, 0.8619047619047619513, 0.8630952380952381375, 0.8642857142857143238, 0.8654761904761905100, 0.8666666666666666963, 0.8678571428571428825, 0.8690476190476190688, 0.8702380952380952550, 0.8714285714285714413, 0.8726190476190476275, 0.8738095238095238138, 0.8750000000000000000, 0.8761904761904761862, 0.8773809523809523725, 0.8785714285714285587, 0.8797619047619047450, 0.8809523809523809312, 0.8821428571428571175, 0.8833333333333333037, 0.8845238095238094900, 0.8857142857142856762, 0.8869047619047618625, 0.8880952380952380487, 0.8892857142857142350, 0.8904761904761904212, 0.8916666666666667185, 0.8928571428571429047, 0.8940476190476190910, 0.8952380952380952772, 0.8964285714285714635, 0.8976190476190476497, 0.8988095238095238360, 0.9000000000000000222, 0.9011904761904762085, 0.9023809523809523947, 0.9035714285714285809, 0.9047619047619047672, 0.9059523809523809534, 0.9071428571428571397, 0.9083333333333333259, 0.9095238095238095122, 0.9107142857142856984, 0.9119047619047618847, 0.9130952380952380709, 0.9142857142857142572, 0.9154761904761904434, 0.9166666666666666297, 0.9178571428571428159, 0.9190476190476190022, 0.9202380952380951884, 0.9214285714285713746, 0.9226190476190476719, 0.9238095238095238582, 0.9250000000000000444, 0.9261904761904762307, 0.9273809523809524169, 0.9285714285714286031, 0.9297619047619047894, 0.9309523809523809756, 0.9321428571428571619, 0.9333333333333333481, 0.9345238095238095344, 0.9357142857142857206, 0.9369047619047619069, 0.9380952380952380931, 0.9392857142857142794, 0.9404761904761904656, 0.9416666666666666519, 0.9428571428571428381, 0.9440476190476190244, 0.9452380952380952106, 0.9464285714285713969, 0.9476190476190475831, 0.9488095238095237693, 0.9499999999999999556, 0.9511904761904761418, 0.9523809523809523281, 0.9535714285714286254, 0.9547619047619048116, 0.9559523809523809978, 0.9571428571428571841, 0.9583333333333333703, 0.9595238095238095566, 0.9607142857142857428, 0.9619047619047619291, 0.9630952380952381153, 0.9642857142857143016, 0.9654761904761904878, 0.9666666666666666741, 0.9678571428571428603, 0.9690476190476190466, 0.9702380952380952328, 0.9714285714285714191, 0.9726190476190476053, 0.9738095238095237915, 0.9749999999999999778, 0.9761904761904761640, 0.9773809523809523503, 0.9785714285714285365, 0.9797619047619047228, 0.9809523809523809090, 0.9821428571428570953, 0.9833333333333332815, 0.9845238095238095788, 0.9857142857142857650, 0.9869047619047619513, 0.9880952380952381375, 0.9892857142857143238, 0.9904761904761905100, 0.9916666666666666963, 0.9928571428571428825, 0.9940476190476190688, 0.9952380952380952550, 0.9964285714285714413, 0.9976190476190476275, 0.9988095238095238138, 1.000000000000000000 ),
 .UNSPECIFIED. ) 
 GEOMETRIC_REPRESENTATION_ITEM ( )  RATIONAL_B_SPLINE_SURFACE ( (
 ( 1.000000000000000000, 0.8660254037844387076, 1.000000000000000000, 0.8660254037844387076, 1.000000000000000000, 0.8660254037844387076, 1.000000000000000000, 0.8660254037844387076, 1.000000000000000000, 0.8660254037844387076, 1.000000000000000000, 0.8660254037844387076, 1.000000000000000000, 0.8660254037844387076, 1.000000000000000000, 0.8660254037844387076, 1.000000000000000000, 0.8660254037844387076, 1.000000000000000000, 0.8660254037844387076, 1.000000000000000000, 0.8660254037844387076, 1.000000000000000000, 0.8660254037844387076, 1.000000000000000000, 0.8660254037844387076, 1.000000000000000000, 0.8660254037844387076, 1.000000000000000000, 0.8660254037844387076, 1.000000000000000000, 0.8660254037844387076, 1.000000000000000000, 0.8660254037844387076, 1.000000000000000000, 0.8660254037844387076, 1.000000000000000000, 0.8660254037844387076, 1.000000000000000000, 0.8660254037844387076, 1.000000000000000000, 0.8660254037844387076, 1.000000000000000000, 0.8660254037844387076, 1.000000000000000000, 0.8660254037844387076, 1.000000000000000000, 0.8660254037844387076, 1.000000000000000000, 0.8660254037844387076, 1.000000000000000000, 0.8660254037844387076, 1.000000000000000000, 0.8660254037844387076, 1.000000000000000000, 0.8660254037844387076, 1.000000000000000000, 0.8660254037844387076, 1.000000000000000000, 0.8660254037844387076, 1.000000000000000000, 0.8660254037844387076, 1.000000000000000000, 0.8660254037844387076, 1.000000000000000000, 0.8660254037844387076, 1.000000000000000000, 0.8660254037844387076, 1.000000000000000000, 0.8660254037844387076, 1.000000000000000000, 0.8660254037844387076, 1.000000000000000000, 0.8660254037844387076, 1.000000000000000000, 0.8660254037844387076, 1.000000000000000000, 0.8660254037844387076, 1.000000000000000000, 0.8660254037844387076, 1.000000000000000000, 0.8660254037844387076, 1.000000000000000000, 0.8660254037844387076, 1.000000000000000000, 0.8660254037844387076, 1.000000000000000000, 0.8660254037844387076, 1.000000000000000000, 0.8660254037844387076, 1.000000000000000000, 0.8660254037844387076, 1.000000000000000000, 0.8660254037844387076, 1.000000000000000000, 0.8660254037844387076, 1.000000000000000000, 0.8660254037844387076, 1.000000000000000000, 0.8660254037844387076, 1.000000000000000000, 0.8660254037844387076, 1.000000000000000000, 0.8660254037844387076, 1.000000000000000000, 0.8660254037844387076, 1.000000000000000000, 0.8660254037844387076, 1.000000000000000000, 0.8660254037844387076, 1.000000000000000000, 0.8660254037844387076, 1.000000000000000000, 0.8660254037844387076, 1.000000000000000000, 0.8660254037844387076, 1.000000000000000000, 0.8660254037844387076, 1.000000000000000000, 0.8660254037844387076, 1.000000000000000000, 0.8660254037844387076, 1.000000000000000000, 0.8660254037844387076, 1.000000000000000000, 0.8660254037844387076, 1.000000000000000000, 0.8660254037844387076, 1.000000000000000000, 0.8660254037844387076, 1.000000000000000000, 0.8660254037844387076, 1.000000000000000000, 0.8660254037844387076, 1.000000000000000000, 0.8660254037844387076, 1.000000000000000000, 0.8660254037844387076, 1.000000000000000000, 0.8660254037844387076, 1.000000000000000000, 0.8660254037844387076, 1.000000000000000000, 0.8660254037844387076, 1.000000000000000000, 0.8660254037844387076, 1.000000000000000000, 0.8660254037844387076, 1.000000000000000000, 0.8660254037844387076, 1.000000000000000000, 0.8660254037844387076, 1.000000000000000000, 0.8660254037844387076, 1.000000000000000000, 0.8660254037844387076, 1.000000000000000000, 0.8660254037844387076, 1.000000000000000000, 0.8660254037844387076, 1.000000000000000000, 0.8660254037844387076, 1.000000000000000000, 0.8660254037844387076, 1.000000000000000000, 0.8660254037844387076, 1.000000000000000000, 0.8660254037844387076, 1.000000000000000000, 0.8660254037844387076, 1.000000000000000000, 0.8660254037844387076, 1.000000000000000000, 0.8660254037844387076, 1.000000000000000000, 0.8660254037844387076, 1.000000000000000000, 0.8660254037844387076, 1.000000000000000000, 0.8660254037844387076, 1.000000000000000000, 0.8660254037844387076, 1.000000000000000000, 0.8660254037844387076, 1.000000000000000000, 0.8660254037844387076, 1.000000000000000000, 0.8660254037844387076, 1.000000000000000000, 0.8660254037844387076, 1.000000000000000000, 0.8660254037844387076, 1.000000000000000000, 0.8660254037844387076, 1.000000000000000000, 0.8660254037844387076, 1.000000000000000000, 0.8660254037844387076, 1.000000000000000000, 0.8660254037844387076, 1.000000000000000000, 0.8660254037844387076, 1.000000000000000000, 0.8660254037844387076, 1.000000000000000000, 0.8660254037844387076, 1.000000000000000000, 0.8660254037844387076, 1.000000000000000000, 0.8660254037844387076, 1.000000000000000000, 0.8660254037844387076, 1.000000000000000000, 0.8660254037844387076, 1.000000000000000000, 0.8660254037844387076, 1.000000000000000000, 0.8660254037844387076, 1.000000000000000000, 0.8660254037844387076, 1.000000000000000000, 0.8660254037844387076, 1.000000000000000000, 0.8660254037844387076, 1.000000000000000000, 0.8660254037844387076, 1.000000000000000000, 0.8660254037844387076, 1.000000000000000000, 0.8660254037844387076, 1.000000000000000000, 0.8660254037844387076, 1.000000000000000000, 0.8660254037844387076, 1.000000000000000000, 0.8660254037844387076, 1.000000000000000000, 0.8660254037844387076, 1.000000000000000000, 0.8660254037844387076, 1.000000000000000000, 0.8660254037844387076, 1.000000000000000000, 0.8660254037844387076, 1.000000000000000000, 0.8660254037844387076, 1.000000000000000000, 0.8660254037844387076, 1.000000000000000000, 0.8660254037844387076, 1.000000000000000000, 0.8660254037844387076, 1.000000000000000000, 0.8660254037844387076, 1.000000000000000000, 0.8660254037844387076, 1.000000000000000000, 0.8660254037844387076, 1.000000000000000000, 0.8660254037844387076, 1.000000000000000000, 0.8660254037844387076, 1.000000000000000000, 0.8660254037844387076, 1.000000000000000000, 0.8660254037844387076, 1.000000000000000000, 0.8660254037844387076, 1.000000000000000000, 0.8660254037844387076, 1.000000000000000000, 0.8660254037844387076, 1.000000000000000000, 0.8660254037844387076, 1.000000000000000000, 0.8660254037844387076, 1.000000000000000000, 0.8660254037844387076, 1.000000000000000000, 0.8660254037844387076, 1.000000000000000000, 0.8660254037844387076, 1.000000000000000000, 0.8660254037844387076, 1.000000000000000000, 0.8660254037844387076, 1.000000000000000000, 0.8660254037844387076, 1.000000000000000000, 0.8660254037844387076, 1.000000000000000000, 0.8660254037844387076, 1.000000000000000000, 0.8660254037844387076, 1.000000000000000000, 0.8660254037844387076, 1.000000000000000000, 0.8660254037844387076, 1.000000000000000000, 0.8660254037844387076, 1.000000000000000000, 0.8660254037844387076, 1.000000000000000000, 0.8660254037844387076, 1.000000000000000000, 0.8660254037844387076, 1.000000000000000000, 0.8660254037844387076, 1.000000000000000000, 0.8660254037844387076, 1.000000000000000000, 0.8660254037844387076, 1.000000000000000000, 0.8660254037844387076, 1.000000000000000000, 0.8660254037844387076, 1.000000000000000000, 0.8660254037844387076, 1.000000000000000000, 0.8660254037844387076, 1.000000000000000000, 0.8660254037844387076, 1.000000000000000000, 0.8660254037844387076, 1.000000000000000000, 0.8660254037844387076, 1.000000000000000000, 0.8660254037844387076, 1.000000000000000000, 0.8660254037844387076, 1.000000000000000000, 0.8660254037844387076, 1.000000000000000000, 0.8660254037844387076, 1.000000000000000000, 0.8660254037844387076, 1.000000000000000000, 0.8660254037844387076, 1.000000000000000000, 0.8660254037844387076, 1.000000000000000000, 0.8660254037844387076, 1.000000000000000000, 0.8660254037844387076, 1.000000000000000000, 0.8660254037844387076, 1.000000000000000000, 0.8660254037844387076, 1.000000000000000000, 0.8660254037844387076, 1.000000000000000000, 0.8660254037844387076, 1.000000000000000000, 0.8660254037844387076, 1.000000000000000000, 0.8660254037844387076, 1.000000000000000000, 0.8660254037844387076, 1.000000000000000000, 0.8660254037844387076, 1.000000000000000000, 0.8660254037844387076, 1.000000000000000000, 0.8660254037844387076, 1.000000000000000000, 0.8660254037844387076, 1.000000000000000000, 0.8660254037844387076, 1.000000000000000000, 0.8660254037844387076, 1.000000000000000000, 0.8660254037844387076, 1.000000000000000000, 0.8660254037844387076, 1.000000000000000000, 0.8660254037844387076, 1.000000000000000000, 0.8660254037844387076, 1.000000000000000000, 0.8660254037844387076, 1.000000000000000000, 0.8660254037844387076, 1.000000000000000000, 0.8660254037844387076, 1.000000000000000000, 0.8660254037844387076, 1.000000000000000000, 0.8660254037844387076, 1.000000000000000000, 0.8660254037844387076, 1.000000000000000000, 0.8660254037844387076, 1.000000000000000000, 0.8660254037844387076, 1.000000000000000000, 0.8660254037844387076, 1.000000000000000000, 0.8660254037844387076, 1.000000000000000000, 0.8660254037844387076, 1.000000000000000000, 0.8660254037844387076, 1.000000000000000000, 0.8660254037844387076, 1.000000000000000000, 0.8660254037844387076, 1.000000000000000000, 0.8660254037844387076, 1.000000000000000000, 0.8660254037844387076, 1.000000000000000000, 0.8660254037844387076, 1.000000000000000000, 0.8660254037844387076, 1.000000000000000000, 0.8660254037844387076, 1.000000000000000000, 0.8660254037844387076, 1.000000000000000000, 0.8660254037844387076, 1.000000000000000000, 0.8660254037844387076, 1.000000000000000000, 0.8660254037844387076, 1.000000000000000000, 0.8660254037844387076, 1.000000000000000000, 0.8660254037844387076, 1.000000000000000000, 0.8660254037844387076, 1.000000000000000000, 0.8660254037844387076, 1.000000000000000000, 0.8660254037844387076, 1.000000000000000000, 0.8660254037844387076, 1.000000000000000000, 0.8660254037844387076, 1.000000000000000000, 0.8660254037844387076, 1.000000000000000000, 0.8660254037844387076, 1.000000000000000000, 0.8660254037844387076, 1.000000000000000000, 0.8660254037844387076, 1.000000000000000000, 0.8660254037844387076, 1.000000000000000000, 0.8660254037844387076, 1.000000000000000000, 0.8660254037844387076, 1.000000000000000000, 0.8660254037844387076, 1.000000000000000000, 0.8660254037844387076, 1.000000000000000000, 0.8660254037844387076, 1.000000000000000000, 0.8660254037844387076, 1.000000000000000000, 0.8660254037844387076, 1.000000000000000000, 0.8660254037844387076, 1.000000000000000000, 0.8660254037844387076, 1.000000000000000000, 0.8660254037844387076, 1.000000000000000000, 0.8660254037844387076, 1.000000000000000000, 0.8660254037844387076, 1.000000000000000000, 0.8660254037844387076, 1.000000000000000000, 0.8660254037844387076, 1.000000000000000000, 0.8660254037844387076, 1.000000000000000000, 0.8660254037844387076, 1.000000000000000000, 0.8660254037844387076, 1.000000000000000000, 0.8660254037844387076, 1.000000000000000000, 0.8660254037844387076, 1.000000000000000000, 0.8660254037844387076, 1.000000000000000000, 0.8660254037844387076, 1.000000000000000000, 0.8660254037844387076, 1.000000000000000000, 0.8660254037844387076, 1.000000000000000000, 0.8660254037844387076, 1.000000000000000000, 0.8660254037844387076, 1.000000000000000000, 0.8660254037844387076, 1.000000000000000000, 0.8660254037844387076, 1.000000000000000000, 0.8660254037844387076, 1.000000000000000000, 0.8660254037844387076, 1.000000000000000000, 0.8660254037844387076, 1.000000000000000000, 0.8660254037844387076, 1.000000000000000000, 0.8660254037844387076, 1.000000000000000000, 0.8660254037844387076, 1.000000000000000000, 0.8660254037844387076, 1.000000000000000000, 0.8660254037844387076, 1.000000000000000000, 0.8660254037844387076, 1.000000000000000000, 0.8660254037844387076, 1.000000000000000000, 0.8660254037844387076, 1.000000000000000000, 0.8660254037844387076, 1.000000000000000000, 0.8660254037844387076, 1.000000000000000000, 0.8660254037844387076, 1.000000000000000000, 0.8660254037844387076, 1.000000000000000000, 0.8660254037844387076, 1.000000000000000000, 0.8660254037844387076, 1.000000000000000000, 0.8660254037844387076, 1.000000000000000000, 0.8660254037844387076, 1.000000000000000000, 0.8660254037844387076, 1.000000000000000000, 0.8660254037844387076, 1.000000000000000000, 0.8660254037844387076, 1.000000000000000000, 0.8660254037844387076, 1.000000000000000000, 0.8660254037844387076, 1.000000000000000000, 0.8660254037844387076, 1.000000000000000000, 0.8660254037844387076, 1.000000000000000000, 0.8660254037844387076, 1.000000000000000000, 0.8660254037844387076, 1.000000000000000000, 0.8660254037844387076, 1.000000000000000000, 0.8660254037844387076, 1.000000000000000000, 0.8660254037844387076, 1.000000000000000000, 0.8660254037844387076, 1.000000000000000000, 0.8660254037844387076, 1.000000000000000000, 0.8660254037844387076, 1.000000000000000000, 0.8660254037844387076, 1.000000000000000000, 0.8660254037844387076, 1.000000000000000000, 0.8660254037844387076, 1.000000000000000000, 0.8660254037844387076, 1.000000000000000000, 0.8660254037844387076, 1.000000000000000000, 0.8660254037844387076, 1.000000000000000000, 0.8660254037844387076, 1.000000000000000000, 0.8660254037844387076, 1.000000000000000000, 0.8660254037844387076, 1.000000000000000000, 0.8660254037844387076, 1.000000000000000000, 0.8660254037844387076, 1.000000000000000000, 0.8660254037844387076, 1.000000000000000000, 0.8660254037844387076, 1.000000000000000000, 0.8660254037844387076, 1.000000000000000000, 0.8660254037844387076, 1.000000000000000000, 0.8660254037844387076, 1.000000000000000000, 0.8660254037844387076, 1.000000000000000000, 0.8660254037844387076, 1.000000000000000000, 0.8660254037844387076, 1.000000000000000000, 0.8660254037844387076, 1.000000000000000000, 0.8660254037844387076, 1.000000000000000000, 0.8660254037844387076, 1.000000000000000000, 0.8660254037844387076, 1.000000000000000000, 0.8660254037844387076, 1.000000000000000000, 0.8660254037844387076, 1.000000000000000000, 0.8660254037844387076, 1.000000000000000000, 0.8660254037844387076, 1.000000000000000000, 0.8660254037844387076, 1.000000000000000000, 0.8660254037844387076, 1.000000000000000000, 0.8660254037844387076, 1.000000000000000000, 0.8660254037844387076, 1.000000000000000000, 0.8660254037844387076, 1.000000000000000000, 0.8660254037844387076, 1.000000000000000000, 0.8660254037844387076, 1.000000000000000000, 0.8660254037844387076, 1.000000000000000000, 0.8660254037844387076, 1.000000000000000000, 0.8660254037844387076, 1.000000000000000000, 0.8660254037844387076, 1.000000000000000000, 0.8660254037844387076, 1.000000000000000000, 0.8660254037844387076, 1.000000000000000000, 0.8660254037844387076, 1.000000000000000000, 0.8660254037844387076, 1.000000000000000000, 0.8660254037844387076, 1.000000000000000000, 0.8660254037844387076, 1.000000000000000000, 0.8660254037844387076, 1.000000000000000000, 0.8660254037844387076, 1.000000000000000000, 0.8660254037844387076, 1.000000000000000000, 0.8660254037844387076, 1.000000000000000000, 0.8660254037844387076, 1.000000000000000000, 0.8660254037844387076, 1.000000000000000000, 0.8660254037844387076, 1.000000000000000000, 0.8660254037844387076, 1.000000000000000000, 0.8660254037844387076, 1.000000000000000000, 0.8660254037844387076, 1.000000000000000000, 0.8660254037844387076, 1.000000000000000000, 0.8660254037844387076, 1.000000000000000000, 0.8660254037844387076, 1.000000000000000000, 0.8660254037844387076, 1.000000000000000000, 0.8660254037844387076, 1.000000000000000000, 0.8660254037844387076, 1.000000000000000000, 0.8660254037844387076, 1.000000000000000000, 0.8660254037844387076, 1.000000000000000000, 0.8660254037844387076, 1.000000000000000000, 0.8660254037844387076, 1.000000000000000000, 0.8660254037844387076, 1.000000000000000000, 0.8660254037844387076, 1.000000000000000000, 0.8660254037844387076, 1.000000000000000000, 0.8660254037844387076, 1.000000000000000000, 0.8660254037844387076, 1.000000000000000000, 0.8660254037844387076, 1.000000000000000000, 0.8660254037844387076, 1.000000000000000000, 0.8660254037844387076, 1.000000000000000000, 0.8660254037844387076, 1.000000000000000000, 0.8660254037844387076, 1.000000000000000000, 0.8660254037844387076, 1.000000000000000000, 0.8660254037844387076, 1.000000000000000000, 0.8660254037844387076, 1.000000000000000000, 0.8660254037844387076, 1.000000000000000000, 0.8660254037844387076, 1.000000000000000000, 0.8660254037844387076, 1.000000000000000000, 0.8660254037844387076, 1.000000000000000000, 0.8660254037844387076, 1.000000000000000000, 0.8660254037844387076, 1.000000000000000000, 0.8660254037844387076, 1.000000000000000000, 0.8660254037844387076, 1.000000000000000000, 0.8660254037844387076, 1.000000000000000000, 0.8660254037844387076, 1.000000000000000000, 0.8660254037844387076, 1.000000000000000000, 0.8660254037844387076, 1.000000000000000000, 0.8660254037844387076, 1.000000000000000000, 0.8660254037844387076, 1.000000000000000000, 0.8660254037844387076, 1.000000000000000000, 0.8660254037844387076, 1.000000000000000000, 0.8660254037844387076, 1.000000000000000000, 0.8660254037844387076, 1.000000000000000000, 0.8660254037844387076, 1.000000000000000000, 0.8660254037844387076, 1.000000000000000000, 0.8660254037844387076, 1.000000000000000000, 0.8660254037844387076, 1.000000000000000000, 0.8660254037844387076, 1.000000000000000000, 0.8660254037844387076, 1.000000000000000000, 0.8660254037844387076, 1.000000000000000000, 0.8660254037844387076, 1.000000000000000000, 0.8660254037844387076, 1.000000000000000000, 0.8660254037844387076, 1.000000000000000000, 0.8660254037844387076, 1.000000000000000000, 0.8660254037844387076, 1.000000000000000000, 0.8660254037844387076, 1.000000000000000000, 0.8660254037844387076, 1.000000000000000000, 0.8660254037844387076, 1.000000000000000000, 0.8660254037844387076, 1.000000000000000000, 0.8660254037844387076, 1.000000000000000000, 0.8660254037844387076, 1.000000000000000000, 0.8660254037844387076, 1.000000000000000000, 0.8660254037844387076, 1.000000000000000000, 0.8660254037844387076, 1.000000000000000000, 0.8660254037844387076, 1.000000000000000000, 0.8660254037844387076, 1.000000000000000000, 0.8660254037844387076, 1.000000000000000000, 0.8660254037844387076, 1.000000000000000000, 0.8660254037844387076, 1.000000000000000000, 0.8660254037844387076, 1.000000000000000000, 0.8660254037844387076, 1.000000000000000000, 0.8660254037844387076, 1.000000000000000000, 0.8660254037844387076, 1.000000000000000000, 0.8660254037844387076, 1.000000000000000000, 0.8660254037844387076, 1.000000000000000000, 0.8660254037844387076, 1.000000000000000000, 0.8660254037844387076, 1.000000000000000000, 0.8660254037844387076, 1.000000000000000000, 0.8660254037844387076, 1.000000000000000000, 0.8660254037844387076, 1.000000000000000000, 0.8660254037844387076, 1.000000000000000000, 0.8660254037844387076, 1.000000000000000000, 0.8660254037844387076, 1.000000000000000000, 0.8660254037844387076, 1.000000000000000000, 0.8660254037844387076, 1.000000000000000000, 0.8660254037844387076, 1.000000000000000000, 0.8660254037844387076, 1.000000000000000000, 0.8660254037844387076, 1.000000000000000000, 0.8660254037844387076, 1.000000000000000000, 0.8660254037844387076, 1.000000000000000000, 0.8660254037844387076, 1.000000000000000000, 0.8660254037844387076, 1.000000000000000000, 0.8660254037844387076, 1.000000000000000000, 0.8660254037844387076, 1.000000000000000000, 0.8660254037844387076, 1.000000000000000000, 0.8660254037844387076, 1.000000000000000000, 0.8660254037844387076, 1.000000000000000000, 0.8660254037844387076, 1.000000000000000000, 0.8660254037844387076, 1.000000000000000000, 0.8660254037844387076, 1.000000000000000000, 0.8660254037844387076, 1.000000000000000000, 0.8660254037844387076, 1.000000000000000000, 0.8660254037844387076, 1.000000000000000000, 0.8660254037844387076, 1.000000000000000000, 0.8660254037844387076, 1.000000000000000000, 0.8660254037844387076, 1.000000000000000000, 0.8660254037844387076, 1.000000000000000000, 0.8660254037844387076, 1.000000000000000000, 0.8660254037844387076, 1.000000000000000000, 0.8660254037844387076, 1.000000000000000000, 0.8660254037844387076, 1.000000000000000000, 0.8660254037844387076, 1.000000000000000000, 0.8660254037844387076, 1.000000000000000000, 0.8660254037844387076, 1.000000000000000000, 0.8660254037844387076, 1.000000000000000000, 0.8660254037844387076, 1.000000000000000000, 0.8660254037844387076, 1.000000000000000000, 0.8660254037844387076, 1.000000000000000000, 0.8660254037844387076, 1.000000000000000000, 0.8660254037844387076, 1.000000000000000000, 0.8660254037844387076, 1.000000000000000000, 0.8660254037844387076, 1.000000000000000000, 0.8660254037844387076, 1.000000000000000000, 0.8660254037844387076, 1.000000000000000000, 0.8660254037844387076, 1.000000000000000000, 0.8660254037844387076, 1.000000000000000000, 0.8660254037844387076, 1.000000000000000000, 0.8660254037844387076, 1.000000000000000000, 0.8660254037844387076, 1.000000000000000000, 0.8660254037844387076, 1.000000000000000000, 0.8660254037844387076, 1.000000000000000000, 0.8660254037844387076, 1.000000000000000000, 0.8660254037844387076, 1.000000000000000000, 0.8660254037844387076, 1.000000000000000000, 0.8660254037844387076, 1.000000000000000000, 0.8660254037844387076, 1.000000000000000000, 0.8660254037844387076, 1.000000000000000000, 0.8660254037844387076, 1.000000000000000000, 0.8660254037844387076, 1.000000000000000000, 0.8660254037844387076, 1.000000000000000000, 0.8660254037844387076, 1.000000000000000000, 0.8660254037844387076, 1.000000000000000000, 0.8660254037844387076, 1.000000000000000000, 0.8660254037844387076, 1.000000000000000000, 0.8660254037844387076, 1.000000000000000000, 0.8660254037844387076, 1.000000000000000000, 0.8660254037844387076, 1.000000000000000000, 0.8660254037844387076, 1.000000000000000000, 0.8660254037844387076, 1.000000000000000000, 0.8660254037844387076, 1.000000000000000000, 0.8660254037844387076, 1.000000000000000000, 0.8660254037844387076, 1.000000000000000000, 0.8660254037844387076, 1.000000000000000000, 0.8660254037844387076, 1.000000000000000000, 0.8660254037844387076, 1.000000000000000000, 0.8660254037844387076, 1.000000000000000000, 0.8660254037844387076, 1.000000000000000000, 0.8660254037844387076, 1.000000000000000000, 0.8660254037844387076, 1.000000000000000000, 0.8660254037844387076, 1.000000000000000000, 0.8660254037844387076, 1.000000000000000000, 0.8660254037844387076, 1.000000000000000000, 0.8660254037844387076, 1.000000000000000000, 0.8660254037844387076, 1.000000000000000000, 0.8660254037844387076, 1.000000000000000000, 0.8660254037844387076, 1.000000000000000000, 0.8660254037844387076, 1.000000000000000000, 0.8660254037844387076, 1.000000000000000000, 0.8660254037844387076, 1.000000000000000000, 0.8660254037844387076, 1.000000000000000000, 0.8660254037844387076, 1.000000000000000000, 0.8660254037844387076, 1.000000000000000000, 0.8660254037844387076, 1.000000000000000000, 0.8660254037844387076, 1.000000000000000000, 0.8660254037844387076, 1.000000000000000000, 0.8660254037844387076, 1.000000000000000000, 0.8660254037844387076, 1.000000000000000000, 0.8660254037844387076, 1.000000000000000000, 0.8660254037844387076, 1.000000000000000000, 0.8660254037844387076, 1.000000000000000000, 0.8660254037844387076, 1.000000000000000000, 0.8660254037844387076, 1.000000000000000000, 0.8660254037844387076, 1.000000000000000000, 0.8660254037844387076, 1.000000000000000000, 0.8660254037844387076, 1.000000000000000000, 0.8660254037844387076, 1.000000000000000000, 0.8660254037844387076, 1.000000000000000000, 0.8660254037844387076, 1.000000000000000000, 0.8660254037844387076, 1.000000000000000000, 0.8660254037844387076, 1.000000000000000000, 0.8660254037844387076, 1.000000000000000000, 0.8660254037844387076, 1.000000000000000000, 0.8660254037844387076, 1.000000000000000000, 0.8660254037844387076, 1.000000000000000000, 0.8660254037844387076, 1.000000000000000000, 0.8660254037844387076, 1.000000000000000000, 0.8660254037844387076, 1.000000000000000000, 0.8660254037844387076, 1.000000000000000000, 0.8660254037844387076, 1.000000000000000000, 0.8660254037844387076, 1.000000000000000000, 0.8660254037844387076, 1.000000000000000000, 0.8660254037844387076, 1.000000000000000000, 0.8660254037844387076, 1.000000000000000000, 0.8660254037844387076, 1.000000000000000000, 0.8660254037844387076, 1.000000000000000000, 0.8660254037844387076, 1.000000000000000000, 0.8660254037844387076, 1.000000000000000000, 0.8660254037844387076, 1.000000000000000000, 0.8660254037844387076, 1.000000000000000000, 0.8660254037844387076, 1.000000000000000000, 0.8660254037844387076, 1.000000000000000000, 0.8660254037844387076, 1.000000000000000000, 0.8660254037844387076, 1.000000000000000000, 0.8660254037844387076, 1.000000000000000000, 0.8660254037844387076, 1.000000000000000000, 0.8660254037844387076, 1.000000000000000000, 0.8660254037844387076, 1.000000000000000000, 0.8660254037844387076, 1.000000000000000000, 0.8660254037844387076, 1.000000000000000000, 0.8660254037844387076, 1.000000000000000000, 0.8660254037844387076, 1.000000000000000000, 0.8660254037844387076, 1.000000000000000000, 0.8660254037844387076, 1.000000000000000000, 0.8660254037844387076, 1.000000000000000000, 0.8660254037844387076, 1.000000000000000000, 0.8660254037844387076, 1.000000000000000000, 0.8660254037844387076, 1.000000000000000000, 0.8660254037844387076, 1.000000000000000000, 0.8660254037844387076, 1.000000000000000000, 0.8660254037844387076, 1.000000000000000000, 0.8660254037844387076, 1.000000000000000000, 0.8660254037844387076, 1.000000000000000000, 0.8660254037844387076, 1.000000000000000000, 0.8660254037844387076, 1.000000000000000000, 0.8660254037844387076, 1.000000000000000000, 0.8660254037844387076, 1.000000000000000000, 0.8660254037844387076, 1.000000000000000000, 0.8660254037844387076, 1.000000000000000000, 0.8660254037844387076, 1.000000000000000000, 0.8660254037844387076, 1.000000000000000000, 0.8660254037844387076, 1.000000000000000000, 0.8660254037844387076, 1.000000000000000000, 0.8660254037844387076, 1.000000000000000000, 0.8660254037844387076, 1.000000000000000000, 0.8660254037844387076, 1.000000000000000000, 0.8660254037844387076, 1.000000000000000000, 0.8660254037844387076, 1.000000000000000000, 0.8660254037844387076, 1.000000000000000000, 0.8660254037844387076, 1.000000000000000000, 0.8660254037844387076, 1.000000000000000000, 0.8660254037844387076, 1.000000000000000000, 0.8660254037844387076, 1.000000000000000000, 0.8660254037844387076, 1.000000000000000000, 0.8660254037844387076, 1.000000000000000000, 0.8660254037844387076, 1.000000000000000000, 0.8660254037844387076, 1.000000000000000000, 0.8660254037844387076, 1.000000000000000000, 0.8660254037844387076, 1.000000000000000000, 0.8660254037844387076, 1.000000000000000000, 0.8660254037844387076, 1.000000000000000000, 0.8660254037844387076, 1.000000000000000000, 0.8660254037844387076, 1.000000000000000000, 0.8660254037844387076, 1.000000000000000000, 0.8660254037844387076, 1.000000000000000000, 0.8660254037844387076, 1.000000000000000000, 0.8660254037844387076, 1.000000000000000000, 0.8660254037844387076, 1.000000000000000000, 0.8660254037844387076, 1.000000000000000000, 0.8660254037844387076, 1.000000000000000000, 0.8660254037844387076, 1.000000000000000000, 0.8660254037844387076, 1.000000000000000000, 0.8660254037844387076, 1.000000000000000000, 0.8660254037844387076, 1.000000000000000000, 0.8660254037844387076, 1.000000000000000000, 0.8660254037844387076, 1.000000000000000000, 0.8660254037844387076, 1.000000000000000000, 0.8660254037844387076, 1.000000000000000000, 0.8660254037844387076, 1.000000000000000000, 0.8660254037844387076, 1.000000000000000000, 0.8660254037844387076, 1.000000000000000000, 0.8660254037844387076, 1.000000000000000000, 0.8660254037844387076, 1.000000000000000000, 0.8660254037844387076, 1.000000000000000000, 0.8660254037844387076, 1.000000000000000000, 0.8660254037844387076, 1.000000000000000000, 0.8660254037844387076, 1.000000000000000000, 0.8660254037844387076, 1.000000000000000000, 0.8660254037844387076, 1.000000000000000000, 0.8660254037844387076, 1.000000000000000000, 0.8660254037844387076, 1.000000000000000000, 0.8660254037844387076, 1.000000000000000000, 0.8660254037844387076, 1.000000000000000000, 0.8660254037844387076, 1.000000000000000000, 0.8660254037844387076, 1.000000000000000000, 0.8660254037844387076, 1.000000000000000000, 0.8660254037844387076, 1.000000000000000000, 0.8660254037844387076, 1.000000000000000000, 0.8660254037844387076, 1.000000000000000000, 0.8660254037844387076, 1.000000000000000000, 0.8660254037844387076, 1.000000000000000000, 0.8660254037844387076, 1.000000000000000000, 0.8660254037844387076, 1.000000000000000000, 0.8660254037844387076, 1.000000000000000000, 0.8660254037844387076, 1.000000000000000000, 0.8660254037844387076, 1.000000000000000000, 0.8660254037844387076, 1.000000000000000000, 0.8660254037844387076, 1.000000000000000000, 0.8660254037844387076, 1.000000000000000000, 0.8660254037844387076, 1.000000000000000000, 0.8660254037844387076, 1.000000000000000000, 0.8660254037844387076, 1.000000000000000000, 0.8660254037844387076, 1.000000000000000000, 0.8660254037844387076, 1.000000000000000000, 0.8660254037844387076, 1.000000000000000000, 0.8660254037844387076, 1.000000000000000000, 0.8660254037844387076, 1.000000000000000000, 0.8660254037844387076, 1.000000000000000000, 0.8660254037844387076, 1.000000000000000000, 0.8660254037844387076, 1.000000000000000000, 0.8660254037844387076, 1.000000000000000000, 0.8660254037844387076, 1.000000000000000000, 0.8660254037844387076, 1.000000000000000000, 0.8660254037844387076, 1.000000000000000000, 0.8660254037844387076, 1.000000000000000000, 0.8660254037844387076, 1.000000000000000000, 0.8660254037844387076, 1.000000000000000000, 0.8660254037844387076, 1.000000000000000000, 0.8660254037844387076, 1.000000000000000000, 0.8660254037844387076, 1.000000000000000000, 0.8660254037844387076, 1.000000000000000000, 0.8660254037844387076, 1.000000000000000000, 0.8660254037844387076, 1.000000000000000000, 0.8660254037844387076, 1.000000000000000000, 0.8660254037844387076, 1.000000000000000000, 0.8660254037844387076, 1.000000000000000000, 0.8660254037844387076, 1.000000000000000000, 0.8660254037844387076, 1.000000000000000000, 0.8660254037844387076, 1.000000000000000000, 0.8660254037844387076, 1.000000000000000000, 0.8660254037844387076, 1.000000000000000000, 0.8660254037844387076, 1.000000000000000000, 0.8660254037844387076, 1.000000000000000000, 0.8660254037844387076, 1.000000000000000000, 0.8660254037844387076, 1.000000000000000000, 0.8660254037844387076, 1.000000000000000000, 0.8660254037844387076, 1.000000000000000000, 0.8660254037844387076, 1.000000000000000000, 0.8660254037844387076, 1.000000000000000000, 0.8660254037844387076, 1.000000000000000000, 0.8660254037844387076, 1.000000000000000000, 0.8660254037844387076, 1.000000000000000000, 0.8660254037844387076, 1.000000000000000000, 0.8660254037844387076, 1.000000000000000000, 0.8660254037844387076, 1.000000000000000000, 0.8660254037844387076, 1.000000000000000000, 0.8660254037844387076, 1.000000000000000000, 0.8660254037844387076, 1.000000000000000000, 0.8660254037844387076, 1.000000000000000000, 0.8660254037844387076, 1.000000000000000000, 0.8660254037844387076, 1.000000000000000000, 0.8660254037844387076, 1.000000000000000000, 0.8660254037844387076, 1.000000000000000000, 0.8660254037844387076, 1.000000000000000000, 0.8660254037844387076, 1.000000000000000000, 0.8660254037844387076, 1.000000000000000000, 0.8660254037844387076, 1.000000000000000000, 0.8660254037844387076, 1.000000000000000000, 0.8660254037844387076, 1.000000000000000000, 0.8660254037844387076, 1.000000000000000000, 0.8660254037844387076, 1.000000000000000000, 0.8660254037844387076, 1.000000000000000000, 0.8660254037844387076, 1.000000000000000000, 0.8660254037844387076, 1.000000000000000000, 0.8660254037844387076, 1.000000000000000000, 0.8660254037844387076, 1.000000000000000000, 0.8660254037844387076, 1.000000000000000000, 0.8660254037844387076, 1.000000000000000000, 0.8660254037844387076, 1.000000000000000000, 0.8660254037844387076, 1.000000000000000000, 0.8660254037844387076, 1.000000000000000000, 0.8660254037844387076, 1.000000000000000000, 0.8660254037844387076, 1.000000000000000000, 0.8660254037844387076, 1.000000000000000000, 0.8660254037844387076, 1.000000000000000000, 0.8660254037844387076, 1.000000000000000000, 0.8660254037844387076, 1.000000000000000000, 0.8660254037844387076, 1.000000000000000000, 0.8660254037844387076, 1.000000000000000000, 0.8660254037844387076, 1.000000000000000000, 0.8660254037844387076, 1.000000000000000000, 0.8660254037844387076, 1.000000000000000000, 0.8660254037844387076, 1.000000000000000000, 0.8660254037844387076, 1.000000000000000000, 0.8660254037844387076, 1.000000000000000000, 0.8660254037844387076, 1.000000000000000000, 0.8660254037844387076, 1.000000000000000000, 0.8660254037844387076, 1.000000000000000000, 0.8660254037844387076, 1.000000000000000000, 0.8660254037844387076, 1.000000000000000000, 0.8660254037844387076, 1.000000000000000000, 0.8660254037844387076, 1.000000000000000000, 0.8660254037844387076, 1.000000000000000000, 0.8660254037844387076, 1.000000000000000000, 0.8660254037844387076, 1.000000000000000000, 0.8660254037844387076, 1.000000000000000000, 0.8660254037844387076, 1.000000000000000000, 0.8660254037844387076, 1.000000000000000000, 0.8660254037844387076, 1.000000000000000000, 0.8660254037844387076, 1.000000000000000000, 0.8660254037844387076, 1.000000000000000000, 0.8660254037844387076, 1.000000000000000000, 0.8660254037844387076, 1.000000000000000000, 0.8660254037844387076, 1.000000000000000000, 0.8660254037844387076, 1.000000000000000000, 0.8660254037844387076, 1.000000000000000000, 0.8660254037844387076, 1.000000000000000000, 0.8660254037844387076, 1.000000000000000000, 0.8660254037844387076, 1.000000000000000000, 0.8660254037844387076, 1.000000000000000000, 0.8660254037844387076, 1.000000000000000000, 0.8660254037844387076, 1.000000000000000000, 0.8660254037844387076, 1.000000000000000000, 0.8660254037844387076, 1.000000000000000000, 0.8660254037844387076, 1.000000000000000000, 0.8660254037844387076, 1.000000000000000000, 0.8660254037844387076, 1.000000000000000000, 0.8660254037844387076, 1.000000000000000000, 0.8660254037844387076, 1.000000000000000000, 0.8660254037844387076, 1.000000000000000000, 0.8660254037844387076, 1.000000000000000000, 0.8660254037844387076, 1.000000000000000000, 0.8660254037844387076, 1.000000000000000000, 0.8660254037844387076, 1.000000000000000000, 0.8660254037844387076, 1.000000000000000000, 0.8660254037844387076, 1.000000000000000000, 0.8660254037844387076, 1.000000000000000000, 0.8660254037844387076, 1.000000000000000000, 0.8660254037844387076, 1.000000000000000000, 0.8660254037844387076, 1.000000000000000000, 0.8660254037844387076, 1.000000000000000000, 0.8660254037844387076, 1.000000000000000000, 0.8660254037844387076, 1.000000000000000000, 0.8660254037844387076, 1.000000000000000000, 0.8660254037844387076, 1.000000000000000000, 0.8660254037844387076, 1.000000000000000000, 0.8660254037844387076, 1.000000000000000000, 0.8660254037844387076, 1.000000000000000000, 0.8660254037844387076, 1.000000000000000000, 0.8660254037844387076, 1.000000000000000000, 0.8660254037844387076, 1.000000000000000000, 0.8660254037844387076, 1.000000000000000000, 0.8660254037844387076, 1.000000000000000000, 0.8660254037844387076, 1.000000000000000000, 0.8660254037844387076, 1.000000000000000000, 0.8660254037844387076, 1.000000000000000000, 0.8660254037844387076, 1.000000000000000000, 0.8660254037844387076, 1.000000000000000000, 0.8660254037844387076, 1.000000000000000000, 0.8660254037844387076, 1.000000000000000000, 0.8660254037844387076, 1.000000000000000000, 0.8660254037844387076, 1.000000000000000000, 0.8660254037844387076, 1.000000000000000000, 0.8660254037844387076, 1.000000000000000000, 0.8660254037844387076, 1.000000000000000000, 0.8660254037844387076, 1.000000000000000000, 0.8660254037844387076, 1.000000000000000000, 0.8660254037844387076, 1.000000000000000000, 0.8660254037844387076, 1.000000000000000000, 0.8660254037844387076, 1.000000000000000000, 0.8660254037844387076, 1.000000000000000000, 0.8660254037844387076, 1.000000000000000000, 0.8660254037844387076, 1.000000000000000000, 0.8660254037844387076, 1.000000000000000000, 0.8660254037844387076, 1.000000000000000000, 0.8660254037844387076, 1.000000000000000000, 0.8660254037844387076, 1.000000000000000000, 0.8660254037844387076, 1.000000000000000000, 0.8660254037844387076, 1.000000000000000000, 0.8660254037844387076, 1.000000000000000000, 0.8660254037844387076, 1.000000000000000000, 0.8660254037844387076, 1.000000000000000000, 0.8660254037844387076, 1.000000000000000000, 0.8660254037844387076, 1.000000000000000000, 0.8660254037844387076, 1.000000000000000000, 0.8660254037844387076, 1.000000000000000000, 0.8660254037844387076, 1.000000000000000000, 0.8660254037844387076, 1.000000000000000000, 0.8660254037844387076, 1.000000000000000000, 0.8660254037844387076, 1.000000000000000000, 0.8660254037844387076, 1.000000000000000000, 0.8660254037844387076, 1.000000000000000000, 0.8660254037844387076, 1.000000000000000000, 0.8660254037844387076, 1.000000000000000000, 0.8660254037844387076, 1.000000000000000000, 0.8660254037844387076, 1.000000000000000000, 0.8660254037844387076, 1.000000000000000000, 0.8660254037844387076, 1.000000000000000000, 0.8660254037844387076, 1.000000000000000000, 0.8660254037844387076, 1.000000000000000000, 0.8660254037844387076, 1.000000000000000000, 0.8660254037844387076, 1.000000000000000000, 0.8660254037844387076, 1.000000000000000000, 0.8660254037844387076, 1.000000000000000000),
 ( 1.000000000000000000, 0.8660254037844387076, 1.000000000000000000, 0.8660254037844387076, 1.000000000000000000, 0.8660254037844387076, 1.000000000000000000, 0.8660254037844387076, 1.000000000000000000, 0.8660254037844387076, 1.000000000000000000, 0.8660254037844387076, 1.000000000000000000, 0.8660254037844387076, 1.000000000000000000, 0.8660254037844387076, 1.000000000000000000, 0.8660254037844387076, 1.000000000000000000, 0.8660254037844387076, 1.000000000000000000, 0.8660254037844387076, 1.000000000000000000, 0.8660254037844387076, 1.000000000000000000, 0.8660254037844387076, 1.000000000000000000, 0.8660254037844387076, 1.000000000000000000, 0.8660254037844387076, 1.000000000000000000, 0.8660254037844387076, 1.000000000000000000, 0.8660254037844387076, 1.000000000000000000, 0.8660254037844387076, 1.000000000000000000, 0.8660254037844387076, 1.000000000000000000, 0.8660254037844387076, 1.000000000000000000, 0.8660254037844387076, 1.000000000000000000, 0.8660254037844387076, 1.000000000000000000, 0.8660254037844387076, 1.000000000000000000, 0.8660254037844387076, 1.000000000000000000, 0.8660254037844387076, 1.000000000000000000, 0.8660254037844387076, 1.000000000000000000, 0.8660254037844387076, 1.000000000000000000, 0.8660254037844387076, 1.000000000000000000, 0.8660254037844387076, 1.000000000000000000, 0.8660254037844387076, 1.000000000000000000, 0.8660254037844387076, 1.000000000000000000, 0.8660254037844387076, 1.000000000000000000, 0.8660254037844387076, 1.000000000000000000, 0.8660254037844387076, 1.000000000000000000, 0.8660254037844387076, 1.000000000000000000, 0.8660254037844387076, 1.000000000000000000, 0.8660254037844387076, 1.000000000000000000, 0.8660254037844387076, 1.000000000000000000, 0.8660254037844387076, 1.000000000000000000, 0.8660254037844387076, 1.000000000000000000, 0.8660254037844387076, 1.000000000000000000, 0.8660254037844387076, 1.000000000000000000, 0.8660254037844387076, 1.000000000000000000, 0.8660254037844387076, 1.000000000000000000, 0.8660254037844387076, 1.000000000000000000, 0.8660254037844387076, 1.000000000000000000, 0.8660254037844387076, 1.000000000000000000, 0.8660254037844387076, 1.000000000000000000, 0.8660254037844387076, 1.000000000000000000, 0.8660254037844387076, 1.000000000000000000, 0.8660254037844387076, 1.000000000000000000, 0.8660254037844387076, 1.000000000000000000, 0.8660254037844387076, 1.000000000000000000, 0.8660254037844387076, 1.000000000000000000, 0.8660254037844387076, 1.000000000000000000, 0.8660254037844387076, 1.000000000000000000, 0.8660254037844387076, 1.000000000000000000, 0.8660254037844387076, 1.000000000000000000, 0.8660254037844387076, 1.000000000000000000, 0.8660254037844387076, 1.000000000000000000, 0.8660254037844387076, 1.000000000000000000, 0.8660254037844387076, 1.000000000000000000, 0.8660254037844387076, 1.000000000000000000, 0.8660254037844387076, 1.000000000000000000, 0.8660254037844387076, 1.000000000000000000, 0.8660254037844387076, 1.000000000000000000, 0.8660254037844387076, 1.000000000000000000, 0.8660254037844387076, 1.000000000000000000, 0.8660254037844387076, 1.000000000000000000, 0.8660254037844387076, 1.000000000000000000, 0.8660254037844387076, 1.000000000000000000, 0.8660254037844387076, 1.000000000000000000, 0.8660254037844387076, 1.000000000000000000, 0.8660254037844387076, 1.000000000000000000, 0.8660254037844387076, 1.000000000000000000, 0.8660254037844387076, 1.000000000000000000, 0.8660254037844387076, 1.000000000000000000, 0.8660254037844387076, 1.000000000000000000, 0.8660254037844387076, 1.000000000000000000, 0.8660254037844387076, 1.000000000000000000, 0.8660254037844387076, 1.000000000000000000, 0.8660254037844387076, 1.000000000000000000, 0.8660254037844387076, 1.000000000000000000, 0.8660254037844387076, 1.000000000000000000, 0.8660254037844387076, 1.000000000000000000, 0.8660254037844387076, 1.000000000000000000, 0.8660254037844387076, 1.000000000000000000, 0.8660254037844387076, 1.000000000000000000, 0.8660254037844387076, 1.000000000000000000, 0.8660254037844387076, 1.000000000000000000, 0.8660254037844387076, 1.000000000000000000, 0.8660254037844387076, 1.000000000000000000, 0.8660254037844387076, 1.000000000000000000, 0.8660254037844387076, 1.000000000000000000, 0.8660254037844387076, 1.000000000000000000, 0.8660254037844387076, 1.000000000000000000, 0.8660254037844387076, 1.000000000000000000, 0.8660254037844387076, 1.000000000000000000, 0.8660254037844387076, 1.000000000000000000, 0.8660254037844387076, 1.000000000000000000, 0.8660254037844387076, 1.000000000000000000, 0.8660254037844387076, 1.000000000000000000, 0.8660254037844387076, 1.000000000000000000, 0.8660254037844387076, 1.000000000000000000, 0.8660254037844387076, 1.000000000000000000, 0.8660254037844387076, 1.000000000000000000, 0.8660254037844387076, 1.000000000000000000, 0.8660254037844387076, 1.000000000000000000, 0.8660254037844387076, 1.000000000000000000, 0.8660254037844387076, 1.000000000000000000, 0.8660254037844387076, 1.000000000000000000, 0.8660254037844387076, 1.000000000000000000, 0.8660254037844387076, 1.000000000000000000, 0.8660254037844387076, 1.000000000000000000, 0.8660254037844387076, 1.000000000000000000, 0.8660254037844387076, 1.000000000000000000, 0.8660254037844387076, 1.000000000000000000, 0.8660254037844387076, 1.000000000000000000, 0.8660254037844387076, 1.000000000000000000, 0.8660254037844387076, 1.000000000000000000, 0.8660254037844387076, 1.000000000000000000, 0.8660254037844387076, 1.000000000000000000, 0.8660254037844387076, 1.000000000000000000, 0.8660254037844387076, 1.000000000000000000, 0.8660254037844387076, 1.000000000000000000, 0.8660254037844387076, 1.000000000000000000, 0.8660254037844387076, 1.000000000000000000, 0.8660254037844387076, 1.000000000000000000, 0.8660254037844387076, 1.000000000000000000, 0.8660254037844387076, 1.000000000000000000, 0.8660254037844387076, 1.000000000000000000, 0.8660254037844387076, 1.000000000000000000, 0.8660254037844387076, 1.000000000000000000, 0.8660254037844387076, 1.000000000000000000, 0.8660254037844387076, 1.000000000000000000, 0.8660254037844387076, 1.000000000000000000, 0.8660254037844387076, 1.000000000000000000, 0.8660254037844387076, 1.000000000000000000, 0.8660254037844387076, 1.000000000000000000, 0.8660254037844387076, 1.000000000000000000, 0.8660254037844387076, 1.000000000000000000, 0.8660254037844387076, 1.000000000000000000, 0.8660254037844387076, 1.000000000000000000, 0.8660254037844387076, 1.000000000000000000, 0.8660254037844387076, 1.000000000000000000, 0.8660254037844387076, 1.000000000000000000, 0.8660254037844387076, 1.000000000000000000, 0.8660254037844387076, 1.000000000000000000, 0.8660254037844387076, 1.000000000000000000, 0.8660254037844387076, 1.000000000000000000, 0.8660254037844387076, 1.000000000000000000, 0.8660254037844387076, 1.000000000000000000, 0.8660254037844387076, 1.000000000000000000, 0.8660254037844387076, 1.000000000000000000, 0.8660254037844387076, 1.000000000000000000, 0.8660254037844387076, 1.000000000000000000, 0.8660254037844387076, 1.000000000000000000, 0.8660254037844387076, 1.000000000000000000, 0.8660254037844387076, 1.000000000000000000, 0.8660254037844387076, 1.000000000000000000, 0.8660254037844387076, 1.000000000000000000, 0.8660254037844387076, 1.000000000000000000, 0.8660254037844387076, 1.000000000000000000, 0.8660254037844387076, 1.000000000000000000, 0.8660254037844387076, 1.000000000000000000, 0.8660254037844387076, 1.000000000000000000, 0.8660254037844387076, 1.000000000000000000, 0.8660254037844387076, 1.000000000000000000, 0.8660254037844387076, 1.000000000000000000, 0.8660254037844387076, 1.000000000000000000, 0.8660254037844387076, 1.000000000000000000, 0.8660254037844387076, 1.000000000000000000, 0.8660254037844387076, 1.000000000000000000, 0.8660254037844387076, 1.000000000000000000, 0.8660254037844387076, 1.000000000000000000, 0.8660254037844387076, 1.000000000000000000, 0.8660254037844387076, 1.000000000000000000, 0.8660254037844387076, 1.000000000000000000, 0.8660254037844387076, 1.000000000000000000, 0.8660254037844387076, 1.000000000000000000, 0.8660254037844387076, 1.000000000000000000, 0.8660254037844387076, 1.000000000000000000, 0.8660254037844387076, 1.000000000000000000, 0.8660254037844387076, 1.000000000000000000, 0.8660254037844387076, 1.000000000000000000, 0.8660254037844387076, 1.000000000000000000, 0.8660254037844387076, 1.000000000000000000, 0.8660254037844387076, 1.000000000000000000, 0.8660254037844387076, 1.000000000000000000, 0.8660254037844387076, 1.000000000000000000, 0.8660254037844387076, 1.000000000000000000, 0.8660254037844387076, 1.000000000000000000, 0.8660254037844387076, 1.000000000000000000, 0.8660254037844387076, 1.000000000000000000, 0.8660254037844387076, 1.000000000000000000, 0.8660254037844387076, 1.000000000000000000, 0.8660254037844387076, 1.000000000000000000, 0.8660254037844387076, 1.000000000000000000, 0.8660254037844387076, 1.000000000000000000, 0.8660254037844387076, 1.000000000000000000, 0.8660254037844387076, 1.000000000000000000, 0.8660254037844387076, 1.000000000000000000, 0.8660254037844387076, 1.000000000000000000, 0.8660254037844387076, 1.000000000000000000, 0.8660254037844387076, 1.000000000000000000, 0.8660254037844387076, 1.000000000000000000, 0.8660254037844387076, 1.000000000000000000, 0.8660254037844387076, 1.000000000000000000, 0.8660254037844387076, 1.000000000000000000, 0.8660254037844387076, 1.000000000000000000, 0.8660254037844387076, 1.000000000000000000, 0.8660254037844387076, 1.000000000000000000, 0.8660254037844387076, 1.000000000000000000, 0.8660254037844387076, 1.000000000000000000, 0.8660254037844387076, 1.000000000000000000, 0.8660254037844387076, 1.000000000000000000, 0.8660254037844387076, 1.000000000000000000, 0.8660254037844387076, 1.000000000000000000, 0.8660254037844387076, 1.000000000000000000, 0.8660254037844387076, 1.000000000000000000, 0.8660254037844387076, 1.000000000000000000, 0.8660254037844387076, 1.000000000000000000, 0.8660254037844387076, 1.000000000000000000, 0.8660254037844387076, 1.000000000000000000, 0.8660254037844387076, 1.000000000000000000, 0.8660254037844387076, 1.000000000000000000, 0.8660254037844387076, 1.000000000000000000, 0.8660254037844387076, 1.000000000000000000, 0.8660254037844387076, 1.000000000000000000, 0.8660254037844387076, 1.000000000000000000, 0.8660254037844387076, 1.000000000000000000, 0.8660254037844387076, 1.000000000000000000, 0.8660254037844387076, 1.000000000000000000, 0.8660254037844387076, 1.000000000000000000, 0.8660254037844387076, 1.000000000000000000, 0.8660254037844387076, 1.000000000000000000, 0.8660254037844387076, 1.000000000000000000, 0.8660254037844387076, 1.000000000000000000, 0.8660254037844387076, 1.000000000000000000, 0.8660254037844387076, 1.000000000000000000, 0.8660254037844387076, 1.000000000000000000, 0.8660254037844387076, 1.000000000000000000, 0.8660254037844387076, 1.000000000000000000, 0.8660254037844387076, 1.000000000000000000, 0.8660254037844387076, 1.000000000000000000, 0.8660254037844387076, 1.000000000000000000, 0.8660254037844387076, 1.000000000000000000, 0.8660254037844387076, 1.000000000000000000, 0.8660254037844387076, 1.000000000000000000, 0.8660254037844387076, 1.000000000000000000, 0.8660254037844387076, 1.000000000000000000, 0.8660254037844387076, 1.000000000000000000, 0.8660254037844387076, 1.000000000000000000, 0.8660254037844387076, 1.000000000000000000, 0.8660254037844387076, 1.000000000000000000, 0.8660254037844387076, 1.000000000000000000, 0.8660254037844387076, 1.000000000000000000, 0.8660254037844387076, 1.000000000000000000, 0.8660254037844387076, 1.000000000000000000, 0.8660254037844387076, 1.000000000000000000, 0.8660254037844387076, 1.000000000000000000, 0.8660254037844387076, 1.000000000000000000, 0.8660254037844387076, 1.000000000000000000, 0.8660254037844387076, 1.000000000000000000, 0.8660254037844387076, 1.000000000000000000, 0.8660254037844387076, 1.000000000000000000, 0.8660254037844387076, 1.000000000000000000, 0.8660254037844387076, 1.000000000000000000, 0.8660254037844387076, 1.000000000000000000, 0.8660254037844387076, 1.000000000000000000, 0.8660254037844387076, 1.000000000000000000, 0.8660254037844387076, 1.000000000000000000, 0.8660254037844387076, 1.000000000000000000, 0.8660254037844387076, 1.000000000000000000, 0.8660254037844387076, 1.000000000000000000, 0.8660254037844387076, 1.000000000000000000, 0.8660254037844387076, 1.000000000000000000, 0.8660254037844387076, 1.000000000000000000, 0.8660254037844387076, 1.000000000000000000, 0.8660254037844387076, 1.000000000000000000, 0.8660254037844387076, 1.000000000000000000, 0.8660254037844387076, 1.000000000000000000, 0.8660254037844387076, 1.000000000000000000, 0.8660254037844387076, 1.000000000000000000, 0.8660254037844387076, 1.000000000000000000, 0.8660254037844387076, 1.000000000000000000, 0.8660254037844387076, 1.000000000000000000, 0.8660254037844387076, 1.000000000000000000, 0.8660254037844387076, 1.000000000000000000, 0.8660254037844387076, 1.000000000000000000, 0.8660254037844387076, 1.000000000000000000, 0.8660254037844387076, 1.000000000000000000, 0.8660254037844387076, 1.000000000000000000, 0.8660254037844387076, 1.000000000000000000, 0.8660254037844387076, 1.000000000000000000, 0.8660254037844387076, 1.000000000000000000, 0.8660254037844387076, 1.000000000000000000, 0.8660254037844387076, 1.000000000000000000, 0.8660254037844387076, 1.000000000000000000, 0.8660254037844387076, 1.000000000000000000, 0.8660254037844387076, 1.000000000000000000, 0.8660254037844387076, 1.000000000000000000, 0.8660254037844387076, 1.000000000000000000, 0.8660254037844387076, 1.000000000000000000, 0.8660254037844387076, 1.000000000000000000, 0.8660254037844387076, 1.000000000000000000, 0.8660254037844387076, 1.000000000000000000, 0.8660254037844387076, 1.000000000000000000, 0.8660254037844387076, 1.000000000000000000, 0.8660254037844387076, 1.000000000000000000, 0.8660254037844387076, 1.000000000000000000, 0.8660254037844387076, 1.000000000000000000, 0.8660254037844387076, 1.000000000000000000, 0.8660254037844387076, 1.000000000000000000, 0.8660254037844387076, 1.000000000000000000, 0.8660254037844387076, 1.000000000000000000, 0.8660254037844387076, 1.000000000000000000, 0.8660254037844387076, 1.000000000000000000, 0.8660254037844387076, 1.000000000000000000, 0.8660254037844387076, 1.000000000000000000, 0.8660254037844387076, 1.000000000000000000, 0.8660254037844387076, 1.000000000000000000, 0.8660254037844387076, 1.000000000000000000, 0.8660254037844387076, 1.000000000000000000, 0.8660254037844387076, 1.000000000000000000, 0.8660254037844387076, 1.000000000000000000, 0.8660254037844387076, 1.000000000000000000, 0.8660254037844387076, 1.000000000000000000, 0.8660254037844387076, 1.000000000000000000, 0.8660254037844387076, 1.000000000000000000, 0.8660254037844387076, 1.000000000000000000, 0.8660254037844387076, 1.000000000000000000, 0.8660254037844387076, 1.000000000000000000, 0.8660254037844387076, 1.000000000000000000, 0.8660254037844387076, 1.000000000000000000, 0.8660254037844387076, 1.000000000000000000, 0.8660254037844387076, 1.000000000000000000, 0.8660254037844387076, 1.000000000000000000, 0.8660254037844387076, 1.000000000000000000, 0.8660254037844387076, 1.000000000000000000, 0.8660254037844387076, 1.000000000000000000, 0.8660254037844387076, 1.000000000000000000, 0.8660254037844387076, 1.000000000000000000, 0.8660254037844387076, 1.000000000000000000, 0.8660254037844387076, 1.000000000000000000, 0.8660254037844387076, 1.000000000000000000, 0.8660254037844387076, 1.000000000000000000, 0.8660254037844387076, 1.000000000000000000, 0.8660254037844387076, 1.000000000000000000, 0.8660254037844387076, 1.000000000000000000, 0.8660254037844387076, 1.000000000000000000, 0.8660254037844387076, 1.000000000000000000, 0.8660254037844387076, 1.000000000000000000, 0.8660254037844387076, 1.000000000000000000, 0.8660254037844387076, 1.000000000000000000, 0.8660254037844387076, 1.000000000000000000, 0.8660254037844387076, 1.000000000000000000, 0.8660254037844387076, 1.000000000000000000, 0.8660254037844387076, 1.000000000000000000, 0.8660254037844387076, 1.000000000000000000, 0.8660254037844387076, 1.000000000000000000, 0.8660254037844387076, 1.000000000000000000, 0.8660254037844387076, 1.000000000000000000, 0.8660254037844387076, 1.000000000000000000, 0.8660254037844387076, 1.000000000000000000, 0.8660254037844387076, 1.000000000000000000, 0.8660254037844387076, 1.000000000000000000, 0.8660254037844387076, 1.000000000000000000, 0.8660254037844387076, 1.000000000000000000, 0.8660254037844387076, 1.000000000000000000, 0.8660254037844387076, 1.000000000000000000, 0.8660254037844387076, 1.000000000000000000, 0.8660254037844387076, 1.000000000000000000, 0.8660254037844387076, 1.000000000000000000, 0.8660254037844387076, 1.000000000000000000, 0.8660254037844387076, 1.000000000000000000, 0.8660254037844387076, 1.000000000000000000, 0.8660254037844387076, 1.000000000000000000, 0.8660254037844387076, 1.000000000000000000, 0.8660254037844387076, 1.000000000000000000, 0.8660254037844387076, 1.000000000000000000, 0.8660254037844387076, 1.000000000000000000, 0.8660254037844387076, 1.000000000000000000, 0.8660254037844387076, 1.000000000000000000, 0.8660254037844387076, 1.000000000000000000, 0.8660254037844387076, 1.000000000000000000, 0.8660254037844387076, 1.000000000000000000, 0.8660254037844387076, 1.000000000000000000, 0.8660254037844387076, 1.000000000000000000, 0.8660254037844387076, 1.000000000000000000, 0.8660254037844387076, 1.000000000000000000, 0.8660254037844387076, 1.000000000000000000, 0.8660254037844387076, 1.000000000000000000, 0.8660254037844387076, 1.000000000000000000, 0.8660254037844387076, 1.000000000000000000, 0.8660254037844387076, 1.000000000000000000, 0.8660254037844387076, 1.000000000000000000, 0.8660254037844387076, 1.000000000000000000, 0.8660254037844387076, 1.000000000000000000, 0.8660254037844387076, 1.000000000000000000, 0.8660254037844387076, 1.000000000000000000, 0.8660254037844387076, 1.000000000000000000, 0.8660254037844387076, 1.000000000000000000, 0.8660254037844387076, 1.000000000000000000, 0.8660254037844387076, 1.000000000000000000, 0.8660254037844387076, 1.000000000000000000, 0.8660254037844387076, 1.000000000000000000, 0.8660254037844387076, 1.000000000000000000, 0.8660254037844387076, 1.000000000000000000, 0.8660254037844387076, 1.000000000000000000, 0.8660254037844387076, 1.000000000000000000, 0.8660254037844387076, 1.000000000000000000, 0.8660254037844387076, 1.000000000000000000, 0.8660254037844387076, 1.000000000000000000, 0.8660254037844387076, 1.000000000000000000, 0.8660254037844387076, 1.000000000000000000, 0.8660254037844387076, 1.000000000000000000, 0.8660254037844387076, 1.000000000000000000, 0.8660254037844387076, 1.000000000000000000, 0.8660254037844387076, 1.000000000000000000, 0.8660254037844387076, 1.000000000000000000, 0.8660254037844387076, 1.000000000000000000, 0.8660254037844387076, 1.000000000000000000, 0.8660254037844387076, 1.000000000000000000, 0.8660254037844387076, 1.000000000000000000, 0.8660254037844387076, 1.000000000000000000, 0.8660254037844387076, 1.000000000000000000, 0.8660254037844387076, 1.000000000000000000, 0.8660254037844387076, 1.000000000000000000, 0.8660254037844387076, 1.000000000000000000, 0.8660254037844387076, 1.000000000000000000, 0.8660254037844387076, 1.000000000000000000, 0.8660254037844387076, 1.000000000000000000, 0.8660254037844387076, 1.000000000000000000, 0.8660254037844387076, 1.000000000000000000, 0.8660254037844387076, 1.000000000000000000, 0.8660254037844387076, 1.000000000000000000, 0.8660254037844387076, 1.000000000000000000, 0.8660254037844387076, 1.000000000000000000, 0.8660254037844387076, 1.000000000000000000, 0.8660254037844387076, 1.000000000000000000, 0.8660254037844387076, 1.000000000000000000, 0.8660254037844387076, 1.000000000000000000, 0.8660254037844387076, 1.000000000000000000, 0.8660254037844387076, 1.000000000000000000, 0.8660254037844387076, 1.000000000000000000, 0.8660254037844387076, 1.000000000000000000, 0.8660254037844387076, 1.000000000000000000, 0.8660254037844387076, 1.000000000000000000, 0.8660254037844387076, 1.000000000000000000, 0.8660254037844387076, 1.000000000000000000, 0.8660254037844387076, 1.000000000000000000, 0.8660254037844387076, 1.000000000000000000, 0.8660254037844387076, 1.000000000000000000, 0.8660254037844387076, 1.000000000000000000, 0.8660254037844387076, 1.000000000000000000, 0.8660254037844387076, 1.000000000000000000, 0.8660254037844387076, 1.000000000000000000, 0.8660254037844387076, 1.000000000000000000, 0.8660254037844387076, 1.000000000000000000, 0.8660254037844387076, 1.000000000000000000, 0.8660254037844387076, 1.000000000000000000, 0.8660254037844387076, 1.000000000000000000, 0.8660254037844387076, 1.000000000000000000, 0.8660254037844387076, 1.000000000000000000, 0.8660254037844387076, 1.000000000000000000, 0.8660254037844387076, 1.000000000000000000, 0.8660254037844387076, 1.000000000000000000, 0.8660254037844387076, 1.000000000000000000, 0.8660254037844387076, 1.000000000000000000, 0.8660254037844387076, 1.000000000000000000, 0.8660254037844387076, 1.000000000000000000, 0.8660254037844387076, 1.000000000000000000, 0.8660254037844387076, 1.000000000000000000, 0.8660254037844387076, 1.000000000000000000, 0.8660254037844387076, 1.000000000000000000, 0.8660254037844387076, 1.000000000000000000, 0.8660254037844387076, 1.000000000000000000, 0.8660254037844387076, 1.000000000000000000, 0.8660254037844387076, 1.000000000000000000, 0.8660254037844387076, 1.000000000000000000, 0.8660254037844387076, 1.000000000000000000, 0.8660254037844387076, 1.000000000000000000, 0.8660254037844387076, 1.000000000000000000, 0.8660254037844387076, 1.000000000000000000, 0.8660254037844387076, 1.000000000000000000, 0.8660254037844387076, 1.000000000000000000, 0.8660254037844387076, 1.000000000000000000, 0.8660254037844387076, 1.000000000000000000, 0.8660254037844387076, 1.000000000000000000, 0.8660254037844387076, 1.000000000000000000, 0.8660254037844387076, 1.000000000000000000, 0.8660254037844387076, 1.000000000000000000, 0.8660254037844387076, 1.000000000000000000, 0.8660254037844387076, 1.000000000000000000, 0.8660254037844387076, 1.000000000000000000, 0.8660254037844387076, 1.000000000000000000, 0.8660254037844387076, 1.000000000000000000, 0.8660254037844387076, 1.000000000000000000, 0.8660254037844387076, 1.000000000000000000, 0.8660254037844387076, 1.000000000000000000, 0.8660254037844387076, 1.000000000000000000, 0.8660254037844387076, 1.000000000000000000, 0.8660254037844387076, 1.000000000000000000, 0.8660254037844387076, 1.000000000000000000, 0.8660254037844387076, 1.000000000000000000, 0.8660254037844387076, 1.000000000000000000, 0.8660254037844387076, 1.000000000000000000, 0.8660254037844387076, 1.000000000000000000, 0.8660254037844387076, 1.000000000000000000, 0.8660254037844387076, 1.000000000000000000, 0.8660254037844387076, 1.000000000000000000, 0.8660254037844387076, 1.000000000000000000, 0.8660254037844387076, 1.000000000000000000, 0.8660254037844387076, 1.000000000000000000, 0.8660254037844387076, 1.000000000000000000, 0.8660254037844387076, 1.000000000000000000, 0.8660254037844387076, 1.000000000000000000, 0.8660254037844387076, 1.000000000000000000, 0.8660254037844387076, 1.000000000000000000, 0.8660254037844387076, 1.000000000000000000, 0.8660254037844387076, 1.000000000000000000, 0.8660254037844387076, 1.000000000000000000, 0.8660254037844387076, 1.000000000000000000, 0.8660254037844387076, 1.000000000000000000, 0.8660254037844387076, 1.000000000000000000, 0.8660254037844387076, 1.000000000000000000, 0.8660254037844387076, 1.000000000000000000, 0.8660254037844387076, 1.000000000000000000, 0.8660254037844387076, 1.000000000000000000, 0.8660254037844387076, 1.000000000000000000, 0.8660254037844387076, 1.000000000000000000, 0.8660254037844387076, 1.000000000000000000, 0.8660254037844387076, 1.000000000000000000, 0.8660254037844387076, 1.000000000000000000, 0.8660254037844387076, 1.000000000000000000, 0.8660254037844387076, 1.000000000000000000, 0.8660254037844387076, 1.000000000000000000, 0.8660254037844387076, 1.000000000000000000, 0.8660254037844387076, 1.000000000000000000, 0.8660254037844387076, 1.000000000000000000, 0.8660254037844387076, 1.000000000000000000, 0.8660254037844387076, 1.000000000000000000, 0.8660254037844387076, 1.000000000000000000, 0.8660254037844387076, 1.000000000000000000, 0.8660254037844387076, 1.000000000000000000, 0.8660254037844387076, 1.000000000000000000, 0.8660254037844387076, 1.000000000000000000, 0.8660254037844387076, 1.000000000000000000, 0.8660254037844387076, 1.000000000000000000, 0.8660254037844387076, 1.000000000000000000, 0.8660254037844387076, 1.000000000000000000, 0.8660254037844387076, 1.000000000000000000, 0.8660254037844387076, 1.000000000000000000, 0.8660254037844387076, 1.000000000000000000, 0.8660254037844387076, 1.000000000000000000, 0.8660254037844387076, 1.000000000000000000, 0.8660254037844387076, 1.000000000000000000, 0.8660254037844387076, 1.000000000000000000, 0.8660254037844387076, 1.000000000000000000, 0.8660254037844387076, 1.000000000000000000, 0.8660254037844387076, 1.000000000000000000, 0.8660254037844387076, 1.000000000000000000, 0.8660254037844387076, 1.000000000000000000, 0.8660254037844387076, 1.000000000000000000, 0.8660254037844387076, 1.000000000000000000, 0.8660254037844387076, 1.000000000000000000, 0.8660254037844387076, 1.000000000000000000, 0.8660254037844387076, 1.000000000000000000, 0.8660254037844387076, 1.000000000000000000, 0.8660254037844387076, 1.000000000000000000, 0.8660254037844387076, 1.000000000000000000, 0.8660254037844387076, 1.000000000000000000, 0.8660254037844387076, 1.000000000000000000, 0.8660254037844387076, 1.000000000000000000, 0.8660254037844387076, 1.000000000000000000, 0.8660254037844387076, 1.000000000000000000, 0.8660254037844387076, 1.000000000000000000, 0.8660254037844387076, 1.000000000000000000, 0.8660254037844387076, 1.000000000000000000, 0.8660254037844387076, 1.000000000000000000, 0.8660254037844387076, 1.000000000000000000, 0.8660254037844387076, 1.000000000000000000, 0.8660254037844387076, 1.000000000000000000, 0.8660254037844387076, 1.000000000000000000, 0.8660254037844387076, 1.000000000000000000, 0.8660254037844387076, 1.000000000000000000, 0.8660254037844387076, 1.000000000000000000, 0.8660254037844387076, 1.000000000000000000, 0.8660254037844387076, 1.000000000000000000, 0.8660254037844387076, 1.000000000000000000, 0.8660254037844387076, 1.000000000000000000, 0.8660254037844387076, 1.000000000000000000, 0.8660254037844387076, 1.000000000000000000, 0.8660254037844387076, 1.000000000000000000, 0.8660254037844387076, 1.000000000000000000, 0.8660254037844387076, 1.000000000000000000, 0.8660254037844387076, 1.000000000000000000, 0.8660254037844387076, 1.000000000000000000, 0.8660254037844387076, 1.000000000000000000, 0.8660254037844387076, 1.000000000000000000, 0.8660254037844387076, 1.000000000000000000, 0.8660254037844387076, 1.000000000000000000, 0.8660254037844387076, 1.000000000000000000, 0.8660254037844387076, 1.000000000000000000, 0.8660254037844387076, 1.000000000000000000, 0.8660254037844387076, 1.000000000000000000, 0.8660254037844387076, 1.000000000000000000, 0.8660254037844387076, 1.000000000000000000, 0.8660254037844387076, 1.000000000000000000, 0.8660254037844387076, 1.000000000000000000, 0.8660254037844387076, 1.000000000000000000, 0.8660254037844387076, 1.000000000000000000, 0.8660254037844387076, 1.000000000000000000, 0.8660254037844387076, 1.000000000000000000, 0.8660254037844387076, 1.000000000000000000, 0.8660254037844387076, 1.000000000000000000, 0.8660254037844387076, 1.000000000000000000, 0.8660254037844387076, 1.000000000000000000, 0.8660254037844387076, 1.000000000000000000, 0.8660254037844387076, 1.000000000000000000, 0.8660254037844387076, 1.000000000000000000, 0.8660254037844387076, 1.000000000000000000, 0.8660254037844387076, 1.000000000000000000, 0.8660254037844387076, 1.000000000000000000, 0.8660254037844387076, 1.000000000000000000, 0.8660254037844387076, 1.000000000000000000, 0.8660254037844387076, 1.000000000000000000, 0.8660254037844387076, 1.000000000000000000, 0.8660254037844387076, 1.000000000000000000, 0.8660254037844387076, 1.000000000000000000, 0.8660254037844387076, 1.000000000000000000, 0.8660254037844387076, 1.000000000000000000, 0.8660254037844387076, 1.000000000000000000, 0.8660254037844387076, 1.000000000000000000, 0.8660254037844387076, 1.000000000000000000, 0.8660254037844387076, 1.000000000000000000, 0.8660254037844387076, 1.000000000000000000, 0.8660254037844387076, 1.000000000000000000, 0.8660254037844387076, 1.000000000000000000, 0.8660254037844387076, 1.000000000000000000, 0.8660254037844387076, 1.000000000000000000, 0.8660254037844387076, 1.000000000000000000, 0.8660254037844387076, 1.000000000000000000, 0.8660254037844387076, 1.000000000000000000, 0.8660254037844387076, 1.000000000000000000, 0.8660254037844387076, 1.000000000000000000, 0.8660254037844387076, 1.000000000000000000, 0.8660254037844387076, 1.000000000000000000, 0.8660254037844387076, 1.000000000000000000, 0.8660254037844387076, 1.000000000000000000, 0.8660254037844387076, 1.000000000000000000, 0.8660254037844387076, 1.000000000000000000, 0.8660254037844387076, 1.000000000000000000, 0.8660254037844387076, 1.000000000000000000, 0.8660254037844387076, 1.000000000000000000, 0.8660254037844387076, 1.000000000000000000, 0.8660254037844387076, 1.000000000000000000, 0.8660254037844387076, 1.000000000000000000, 0.8660254037844387076, 1.000000000000000000, 0.8660254037844387076, 1.000000000000000000, 0.8660254037844387076, 1.000000000000000000, 0.8660254037844387076, 1.000000000000000000, 0.8660254037844387076, 1.000000000000000000, 0.8660254037844387076, 1.000000000000000000, 0.8660254037844387076, 1.000000000000000000, 0.8660254037844387076, 1.000000000000000000, 0.8660254037844387076, 1.000000000000000000, 0.8660254037844387076, 1.000000000000000000, 0.8660254037844387076, 1.000000000000000000, 0.8660254037844387076, 1.000000000000000000, 0.8660254037844387076, 1.000000000000000000, 0.8660254037844387076, 1.000000000000000000, 0.8660254037844387076, 1.000000000000000000, 0.8660254037844387076, 1.000000000000000000, 0.8660254037844387076, 1.000000000000000000, 0.8660254037844387076, 1.000000000000000000, 0.8660254037844387076, 1.000000000000000000, 0.8660254037844387076, 1.000000000000000000, 0.8660254037844387076, 1.000000000000000000, 0.8660254037844387076, 1.000000000000000000, 0.8660254037844387076, 1.000000000000000000, 0.8660254037844387076, 1.000000000000000000, 0.8660254037844387076, 1.000000000000000000, 0.8660254037844387076, 1.000000000000000000, 0.8660254037844387076, 1.000000000000000000, 0.8660254037844387076, 1.000000000000000000, 0.8660254037844387076, 1.000000000000000000, 0.8660254037844387076, 1.000000000000000000, 0.8660254037844387076, 1.000000000000000000, 0.8660254037844387076, 1.000000000000000000, 0.8660254037844387076, 1.000000000000000000, 0.8660254037844387076, 1.000000000000000000, 0.8660254037844387076, 1.000000000000000000, 0.8660254037844387076, 1.000000000000000000, 0.8660254037844387076, 1.000000000000000000, 0.8660254037844387076, 1.000000000000000000, 0.8660254037844387076, 1.000000000000000000, 0.8660254037844387076, 1.000000000000000000, 0.8660254037844387076, 1.000000000000000000, 0.8660254037844387076, 1.000000000000000000, 0.8660254037844387076, 1.000000000000000000, 0.8660254037844387076, 1.000000000000000000, 0.8660254037844387076, 1.000000000000000000, 0.8660254037844387076, 1.000000000000000000, 0.8660254037844387076, 1.000000000000000000, 0.8660254037844387076, 1.000000000000000000, 0.8660254037844387076, 1.000000000000000000, 0.8660254037844387076, 1.000000000000000000, 0.8660254037844387076, 1.000000000000000000, 0.8660254037844387076, 1.000000000000000000, 0.8660254037844387076, 1.000000000000000000, 0.8660254037844387076, 1.000000000000000000, 0.8660254037844387076, 1.000000000000000000, 0.8660254037844387076, 1.000000000000000000, 0.8660254037844387076, 1.000000000000000000, 0.8660254037844387076, 1.000000000000000000, 0.8660254037844387076, 1.000000000000000000, 0.8660254037844387076, 1.000000000000000000, 0.8660254037844387076, 1.000000000000000000, 0.8660254037844387076, 1.000000000000000000, 0.8660254037844387076, 1.000000000000000000, 0.8660254037844387076, 1.000000000000000000, 0.8660254037844387076, 1.000000000000000000, 0.8660254037844387076, 1.000000000000000000, 0.8660254037844387076, 1.000000000000000000, 0.8660254037844387076, 1.000000000000000000, 0.8660254037844387076, 1.000000000000000000, 0.8660254037844387076, 1.000000000000000000, 0.8660254037844387076, 1.000000000000000000, 0.8660254037844387076, 1.000000000000000000, 0.8660254037844387076, 1.000000000000000000, 0.8660254037844387076, 1.000000000000000000, 0.8660254037844387076, 1.000000000000000000, 0.8660254037844387076, 1.000000000000000000, 0.8660254037844387076, 1.000000000000000000, 0.8660254037844387076, 1.000000000000000000, 0.8660254037844387076, 1.000000000000000000, 0.8660254037844387076, 1.000000000000000000, 0.8660254037844387076, 1.000000000000000000, 0.8660254037844387076, 1.000000000000000000, 0.8660254037844387076, 1.000000000000000000, 0.8660254037844387076, 1.000000000000000000, 0.8660254037844387076, 1.000000000000000000, 0.8660254037844387076, 1.000000000000000000, 0.8660254037844387076, 1.000000000000000000, 0.8660254037844387076, 1.000000000000000000, 0.8660254037844387076, 1.000000000000000000, 0.8660254037844387076, 1.000000000000000000, 0.8660254037844387076, 1.000000000000000000, 0.8660254037844387076, 1.000000000000000000, 0.8660254037844387076, 1.000000000000000000, 0.8660254037844387076, 1.000000000000000000, 0.8660254037844387076, 1.000000000000000000, 0.8660254037844387076, 1.000000000000000000, 0.8660254037844387076, 1.000000000000000000, 0.8660254037844387076, 1.000000000000000000, 0.8660254037844387076, 1.000000000000000000, 0.8660254037844387076, 1.000000000000000000, 0.8660254037844387076, 1.000000000000000000, 0.8660254037844387076, 1.000000000000000000, 0.8660254037844387076, 1.000000000000000000, 0.8660254037844387076, 1.000000000000000000, 0.8660254037844387076, 1.000000000000000000, 0.8660254037844387076, 1.000000000000000000, 0.8660254037844387076, 1.000000000000000000, 0.8660254037844387076, 1.000000000000000000, 0.8660254037844387076, 1.000000000000000000, 0.8660254037844387076, 1.000000000000000000, 0.8660254037844387076, 1.000000000000000000, 0.8660254037844387076, 1.000000000000000000, 0.8660254037844387076, 1.000000000000000000, 0.8660254037844387076, 1.000000000000000000, 0.8660254037844387076, 1.000000000000000000, 0.8660254037844387076, 1.000000000000000000, 0.8660254037844387076, 1.000000000000000000, 0.8660254037844387076, 1.000000000000000000, 0.8660254037844387076, 1.000000000000000000, 0.8660254037844387076, 1.000000000000000000, 0.8660254037844387076, 1.000000000000000000, 0.8660254037844387076, 1.000000000000000000, 0.8660254037844387076, 1.000000000000000000, 0.8660254037844387076, 1.000000000000000000, 0.8660254037844387076, 1.000000000000000000, 0.8660254037844387076, 1.000000000000000000, 0.8660254037844387076, 1.000000000000000000, 0.8660254037844387076, 1.000000000000000000, 0.8660254037844387076, 1.000000000000000000, 0.8660254037844387076, 1.000000000000000000, 0.8660254037844387076, 1.000000000000000000, 0.8660254037844387076, 1.000000000000000000, 0.8660254037844387076, 1.000000000000000000, 0.8660254037844387076, 1.000000000000000000, 0.8660254037844387076, 1.000000000000000000, 0.8660254037844387076, 1.000000000000000000, 0.8660254037844387076, 1.000000000000000000, 0.8660254037844387076, 1.000000000000000000, 0.8660254037844387076, 1.000000000000000000, 0.8660254037844387076, 1.000000000000000000, 0.8660254037844387076, 1.000000000000000000, 0.8660254037844387076, 1.000000000000000000, 0.8660254037844387076, 1.000000000000000000, 0.8660254037844387076, 1.000000000000000000, 0.8660254037844387076, 1.000000000000000000, 0.8660254037844387076, 1.000000000000000000, 0.8660254037844387076, 1.000000000000000000, 0.8660254037844387076, 1.000000000000000000, 0.8660254037844387076, 1.000000000000000000, 0.8660254037844387076, 1.000000000000000000, 0.8660254037844387076, 1.000000000000000000, 0.8660254037844387076, 1.000000000000000000, 0.8660254037844387076, 1.000000000000000000, 0.8660254037844387076, 1.000000000000000000, 0.8660254037844387076, 1.000000000000000000, 0.8660254037844387076, 1.000000000000000000, 0.8660254037844387076, 1.000000000000000000, 0.8660254037844387076, 1.000000000000000000, 0.8660254037844387076, 1.000000000000000000, 0.8660254037844387076, 1.000000000000000000, 0.8660254037844387076, 1.000000000000000000, 0.8660254037844387076, 1.000000000000000000, 0.8660254037844387076, 1.000000000000000000, 0.8660254037844387076, 1.000000000000000000, 0.8660254037844387076, 1.000000000000000000, 0.8660254037844387076, 1.000000000000000000, 0.8660254037844387076, 1.000000000000000000, 0.8660254037844387076, 1.000000000000000000, 0.8660254037844387076, 1.000000000000000000, 0.8660254037844387076, 1.000000000000000000, 0.8660254037844387076, 1.000000000000000000, 0.8660254037844387076, 1.000000000000000000, 0.8660254037844387076, 1.000000000000000000, 0.8660254037844387076, 1.000000000000000000, 0.8660254037844387076, 1.000000000000000000, 0.8660254037844387076, 1.000000000000000000, 0.8660254037844387076, 1.000000000000000000, 0.8660254037844387076, 1.000000000000000000, 0.8660254037844387076, 1.000000000000000000, 0.8660254037844387076, 1.000000000000000000, 0.8660254037844387076, 1.000000000000000000) ) ) 
 REPRESENTATION_ITEM ( '' )  SURFACE ( )  );
#14514 = CARTESIAN_POINT ( 'NONE',  ( 5.000000000000000000, 12.50000000000000000, -6.123233995736766282E-16 ) ) ;
#14515 = CARTESIAN_POINT ( 'NONE',  ( 1.060575238724906964E-15, 5.250000000000000888, 5.773502691896257311 ) ) ;
#14516 = ADVANCED_FACE ( 'NONE', ( #29390 ), #14931, .T. ) ;
#14517 = CARTESIAN_POINT ( 'NONE',  ( 9.457646018065525792E-16, -59.06249999863440792, 5.148502694627439702 ) ) ;
#14518 = DIRECTION ( 'NONE',  ( 1.000000000000000000, 0.000000000000000000, 0.000000000000000000 ) ) ;
#14519 = CARTESIAN_POINT ( 'NONE',  ( 5.000000000000000888, -2.458333330602146205, 2.886751345948126879 ) ) ;
#14521 = EDGE_LOOP ( 'NONE', ( #15469, #44445, #4035, #45108 ) ) ;
#14520 = CARTESIAN_POINT ( 'NONE',  ( 4.458734124999999437, -31.81249999863440436, -5.460374474430324690E-16 ) ) ;
#14522 = CARTESIAN_POINT ( 'NONE',  ( 2.499999999999998668, 17.79166666939785557, -4.330127018922193649 ) ) ;
#14523 = CARTESIAN_POINT ( 'NONE',  ( 3.061616997868383141E-16, -156.7500000000000000, -5.000000000000000000 ) ) ;
#14524 = ADVANCED_FACE ( 'NONE', ( #48397 ), #29718, .T. ) ;
#14525 = CARTESIAN_POINT ( 'NONE',  ( 5.000000000000000000, -19.49999999999999645, -6.123233995736766282E-16 ) ) ;
#14526 = CARTESIAN_POINT ( 'NONE',  ( 5.000000000000000000, -44.41666666666665719, -2.886751345948129988 ) ) ;
#14527 = ADVANCED_FACE ( 'NONE', ( #26187 ), #45164, .T. ) ;
#14528 = CARTESIAN_POINT ( 'NONE',  ( -4.458734124999999437, -24.56249999863440436, 0.000000000000000000 ) ) ;
#14529 = CARTESIAN_POINT ( 'NONE',  ( 1.975475456537005874E-15, -1.624999997268813834, 5.000000000000000000 ) ) ;
#14530 = CARTESIAN_POINT ( 'NONE',  ( 4.458734124999998549, -67.72916666530107932, -2.574251347313721627 ) ) ;
#14531 = CARTESIAN_POINT ( 'NONE',  ( 3.152801135295366208, -144.8125000013655779, 3.152801135295367985 ) ) ;
#14532 = VECTOR ( 'NONE', #8194, 1000.000000000000000 ) ;
#14533 = CARTESIAN_POINT ( 'NONE',  ( 2.229367062499998831, -75.64583333196773651, -3.861377020970580887 ) ) ;
#14534 = CARTESIAN_POINT ( 'NONE',  ( -50.55543936806279248, -140.3125000013656063, 0.3552334253322060320 ) ) ;
#14535 = CARTESIAN_POINT ( 'NONE',  ( 4.458734124999999437, -32.06249999863440792, -5.460374474430324690E-16 ) ) ;
#14536 = CARTESIAN_POINT ( 'NONE',  ( -2.499999999999996447, -68.70833333060214443, 4.330127018922195425 ) ) ;
#14537 = VERTEX_POINT ( 'NONE', #60619 ) ;
#14538 = CARTESIAN_POINT ( 'NONE',  ( 1.975475456537005874E-15, -79.62499999726881583, 5.000000000000000000 ) ) ;
#14539 = ORIENTED_EDGE ( 'NONE', *, *, #33062, .F. ) ;
#14540 = CARTESIAN_POINT ( 'NONE',  ( 9.457646018065525792E-16, -75.31249999863440792, 5.148502694627439702 ) ) ;
#14541 = CARTESIAN_POINT ( 'NONE',  ( -1.339745962155610925, 8.330341803992665106, 5.000000000000000000 ) ) ;
#14542 = EDGE_LOOP ( 'NONE', ( #19737, #22051, #20406, #41451 ) ) ;
#14543 = AXIS2_PLACEMENT_3D ( 'NONE', #87, #10672, #54749 ) ;
#14544 = CARTESIAN_POINT ( 'NONE',  ( -2.499999999999996447, -77.70833333060214443, 4.330127018922195425 ) ) ;
#14545 = EDGE_CURVE ( 'NONE', #29728, #46916, #34961, .T. ) ;
#14546 = CARTESIAN_POINT ( 'NONE',  ( 4.458734125000001214, -61.14583333196773651, 2.574251347313718519 ) ) ;
#14547 = CARTESIAN_POINT ( 'NONE',  ( -4.458734124999999437, 2.354166668032262599, -2.574251347313719407 ) ) ;
#14548 = ORIENTED_EDGE ( 'NONE', *, *, #52476, .F. ) ;
#14549 = CARTESIAN_POINT ( 'NONE',  ( 2.071067811865392461, -142.1875000000000284, 5.000000000000084377 ) ) ;
#14550 = CARTESIAN_POINT ( 'NONE',  ( -4.999999999999998224, -59.79166666393547303, 2.886751345948131764 ) ) ;
#14551 = CARTESIAN_POINT ( 'NONE',  ( -4.458734124999998549, 12.77083333469892601, 2.574251347313722516 ) ) ;
#14552 = CARTESIAN_POINT ( 'NONE',  ( -59.44456063193725015, -145.5625000013656063, -0.3552334253322034230 ) ) ;
#14553 = CARTESIAN_POINT ( 'NONE',  ( 2.499999999999998668, -24.33333333333333215, -4.330127018922193649 ) ) ;
#14554 = CARTESIAN_POINT ( 'NONE',  ( -4.458734124999999437, -164.0000000013656063, -1.846868145590735644 ) ) ;
#14555 = ORIENTED_EDGE ( 'NONE', *, *, #39634, .T. ) ;
#14556 = CARTESIAN_POINT ( 'NONE',  ( -4.458734124999999437, -76.31249999863440792, 0.000000000000000000 ) ) ;
#14557 = CARTESIAN_POINT ( 'NONE',  ( 2.499999999999998668, -0.2083333306021478704, -4.330127018922193649 ) ) ;
#14558 = CARTESIAN_POINT ( 'NONE',  ( 4.458734124999998549, 4.270833334698926897, -2.574251347313721627 ) ) ;
#14559 = CARTESIAN_POINT ( 'NONE',  ( -6.972266317189433020E-16, 19.75000000000000000, -5.000000000000000000 ) ) ;
#14560 = CARTESIAN_POINT ( 'NONE',  ( 4.458734124999998549, -65.97916666530106511, -2.574251347313721627 ) ) ;
#14561 = CARTESIAN_POINT ( 'NONE',  ( -5.000000000000000000, -22.87499999726881228, 0.000000000000000000 ) ) ;
#14562 = CARTESIAN_POINT ( 'NONE',  ( -6.972266317189433020E-16, -11.12499999726881406, -5.000000000000000000 ) ) ;
#14563 = CARTESIAN_POINT ( 'NONE',  ( 2.499999999999998668, -28.20833333060214798, -4.330127018922193649 ) ) ;
#14564 = DIRECTION ( 'NONE',  ( 0.000000000000000000, 0.000000000000000000, 1.000000000000000000 ) ) ;
#14565 = CARTESIAN_POINT ( 'NONE',  ( 1.975475456537005874E-15, -43.62499999726880873, 5.000000000000000000 ) ) ;
#14566 = CARTESIAN_POINT ( 'NONE',  ( 2.229367062500001939, -46.97916666530106511, 3.861377020970579999 ) ) ;
#14567 = CARTESIAN_POINT ( 'NONE',  ( 2.229367062500001939, -28.22916666530107221, 3.861377020970579999 ) ) ;
#14568 = CARTESIAN_POINT ( 'NONE',  ( 4.458734125000000326, 4.854166668032262599, 2.574251347313718519 ) ) ;
#14569 = DIRECTION ( 'NONE',  ( -0.000000000000000000, 1.000000000000000000, -0.000000000000000000 ) ) ;
#14570 = CARTESIAN_POINT ( 'NONE',  ( 5.000000000000000888, 27.41666666666666785, 2.886751345948126879 ) ) ;
#14571 = CARTESIAN_POINT ( 'NONE',  ( -5.000000000000000888, -147.5625000027311842, 2.071067811865474617 ) ) ;
#14572 = CARTESIAN_POINT ( 'NONE',  ( -2.229367062500000163, -39.47916666530107221, -3.861377020970580443 ) ) ;
#14573 = CARTESIAN_POINT ( 'NONE',  ( 1.060575238724906964E-15, -73.62499999726881583, 5.773502691896257311 ) ) ;
#14574 = CARTESIAN_POINT ( 'NONE',  ( -59.29741812935640155, -145.8750000013655779, -2.196230717870135685 ) ) ;
#14575 = CARTESIAN_POINT ( 'NONE',  ( 3.061616997868383141E-16, -141.7500000000000284, -5.000000000000000000 ) ) ;
#14576 = EDGE_CURVE ( 'NONE', #9561, #62900, #61274, .T. ) ;
#14577 = EDGE_CURVE ( 'NONE', #37707, #26290, #22517, .T. ) ;
#14578 = CARTESIAN_POINT ( 'NONE',  ( 4.458734124999999437, -73.06249999863439371, -5.460374474430324690E-16 ) ) ;
#14579 = CARTESIAN_POINT ( 'NONE',  ( -3.152801135295367985, -165.0625000013656063, 3.152801135295367096 ) ) ;
#14580 = CARTESIAN_POINT ( 'NONE',  ( 2.229367062500001939, -31.97916666530106866, 3.861377020970579999 ) ) ;
#14581 = EDGE_CURVE ( 'NONE', #15950, #54748, #60896, .T. ) ;
#14582 = CARTESIAN_POINT ( 'NONE',  ( -2.499999999999996447, -27.70833333060214798, 4.330127018922195425 ) ) ;
#14583 = DIRECTION ( 'NONE',  ( -0.000000000000000000, 1.000000000000000000, -0.000000000000000000 ) ) ;
#14584 = CARTESIAN_POINT ( 'NONE',  ( 5.000000000000000888, -20.58333333333333570, 2.886751345948126879 ) ) ;
#14585 = CARTESIAN_POINT ( 'NONE',  ( -1.846868145590737420, -145.7500000013655779, 4.458734124999999437 ) ) ;
#14586 = VERTEX_POINT ( 'NONE', #40337 ) ;
#14587 = CARTESIAN_POINT ( 'NONE',  ( 2.500000000000002220, -89.54166666393547303, 4.330127018922192761 ) ) ;
#14588 = CARTESIAN_POINT ( 'NONE',  ( 2.229367062499998831, -57.89583333196773651, -3.861377020970580887 ) ) ;
#14589 = CARTESIAN_POINT ( 'NONE',  ( 5.000000000000000000, 27.62500000273118417, -6.123233995736766282E-16 ) ) ;
#14590 = CARTESIAN_POINT ( 'NONE',  ( -6.972266317189433020E-16, 13.87500000273118594, -5.000000000000000000 ) ) ;
#14591 = CARTESIAN_POINT ( 'NONE',  ( -4.999999999999999112, 21.08333333333333215, 2.886751345948131764 ) ) ;
#14592 =( REPRESENTATION_RELATIONSHIP ('NONE','NONE', #27855, #25037 ) REPRESENTATION_RELATIONSHIP_WITH_TRANSFORMATION ( #54589 )SHAPE_REPRESENTATION_RELATIONSHIP( ) );
#14593 = EDGE_CURVE ( 'NONE', #6014, #29366, #58806, .T. ) ;
#14594 =( BOUNDED_CURVE ( )  B_SPLINE_CURVE ( 2, ( #20996, #60246, #15849, #20683, #40601, #50899, #16164, #41228, #10701 ),
 .UNSPECIFIED., .F., .F. ) 
 B_SPLINE_CURVE_WITH_KNOTS ( ( 3, 2, 2, 2, 3 ),
 ( 0.2416666666666668628, 0.2458333333333335147, 0.2500000000000002220, 0.2541666666666668739, 0.2583333333333335813 ),
 .UNSPECIFIED. ) 
 CURVE ( )  GEOMETRIC_REPRESENTATION_ITEM ( )  RATIONAL_B_SPLINE_CURVE ( ( 0.9999999999999964473, 0.9238795325112902912, 1.000000000000000000, 0.9238795325112867385, 1.000000000000000000, 0.9238795325112867385, 1.000000000000000000, 0.9238795325112826307, 1.000000000000003997 ) ) 
 REPRESENTATION_ITEM ( '' )  );
#14595 = CARTESIAN_POINT ( 'NONE',  ( 6.123233995736766282E-16, -170.0000000000000000, -5.000000000000000000 ) ) ;
#14596 = CARTESIAN_POINT ( 'NONE',  ( -4.458734124999998549, -5.229166665301072214, 2.574251347313722516 ) ) ;
#14597 = CARTESIAN_POINT ( 'NONE',  ( 0.000000000000000000, -170.0000000000000000, 5.000000000000000000 ) ) ;
#14598 = CARTESIAN_POINT ( 'NONE',  ( -9.184850993605147944E-16, -165.3750000027312126, 5.000000000000000000 ) ) ;
#14599 = CARTESIAN_POINT ( 'NONE',  ( 2.071067811865370256, -157.9375000027312126, -5.000000000000105693 ) ) ;
#14600 = EDGE_CURVE ( 'NONE', #52848, #38301, #12420, .T. ) ;
#14601 = ADVANCED_FACE ( 'NONE', ( #10755 ), #55469, .T. ) ;
#14602 = DIRECTION ( 'NONE',  ( -0.000000000000000000, 1.000000000000000000, -0.000000000000000000 ) ) ;
#14604 = CARTESIAN_POINT ( 'NONE',  ( -4.458734124999998549, -23.22916666530107221, 2.574251347313722516 ) ) ;
#14603 = CARTESIAN_POINT ( 'NONE',  ( 0.000000000000000000, -170.0000000000000000, 5.000000000000000000 ) ) ;
#14605 = DIRECTION ( 'NONE',  ( -0.000000000000000000, 1.000000000000000000, -0.000000000000000000 ) ) ;
#14606 = CARTESIAN_POINT ( 'NONE',  ( -2.229367062499996610, -56.14583333196773651, 3.861377020970582219 ) ) ;
#14607 = CARTESIAN_POINT ( 'NONE',  ( -4.458734125000000326, -154.2500000013656063, -1.846868145590735644 ) ) ;
#14608 = EDGE_CURVE ( 'NONE', #55393, #3859, #41144, .T. ) ;
#14609 =( BOUNDED_CURVE ( )  B_SPLINE_CURVE ( 2, ( #55767, #36457, #56084, #12004, #31632, #51268, #7201, #7830, #47064 ),
 .UNSPECIFIED., .F., .F. ) 
 B_SPLINE_CURVE_WITH_KNOTS ( ( 3, 2, 2, 2, 3 ),
 ( 0.07678571428571429047, 0.07738095238095238360, 0.07857142857142856984, 0.07976190476190475609, 0.08035714285714286309 ),
 .UNSPECIFIED. ) 
 CURVE ( )  GEOMETRIC_REPRESENTATION_ITEM ( )  RATIONAL_B_SPLINE_CURVE ( ( 0.9330127018922194093, 0.9330127018922194093, 1.000000000000000000, 0.8660254037844387076, 1.000000000000000000, 0.8660254037844387076, 1.000000000000000000, 0.9330127018922185211, 0.9330127018922192983 ) ) 
 REPRESENTATION_ITEM ( '' )  );
#14610 = CARTESIAN_POINT ( 'NONE',  ( 5.000000000000000000, -48.29166666393547303, -2.886751345948129988 ) ) ;
#14611 = VERTEX_POINT ( 'NONE', #22004 ) ;
#14612 = CARTESIAN_POINT ( 'NONE',  ( 2.229367062500001939, 3.770833334698926009, 3.861377020970579999 ) ) ;
#14613 = EDGE_LOOP ( 'NONE', ( #16777, #40892, #48704, #42292 ) ) ;
#14615 = FACE_OUTER_BOUND ( 'NONE', #15784, .T. ) ;
#14614 = CARTESIAN_POINT ( 'NONE',  ( -6.972266317189433020E-16, -3.124999997268813612, -5.000000000000000000 ) ) ;
#14616 = CARTESIAN_POINT ( 'NONE',  ( 4.458734124999999437, -158.5000000013656631, 1.846868145590737864 ) ) ;
#14617 = ORIENTED_EDGE ( 'NONE', *, *, #13991, .F. ) ;
#14618 = UNCERTAINTY_MEASURE_WITH_UNIT (LENGTH_MEASURE( 1.000000000000000082E-05 ), #20010, 'distance_accuracy_value', 'NONE');
#14619 = CARTESIAN_POINT ( 'NONE',  ( -6.972266317189433020E-16, -7.249999999999998224, -5.000000000000000000 ) ) ;
#14620 = CARTESIAN_POINT ( 'NONE',  ( -58.24261429053147765, -134.2500000000000284, -3.805975901505573855 ) ) ;
#14621 = CARTESIAN_POINT ( 'NONE',  ( 1.975475456537005874E-15, -58.62499999726879452, 5.000000000000000000 ) ) ;
#14622 = CARTESIAN_POINT ( 'NONE',  ( 4.458734124999998549, -43.97916666530105800, -2.574251347313721627 ) ) ;
#14623 = ORIENTED_EDGE ( 'NONE', *, *, #8402, .T. ) ;
#14624 = DIRECTION ( 'NONE',  ( -0.000000000000000000, 1.000000000000000000, -0.000000000000000000 ) ) ;
#14625 = CARTESIAN_POINT ( 'NONE',  ( -2.229367062500000163, 19.52083333469893134, -3.861377020970580443 ) ) ;
#14626 = DIRECTION ( 'NONE',  ( -0.000000000000000000, 1.000000000000000000, -0.000000000000000000 ) ) ;
#14627 = ORIENTED_EDGE ( 'NONE', *, *, #11828, .T. ) ;
#14628 = CARTESIAN_POINT ( 'NONE',  ( -4.458734124999999437, 26.68750000136559564, 0.000000000000000000 ) ) ;
#14629 = CARTESIAN_POINT ( 'NONE',  ( -59.98410592259440222, -125.2500000027311984, -0.3983568153799752487 ) ) ;
#14630 = FACE_OUTER_BOUND ( 'NONE', #12658, .T. ) ;
#14631 = CARTESIAN_POINT ( 'NONE',  ( -51.59932184632553032, -135.0000000000000568, 3.354125322473584525 ) ) ;
#14632 = CARTESIAN_POINT ( 'NONE',  ( 4.458734125000000326, -59.89583333196774362, 2.574251347313718519 ) ) ;
#14633 = CARTESIAN_POINT ( 'NONE',  ( -6.972266317189433020E-16, -62.12499999726880162, -5.000000000000000000 ) ) ;
#14634 = CARTESIAN_POINT ( 'NONE',  ( -4.458734124999998549, 15.77083333469892601, 2.574251347313722516 ) ) ;
#14635 = CARTESIAN_POINT ( 'NONE',  ( -1.339745962155610925, 7.205341801261477386, 5.000000000000000000 ) ) ;
#14636 = CARTESIAN_POINT ( 'NONE',  ( 9.457646018065525792E-16, -51.31249999863440792, 5.148502694627439702 ) ) ;
#14637 = CARTESIAN_POINT ( 'NONE',  ( -4.999999999999999112, -9.791666663935476578, 2.886751345948131764 ) ) ;
#14638 = DIRECTION ( 'NONE',  ( 0.000000000000000000, 0.000000000000000000, 1.000000000000000000 ) ) ;
#14639 = CARTESIAN_POINT ( 'NONE',  ( 0.000000000000000000, -170.0000000000000000, 5.000000000000000000 ) ) ;
#14640 = DIRECTION ( 'NONE',  ( -0.000000000000000000, 1.000000000000000000, -0.000000000000000000 ) ) ;
#14641 = CARTESIAN_POINT ( 'NONE',  ( 4.458734124999998549, -107.7291666653010509, -2.574251347313721627 ) ) ;
#14642 = CARTESIAN_POINT ( 'NONE',  ( -3.152548672688508926E-16, -9.812499998634406140, -5.148502694627439702 ) ) ;
#14643 = ORIENTED_EDGE ( 'NONE', *, *, #27594, .T. ) ;
#14644 = CARTESIAN_POINT ( 'NONE',  ( 5.000000000000000888, -9.458333330602146205, 2.886751345948126879 ) ) ;
#14645 = CARTESIAN_POINT ( 'NONE',  ( -4.458734124999999437, -98.39583333196773651, -2.574251347313719407 ) ) ;
#14646 = CARTESIAN_POINT ( 'NONE',  ( 3.535533905932736864, -160.2500000027312126, 3.535533905932738641 ) ) ;
#14647 = CARTESIAN_POINT ( 'NONE',  ( -4.458734124999999437, -99.64583333196773651, -2.574251347313719407 ) ) ;
#14648 = CARTESIAN_POINT ( 'NONE',  ( 2.071067811865540342, -163.3125000027312126, 4.999999999999936051 ) ) ;
#14649 = CARTESIAN_POINT ( 'NONE',  ( 1.060575238724906964E-15, -55.62499999726880873, 5.773502691896257311 ) ) ;
#14650 = CARTESIAN_POINT ( 'NONE',  ( -6.972266317189433020E-16, -5.249999999999998224, -5.000000000000000000 ) ) ;
#14651 = CARTESIAN_POINT ( 'NONE',  ( -52.10840900171896806, -128.1875000013656063, 3.393966926194110556 ) ) ;
#14652 = CARTESIAN_POINT ( 'NONE',  ( -51.60603307380591787, -146.9375000013656063, -2.891590998281053704 ) ) ;
#14653 = CARTESIAN_POINT ( 'NONE',  ( -2.229367062500000163, -18.47916666530106866, -3.861377020970580443 ) ) ;
#14654 = CARTESIAN_POINT ( 'NONE',  ( 9.457646018065525792E-16, 4.687500001365596525, 5.148502694627439702 ) ) ;
#14655 = CARTESIAN_POINT ( 'NONE',  ( 4.458734124999999437, -61.06249999863440081, -5.460374474430324690E-16 ) ) ;
#14656 = CARTESIAN_POINT ( 'NONE',  ( -1.339745962155613812, -54.20534180126147561, -5.000000000000000000 ) ) ;
#14657 = CARTESIAN_POINT ( 'NONE',  ( -4.458734124999999437, -13.31249999863440259, 0.000000000000000000 ) ) ;
#14658 = CARTESIAN_POINT ( 'NONE',  ( 0.000000000000000000, -120.0000000000000000, 5.000000000000000000 ) ) ;
#14659 = CARTESIAN_POINT ( 'NONE',  ( 3.535533905932736864, -154.1250000000000000, 3.535533905932738641 ) ) ;
#14660 = CARTESIAN_POINT ( 'NONE',  ( -2.499999999999996447, -4.833333333333335702, 4.330127018922195425 ) ) ;
#14661 = ORIENTED_EDGE ( 'NONE', *, *, #1911, .T. ) ;
#14662 = CARTESIAN_POINT ( 'NONE',  ( 2.229367062499998831, -41.89583333196773651, -3.861377020970580887 ) ) ;
#14663 =( BOUNDED_CURVE ( )  B_SPLINE_CURVE ( 2, ( #58412, #39093, #30401, #10462, #58722, #25263, #19479, #19797, #5333 ),
 .UNSPECIFIED., .F., .F. ) 
 B_SPLINE_CURVE_WITH_KNOTS ( ( 3, 2, 2, 2, 3 ),
 ( 0.6520833333333333481, 0.6527777777777777901, 0.6541666666666666741, 0.6555555555555555580, 0.6562500000000000000 ),
 .UNSPECIFIED. ) 
 CURVE ( )  GEOMETRIC_REPRESENTATION_ITEM ( )  RATIONAL_B_SPLINE_CURVE ( ( 0.9330127018922194093, 0.9330127018922194093, 1.000000000000000000, 0.8660254037844387076, 1.000000000000000000, 0.8660254037844387076, 1.000000000000000000, 0.9330127018922194093, 0.9330127018922194093 ) ) 
 REPRESENTATION_ITEM ( '' )  );
#14664 = DIRECTION ( 'NONE',  ( -0.000000000000000000, 1.000000000000000000, -0.000000000000000000 ) ) ;
#14665 = CARTESIAN_POINT ( 'NONE',  ( -2.500000000000000444, -12.16666666666666607, -4.330127018922193649 ) ) ;
#14666 = CARTESIAN_POINT ( 'NONE',  ( 1.975475456537005874E-15, -81.74999999999998579, 5.000000000000000000 ) ) ;
#14667 = CARTESIAN_POINT ( 'NONE',  ( -4.458734124999998549, -85.22916666530107932, 2.574251347313722516 ) ) ;
#14668 = CARTESIAN_POINT ( 'NONE',  ( 2.229367062500001939, 16.77083333469892779, 3.861377020970579999 ) ) ;
#14669 = CARTESIAN_POINT ( 'NONE',  ( 4.458734124999999437, 9.187500001365592084, -5.460374474430324690E-16 ) ) ;
#14670 = CARTESIAN_POINT ( 'NONE',  ( 5.000000000000000000, -0.5000000000000004441, -6.123233995736766282E-16 ) ) ;
#14671 = CARTESIAN_POINT ( 'NONE',  ( -2.071067811865435981, -165.4375000027311557, 5.000000000000041744 ) ) ;
#14672 = CARTESIAN_POINT ( 'NONE',  ( -4.458734124999999437, -89.56249999863440792, 0.000000000000000000 ) ) ;
#14673 = CARTESIAN_POINT ( 'NONE',  ( 4.458734124999998549, 23.02083333469892423, -2.574251347313721627 ) ) ;
#14674 = CARTESIAN_POINT ( 'NONE',  ( -5.000000000000000000, -74.08333333333332860, -2.886751345948128211 ) ) ;
#14675 = CARTESIAN_POINT ( 'NONE',  ( -2.500000000000000444, 15.95833333606451809, -4.330127018922193649 ) ) ;
#14677 = ORIENTED_EDGE ( 'NONE', *, *, #16143, .F. ) ;
#14676 = ADVANCED_FACE ( 'NONE', ( #27448 ), #51285, .T. ) ;
#14678 = CARTESIAN_POINT ( 'NONE',  ( -2.500000000000000444, -7.041666663935481907, -4.330127018922193649 ) ) ;
#14679 = ORIENTED_EDGE ( 'NONE', *, *, #13935, .F. ) ;
#14681 = CARTESIAN_POINT ( 'NONE',  ( -2.500000000000000444, -35.16666666666666430, -4.330127018922193649 ) ) ;
#14680 = CYLINDRICAL_SURFACE ( 'NONE', #30619, 5.000000000000000000 ) ;
#14682 = CARTESIAN_POINT ( 'NONE',  ( -2.229367062499996610, -39.14583333196773651, 3.861377020970582219 ) ) ;
#14683 = ADVANCED_FACE ( 'NONE', ( #12973 ), #57373, .F. ) ;
#14684 = ADVANCED_FACE ( 'NONE', ( #22323 ), #51597, .T. ) ;
#14685 = CARTESIAN_POINT ( 'NONE',  ( 5.000000000000000000, -34.29166666393547303, -2.886751345948129988 ) ) ;
#14687 = ORIENTED_EDGE ( 'NONE', *, *, #445, .T. ) ;
#14686 = CARTESIAN_POINT ( 'NONE',  ( -4.458734124999998549, -65.22916666530106511, 2.574251347313722516 ) ) ;
#14688 = CARTESIAN_POINT ( 'NONE',  ( -52.10840900171896806, -152.4375000013656063, 3.393966926194110556 ) ) ;
#14689 = CARTESIAN_POINT ( 'NONE',  ( 4.458734124999998549, -14.72916666530107399, -2.574251347313721627 ) ) ;
#14691 = VERTEX_POINT ( 'NONE', #46759 ) ;
#14690 = CARTESIAN_POINT ( 'NONE',  ( 2.229367062500001939, -15.22916666530107399, 3.861377020970579999 ) ) ;
#14692 = CARTESIAN_POINT ( 'NONE',  ( 5.000000000000000000, -82.50000000000000000, -6.123233995736766282E-16 ) ) ;
#14693 = CARTESIAN_POINT ( 'NONE',  ( -3.152548672688508926E-16, -58.81249999863440081, -5.148502694627439702 ) ) ;
#14694 =( BOUNDED_CURVE ( )  B_SPLINE_CURVE ( 2, ( #62568, #7269, #7895, #27500, #47129, #41974, #61616, #22695, #27192 ),
 .UNSPECIFIED., .F., .F. ) 
 B_SPLINE_CURVE_WITH_KNOTS ( ( 3, 2, 2, 2, 3 ),
 ( 0.05833333333333338283, 0.06250000000000005551, 0.06666666666666672125, 0.07083333333333338699, 0.07500000000000005274 ),
 .UNSPECIFIED. ) 
 CURVE ( )  GEOMETRIC_REPRESENTATION_ITEM ( )  RATIONAL_B_SPLINE_CURVE ( ( 0.9999999999999991118, 0.9238795325112876267, 1.000000000000000000, 0.9238795325112867385, 1.000000000000000000, 0.9238795325112867385, 1.000000000000000000, 0.9238795325112857393, 1.000000000000001110 ) ) 
 REPRESENTATION_ITEM ( '' )  );
#14695 = CARTESIAN_POINT ( 'NONE',  ( -3.535250795749689387E-16, -82.12499999726883004, -5.773502691896257311 ) ) ;
#14697 = ORIENTED_EDGE ( 'NONE', *, *, #6177, .F. ) ;
#14696 = CARTESIAN_POINT ( 'NONE',  ( -5.000000000000000000, -18.08333333333333215, -2.886751345948128211 ) ) ;
#14698 = CARTESIAN_POINT ( 'NONE',  ( -49.85088928181150436, -144.5625000000000284, -1.666127454062680702 ) ) ;
#14699 = CARTESIAN_POINT ( 'NONE',  ( 2.229367062500001939, -29.22916666530107221, 3.861377020970579999 ) ) ;
#14700 = VERTEX_POINT ( 'NONE', #47082 ) ;
#14701 = CARTESIAN_POINT ( 'NONE',  ( 3.152801135295367541, -168.5625000013656063, -3.152801135295367541 ) ) ;
#14702 = CARTESIAN_POINT ( 'NONE',  ( -3.152548672688508926E-16, -107.8124999986343937, -5.148502694627439702 ) ) ;
#14703 = CARTESIAN_POINT ( 'NONE',  ( -6.972266317189433020E-16, -55.12499999726880873, -5.000000000000000000 ) ) ;
#14704 = VERTEX_POINT ( 'NONE', #27767 ) ;
#14705 = CARTESIAN_POINT ( 'NONE',  ( -58.39396692619412477, -147.6875000013656063, 2.891590998281057701 ) ) ;
#14706 = CARTESIAN_POINT ( 'NONE',  ( -50.18089887299979068, -137.8125000027312126, 2.462841084822635640 ) ) ;
#14707 = CARTESIAN_POINT ( 'NONE',  ( 4.458734124999999437, -40.81249999863440081, -5.460374474430324690E-16 ) ) ;
#14708 = CARTESIAN_POINT ( 'NONE',  ( -4.458734125000000326, -148.1250000013655779, 1.846868145590734089 ) ) ;
#14709 = CARTESIAN_POINT ( 'NONE',  ( -7.500000000000346390, -3.105855721450154316, -7.659356991636309786 ) ) ;
#14710 = CARTESIAN_POINT ( 'NONE',  ( -2.499999999999996447, 0.1666666666666656582, 4.330127018922195425 ) ) ;
#14711 = CARTESIAN_POINT ( 'NONE',  ( 4.458734124999998549, -10.72916666530106866, -2.574251347313721627 ) ) ;
#14712 = CARTESIAN_POINT ( 'NONE',  ( -4.458734124999999437, -100.5624999986344079, 0.000000000000000000 ) ) ;
#14713 = ORIENTED_EDGE ( 'NONE', *, *, #47658, .F. ) ;
#14714 = CARTESIAN_POINT ( 'NONE',  ( -4.458734124999999437, -146.1875000013656063, -5.460374474430324690E-16 ) ) ;
#14715 = CARTESIAN_POINT ( 'NONE',  ( -4.458734124999999437, -33.56249999863440792, 0.000000000000000000 ) ) ;
#14716 = CARTESIAN_POINT ( 'NONE',  ( -3.535250795749689387E-16, 7.875000002731186832, -5.773502691896257311 ) ) ;
#14717 = DIRECTION ( 'NONE',  ( -0.000000000000000000, 1.000000000000000000, -0.000000000000000000 ) ) ;
#14718 = CARTESIAN_POINT ( 'NONE',  ( -59.59170313451811296, -134.5000000013656063, 1.485763867205729394 ) ) ;
#14719 = CARTESIAN_POINT ( 'NONE',  ( -4.458734124999998549, -73.47916666530106511, 2.574251347313722516 ) ) ;
#14720 = CARTESIAN_POINT ( 'NONE',  ( 6.123233995736766282E-16, -120.0000000000000000, -5.000000000000000000 ) ) ;
#14721 = CARTESIAN_POINT ( 'NONE',  ( 1.339745962155612702, -54.16965819600732601, -5.000000000000000000 ) ) ;
#14722 = CARTESIAN_POINT ( 'NONE',  ( 0.000000000000000000, -120.0000000000000000, 0.000000000000000000 ) ) ;
#14723 = CARTESIAN_POINT ( 'NONE',  ( -2.229367062500000163, 5.270833334698927786, -3.861377020970580443 ) ) ;
#14724 = VERTEX_POINT ( 'NONE', #22961 ) ;
#14725 = DIRECTION ( 'NONE',  ( -0.000000000000000000, 1.000000000000000000, -0.000000000000000000 ) ) ;
#14726 = CARTESIAN_POINT ( 'NONE',  ( 2.499999999999998668, 9.666666666666667851, -4.330127018922193649 ) ) ;
#14728 = CARTESIAN_POINT ( 'NONE',  ( 9.457646018065525792E-16, -31.06249999863440436, 5.148502694627439702 ) ) ;
#14727 = CARTESIAN_POINT ( 'NONE',  ( 5.000000000000000888, -95.58333333333332860, 2.886751345948126879 ) ) ;
#14729 = CARTESIAN_POINT ( 'NONE',  ( -2.500000000000000444, -23.04166666393548013, -4.330127018922193649 ) ) ;
#14730 = CARTESIAN_POINT ( 'NONE',  ( 9.457646018065525792E-16, -79.31249999863439371, 5.148502694627439702 ) ) ;
#14731 = CARTESIAN_POINT ( 'NONE',  ( 4.458734125000000326, 23.85416666803225993, 2.574251347313718519 ) ) ;
#14732 = CARTESIAN_POINT ( 'NONE',  ( 1.975475456537005874E-15, -18.74999999999999645, 5.000000000000000000 ) ) ;
#14733 = AXIS2_PLACEMENT_3D ( 'NONE', #8478, #37746, #48641 ) ;
#14734 = CARTESIAN_POINT ( 'NONE',  ( -57.89159099828107458, -143.6875000013656063, -3.393966926194107447 ) ) ;
#14735 = CARTESIAN_POINT ( 'NONE',  ( 9.457646018065525792E-16, -2.062499998634406584, 5.148502694627439702 ) ) ;
#14736 = FACE_OUTER_BOUND ( 'NONE', #55932, .T. ) ;
#14737 = CARTESIAN_POINT ( 'NONE',  ( 2.229367062500001939, -43.22916666530107932, 3.861377020970579999 ) ) ;
#14738 = CARTESIAN_POINT ( 'NONE',  ( -6.972266317189433020E-16, -51.12499999726880873, -5.000000000000000000 ) ) ;
#14739 = CARTESIAN_POINT ( 'NONE',  ( -4.458734124999999437, -0.3124999986344051406, 0.000000000000000000 ) ) ;
#14740 = ORIENTED_EDGE ( 'NONE', *, *, #25191, .T. ) ;
#14741 = CARTESIAN_POINT ( 'NONE',  ( -2.229367062500000163, -24.72916666530106866, -3.861377020970580443 ) ) ;
#14742 = CARTESIAN_POINT ( 'NONE',  ( -3.152548672688508926E-16, -69.56249999863439371, -5.148502694627439702 ) ) ;
#14743 = CARTESIAN_POINT ( 'NONE',  ( -4.999999999999999112, -102.7916666639354588, 2.886751345948131764 ) ) ;
#14744 = CARTESIAN_POINT ( 'NONE',  ( -2.229367062499996610, 24.85416666803225993, 3.861377020970582219 ) ) ;
#14745 = CARTESIAN_POINT ( 'NONE',  ( -4.999999999999998224, -64.91666666666665719, 2.886751345948131764 ) ) ;
#14746 = LINE ( 'NONE', #53993, #34744 ) ;
#14747 = CARTESIAN_POINT ( 'NONE',  ( 2.229367062500001939, -72.22916666530107932, 3.861377020970579999 ) ) ;
#14748 = CARTESIAN_POINT ( 'NONE',  ( 5.000000000000000000, -61.50000000000000000, -6.123233995736766282E-16 ) ) ;
#14749 = CARTESIAN_POINT ( 'NONE',  ( 2.500000000000002220, -73.66666666666665719, 4.330127018922192761 ) ) ;
#14750 = CARTESIAN_POINT ( 'NONE',  ( 5.000000000000000000, -156.1250000027311842, 0.000000000000000000 ) ) ;
#14751 = VERTEX_POINT ( 'NONE', #36797 ) ;
#14752 = CARTESIAN_POINT ( 'NONE',  ( 6.123233995736766282E-16, -120.0000000000000000, -5.000000000000000000 ) ) ;
#14753 = CARTESIAN_POINT ( 'NONE',  ( -6.972266317189433020E-16, 2.875000002731185500, -5.000000000000000000 ) ) ;
#14754 = CARTESIAN_POINT ( 'NONE',  ( 5.000000000000000000, -20.41666666666666430, -2.886751345948129988 ) ) ;
#14755 = CARTESIAN_POINT ( 'NONE',  ( -2.229367062500000163, -20.47916666530107221, -3.861377020970580443 ) ) ;
#14756 = CARTESIAN_POINT ( 'NONE',  ( 9.457646018065525792E-16, -85.06249999863440792, 5.148502694627439702 ) ) ;
#14757 = CARTESIAN_POINT ( 'NONE',  ( 3.152801135295367541, -166.5625000013656063, -3.152801135295367541 ) ) ;
#14758 = CARTESIAN_POINT ( 'NONE',  ( 1.060575238724906964E-15, -18.62499999726881583, 5.773502691896257311 ) ) ;
#14760 = VERTEX_POINT ( 'NONE', #12663 ) ;
#14759 = CARTESIAN_POINT ( 'NONE',  ( 2.229367062500001939, -48.97916666530107221, 3.861377020970579999 ) ) ;
#14761 = LINE ( 'NONE', #9937, #40768 ) ;
#14762 = CARTESIAN_POINT ( 'NONE',  ( 1.062108568985190270E-13, -28.12499999726880873, -4.999999999999999112 ) ) ;
#14764 = ORIENTED_EDGE ( 'NONE', *, *, #61736, .T. ) ;
#14763 = CARTESIAN_POINT ( 'NONE',  ( -4.458734124999999437, 0.4375000013655955255, 0.000000000000000000 ) ) ;
#14765 = CARTESIAN_POINT ( 'NONE',  ( -52.10840900171896806, -154.1875000013656063, 3.393966926194110556 ) ) ;
#14766 = CARTESIAN_POINT ( 'NONE',  ( 1.060575238724906964E-15, -67.75000000000000000, 5.773502691896257311 ) ) ;
#14767 = CARTESIAN_POINT ( 'NONE',  ( -8.190561711645485556E-16, -156.9375000013655779, 4.458734124999999437 ) ) ;
#14768 = CARTESIAN_POINT ( 'NONE',  ( -4.458734124999999437, -40.64583333196773651, -2.574251347313719407 ) ) ;
#14769 = CARTESIAN_POINT ( 'NONE',  ( 4.769696007084728073, -114.9999999999999858, -1.500000000000000444 ) ) ;
#14770 = CARTESIAN_POINT ( 'NONE',  ( -2.071067811865478170, -162.3125000000000284, 5.000000000000000000 ) ) ;
#14771 = CARTESIAN_POINT ( 'NONE',  ( 1.975475456537005874E-15, -56.62499999726880162, 5.000000000000000000 ) ) ;
#14772 = CARTESIAN_POINT ( 'NONE',  ( -50.70258187064364108, -126.3750000013656489, 2.196230717870141014 ) ) ;
#14773 = CARTESIAN_POINT ( 'NONE',  ( 2.229367062499998831, -8.895833331967736513, -3.861377020970580887 ) ) ;
#14774 = CARTESIAN_POINT ( 'NONE',  ( -4.458734124999999437, -48.64583333196773651, -2.574251347313719407 ) ) ;
#14775 = VECTOR ( 'NONE', #58790, 1000.000000000000000 ) ;
#14776 = CARTESIAN_POINT ( 'NONE',  ( -1.339745962155613812, -8.080341798530294994, -5.000000000000000000 ) ) ;
#14777 = CARTESIAN_POINT ( 'NONE',  ( -1.846868145590737420, -146.7500000013656063, 4.458734124999999437 ) ) ;
#14778 = CARTESIAN_POINT ( 'NONE',  ( -4.458734124999998549, -88.47916666530107932, 2.574251347313722516 ) ) ;
#14779 = CARTESIAN_POINT ( 'NONE',  ( 3.535533905932736864, -167.2500000027312126, 3.535533905932738641 ) ) ;
#14780 = EDGE_LOOP ( 'NONE', ( #33898, #20820, #59954, #16927 ) ) ;
#14781 = CARTESIAN_POINT ( 'NONE',  ( -1.339745962155610925, -31.79465819873851373, 5.000000000000000000 ) ) ;
#14782 = CARTESIAN_POINT ( 'NONE',  ( 6.123233995736766282E-16, -170.0000000000000000, -5.000000000000000000 ) ) ;
#14783 = PRODUCT_DEFINITION_SHAPE ( 'NONE', 'NONE',  #53574 ) ;
#14784 = CARTESIAN_POINT ( 'NONE',  ( -57.46284108482265651, -149.0625000027312126, 4.819101127000239515 ) ) ;
#14785 = CARTESIAN_POINT ( 'NONE',  ( -1.339745962155610925, -61.79465819873851729, 5.000000000000000000 ) ) ;
#14786 = EDGE_CURVE ( 'NONE', #39907, #59424, #52222, .T. ) ;
#14787 = ORIENTED_EDGE ( 'NONE', *, *, #42120, .F. ) ;
#14788 = CARTESIAN_POINT ( 'NONE',  ( -2.229367062500000163, 0.5208333346989266754, -3.861377020970580443 ) ) ;
#14789 =( BOUNDED_CURVE ( )  B_SPLINE_CURVE ( 2, ( #3970, #23591, #62828, #33547, #38672, #53476, #25155, #39304, #20013 ),
 .UNSPECIFIED., .F., .F. ) 
 B_SPLINE_CURVE_WITH_KNOTS ( ( 3, 2, 2, 2, 3 ),
 ( 0.3583333333333336146, 0.3625000000000002665, 0.3666666666666669183, 0.3708333333333336257, 0.3750000000000002776 ),
 .UNSPECIFIED. ) 
 CURVE ( )  GEOMETRIC_REPRESENTATION_ITEM ( )  RATIONAL_B_SPLINE_CURVE ( ( 0.9999999999999948930, 0.9238795325112918455, 1.000000000000000000, 0.9238795325112867385, 1.000000000000000000, 0.9238795325112867385, 1.000000000000000000, 0.9238795325112816315, 1.000000000000005107 ) ) 
 REPRESENTATION_ITEM ( '' )  );
#14790 = DIRECTION ( 'NONE',  ( 0.000000000000000000, 1.000000000000000000, 0.000000000000000000 ) ) ;
#14791 = CARTESIAN_POINT ( 'NONE',  ( -2.229367062499996610, -17.39583333196773651, 3.861377020970582219 ) ) ;
#14792 = CARTESIAN_POINT ( 'NONE',  ( -6.972266317189433020E-16, 1.875000002731185722, -5.000000000000000000 ) ) ;
#14793 = CARTESIAN_POINT ( 'NONE',  ( 4.458734125000001214, -0.8958333319677401763, 2.574251347313718519 ) ) ;
#14794 = CARTESIAN_POINT ( 'NONE',  ( -2.500000000000000444, 3.958333336064518093, -4.330127018922193649 ) ) ;
#14795 = CARTESIAN_POINT ( 'NONE',  ( -3.152801135295367096, -154.0625000013656063, -3.152801135295367541 ) ) ;
#14796 = CARTESIAN_POINT ( 'NONE',  ( 4.458734124999999437, 22.93750000136559564, -5.460374474430324690E-16 ) ) ;
#14797 = ORIENTED_EDGE ( 'NONE', *, *, #24861, .F. ) ;
#14798 = CARTESIAN_POINT ( 'NONE',  ( -4.458734124999999437, -99.31249999863440792, 0.000000000000000000 ) ) ;
#14799 = DIRECTION ( 'NONE',  ( 0.000000000000000000, 1.000000000000000000, 0.000000000000000000 ) ) ;
#14800 = CARTESIAN_POINT ( 'NONE',  ( 2.229367062499998831, -12.64583333196774007, -3.861377020970580887 ) ) ;
#14801 = CARTESIAN_POINT ( 'NONE',  ( 1.975475456537005874E-15, -33.62499999726880873, 5.000000000000000000 ) ) ;
#14802 = CARTESIAN_POINT ( 'NONE',  ( 5.000000000000000888, 29.41666666666666785, 2.886751345948126879 ) ) ;
#14803 = CARTESIAN_POINT ( 'NONE',  ( -55.35523342533222291, -153.3125000013656063, 4.444560631937231499 ) ) ;
#14804 = CARTESIAN_POINT ( 'NONE',  ( 2.500000000000002220, -42.54166666393548013, 4.330127018922192761 ) ) ;
#14805 = LINE ( 'NONE', #50182, #6568 ) ;
#14806 = CARTESIAN_POINT ( 'NONE',  ( 4.458734124999998549, 12.27083333469892423, -2.574251347313721627 ) ) ;
#14807 = CARTESIAN_POINT ( 'NONE',  ( 6.874999999999997335, -4.690970937165716670, -7.298562697733105509 ) ) ;
#14808 = ORIENTED_EDGE ( 'NONE', *, *, #43189, .T. ) ;
#14809 = CARTESIAN_POINT ( 'NONE',  ( 2.229367062500001939, 16.02083333469892779, 3.861377020970579999 ) ) ;
#14810 = CARTESIAN_POINT ( 'NONE',  ( 4.458734124999998549, -63.72916666530107221, -2.574251347313721627 ) ) ;
#14811 = ORIENTED_EDGE ( 'NONE', *, *, #29103, .T. ) ;
#14812 = CARTESIAN_POINT ( 'NONE',  ( -3.152548672688508926E-16, -10.81249999863440792, -5.148502694627439702 ) ) ;
#14813 = CYLINDRICAL_SURFACE ( 'NONE', #37053, 5.000000000000000000 ) ;
#14814 = CARTESIAN_POINT ( 'NONE',  ( -2.500000000000000444, 2.833333333333333481, -4.330127018922193649 ) ) ;
#14815 = CARTESIAN_POINT ( 'NONE',  ( -3.152801135295367096, -168.0625000013656063, -3.152801135295367541 ) ) ;
#14816 = CARTESIAN_POINT ( 'NONE',  ( 5.000000000000000888, -63.45833333060215153, 2.886751345948126879 ) ) ;
#14817 = CARTESIAN_POINT ( 'NONE',  ( 4.458734124999999437, -53.81249999863439371, -5.460374474430324690E-16 ) ) ;
#14818 = CARTESIAN_POINT ( 'NONE',  ( -2.500000000000000444, -90.04166666393547303, -4.330127018922193649 ) ) ;
#14819 = CARTESIAN_POINT ( 'NONE',  ( 2.229367062499998831, -34.64583333196772941, -3.861377020970580887 ) ) ;
#14820 = CARTESIAN_POINT ( 'NONE',  ( -1.339745962155610925, -76.79465819873853150, 5.000000000000000000 ) ) ;
#14821 = CARTESIAN_POINT ( 'NONE',  ( 3.535533905932736864, -142.2500000027311842, 3.535533905932738641 ) ) ;
#14822 = LINE ( 'NONE', #25766, #10044 ) ;
#14823 = CARTESIAN_POINT ( 'NONE',  ( 4.458734124999997661, -154.7500000013656063, 1.846868145590737864 ) ) ;
#14824 = CARTESIAN_POINT ( 'NONE',  ( 5.000000000000000000, -40.49999999999999289, -6.123233995736766282E-16 ) ) ;
#14825 = CARTESIAN_POINT ( 'NONE',  ( -5.000000000000000000, -19.87499999726880873, 0.000000000000000000 ) ) ;
#14826 = CARTESIAN_POINT ( 'NONE',  ( -58.80597590150559739, -135.0000000000000284, 3.242614290531460330 ) ) ;
#14827 = ORIENTED_EDGE ( 'NONE', *, *, #54323, .T. ) ;
#14828 = CARTESIAN_POINT ( 'NONE',  ( -2.229367062499996610, -103.1458333319677365, 3.861377020970582219 ) ) ;
#14829 = CARTESIAN_POINT ( 'NONE',  ( 9.457646018065525792E-16, 2.687500001365594304, 5.148502694627439702 ) ) ;
#14830 = CARTESIAN_POINT ( 'NONE',  ( 1.975475456537005874E-15, -80.74999999999998579, 5.000000000000000000 ) ) ;
#14831 = CARTESIAN_POINT ( 'NONE',  ( 2.500000000000002220, -3.666666666666665186, 4.330127018922192761 ) ) ;
#14832 = CARTESIAN_POINT ( 'NONE',  ( -2.229367062499996610, -69.14583333196773651, 3.861377020970582219 ) ) ;
#14833 = CARTESIAN_POINT ( 'NONE',  ( 0.000000000000000000, 0.000000000000000000, -0.5251556536572846712 ) ) ;
#14834 = CARTESIAN_POINT ( 'NONE',  ( -4.999999999999999112, -1.791666663935480353, 2.886751345948131764 ) ) ;
#14836 = EDGE_LOOP ( 'NONE', ( #31588, #21110, #31381, #54750 ) ) ;
#14835 = CARTESIAN_POINT ( 'NONE',  ( 9.457646018065525792E-16, -33.06249999863440792, 5.148502694627439702 ) ) ;
#14837 = CARTESIAN_POINT ( 'NONE',  ( -57.46284108482265651, -144.0625000027312126, 4.819101127000238627 ) ) ;
#14838 = CARTESIAN_POINT ( 'NONE',  ( -5.000000000000000000, -47.95833333060215153, -2.886751345948128211 ) ) ;
#14839 =( BOUNDED_CURVE ( )  B_SPLINE_CURVE ( 2, ( #647, #6110, #59501, #10285, #983, #59829, #40820, #25725, #1305 ),
 .UNSPECIFIED., .F., .F. ) 
 B_SPLINE_CURVE_WITH_KNOTS ( ( 3, 2, 2, 2, 3 ),
 ( 0.06458333333333333981, 0.06527777777777778179, 0.06666666666666666574, 0.06805555555555554970, 0.06875000000000000555 ),
 .UNSPECIFIED. ) 
 CURVE ( )  GEOMETRIC_REPRESENTATION_ITEM ( )  RATIONAL_B_SPLINE_CURVE ( ( 0.9330127018922194093, 0.9330127018922200755, 1.000000000000000000, 0.8660254037844387076, 1.000000000000000000, 0.8660254037844387076, 1.000000000000000000, 0.9330127018922187432, 0.9330127018922194093 ) ) 
 REPRESENTATION_ITEM ( '' )  );
#14840 = CARTESIAN_POINT ( 'NONE',  ( -6.972266317189433020E-16, -11.25000000000000178, -5.000000000000000000 ) ) ;
#14841 = CARTESIAN_POINT ( 'NONE',  ( -5.000000000000000000, -46.08333333333333570, -2.886751345948128211 ) ) ;
#14844 = CARTESIAN_POINT ( 'NONE',  ( -2.229367062499996610, -25.39583333196773651, 3.861377020970582219 ) ) ;
#14843 =( BOUNDED_CURVE ( )  B_SPLINE_CURVE ( 2, ( #34599, #10168, #29772, #4393, #48139, #24012, #3775, #18563, #38186 ),
 .UNSPECIFIED., .F., .F. ) 
 B_SPLINE_CURVE_WITH_KNOTS ( ( 3, 2, 2, 2, 3 ),
 ( 0.01458333333333333356, 0.01527777777777777728, 0.01666666666666666644, 0.01805555555555555386, 0.01874999999999999931 ),
 .UNSPECIFIED. ) 
 CURVE ( )  GEOMETRIC_REPRESENTATION_ITEM ( )  RATIONAL_B_SPLINE_CURVE ( ( 0.9330127018922192983, 0.9330127018922194093, 1.000000000000000000, 0.8660254037844387076, 1.000000000000000000, 0.8660254037844387076, 1.000000000000000000, 0.9330127018922194093, 0.9330127018922194093 ) ) 
 REPRESENTATION_ITEM ( '' )  );
#14842 = CARTESIAN_POINT ( 'NONE',  ( 0.000000000000000000, -170.0000000000000000, 0.000000000000000000 ) ) ;
#14845 = CARTESIAN_POINT ( 'NONE',  ( 2.071067811865645591, -155.1875000000000000, 4.999999999999830358 ) ) ;
#14846 = CARTESIAN_POINT ( 'NONE',  ( -4.458734124999999437, -68.31249999863439371, 0.000000000000000000 ) ) ;
#14847 = CARTESIAN_POINT ( 'NONE',  ( -3.152801135295367985, -143.0625000013655779, 3.152801135295367096 ) ) ;
#14848 = CARTESIAN_POINT ( 'NONE',  ( -3.152548672688508926E-16, -82.56249999863442213, -5.148502694627439702 ) ) ;
#14849 = CARTESIAN_POINT ( 'NONE',  ( -55.35523342533222291, -137.5625000013656063, 4.444560631937231499 ) ) ;
#14850 = CARTESIAN_POINT ( 'NONE',  ( 4.458734124999998549, -32.97916666530106511, -2.574251347313721627 ) ) ;
#14851 = CARTESIAN_POINT ( 'NONE',  ( -2.499999999999996447, -73.70833333060214443, 4.330127018922195425 ) ) ;
#14852 = VERTEX_POINT ( 'NONE', #32278 ) ;
#14853 = CARTESIAN_POINT ( 'NONE',  ( 0.000000000000000000, -170.0000000000000000, 5.000000000000000000 ) ) ;
#14854 = ORIENTED_EDGE ( 'NONE', *, *, #55946, .F. ) ;
#14855 = CARTESIAN_POINT ( 'NONE',  ( 4.458734124999998549, -71.97916666530107932, -2.574251347313721627 ) ) ;
#14856 = CARTESIAN_POINT ( 'NONE',  ( -51.75738570946856498, -150.7500000000000284, 3.805975901505576964 ) ) ;
#14857 = VERTEX_POINT ( 'NONE', #3345 ) ;
#14858 = CARTESIAN_POINT ( 'NONE',  ( 2.500000000000002220, 27.33333333333333215, 4.330127018922192761 ) ) ;
#14859 = CARTESIAN_POINT ( 'NONE',  ( 2.500000000000002220, -12.66666666666666607, 4.330127018922192761 ) ) ;
#14861 = EDGE_CURVE ( 'NONE', #30862, #13218, #7846, .T. ) ;
#14860 = CARTESIAN_POINT ( 'NONE',  ( -3.152548672688508926E-16, -59.81249999863440792, -5.148502694627439702 ) ) ;
#14862 = CARTESIAN_POINT ( 'NONE',  ( -4.458734124999999437, -2.562499998634407028, 0.000000000000000000 ) ) ;
#14863 = ORIENTED_EDGE ( 'NONE', *, *, #41328, .T. ) ;
#14864 = VECTOR ( 'NONE', #47533, 1000.000000000000000 ) ;
#14865 = FACE_OUTER_BOUND ( 'NONE', #9176, .T. ) ;
#14866 = CARTESIAN_POINT ( 'NONE',  ( -56.37266686252615955, -135.0000000000000284, -4.242180533871957593 ) ) ;
#14867 =( BOUNDED_CURVE ( )  B_SPLINE_CURVE ( 2, ( #54489, #29705, #10417, #4633, #30028, #49657, #10738, #45148, #21348 ),
 .UNSPECIFIED., .F., .F. ) 
 B_SPLINE_CURVE_WITH_KNOTS ( ( 3, 2, 2, 2, 3 ),
 ( 0.09166666666666674346, 0.09583333333333342308, 0.1000000000000000888, 0.1041666666666667546, 0.1083333333333334203 ),
 .UNSPECIFIED. ) 
 CURVE ( )  GEOMETRIC_REPRESENTATION_ITEM ( )  RATIONAL_B_SPLINE_CURVE ( ( 0.9999999999999984457, 0.9238795325112882928, 1.000000000000000000, 0.9238795325112867385, 1.000000000000000000, 0.9238795325112867385, 1.000000000000000000, 0.9238795325112851842, 1.000000000000001554 ) ) 
 REPRESENTATION_ITEM ( '' )  );
#14868 = CARTESIAN_POINT ( 'NONE',  ( -4.458734124999999437, 12.68750000136559564, 0.000000000000000000 ) ) ;
#14869 = CARTESIAN_POINT ( 'NONE',  ( -55.35523342533222291, -141.3125000013656063, 4.444560631937231499 ) ) ;
#14870 = CARTESIAN_POINT ( 'NONE',  ( 5.000000000000000888, -27.45833333060214798, 2.886751345948126879 ) ) ;
#14871 = CARTESIAN_POINT ( 'NONE',  ( 1.846868145590736310, -163.6250000013656063, 4.458734124999997661 ) ) ;
#14872 = ORIENTED_EDGE ( 'NONE', *, *, #56312, .T. ) ;
#14873 = CARTESIAN_POINT ( 'NONE',  ( 4.458734124999999437, -78.81249999863440792, -5.460374474430324690E-16 ) ) ;
#14874 = CARTESIAN_POINT ( 'NONE',  ( 2.499999999999998668, -39.33333333333332860, -4.330127018922193649 ) ) ;
#14875 = CARTESIAN_POINT ( 'NONE',  ( -2.229367062499996610, 1.854166668032262377, 3.861377020970582219 ) ) ;
#14876 = CARTESIAN_POINT ( 'NONE',  ( -5.000000000000000000, -87.00000000000000000, 0.000000000000000000 ) ) ;
#14877 = EDGE_CURVE ( 'NONE', #23954, #48784, #4161, .T. ) ;
#14878 = CARTESIAN_POINT ( 'NONE',  ( -4.999999999999998224, -42.79166666393548013, 2.886751345948131764 ) ) ;
#14879 = CARTESIAN_POINT ( 'NONE',  ( -4.458734124999999437, -63.64583333196773651, -2.574251347313719407 ) ) ;
#14880 = CARTESIAN_POINT ( 'NONE',  ( -3.535250795749689387E-16, -25.12499999726881228, -5.773502691896257311 ) ) ;
#14881 = EDGE_CURVE ( 'NONE', #6575, #800, #49792, .T. ) ;
#14882 = CARTESIAN_POINT ( 'NONE',  ( 1.975475456537005874E-15, -0.6249999972688137229, 5.000000000000000000 ) ) ;
#14883 = CARTESIAN_POINT ( 'NONE',  ( 5.000000000000000000, -61.50000000000000000, -6.123233995736766282E-16 ) ) ;
#14884 = CARTESIAN_POINT ( 'NONE',  ( 2.493747252781420335E-13, -43.12499999726882294, -5.000000000000000000 ) ) ;
#14885 = CARTESIAN_POINT ( 'NONE',  ( -2.229367062499996610, -47.14583333196774362, 3.861377020970582219 ) ) ;
#14886 = CARTESIAN_POINT ( 'NONE',  ( -4.458734124999999437, -30.56249999863440436, 0.000000000000000000 ) ) ;
#14887 = CARTESIAN_POINT ( 'NONE',  ( -2.229367062499996610, 9.604166668032261711, 3.861377020970582219 ) ) ;
#14888 =( BOUNDED_CURVE ( )  B_SPLINE_CURVE ( 2, ( #32553, #37382, #47969, #13251, #3302, #2988, #42202, #3924, #52178 ),
 .UNSPECIFIED., .F., .F. ) 
 B_SPLINE_CURVE_WITH_KNOTS ( ( 3, 2, 2, 2, 3 ),
 ( 0.5410714285714285365, 0.5416666666666666297, 0.5428571428571428159, 0.5440476190476190022, 0.5446428571428570953 ),
 .UNSPECIFIED. ) 
 CURVE ( )  GEOMETRIC_REPRESENTATION_ITEM ( )  RATIONAL_B_SPLINE_CURVE ( ( 0.9330127018922194093, 0.9330127018922194093, 1.000000000000000000, 0.8660254037844387076, 1.000000000000000000, 0.8660254037844387076, 1.000000000000000000, 0.9330127018922194093, 0.9330127018922194093 ) ) 
 REPRESENTATION_ITEM ( '' )  );
#14889 = CARTESIAN_POINT ( 'NONE',  ( 0.000000000000000000, -170.0000000000000000, 0.000000000000000000 ) ) ;
#14890 = CARTESIAN_POINT ( 'NONE',  ( 5.000000000000000000, 24.58333333333333215, -2.886751345948129988 ) ) ;
#14891 = CARTESIAN_POINT ( 'NONE',  ( -5.000000000000000888, -150.6875000027312126, -2.071067811865475949 ) ) ;
#14892 = CARTESIAN_POINT ( 'NONE',  ( -1.339745962155612258, 29.20534180126147916, 5.000000000000000000 ) ) ;
#14893 = CARTESIAN_POINT ( 'NONE',  ( -4.458734124999998549, -36.22916666530106511, 2.574251347313722516 ) ) ;
#14894 = CARTESIAN_POINT ( 'NONE',  ( -2.499999999999996447, -72.70833333060214443, 4.330127018922195425 ) ) ;
#14895 = EDGE_CURVE ( 'NONE', #46124, #43789, #62954, .T. ) ;
#14896 = CARTESIAN_POINT ( 'NONE',  ( -59.29741812935640155, -143.8750000013655779, -2.196230717870135685 ) ) ;
#14897 = CARTESIAN_POINT ( 'NONE',  ( 3.535533905932736864, -143.1250000000000000, 3.535533905932738641 ) ) ;
#14898 = CARTESIAN_POINT ( 'NONE',  ( 3.535533905932738197, -141.0000000027311842, -3.535533905932738197 ) ) ;
#14899 = CARTESIAN_POINT ( 'NONE',  ( -4.458734124999999437, -72.56249999863439371, 0.000000000000000000 ) ) ;
#14900 = CARTESIAN_POINT ( 'NONE',  ( -4.458734125000000326, -164.1250000013656063, 1.846868145590734089 ) ) ;
#14901 = CARTESIAN_POINT ( 'NONE',  ( 4.458734124999998549, -33.72916666530107221, -2.574251347313721627 ) ) ;
#14902 = CARTESIAN_POINT ( 'NONE',  ( 7.894787914004607998, 1.243647571710251278E-13, -7.591390474663425536 ) ) ;
#14903 = CARTESIAN_POINT ( 'NONE',  ( 0.000000000000000000, -120.0000000000000000, 0.000000000000000000 ) ) ;
#14904 = CARTESIAN_POINT ( 'NONE',  ( 5.000000000000000000, -24.41666666666666430, -2.886751345948129988 ) ) ;
#14905 = CARTESIAN_POINT ( 'NONE',  ( -4.458734125000000326, -144.0000000013655779, -1.846868145590735644 ) ) ;
#14906 = ORIENTED_EDGE ( 'NONE', *, *, #59057, .F. ) ;
#14907 = AXIS2_PLACEMENT_3D ( 'NONE', #5302, #59985, #36168 ) ;
#14908 = CARTESIAN_POINT ( 'NONE',  ( 5.000000000000000000, -90.29166666393547303, -2.886751345948129988 ) ) ;
#14909 = VERTEX_POINT ( 'NONE', #4577 ) ;
#14910 = CARTESIAN_POINT ( 'NONE',  ( -2.229367062499996610, -60.39583333196774362, 3.861377020970582219 ) ) ;
#14911 = CARTESIAN_POINT ( 'NONE',  ( -5.000000000000000000, 22.04166666939785202, -2.886751345948128211 ) ) ;
#14912 = CARTESIAN_POINT ( 'NONE',  ( -2.500000000000000444, 14.83333333333333215, -4.330127018922193649 ) ) ;
#14913 = CARTESIAN_POINT ( 'NONE',  ( -2.229367062499996610, -53.14583333196773651, 3.861377020970582219 ) ) ;
#14914 = AXIS2_PLACEMENT_3D ( 'NONE', #57448, #13372, #61957 ) ;
#14915 = CARTESIAN_POINT ( 'NONE',  ( 2.229367062499998831, -4.645833331967740065, -3.861377020970580887 ) ) ;
#14916 = CARTESIAN_POINT ( 'NONE',  ( -4.999999999999998224, -22.91666666666666785, 2.886751345948131764 ) ) ;
#14917 = EDGE_CURVE ( 'NONE', #62567, #27206, #23875, .T. ) ;
#14918 = CARTESIAN_POINT ( 'NONE',  ( -1.339745962155610925, -76.79465819873853150, 5.000000000000000000 ) ) ;
#14919 = CARTESIAN_POINT ( 'NONE',  ( 2.071067811865582087, -158.3125000027312126, 4.999999999999894307 ) ) ;
#14920 = CARTESIAN_POINT ( 'NONE',  ( -5.134616530693496727E-16, 8.716839668575667943, -7.700121441565823233 ) ) ;
#14922 = CARTESIAN_POINT ( 'NONE',  ( 2.229367062499998831, -19.64583333196774007, -3.861377020970580887 ) ) ;
#14921 = CARTESIAN_POINT ( 'NONE',  ( -6.972266317189433020E-16, -0.1249999972688142225, -5.000000000000000000 ) ) ;
#14923 = CARTESIAN_POINT ( 'NONE',  ( 6.123233995736766282E-16, -120.0000000000000000, -5.000000000000000000 ) ) ;
#14924 = CARTESIAN_POINT ( 'NONE',  ( -4.458734124999999437, -55.31249999863440081, 0.000000000000000000 ) ) ;
#14925 = CARTESIAN_POINT ( 'NONE',  ( 1.846868145590735200, -155.5000000013655779, -4.458734125000000326 ) ) ;
#14926 = CARTESIAN_POINT ( 'NONE',  ( -5.000000000000000000, -54.87499999726880162, 0.000000000000000000 ) ) ;
#14927 = VERTEX_POINT ( 'NONE', #57992 ) ;
#14928 = CARTESIAN_POINT ( 'NONE',  ( 5.000000000000000000, -26.49999999999999645, -6.123233995736766282E-16 ) ) ;
#14929 = CARTESIAN_POINT ( 'NONE',  ( -2.229367062499996610, 6.604166668032259935, 3.861377020970582219 ) ) ;
#14930 = VERTEX_POINT ( 'NONE', #44124 ) ;
#14932 = CARTESIAN_POINT ( 'NONE',  ( -1.339745962155613812, -68.08034179853028434, -5.000000000000000000 ) ) ;
#14931 = CYLINDRICAL_SURFACE ( 'NONE', #37887, 5.000000000000000000 ) ;
#14933 = CARTESIAN_POINT ( 'NONE',  ( -3.152801135295367985, -157.8125000013656063, 3.152801135295367096 ) ) ;
#14934 = VERTEX_POINT ( 'NONE', #34468 ) ;
#14935 = CARTESIAN_POINT ( 'NONE',  ( 2.500000000000002220, -87.54166666393547303, 4.330127018922192761 ) ) ;
#14936 = CARTESIAN_POINT ( 'NONE',  ( -58.24261429053147765, -132.2500000000000284, -3.805975901505573855 ) ) ;
#14937 = CARTESIAN_POINT ( 'NONE',  ( -5.000000000000000000, -58.87499999726880873, 0.000000000000000000 ) ) ;
#14939 = EDGE_CURVE ( 'NONE', #62925, #47452, #49283, .T. ) ;
#14938 = CARTESIAN_POINT ( 'NONE',  ( 2.229367062499998831, -42.89583333196773651, -3.861377020970580887 ) ) ;
#14940 = ORIENTED_EDGE ( 'NONE', *, *, #56329, .T. ) ;
#14941 = EDGE_CURVE ( 'NONE', #34224, #28303, #30437, .T. ) ;
#14942 = EDGE_CURVE ( 'NONE', #56674, #28481, #8784, .T. ) ;
#14943 = CARTESIAN_POINT ( 'NONE',  ( -2.071067811865391128, -145.6875000000000284, -5.000000000000086153 ) ) ;
#14944 = CARTESIAN_POINT ( 'NONE',  ( 2.229367062499998831, 17.35416666803225993, -3.861377020970580887 ) ) ;
#14945 = CARTESIAN_POINT ( 'NONE',  ( -1.339745962155610925, -84.79465819873851729, 5.000000000000000000 ) ) ;
#14946 = VERTEX_POINT ( 'NONE', #52850 ) ;
#14947 = CARTESIAN_POINT ( 'NONE',  ( -2.229367062499996610, 28.85416666803226349, 3.861377020970582219 ) ) ;
#14948 = CARTESIAN_POINT ( 'NONE',  ( -53.51423613279429503, -152.2500000013656347, 4.591703134518082763 ) ) ;
#14949 = DIRECTION ( 'NONE',  ( 0.4999999999999951150, 0.000000000000000000, -0.8660254037844414832 ) ) ;
#14950 = CARTESIAN_POINT ( 'NONE',  ( -50.61409141273333745, -135.0000000000000568, -1.008919204746617782 ) ) ;
#14951 = CARTESIAN_POINT ( 'NONE',  ( -55.00000000000002132, 15.00000000000000000, -5.000000000000000000 ) ) ;
#14952 = CARTESIAN_POINT ( 'NONE',  ( 2.229367062499998831, -61.64583333196774362, -3.861377020970580887 ) ) ;
#14953 = CARTESIAN_POINT ( 'NONE',  ( 2.387978478801324300, 7.281554020289410012, -7.069802615102035226 ) ) ;
#14954 = CARTESIAN_POINT ( 'NONE',  ( 2.229367062499998831, 15.35416666803225993, -3.861377020970580887 ) ) ;
#14955 = EDGE_CURVE ( 'NONE', #58407, #30540, #25940, .T. ) ;
#14956 = AXIS2_PLACEMENT_3D ( 'NONE', #26283, #16002, #55254 ) ;
#14957 = CARTESIAN_POINT ( 'NONE',  ( -6.000000000000000000, -120.0000000000000000, 1.499999999999999556 ) ) ;
#14958 = CARTESIAN_POINT ( 'NONE',  ( 4.458734124999999437, -52.06249999863440792, -5.460374474430324690E-16 ) ) ;
#14959 = CARTESIAN_POINT ( 'NONE',  ( 1.060575238724906964E-15, -11.62499999726881761, 5.773502691896257311 ) ) ;
#14960 = CARTESIAN_POINT ( 'NONE',  ( 1.975475456537005874E-15, 5.250000000000000000, 5.000000000000000000 ) ) ;
#14961 = EDGE_CURVE ( 'NONE', #43716, #62883, #59190, .T. ) ;
#14962 = CARTESIAN_POINT ( 'NONE',  ( 0.000000000000000000, -120.0000000000000000, 0.000000000000000000 ) ) ;
#14963 = CARTESIAN_POINT ( 'NONE',  ( -2.229367062500000163, -87.72916666530107932, -3.861377020970580443 ) ) ;
#14964 = CARTESIAN_POINT ( 'NONE',  ( 2.229367062500001939, -106.9791666653010651, 3.861377020970579999 ) ) ;
#14965 = CARTESIAN_POINT ( 'NONE',  ( 4.458734125000000326, -15.14583333196773474, 2.574251347313718519 ) ) ;
#14966 = ORIENTED_EDGE ( 'NONE', *, *, #31900, .F. ) ;
#14967 = CARTESIAN_POINT ( 'NONE',  ( -3.535533905932737309, -169.6250000000000284, -3.535533905932738197 ) ) ;
#14968 = CARTESIAN_POINT ( 'NONE',  ( 4.458734124999999437, -98.81249999863440792, -5.460374474430324690E-16 ) ) ;
#14969 = CARTESIAN_POINT ( 'NONE',  ( 5.000000000000000888, -161.0625000027312126, -2.071067811865475505 ) ) ;
#14970 = CARTESIAN_POINT ( 'NONE',  ( 2.229367062500001939, -98.22916666530105090, 3.861377020970579999 ) ) ;
#14971 = CARTESIAN_POINT ( 'NONE',  ( 2.499999999999998668, -19.20833333060214798, -4.330127018922193649 ) ) ;
#14972 = CARTESIAN_POINT ( 'NONE',  ( -5.000000000000000000, -57.95833333060215153, -2.886751345948128211 ) ) ;
#14973 = CARTESIAN_POINT ( 'NONE',  ( 1.975475456537005874E-15, -5.750000000000000000, 5.000000000000000000 ) ) ;
#14974 =( BOUNDED_CURVE ( )  B_SPLINE_CURVE ( 2, ( #54972, #45952, #60128, #35042, #1598, #16375, #35994, #59485, #21522 ),
 .UNSPECIFIED., .F., .F. ) 
 B_SPLINE_CURVE_WITH_KNOTS ( ( 3, 2, 2, 2, 3 ),
 ( 0.008928571428571429811, 0.009523809523809524669, 0.01071428571428571438, 0.01190476190476190410, 0.01250000000000000069 ),
 .UNSPECIFIED. ) 
 CURVE ( )  GEOMETRIC_REPRESENTATION_ITEM ( )  RATIONAL_B_SPLINE_CURVE ( ( 0.9330127018922192983, 0.9330127018922194093, 1.000000000000000000, 0.8660254037844387076, 1.000000000000000000, 0.8660254037844387076, 1.000000000000000000, 0.9330127018922191873, 0.9330127018922192983 ) ) 
 REPRESENTATION_ITEM ( '' )  );
#14975 = CARTESIAN_POINT ( 'NONE',  ( -55.35523342533222291, -154.5625000013656347, 4.444560631937231499 ) ) ;
#14976 = CARTESIAN_POINT ( 'NONE',  ( -50.70258187064364108, -146.1250000013656063, 2.196230717870141014 ) ) ;
#14977 = CARTESIAN_POINT ( 'NONE',  ( 9.457646018065525792E-16, -19.06249999863440792, 5.148502694627439702 ) ) ;
#14978 = CARTESIAN_POINT ( 'NONE',  ( 4.458734125000001214, 7.854166668032260823, 2.574251347313718519 ) ) ;
#14979 = CARTESIAN_POINT ( 'NONE',  ( -4.458734124999999437, -59.56249999863440081, 0.000000000000000000 ) ) ;
#14980 = CARTESIAN_POINT ( 'NONE',  ( 1.339745962155612702, -94.16965819600731891, -5.000000000000000000 ) ) ;
#14981 = CARTESIAN_POINT ( 'NONE',  ( 4.458734125000000326, -16.89583333196773651, 2.574251347313718519 ) ) ;
#14982 = CARTESIAN_POINT ( 'NONE',  ( 0.000000000000000000, -120.0000000000000000, 0.000000000000000000 ) ) ;
#14983 = CARTESIAN_POINT ( 'NONE',  ( 5.000000000000000000, -153.0625000000000000, 2.071067811865478614 ) ) ;
#14984 = CARTESIAN_POINT ( 'NONE',  ( 5.000000000000000000, -3.500000000000003109, -6.123233995736766282E-16 ) ) ;
#14985 = VERTEX_POINT ( 'NONE', #24202 ) ;
#14986 = CARTESIAN_POINT ( 'NONE',  ( 2.229367062499998831, -48.89583333196772941, -3.861377020970580887 ) ) ;
#14987 = CARTESIAN_POINT ( 'NONE',  ( -2.499999999999996447, 26.16666666666666430, 4.330127018922195425 ) ) ;
#14988 = CARTESIAN_POINT ( 'NONE',  ( -6.486836893983275232, 4.915077010913945443, -7.231838333420560261 ) ) ;
#14989 = CARTESIAN_POINT ( 'NONE',  ( -6.127431526422343306E-17, 9.147862274876549904, -8.047472243342932430 ) ) ;
#14990 = CARTESIAN_POINT ( 'NONE',  ( -2.229367062500000163, -90.47916666530106511, -3.861377020970580443 ) ) ;
#14991 = CARTESIAN_POINT ( 'NONE',  ( 2.229367062499998831, 19.10416666803225993, -3.861377020970580887 ) ) ;
#14992 = CARTESIAN_POINT ( 'NONE',  ( -2.229367062500000163, 9.520833334698927786, -3.861377020970580443 ) ) ;
#14993 =( BOUNDED_CURVE ( )  B_SPLINE_CURVE ( 2, ( #8605, #47829, #53296, #57821, #28215, #3790, #37883, #52363, #19189 ),
 .UNSPECIFIED., .F., .F. ) 
 B_SPLINE_CURVE_WITH_KNOTS ( ( 3, 2, 2, 2, 3 ),
 ( 0.1145833333333333426, 0.1152777777777777846, 0.1166666666666666685, 0.1180555555555555525, 0.1187500000000000083 ),
 .UNSPECIFIED. ) 
 CURVE ( )  GEOMETRIC_REPRESENTATION_ITEM ( )  RATIONAL_B_SPLINE_CURVE ( ( 0.9330127018922194093, 0.9330127018922200755, 1.000000000000000000, 0.8660254037844387076, 1.000000000000000000, 0.8660254037844387076, 1.000000000000000000, 0.9330127018922187432, 0.9330127018922194093 ) ) 
 REPRESENTATION_ITEM ( '' )  );
#14994 = CARTESIAN_POINT ( 'NONE',  ( -2.500000000000000444, -44.16666666666665719, -4.330127018922193649 ) ) ;
#14995 = CARTESIAN_POINT ( 'NONE',  ( -2.229367062500000163, -87.72916666530107932, -3.861377020970580443 ) ) ;
#14996 = CARTESIAN_POINT ( 'NONE',  ( 4.458734125000001214, 19.85416666803226349, 2.574251347313718519 ) ) ;
#14997 = CARTESIAN_POINT ( 'NONE',  ( 5.000000000000000888, -74.58333333333332860, 2.886751345948126879 ) ) ;
#14998 = CARTESIAN_POINT ( 'NONE',  ( -4.999999999999999112, 7.208333336064517205, 2.886751345948131764 ) ) ;
#14999 = ORIENTED_EDGE ( 'NONE', *, *, #30650, .T. ) ;
#15000 = CARTESIAN_POINT ( 'NONE',  ( 2.499999999999998668, -102.3333333333333286, -4.330127018922193649 ) ) ;
#15001 = ORIENTED_EDGE ( 'NONE', *, *, #5119, .T. ) ;
#15002 = VECTOR ( 'NONE', #45794, 1000.000000000000000 ) ;
#15004 = CARTESIAN_POINT ( 'NONE',  ( -4.999999999999999112, -33.91666666666666430, 2.886751345948131764 ) ) ;
#15003 = CARTESIAN_POINT ( 'NONE',  ( 1.975475456537005874E-15, -4.749999999999999112, 5.000000000000000000 ) ) ;
#15005 = CARTESIAN_POINT ( 'NONE',  ( -3.152548672688508926E-16, -40.56249999863440081, -5.148502694627439702 ) ) ;
#15006 = VECTOR ( 'NONE', #3526, 1000.000000000000000 ) ;
#15007 = CARTESIAN_POINT ( 'NONE',  ( 5.000000000000000888, -33.45833333060215153, 2.886751345948126879 ) ) ;
#15008 = ORIENTED_EDGE ( 'NONE', *, *, #44726, .T. ) ;
#15009 = CARTESIAN_POINT ( 'NONE',  ( -55.35523342533222291, -149.5625000013656063, 4.444560631937231499 ) ) ;
#15010 = CARTESIAN_POINT ( 'NONE',  ( -4.458734124999999437, -11.39583333196774007, -2.574251347313719407 ) ) ;
#15012 = ORIENTED_EDGE ( 'NONE', *, *, #61486, .F. ) ;
#15011 = CARTESIAN_POINT ( 'NONE',  ( -4.458734124999999437, -16.56249999863440436, 0.000000000000000000 ) ) ;
#15013 = CARTESIAN_POINT ( 'NONE',  ( -5.000000000000000000, -84.08333333333332860, -2.886751345948128211 ) ) ;
#15014 = CARTESIAN_POINT ( 'NONE',  ( 4.458734125000000326, -169.3750000013656347, -1.846868145590734978 ) ) ;
#15015 = CARTESIAN_POINT ( 'NONE',  ( -4.458734124999999437, -56.64583333196773651, -2.574251347313719407 ) ) ;
#15016 = CARTESIAN_POINT ( 'NONE',  ( 1.060575238724906964E-15, -83.62499999726881583, 5.773502691896257311 ) ) ;
#15018 = EDGE_LOOP ( 'NONE', ( #39066, #19526, #59859, #56243 ) ) ;
#15017 = DIRECTION ( 'NONE',  ( -0.000000000000000000, 1.000000000000000000, -0.000000000000000000 ) ) ;
#15019 = CARTESIAN_POINT ( 'NONE',  ( -60.14911071818854538, -144.0625000000000284, 1.666127454062681368 ) ) ;
#15020 = CARTESIAN_POINT ( 'NONE',  ( -4.458734124999999437, -28.64583333196774007, -2.574251347313719407 ) ) ;
#15021 = CARTESIAN_POINT ( 'NONE',  ( -2.499999999999996447, -49.83333333333332860, 4.330127018922195425 ) ) ;
#15022 = ORIENTED_EDGE ( 'NONE', *, *, #62834, .F. ) ;
#15023 = EDGE_CURVE ( 'NONE', #41751, #10933, #18977, .T. ) ;
#15024 = CONTEXT_DEPENDENT_SHAPE_REPRESENTATION ( #36399, #3992 ) ;
#15025 = CARTESIAN_POINT ( 'NONE',  ( -3.152801135295367096, -163.3125000013656063, -3.152801135295367541 ) ) ;
#15026 = CARTESIAN_POINT ( 'NONE',  ( -2.229367062500000163, -102.7291666653010651, -3.861377020970580443 ) ) ;
#15027 = CARTESIAN_POINT ( 'NONE',  ( -6.972266317189433020E-16, -23.24999999999999645, -5.000000000000000000 ) ) ;
#15028 = VERTEX_POINT ( 'NONE', #49597 ) ;
#15029 = CARTESIAN_POINT ( 'NONE',  ( -50.40829686548195099, -148.2500000013656347, -1.485763867205728284 ) ) ;
#15030 = CARTESIAN_POINT ( 'NONE',  ( 9.457646018065525792E-16, -73.31249999863440792, 5.148502694627439702 ) ) ;
#15031 = CARTESIAN_POINT ( 'NONE',  ( -50.01589407740564042, -138.7500000027312126, 0.3983568153799778022 ) ) ;
#15032 = CARTESIAN_POINT ( 'NONE',  ( -4.458734124999999437, -43.31249999863440081, 0.000000000000000000 ) ) ;
#15033 = CARTESIAN_POINT ( 'NONE',  ( -3.152801135295367985, -147.0625000013655779, 3.152801135295367096 ) ) ;
#15034 = EDGE_CURVE ( 'NONE', #20024, #1425, #54752, .T. ) ;
#15035 = CARTESIAN_POINT ( 'NONE',  ( 1.975475456537005874E-15, 6.375000002731185944, 5.000000000000000000 ) ) ;
#15036 = CARTESIAN_POINT ( 'NONE',  ( -4.999999999999998224, 0.08333333333333454995, 2.886751345948131764 ) ) ;
#15037 = EDGE_CURVE ( 'NONE', #5644, #29232, #43574, .T. ) ;
#15038 = CARTESIAN_POINT ( 'NONE',  ( -2.229367062499996610, -15.14583333196773474, 3.861377020970582219 ) ) ;
#15039 = CARTESIAN_POINT ( 'NONE',  ( 5.000000000000000000, -102.4166666666666572, -2.886751345948129988 ) ) ;
#15040 = ORIENTED_EDGE ( 'NONE', *, *, #52830, .T. ) ;
#15041 = CARTESIAN_POINT ( 'NONE',  ( -1.975475456537005874E-15, 28.37500000273118772, 5.000000000000000000 ) ) ;
#15042 = CARTESIAN_POINT ( 'NONE',  ( 4.458734125000001214, -34.14583333196772941, 2.574251347313718519 ) ) ;
#15043 = CARTESIAN_POINT ( 'NONE',  ( 1.060575238724906964E-15, 6.375000002731185056, 5.773502691896257311 ) ) ;
#15044 = CARTESIAN_POINT ( 'NONE',  ( -6.972266317189433020E-16, -86.12499999726880162, -5.000000000000000000 ) ) ;
#15045 = CARTESIAN_POINT ( 'NONE',  ( -59.29741812935640155, -133.6250000013655779, -2.196230717870135685 ) ) ;
#15046 = CARTESIAN_POINT ( 'NONE',  ( -4.458734124999999437, -73.64583333196773651, -2.574251347313719407 ) ) ;
#15047 = ADVANCED_FACE ( 'NONE', ( #35444 ), #59254, .T. ) ;
#15048 = DIRECTION ( 'NONE',  ( 1.000000000000000000, 0.000000000000000000, 0.000000000000000000 ) ) ;
#15049 = CARTESIAN_POINT ( 'NONE',  ( -6.972266317189433020E-16, -70.25000000000000000, -5.000000000000000000 ) ) ;
#15050 = CYLINDRICAL_SURFACE ( 'NONE', #62423, 5.000000000000000000 ) ;
#15051 = CARTESIAN_POINT ( 'NONE',  ( 4.458734124999999437, 6.937500001365594748, -5.460374474430324690E-16 ) ) ;
#15052 =( BOUNDED_CURVE ( )  B_SPLINE_CURVE ( 2, ( #59643, #59968, #60607, #40645, #10100, #40959, #50620, #5600, #1753 ),
 .UNSPECIFIED., .F., .F. ) 
 B_SPLINE_CURVE_WITH_KNOTS ( ( 3, 2, 2, 2, 3 ),
 ( 0.7446428571428571619, 0.7452380952380952550, 0.7464285714285714413, 0.7476190476190476275, 0.7482142857142857206 ),
 .UNSPECIFIED. ) 
 CURVE ( )  GEOMETRIC_REPRESENTATION_ITEM ( )  RATIONAL_B_SPLINE_CURVE ( ( 0.9330127018922194093, 0.9330127018922194093, 1.000000000000000000, 0.8660254037844387076, 1.000000000000000000, 0.8660254037844387076, 1.000000000000000000, 0.9330127018922194093, 0.9330127018922194093 ) ) 
 REPRESENTATION_ITEM ( '' )  );
#15053 = ORIENTED_EDGE ( 'NONE', *, *, #51137, .T. ) ;
#15054 = AXIS2_PLACEMENT_3D ( 'NONE', #4476, #28290, #53052 ) ;
#15055 = CARTESIAN_POINT ( 'NONE',  ( 2.071067811865560326, -145.8125000000000284, -4.999999999999914735 ) ) ;
#15056 = ADVANCED_FACE ( 'NONE', ( #5863 ), #35137, .F. ) ;
#15057 = CARTESIAN_POINT ( 'NONE',  ( -1.339745962155613812, -76.20534180126146850, -5.000000000000000000 ) ) ;
#15059 = CARTESIAN_POINT ( 'NONE',  ( -2.229367062500000163, -31.47916666530107577, -3.861377020970580443 ) ) ;
#15058 = CARTESIAN_POINT ( 'NONE',  ( 2.499999999999998668, -98.33333333333332860, -4.330127018922193649 ) ) ;
#15060 = CARTESIAN_POINT ( 'NONE',  ( 2.500000000000002220, -95.66666666666664298, 4.330127018922192761 ) ) ;
#15061 = CARTESIAN_POINT ( 'NONE',  ( 4.458734124999998549, -82.97916666530107932, -2.574251347313721627 ) ) ;
#15062 = VECTOR ( 'NONE', #36309, 1000.000000000000000 ) ;
#15063 = CARTESIAN_POINT ( 'NONE',  ( -4.458734124999999437, 19.43750000136559208, 0.000000000000000000 ) ) ;
#15064 = CARTESIAN_POINT ( 'NONE',  ( -2.499999999999996447, 27.16666666666666430, 4.330127018922195425 ) ) ;
#15065 = VECTOR ( 'NONE', #23602, 1000.000000000000000 ) ;
#15066 = CARTESIAN_POINT ( 'NONE',  ( -50.40829686548195099, -137.0000000013655779, -1.485763867205728284 ) ) ;
#15067 = ADVANCED_FACE ( 'NONE', ( #55392 ), #11308, .T. ) ;
#15068 = CARTESIAN_POINT ( 'NONE',  ( -2.229367062500000163, -1.479166665301071770, -3.861377020970580443 ) ) ;
#15069 = CARTESIAN_POINT ( 'NONE',  ( 4.458734125000001214, 20.85416666803226349, 2.574251347313718519 ) ) ;
#15070 = CARTESIAN_POINT ( 'NONE',  ( -2.229367062500000163, -44.72916666530106511, -3.861377020970580443 ) ) ;
#15071 = CARTESIAN_POINT ( 'NONE',  ( -2.229367062499996610, 2.854166668032259935, 3.861377020970582219 ) ) ;
#15072 = CARTESIAN_POINT ( 'NONE',  ( -2.229367062500000163, -22.72916666530107221, -3.861377020970580443 ) ) ;
#15073 = CARTESIAN_POINT ( 'NONE',  ( 4.458734124999999437, -67.81249999863440792, -5.460374474430324690E-16 ) ) ;
#15074 = CARTESIAN_POINT ( 'NONE',  ( 1.060575238724906964E-15, -106.6249999972688016, 5.773502691896257311 ) ) ;
#15075 = CARTESIAN_POINT ( 'NONE',  ( 9.457646018065525792E-16, 24.93750000136559564, 5.148502694627439702 ) ) ;
#15076 = CARTESIAN_POINT ( 'NONE',  ( 1.339745962155615144, -58.58034179853029855, 4.999999999999999112 ) ) ;
#15077 = CARTESIAN_POINT ( 'NONE',  ( -58.24261429053147765, -153.3750000027312126, -3.805975901505573855 ) ) ;
#15078 = CARTESIAN_POINT ( 'NONE',  ( -4.458734124999997661, -70.47916666530107932, 2.574251347313722516 ) ) ;
#15079 = CARTESIAN_POINT ( 'NONE',  ( 2.499999999999998668, -59.33333333333333570, -4.330127018922193649 ) ) ;
#15080 = CARTESIAN_POINT ( 'NONE',  ( -2.499999999999996447, -65.70833333060213022, 4.330127018922195425 ) ) ;
#15081 = CARTESIAN_POINT ( 'NONE',  ( 5.000000000000000000, 25.62500000273118417, -6.123233995736766282E-16 ) ) ;
#15082 = ORIENTED_EDGE ( 'NONE', *, *, #40113, .T. ) ;
#15083 = CARTESIAN_POINT ( 'NONE',  ( 1.339745962155612702, 6.705341801261480050, -5.000000000000000000 ) ) ;
#15084 =( BOUNDED_CURVE ( )  B_SPLINE_CURVE ( 2, ( #48717, #43571, #49681, #54184, #4658, #20091, #23968, #35214, #63215 ),
 .UNSPECIFIED., .F., .F. ) 
 B_SPLINE_CURVE_WITH_KNOTS ( ( 3, 2, 2, 2, 3 ),
 ( 0.8583333333333330595, 0.8624999999999998224, 0.8666666666666664742, 0.8708333333333332371, 0.8749999999999998890 ),
 .UNSPECIFIED. ) 
 CURVE ( )  GEOMETRIC_REPRESENTATION_ITEM ( )  RATIONAL_B_SPLINE_CURVE ( ( 1.000000000000003997, 0.9238795325112826307, 1.000000000000000000, 0.9238795325112867385, 1.000000000000000000, 0.9238795325112867385, 1.000000000000000000, 0.9238795325112887369, 0.9999999999999980016 ) ) 
 REPRESENTATION_ITEM ( '' )  );
#15085 = CARTESIAN_POINT ( 'NONE',  ( -1.339745962155610925, -98.79465819873853150, 5.000000000000000000 ) ) ;
#15086 = CARTESIAN_POINT ( 'NONE',  ( 2.500000000000002220, -17.66666666666666430, 4.330127018922192761 ) ) ;
#15087 = CARTESIAN_POINT ( 'NONE',  ( -4.458734124999999437, -24.31249999863440436, 0.000000000000000000 ) ) ;
#15088 = CARTESIAN_POINT ( 'NONE',  ( 2.229367062500001939, -83.97916666530106511, 3.861377020970579999 ) ) ;
#15089 = CARTESIAN_POINT ( 'NONE',  ( 3.152801135295366208, -166.8125000013656063, 3.152801135295367985 ) ) ;
#15090 = CARTESIAN_POINT ( 'NONE',  ( 2.500000000000002220, -16.54166666393548368, 4.330127018922192761 ) ) ;
#15092 = ORIENTED_EDGE ( 'NONE', *, *, #10529, .F. ) ;
#15091 = CARTESIAN_POINT ( 'NONE',  ( 4.458734124999998549, -50.72916666530107932, -2.574251347313721627 ) ) ;
#15093 = CARTESIAN_POINT ( 'NONE',  ( 5.000000000000000000, -35.29166666393547303, -2.886751345948130876 ) ) ;
#15095 = EDGE_LOOP ( 'NONE', ( #18898, #20985, #48579, #36325 ) ) ;
#15094 = CARTESIAN_POINT ( 'NONE',  ( 4.458734125000001214, -0.1458333319677394824, 2.574251347313718519 ) ) ;
#15096 = CARTESIAN_POINT ( 'NONE',  ( -57.89159099828107458, -149.6875000013656063, -3.393966926194107447 ) ) ;
#15097 = CARTESIAN_POINT ( 'NONE',  ( 5.000000000000000000, -64.50000000000000000, -6.123233995736766282E-16 ) ) ;
#15098 = CARTESIAN_POINT ( 'NONE',  ( 4.458734124999999437, -151.7500000013655779, 1.846868145590737864 ) ) ;
#15099 = CARTESIAN_POINT ( 'NONE',  ( 4.458734124999999437, -41.06249999863440081, -5.460374474430324690E-16 ) ) ;
#15100 = CARTESIAN_POINT ( 'NONE',  ( 5.000000000000000888, -68.45833333060214443, 2.886751345948126879 ) ) ;
#15101 = CARTESIAN_POINT ( 'NONE',  ( 2.071067811865475505, -162.8125000000000000, -5.000000000000000888 ) ) ;
#15102 = DIRECTION ( 'NONE',  ( 0.000000000000000000, 0.000000000000000000, 1.000000000000000000 ) ) ;
#15103 = CARTESIAN_POINT ( 'NONE',  ( -50.55543936806279248, -126.3125000013655921, 0.3552334253322060320 ) ) ;
#15104 = CIRCLE ( 'NONE', #1820, 11.00000000000000000 ) ;
#15105 = CARTESIAN_POINT ( 'NONE',  ( 2.229367062500001939, -9.229166665301075767, 3.861377020970579999 ) ) ;
#15106 = AXIS2_PLACEMENT_3D ( 'NONE', #57392, #13313, #52558 ) ;
#15107 = CARTESIAN_POINT ( 'NONE',  ( 4.458734124999998549, -43.97916666530105800, -2.574251347313721627 ) ) ;
#15108 = CARTESIAN_POINT ( 'NONE',  ( 2.500000000000002220, -89.66666666666665719, 4.330127018922192761 ) ) ;
#15109 = CARTESIAN_POINT ( 'NONE',  ( 3.152801135295367541, -148.3125000013655779, -3.152801135295367541 ) ) ;
#15110 = CARTESIAN_POINT ( 'NONE',  ( 4.458734124999999437, -90.06249999863440792, -5.460374474430324690E-16 ) ) ;
#15111 = CARTESIAN_POINT ( 'NONE',  ( -59.98410592259440222, -150.1250000000000284, -0.3983568153799752487 ) ) ;
#15112 = ORIENTED_EDGE ( 'NONE', *, *, #11189, .T. ) ;
#15113 = CARTESIAN_POINT ( 'NONE',  ( -5.000000000000000000, -32.08333333333332860, -2.886751345948128211 ) ) ;
#15114 = DIRECTION ( 'NONE',  ( 0.000000000000000000, 0.000000000000000000, 1.000000000000000000 ) ) ;
#15115 = CARTESIAN_POINT ( 'NONE',  ( -56.66612745406270335, -151.4375000027311842, -5.149110718188516067 ) ) ;
#15116 = DIRECTION ( 'NONE',  ( -0.000000000000000000, 1.000000000000000000, -0.000000000000000000 ) ) ;
#15117 = VERTEX_POINT ( 'NONE', #725 ) ;
#15118 = CARTESIAN_POINT ( 'NONE',  ( 4.458734124999999437, 3.187500001365594304, -5.460374474430324690E-16 ) ) ;
#15119 = CARTESIAN_POINT ( 'NONE',  ( 5.000000000000000888, -50.45833333060213732, 2.886751345948126879 ) ) ;
#15120 = CARTESIAN_POINT ( 'NONE',  ( 4.458734124999998549, -18.97916666530107221, -2.574251347313721627 ) ) ;
#15121 = CARTESIAN_POINT ( 'NONE',  ( -6.972266317189433020E-16, -101.1249999972688158, -5.000000000000000000 ) ) ;
#15122 = CARTESIAN_POINT ( 'NONE',  ( -3.152548672688508926E-16, -4.562499998634401699, -5.148502694627439702 ) ) ;
#15123 = CARTESIAN_POINT ( 'NONE',  ( 4.458734124999999437, -149.3750000013656063, -1.846868145590734978 ) ) ;
#15124 = CARTESIAN_POINT ( 'NONE',  ( 2.229367062499998831, 21.10416666803226349, -3.861377020970580887 ) ) ;
#15125 = ORIENTED_EDGE ( 'NONE', *, *, #16199, .F. ) ;
#15126 = CARTESIAN_POINT ( 'NONE',  ( 4.458734124999999437, -99.81249999863440792, -5.460374474430324690E-16 ) ) ;
#15127 = CARTESIAN_POINT ( 'NONE',  ( -1.339745962155610925, -74.79465819873854571, 5.000000000000000000 ) ) ;
#15128 = CYLINDRICAL_SURFACE ( 'NONE', #39185, 5.000000000000000000 ) ;
#15129 = CARTESIAN_POINT ( 'NONE',  ( 2.229367062499998831, -14.64583333196773474, -3.861377020970580887 ) ) ;
#15130 = LINE ( 'NONE', #49853, #7824 ) ;
#15131 = CARTESIAN_POINT ( 'NONE',  ( 1.975475456537005874E-15, -12.74999999999999822, 5.000000000000000000 ) ) ;
#15132 = CARTESIAN_POINT ( 'NONE',  ( -58.39396692619412477, -152.4375000013656063, 2.891590998281057701 ) ) ;
#15133 = CARTESIAN_POINT ( 'NONE',  ( -5.000000000000000000, -40.95833333060215153, -2.886751345948128211 ) ) ;
#15134 = CARTESIAN_POINT ( 'NONE',  ( -51.75738570946856498, -148.7500000000000284, 3.805975901505576964 ) ) ;
#15135 = CARTESIAN_POINT ( 'NONE',  ( 4.458734124999999437, 12.18750000136559564, -5.460374474430324690E-16 ) ) ;
#15136 = CARTESIAN_POINT ( 'NONE',  ( -6.972266317189433020E-16, -84.24999999999998579, -5.000000000000000000 ) ) ;
#15137 = CARTESIAN_POINT ( 'NONE',  ( 1.975475456537005874E-15, -87.75000000000001421, 5.000000000000000000 ) ) ;
#15138 = CARTESIAN_POINT ( 'NONE',  ( -4.458734124999999437, 19.60416666803225993, -2.574251347313719407 ) ) ;
#15139 = CARTESIAN_POINT ( 'NONE',  ( -2.229367062500000163, -62.47916666530106511, -3.861377020970580443 ) ) ;
#15140 = ORIENTED_EDGE ( 'NONE', *, *, #14881, .F. ) ;
#15141 = CARTESIAN_POINT ( 'NONE',  ( 2.229367062500001939, -10.22916666530106866, 3.861377020970579999 ) ) ;
#15142 = VECTOR ( 'NONE', #34667, 1000.000000000000000 ) ;
#15143 = CARTESIAN_POINT ( 'NONE',  ( -5.000000000000000000, 5.999999999999998224, 0.000000000000000000 ) ) ;
#15144 = CARTESIAN_POINT ( 'NONE',  ( 3.152801135295366208, -167.5625000013656063, 3.152801135295367985 ) ) ;
#15145 = CARTESIAN_POINT ( 'NONE',  ( -58.24261429053147765, -142.2500000000000284, -3.805975901505573855 ) ) ;
#15146 = CARTESIAN_POINT ( 'NONE',  ( 9.457646018065525792E-16, -54.06249999863440081, 5.148502694627439702 ) ) ;
#15147 = CARTESIAN_POINT ( 'NONE',  ( 5.000000000000000888, -87.45833333060214443, 2.886751345948126879 ) ) ;
#15148 = AXIS2_PLACEMENT_3D ( 'NONE', #63663, #19580, #58819 ) ;
#15149 = CARTESIAN_POINT ( 'NONE',  ( 4.458734124999998549, -35.72916666530107221, -2.574251347313721627 ) ) ;
#15150 = DIRECTION ( 'NONE',  ( 0.000000000000000000, 0.000000000000000000, 1.000000000000000000 ) ) ;
#15151 = CARTESIAN_POINT ( 'NONE',  ( -6.972266317189433020E-16, -75.12499999726880162, -5.000000000000000000 ) ) ;
#15152 = CARTESIAN_POINT ( 'NONE',  ( -4.330127018922205195, 30.00000000000000000, -7.499999999999943157 ) ) ;
#15153 = CARTESIAN_POINT ( 'NONE',  ( 4.458734124999999437, -153.6250000013655779, -1.846868145590734978 ) ) ;
#15154 = CARTESIAN_POINT ( 'NONE',  ( -5.000000000000000000, -43.00000000000000000, 0.000000000000000000 ) ) ;
#15155 = CARTESIAN_POINT ( 'NONE',  ( 2.499999999999998668, -98.20833333060214443, -4.330127018922193649 ) ) ;
#15156 = CARTESIAN_POINT ( 'NONE',  ( -59.31337900967797339, -134.9999999999999716, -1.887341660144209454 ) ) ;
#15157 = ORIENTED_EDGE ( 'NONE', *, *, #36172, .F. ) ;
#15158 = CARTESIAN_POINT ( 'NONE',  ( -2.229367062499996610, -100.1458333319677365, 3.861377020970582219 ) ) ;
#15159 = CARTESIAN_POINT ( 'NONE',  ( -3.152548672688508926E-16, 1.187500001365596081, -5.148502694627439702 ) ) ;
#15160 = DIRECTION ( 'NONE',  ( -0.000000000000000000, 1.000000000000000000, -0.000000000000000000 ) ) ;
#15161 = CARTESIAN_POINT ( 'NONE',  ( 5.000000000000000888, -0.5833333333333350357, 2.886751345948126879 ) ) ;
#15162 = CARTESIAN_POINT ( 'NONE',  ( -4.458734124999999437, -69.39583333196773651, -2.574251347313719407 ) ) ;
#15163 = CARTESIAN_POINT ( 'NONE',  ( -1.339745962155610925, 20.20534180126147916, 5.000000000000000000 ) ) ;
#15164 = CARTESIAN_POINT ( 'NONE',  ( -3.535250795749689387E-16, -2.124999997268814944, -5.773502691896257311 ) ) ;
#15166 = EDGE_LOOP ( 'NONE', ( #61885, #59163, #13375, #9628 ) ) ;
#15165 = CARTESIAN_POINT ( 'NONE',  ( 4.458734124999998549, -33.72916666530106511, -2.574251347313721627 ) ) ;
#15167 = CARTESIAN_POINT ( 'NONE',  ( -5.000000000000000000, -78.00000000000000000, 0.000000000000000000 ) ) ;
#15168 = CARTESIAN_POINT ( 'NONE',  ( -9.184850993605147944E-16, -157.2500000000000000, 5.000000000000000000 ) ) ;
#15169 = ORIENTED_EDGE ( 'NONE', *, *, #18863, .T. ) ;
#15170 = CARTESIAN_POINT ( 'NONE',  ( 2.500000000000002220, 5.333333333333332149, 4.330127018922192761 ) ) ;
#15171 = CARTESIAN_POINT ( 'NONE',  ( -5.000000000000000000, -52.00000000000000711, 0.000000000000000000 ) ) ;
#15173 = CARTESIAN_POINT ( 'NONE',  ( -2.229367062500000163, -25.72916666530106866, -3.861377020970580443 ) ) ;
#15172 = CARTESIAN_POINT ( 'NONE',  ( 1.975475456537005874E-15, -26.62499999726881228, 5.000000000000000000 ) ) ;
#15174 = CARTESIAN_POINT ( 'NONE',  ( 4.458734125000001214, -71.89583333196773651, 2.574251347313718519 ) ) ;
#15175 = CARTESIAN_POINT ( 'NONE',  ( -8.190561711645485556E-16, -144.9375000013656063, 4.458734124999999437 ) ) ;
#15176 = CARTESIAN_POINT ( 'NONE',  ( 4.458734124999998549, -83.72916666530107932, -2.574251347313721627 ) ) ;
#15177 = CARTESIAN_POINT ( 'NONE',  ( -59.59170313451811296, -138.7500000013656063, 1.485763867205729394 ) ) ;
#15178 = CARTESIAN_POINT ( 'NONE',  ( -4.458734124999999437, -28.56249999863440081, 0.000000000000000000 ) ) ;
#15179 =( BOUNDED_CURVE ( )  B_SPLINE_CURVE ( 2, ( #50450, #39573, #58577, #24796, #30818 ),
 .UNSPECIFIED., .F., .F. ) 
 B_SPLINE_CURVE_WITH_KNOTS ( ( 3, 2, 3 ),
 ( 0.000000000000000000, 0.004166666666666670078, 0.008333333333333340157 ),
 .UNSPECIFIED. ) 
 CURVE ( )  GEOMETRIC_REPRESENTATION_ITEM ( )  RATIONAL_B_SPLINE_CURVE ( ( 1.000000000000000000, 0.9238795325112867385, 1.000000000000000000, 0.9238795325112866275, 1.000000000000000222 ) ) 
 REPRESENTATION_ITEM ( '' )  );
#15180 = CARTESIAN_POINT ( 'NONE',  ( -3.535250795749689387E-16, -74.12499999726880162, -5.773502691896257311 ) ) ;
#15181 = EDGE_LOOP ( 'NONE', ( #39686, #12419, #29485, #56570 ) ) ;
#15182 = CARTESIAN_POINT ( 'NONE',  ( 8.660254037844342889, 45.00000000000000000, 0.000000000000000000 ) ) ;
#15183 = EDGE_LOOP ( 'NONE', ( #5144, #9199, #22867, #9142 ) ) ;
#15184 = CARTESIAN_POINT ( 'NONE',  ( -4.458734124999998549, -73.47916666530106511, 2.574251347313722516 ) ) ;
#15185 = CARTESIAN_POINT ( 'NONE',  ( 2.500000000000002220, -21.66666666666666785, 4.330127018922192761 ) ) ;
#15186 = ORIENTED_EDGE ( 'NONE', *, *, #60858, .T. ) ;
#15187 = CARTESIAN_POINT ( 'NONE',  ( -2.500000000000000444, 16.83333333333333215, -4.330127018922193649 ) ) ;
#15188 = VECTOR ( 'NONE', #21718, 1000.000000000000000 ) ;
#15189 = CYLINDRICAL_SURFACE ( 'NONE', #44529, 5.000000000000000000 ) ;
#15190 = CARTESIAN_POINT ( 'NONE',  ( 2.229367062499998831, -57.89583333196773651, -3.861377020970580887 ) ) ;
#15191 = AXIS2_PLACEMENT_3D ( 'NONE', #62961, #546, #24027 ) ;
#15192 = CARTESIAN_POINT ( 'NONE',  ( 4.458734125000001214, -4.145833331967740065, 2.574251347313718519 ) ) ;
#15193 = ORIENTED_EDGE ( 'NONE', *, *, #4707, .F. ) ;
#15194 = CARTESIAN_POINT ( 'NONE',  ( 3.535533905932738197, -141.8750000000000000, -3.535533905932738197 ) ) ;
#15195 = DIRECTION ( 'NONE',  ( 0.000000000000000000, 0.000000000000000000, 1.000000000000000000 ) ) ;
#15196 = CARTESIAN_POINT ( 'NONE',  ( -4.458734124999998549, 15.77083333469892601, 2.574251347313722516 ) ) ;
#15197 = CARTESIAN_POINT ( 'NONE',  ( -50.40829686548195099, -142.0000000013656063, -1.485763867205728284 ) ) ;
#15198 = CARTESIAN_POINT ( 'NONE',  ( 1.339745962155615144, -32.70534180126148271, 4.999999999999999112 ) ) ;
#15199 = CARTESIAN_POINT ( 'NONE',  ( 4.458734124999999437, -162.3750000013656063, -1.846868145590734978 ) ) ;
#15200 = EDGE_LOOP ( 'NONE', ( #10228, #11223, #4733, #47733 ) ) ;
#15201 = CARTESIAN_POINT ( 'NONE',  ( 9.457646018065525792E-16, -83.06249999863439371, 5.148502694627439702 ) ) ;
#15202 = CARTESIAN_POINT ( 'NONE',  ( -1.339745962155613812, -70.08034179853029855, -5.000000000000000000 ) ) ;
#15203 = CARTESIAN_POINT ( 'NONE',  ( 4.458734125000001214, 0.1041666680322607674, 2.574251347313718519 ) ) ;
#15204 = CARTESIAN_POINT ( 'NONE',  ( 2.499999999999998668, -83.33333333333332860, -4.330127018922193649 ) ) ;
#15205 = CARTESIAN_POINT ( 'NONE',  ( -9.184850993605147944E-16, -162.3750000027311842, 5.000000000000000000 ) ) ;
#15206 = CARTESIAN_POINT ( 'NONE',  ( -4.458734124999999437, -65.56249999863440792, 0.000000000000000000 ) ) ;
#15207 = CARTESIAN_POINT ( 'NONE',  ( -5.000000000000000000, -25.95833333060214798, -2.886751345948128211 ) ) ;
#15208 = CARTESIAN_POINT ( 'NONE',  ( -5.000000000000000000, -29.08333333333332860, -2.886751345948128211 ) ) ;
#15209 = CARTESIAN_POINT ( 'NONE',  ( 2.229367062499998831, 28.35416666803225993, -3.861377020970580887 ) ) ;
#15210 = DIRECTION ( 'NONE',  ( -0.000000000000000000, -1.000000000000000000, -0.000000000000000000 ) ) ;
#15211 = FILL_AREA_STYLE_COLOUR ( '', #23386 ) ;
#15212 = CARTESIAN_POINT ( 'NONE',  ( 4.458734124999998549, -46.72916666530106511, -2.574251347313721627 ) ) ;
#15213 = CARTESIAN_POINT ( 'NONE',  ( -2.229367062499996610, -30.39583333196773651, 3.861377020970582219 ) ) ;
#15214 = CARTESIAN_POINT ( 'NONE',  ( 9.457646018065525792E-16, 4.687500001365595637, 5.148502694627439702 ) ) ;
#15215 = CARTESIAN_POINT ( 'NONE',  ( -1.339745962155613812, -10.08034179853029144, -5.000000000000000000 ) ) ;
#15216 = CARTESIAN_POINT ( 'NONE',  ( 5.000000000000000888, 18.41666666666666430, 2.886751345948126879 ) ) ;
#15217 = CARTESIAN_POINT ( 'NONE',  ( 5.000000000000000000, -149.1875000027312410, 2.071067811865478614 ) ) ;
#15218 = CARTESIAN_POINT ( 'NONE',  ( 2.500000000000002220, -54.54166666393548013, 4.330127018922192761 ) ) ;
#15219 = CARTESIAN_POINT ( 'NONE',  ( 9.457646018065525792E-16, -35.06249999863440792, 5.148502694627439702 ) ) ;
#15220 = CARTESIAN_POINT ( 'NONE',  ( 5.000000000000000000, -72.37499999726880162, -6.123233995736766282E-16 ) ) ;
#15221 = CARTESIAN_POINT ( 'NONE',  ( -59.44456063193725015, -143.8125000013656063, -0.3552334253322034230 ) ) ;
#15222 = CARTESIAN_POINT ( 'NONE',  ( 2.499999999999998668, -24.20833333060214443, -4.330127018922193649 ) ) ;
#15223 = CARTESIAN_POINT ( 'NONE',  ( 3.096526599377912525, -6.872473572140722631, -5.976664475826341615E-15 ) ) ;
#15224 = CARTESIAN_POINT ( 'NONE',  ( 9.457646018065525792E-16, -80.31249999863440792, 5.148502694627439702 ) ) ;
#15225 = CARTESIAN_POINT ( 'NONE',  ( -4.458734124999999437, -166.2500000013656063, -1.846868145590735644 ) ) ;
#15226 =( BOUNDED_CURVE ( )  B_SPLINE_CURVE ( 2, ( #58916, #14845, #38355, #57981, #43172, #42861, #62506, #57676, #13906 ),
 .UNSPECIFIED., .F., .F. ) 
 B_SPLINE_CURVE_WITH_KNOTS ( ( 3, 2, 2, 2, 3 ),
 ( 0.4916666666666670849, 0.4958333333333337922, 0.5000000000000004441, 0.5041666666666670960, 0.5083333333333337478 ),
 .UNSPECIFIED. ) 
 CURVE ( )  GEOMETRIC_REPRESENTATION_ITEM ( )  RATIONAL_B_SPLINE_CURVE ( ( 0.9999999999999918954, 0.9238795325112948431, 1.000000000000000000, 0.9238795325112867385, 1.000000000000000000, 0.9238795325112867385, 1.000000000000000000, 0.9238795325112786339, 1.000000000000008216 ) ) 
 REPRESENTATION_ITEM ( '' )  );
#15227 = CARTESIAN_POINT ( 'NONE',  ( -2.071067811865580754, -160.6875000000000284, -4.999999999999894307 ) ) ;
#15228 = DIRECTION ( 'NONE',  ( 0.000000000000000000, 0.000000000000000000, 1.000000000000000000 ) ) ;
#15229 = CARTESIAN_POINT ( 'NONE',  ( 5.000000000000000888, -27.58333333333333215, 2.886751345948126879 ) ) ;
#15230 = CARTESIAN_POINT ( 'NONE',  ( -8.190561711645485556E-16, -144.6875000013656063, 4.458734124999999437 ) ) ;
#15231 = ORIENTED_EDGE ( 'NONE', *, *, #25554, .F. ) ;
#15232 = CARTESIAN_POINT ( 'NONE',  ( 4.458734125000001214, 27.85416666803225993, 2.574251347313718519 ) ) ;
#15233 = ORIENTED_EDGE ( 'NONE', *, *, #58244, .F. ) ;
#15234 = CARTESIAN_POINT ( 'NONE',  ( -3.152548672688508926E-16, -59.81249999863440792, -5.148502694627439702 ) ) ;
#15235 =( BOUNDED_CURVE ( )  B_SPLINE_CURVE ( 2, ( #39438, #33677, #24659, #53297, #23727, #19827, #9848, #49419, #20156 ),
 .UNSPECIFIED., .F., .F. ) 
 B_SPLINE_CURVE_WITH_KNOTS ( ( 3, 2, 2, 2, 3 ),
 ( 0.9553571428571429047, 0.9559523809523809978, 0.9571428571428571841, 0.9583333333333333703, 0.9589285714285714635 ),
 .UNSPECIFIED. ) 
 CURVE ( )  GEOMETRIC_REPRESENTATION_ITEM ( )  RATIONAL_B_SPLINE_CURVE ( ( 0.9330127018922194093, 0.9330127018922194093, 1.000000000000000000, 0.8660254037844387076, 1.000000000000000000, 0.8660254037844387076, 1.000000000000000000, 0.9330127018922194093, 0.9330127018922194093 ) ) 
 REPRESENTATION_ITEM ( '' )  );
#15236 = CARTESIAN_POINT ( 'NONE',  ( 5.000000000000000888, 19.54166666939785202, 2.886751345948126879 ) ) ;
#15237 = CARTESIAN_POINT ( 'NONE',  ( 1.975475456537005874E-15, -90.62499999726880162, 5.000000000000000000 ) ) ;
#15238 = CARTESIAN_POINT ( 'NONE',  ( 5.000000000000000000, 14.49999999999999822, -6.123233995736766282E-16 ) ) ;
#15239 = EDGE_CURVE ( 'NONE', #55226, #35208, #4994, .T. ) ;
#15240 = AXIS2_PLACEMENT_3D ( 'NONE', #45868, #54889, #51020 ) ;
#15241 = CARTESIAN_POINT ( 'NONE',  ( 2.229367062500001939, -50.97916666530107221, 3.861377020970579999 ) ) ;
#15242 = CARTESIAN_POINT ( 'NONE',  ( 4.458734124999999437, -7.812499998634405252, -5.460374474430324690E-16 ) ) ;
#15243 = CARTESIAN_POINT ( 'NONE',  ( -48.00000000000002132, -135.0000000000000284, -4.041451884327376121 ) ) ;
#15244 = CARTESIAN_POINT ( 'NONE',  ( -49.85088928181150436, -145.6875000027311842, -1.666127454062680480 ) ) ;
#15245 = CARTESIAN_POINT ( 'NONE',  ( 2.500000000000002220, -91.54166666393547303, 4.330127018922192761 ) ) ;
#15246 = DIRECTION ( 'NONE',  ( -0.000000000000000000, 1.000000000000000000, -0.000000000000000000 ) ) ;
#15247 = DIRECTION ( 'NONE',  ( 0.000000000000000000, 0.000000000000000000, 1.000000000000000000 ) ) ;
#15249 = CARTESIAN_POINT ( 'NONE',  ( -4.458734124999999437, -20.31249999863440081, 0.000000000000000000 ) ) ;
#15248 = CARTESIAN_POINT ( 'NONE',  ( -1.339745962155613812, -79.20534180126146850, -5.000000000000000000 ) ) ;
#15250 = CARTESIAN_POINT ( 'NONE',  ( -4.999999999999998224, -77.79166666393547303, 2.886751345948131764 ) ) ;
#15251 = CARTESIAN_POINT ( 'NONE',  ( 4.458734124999999437, -55.81249999863440081, -5.460374474430324690E-16 ) ) ;
#15252 = CARTESIAN_POINT ( 'NONE',  ( -3.152801135295367096, -156.3125000013656063, -3.152801135295367541 ) ) ;
#15253 = EDGE_CURVE ( 'NONE', #38618, #2392, #50166, .T. ) ;
#15254 = CARTESIAN_POINT ( 'NONE',  ( -5.000000000000000000, -55.95833333060215153, -2.886751345948128211 ) ) ;
#15255 = ORIENTED_EDGE ( 'NONE', *, *, #41745, .T. ) ;
#15256 = DIRECTION ( 'NONE',  ( -0.000000000000000000, -0.000000000000000000, 1.000000000000000000 ) ) ;
#15258 = EDGE_CURVE ( 'NONE', #38746, #55791, #34555, .T. ) ;
#15257 = CARTESIAN_POINT ( 'NONE',  ( -3.152548672688508926E-16, 3.187500001365594748, -5.148502694627439702 ) ) ;
#15259 = EDGE_LOOP ( 'NONE', ( #38799, #13296, #11158, #43662 ) ) ;
#15261 = CYLINDRICAL_SURFACE ( 'NONE', #26543, 5.000000000000000000 ) ;
#15260 = CARTESIAN_POINT ( 'NONE',  ( 5.000000000000000888, -4.583333333333334814, 2.886751345948126879 ) ) ;
#15262 = CARTESIAN_POINT ( 'NONE',  ( 3.152801135295367541, -158.3125000013656063, -3.152801135295367541 ) ) ;
#15263 = VERTEX_POINT ( 'NONE', #41846 ) ;
#15264 = CARTESIAN_POINT ( 'NONE',  ( 5.000000000000000000, -23.29166666393548368, -2.886751345948130876 ) ) ;
#15265 = CARTESIAN_POINT ( 'NONE',  ( -53.33387254593733928, -130.8125000000000568, 5.149110718188519620 ) ) ;
#15266 = CARTESIAN_POINT ( 'NONE',  ( 2.071067811865561215, -161.3125000027312126, 4.999999999999913847 ) ) ;
#15267 = CARTESIAN_POINT ( 'NONE',  ( -2.229367062500000163, -43.72916666530106511, -3.861377020970580443 ) ) ;
#15268 = ORIENTED_EDGE ( 'NONE', *, *, #8289, .T. ) ;
#15269 = EDGE_CURVE ( 'NONE', #25522, #35059, #36652, .T. ) ;
#15270 = CARTESIAN_POINT ( 'NONE',  ( 1.975475456537005874E-15, -103.6249999972687874, 5.000000000000000000 ) ) ;
#15271 = CARTESIAN_POINT ( 'NONE',  ( 4.458734124999998549, 11.27083333469892779, -2.574251347313721627 ) ) ;
#15272 = CARTESIAN_POINT ( 'NONE',  ( 4.458734125000001214, 28.10416666803225993, 2.574251347313718519 ) ) ;
#15273 = CARTESIAN_POINT ( 'NONE',  ( -58.80597590150559739, -124.1250000027312126, 3.242614290531460330 ) ) ;
#15274 = DIRECTION ( 'NONE',  ( 0.000000000000000000, 0.000000000000000000, 1.000000000000000000 ) ) ;
#15275 = CARTESIAN_POINT ( 'NONE',  ( 6.123233995736766282E-16, -170.0000000000000000, -5.000000000000000000 ) ) ;
#15276 =( BOUNDED_CURVE ( )  B_SPLINE_CURVE ( 2, ( #27008, #2573, #18302, #37925, #36982, #37293, #22189, #46951, #12841 ),
 .UNSPECIFIED., .F., .F. ) 
 B_SPLINE_CURVE_WITH_KNOTS ( ( 3, 2, 2, 2, 3 ),
 ( 0.2482142857142857206, 0.2488095238095238138, 0.2500000000000000000, 0.2511904761904761862, 0.2517857142857142794 ),
 .UNSPECIFIED. ) 
 CURVE ( )  GEOMETRIC_REPRESENTATION_ITEM ( )  RATIONAL_B_SPLINE_CURVE ( ( 0.9330127018922194093, 0.9330127018922194093, 1.000000000000000000, 0.8660254037844387076, 1.000000000000000000, 0.8660254037844387076, 1.000000000000000000, 0.9330127018922194093, 0.9330127018922194093 ) ) 
 REPRESENTATION_ITEM ( '' )  );
#15277 = CARTESIAN_POINT ( 'NONE',  ( -4.999999999999998224, -102.9166666666666714, 2.886751345948131764 ) ) ;
#15278 = CARTESIAN_POINT ( 'NONE',  ( 2.229367062499998831, -67.64583333196773651, -3.861377020970580887 ) ) ;
#15279 = CYLINDRICAL_SURFACE ( 'NONE', #51024, 5.000000000000000000 ) ;
#15280 = CARTESIAN_POINT ( 'NONE',  ( 4.458734125000001214, 18.10416666803225638, 2.574251347313718519 ) ) ;
#15281 = VECTOR ( 'NONE', #28084, 1000.000000000000000 ) ;
#15282 = CARTESIAN_POINT ( 'NONE',  ( 1.339745962155615144, -33.70534180126148271, 4.999999999999999112 ) ) ;
#15283 = CARTESIAN_POINT ( 'NONE',  ( 4.458734125000001214, -49.14583333196772941, 2.574251347313718519 ) ) ;
#15284 = EDGE_CURVE ( 'NONE', #32980, #62925, #43208, .T. ) ;
#15285 = CARTESIAN_POINT ( 'NONE',  ( -3.535250795749689387E-16, -9.124999997268815832, -5.773502691896257311 ) ) ;
#15286 = CARTESIAN_POINT ( 'NONE',  ( -58.24261429053147765, -145.2500000000000284, -3.805975901505573855 ) ) ;
#15287 = CARTESIAN_POINT ( 'NONE',  ( -51.75738570946856498, -146.7500000000000284, 3.805975901505576964 ) ) ;
#15288 = CARTESIAN_POINT ( 'NONE',  ( -4.458734124999999437, -87.64583333196773651, -2.574251347313719407 ) ) ;
#15289 = CARTESIAN_POINT ( 'NONE',  ( -5.000000000000000000, 11.04166666939785202, -2.886751345948128211 ) ) ;
#15290 = CARTESIAN_POINT ( 'NONE',  ( 4.458734124999998549, -17.97916666530106866, -2.574251347313721627 ) ) ;
#15291 = ORIENTED_EDGE ( 'NONE', *, *, #24846, .T. ) ;
#15292 = CARTESIAN_POINT ( 'NONE',  ( -2.071067811865415109, -163.4375000027311842, 5.000000000000062172 ) ) ;
#15293 = CARTESIAN_POINT ( 'NONE',  ( -2.229367062499996610, -103.1458333319677365, 3.861377020970582219 ) ) ;
#15294 = CARTESIAN_POINT ( 'NONE',  ( -2.071067811865478170, -160.4375000027312126, 5.000000000000000000 ) ) ;
#15295 = CARTESIAN_POINT ( 'NONE',  ( -4.458734124999999437, -97.64583333196772230, -2.574251347313719407 ) ) ;
#15296 = CARTESIAN_POINT ( 'NONE',  ( -6.972266317189433020E-16, -12.24999999999999645, -5.000000000000000000 ) ) ;
#15297 = CARTESIAN_POINT ( 'NONE',  ( -5.000000000000000000, -55.87499999726880162, 0.000000000000000000 ) ) ;
#15298 = CARTESIAN_POINT ( 'NONE',  ( 1.339745962155612702, -62.16965819600734022, -5.000000000000000000 ) ) ;
#15299 = CARTESIAN_POINT ( 'NONE',  ( -52.80376928212989185, -154.1250000013656347, -4.297418129356379346 ) ) ;
#15300 = B_SPLINE_CURVE_WITH_KNOTS ( 'NONE', 3,
 ( #14826, #34440, #39587, #54069, #18713, #10008, #29620, #5192, #44413, #374, #19978, #59224, #15156, #57965, #54401, #33515, #53133, #10331, #29941, #9065, #28675, #40240, #30583, #49879 ),
 .UNSPECIFIED., .F., .F.,
 ( 4, 2, 2, 2, 2, 2, 2, 2, 2, 2, 2, 4 ),
 ( 0.000000000000000000, 0.001161859418553695721, 0.001742789127830540220, 0.002323718837107384503, 0.003485578255661076971, 0.004647437674214769873, 0.005809297092768463643, 0.006390226802045317032, 0.006971156511322169555, 0.007552086220599022945, 0.008133015929875876335, 0.009294875348429583115 ),
 .UNSPECIFIED. ) ;
#15301 = CARTESIAN_POINT ( 'NONE',  ( -53.51423613279429503, -144.2500000013656063, 4.591703134518083651 ) ) ;
#15302 = CARTESIAN_POINT ( 'NONE',  ( 9.457646018065525792E-16, -17.06249999863440792, 5.148502694627439702 ) ) ;
#15303 = CARTESIAN_POINT ( 'NONE',  ( 4.458734124999998549, 8.020833334698926009, -2.574251347313721627 ) ) ;
#15304 = CARTESIAN_POINT ( 'NONE',  ( 2.229367062500001939, -66.22916666530106511, 3.861377020970579999 ) ) ;
#15305 = CARTESIAN_POINT ( 'NONE',  ( 5.000000000000000000, -94.29166666393547303, -2.886751345948130876 ) ) ;
#15306 = CARTESIAN_POINT ( 'NONE',  ( 9.457646018065525792E-16, -18.06249999863440792, 5.148502694627439702 ) ) ;
#15307 = DIRECTION ( 'NONE',  ( -0.000000000000000000, 1.000000000000000000, -0.000000000000000000 ) ) ;
#15308 = CARTESIAN_POINT ( 'NONE',  ( 5.000000000000000888, -154.9375000000000000, -2.071067811865475505 ) ) ;
#15309 = CARTESIAN_POINT ( 'NONE',  ( -2.500000000000000444, -5.166666666666666963, -4.330127018922193649 ) ) ;
#15310 = CARTESIAN_POINT ( 'NONE',  ( -1.846868145590737420, -157.7500000013656063, 4.458734124999999437 ) ) ;
#15311 = ORIENTED_EDGE ( 'NONE', *, *, #55494, .F. ) ;
#15312 = CARTESIAN_POINT ( 'NONE',  ( -2.229367062499996610, -47.39583333196774362, 3.861377020970582219 ) ) ;
#15313 = CARTESIAN_POINT ( 'NONE',  ( 2.499999999999998668, -44.20833333060214443, -4.330127018922193649 ) ) ;
#15314 = CARTESIAN_POINT ( 'NONE',  ( 5.000000000000000000, -66.50000000000000000, -6.123233995736766282E-16 ) ) ;
#15315 = CARTESIAN_POINT ( 'NONE',  ( -5.000000000000000000, 30.00000000000000000, 0.000000000000000000 ) ) ;
#15316 = CARTESIAN_POINT ( 'NONE',  ( -2.229367062500000163, -88.47916666530106511, -3.861377020970580443 ) ) ;
#15317 = CARTESIAN_POINT ( 'NONE',  ( 4.458734125000001214, 17.85416666803225993, 2.574251347313718519 ) ) ;
#15318 = EDGE_CURVE ( 'NONE', #20975, #17776, #32840, .T. ) ;
#15319 = CARTESIAN_POINT ( 'NONE',  ( 4.458734124999999437, 7.187500001365594748, -5.460374474430324690E-16 ) ) ;
#15320 = CARTESIAN_POINT ( 'NONE',  ( 0.000000000000000000, -170.0000000000000000, 5.000000000000000000 ) ) ;
#15321 = CARTESIAN_POINT ( 'NONE',  ( 2.500000000000002220, -17.66666666666666430, 4.330127018922192761 ) ) ;
#15322 = CARTESIAN_POINT ( 'NONE',  ( 2.229367062500001939, 21.77083333469892779, 3.861377020970579999 ) ) ;
#15323 = CARTESIAN_POINT ( 'NONE',  ( 5.000000000000000888, -73.58333333333334281, 2.886751345948126879 ) ) ;
#15324 = CARTESIAN_POINT ( 'NONE',  ( -5.000000000000000000, 10.04166666939785202, -2.886751345948128211 ) ) ;
#15325 = VERTEX_POINT ( 'NONE', #28004 ) ;
#15326 = CARTESIAN_POINT ( 'NONE',  ( -4.999999999999998224, 8.083333333333332149, 2.886751345948131764 ) ) ;
#15327 = VERTEX_POINT ( 'NONE', #17731 ) ;
#15328 = AXIS2_PLACEMENT_3D ( 'NONE', #17219, #41645, #51957 ) ;
#15329 = FACE_OUTER_BOUND ( 'NONE', #41496, .T. ) ;
#15330 = CARTESIAN_POINT ( 'NONE',  ( -4.458734124999999437, -38.39583333196773651, -2.574251347313719407 ) ) ;
#15331 = VECTOR ( 'NONE', #47247, 1000.000000000000000 ) ;
#15332 = CARTESIAN_POINT ( 'NONE',  ( -5.000000000000000000, -40.87499999726880162, 0.000000000000000000 ) ) ;
#15333 = EDGE_LOOP ( 'NONE', ( #12100, #34174, #3089, #54856 ) ) ;
#15334 = CARTESIAN_POINT ( 'NONE',  ( -59.44456063193725015, -145.8125000013656063, -0.3552334253322034230 ) ) ;
#15336 = EDGE_CURVE ( 'NONE', #54054, #31959, #56769, .T. ) ;
#15335 = CARTESIAN_POINT ( 'NONE',  ( 2.229367062499998831, -11.64583333196774007, -3.861377020970580887 ) ) ;
#15338 = ORIENTED_EDGE ( 'NONE', *, *, #20124, .F. ) ;
#15337 = CARTESIAN_POINT ( 'NONE',  ( 9.457646018065525792E-16, -19.31249999863440792, 5.148502694627439702 ) ) ;
#15339 = CARTESIAN_POINT ( 'NONE',  ( 5.000000000000000000, -81.50000000000000000, -6.123233995736766282E-16 ) ) ;
#15340 = CARTESIAN_POINT ( 'NONE',  ( -4.458734124999999437, -166.9375000013655779, -5.460374474430324690E-16 ) ) ;
#15341 = CARTESIAN_POINT ( 'NONE',  ( 2.229367062499998831, -64.89583333196773651, -3.861377020970580887 ) ) ;
#15342 = CARTESIAN_POINT ( 'NONE',  ( 5.000000000000000888, -85.45833333060213022, 2.886751345948126879 ) ) ;
#15344 = ORIENTED_EDGE ( 'NONE', *, *, #23548, .F. ) ;
#15343 = CARTESIAN_POINT ( 'NONE',  ( -4.999999999999998224, -31.91666666666666430, 2.886751345948131764 ) ) ;
#15345 = CARTESIAN_POINT ( 'NONE',  ( -56.66612745406270335, -141.3125000000000000, -5.149110718188516067 ) ) ;
#15346 = CARTESIAN_POINT ( 'NONE',  ( -2.229367062500000163, -29.72916666530107221, -3.861377020970580443 ) ) ;
#15347 = CARTESIAN_POINT ( 'NONE',  ( -5.000000000000000000, -50.00000000000000000, 0.000000000000000000 ) ) ;
#15348 = VERTEX_POINT ( 'NONE', #32198 ) ;
#15349 = PRODUCT_CONTEXT ( 'NONE', #4731, 'mechanical' ) ;
#15350 = CARTESIAN_POINT ( 'NONE',  ( -1.846868145590737420, -163.0000000013655779, 4.458734124999999437 ) ) ;
#15351 = CARTESIAN_POINT ( 'NONE',  ( -2.229367062499996610, -109.3958333319677365, 3.861377020970582219 ) ) ;
#15352 = CARTESIAN_POINT ( 'NONE',  ( 5.000000000000000000, 20.49999999999999645, -6.123233995736766282E-16 ) ) ;
#15353 = ORIENTED_EDGE ( 'NONE', *, *, #21754, .F. ) ;
#15354 = CARTESIAN_POINT ( 'NONE',  ( -52.10840900171896806, -144.4375000013656063, 3.393966926194110556 ) ) ;
#15355 = CARTESIAN_POINT ( 'NONE',  ( -2.229367062499996610, -73.39583333196773651, 3.861377020970582219 ) ) ;
#15356 = CARTESIAN_POINT ( 'NONE',  ( -52.53715891517739323, -133.5625000027312410, -4.819101127000233298 ) ) ;
#15357 = CARTESIAN_POINT ( 'NONE',  ( -3.152548672688508926E-16, -42.56249999863439371, -5.148502694627439702 ) ) ;
#15358 = CARTESIAN_POINT ( 'NONE',  ( 3.152801135295366208, -147.8125000013655779, 3.152801135295367985 ) ) ;
#15359 = CARTESIAN_POINT ( 'NONE',  ( -1.339745962155617365, 23.20534180126148271, 4.999999999999998224 ) ) ;
#15360 = CARTESIAN_POINT ( 'NONE',  ( -4.458734124999997661, -49.22916666530106511, 2.574251347313722516 ) ) ;
#15361 = CARTESIAN_POINT ( 'NONE',  ( 1.339745962155613146, 29.29465819873852084, 5.000000000000000888 ) ) ;
#15362 = EDGE_CURVE ( 'NONE', #22221, #4851, #13792, .T. ) ;
#15363 = CARTESIAN_POINT ( 'NONE',  ( -2.229367062499996610, -14.14583333196774184, 3.861377020970582219 ) ) ;
#15364 =( BOUNDED_CURVE ( )  B_SPLINE_CURVE ( 2, ( #12187, #17330, #46603, #36952, #55634, #55944, #31801, #51434, #56579 ),
 .UNSPECIFIED., .F., .F. ) 
 B_SPLINE_CURVE_WITH_KNOTS ( ( 3, 2, 2, 2, 3 ),
 ( 0.6895833333333333259, 0.6902777777777777679, 0.6916666666666666519, 0.6930555555555555358, 0.6937499999999999778 ),
 .UNSPECIFIED. ) 
 CURVE ( )  GEOMETRIC_REPRESENTATION_ITEM ( )  RATIONAL_B_SPLINE_CURVE ( ( 0.9330127018922194093, 0.9330127018922194093, 1.000000000000000000, 0.8660254037844387076, 1.000000000000000000, 0.8660254037844387076, 1.000000000000000000, 0.9330127018922194093, 0.9330127018922194093 ) ) 
 REPRESENTATION_ITEM ( '' )  );
#15365 = CARTESIAN_POINT ( 'NONE',  ( -4.999999999999999112, -100.9166666666666430, 2.886751345948131764 ) ) ;
#15366 = CARTESIAN_POINT ( 'NONE',  ( 1.846868145590735200, -140.5000000013656347, -4.458734125000000326 ) ) ;
#15367 = CARTESIAN_POINT ( 'NONE',  ( -2.229367062500000163, -31.72916666530107577, -3.861377020970580443 ) ) ;
#15368 = CARTESIAN_POINT ( 'NONE',  ( 5.000000000000000000, 6.708333336064521646, -2.886751345948129988 ) ) ;
#15369 = CARTESIAN_POINT ( 'NONE',  ( -1.339745962155610925, -52.79465819873851729, 5.000000000000000000 ) ) ;
#15370 = CARTESIAN_POINT ( 'NONE',  ( -55.35523342533222291, -130.3125000013656063, 4.444560631937231499 ) ) ;
#15371 = CARTESIAN_POINT ( 'NONE',  ( 4.458734125000001214, -76.14583333196773651, 2.574251347313718519 ) ) ;
#15372 = FACE_OUTER_BOUND ( 'NONE', #58463, .T. ) ;
#15373 = CARTESIAN_POINT ( 'NONE',  ( 5.000000000000000888, -54.45833333060214443, 2.886751345948126879 ) ) ;
#15374 = CARTESIAN_POINT ( 'NONE',  ( -6.000000000000000000, -120.0000000000000000, -1.500000000000000000 ) ) ;
#15375 = CARTESIAN_POINT ( 'NONE',  ( 2.229367062499998831, -0.8958333319677401763, -3.861377020970580887 ) ) ;
#15376 = ORIENTED_EDGE ( 'NONE', *, *, #389, .F. ) ;
#15377 = CARTESIAN_POINT ( 'NONE',  ( -6.972266317189433020E-16, -57.25000000000000000, -5.000000000000000000 ) ) ;
#15379 = CARTESIAN_POINT ( 'NONE',  ( 9.457646018065525792E-16, -36.06249999863441502, 5.148502694627439702 ) ) ;
#15378 = CARTESIAN_POINT ( 'NONE',  ( 2.229367062499998831, -85.64583333196773651, -3.861377020970580887 ) ) ;
#15380 = CARTESIAN_POINT ( 'NONE',  ( -51.19402409849444524, -143.6250000027312126, -3.242614290531456334 ) ) ;
#15381 = CARTESIAN_POINT ( 'NONE',  ( -4.458734124999998549, -80.47916666530106511, 2.574251347313722516 ) ) ;
#15382 = AXIS2_PLACEMENT_3D ( 'NONE', #60119, #40162, #54963 ) ;
#15383 = CARTESIAN_POINT ( 'NONE',  ( -2.229367062500000163, 19.27083333469892779, -3.861377020970580443 ) ) ;
#15384 = CYLINDRICAL_SURFACE ( 'NONE', #3779, 5.000000000000000000 ) ;
#15385 = CARTESIAN_POINT ( 'NONE',  ( -52.80376928212989185, -135.8750000013655779, -4.297418129356379346 ) ) ;
#15386 =( BOUNDED_CURVE ( )  B_SPLINE_CURVE ( 2, ( #24967, #29135, #28831, #20142, #38478, #58107, #14665, #39739, #43614 ),
 .UNSPECIFIED., .F., .F. ) 
 B_SPLINE_CURVE_WITH_KNOTS ( ( 3, 2, 2, 2, 3 ),
 ( 0.3479166666666666519, 0.3486111111111110938, 0.3499999999999999778, 0.3513888888888888618, 0.3520833333333333592 ),
 .UNSPECIFIED. ) 
 CURVE ( )  GEOMETRIC_REPRESENTATION_ITEM ( )  RATIONAL_B_SPLINE_CURVE ( ( 0.9330127018922194093, 0.9330127018922194093, 1.000000000000000000, 0.8660254037844387076, 1.000000000000000000, 0.8660254037844387076, 1.000000000000000000, 0.9330127018922167448, 0.9330127018922194093 ) ) 
 REPRESENTATION_ITEM ( '' )  );
#15387 = CARTESIAN_POINT ( 'NONE',  ( -4.458734124999999437, -1.312499998634406140, 0.000000000000000000 ) ) ;
#15388 = CARTESIAN_POINT ( 'NONE',  ( 2.229367062500001939, 21.77083333469892779, 3.861377020970579999 ) ) ;
#15389 = CARTESIAN_POINT ( 'NONE',  ( 4.458734124999998549, -50.97916666530107221, -2.574251347313721627 ) ) ;
#15390 = CARTESIAN_POINT ( 'NONE',  ( 1.339745962155612702, -15.29465819873851906, -5.000000000000000000 ) ) ;
#15391 = CARTESIAN_POINT ( 'NONE',  ( -3.152548672688508926E-16, -5.562499998634400811, -5.148502694627439702 ) ) ;
#15392 = ORIENTED_EDGE ( 'NONE', *, *, #33369, .T. ) ;
#15393 = CARTESIAN_POINT ( 'NONE',  ( 4.458734124999999437, -28.06249999863440081, -5.460374474430324690E-16 ) ) ;
#15394 = CARTESIAN_POINT ( 'NONE',  ( -59.44456063193725015, -132.8125000013656063, -0.3552334253322034230 ) ) ;
#15395 = CARTESIAN_POINT ( 'NONE',  ( -2.229367062499996610, -73.14583333196773651, 3.861377020970582219 ) ) ;
#15396 = CARTESIAN_POINT ( 'NONE',  ( -5.000000000000000000, -102.9583333306021302, -2.886751345948128211 ) ) ;
#15397 = CARTESIAN_POINT ( 'NONE',  ( 2.229367062500001939, 27.02083333469892423, 3.861377020970579999 ) ) ;
#15398 = ADVANCED_FACE ( 'NONE', ( #27066 ), #46682, .T. ) ;
#15399 = ADVANCED_FACE ( 'NONE', ( #42480 ), #18037, .T. ) ;
#15400 = CARTESIAN_POINT ( 'NONE',  ( 5.000000000000000000, 26.70833333606451632, -2.886751345948130876 ) ) ;
#15401 = FACE_OUTER_BOUND ( 'NONE', #14836, .T. ) ;
#15402 = CARTESIAN_POINT ( 'NONE',  ( -4.458734124999999437, -77.64583333196773651, -2.574251347313719407 ) ) ;
#15403 = CARTESIAN_POINT ( 'NONE',  ( -4.999999999999999112, -57.91666666666665719, 2.886751345948131764 ) ) ;
#15404 = ADVANCED_FACE ( 'NONE', ( #43734 ), #9957, .F. ) ;
#15405 = CARTESIAN_POINT ( 'NONE',  ( -9.184850993605147944E-16, -152.2500000000000000, 5.000000000000000000 ) ) ;
#15406 = CARTESIAN_POINT ( 'NONE',  ( 5.000000000000000000, 25.70833333606452342, -2.886751345948129988 ) ) ;
#15407 = ORIENTED_EDGE ( 'NONE', *, *, #43238, .F. ) ;
#15408 = LINE ( 'NONE', #48849, #35592 ) ;
#15409 = EDGE_CURVE ( 'NONE', #7881, #19063, #48565, .T. ) ;
#15410 = LINE ( 'NONE', #29863, #36046 ) ;
#15411 = CARTESIAN_POINT ( 'NONE',  ( -2.499999999999996447, -16.83333333333333215, 4.330127018922195425 ) ) ;
#15412 = CARTESIAN_POINT ( 'NONE',  ( -4.458734124999999437, -21.31249999863440436, 0.000000000000000000 ) ) ;
#15413 = EDGE_CURVE ( 'NONE', #7221, #49592, #63331, .T. ) ;
#15414 = CARTESIAN_POINT ( 'NONE',  ( -4.458734124999999437, -80.31249999863440792, 0.000000000000000000 ) ) ;
#15415 = EDGE_CURVE ( 'NONE', #37124, #32095, #25560, .T. ) ;
#15416 = CARTESIAN_POINT ( 'NONE',  ( -3.535250795749689387E-16, -21.12499999726881228, -5.773502691896257311 ) ) ;
#15418 = EDGE_LOOP ( 'NONE', ( #8211, #35666, #9468, #29698 ) ) ;
#15417 = CARTESIAN_POINT ( 'NONE',  ( -4.458734124999999437, -47.39583333196774362, -2.574251347313719407 ) ) ;
#15419 = DIRECTION ( 'NONE',  ( -0.000000000000000000, 1.000000000000000000, -0.000000000000000000 ) ) ;
#15420 = CARTESIAN_POINT ( 'NONE',  ( 2.499999999999998668, -74.20833333060214443, -4.330127018922193649 ) ) ;
#15422 = VERTEX_POINT ( 'NONE', #9021 ) ;
#15421 = CARTESIAN_POINT ( 'NONE',  ( -2.229367062499996610, 3.604166668032260379, 3.861377020970582219 ) ) ;
#15423 = CARTESIAN_POINT ( 'NONE',  ( -58.39396692619412477, -151.4375000013656063, 2.891590998281057701 ) ) ;
#15424 = CARTESIAN_POINT ( 'NONE',  ( 5.000000000000000000, -65.50000000000000000, -6.123233995736766282E-16 ) ) ;
#15425 = EDGE_CURVE ( 'NONE', #55214, #24763, #47724, .T. ) ;
#15426 = CARTESIAN_POINT ( 'NONE',  ( -1.846868145590734756, -152.3750000013655779, -4.458734125000000326 ) ) ;
#15427 = CARTESIAN_POINT ( 'NONE',  ( 4.458734125000001214, -44.14583333196773651, 2.574251347313718519 ) ) ;
#15428 = CARTESIAN_POINT ( 'NONE',  ( -6.972266317189433020E-16, -23.24999999999999645, -5.000000000000000000 ) ) ;
#15429 = CARTESIAN_POINT ( 'NONE',  ( 3.535533905932736864, -164.1250000000000284, 3.535533905932738641 ) ) ;
#15430 = EDGE_CURVE ( 'NONE', #59704, #44176, #43110, .T. ) ;
#15431 = EDGE_CURVE ( 'NONE', #52288, #54333, #6226, .T. ) ;
#15432 = CARTESIAN_POINT ( 'NONE',  ( -55.00000000000002132, -155.0000000000000284, 1.734723475976807094E-15 ) ) ;
#15433 = VECTOR ( 'NONE', #45858, 1000.000000000000000 ) ;
#15434 = CARTESIAN_POINT ( 'NONE',  ( -51.60603307380591787, -126.1875000013656063, -2.891590998281053704 ) ) ;
#15435 = CARTESIAN_POINT ( 'NONE',  ( -2.229367062499996610, -10.39583333196773829, 3.861377020970582219 ) ) ;
#15436 = CARTESIAN_POINT ( 'NONE',  ( -2.229367062499996610, -47.39583333196774362, 3.861377020970582219 ) ) ;
#15437 = CARTESIAN_POINT ( 'NONE',  ( 1.243387493232115550E-13, -19.25000000000000000, -5.000000000000000000 ) ) ;
#15438 = CARTESIAN_POINT ( 'NONE',  ( 4.458734124999999437, -145.4375000013656063, 0.000000000000000000 ) ) ;
#15439 = CARTESIAN_POINT ( 'NONE',  ( 2.229367062499998831, -86.89583333196773651, -3.861377020970580887 ) ) ;
#15440 = ORIENTED_EDGE ( 'NONE', *, *, #8031, .T. ) ;
#15441 = CARTESIAN_POINT ( 'NONE',  ( -2.500000000000000444, 13.95833333606451809, -4.330127018922193649 ) ) ;
#15442 = LINE ( 'NONE', #9962, #15896 ) ;
#15443 = CARTESIAN_POINT ( 'NONE',  ( -59.81910112700025905, -148.3125000027312126, -2.462841084822630311 ) ) ;
#15444 =( BOUNDED_CURVE ( )  B_SPLINE_CURVE ( 2, ( #2508, #42043, #47199, #36589, #11513, #60421, #56545, #56225, #12146 ),
 .UNSPECIFIED., .F., .F. ) 
 B_SPLINE_CURVE_WITH_KNOTS ( ( 3, 2, 2, 2, 3 ),
 ( 0.08392857142857143571, 0.08452380952380952883, 0.08571428571428571508, 0.08690476190476190133, 0.08750000000000000833 ),
 .UNSPECIFIED. ) 
 CURVE ( )  GEOMETRIC_REPRESENTATION_ITEM ( )  RATIONAL_B_SPLINE_CURVE ( ( 0.9330127018922192983, 0.9330127018922200755, 1.000000000000000000, 0.8660254037844387076, 1.000000000000000000, 0.8660254037844387076, 1.000000000000000000, 0.9330127018922185211, 0.9330127018922192983 ) ) 
 REPRESENTATION_ITEM ( '' )  );
#15445 = CARTESIAN_POINT ( 'NONE',  ( 2.500000000000002220, -38.66666666666667140, 4.330127018922192761 ) ) ;
#15446 = EDGE_LOOP ( 'NONE', ( #28783, #3998, #24341, #561 ) ) ;
#15447 = CARTESIAN_POINT ( 'NONE',  ( -4.458734124999999437, 3.604166668032260379, -2.574251347313719407 ) ) ;
#15448 = CARTESIAN_POINT ( 'NONE',  ( 1.339745962155565406, -19.70534180126148271, 5.000000000000028422 ) ) ;
#15449 = CARTESIAN_POINT ( 'NONE',  ( 4.458734124999999437, -20.06249999863440081, -5.460374474430324690E-16 ) ) ;
#15450 = CARTESIAN_POINT ( 'NONE',  ( -6.972266317189433020E-16, 11.87500000273118594, -5.000000000000000000 ) ) ;
#15451 = CARTESIAN_POINT ( 'NONE',  ( -2.229367062500000163, -5.479166665301072214, -3.861377020970580443 ) ) ;
#15452 = CARTESIAN_POINT ( 'NONE',  ( -6.972266317189433020E-16, 3.875000002731185500, -5.000000000000000000 ) ) ;
#15453 = CARTESIAN_POINT ( 'NONE',  ( -1.846868145590734756, -148.1250000013655779, -4.458734124999999437 ) ) ;
#15454 = CARTESIAN_POINT ( 'NONE',  ( -4.458734124999999437, 17.43750000136559208, 0.000000000000000000 ) ) ;
#15455 = ORIENTED_EDGE ( 'NONE', *, *, #7134, .F. ) ;
#15456 = CARTESIAN_POINT ( 'NONE',  ( 9.457646018065525792E-16, -98.06249999863440792, 5.148502694627439702 ) ) ;
#15457 = CARTESIAN_POINT ( 'NONE',  ( -5.000000000000000000, -26.95833333060214798, -2.886751345948128211 ) ) ;
#15458 = CARTESIAN_POINT ( 'NONE',  ( 4.458734125000001214, -20.89583333196774007, 2.574251347313718519 ) ) ;
#15459 = CARTESIAN_POINT ( 'NONE',  ( 5.000000000000000888, -25.45833333060214443, 2.886751345948126879 ) ) ;
#15460 = CARTESIAN_POINT ( 'NONE',  ( 1.975475456537005874E-15, -88.62499999726880162, 5.000000000000000000 ) ) ;
#15461 = CARTESIAN_POINT ( 'NONE',  ( -50.70258187064364108, -148.1250000013656063, 2.196230717870141014 ) ) ;
#15462 = CARTESIAN_POINT ( 'NONE',  ( -4.999999999999999112, -43.79166666393546592, 2.886751345948131764 ) ) ;
#15463 = CARTESIAN_POINT ( 'NONE',  ( -51.19402409849444524, -148.5000000000000284, -3.242614290531456334 ) ) ;
#15464 = CARTESIAN_POINT ( 'NONE',  ( -4.458734124999999437, 12.60416666803226349, -2.574251347313719407 ) ) ;
#15465 = CARTESIAN_POINT ( 'NONE',  ( -2.499999999999996447, -8.708333330602144429, 4.330127018922195425 ) ) ;
#15466 = LINE ( 'NONE', #44396, #23342 ) ;
#15467 = CARTESIAN_POINT ( 'NONE',  ( 4.458734125000000326, 13.10416666803226171, 2.574251347313718519 ) ) ;
#15468 = CARTESIAN_POINT ( 'NONE',  ( -3.152548672688508926E-16, -59.56249999863440081, -5.148502694627439702 ) ) ;
#15469 = ORIENTED_EDGE ( 'NONE', *, *, #26473, .F. ) ;
#15470 = VECTOR ( 'NONE', #2830, 1000.000000000000000 ) ;
#15471 = CARTESIAN_POINT ( 'NONE',  ( -2.229367062499996610, -12.39583333196774007, 3.861377020970582219 ) ) ;
#15472 =( BOUNDED_CURVE ( )  B_SPLINE_CURVE ( 2, ( #24973, #34607, #4398, #24651, #537, #24019, #33669, #44257, #29778 ),
 .UNSPECIFIED., .F., .F. ) 
 B_SPLINE_CURVE_WITH_KNOTS ( ( 3, 2, 2, 2, 3 ),
 ( 0.1479166666666666685, 0.1486111111111111105, 0.1499999999999999944, 0.1513888888888888784, 0.1520833333333333481 ),
 .UNSPECIFIED. ) 
 CURVE ( )  GEOMETRIC_REPRESENTATION_ITEM ( )  RATIONAL_B_SPLINE_CURVE ( ( 0.9330127018922194093, 0.9330127018922194093, 1.000000000000000000, 0.8660254037844387076, 1.000000000000000000, 0.8660254037844387076, 1.000000000000000000, 0.9330127018922180770, 0.9330127018922194093 ) ) 
 REPRESENTATION_ITEM ( '' )  );
#15473 = CARTESIAN_POINT ( 'NONE',  ( 2.500000000000002220, 4.333333333333331261, 4.330127018922192761 ) ) ;
#15474 = CARTESIAN_POINT ( 'NONE',  ( -4.458734124999999437, -161.9375000013655779, -5.460374474430324690E-16 ) ) ;
#15475 = CARTESIAN_POINT ( 'NONE',  ( 2.499999999999998668, -63.20833333060215153, -4.330127018922193649 ) ) ;
#15476 = CARTESIAN_POINT ( 'NONE',  ( 9.457646018065525792E-16, -59.06249999863439371, 5.148502694627439702 ) ) ;
#15477 = CARTESIAN_POINT ( 'NONE',  ( -5.000000000000000000, -90.87499999726880162, 0.000000000000000000 ) ) ;
#15478 = CARTESIAN_POINT ( 'NONE',  ( -4.458734124999999437, -33.31249999863440792, 0.000000000000000000 ) ) ;
#15479 = FACE_OUTER_BOUND ( 'NONE', #47367, .T. ) ;
#15480 = CARTESIAN_POINT ( 'NONE',  ( 1.975475456537005874E-15, -52.75000000000000000, 5.000000000000000000 ) ) ;
#15481 = CARTESIAN_POINT ( 'NONE',  ( 0.000000000000000000, 15.00000000000000000, 0.000000000000000000 ) ) ;
#15482 = CARTESIAN_POINT ( 'NONE',  ( -5.000000000000000000, -49.00000000000000000, 0.000000000000000000 ) ) ;
#15483 = CARTESIAN_POINT ( 'NONE',  ( -1.846868145590734756, -154.3750000013655779, -4.458734124999999437 ) ) ;
#15484 = CARTESIAN_POINT ( 'NONE',  ( 5.000000000000000000, -43.50000000000000000, -6.123233995736766282E-16 ) ) ;
#15485 = CARTESIAN_POINT ( 'NONE',  ( -2.499999999999996447, -13.83333333333333570, 4.330127018922195425 ) ) ;
#15486 = CARTESIAN_POINT ( 'NONE',  ( 1.339745962155615144, -6.580341798530292330, 4.999999999999999112 ) ) ;
#15487 = ORIENTED_EDGE ( 'NONE', *, *, #48630, .F. ) ;
#15488 = CARTESIAN_POINT ( 'NONE',  ( 4.458734124999998549, -103.7291666653010651, -2.574251347313721627 ) ) ;
#15489 = CARTESIAN_POINT ( 'NONE',  ( 4.458734125000001214, 0.8541666680322613781, 2.574251347313718519 ) ) ;
#15490 = CARTESIAN_POINT ( 'NONE',  ( 1.339745962155612702, -59.29465819873853150, -5.000000000000000000 ) ) ;
#15491 = CARTESIAN_POINT ( 'NONE',  ( -4.999999999999999112, -4.916666666666666075, 2.886751345948131764 ) ) ;
#15492 = CARTESIAN_POINT ( 'NONE',  ( 9.457646018065525792E-16, -68.06249999863440792, 5.148502694627439702 ) ) ;
#15493 = DIRECTION ( 'NONE',  ( -0.000000000000000000, 1.000000000000000000, -0.000000000000000000 ) ) ;
#15494 = CARTESIAN_POINT ( 'NONE',  ( 2.500000000000002220, -8.541666663935483683, 4.330127018922192761 ) ) ;
#15496 = ORIENTED_EDGE ( 'NONE', *, *, #14147, .T. ) ;
#15495 = CARTESIAN_POINT ( 'NONE',  ( 2.229367062499998831, -32.64583333196773651, -3.861377020970580887 ) ) ;
#15497 = CARTESIAN_POINT ( 'NONE',  ( -51.75738570946856498, -149.8750000027312126, 3.805975901505576964 ) ) ;
#15498 = FACE_OUTER_BOUND ( 'NONE', #22388, .T. ) ;
#15499 = EDGE_LOOP ( 'NONE', ( #60362, #58684, #13749, #40896 ) ) ;
#15500 = CARTESIAN_POINT ( 'NONE',  ( 5.000000000000000000, -101.3749999972688158, -6.123233995736766282E-16 ) ) ;
#15501 = CARTESIAN_POINT ( 'NONE',  ( 5.000000000000000888, -50.58333333333332860, 2.886751345948126879 ) ) ;
#15502 = EDGE_CURVE ( 'NONE', #27082, #29335, #32517, .T. ) ;
#15504 = CARTESIAN_POINT ( 'NONE',  ( 4.458734125000001214, -24.14583333196773651, 2.574251347313718519 ) ) ;
#15503 = CARTESIAN_POINT ( 'NONE',  ( 1.339745962155615144, -46.58034179853028434, 4.999999999999999112 ) ) ;
#15505 = CARTESIAN_POINT ( 'NONE',  ( -5.000000000000000000, -41.95833333060214443, -2.886751345948128211 ) ) ;
#15506 = CARTESIAN_POINT ( 'NONE',  ( -4.458734124999999437, -77.39583333196772230, -2.574251347313719407 ) ) ;
#15507 = CARTESIAN_POINT ( 'NONE',  ( 4.458734124999999437, -145.7500000013655779, 1.846868145590737864 ) ) ;
#15508 = CARTESIAN_POINT ( 'NONE',  ( 9.457646018065525792E-16, -82.06249999863442213, 5.148502694627439702 ) ) ;
#15509 = CARTESIAN_POINT ( 'NONE',  ( -59.44456063193725015, -137.8125000013656063, -0.3552334253322034230 ) ) ;
#15510 = CARTESIAN_POINT ( 'NONE',  ( -4.458734124999999437, -30.64583333196774007, -2.574251347313719407 ) ) ;
#15511 = CARTESIAN_POINT ( 'NONE',  ( -5.000000000000000000, -73.87499999726880162, 0.000000000000000000 ) ) ;
#15512 = ADVANCED_FACE ( 'NONE', ( #40504 ), #35695, .T. ) ;
#15513 = EDGE_LOOP ( 'NONE', ( #12896, #50473, #61408, #59082 ) ) ;
#15514 = CARTESIAN_POINT ( 'NONE',  ( 2.500000000000002220, -51.66666666666666430, 4.330127018922192761 ) ) ;
#15515 = VERTEX_POINT ( 'NONE', #20260 ) ;
#15516 = CARTESIAN_POINT ( 'NONE',  ( -2.229367062499996610, -74.39583333196773651, 3.861377020970582219 ) ) ;
#15517 = CARTESIAN_POINT ( 'NONE',  ( 1.975475456537005874E-15, -21.75000000000000000, 5.000000000000000000 ) ) ;
#15518 = VERTEX_POINT ( 'NONE', #5777 ) ;
#15519 = CARTESIAN_POINT ( 'NONE',  ( 1.975475456537005874E-15, 12.24999999999999822, 5.000000000000000000 ) ) ;
#15521 = VECTOR ( 'NONE', #15160, 1000.000000000000000 ) ;
#15520 = CARTESIAN_POINT ( 'NONE',  ( 5.000000000000000888, -31.45833333060214798, 2.886751345948126879 ) ) ;
#15522 = CARTESIAN_POINT ( 'NONE',  ( 4.458734125000001214, -60.14583333196774362, 2.574251347313718519 ) ) ;
#15523 = CARTESIAN_POINT ( 'NONE',  ( -4.458734124999998549, -6.479166665301073103, 2.574251347313722516 ) ) ;
#15524 = ORIENTED_EDGE ( 'NONE', *, *, #38979, .F. ) ;
#15525 = DIRECTION ( 'NONE',  ( -0.000000000000000000, 1.000000000000000000, -0.000000000000000000 ) ) ;
#15526 = CARTESIAN_POINT ( 'NONE',  ( 4.458734125000001214, 13.10416666803226171, 2.574251347313718519 ) ) ;
#15527 = CARTESIAN_POINT ( 'NONE',  ( -55.35523342533222291, -142.3125000013656063, 4.444560631937231499 ) ) ;
#15528 = CARTESIAN_POINT ( 'NONE',  ( 1.339745962155612702, -27.16965819600733312, -5.000000000000000000 ) ) ;
#15529 = CARTESIAN_POINT ( 'NONE',  ( -4.458734124999999437, -160.9375000013655779, -5.460374474430324690E-16 ) ) ;
#15530 = FACE_OUTER_BOUND ( 'NONE', #23752, .T. ) ;
#15531 = VERTEX_POINT ( 'NONE', #50156 ) ;
#15532 = CARTESIAN_POINT ( 'NONE',  ( 2.229367062500001939, -83.97916666530106511, 3.861377020970579999 ) ) ;
#15533 = DIRECTION ( 'NONE',  ( -0.000000000000000000, 1.000000000000000000, -0.000000000000000000 ) ) ;
#15534 = CARTESIAN_POINT ( 'NONE',  ( -4.458734124999999437, 0.6041666680322611560, -2.574251347313719407 ) ) ;
#15535 = DIRECTION ( 'NONE',  ( -0.000000000000000000, 1.000000000000000000, -0.000000000000000000 ) ) ;
#15536 = CARTESIAN_POINT ( 'NONE',  ( -4.999999999999999112, -86.91666666666667140, 2.886751345948131764 ) ) ;
#15537 = CARTESIAN_POINT ( 'NONE',  ( 1.975475456537005874E-15, -88.74999999999998579, 5.000000000000000000 ) ) ;
#15538 = CARTESIAN_POINT ( 'NONE',  ( -2.229367062500000163, -67.72916666530106511, -3.861377020970580443 ) ) ;
#15539 = CARTESIAN_POINT ( 'NONE',  ( 2.500000000000002220, -25.54166666393547658, 4.330127018922192761 ) ) ;
#15540 = CARTESIAN_POINT ( 'NONE',  ( -2.499999999999996447, -72.70833333060214443, 4.330127018922195425 ) ) ;
#15541 = CARTESIAN_POINT ( 'NONE',  ( 5.000000000000000888, -110.4583333306021586, 2.886751345948126879 ) ) ;
#15542 = CARTESIAN_POINT ( 'NONE',  ( 5.000000000000000000, -43.37499999726880873, -6.123233995736766282E-16 ) ) ;
#15543 = CARTESIAN_POINT ( 'NONE',  ( -3.152548672688508926E-16, -46.56249999863440792, -5.148502694627439702 ) ) ;
#15544 = CARTESIAN_POINT ( 'NONE',  ( 4.458734124999998549, -32.97916666530106511, -2.574251347313721627 ) ) ;
#15545 = CARTESIAN_POINT ( 'NONE',  ( -4.458734124999999437, 4.437500001365595637, 0.000000000000000000 ) ) ;
#15546 = CARTESIAN_POINT ( 'NONE',  ( -2.071067811865548780, -161.8125000027312126, -4.999999999999926281 ) ) ;
#15547 = CARTESIAN_POINT ( 'NONE',  ( -3.535250795749689387E-16, 21.75000000000000000, -5.773502691896257311 ) ) ;
#15548 = CARTESIAN_POINT ( 'NONE',  ( 3.061616997868383141E-16, -143.8750000027312126, -5.000000000000000000 ) ) ;
#15549 = CARTESIAN_POINT ( 'NONE',  ( 0.000000000000000000, -120.0000000000000000, 5.000000000000000000 ) ) ;
#15550 = CARTESIAN_POINT ( 'NONE',  ( 9.457646018065525792E-16, -39.06249999863440081, 5.148502694627439702 ) ) ;
#15551 = CARTESIAN_POINT ( 'NONE',  ( 2.499999999999998668, -75.20833333060214443, -4.330127018922193649 ) ) ;
#15552 =( BOUNDED_CURVE ( )  B_SPLINE_CURVE ( 2, ( #57157, #7940, #38151, #42651, #23047, #52937, #42336, #58074, #27544 ),
 .UNSPECIFIED., .F., .F. ) 
 B_SPLINE_CURVE_WITH_KNOTS ( ( 3, 2, 2, 2, 3 ),
 ( 0.1375000000000000111, 0.1380952380952381042, 0.1392857142857142905, 0.1404761904761904767, 0.1410714285714285698 ),
 .UNSPECIFIED. ) 
 CURVE ( )  GEOMETRIC_REPRESENTATION_ITEM ( )  RATIONAL_B_SPLINE_CURVE ( ( 0.9330127018922194093, 0.9330127018922194093, 1.000000000000000000, 0.8660254037844387076, 1.000000000000000000, 0.8660254037844387076, 1.000000000000000000, 0.9330127018922194093, 0.9330127018922194093 ) ) 
 REPRESENTATION_ITEM ( '' )  );
#15553 = CARTESIAN_POINT ( 'NONE',  ( -54.64476657466781973, -145.0625000013656063, -4.444560631937228834 ) ) ;
#15554 = DIRECTION ( 'NONE',  ( -0.6485228581062915110, 0.000000000000000000, -0.7611951803011149931 ) ) ;
#15555 = CARTESIAN_POINT ( 'NONE',  ( -3.749999999999998224, -6.495190528383296247, -6.991905250253752868 ) ) ;
#15556 = CARTESIAN_POINT ( 'NONE',  ( -2.229367062500000163, -78.72916666530106511, -3.861377020970580443 ) ) ;
#15557 = CARTESIAN_POINT ( 'NONE',  ( -4.458734125000000326, -165.1250000013656347, 1.846868145590734089 ) ) ;
#15558 = CARTESIAN_POINT ( 'NONE',  ( -2.500000000000000444, -33.16666666666666430, -4.330127018922193649 ) ) ;
#15559 = CARTESIAN_POINT ( 'NONE',  ( 2.499999999999998668, 13.79166666939785202, -4.330127018922193649 ) ) ;
#15560 = CARTESIAN_POINT ( 'NONE',  ( 5.000000000000000888, -29.58333333333332504, 2.886751345948126879 ) ) ;
#15561 = CARTESIAN_POINT ( 'NONE',  ( -4.458734124999999437, -143.9375000013656063, -5.460374474430324690E-16 ) ) ;
#15562 = ORIENTED_EDGE ( 'NONE', *, *, #31225, .F. ) ;
#15563 = CARTESIAN_POINT ( 'NONE',  ( -4.458734124999999437, 25.35416666803225993, -2.574251347313719407 ) ) ;
#15564 = ORIENTED_EDGE ( 'NONE', *, *, #46332, .T. ) ;
#15565 = CARTESIAN_POINT ( 'NONE',  ( 2.229367062499998831, -59.89583333196774362, -3.861377020970580887 ) ) ;
#15566 = CARTESIAN_POINT ( 'NONE',  ( -5.000000000000000000, 22.12500000273118417, 0.000000000000000000 ) ) ;
#15567 = CARTESIAN_POINT ( 'NONE',  ( -5.000000000000000000, -60.87499999726880873, 0.000000000000000000 ) ) ;
#15568 = CARTESIAN_POINT ( 'NONE',  ( -2.500000000000000444, 13.83333333333333215, -4.330127018922193649 ) ) ;
#15569 = VECTOR ( 'NONE', #33688, 1000.000000000000000 ) ;
#15570 = CARTESIAN_POINT ( 'NONE',  ( -4.458734124999999437, -50.31249999863440792, 0.000000000000000000 ) ) ;
#15571 = CARTESIAN_POINT ( 'NONE',  ( 4.458734124999999437, -9.812499998634406140, -5.460374474430324690E-16 ) ) ;
#15572 =( BOUNDED_CURVE ( )  B_SPLINE_CURVE ( 2, ( #25911, #45529, #24961, #1490, #44566, #524, #39733, #34929, #15632 ),
 .UNSPECIFIED., .F., .F. ) 
 B_SPLINE_CURVE_WITH_KNOTS ( ( 3, 2, 2, 2, 3 ),
 ( 0.9062500000000000000, 0.9069444444444444420, 0.9083333333333333259, 0.9097222222222222099, 0.9104166666666666519 ),
 .UNSPECIFIED. ) 
 CURVE ( )  GEOMETRIC_REPRESENTATION_ITEM ( )  RATIONAL_B_SPLINE_CURVE ( ( 0.9330127018922194093, 0.9330127018922194093, 1.000000000000000000, 0.8660254037844387076, 1.000000000000000000, 0.8660254037844387076, 1.000000000000000000, 0.9330127018922194093, 0.9330127018922194093 ) ) 
 REPRESENTATION_ITEM ( '' )  );
#15573 = CARTESIAN_POINT ( 'NONE',  ( -5.000000000000000000, -23.08333333333333215, -2.886751345948128211 ) ) ;
#15574 = CARTESIAN_POINT ( 'NONE',  ( -2.500000000000000444, -64.04166666393547303, -4.330127018922193649 ) ) ;
#15575 = CARTESIAN_POINT ( 'NONE',  ( 2.499999999999998668, -91.20833333060214443, -4.330127018922193649 ) ) ;
#15576 = CARTESIAN_POINT ( 'NONE',  ( 5.000000000000000000, -11.37499999726881583, -6.123233995736766282E-16 ) ) ;
#15577 = CARTESIAN_POINT ( 'NONE',  ( 5.000000000000000000, -56.37499999726880162, -6.123233995736766282E-16 ) ) ;
#15579 = CARTESIAN_POINT ( 'NONE',  ( 2.229367062500001939, -23.97916666530107577, 3.861377020970579999 ) ) ;
#15578 = CARTESIAN_POINT ( 'NONE',  ( -1.339745962155623360, 15.20534180126147739, 4.999999999999991118 ) ) ;
#15580 = CARTESIAN_POINT ( 'NONE',  ( -1.336351044127974539E-14, 24.37500000273118417, 5.000000000000000000 ) ) ;
#15581 = CARTESIAN_POINT ( 'NONE',  ( -4.458734124999999437, -58.31249999863440081, 0.000000000000000000 ) ) ;
#15582 = CARTESIAN_POINT ( 'NONE',  ( 4.458734124999999437, -156.7500000013656063, 1.846868145590737864 ) ) ;
#15583 = CARTESIAN_POINT ( 'NONE',  ( 5.000000000000000000, -56.37499999726880162, -6.123233995736766282E-16 ) ) ;
#15584 = ORIENTED_EDGE ( 'NONE', *, *, #38126, .T. ) ;
#15585 = CARTESIAN_POINT ( 'NONE',  ( 1.339745962155600711, 13.29465819873851729, 5.000000000000007994 ) ) ;
#15586 = CARTESIAN_POINT ( 'NONE',  ( -4.458734124999999437, -0.6458333319677399542, -2.574251347313719407 ) ) ;
#15587 = ORIENTED_EDGE ( 'NONE', *, *, #32677, .F. ) ;
#15589 = CARTESIAN_POINT ( 'NONE',  ( 2.500000000000002220, -9.541666663935483683, 4.330127018922192761 ) ) ;
#15588 = CARTESIAN_POINT ( 'NONE',  ( -5.000000000000000000, -27.99999999999999645, 0.000000000000000000 ) ) ;
#15590 = CARTESIAN_POINT ( 'NONE',  ( -4.458734125000001214, -155.8750000013655779, 1.846868145590734089 ) ) ;
#15591 = ORIENTED_EDGE ( 'NONE', *, *, #61039, .T. ) ;
#15592 = CARTESIAN_POINT ( 'NONE',  ( 5.000000000000000000, 25.50000000000000000, -6.123233995736766282E-16 ) ) ;
#15593 = CARTESIAN_POINT ( 'NONE',  ( -54.60164318462004474, -129.3750000000000284, -4.984105922594373794 ) ) ;
#15594 = CARTESIAN_POINT ( 'NONE',  ( 3.061616997868383141E-16, -160.8750000027311842, -5.000000000000000000 ) ) ;
#15595 = CARTESIAN_POINT ( 'NONE',  ( -4.458734124999999437, -44.56249999863440081, 0.000000000000000000 ) ) ;
#15596 = ORIENTED_EDGE ( 'NONE', *, *, #11849, .F. ) ;
#15597 = CARTESIAN_POINT ( 'NONE',  ( 4.458734124999998549, 14.27083333469892779, -2.574251347313721627 ) ) ;
#15598 = CARTESIAN_POINT ( 'NONE',  ( -3.152548672688508926E-16, 28.43750000136559208, -5.148502694627439702 ) ) ;
#15599 = CARTESIAN_POINT ( 'NONE',  ( -59.29741812935640155, -152.6250000013656063, -2.196230717870135685 ) ) ;
#15600 = LINE ( 'NONE', #35218, #62412 ) ;
#15601 = CARTESIAN_POINT ( 'NONE',  ( 7.500000000000000000, -5.637851296924623057E-15, -6.991905250253753756 ) ) ;
#15602 = CARTESIAN_POINT ( 'NONE',  ( 0.000000000000000000, -120.0000000000000000, 5.000000000000000000 ) ) ;
#15603 = CARTESIAN_POINT ( 'NONE',  ( 4.458734124999999437, -62.81249999863440792, -5.460374474430324690E-16 ) ) ;
#15604 = FACE_OUTER_BOUND ( 'NONE', #18590, .T. ) ;
#15605 = CARTESIAN_POINT ( 'NONE',  ( -3.152548672688508926E-16, 16.43750000136559564, -5.148502694627439702 ) ) ;
#15606 = EDGE_CURVE ( 'NONE', #42322, #26829, #45017, .T. ) ;
#15607 = LINE ( 'NONE', #14957, #22787 ) ;
#15608 = CARTESIAN_POINT ( 'NONE',  ( -2.229367062500000163, -49.72916666530107221, -3.861377020970580443 ) ) ;
#15609 = CARTESIAN_POINT ( 'NONE',  ( 2.500000000000002220, -8.541666663935483683, 4.330127018922192761 ) ) ;
#15610 = CARTESIAN_POINT ( 'NONE',  ( -5.000000000000000000, 4.916666666666666075, -2.886751345948128211 ) ) ;
#15611 = CARTESIAN_POINT ( 'NONE',  ( -2.499999999999996447, -65.70833333060213022, 4.330127018922195425 ) ) ;
#15612 = CARTESIAN_POINT ( 'NONE',  ( -4.458734124999999437, -88.64583333196773651, -2.574251347313719407 ) ) ;
#15613 = CARTESIAN_POINT ( 'NONE',  ( 1.339745962155615144, -104.5803417985302701, 4.999999999999999112 ) ) ;
#15614 = CARTESIAN_POINT ( 'NONE',  ( 9.457646018065525792E-16, -16.31249999863440436, 5.148502694627439702 ) ) ;
#15615 =( BOUNDED_CURVE ( )  B_SPLINE_CURVE ( 2, ( #37248, #12794, #7984, #35225, #50654, #11089, #16561, #1790, #11408 ),
 .UNSPECIFIED., .F., .F. ) 
 B_SPLINE_CURVE_WITH_KNOTS ( ( 3, 2, 2, 2, 3 ),
 ( 0.2562499999999999778, 0.2569444444444444198, 0.2583333333333333592, 0.2597222222222222432, 0.2604166666666666852 ),
 .UNSPECIFIED. ) 
 CURVE ( )  GEOMETRIC_REPRESENTATION_ITEM ( )  RATIONAL_B_SPLINE_CURVE ( ( 0.9330127018922194093, 0.9330127018922194093, 1.000000000000000000, 0.8660254037844387076, 1.000000000000000000, 0.8660254037844387076, 1.000000000000000000, 0.9330127018922194093, 0.9330127018922194093 ) ) 
 REPRESENTATION_ITEM ( '' )  );
#15616 = ORIENTED_EDGE ( 'NONE', *, *, #20028, .T. ) ;
#15617 = CARTESIAN_POINT ( 'NONE',  ( -1.339745962155610925, -46.66965819600733312, 5.000000000000000000 ) ) ;
#15618 = CARTESIAN_POINT ( 'NONE',  ( 2.229367062499998831, -101.6458333319677365, -3.861377020970580887 ) ) ;
#15619 = CARTESIAN_POINT ( 'NONE',  ( -3.535533905932737309, -160.7500000027312126, -3.535533905932738197 ) ) ;
#15620 = VERTEX_POINT ( 'NONE', #39539 ) ;
#15621 = CARTESIAN_POINT ( 'NONE',  ( 9.457646018065525792E-16, -96.31249999863439371, 5.148502694627439702 ) ) ;
#15622 = CARTESIAN_POINT ( 'NONE',  ( -2.500000000000000444, 21.83333333333333215, -4.330127018922193649 ) ) ;
#15623 = CARTESIAN_POINT ( 'NONE',  ( -5.000000000000000000, -59.87499999726880873, 0.000000000000000000 ) ) ;
#15624 = CARTESIAN_POINT ( 'NONE',  ( -4.999999999999998224, 19.20833333606451632, 2.886751345948131764 ) ) ;
#15625 = CARTESIAN_POINT ( 'NONE',  ( -59.29741812935640155, -126.6250000013656489, -2.196230717870135685 ) ) ;
#15626 = CARTESIAN_POINT ( 'NONE',  ( -54.64476657466781973, -142.8125000013656063, -4.444560631937228834 ) ) ;
#15627 = CARTESIAN_POINT ( 'NONE',  ( 4.458734124999998549, -16.72916666530107577, -2.574251347313721627 ) ) ;
#15628 = CARTESIAN_POINT ( 'NONE',  ( 2.229367062499998831, 5.104166668032261711, -3.861377020970580887 ) ) ;
#15629 = CARTESIAN_POINT ( 'NONE',  ( 4.458734124999999437, -63.06249999863440792, -5.460374474430324690E-16 ) ) ;
#15630 = CARTESIAN_POINT ( 'NONE',  ( 2.500000000000002220, -94.54166666393547303, 4.330127018922192761 ) ) ;
#15631 = CARTESIAN_POINT ( 'NONE',  ( -4.458734124999999437, -18.39583333196774007, -2.574251347313719407 ) ) ;
#15632 = CARTESIAN_POINT ( 'NONE',  ( -6.972266317189433020E-16, -80.12499999726881583, -5.000000000000000000 ) ) ;
#15633 = CARTESIAN_POINT ( 'NONE',  ( -2.071067811865475061, -155.6875000000000284, -5.000000000000000888 ) ) ;
#15634 = CARTESIAN_POINT ( 'NONE',  ( -5.000000000000000000, -9.083333333333333925, -2.886751345948128211 ) ) ;
#15635 = CARTESIAN_POINT ( 'NONE',  ( 4.458734124999999437, -157.4375000013655779, 0.000000000000000000 ) ) ;
#15636 = VERTEX_POINT ( 'NONE', #55322 ) ;
#15637 = CARTESIAN_POINT ( 'NONE',  ( -4.458734124999997661, -47.47916666530106511, 2.574251347313722516 ) ) ;
#15638 = FACE_OUTER_BOUND ( 'NONE', #48883, .T. ) ;
#15639 = CARTESIAN_POINT ( 'NONE',  ( -51.75738570946856498, -155.0000000000000284, 3.805975901505577408 ) ) ;
#15640 = CARTESIAN_POINT ( 'NONE',  ( -4.999999999999999112, 29.08333333333333215, 2.886751345948131764 ) ) ;
#15641 = CARTESIAN_POINT ( 'NONE',  ( 2.229367062499998831, 4.354166668032260823, -3.861377020970580887 ) ) ;
#15642 = CARTESIAN_POINT ( 'NONE',  ( 0.000000000000000000, -120.0000000000000000, 0.000000000000000000 ) ) ;
#15643 = FACE_OUTER_BOUND ( 'NONE', #23072, .T. ) ;
#15644 = DIRECTION ( 'NONE',  ( -0.4999999999999951705, 0.000000000000000000, 0.8660254037844414832 ) ) ;
#15645 = CARTESIAN_POINT ( 'NONE',  ( -4.458734124999999437, 22.43750000136559564, 0.000000000000000000 ) ) ;
#15646 = CARTESIAN_POINT ( 'NONE',  ( 1.060575238724906964E-15, -74.75000000000000000, 5.773502691896257311 ) ) ;
#15647 = CARTESIAN_POINT ( 'NONE',  ( -5.000000000000000000, 6.125000002731185056, 0.000000000000000000 ) ) ;
#15648 = ORIENTED_EDGE ( 'NONE', *, *, #33834, .F. ) ;
#15649 = LINE ( 'NONE', #35265, #34548 ) ;
#15650 = ORIENTED_EDGE ( 'NONE', *, *, #47358, .T. ) ;
#15651 = CARTESIAN_POINT ( 'NONE',  ( -3.152548672688508926E-16, -36.56249999863441502, -5.148502694627439702 ) ) ;
#15652 = CARTESIAN_POINT ( 'NONE',  ( -3.535250795749689387E-16, -40.12499999726880162, -5.773502691896257311 ) ) ;
#15653 = EDGE_LOOP ( 'NONE', ( #608, #39296, #54029, #31022 ) ) ;
#15654 = CARTESIAN_POINT ( 'NONE',  ( -2.229367062499996610, -12.14583333196774007, 3.861377020970582219 ) ) ;
#15655 = EDGE_LOOP ( 'NONE', ( #44077, #34658, #57620, #14224 ) ) ;
#15656 = CARTESIAN_POINT ( 'NONE',  ( 5.000000000000000000, -81.41666666666667140, -2.886751345948129988 ) ) ;
#15657 = CYLINDRICAL_SURFACE ( 'NONE', #55619, 5.000000000000000000 ) ;
#15658 = CARTESIAN_POINT ( 'NONE',  ( 4.458734124999999437, -63.06249999863440792, -5.460374474430324690E-16 ) ) ;
#15659 =( BOUNDED_CURVE ( )  B_SPLINE_CURVE ( 2, ( #59845, #55338, #40209, #667, #11254, #15457, #25741, #55972, #50821 ),
 .UNSPECIFIED., .F., .F. ) 
 B_SPLINE_CURVE_WITH_KNOTS ( ( 3, 2, 2, 2, 3 ),
 ( 0.4645833333333333481, 0.4652777777777777901, 0.4666666666666666741, 0.4680555555555555580, 0.4687500000000000000 ),
 .UNSPECIFIED. ) 
 CURVE ( )  GEOMETRIC_REPRESENTATION_ITEM ( )  RATIONAL_B_SPLINE_CURVE ( ( 0.9330127018922194093, 0.9330127018922194093, 1.000000000000000000, 0.8660254037844387076, 1.000000000000000000, 0.8660254037844387076, 1.000000000000000000, 0.9330127018922194093, 0.9330127018922194093 ) ) 
 REPRESENTATION_ITEM ( '' )  );
#15660 = CARTESIAN_POINT ( 'NONE',  ( -5.000000000000000000, -85.95833333060213022, -2.886751345948128211 ) ) ;
#15662 = ORIENTED_EDGE ( 'NONE', *, *, #45553, .T. ) ;
#15661 = DIRECTION ( 'NONE',  ( -0.000000000000000000, 1.000000000000000000, -0.000000000000000000 ) ) ;
#15663 = CARTESIAN_POINT ( 'NONE',  ( -53.33387254593733928, -140.8125000000000284, 5.149110718188519620 ) ) ;
#15664 = CARTESIAN_POINT ( 'NONE',  ( 2.229367062499998831, -24.89583333196773651, -3.861377020970580887 ) ) ;
#15665 = CARTESIAN_POINT ( 'NONE',  ( -6.972266317189433020E-16, -84.24999999999998579, -5.000000000000000000 ) ) ;
#15666 = VERTEX_POINT ( 'NONE', #59177 ) ;
#15667 = APPLICATION_PROTOCOL_DEFINITION ( 'draft international standard', 'automotive_design', 1998, #242 ) ;
#15668 = CARTESIAN_POINT ( 'NONE',  ( -8.190561711645485556E-16, -162.9375000013655779, 4.458734124999999437 ) ) ;
#15669 = CARTESIAN_POINT ( 'NONE',  ( 9.457646018065525792E-16, 27.93750000136559208, 5.148502694627439702 ) ) ;
#15670 = CARTESIAN_POINT ( 'NONE',  ( 2.071067811865306751, -155.8125000000000284, -5.000000000000171418 ) ) ;
#15671 = ORIENTED_EDGE ( 'NONE', *, *, #40871, .F. ) ;
#15672 = CARTESIAN_POINT ( 'NONE',  ( -51.60603307380591787, -148.1875000013656063, -2.891590998281053704 ) ) ;
#15673 = CARTESIAN_POINT ( 'NONE',  ( 4.458734124999999437, -75.06249999863440792, -5.460374474430324690E-16 ) ) ;
#15674 = CARTESIAN_POINT ( 'NONE',  ( -50.18089887299979068, -133.8125000027312126, 2.462841084822635640 ) ) ;
#15675 = CARTESIAN_POINT ( 'NONE',  ( -4.458734124999997661, -45.22916666530106511, 2.574251347313722516 ) ) ;
#15676 = CARTESIAN_POINT ( 'NONE',  ( 1.846868145590736310, -143.8750000013656063, 4.458734124999997661 ) ) ;
#15677 = CARTESIAN_POINT ( 'NONE',  ( -7.499999999999999112, 4.651022038490018495, -7.928862870699868282 ) ) ;
#15678 = CARTESIAN_POINT ( 'NONE',  ( 9.457646018065525792E-16, -50.06249999863440792, 5.148502694627439702 ) ) ;
#15679 = CARTESIAN_POINT ( 'NONE',  ( -1.339745962155613812, -71.20534180126148271, -5.000000000000000000 ) ) ;
#15680 = EDGE_CURVE ( 'NONE', #35595, #5760, #14839, .T. ) ;
#15681 = CARTESIAN_POINT ( 'NONE',  ( -4.458734124999999437, -16.39583333196773651, -2.574251347313719407 ) ) ;
#15682 = CARTESIAN_POINT ( 'NONE',  ( 5.000000000000000000, -99.50000000000000000, -6.123233995736766282E-16 ) ) ;
#15683 = CARTESIAN_POINT ( 'NONE',  ( -3.535533905932737309, -167.6250000000000284, -3.535533905932738197 ) ) ;
#15684 = CARTESIAN_POINT ( 'NONE',  ( 2.229367062499998831, -31.89583333196773651, -3.861377020970580887 ) ) ;
#15685 = CARTESIAN_POINT ( 'NONE',  ( -2.499999999999996447, 6.291666669397851130, 4.330127018922195425 ) ) ;
#15686 = CARTESIAN_POINT ( 'NONE',  ( -6.972266317189433020E-16, -75.12499999726880162, -5.000000000000000000 ) ) ;
#15687 = CARTESIAN_POINT ( 'NONE',  ( -56.48576386720575471, -130.7500000013656063, -4.591703134518078322 ) ) ;
#15688 = CARTESIAN_POINT ( 'NONE',  ( -4.458734124999999437, -76.64583333196775072, -2.574251347313719407 ) ) ;
#15689 = CARTESIAN_POINT ( 'NONE',  ( -5.000000000000000888, -166.4375000000000853, 2.071067811865474617 ) ) ;
#15690 = CARTESIAN_POINT ( 'NONE',  ( 0.000000000000000000, -120.0000000000000000, 5.000000000000000000 ) ) ;
#15691 = DIRECTION ( 'NONE',  ( -0.000000000000000000, 1.000000000000000000, -0.000000000000000000 ) ) ;
#15692 = CARTESIAN_POINT ( 'NONE',  ( 4.458734124999998549, 1.020833334698927120, -2.574251347313721627 ) ) ;
#15693 = ORIENTED_EDGE ( 'NONE', *, *, #25113, .F. ) ;
#15694 = CARTESIAN_POINT ( 'NONE',  ( 6.123233995736766282E-16, -170.0000000000000000, -5.000000000000000000 ) ) ;
#15695 = CARTESIAN_POINT ( 'NONE',  ( 1.975475456537005874E-15, 12.24999999999999822, 5.000000000000000000 ) ) ;
#15697 = CARTESIAN_POINT ( 'NONE',  ( -3.152548672688508926E-16, -34.56249999863440792, -5.148502694627439702 ) ) ;
#15696 = CARTESIAN_POINT ( 'NONE',  ( 4.458734125000001214, -85.89583333196773651, 2.574251347313718519 ) ) ;
#15698 = EDGE_CURVE ( 'NONE', #28303, #54373, #38693, .T. ) ;
#15699 = CARTESIAN_POINT ( 'NONE',  ( 1.975475456537005874E-15, -9.750000000000000000, 5.000000000000000000 ) ) ;
#15700 = CARTESIAN_POINT ( 'NONE',  ( 9.457646018065525792E-16, -82.31249999863440792, 5.148502694627439702 ) ) ;
#15701 = CARTESIAN_POINT ( 'NONE',  ( 4.458734124999999437, 19.93750000136559208, -5.460374474430324690E-16 ) ) ;
#15702 = CARTESIAN_POINT ( 'NONE',  ( 1.975475456537005874E-15, -52.75000000000000000, 5.000000000000000000 ) ) ;
#15703 = CARTESIAN_POINT ( 'NONE',  ( -57.89159099828107458, -139.6875000013656063, -3.393966926194107447 ) ) ;
#15704 = CARTESIAN_POINT ( 'NONE',  ( -4.458734124999999437, -0.3124999986344051406, 0.000000000000000000 ) ) ;
#15705 = CARTESIAN_POINT ( 'NONE',  ( 4.458734124999998549, 22.02083333469892779, -2.574251347313721627 ) ) ;
#15706 = EDGE_CURVE ( 'NONE', #18224, #49905, #31174, .T. ) ;
#15707 = CARTESIAN_POINT ( 'NONE',  ( -3.152548672688508926E-16, -46.81249999863440792, -5.148502694627439702 ) ) ;
#15708 = CARTESIAN_POINT ( 'NONE',  ( -5.000000000000000000, -45.87499999726880873, 0.000000000000000000 ) ) ;
#15709 = CARTESIAN_POINT ( 'NONE',  ( 9.457646018065525792E-16, -87.06249999863440792, 5.148502694627439702 ) ) ;
#15710 = CARTESIAN_POINT ( 'NONE',  ( 4.458734124999998549, -4.729166665301071326, -2.574251347313721627 ) ) ;
#15711 = CARTESIAN_POINT ( 'NONE',  ( -4.458734124999999437, -27.64583333196774007, -2.574251347313719407 ) ) ;
#15712 = CARTESIAN_POINT ( 'NONE',  ( -53.51423613279429503, -133.5000000013656347, 4.591703134518082763 ) ) ;
#15713 = CARTESIAN_POINT ( 'NONE',  ( -4.458734124999998549, -75.22916666530106511, 2.574251347313722516 ) ) ;
#15714 = CARTESIAN_POINT ( 'NONE',  ( -4.999999999999999112, -110.7916666639354730, 2.886751345948131764 ) ) ;
#15715 = CARTESIAN_POINT ( 'NONE',  ( -4.458734124999998549, 24.77083333469893134, 2.574251347313722516 ) ) ;
#15716 = CARTESIAN_POINT ( 'NONE',  ( -1.339745962155610925, -64.79465819873851729, 5.000000000000000000 ) ) ;
#15717 = CARTESIAN_POINT ( 'NONE',  ( -2.071067811865391128, -145.8125000027312410, -5.000000000000086153 ) ) ;
#15718 = CARTESIAN_POINT ( 'NONE',  ( 4.458734124999999437, -80.06249999863440792, -5.460374474430324690E-16 ) ) ;
#15719 = CARTESIAN_POINT ( 'NONE',  ( 5.000000000000000000, -61.41666666666665719, -2.886751345948129988 ) ) ;
#15720 = CARTESIAN_POINT ( 'NONE',  ( -6.972266317189433020E-16, -90.12499999726880162, -5.000000000000000000 ) ) ;
#15721 = CARTESIAN_POINT ( 'NONE',  ( -5.000000000000000000, 26.12500000273118417, 0.000000000000000000 ) ) ;
#15722 = ORIENTED_EDGE ( 'NONE', *, *, #20853, .T. ) ;
#15723 = CARTESIAN_POINT ( 'NONE',  ( -2.500000000000000444, -57.16666666666667140, -4.330127018922193649 ) ) ;
#15724 = DIRECTION ( 'NONE',  ( -0.000000000000000000, 1.000000000000000000, -0.000000000000000000 ) ) ;
#15726 = CARTESIAN_POINT ( 'NONE',  ( 5.000000000000000888, -19.58333333333333215, 2.886751345948126879 ) ) ;
#15725 = LINE ( 'NONE', #26648, #58493 ) ;
#15727 = CARTESIAN_POINT ( 'NONE',  ( 4.458734124999999437, -19.81249999863440081, -5.460374474430324690E-16 ) ) ;
#15728 = CARTESIAN_POINT ( 'NONE',  ( -4.458734124999999437, -83.39583333196773651, -2.574251347313719407 ) ) ;
#15729 = CARTESIAN_POINT ( 'NONE',  ( 5.000000000000000000, -23.29166666393548368, -2.886751345948129988 ) ) ;
#15730 = EDGE_CURVE ( 'NONE', #57534, #26333, #20901, .T. ) ;
#15732 = VERTEX_POINT ( 'NONE', #35058 ) ;
#15731 = CARTESIAN_POINT ( 'NONE',  ( -4.458734124999998549, -52.22916666530106511, 2.574251347313722516 ) ) ;
#15733 = CARTESIAN_POINT ( 'NONE',  ( 2.500000000000002220, -65.66666666666667140, 4.330127018922192761 ) ) ;
#15734 = CARTESIAN_POINT ( 'NONE',  ( 2.499999999999998668, -59.20833333060214443, -4.330127018922193649 ) ) ;
#15736 = VERTEX_POINT ( 'NONE', #54670 ) ;
#15735 = CARTESIAN_POINT ( 'NONE',  ( 2.229367062499998831, -2.895833331967738289, -3.861377020970580887 ) ) ;
#15737 = CARTESIAN_POINT ( 'NONE',  ( -52.10840900171896806, -151.1875000013656063, 3.393966926194110556 ) ) ;
#15738 = CARTESIAN_POINT ( 'NONE',  ( -5.000000000000000000, -66.08333333333332860, -2.886751345948128211 ) ) ;
#15739 = CARTESIAN_POINT ( 'NONE',  ( -8.190561711645485556E-16, -151.9375000013655779, 4.458734124999999437 ) ) ;
#15740 = CARTESIAN_POINT ( 'NONE',  ( -4.458734124999998549, -45.47916666530105800, 2.574251347313722516 ) ) ;
#15741 = LINE ( 'NONE', #20247, #20391 ) ;
#15742 = CARTESIAN_POINT ( 'NONE',  ( 2.071067811865476394, -157.1875000000000284, 5.000000000000000000 ) ) ;
#15743 = CYLINDRICAL_SURFACE ( 'NONE', #29228, 5.000000000000000000 ) ;
#15744 = CARTESIAN_POINT ( 'NONE',  ( -56.66612745406270335, -152.3125000000000000, -5.149110718188516067 ) ) ;
#15745 = CARTESIAN_POINT ( 'NONE',  ( 2.229367062499998831, -9.895833331967738289, -3.861377020970580887 ) ) ;
#15746 = CARTESIAN_POINT ( 'NONE',  ( 2.229367062499998831, -44.89583333196774362, -3.861377020970580887 ) ) ;
#15747 =( BOUNDED_CURVE ( )  B_SPLINE_CURVE ( 2, ( #12898, #56670, #60856, #61807, #27375, #21928, #12277, #31248, #17428 ),
 .UNSPECIFIED., .F., .F. ) 
 B_SPLINE_CURVE_WITH_KNOTS ( ( 3, 2, 2, 2, 3 ),
 ( 0.5916666666666671182, 0.5958333333333335480, 0.6000000000000000888, 0.6041666666666665186, 0.6083333333333329485 ),
 .UNSPECIFIED. ) 
 CURVE ( )  GEOMETRIC_REPRESENTATION_ITEM ( )  RATIONAL_B_SPLINE_CURVE ( ( 0.9999999999999918954, 0.9238795325112948431, 1.000000000000000000, 0.9238795325112867385, 1.000000000000000000, 0.9238795325112867385, 1.000000000000000000, 0.9238795325112928447, 0.9999999999999938938 ) ) 
 REPRESENTATION_ITEM ( '' )  );
#15748 = CARTESIAN_POINT ( 'NONE',  ( -75.00000000000000000, 0.000000000000000000, 8.999999999999998224 ) ) ;
#15749 = CARTESIAN_POINT ( 'NONE',  ( -4.458734125000001214, -145.8750000013656063, 1.846868145590734089 ) ) ;
#15750 = CARTESIAN_POINT ( 'NONE',  ( 2.229367062499998831, -92.89583333196773651, -3.861377020970580887 ) ) ;
#15751 = DIRECTION ( 'NONE',  ( 0.000000000000000000, 0.000000000000000000, 1.000000000000000000 ) ) ;
#15752 = ORIENTED_EDGE ( 'NONE', *, *, #52232, .T. ) ;
#15753 = DIRECTION ( 'NONE',  ( 0.000000000000000000, 1.000000000000000000, 0.000000000000000000 ) ) ;
#15754 = CARTESIAN_POINT ( 'NONE',  ( -2.229367062500000163, 26.27083333469892779, -3.861377020970580443 ) ) ;
#15755 = CARTESIAN_POINT ( 'NONE',  ( -51.75738570946856498, -144.8750000027312126, 3.805975901505576964 ) ) ;
#15756 = DIRECTION ( 'NONE',  ( 1.000000000000000000, 0.000000000000000000, 0.000000000000000000 ) ) ;
#15757 = ORIENTED_EDGE ( 'NONE', *, *, #54792, .T. ) ;
#15758 = CARTESIAN_POINT ( 'NONE',  ( -3.152548672688508926E-16, -2.562499998634407028, -5.148502694627439702 ) ) ;
#15759 = VECTOR ( 'NONE', #58471, 1000.000000000000000 ) ;
#15760 = EDGE_CURVE ( 'NONE', #40578, #10208, #20586, .T. ) ;
#15761 = EDGE_CURVE ( 'NONE', #55261, #54893, #45335, .T. ) ;
#15762 = CARTESIAN_POINT ( 'NONE',  ( -6.972266317189433020E-16, 6.750000000000000000, -5.000000000000000000 ) ) ;
#15763 = CARTESIAN_POINT ( 'NONE',  ( 9.457646018065525792E-16, -18.31249999863440436, 5.148502694627439702 ) ) ;
#15764 = CARTESIAN_POINT ( 'NONE',  ( 1.339745962155612702, 11.83034180399266688, -5.000000000000000000 ) ) ;
#15765 = CARTESIAN_POINT ( 'NONE',  ( 2.229367062500001939, -9.979166665301068662, 3.861377020970579999 ) ) ;
#15766 = CARTESIAN_POINT ( 'NONE',  ( -5.000000000000000000, -73.87499999726880162, 0.000000000000000000 ) ) ;
#15767 = CARTESIAN_POINT ( 'NONE',  ( 1.846868145590735200, -149.2500000013656063, -4.458734124999999437 ) ) ;
#15768 = CARTESIAN_POINT ( 'NONE',  ( -4.458734124999999437, 14.43750000136559386, 0.000000000000000000 ) ) ;
#15769 = ORIENTED_EDGE ( 'NONE', *, *, #46703, .T. ) ;
#15770 = DIRECTION ( 'NONE',  ( -0.000000000000000000, 1.000000000000000000, -0.000000000000000000 ) ) ;
#15771 = DIRECTION ( 'NONE',  ( -0.000000000000000000, 1.000000000000000000, -0.000000000000000000 ) ) ;
#15772 = CARTESIAN_POINT ( 'NONE',  ( 4.458734124999998549, -16.72916666530107577, -2.574251347313721627 ) ) ;
#15773 = EDGE_CURVE ( 'NONE', #29768, #62355, #30054, .T. ) ;
#15774 = CARTESIAN_POINT ( 'NONE',  ( 2.499999999999998668, -88.20833333060214443, -4.330127018922193649 ) ) ;
#15775 = CARTESIAN_POINT ( 'NONE',  ( -59.44456063193725015, -151.5625000013656063, -0.3552334253322034230 ) ) ;
#15776 = CARTESIAN_POINT ( 'NONE',  ( -2.500000000000000444, -47.04166666393547303, -4.330127018922193649 ) ) ;
#15777 = CARTESIAN_POINT ( 'NONE',  ( 5.000000000000000888, -74.58333333333332860, 2.886751345948126879 ) ) ;
#15778 = CARTESIAN_POINT ( 'NONE',  ( 4.458734125000000326, 16.10416666803225993, 2.574251347313718519 ) ) ;
#15779 = CARTESIAN_POINT ( 'NONE',  ( 1.975475456537005874E-15, -41.74999999999999289, 5.000000000000000000 ) ) ;
#15780 = EDGE_CURVE ( 'NONE', #49422, #50022, #37537, .T. ) ;
#15781 = DIRECTION ( 'NONE',  ( -0.000000000000000000, 1.000000000000000000, -0.000000000000000000 ) ) ;
#15782 = CARTESIAN_POINT ( 'NONE',  ( -4.458734124999999437, 13.60416666803226171, -2.574251347313719407 ) ) ;
#15783 = CARTESIAN_POINT ( 'NONE',  ( 9.457646018065525792E-16, -65.06249999863440792, 5.148502694627439702 ) ) ;
#15784 = EDGE_LOOP ( 'NONE', ( #27990, #60931, #25709, #19457 ) ) ;
#15785 = CARTESIAN_POINT ( 'NONE',  ( -2.229367062500000163, -15.72916666530107399, -3.861377020970580443 ) ) ;
#15786 = CARTESIAN_POINT ( 'NONE',  ( 1.060575238724906964E-15, 3.249999999999999556, 5.773502691896257311 ) ) ;
#15787 = CARTESIAN_POINT ( 'NONE',  ( 3.152801135295366208, -162.5625000013656063, 3.152801135295367985 ) ) ;
#15788 = CARTESIAN_POINT ( 'NONE',  ( -5.000000000000000000, -40.87499999726880162, 0.000000000000000000 ) ) ;
#15789 = CARTESIAN_POINT ( 'NONE',  ( -4.458734124999999437, -57.39583333196773651, -2.574251347313719407 ) ) ;
#15790 = CARTESIAN_POINT ( 'NONE',  ( -5.000000000000000000, -94.95833333060213022, -2.886751345948128211 ) ) ;
#15791 = CARTESIAN_POINT ( 'NONE',  ( -4.458734124999997661, -34.22916666530107221, 2.574251347313722516 ) ) ;
#15792 = CARTESIAN_POINT ( 'NONE',  ( -6.972266317189433020E-16, 19.87500000273118417, -5.000000000000000000 ) ) ;
#15793 = DIRECTION ( 'NONE',  ( 0.000000000000000000, 0.000000000000000000, 1.000000000000000000 ) ) ;
#15794 = CARTESIAN_POINT ( 'NONE',  ( 0.000000000000000000, -170.0000000000000000, 5.000000000000000000 ) ) ;
#15795 = CARTESIAN_POINT ( 'NONE',  ( -59.81910112700027327, -141.1875000000000000, -2.462841084822392279 ) ) ;
#15796 = CARTESIAN_POINT ( 'NONE',  ( 1.846868145590736310, -150.8750000013655779, 4.458734124999997661 ) ) ;
#15797 = CARTESIAN_POINT ( 'NONE',  ( 5.000000000000000000, -42.49999999999999289, -6.123233995736766282E-16 ) ) ;
#15798 = CARTESIAN_POINT ( 'NONE',  ( -4.999999999999998224, -57.79166666393548013, 2.886751345948131764 ) ) ;
#15799 = CARTESIAN_POINT ( 'NONE',  ( 1.339745962155612702, -86.16965819600731891, -5.000000000000000000 ) ) ;
#15800 = ORIENTED_EDGE ( 'NONE', *, *, #42579, .F. ) ;
#15801 = CARTESIAN_POINT ( 'NONE',  ( -4.458734124999999437, -105.3124999986344221, 0.000000000000000000 ) ) ;
#15802 = CARTESIAN_POINT ( 'NONE',  ( -4.458734124999999437, 0.4375000013655955255, 0.000000000000000000 ) ) ;
#15803 = CARTESIAN_POINT ( 'NONE',  ( -4.999999999999998224, -96.79166666393545881, 2.886751345948131764 ) ) ;
#15804 = CARTESIAN_POINT ( 'NONE',  ( 1.060575238724906964E-15, -0.7500000000000007772, 5.773502691896257311 ) ) ;
#15805 = CARTESIAN_POINT ( 'NONE',  ( -3.152548672688508926E-16, -66.56249999863440792, -5.148502694627439702 ) ) ;
#15806 = VECTOR ( 'NONE', #35220, 1000.000000000000000 ) ;
#15807 = CARTESIAN_POINT ( 'NONE',  ( -4.999999999999998224, -25.91666666666666430, 2.886751345948131764 ) ) ;
#15808 = CARTESIAN_POINT ( 'NONE',  ( 5.000000000000000000, -5.291666663935480130, -2.886751345948129988 ) ) ;
#15810 = VERTEX_POINT ( 'NONE', #17024 ) ;
#15809 = CARTESIAN_POINT ( 'NONE',  ( 2.229367062500001939, -34.97916666530107221, 3.861377020970579999 ) ) ;
#15811 = DIRECTION ( 'NONE',  ( 0.000000000000000000, 0.000000000000000000, 1.000000000000000000 ) ) ;
#15812 = CARTESIAN_POINT ( 'NONE',  ( 1.975475456537005874E-15, -6.749999999999999112, 5.000000000000000000 ) ) ;
#15814 = ORIENTED_EDGE ( 'NONE', *, *, #1635, .T. ) ;
#15813 = CARTESIAN_POINT ( 'NONE',  ( -4.458734124999999437, 14.35416666803226171, -2.574251347313719407 ) ) ;
#15815 = CARTESIAN_POINT ( 'NONE',  ( 1.975475456537005874E-15, -101.7499999999999858, 5.000000000000000000 ) ) ;
#15816 = CARTESIAN_POINT ( 'NONE',  ( -5.000000000000000000, -49.00000000000000000, 0.000000000000000000 ) ) ;
#15817 = CARTESIAN_POINT ( 'NONE',  ( 2.229367062500001939, -28.22916666530107221, 3.861377020970579999 ) ) ;
#15818 = CARTESIAN_POINT ( 'NONE',  ( 5.000000000000000888, -4.583333333333334814, 2.886751345948126879 ) ) ;
#15819 = CARTESIAN_POINT ( 'NONE',  ( -2.229367062499996610, -74.14583333196773651, 3.861377020970582219 ) ) ;
#15820 =( BOUNDED_CURVE ( )  B_SPLINE_CURVE ( 2, ( #13385, #42332, #57153, #13068, #4056, #39388, #34244, #8871, #28797 ),
 .UNSPECIFIED., .F., .F. ) 
 B_SPLINE_CURVE_WITH_KNOTS ( ( 3, 2, 2, 2, 3 ),
 ( 0.3062500000000000222, 0.3069444444444444642, 0.3083333333333333481, 0.3097222222222222321, 0.3104166666666666741 ),
 .UNSPECIFIED. ) 
 CURVE ( )  GEOMETRIC_REPRESENTATION_ITEM ( )  RATIONAL_B_SPLINE_CURVE ( ( 0.9330127018922194093, 0.9330127018922194093, 1.000000000000000000, 0.8660254037844387076, 1.000000000000000000, 0.8660254037844387076, 1.000000000000000000, 0.9330127018922194093, 0.9330127018922194093 ) ) 
 REPRESENTATION_ITEM ( '' )  );
#15821 = CARTESIAN_POINT ( 'NONE',  ( -5.000000000000000888, -169.5625000000000284, -2.071067811865475949 ) ) ;
#15822 = CARTESIAN_POINT ( 'NONE',  ( -2.229367062499996610, -80.14583333196773651, 3.861377020970582219 ) ) ;
#15823 = CARTESIAN_POINT ( 'NONE',  ( -52.10840900171896806, -134.4375000013656063, 3.393966926194110556 ) ) ;
#15824 = CARTESIAN_POINT ( 'NONE',  ( -2.229367062499996610, -28.39583333196774007, 3.861377020970582219 ) ) ;
#15825 = ORIENTED_EDGE ( 'NONE', *, *, #4348, .F. ) ;
#15826 = LINE ( 'NONE', #20006, #16626 ) ;
#15827 = ORIENTED_EDGE ( 'NONE', *, *, #38463, .F. ) ;
#15828 = CARTESIAN_POINT ( 'NONE',  ( -2.229367062499996610, -76.39583333196773651, 3.861377020970582219 ) ) ;
#15829 = CARTESIAN_POINT ( 'NONE',  ( 6.123233995736766282E-16, -120.0000000000000000, -5.000000000000000000 ) ) ;
#15830 = ORIENTED_EDGE ( 'NONE', *, *, #49097, .F. ) ;
#15831 = CARTESIAN_POINT ( 'NONE',  ( 1.975475456537005874E-15, -14.62499999726881228, 5.000000000000000000 ) ) ;
#15832 =( REPRESENTATION_RELATIONSHIP ('NONE','NONE', #27855, #49651 ) REPRESENTATION_RELATIONSHIP_WITH_TRANSFORMATION ( #40416 )SHAPE_REPRESENTATION_RELATIONSHIP( ) );
#15833 = CARTESIAN_POINT ( 'NONE',  ( -50.75781946612335105, -135.0000000000005969, -1.372666862511563224 ) ) ;
#15834 = CARTESIAN_POINT ( 'NONE',  ( 4.458734125000001214, -67.14583333196773651, 2.574251347313718519 ) ) ;
#15835 = CARTESIAN_POINT ( 'NONE',  ( -3.152548672688508926E-16, -1.812499998634406362, -5.148502694627439702 ) ) ;
#15836 = ORIENTED_EDGE ( 'NONE', *, *, #56237, .F. ) ;
#15837 = ADVANCED_FACE ( 'NONE', ( #46294 ), #51126, .T. ) ;
#15838 = CARTESIAN_POINT ( 'NONE',  ( 0.000000000000000000, 0.000000000000000000, -8.499999999999998224 ) ) ;
#15839 = CARTESIAN_POINT ( 'NONE',  ( 1.339745962155612702, -91.29465819873853150, -5.000000000000000000 ) ) ;
#15840 = CARTESIAN_POINT ( 'NONE',  ( -4.458734124999998549, 9.770833334698927786, 2.574251347313722516 ) ) ;
#15841 = CARTESIAN_POINT ( 'NONE',  ( -52.80376928212989185, -139.8750000013655779, -4.297418129356379346 ) ) ;
#15842 = CARTESIAN_POINT ( 'NONE',  ( 5.000000000000000000, -47.37499999726880873, -6.123233995736766282E-16 ) ) ;
#15843 = CARTESIAN_POINT ( 'NONE',  ( -3.152801135295367985, -160.8125000013656063, 3.152801135295367096 ) ) ;
#15844 =( BOUNDED_CURVE ( )  B_SPLINE_CURVE ( 2, ( #3741, #19136, #38753, #14318, #23362, #38443, #48101, #33940, #29097 ),
 .UNSPECIFIED., .F., .F. ) 
 B_SPLINE_CURVE_WITH_KNOTS ( ( 3, 2, 2, 2, 3 ),
 ( 0.5354166666666666519, 0.5361111111111110938, 0.5374999999999999778, 0.5388888888888888618, 0.5395833333333333037 ),
 .UNSPECIFIED. ) 
 CURVE ( )  GEOMETRIC_REPRESENTATION_ITEM ( )  RATIONAL_B_SPLINE_CURVE ( ( 0.9330127018922194093, 0.9330127018922194093, 1.000000000000000000, 0.8660254037844387076, 1.000000000000000000, 0.8660254037844387076, 1.000000000000000000, 0.9330127018922194093, 0.9330127018922194093 ) ) 
 REPRESENTATION_ITEM ( '' )  );
#15845 = CARTESIAN_POINT ( 'NONE',  ( 4.458734124999998549, 29.02083333469893134, -2.574251347313721627 ) ) ;
#15846 = ORIENTED_EDGE ( 'NONE', *, *, #2774, .T. ) ;
#15847 = CARTESIAN_POINT ( 'NONE',  ( -4.458734124999999437, -82.31249999863440792, 0.000000000000000000 ) ) ;
#15848 = CARTESIAN_POINT ( 'NONE',  ( 4.458734124999998549, -5.729166665301072214, -2.574251347313721627 ) ) ;
#15849 = CARTESIAN_POINT ( 'NONE',  ( -50.01589407740564042, -147.6250000000000284, 0.3983568153799778022 ) ) ;
#15850 = DIRECTION ( 'NONE',  ( 0.000000000000000000, 0.000000000000000000, 1.000000000000000000 ) ) ;
#15851 = CARTESIAN_POINT ( 'NONE',  ( -4.458734124999999437, -72.56249999863439371, 0.000000000000000000 ) ) ;
#15852 = CARTESIAN_POINT ( 'NONE',  ( -5.000000000000000000, -30.95833333060214443, -2.886751345948128211 ) ) ;
#15853 = CARTESIAN_POINT ( 'NONE',  ( -4.458734124999999437, 29.68750000136559208, 0.000000000000000000 ) ) ;
#15854 = CARTESIAN_POINT ( 'NONE',  ( 1.975475456537005874E-15, -3.750000000000001776, 5.000000000000000000 ) ) ;
#15855 = CARTESIAN_POINT ( 'NONE',  ( 2.229367062499998831, 27.35416666803225993, -3.861377020970580887 ) ) ;
#15856 = EDGE_CURVE ( 'NONE', #52220, #14909, #39450, .T. ) ;
#15857 = CARTESIAN_POINT ( 'NONE',  ( 4.458734124999999437, -45.81249999863440081, -5.460374474430324690E-16 ) ) ;
#15858 = CARTESIAN_POINT ( 'NONE',  ( -3.152548672688508926E-16, -33.81249999863440792, -5.148502694627439702 ) ) ;
#15859 = CARTESIAN_POINT ( 'NONE',  ( 9.457646018065525792E-16, 1.687500001365593194, 5.148502694627439702 ) ) ;
#15860 = DIRECTION ( 'NONE',  ( 1.000000000000000000, 0.000000000000000000, 0.000000000000000000 ) ) ;
#15861 = CARTESIAN_POINT ( 'NONE',  ( -5.000000000000000000, 17.91666666666666430, -2.886751345948128211 ) ) ;
#15862 = EDGE_CURVE ( 'NONE', #33371, #30129, #36639, .T. ) ;
#15863 = CARTESIAN_POINT ( 'NONE',  ( 3.535533905932736864, -146.2500000027311842, 3.535533905932738641 ) ) ;
#15864 = DIRECTION ( 'NONE',  ( 0.000000000000000000, 0.000000000000000000, 1.000000000000000000 ) ) ;
#15865 = CARTESIAN_POINT ( 'NONE',  ( -4.458734124999999437, -43.39583333196774362, -2.574251347313719407 ) ) ;
#15866 = CARTESIAN_POINT ( 'NONE',  ( -5.000000000000000000, -71.87499999726880162, 0.000000000000000000 ) ) ;
#15867 = CARTESIAN_POINT ( 'NONE',  ( -59.59170313451811296, -142.7500000013656063, 1.485763867205729394 ) ) ;
#15868 = CARTESIAN_POINT ( 'NONE',  ( 6.123233995736766282E-16, -120.0000000000000000, -5.000000000000000000 ) ) ;
#15869 = EDGE_CURVE ( 'NONE', #51679, #54583, #52249, .T. ) ;
#15870 = CARTESIAN_POINT ( 'NONE',  ( 3.750000000000004441, -6.495190528383289141, 0.000000000000000000 ) ) ;
#15871 = CARTESIAN_POINT ( 'NONE',  ( -4.458734124999999437, -81.64583333196773651, -2.574251347313719407 ) ) ;
#15872 = CARTESIAN_POINT ( 'NONE',  ( -3.152801135295367985, -163.0625000013656063, 3.152801135295367096 ) ) ;
#15873 = DIRECTION ( 'NONE',  ( -0.000000000000000000, 1.000000000000000000, -0.000000000000000000 ) ) ;
#15874 = CARTESIAN_POINT ( 'NONE',  ( 5.000000000000000000, 13.70833333606451987, -2.886751345948130876 ) ) ;
#15875 = CARTESIAN_POINT ( 'NONE',  ( -2.500000000000000444, -27.16666666666666430, -4.330127018922193649 ) ) ;
#15876 = CARTESIAN_POINT ( 'NONE',  ( -8.190561711645485556E-16, -141.6875000013656063, 4.458734124999999437 ) ) ;
#15877 = ORIENTED_EDGE ( 'NONE', *, *, #11497, .T. ) ;
#15878 = CARTESIAN_POINT ( 'NONE',  ( -2.229367062499996610, 20.60416666803225993, 3.861377020970582219 ) ) ;
#15879 = VERTEX_POINT ( 'NONE', #46610 ) ;
#15880 = CARTESIAN_POINT ( 'NONE',  ( -2.229367062500000163, -59.72916666530106511, -3.861377020970580443 ) ) ;
#15881 = CARTESIAN_POINT ( 'NONE',  ( -4.999999999999999112, 21.20833333606451987, 2.886751345948131764 ) ) ;
#15882 = CARTESIAN_POINT ( 'NONE',  ( -49.85088928181150436, -138.6875000027312126, -1.666127454062680480 ) ) ;
#15883 = CARTESIAN_POINT ( 'NONE',  ( 5.000000000000000888, 12.41666666666666607, 2.886751345948126879 ) ) ;
#15884 = CARTESIAN_POINT ( 'NONE',  ( -4.458734124999999437, -51.39583333196773651, -2.574251347313719407 ) ) ;
#15885 = CARTESIAN_POINT ( 'NONE',  ( 4.458734124999999437, -12.81249999863440259, -5.460374474430324690E-16 ) ) ;
#15886 = CARTESIAN_POINT ( 'NONE',  ( 7.922811941611899833, 4.628808333142401032, -8.057670691780701944 ) ) ;
#15887 = DIRECTION ( 'NONE',  ( -0.000000000000000000, 1.000000000000000000, -0.000000000000000000 ) ) ;
#15888 = CARTESIAN_POINT ( 'NONE',  ( -1.339745962155610925, 0.3303418039926660499, 5.000000000000000000 ) ) ;
#15889 = DIRECTION ( 'NONE',  ( 0.000000000000000000, 0.000000000000000000, 1.000000000000000000 ) ) ;
#15890 = CARTESIAN_POINT ( 'NONE',  ( -6.972266317189433020E-16, -66.12499999726881583, -5.000000000000000000 ) ) ;
#15892 = CARTESIAN_POINT ( 'NONE',  ( -4.458734124999999437, -15.64583333196773474, -2.574251347313719407 ) ) ;
#15891 = LINE ( 'NONE', #49340, #15002 ) ;
#15893 = CARTESIAN_POINT ( 'NONE',  ( -4.458734124999999437, -60.31249999863440081, 0.000000000000000000 ) ) ;
#15894 = CARTESIAN_POINT ( 'NONE',  ( -3.152801135295367985, -153.0625000013656063, 3.152801135295367096 ) ) ;
#15895 = CARTESIAN_POINT ( 'NONE',  ( 4.458734125000001214, -64.89583333196773651, 2.574251347313718519 ) ) ;
#15896 = VECTOR ( 'NONE', #35061, 1000.000000000000000 ) ;
#15897 = CARTESIAN_POINT ( 'NONE',  ( 2.499999999999998668, -53.20833333060213732, -4.330127018922193649 ) ) ;
#15898 = VERTEX_POINT ( 'NONE', #2556 ) ;
#15899 = CARTESIAN_POINT ( 'NONE',  ( -2.500000000000000444, 24.95833333606451987, -4.330127018922193649 ) ) ;
#15900 = CARTESIAN_POINT ( 'NONE',  ( -4.458734124999998549, -1.479166665301071770, 2.574251347313722516 ) ) ;
#15901 = ORIENTED_EDGE ( 'NONE', *, *, #48802, .T. ) ;
#15903 = CARTESIAN_POINT ( 'NONE',  ( -1.339745962155613812, -86.20534180126146850, -5.000000000000000000 ) ) ;
#15902 = CARTESIAN_POINT ( 'NONE',  ( 0.000000000000000000, -170.0000000000000000, 0.000000000000000000 ) ) ;
#15904 = CARTESIAN_POINT ( 'NONE',  ( 3.152801135295367541, -157.3125000013656063, -3.152801135295367541 ) ) ;
#15905 = VERTEX_POINT ( 'NONE', #37276 ) ;
#15906 = CARTESIAN_POINT ( 'NONE',  ( -5.000000000000000000, -10.08333333333333393, -2.886751345948128211 ) ) ;
#15907 = CARTESIAN_POINT ( 'NONE',  ( -60.14911071818854538, -129.0625000000000000, 1.666127454062681368 ) ) ;
#15908 = CARTESIAN_POINT ( 'NONE',  ( 3.061616997868383141E-16, -152.7500000000000000, -5.000000000000000000 ) ) ;
#15909 = CARTESIAN_POINT ( 'NONE',  ( -2.229367062499996610, -50.39583333196772941, 3.861377020970582219 ) ) ;
#15910 = VERTEX_POINT ( 'NONE', #56271 ) ;
#15911 = CARTESIAN_POINT ( 'NONE',  ( -5.000000000000000000, -109.8749999972688016, 0.000000000000000000 ) ) ;
#15912 = CARTESIAN_POINT ( 'NONE',  ( -2.229367062500000163, 14.52083333469892779, -3.861377020970580443 ) ) ;
#15913 = CARTESIAN_POINT ( 'NONE',  ( -2.229367062499996610, -90.39583333196773651, 3.861377020970582219 ) ) ;
#15914 = CARTESIAN_POINT ( 'NONE',  ( -52.80376928212989185, -153.8750000013655779, -4.297418129356379346 ) ) ;
#15915 = CARTESIAN_POINT ( 'NONE',  ( -6.972266317189433020E-16, -44.25000000000000000, -5.000000000000000000 ) ) ;
#15916 = CARTESIAN_POINT ( 'NONE',  ( 7.500000000000000000, -4.330127018922199866, -7.422398894150035176 ) ) ;
#15917 = CARTESIAN_POINT ( 'NONE',  ( -2.229367062499996610, -64.14583333196773651, 3.861377020970582219 ) ) ;
#15918 = CARTESIAN_POINT ( 'NONE',  ( -2.499999999999996447, -49.70833333060213732, 4.330127018922195425 ) ) ;
#15919 = CARTESIAN_POINT ( 'NONE',  ( -2.229367062499996610, 10.85416666803225993, 3.861377020970582219 ) ) ;
#15920 =( BOUNDED_CURVE ( )  B_SPLINE_CURVE ( 2, ( #18835, #4367, #40361, #1156, #34908, #20755, #30390, #15925, #5639 ),
 .UNSPECIFIED., .F., .F. ) 
 B_SPLINE_CURVE_WITH_KNOTS ( ( 3, 2, 2, 2, 3 ),
 ( 0.03958333333333333842, 0.04027777777777778040, 0.04166666666666666435, 0.04305555555555555525, 0.04375000000000000416 ),
 .UNSPECIFIED. ) 
 CURVE ( )  GEOMETRIC_REPRESENTATION_ITEM ( )  RATIONAL_B_SPLINE_CURVE ( ( 0.9330127018922192983, 0.9330127018922196314, 1.000000000000000000, 0.8660254037844387076, 1.000000000000000000, 0.8660254037844387076, 1.000000000000000000, 0.9330127018922189652, 0.9330127018922192983 ) ) 
 REPRESENTATION_ITEM ( '' )  );
#15921 = CARTESIAN_POINT ( 'NONE',  ( -5.000000000000000000, 6.999999999999999112, 0.000000000000000000 ) ) ;
#15922 = CARTESIAN_POINT ( 'NONE',  ( -1.339745962155564296, -27.20534180126147916, -5.000000000000028422 ) ) ;
#15923 = CARTESIAN_POINT ( 'NONE',  ( -4.458734124999999437, -54.56249999863440081, 0.000000000000000000 ) ) ;
#15924 = CARTESIAN_POINT ( 'NONE',  ( -4.999999999999999112, -8.791666663935483683, 2.886751345948131764 ) ) ;
#15925 = CARTESIAN_POINT ( 'NONE',  ( -1.339745962155608039, 24.79465819873852439, -5.000000000000004441 ) ) ;
#15926 = DIRECTION ( 'NONE',  ( 0.000000000000000000, 0.000000000000000000, 1.000000000000000000 ) ) ;
#15927 = FACE_OUTER_BOUND ( 'NONE', #36222, .T. ) ;
#15928 = DIRECTION ( 'NONE',  ( -0.000000000000000000, 1.000000000000000000, -0.000000000000000000 ) ) ;
#15929 = CARTESIAN_POINT ( 'NONE',  ( -3.152548672688508926E-16, -18.81249999863440792, -5.148502694627439702 ) ) ;
#15930 = ORIENTED_EDGE ( 'NONE', *, *, #35905, .F. ) ;
#15931 = CARTESIAN_POINT ( 'NONE',  ( 1.339745962155615144, -31.70534180126147916, 4.999999999999999112 ) ) ;
#15932 = CARTESIAN_POINT ( 'NONE',  ( -2.229367062499996610, -102.1458333319677365, 3.861377020970582219 ) ) ;
#15933 = CARTESIAN_POINT ( 'NONE',  ( 3.061616997868383141E-16, -155.8750000027311842, -5.000000000000000000 ) ) ;
#15934 = ORIENTED_EDGE ( 'NONE', *, *, #14250, .T. ) ;
#15935 = CARTESIAN_POINT ( 'NONE',  ( -3.152548672688508926E-16, -98.81249999863440792, -5.148502694627439702 ) ) ;
#15936 = CARTESIAN_POINT ( 'NONE',  ( 4.458734124999998549, -25.72916666530107221, -2.574251347313721627 ) ) ;
#15937 = CARTESIAN_POINT ( 'NONE',  ( 5.000000000000000888, -55.45833333060214443, 2.886751345948126879 ) ) ;
#15938 = CARTESIAN_POINT ( 'NONE',  ( 1.975475456537005874E-15, -62.62499999726880873, 5.000000000000000000 ) ) ;
#15939 = CARTESIAN_POINT ( 'NONE',  ( -56.48576386720575471, -126.7500000013655921, -4.591703134518078322 ) ) ;
#15940 =( BOUNDED_CURVE ( )  B_SPLINE_CURVE ( 2, ( #48265, #39558, #34412, #24148, #38313 ),
 .UNSPECIFIED., .F., .F. ) 
 B_SPLINE_CURVE_WITH_KNOTS ( ( 3, 2, 3 ),
 ( 0.000000000000000000, 0.004166666666666670078, 0.008333333333333340157 ),
 .UNSPECIFIED. ) 
 CURVE ( )  GEOMETRIC_REPRESENTATION_ITEM ( )  RATIONAL_B_SPLINE_CURVE ( ( 1.000000000000000000, 0.9238795325112867385, 1.000000000000000000, 0.9238795325112866275, 1.000000000000000222 ) ) 
 REPRESENTATION_ITEM ( '' )  );
#15941 = CARTESIAN_POINT ( 'NONE',  ( -59.29741812935640155, -144.6250000013656063, -2.196230717870135685 ) ) ;
#15942 = CARTESIAN_POINT ( 'NONE',  ( 2.229367062500001939, -25.97916666530106866, 3.861377020970579999 ) ) ;
#15943 = CARTESIAN_POINT ( 'NONE',  ( -2.229367062500000163, -63.72916666530106511, -3.861377020970580443 ) ) ;
#15944 = DIRECTION ( 'NONE',  ( 0.000000000000000000, 0.000000000000000000, 1.000000000000000000 ) ) ;
#15945 = CARTESIAN_POINT ( 'NONE',  ( 2.229367062500001939, -19.97916666530107221, 3.861377020970579999 ) ) ;
#15946 = DIRECTION ( 'NONE',  ( -0.000000000000000000, 1.000000000000000000, -0.000000000000000000 ) ) ;
#15947 = CARTESIAN_POINT ( 'NONE',  ( -5.000000000000000000, -151.5000000000000284, -6.123233995736766282E-16 ) ) ;
#15948 = CARTESIAN_POINT ( 'NONE',  ( 1.060575238724906964E-15, -9.750000000000001776, 5.773502691896257311 ) ) ;
#15949 = CARTESIAN_POINT ( 'NONE',  ( 3.152801135295367541, -150.3125000013655779, -3.152801135295367541 ) ) ;
#15950 = VERTEX_POINT ( 'NONE', #3193 ) ;
#15951 = CARTESIAN_POINT ( 'NONE',  ( 9.457646018065525792E-16, -46.31249999863440792, 5.148502694627439702 ) ) ;
#15952 = CARTESIAN_POINT ( 'NONE',  ( -9.184850993605147944E-16, -150.2500000000000284, 5.000000000000000000 ) ) ;
#15953 = DIRECTION ( 'NONE',  ( -0.000000000000000000, 1.000000000000000000, -0.000000000000000000 ) ) ;
#15954 = CARTESIAN_POINT ( 'NONE',  ( 4.458734124999999437, -89.81249999863440792, -5.460374474430324690E-16 ) ) ;
#15955 = B_SPLINE_CURVE_WITH_KNOTS ( 'NONE', 3,
 ( #42999, #13730, #9531, #5026, #28522, #24645, #8906, #4091, #62644, #14989 ),
 .UNSPECIFIED., .F., .F.,
 ( 4, 2, 2, 2, 4 ),
 ( 0.000000000000000000, 0.002305503304226491634, 0.004611006608452983269, 0.006916509912679474036, 0.009222013216905963068 ),
 .UNSPECIFIED. ) ;
#15956 = CARTESIAN_POINT ( 'NONE',  ( 4.458734124999998549, 4.270833334698926897, -2.574251347313721627 ) ) ;
#15957 = CARTESIAN_POINT ( 'NONE',  ( -2.071067811865432873, -142.6875000000000284, -5.000000000000041744 ) ) ;
#15958 = CARTESIAN_POINT ( 'NONE',  ( -6.972266317189433020E-16, -95.12499999726880162, -5.000000000000000000 ) ) ;
#15959 = CARTESIAN_POINT ( 'NONE',  ( 0.000000000000000000, -120.0000000000000000, 0.000000000000000000 ) ) ;
#15960 = CARTESIAN_POINT ( 'NONE',  ( 9.457646018065525792E-16, 16.68750000136559564, 5.148502694627439702 ) ) ;
#15961 = CARTESIAN_POINT ( 'NONE',  ( -2.499999999999996447, -75.83333333333334281, 4.330127018922195425 ) ) ;
#15962 = CARTESIAN_POINT ( 'NONE',  ( -2.500000000000000444, 10.95833333606451632, -4.330127018922193649 ) ) ;
#15963 = ORIENTED_EDGE ( 'NONE', *, *, #46410, .F. ) ;
#15964 = ORIENTED_EDGE ( 'NONE', *, *, #37421, .T. ) ;
#15965 = CARTESIAN_POINT ( 'NONE',  ( 6.123233995736766282E-16, -120.0000000000000000, -5.000000000000000000 ) ) ;
#15966 = CARTESIAN_POINT ( 'NONE',  ( -4.458734124999998549, -45.22916666530106511, 2.574251347313722516 ) ) ;
#15967 = CARTESIAN_POINT ( 'NONE',  ( 1.060575238724906964E-15, -38.62499999726881583, 5.773502691896257311 ) ) ;
#15968 = ORIENTED_EDGE ( 'NONE', *, *, #4349, .T. ) ;
#15969 = CARTESIAN_POINT ( 'NONE',  ( -4.458734124999999437, -20.31249999863440081, 0.000000000000000000 ) ) ;
#15970 = ORIENTED_EDGE ( 'NONE', *, *, #1131, .T. ) ;
#15971 = CARTESIAN_POINT ( 'NONE',  ( -5.000000000000000000, -83.08333333333332860, -2.886751345948128211 ) ) ;
#15972 = CARTESIAN_POINT ( 'NONE',  ( -4.458734124999999437, -168.9375000013656063, -5.460374474430324690E-16 ) ) ;
#15973 = CARTESIAN_POINT ( 'NONE',  ( 5.000000000000000000, -86.29166666393547303, -2.886751345948129988 ) ) ;
#15975 = EDGE_LOOP ( 'NONE', ( #22319, #15814, #18805, #19760 ) ) ;
#15974 = CARTESIAN_POINT ( 'NONE',  ( 1.339745962155565406, -20.58034179853029144, 5.000000000000028422 ) ) ;
#15976 = CARTESIAN_POINT ( 'NONE',  ( -50.01589407740564042, -139.6250000000000284, 0.3983568153799778022 ) ) ;
#15977 = CARTESIAN_POINT ( 'NONE',  ( -4.458734124999999437, -31.56249999863440436, 0.000000000000000000 ) ) ;
#15978 = CARTESIAN_POINT ( 'NONE',  ( -1.339745962155610925, -49.79465819873851729, 5.000000000000000000 ) ) ;
#15979 = VERTEX_POINT ( 'NONE', #22493 ) ;
#15980 = AXIS2_PLACEMENT_3D ( 'NONE', #33798, #53106, #3910 ) ;
#15981 = APPLICATION_PROTOCOL_DEFINITION ( 'draft international standard', 'automotive_design', 1998, #51998 ) ;
#15982 = CARTESIAN_POINT ( 'NONE',  ( 9.457646018065525792E-16, -75.06249999863439371, 5.148502694627439702 ) ) ;
#15983 = CARTESIAN_POINT ( 'NONE',  ( 4.458734124999999437, 27.18750000136559564, -5.460374474430324690E-16 ) ) ;
#15984 = CARTESIAN_POINT ( 'NONE',  ( -6.972266317189433020E-16, 20.74999999999999645, -5.000000000000000000 ) ) ;
#15985 = ORIENTED_EDGE ( 'NONE', *, *, #44872, .F. ) ;
#15986 = DIRECTION ( 'NONE',  ( -0.000000000000000000, 1.000000000000000000, -0.000000000000000000 ) ) ;
#15987 = CARTESIAN_POINT ( 'NONE',  ( -53.51423613279429503, -143.5000000013656063, 4.591703134518083651 ) ) ;
#15988 = CARTESIAN_POINT ( 'NONE',  ( -4.458734124999998549, -76.47916666530105090, 2.574251347313722516 ) ) ;
#15989 = CARTESIAN_POINT ( 'NONE',  ( -49.85088928181150436, -134.6875000027312126, -1.666127454062680702 ) ) ;
#15990 = CARTESIAN_POINT ( 'NONE',  ( -3.152548672688508926E-16, -44.56249999863440081, -5.148502694627439702 ) ) ;
#15991 = CARTESIAN_POINT ( 'NONE',  ( -3.152801135295367096, -141.3125000013655779, -3.152801135295367541 ) ) ;
#15992 =( BOUNDED_CURVE ( )  B_SPLINE_CURVE ( 2, ( #19240, #38855, #58798, #54294, #48826, #34675, #14729, #14415, #59450 ),
 .UNSPECIFIED., .F., .F. ) 
 B_SPLINE_CURVE_WITH_KNOTS ( ( 3, 2, 2, 2, 3 ),
 ( 0.3696428571428571619, 0.3702380952380952550, 0.3714285714285714413, 0.3726190476190476275, 0.3732142857142857206 ),
 .UNSPECIFIED. ) 
 CURVE ( )  GEOMETRIC_REPRESENTATION_ITEM ( )  RATIONAL_B_SPLINE_CURVE ( ( 0.9330127018922194093, 0.9330127018922194093, 1.000000000000000000, 0.8660254037844387076, 1.000000000000000000, 0.8660254037844387076, 1.000000000000000000, 0.9330127018922194093, 0.9330127018922194093 ) ) 
 REPRESENTATION_ITEM ( '' )  );
#15993 = CARTESIAN_POINT ( 'NONE',  ( 2.500000000000002220, -84.54166666393547303, 4.330127018922192761 ) ) ;
#15994 = CARTESIAN_POINT ( 'NONE',  ( 4.458734124999998549, -48.72916666530106511, -2.574251347313721627 ) ) ;
#15995 = CARTESIAN_POINT ( 'NONE',  ( -2.229367062499996610, -43.14583333196773651, 3.861377020970582219 ) ) ;
#15996 = CARTESIAN_POINT ( 'NONE',  ( -4.999999999999998224, -70.91666666666667140, 2.886751345948131764 ) ) ;
#15997 = CARTESIAN_POINT ( 'NONE',  ( -4.458734124999999437, -18.39583333196774007, -2.574251347313719407 ) ) ;
#15998 = CARTESIAN_POINT ( 'NONE',  ( -5.000000000000000000, -103.0000000000000142, 0.000000000000000000 ) ) ;
#15999 = CARTESIAN_POINT ( 'NONE',  ( 4.458734124999999437, -139.6875000013656063, 0.000000000000000000 ) ) ;
#16000 = CARTESIAN_POINT ( 'NONE',  ( 4.458734124999999437, -36.06249999863440792, -5.460374474430324690E-16 ) ) ;
#16001 = CARTESIAN_POINT ( 'NONE',  ( -5.000000000000000000, 6.041666669397850242, -2.886751345948128211 ) ) ;
#16002 = DIRECTION ( 'NONE',  ( -0.000000000000000000, 1.000000000000000000, -0.000000000000000000 ) ) ;
#16003 = CARTESIAN_POINT ( 'NONE',  ( -50.40829686548195099, -131.0000000013656063, -1.485763867205728284 ) ) ;
#16004 = CARTESIAN_POINT ( 'NONE',  ( -3.152548672688508926E-16, -75.81249999863440792, -5.148502694627439702 ) ) ;
#16005 = CARTESIAN_POINT ( 'NONE',  ( -5.000000000000000000, -166.5000000000000000, -6.123233995736766282E-16 ) ) ;
#16006 = CARTESIAN_POINT ( 'NONE',  ( -7.640563834021360018E-16, -9.147862274876560562, -8.047472243342937759 ) ) ;
#16007 = CARTESIAN_POINT ( 'NONE',  ( -4.458734124999999437, -1.562499998634406140, 0.000000000000000000 ) ) ;
#16008 = ORIENTED_EDGE ( 'NONE', *, *, #49514, .F. ) ;
#16009 = CARTESIAN_POINT ( 'NONE',  ( 1.339745962155615144, -30.70534180126147916, 4.999999999999999112 ) ) ;
#16010 = CARTESIAN_POINT ( 'NONE',  ( 5.000000000000000000, -57.41666666666667140, -2.886751345948130876 ) ) ;
#16012 = CARTESIAN_POINT ( 'NONE',  ( 2.229367062500001939, -33.97916666530107221, 3.861377020970579999 ) ) ;
#16011 = CARTESIAN_POINT ( 'NONE',  ( -4.458734124999999437, -88.31249999863439371, 0.000000000000000000 ) ) ;
#16013 = DIRECTION ( 'NONE',  ( 0.000000000000000000, 0.000000000000000000, 1.000000000000000000 ) ) ;
#16014 = CARTESIAN_POINT ( 'NONE',  ( 4.458734124999998549, -81.97916666530106511, -2.574251347313721627 ) ) ;
#16015 = CARTESIAN_POINT ( 'NONE',  ( 2.229367062500001939, 19.77083333469892779, 3.861377020970579999 ) ) ;
#16016 = CARTESIAN_POINT ( 'NONE',  ( -75.00000000000002842, 15.00000000000000000, -5.000000000000000000 ) ) ;
#16017 = CARTESIAN_POINT ( 'NONE',  ( -59.44456063193725015, -136.5625000013656063, -0.3552334253322034230 ) ) ;
#16018 = CARTESIAN_POINT ( 'NONE',  ( -2.229367062500000163, -7.479166665301073991, -3.861377020970580443 ) ) ;
#16019 = CARTESIAN_POINT ( 'NONE',  ( -4.458734124999999437, 20.43750000136559208, 0.000000000000000000 ) ) ;
#16020 = CARTESIAN_POINT ( 'NONE',  ( 2.229367062500001939, -49.22916666530107221, 3.861377020970579999 ) ) ;
#16021 = CARTESIAN_POINT ( 'NONE',  ( 1.339745962155612702, -105.2946581987385173, -5.000000000000000000 ) ) ;
#16022 = CARTESIAN_POINT ( 'NONE',  ( 4.458734124999999437, -82.81249999863440792, -5.460374474430324690E-16 ) ) ;
#16023 = CARTESIAN_POINT ( 'NONE',  ( -4.458734124999997661, -3.229166665301069550, 2.574251347313722516 ) ) ;
#16024 = CARTESIAN_POINT ( 'NONE',  ( -1.339745962155610925, -30.79465819873851373, 5.000000000000000000 ) ) ;
#16025 = VERTEX_POINT ( 'NONE', #52072 ) ;
#16026 = CARTESIAN_POINT ( 'NONE',  ( -4.458734124999999437, -32.56249999863440792, 0.000000000000000000 ) ) ;
#16027 = CARTESIAN_POINT ( 'NONE',  ( -52.10840900171896806, -130.4375000013656063, 3.393966926194110556 ) ) ;
#16028 = CARTESIAN_POINT ( 'NONE',  ( -2.229367062500000163, -74.47916666530106511, -3.861377020970580443 ) ) ;
#16029 = CARTESIAN_POINT ( 'NONE',  ( -2.499999999999996447, -108.7083333306021444, 4.330127018922195425 ) ) ;
#16030 = VECTOR ( 'NONE', #62769, 1000.000000000000000 ) ;
#16031 = CARTESIAN_POINT ( 'NONE',  ( -3.152548672688508926E-16, 20.43750000136559208, -5.148502694627439702 ) ) ;
#16032 = CYLINDRICAL_SURFACE ( 'NONE', #16255, 5.000000000000000000 ) ;
#16033 = CARTESIAN_POINT ( 'NONE',  ( 9.457646018065525792E-16, -77.31249999863440792, 5.148502694627439702 ) ) ;
#16034 = CARTESIAN_POINT ( 'NONE',  ( -5.000000000000000000, -59.08333333333334281, -2.886751345948128211 ) ) ;
#16035 = CARTESIAN_POINT ( 'NONE',  ( -52.53715891517739323, -151.4375000000000284, -4.819101127000233298 ) ) ;
#16036 = CARTESIAN_POINT ( 'NONE',  ( -2.499999999999996447, 25.29166666939785202, 4.330127018922195425 ) ) ;
#16037 = ORIENTED_EDGE ( 'NONE', *, *, #8040, .F. ) ;
#16038 = CARTESIAN_POINT ( 'NONE',  ( 0.000000000000000000, -170.0000000000000000, 5.000000000000000000 ) ) ;
#16039 = CARTESIAN_POINT ( 'NONE',  ( -9.184850993605147944E-16, -158.3750000027311842, 5.000000000000000000 ) ) ;
#16040 =( BOUNDED_CURVE ( )  B_SPLINE_CURVE ( 2, ( #52867, #32296, #18133, #23286, #37139, #37446, #51616, #57077, #27161 ),
 .UNSPECIFIED., .F., .F. ) 
 B_SPLINE_CURVE_WITH_KNOTS ( ( 3, 2, 2, 2, 3 ),
 ( 0.9562500000000000444, 0.9569444444444444864, 0.9583333333333333703, 0.9597222222222222543, 0.9604166666666666963 ),
 .UNSPECIFIED. ) 
 CURVE ( )  GEOMETRIC_REPRESENTATION_ITEM ( )  RATIONAL_B_SPLINE_CURVE ( ( 0.9330127018922194093, 0.9330127018922194093, 1.000000000000000000, 0.8660254037844387076, 1.000000000000000000, 0.8660254037844387076, 1.000000000000000000, 0.9330127018922194093, 0.9330127018922194093 ) ) 
 REPRESENTATION_ITEM ( '' )  );
#16041 = CARTESIAN_POINT ( 'NONE',  ( -2.500000000000000444, -22.16666666666666785, -4.330127018922193649 ) ) ;
#16042 = CARTESIAN_POINT ( 'NONE',  ( 4.458734124999999437, -25.81249999863440792, -5.460374474430324690E-16 ) ) ;
#16043 = EDGE_CURVE ( 'NONE', #22858, #13416, #52617, .T. ) ;
#16044 = CARTESIAN_POINT ( 'NONE',  ( 9.457646018065525792E-16, -89.06249999863439371, 5.148502694627439702 ) ) ;
#16045 = CARTESIAN_POINT ( 'NONE',  ( 1.060575238724906964E-15, -24.62499999726881228, 5.773502691896257311 ) ) ;
#16047 = VERTEX_POINT ( 'NONE', #22170 ) ;
#16046 = CARTESIAN_POINT ( 'NONE',  ( -4.458734124999999437, -53.31249999863439371, 0.000000000000000000 ) ) ;
#16048 = LINE ( 'NONE', #46275, #29449 ) ;
#16049 = CARTESIAN_POINT ( 'NONE',  ( 5.000000000000000000, -74.29166666393547303, -2.886751345948130876 ) ) ;
#16051 = VERTEX_POINT ( 'NONE', #17340 ) ;
#16050 = CARTESIAN_POINT ( 'NONE',  ( -2.229367062500000163, -2.729166665301069550, -3.861377020970580443 ) ) ;
#16052 = CARTESIAN_POINT ( 'NONE',  ( -57.19623071787016499, -150.3750000013656063, 4.297418129356382899 ) ) ;
#16053 = CARTESIAN_POINT ( 'NONE',  ( 2.500000000000002220, -68.66666666666667140, 4.330127018922192761 ) ) ;
#16054 = CARTESIAN_POINT ( 'NONE',  ( -4.458734125000001214, -151.1250000013655779, 1.846868145590734089 ) ) ;
#16055 = CARTESIAN_POINT ( 'NONE',  ( 4.458734125000001214, -49.14583333196772941, 2.574251347313718519 ) ) ;
#16056 = DIRECTION ( 'NONE',  ( -0.000000000000000000, 1.000000000000000000, -0.000000000000000000 ) ) ;
#16057 = CARTESIAN_POINT ( 'NONE',  ( -5.000000000000000888, -158.4375000000000568, 2.071067811865474617 ) ) ;
#16058 = DIRECTION ( 'NONE',  ( -0.000000000000000000, 1.000000000000000000, -0.000000000000000000 ) ) ;
#16059 = CARTESIAN_POINT ( 'NONE',  ( -52.53715891517739323, -153.4375000000000284, -4.819101127000233298 ) ) ;
#16060 = CARTESIAN_POINT ( 'NONE',  ( 4.458734125000001214, -11.14583333196774007, 2.574251347313718519 ) ) ;
#16061 = CARTESIAN_POINT ( 'NONE',  ( -4.458734124999998549, -53.47916666530106511, 2.574251347313722516 ) ) ;
#16062 = ADVANCED_FACE ( 'NONE', ( #21539 ), #41767, .T. ) ;
#16063 = CARTESIAN_POINT ( 'NONE',  ( 1.339745962155615144, 10.29465819873852084, 4.999999999999999112 ) ) ;
#16064 = CARTESIAN_POINT ( 'NONE',  ( 1.846868145590735200, -144.2500000013656063, -4.458734125000000326 ) ) ;
#16065 = EDGE_CURVE ( 'NONE', #34014, #62883, #42089, .T. ) ;
#16066 = CARTESIAN_POINT ( 'NONE',  ( -3.152548672688508926E-16, -96.81249999863440792, -5.148502694627439702 ) ) ;
#16067 = CARTESIAN_POINT ( 'NONE',  ( -2.500000000000000444, -107.1666666666666572, -4.330127018922193649 ) ) ;
#16068 = ORIENTED_EDGE ( 'NONE', *, *, #52213, .T. ) ;
#16069 = CARTESIAN_POINT ( 'NONE',  ( 1.339745962155612702, -19.16965819600733312, -5.000000000000000000 ) ) ;
#16070 = CARTESIAN_POINT ( 'NONE',  ( 2.229367062500001939, 27.77083333469892779, 3.861377020970579999 ) ) ;
#16071 = CARTESIAN_POINT ( 'NONE',  ( -59.98410592259440222, -148.2500000027312126, -0.3983568153799752487 ) ) ;
#16072 = AXIS2_PLACEMENT_3D ( 'NONE', #55199, #16276, #1496 ) ;
#16073 = CARTESIAN_POINT ( 'NONE',  ( 1.975475456537005874E-15, 14.25000000000000000, 5.000000000000000000 ) ) ;
#16074 = ORIENTED_EDGE ( 'NONE', *, *, #33852, .T. ) ;
#16075 = EDGE_CURVE ( 'NONE', #51351, #20487, #8013, .T. ) ;
#16076 = CARTESIAN_POINT ( 'NONE',  ( 4.458734125000001214, -0.8958333319677401763, 2.574251347313718519 ) ) ;
#16077 = VECTOR ( 'NONE', #27865, 1000.000000000000000 ) ;
#16078 = CARTESIAN_POINT ( 'NONE',  ( 5.000000000000000000, 6.583333333333333037, -2.886751345948130876 ) ) ;
#16079 = CARTESIAN_POINT ( 'NONE',  ( -2.229367062500000163, -16.72916666530107577, -3.861377020970580443 ) ) ;
#16080 = CARTESIAN_POINT ( 'NONE',  ( -55.00000000000001421, -135.0000000000000284, 8.082903768654762899 ) ) ;
#16081 = CARTESIAN_POINT ( 'NONE',  ( -3.152548672688508926E-16, -7.562499998634404363, -5.148502694627439702 ) ) ;
#16082 = CARTESIAN_POINT ( 'NONE',  ( -6.972266317189433020E-16, -40.24999999999999289, -5.000000000000000000 ) ) ;
#16083 = CARTESIAN_POINT ( 'NONE',  ( -3.152801135295367096, -150.0625000013655779, -3.152801135295367541 ) ) ;
#16084 = CARTESIAN_POINT ( 'NONE',  ( 2.229367062500001939, 17.77083333469892779, 3.861377020970579999 ) ) ;
#16085 = ORIENTED_EDGE ( 'NONE', *, *, #25634, .F. ) ;
#16086 = CARTESIAN_POINT ( 'NONE',  ( -9.184850993605147944E-16, -148.2500000000000284, 5.000000000000000000 ) ) ;
#16087 = CARTESIAN_POINT ( 'NONE',  ( 1.975475456537005874E-15, -12.74999999999999822, 5.000000000000000000 ) ) ;
#16088 = CARTESIAN_POINT ( 'NONE',  ( -4.458734124999999437, -19.31249999863440081, 0.000000000000000000 ) ) ;
#16089 = CARTESIAN_POINT ( 'NONE',  ( -54.60164318462004474, -143.3750000000000284, -4.984105922594373794 ) ) ;
#16090 = CARTESIAN_POINT ( 'NONE',  ( -1.339745962155613812, -6.205341801261478274, -5.000000000000000000 ) ) ;
#16091 = CARTESIAN_POINT ( 'NONE',  ( -50.55543936806279248, -148.0625000013656063, 0.3552334253322060320 ) ) ;
#16092 = EDGE_CURVE ( 'NONE', #328, #1738, #2117, .T. ) ;
#16093 = CARTESIAN_POINT ( 'NONE',  ( 2.499999999999998668, -46.20833333060214443, -4.330127018922193649 ) ) ;
#16094 = LINE ( 'NONE', #54700, #40170 ) ;
#16095 = CARTESIAN_POINT ( 'NONE',  ( 2.229367062499998831, 10.35416666803225993, -3.861377020970580887 ) ) ;
#16096 = CYLINDRICAL_SURFACE ( 'NONE', #31446, 5.000000000000000000 ) ;
#16097 = DIRECTION ( 'NONE',  ( 0.000000000000000000, 0.000000000000000000, 1.000000000000000000 ) ) ;
#16098 = CARTESIAN_POINT ( 'NONE',  ( -4.458734124999997661, 14.77083333469892779, 2.574251347313722516 ) ) ;
#16099 = CARTESIAN_POINT ( 'NONE',  ( 4.458734124999999437, -69.81249999863439371, -5.460374474430324690E-16 ) ) ;
#16100 = CARTESIAN_POINT ( 'NONE',  ( -4.458734124999999437, -16.64583333196773651, -2.574251347313719407 ) ) ;
#16101 = CARTESIAN_POINT ( 'NONE',  ( -3.535250795749689387E-16, 3.750000000000000000, -5.773502691896257311 ) ) ;
#16102 = CARTESIAN_POINT ( 'NONE',  ( -1.846868145590737420, -163.7500000013655779, 4.458734124999999437 ) ) ;
#16103 = CARTESIAN_POINT ( 'NONE',  ( 7.204675194429079505E-15, 25.87500000273118062, -5.000000000000000000 ) ) ;
#16104 = CARTESIAN_POINT ( 'NONE',  ( 4.458734124999998549, -60.72916666530106511, -2.574251347313721627 ) ) ;
#16105 = CARTESIAN_POINT ( 'NONE',  ( -5.000000000000000000, -93.95833333060213022, -2.886751345948128211 ) ) ;
#16106 = CARTESIAN_POINT ( 'NONE',  ( 2.500000000000002220, -38.66666666666667140, 4.330127018922192761 ) ) ;
#16107 = CARTESIAN_POINT ( 'NONE',  ( -2.499999999999996447, -69.83333333333332860, 4.330127018922195425 ) ) ;
#16108 = CARTESIAN_POINT ( 'NONE',  ( -59.98410592259440222, -152.2500000027312410, -0.3983568153799752487 ) ) ;
#16109 = CARTESIAN_POINT ( 'NONE',  ( -2.229367062499996610, -36.14583333196773651, 3.861377020970582219 ) ) ;
#16110 = CARTESIAN_POINT ( 'NONE',  ( 5.000000000000000000, -51.37499999726881583, -6.123233995736766282E-16 ) ) ;
#16111 = CARTESIAN_POINT ( 'NONE',  ( -3.535250795749689387E-16, -45.25000000000000000, -5.773502691896257311 ) ) ;
#16112 = ORIENTED_EDGE ( 'NONE', *, *, #35304, .T. ) ;
#16113 = CARTESIAN_POINT ( 'NONE',  ( 2.229367062499998831, -108.6458333319677365, -3.861377020970580887 ) ) ;
#16114 = CARTESIAN_POINT ( 'NONE',  ( 2.229367062499998831, -2.895833331967738289, -3.861377020970580887 ) ) ;
#16115 = AXIS2_PLACEMENT_3D ( 'NONE', #22416, #41062, #57152 ) ;
#16116 = CARTESIAN_POINT ( 'NONE',  ( 1.975475456537005874E-15, -30.62499999726881228, 5.000000000000000000 ) ) ;
#16117 = CARTESIAN_POINT ( 'NONE',  ( -3.535250795749689387E-16, -3.250000000000003109, -5.773502691896257311 ) ) ;
#16118 = EDGE_CURVE ( 'NONE', #29717, #29222, #8660, .T. ) ;
#16119 = CARTESIAN_POINT ( 'NONE',  ( 2.229367062499998831, -70.64583333196773651, -3.861377020970580887 ) ) ;
#16120 = AXIS2_PLACEMENT_3D ( 'NONE', #33944, #43583, #54194 ) ;
#16121 =( BOUNDED_CURVE ( )  B_SPLINE_CURVE ( 2, ( #14471, #53715, #28009, #59183, #10290, #45022, #59834, #1310, #49209 ),
 .UNSPECIFIED., .F., .F. ) 
 B_SPLINE_CURVE_WITH_KNOTS ( ( 3, 2, 2, 2, 3 ),
 ( 0.7946428571428570953, 0.7952380952380951884, 0.7964285714285713746, 0.7976190476190476719, 0.7982142857142857650 ),
 .UNSPECIFIED. ) 
 CURVE ( )  GEOMETRIC_REPRESENTATION_ITEM ( )  RATIONAL_B_SPLINE_CURVE ( ( 0.9330127018922194093, 0.9330127018922194093, 1.000000000000000000, 0.8660254037844387076, 1.000000000000000000, 0.8660254037844387076, 1.000000000000000000, 0.9330127018922194093, 0.9330127018922194093 ) ) 
 REPRESENTATION_ITEM ( '' )  );
#16122 = CARTESIAN_POINT ( 'NONE',  ( -50.18089887299978358, -147.8125000027312126, 2.462841084822545934 ) ) ;
#16123 = EDGE_CURVE ( 'NONE', #11139, #53594, #54302, .T. ) ;
#16124 = EDGE_CURVE ( 'NONE', #49284, #52288, #23124, .T. ) ;
#16125 = CARTESIAN_POINT ( 'NONE',  ( -2.499999999999996447, -6.708333330602149758, 4.330127018922195425 ) ) ;
#16127 = EDGE_LOOP ( 'NONE', ( #52588, #45230, #49890, #48221 ) ) ;
#16126 = CARTESIAN_POINT ( 'NONE',  ( -4.458734124999998549, -38.22916666530107932, 2.574251347313722516 ) ) ;
#16128 = LINE ( 'NONE', #55051, #10130 ) ;
#16129 = CARTESIAN_POINT ( 'NONE',  ( -4.999999999999998224, 28.20833333606451987, 2.886751345948131764 ) ) ;
#16131 = EDGE_LOOP ( 'NONE', ( #60699, #36025, #56986, #60542 ) ) ;
#16130 = CARTESIAN_POINT ( 'NONE',  ( 4.458734125000001214, 12.85416666803226171, 2.574251347313718519 ) ) ;
#16132 = CARTESIAN_POINT ( 'NONE',  ( 2.500000000000002220, -101.5416666639354588, 4.330127018922192761 ) ) ;
#16133 = CARTESIAN_POINT ( 'NONE',  ( 2.499999999999998668, -48.33333333333332860, -4.330127018922193649 ) ) ;
#16134 = CARTESIAN_POINT ( 'NONE',  ( 4.458734124999999437, -33.06249999863440792, -5.460374474430324690E-16 ) ) ;
#16135 = CARTESIAN_POINT ( 'NONE',  ( -4.999999999999998224, 14.20833333606451987, 2.886751345948131764 ) ) ;
#16136 = CARTESIAN_POINT ( 'NONE',  ( 4.458734124999999437, -73.81249999863440792, -5.460374474430324690E-16 ) ) ;
#16137 = CARTESIAN_POINT ( 'NONE',  ( 4.458734124999999437, -139.6875000013656063, 0.000000000000000000 ) ) ;
#16138 = CARTESIAN_POINT ( 'NONE',  ( -4.458734124999999437, -83.39583333196772230, -2.574251347313719407 ) ) ;
#16139 = CARTESIAN_POINT ( 'NONE',  ( -59.44456063193725015, -134.8125000013656063, -0.3552334253322034230 ) ) ;
#16140 = CARTESIAN_POINT ( 'NONE',  ( -2.229367062500000163, -37.72916666530107221, -3.861377020970580443 ) ) ;
#16141 = ORIENTED_EDGE ( 'NONE', *, *, #26357, .F. ) ;
#16143 = EDGE_CURVE ( 'NONE', #8862, #10824, #21060, .T. ) ;
#16142 = ORIENTED_EDGE ( 'NONE', *, *, #41855, .F. ) ;
#16144 = CARTESIAN_POINT ( 'NONE',  ( 2.229367062499998831, -79.89583333196773651, -3.861377020970580887 ) ) ;
#16145 = ORIENTED_EDGE ( 'NONE', *, *, #9091, .T. ) ;
#16146 = FACE_OUTER_BOUND ( 'NONE', #62197, .T. ) ;
#16147 = CARTESIAN_POINT ( 'NONE',  ( -5.000000000000000000, -75.87499999726880162, 0.000000000000000000 ) ) ;
#16148 = CARTESIAN_POINT ( 'NONE',  ( 4.458734125000001214, -65.14583333196773651, 2.574251347313718519 ) ) ;
#16149 = CARTESIAN_POINT ( 'NONE',  ( 4.458734124999999437, -4.062499998634408804, -5.460374474430324690E-16 ) ) ;
#16150 = ORIENTED_EDGE ( 'NONE', *, *, #32699, .T. ) ;
#16151 = CARTESIAN_POINT ( 'NONE',  ( -1.339745962155613812, -85.20534180126148271, -5.000000000000000000 ) ) ;
#16152 = CARTESIAN_POINT ( 'NONE',  ( -4.999999999999998224, 3.208333336064520758, 2.886751345948131764 ) ) ;
#16153 = ORIENTED_EDGE ( 'NONE', *, *, #51519, .F. ) ;
#16154 = CARTESIAN_POINT ( 'NONE',  ( 2.499999999999998668, -27.33333333333333570, -4.330127018922193649 ) ) ;
#16155 = CARTESIAN_POINT ( 'NONE',  ( 2.229367062500001939, 9.020833334698927786, 3.861377020970579999 ) ) ;
#16156 = CARTESIAN_POINT ( 'NONE',  ( -6.972266317189433020E-16, -76.24999999999998579, -5.000000000000000000 ) ) ;
#16157 = CARTESIAN_POINT ( 'NONE',  ( 3.152801135295367541, -159.3125000013656063, -3.152801135295367541 ) ) ;
#16158 = CARTESIAN_POINT ( 'NONE',  ( 2.499999999999998668, -75.20833333060214443, -4.330127018922193649 ) ) ;
#16159 = ORIENTED_EDGE ( 'NONE', *, *, #33355, .F. ) ;
#16160 = CARTESIAN_POINT ( 'NONE',  ( -2.229367062500000163, -82.47916666530106511, -3.861377020970580443 ) ) ;
#16161 = DIRECTION ( 'NONE',  ( 0.000000000000000000, 0.000000000000000000, 1.000000000000000000 ) ) ;
#16162 = CARTESIAN_POINT ( 'NONE',  ( -4.458734124999998549, -2.229166665301068662, 2.574251347313722516 ) ) ;
#16163 = VECTOR ( 'NONE', #41180, 1000.000000000000000 ) ;
#16164 = CARTESIAN_POINT ( 'NONE',  ( -54.60164318462004474, -147.3750000000000284, -4.984105922594373794 ) ) ;
#16165 = DIRECTION ( 'NONE',  ( -0.000000000000000000, 1.000000000000000000, -0.000000000000000000 ) ) ;
#16166 = CARTESIAN_POINT ( 'NONE',  ( -3.152548672688508926E-16, -72.81249999863439371, -5.148502694627439702 ) ) ;
#16167 = VECTOR ( 'NONE', #5312, 1000.000000000000000 ) ;
#16168 = CARTESIAN_POINT ( 'NONE',  ( -3.535250795749689387E-16, -32.12499999726880873, -5.773502691896257311 ) ) ;
#16169 = CARTESIAN_POINT ( 'NONE',  ( 5.000000000000000000, 12.62500000273118417, -6.123233995736766282E-16 ) ) ;
#16170 = CARTESIAN_POINT ( 'NONE',  ( -4.999999999999998224, -0.7916666639354794643, 2.886751345948131764 ) ) ;
#16171 =( BOUNDED_CURVE ( )  B_SPLINE_CURVE ( 2, ( #50466, #6405, #40794, #51642, #7576, #52585, #48058, #42917, #56472 ),
 .UNSPECIFIED., .F., .F. ) 
 B_SPLINE_CURVE_WITH_KNOTS ( ( 3, 2, 2, 2, 3 ),
 ( 0.5250000000000004663, 0.5291666666666671182, 0.5333333333333338810, 0.5375000000000005329, 0.5416666666666671848 ),
 .UNSPECIFIED. ) 
 CURVE ( )  GEOMETRIC_REPRESENTATION_ITEM ( )  RATIONAL_B_SPLINE_CURVE ( ( 0.9999999999999918954, 0.9238795325112948431, 1.000000000000000000, 0.9238795325112867385, 1.000000000000000000, 0.9238795325112867385, 1.000000000000000000, 0.9238795325112766355, 1.000000000000010214 ) ) 
 REPRESENTATION_ITEM ( '' )  );
#16172 = CARTESIAN_POINT ( 'NONE',  ( 1.339745962155615144, -82.58034179853028434, 4.999999999999999112 ) ) ;
#16173 = CARTESIAN_POINT ( 'NONE',  ( -2.229367062500000163, -52.47916666530107221, -3.861377020970580443 ) ) ;
#16174 = CARTESIAN_POINT ( 'NONE',  ( 4.458734124999998549, -33.97916666530107221, -2.574251347313721627 ) ) ;
#16175 = CARTESIAN_POINT ( 'NONE',  ( 2.229367062500001939, -0.2291666653010705768, 3.861377020970579999 ) ) ;
#16176 = DIRECTION ( 'NONE',  ( -0.000000000000000000, 1.000000000000000000, -0.000000000000000000 ) ) ;
#16177 = CARTESIAN_POINT ( 'NONE',  ( 1.060575238724906964E-15, 19.25000000000000000, 5.773502691896257311 ) ) ;
#16178 = CARTESIAN_POINT ( 'NONE',  ( 5.000000000000000000, -144.1875000027312126, 2.071067811865478614 ) ) ;
#16179 = CARTESIAN_POINT ( 'NONE',  ( 1.339745962155612702, -26.16965819600733312, -5.000000000000000000 ) ) ;
#16180 = CARTESIAN_POINT ( 'NONE',  ( 9.457646018065525792E-16, -42.06249999863440081, 5.148502694627439702 ) ) ;
#16181 = CARTESIAN_POINT ( 'NONE',  ( 2.500000000000002220, -80.54166666393547303, 4.330127018922192761 ) ) ;
#16182 = CARTESIAN_POINT ( 'NONE',  ( -55.35523342533222291, -139.5625000013656063, 4.444560631937231499 ) ) ;
#16183 = DIRECTION ( 'NONE',  ( -0.000000000000000000, 1.000000000000000000, -0.000000000000000000 ) ) ;
#16184 = CARTESIAN_POINT ( 'NONE',  ( 3.061616997868383141E-16, -140.8750000027312126, -5.000000000000000000 ) ) ;
#16185 = CARTESIAN_POINT ( 'NONE',  ( 4.458734125000000326, -80.14583333196773651, 2.574251347313718519 ) ) ;
#16186 = CARTESIAN_POINT ( 'NONE',  ( 4.458734124999997661, -162.7500000013655779, 1.846868145590737864 ) ) ;
#16187 = CARTESIAN_POINT ( 'NONE',  ( -5.000000000000000888, -159.5625000027312126, 2.071067811865474617 ) ) ;
#16188 = CARTESIAN_POINT ( 'NONE',  ( -4.999999999999999112, -25.91666666666666430, 2.886751345948131764 ) ) ;
#16189 = CARTESIAN_POINT ( 'NONE',  ( -4.999999999999998224, -56.91666666666667140, 2.886751345948131764 ) ) ;
#16190 = ORIENTED_EDGE ( 'NONE', *, *, #34705, .T. ) ;
#16191 = CARTESIAN_POINT ( 'NONE',  ( -2.229367062499996610, 24.60416666803225993, 3.861377020970582219 ) ) ;
#16192 = ORIENTED_EDGE ( 'NONE', *, *, #38989, .F. ) ;
#16193 = CARTESIAN_POINT ( 'NONE',  ( 5.000000000000000000, 20.62500000273118772, -6.123233995736766282E-16 ) ) ;
#16194 = CARTESIAN_POINT ( 'NONE',  ( -1.339745962155613812, -3.080341798530293218, -5.000000000000000000 ) ) ;
#16195 = CARTESIAN_POINT ( 'NONE',  ( 2.499999999999998668, 12.66666666666666607, -4.330127018922193649 ) ) ;
#16196 = CARTESIAN_POINT ( 'NONE',  ( 4.458734124999998549, -48.72916666530106511, -2.574251347313721627 ) ) ;
#16197 = CARTESIAN_POINT ( 'NONE',  ( 4.458734124999998549, -12.72916666530107044, -2.574251347313721627 ) ) ;
#16198 = LINE ( 'NONE', #60280, #14359 ) ;
#16199 = EDGE_CURVE ( 'NONE', #38064, #5879, #53546, .T. ) ;
#16200 = EDGE_CURVE ( 'NONE', #9714, #62942, #25178, .T. ) ;
#16201 = CARTESIAN_POINT ( 'NONE',  ( 1.339745962155615144, -99.58034179853028434, 4.999999999999999112 ) ) ;
#16202 = CARTESIAN_POINT ( 'NONE',  ( 2.499999999999998668, -1.333333333333332149, -4.330127018922193649 ) ) ;
#16203 = EDGE_CURVE ( 'NONE', #47984, #25841, #16550, .T. ) ;
#16204 = CARTESIAN_POINT ( 'NONE',  ( 3.061616997868383141E-16, -153.7500000000000000, -5.000000000000000000 ) ) ;
#16205 = CARTESIAN_POINT ( 'NONE',  ( -5.000000000000000000, -35.00000000000000000, 0.000000000000000000 ) ) ;
#16206 = CARTESIAN_POINT ( 'NONE',  ( 1.975475456537005874E-15, -38.62499999726880873, 5.000000000000000000 ) ) ;
#16208 = CARTESIAN_POINT ( 'NONE',  ( 2.229367062499998831, -11.89583333196774007, -3.861377020970580887 ) ) ;
#16207 = CARTESIAN_POINT ( 'NONE',  ( -5.000000000000000000, -59.00000000000000000, 0.000000000000000000 ) ) ;
#16209 = EDGE_CURVE ( 'NONE', #20078, #50991, #49025, .T. ) ;
#16210 = VECTOR ( 'NONE', #13942, 1000.000000000000000 ) ;
#16211 = LINE ( 'NONE', #6885, #889 ) ;
#16212 = CARTESIAN_POINT ( 'NONE',  ( 4.458734124999999437, -58.81249999863440081, -5.460374474430324690E-16 ) ) ;
#16213 = CARTESIAN_POINT ( 'NONE',  ( -4.458734125000000326, -151.2500000013656063, -1.846868145590735644 ) ) ;
#16214 = CARTESIAN_POINT ( 'NONE',  ( 4.458734125000001214, -67.89583333196773651, 2.574251347313718519 ) ) ;
#16215 = VECTOR ( 'NONE', #12777, 1000.000000000000000 ) ;
#16216 = EDGE_CURVE ( 'NONE', #46845, #47715, #60525, .T. ) ;
#16217 = ADVANCED_FACE ( 'NONE', ( #10514 ), #252, .T. ) ;
#16218 = CARTESIAN_POINT ( 'NONE',  ( 5.000000000000000000, -57.29166666393548013, -2.886751345948129988 ) ) ;
#16219 = VERTEX_POINT ( 'NONE', #11157 ) ;
#16220 = CARTESIAN_POINT ( 'NONE',  ( 2.500000000000002220, -26.66666666666666430, 4.330127018922192761 ) ) ;
#16221 = ORIENTED_EDGE ( 'NONE', *, *, #13315, .F. ) ;
#16223 = CARTESIAN_POINT ( 'NONE',  ( 2.499999999999998668, -103.3333333333333286, -4.330127018922193649 ) ) ;
#16222 = CARTESIAN_POINT ( 'NONE',  ( 1.975475456537005874E-15, -21.75000000000000000, 5.000000000000000000 ) ) ;
#16224 = CARTESIAN_POINT ( 'NONE',  ( -1.846868145590734756, -153.1250000013656063, -4.458734125000000326 ) ) ;
#16225 = EDGE_CURVE ( 'NONE', #2151, #51364, #44518, .T. ) ;
#16226 = ORIENTED_EDGE ( 'NONE', *, *, #49152, .F. ) ;
#16227 =( BOUNDED_CURVE ( )  B_SPLINE_CURVE ( 2, ( #45498, #25242, #179, #20097, #44857, #820, #20746, #39703, #20425 ),
 .UNSPECIFIED., .F., .F. ) 
 B_SPLINE_CURVE_WITH_KNOTS ( ( 3, 2, 2, 2, 3 ),
 ( 0.1416666666666667740, 0.1458333333333334814, 0.1500000000000001332, 0.1541666666666668406, 0.1583333333333334925 ),
 .UNSPECIFIED. ) 
 CURVE ( )  GEOMETRIC_REPRESENTATION_ITEM ( )  RATIONAL_B_SPLINE_CURVE ( ( 0.9999999999999980016, 0.9238795325112887369, 1.000000000000000000, 0.9238795325112867385, 1.000000000000000000, 0.9238795325112867385, 1.000000000000000000, 0.9238795325112837409, 1.000000000000003109 ) ) 
 REPRESENTATION_ITEM ( '' )  );
#16228 = EDGE_CURVE ( 'NONE', #23523, #31695, #58436, .T. ) ;
#16229 = DIRECTION ( 'NONE',  ( -0.000000000000000000, 1.000000000000000000, -0.000000000000000000 ) ) ;
#16230 = CARTESIAN_POINT ( 'NONE',  ( -58.80597590150559739, -129.0000000000000284, 3.242614290531460330 ) ) ;
#16231 = CARTESIAN_POINT ( 'NONE',  ( 5.000000000000000888, -80.45833333060213022, 2.886751345948126879 ) ) ;
#16232 = CARTESIAN_POINT ( 'NONE',  ( -3.152548672688508926E-16, -48.81249999863440792, -5.148502694627439702 ) ) ;
#16233 = ORIENTED_EDGE ( 'NONE', *, *, #37254, .F. ) ;
#16234 = VECTOR ( 'NONE', #6505, 1000.000000000000000 ) ;
#16235 = EDGE_CURVE ( 'NONE', #34949, #18684, #53918, .T. ) ;
#16236 = CARTESIAN_POINT ( 'NONE',  ( -2.500000000000000444, -110.0416666639354730, -4.330127018922193649 ) ) ;
#16237 = CARTESIAN_POINT ( 'NONE',  ( -2.229367062500000163, 13.52083333469892779, -3.861377020970580443 ) ) ;
#16238 = CARTESIAN_POINT ( 'NONE',  ( 9.457646018065525792E-16, 22.93750000136559919, 5.148502694627439702 ) ) ;
#16239 = CARTESIAN_POINT ( 'NONE',  ( -53.51423613279429503, -154.2500000013656063, 4.591703134518082763 ) ) ;
#16240 = LINE ( 'NONE', #11401, #25430 ) ;
#16241 = CARTESIAN_POINT ( 'NONE',  ( 2.500000000000002220, -25.66666666666666430, 4.330127018922192761 ) ) ;
#16242 = ORIENTED_EDGE ( 'NONE', *, *, #50054, .F. ) ;
#16243 = CARTESIAN_POINT ( 'NONE',  ( -4.458734124999997661, -66.22916666530106511, 2.574251347313722516 ) ) ;
#16244 = CARTESIAN_POINT ( 'NONE',  ( 1.282512619718868541, 8.391164935524033197, -7.795653906408837486 ) ) ;
#16245 = CARTESIAN_POINT ( 'NONE',  ( 9.457646018065525792E-16, 10.93750000136559208, 5.148502694627439702 ) ) ;
#16246 = CARTESIAN_POINT ( 'NONE',  ( -50.18089887299979068, -152.8125000027311842, 2.462841084822613436 ) ) ;
#16247 = CARTESIAN_POINT ( 'NONE',  ( -4.458734124999999437, -55.64583333196773651, -2.574251347313719407 ) ) ;
#16248 = CARTESIAN_POINT ( 'NONE',  ( 5.000000000000000000, -17.29166666393548368, -2.886751345948129988 ) ) ;
#16249 = DIRECTION ( 'NONE',  ( -0.000000000000000000, 1.000000000000000000, -0.000000000000000000 ) ) ;
#16250 = CARTESIAN_POINT ( 'NONE',  ( 7.499999999999999112, -2.930060224340428565, -0.4701183149080248036 ) ) ;
#16251 = CARTESIAN_POINT ( 'NONE',  ( -6.972266317189433020E-16, -87.25000000000001421, -5.000000000000000000 ) ) ;
#16252 = CARTESIAN_POINT ( 'NONE',  ( 1.339745962155612702, -104.1696581960073331, -5.000000000000000000 ) ) ;
#16253 = CARTESIAN_POINT ( 'NONE',  ( 4.458734125000000326, -14.14583333196774184, 2.574251347313718519 ) ) ;
#16254 = ORIENTED_EDGE ( 'NONE', *, *, #41668, .T. ) ;
#16255 = AXIS2_PLACEMENT_3D ( 'NONE', #50123, #46581, #45936 ) ;
#16256 = CARTESIAN_POINT ( 'NONE',  ( -3.535533905932737309, -143.7500000027311842, -3.535533905932738197 ) ) ;
#16257 = CARTESIAN_POINT ( 'NONE',  ( 9.457646018065525792E-16, -105.0624999986344079, 5.148502694627439702 ) ) ;
#16258 = CARTESIAN_POINT ( 'NONE',  ( 5.000000000000000888, -157.0625000027311842, -2.071067811865475505 ) ) ;
#16259 = ORIENTED_EDGE ( 'NONE', *, *, #2076, .T. ) ;
#16260 = CARTESIAN_POINT ( 'NONE',  ( -4.458734124999999437, -101.5624999986344079, 0.000000000000000000 ) ) ;
#16261 = VECTOR ( 'NONE', #40657, 1000.000000000000000 ) ;
#16262 = CARTESIAN_POINT ( 'NONE',  ( -2.229367062499996610, -28.14583333196774007, 3.861377020970582219 ) ) ;
#16263 = CARTESIAN_POINT ( 'NONE',  ( -2.500000000000000444, -61.04166666393547303, -4.330127018922193649 ) ) ;
#16264 = CARTESIAN_POINT ( 'NONE',  ( -59.44456063193725015, -124.5625000013655921, -0.3552334253322034230 ) ) ;
#16265 = CARTESIAN_POINT ( 'NONE',  ( -50.55543936806279248, -143.0625000013656063, 0.3552334253322060320 ) ) ;
#16266 = CARTESIAN_POINT ( 'NONE',  ( -4.458734124999999437, -23.31249999863440436, 0.000000000000000000 ) ) ;
#16267 = CARTESIAN_POINT ( 'NONE',  ( 4.458734124999999437, -64.06249999863440792, -5.460374474430324690E-16 ) ) ;
#16268 = CARTESIAN_POINT ( 'NONE',  ( -5.000000000000000000, -39.95833333060214443, -2.886751345948128211 ) ) ;
#16269 = CARTESIAN_POINT ( 'NONE',  ( -2.229367062499996610, -18.14583333196773651, 3.861377020970582219 ) ) ;
#16270 = PLANE ( 'NONE',  #62054 ) ;
#16271 = CARTESIAN_POINT ( 'NONE',  ( 3.535533905932738197, -149.8750000000000000, -3.535533905932738197 ) ) ;
#16272 = CARTESIAN_POINT ( 'NONE',  ( 2.500000000000002220, -11.66666666666666607, 4.330127018922192761 ) ) ;
#16273 = CARTESIAN_POINT ( 'NONE',  ( -1.846868145590734756, -153.1250000013656063, -4.458734125000000326 ) ) ;
#16274 = VERTEX_POINT ( 'NONE', #50715 ) ;
#16275 = CARTESIAN_POINT ( 'NONE',  ( 4.458734125000000326, -48.14583333196773651, 2.574251347313718519 ) ) ;
#16276 = DIRECTION ( 'NONE',  ( -0.000000000000000000, 1.000000000000000000, -0.000000000000000000 ) ) ;
#16277 = CARTESIAN_POINT ( 'NONE',  ( -7.970070017554212960, 4.546953124339755625, -8.057670357645356773 ) ) ;
#16278 = CARTESIAN_POINT ( 'NONE',  ( -4.999999999999999112, 27.08333333333333215, 2.886751345948131764 ) ) ;
#16279 = CARTESIAN_POINT ( 'NONE',  ( 2.229367062499998831, 3.354166668032259935, -3.861377020970580887 ) ) ;
#16280 = CARTESIAN_POINT ( 'NONE',  ( -1.339745962155613812, -74.08034179853029855, -5.000000000000000000 ) ) ;
#16281 = CARTESIAN_POINT ( 'NONE',  ( -6.972266317189433020E-16, 13.74999999999999822, -5.000000000000000000 ) ) ;
#16282 = CARTESIAN_POINT ( 'NONE',  ( -1.049326080737009628E-13, -17.75000000000000355, 5.000000000000000000 ) ) ;
#16283 = CARTESIAN_POINT ( 'NONE',  ( -4.458734124999999437, 17.43750000136559208, 0.000000000000000000 ) ) ;
#16284 = CARTESIAN_POINT ( 'NONE',  ( -2.499999999999996447, -78.83333333333332860, 4.330127018922195425 ) ) ;
#16285 = CARTESIAN_POINT ( 'NONE',  ( 2.499999999999998668, 7.791666669397852019, -4.330127018922193649 ) ) ;
#16286 = VERTEX_POINT ( 'NONE', #32364 ) ;
#16287 = CARTESIAN_POINT ( 'NONE',  ( -5.000000000000000000, -98.08333333333332860, -2.886751345948128211 ) ) ;
#16288 = VERTEX_POINT ( 'NONE', #16622 ) ;
#16289 = CARTESIAN_POINT ( 'NONE',  ( 7.204675194429079505E-15, 26.74999999999999645, -5.000000000000000000 ) ) ;
#16290 = CARTESIAN_POINT ( 'NONE',  ( -2.229367062499996610, -42.14583333196773651, 3.861377020970582219 ) ) ;
#16291 = CARTESIAN_POINT ( 'NONE',  ( 4.458734125000000326, -162.6250000013655779, -1.846868145590734978 ) ) ;
#16292 = CARTESIAN_POINT ( 'NONE',  ( -5.000000000000000000, -41.95833333060214443, -2.886751345948128211 ) ) ;
#16293 = ORIENTED_EDGE ( 'NONE', *, *, #27086, .T. ) ;
#16294 = CARTESIAN_POINT ( 'NONE',  ( -2.229367062500000163, -15.47916666530107399, -3.861377020970580443 ) ) ;
#16295 = EDGE_LOOP ( 'NONE', ( #21198, #42556, #43882, #25228 ) ) ;
#16296 = CARTESIAN_POINT ( 'NONE',  ( 5.000000000000000000, -86.41666666666667140, -2.886751345948129988 ) ) ;
#16297 = CARTESIAN_POINT ( 'NONE',  ( -4.458734124999999437, -167.9375000013655779, -5.460374474430324690E-16 ) ) ;
#16298 = AXIS2_PLACEMENT_3D ( 'NONE', #6007, #55840, #54880 ) ;
#16299 = CARTESIAN_POINT ( 'NONE',  ( 2.499999999999998668, -88.20833333060214443, -4.330127018922193649 ) ) ;
#16300 = ORIENTED_EDGE ( 'NONE', *, *, #5983, .F. ) ;
#16301 = CARTESIAN_POINT ( 'NONE',  ( -49.85088928181150436, -141.5625000000000568, -1.666127454062680702 ) ) ;
#16302 = VECTOR ( 'NONE', #48940, 1000.000000000000000 ) ;
#16303 = CARTESIAN_POINT ( 'NONE',  ( 4.458734124999999437, -30.06249999863440436, -5.460374474430324690E-16 ) ) ;
#16304 = DIRECTION ( 'NONE',  ( 0.000000000000000000, 1.000000000000000000, 0.000000000000000000 ) ) ;
#16305 = ORIENTED_EDGE ( 'NONE', *, *, #55150, .F. ) ;
#16306 =( BOUNDED_CURVE ( )  B_SPLINE_CURVE ( 2, ( #45658, #46296, #26352, #41770, #1615, #26677, #21541, #45974, #41137 ),
 .UNSPECIFIED., .F., .F. ) 
 B_SPLINE_CURVE_WITH_KNOTS ( ( 3, 2, 2, 2, 3 ),
 ( 0.4750000000000004219, 0.4791666666666671293, 0.4833333333333337811, 0.4875000000000004330, 0.4916666666666670849 ),
 .UNSPECIFIED. ) 
 CURVE ( )  GEOMETRIC_REPRESENTATION_ITEM ( )  RATIONAL_B_SPLINE_CURVE ( ( 0.9999999999999918954, 0.9238795325112948431, 1.000000000000000000, 0.9238795325112867385, 1.000000000000000000, 0.9238795325112867385, 1.000000000000000000, 0.9238795325112786339, 1.000000000000008216 ) ) 
 REPRESENTATION_ITEM ( '' )  );
#16307 = EDGE_CURVE ( 'NONE', #49482, #41437, #56509, .T. ) ;
#16308 = CARTESIAN_POINT ( 'NONE',  ( 2.229367062499998831, -74.64583333196773651, -3.861377020970580887 ) ) ;
#16309 = CARTESIAN_POINT ( 'NONE',  ( 4.458734124999999437, -109.0624999986343937, -5.460374474430324690E-16 ) ) ;
#16310 = CARTESIAN_POINT ( 'NONE',  ( -59.98410592259440222, -137.2500000027312126, -0.3983568153799752487 ) ) ;
#16311 = ORIENTED_EDGE ( 'NONE', *, *, #14160, .F. ) ;
#16312 = CARTESIAN_POINT ( 'NONE',  ( -5.000000000000000000, -26.08333333333332860, -2.886751345948128211 ) ) ;
#16313 = CARTESIAN_POINT ( 'NONE',  ( -59.29741812935640155, -143.8750000013655779, -2.196230717870135685 ) ) ;
#16314 = CARTESIAN_POINT ( 'NONE',  ( 4.458734124999999437, -78.06249999863440792, -5.460374474430324690E-16 ) ) ;
#16315 = CARTESIAN_POINT ( 'NONE',  ( -49.85088928181150436, -135.6875000027312126, -1.666127454062680702 ) ) ;
#16316 = CARTESIAN_POINT ( 'NONE',  ( -2.229367062499996610, -44.14583333196774362, 3.861377020970582219 ) ) ;
#16317 = CARTESIAN_POINT ( 'NONE',  ( 4.458734124999999437, -143.6250000013656347, -1.846868145590734978 ) ) ;
#16318 = CARTESIAN_POINT ( 'NONE',  ( 1.975475456537005874E-15, 20.24999999999999289, 5.000000000000000000 ) ) ;
#16319 = CARTESIAN_POINT ( 'NONE',  ( 2.229367062499998831, -47.64583333196774362, -3.861377020970580887 ) ) ;
#16320 = CARTESIAN_POINT ( 'NONE',  ( 4.458734124999999437, -43.81249999863440081, -5.460374474430324690E-16 ) ) ;
#16321 = CARTESIAN_POINT ( 'NONE',  ( 4.458734124999999437, 27.18750000136559564, -5.460374474430324690E-16 ) ) ;
#16322 = CARTESIAN_POINT ( 'NONE',  ( -2.229367062500000163, -17.47916666530106866, -3.861377020970580443 ) ) ;
#16323 = VECTOR ( 'NONE', #15873, 1000.000000000000000 ) ;
#16324 = CARTESIAN_POINT ( 'NONE',  ( 2.500000000000002220, -98.66666666666665719, 4.330127018922192761 ) ) ;
#16325 =( BOUNDED_CURVE ( )  B_SPLINE_CURVE ( 2, ( #54376, #38928, #28959, #4523, #48582, #58562, #53728, #9659, #48897 ),
 .UNSPECIFIED., .F., .F. ) 
 B_SPLINE_CURVE_WITH_KNOTS ( ( 3, 2, 2, 2, 3 ),
 ( 0.5854166666666666963, 0.5861111111111111382, 0.5875000000000000222, 0.5888888888888889062, 0.5895833333333333481 ),
 .UNSPECIFIED. ) 
 CURVE ( )  GEOMETRIC_REPRESENTATION_ITEM ( )  RATIONAL_B_SPLINE_CURVE ( ( 0.9330127018922194093, 0.9330127018922194093, 1.000000000000000000, 0.8660254037844387076, 1.000000000000000000, 0.8660254037844387076, 1.000000000000000000, 0.9330127018922194093, 0.9330127018922194093 ) ) 
 REPRESENTATION_ITEM ( '' )  );
#16326 = CARTESIAN_POINT ( 'NONE',  ( -2.071067811865446640, -167.3125000000000000, 5.000000000000031086 ) ) ;
#16327 = CARTESIAN_POINT ( 'NONE',  ( 4.458734124999998549, -37.97916666530107932, -2.574251347313721627 ) ) ;
#16328 = CARTESIAN_POINT ( 'NONE',  ( 5.000000000000000000, 2.625000002731185500, -6.123233995736766282E-16 ) ) ;
#16329 = CARTESIAN_POINT ( 'NONE',  ( -58.39396692619412477, -127.4375000013656063, 2.891590998281057701 ) ) ;
#16330 = CARTESIAN_POINT ( 'NONE',  ( -4.458734124999998549, -78.47916666530107932, 2.574251347313722516 ) ) ;
#16331 = CARTESIAN_POINT ( 'NONE',  ( 5.000000000000000000, 24.50000000000000000, -6.123233995736766282E-16 ) ) ;
#16332 = CARTESIAN_POINT ( 'NONE',  ( -49.85088928181150436, -140.6875000027312410, -1.666127454062680480 ) ) ;
#16333 = CARTESIAN_POINT ( 'NONE',  ( -4.458734124999999437, -1.645833331967737401, -2.574251347313719407 ) ) ;
#16334 = EDGE_LOOP ( 'NONE', ( #6071, #40400, #26907, #53856 ) ) ;
#16335 = CARTESIAN_POINT ( 'NONE',  ( 5.000000000000000000, 24.62500000273118417, -6.123233995736766282E-16 ) ) ;
#16336 = CARTESIAN_POINT ( 'NONE',  ( -1.339745962155610925, -75.79465819873853150, 5.000000000000000000 ) ) ;
#16337 = CARTESIAN_POINT ( 'NONE',  ( 2.229367062500001939, -89.97916666530106511, 3.861377020970579999 ) ) ;
#16338 = CARTESIAN_POINT ( 'NONE',  ( 5.000000000000000000, -169.1250000027312126, 0.000000000000000000 ) ) ;
#16339 = CARTESIAN_POINT ( 'NONE',  ( 2.229367062500001939, -86.22916666530107932, 3.861377020970579999 ) ) ;
#16340 = CARTESIAN_POINT ( 'NONE',  ( 9.457646018065525792E-16, 18.68750000136559208, 5.148502694627439702 ) ) ;
#16341 = CARTESIAN_POINT ( 'NONE',  ( 1.339745962155612702, -77.16965819600731891, -5.000000000000000000 ) ) ;
#16342 = CARTESIAN_POINT ( 'NONE',  ( -59.59170313451811296, -139.5000000013656063, 1.485763867205729394 ) ) ;
#16343 = CARTESIAN_POINT ( 'NONE',  ( -3.152548672688508926E-16, -7.562499998634404363, -5.148502694627439702 ) ) ;
#16344 = CARTESIAN_POINT ( 'NONE',  ( -4.458734124999999437, 24.43750000136559208, 0.000000000000000000 ) ) ;
#16345 = CARTESIAN_POINT ( 'NONE',  ( -4.458734124999999437, -47.56249999863440792, 0.000000000000000000 ) ) ;
#16346 = CARTESIAN_POINT ( 'NONE',  ( -6.972266317189433020E-16, -38.12499999726880873, -5.000000000000000000 ) ) ;
#16347 = CARTESIAN_POINT ( 'NONE',  ( -2.229367062500000163, -87.47916666530107932, -3.861377020970580443 ) ) ;
#16348 = CARTESIAN_POINT ( 'NONE',  ( -4.458734124999999437, -3.312499998634407916, 0.000000000000000000 ) ) ;
#16349 = DIRECTION ( 'NONE',  ( -0.000000000000000000, 1.000000000000000000, -0.000000000000000000 ) ) ;
#16350 = ORIENTED_EDGE ( 'NONE', *, *, #59851, .F. ) ;
#16351 = CARTESIAN_POINT ( 'NONE',  ( -3.152548672688508926E-16, -31.81249999863440436, -5.148502694627439702 ) ) ;
#16352 = AXIS2_PLACEMENT_3D ( 'NONE', #40548, #11911, #36684 ) ;
#16353 = CARTESIAN_POINT ( 'NONE',  ( -59.29741812935640155, -132.8750000013656063, -2.196230717870135685 ) ) ;
#16354 = CARTESIAN_POINT ( 'NONE',  ( 9.457646018065525792E-16, -76.06249999863440792, 5.148502694627439702 ) ) ;
#16355 = CARTESIAN_POINT ( 'NONE',  ( 5.000000000000000888, -110.4583333306021586, 2.886751345948126879 ) ) ;
#16356 = VECTOR ( 'NONE', #7148, 1000.000000000000000 ) ;
#16357 = CARTESIAN_POINT ( 'NONE',  ( -4.458734124999998549, 20.77083333469892779, 2.574251347313722516 ) ) ;
#16358 = CARTESIAN_POINT ( 'NONE',  ( 0.000000000000000000, -170.0000000000000000, 5.000000000000000000 ) ) ;
#16359 = CARTESIAN_POINT ( 'NONE',  ( -2.229367062499996610, -79.39583333196773651, 3.861377020970582219 ) ) ;
#16360 = CARTESIAN_POINT ( 'NONE',  ( -5.000000000000000000, -63.08333333333332860, -2.886751345948128211 ) ) ;
#16361 = DIRECTION ( 'NONE',  ( 0.000000000000000000, 0.000000000000000000, 1.000000000000000000 ) ) ;
#16362 = CARTESIAN_POINT ( 'NONE',  ( -2.500000000000000444, 24.95833333606451987, -4.330127018922193649 ) ) ;
#16363 = ORIENTED_EDGE ( 'NONE', *, *, #56675, .F. ) ;
#16364 = CARTESIAN_POINT ( 'NONE',  ( -1.339745962155613812, -73.08034179853029855, -5.000000000000000000 ) ) ;
#16365 = CARTESIAN_POINT ( 'NONE',  ( 1.975475456537005874E-15, -69.74999999999998579, 5.000000000000000000 ) ) ;
#16367 = CARTESIAN_POINT ( 'NONE',  ( 5.000000000000000000, -22.50000000000000000, -6.123233995736766282E-16 ) ) ;
#16366 = CARTESIAN_POINT ( 'NONE',  ( 1.975475456537005874E-15, -60.62499999726880162, 5.000000000000000000 ) ) ;
#16368 = CARTESIAN_POINT ( 'NONE',  ( 2.229367062500001939, -27.97916666530107221, 3.861377020970579999 ) ) ;
#16369 = AXIS2_PLACEMENT_3D ( 'NONE', #36720, #37037, #2007 ) ;
#16370 = CARTESIAN_POINT ( 'NONE',  ( -4.458734124999999437, -86.31249999863439371, 0.000000000000000000 ) ) ;
#16371 = CARTESIAN_POINT ( 'NONE',  ( -5.000000000000000000, -20.95833333060214798, -2.886751345948128211 ) ) ;
#16373 = ORIENTED_EDGE ( 'NONE', *, *, #33581, .T. ) ;
#16372 = CARTESIAN_POINT ( 'NONE',  ( -3.152548672688508926E-16, -56.56249999863439371, -5.148502694627439702 ) ) ;
#16374 = CARTESIAN_POINT ( 'NONE',  ( 5.000000000000000888, -49.58333333333332149, 2.886751345948126879 ) ) ;
#16375 = CARTESIAN_POINT ( 'NONE',  ( 5.000000000000000888, 27.54166666939785557, 2.886751345948126879 ) ) ;
#16377 = ORIENTED_EDGE ( 'NONE', *, *, #62021, .T. ) ;
#16376 = CARTESIAN_POINT ( 'NONE',  ( -4.458734124999998549, -4.479166665301070438, 2.574251347313722516 ) ) ;
#16378 = CARTESIAN_POINT ( 'NONE',  ( 2.500000000000002220, -70.66666666666667140, 4.330127018922192761 ) ) ;
#16379 = CARTESIAN_POINT ( 'NONE',  ( 4.458734125000000326, -153.6250000013655779, -1.846868145590734978 ) ) ;
#16380 = CARTESIAN_POINT ( 'NONE',  ( -2.229367062499996610, -46.39583333196774362, 3.861377020970582219 ) ) ;
#16381 = CARTESIAN_POINT ( 'NONE',  ( -6.972266317189433020E-16, 24.87500000273118417, -5.000000000000000000 ) ) ;
#16382 =( BOUNDED_CURVE ( )  B_SPLINE_CURVE ( 2, ( #3362, #8493, #42890, #7867, #46467, #47099, #36818, #62537, #3049 ),
 .UNSPECIFIED., .F., .F. ) 
 B_SPLINE_CURVE_WITH_KNOTS ( ( 3, 2, 2, 2, 3 ),
 ( 0.8482142857142856984, 0.8488095238095237915, 0.8499999999999999778, 0.8511904761904761640, 0.8517857142857142572 ),
 .UNSPECIFIED. ) 
 CURVE ( )  GEOMETRIC_REPRESENTATION_ITEM ( )  RATIONAL_B_SPLINE_CURVE ( ( 0.9330127018922194093, 0.9330127018922194093, 1.000000000000000000, 0.8660254037844387076, 1.000000000000000000, 0.8660254037844387076, 1.000000000000000000, 0.9330127018922194093, 0.9330127018922194093 ) ) 
 REPRESENTATION_ITEM ( '' )  );
#16383 = CARTESIAN_POINT ( 'NONE',  ( -3.535533905932738641, -157.3750000000000284, 3.535533905932737309 ) ) ;
#16384 = CARTESIAN_POINT ( 'NONE',  ( -1.339745962155613812, -86.20534180126146850, -5.000000000000000000 ) ) ;
#16385 = CARTESIAN_POINT ( 'NONE',  ( -59.81910112700025905, -153.1875000000000284, -2.462841084822630311 ) ) ;
#16386 = CARTESIAN_POINT ( 'NONE',  ( -2.229367062499996610, -17.39583333196773651, 3.861377020970582219 ) ) ;
#16387 = CARTESIAN_POINT ( 'NONE',  ( 2.229367062499998831, -53.89583333196773651, -3.861377020970580887 ) ) ;
#16388 = CYLINDRICAL_SURFACE ( 'NONE', #607, 5.000000000000000000 ) ;
#16389 = CARTESIAN_POINT ( 'NONE',  ( 3.152801135295366208, -145.5625000013655779, 3.152801135295367985 ) ) ;
#16390 = CARTESIAN_POINT ( 'NONE',  ( -4.458734124999999437, -95.64583333196772230, -2.574251347313719407 ) ) ;
#16391 = DIRECTION ( 'NONE',  ( -0.000000000000000000, 1.000000000000000000, -0.000000000000000000 ) ) ;
#16392 = VERTEX_POINT ( 'NONE', #7931 ) ;
#16393 = CARTESIAN_POINT ( 'NONE',  ( -57.19623071787016499, -152.6250000013656063, 4.297418129356382899 ) ) ;
#16394 = CARTESIAN_POINT ( 'NONE',  ( 4.458734124999999437, 25.93750000136559564, -5.460374474430324690E-16 ) ) ;
#16395 = CARTESIAN_POINT ( 'NONE',  ( -55.39835681537999790, -146.0000000027312126, 4.984105922594378235 ) ) ;
#16396 = CYLINDRICAL_SURFACE ( 'NONE', #63020, 5.000000000000000000 ) ;
#16397 = AXIS2_PLACEMENT_3D ( 'NONE', #56987, #61077, #20560 ) ;
#16398 = VERTEX_POINT ( 'NONE', #41056 ) ;
#16399 = CARTESIAN_POINT ( 'NONE',  ( 4.458734124999999437, -4.812499998634402587, -5.460374474430324690E-16 ) ) ;
#16400 = CARTESIAN_POINT ( 'NONE',  ( 3.061616997868383141E-16, -164.7500000000000000, -5.000000000000000000 ) ) ;
#16401 = CARTESIAN_POINT ( 'NONE',  ( -4.458734124999999437, -23.56249999863440436, 0.000000000000000000 ) ) ;
#16402 = CARTESIAN_POINT ( 'NONE',  ( 2.499999999999998668, -72.33333333333332860, -4.330127018922193649 ) ) ;
#16403 = CARTESIAN_POINT ( 'NONE',  ( 4.458734124999999437, -8.812499998634406140, -5.460374474430324690E-16 ) ) ;
#16404 = CARTESIAN_POINT ( 'NONE',  ( 5.000000000000000888, 6.541666669397851130, 2.886751345948126879 ) ) ;
#16405 = CARTESIAN_POINT ( 'NONE',  ( 1.846868145590736310, -148.6250000013655779, 4.458734124999997661 ) ) ;
#16406 =( BOUNDED_CURVE ( )  B_SPLINE_CURVE ( 2, ( #17861, #61624, #62257, #8221, #17559, #4025, #18176, #3086, #61942 ),
 .UNSPECIFIED., .F., .F. ) 
 B_SPLINE_CURVE_WITH_KNOTS ( ( 3, 2, 2, 2, 3 ),
 ( 0.3160714285714285587, 0.3166666666666666519, 0.3178571428571428381, 0.3190476190476190244, 0.3196428571428571175 ),
 .UNSPECIFIED. ) 
 CURVE ( )  GEOMETRIC_REPRESENTATION_ITEM ( )  RATIONAL_B_SPLINE_CURVE ( ( 0.9330127018922194093, 0.9330127018922194093, 1.000000000000000000, 0.8660254037844387076, 1.000000000000000000, 0.8660254037844387076, 1.000000000000000000, 0.9330127018922194093, 0.9330127018922194093 ) ) 
 REPRESENTATION_ITEM ( '' )  );
#16407 = CARTESIAN_POINT ( 'NONE',  ( -4.458734124999997661, 13.52083333469892779, 2.574251347313722516 ) ) ;
#16408 = ORIENTED_EDGE ( 'NONE', *, *, #49952, .F. ) ;
#16409 = CARTESIAN_POINT ( 'NONE',  ( 1.975475456537005874E-15, -13.62499999726881228, 5.000000000000000000 ) ) ;
#16410 = CARTESIAN_POINT ( 'NONE',  ( -6.972266317189433020E-16, -21.24999999999999289, -5.000000000000000000 ) ) ;
#16411 = CARTESIAN_POINT ( 'NONE',  ( -4.458734124999999437, -18.31249999863440792, 0.000000000000000000 ) ) ;
#16412 = EDGE_CURVE ( 'NONE', #7881, #58981, #56013, .T. ) ;
#16413 = CARTESIAN_POINT ( 'NONE',  ( 5.000000000000000000, -85.29166666393547303, -2.886751345948130876 ) ) ;
#16414 = CARTESIAN_POINT ( 'NONE',  ( 0.000000000000000000, -170.0000000000000000, 0.000000000000000000 ) ) ;
#16415 = CARTESIAN_POINT ( 'NONE',  ( -59.29741812935640155, -150.6250000013656063, -2.196230717870135685 ) ) ;
#16416 = CARTESIAN_POINT ( 'NONE',  ( 1.060575238724906964E-15, -45.62499999726880873, 5.773502691896257311 ) ) ;
#16417 = CARTESIAN_POINT ( 'NONE',  ( -2.499999999999996447, -1.708333330602145761, 4.330127018922195425 ) ) ;
#16418 = CARTESIAN_POINT ( 'NONE',  ( 4.458734125000000326, 10.10416666803226171, 2.574251347313718519 ) ) ;
#16419 = DIRECTION ( 'NONE',  ( 0.000000000000000000, -1.000000000000000000, 0.000000000000000000 ) ) ;
#16420 = CARTESIAN_POINT ( 'NONE',  ( -6.972266317189433020E-16, 9.750000000000000000, -5.000000000000000000 ) ) ;
#16421 = CARTESIAN_POINT ( 'NONE',  ( 4.458734124999998549, 14.27083333469892601, -2.574251347313721627 ) ) ;
#16422 = CARTESIAN_POINT ( 'NONE',  ( 2.229367062500001939, -66.97916666530106511, 3.861377020970579999 ) ) ;
#16423 = CARTESIAN_POINT ( 'NONE',  ( -3.152548672688508926E-16, -16.81249999863440436, -5.148502694627439702 ) ) ;
#16424 = CARTESIAN_POINT ( 'NONE',  ( -2.500000000000000444, 0.8333333333333317050, -4.330127018922193649 ) ) ;
#16425 = CARTESIAN_POINT ( 'NONE',  ( -4.458734125000000326, -163.0000000013655779, -1.846868145590735644 ) ) ;
#16426 = CARTESIAN_POINT ( 'NONE',  ( -1.339745962155614700, 26.33034180399265978, 4.999999999999999112 ) ) ;
#16427 = CARTESIAN_POINT ( 'NONE',  ( 2.229367062499998831, -60.64583333196774362, -3.861377020970580887 ) ) ;
#16428 = CARTESIAN_POINT ( 'NONE',  ( 2.500000000000002220, -94.54166666393547303, 4.330127018922192761 ) ) ;
#16429 = EDGE_CURVE ( 'NONE', #49453, #59631, #34187, .T. ) ;
#16430 = CARTESIAN_POINT ( 'NONE',  ( -6.972266317189433020E-16, -80.24999999999998579, -5.000000000000000000 ) ) ;
#16431 = CARTESIAN_POINT ( 'NONE',  ( 0.000000000000000000, -120.0000000000000000, 0.000000000000000000 ) ) ;
#16432 = CARTESIAN_POINT ( 'NONE',  ( -2.229367062500000163, -37.47916666530107221, -3.861377020970580443 ) ) ;
#16433 = CARTESIAN_POINT ( 'NONE',  ( -4.999999999999998224, -90.79166666393547303, 2.886751345948131764 ) ) ;
#16434 = CARTESIAN_POINT ( 'NONE',  ( -5.000000000000000000, -46.00000000000000000, 0.000000000000000000 ) ) ;
#16435 = CARTESIAN_POINT ( 'NONE',  ( -6.972266317189433020E-16, -17.12499999726881583, -5.000000000000000000 ) ) ;
#16436 = ORIENTED_EDGE ( 'NONE', *, *, #46497, .T. ) ;
#16437 = CARTESIAN_POINT ( 'NONE',  ( 4.458734124999998549, -106.7291666653010651, -2.574251347313721627 ) ) ;
#16438 = CARTESIAN_POINT ( 'NONE',  ( 4.458734124999999437, -4.062499998634408804, -5.460374474430324690E-16 ) ) ;
#16439 = PRODUCT_DEFINITION_FORMATION_WITH_SPECIFIED_SOURCE ( 'ANY', '', #19399, .NOT_KNOWN. ) ;
#16440 = CARTESIAN_POINT ( 'NONE',  ( -6.972266317189433020E-16, -9.124999997268814056, -5.000000000000000000 ) ) ;
#16441 = CARTESIAN_POINT ( 'NONE',  ( -2.499999999999996447, -9.833333333333332149, 4.330127018922195425 ) ) ;
#16442 = CARTESIAN_POINT ( 'NONE',  ( -3.152548672688508926E-16, -73.56249999863439371, -5.148502694627439702 ) ) ;
#16443 = CARTESIAN_POINT ( 'NONE',  ( 1.975475456537005874E-15, -22.62499999726880873, 5.000000000000000000 ) ) ;
#16444 = CARTESIAN_POINT ( 'NONE',  ( 2.500000000000002220, -7.541666663935481907, 4.330127018922192761 ) ) ;
#16445 = VECTOR ( 'NONE', #43446, 1000.000000000000000 ) ;
#16447 = ORIENTED_EDGE ( 'NONE', *, *, #1594, .F. ) ;
#16446 = CARTESIAN_POINT ( 'NONE',  ( -3.152548672688508926E-16, -37.56249999863440792, -5.148502694627439702 ) ) ;
#16448 = CARTESIAN_POINT ( 'NONE',  ( 5.000000000000000000, -22.37499999726881228, -6.123233995736766282E-16 ) ) ;
#16450 = ORIENTED_EDGE ( 'NONE', *, *, #9423, .T. ) ;
#16449 = CARTESIAN_POINT ( 'NONE',  ( -2.229367062499996610, 10.60416666803225993, 3.861377020970582219 ) ) ;
#16451 = CARTESIAN_POINT ( 'NONE',  ( -55.39835681537999790, -141.0000000027312126, 4.984105922594378235 ) ) ;
#16452 = CARTESIAN_POINT ( 'NONE',  ( -3.535250795749689387E-16, -57.25000000000000000, -5.773502691896257311 ) ) ;
#16453 = CARTESIAN_POINT ( 'NONE',  ( -3.152548672688508926E-16, -29.81249999863440436, -5.148502694627439702 ) ) ;
#16454 = CARTESIAN_POINT ( 'NONE',  ( 2.500000000000002220, -4.666666666666666075, 4.330127018922192761 ) ) ;
#16455 = CARTESIAN_POINT ( 'NONE',  ( 2.229367062500001939, -77.97916666530106511, 3.861377020970579999 ) ) ;
#16456 = CARTESIAN_POINT ( 'NONE',  ( 1.846868145590736310, -141.8750000013656063, 4.458734124999999437 ) ) ;
#16457 = CARTESIAN_POINT ( 'NONE',  ( 2.229367062500001939, -86.97916666530107932, 3.861377020970579999 ) ) ;
#16458 = CARTESIAN_POINT ( 'NONE',  ( -50.40829686548195099, -135.2500000013656347, -1.485763867205728284 ) ) ;
#16459 = CARTESIAN_POINT ( 'NONE',  ( -4.458734124999998549, -37.47916666530107221, 2.574251347313722516 ) ) ;
#16460 = CARTESIAN_POINT ( 'NONE',  ( 1.255007937094098239E-14, 23.87500000273118417, -4.999999999999999112 ) ) ;
#16461 = VERTEX_POINT ( 'NONE', #32042 ) ;
#16462 = CARTESIAN_POINT ( 'NONE',  ( 2.229367062499998831, -76.89583333196773651, -3.861377020970580887 ) ) ;
#16463 = DIRECTION ( 'NONE',  ( 0.000000000000000000, 0.000000000000000000, 1.000000000000000000 ) ) ;
#16464 = ORIENTED_EDGE ( 'NONE', *, *, #11829, .T. ) ;
#16465 = LINE ( 'NONE', #20666, #41887 ) ;
#16466 = CARTESIAN_POINT ( 'NONE',  ( 6.123233995736766282E-16, -170.0000000000000000, -5.000000000000000000 ) ) ;
#16467 = CARTESIAN_POINT ( 'NONE',  ( -3.152548672688508926E-16, -65.81249999863440792, -5.148502694627439702 ) ) ;
#16468 = CARTESIAN_POINT ( 'NONE',  ( -4.458734124999998549, -9.479166665301070438, 2.574251347313722516 ) ) ;
#16469 = VERTEX_POINT ( 'NONE', #31094 ) ;
#16470 = CARTESIAN_POINT ( 'NONE',  ( -5.000000000000000888, -156.5625000027311842, 2.071067811865474617 ) ) ;
#16471 = DIRECTION ( 'NONE',  ( 1.000000000000000000, 0.000000000000000000, 0.000000000000000000 ) ) ;
#16472 = EDGE_LOOP ( 'NONE', ( #56444, #22989, #50219, #50128 ) ) ;
#16473 = CARTESIAN_POINT ( 'NONE',  ( 2.500000000000002220, -91.66666666666665719, 4.330127018922192761 ) ) ;
#16474 = CARTESIAN_POINT ( 'NONE',  ( 4.458734124999998549, 5.270833334698926897, -2.574251347313721627 ) ) ;
#16475 = VECTOR ( 'NONE', #53104, 1000.000000000000000 ) ;
#16476 = CARTESIAN_POINT ( 'NONE',  ( -6.972266317189433020E-16, -64.24999999999998579, -5.000000000000000000 ) ) ;
#16477 = CARTESIAN_POINT ( 'NONE',  ( -8.190561711645485556E-16, -159.6875000013655779, 4.458734124999999437 ) ) ;
#16478 = DIRECTION ( 'NONE',  ( -0.000000000000000000, 1.000000000000000000, -0.000000000000000000 ) ) ;
#16479 = ORIENTED_EDGE ( 'NONE', *, *, #10548, .F. ) ;
#16480 = CARTESIAN_POINT ( 'NONE',  ( -2.229367062499996610, -89.14583333196773651, 3.861377020970582219 ) ) ;
#16481 = CARTESIAN_POINT ( 'NONE',  ( 5.000000000000000000, -29.37499999726881228, -6.123233995736766282E-16 ) ) ;
#16482 = CARTESIAN_POINT ( 'NONE',  ( -2.229367062499996610, -4.145833331967739177, 3.861377020970582219 ) ) ;
#16483 = AXIS2_PLACEMENT_3D ( 'NONE', #14191, #48603, #4543 ) ;
#16484 = EDGE_CURVE ( 'NONE', #17652, #30039, #49414, .T. ) ;
#16485 = CYLINDRICAL_SURFACE ( 'NONE', #19084, 5.000000000000000000 ) ;
#16486 = CARTESIAN_POINT ( 'NONE',  ( 1.060575238724906964E-15, -28.62499999726881228, 5.773502691896257311 ) ) ;
#16487 = CYLINDRICAL_SURFACE ( 'NONE', #55481, 5.000000000000000000 ) ;
#16488 = CARTESIAN_POINT ( 'NONE',  ( 4.458734125000000326, 24.10416666803225993, 2.574251347313718519 ) ) ;
#16489 = CARTESIAN_POINT ( 'NONE',  ( 5.000000000000000000, -104.5000000000000142, -6.123233995736766282E-16 ) ) ;
#16490 = CARTESIAN_POINT ( 'NONE',  ( 9.457646018065525792E-16, 25.93750000136559564, 5.148502694627439702 ) ) ;
#16491 = CARTESIAN_POINT ( 'NONE',  ( -2.229367062500000163, -49.47916666530107221, -3.861377020970580443 ) ) ;
#16492 = CARTESIAN_POINT ( 'NONE',  ( -4.458734124999999437, -35.56249999863440792, 0.000000000000000000 ) ) ;
#16493 = CARTESIAN_POINT ( 'NONE',  ( -4.458734124999999437, 1.437500001365592972, 0.000000000000000000 ) ) ;
#16494 = CARTESIAN_POINT ( 'NONE',  ( 5.000000000000000000, 14.58333333333333215, -2.886751345948129988 ) ) ;
#16495 = CARTESIAN_POINT ( 'NONE',  ( 2.071067811865475505, -145.9375000027312126, -5.000000000000000888 ) ) ;
#16497 = EDGE_CURVE ( 'NONE', #48477, #11293, #27630, .T. ) ;
#16496 = CARTESIAN_POINT ( 'NONE',  ( 0.000000000000000000, -170.0000000000000000, 5.000000000000000000 ) ) ;
#16498 = CARTESIAN_POINT ( 'NONE',  ( 4.458734125000001214, -40.89583333196773651, 2.574251347313718519 ) ) ;
#16499 = CARTESIAN_POINT ( 'NONE',  ( 2.500000000000002220, -77.54166666393547303, 4.330127018922192761 ) ) ;
#16500 = CARTESIAN_POINT ( 'NONE',  ( -50.40829686548195099, -138.2500000013656063, -1.485763867205728284 ) ) ;
#16501 =( BOUNDED_CURVE ( )  B_SPLINE_CURVE ( 2, ( #54430, #17423, #31886, #30930, #46367, #56665, #2951, #35765, #16460 ),
 .UNSPECIFIED., .F., .F. ) 
 B_SPLINE_CURVE_WITH_KNOTS ( ( 3, 2, 2, 2, 3 ),
 ( 0.03958333333333333842, 0.04027777777777778040, 0.04166666666666666435, 0.04305555555555555525, 0.04375000000000000416 ),
 .UNSPECIFIED. ) 
 CURVE ( )  GEOMETRIC_REPRESENTATION_ITEM ( )  RATIONAL_B_SPLINE_CURVE ( ( 0.9330127018922192983, 0.9330127018922196314, 1.000000000000000000, 0.8660254037844387076, 1.000000000000000000, 0.8660254037844387076, 1.000000000000000000, 0.9330127018922189652, 0.9330127018922192983 ) ) 
 REPRESENTATION_ITEM ( '' )  );
#16502 = CARTESIAN_POINT ( 'NONE',  ( 5.000000000000000000, -22.41666666666666785, -2.886751345948130876 ) ) ;
#16503 = EDGE_CURVE ( 'NONE', #13218, #11760, #55642, .T. ) ;
#16504 = CARTESIAN_POINT ( 'NONE',  ( 4.458734124999999437, -84.06249999863439371, -5.460374474430324690E-16 ) ) ;
#16505 = CARTESIAN_POINT ( 'NONE',  ( 1.846868145590736310, -161.8750000013656063, 4.458734124999997661 ) ) ;
#16506 = CARTESIAN_POINT ( 'NONE',  ( 0.000000000000000000, 15.00000000000000000, 0.000000000000000000 ) ) ;
#16507 = CARTESIAN_POINT ( 'NONE',  ( -2.500000000000000444, -29.16666666666666785, -4.330127018922193649 ) ) ;
#16508 = CARTESIAN_POINT ( 'NONE',  ( 4.458734124999999437, -139.5000000013655779, 1.846868145590737864 ) ) ;
#16509 = ORIENTED_EDGE ( 'NONE', *, *, #36121, .T. ) ;
#16510 = CARTESIAN_POINT ( 'NONE',  ( -3.152548672688508926E-16, 23.18750000136559208, -5.148502694627439702 ) ) ;
#16511 = ORIENTED_EDGE ( 'NONE', *, *, #51470, .F. ) ;
#16512 = CARTESIAN_POINT ( 'NONE',  ( 9.457646018065525792E-16, -91.06249999863439371, 5.148502694627439702 ) ) ;
#16513 = CARTESIAN_POINT ( 'NONE',  ( -2.229367062500000163, 12.27083333469892601, -3.861377020970580443 ) ) ;
#16514 = CARTESIAN_POINT ( 'NONE',  ( -5.000000000000000000, 15.12500000273118417, 0.000000000000000000 ) ) ;
#16515 = CARTESIAN_POINT ( 'NONE',  ( -2.499999999999996447, -2.708333330602146649, 4.330127018922195425 ) ) ;
#16516 = CARTESIAN_POINT ( 'NONE',  ( 2.500000000000002220, 7.333333333333333925, 4.330127018922192761 ) ) ;
#16517 = CARTESIAN_POINT ( 'NONE',  ( -4.458734124999997661, -57.22916666530107932, 2.574251347313722516 ) ) ;
#16518 = CARTESIAN_POINT ( 'NONE',  ( 2.229367062499998831, -12.64583333196774007, -3.861377020970580887 ) ) ;
#16519 = CARTESIAN_POINT ( 'NONE',  ( 1.339745962155612702, -61.16965819600733312, -5.000000000000000000 ) ) ;
#16520 = CARTESIAN_POINT ( 'NONE',  ( -58.39396692619412477, -136.6875000013656063, 2.891590998281057701 ) ) ;
#16521 = CARTESIAN_POINT ( 'NONE',  ( -5.000000000000000000, -63.87499999726880873, 0.000000000000000000 ) ) ;
#16522 = CARTESIAN_POINT ( 'NONE',  ( -5.000000000000000000, -37.00000000000000711, 0.000000000000000000 ) ) ;
#16523 = CARTESIAN_POINT ( 'NONE',  ( -2.500000000000000444, -62.16666666666666430, -4.330127018922193649 ) ) ;
#16524 = CARTESIAN_POINT ( 'NONE',  ( -5.000000000000000000, -34.08333333333332860, -2.886751345948128211 ) ) ;
#16525 = CARTESIAN_POINT ( 'NONE',  ( 1.975475456537005874E-15, -56.62499999726880162, 5.000000000000000000 ) ) ;
#16526 = CARTESIAN_POINT ( 'NONE',  ( 2.229367062499998831, -16.89583333196773651, -3.861377020970580887 ) ) ;
#16527 = LINE ( 'NONE', #36151, #12171 ) ;
#16528 = CARTESIAN_POINT ( 'NONE',  ( -2.229367062500000163, -59.47916666530106511, -3.861377020970580443 ) ) ;
#16529 = CARTESIAN_POINT ( 'NONE',  ( 3.152801135295366208, -151.8125000013655779, 3.152801135295367985 ) ) ;
#16530 = AXIS2_PLACEMENT_3D ( 'NONE', #55758, #59959, #35822 ) ;
#16531 = EDGE_CURVE ( 'NONE', #34465, #9066, #60146, .T. ) ;
#16532 = CARTESIAN_POINT ( 'NONE',  ( 2.229367062500001939, -73.97916666530106511, 3.861377020970579999 ) ) ;
#16533 = CARTESIAN_POINT ( 'NONE',  ( -57.19623071787017210, -147.6250000013655779, 4.297418129356382899 ) ) ;
#16534 = CARTESIAN_POINT ( 'NONE',  ( -2.229367062499996610, -21.39583333196774007, 3.861377020970582219 ) ) ;
#16535 = CARTESIAN_POINT ( 'NONE',  ( 2.500000000000002220, -61.54166666393547303, 4.330127018922192761 ) ) ;
#16536 = ORIENTED_EDGE ( 'NONE', *, *, #31543, .F. ) ;
#16537 = FACE_OUTER_BOUND ( 'NONE', #48791, .T. ) ;
#16538 = ORIENTED_EDGE ( 'NONE', *, *, #20941, .F. ) ;
#16540 = CARTESIAN_POINT ( 'NONE',  ( -6.972266317189433020E-16, -86.25000000000001421, -5.000000000000000000 ) ) ;
#16539 = CARTESIAN_POINT ( 'NONE',  ( -6.972266317189433020E-16, -28.25000000000000000, -5.000000000000000000 ) ) ;
#16541 = CARTESIAN_POINT ( 'NONE',  ( 4.458734124999999437, -154.5000000013656347, 1.846868145590737864 ) ) ;
#16542 = ORIENTED_EDGE ( 'NONE', *, *, #30358, .T. ) ;
#16543 = CARTESIAN_POINT ( 'NONE',  ( 1.339745962155615144, -54.70534180126148271, 4.999999999999999112 ) ) ;
#16544 = CARTESIAN_POINT ( 'NONE',  ( -51.75738570946856498, -127.7500000000000284, 3.805975901505576964 ) ) ;
#16545 = CARTESIAN_POINT ( 'NONE',  ( 1.339745962155612702, 15.70534180126147916, -5.000000000000000000 ) ) ;
#16546 = CARTESIAN_POINT ( 'NONE',  ( 4.458734124999998549, -45.97916666530106511, -2.574251347313721627 ) ) ;
#16547 = ORIENTED_EDGE ( 'NONE', *, *, #8658, .T. ) ;
#16548 = CARTESIAN_POINT ( 'NONE',  ( -2.071067811865562991, -145.3124999999999716, 4.999999999999913847 ) ) ;
#16549 = CARTESIAN_POINT ( 'NONE',  ( -4.458734124999998549, 15.77083333469892601, 2.574251347313722516 ) ) ;
#16550 =( BOUNDED_CURVE ( )  B_SPLINE_CURVE ( 2, ( #15027, #569, #5703, #40737, #44609, #39776, #54909, #30779, #55235 ),
 .UNSPECIFIED., .F., .F. ) 
 B_SPLINE_CURVE_WITH_KNOTS ( ( 3, 2, 2, 2, 3 ),
 ( 0.4437499999999999778, 0.4444444444444444198, 0.4458333333333333592, 0.4472222222222222432, 0.4479166666666666852 ),
 .UNSPECIFIED. ) 
 CURVE ( )  GEOMETRIC_REPRESENTATION_ITEM ( )  RATIONAL_B_SPLINE_CURVE ( ( 0.9330127018922194093, 0.9330127018922194093, 1.000000000000000000, 0.8660254037844387076, 1.000000000000000000, 0.8660254037844387076, 1.000000000000000000, 0.9330127018922194093, 0.9330127018922194093 ) ) 
 REPRESENTATION_ITEM ( '' )  );
#16551 = CARTESIAN_POINT ( 'NONE',  ( -2.229367062500000163, 23.52083333469892779, -3.861377020970580443 ) ) ;
#16552 = CARTESIAN_POINT ( 'NONE',  ( -51.60603307380591787, -149.9375000013656063, -2.891590998281053704 ) ) ;
#16553 = CARTESIAN_POINT ( 'NONE',  ( 1.975475456537005874E-15, -13.62499999726881228, 5.000000000000000000 ) ) ;
#16554 = CARTESIAN_POINT ( 'NONE',  ( 1.975475456537005874E-15, 5.249999999999999112, 5.000000000000000000 ) ) ;
#16555 = ORIENTED_EDGE ( 'NONE', *, *, #36817, .T. ) ;
#16556 = CARTESIAN_POINT ( 'NONE',  ( 4.458734124999998549, -72.72916666530107932, -2.574251347313721627 ) ) ;
#16557 = CARTESIAN_POINT ( 'NONE',  ( 1.339745962155615144, -28.58034179853029144, 4.999999999999999112 ) ) ;
#16558 = CARTESIAN_POINT ( 'NONE',  ( -4.458734124999999437, 10.60416666803225993, -2.574251347313719407 ) ) ;
#16559 = CARTESIAN_POINT ( 'NONE',  ( -2.480964764533239819E-13, -60.62499999726880873, 5.000000000000000000 ) ) ;
#16560 = EDGE_CURVE ( 'NONE', #42800, #53365, #62209, .T. ) ;
#16561 = CARTESIAN_POINT ( 'NONE',  ( -2.500000000000000444, -2.041666663935480575, -4.330127018922193649 ) ) ;
#16562 = EDGE_CURVE ( 'NONE', #19510, #42943, #33936, .T. ) ;
#16563 = CARTESIAN_POINT ( 'NONE',  ( 9.457646018065525792E-16, -56.31249999863440081, 5.148502694627439702 ) ) ;
#16564 = CARTESIAN_POINT ( 'NONE',  ( 5.000000000000000888, -13.45833333060214976, 2.886751345948126879 ) ) ;
#16565 = CARTESIAN_POINT ( 'NONE',  ( -1.339745962155613812, -20.08034179853029144, -5.000000000000000000 ) ) ;
#16566 = EDGE_CURVE ( 'NONE', #42874, #44687, #46991, .T. ) ;
#16567 = CARTESIAN_POINT ( 'NONE',  ( 1.975475456537005874E-15, 9.375000002731185944, 5.000000000000000000 ) ) ;
#16568 = CARTESIAN_POINT ( 'NONE',  ( 4.458734124999998549, -19.97916666530107221, -2.574251347313721627 ) ) ;
#16569 = ORIENTED_EDGE ( 'NONE', *, *, #3224, .F. ) ;
#16570 = LINE ( 'NONE', #41954, #58707 ) ;
#16571 = CARTESIAN_POINT ( 'NONE',  ( 4.458734124999998549, -102.7291666653010509, -2.574251347313721627 ) ) ;
#16572 = CARTESIAN_POINT ( 'NONE',  ( 3.061616997868383141E-16, -157.8750000027311842, -5.000000000000000000 ) ) ;
#16573 = ORIENTED_EDGE ( 'NONE', *, *, #49454, .T. ) ;
#16574 = CARTESIAN_POINT ( 'NONE',  ( -2.229367062500000163, -104.7291666653010651, -3.861377020970580443 ) ) ;
#16575 = AXIS2_PLACEMENT_3D ( 'NONE', #18345, #56014, #31558 ) ;
#16576 = CARTESIAN_POINT ( 'NONE',  ( -4.458734124999998549, -28.22916666530106866, 2.574251347313722516 ) ) ;
#16577 = CARTESIAN_POINT ( 'NONE',  ( 1.060575238724906964E-15, -64.62499999726881583, 5.773502691896257311 ) ) ;
#16578 = EDGE_CURVE ( 'NONE', #50806, #13144, #42325, .T. ) ;
#16579 = CARTESIAN_POINT ( 'NONE',  ( -55.35523342533222291, -150.5625000013656063, 4.444560631937231499 ) ) ;
#16580 = CARTESIAN_POINT ( 'NONE',  ( -57.19623071787016499, -144.3750000013656063, 4.297418129356382899 ) ) ;
#16581 = CARTESIAN_POINT ( 'NONE',  ( 2.229367062500001939, -20.97916666530107221, 3.861377020970579999 ) ) ;
#16582 = EDGE_CURVE ( 'NONE', #1775, #6968, #23668, .T. ) ;
#16583 = CARTESIAN_POINT ( 'NONE',  ( 4.458734125000000326, -66.14583333196773651, 2.574251347313718519 ) ) ;
#16584 = CARTESIAN_POINT ( 'NONE',  ( 9.457646018065525792E-16, -23.06249999863440792, 5.148502694627439702 ) ) ;
#16585 = CARTESIAN_POINT ( 'NONE',  ( -5.000000000000000000, -33.00000000000000000, 0.000000000000000000 ) ) ;
#16586 = CARTESIAN_POINT ( 'NONE',  ( -3.535533905932738641, -151.3750000000000000, 3.535533905932737309 ) ) ;
#16587 = CARTESIAN_POINT ( 'NONE',  ( -2.499999999999996447, -11.83333333333333393, 4.330127018922195425 ) ) ;
#16588 = CARTESIAN_POINT ( 'NONE',  ( -4.458734124999999437, -149.9375000013656063, -5.460374474430324690E-16 ) ) ;
#16589 = ORIENTED_EDGE ( 'NONE', *, *, #8040, .T. ) ;
#16590 = CARTESIAN_POINT ( 'NONE',  ( -4.458734124999999437, -50.56249999863440792, 0.000000000000000000 ) ) ;
#16591 = CARTESIAN_POINT ( 'NONE',  ( 6.972266317189433020E-16, 29.74999999999999645, -5.000000000000000000 ) ) ;
#16592 = CARTESIAN_POINT ( 'NONE',  ( -60.14911071818854538, -136.0625000000000000, 1.666127454062681146 ) ) ;
#16593 = EDGE_CURVE ( 'NONE', #39445, #4086, #8865, .T. ) ;
#16594 = CARTESIAN_POINT ( 'NONE',  ( -5.000000000000000000, 28.91666666666666430, -2.886751345948128211 ) ) ;
#16595 = CARTESIAN_POINT ( 'NONE',  ( -49.85088928181150436, -152.5625000000000284, -1.666127454062680480 ) ) ;
#16596 = CARTESIAN_POINT ( 'NONE',  ( -4.458734124999998549, 1.770833334698927786, 2.574251347313722516 ) ) ;
#16597 = LINE ( 'NONE', #2144, #4135 ) ;
#16598 = CARTESIAN_POINT ( 'NONE',  ( 5.000000000000000888, 13.41666666666666785, 2.886751345948126879 ) ) ;
#16599 = CARTESIAN_POINT ( 'NONE',  ( 5.000000000000000000, -17.50000000000000000, -6.123233995736766282E-16 ) ) ;
#16600 = CARTESIAN_POINT ( 'NONE',  ( 2.229367062499998831, 17.10416666803225993, -3.861377020970580887 ) ) ;
#16601 = CARTESIAN_POINT ( 'NONE',  ( -5.000000000000000000, 3.125000002731185944, 0.000000000000000000 ) ) ;
#16602 = ORIENTED_EDGE ( 'NONE', *, *, #2169, .F. ) ;
#16603 = DIRECTION ( 'NONE',  ( 7.709882115452476194E-16, 0.000000000000000000, -1.000000000000000000 ) ) ;
#16604 = ORIENTED_EDGE ( 'NONE', *, *, #46256, .T. ) ;
#16605 =( BOUNDED_CURVE ( )  B_SPLINE_CURVE ( 2, ( #21960, #51241, #7487, #6533, #60887, #21648, #27100, #30649, #50271 ),
 .UNSPECIFIED., .F., .F. ) 
 B_SPLINE_CURVE_WITH_KNOTS ( ( 3, 2, 2, 2, 3 ),
 ( 0.5187500000000000444, 0.5194444444444444864, 0.5208333333333333703, 0.5222222222222222543, 0.5229166666666666963 ),
 .UNSPECIFIED. ) 
 CURVE ( )  GEOMETRIC_REPRESENTATION_ITEM ( )  RATIONAL_B_SPLINE_CURVE ( ( 0.9330127018922194093, 0.9330127018922194093, 1.000000000000000000, 0.8660254037844387076, 1.000000000000000000, 0.8660254037844387076, 1.000000000000000000, 0.9330127018922194093, 0.9330127018922194093 ) ) 
 REPRESENTATION_ITEM ( '' )  );
#16606 = CARTESIAN_POINT ( 'NONE',  ( -2.229367062499996610, -46.14583333196774362, 3.861377020970582219 ) ) ;
#16607 = CARTESIAN_POINT ( 'NONE',  ( 4.458734124999999437, -164.6875000013655779, 0.000000000000000000 ) ) ;
#16608 = CARTESIAN_POINT ( 'NONE',  ( 5.000000000000000000, -46.37499999726880873, -6.123233995736766282E-16 ) ) ;
#16609 = ORIENTED_EDGE ( 'NONE', *, *, #24363, .F. ) ;
#16610 = CARTESIAN_POINT ( 'NONE',  ( -3.152548672688508926E-16, -18.56249999863440792, -5.148502694627439702 ) ) ;
#16611 = VERTEX_POINT ( 'NONE', #57458 ) ;
#16612 = CARTESIAN_POINT ( 'NONE',  ( 1.060575238724906964E-15, -87.75000000000000000, 5.773502691896257311 ) ) ;
#16613 = CARTESIAN_POINT ( 'NONE',  ( 1.846868145590735200, -164.2500000013656063, -4.458734125000000326 ) ) ;
#16615 = ORIENTED_EDGE ( 'NONE', *, *, #45680, .T. ) ;
#16614 = FACE_OUTER_BOUND ( 'NONE', #7997, .T. ) ;
#16616 = CARTESIAN_POINT ( 'NONE',  ( -59.81910112700025905, -141.1875000000000000, -2.462841084822630311 ) ) ;
#16617 = CARTESIAN_POINT ( 'NONE',  ( 2.229367062500001939, -33.22916666530106511, 3.861377020970579999 ) ) ;
#16618 = CARTESIAN_POINT ( 'NONE',  ( -2.499999999999996447, 23.29166666939785202, 4.330127018922195425 ) ) ;
#16619 = ORIENTED_EDGE ( 'NONE', *, *, #38648, .T. ) ;
#16620 = CARTESIAN_POINT ( 'NONE',  ( 9.457646018065525792E-16, -78.06249999863440792, 5.148502694627439702 ) ) ;
#16621 = CARTESIAN_POINT ( 'NONE',  ( -4.458734124999999437, 28.60416666803226349, -2.574251347313719407 ) ) ;
#16622 = CARTESIAN_POINT ( 'NONE',  ( -58.24261429053147765, -136.3750000027312126, -3.805975901505573855 ) ) ;
#16623 = ORIENTED_EDGE ( 'NONE', *, *, #62111, .F. ) ;
#16624 = CARTESIAN_POINT ( 'NONE',  ( -3.535533905932738641, -161.3750000000000284, 3.535533905932737309 ) ) ;
#16625 = CARTESIAN_POINT ( 'NONE',  ( -54.64476657466781973, -143.0625000013656063, -4.444560631937228834 ) ) ;
#16626 = VECTOR ( 'NONE', #10358, 1000.000000000000000 ) ;
#16627 = CARTESIAN_POINT ( 'NONE',  ( 4.458734124999998549, -80.97916666530106511, -2.574251347313721627 ) ) ;
#16628 = CARTESIAN_POINT ( 'NONE',  ( -59.98410592259440222, -134.2500000027312126, -0.3983568153799752487 ) ) ;
#16629 = CARTESIAN_POINT ( 'NONE',  ( 2.500000000000002220, 22.33333333333333215, 4.330127018922192761 ) ) ;
#16630 = CARTESIAN_POINT ( 'NONE',  ( 4.458734124999999437, -142.6875000013656063, 0.000000000000000000 ) ) ;
#16631 = FACE_OUTER_BOUND ( 'NONE', #24265, .T. ) ;
#16632 = CARTESIAN_POINT ( 'NONE',  ( -4.458734124999997661, -51.22916666530107932, 2.574251347313722516 ) ) ;
#16633 = CARTESIAN_POINT ( 'NONE',  ( -4.458734124999997661, -46.22916666530106511, 2.574251347313722516 ) ) ;
#16634 = CARTESIAN_POINT ( 'NONE',  ( 2.229367062499998831, 28.35416666803225993, -3.861377020970580887 ) ) ;
#16635 = CARTESIAN_POINT ( 'NONE',  ( 1.060575238724906964E-15, -107.7499999999999858, 5.773502691896257311 ) ) ;
#16636 = FACE_OUTER_BOUND ( 'NONE', #55952, .T. ) ;
#16637 = ADVANCED_FACE ( 'NONE', ( #29093 ), #43265, .T. ) ;
#16638 = CARTESIAN_POINT ( 'NONE',  ( -4.458734124999998549, -41.47916666530107221, 2.574251347313722516 ) ) ;
#16639 = CARTESIAN_POINT ( 'NONE',  ( -2.499999999999996447, 3.291666669397851575, 4.330127018922195425 ) ) ;
#16640 = CARTESIAN_POINT ( 'NONE',  ( 2.499999999999998668, 16.79166666939785202, -4.330127018922193649 ) ) ;
#16641 = CARTESIAN_POINT ( 'NONE',  ( -59.44456063193725015, -130.5625000013656063, -0.3552334253322034230 ) ) ;
#16642 = CARTESIAN_POINT ( 'NONE',  ( -3.152548672688508926E-16, -80.81249999863440792, -5.148502694627439702 ) ) ;
#16643 = CARTESIAN_POINT ( 'NONE',  ( 1.339745962155615144, -34.70534180126148271, 4.999999999999999112 ) ) ;
#16644 = CARTESIAN_POINT ( 'NONE',  ( -2.229367062500000163, -97.47916666530105090, -3.861377020970580443 ) ) ;
#16645 = CARTESIAN_POINT ( 'NONE',  ( -4.458734124999997661, -2.479166665301069106, 2.574251347313722516 ) ) ;
#16646 = ORIENTED_EDGE ( 'NONE', *, *, #46409, .F. ) ;
#16647 = CARTESIAN_POINT ( 'NONE',  ( -49.85088928181150436, -139.5624999999999716, -1.666127454062680480 ) ) ;
#16648 = CARTESIAN_POINT ( 'NONE',  ( -5.000000000000000000, -14.87499999726881228, 0.000000000000000000 ) ) ;
#16649 = CARTESIAN_POINT ( 'NONE',  ( 2.229367062499998831, -88.64583333196773651, -3.861377020970580887 ) ) ;
#16650 = CYLINDRICAL_SURFACE ( 'NONE', #62365, 5.000000000000000000 ) ;
#16651 = CARTESIAN_POINT ( 'NONE',  ( -4.458734124999999437, -85.56249999863439371, 0.000000000000000000 ) ) ;
#16652 = CARTESIAN_POINT ( 'NONE',  ( -2.229367062500000163, 11.27083333469892601, -3.861377020970580443 ) ) ;
#16653 = CARTESIAN_POINT ( 'NONE',  ( -6.972266317189433020E-16, -39.25000000000000000, -5.000000000000000000 ) ) ;
#16654 = CARTESIAN_POINT ( 'NONE',  ( -57.89159099828107458, -135.6875000013656063, -3.393966926194107447 ) ) ;
#16655 = CARTESIAN_POINT ( 'NONE',  ( -4.458734124999999437, -5.395833331967740953, -2.574251347313719407 ) ) ;
#16656 = CARTESIAN_POINT ( 'NONE',  ( -4.458734124999999437, 15.35416666803225993, -2.574251347313719407 ) ) ;
#16657 = CARTESIAN_POINT ( 'NONE',  ( -3.152548672688508926E-16, -45.81249999863440081, -5.148502694627439702 ) ) ;
#16658 = CARTESIAN_POINT ( 'NONE',  ( 1.975475456537005874E-15, -38.62499999726880873, 5.000000000000000000 ) ) ;
#16659 = CARTESIAN_POINT ( 'NONE',  ( 4.458734124999998549, -84.72916666530106511, -2.574251347313721627 ) ) ;
#16660 = CARTESIAN_POINT ( 'NONE',  ( -2.229367062500000163, -2.479166665301069106, -3.861377020970580443 ) ) ;
#16661 = FILL_AREA_STYLE_COLOUR ( '', #62723 ) ;
#16662 = ADVANCED_FACE ( 'NONE', ( #27847 ), #38749, .T. ) ;
#16663 = ORIENTED_EDGE ( 'NONE', *, *, #2696, .F. ) ;
#16664 = EDGE_CURVE ( 'NONE', #15620, #63145, #24807, .T. ) ;
#16665 = CARTESIAN_POINT ( 'NONE',  ( 2.229367062499998831, -32.89583333196773651, -3.861377020970580887 ) ) ;
#16666 = CARTESIAN_POINT ( 'NONE',  ( -57.19623071787017210, -132.6250000013656347, 4.297418129356382899 ) ) ;
#16667 = EDGE_CURVE ( 'NONE', #53830, #52296, #51506, .T. ) ;
#16668 = CARTESIAN_POINT ( 'NONE',  ( 2.229367062499998831, -72.64583333196773651, -3.861377020970580887 ) ) ;
#16669 = CARTESIAN_POINT ( 'NONE',  ( 4.458734124999998549, 28.02083333469892779, -2.574251347313721627 ) ) ;
#16670 = CARTESIAN_POINT ( 'NONE',  ( -2.229367062499996610, 18.85416666803225993, 3.861377020970582219 ) ) ;
#16671 = EDGE_CURVE ( 'NONE', #14946, #13464, #14090, .T. ) ;
#16672 = CARTESIAN_POINT ( 'NONE',  ( -5.000000000000000000, -57.95833333060216574, -2.886751345948128211 ) ) ;
#16673 = CARTESIAN_POINT ( 'NONE',  ( -5.000000000000000888, -145.5625000027311842, 2.071067811865474617 ) ) ;
#16674 = CARTESIAN_POINT ( 'NONE',  ( -3.152548672688508926E-16, -78.81249999863442213, -5.148502694627439702 ) ) ;
#16675 = CARTESIAN_POINT ( 'NONE',  ( 2.499999999999998668, -66.33333333333332860, -4.330127018922193649 ) ) ;
#16676 = CARTESIAN_POINT ( 'NONE',  ( -4.999999999999998224, -74.91666666666665719, 2.886751345948131764 ) ) ;
#16677 = CARTESIAN_POINT ( 'NONE',  ( -5.000000000000000000, 18.04166666939785557, -2.886751345948128211 ) ) ;
#16678 = ORIENTED_EDGE ( 'NONE', *, *, #49262, .F. ) ;
#16679 = CARTESIAN_POINT ( 'NONE',  ( -2.499999999999996447, -56.83333333333333570, 4.330127018922195425 ) ) ;
#16680 = CARTESIAN_POINT ( 'NONE',  ( -5.000000000000000000, -168.6250000027312126, -6.123233995736766282E-16 ) ) ;
#16682 = CARTESIAN_POINT ( 'NONE',  ( -2.500000000000000444, -23.16666666666666785, -4.330127018922193649 ) ) ;
#16681 = CARTESIAN_POINT ( 'NONE',  ( 0.000000000000000000, -120.0000000000000000, 5.000000000000000000 ) ) ;
#16683 = CARTESIAN_POINT ( 'NONE',  ( 2.229367062499998831, -29.64583333196773296, -3.861377020970580887 ) ) ;
#16684 = APPLICATION_CONTEXT ( 'automotive_design' ) ;
#16685 = CARTESIAN_POINT ( 'NONE',  ( 1.339745962155612702, -62.29465819873851729, -5.000000000000000000 ) ) ;
#16686 =( BOUNDED_CURVE ( )  B_SPLINE_CURVE ( 2, ( #53312, #9246, #28860, #15343, #10828, #29799, #5375, #53937, #59734 ),
 .UNSPECIFIED., .F., .F. ) 
 B_SPLINE_CURVE_WITH_KNOTS ( ( 3, 2, 2, 2, 3 ),
 ( 0.5145833333333332815, 0.5152777777777777235, 0.5166666666666667185, 0.5180555555555556024, 0.5187500000000000444 ),
 .UNSPECIFIED. ) 
 CURVE ( )  GEOMETRIC_REPRESENTATION_ITEM ( )  RATIONAL_B_SPLINE_CURVE ( ( 0.9330127018922194093, 0.9330127018922194093, 1.000000000000000000, 0.8660254037844387076, 1.000000000000000000, 0.8660254037844387076, 1.000000000000000000, 0.9330127018922194093, 0.9330127018922194093 ) ) 
 REPRESENTATION_ITEM ( '' )  );
#16687 = CARTESIAN_POINT ( 'NONE',  ( 1.060575238724906964E-15, -25.62499999726881583, 5.773502691896257311 ) ) ;
#16689 = VERTEX_POINT ( 'NONE', #63533 ) ;
#16688 = CARTESIAN_POINT ( 'NONE',  ( -4.458734124999999437, -57.31249999863440081, 0.000000000000000000 ) ) ;
#16690 = DIRECTION ( 'NONE',  ( -0.000000000000000000, 1.000000000000000000, -0.000000000000000000 ) ) ;
#16691 = CARTESIAN_POINT ( 'NONE',  ( 6.123233995736766282E-16, -170.0000000000000000, -5.000000000000000000 ) ) ;
#16693 = EDGE_LOOP ( 'NONE', ( #39071, #62638, #27848, #35700 ) ) ;
#16692 = CARTESIAN_POINT ( 'NONE',  ( 2.229367062500001939, -3.229166665301069550, 3.861377020970579999 ) ) ;
#16694 = CARTESIAN_POINT ( 'NONE',  ( 2.499999999999998668, -72.33333333333332860, -4.330127018922193649 ) ) ;
#16695 = CARTESIAN_POINT ( 'NONE',  ( -56.48576386720575471, -140.7500000013655779, -4.591703134518078322 ) ) ;
#16696 = CARTESIAN_POINT ( 'NONE',  ( -2.229367062500000163, -47.72916666530106511, -3.861377020970580443 ) ) ;
#16697 = DIRECTION ( 'NONE',  ( -0.000000000000000000, 1.000000000000000000, -0.000000000000000000 ) ) ;
#16698 = CARTESIAN_POINT ( 'NONE',  ( 5.000000000000000000, -159.0625000000000284, 2.071067811865478614 ) ) ;
#16699 = CARTESIAN_POINT ( 'NONE',  ( -5.000000000000000000, -72.87499999726880162, 0.000000000000000000 ) ) ;
#16700 = CARTESIAN_POINT ( 'NONE',  ( 2.499999999999998668, -10.20833333060214621, -4.330127018922193649 ) ) ;
#16701 = CARTESIAN_POINT ( 'NONE',  ( -58.24261429053147765, -153.2500000000000284, -3.805975901505573855 ) ) ;
#16702 = CARTESIAN_POINT ( 'NONE',  ( -3.152548672688508926E-16, -17.81249999863440792, -5.148502694627439702 ) ) ;
#16703 = CARTESIAN_POINT ( 'NONE',  ( 4.458734124999999437, -53.06249999863440792, -5.460374474430324690E-16 ) ) ;
#16704 =( BOUNDED_CURVE ( )  B_SPLINE_CURVE ( 2, ( #45077, #6807, #29955, #21601, #60526, #1044, #1673, #54737, #16766 ),
 .UNSPECIFIED., .F., .F. ) 
 B_SPLINE_CURVE_WITH_KNOTS ( ( 3, 2, 2, 2, 3 ),
 ( 0.6053571428571428159, 0.6059523809523809090, 0.6071428571428570953, 0.6083333333333332815, 0.6089285714285714857 ),
 .UNSPECIFIED. ) 
 CURVE ( )  GEOMETRIC_REPRESENTATION_ITEM ( )  RATIONAL_B_SPLINE_CURVE ( ( 0.9330127018922194093, 0.9330127018922194093, 1.000000000000000000, 0.8660254037844387076, 1.000000000000000000, 0.8660254037844387076, 1.000000000000000000, 0.9330127018922130810, 0.9330127018922194093 ) ) 
 REPRESENTATION_ITEM ( '' )  );
#16705 = CARTESIAN_POINT ( 'NONE',  ( 5.000000000000000000, 10.49999999999999822, -6.123233995736766282E-16 ) ) ;
#16706 = SURFACE_STYLE_FILL_AREA ( #7381 ) ;
#16707 = CARTESIAN_POINT ( 'NONE',  ( 3.152801135295366208, -142.5625000013655779, 3.152801135295367985 ) ) ;
#16708 = CARTESIAN_POINT ( 'NONE',  ( 2.229367062500001939, -92.22916666530106511, 3.861377020970579999 ) ) ;
#16709 = CARTESIAN_POINT ( 'NONE',  ( 1.339745962155612702, -8.169658196007333117, -5.000000000000000000 ) ) ;
#16710 = ORIENTED_EDGE ( 'NONE', *, *, #52376, .T. ) ;
#16711 = CARTESIAN_POINT ( 'NONE',  ( -4.458734124999999437, 24.43750000136559208, 0.000000000000000000 ) ) ;
#16712 = CARTESIAN_POINT ( 'NONE',  ( -51.75738570946856498, -145.8750000027312126, 3.805975901505576964 ) ) ;
#16713 = CARTESIAN_POINT ( 'NONE',  ( 0.000000000000000000, -120.0000000000000000, 0.000000000000000000 ) ) ;
#16714 = CARTESIAN_POINT ( 'NONE',  ( 2.229367062500001939, -3.979166665301070438, 3.861377020970579999 ) ) ;
#16715 = EDGE_CURVE ( 'NONE', #54593, #2442, #34239, .T. ) ;
#16716 = CARTESIAN_POINT ( 'NONE',  ( -8.190561711645485556E-16, -148.9375000013656063, 4.458734124999999437 ) ) ;
#16717 = CARTESIAN_POINT ( 'NONE',  ( -4.458734124999998549, -24.47916666530107577, 2.574251347313722516 ) ) ;
#16718 = CARTESIAN_POINT ( 'NONE',  ( -4.458734124999998549, -65.47916666530107932, 2.574251347313722516 ) ) ;
#16719 = CARTESIAN_POINT ( 'NONE',  ( -6.972266317189433020E-16, -70.25000000000000000, -5.000000000000000000 ) ) ;
#16720 = CARTESIAN_POINT ( 'NONE',  ( -4.458734124999999437, -7.312499998634404363, 0.000000000000000000 ) ) ;
#16721 = CARTESIAN_POINT ( 'NONE',  ( 6.439685834477092641, -4.942299687812566233, -7.659344964963564983 ) ) ;
#16722 = CARTESIAN_POINT ( 'NONE',  ( 3.152801135295367541, -146.3125000013655779, -3.152801135295367541 ) ) ;
#16723 = CARTESIAN_POINT ( 'NONE',  ( 2.229367062500001939, 15.77083333469892601, 3.861377020970579999 ) ) ;
#16724 = ORIENTED_EDGE ( 'NONE', *, *, #51239, .T. ) ;
#16725 = CARTESIAN_POINT ( 'NONE',  ( -2.500000000000000444, -63.04166666393547303, -4.330127018922193649 ) ) ;
#16726 = CARTESIAN_POINT ( 'NONE',  ( -1.339745962155610925, -20.79465819873852084, 5.000000000000000000 ) ) ;
#16728 = CARTESIAN_POINT ( 'NONE',  ( 4.458734125000001214, -16.89583333196773651, 2.574251347313718519 ) ) ;
#16727 = CARTESIAN_POINT ( 'NONE',  ( 1.060575238724906964E-15, -85.74999999999998579, 5.773502691896257311 ) ) ;
#16729 = LINE ( 'NONE', #56616, #3693 ) ;
#16730 = CARTESIAN_POINT ( 'NONE',  ( -60.14911071818854538, -138.0625000000000000, 1.666127454062681146 ) ) ;
#16731 = CARTESIAN_POINT ( 'NONE',  ( -54.64476657466781973, -146.8125000013656063, -4.444560631937228834 ) ) ;
#16732 = CARTESIAN_POINT ( 'NONE',  ( 1.060575238724906964E-15, -47.62499999726881583, 5.773502691896257311 ) ) ;
#16733 = CARTESIAN_POINT ( 'NONE',  ( -58.24261429053147765, -148.2500000000000284, -3.805975901505573855 ) ) ;
#16734 = CARTESIAN_POINT ( 'NONE',  ( 2.229367062499998831, 9.354166668032261711, -3.861377020970580887 ) ) ;
#16735 = CYLINDRICAL_SURFACE ( 'NONE', #24278, 5.000000000000000000 ) ;
#16736 = CARTESIAN_POINT ( 'NONE',  ( 2.499999999999998668, -60.20833333060214443, -4.330127018922193649 ) ) ;
#16737 = CARTESIAN_POINT ( 'NONE',  ( 2.229367062499998831, 14.35416666803226171, -3.861377020970580887 ) ) ;
#16738 = CARTESIAN_POINT ( 'NONE',  ( 4.458734124999998549, -67.72916666530107932, -2.574251347313721627 ) ) ;
#16739 = CARTESIAN_POINT ( 'NONE',  ( 4.458734125000000326, -13.14583333196774184, 2.574251347313718519 ) ) ;
#16740 = CARTESIAN_POINT ( 'NONE',  ( -5.000000000000000000, 0.9166666666666664076, -2.886751345948128211 ) ) ;
#16741 = CARTESIAN_POINT ( 'NONE',  ( -1.846868145590734756, -165.1250000013656063, -4.458734125000000326 ) ) ;
#16742 = CARTESIAN_POINT ( 'NONE',  ( 1.975475456537005874E-15, -2.750000000000000888, 5.000000000000000000 ) ) ;
#16743 = CARTESIAN_POINT ( 'NONE',  ( 4.458734124999998549, -58.72916666530106511, -2.574251347313721627 ) ) ;
#16744 = CARTESIAN_POINT ( 'NONE',  ( -3.535250795749689387E-16, -92.12499999726880162, -5.773502691896257311 ) ) ;
#16745 = DIRECTION ( 'NONE',  ( 0.000000000000000000, 0.000000000000000000, 1.000000000000000000 ) ) ;
#16746 = CARTESIAN_POINT ( 'NONE',  ( 3.535533905932736864, -139.2500000027311842, 3.535533905932738641 ) ) ;
#16747 = CARTESIAN_POINT ( 'NONE',  ( 4.458734125000000326, -35.89583333196773651, 2.574251347313718519 ) ) ;
#16748 = CARTESIAN_POINT ( 'NONE',  ( 2.499999999999998668, -51.20833333060213732, -4.330127018922193649 ) ) ;
#16749 = CARTESIAN_POINT ( 'NONE',  ( 5.000000000000000888, -46.58333333333334991, 2.886751345948126879 ) ) ;
#16750 = CARTESIAN_POINT ( 'NONE',  ( -4.999999999999998224, 19.08333333333333570, 2.886751345948131764 ) ) ;
#16751 = CARTESIAN_POINT ( 'NONE',  ( 0.000000000000000000, -120.0000000000000000, 0.000000000000000000 ) ) ;
#16752 = EDGE_LOOP ( 'NONE', ( #46278, #23428, #35696, #51316 ) ) ;
#16753 = CARTESIAN_POINT ( 'NONE',  ( 9.457646018065525792E-16, -105.0624999986344079, 5.148502694627439702 ) ) ;
#16754 = CARTESIAN_POINT ( 'NONE',  ( 4.458734125000001214, -0.1458333319677394824, 2.574251347313718519 ) ) ;
#16755 =( BOUNDED_CURVE ( )  B_SPLINE_CURVE ( 2, ( #51017, #44586, #35586, #1508, #54569, #10816, #30428, #59720, #36221 ),
 .UNSPECIFIED., .F., .F. ) 
 B_SPLINE_CURVE_WITH_KNOTS ( ( 3, 2, 2, 2, 3 ),
 ( 0.7803571428571428603, 0.7809523809523809534, 0.7821428571428571397, 0.7833333333333333259, 0.7839285714285714191 ),
 .UNSPECIFIED. ) 
 CURVE ( )  GEOMETRIC_REPRESENTATION_ITEM ( )  RATIONAL_B_SPLINE_CURVE ( ( 0.9330127018922194093, 0.9330127018922194093, 1.000000000000000000, 0.8660254037844387076, 1.000000000000000000, 0.8660254037844387076, 1.000000000000000000, 0.9330127018922194093, 0.9330127018922194093 ) ) 
 REPRESENTATION_ITEM ( '' )  );
#16756 = CARTESIAN_POINT ( 'NONE',  ( 5.000000000000000000, -89.37499999726880162, -6.123233995736766282E-16 ) ) ;
#16757 = CARTESIAN_POINT ( 'NONE',  ( 5.000000000000000888, -9.583333333333333925, 2.886751345948126879 ) ) ;
#16758 = CARTESIAN_POINT ( 'NONE',  ( 4.458734125000000326, -71.89583333196773651, 2.574251347313718519 ) ) ;
#16759 = CARTESIAN_POINT ( 'NONE',  ( -6.972266317189433020E-16, -22.12499999726881228, -5.000000000000000000 ) ) ;
#16760 = CARTESIAN_POINT ( 'NONE',  ( -2.500000000000000444, -10.04166666393547658, -4.330127018922193649 ) ) ;
#16762 = VERTEX_POINT ( 'NONE', #50567 ) ;
#16761 = CARTESIAN_POINT ( 'NONE',  ( 4.458734125000001214, -36.89583333196773651, 2.574251347313718519 ) ) ;
#16763 = DIRECTION ( 'NONE',  ( -0.000000000000000000, 1.000000000000000000, -0.000000000000000000 ) ) ;
#16765 = ORIENTED_EDGE ( 'NONE', *, *, #21624, .F. ) ;
#16764 = CARTESIAN_POINT ( 'NONE',  ( 4.458734124999998549, 12.02083333469892601, -2.574251347313721627 ) ) ;
#16766 = CARTESIAN_POINT ( 'NONE',  ( 2.493747252781420335E-13, -56.12499999726880873, -5.000000000000000000 ) ) ;
#16767 = CARTESIAN_POINT ( 'NONE',  ( 5.000000000000000000, -56.41666666666666430, -2.886751345948129988 ) ) ;
#16768 = CARTESIAN_POINT ( 'NONE',  ( 4.458734125000001214, -31.14583333196773651, 2.574251347313718519 ) ) ;
#16769 = CARTESIAN_POINT ( 'NONE',  ( 1.339745962155612702, -10.29465819873852084, -5.000000000000000000 ) ) ;
#16770 = CARTESIAN_POINT ( 'NONE',  ( 4.458734124999998549, -73.72916666530106511, -2.574251347313721627 ) ) ;
#16771 = CARTESIAN_POINT ( 'NONE',  ( -2.071067811865475061, -168.6875000000000568, -5.000000000000000888 ) ) ;
#16773 = EDGE_CURVE ( 'NONE', #16917, #34735, #1363, .T. ) ;
#16772 = CARTESIAN_POINT ( 'NONE',  ( -2.229367062499996610, -88.14583333196773651, 3.861377020970582219 ) ) ;
#16774 = CARTESIAN_POINT ( 'NONE',  ( -58.39396692619412477, -135.6875000013656063, 2.891590998281057701 ) ) ;
#16775 = CARTESIAN_POINT ( 'NONE',  ( 4.458734124999999437, -34.06249999863440792, -5.460374474430324690E-16 ) ) ;
#16776 = CARTESIAN_POINT ( 'NONE',  ( 5.000000000000000888, -70.45833333060214443, 2.886751345948126879 ) ) ;
#16777 = ORIENTED_EDGE ( 'NONE', *, *, #57115, .F. ) ;
#16778 = CARTESIAN_POINT ( 'NONE',  ( 4.458734124999999437, -79.06249999863440792, -5.460374474430324690E-16 ) ) ;
#16779 = CARTESIAN_POINT ( 'NONE',  ( -6.972266317189433020E-16, 3.749999999999999556, -5.000000000000000000 ) ) ;
#16780 = ORIENTED_EDGE ( 'NONE', *, *, #59026, .T. ) ;
#16781 = CARTESIAN_POINT ( 'NONE',  ( -5.000000000000000000, -3.958333330602147537, -2.886751345948128211 ) ) ;
#16782 =( BOUNDED_CURVE ( )  B_SPLINE_CURVE ( 2, ( #42302, #52283, #47448, #56484, #3400, #23016, #32976, #37805, #27200 ),
 .UNSPECIFIED., .F., .F. ) 
 B_SPLINE_CURVE_WITH_KNOTS ( ( 3, 2, 2, 2, 3 ),
 ( 0.1750000000000001554, 0.1791666666666668351, 0.1833333333333334869, 0.1875000000000001665, 0.1916666666666668462 ),
 .UNSPECIFIED. ) 
 CURVE ( )  GEOMETRIC_REPRESENTATION_ITEM ( )  RATIONAL_B_SPLINE_CURVE ( ( 0.9999999999999970024, 0.9238795325112897361, 1.000000000000000000, 0.9238795325112867385, 1.000000000000000000, 0.9238795325112867385, 1.000000000000000000, 0.9238795325112837409, 1.000000000000003109 ) ) 
 REPRESENTATION_ITEM ( '' )  );
#16783 = DIRECTION ( 'NONE',  ( -0.000000000000000000, 1.000000000000000000, -0.000000000000000000 ) ) ;
#16784 = CARTESIAN_POINT ( 'NONE',  ( 4.458734124999998549, -61.97916666530106511, -2.574251347313721627 ) ) ;
#16785 = CARTESIAN_POINT ( 'NONE',  ( -3.152548672688508926E-16, -11.81249999863440969, -5.148502694627439702 ) ) ;
#16786 = ORIENTED_EDGE ( 'NONE', *, *, #25113, .T. ) ;
#16787 = CARTESIAN_POINT ( 'NONE',  ( -2.500000000000000444, -85.16666666666667140, -4.330127018922193649 ) ) ;
#16788 = CARTESIAN_POINT ( 'NONE',  ( -5.000000000000000000, -92.87499999726881583, 0.000000000000000000 ) ) ;
#16789 = VERTEX_POINT ( 'NONE', #6829 ) ;
#16790 = CARTESIAN_POINT ( 'NONE',  ( 4.458734124999999437, -8.062499998634404363, -5.460374474430324690E-16 ) ) ;
#16791 = CARTESIAN_POINT ( 'NONE',  ( 1.975475456537005874E-15, -32.62499999726880873, 5.000000000000000000 ) ) ;
#16792 = CARTESIAN_POINT ( 'NONE',  ( -4.458734124999999437, 7.687500001365594748, 0.000000000000000000 ) ) ;
#16793 = CARTESIAN_POINT ( 'NONE',  ( -1.339745962155613812, -76.20534180126146850, -5.000000000000000000 ) ) ;
#16794 = CARTESIAN_POINT ( 'NONE',  ( 3.152801135295366208, -157.5625000013656063, 3.152801135295367985 ) ) ;
#16795 = DIRECTION ( 'NONE',  ( 0.000000000000000000, 0.000000000000000000, 1.000000000000000000 ) ) ;
#16796 = ORIENTED_EDGE ( 'NONE', *, *, #45704, .F. ) ;
#16797 = CARTESIAN_POINT ( 'NONE',  ( 4.458734124999999437, -87.81249999863439371, -5.460374474430324690E-16 ) ) ;
#16798 = CARTESIAN_POINT ( 'NONE',  ( 1.339745962155615144, -29.58034179853029499, 4.999999999999999112 ) ) ;
#16799 = CARTESIAN_POINT ( 'NONE',  ( -3.152548672688508926E-16, -3.562499998634408360, -5.148502694627439702 ) ) ;
#16800 = CARTESIAN_POINT ( 'NONE',  ( 1.975475456537005874E-15, -71.62499999726878741, 5.000000000000000000 ) ) ;
#16801 = CARTESIAN_POINT ( 'NONE',  ( 2.500000000000002220, -32.54166666393547303, 4.330127018922192761 ) ) ;
#16802 = CYLINDRICAL_SURFACE ( 'NONE', #35525, 5.000000000000000000 ) ;
#16803 = CARTESIAN_POINT ( 'NONE',  ( -4.458734124999999437, 22.68750000136559564, 0.000000000000000000 ) ) ;
#16804 = CARTESIAN_POINT ( 'NONE',  ( -6.972266317189433020E-16, -104.2500000000000000, -5.000000000000000000 ) ) ;
#16805 = CARTESIAN_POINT ( 'NONE',  ( 2.229367062499998831, 29.35416666803225993, -3.861377020970580887 ) ) ;
#16806 = CARTESIAN_POINT ( 'NONE',  ( -4.458734124999999437, -53.31249999863439371, 0.000000000000000000 ) ) ;
#16807 = CARTESIAN_POINT ( 'NONE',  ( -2.229367062500000163, -35.72916666530107221, -3.861377020970580443 ) ) ;
#16808 = CARTESIAN_POINT ( 'NONE',  ( 2.229367062500001939, 0.7708333346989268975, 3.861377020970579999 ) ) ;
#16809 = CARTESIAN_POINT ( 'NONE',  ( 5.000000000000000000, 16.58333333333333215, -2.886751345948129988 ) ) ;
#16810 = CARTESIAN_POINT ( 'NONE',  ( -2.071067811865478170, -145.4375000027312694, 5.000000000000000000 ) ) ;
#16811 = CARTESIAN_POINT ( 'NONE',  ( 6.123233995736766282E-16, -120.0000000000000000, -5.000000000000000000 ) ) ;
#16812 = CARTESIAN_POINT ( 'NONE',  ( -4.458734124999999437, -41.39583333196773651, -2.574251347313719407 ) ) ;
#16813 = CARTESIAN_POINT ( 'NONE',  ( 2.499999999999998668, -78.20833333060214443, -4.330127018922193649 ) ) ;
#16814 = CARTESIAN_POINT ( 'NONE',  ( -59.44456063193725015, -141.8125000013656063, -0.3552334253322034230 ) ) ;
#16815 = VECTOR ( 'NONE', #41849, 1000.000000000000000 ) ;
#16816 = LINE ( 'NONE', #42206, #14397 ) ;
#16817 = CARTESIAN_POINT ( 'NONE',  ( 1.975475456537005874E-15, 18.24999999999999645, 5.000000000000000000 ) ) ;
#16818 = CARTESIAN_POINT ( 'NONE',  ( 4.458734125000000326, -87.14583333196773651, 2.574251347313718519 ) ) ;
#16819 = CARTESIAN_POINT ( 'NONE',  ( -4.458734125000000326, -160.1250000013655779, 1.846868145590734089 ) ) ;
#16820 = CARTESIAN_POINT ( 'NONE',  ( -3.080866544137490504, -6.881514909249304424, -7.026396753507435200 ) ) ;
#16821 = CARTESIAN_POINT ( 'NONE',  ( -5.000000000000000000, -32.08333333333333570, -2.886751345948128211 ) ) ;
#16822 = CARTESIAN_POINT ( 'NONE',  ( -4.458734124999999437, -140.9375000013656063, -5.460374474430324690E-16 ) ) ;
#16823 = EDGE_LOOP ( 'NONE', ( #11669, #60691, #35652, #30820, #5625, #44534, #19387, #10988, #9005, #25928, #25901, #18274 ) ) ;
#16824 = CARTESIAN_POINT ( 'NONE',  ( -4.458734124999998549, 21.52083333469893134, 2.574251347313722516 ) ) ;
#16825 = ORIENTED_EDGE ( 'NONE', *, *, #33478, .T. ) ;
#16826 = CARTESIAN_POINT ( 'NONE',  ( 2.229367062500001939, -92.97916666530106511, 3.861377020970579999 ) ) ;
#16827 = CARTESIAN_POINT ( 'NONE',  ( 9.457646018065525792E-16, 14.68750000136559208, 5.148502694627439702 ) ) ;
#16828 = CARTESIAN_POINT ( 'NONE',  ( -2.499999999999996447, 15.29166666939785202, 4.330127018922195425 ) ) ;
#16829 = CARTESIAN_POINT ( 'NONE',  ( -1.339745962155610925, -34.66965819600733312, 5.000000000000000000 ) ) ;
#16830 = CARTESIAN_POINT ( 'NONE',  ( -3.535250795749689387E-16, 10.74999999999999822, -5.773502691896257311 ) ) ;
#16831 = CARTESIAN_POINT ( 'NONE',  ( 9.457646018065525792E-16, -55.06249999863440081, 5.148502694627439702 ) ) ;
#16832 = CARTESIAN_POINT ( 'NONE',  ( 4.458734125000001214, -12.89583333196774184, 2.574251347313718519 ) ) ;
#16833 = CARTESIAN_POINT ( 'NONE',  ( 7.500000000000000000, 1.572594658376109011, -7.069792055233639516 ) ) ;
#16834 = CARTESIAN_POINT ( 'NONE',  ( -55.35523342533222291, -136.5625000013656063, 4.444560631937231499 ) ) ;
#16835 = CARTESIAN_POINT ( 'NONE',  ( -2.499999999999996447, -63.70833333060215153, 4.330127018922195425 ) ) ;
#16836 = CARTESIAN_POINT ( 'NONE',  ( 5.000000000000000000, -33.29166666393547303, -2.886751345948130876 ) ) ;
#16837 = CARTESIAN_POINT ( 'NONE',  ( -5.000000000000000000, -74.87499999726880162, 0.000000000000000000 ) ) ;
#16838 = CARTESIAN_POINT ( 'NONE',  ( -3.535250795749689387E-16, -38.24999999999999289, -5.773502691896257311 ) ) ;
#16839 = CARTESIAN_POINT ( 'NONE',  ( -1.339745962155610925, 13.33034180399266688, 5.000000000000000000 ) ) ;
#16840 = CARTESIAN_POINT ( 'NONE',  ( 4.458734124999999437, -16.06249999863440436, -5.460374474430324690E-16 ) ) ;
#16841 = CARTESIAN_POINT ( 'NONE',  ( -7.640563834021360018E-16, -9.147862274876560562, -8.047472243342937759 ) ) ;
#16842 = CARTESIAN_POINT ( 'NONE',  ( 4.458734124999999437, -61.81249999863440081, -5.460374474430324690E-16 ) ) ;
#16843 = CARTESIAN_POINT ( 'NONE',  ( 3.152801135295367541, -153.5625000013656063, -3.152801135295367541 ) ) ;
#16845 = ADVANCED_FACE ( 'NONE', ( #59014 ), #21621, .F. ) ;
#16844 = CARTESIAN_POINT ( 'NONE',  ( 2.229367062499998831, -72.64583333196773651, -3.861377020970580887 ) ) ;
#16846 = CARTESIAN_POINT ( 'NONE',  ( -59.59170313451811296, -147.7500000013655779, 1.485763867205729394 ) ) ;
#16847 = CARTESIAN_POINT ( 'NONE',  ( 9.457646018065525792E-16, -17.31249999863440436, 5.148502694627439702 ) ) ;
#16848 = CARTESIAN_POINT ( 'NONE',  ( 1.060575238724906964E-15, -60.62499999726880873, 5.773502691896257311 ) ) ;
#16849 = ORIENTED_EDGE ( 'NONE', *, *, #23213, .F. ) ;
#16850 = DIRECTION ( 'NONE',  ( -0.000000000000000000, 1.000000000000000000, -0.000000000000000000 ) ) ;
#16851 = ORIENTED_EDGE ( 'NONE', *, *, #12931, .F. ) ;
#16852 = CARTESIAN_POINT ( 'NONE',  ( 9.457646018065525792E-16, -63.31249999863440081, 5.148502694627439702 ) ) ;
#16853 = CARTESIAN_POINT ( 'NONE',  ( -59.98410592259440222, -149.2500000027312126, -0.3983568153799752487 ) ) ;
#16854 = CARTESIAN_POINT ( 'NONE',  ( 3.152801135295366208, -150.5625000013655779, 3.152801135295367985 ) ) ;
#16855 = EDGE_LOOP ( 'NONE', ( #63589, #21899, #55408, #54991 ) ) ;
#16856 = CARTESIAN_POINT ( 'NONE',  ( -6.972266317189433020E-16, -12.12499999726881583, -5.000000000000000000 ) ) ;
#16857 = CARTESIAN_POINT ( 'NONE',  ( 0.000000000000000000, -120.0000000000000000, 0.000000000000000000 ) ) ;
#16858 = CARTESIAN_POINT ( 'NONE',  ( -6.324555320336756381, 0.000000000000000000, -9.000000000000001776 ) ) ;
#16859 = CARTESIAN_POINT ( 'NONE',  ( -4.458734124999999437, -49.64583333196772941, -2.574251347313719407 ) ) ;
#16860 = ORIENTED_EDGE ( 'NONE', *, *, #16715, .T. ) ;
#16861 = AXIS2_PLACEMENT_3D ( 'NONE', #60793, #7713, #51142 ) ;
#16862 = EDGE_CURVE ( 'NONE', #54373, #40878, #27256, .T. ) ;
#16863 = CARTESIAN_POINT ( 'NONE',  ( -2.499999999999996447, 17.29166666939785557, 4.330127018922195425 ) ) ;
#16864 = ADVANCED_FACE ( 'NONE', ( #10124 ), #36091, .T. ) ;
#16865 = AXIS2_PLACEMENT_3D ( 'NONE', #50035, #15307, #6616 ) ;
#16866 = CARTESIAN_POINT ( 'NONE',  ( 2.229367062499998831, 6.354166668032262599, -3.861377020970580887 ) ) ;
#16867 = CARTESIAN_POINT ( 'NONE',  ( -4.458734124999999437, 22.68750000136559564, 0.000000000000000000 ) ) ;
#16868 = CARTESIAN_POINT ( 'NONE',  ( -59.44456063193725015, -147.5625000013656063, -0.3552334253322034230 ) ) ;
#16869 = DIRECTION ( 'NONE',  ( 0.000000000000000000, 0.000000000000000000, 1.000000000000000000 ) ) ;
#16870 = ORIENTED_EDGE ( 'NONE', *, *, #16578, .F. ) ;
#16871 = CARTESIAN_POINT ( 'NONE',  ( 2.229367062500001939, -68.97916666530107932, 3.861377020970579999 ) ) ;
#16872 = CARTESIAN_POINT ( 'NONE',  ( 5.000000000000000888, -28.45833333060214443, 2.886751345948126879 ) ) ;
#16873 = CARTESIAN_POINT ( 'NONE',  ( 9.457646018065525792E-16, 13.93750000136559564, 5.148502694627439702 ) ) ;
#16874 = EDGE_CURVE ( 'NONE', #59810, #41033, #44533, .T. ) ;
#16875 =( BOUNDED_CURVE ( )  B_SPLINE_CURVE ( 2, ( #55152, #40342, #6268, #60302, #59662, #16231, #26193, #35528, #49357 ),
 .UNSPECIFIED., .F., .F. ) 
 B_SPLINE_CURVE_WITH_KNOTS ( ( 3, 2, 2, 2, 3 ),
 ( 0.9104166666666666519, 0.9111111111111110938, 0.9124999999999999778, 0.9138888888888888618, 0.9145833333333333037 ),
 .UNSPECIFIED. ) 
 CURVE ( )  GEOMETRIC_REPRESENTATION_ITEM ( )  RATIONAL_B_SPLINE_CURVE ( ( 0.9330127018922194093, 0.9330127018922194093, 1.000000000000000000, 0.8660254037844387076, 1.000000000000000000, 0.8660254037844387076, 1.000000000000000000, 0.9330127018922194093, 0.9330127018922194093 ) ) 
 REPRESENTATION_ITEM ( '' )  );
#16876 = CARTESIAN_POINT ( 'NONE',  ( -6.972266317189433020E-16, -60.12499999726880873, -5.000000000000000000 ) ) ;
#16877 = DIRECTION ( 'NONE',  ( -0.000000000000000000, 1.000000000000000000, -0.000000000000000000 ) ) ;
#16878 = CARTESIAN_POINT ( 'NONE',  ( -2.229367062499996610, -52.39583333196773651, 3.861377020970582219 ) ) ;
#16879 = CARTESIAN_POINT ( 'NONE',  ( 2.500000000000002220, -13.54166666393548013, 4.330127018922192761 ) ) ;
#16880 = CARTESIAN_POINT ( 'NONE',  ( -1.339745962155610925, -32.66965819600733312, 5.000000000000000000 ) ) ;
#16881 = LINE ( 'NONE', #22351, #8001 ) ;
#16882 = CARTESIAN_POINT ( 'NONE',  ( 6.123233995736766282E-16, -170.0000000000000000, -5.000000000000000000 ) ) ;
#16883 = CARTESIAN_POINT ( 'NONE',  ( 4.458734124999999437, -20.06249999863440081, -5.460374474430324690E-16 ) ) ;
#16884 = ORIENTED_EDGE ( 'NONE', *, *, #7133, .F. ) ;
#16885 = CARTESIAN_POINT ( 'NONE',  ( 1.975475456537005874E-15, -4.624999997268815832, 5.000000000000000000 ) ) ;
#16886 = CARTESIAN_POINT ( 'NONE',  ( -4.458734124999998549, -109.2291666653010793, 2.574251347313722516 ) ) ;
#16887 = CARTESIAN_POINT ( 'NONE',  ( -2.071067811865475061, -156.8125000027311842, -5.000000000000000888 ) ) ;
#16888 = ORIENTED_EDGE ( 'NONE', *, *, #7288, .F. ) ;
#16889 = CARTESIAN_POINT ( 'NONE',  ( 4.458734124999998549, -102.9791666653010651, -2.574251347313721627 ) ) ;
#16890 = CARTESIAN_POINT ( 'NONE',  ( -3.152548672688508926E-16, -26.56249999863440792, -5.148502694627439702 ) ) ;
#16891 = CARTESIAN_POINT ( 'NONE',  ( -5.000000000000000000, -60.87499999726880873, 0.000000000000000000 ) ) ;
#16892 = CARTESIAN_POINT ( 'NONE',  ( -57.19623071787017210, -151.6250000013656063, 4.297418129356382899 ) ) ;
#16893 = CARTESIAN_POINT ( 'NONE',  ( -5.000000000000000000, -148.5000000000000284, -6.123233995736766282E-16 ) ) ;
#16894 = EDGE_CURVE ( 'NONE', #29389, #31402, #3039, .T. ) ;
#16895 = CARTESIAN_POINT ( 'NONE',  ( 4.458734124999998549, -23.72916666530107577, -2.574251347313721627 ) ) ;
#16896 = CARTESIAN_POINT ( 'NONE',  ( 4.458734125000000326, -69.14583333196773651, 2.574251347313718519 ) ) ;
#16897 = CARTESIAN_POINT ( 'NONE',  ( -5.000000000000000000, -90.00000000000000000, 0.000000000000000000 ) ) ;
#16898 = CARTESIAN_POINT ( 'NONE',  ( 4.458734124999999437, -22.81249999863440436, -5.460374474430324690E-16 ) ) ;
#16899 = CARTESIAN_POINT ( 'NONE',  ( 2.499999999999998668, -32.20833333060215153, -4.330127018922193649 ) ) ;
#16900 = CARTESIAN_POINT ( 'NONE',  ( 5.000000000000000000, -152.0625000000000284, 2.071067811865478614 ) ) ;
#16901 = CARTESIAN_POINT ( 'NONE',  ( -5.000000000000000000, -12.99999999999999822, 0.000000000000000000 ) ) ;
#16902 = CARTESIAN_POINT ( 'NONE',  ( 2.730187237215162345E-16, -151.1875000013656063, -4.458734124999999437 ) ) ;
#16903 = ORIENTED_EDGE ( 'NONE', *, *, #7853, .F. ) ;
#16904 = CARTESIAN_POINT ( 'NONE',  ( 4.458734125000000326, -52.14583333196773651, 2.574251347313718519 ) ) ;
#16905 = CARTESIAN_POINT ( 'NONE',  ( 5.000000000000000888, -90.58333333333332860, 2.886751345948126879 ) ) ;
#16906 = CARTESIAN_POINT ( 'NONE',  ( 5.000000000000000888, 24.41666666666666785, 2.886751345948126879 ) ) ;
#16907 = CARTESIAN_POINT ( 'NONE',  ( -51.75738570946856498, -152.7500000000000284, 3.805975901505576964 ) ) ;
#16908 = VECTOR ( 'NONE', #4487, 1000.000000000000000 ) ;
#16909 = CARTESIAN_POINT ( 'NONE',  ( 2.229367062500001939, 5.020833334698926897, 3.861377020970579999 ) ) ;
#16910 = FACE_OUTER_BOUND ( 'NONE', #44839, .T. ) ;
#16911 = CARTESIAN_POINT ( 'NONE',  ( 1.339745962155612702, 13.70534180126148094, -5.000000000000000000 ) ) ;
#16912 = LINE ( 'NONE', #42303, #38597 ) ;
#16913 = CARTESIAN_POINT ( 'NONE',  ( 4.458734124999999437, 16.93750000136559564, -5.460374474430324690E-16 ) ) ;
#16914 = CARTESIAN_POINT ( 'NONE',  ( 5.000000000000000000, 5.708333336064518981, -2.886751345948129988 ) ) ;
#16915 = ORIENTED_EDGE ( 'NONE', *, *, #16307, .F. ) ;
#16916 = CARTESIAN_POINT ( 'NONE',  ( 5.000000000000000000, 26.58333333333333215, -2.886751345948130876 ) ) ;
#16917 = VERTEX_POINT ( 'NONE', #22256 ) ;
#16918 = CARTESIAN_POINT ( 'NONE',  ( 5.000000000000000000, -85.41666666666665719, -2.886751345948130876 ) ) ;
#16919 = CARTESIAN_POINT ( 'NONE',  ( -4.458734124999999437, -41.31249999863440081, 0.000000000000000000 ) ) ;
#16920 = CARTESIAN_POINT ( 'NONE',  ( -1.846868145590737420, -165.0000000013655779, 4.458734124999999437 ) ) ;
#16921 = EDGE_CURVE ( 'NONE', #56964, #33079, #7919, .T. ) ;
#16922 = EDGE_CURVE ( 'NONE', #51005, #44335, #58054, .T. ) ;
#16923 = CARTESIAN_POINT ( 'NONE',  ( 5.000000000000000000, -43.37499999726880873, -6.123233995736766282E-16 ) ) ;
#16924 = EDGE_CURVE ( 'NONE', #11571, #41628, #42488, .T. ) ;
#16925 = ORIENTED_EDGE ( 'NONE', *, *, #13075, .T. ) ;
#16926 = CARTESIAN_POINT ( 'NONE',  ( 4.458734124999999437, -18.81249999863440792, -5.460374474430324690E-16 ) ) ;
#16927 = ORIENTED_EDGE ( 'NONE', *, *, #7588, .F. ) ;
#16928 =( BOUNDED_CURVE ( )  B_SPLINE_CURVE ( 2, ( #33152, #52766, #19603, #57292, #8394, #47615, #38897, #27995, #3568 ),
 .UNSPECIFIED., .F., .F. ) 
 B_SPLINE_CURVE_WITH_KNOTS ( ( 3, 2, 2, 2, 3 ),
 ( 0.3687500000000000222, 0.3694444444444444642, 0.3708333333333333481, 0.3722222222222222321, 0.3729166666666666741 ),
 .UNSPECIFIED. ) 
 CURVE ( )  GEOMETRIC_REPRESENTATION_ITEM ( )  RATIONAL_B_SPLINE_CURVE ( ( 0.9330127018922194093, 0.9330127018922194093, 1.000000000000000000, 0.8660254037844387076, 1.000000000000000000, 0.8660254037844387076, 1.000000000000000000, 0.9330127018922194093, 0.9330127018922194093 ) ) 
 REPRESENTATION_ITEM ( '' )  );
#16929 = CARTESIAN_POINT ( 'NONE',  ( 1.060575238724906964E-15, -89.74999999999998579, 5.773502691896257311 ) ) ;
#16930 = CARTESIAN_POINT ( 'NONE',  ( 4.458734124999999437, -166.5000000013655779, 1.846868145590737864 ) ) ;
#16931 =( BOUNDED_CURVE ( )  B_SPLINE_CURVE ( 2, ( #53846, #18797, #4963, #62884, #63199, #48698, #10103, #156, #19109 ),
 .UNSPECIFIED., .F., .F. ) 
 B_SPLINE_CURVE_WITH_KNOTS ( ( 3, 2, 2, 2, 3 ),
 ( 0.7196428571428571397, 0.7202380952380952328, 0.7214285714285714191, 0.7226190476190476053, 0.7232142857142856984 ),
 .UNSPECIFIED. ) 
 CURVE ( )  GEOMETRIC_REPRESENTATION_ITEM ( )  RATIONAL_B_SPLINE_CURVE ( ( 0.9330127018922194093, 0.9330127018922194093, 1.000000000000000000, 0.8660254037844387076, 1.000000000000000000, 0.8660254037844387076, 1.000000000000000000, 0.9330127018922194093, 0.9330127018922194093 ) ) 
 REPRESENTATION_ITEM ( '' )  );
#16933 = ORIENTED_EDGE ( 'NONE', *, *, #39284, .F. ) ;
#16932 = CARTESIAN_POINT ( 'NONE',  ( -5.000000000000000000, -18.99999999999999645, 0.000000000000000000 ) ) ;
#16934 = CARTESIAN_POINT ( 'NONE',  ( -59.98410592259440222, -139.1250000000000284, -0.3983568153799752487 ) ) ;
#16935 = CARTESIAN_POINT ( 'NONE',  ( 4.458734124999998549, -33.97916666530107221, -2.574251347313721627 ) ) ;
#16936 = CARTESIAN_POINT ( 'NONE',  ( -6.972266317189433020E-16, 22.87500000273118417, -5.000000000000000000 ) ) ;
#16937 = EDGE_CURVE ( 'NONE', #41952, #33720, #33820, .T. ) ;
#16938 = EDGE_LOOP ( 'NONE', ( #45880, #35452, #23660, #9410 ) ) ;
#16939 = CARTESIAN_POINT ( 'NONE',  ( 2.229367062500001939, -74.97916666530106511, 3.861377020970579999 ) ) ;
#16940 = EDGE_CURVE ( 'NONE', #35906, #35595, #12281, .T. ) ;
#16941 = CARTESIAN_POINT ( 'NONE',  ( -2.229367062499996610, 24.85416666803225993, 3.861377020970582219 ) ) ;
#16942 = CARTESIAN_POINT ( 'NONE',  ( -6.972266317189433020E-16, -18.25000000000000000, -5.000000000000000000 ) ) ;
#16943 = ORIENTED_EDGE ( 'NONE', *, *, #41756, .T. ) ;
#16944 = CARTESIAN_POINT ( 'NONE',  ( -6.972266317189433020E-16, 4.875000002731184168, -5.000000000000000000 ) ) ;
#16945 = CARTESIAN_POINT ( 'NONE',  ( -58.39396692619412477, -142.6875000013656063, 2.891590998281057701 ) ) ;
#16946 = CARTESIAN_POINT ( 'NONE',  ( 9.457646018065525792E-16, -80.31249999863440792, 5.148502694627439702 ) ) ;
#16947 = CARTESIAN_POINT ( 'NONE',  ( -53.33387254593733928, -130.9375000027312126, 5.149110718188519620 ) ) ;
#16948 = FACE_OUTER_BOUND ( 'NONE', #12883, .T. ) ;
#16949 = CARTESIAN_POINT ( 'NONE',  ( 2.730187237215162345E-16, -141.4375000013656063, -4.458734124999999437 ) ) ;
#16950 = CARTESIAN_POINT ( 'NONE',  ( -5.000000000000000000, 6.125000002731185056, 0.000000000000000000 ) ) ;
#16951 = CARTESIAN_POINT ( 'NONE',  ( -2.229367062499996610, -57.14583333196773651, 3.861377020970582219 ) ) ;
#16952 = CARTESIAN_POINT ( 'NONE',  ( -2.229367062500000163, -43.47916666530106511, -3.861377020970580443 ) ) ;
#16953 = CARTESIAN_POINT ( 'NONE',  ( -3.152548672688508926E-16, 28.43750000136559208, -5.148502694627439702 ) ) ;
#16954 = CARTESIAN_POINT ( 'NONE',  ( -3.535250795749689387E-16, -107.2499999999999858, -5.773502691896257311 ) ) ;
#16955 = AXIS2_PLACEMENT_3D ( 'NONE', #37433, #62204, #57065 ) ;
#16956 = CARTESIAN_POINT ( 'NONE',  ( -5.000000000000000000, 3.916666666666665630, -2.886751345948128211 ) ) ;
#16957 = CARTESIAN_POINT ( 'NONE',  ( 4.458734124999998549, -38.97916666530107221, -2.574251347313721627 ) ) ;
#16958 = CARTESIAN_POINT ( 'NONE',  ( -2.500000000000000444, -0.04166666393548221214, -4.330127018922193649 ) ) ;
#16959 = DIRECTION ( 'NONE',  ( 1.000000000000000000, 0.000000000000000000, -0.000000000000000000 ) ) ;
#16960 = CARTESIAN_POINT ( 'NONE',  ( -2.499999999999996447, -45.70833333060214443, 4.330127018922195425 ) ) ;
#16961 =( BOUNDED_SURFACE ( )  B_SPLINE_SURFACE ( 3, 2, ( 
 ( #33977, #49723, #14355 ),
 ( #59062, #24644, #53598 ),
 ( #530, #5025, #19495 ),
 ( #39110, #58738, #9834 ),
 ( #49078, #44251, #215 ),
 ( #14988, #34598, #60030 ),
 ( #41339, #55835, #25918 ),
 ( #51008, #45536, #16277 ) ),
 .UNSPECIFIED., .F., .F., .F. ) 
 B_SPLINE_SURFACE_WITH_KNOTS ( ( 4, 2, 2, 4 ),
 ( 3, 3 ),
 ( 0.03861844051980969916, 0.04325213341840641879, 0.04556897986770477860, 0.04788582631700313841 ),
 ( 0.000000000000000000, 1.000000000000000000 ),
 .UNSPECIFIED. ) 
 GEOMETRIC_REPRESENTATION_ITEM ( )  RATIONAL_B_SPLINE_SURFACE ( (
 ( 1.000000000000000000, 0.8047781759831920123, 1.000000000000000000),
 ( 1.000000000000000000, 0.8123762462803147955, 1.000000000000000000),
 ( 1.000000000000000000, 0.8190659850619289584, 1.000000000000000000),
 ( 1.000000000000000000, 0.8191937571012362085, 1.000000000000000000),
 ( 1.000000000000000000, 0.8176092952779873135, 1.000000000000000000),
 ( 1.000000000000000000, 0.8122962088597077690, 1.000000000000000000),
 ( 1.000000000000000000, 0.8086311330827508081, 1.000000000000000000),
 ( 1.000000000000000000, 0.8047712282214326551, 1.000000000000000000) ) ) 
 REPRESENTATION_ITEM ( '' )  SURFACE ( )  );
#16962 = CARTESIAN_POINT ( 'NONE',  ( 4.458734125000001214, -78.14583333196775072, 2.574251347313718519 ) ) ;
#16963 = CARTESIAN_POINT ( 'NONE',  ( -53.33387254593716875, -141.9375000027312126, 5.149110718188532942 ) ) ;
#16964 = CARTESIAN_POINT ( 'NONE',  ( 2.229367062499998831, -98.64583333196773651, -3.861377020970580887 ) ) ;
#16965 = CARTESIAN_POINT ( 'NONE',  ( 4.458734125000000326, -4.145833331967739177, 2.574251347313718519 ) ) ;
#16966 = ORIENTED_EDGE ( 'NONE', *, *, #54232, .F. ) ;
#16967 = CARTESIAN_POINT ( 'NONE',  ( -56.66612745406293783, -139.3125000000000284, -5.149110718188535607 ) ) ;
#16968 = CARTESIAN_POINT ( 'NONE',  ( -4.999999999999998224, -35.79166666393547303, 2.886751345948131764 ) ) ;
#16969 = CARTESIAN_POINT ( 'NONE',  ( -4.458734124999999437, -94.31249999863440792, 0.000000000000000000 ) ) ;
#16970 = CARTESIAN_POINT ( 'NONE',  ( -1.339745962155613812, -5.205341801261476498, -5.000000000000000000 ) ) ;
#16971 = CARTESIAN_POINT ( 'NONE',  ( -4.458734124999998549, -86.47916666530107932, 2.574251347313722516 ) ) ;
#16972 = CARTESIAN_POINT ( 'NONE',  ( -2.229367062499996610, 11.60416666803225993, 3.861377020970582219 ) ) ;
#16973 = CARTESIAN_POINT ( 'NONE',  ( -2.499999999999996447, -29.83333333333332860, 4.330127018922195425 ) ) ;
#16974 = CARTESIAN_POINT ( 'NONE',  ( -50.55543936806279248, -134.0625000013656063, 0.3552334253322060320 ) ) ;
#16975 = CARTESIAN_POINT ( 'NONE',  ( 4.458734124999999437, -6.812499998634404363, -5.460374474430324690E-16 ) ) ;
#16976 = CARTESIAN_POINT ( 'NONE',  ( 2.229367062499998831, 15.10416666803225993, -3.861377020970580887 ) ) ;
#16977 = CARTESIAN_POINT ( 'NONE',  ( 2.229367062500001939, -52.22916666530107221, 3.861377020970579999 ) ) ;
#16978 = CARTESIAN_POINT ( 'NONE',  ( 1.339745962155615144, -11.70534180126147739, 4.999999999999999112 ) ) ;
#16979 = CARTESIAN_POINT ( 'NONE',  ( -3.152548672688508926E-16, -83.56249999863440792, -5.148502694627439702 ) ) ;
#16980 = CARTESIAN_POINT ( 'NONE',  ( 4.458734125000000326, -6.895833331967734736, 2.574251347313718519 ) ) ;
#16981 = ORIENTED_EDGE ( 'NONE', *, *, #35831, .T. ) ;
#16982 = CARTESIAN_POINT ( 'NONE',  ( 2.229367062500001939, -38.22916666530107221, 3.861377020970579999 ) ) ;
#16983 =( BOUNDED_CURVE ( )  B_SPLINE_CURVE ( 2, ( #6597, #32540, #17755, #52167, #51851, #7793, #27396, #45510, #37371 ),
 .UNSPECIFIED., .F., .F. ) 
 B_SPLINE_CURVE_WITH_KNOTS ( ( 3, 2, 2, 2, 3 ),
 ( 0.5416666666666671848, 0.5458333333333338366, 0.5500000000000004885, 0.5541666666666671404, 0.5583333333333337922 ),
 .UNSPECIFIED. ) 
 CURVE ( )  GEOMETRIC_REPRESENTATION_ITEM ( )  RATIONAL_B_SPLINE_CURVE ( ( 0.9999999999999898970, 0.9238795325112968415, 1.000000000000000000, 0.9238795325112867385, 1.000000000000000000, 0.9238795325112867385, 1.000000000000000000, 0.9238795325112786339, 1.000000000000008216 ) ) 
 REPRESENTATION_ITEM ( '' )  );
#16984 = CARTESIAN_POINT ( 'NONE',  ( -59.29741812935640155, -126.8750000013656205, -2.196230717870135685 ) ) ;
#16985 = CARTESIAN_POINT ( 'NONE',  ( 4.458734125000001214, -79.89583333196773651, 2.574251347313718519 ) ) ;
#16986 = CARTESIAN_POINT ( 'NONE',  ( 2.499999999999998668, -109.2083333306021444, -4.330127018922193649 ) ) ;
#16987 = CARTESIAN_POINT ( 'NONE',  ( -4.458734124999999437, -150.2500000013656347, -1.846868145590735644 ) ) ;
#16988 = CARTESIAN_POINT ( 'NONE',  ( -4.458734124999999437, 18.68750000136559564, 0.000000000000000000 ) ) ;
#16989 = CARTESIAN_POINT ( 'NONE',  ( -6.972266317189433020E-16, -94.25000000000000000, -5.000000000000000000 ) ) ;
#16990 = CARTESIAN_POINT ( 'NONE',  ( 5.000000000000000000, -66.50000000000000000, -6.123233995736766282E-16 ) ) ;
#16991 = CARTESIAN_POINT ( 'NONE',  ( 9.457646018065525792E-16, -82.31249999863440792, 5.148502694627439702 ) ) ;
#16992 = CARTESIAN_POINT ( 'NONE',  ( 5.000000000000000000, -65.41666666666665719, -2.886751345948129988 ) ) ;
#16993 = DIRECTION ( 'NONE',  ( 0.000000000000000000, 0.000000000000000000, 1.000000000000000000 ) ) ;
#16994 = CARTESIAN_POINT ( 'NONE',  ( 2.500000000000002220, 17.45833333606451987, 4.330127018922192761 ) ) ;
#16995 = VERTEX_POINT ( 'NONE', #26761 ) ;
#16996 = CARTESIAN_POINT ( 'NONE',  ( 2.500000000000002220, -18.54166666393547658, 4.330127018922192761 ) ) ;
#16997 = CARTESIAN_POINT ( 'NONE',  ( 1.975475456537005874E-15, 7.249999999999998224, 5.000000000000000000 ) ) ;
#16999 = CARTESIAN_POINT ( 'NONE',  ( 5.000000000000000888, -24.58333333333333215, 2.886751345948126879 ) ) ;
#16998 = CARTESIAN_POINT ( 'NONE',  ( 5.000000000000000888, -0.5833333333333350357, 2.886751345948126879 ) ) ;
#17000 = CARTESIAN_POINT ( 'NONE',  ( -4.458734124999998549, -29.22916666530107221, 2.574251347313722516 ) ) ;
#17001 = CARTESIAN_POINT ( 'NONE',  ( 4.458734125000000326, -89.89583333196773651, 2.574251347313718519 ) ) ;
#17002 = ADVANCED_FACE ( 'NONE', ( #46690 ), #8411, .T. ) ;
#17003 = CARTESIAN_POINT ( 'NONE',  ( -4.999999999999999112, -27.79166666393547658, 2.886751345948131764 ) ) ;
#17005 = ORIENTED_EDGE ( 'NONE', *, *, #46814, .T. ) ;
#17004 = CARTESIAN_POINT ( 'NONE',  ( -4.458734124999999437, -53.39583333196773651, -2.574251347313719407 ) ) ;
#17006 = CARTESIAN_POINT ( 'NONE',  ( -59.29741812935640155, -153.8750000013655779, -2.196230717870135685 ) ) ;
#17008 = VERTEX_POINT ( 'NONE', #21933 ) ;
#17007 = CARTESIAN_POINT ( 'NONE',  ( 4.458734125000001214, -3.145833331967738733, 2.574251347313718519 ) ) ;
#17009 = CARTESIAN_POINT ( 'NONE',  ( 2.500000000000002220, -72.66666666666667140, 4.330127018922192761 ) ) ;
#17010 = CARTESIAN_POINT ( 'NONE',  ( -57.19623071787016499, -139.3750000013656063, 4.297418129356382899 ) ) ;
#17011 = CARTESIAN_POINT ( 'NONE',  ( 4.458734124999998549, -49.97916666530106511, -2.574251347313721627 ) ) ;
#17012 = CARTESIAN_POINT ( 'NONE',  ( -2.499999999999996447, 0.2916666693978525737, 4.330127018922195425 ) ) ;
#17013 = EDGE_CURVE ( 'NONE', #2252, #29860, #61813, .T. ) ;
#17014 = CARTESIAN_POINT ( 'NONE',  ( -3.535250795749689387E-16, -70.12499999726880162, -5.773502691896257311 ) ) ;
#17015 = CARTESIAN_POINT ( 'NONE',  ( -2.499999999999996447, -85.83333333333332860, 4.330127018922195425 ) ) ;
#17016 = CARTESIAN_POINT ( 'NONE',  ( -59.98410592259440222, -152.1250000000000284, -0.3983568153799752487 ) ) ;
#17017 = EDGE_CURVE ( 'NONE', #58981, #50378, #7778, .T. ) ;
#17018 = CARTESIAN_POINT ( 'NONE',  ( 9.457646018065525792E-16, -16.31249999863440436, 5.148502694627439702 ) ) ;
#17019 = CARTESIAN_POINT ( 'NONE',  ( 9.457646018065525792E-16, -52.31249999863440792, 5.148502694627439702 ) ) ;
#17020 = CARTESIAN_POINT ( 'NONE',  ( -1.339745962155610925, -58.66965819600732601, 5.000000000000000000 ) ) ;
#17021 =( LENGTH_UNIT ( ) NAMED_UNIT ( * ) SI_UNIT ( .MILLI., .METRE. ) );
#17022 = CARTESIAN_POINT ( 'NONE',  ( -4.458734125000001214, -140.8750000013656063, 1.846868145590734089 ) ) ;
#17023 = CARTESIAN_POINT ( 'NONE',  ( 4.458734125000001214, -92.14583333196775072, 2.574251347313718519 ) ) ;
#17024 = CARTESIAN_POINT ( 'NONE',  ( -6.972266317189433020E-16, -1.250000000000000000, -5.000000000000000000 ) ) ;
#17025 = ORIENTED_EDGE ( 'NONE', *, *, #62903, .F. ) ;
#17026 = ADVANCED_FACE ( 'NONE', ( #22579 ), #37357, .T. ) ;
#17027 = DIRECTION ( 'NONE',  ( -0.000000000000000000, 1.000000000000000000, -0.000000000000000000 ) ) ;
#17028 = CARTESIAN_POINT ( 'NONE',  ( -56.66612745406270335, -141.4375000027312410, -5.149110718188516067 ) ) ;
#17029 = EDGE_CURVE ( 'NONE', #46822, #12246, #15725, .T. ) ;
#17030 = CARTESIAN_POINT ( 'NONE',  ( 2.229367062499998831, -1.645833331967737401, -3.861377020970580887 ) ) ;
#17031 = CARTESIAN_POINT ( 'NONE',  ( -4.458734124999999437, -94.64583333196773651, -2.574251347313719407 ) ) ;
#17032 = ADVANCED_FACE ( 'NONE', ( #30508 ), #7038, .T. ) ;
#17033 = CARTESIAN_POINT ( 'NONE',  ( -3.152801135295367096, -148.3125000013655779, -3.152801135295367541 ) ) ;
#17034 = CARTESIAN_POINT ( 'NONE',  ( 4.458734124999999437, -25.06249999863440792, -5.460374474430324690E-16 ) ) ;
#17035 = CYLINDRICAL_SURFACE ( 'NONE', #51944, 5.000000000000000000 ) ;
#17036 = CARTESIAN_POINT ( 'NONE',  ( -56.48576386720575471, -141.7500000013656063, -4.591703134518078322 ) ) ;
#17037 = CARTESIAN_POINT ( 'NONE',  ( -2.229367062499996610, -63.39583333196774362, 3.861377020970582219 ) ) ;
#17038 = CARTESIAN_POINT ( 'NONE',  ( -2.071067811865308972, -154.4375000027312126, 5.000000000000169642 ) ) ;
#17039 = CARTESIAN_POINT ( 'NONE',  ( 5.000000000000000888, 23.54166666939785202, 2.886751345948126879 ) ) ;
#17040 = CARTESIAN_POINT ( 'NONE',  ( 1.846868145590736310, -143.6250000013655779, 4.458734124999997661 ) ) ;
#17041 = CARTESIAN_POINT ( 'NONE',  ( -4.458734124999999437, 11.43750000136559564, 0.000000000000000000 ) ) ;
#17042 = ORIENTED_EDGE ( 'NONE', *, *, #3241, .T. ) ;
#17043 = CARTESIAN_POINT ( 'NONE',  ( -58.24261429053147765, -150.3750000027312126, -3.805975901505573855 ) ) ;
#17044 = DIRECTION ( 'NONE',  ( 0.000000000000000000, 0.000000000000000000, 1.000000000000000000 ) ) ;
#17046 = CARTESIAN_POINT ( 'NONE',  ( -4.458734124999999437, -23.31249999863440436, 0.000000000000000000 ) ) ;
#17045 = CARTESIAN_POINT ( 'NONE',  ( -2.500000000000000444, -86.16666666666667140, -4.330127018922193649 ) ) ;
#17047 = CARTESIAN_POINT ( 'NONE',  ( 1.975475456537005874E-15, -5.750000000000000000, 5.000000000000000000 ) ) ;
#17048 = DIRECTION ( 'NONE',  ( -0.6485228581062915110, 0.000000000000000000, -0.7611951803011149931 ) ) ;
#17049 = VECTOR ( 'NONE', #49929, 1000.000000000000000 ) ;
#17050 = CARTESIAN_POINT ( 'NONE',  ( -58.39396692619412477, -145.4375000013656063, 2.891590998281057701 ) ) ;
#17051 = CARTESIAN_POINT ( 'NONE',  ( -4.999999999999999112, -46.79166666393546592, 2.886751345948131764 ) ) ;
#17052 = CARTESIAN_POINT ( 'NONE',  ( 5.000000000000000888, -24.58333333333333215, 2.886751345948126879 ) ) ;
#17053 = CARTESIAN_POINT ( 'NONE',  ( -4.458734124999997661, 9.770833334698927786, 2.574251347313722516 ) ) ;
#17054 = CARTESIAN_POINT ( 'NONE',  ( 5.000000000000000888, -56.45833333060214443, 2.886751345948126879 ) ) ;
#17055 = CARTESIAN_POINT ( 'NONE',  ( 4.458734125000000326, 5.104166668032261711, 2.574251347313718519 ) ) ;
#17056 = CARTESIAN_POINT ( 'NONE',  ( -2.229367062499996610, -68.14583333196773651, 3.861377020970582219 ) ) ;
#17057 = CARTESIAN_POINT ( 'NONE',  ( 4.458734124999998549, -18.97916666530106511, -2.574251347313721627 ) ) ;
#17058 = CARTESIAN_POINT ( 'NONE',  ( 5.000000000000000000, -1.500000000000001332, -6.123233995736766282E-16 ) ) ;
#17059 = CARTESIAN_POINT ( 'NONE',  ( 4.458734125000000326, -160.3750000013656063, -1.846868145590734978 ) ) ;
#17060 = CARTESIAN_POINT ( 'NONE',  ( -1.339745962155618253, 22.20534180126147916, 4.999999999999996447 ) ) ;
#17061 = CARTESIAN_POINT ( 'NONE',  ( -3.152548672688508926E-16, -61.56249999863440792, -5.148502694627439702 ) ) ;
#17062 = CARTESIAN_POINT ( 'NONE',  ( 5.000000000000000888, -92.45833333060215864, 2.886751345948126879 ) ) ;
#17063 =( BOUNDED_SURFACE ( )  B_SPLINE_SURFACE ( 1, 2, ( 
 ( #22155, #17943, #52680, #17643, #41749, #47230, #3173, #42386, #62026, #13441, #61398, #33066, #41435, #17006, #2856, #36621, #12807, #42073, #32428, #56254, #31793, #51425, #7368, #46595, #33998, #47839, #28853, #43328, #39131, #53305, #23419, #19196, #58758, #48781, #34306, #63279, #14688, #62969, #23733, #8927, #44273, #53929, #33684, #9239, #43637, #9552, #38809, #33372, #8615, #19517, #29157, #43022, #39446, #4723, #24349, #19833, #63597, #4113, #29468, #9858, #48475, #58451, #18582, #43949, #49101, #3798, #18885, #38500, #58128, #5047, #38205, #62662, #53621, #57830, #28223, #24665, #4411, #24035, #235, #34623, #14374, #59083, #15009, #13750, #52986, #28540, #14059, #48160, #2697, #12344, #46118, #6566, #31312, #31955, #6889, #61560, #2387, #21363, #51587, #1760, #7525, #49423, #31643, #27136, #26181, #26504, #2081, #40966, #21997, #60614, #39757, #16846, #29790, #16533, #10190, #55464, #36789, #46751, #45800, #24985, #56093, #50628, #50948, #60926, #31001, #22316, #5367, #44592, #34957, #36156, #56421, #21687, #552, #41918, #17494, #54248, #41591, #20161, #59402, #55777, #36466, #61242, #15334, #11380, #11693, #41277, #51277, #12013, #7210, #26822, #46441, #17164, #3960, #37420, #42550, #33224, #23580, #23886, #42238, #28077, #32270, #28387, #43176, #37116, #3338, #62189, #51898, #47694, #57985, #4268, #13607, #42865, #12965, #48318, #52843, #32590, #48006, #63133, #3646, #52215, #7839, #22954, #18110, #8777, #62818, #9090, #57054, #56734, #47075, #57681, #8160, #22639, #37732, #27759, #57366, #27441, #12654, #23258, #13287, #3023, #52535, #61880, #28698, #17796, #47387, #62511, #32912, #18427, #8469, #38049, #18734, #38359, #13910, #33538, #53153, #43488, #399, #9708, #4570, #14219, #5213, #45087, #58613, #20001, #25145, #54746, #10031, #29644, #49277, #48944, #14534, #29312, #49588, #5530, #24832, #4892, #44438, #24516, #19365, #34803, #44117, #38661, #717, #39930, #48631, #81, #34462, #44756, #43800, #24193, #39609, #53465, #54092, #34153, #58300, #15177, #20328, #59247, #54425, #33846, #59576, #9395, #10354, #19681, #29005, #29963, #63447, #10666, #38976, #53775, #15509, #39293, #35130, #58920, #14849, #30282, #49902, #5856, #25464, #19044, #26423, #46040, #55385, #50230, #59902, #50872, #27060, #40574, #2005, #7131, #36716, #55707, #11620, #31240, #30927, #60215, #11302, #31566, #51199, #6816, #50553, #21608, #6497, #1372, #16774, #26109, #20658, #46363, #21920, #30606, #45729, #16458, #26747, #25794, #6178, #41203, #35436, #36077, #16139, #40262, #60847, #2317, #36391, #56022, #15823, #41518, #61170, #51515, #1052, #17093, #55062, #56347, #35761, #11937, #12269, #10986, #45405, #1680, #31881, #7452, #20973, #21282, #40889, #60535, #62745, #13535, #47000, #52142, #42790, #33155, #33456, #51821, #37653, #41841, #37977, #52769, #46678, #12891, #8084, #61488, #57296, #3882, #13836, #23180, #52463, #22565, #57915, #62434, #42163, #57608, #9014, #13212, #61799, #17420, #32510, #27688, #18352, #8698, #18666, #2948, #2624, #56660, #3571, #17725, #32191, #47314, #37341, #3266, #37034, #28310, #47927, #23501, #53073, #8399, #22241, #22878, #56974, #43104, #42471, #12578, #32834, #38288, #7763, #27366, #27999, #62113, #18031, #47618, #28934, #641, #54349, #53704, #29244, #3, #29566, #19606, #53390, #28625, #39533, #49197, #63057, #59495, #5137, #24753, #39852, #19919, #24125, #49513, #34720, #9636, #39218, #38584, #44358, #321, #23811, #19286, #43726, #63370, #59171, #58215, #18969, #9949, #14143, #48242, #5452, #48869, #4815, #20250, #54664, #24436, #44039, #58843, #25070, #14772, #15103, #38901, #15434, #35052, #44680, #34391, #58537, #54017, #4198, #10279, #43414, #29884, #14459, #33770, #34081, #9321, #48558, #4497, #51117, #25719, #26035, #1607, #20895, #41129, #60138, #59823, #36004 ),
 ( #30199, #49828, #54982, #45329, #11860, #45649, #977, #55635, #11550, #31167, #50799, #60776, #1299, #2244, #45963, #6735, #40497, #26344, #21205, #11230, #50149, #40811, #1927, #45011, #60459, #16059, #5772, #21532, #16701, #16385, #36319, #25390, #31476, #7054, #61093, #36632, #55945, #20580, #26667, #6104, #46287, #21848, #40187, #15744, #35688, #41444, #17016, #10587, #55316, #35359, #50484, #10911, #30526, #30855, #6423, #52383, #23106, #43031, #61409, #47240, #51436, #47542, #62352, #56264, #22487, #61725, #7377, #3184, #13454, #23429, #32756, #62036, #32114, #3806, #8321, #51750, #3492, #18592, #22802, #7692, #26985, #42082, #37269, #27920, #42710, #28233, #12502, #12188, #2549, #13137, #27298, #41759, #56896, #46923, #17653, #46604, #31802, #42395, #12816, #22164, #8005, #17332, #47848, #36954, #2868, #17953, #32437, #37577, #56582, #52066, #27608, #57217, #18275, #37901, #57531, #33076, #52688, #8624, #62671, #33381, #24359, #562, #14067, #39142, #44284, #10200, #29168, #48792, #4734, #4421, #33695, #28863, #5057, #24676, #43960, #48485, #63607, #24046, #38509, #53939, #43648, #57840, #19843, #59093, #4122, #63288, #53631, #246, #62980, #23744, #58137, #43337, #38820, #53314, #19206, #8936, #13759, #19527, #58461, #52996, #9562, #28550, #29801, #48169, #9248, #58768, #14384, #14698, #18895, #34008, #34315, #9869, #29479, #49112, #39458, #15019, #34634, #54260, #49434, #5377, #24994, #38217, #44602, #21124, #26258, #55863, #11149, #30771, #50392, #50071, #59737, #10830, #50709, #6652, #25948, #30444, #45563, #6027, #20495, #35924, #25631, #39767, #1844, #41049, #49751, #45245, #35603, #45881, #44932, #5696, #1521, #54585, #55227, #35280, #59414, #16301, #21449, #6341, #60378, #15345, #60696, #16616, #6975, #46204, #36235, #10506, #11776, #15663, #40731, #31394, #34969, #30121, #54902, #51033, #55553, #11465, #1213, #25311, #60052, #26586, #20171, #40094, #20810, #31086, #888, #40413, #15976, #56819, #61008, #57138, #8239, #2165, #32036, #7613, #16934, #12736, #23032, #32994, #42318, #7923, #41676, #13373, #61958, #61327, #13055, #28158, #32359, #17249, #36548, #51672, #46835, #17880, #32672, #37820, #22079, #21771, #12101, #22721, #61643, #31725, #27528, #51981, #47158, #3104, #37500, #56502, #51357, #56180, #52304, #41364, #36872, #27841, #47463, #57449, #3415, #42635, #62277, #27218, #12425, #2783, #18199, #52611, #8546, #22404, #7297, #42002, #2469, #26908, #17575, #46527, #37194, #4975, #13684, #33619, #63211, #9788, #8859, #33303, #29084, #18514, #19124, #62897, #23351, #43879, #53858, #58380, #24275, #3729, #49031, #24598, #34545, #10118, #14620, #38136, #44204, #43257, #48714, #34232, #62594, #57761, #23661, #169, #63527, #38742, #18811, #52921, #23963, #19768, #29396, #48089, #53238, #19448, #39377, #54179, #28475, #14307, #42951, #39063, #59008, #47774, #13990, #9172, #4044, #33929, #14936, #38433, #58692, #53552, #58060, #28786, #48402, #4344, #43566, #9476, #4653, #44846, #24919, #59661, #10759, #45490, #60301, #1772, #49677, #29724, #39692, #50317, #5622, #15265, #30371, #25235, #54828, #485, #49356, #20738, #49992, #44525, #45171, #20087, #21373, #59332, #809, #59984, #35210, #11075, #5301, #20416, #40016, #40982, #1453, #25874, #15593, #21054, #40341, #5945, #25551, #15907, #16230, #11390, #40661, #36167, #55151, #34889, #1138, #35527, #35850, #30698, #54512, #6267, #55475, #31010, #50639, #6577, #26192, #45811, #60624, #30048, #16544, #55788, #10435, #12355, #46764, #12670, #2709, #36480, #11706, #22651, #32282, #46130, #42561, #51910, #7850, #22964, #3033, #7224, #32600, #17807, #36801, #22329, #21699, #27453, #47086, #6901, #2398, #26839, #46453, #42250, #41290, #2097, #56746, #60939, #31325, #52225, #31968, #56433, #3347, #37745, #51604, #7536, #41930, #8170, #61572 ) ),
 .UNSPECIFIED., .F., .F., .F. ) 
 B_SPLINE_SURFACE_WITH_KNOTS ( ( 2, 2 ),
 ( 3, 2, 2, 2, 2, 2, 2, 2, 2, 2, 2, 2, 2, 2, 2, 2, 2, 2, 2, 2, 2, 2, 2, 2, 2, 2, 2, 2, 2, 2, 2, 2, 2, 2, 2, 2, 2, 2, 2, 2, 2, 2, 2, 2, 2, 2, 2, 2, 2, 2, 2, 2, 2, 2, 2, 2, 2, 2, 2, 2, 2, 2, 2, 2, 2, 2, 2, 2, 2, 2, 2, 2, 2, 2, 2, 2, 2, 2, 2, 2, 2, 2, 2, 2, 2, 2, 2, 2, 2, 2, 2, 2, 2, 2, 2, 2, 2, 2, 2, 2, 2, 2, 2, 2, 2, 2, 2, 2, 2, 2, 2, 2, 2, 2, 2, 2, 2, 2, 2, 2, 2, 2, 2, 2, 2, 2, 2, 2, 2, 2, 2, 2, 2, 2, 2, 2, 2, 2, 2, 2, 2, 2, 2, 2, 2, 2, 2, 2, 2, 2, 2, 2, 2, 2, 2, 2, 2, 2, 2, 2, 2, 2, 2, 2, 2, 2, 2, 2, 2, 2, 2, 2, 2, 2, 2, 2, 2, 2, 2, 2, 2, 2, 2, 2, 2, 2, 2, 2, 2, 2, 2, 2, 2, 2, 2, 2, 2, 2, 2, 2, 2, 2, 2, 2, 2, 2, 2, 2, 2, 2, 2, 2, 2, 2, 2, 2, 2, 2, 2, 2, 2, 2, 2, 2, 2, 2, 2, 2, 2, 2, 2, 2, 2, 2, 2, 2, 2, 2, 2, 2, 3 ),
 ( 0.000000000000000000, 1.000000000000000000 ),
 ( 0.000000000000000000, 0.004166666666666666609, 0.008333333333333333218, 0.01250000000000000069, 0.01666666666666666644, 0.02083333333333333218, 0.02500000000000000139, 0.02916666666666666713, 0.03333333333333333287, 0.03749999999999999861, 0.04166666666666666435, 0.04583333333333333010, 0.05000000000000000278, 0.05416666666666666852, 0.05833333333333333426, 0.06250000000000000000, 0.06666666666666666574, 0.07083333333333333148, 0.07499999999999999722, 0.07916666666666666297, 0.08333333333333332871, 0.08749999999999999445, 0.09166666666666666019, 0.09583333333333333981, 0.1000000000000000056, 0.1041666666666666713, 0.1083333333333333370, 0.1125000000000000028, 0.1166666666666666685, 0.1208333333333333343, 0.1250000000000000000, 0.1291666666666666796, 0.1333333333333333315, 0.1375000000000000111, 0.1416666666666666630, 0.1458333333333333426, 0.1499999999999999944, 0.1541666666666666741, 0.1583333333333333259, 0.1625000000000000056, 0.1666666666666666574, 0.1708333333333333370, 0.1749999999999999889, 0.1791666666666666685, 0.1833333333333333204, 0.1875000000000000000, 0.1916666666666666796, 0.1958333333333333315, 0.2000000000000000111, 0.2041666666666666630, 0.2083333333333333426, 0.2124999999999999944, 0.2166666666666666741, 0.2208333333333333259, 0.2250000000000000056, 0.2291666666666666574, 0.2333333333333333370, 0.2374999999999999889, 0.2416666666666666685, 0.2458333333333333204, 0.2500000000000000000, 0.2541666666666666519, 0.2583333333333333592, 0.2625000000000000111, 0.2666666666666666630, 0.2708333333333333148, 0.2750000000000000222, 0.2791666666666666741, 0.2833333333333333259, 0.2874999999999999778, 0.2916666666666666852, 0.2958333333333333370, 0.2999999999999999889, 0.3041666666666666408, 0.3083333333333333481, 0.3125000000000000000, 0.3166666666666666519, 0.3208333333333333592, 0.3250000000000000111, 0.3291666666666666630, 0.3333333333333333148, 0.3375000000000000222, 0.3416666666666666741, 0.3458333333333333259, 0.3499999999999999778, 0.3541666666666666852, 0.3583333333333333370, 0.3624999999999999889, 0.3666666666666666408, 0.3708333333333333481, 0.3750000000000000000, 0.3791666666666666519, 0.3833333333333333592, 0.3875000000000000111, 0.3916666666666666630, 0.3958333333333333148, 0.4000000000000000222, 0.4041666666666666741, 0.4083333333333333259, 0.4124999999999999778, 0.4166666666666666852, 0.4208333333333333370, 0.4249999999999999889, 0.4291666666666666408, 0.4333333333333333481, 0.4375000000000000000, 0.4416666666666666519, 0.4458333333333333592, 0.4500000000000000111, 0.4541666666666666630, 0.4583333333333333148, 0.4625000000000000222, 0.4666666666666666741, 0.4708333333333333259, 0.4749999999999999778, 0.4791666666666666852, 0.4833333333333333370, 0.4874999999999999889, 0.4916666666666666408, 0.4958333333333333481, 0.5000000000000000000, 0.5041666666666666519, 0.5083333333333333037, 0.5124999999999999556, 0.5166666666666667185, 0.5208333333333333703, 0.5250000000000000222, 0.5291666666666666741, 0.5333333333333333259, 0.5374999999999999778, 0.5416666666666666297, 0.5458333333333332815, 0.5500000000000000444, 0.5541666666666666963, 0.5583333333333333481, 0.5625000000000000000, 0.5666666666666666519, 0.5708333333333333037, 0.5749999999999999556, 0.5791666666666667185, 0.5833333333333333703, 0.5875000000000000222, 0.5916666666666666741, 0.5958333333333333259, 0.5999999999999999778, 0.6041666666666666297, 0.6083333333333332815, 0.6125000000000000444, 0.6166666666666666963, 0.6208333333333333481, 0.6250000000000000000, 0.6291666666666666519, 0.6333333333333333037, 0.6374999999999999556, 0.6416666666666667185, 0.6458333333333333703, 0.6500000000000000222, 0.6541666666666666741, 0.6583333333333333259, 0.6624999999999999778, 0.6666666666666666297, 0.6708333333333332815, 0.6750000000000000444, 0.6791666666666666963, 0.6833333333333333481, 0.6875000000000000000, 0.6916666666666666519, 0.6958333333333333037, 0.6999999999999999556, 0.7041666666666667185, 0.7083333333333333703, 0.7125000000000000222, 0.7166666666666666741, 0.7208333333333333259, 0.7249999999999999778, 0.7291666666666666297, 0.7333333333333332815, 0.7375000000000000444, 0.7416666666666666963, 0.7458333333333333481, 0.7500000000000000000, 0.7541666666666666519, 0.7583333333333333037, 0.7624999999999999556, 0.7666666666666667185, 0.7708333333333333703, 0.7750000000000000222, 0.7791666666666666741, 0.7833333333333333259, 0.7874999999999999778, 0.7916666666666666297, 0.7958333333333332815, 0.8000000000000000444, 0.8041666666666666963, 0.8083333333333333481, 0.8125000000000000000, 0.8166666666666666519, 0.8208333333333333037, 0.8249999999999999556, 0.8291666666666667185, 0.8333333333333333703, 0.8375000000000000222, 0.8416666666666666741, 0.8458333333333333259, 0.8499999999999999778, 0.8541666666666666297, 0.8583333333333332815, 0.8625000000000000444, 0.8666666666666666963, 0.8708333333333333481, 0.8750000000000000000, 0.8791666666666666519, 0.8833333333333333037, 0.8874999999999999556, 0.8916666666666667185, 0.8958333333333333703, 0.9000000000000000222, 0.9041666666666666741, 0.9083333333333333259, 0.9124999999999999778, 0.9166666666666666297, 0.9208333333333332815, 0.9250000000000000444, 0.9291666666666666963, 0.9333333333333333481, 0.9375000000000000000, 0.9416666666666666519, 0.9458333333333333037, 0.9499999999999999556, 0.9541666666666667185, 0.9583333333333333703, 0.9625000000000000222, 0.9666666666666666741, 0.9708333333333333259, 0.9749999999999999778, 0.9791666666666666297, 0.9833333333333332815, 0.9875000000000000444, 0.9916666666666666963, 0.9958333333333333481, 1.000000000000000000 ),
 .UNSPECIFIED. ) 
 GEOMETRIC_REPRESENTATION_ITEM ( )  RATIONAL_B_SPLINE_SURFACE ( (
 ( 1.000000000000000000, 0.9238795325112867385, 1.000000000000000000, 0.9238795325112867385, 1.000000000000000000, 0.9238795325112867385, 1.000000000000000000, 0.9238795325112867385, 1.000000000000000000, 0.9238795325112867385, 1.000000000000000000, 0.9238795325112867385, 1.000000000000000000, 0.9238795325112867385, 1.000000000000000000, 0.9238795325112867385, 1.000000000000000000, 0.9238795325112867385, 1.000000000000000000, 0.9238795325112867385, 1.000000000000000000, 0.9238795325112867385, 1.000000000000000000, 0.9238795325112867385, 1.000000000000000000, 0.9238795325112867385, 1.000000000000000000, 0.9238795325112867385, 1.000000000000000000, 0.9238795325112867385, 1.000000000000000000, 0.9238795325112867385, 1.000000000000000000, 0.9238795325112867385, 1.000000000000000000, 0.9238795325112867385, 1.000000000000000000, 0.9238795325112867385, 1.000000000000000000, 0.9238795325112867385, 1.000000000000000000, 0.9238795325112867385, 1.000000000000000000, 0.9238795325112867385, 1.000000000000000000, 0.9238795325112867385, 1.000000000000000000, 0.9238795325112867385, 1.000000000000000000, 0.9238795325112867385, 1.000000000000000000, 0.9238795325112867385, 1.000000000000000000, 0.9238795325112867385, 1.000000000000000000, 0.9238795325112867385, 1.000000000000000000, 0.9238795325112867385, 1.000000000000000000, 0.9238795325112867385, 1.000000000000000000, 0.9238795325112867385, 1.000000000000000000, 0.9238795325112867385, 1.000000000000000000, 0.9238795325112867385, 1.000000000000000000, 0.9238795325112867385, 1.000000000000000000, 0.9238795325112867385, 1.000000000000000000, 0.9238795325112867385, 1.000000000000000000, 0.9238795325112867385, 1.000000000000000000, 0.9238795325112867385, 1.000000000000000000, 0.9238795325112867385, 1.000000000000000000, 0.9238795325112867385, 1.000000000000000000, 0.9238795325112867385, 1.000000000000000000, 0.9238795325112867385, 1.000000000000000000, 0.9238795325112867385, 1.000000000000000000, 0.9238795325112867385, 1.000000000000000000, 0.9238795325112867385, 1.000000000000000000, 0.9238795325112867385, 1.000000000000000000, 0.9238795325112867385, 1.000000000000000000, 0.9238795325112867385, 1.000000000000000000, 0.9238795325112867385, 1.000000000000000000, 0.9238795325112867385, 1.000000000000000000, 0.9238795325112867385, 1.000000000000000000, 0.9238795325112867385, 1.000000000000000000, 0.9238795325112867385, 1.000000000000000000, 0.9238795325112867385, 1.000000000000000000, 0.9238795325112867385, 1.000000000000000000, 0.9238795325112867385, 1.000000000000000000, 0.9238795325112867385, 1.000000000000000000, 0.9238795325112867385, 1.000000000000000000, 0.9238795325112867385, 1.000000000000000000, 0.9238795325112867385, 1.000000000000000000, 0.9238795325112867385, 1.000000000000000000, 0.9238795325112867385, 1.000000000000000000, 0.9238795325112867385, 1.000000000000000000, 0.9238795325112867385, 1.000000000000000000, 0.9238795325112867385, 1.000000000000000000, 0.9238795325112867385, 1.000000000000000000, 0.9238795325112867385, 1.000000000000000000, 0.9238795325112867385, 1.000000000000000000, 0.9238795325112867385, 1.000000000000000000, 0.9238795325112867385, 1.000000000000000000, 0.9238795325112867385, 1.000000000000000000, 0.9238795325112867385, 1.000000000000000000, 0.9238795325112867385, 1.000000000000000000, 0.9238795325112867385, 1.000000000000000000, 0.9238795325112867385, 1.000000000000000000, 0.9238795325112867385, 1.000000000000000000, 0.9238795325112867385, 1.000000000000000000, 0.9238795325112867385, 1.000000000000000000, 0.9238795325112867385, 1.000000000000000000, 0.9238795325112867385, 1.000000000000000000, 0.9238795325112867385, 1.000000000000000000, 0.9238795325112867385, 1.000000000000000000, 0.9238795325112867385, 1.000000000000000000, 0.9238795325112867385, 1.000000000000000000, 0.9238795325112867385, 1.000000000000000000, 0.9238795325112867385, 1.000000000000000000, 0.9238795325112867385, 1.000000000000000000, 0.9238795325112867385, 1.000000000000000000, 0.9238795325112867385, 1.000000000000000000, 0.9238795325112867385, 1.000000000000000000, 0.9238795325112867385, 1.000000000000000000, 0.9238795325112867385, 1.000000000000000000, 0.9238795325112867385, 1.000000000000000000, 0.9238795325112867385, 1.000000000000000000, 0.9238795325112867385, 1.000000000000000000, 0.9238795325112867385, 1.000000000000000000, 0.9238795325112867385, 1.000000000000000000, 0.9238795325112867385, 1.000000000000000000, 0.9238795325112867385, 1.000000000000000000, 0.9238795325112867385, 1.000000000000000000, 0.9238795325112867385, 1.000000000000000000, 0.9238795325112867385, 1.000000000000000000, 0.9238795325112867385, 1.000000000000000000, 0.9238795325112867385, 1.000000000000000000, 0.9238795325112867385, 1.000000000000000000, 0.9238795325112867385, 1.000000000000000000, 0.9238795325112867385, 1.000000000000000000, 0.9238795325112867385, 1.000000000000000000, 0.9238795325112867385, 1.000000000000000000, 0.9238795325112867385, 1.000000000000000000, 0.9238795325112867385, 1.000000000000000000, 0.9238795325112867385, 1.000000000000000000, 0.9238795325112867385, 1.000000000000000000, 0.9238795325112867385, 1.000000000000000000, 0.9238795325112867385, 1.000000000000000000, 0.9238795325112867385, 1.000000000000000000, 0.9238795325112867385, 1.000000000000000000, 0.9238795325112867385, 1.000000000000000000, 0.9238795325112867385, 1.000000000000000000, 0.9238795325112867385, 1.000000000000000000, 0.9238795325112867385, 1.000000000000000000, 0.9238795325112867385, 1.000000000000000000, 0.9238795325112867385, 1.000000000000000000, 0.9238795325112867385, 1.000000000000000000, 0.9238795325112867385, 1.000000000000000000, 0.9238795325112867385, 1.000000000000000000, 0.9238795325112867385, 1.000000000000000000, 0.9238795325112867385, 1.000000000000000000, 0.9238795325112867385, 1.000000000000000000, 0.9238795325112867385, 1.000000000000000000, 0.9238795325112867385, 1.000000000000000000, 0.9238795325112867385, 1.000000000000000000, 0.9238795325112867385, 1.000000000000000000, 0.9238795325112867385, 1.000000000000000000, 0.9238795325112867385, 1.000000000000000000, 0.9238795325112867385, 1.000000000000000000, 0.9238795325112867385, 1.000000000000000000, 0.9238795325112867385, 1.000000000000000000, 0.9238795325112867385, 1.000000000000000000, 0.9238795325112867385, 1.000000000000000000, 0.9238795325112867385, 1.000000000000000000, 0.9238795325112867385, 1.000000000000000000, 0.9238795325112867385, 1.000000000000000000, 0.9238795325112867385, 1.000000000000000000, 0.9238795325112867385, 1.000000000000000000, 0.9238795325112867385, 1.000000000000000000, 0.9238795325112867385, 1.000000000000000000, 0.9238795325112867385, 1.000000000000000000, 0.9238795325112867385, 1.000000000000000000, 0.9238795325112867385, 1.000000000000000000, 0.9238795325112867385, 1.000000000000000000, 0.9238795325112867385, 1.000000000000000000, 0.9238795325112867385, 1.000000000000000000, 0.9238795325112867385, 1.000000000000000000, 0.9238795325112867385, 1.000000000000000000, 0.9238795325112867385, 1.000000000000000000, 0.9238795325112867385, 1.000000000000000000, 0.9238795325112867385, 1.000000000000000000, 0.9238795325112867385, 1.000000000000000000, 0.9238795325112867385, 1.000000000000000000, 0.9238795325112867385, 1.000000000000000000, 0.9238795325112867385, 1.000000000000000000, 0.9238795325112867385, 1.000000000000000000, 0.9238795325112867385, 1.000000000000000000, 0.9238795325112867385, 1.000000000000000000, 0.9238795325112867385, 1.000000000000000000, 0.9238795325112867385, 1.000000000000000000, 0.9238795325112867385, 1.000000000000000000, 0.9238795325112867385, 1.000000000000000000, 0.9238795325112867385, 1.000000000000000000, 0.9238795325112867385, 1.000000000000000000, 0.9238795325112867385, 1.000000000000000000, 0.9238795325112867385, 1.000000000000000000, 0.9238795325112867385, 1.000000000000000000, 0.9238795325112867385, 1.000000000000000000, 0.9238795325112867385, 1.000000000000000000, 0.9238795325112867385, 1.000000000000000000, 0.9238795325112867385, 1.000000000000000000, 0.9238795325112867385, 1.000000000000000000, 0.9238795325112867385, 1.000000000000000000, 0.9238795325112867385, 1.000000000000000000, 0.9238795325112867385, 1.000000000000000000, 0.9238795325112867385, 1.000000000000000000, 0.9238795325112867385, 1.000000000000000000, 0.9238795325112867385, 1.000000000000000000, 0.9238795325112867385, 1.000000000000000000, 0.9238795325112867385, 1.000000000000000000, 0.9238795325112867385, 1.000000000000000000, 0.9238795325112867385, 1.000000000000000000, 0.9238795325112867385, 1.000000000000000000, 0.9238795325112867385, 1.000000000000000000, 0.9238795325112867385, 1.000000000000000000, 0.9238795325112867385, 1.000000000000000000, 0.9238795325112867385, 1.000000000000000000, 0.9238795325112867385, 1.000000000000000000, 0.9238795325112867385, 1.000000000000000000, 0.9238795325112867385, 1.000000000000000000, 0.9238795325112867385, 1.000000000000000000, 0.9238795325112867385, 1.000000000000000000, 0.9238795325112867385, 1.000000000000000000, 0.9238795325112867385, 1.000000000000000000, 0.9238795325112867385, 1.000000000000000000, 0.9238795325112867385, 1.000000000000000000, 0.9238795325112867385, 1.000000000000000000, 0.9238795325112867385, 1.000000000000000000, 0.9238795325112867385, 1.000000000000000000, 0.9238795325112867385, 1.000000000000000000, 0.9238795325112867385, 1.000000000000000000, 0.9238795325112867385, 1.000000000000000000, 0.9238795325112867385, 1.000000000000000000, 0.9238795325112867385, 1.000000000000000000, 0.9238795325112867385, 1.000000000000000000, 0.9238795325112867385, 1.000000000000000000, 0.9238795325112867385, 1.000000000000000000, 0.9238795325112867385, 1.000000000000000000, 0.9238795325112867385, 1.000000000000000000, 0.9238795325112867385, 1.000000000000000000, 0.9238795325112867385, 1.000000000000000000, 0.9238795325112867385, 1.000000000000000000, 0.9238795325112867385, 1.000000000000000000, 0.9238795325112867385, 1.000000000000000000, 0.9238795325112867385, 1.000000000000000000, 0.9238795325112867385, 1.000000000000000000, 0.9238795325112867385, 1.000000000000000000, 0.9238795325112867385, 1.000000000000000000, 0.9238795325112867385, 1.000000000000000000, 0.9238795325112867385, 1.000000000000000000, 0.9238795325112867385, 1.000000000000000000, 0.9238795325112867385, 1.000000000000000000, 0.9238795325112867385, 1.000000000000000000, 0.9238795325112867385, 1.000000000000000000, 0.9238795325112867385, 1.000000000000000000, 0.9238795325112867385, 1.000000000000000000, 0.9238795325112867385, 1.000000000000000000, 0.9238795325112867385, 1.000000000000000000, 0.9238795325112867385, 1.000000000000000000, 0.9238795325112867385, 1.000000000000000000, 0.9238795325112867385, 1.000000000000000000, 0.9238795325112867385, 1.000000000000000000, 0.9238795325112867385, 1.000000000000000000),
 ( 1.000000000000000000, 0.9238795325112867385, 1.000000000000000000, 0.9238795325112867385, 1.000000000000000000, 0.9238795325112867385, 1.000000000000000000, 0.9238795325112867385, 1.000000000000000000, 0.9238795325112867385, 1.000000000000000000, 0.9238795325112867385, 1.000000000000000000, 0.9238795325112867385, 1.000000000000000000, 0.9238795325112867385, 1.000000000000000000, 0.9238795325112867385, 1.000000000000000000, 0.9238795325112867385, 1.000000000000000000, 0.9238795325112867385, 1.000000000000000000, 0.9238795325112867385, 1.000000000000000000, 0.9238795325112867385, 1.000000000000000000, 0.9238795325112867385, 1.000000000000000000, 0.9238795325112867385, 1.000000000000000000, 0.9238795325112867385, 1.000000000000000000, 0.9238795325112867385, 1.000000000000000000, 0.9238795325112867385, 1.000000000000000000, 0.9238795325112867385, 1.000000000000000000, 0.9238795325112867385, 1.000000000000000000, 0.9238795325112867385, 1.000000000000000000, 0.9238795325112867385, 1.000000000000000000, 0.9238795325112867385, 1.000000000000000000, 0.9238795325112867385, 1.000000000000000000, 0.9238795325112867385, 1.000000000000000000, 0.9238795325112867385, 1.000000000000000000, 0.9238795325112867385, 1.000000000000000000, 0.9238795325112867385, 1.000000000000000000, 0.9238795325112867385, 1.000000000000000000, 0.9238795325112867385, 1.000000000000000000, 0.9238795325112867385, 1.000000000000000000, 0.9238795325112867385, 1.000000000000000000, 0.9238795325112867385, 1.000000000000000000, 0.9238795325112867385, 1.000000000000000000, 0.9238795325112867385, 1.000000000000000000, 0.9238795325112867385, 1.000000000000000000, 0.9238795325112867385, 1.000000000000000000, 0.9238795325112867385, 1.000000000000000000, 0.9238795325112867385, 1.000000000000000000, 0.9238795325112867385, 1.000000000000000000, 0.9238795325112867385, 1.000000000000000000, 0.9238795325112867385, 1.000000000000000000, 0.9238795325112867385, 1.000000000000000000, 0.9238795325112867385, 1.000000000000000000, 0.9238795325112867385, 1.000000000000000000, 0.9238795325112867385, 1.000000000000000000, 0.9238795325112867385, 1.000000000000000000, 0.9238795325112867385, 1.000000000000000000, 0.9238795325112867385, 1.000000000000000000, 0.9238795325112867385, 1.000000000000000000, 0.9238795325112867385, 1.000000000000000000, 0.9238795325112867385, 1.000000000000000000, 0.9238795325112867385, 1.000000000000000000, 0.9238795325112867385, 1.000000000000000000, 0.9238795325112867385, 1.000000000000000000, 0.9238795325112867385, 1.000000000000000000, 0.9238795325112867385, 1.000000000000000000, 0.9238795325112867385, 1.000000000000000000, 0.9238795325112867385, 1.000000000000000000, 0.9238795325112867385, 1.000000000000000000, 0.9238795325112867385, 1.000000000000000000, 0.9238795325112867385, 1.000000000000000000, 0.9238795325112867385, 1.000000000000000000, 0.9238795325112867385, 1.000000000000000000, 0.9238795325112867385, 1.000000000000000000, 0.9238795325112867385, 1.000000000000000000, 0.9238795325112867385, 1.000000000000000000, 0.9238795325112867385, 1.000000000000000000, 0.9238795325112867385, 1.000000000000000000, 0.9238795325112867385, 1.000000000000000000, 0.9238795325112867385, 1.000000000000000000, 0.9238795325112867385, 1.000000000000000000, 0.9238795325112867385, 1.000000000000000000, 0.9238795325112867385, 1.000000000000000000, 0.9238795325112867385, 1.000000000000000000, 0.9238795325112867385, 1.000000000000000000, 0.9238795325112867385, 1.000000000000000000, 0.9238795325112867385, 1.000000000000000000, 0.9238795325112867385, 1.000000000000000000, 0.9238795325112867385, 1.000000000000000000, 0.9238795325112867385, 1.000000000000000000, 0.9238795325112867385, 1.000000000000000000, 0.9238795325112867385, 1.000000000000000000, 0.9238795325112867385, 1.000000000000000000, 0.9238795325112867385, 1.000000000000000000, 0.9238795325112867385, 1.000000000000000000, 0.9238795325112867385, 1.000000000000000000, 0.9238795325112867385, 1.000000000000000000, 0.9238795325112867385, 1.000000000000000000, 0.9238795325112867385, 1.000000000000000000, 0.9238795325112867385, 1.000000000000000000, 0.9238795325112867385, 1.000000000000000000, 0.9238795325112867385, 1.000000000000000000, 0.9238795325112867385, 1.000000000000000000, 0.9238795325112867385, 1.000000000000000000, 0.9238795325112867385, 1.000000000000000000, 0.9238795325112867385, 1.000000000000000000, 0.9238795325112867385, 1.000000000000000000, 0.9238795325112867385, 1.000000000000000000, 0.9238795325112867385, 1.000000000000000000, 0.9238795325112867385, 1.000000000000000000, 0.9238795325112867385, 1.000000000000000000, 0.9238795325112867385, 1.000000000000000000, 0.9238795325112867385, 1.000000000000000000, 0.9238795325112867385, 1.000000000000000000, 0.9238795325112867385, 1.000000000000000000, 0.9238795325112867385, 1.000000000000000000, 0.9238795325112867385, 1.000000000000000000, 0.9238795325112867385, 1.000000000000000000, 0.9238795325112867385, 1.000000000000000000, 0.9238795325112867385, 1.000000000000000000, 0.9238795325112867385, 1.000000000000000000, 0.9238795325112867385, 1.000000000000000000, 0.9238795325112867385, 1.000000000000000000, 0.9238795325112867385, 1.000000000000000000, 0.9238795325112867385, 1.000000000000000000, 0.9238795325112867385, 1.000000000000000000, 0.9238795325112867385, 1.000000000000000000, 0.9238795325112867385, 1.000000000000000000, 0.9238795325112867385, 1.000000000000000000, 0.9238795325112867385, 1.000000000000000000, 0.9238795325112867385, 1.000000000000000000, 0.9238795325112867385, 1.000000000000000000, 0.9238795325112867385, 1.000000000000000000, 0.9238795325112867385, 1.000000000000000000, 0.9238795325112867385, 1.000000000000000000, 0.9238795325112867385, 1.000000000000000000, 0.9238795325112867385, 1.000000000000000000, 0.9238795325112867385, 1.000000000000000000, 0.9238795325112867385, 1.000000000000000000, 0.9238795325112867385, 1.000000000000000000, 0.9238795325112867385, 1.000000000000000000, 0.9238795325112867385, 1.000000000000000000, 0.9238795325112867385, 1.000000000000000000, 0.9238795325112867385, 1.000000000000000000, 0.9238795325112867385, 1.000000000000000000, 0.9238795325112867385, 1.000000000000000000, 0.9238795325112867385, 1.000000000000000000, 0.9238795325112867385, 1.000000000000000000, 0.9238795325112867385, 1.000000000000000000, 0.9238795325112867385, 1.000000000000000000, 0.9238795325112867385, 1.000000000000000000, 0.9238795325112867385, 1.000000000000000000, 0.9238795325112867385, 1.000000000000000000, 0.9238795325112867385, 1.000000000000000000, 0.9238795325112867385, 1.000000000000000000, 0.9238795325112867385, 1.000000000000000000, 0.9238795325112867385, 1.000000000000000000, 0.9238795325112867385, 1.000000000000000000, 0.9238795325112867385, 1.000000000000000000, 0.9238795325112867385, 1.000000000000000000, 0.9238795325112867385, 1.000000000000000000, 0.9238795325112867385, 1.000000000000000000, 0.9238795325112867385, 1.000000000000000000, 0.9238795325112867385, 1.000000000000000000, 0.9238795325112867385, 1.000000000000000000, 0.9238795325112867385, 1.000000000000000000, 0.9238795325112867385, 1.000000000000000000, 0.9238795325112867385, 1.000000000000000000, 0.9238795325112867385, 1.000000000000000000, 0.9238795325112867385, 1.000000000000000000, 0.9238795325112867385, 1.000000000000000000, 0.9238795325112867385, 1.000000000000000000, 0.9238795325112867385, 1.000000000000000000, 0.9238795325112867385, 1.000000000000000000, 0.9238795325112867385, 1.000000000000000000, 0.9238795325112867385, 1.000000000000000000, 0.9238795325112867385, 1.000000000000000000, 0.9238795325112867385, 1.000000000000000000, 0.9238795325112867385, 1.000000000000000000, 0.9238795325112867385, 1.000000000000000000, 0.9238795325112867385, 1.000000000000000000, 0.9238795325112867385, 1.000000000000000000, 0.9238795325112867385, 1.000000000000000000, 0.9238795325112867385, 1.000000000000000000, 0.9238795325112867385, 1.000000000000000000, 0.9238795325112867385, 1.000000000000000000, 0.9238795325112867385, 1.000000000000000000, 0.9238795325112867385, 1.000000000000000000, 0.9238795325112867385, 1.000000000000000000, 0.9238795325112867385, 1.000000000000000000, 0.9238795325112867385, 1.000000000000000000, 0.9238795325112867385, 1.000000000000000000, 0.9238795325112867385, 1.000000000000000000, 0.9238795325112867385, 1.000000000000000000, 0.9238795325112867385, 1.000000000000000000, 0.9238795325112867385, 1.000000000000000000, 0.9238795325112867385, 1.000000000000000000, 0.9238795325112867385, 1.000000000000000000, 0.9238795325112867385, 1.000000000000000000, 0.9238795325112867385, 1.000000000000000000, 0.9238795325112867385, 1.000000000000000000, 0.9238795325112867385, 1.000000000000000000, 0.9238795325112867385, 1.000000000000000000, 0.9238795325112867385, 1.000000000000000000, 0.9238795325112867385, 1.000000000000000000, 0.9238795325112867385, 1.000000000000000000, 0.9238795325112867385, 1.000000000000000000, 0.9238795325112867385, 1.000000000000000000, 0.9238795325112867385, 1.000000000000000000, 0.9238795325112867385, 1.000000000000000000, 0.9238795325112867385, 1.000000000000000000, 0.9238795325112867385, 1.000000000000000000, 0.9238795325112867385, 1.000000000000000000, 0.9238795325112867385, 1.000000000000000000, 0.9238795325112867385, 1.000000000000000000, 0.9238795325112867385, 1.000000000000000000, 0.9238795325112867385, 1.000000000000000000, 0.9238795325112867385, 1.000000000000000000, 0.9238795325112867385, 1.000000000000000000, 0.9238795325112867385, 1.000000000000000000, 0.9238795325112867385, 1.000000000000000000, 0.9238795325112867385, 1.000000000000000000, 0.9238795325112867385, 1.000000000000000000, 0.9238795325112867385, 1.000000000000000000, 0.9238795325112867385, 1.000000000000000000, 0.9238795325112867385, 1.000000000000000000, 0.9238795325112867385, 1.000000000000000000, 0.9238795325112867385, 1.000000000000000000, 0.9238795325112867385, 1.000000000000000000, 0.9238795325112867385, 1.000000000000000000, 0.9238795325112867385, 1.000000000000000000, 0.9238795325112867385, 1.000000000000000000, 0.9238795325112867385, 1.000000000000000000, 0.9238795325112867385, 1.000000000000000000, 0.9238795325112867385, 1.000000000000000000, 0.9238795325112867385, 1.000000000000000000, 0.9238795325112867385, 1.000000000000000000, 0.9238795325112867385, 1.000000000000000000, 0.9238795325112867385, 1.000000000000000000, 0.9238795325112867385, 1.000000000000000000, 0.9238795325112867385, 1.000000000000000000, 0.9238795325112867385, 1.000000000000000000, 0.9238795325112867385, 1.000000000000000000, 0.9238795325112867385, 1.000000000000000000, 0.9238795325112867385, 1.000000000000000000, 0.9238795325112867385, 1.000000000000000000, 0.9238795325112867385, 1.000000000000000000, 0.9238795325112867385, 1.000000000000000000, 0.9238795325112867385, 1.000000000000000000) ) ) 
 REPRESENTATION_ITEM ( '' )  SURFACE ( )  );
#17064 = DIRECTION ( 'NONE',  ( -0.000000000000000000, 1.000000000000000000, -0.000000000000000000 ) ) ;
#17065 = CARTESIAN_POINT ( 'NONE',  ( 4.458734124999998549, -34.72916666530107221, -2.574251347313721627 ) ) ;
#17066 = FACE_OUTER_BOUND ( 'NONE', #52238, .T. ) ;
#17067 = CARTESIAN_POINT ( 'NONE',  ( -4.458734124999999437, -60.56249999863440081, 0.000000000000000000 ) ) ;
#17068 = CARTESIAN_POINT ( 'NONE',  ( 5.000000000000000000, -51.41666666666666430, -2.886751345948129988 ) ) ;
#17069 = CARTESIAN_POINT ( 'NONE',  ( -4.999999999999998224, -40.91666666666667140, 2.886751345948131764 ) ) ;
#17070 = DIRECTION ( 'NONE',  ( 0.4999999999999948930, 0.000000000000000000, -0.8660254037844415942 ) ) ;
#17071 = VERTEX_POINT ( 'NONE', #16366 ) ;
#17072 = CARTESIAN_POINT ( 'NONE',  ( 4.458734124999999437, -105.8124999986344221, -5.460374474430324690E-16 ) ) ;
#17073 = CARTESIAN_POINT ( 'NONE',  ( -2.229367062500000163, 0.2708333346989263979, -3.861377020970580443 ) ) ;
#17074 = CARTESIAN_POINT ( 'NONE',  ( 1.975475456537005874E-15, 23.37500000273118417, 5.000000000000000000 ) ) ;
#17075 = CARTESIAN_POINT ( 'NONE',  ( -3.535250795749689387E-16, -5.249999999999997335, -5.773502691896257311 ) ) ;
#17076 = CARTESIAN_POINT ( 'NONE',  ( -3.152548672688508926E-16, -69.56249999863439371, -5.148502694627439702 ) ) ;
#17078 = CARTESIAN_POINT ( 'NONE',  ( -2.500000000000000444, -31.04166666393548368, -4.330127018922193649 ) ) ;
#17077 =( BOUNDED_CURVE ( )  B_SPLINE_CURVE ( 2, ( #22860, #56952, #2300, #52121, #46343, #18010, #42451, #60830, #8064 ),
 .UNSPECIFIED., .F., .F. ) 
 B_SPLINE_CURVE_WITH_KNOTS ( ( 3, 2, 2, 2, 3 ),
 ( 0.9196428571428570953, 0.9202380952380951884, 0.9214285714285713746, 0.9226190476190476719, 0.9232142857142857650 ),
 .UNSPECIFIED. ) 
 CURVE ( )  GEOMETRIC_REPRESENTATION_ITEM ( )  RATIONAL_B_SPLINE_CURVE ( ( 0.9330127018922194093, 0.9330127018922194093, 1.000000000000000000, 0.8660254037844387076, 1.000000000000000000, 0.8660254037844387076, 1.000000000000000000, 0.9330127018922194093, 0.9330127018922194093 ) ) 
 REPRESENTATION_ITEM ( '' )  );
#17079 = CARTESIAN_POINT ( 'NONE',  ( -3.535250795749689387E-16, -11.12499999726881761, -5.773502691896257311 ) ) ;
#17081 = VERTEX_POINT ( 'NONE', #959 ) ;
#17080 = CARTESIAN_POINT ( 'NONE',  ( 4.458734125000001214, -39.89583333196772941, 2.574251347313718519 ) ) ;
#17082 = FACE_OUTER_BOUND ( 'NONE', #60665, .T. ) ;
#17084 = ORIENTED_EDGE ( 'NONE', *, *, #60657, .F. ) ;
#17083 = CARTESIAN_POINT ( 'NONE',  ( 2.229367062499998831, 13.10416666803226171, -3.861377020970580887 ) ) ;
#17085 = CARTESIAN_POINT ( 'NONE',  ( 5.000000000000000000, -81.50000000000000000, -6.123233995736766282E-16 ) ) ;
#17086 = CARTESIAN_POINT ( 'NONE',  ( 2.499999999999998668, -56.33333333333333570, -4.330127018922193649 ) ) ;
#17087 = CARTESIAN_POINT ( 'NONE',  ( -4.458734124999999437, -160.1875000013655779, -5.460374474430324690E-16 ) ) ;
#17088 = CARTESIAN_POINT ( 'NONE',  ( -4.458734124999999437, -33.64583333196772941, -2.574251347313719407 ) ) ;
#17089 = CARTESIAN_POINT ( 'NONE',  ( -4.999999999999998224, -86.91666666666667140, 2.886751345948131764 ) ) ;
#17090 = CARTESIAN_POINT ( 'NONE',  ( -2.229367062500000163, -79.47916666530106511, -3.861377020970580443 ) ) ;
#17091 = CARTESIAN_POINT ( 'NONE',  ( 1.846868145590735200, -140.5000000013656347, -4.458734125000000326 ) ) ;
#17092 = CARTESIAN_POINT ( 'NONE',  ( 2.229367062499998831, -86.64583333196773651, -3.861377020970580887 ) ) ;
#17093 = CARTESIAN_POINT ( 'NONE',  ( -52.80376928212989185, -134.1250000013656347, -4.297418129356379346 ) ) ;
#17094 = CARTESIAN_POINT ( 'NONE',  ( -4.458734124999999437, -2.645833331967737845, -2.574251347313719407 ) ) ;
#17095 = CARTESIAN_POINT ( 'NONE',  ( -4.458734124999998549, -34.47916666530107221, 2.574251347313722516 ) ) ;
#17096 = CARTESIAN_POINT ( 'NONE',  ( -6.972266317189433020E-16, -16.12499999726881228, -5.000000000000000000 ) ) ;
#17097 = CARTESIAN_POINT ( 'NONE',  ( -3.152548672688508926E-16, -79.81249999863440792, -5.148502694627439702 ) ) ;
#17098 = CARTESIAN_POINT ( 'NONE',  ( 5.000000000000000000, 3.499999999999999556, -6.123233995736766282E-16 ) ) ;
#17099 = ORIENTED_EDGE ( 'NONE', *, *, #46857, .F. ) ;
#17100 = FACE_OUTER_BOUND ( 'NONE', #9333, .T. ) ;
#17101 = DIRECTION ( 'NONE',  ( -0.000000000000000000, 1.000000000000000000, -0.000000000000000000 ) ) ;
#17102 = CARTESIAN_POINT ( 'NONE',  ( -4.458734124999999437, -68.64583333196773651, -2.574251347313719407 ) ) ;
#17103 = CARTESIAN_POINT ( 'NONE',  ( -2.229367062499996610, -10.39583333196773829, 3.861377020970582219 ) ) ;
#17104 = ORIENTED_EDGE ( 'NONE', *, *, #3872, .T. ) ;
#17105 = CARTESIAN_POINT ( 'NONE',  ( -6.972266317189433020E-16, -5.249999999999998224, -5.000000000000000000 ) ) ;
#17106 = CARTESIAN_POINT ( 'NONE',  ( -5.000000000000000888, -146.5625000027311842, 2.071067811865474617 ) ) ;
#17107 = CARTESIAN_POINT ( 'NONE',  ( -4.458734124999998549, -4.479166665301070438, 2.574251347313722516 ) ) ;
#17108 = DIRECTION ( 'NONE',  ( -0.000000000000000000, 1.000000000000000000, -0.000000000000000000 ) ) ;
#17109 = CARTESIAN_POINT ( 'NONE',  ( 4.458734124999998549, 7.270833334698928674, -2.574251347313721627 ) ) ;
#17110 = DIRECTION ( 'NONE',  ( -0.000000000000000000, 1.000000000000000000, -0.000000000000000000 ) ) ;
#17111 = CARTESIAN_POINT ( 'NONE',  ( 1.846868145590736310, -155.6250000013655779, 4.458734124999997661 ) ) ;
#17112 = DIRECTION ( 'NONE',  ( -0.000000000000000000, 1.000000000000000000, -0.000000000000000000 ) ) ;
#17113 = VERTEX_POINT ( 'NONE', #10893 ) ;
#17114 = CARTESIAN_POINT ( 'NONE',  ( -2.229367062499996610, -85.14583333196773651, 3.861377020970582219 ) ) ;
#17115 = CARTESIAN_POINT ( 'NONE',  ( 1.975475456537005874E-15, -20.62499999726881228, 5.000000000000000000 ) ) ;
#17116 = CARTESIAN_POINT ( 'NONE',  ( 4.458734125000001214, -3.895833331967739621, 2.574251347313718519 ) ) ;
#17117 = LINE ( 'NONE', #61830, #58078 ) ;
#17118 = CARTESIAN_POINT ( 'NONE',  ( -5.000000000000000000, -31.95833333060214443, -2.886751345948128211 ) ) ;
#17119 = LINE ( 'NONE', #51229, #36805 ) ;
#17120 = CARTESIAN_POINT ( 'NONE',  ( -4.458734124999997661, 25.77083333469893134, 2.574251347313722516 ) ) ;
#17121 = CARTESIAN_POINT ( 'NONE',  ( 1.975475456537005874E-15, -10.75000000000000000, 5.000000000000000000 ) ) ;
#17122 = CARTESIAN_POINT ( 'NONE',  ( 5.000000000000000888, -82.45833333060214443, 2.886751345948126879 ) ) ;
#17123 = CARTESIAN_POINT ( 'NONE',  ( -2.229367062499996610, -50.14583333196772941, 3.861377020970582219 ) ) ;
#17124 = CARTESIAN_POINT ( 'NONE',  ( 9.457646018065525792E-16, -38.31249999863440792, 5.148502694627439702 ) ) ;
#17125 = CARTESIAN_POINT ( 'NONE',  ( 9.457646018065525792E-16, -5.312499998634401699, 5.148502694627439702 ) ) ;
#17126 =( BOUNDED_CURVE ( )  B_SPLINE_CURVE ( 2, ( #28214, #22782, #33056, #51732, #3788, #23410, #16996, #32096, #2846 ),
 .UNSPECIFIED., .F., .F. ) 
 B_SPLINE_CURVE_WITH_KNOTS ( ( 3, 2, 2, 2, 3 ),
 ( 0.3375000000000000222, 0.3380952380952381153, 0.3392857142857143016, 0.3404761904761904878, 0.3410714285714285809 ),
 .UNSPECIFIED. ) 
 CURVE ( )  GEOMETRIC_REPRESENTATION_ITEM ( )  RATIONAL_B_SPLINE_CURVE ( ( 0.9330127018922194093, 0.9330127018922194093, 1.000000000000000000, 0.8660254037844387076, 1.000000000000000000, 0.8660254037844387076, 1.000000000000000000, 0.9330127018922194093, 0.9330127018922194093 ) ) 
 REPRESENTATION_ITEM ( '' )  );
#17127 = AXIS2_PLACEMENT_3D ( 'NONE', #34367, #44016, #9925 ) ;
#17128 = CARTESIAN_POINT ( 'NONE',  ( 6.158835246850667461E-14, 8.875000002731182391, -4.999999999999999112 ) ) ;
#17129 = CARTESIAN_POINT ( 'NONE',  ( -4.999999999999999112, 14.08333333333333393, 2.886751345948131764 ) ) ;
#17130 = CARTESIAN_POINT ( 'NONE',  ( -3.535533905932738641, -142.5000000027311842, 3.535533905932737309 ) ) ;
#17131 = DIRECTION ( 'NONE',  ( 0.000000000000000000, 0.000000000000000000, 1.000000000000000000 ) ) ;
#17132 = CARTESIAN_POINT ( 'NONE',  ( 4.458734125000001214, -42.89583333196773651, 2.574251347313718519 ) ) ;
#17133 = CARTESIAN_POINT ( 'NONE',  ( 1.060575238724906964E-15, -76.62499999726881583, 5.773502691896257311 ) ) ;
#17134 = AXIS2_PLACEMENT_3D ( 'NONE', #34709, #44347, #48859 ) ;
#17135 = VECTOR ( 'NONE', #36815, 1000.000000000000000 ) ;
#17136 = CARTESIAN_POINT ( 'NONE',  ( -52.10840900171896806, -139.4375000013656063, 3.393966926194110556 ) ) ;
#17137 = CARTESIAN_POINT ( 'NONE',  ( -6.972266317189433020E-16, -27.24999999999999645, -5.000000000000000000 ) ) ;
#17138 = CARTESIAN_POINT ( 'NONE',  ( 1.975475456537005874E-15, -76.62499999726880162, 5.000000000000000000 ) ) ;
#17139 = CARTESIAN_POINT ( 'NONE',  ( -4.458734124999999437, -83.56249999863439371, 0.000000000000000000 ) ) ;
#17140 = CARTESIAN_POINT ( 'NONE',  ( -4.458734124999999437, -163.1875000013655779, -5.460374474430324690E-16 ) ) ;
#17141 = CARTESIAN_POINT ( 'NONE',  ( -2.499999999999996447, -31.83333333333333215, 4.330127018922195425 ) ) ;
#17142 = CARTESIAN_POINT ( 'NONE',  ( -5.000000000000000000, -56.99999999999999289, 0.000000000000000000 ) ) ;
#17143 = ORIENTED_EDGE ( 'NONE', *, *, #14577, .F. ) ;
#17144 = CARTESIAN_POINT ( 'NONE',  ( 4.458734125000001214, 15.85416666803226171, 2.574251347313718519 ) ) ;
#17145 = ORIENTED_EDGE ( 'NONE', *, *, #30747, .F. ) ;
#17146 = CARTESIAN_POINT ( 'NONE',  ( -4.458734124999999437, -88.39583333196773651, -2.574251347313719407 ) ) ;
#17147 = CARTESIAN_POINT ( 'NONE',  ( 4.458734124999998549, 11.02083333469892779, -2.574251347313721627 ) ) ;
#17148 = CARTESIAN_POINT ( 'NONE',  ( -2.500000000000000444, 13.95833333606451809, -4.330127018922193649 ) ) ;
#17149 = CARTESIAN_POINT ( 'NONE',  ( 5.000000000000000000, -16.50000000000000000, -6.123233995736766282E-16 ) ) ;
#17150 = CARTESIAN_POINT ( 'NONE',  ( -2.499999999999996447, 6.166666666666667851, 4.330127018922195425 ) ) ;
#17151 = CARTESIAN_POINT ( 'NONE',  ( -4.458734124999999437, -54.39583333196773651, -2.574251347313719407 ) ) ;
#17152 = CARTESIAN_POINT ( 'NONE',  ( 2.499999999999998668, -6.333333333333336590, -4.330127018922193649 ) ) ;
#17153 = CARTESIAN_POINT ( 'NONE',  ( -1.339745962155613812, -52.20534180126148271, -5.000000000000000000 ) ) ;
#17154 = CARTESIAN_POINT ( 'NONE',  ( 0.000000000000000000, -170.0000000000000000, 5.000000000000000000 ) ) ;
#17155 = CARTESIAN_POINT ( 'NONE',  ( -5.000000000000000000, -64.00000000000000000, 0.000000000000000000 ) ) ;
#17156 = DIRECTION ( 'NONE',  ( -0.000000000000000000, 1.000000000000000000, -0.000000000000000000 ) ) ;
#17157 = CARTESIAN_POINT ( 'NONE',  ( -2.500000000000000444, -39.16666666666667140, -4.330127018922193649 ) ) ;
#17158 = CARTESIAN_POINT ( 'NONE',  ( 2.500000000000002220, -107.6666666666666572, 4.330127018922192761 ) ) ;
#17159 =( BOUNDED_CURVE ( )  B_SPLINE_CURVE ( 2, ( #52564, #8497, #47722, #3680, #3989, #23294, #18462, #33254, #52874 ),
 .UNSPECIFIED., .F., .F. ) 
 B_SPLINE_CURVE_WITH_KNOTS ( ( 3, 2, 2, 2, 3 ),
 ( 0.5089285714285713969, 0.5095238095238094900, 0.5107142857142856762, 0.5119047619047618625, 0.5124999999999999556 ),
 .UNSPECIFIED. ) 
 CURVE ( )  GEOMETRIC_REPRESENTATION_ITEM ( )  RATIONAL_B_SPLINE_CURVE ( ( 0.9330127018922194093, 0.9330127018922194093, 1.000000000000000000, 0.8660254037844387076, 1.000000000000000000, 0.8660254037844387076, 1.000000000000000000, 0.9330127018922194093, 0.9330127018922194093 ) ) 
 REPRESENTATION_ITEM ( '' )  );
#17160 = CARTESIAN_POINT ( 'NONE',  ( 4.458734124999998549, -12.97916666530107044, -2.574251347313721627 ) ) ;
#17161 = CARTESIAN_POINT ( 'NONE',  ( -3.152548672688508926E-16, -63.56249999863440792, -5.148502694627439702 ) ) ;
#17162 = CARTESIAN_POINT ( 'NONE',  ( -4.458734124999999437, -150.1875000013656063, -5.460374474430324690E-16 ) ) ;
#17163 = CARTESIAN_POINT ( 'NONE',  ( 9.457646018065525792E-16, -72.06249999863439371, 5.148502694627439702 ) ) ;
#17164 = CARTESIAN_POINT ( 'NONE',  ( -50.40829686548195099, -145.2500000013656347, -1.485763867205728284 ) ) ;
#17165 = CARTESIAN_POINT ( 'NONE',  ( -4.458734124999999437, -19.56249999863440081, 0.000000000000000000 ) ) ;
#17166 = CARTESIAN_POINT ( 'NONE',  ( 5.000000000000000000, -60.29166666393546592, -2.886751345948129988 ) ) ;
#17167 = EDGE_LOOP ( 'NONE', ( #31869, #26738, #49910, #16373 ) ) ;
#17168 = CARTESIAN_POINT ( 'NONE',  ( -5.000000000000000000, -49.08333333333332860, -2.886751345948128211 ) ) ;
#17169 = ORIENTED_EDGE ( 'NONE', *, *, #10671, .T. ) ;
#17170 = CARTESIAN_POINT ( 'NONE',  ( -3.152548672688508926E-16, -62.81249999863440792, -5.148502694627439702 ) ) ;
#17171 = DIRECTION ( 'NONE',  ( 0.000000000000000000, 0.000000000000000000, 1.000000000000000000 ) ) ;
#17172 = CARTESIAN_POINT ( 'NONE',  ( 4.458734124999999437, -153.5000000013656063, 1.846868145590737864 ) ) ;
#17173 = ORIENTED_EDGE ( 'NONE', *, *, #51051, .F. ) ;
#17174 = AXIS2_PLACEMENT_3D ( 'NONE', #6853, #2352, #15864 ) ;
#17175 = CARTESIAN_POINT ( 'NONE',  ( -4.999999999999998224, 27.20833333606451276, 2.886751345948131764 ) ) ;
#17176 = CARTESIAN_POINT ( 'NONE',  ( 4.729367062499999719, -169.2812500020484094, 0.000000000000000000 ) ) ;
#17177 = CARTESIAN_POINT ( 'NONE',  ( -5.000000000000000000, -74.87499999726880162, 0.000000000000000000 ) ) ;
#17178 = CARTESIAN_POINT ( 'NONE',  ( -4.458734124999999437, -50.64583333196773651, -2.574251347313719407 ) ) ;
#17179 = ORIENTED_EDGE ( 'NONE', *, *, #35730, .F. ) ;
#17180 = CARTESIAN_POINT ( 'NONE',  ( 1.339745962155615144, 10.41965820146970501, 4.999999999999999112 ) ) ;
#17181 = VECTOR ( 'NONE', #56786, 1000.000000000000000 ) ;
#17182 = CARTESIAN_POINT ( 'NONE',  ( 9.457646018065525792E-16, 9.937500001365592084, 5.148502694627439702 ) ) ;
#17183 = CARTESIAN_POINT ( 'NONE',  ( -4.458734124999998549, 21.77083333469892779, 2.574251347313722516 ) ) ;
#17184 = CARTESIAN_POINT ( 'NONE',  ( -59.29741812935640155, -149.6250000013655779, -2.196230717870135685 ) ) ;
#17185 = CARTESIAN_POINT ( 'NONE',  ( -2.500000000000000444, -24.04166666393548368, -4.330127018922193649 ) ) ;
#17186 = CARTESIAN_POINT ( 'NONE',  ( 3.535533905932738197, -164.8750000000000284, -3.535533905932738197 ) ) ;
#17187 = ORIENTED_EDGE ( 'NONE', *, *, #19220, .T. ) ;
#17188 = CARTESIAN_POINT ( 'NONE',  ( 9.457646018065525792E-16, -73.06249999863439371, 5.148502694627439702 ) ) ;
#17189 = CARTESIAN_POINT ( 'NONE',  ( -1.339745962155613812, -50.08034179853029855, -5.000000000000000000 ) ) ;
#17190 = CARTESIAN_POINT ( 'NONE',  ( -2.229367062499996610, 13.85416666803226171, 3.861377020970582219 ) ) ;
#17191 = CARTESIAN_POINT ( 'NONE',  ( -2.499999999999996447, -41.83333333333333570, 4.330127018922195425 ) ) ;
#17192 = CARTESIAN_POINT ( 'NONE',  ( 9.457646018065525792E-16, -57.31249999863440081, 5.148502694627439702 ) ) ;
#17193 = CARTESIAN_POINT ( 'NONE',  ( -2.499999999999996447, -15.70833333060214443, 4.330127018922195425 ) ) ;
#17194 = LINE ( 'NONE', #46783, #9105 ) ;
#17195 = CARTESIAN_POINT ( 'NONE',  ( 2.071067811865561215, -161.1874999999999716, 4.999999999999913847 ) ) ;
#17196 = CARTESIAN_POINT ( 'NONE',  ( -5.000000000000000000, 18.91666666666666430, -2.886751345948128211 ) ) ;
#17197 = CARTESIAN_POINT ( 'NONE',  ( 9.457646018065525792E-16, -34.06249999863440792, 5.148502694627439702 ) ) ;
#17198 = CARTESIAN_POINT ( 'NONE',  ( 4.458734124999999437, -19.06249999863440792, -5.460374474430324690E-16 ) ) ;
#17199 = ORIENTED_EDGE ( 'NONE', *, *, #20005, .T. ) ;
#17200 = LINE ( 'NONE', #50988, #5177 ) ;
#17201 = CARTESIAN_POINT ( 'NONE',  ( -3.152548672688508926E-16, -109.5624999986344079, -5.148502694627439702 ) ) ;
#17202 = CARTESIAN_POINT ( 'NONE',  ( -5.000000000000000888, -158.6875000027312126, -2.071067811865475949 ) ) ;
#17203 = ORIENTED_EDGE ( 'NONE', *, *, #44904, .T. ) ;
#17204 = CARTESIAN_POINT ( 'NONE',  ( -3.152548672688508926E-16, -101.8124999986344079, -5.148502694627439702 ) ) ;
#17205 = EDGE_CURVE ( 'NONE', #57064, #14704, #51349, .T. ) ;
#17206 = CARTESIAN_POINT ( 'NONE',  ( -4.458734124999999437, -26.31249999863440792, 0.000000000000000000 ) ) ;
#17207 = CARTESIAN_POINT ( 'NONE',  ( 2.500000000000002220, -62.54166666393547303, 4.330127018922192761 ) ) ;
#17208 = CARTESIAN_POINT ( 'NONE',  ( -57.89159099828107458, -152.9375000013656063, -3.393966926194107447 ) ) ;
#17209 = CARTESIAN_POINT ( 'NONE',  ( -5.000000000000000000, -146.5000000000000284, -6.123233995736766282E-16 ) ) ;
#17210 = CARTESIAN_POINT ( 'NONE',  ( 4.458734124999999437, -29.81249999863440436, -5.460374474430324690E-16 ) ) ;
#17211 = CARTESIAN_POINT ( 'NONE',  ( -2.229367062500000163, -67.72916666530106511, -3.861377020970580443 ) ) ;
#17212 = DIRECTION ( 'NONE',  ( 0.000000000000000000, 0.000000000000000000, 1.000000000000000000 ) ) ;
#17213 = CARTESIAN_POINT ( 'NONE',  ( 4.458734124999999437, -24.81249999863440436, -5.460374474430324690E-16 ) ) ;
#17214 = CARTESIAN_POINT ( 'NONE',  ( 1.975475456537005874E-15, 14.25000000000000000, 5.000000000000000000 ) ) ;
#17215 = CARTESIAN_POINT ( 'NONE',  ( 5.000000000000000000, -153.0000000000000284, 0.000000000000000000 ) ) ;
#17216 = CARTESIAN_POINT ( 'NONE',  ( 5.000000000000000000, -14.49999999999999822, -6.123233995736766282E-16 ) ) ;
#17217 = CARTESIAN_POINT ( 'NONE',  ( 4.458734125000000326, -152.3750000013655779, -1.846868145590734978 ) ) ;
#17218 = ORIENTED_EDGE ( 'NONE', *, *, #16075, .T. ) ;
#17219 = CARTESIAN_POINT ( 'NONE',  ( 0.000000000000000000, -120.0000000000000000, 0.000000000000000000 ) ) ;
#17220 = CARTESIAN_POINT ( 'NONE',  ( 4.458734124999998549, -52.97916666530107932, -2.574251347313721627 ) ) ;
#17221 = CARTESIAN_POINT ( 'NONE',  ( 2.499999999999998668, -84.20833333060214443, -4.330127018922193649 ) ) ;
#17222 = CYLINDRICAL_SURFACE ( 'NONE', #48383, 5.000000000000000000 ) ;
#17223 = CARTESIAN_POINT ( 'NONE',  ( -5.000000000000000000, 22.91666666666666430, -2.886751345948128211 ) ) ;
#17224 = VECTOR ( 'NONE', #37862, 1000.000000000000000 ) ;
#17225 = PLANE ( 'NONE',  #28506 ) ;
#17226 = CARTESIAN_POINT ( 'NONE',  ( 9.457646018065525792E-16, -1.062499998634405696, 5.148502694627439702 ) ) ;
#17227 = EDGE_CURVE ( 'NONE', #9589, #9483, #45308, .T. ) ;
#17228 = CARTESIAN_POINT ( 'NONE',  ( -4.330127018922101279, 45.00000000000000000, 7.500000000000002665 ) ) ;
#17229 = EDGE_CURVE ( 'NONE', #62891, #19199, #36283, .T. ) ;
#17230 = CARTESIAN_POINT ( 'NONE',  ( 3.061616997868383141E-16, -140.7500000000000000, -5.000000000000000000 ) ) ;
#17231 = FACE_OUTER_BOUND ( 'NONE', #30934, .T. ) ;
#17232 = CARTESIAN_POINT ( 'NONE',  ( -2.229367062499996610, 15.60416666803225993, 3.861377020970582219 ) ) ;
#17233 = CARTESIAN_POINT ( 'NONE',  ( -5.000000000000000000, 5.041666669397853795, -2.886751345948128211 ) ) ;
#17234 = EDGE_LOOP ( 'NONE', ( #9505, #55140, #50694, #43347 ) ) ;
#17235 = CARTESIAN_POINT ( 'NONE',  ( 1.975475456537005874E-15, 17.25000000000000000, 5.000000000000000000 ) ) ;
#17236 = ORIENTED_EDGE ( 'NONE', *, *, #16671, .F. ) ;
#17237 = B_SPLINE_CURVE_WITH_KNOTS ( 'NONE', 3,
 ( #36986, #22193, #20359, #55414, #44787, #41794, #59605, #749, #61438 ),
 .UNSPECIFIED., .F., .F.,
 ( 4, 2, 1, 2, 4 ),
 ( 0.000000000000000000, 0.002165063509461097498, 0.004330127018922194995, 0.006495190528383292493, 0.008660254037844389990 ),
 .UNSPECIFIED. ) ;
#17238 = CARTESIAN_POINT ( 'NONE',  ( 3.535533905932736864, -168.2500000027312126, 3.535533905932738641 ) ) ;
#17239 = CARTESIAN_POINT ( 'NONE',  ( 4.458734124999999437, -44.81249999863440081, -5.460374474430324690E-16 ) ) ;
#17240 = CARTESIAN_POINT ( 'NONE',  ( 1.846868145590735200, -163.5000000013655779, -4.458734125000000326 ) ) ;
#17241 = CARTESIAN_POINT ( 'NONE',  ( 5.000000000000000000, -44.37499999726880873, -6.123233995736766282E-16 ) ) ;
#17242 = EDGE_LOOP ( 'NONE', ( #55441, #6970, #26261, #54435 ) ) ;
#17243 = CARTESIAN_POINT ( 'NONE',  ( 4.458734125000001214, -19.89583333196773651, 2.574251347313718519 ) ) ;
#17244 = ORIENTED_EDGE ( 'NONE', *, *, #36996, .T. ) ;
#17245 = CARTESIAN_POINT ( 'NONE',  ( 2.499999999999998668, -88.33333333333332860, -4.330127018922193649 ) ) ;
#17246 = CARTESIAN_POINT ( 'NONE',  ( -1.846868145590737420, -163.7500000013655779, 4.458734124999999437 ) ) ;
#17248 = VERTEX_POINT ( 'NONE', #36613 ) ;
#17247 = CARTESIAN_POINT ( 'NONE',  ( 1.339745962155729053, -55.29465819873851729, -4.999999999999933387 ) ) ;
#17249 = CARTESIAN_POINT ( 'NONE',  ( -56.66612745406270335, -138.3125000000000000, -5.149110718188516067 ) ) ;
#17250 = CARTESIAN_POINT ( 'NONE',  ( 4.458734124999999437, -34.06249999863440792, -5.460374474430324690E-16 ) ) ;
#17251 = CARTESIAN_POINT ( 'NONE',  ( -5.000000000000000888, -147.6875000027312126, -2.071067811865475949 ) ) ;
#17252 = EDGE_LOOP ( 'NONE', ( #3423, #42844, #31379, #39314 ) ) ;
#17253 =( BOUNDED_CURVE ( )  B_SPLINE_CURVE ( 2, ( #24887, #4831, #33169, #24450, #53093, #63385, #29580, #37989, #4512 ),
 .UNSPECIFIED., .F., .F. ) 
 B_SPLINE_CURVE_WITH_KNOTS ( ( 3, 2, 2, 2, 3 ),
 ( 0.7125000000000000222, 0.7130952380952381153, 0.7142857142857143016, 0.7154761904761904878, 0.7160714285714285809 ),
 .UNSPECIFIED. ) 
 CURVE ( )  GEOMETRIC_REPRESENTATION_ITEM ( )  RATIONAL_B_SPLINE_CURVE ( ( 0.9330127018922194093, 0.9330127018922194093, 1.000000000000000000, 0.8660254037844387076, 1.000000000000000000, 0.8660254037844387076, 1.000000000000000000, 0.9330127018922194093, 0.9330127018922194093 ) ) 
 REPRESENTATION_ITEM ( '' )  );
#17254 = EDGE_CURVE ( 'NONE', #61583, #21697, #56247, .T. ) ;
#17255 = CARTESIAN_POINT ( 'NONE',  ( -2.229367062499996610, -76.14583333196773651, 3.861377020970582219 ) ) ;
#17256 = CARTESIAN_POINT ( 'NONE',  ( -4.458734124999999437, 22.60416666803225993, -2.574251347313719407 ) ) ;
#17257 = VERTEX_POINT ( 'NONE', #59804 ) ;
#17258 = DIRECTION ( 'NONE',  ( -0.000000000000000000, 1.000000000000000000, -0.000000000000000000 ) ) ;
#17259 = CARTESIAN_POINT ( 'NONE',  ( -50.70258187064364108, -144.3750000013656063, 2.196230717870141014 ) ) ;
#17260 = CARTESIAN_POINT ( 'NONE',  ( 2.229367062499998831, -80.89583333196773651, -3.861377020970580887 ) ) ;
#17261 = CARTESIAN_POINT ( 'NONE',  ( -51.19402409849444524, -131.6250000027312126, -3.242614290531456334 ) ) ;
#17262 = CARTESIAN_POINT ( 'NONE',  ( 5.000000000000000888, -142.9375000000000284, -2.071067811865475505 ) ) ;
#17263 = CARTESIAN_POINT ( 'NONE',  ( 5.000000000000000000, 24.50000000000000000, -6.123233995736766282E-16 ) ) ;
#17264 = CARTESIAN_POINT ( 'NONE',  ( 2.229367062499998831, -54.64583333196773651, -3.861377020970580887 ) ) ;
#17265 = CARTESIAN_POINT ( 'NONE',  ( 4.458734124999998549, -47.72916666530106511, -2.574251347313721627 ) ) ;
#17266 = CARTESIAN_POINT ( 'NONE',  ( -2.499999999999996447, 21.16666666666666785, 4.330127018922195425 ) ) ;
#17267 = VECTOR ( 'NONE', #29786, 1000.000000000000000 ) ;
#17268 = CARTESIAN_POINT ( 'NONE',  ( -4.999999999999999112, -108.9166666666666572, 2.886751345948131764 ) ) ;
#17269 = CARTESIAN_POINT ( 'NONE',  ( 2.499999999999998668, -3.333333333333333925, -4.330127018922193649 ) ) ;
#17270 = CARTESIAN_POINT ( 'NONE',  ( 4.458734124999998549, -40.97916666530107932, -2.574251347313721627 ) ) ;
#17271 = CARTESIAN_POINT ( 'NONE',  ( -2.500000000000000444, 2.958333336064520314, -4.330127018922193649 ) ) ;
#17272 = CARTESIAN_POINT ( 'NONE',  ( 5.000000000000000000, 16.70833333606451987, -2.886751345948130876 ) ) ;
#17273 = DIRECTION ( 'NONE',  ( -0.000000000000000000, 1.000000000000000000, -0.000000000000000000 ) ) ;
#17274 = CARTESIAN_POINT ( 'NONE',  ( -3.152548672688508926E-16, -79.81249999863440792, -5.148502694627439702 ) ) ;
#17275 = CARTESIAN_POINT ( 'NONE',  ( 0.000000000000000000, -170.0000000000000000, 0.000000000000000000 ) ) ;
#17276 = CARTESIAN_POINT ( 'NONE',  ( -4.458734124999997661, -105.2291666653010651, 2.574251347313722516 ) ) ;
#17277 = CARTESIAN_POINT ( 'NONE',  ( 2.229367062500001939, -8.229166665301073991, 3.861377020970579999 ) ) ;
#17278 = ORIENTED_EDGE ( 'NONE', *, *, #60157, .F. ) ;
#17279 = CARTESIAN_POINT ( 'NONE',  ( -1.339745962155613812, -15.08034179853029322, -5.000000000000000000 ) ) ;
#17280 = CARTESIAN_POINT ( 'NONE',  ( 2.229367062500001939, -91.97916666530106511, 3.861377020970579999 ) ) ;
#17281 = CARTESIAN_POINT ( 'NONE',  ( 2.071067811865476394, -168.3125000027312410, 5.000000000000000000 ) ) ;
#17282 = CARTESIAN_POINT ( 'NONE',  ( 4.458734125000001214, -88.14583333196773651, 2.574251347313718519 ) ) ;
#17283 = EDGE_CURVE ( 'NONE', #12901, #16392, #55925, .T. ) ;
#17284 = CARTESIAN_POINT ( 'NONE',  ( -4.458734124999999437, 12.35416666803226171, -2.574251347313719407 ) ) ;
#17285 = CARTESIAN_POINT ( 'NONE',  ( -6.972266317189433020E-16, -94.12499999726880162, -5.000000000000000000 ) ) ;
#17286 = CARTESIAN_POINT ( 'NONE',  ( -58.39396692619412477, -132.4375000013656063, 2.891590998281057701 ) ) ;
#17287 = CARTESIAN_POINT ( 'NONE',  ( 2.229367062499998831, -7.645833331967735624, -3.861377020970580887 ) ) ;
#17288 = CARTESIAN_POINT ( 'NONE',  ( 4.458734125000001214, 17.85416666803225993, 2.574251347313718519 ) ) ;
#17289 = CARTESIAN_POINT ( 'NONE',  ( 2.229367062500001939, -55.22916666530107221, 3.861377020970579999 ) ) ;
#17290 = FACE_OUTER_BOUND ( 'NONE', #30285, .T. ) ;
#17291 = CARTESIAN_POINT ( 'NONE',  ( -6.972266317189433020E-16, -37.25000000000000000, -5.000000000000000000 ) ) ;
#17292 = CARTESIAN_POINT ( 'NONE',  ( 4.458734124999999437, -8.812499998634406140, -5.460374474430324690E-16 ) ) ;
#17293 = VERTEX_POINT ( 'NONE', #46268 ) ;
#17294 = CARTESIAN_POINT ( 'NONE',  ( -4.458734124999999437, -35.56249999863440792, 0.000000000000000000 ) ) ;
#17295 = CARTESIAN_POINT ( 'NONE',  ( -50.55543936806279248, -126.3125000013655921, 0.3552334253322060320 ) ) ;
#17296 = CARTESIAN_POINT ( 'NONE',  ( 2.500000000000002220, -76.66666666666665719, 4.330127018922192761 ) ) ;
#17297 = CARTESIAN_POINT ( 'NONE',  ( -2.229367062500000163, -81.47916666530106511, -3.861377020970580443 ) ) ;
#17298 = CARTESIAN_POINT ( 'NONE',  ( 4.458734125000001214, 22.85416666803225993, 2.574251347313718519 ) ) ;
#17299 = CARTESIAN_POINT ( 'NONE',  ( -1.846868145590734756, -150.3750000013655779, -4.458734124999999437 ) ) ;
#17300 = CARTESIAN_POINT ( 'NONE',  ( -2.229367062499996610, 21.85416666803226349, 3.861377020970582219 ) ) ;
#17301 = DIRECTION ( 'NONE',  ( 0.000000000000000000, 1.000000000000000000, 0.000000000000000000 ) ) ;
#17302 = EDGE_CURVE ( 'NONE', #34331, #60539, #9583, .T. ) ;
#17303 = CARTESIAN_POINT ( 'NONE',  ( -1.339745962155564296, -26.08034179853029499, -5.000000000000028422 ) ) ;
#17304 = CARTESIAN_POINT ( 'NONE',  ( -2.229367062500000163, -82.72916666530106511, -3.861377020970580443 ) ) ;
#17305 = CARTESIAN_POINT ( 'NONE',  ( -5.000000000000000000, -67.08333333333332860, -2.886751345948128211 ) ) ;
#17306 =( BOUNDED_CURVE ( )  B_SPLINE_CURVE ( 2, ( #20576, #55312, #24750, #974, #20891, #30851, #5132, #59168, #49510 ),
 .UNSPECIFIED., .F., .F. ) 
 B_SPLINE_CURVE_WITH_KNOTS ( ( 3, 2, 2, 2, 3 ),
 ( 0.3196428571428571175, 0.3202380952380952106, 0.3214285714285714524, 0.3226190476190476386, 0.3232142857142857317 ),
 .UNSPECIFIED. ) 
 CURVE ( )  GEOMETRIC_REPRESENTATION_ITEM ( )  RATIONAL_B_SPLINE_CURVE ( ( 0.9330127018922194093, 0.9330127018922194093, 1.000000000000000000, 0.8660254037844387076, 1.000000000000000000, 0.8660254037844387076, 1.000000000000000000, 0.9330127018922194093, 0.9330127018922194093 ) ) 
 REPRESENTATION_ITEM ( '' )  );
#17307 = LINE ( 'NONE', #7032, #60397 ) ;
#17308 = CARTESIAN_POINT ( 'NONE',  ( 1.060575238724906964E-15, 21.37500000273118417, 5.773502691896257311 ) ) ;
#17309 = VERTEX_POINT ( 'NONE', #20876 ) ;
#17310 = CARTESIAN_POINT ( 'NONE',  ( 1.339745962155612702, -35.29465819873851729, -5.000000000000000000 ) ) ;
#17311 = EDGE_CURVE ( 'NONE', #33407, #50926, #5079, .T. ) ;
#17312 =( BOUNDED_CURVE ( )  B_SPLINE_CURVE ( 2, ( #23335, #26896, #2770, #18502, #13358, #22710, #17867, #47453, #22069 ),
 .UNSPECIFIED., .F., .F. ) 
 B_SPLINE_CURVE_WITH_KNOTS ( ( 3, 2, 2, 2, 3 ),
 ( 0.4395833333333333259, 0.4402777777777777679, 0.4416666666666666519, 0.4430555555555555358, 0.4437499999999999778 ),
 .UNSPECIFIED. ) 
 CURVE ( )  GEOMETRIC_REPRESENTATION_ITEM ( )  RATIONAL_B_SPLINE_CURVE ( ( 0.9330127018922194093, 0.9330127018922194093, 1.000000000000000000, 0.8660254037844387076, 1.000000000000000000, 0.8660254037844387076, 1.000000000000000000, 0.9330127018922194093, 0.9330127018922194093 ) ) 
 REPRESENTATION_ITEM ( '' )  );
#17313 = VECTOR ( 'NONE', #34475, 1000.000000000000000 ) ;
#17314 = CARTESIAN_POINT ( 'NONE',  ( 1.975475456537005874E-15, -52.62499999726880873, 5.000000000000000000 ) ) ;
#17316 = CARTESIAN_POINT ( 'NONE',  ( 2.499999999999998668, -24.33333333333333215, -4.330127018922193649 ) ) ;
#17315 = PLANE ( 'NONE',  #34702 ) ;
#17317 = CARTESIAN_POINT ( 'NONE',  ( 9.457646018065525792E-16, -30.06249999863440081, 5.148502694627439702 ) ) ;
#17318 = VECTOR ( 'NONE', #60683, 1000.000000000000000 ) ;
#17319 = CARTESIAN_POINT ( 'NONE',  ( 4.458734124999999437, -86.81249999863439371, -5.460374474430324690E-16 ) ) ;
#17320 = CARTESIAN_POINT ( 'NONE',  ( 5.000000000000000888, -31.45833333060214798, 2.886751345948126879 ) ) ;
#17322 = VERTEX_POINT ( 'NONE', #11213 ) ;
#17321 = CARTESIAN_POINT ( 'NONE',  ( -2.229367062500000163, -56.47916666530107221, -3.861377020970580443 ) ) ;
#17323 = CARTESIAN_POINT ( 'NONE',  ( -6.972266317189433020E-16, -62.12499999726880162, -5.000000000000000000 ) ) ;
#17325 = ORIENTED_EDGE ( 'NONE', *, *, #11129, .T. ) ;
#17324 = CARTESIAN_POINT ( 'NONE',  ( -2.229367062499996610, -6.395833331967741842, 3.861377020970582219 ) ) ;
#17326 = CARTESIAN_POINT ( 'NONE',  ( 5.000000000000000000, -70.41666666666667140, -2.886751345948129988 ) ) ;
#17327 = CARTESIAN_POINT ( 'NONE',  ( -57.89159099828107458, -140.6875000013656063, -3.393966926194107447 ) ) ;
#17328 = CARTESIAN_POINT ( 'NONE',  ( 4.458734125000001214, -51.14583333196772941, 2.574251347313718519 ) ) ;
#17329 = CARTESIAN_POINT ( 'NONE',  ( -2.500000000000000444, -79.04166666393547303, -4.330127018922193649 ) ) ;
#17331 = ORIENTED_EDGE ( 'NONE', *, *, #31543, .T. ) ;
#17330 = CARTESIAN_POINT ( 'NONE',  ( -1.339745962155610925, -53.66965819600733312, 5.000000000000000000 ) ) ;
#17332 = CARTESIAN_POINT ( 'NONE',  ( -50.18089887299979068, -148.6875000000000568, 2.462841084822635640 ) ) ;
#17333 = EDGE_CURVE ( 'NONE', #24403, #40939, #16171, .T. ) ;
#17334 = CARTESIAN_POINT ( 'NONE',  ( 4.458734124999998549, -18.97916666530107221, -2.574251347313721627 ) ) ;
#17335 = CARTESIAN_POINT ( 'NONE',  ( -2.229367062499996610, -56.39583333196773651, 3.861377020970582219 ) ) ;
#17336 = FACE_OUTER_BOUND ( 'NONE', #17242, .T. ) ;
#17337 =( NAMED_UNIT ( * ) PLANE_ANGLE_UNIT ( ) SI_UNIT ( $, .RADIAN. ) );
#17338 = CARTESIAN_POINT ( 'NONE',  ( 2.730187237215162345E-16, -142.1875000013656063, -4.458734124999999437 ) ) ;
#17339 = CARTESIAN_POINT ( 'NONE',  ( 4.458734125000001214, -100.1458333319677365, 2.574251347313718519 ) ) ;
#17340 = CARTESIAN_POINT ( 'NONE',  ( 1.975475456537005874E-15, -60.75000000000000000, 5.000000000000000000 ) ) ;
#17341 =( BOUNDED_CURVE ( )  B_SPLINE_CURVE ( 2, ( #33903, #58984, #53214, #34210, #8837, #48381, #53526, #43233, #44497 ),
 .UNSPECIFIED., .F., .F. ) 
 B_SPLINE_CURVE_WITH_KNOTS ( ( 3, 2, 2, 2, 3 ),
 ( 0.2416666666666668628, 0.2458333333333335147, 0.2500000000000002220, 0.2541666666666668739, 0.2583333333333335813 ),
 .UNSPECIFIED. ) 
 CURVE ( )  GEOMETRIC_REPRESENTATION_ITEM ( )  RATIONAL_B_SPLINE_CURVE ( ( 0.9999999999999964473, 0.9238795325112902912, 1.000000000000000000, 0.9238795325112867385, 1.000000000000000000, 0.9238795325112867385, 1.000000000000000000, 0.9238795325112826307, 1.000000000000003997 ) ) 
 REPRESENTATION_ITEM ( '' )  );
#17342 = ORIENTED_EDGE ( 'NONE', *, *, #51926, .T. ) ;
#17343 = CARTESIAN_POINT ( 'NONE',  ( -57.19623071787016499, -153.6250000013655779, 4.297418129356382899 ) ) ;
#17344 = CARTESIAN_POINT ( 'NONE',  ( -56.66612745406270335, -143.4375000027312410, -5.149110718188516067 ) ) ;
#17345 = FACE_OUTER_BOUND ( 'NONE', #19545, .T. ) ;
#17346 = CARTESIAN_POINT ( 'NONE',  ( -4.458734124999999437, -7.312499998634404363, 0.000000000000000000 ) ) ;
#17347 = CARTESIAN_POINT ( 'NONE',  ( 4.458734124999998549, -96.97916666530105090, -2.574251347313721627 ) ) ;
#17348 = CARTESIAN_POINT ( 'NONE',  ( 4.458734124999999437, -148.7500000013656063, 1.846868145590737864 ) ) ;
#17349 = CARTESIAN_POINT ( 'NONE',  ( -2.229367062499996610, -21.39583333196774007, 3.861377020970582219 ) ) ;
#17350 = CARTESIAN_POINT ( 'NONE',  ( -6.972266317189433020E-16, -46.24999999999999289, -5.000000000000000000 ) ) ;
#17351 = CARTESIAN_POINT ( 'NONE',  ( -55.35523342533222291, -136.3125000013656063, 4.444560631937231499 ) ) ;
#17352 = CARTESIAN_POINT ( 'NONE',  ( -3.152548672688508926E-16, -62.81249999863440792, -5.148502694627439702 ) ) ;
#17353 = CARTESIAN_POINT ( 'NONE',  ( -2.500000000000000444, -84.04166666393547303, -4.330127018922193649 ) ) ;
#17354 = CARTESIAN_POINT ( 'NONE',  ( 1.339745962155612702, 6.830341803992665994, -5.000000000000000000 ) ) ;
#17355 = CARTESIAN_POINT ( 'NONE',  ( 1.846868145590735200, -143.2500000013655779, -4.458734124999999437 ) ) ;
#17356 = VECTOR ( 'NONE', #51646, 1000.000000000000000 ) ;
#17357 =( BOUNDED_CURVE ( )  B_SPLINE_CURVE ( 2, ( #31403, #50403, #51041, #26918, #2174, #26595, #40422, #61018, #16944 ),
 .UNSPECIFIED., .F., .F. ) 
 B_SPLINE_CURVE_WITH_KNOTS ( ( 3, 2, 2, 2, 3 ),
 ( 0.1696428571428571508, 0.1702380952380952439, 0.1714285714285714302, 0.1726190476190476164, 0.1732142857142857095 ),
 .UNSPECIFIED. ) 
 CURVE ( )  GEOMETRIC_REPRESENTATION_ITEM ( )  RATIONAL_B_SPLINE_CURVE ( ( 0.9330127018922194093, 0.9330127018922194093, 1.000000000000000000, 0.8660254037844387076, 1.000000000000000000, 0.8660254037844387076, 1.000000000000000000, 0.9330127018922194093, 0.9330127018922194093 ) ) 
 REPRESENTATION_ITEM ( '' )  );
#17358 = CARTESIAN_POINT ( 'NONE',  ( 2.229367062499998831, 11.10416666803225993, -3.861377020970580887 ) ) ;
#17359 = ORIENTED_EDGE ( 'NONE', *, *, #49692, .F. ) ;
#17360 = DIRECTION ( 'NONE',  ( -0.000000000000000000, 1.000000000000000000, -0.000000000000000000 ) ) ;
#17361 = CARTESIAN_POINT ( 'NONE',  ( 5.000000000000000000, -66.29166666393547303, -2.886751345948130876 ) ) ;
#17363 = CARTESIAN_POINT ( 'NONE',  ( -2.229367062499996610, -22.14583333196773651, 3.861377020970582219 ) ) ;
#17362 = CARTESIAN_POINT ( 'NONE',  ( 5.000000000000000000, -92.41666666666665719, -2.886751345948129988 ) ) ;
#17364 = CYLINDRICAL_SURFACE ( 'NONE', #47972, 5.000000000000000000 ) ;
#17365 = CARTESIAN_POINT ( 'NONE',  ( -4.458734124999998549, -70.47916666530107932, 2.574251347313722516 ) ) ;
#17366 = CARTESIAN_POINT ( 'NONE',  ( 4.458734125000000326, 28.85416666803226704, 2.574251347313718519 ) ) ;
#17367 = CARTESIAN_POINT ( 'NONE',  ( 1.339745962155615144, -76.58034179853029855, 4.999999999999999112 ) ) ;
#17368 = CARTESIAN_POINT ( 'NONE',  ( -51.60603307380591787, -146.9375000013656063, -2.891590998281053704 ) ) ;
#17369 = ADVANCED_FACE ( 'NONE', ( #42606 ), #17849, .T. ) ;
#17370 = EDGE_CURVE ( 'NONE', #7918, #47469, #47745, .T. ) ;
#17371 = CARTESIAN_POINT ( 'NONE',  ( 5.000000000000000888, -52.45833333060213732, 2.886751345948126879 ) ) ;
#17372 = CARTESIAN_POINT ( 'NONE',  ( -56.66612745406280993, -148.3125000000000000, -5.149110718188524061 ) ) ;
#17373 = CARTESIAN_POINT ( 'NONE',  ( 2.229367062499998831, 6.354166668032262599, -3.861377020970580887 ) ) ;
#17374 = CARTESIAN_POINT ( 'NONE',  ( 1.975475456537005874E-15, -24.74999999999999645, 5.000000000000000000 ) ) ;
#17376 = EDGE_CURVE ( 'NONE', #58377, #30399, #29676, .T. ) ;
#17375 = DIRECTION ( 'NONE',  ( -0.000000000000000000, 1.000000000000000000, -0.000000000000000000 ) ) ;
#17377 = CARTESIAN_POINT ( 'NONE',  ( 4.458734124999999437, 6.187500001365593860, -5.460374474430324690E-16 ) ) ;
#17378 = CARTESIAN_POINT ( 'NONE',  ( 4.458734125000001214, -72.89583333196775072, 2.574251347313718519 ) ) ;
#17379 = VECTOR ( 'NONE', #57638, 1000.000000000000000 ) ;
#17380 = CARTESIAN_POINT ( 'NONE',  ( 4.458734124999999437, -18.06249999863440792, -5.460374474430324690E-16 ) ) ;
#17381 = ADVANCED_FACE ( 'NONE', ( #2751 ), #47436, .T. ) ;
#17382 = CARTESIAN_POINT ( 'NONE',  ( -5.000000000000000000, -1.083333333333331927, -2.886751345948128211 ) ) ;
#17383 = CARTESIAN_POINT ( 'NONE',  ( -1.846868145590734756, -159.1250000013656063, -4.458734125000000326 ) ) ;
#17384 = DIRECTION ( 'NONE',  ( -0.000000000000000000, 1.000000000000000000, -0.000000000000000000 ) ) ;
#17385 = CARTESIAN_POINT ( 'NONE',  ( 9.457646018065525792E-16, -65.06249999863440792, 5.148502694627439702 ) ) ;
#17386 = CARTESIAN_POINT ( 'NONE',  ( 2.500000000000002220, -98.54166666393545881, 4.330127018922192761 ) ) ;
#17387 = EDGE_CURVE ( 'NONE', #28986, #57284, #3073, .T. ) ;
#17388 = EDGE_CURVE ( 'NONE', #29321, #53941, #40775, .T. ) ;
#17389 = CARTESIAN_POINT ( 'NONE',  ( 1.975475456537005874E-15, -35.75000000000000711, 5.000000000000000000 ) ) ;
#17390 = CARTESIAN_POINT ( 'NONE',  ( 2.229367062499998831, -40.64583333196773651, -3.861377020970580887 ) ) ;
#17391 = ADVANCED_FACE ( 'NONE', ( #32323 ), #13023, .T. ) ;
#17392 = CARTESIAN_POINT ( 'NONE',  ( 2.500000000000002220, -60.66666666666665719, 4.330127018922192761 ) ) ;
#17393 = CARTESIAN_POINT ( 'NONE',  ( -2.229367062500000163, -68.72916666530107932, -3.861377020970580443 ) ) ;
#17394 = CARTESIAN_POINT ( 'NONE',  ( -4.999999999999999112, -47.91666666666667140, 2.886751345948131764 ) ) ;
#17395 = EDGE_CURVE ( 'NONE', #19443, #24216, #7168, .T. ) ;
#17396 = FACE_OUTER_BOUND ( 'NONE', #20907, .T. ) ;
#17397 = VERTEX_POINT ( 'NONE', #62244 ) ;
#17398 = CARTESIAN_POINT ( 'NONE',  ( -2.499999999999996447, -84.83333333333332860, 4.330127018922195425 ) ) ;
#17399 = CARTESIAN_POINT ( 'NONE',  ( 3.061616997868383141E-16, -143.8750000027312126, -5.000000000000000000 ) ) ;
#17400 = EDGE_CURVE ( 'NONE', #30363, #28142, #51127, .T. ) ;
#17401 = CARTESIAN_POINT ( 'NONE',  ( 2.500000000000002220, -6.666666666666667851, 4.330127018922192761 ) ) ;
#17402 = ADVANCED_FACE ( 'NONE', ( #451 ), #20055, .F. ) ;
#17403 = CARTESIAN_POINT ( 'NONE',  ( 9.457646018065525792E-16, -70.06249999863439371, 5.148502694627439702 ) ) ;
#17404 = CARTESIAN_POINT ( 'NONE',  ( -4.999999999999998224, -30.79166666393548013, 2.886751345948131764 ) ) ;
#17405 = CARTESIAN_POINT ( 'NONE',  ( 1.060575238724906964E-15, -12.62499999726881050, 5.773502691896257311 ) ) ;
#17407 = ORIENTED_EDGE ( 'NONE', *, *, #19682, .T. ) ;
#17406 = CARTESIAN_POINT ( 'NONE',  ( -2.229367062500000163, -41.47916666530107932, -3.861377020970580443 ) ) ;
#17408 = DIRECTION ( 'NONE',  ( -0.000000000000000000, 1.000000000000000000, -0.000000000000000000 ) ) ;
#17410 = ORIENTED_EDGE ( 'NONE', *, *, #7587, .T. ) ;
#17409 = CARTESIAN_POINT ( 'NONE',  ( -4.458734124999998549, 5.520833334698927786, 2.574251347313722516 ) ) ;
#17411 = CARTESIAN_POINT ( 'NONE',  ( -5.000000000000000888, -151.4375000000000000, 2.071067811865474617 ) ) ;
#17412 = CARTESIAN_POINT ( 'NONE',  ( 5.000000000000000888, -57.58333333333334281, 2.886751345948126879 ) ) ;
#17413 = CARTESIAN_POINT ( 'NONE',  ( -4.458734124999999437, -162.1875000013655779, -5.460374474430324690E-16 ) ) ;
#17414 = CARTESIAN_POINT ( 'NONE',  ( 4.458734124999998549, -33.97916666530107221, -2.574251347313721627 ) ) ;
#17415 = CARTESIAN_POINT ( 'NONE',  ( 2.071067811865392461, -145.1875000000000568, 5.000000000000084377 ) ) ;
#17416 = CARTESIAN_POINT ( 'NONE',  ( -3.152548672688508926E-16, -79.56249999863440792, -5.148502694627439702 ) ) ;
#17417 = CARTESIAN_POINT ( 'NONE',  ( 3.535533905932736864, -167.1250000000000284, 3.535533905932738641 ) ) ;
#17418 = CARTESIAN_POINT ( 'NONE',  ( -4.458734124999998549, -89.22916666530106511, 2.574251347313722516 ) ) ;
#17419 = VECTOR ( 'NONE', #22690, 1000.000000000000000 ) ;
#17420 = CARTESIAN_POINT ( 'NONE',  ( -50.70258187064364108, -131.3750000013656347, 2.196230717870141014 ) ) ;
#17421 = CARTESIAN_POINT ( 'NONE',  ( 4.458734124999999437, -0.06249999863440491854, -5.460374474430324690E-16 ) ) ;
#17422 = CARTESIAN_POINT ( 'NONE',  ( 2.229367062500001939, -36.22916666530107221, 3.861377020970579999 ) ) ;
#17423 = CARTESIAN_POINT ( 'NONE',  ( -1.339745962155617365, 24.33034180399266688, 4.999999999999998224 ) ) ;
#17424 = CARTESIAN_POINT ( 'NONE',  ( -2.229367062500000163, -82.72916666530106511, -3.861377020970580443 ) ) ;
#17425 = CARTESIAN_POINT ( 'NONE',  ( -2.500000000000000444, 15.95833333606451809, -4.330127018922193649 ) ) ;
#17426 = ORIENTED_EDGE ( 'NONE', *, *, #20404, .F. ) ;
#17427 = CARTESIAN_POINT ( 'NONE',  ( -2.499999999999996447, -94.70833333060213022, 4.330127018922195425 ) ) ;
#17428 = CARTESIAN_POINT ( 'NONE',  ( 3.061616997868383141E-16, -151.7500000000000284, -5.000000000000000000 ) ) ;
#17429 = CARTESIAN_POINT ( 'NONE',  ( 2.229367062499998831, -67.89583333196773651, -3.861377020970580887 ) ) ;
#17430 = CARTESIAN_POINT ( 'NONE',  ( -3.152548672688508926E-16, -6.812499998634404363, -5.148502694627439702 ) ) ;
#17431 = ORIENTED_EDGE ( 'NONE', *, *, #24057, .T. ) ;
#17432 = CARTESIAN_POINT ( 'NONE',  ( 3.061616997868383141E-16, -163.7500000000000000, -5.000000000000000000 ) ) ;
#17433 = DIRECTION ( 'NONE',  ( -0.000000000000000000, 1.000000000000000000, -0.000000000000000000 ) ) ;
#17434 = CARTESIAN_POINT ( 'NONE',  ( -4.458734124999998549, -9.479166665301070438, 2.574251347313722516 ) ) ;
#17435 = DIRECTION ( 'NONE',  ( 0.000000000000000000, 0.000000000000000000, 1.000000000000000000 ) ) ;
#17436 = CARTESIAN_POINT ( 'NONE',  ( 4.458734124999999437, 4.187500001365595637, -5.460374474430324690E-16 ) ) ;
#17437 = CARTESIAN_POINT ( 'NONE',  ( 1.339745962155612702, -64.29465819873851729, -5.000000000000000000 ) ) ;
#17438 = CARTESIAN_POINT ( 'NONE',  ( -4.458734125000000326, -158.8750000013655779, 1.846868145590734089 ) ) ;
#17439 = CARTESIAN_POINT ( 'NONE',  ( -4.458734124999997661, 26.52083333469892779, 2.574251347313722516 ) ) ;
#17440 = ORIENTED_EDGE ( 'NONE', *, *, #59318, .T. ) ;
#17441 = CARTESIAN_POINT ( 'NONE',  ( 2.229367062500001939, -85.97916666530107932, 3.861377020970579999 ) ) ;
#17442 = CARTESIAN_POINT ( 'NONE',  ( -2.500000000000000444, -78.16666666666665719, -4.330127018922193649 ) ) ;
#17443 = CARTESIAN_POINT ( 'NONE',  ( -4.458734124999999437, -7.395833331967734736, -2.574251347313719407 ) ) ;
#17444 = CARTESIAN_POINT ( 'NONE',  ( -2.500000000000000444, 19.83333333333333570, -4.330127018922193649 ) ) ;
#17445 = DIRECTION ( 'NONE',  ( -0.000000000000000000, 1.000000000000000000, -0.000000000000000000 ) ) ;
#17446 =( BOUNDED_CURVE ( )  B_SPLINE_CURVE ( 2, ( #1360, #30272, #40564, #16129, #50860, #21597, #7120, #55052, #35120 ),
 .UNSPECIFIED., .F., .F. ) 
 B_SPLINE_CURVE_WITH_KNOTS ( ( 3, 2, 2, 2, 3 ),
 ( 0.005357142857142858060, 0.005952380952380952051, 0.007142857142857142634, 0.008333333333333333218, 0.008928571428571429811 ),
 .UNSPECIFIED. ) 
 CURVE ( )  GEOMETRIC_REPRESENTATION_ITEM ( )  RATIONAL_B_SPLINE_CURVE ( ( 0.9330127018922192983, 0.9330127018922194093, 1.000000000000000000, 0.8660254037844387076, 1.000000000000000000, 0.8660254037844387076, 1.000000000000000000, 0.9330127018922191873, 0.9330127018922192983 ) ) 
 REPRESENTATION_ITEM ( '' )  );
#17447 = DIRECTION ( 'NONE',  ( -0.000000000000000000, 1.000000000000000000, -0.000000000000000000 ) ) ;
#17448 = CARTESIAN_POINT ( 'NONE',  ( 1.060575238724906964E-15, -34.62499999726880873, 5.773502691896257311 ) ) ;
#17449 = DIRECTION ( 'NONE',  ( -0.000000000000000000, 1.000000000000000000, -0.000000000000000000 ) ) ;
#17450 = CARTESIAN_POINT ( 'NONE',  ( -4.458734124999999437, 25.68750000136559208, 0.000000000000000000 ) ) ;
#17451 = CARTESIAN_POINT ( 'NONE',  ( -2.499999999999996447, -20.70833333060214798, 4.330127018922195425 ) ) ;
#17452 = CARTESIAN_POINT ( 'NONE',  ( -4.458734124999999437, 21.60416666803226349, -2.574251347313719407 ) ) ;
#17453 = CARTESIAN_POINT ( 'NONE',  ( 9.457646018065525792E-16, -59.06249999863439371, 5.148502694627439702 ) ) ;
#17454 = CARTESIAN_POINT ( 'NONE',  ( -4.458734124999999437, -2.562499998634407028, 0.000000000000000000 ) ) ;
#17455 = DIRECTION ( 'NONE',  ( -0.000000000000000000, 1.000000000000000000, -0.000000000000000000 ) ) ;
#17456 = CARTESIAN_POINT ( 'NONE',  ( -2.499999999999996447, 15.16666666666666607, 4.330127018922195425 ) ) ;
#17457 = CARTESIAN_POINT ( 'NONE',  ( -5.000000000000000888, -141.6875000027312126, -2.071067811865475949 ) ) ;
#17458 = CARTESIAN_POINT ( 'NONE',  ( -1.339745962155613812, -52.20534180126148271, -5.000000000000000000 ) ) ;
#17459 = VECTOR ( 'NONE', #41732, 1000.000000000000000 ) ;
#17460 = CARTESIAN_POINT ( 'NONE',  ( -2.229367062500000163, -45.47916666530106511, -3.861377020970580443 ) ) ;
#17461 = CARTESIAN_POINT ( 'NONE',  ( 5.000000000000000888, -79.45833333060214443, 2.886751345948126879 ) ) ;
#17462 = CARTESIAN_POINT ( 'NONE',  ( -59.44456063193725015, -140.8125000013656063, -0.3552334253322034230 ) ) ;
#17463 = CARTESIAN_POINT ( 'NONE',  ( 4.458734124999999437, -139.5625000013656063, 0.000000000000000000 ) ) ;
#17464 =( BOUNDED_CURVE ( )  B_SPLINE_CURVE ( 2, ( #27745, #18722, #38346, #3323, #41901, #62172, #61548, #17479, #18094 ),
 .UNSPECIFIED., .F., .F. ) 
 B_SPLINE_CURVE_WITH_KNOTS ( ( 3, 2, 2, 2, 3 ),
 ( 0.4982142857142857206, 0.4988095238095238138, 0.5000000000000000000, 0.5011904761904761862, 0.5017857142857142794 ),
 .UNSPECIFIED. ) 
 CURVE ( )  GEOMETRIC_REPRESENTATION_ITEM ( )  RATIONAL_B_SPLINE_CURVE ( ( 0.9330127018922194093, 0.9330127018922194093, 1.000000000000000000, 0.8660254037844387076, 1.000000000000000000, 0.8660254037844387076, 1.000000000000000000, 0.9330127018922194093, 0.9330127018922194093 ) ) 
 REPRESENTATION_ITEM ( '' )  );
#17465 = CARTESIAN_POINT ( 'NONE',  ( -6.972266317189433020E-16, -36.25000000000000000, -5.000000000000000000 ) ) ;
#17466 = CARTESIAN_POINT ( 'NONE',  ( -4.458734124999999437, -87.56249999863439371, 0.000000000000000000 ) ) ;
#17467 = CARTESIAN_POINT ( 'NONE',  ( 4.458734124999999437, -159.6250000013655779, -1.846868145590734978 ) ) ;
#17468 = CARTESIAN_POINT ( 'NONE',  ( -3.535250795749689387E-16, -31.25000000000000000, -5.773502691896257311 ) ) ;
#17469 = ORIENTED_EDGE ( 'NONE', *, *, #22773, .F. ) ;
#17470 = ADVANCED_FACE ( 'NONE', ( #30016 ), #63494, .T. ) ;
#17471 = CARTESIAN_POINT ( 'NONE',  ( -4.458734124999999437, 15.35416666803225993, -2.574251347313719407 ) ) ;
#17472 = ORIENTED_EDGE ( 'NONE', *, *, #4642, .F. ) ;
#17473 = CARTESIAN_POINT ( 'NONE',  ( 4.458734124999998549, -94.72916666530106511, -2.574251347313721627 ) ) ;
#17474 = CARTESIAN_POINT ( 'NONE',  ( -3.152548672688508926E-16, 16.18750000136559564, -5.148502694627439702 ) ) ;
#17475 = CARTESIAN_POINT ( 'NONE',  ( 5.000000000000000000, 17.70833333606451632, -2.886751345948129988 ) ) ;
#17476 = CARTESIAN_POINT ( 'NONE',  ( -4.999999999999998224, -34.79166666393547303, 2.886751345948131764 ) ) ;
#17477 = CARTESIAN_POINT ( 'NONE',  ( -4.999999999999999112, 6.083333333333333037, 2.886751345948131764 ) ) ;
#17478 = CARTESIAN_POINT ( 'NONE',  ( -4.458734124999999437, -54.31249999863440081, 0.000000000000000000 ) ) ;
#17479 = CARTESIAN_POINT ( 'NONE',  ( -1.339745962155613812, -40.20534180126147561, -5.000000000000000000 ) ) ;
#17480 = CARTESIAN_POINT ( 'NONE',  ( -4.999999999999999112, -78.91666666666665719, 2.886751345948131764 ) ) ;
#17481 = EDGE_CURVE ( 'NONE', #19195, #38618, #34512, .T. ) ;
#17482 = CARTESIAN_POINT ( 'NONE',  ( 2.493747252781420335E-13, -43.12499999726882294, -5.000000000000000000 ) ) ;
#17483 = FACE_OUTER_BOUND ( 'NONE', #53970, .T. ) ;
#17484 = CARTESIAN_POINT ( 'NONE',  ( -5.000000000000000000, -25.95833333060214798, -2.886751345948128211 ) ) ;
#17485 = CYLINDRICAL_SURFACE ( 'NONE', #4266, 5.000000000000000000 ) ;
#17486 = CARTESIAN_POINT ( 'NONE',  ( 2.499999999999998668, -37.33333333333332860, -4.330127018922193649 ) ) ;
#17487 = DIRECTION ( 'NONE',  ( -0.000000000000000000, 1.000000000000000000, -0.000000000000000000 ) ) ;
#17489 = CARTESIAN_POINT ( 'NONE',  ( -3.152548672688508926E-16, -20.81249999863440081, -5.148502694627439702 ) ) ;
#17488 = CARTESIAN_POINT ( 'NONE',  ( -5.000000000000000000, -48.00000000000000000, 0.000000000000000000 ) ) ;
#17490 = FACE_OUTER_BOUND ( 'NONE', #57182, .T. ) ;
#17491 = CARTESIAN_POINT ( 'NONE',  ( -4.458734124999998549, -65.22916666530106511, 2.574251347313722516 ) ) ;
#17492 = CARTESIAN_POINT ( 'NONE',  ( -8.190561711645485556E-16, -149.9375000013656063, 4.458734124999999437 ) ) ;
#17493 = CARTESIAN_POINT ( 'NONE',  ( 2.229367062499998831, -71.64583333196773651, -3.861377020970580887 ) ) ;
#17494 = CARTESIAN_POINT ( 'NONE',  ( -50.55543936806279248, -146.3125000013656063, 0.3552334253322060320 ) ) ;
#17495 = CARTESIAN_POINT ( 'NONE',  ( -4.458734124999999437, -17.56249999863440792, 0.000000000000000000 ) ) ;
#17496 = CARTESIAN_POINT ( 'NONE',  ( 5.000000000000000000, -61.37499999726880873, -6.123233995736766282E-16 ) ) ;
#17497 = EDGE_LOOP ( 'NONE', ( #57513, #18903, #16150, #18431 ) ) ;
#17498 = CARTESIAN_POINT ( 'NONE',  ( 2.499999999999998668, -85.20833333060214443, -4.330127018922193649 ) ) ;
#17499 = ORIENTED_EDGE ( 'NONE', *, *, #53609, .F. ) ;
#17500 = CARTESIAN_POINT ( 'NONE',  ( -2.229367062499996610, -62.39583333196774362, 3.861377020970582219 ) ) ;
#17501 = CARTESIAN_POINT ( 'NONE',  ( 1.339745962155612702, -21.16965819600733312, -5.000000000000000000 ) ) ;
#17502 = CARTESIAN_POINT ( 'NONE',  ( -5.000000000000000000, -5.874999997268811391, 0.000000000000000000 ) ) ;
#17503 = CARTESIAN_POINT ( 'NONE',  ( -3.152801135295367096, -152.0625000013655779, -3.152801135295367541 ) ) ;
#17504 = ORIENTED_EDGE ( 'NONE', *, *, #39698, .T. ) ;
#17505 = AXIS2_PLACEMENT_3D ( 'NONE', #60329, #40042, #34575 ) ;
#17506 = CARTESIAN_POINT ( 'NONE',  ( -75.00000000000000000, 0.000000000000000000, 8.999999999999998224 ) ) ;
#17507 = DIRECTION ( 'NONE',  ( 0.000000000000000000, 0.000000000000000000, 1.000000000000000000 ) ) ;
#17508 = CARTESIAN_POINT ( 'NONE',  ( -6.972266317189433020E-16, -56.12499999726880162, -5.000000000000000000 ) ) ;
#17509 = CARTESIAN_POINT ( 'NONE',  ( 9.457646018065525792E-16, -53.31249999863441502, 5.148502694627439702 ) ) ;
#17510 = ORIENTED_EDGE ( 'NONE', *, *, #33833, .T. ) ;
#17511 = CARTESIAN_POINT ( 'NONE',  ( 3.750000000000005329, 6.495190528383288253, 0.000000000000000000 ) ) ;
#17512 = CARTESIAN_POINT ( 'NONE',  ( 2.229367062500001939, 7.020833334698928674, 3.861377020970579999 ) ) ;
#17513 = CARTESIAN_POINT ( 'NONE',  ( -4.458734124999999437, 23.60416666803225993, -2.574251347313719407 ) ) ;
#17514 = CARTESIAN_POINT ( 'NONE',  ( -57.89159099828107458, -150.6875000013656063, -3.393966926194107447 ) ) ;
#17515 = CARTESIAN_POINT ( 'NONE',  ( 5.000000000000000000, -77.50000000000000000, -6.123233995736766282E-16 ) ) ;
#17516 = CARTESIAN_POINT ( 'NONE',  ( 1.846868145590736310, -167.6250000013656347, 4.458734124999997661 ) ) ;
#17517 =( BOUNDED_CURVE ( )  B_SPLINE_CURVE ( 2, ( #50262, #45438, #41232, #44792, #55733, #59933, #40607, #5891, #6845 ),
 .UNSPECIFIED., .F., .F. ) 
 B_SPLINE_CURVE_WITH_KNOTS ( ( 3, 2, 2, 2, 3 ),
 ( 0.04821428571428571647, 0.04880952380952380959, 0.05000000000000000278, 0.05119047619047618902, 0.05178571428571428908 ),
 .UNSPECIFIED. ) 
 CURVE ( )  GEOMETRIC_REPRESENTATION_ITEM ( )  RATIONAL_B_SPLINE_CURVE ( ( 0.9330127018922194093, 0.9330127018922197424, 1.000000000000000000, 0.8660254037844387076, 1.000000000000000000, 0.8660254037844387076, 1.000000000000000000, 0.9330127018922189652, 0.9330127018922194093 ) ) 
 REPRESENTATION_ITEM ( '' )  );
#17518 = ORIENTED_EDGE ( 'NONE', *, *, #34267, .T. ) ;
#17519 = CARTESIAN_POINT ( 'NONE',  ( 4.458734124999999437, -70.81249999863439371, -5.460374474430324690E-16 ) ) ;
#17520 = CARTESIAN_POINT ( 'NONE',  ( -4.458734124999999437, 5.604166668032262599, -2.574251347313719407 ) ) ;
#17521 = ADVANCED_FACE ( 'NONE', ( #14276 ), #48373, .T. ) ;
#17522 = CARTESIAN_POINT ( 'NONE',  ( -2.500000000000000444, -42.16666666666667140, -4.330127018922193649 ) ) ;
#17523 = CARTESIAN_POINT ( 'NONE',  ( 2.229367062499998831, -60.89583333196774362, -3.861377020970580887 ) ) ;
#17524 = CARTESIAN_POINT ( 'NONE',  ( -3.535250795749689387E-16, -17.12499999726881583, -5.773502691896257311 ) ) ;
#17525 = DIRECTION ( 'NONE',  ( 0.000000000000000000, 0.000000000000000000, 1.000000000000000000 ) ) ;
#17526 = CARTESIAN_POINT ( 'NONE',  ( 1.975475456537005874E-15, -49.62499999726880873, 5.000000000000000000 ) ) ;
#17527 = CARTESIAN_POINT ( 'NONE',  ( 1.339745962155615144, 19.41965820146970501, 4.999999999999999112 ) ) ;
#17528 = DIRECTION ( 'NONE',  ( 0.000000000000000000, 1.000000000000000000, 0.000000000000000000 ) ) ;
#17529 = CARTESIAN_POINT ( 'NONE',  ( -4.458734124999998549, -35.22916666530107221, 2.574251347313722516 ) ) ;
#17530 = CARTESIAN_POINT ( 'NONE',  ( 4.458734125000000326, -24.14583333196774362, 2.574251347313718519 ) ) ;
#17531 = ORIENTED_EDGE ( 'NONE', *, *, #15862, .F. ) ;
#17532 = CARTESIAN_POINT ( 'NONE',  ( -6.972266317189433020E-16, -36.25000000000000000, -5.000000000000000000 ) ) ;
#17533 = CARTESIAN_POINT ( 'NONE',  ( 5.000000000000000888, 29.41666666666666785, 2.886751345948126879 ) ) ;
#17534 = CARTESIAN_POINT ( 'NONE',  ( -5.000000000000000888, -153.5625000027312126, 2.071067811865474617 ) ) ;
#17535 = ORIENTED_EDGE ( 'NONE', *, *, #61829, .T. ) ;
#17536 = CARTESIAN_POINT ( 'NONE',  ( -4.458734124999998549, -104.4791666653010651, 2.574251347313722516 ) ) ;
#17537 = CARTESIAN_POINT ( 'NONE',  ( 4.458734125000001214, -33.89583333196773651, 2.574251347313718519 ) ) ;
#17538 = CARTESIAN_POINT ( 'NONE',  ( -5.000000000000000000, -62.95833333060214443, -2.886751345948128211 ) ) ;
#17539 = CARTESIAN_POINT ( 'NONE',  ( -59.29741812935640155, -151.8750000013655779, -2.196230717870135685 ) ) ;
#17540 = CARTESIAN_POINT ( 'NONE',  ( 3.061616997868383141E-16, -145.7500000000000284, -5.000000000000000000 ) ) ;
#17541 = CARTESIAN_POINT ( 'NONE',  ( 4.458734124999999437, -26.81249999863440081, -5.460374474430324690E-16 ) ) ;
#17542 = CARTESIAN_POINT ( 'NONE',  ( -2.229367062499996610, -69.39583333196773651, 3.861377020970582219 ) ) ;
#17543 = CARTESIAN_POINT ( 'NONE',  ( -9.184850993605147944E-16, -141.3750000027312126, 5.000000000000000000 ) ) ;
#17544 = CARTESIAN_POINT ( 'NONE',  ( -4.458734124999999437, -26.31249999863440792, 0.000000000000000000 ) ) ;
#17545 = CARTESIAN_POINT ( 'NONE',  ( 1.975475456537005874E-15, -32.74999999999999289, 5.000000000000000000 ) ) ;
#17546 = CARTESIAN_POINT ( 'NONE',  ( 5.000000000000000888, 18.54166666939785202, 2.886751345948126879 ) ) ;
#17547 = CARTESIAN_POINT ( 'NONE',  ( 2.499999999999998668, -17.33333333333333215, -4.330127018922193649 ) ) ;
#17548 = CARTESIAN_POINT ( 'NONE',  ( -4.458734124999999437, -147.9375000013656063, -5.460374474430324690E-16 ) ) ;
#17549 = ORIENTED_EDGE ( 'NONE', *, *, #53458, .T. ) ;
#17550 = CARTESIAN_POINT ( 'NONE',  ( -6.972266317189433020E-16, -82.24999999999998579, -5.000000000000000000 ) ) ;
#17551 = CARTESIAN_POINT ( 'NONE',  ( -2.229367062499996610, -50.39583333196772941, 3.861377020970582219 ) ) ;
#17552 =( BOUNDED_CURVE ( )  B_SPLINE_CURVE ( 2, ( #30701, #25558, #31658, #11711, #50326, #60944, #5949, #17180, #45175 ),
 .UNSPECIFIED., .F., .F. ) 
 B_SPLINE_CURVE_WITH_KNOTS ( ( 3, 2, 2, 2, 3 ),
 ( 0.1520833333333333481, 0.1527777777777777901, 0.1541666666666666741, 0.1555555555555555580, 0.1562500000000000000 ),
 .UNSPECIFIED. ) 
 CURVE ( )  GEOMETRIC_REPRESENTATION_ITEM ( )  RATIONAL_B_SPLINE_CURVE ( ( 0.9330127018922194093, 0.9330127018922207416, 1.000000000000000000, 0.8660254037844387076, 1.000000000000000000, 0.8660254037844387076, 1.000000000000000000, 0.9330127018922194093, 0.9330127018922194093 ) ) 
 REPRESENTATION_ITEM ( '' )  );
#17553 = DIRECTION ( 'NONE',  ( -0.000000000000000000, 1.000000000000000000, -0.000000000000000000 ) ) ;
#17554 = CARTESIAN_POINT ( 'NONE',  ( 6.158835246850667461E-14, -1.250000000000002442, -4.999999999999999112 ) ) ;
#17555 = CARTESIAN_POINT ( 'NONE',  ( 5.000000000000000000, 26.58333333333333570, -2.886751345948129988 ) ) ;
#17556 = DIRECTION ( 'NONE',  ( 0.000000000000000000, 0.000000000000000000, 1.000000000000000000 ) ) ;
#17557 = CARTESIAN_POINT ( 'NONE',  ( 4.458734124999998549, -0.7291666653010709931, -2.574251347313721627 ) ) ;
#17558 = CARTESIAN_POINT ( 'NONE',  ( -2.500000000000000444, -11.16666666666666430, -4.330127018922193649 ) ) ;
#17559 = CARTESIAN_POINT ( 'NONE',  ( 5.000000000000000000, -14.49999999999999822, -6.123233995736766282E-16 ) ) ;
#17560 = CARTESIAN_POINT ( 'NONE',  ( 1.339745962155612702, -87.16965819600731891, -5.000000000000000000 ) ) ;
#17561 = CARTESIAN_POINT ( 'NONE',  ( -3.152548672688508926E-16, 11.18750000136559564, -5.148502694627439702 ) ) ;
#17562 = ORIENTED_EDGE ( 'NONE', *, *, #5516, .T. ) ;
#17563 = CARTESIAN_POINT ( 'NONE',  ( -6.972266317189433020E-16, -30.12499999726880873, -5.000000000000000000 ) ) ;
#17564 = VERTEX_POINT ( 'NONE', #58976 ) ;
#17565 = DIRECTION ( 'NONE',  ( 0.000000000000000000, 0.000000000000000000, 1.000000000000000000 ) ) ;
#17566 = CARTESIAN_POINT ( 'NONE',  ( 4.458734124999999437, -50.81249999863440792, -5.460374474430324690E-16 ) ) ;
#17567 = CARTESIAN_POINT ( 'NONE',  ( -4.458734124999999437, -163.1875000013655779, -5.460374474430324690E-16 ) ) ;
#17568 = CARTESIAN_POINT ( 'NONE',  ( 5.000000000000000888, -43.45833333060214443, 2.886751345948126879 ) ) ;
#17569 = VERTEX_POINT ( 'NONE', #43536 ) ;
#17570 = CARTESIAN_POINT ( 'NONE',  ( -4.458734124999999437, -25.39583333196773651, -2.574251347313719407 ) ) ;
#17571 = ORIENTED_EDGE ( 'NONE', *, *, #6431, .F. ) ;
#17572 = CARTESIAN_POINT ( 'NONE',  ( 2.500000000000002220, -53.66666666666667140, 4.330127018922192761 ) ) ;
#17573 = CARTESIAN_POINT ( 'NONE',  ( -1.846868145590737420, -164.7500000013656063, 4.458734124999999437 ) ) ;
#17574 = CARTESIAN_POINT ( 'NONE',  ( 5.000000000000000000, -39.29166666393548724, -2.886751345948130876 ) ) ;
#17575 = CARTESIAN_POINT ( 'NONE',  ( -51.75738570946856498, -135.7500000000000284, 3.805975901505576964 ) ) ;
#17576 = EDGE_CURVE ( 'NONE', #41033, #21097, #42842, .T. ) ;
#17577 = CARTESIAN_POINT ( 'NONE',  ( -4.458734124999999437, -38.64583333196772941, -2.574251347313719407 ) ) ;
#17578 = CARTESIAN_POINT ( 'NONE',  ( -2.500000000000000444, 19.95833333606451987, -4.330127018922193649 ) ) ;
#17579 = ORIENTED_EDGE ( 'NONE', *, *, #11849, .T. ) ;
#17580 = CONTEXT_DEPENDENT_SHAPE_REPRESENTATION ( #48316, #53811 ) ;
#17581 = CARTESIAN_POINT ( 'NONE',  ( -4.458734124999999437, -82.39583333196773651, -2.574251347313719407 ) ) ;
#17582 = CARTESIAN_POINT ( 'NONE',  ( -4.458734124999999437, 25.68750000136559208, 0.000000000000000000 ) ) ;
#17583 = CARTESIAN_POINT ( 'NONE',  ( 1.339745962155612702, 24.83034180399266333, -5.000000000000000000 ) ) ;
#17584 = ORIENTED_EDGE ( 'NONE', *, *, #40951, .T. ) ;
#17585 = CYLINDRICAL_SURFACE ( 'NONE', #53116, 5.000000000000000000 ) ;
#17586 = CARTESIAN_POINT ( 'NONE',  ( -56.48576386720575471, -139.0000000013655779, -4.591703134518078322 ) ) ;
#17587 = CARTESIAN_POINT ( 'NONE',  ( 4.458734125000001214, -79.14583333196772230, 2.574251347313718519 ) ) ;
#17588 = CARTESIAN_POINT ( 'NONE',  ( -58.80597590150559739, -132.1250000027312126, 3.242614290531460330 ) ) ;
#17589 = CARTESIAN_POINT ( 'NONE',  ( 0.000000000000000000, -120.0000000000000000, 5.000000000000000000 ) ) ;
#17590 = CYLINDRICAL_SURFACE ( 'NONE', #8955, 5.000000000000000000 ) ;
#17591 = CARTESIAN_POINT ( 'NONE',  ( 2.500000000000002220, -13.54166666393548013, 4.330127018922192761 ) ) ;
#17592 = CARTESIAN_POINT ( 'NONE',  ( -4.458734124999999437, -55.39583333196773651, -2.574251347313719407 ) ) ;
#17593 = CARTESIAN_POINT ( 'NONE',  ( -2.500000000000000444, -72.04166666393548724, -4.330127018922193649 ) ) ;
#17594 = VECTOR ( 'NONE', #47304, 1000.000000000000000 ) ;
#17595 = CARTESIAN_POINT ( 'NONE',  ( 2.229367062499998831, 27.35416666803225993, -3.861377020970580887 ) ) ;
#17596 = CARTESIAN_POINT ( 'NONE',  ( 2.499999999999998668, -104.3333333333333286, -4.330127018922193649 ) ) ;
#17597 = CARTESIAN_POINT ( 'NONE',  ( -5.000000000000000000, 4.000000000000000000, 0.000000000000000000 ) ) ;
#17598 = CARTESIAN_POINT ( 'NONE',  ( -4.458734124999999437, -39.56249999863440081, 0.000000000000000000 ) ) ;
#17599 = CARTESIAN_POINT ( 'NONE',  ( -2.499999999999996447, -0.7083333306021483144, 4.330127018922195425 ) ) ;
#17600 = CARTESIAN_POINT ( 'NONE',  ( -59.81910112700025905, -154.1875000000000284, -2.462841084822619209 ) ) ;
#17601 = CYLINDRICAL_SURFACE ( 'NONE', #36758, 5.000000000000000000 ) ;
#17602 = CARTESIAN_POINT ( 'NONE',  ( 9.457646018065525792E-16, -78.31249999863442213, 5.148502694627439702 ) ) ;
#17603 = CARTESIAN_POINT ( 'NONE',  ( -4.458734124999999437, -100.3124999986344079, 0.000000000000000000 ) ) ;
#17604 = CARTESIAN_POINT ( 'NONE',  ( 2.229367062500001939, -6.229166665301072214, 3.861377020970579999 ) ) ;
#17605 = ORIENTED_EDGE ( 'NONE', *, *, #20483, .T. ) ;
#17606 = CARTESIAN_POINT ( 'NONE',  ( 1.975475456537005874E-15, -85.62499999726880162, 5.000000000000000000 ) ) ;
#17607 = CARTESIAN_POINT ( 'NONE',  ( 4.458734124999999437, -94.81249999863440792, -5.460374474430324690E-16 ) ) ;
#17608 = CARTESIAN_POINT ( 'NONE',  ( -5.000000000000000888, -164.6875000027311842, -2.071067811865475949 ) ) ;
#17609 = CARTESIAN_POINT ( 'NONE',  ( -4.458734124999998549, -84.47916666530107932, 2.574251347313722516 ) ) ;
#17610 = CARTESIAN_POINT ( 'NONE',  ( 4.458734124999998549, 13.02083333469892779, -2.574251347313721627 ) ) ;
#17611 = DIRECTION ( 'NONE',  ( -0.000000000000000000, 1.000000000000000000, -0.000000000000000000 ) ) ;
#17612 = CARTESIAN_POINT ( 'NONE',  ( -55.35523342533222291, -134.3125000013656063, 4.444560631937231499 ) ) ;
#17613 = CARTESIAN_POINT ( 'NONE',  ( 4.458734124999998549, -12.72916666530106866, -2.574251347313721627 ) ) ;
#17614 = CARTESIAN_POINT ( 'NONE',  ( -4.458734124999998549, 18.52083333469892779, 2.574251347313722516 ) ) ;
#17615 = CARTESIAN_POINT ( 'NONE',  ( -4.458734124999997661, -53.47916666530107221, 2.574251347313722516 ) ) ;
#17616 = CARTESIAN_POINT ( 'NONE',  ( 3.061616997868383141E-16, -168.7500000000000000, -5.000000000000000000 ) ) ;
#17617 = CARTESIAN_POINT ( 'NONE',  ( 0.000000000000000000, -170.0000000000000000, 0.000000000000000000 ) ) ;
#17618 = CARTESIAN_POINT ( 'NONE',  ( -4.458734124999999437, -7.395833331967734736, -2.574251347313719407 ) ) ;
#17619 = CARTESIAN_POINT ( 'NONE',  ( -6.972266317189433020E-16, -29.25000000000000000, -5.000000000000000000 ) ) ;
#17620 = ORIENTED_EDGE ( 'NONE', *, *, #24837, .T. ) ;
#17621 = CARTESIAN_POINT ( 'NONE',  ( 2.229367062499998831, -35.89583333196773651, -3.861377020970580887 ) ) ;
#17622 = CARTESIAN_POINT ( 'NONE',  ( -52.80376928212989185, -126.1250000013656205, -4.297418129356379346 ) ) ;
#17623 = CARTESIAN_POINT ( 'NONE',  ( 7.204675194429079505E-15, 26.87500000273118417, -5.000000000000000000 ) ) ;
#17624 = CARTESIAN_POINT ( 'NONE',  ( 9.457646018065525792E-16, -79.06249999863440792, 5.148502694627439702 ) ) ;
#17625 = CARTESIAN_POINT ( 'NONE',  ( 4.458734124999998549, 26.02083333469892779, -2.574251347313721627 ) ) ;
#17626 = CARTESIAN_POINT ( 'NONE',  ( 4.458734124999997661, -150.7500000013656347, 1.846868145590737864 ) ) ;
#17627 = CARTESIAN_POINT ( 'NONE',  ( -2.229367062500000163, 15.52083333469892779, -3.861377020970580443 ) ) ;
#17628 = CARTESIAN_POINT ( 'NONE',  ( -50.18089887299976937, -137.8125000027312126, 2.462841084822337656 ) ) ;
#17629 = CARTESIAN_POINT ( 'NONE',  ( 2.229367062499998831, -85.89583333196773651, -3.861377020970580887 ) ) ;
#17630 = CARTESIAN_POINT ( 'NONE',  ( -3.535250795749689387E-16, -64.25000000000000000, -5.773502691896257311 ) ) ;
#17631 = CARTESIAN_POINT ( 'NONE',  ( 4.648177544792955347E-16, 29.75000000000000355, -5.000000000000000000 ) ) ;
#17632 = CARTESIAN_POINT ( 'NONE',  ( 2.500000000000002220, 19.45833333606451632, 4.330127018922192761 ) ) ;
#17633 = VERTEX_POINT ( 'NONE', #774 ) ;
#17634 = CARTESIAN_POINT ( 'NONE',  ( -6.972266317189433020E-16, -66.12499999726881583, -5.000000000000000000 ) ) ;
#17636 = CARTESIAN_POINT ( 'NONE',  ( 5.000000000000000888, -27.58333333333333215, 2.886751345948126879 ) ) ;
#17635 = FACE_OUTER_BOUND ( 'NONE', #63392, .T. ) ;
#17637 = CARTESIAN_POINT ( 'NONE',  ( 2.229367062500001939, -31.97916666530106866, 3.861377020970579999 ) ) ;
#17638 = CARTESIAN_POINT ( 'NONE',  ( -2.500000000000000444, 4.833333333333332149, -4.330127018922193649 ) ) ;
#17639 =( BOUNDED_CURVE ( )  B_SPLINE_CURVE ( 2, ( #54868, #30411, #5993, #37165, #16585, #61929, #17848, #56471, #36205 ),
 .UNSPECIFIED., .F., .F. ) 
 B_SPLINE_CURVE_WITH_KNOTS ( ( 3, 2, 2, 2, 3 ),
 ( 0.4482142857142857317, 0.4488095238095238249, 0.4500000000000000111, 0.4511904761904761973, 0.4517857142857142905 ),
 .UNSPECIFIED. ) 
 CURVE ( )  GEOMETRIC_REPRESENTATION_ITEM ( )  RATIONAL_B_SPLINE_CURVE ( ( 0.9330127018922194093, 0.9330127018922194093, 1.000000000000000000, 0.8660254037844387076, 1.000000000000000000, 0.8660254037844387076, 1.000000000000000000, 0.9330127018922194093, 0.9330127018922194093 ) ) 
 REPRESENTATION_ITEM ( '' )  );
#17640 = CARTESIAN_POINT ( 'NONE',  ( 2.500000000000002220, -26.54166666393547658, 4.330127018922192761 ) ) ;
#17642 = ORIENTED_EDGE ( 'NONE', *, *, #63242, .T. ) ;
#17641 = CARTESIAN_POINT ( 'NONE',  ( -2.229367062499996610, -59.14583333196773651, 3.861377020970582219 ) ) ;
#17643 = CARTESIAN_POINT ( 'NONE',  ( -53.51423613279429503, -154.5000000013655779, 4.591703134518082763 ) ) ;
#17645 = ORIENTED_EDGE ( 'NONE', *, *, #13796, .F. ) ;
#17644 = CARTESIAN_POINT ( 'NONE',  ( 4.458734124999998549, -10.97916666530107044, -2.574251347313721627 ) ) ;
#17646 = CARTESIAN_POINT ( 'NONE',  ( -5.000000000000000000, -71.00000000000000000, 0.000000000000000000 ) ) ;
#17647 = CARTESIAN_POINT ( 'NONE',  ( -55.35523342533222291, -137.3125000013656063, 4.444560631937231499 ) ) ;
#17648 = AXIS2_PLACEMENT_3D ( 'NONE', #5224, #20338, #10363 ) ;
#17649 = CARTESIAN_POINT ( 'NONE',  ( -4.458734124999998549, -49.47916666530106511, 2.574251347313722516 ) ) ;
#17650 = CARTESIAN_POINT ( 'NONE',  ( 5.000000000000000888, -77.45833333060213022, 2.886751345948126879 ) ) ;
#17652 = VERTEX_POINT ( 'NONE', #10082 ) ;
#17651 = CARTESIAN_POINT ( 'NONE',  ( -6.972266317189433020E-16, -13.25000000000000000, -5.000000000000000000 ) ) ;
#17653 = CARTESIAN_POINT ( 'NONE',  ( -59.98410592259440222, -149.1250000000000284, -0.3983568153799752487 ) ) ;
#17654 = EDGE_CURVE ( 'NONE', #62091, #21757, #24566, .T. ) ;
#17655 = CARTESIAN_POINT ( 'NONE',  ( -4.458734124999999437, -17.64583333196773651, -2.574251347313719407 ) ) ;
#17656 = CARTESIAN_POINT ( 'NONE',  ( 2.229367062500001939, -55.22916666530107221, 3.861377020970579999 ) ) ;
#17657 = CARTESIAN_POINT ( 'NONE',  ( -5.000000000000000000, -24.08333333333333215, -2.886751345948128211 ) ) ;
#17658 = CARTESIAN_POINT ( 'NONE',  ( -4.458734125000000326, -142.0000000013655495, -1.846868145590735644 ) ) ;
#17659 = CARTESIAN_POINT ( 'NONE',  ( -2.229367062500000163, -98.72916666530105090, -3.861377020970580443 ) ) ;
#17660 = CARTESIAN_POINT ( 'NONE',  ( 0.000000000000000000, -170.0000000000000000, 0.000000000000000000 ) ) ;
#17661 = ORIENTED_EDGE ( 'NONE', *, *, #3313, .F. ) ;
#17662 = CARTESIAN_POINT ( 'NONE',  ( -54.64476657466781973, -153.0625000013656063, -4.444560631937228834 ) ) ;
#17663 = CARTESIAN_POINT ( 'NONE',  ( -49.85088928181150436, -143.6875000027312126, -1.666127454062680702 ) ) ;
#17664 = EDGE_CURVE ( 'NONE', #57381, #27617, #29693, .T. ) ;
#17665 = DIRECTION ( 'NONE',  ( 0.000000000000000000, 0.000000000000000000, 1.000000000000000000 ) ) ;
#17666 = CARTESIAN_POINT ( 'NONE',  ( -3.152548672688508926E-16, -5.562499998634402587, -5.148502694627439702 ) ) ;
#17667 = CARTESIAN_POINT ( 'NONE',  ( -4.458734124999999437, -95.64583333196773651, -2.574251347313719407 ) ) ;
#17668 = CARTESIAN_POINT ( 'NONE',  ( 1.846868145590736310, -146.8750000013656063, 4.458734124999999437 ) ) ;
#17669 = CARTESIAN_POINT ( 'NONE',  ( -4.458734124999998549, -20.47916666530107577, 2.574251347313722516 ) ) ;
#17670 = ADVANCED_FACE ( 'NONE', ( #23935 ), #9756, .T. ) ;
#17671 = CARTESIAN_POINT ( 'NONE',  ( -6.972266317189433020E-16, 1.875000002731185722, -5.000000000000000000 ) ) ;
#17672 = CARTESIAN_POINT ( 'NONE',  ( -52.80376928212989185, -137.8750000013655779, -4.297418129356379346 ) ) ;
#17673 = CARTESIAN_POINT ( 'NONE',  ( 4.458734125000001214, -64.14583333196773651, 2.574251347313718519 ) ) ;
#17674 = CARTESIAN_POINT ( 'NONE',  ( -5.000000000000000888, -154.5625000027311842, 2.071067811865474617 ) ) ;
#17675 = CARTESIAN_POINT ( 'NONE',  ( -8.190561711645485556E-16, -146.6875000013656063, 4.458734124999999437 ) ) ;
#17676 = CARTESIAN_POINT ( 'NONE',  ( 2.229367062499998831, 12.10416666803226171, -3.861377020970580887 ) ) ;
#17677 = ORIENTED_EDGE ( 'NONE', *, *, #31726, .T. ) ;
#17678 = CARTESIAN_POINT ( 'NONE',  ( -5.000000000000000000, -52.95833333060214443, -2.886751345948128211 ) ) ;
#17679 = CARTESIAN_POINT ( 'NONE',  ( 0.000000000000000000, -120.0000000000000000, 0.000000000000000000 ) ) ;
#17681 = CARTESIAN_POINT ( 'NONE',  ( -4.458734124999999437, -22.31249999863440436, 0.000000000000000000 ) ) ;
#17680 = CARTESIAN_POINT ( 'NONE',  ( -5.000000000000000000, -89.00000000000000000, 0.000000000000000000 ) ) ;
#17682 = CARTESIAN_POINT ( 'NONE',  ( 1.339745962155615144, -36.70534180126148271, 4.999999999999999112 ) ) ;
#17683 = CARTESIAN_POINT ( 'NONE',  ( 9.457646018065525792E-16, -73.31249999863440792, 5.148502694627439702 ) ) ;
#17684 = CARTESIAN_POINT ( 'NONE',  ( 4.458734124999998549, 27.02083333469892068, -2.574251347313721627 ) ) ;
#17685 = CARTESIAN_POINT ( 'NONE',  ( 2.500000000000002220, -76.54166666393547303, 4.330127018922192761 ) ) ;
#17686 = CARTESIAN_POINT ( 'NONE',  ( -56.48576386720575471, -145.7500000013655779, -4.591703134518078322 ) ) ;
#17687 = CARTESIAN_POINT ( 'NONE',  ( 4.458734124999999437, 2.187500001365593416, -5.460374474430324690E-16 ) ) ;
#17688 = FACE_OUTER_BOUND ( 'NONE', #4824, .T. ) ;
#17689 = DIRECTION ( 'NONE',  ( -0.000000000000000000, 1.000000000000000000, -0.000000000000000000 ) ) ;
#17690 = CARTESIAN_POINT ( 'NONE',  ( -4.458734124999997661, 5.770833334698928674, 2.574251347313722516 ) ) ;
#17691 = CARTESIAN_POINT ( 'NONE',  ( 9.457646018065525792E-16, -73.06249999863440792, 5.148502694627439702 ) ) ;
#17692 = CARTESIAN_POINT ( 'NONE',  ( 4.458734124999999437, -20.06249999863440081, -5.460374474430324690E-16 ) ) ;
#17693 =( BOUNDED_CURVE ( )  B_SPLINE_CURVE ( 2, ( #30577, #9681, #5189, #1343, #25438, #24486, #45058, #58892, #34126 ),
 .UNSPECIFIED., .F., .F. ) 
 B_SPLINE_CURVE_WITH_KNOTS ( ( 3, 2, 2, 2, 3 ),
 ( 0.8270833333333332815, 0.8277777777777777235, 0.8291666666666667185, 0.8305555555555556024, 0.8312500000000000444 ),
 .UNSPECIFIED. ) 
 CURVE ( )  GEOMETRIC_REPRESENTATION_ITEM ( )  RATIONAL_B_SPLINE_CURVE ( ( 0.9330127018922194093, 0.9330127018922194093, 1.000000000000000000, 0.8660254037844387076, 1.000000000000000000, 0.8660254037844387076, 1.000000000000000000, 0.9330127018922194093, 0.9330127018922194093 ) ) 
 REPRESENTATION_ITEM ( '' )  );
#17694 = CARTESIAN_POINT ( 'NONE',  ( 1.060575238724906964E-15, -2.750000000000002220, 5.773502691896257311 ) ) ;
#17695 = CARTESIAN_POINT ( 'NONE',  ( -1.846868145590734756, -158.1250000013656063, -4.458734125000000326 ) ) ;
#17696 = CARTESIAN_POINT ( 'NONE',  ( -1.339745962155613368, 28.91965820146970501, -5.000000000000000000 ) ) ;
#17697 = CARTESIAN_POINT ( 'NONE',  ( 2.229367062499998831, -62.64583333196774362, -3.861377020970580887 ) ) ;
#17698 = CARTESIAN_POINT ( 'NONE',  ( -3.535250795749689387E-16, -98.12499999726881583, -5.773502691896257311 ) ) ;
#17699 = CARTESIAN_POINT ( 'NONE',  ( -4.458734124999999437, -39.39583333196773651, -2.574251347313719407 ) ) ;
#17700 = ADVANCED_FACE ( 'NONE', ( #48679 ), #58029, .T. ) ;
#17701 = CARTESIAN_POINT ( 'NONE',  ( -4.458734124999999437, -107.6458333319677223, -2.574251347313719407 ) ) ;
#17702 = CARTESIAN_POINT ( 'NONE',  ( -2.229367062499996610, -69.39583333196773651, 3.861377020970582219 ) ) ;
#17703 = CARTESIAN_POINT ( 'NONE',  ( -2.500000000000000444, -48.16666666666666430, -4.330127018922193649 ) ) ;
#17704 = CARTESIAN_POINT ( 'NONE',  ( 2.499999999999998668, -57.20833333060214443, -4.330127018922193649 ) ) ;
#17705 = FACE_OUTER_BOUND ( 'NONE', #23555, .T. ) ;
#17706 = ORIENTED_EDGE ( 'NONE', *, *, #46410, .T. ) ;
#17707 = DIRECTION ( 'NONE',  ( -0.000000000000000000, 1.000000000000000000, -0.000000000000000000 ) ) ;
#17708 = DIRECTION ( 'NONE',  ( -0.000000000000000000, 1.000000000000000000, -0.000000000000000000 ) ) ;
#17709 = CARTESIAN_POINT ( 'NONE',  ( 5.000000000000000000, -5.416666666666666963, -2.886751345948129988 ) ) ;
#17710 = CARTESIAN_POINT ( 'NONE',  ( -4.458734124999999437, -75.39583333196773651, -2.574251347313719407 ) ) ;
#17711 = DIRECTION ( 'NONE',  ( -0.6485228581062915110, 0.000000000000000000, -0.7611951803011149931 ) ) ;
#17712 = CARTESIAN_POINT ( 'NONE',  ( -5.000000000000000000, -14.87499999726881228, 0.000000000000000000 ) ) ;
#17714 = ORIENTED_EDGE ( 'NONE', *, *, #15336, .T. ) ;
#17713 = CARTESIAN_POINT ( 'NONE',  ( 9.457646018065525792E-16, -42.06249999863440081, 5.148502694627439702 ) ) ;
#17715 = CARTESIAN_POINT ( 'NONE',  ( 1.339745962155612702, -100.1696581960073473, -5.000000000000000000 ) ) ;
#17717 = ORIENTED_EDGE ( 'NONE', *, *, #63257, .F. ) ;
#17716 = CARTESIAN_POINT ( 'NONE',  ( 2.229367062500001939, 4.770833334698926897, 3.861377020970579999 ) ) ;
#17718 = CARTESIAN_POINT ( 'NONE',  ( -6.972266317189433020E-16, -81.12499999726881583, -5.000000000000000000 ) ) ;
#17719 = CARTESIAN_POINT ( 'NONE',  ( -3.535250795749689387E-16, -58.24999999999999289, -5.773502691896257311 ) ) ;
#17720 = CARTESIAN_POINT ( 'NONE',  ( 3.152801135295366208, -158.8125000013656063, 3.152801135295367985 ) ) ;
#17721 = CARTESIAN_POINT ( 'NONE',  ( -4.458734124999999437, -34.64583333196773651, -2.574251347313719407 ) ) ;
#17722 = CARTESIAN_POINT ( 'NONE',  ( 4.458734124999998549, -79.72916666530107932, -2.574251347313721627 ) ) ;
#17723 = CARTESIAN_POINT ( 'NONE',  ( 2.071067811865475505, -166.8125000000000000, -5.000000000000000888 ) ) ;
#17724 = CARTESIAN_POINT ( 'NONE',  ( 4.458734125000001214, -89.89583333196775072, 2.574251347313718519 ) ) ;
#17725 = CARTESIAN_POINT ( 'NONE',  ( -59.59170313451811296, -130.7500000013656063, 1.485763867205729394 ) ) ;
#17726 = CARTESIAN_POINT ( 'NONE',  ( 4.458734125000001214, -2.145833331967737845, 2.574251347313718519 ) ) ;
#17727 = CARTESIAN_POINT ( 'NONE',  ( -2.229367062500000163, -39.72916666530107221, -3.861377020970580443 ) ) ;
#17728 = ADVANCED_FACE ( 'NONE', ( #43848 ), #49324, .T. ) ;
#17729 = ADVANCED_FACE ( 'NONE', ( #48996 ), #9139, .T. ) ;
#17730 = CARTESIAN_POINT ( 'NONE',  ( -2.229367062499996610, -81.39583333196773651, 3.861377020970582219 ) ) ;
#17731 = CARTESIAN_POINT ( 'NONE',  ( 3.061616997868383141E-16, -154.7500000000000000, -5.000000000000000000 ) ) ;
#17732 = ORIENTED_EDGE ( 'NONE', *, *, #45025, .F. ) ;
#17733 =( BOUNDED_CURVE ( )  B_SPLINE_CURVE ( 2, ( #44829, #35197, #54495, #24904, #45153, #30682, #1119, #15248, #54159 ),
 .UNSPECIFIED., .F., .F. ) 
 B_SPLINE_CURVE_WITH_KNOTS ( ( 3, 2, 2, 2, 3 ),
 ( 0.7767857142857143016, 0.7773809523809523947, 0.7785714285714285809, 0.7797619047619047672, 0.7803571428571428603 ),
 .UNSPECIFIED. ) 
 CURVE ( )  GEOMETRIC_REPRESENTATION_ITEM ( )  RATIONAL_B_SPLINE_CURVE ( ( 0.9330127018922194093, 0.9330127018922194093, 1.000000000000000000, 0.8660254037844387076, 1.000000000000000000, 0.8660254037844387076, 1.000000000000000000, 0.9330127018922194093, 0.9330127018922194093 ) ) 
 REPRESENTATION_ITEM ( '' )  );
#17734 = CYLINDRICAL_SURFACE ( 'NONE', #29088, 5.000000000000000000 ) ;
#17735 = CARTESIAN_POINT ( 'NONE',  ( 2.229367062500001939, -68.22916666530106511, 3.861377020970579999 ) ) ;
#17736 = CARTESIAN_POINT ( 'NONE',  ( -4.458734124999997661, -37.22916666530107221, 2.574251347313722516 ) ) ;
#17737 = CARTESIAN_POINT ( 'NONE',  ( 4.458734125000001214, -10.14583333196773829, 2.574251347313718519 ) ) ;
#17738 = ORIENTED_EDGE ( 'NONE', *, *, #33852, .F. ) ;
#17739 = EDGE_CURVE ( 'NONE', #51645, #22889, #14466, .T. ) ;
#17740 = CARTESIAN_POINT ( 'NONE',  ( 6.123233995736766282E-16, -120.0000000000000000, -5.000000000000000000 ) ) ;
#17741 = CARTESIAN_POINT ( 'NONE',  ( 3.061616997868383141E-16, -146.8750000027312126, -5.000000000000000000 ) ) ;
#17742 = CARTESIAN_POINT ( 'NONE',  ( -4.458734124999998549, -5.479166665301072214, 2.574251347313722516 ) ) ;
#17743 = EDGE_CURVE ( 'NONE', #16398, #8313, #9174, .T. ) ;
#17744 = CARTESIAN_POINT ( 'NONE',  ( -6.972266317189433020E-16, -85.12499999726880162, -5.000000000000000000 ) ) ;
#17745 = CARTESIAN_POINT ( 'NONE',  ( 4.458734125000001214, 2.104166668032262599, 2.574251347313718519 ) ) ;
#17746 = CARTESIAN_POINT ( 'NONE',  ( -5.000000000000000000, -43.08333333333333570, -2.886751345948128211 ) ) ;
#17747 = CARTESIAN_POINT ( 'NONE',  ( 4.458734124999999437, -156.3750000013655779, -1.846868145590734978 ) ) ;
#17748 = CARTESIAN_POINT ( 'NONE',  ( -3.152548672688508926E-16, 26.18750000136560274, -5.148502694627439702 ) ) ;
#17749 = ORIENTED_EDGE ( 'NONE', *, *, #58946, .T. ) ;
#17750 = CARTESIAN_POINT ( 'NONE',  ( 4.458734124999998549, -88.72916666530106511, -2.574251347313721627 ) ) ;
#17751 = DIRECTION ( 'NONE',  ( 1.000000000000000000, 0.000000000000000000, 0.000000000000000000 ) ) ;
#17752 = CARTESIAN_POINT ( 'NONE',  ( -2.229367062499996610, -11.14583333196773829, 3.861377020970582219 ) ) ;
#17753 = CYLINDRICAL_SURFACE ( 'NONE', #15980, 5.000000000000000000 ) ;
#17754 = CARTESIAN_POINT ( 'NONE',  ( 1.339745962155615144, -23.58034179853029144, 4.999999999999999112 ) ) ;
#17755 = CARTESIAN_POINT ( 'NONE',  ( -50.01589407740564042, -138.6250000000000284, 0.3983568153799778022 ) ) ;
#17756 = CARTESIAN_POINT ( 'NONE',  ( -4.999999999999999112, -36.79166666393548013, 2.886751345948131764 ) ) ;
#17757 = DIRECTION ( 'NONE',  ( 0.000000000000000000, 0.000000000000000000, 1.000000000000000000 ) ) ;
#17758 = CARTESIAN_POINT ( 'NONE',  ( 4.458734124999998549, 23.27083333469892423, -2.574251347313721627 ) ) ;
#17759 = CARTESIAN_POINT ( 'NONE',  ( -3.152548672688508926E-16, 25.43750000136559208, -5.148502694627439702 ) ) ;
#17760 = CARTESIAN_POINT ( 'NONE',  ( -2.229367062499996610, -54.14583333196773651, 3.861377020970582219 ) ) ;
#17761 = CARTESIAN_POINT ( 'NONE',  ( 4.458734125000000326, -4.145833331967739177, 2.574251347313718519 ) ) ;
#17762 = CARTESIAN_POINT ( 'NONE',  ( -5.000000000000001776, 0.000000000000000000, -9.974600000000000577 ) ) ;
#17763 = CARTESIAN_POINT ( 'NONE',  ( 5.000000000000000000, 17.58333333333333215, -2.886751345948129988 ) ) ;
#17764 = CARTESIAN_POINT ( 'NONE',  ( 5.000000000000000000, -140.1250000027312126, 0.000000000000000000 ) ) ;
#17765 = CARTESIAN_POINT ( 'NONE',  ( 5.000000000000000000, -69.41666666666667140, -2.886751345948130876 ) ) ;
#17766 = CARTESIAN_POINT ( 'NONE',  ( -4.458734124999999437, -49.31249999863440792, 0.000000000000000000 ) ) ;
#17767 = CARTESIAN_POINT ( 'NONE',  ( 5.000000000000000000, -82.37499999726881583, -6.123233995736766282E-16 ) ) ;
#17768 = CARTESIAN_POINT ( 'NONE',  ( -57.89159099828107458, -135.9375000013656063, -3.393966926194107447 ) ) ;
#17769 = CARTESIAN_POINT ( 'NONE',  ( 7.897850199329715437, -1.533397866934079312, -7.634054012537967893 ) ) ;
#17770 = CARTESIAN_POINT ( 'NONE',  ( 4.458734124999998549, -85.97916666530107932, -2.574251347313721627 ) ) ;
#17771 = CARTESIAN_POINT ( 'NONE',  ( -3.152801135295367096, -157.3125000013656063, -3.152801135295367541 ) ) ;
#17772 = CARTESIAN_POINT ( 'NONE',  ( -2.500000000000000444, -34.16666666666666430, -4.330127018922193649 ) ) ;
#17773 = CARTESIAN_POINT ( 'NONE',  ( -4.999999999999998224, 24.08333333333333215, 2.886751345948131764 ) ) ;
#17774 = ORIENTED_EDGE ( 'NONE', *, *, #5933, .F. ) ;
#17775 = CARTESIAN_POINT ( 'NONE',  ( 4.458734124999999437, 18.93750000136559564, -5.460374474430324690E-16 ) ) ;
#17776 = VERTEX_POINT ( 'NONE', #21019 ) ;
#17777 = CARTESIAN_POINT ( 'NONE',  ( -4.458734124999999437, -97.39583333196773651, -2.574251347313719407 ) ) ;
#17778 = CARTESIAN_POINT ( 'NONE',  ( 4.458734124999998549, 9.020833334698927786, -2.574251347313721627 ) ) ;
#17779 = CARTESIAN_POINT ( 'NONE',  ( 2.500000000000002220, 17.45833333606451987, 4.330127018922192761 ) ) ;
#17780 = CARTESIAN_POINT ( 'NONE',  ( -2.499999999999996447, -28.70833333060214798, 4.330127018922195425 ) ) ;
#17781 = CARTESIAN_POINT ( 'NONE',  ( -5.000000000000000000, 10.91666666666666607, -2.886751345948128211 ) ) ;
#17782 = CARTESIAN_POINT ( 'NONE',  ( -2.229367062499996610, -54.14583333196773651, 3.861377020970582219 ) ) ;
#17783 = CARTESIAN_POINT ( 'NONE',  ( 1.975475456537005874E-15, -7.750000000000000000, 5.000000000000000000 ) ) ;
#17784 = CARTESIAN_POINT ( 'NONE',  ( 5.000000000000000000, -78.41666666666667140, -2.886751345948129988 ) ) ;
#17785 = CARTESIAN_POINT ( 'NONE',  ( 1.975475456537005874E-15, 20.24999999999999289, 5.000000000000000000 ) ) ;
#17786 = CARTESIAN_POINT ( 'NONE',  ( 2.500000000000002220, 7.458333336064517205, 4.330127018922192761 ) ) ;
#17787 = CARTESIAN_POINT ( 'NONE',  ( 0.000000000000000000, -120.0000000000000000, 5.000000000000000000 ) ) ;
#17788 = CARTESIAN_POINT ( 'NONE',  ( -4.999999999999999112, -41.91666666666667140, 2.886751345948131764 ) ) ;
#17789 = LINE ( 'NONE', #26495, #11980 ) ;
#17791 = CARTESIAN_POINT ( 'NONE',  ( 9.457646018065525792E-16, -18.31249999863440436, 5.148502694627439702 ) ) ;
#17790 = CARTESIAN_POINT ( 'NONE',  ( -2.499999999999996447, 14.16666666666666785, 4.330127018922195425 ) ) ;
#17792 = CARTESIAN_POINT ( 'NONE',  ( 2.500000000000002220, -107.5416666639354730, 4.330127018922192761 ) ) ;
#17793 = CARTESIAN_POINT ( 'NONE',  ( -4.458734124999999437, -65.31249999863440792, 0.000000000000000000 ) ) ;
#17794 = CARTESIAN_POINT ( 'NONE',  ( -3.152801135295367096, -148.3125000013655779, -3.152801135295367541 ) ) ;
#17795 = CARTESIAN_POINT ( 'NONE',  ( 4.458734125000001214, -71.89583333196773651, 2.574251347313718519 ) ) ;
#17796 = CARTESIAN_POINT ( 'NONE',  ( -56.48576386720575471, -142.0000000013656063, -4.591703134518078322 ) ) ;
#17797 = CARTESIAN_POINT ( 'NONE',  ( 2.229367062500001939, -23.22916666530107221, 3.861377020970579999 ) ) ;
#17798 = CARTESIAN_POINT ( 'NONE',  ( -4.999999999999999112, -59.79166666393547303, 2.886751345948131764 ) ) ;
#17800 = ORIENTED_EDGE ( 'NONE', *, *, #1286, .F. ) ;
#17799 = EDGE_CURVE ( 'NONE', #9375, #38618, #62587, .T. ) ;
#17801 = CYLINDRICAL_SURFACE ( 'NONE', #35363, 5.000000000000000000 ) ;
#17802 = ORIENTED_EDGE ( 'NONE', *, *, #40450, .F. ) ;
#17803 = CARTESIAN_POINT ( 'NONE',  ( -2.229367062500000163, -68.72916666530107932, -3.861377020970580443 ) ) ;
#17804 = CARTESIAN_POINT ( 'NONE',  ( -6.972266317189433020E-16, -7.124999997268814056, -5.000000000000000000 ) ) ;
#17805 = DIRECTION ( 'NONE',  ( -0.000000000000000000, 1.000000000000000000, -0.000000000000000000 ) ) ;
#17806 = ORIENTED_EDGE ( 'NONE', *, *, #26651, .F. ) ;
#17807 = CARTESIAN_POINT ( 'NONE',  ( -49.85088928181150436, -126.5625000000000426, -1.666127454062680702 ) ) ;
#17808 = CARTESIAN_POINT ( 'NONE',  ( -75.00000000000002842, 15.00000000000000000, 5.000000000000000000 ) ) ;
#17809 = CARTESIAN_POINT ( 'NONE',  ( 4.458734124999999437, -55.06249999863440081, -5.460374474430324690E-16 ) ) ;
#17810 = ORIENTED_EDGE ( 'NONE', *, *, #57781, .F. ) ;
#17811 =( BOUNDED_CURVE ( )  B_SPLINE_CURVE ( 2, ( #50500, #30220, #41463, #2568, #7396, #17674, #61114, #17038, #46622 ),
 .UNSPECIFIED., .F., .F. ) 
 B_SPLINE_CURVE_WITH_KNOTS ( ( 3, 2, 2, 2, 3 ),
 ( 0.4750000000000004219, 0.4791666666666671293, 0.4833333333333337811, 0.4875000000000004330, 0.4916666666666670849 ),
 .UNSPECIFIED. ) 
 CURVE ( )  GEOMETRIC_REPRESENTATION_ITEM ( )  RATIONAL_B_SPLINE_CURVE ( ( 0.9999999999999918954, 0.9238795325112948431, 1.000000000000000000, 0.9238795325112867385, 1.000000000000000000, 0.9238795325112867385, 1.000000000000000000, 0.9238795325112786339, 1.000000000000008216 ) ) 
 REPRESENTATION_ITEM ( '' )  );
#17812 = CARTESIAN_POINT ( 'NONE',  ( -2.499999999999996447, 2.291666669397850686, 4.330127018922195425 ) ) ;
#17813 = CARTESIAN_POINT ( 'NONE',  ( -4.458734124999999437, 10.68750000136559386, 0.000000000000000000 ) ) ;
#17814 = ADVANCED_FACE ( 'NONE', ( #11037 ), #20381, .T. ) ;
#17815 = CARTESIAN_POINT ( 'NONE',  ( 4.458734125000001214, 20.10416666803225993, 2.574251347313718519 ) ) ;
#17816 = CARTESIAN_POINT ( 'NONE',  ( -55.35523342533222291, -150.3125000013656063, 4.444560631937231499 ) ) ;
#17817 = CARTESIAN_POINT ( 'NONE',  ( 1.975475456537005874E-15, -78.62499999726881583, 5.000000000000000000 ) ) ;
#17818 = FACE_OUTER_BOUND ( 'NONE', #34033, .T. ) ;
#17820 = EDGE_CURVE ( 'NONE', #34481, #14927, #35179, .T. ) ;
#17819 = ORIENTED_EDGE ( 'NONE', *, *, #21284, .T. ) ;
#17821 = CARTESIAN_POINT ( 'NONE',  ( 4.458734124999999437, -68.81249999863439371, -5.460374474430324690E-16 ) ) ;
#17822 = CARTESIAN_POINT ( 'NONE',  ( 6.123233995736766282E-16, -170.0000000000000000, -5.000000000000000000 ) ) ;
#17823 = CARTESIAN_POINT ( 'NONE',  ( 4.458734125000001214, 6.104166668032262599, 2.574251347313718519 ) ) ;
#17824 = EDGE_CURVE ( 'NONE', #37366, #11915, #47362, .T. ) ;
#17825 = CARTESIAN_POINT ( 'NONE',  ( 1.339745962155615144, -69.58034179853028434, 4.999999999999999112 ) ) ;
#17826 = CARTESIAN_POINT ( 'NONE',  ( -3.152548672688508926E-16, -61.81249999863440081, -5.148502694627439702 ) ) ;
#17827 = CARTESIAN_POINT ( 'NONE',  ( 5.000000000000000888, -21.45833333060215153, 2.886751345948126879 ) ) ;
#17828 = CARTESIAN_POINT ( 'NONE',  ( -6.972266317189433020E-16, 4.749999999999999112, -5.000000000000000000 ) ) ;
#17829 = CARTESIAN_POINT ( 'NONE',  ( 4.336808689942017736E-16, 8.660254037844390851, -1.000000000000000888 ) ) ;
#17830 = CARTESIAN_POINT ( 'NONE',  ( -6.972266317189433020E-16, -76.24999999999998579, -5.000000000000000000 ) ) ;
#17831 = CARTESIAN_POINT ( 'NONE',  ( 6.123233995736766282E-16, -120.0000000000000000, -5.000000000000000000 ) ) ;
#17832 = CARTESIAN_POINT ( 'NONE',  ( 9.457646018065525792E-16, -43.06249999863440081, 5.148502694627439702 ) ) ;
#17833 = CARTESIAN_POINT ( 'NONE',  ( -4.458734124999999437, -19.56249999863440081, 0.000000000000000000 ) ) ;
#17834 = ORIENTED_EDGE ( 'NONE', *, *, #48322, .F. ) ;
#17835 = CARTESIAN_POINT ( 'NONE',  ( -2.500000000000000444, -5.041666663935480130, -4.330127018922193649 ) ) ;
#17836 = CARTESIAN_POINT ( 'NONE',  ( -2.229367062499996610, -108.1458333319677365, 3.861377020970582219 ) ) ;
#17837 = CARTESIAN_POINT ( 'NONE',  ( 3.061616997868383141E-16, -152.8750000027311842, -5.000000000000000000 ) ) ;
#17838 = VERTEX_POINT ( 'NONE', #35814 ) ;
#17839 = CARTESIAN_POINT ( 'NONE',  ( -4.458734124999998549, -109.4791666653010651, 2.574251347313722516 ) ) ;
#17840 = CARTESIAN_POINT ( 'NONE',  ( -4.458734124999998549, -34.22916666530107221, 2.574251347313722516 ) ) ;
#17841 = CARTESIAN_POINT ( 'NONE',  ( 1.060575238724906964E-15, -66.62499999726881583, 5.773502691896257311 ) ) ;
#17842 = CARTESIAN_POINT ( 'NONE',  ( -50.70258187064364108, -147.3750000013656063, 2.196230717870141014 ) ) ;
#17843 = CARTESIAN_POINT ( 'NONE',  ( 3.061616997868383141E-16, -146.7500000000000284, -5.000000000000000000 ) ) ;
#17844 = CARTESIAN_POINT ( 'NONE',  ( 2.229367062500001939, -27.97916666530107221, 3.861377020970579999 ) ) ;
#17845 = CARTESIAN_POINT ( 'NONE',  ( -4.458734124999999437, -70.64583333196773651, -2.574251347313719407 ) ) ;
#17846 = CARTESIAN_POINT ( 'NONE',  ( -4.458734124999999437, -169.2500000013655779, -1.846868145590735644 ) ) ;
#17847 = CARTESIAN_POINT ( 'NONE',  ( -4.458734124999999437, -26.39583333196774007, -2.574251347313719407 ) ) ;
#17848 = CARTESIAN_POINT ( 'NONE',  ( -2.500000000000000444, -33.16666666666666430, -4.330127018922193649 ) ) ;
#17849 = CYLINDRICAL_SURFACE ( 'NONE', #25621, 5.000000000000000000 ) ;
#17850 = CARTESIAN_POINT ( 'NONE',  ( 5.000000000000000888, -14.58333333333333037, 2.886751345948126879 ) ) ;
#17851 = CARTESIAN_POINT ( 'NONE',  ( 4.458734124999999437, -149.4375000013656063, 0.000000000000000000 ) ) ;
#17852 = ORIENTED_EDGE ( 'NONE', *, *, #18155, .T. ) ;
#17853 = CARTESIAN_POINT ( 'NONE',  ( 6.123233995736766282E-16, -120.0000000000000000, -5.000000000000000000 ) ) ;
#17854 = CARTESIAN_POINT ( 'NONE',  ( -3.152548672688508926E-16, -49.81249999863440081, -5.148502694627439702 ) ) ;
#17855 = CARTESIAN_POINT ( 'NONE',  ( 5.000000000000000000, -84.29166666393547303, -2.886751345948130876 ) ) ;
#17856 = CARTESIAN_POINT ( 'NONE',  ( 6.123233995736766282E-16, -170.0000000000000000, -5.000000000000000000 ) ) ;
#17857 = CARTESIAN_POINT ( 'NONE',  ( -4.999999999999999112, 24.08333333333333215, 2.886751345948131764 ) ) ;
#17858 = CARTESIAN_POINT ( 'NONE',  ( 0.000000000000000000, -114.9999999999999858, 0.000000000000000000 ) ) ;
#17859 = CARTESIAN_POINT ( 'NONE',  ( 4.458734124999999437, -0.8124999986344055847, -5.460374474430324690E-16 ) ) ;
#17860 = CARTESIAN_POINT ( 'NONE',  ( 2.500000000000002220, 19.33333333333333570, 4.330127018922192761 ) ) ;
#17861 = CARTESIAN_POINT ( 'NONE',  ( -6.972266317189433020E-16, -14.24999999999999822, -5.000000000000000000 ) ) ;
#17862 = CARTESIAN_POINT ( 'NONE',  ( -1.339745962155613812, -74.20534180126145429, -5.000000000000000000 ) ) ;
#17863 = CARTESIAN_POINT ( 'NONE',  ( 2.229367062499998831, 9.104166668032261711, -3.861377020970580887 ) ) ;
#17864 = ORIENTED_EDGE ( 'NONE', *, *, #26805, .T. ) ;
#17865 = DIRECTION ( 'NONE',  ( 1.387778780781445676E-15, 0.000000000000000000, -1.000000000000000000 ) ) ;
#17866 = ORIENTED_EDGE ( 'NONE', *, *, #23328, .T. ) ;
#17867 = CARTESIAN_POINT ( 'NONE',  ( -2.500000000000000444, -24.04166666393548368, -4.330127018922193649 ) ) ;
#17868 = CARTESIAN_POINT ( 'NONE',  ( -4.458734124999999437, -49.31249999863440792, 0.000000000000000000 ) ) ;
#17869 = CARTESIAN_POINT ( 'NONE',  ( 1.846868145590736310, -159.8750000013655779, 4.458734124999999437 ) ) ;
#17870 = AXIS2_PLACEMENT_3D ( 'NONE', #20523, #63631, #15048 ) ;
#17871 = ADVANCED_FACE ( 'NONE', ( #5910 ), #57696, .F. ) ;
#17872 = CARTESIAN_POINT ( 'NONE',  ( 1.060575238724906964E-15, -44.62499999726881583, 5.773502691896257311 ) ) ;
#17873 = ORIENTED_EDGE ( 'NONE', *, *, #60583, .T. ) ;
#17874 = CARTESIAN_POINT ( 'NONE',  ( 4.458734125000001214, -25.89583333196774007, 2.574251347313718519 ) ) ;
#17875 = VERTEX_POINT ( 'NONE', #38872 ) ;
#17876 = DIRECTION ( 'NONE',  ( 7.709882115452476194E-16, 0.000000000000000000, -1.000000000000000000 ) ) ;
#17877 = CARTESIAN_POINT ( 'NONE',  ( -1.846868145590734756, -165.1250000013656063, -4.458734125000000326 ) ) ;
#17878 =( BOUNDED_CURVE ( )  B_SPLINE_CURVE ( 2, ( #16346, #41406, #12464, #35968, #41718, #12776, #26951, #61685, #16658 ),
 .UNSPECIFIED., .F., .F. ) 
 B_SPLINE_CURVE_WITH_KNOTS ( ( 3, 2, 2, 2, 3 ),
 ( 0.5604166666666666741, 0.5611111111111111160, 0.5625000000000000000, 0.5638888888888888840, 0.5645833333333333259 ),
 .UNSPECIFIED. ) 
 CURVE ( )  GEOMETRIC_REPRESENTATION_ITEM ( )  RATIONAL_B_SPLINE_CURVE ( ( 0.9330127018922194093, 0.9330127018922194093, 1.000000000000000000, 0.8660254037844387076, 1.000000000000000000, 0.8660254037844387076, 1.000000000000000000, 0.9330127018922194093, 0.9330127018922194093 ) ) 
 REPRESENTATION_ITEM ( '' )  );
#17879 = CARTESIAN_POINT ( 'NONE',  ( 2.499999999999998668, -39.20833333060214443, -4.330127018922193649 ) ) ;
#17880 = CARTESIAN_POINT ( 'NONE',  ( -60.14911071818854538, -138.0625000000000000, 1.666127454062681368 ) ) ;
#17881 = CARTESIAN_POINT ( 'NONE',  ( 9.457646018065525792E-16, -39.31249999863439371, 5.148502694627439702 ) ) ;
#17882 = DIRECTION ( 'NONE',  ( -0.000000000000000000, 1.000000000000000000, -0.000000000000000000 ) ) ;
#17883 = ORIENTED_EDGE ( 'NONE', *, *, #19663, .F. ) ;
#17884 = CARTESIAN_POINT ( 'NONE',  ( -4.458734124999999437, -84.39583333196773651, -2.574251347313719407 ) ) ;
#17885 = CARTESIAN_POINT ( 'NONE',  ( 4.458734124999999437, 25.18750000136559208, -5.460374474430324690E-16 ) ) ;
#17886 = CARTESIAN_POINT ( 'NONE',  ( 2.500000000000002220, -12.54166666393548013, 4.330127018922192761 ) ) ;
#17887 = VERTEX_POINT ( 'NONE', #52741 ) ;
#17888 = CARTESIAN_POINT ( 'NONE',  ( 1.339745962155612702, 14.70534180126147916, -5.000000000000000000 ) ) ;
#17889 = CARTESIAN_POINT ( 'NONE',  ( -53.51423613279429503, -139.5000000013656063, 4.591703134518083651 ) ) ;
#17890 = CARTESIAN_POINT ( 'NONE',  ( 4.458734125000001214, -87.14583333196772230, 2.574251347313718519 ) ) ;
#17891 = CARTESIAN_POINT ( 'NONE',  ( -57.46284108482265651, -131.0625000027312410, 4.819101127000239515 ) ) ;
#17892 = CARTESIAN_POINT ( 'NONE',  ( 5.000000000000000000, -143.0625000000000000, 2.071067811865478614 ) ) ;
#17893 = DIRECTION ( 'NONE',  ( 0.000000000000000000, 0.000000000000000000, 1.000000000000000000 ) ) ;
#17894 = CARTESIAN_POINT ( 'NONE',  ( 4.458734125000000326, -52.89583333196772941, 2.574251347313718519 ) ) ;
#17895 = CARTESIAN_POINT ( 'NONE',  ( -4.458734124999999437, 20.68750000136559208, 0.000000000000000000 ) ) ;
#17896 = CARTESIAN_POINT ( 'NONE',  ( 2.499999999999998668, -106.3333333333333286, -4.330127018922193649 ) ) ;
#17897 = LINE ( 'NONE', #22104, #48417 ) ;
#17898 = CARTESIAN_POINT ( 'NONE',  ( 9.457646018065525792E-16, -42.31249999863440081, 5.148502694627439702 ) ) ;
#17899 = CARTESIAN_POINT ( 'NONE',  ( -3.535250795749689387E-16, -4.124999997268816720, -5.773502691896257311 ) ) ;
#17900 = CARTESIAN_POINT ( 'NONE',  ( -60.14911071818854538, -154.0625000000000000, 1.666127454062681146 ) ) ;
#17901 = CARTESIAN_POINT ( 'NONE',  ( -6.972266317189433020E-16, -70.12499999726880162, -5.000000000000000000 ) ) ;
#17902 = CARTESIAN_POINT ( 'NONE',  ( -4.458734124999999437, -86.56249999863439371, 0.000000000000000000 ) ) ;
#17903 = CARTESIAN_POINT ( 'NONE',  ( -3.152548672688508926E-16, -101.5624999986343937, -5.148502694627439702 ) ) ;
#17904 =( BOUNDED_CURVE ( )  B_SPLINE_CURVE ( 2, ( #18869, #17628, #48145, #3157, #4097, #23720, #2840, #38486, #58113 ),
 .UNSPECIFIED., .F., .F. ) 
 B_SPLINE_CURVE_WITH_KNOTS ( ( 3, 2, 2, 2, 3 ),
 ( 0.5416666666666671848, 0.5458333333333338366, 0.5500000000000004885, 0.5541666666666671404, 0.5583333333333337922 ),
 .UNSPECIFIED. ) 
 CURVE ( )  GEOMETRIC_REPRESENTATION_ITEM ( )  RATIONAL_B_SPLINE_CURVE ( ( 0.9999999999999898970, 0.9238795325112968415, 1.000000000000000000, 0.9238795325112867385, 1.000000000000000000, 0.9238795325112867385, 1.000000000000000000, 0.9238795325112786339, 1.000000000000008216 ) ) 
 REPRESENTATION_ITEM ( '' )  );
#17905 = CARTESIAN_POINT ( 'NONE',  ( -2.229367062499996610, -5.395833331967740953, 3.861377020970582219 ) ) ;
#17906 = ORIENTED_EDGE ( 'NONE', *, *, #29564, .F. ) ;
#17907 = FACE_OUTER_BOUND ( 'NONE', #33974, .T. ) ;
#17908 = CARTESIAN_POINT ( 'NONE',  ( 9.457646018065525792E-16, -92.06249999863439371, 5.148502694627439702 ) ) ;
#17909 = CARTESIAN_POINT ( 'NONE',  ( 5.000000000000000000, -167.1250000027312126, 0.000000000000000000 ) ) ;
#17910 = CARTESIAN_POINT ( 'NONE',  ( -4.458734124999999437, -90.64583333196773651, -2.574251347313719407 ) ) ;
#17911 = CARTESIAN_POINT ( 'NONE',  ( -3.152548672688508926E-16, 11.18750000136559386, -5.148502694627439702 ) ) ;
#17912 = CARTESIAN_POINT ( 'NONE',  ( -1.339745962155610925, -15.79465819873852261, 5.000000000000000000 ) ) ;
#17913 = AXIS2_PLACEMENT_3D ( 'NONE', #44428, #388, #28996 ) ;
#17914 = CARTESIAN_POINT ( 'NONE',  ( -50.55543936806279248, -132.0625000013656063, 0.3552334253322060320 ) ) ;
#17915 = CARTESIAN_POINT ( 'NONE',  ( -4.458734124999999437, -10.39583333196773474, -2.574251347313719407 ) ) ;
#17916 = CARTESIAN_POINT ( 'NONE',  ( -4.458734124999999437, 14.35416666803226171, -2.574251347313719407 ) ) ;
#17917 = CARTESIAN_POINT ( 'NONE',  ( -3.152548672688508926E-16, -55.81249999863440081, -5.148502694627439702 ) ) ;
#17918 = DIRECTION ( 'NONE',  ( 0.000000000000000000, 0.000000000000000000, 1.000000000000000000 ) ) ;
#17919 = CARTESIAN_POINT ( 'NONE',  ( -6.972266317189433020E-16, 13.87500000273118594, -5.000000000000000000 ) ) ;
#17920 = CARTESIAN_POINT ( 'NONE',  ( -3.152548672688508926E-16, -9.562499998634409692, -5.148502694627439702 ) ) ;
#17921 = ORIENTED_EDGE ( 'NONE', *, *, #56601, .F. ) ;
#17922 = CARTESIAN_POINT ( 'NONE',  ( 4.458734125000000326, -33.14583333196774362, 2.574251347313718519 ) ) ;
#17923 = CARTESIAN_POINT ( 'NONE',  ( -55.35523342533222291, -127.5625000013655921, 4.444560631937231499 ) ) ;
#17924 = CARTESIAN_POINT ( 'NONE',  ( 1.339745962155615144, -68.70534180126148271, 4.999999999999999112 ) ) ;
#17925 = CARTESIAN_POINT ( 'NONE',  ( -4.458734124999998549, -80.22916666530106511, 2.574251347313722516 ) ) ;
#17926 = CARTESIAN_POINT ( 'NONE',  ( 4.458734124999999437, 21.93750000136559208, -5.460374474430324690E-16 ) ) ;
#17927 = CARTESIAN_POINT ( 'NONE',  ( -2.229367062500000163, 13.52083333469892779, -3.861377020970580443 ) ) ;
#17928 = CARTESIAN_POINT ( 'NONE',  ( 5.000000000000000000, -55.41666666666667140, -2.886751345948130876 ) ) ;
#17929 = CARTESIAN_POINT ( 'NONE',  ( 2.229367062500001939, -82.22916666530106511, 3.861377020970579999 ) ) ;
#17930 = CARTESIAN_POINT ( 'NONE',  ( 2.500000000000002220, -67.66666666666667140, 4.330127018922192761 ) ) ;
#17931 = CYLINDRICAL_SURFACE ( 'NONE', #26450, 5.000000000000000000 ) ;
#17932 = CARTESIAN_POINT ( 'NONE',  ( 5.000000000000000000, 19.62500000273118772, -6.123233995736766282E-16 ) ) ;
#17933 = ORIENTED_EDGE ( 'NONE', *, *, #5989, .F. ) ;
#17934 = CARTESIAN_POINT ( 'NONE',  ( 3.535533905932738197, -147.0000000027311842, -3.535533905932738197 ) ) ;
#17935 = CARTESIAN_POINT ( 'NONE',  ( -2.499999999999996447, -79.70833333060213022, 4.330127018922195425 ) ) ;
#17937 = CARTESIAN_POINT ( 'NONE',  ( 5.000000000000000000, -28.41666666666666430, -2.886751345948129988 ) ) ;
#17936 = DIRECTION ( 'NONE',  ( 1.000000000000000000, 0.000000000000000000, 0.000000000000000000 ) ) ;
#17938 = CARTESIAN_POINT ( 'NONE',  ( -2.229367062500000163, -33.47916666530107221, -3.861377020970580443 ) ) ;
#17939 = CARTESIAN_POINT ( 'NONE',  ( 1.975475456537005874E-15, -1.749999999999999334, 5.000000000000000000 ) ) ;
#17940 = CARTESIAN_POINT ( 'NONE',  ( -2.500000000000000444, -29.04166666393548013, -4.330127018922193649 ) ) ;
#17942 = ORIENTED_EDGE ( 'NONE', *, *, #36617, .F. ) ;
#17941 = CARTESIAN_POINT ( 'NONE',  ( -4.458734124999998549, -58.22916666530105800, 2.574251347313722516 ) ) ;
#17943 = CARTESIAN_POINT ( 'NONE',  ( -57.19623071787017210, -154.6250000013656063, 4.297418129356382899 ) ) ;
#17945 = ORIENTED_EDGE ( 'NONE', *, *, #58229, .F. ) ;
#17944 = CARTESIAN_POINT ( 'NONE',  ( -4.458734124999999437, -10.64583333196773829, -2.574251347313719407 ) ) ;
#17946 = CARTESIAN_POINT ( 'NONE',  ( 1.060575238724906964E-15, -74.75000000000000000, 5.773502691896257311 ) ) ;
#17947 = CARTESIAN_POINT ( 'NONE',  ( -58.39396692619412477, -140.4375000013656063, 2.891590998281057701 ) ) ;
#17948 = EDGE_CURVE ( 'NONE', #56025, #15620, #57582, .T. ) ;
#17949 = CARTESIAN_POINT ( 'NONE',  ( -3.152548672688508926E-16, -50.81249999863440792, -5.148502694627439702 ) ) ;
#17950 = CARTESIAN_POINT ( 'NONE',  ( -3.535250795749689387E-16, -77.12499999726880162, -5.773502691896257311 ) ) ;
#17952 = ORIENTED_EDGE ( 'NONE', *, *, #62555, .F. ) ;
#17951 = CARTESIAN_POINT ( 'NONE',  ( -9.184850993605147944E-16, -145.3750000027312126, 5.000000000000000000 ) ) ;
#17953 = CARTESIAN_POINT ( 'NONE',  ( -52.53715891517739323, -148.4375000000000284, -4.819101127000233298 ) ) ;
#17954 = CARTESIAN_POINT ( 'NONE',  ( -4.458734124999999437, -20.64583333196774007, -2.574251347313719407 ) ) ;
#17956 = ORIENTED_EDGE ( 'NONE', *, *, #25193, .T. ) ;
#17955 = CARTESIAN_POINT ( 'NONE',  ( -3.152548672688508926E-16, -55.81249999863440081, -5.148502694627439702 ) ) ;
#17957 = AXIS2_PLACEMENT_3D ( 'NONE', #13757, #8003, #33379 ) ;
#17958 = CARTESIAN_POINT ( 'NONE',  ( 4.458734124999999437, -142.4375000013656063, 0.000000000000000000 ) ) ;
#17959 = CARTESIAN_POINT ( 'NONE',  ( 9.457646018065525792E-16, -100.3124999986344079, 5.148502694627439702 ) ) ;
#17960 = CARTESIAN_POINT ( 'NONE',  ( -9.184850993605147944E-16, -148.3750000027312126, 5.000000000000000000 ) ) ;
#17961 = EDGE_LOOP ( 'NONE', ( #20617, #34728, #5998, #54733 ) ) ;
#17962 = CARTESIAN_POINT ( 'NONE',  ( -54.64476657466781973, -151.0625000013656063, -4.444560631937228834 ) ) ;
#17963 = CARTESIAN_POINT ( 'NONE',  ( -50.01589407740564042, -141.7500000027312126, 0.3983568153799778022 ) ) ;
#17964 = CARTESIAN_POINT ( 'NONE',  ( -2.229367062500000163, -5.479166665301072214, -3.861377020970580443 ) ) ;
#17965 = CARTESIAN_POINT ( 'NONE',  ( 4.458734124999999437, -96.06249999863440792, -5.460374474430324690E-16 ) ) ;
#17966 = CARTESIAN_POINT ( 'NONE',  ( -4.458734124999999437, -149.1875000013656063, -5.460374474430324690E-16 ) ) ;
#17967 = CARTESIAN_POINT ( 'NONE',  ( -2.229367062499996610, -28.39583333196774007, 3.861377020970582219 ) ) ;
#17968 = CARTESIAN_POINT ( 'NONE',  ( -5.000000000000000000, -67.00000000000000000, 0.000000000000000000 ) ) ;
#17969 = CARTESIAN_POINT ( 'NONE',  ( -59.59170313451811296, -135.5000000013656063, 1.485763867205729394 ) ) ;
#17970 = CARTESIAN_POINT ( 'NONE',  ( 4.458734124999998549, -63.97916666530107221, -2.574251347313721627 ) ) ;
#17971 = CARTESIAN_POINT ( 'NONE',  ( 1.975475456537005874E-15, -90.74999999999998579, 5.000000000000000000 ) ) ;
#17972 = CARTESIAN_POINT ( 'NONE',  ( 1.339745962155615144, -88.58034179853028434, 4.999999999999999112 ) ) ;
#17973 = CARTESIAN_POINT ( 'NONE',  ( -4.458734124999999437, -142.0000000013655495, -1.846868145590735644 ) ) ;
#17974 = CARTESIAN_POINT ( 'NONE',  ( -4.458734124999999437, 9.437500001365593860, 0.000000000000000000 ) ) ;
#17975 = VERTEX_POINT ( 'NONE', #61215 ) ;
#17976 = CARTESIAN_POINT ( 'NONE',  ( 1.975475456537005874E-15, -82.62499999726878741, 5.000000000000000000 ) ) ;
#17977 = DIRECTION ( 'NONE',  ( 0.000000000000000000, 0.000000000000000000, 1.000000000000000000 ) ) ;
#17979 = CARTESIAN_POINT ( 'NONE',  ( 4.458734124999998549, -24.72916666530106866, -2.574251347313721627 ) ) ;
#17978 = CARTESIAN_POINT ( 'NONE',  ( -4.999999999999999112, -88.91666666666667140, 2.886751345948131764 ) ) ;
#17980 = DIRECTION ( 'NONE',  ( 0.000000000000000000, 0.000000000000000000, 1.000000000000000000 ) ) ;
#17981 = CARTESIAN_POINT ( 'NONE',  ( 4.458734124999998549, -71.97916666530107932, -2.574251347313721627 ) ) ;
#17982 = FACE_OUTER_BOUND ( 'NONE', #40241, .T. ) ;
#17983 = CARTESIAN_POINT ( 'NONE',  ( 5.000000000000000888, -76.45833333060215864, 2.886751345948126879 ) ) ;
#17984 =( BOUNDED_CURVE ( )  B_SPLINE_CURVE ( 2, ( #14650, #19799, #34268, #38465, #9820, #53894, #33652, #9513, #14973 ),
 .UNSPECIFIED., .F., .F. ) 
 B_SPLINE_CURVE_WITH_KNOTS ( ( 3, 2, 2, 2, 3 ),
 ( 0.2517857142857142794, 0.2523809523809523725, 0.2535714285714285587, 0.2547619047619047450, 0.2553571428571428381 ),
 .UNSPECIFIED. ) 
 CURVE ( )  GEOMETRIC_REPRESENTATION_ITEM ( )  RATIONAL_B_SPLINE_CURVE ( ( 0.9330127018922194093, 0.9330127018922194093, 1.000000000000000000, 0.8660254037844387076, 1.000000000000000000, 0.8660254037844387076, 1.000000000000000000, 0.9330127018922194093, 0.9330127018922194093 ) ) 
 REPRESENTATION_ITEM ( '' )  );
#17985 = CARTESIAN_POINT ( 'NONE',  ( -59.59170313451811296, -144.5000000013656063, 1.485763867205729394 ) ) ;
#17986 = CARTESIAN_POINT ( 'NONE',  ( 4.458734125000000326, 2.104166668032262599, 2.574251347313718519 ) ) ;
#17987 = CYLINDRICAL_SURFACE ( 'NONE', #20158, 5.000000000000000000 ) ;
#17988 = CARTESIAN_POINT ( 'NONE',  ( 1.975475456537005874E-15, 20.37500000273118417, 5.000000000000000000 ) ) ;
#17989 = CARTESIAN_POINT ( 'NONE',  ( -3.152548672688508926E-16, 9.437500001365593860, -5.148502694627439702 ) ) ;
#17990 = CARTESIAN_POINT ( 'NONE',  ( -2.229367062500000163, -74.47916666530106511, -3.861377020970580443 ) ) ;
#17991 = CARTESIAN_POINT ( 'NONE',  ( 4.458734124999999437, -19.06249999863440792, -5.460374474430324690E-16 ) ) ;
#17992 = CARTESIAN_POINT ( 'NONE',  ( 2.500000000000002220, -7.666666666666668739, 4.330127018922192761 ) ) ;
#17993 = CARTESIAN_POINT ( 'NONE',  ( 1.846868145590736310, -159.6250000013656063, 4.458734124999999437 ) ) ;
#17994 = CARTESIAN_POINT ( 'NONE',  ( 1.975475456537005874E-15, -104.6249999972688016, 5.000000000000000000 ) ) ;
#17995 = CARTESIAN_POINT ( 'NONE',  ( -4.458734124999999437, -63.31249999863440792, 0.000000000000000000 ) ) ;
#17996 = CARTESIAN_POINT ( 'NONE',  ( -5.000000000000000000, -100.9583333306021444, -2.886751345948128211 ) ) ;
#17997 = ADVANCED_FACE ( 'NONE', ( #18002 ), #48532, .T. ) ;
#17998 = CONICAL_SURFACE ( 'NONE', #21086, 4.174999999999999822, 0.9599310885968795892 ) ;
#17999 =( BOUNDED_CURVE ( )  B_SPLINE_CURVE ( 2, ( #59997, #14635, #34249, #54527, #15921, #45504, #25571, #40032, #19465 ),
 .UNSPECIFIED., .F., .F. ) 
 B_SPLINE_CURVE_WITH_KNOTS ( ( 3, 2, 2, 2, 3 ),
 ( 0.1895833333333333259, 0.1902777777777777679, 0.1916666666666666796, 0.1930555555555555636, 0.1937500000000000056 ),
 .UNSPECIFIED. ) 
 CURVE ( )  GEOMETRIC_REPRESENTATION_ITEM ( )  RATIONAL_B_SPLINE_CURVE ( ( 0.9330127018922194093, 0.9330127018922194093, 1.000000000000000000, 0.8660254037844387076, 1.000000000000000000, 0.8660254037844387076, 1.000000000000000000, 0.9330127018922194093, 0.9330127018922194093 ) ) 
 REPRESENTATION_ITEM ( '' )  );
#18000 = CARTESIAN_POINT ( 'NONE',  ( 5.000000000000000888, -41.58333333333333570, 2.886751345948126879 ) ) ;
#18001 = CARTESIAN_POINT ( 'NONE',  ( -3.152548672688508926E-16, -42.56249999863439371, -5.148502694627439702 ) ) ;
#18002 = FACE_OUTER_BOUND ( 'NONE', #25798, .T. ) ;
#18003 = CARTESIAN_POINT ( 'NONE',  ( 4.458734124999998549, -107.9791666653010651, -2.574251347313721627 ) ) ;
#18004 = CARTESIAN_POINT ( 'NONE',  ( -4.458734124999999437, -66.64583333196773651, -2.574251347313719407 ) ) ;
#18005 = CARTESIAN_POINT ( 'NONE',  ( -5.000000000000000000, -49.08333333333332860, -2.886751345948128211 ) ) ;
#18006 = CARTESIAN_POINT ( 'NONE',  ( 5.000000000000000000, -57.37499999726880162, -6.123233995736766282E-16 ) ) ;
#18007 = CARTESIAN_POINT ( 'NONE',  ( 1.975475456537005874E-15, -89.74999999999998579, 5.000000000000000000 ) ) ;
#18008 = ORIENTED_EDGE ( 'NONE', *, *, #59061, .F. ) ;
#18009 = CARTESIAN_POINT ( 'NONE',  ( 4.458734124999999437, -109.8124999986343937, -5.460374474430324690E-16 ) ) ;
#18010 = CARTESIAN_POINT ( 'NONE',  ( -5.000000000000000000, -99.95833333060213022, -2.886751345948128211 ) ) ;
#18011 = CARTESIAN_POINT ( 'NONE',  ( -4.999999999999999112, -11.91666666666666607, 2.886751345948131764 ) ) ;
#18012 = CARTESIAN_POINT ( 'NONE',  ( 2.229367062499998831, -15.64583333196773651, -3.861377020970580887 ) ) ;
#18013 = CARTESIAN_POINT ( 'NONE',  ( -4.458734124999999437, -79.39583333196773651, -2.574251347313719407 ) ) ;
#18014 = CARTESIAN_POINT ( 'NONE',  ( 1.339745962155612702, -59.16965819600732601, -5.000000000000000000 ) ) ;
#18015 = EDGE_CURVE ( 'NONE', #55065, #54054, #5461, .T. ) ;
#18016 = CARTESIAN_POINT ( 'NONE',  ( 5.000000000000000888, -13.45833333060214976, 2.886751345948126879 ) ) ;
#18018 = ORIENTED_EDGE ( 'NONE', *, *, #1126, .T. ) ;
#18017 = CARTESIAN_POINT ( 'NONE',  ( -2.229367062500000163, -45.47916666530106511, -3.861377020970580443 ) ) ;
#18019 = CARTESIAN_POINT ( 'NONE',  ( 1.339745962155615144, -41.70534180126147561, 4.999999999999999112 ) ) ;
#18020 = EDGE_CURVE ( 'NONE', #19960, #49819, #23152, .T. ) ;
#18022 = VERTEX_POINT ( 'NONE', #53676 ) ;
#18021 = CARTESIAN_POINT ( 'NONE',  ( 4.458734124999998549, 8.020833334698926009, -2.574251347313721627 ) ) ;
#18023 = DIRECTION ( 'NONE',  ( 0.000000000000000000, 0.000000000000000000, -1.000000000000000000 ) ) ;
#18024 = CARTESIAN_POINT ( 'NONE',  ( 1.060575238724906964E-15, -61.75000000000000000, 5.773502691896257311 ) ) ;
#18025 = CARTESIAN_POINT ( 'NONE',  ( -4.458734125000000326, -162.2500000013656347, -1.846868145590735644 ) ) ;
#18026 = CARTESIAN_POINT ( 'NONE',  ( -4.458734124999998549, -36.47916666530107221, 2.574251347313722516 ) ) ;
#18027 = CARTESIAN_POINT ( 'NONE',  ( -2.500000000000000444, -87.16666666666667140, -4.330127018922193649 ) ) ;
#18028 = CARTESIAN_POINT ( 'NONE',  ( 2.229367062499998831, -82.64583333196773651, -3.861377020970580887 ) ) ;
#18029 = CARTESIAN_POINT ( 'NONE',  ( 3.535533905932736864, -168.1250000000000284, 3.535533905932738641 ) ) ;
#18030 = DIRECTION ( 'NONE',  ( -0.000000000000000000, 1.000000000000000000, -0.000000000000000000 ) ) ;
#18031 = CARTESIAN_POINT ( 'NONE',  ( -50.55543936806279248, -129.3125000013656063, 0.3552334253322060320 ) ) ;
#18032 = CARTESIAN_POINT ( 'NONE',  ( -4.458734124999998549, -4.479166665301070438, 2.574251347313722516 ) ) ;
#18033 = ADVANCED_FACE ( 'NONE', ( #57266 ), #13184, .T. ) ;
#18034 = CARTESIAN_POINT ( 'NONE',  ( 9.457646018065525792E-16, -42.31249999863440081, 5.148502694627439702 ) ) ;
#18035 = CARTESIAN_POINT ( 'NONE',  ( 5.000000000000000000, -151.1875000027312410, 2.071067811865478614 ) ) ;
#18036 = CARTESIAN_POINT ( 'NONE',  ( 2.229367062500001939, -86.22916666530107932, 3.861377020970579999 ) ) ;
#18037 = CYLINDRICAL_SURFACE ( 'NONE', #12219, 5.000000000000000000 ) ;
#18038 = ORIENTED_EDGE ( 'NONE', *, *, #9096, .F. ) ;
#18039 = CARTESIAN_POINT ( 'NONE',  ( 1.975475456537005874E-15, -47.74999999999999289, 5.000000000000000000 ) ) ;
#18040 = CARTESIAN_POINT ( 'NONE',  ( -2.229367062499996610, -68.39583333196773651, 3.861377020970582219 ) ) ;
#18041 = CARTESIAN_POINT ( 'NONE',  ( 4.458734124999999437, -145.6875000013656063, 0.000000000000000000 ) ) ;
#18042 = ORIENTED_EDGE ( 'NONE', *, *, #44884, .F. ) ;
#18043 = CARTESIAN_POINT ( 'NONE',  ( -5.147856630858197489E-14, 3.375000002731183280, 5.000000000000000000 ) ) ;
#18044 = CARTESIAN_POINT ( 'NONE',  ( 2.500000000000002220, 17.33333333333333215, 4.330127018922192761 ) ) ;
#18045 = EDGE_CURVE ( 'NONE', #29318, #60194, #12034, .T. ) ;
#18046 = CARTESIAN_POINT ( 'NONE',  ( -4.458734124999999437, -12.56249999863440259, 0.000000000000000000 ) ) ;
#18047 = CARTESIAN_POINT ( 'NONE',  ( -4.999999999999998224, 3.083333333333333925, 2.886751345948131764 ) ) ;
#18048 = CARTESIAN_POINT ( 'NONE',  ( 4.458734125000001214, 4.104166668032260823, 2.574251347313718519 ) ) ;
#18049 = CARTESIAN_POINT ( 'NONE',  ( -1.339745962155613812, -80.20534180126148271, -5.000000000000000000 ) ) ;
#18050 = CARTESIAN_POINT ( 'NONE',  ( -4.458734124999999437, -158.9375000013655779, -5.460374474430324690E-16 ) ) ;
#18051 =( BOUNDED_CURVE ( )  B_SPLINE_CURVE ( 2, ( #57248, #62699, #53028, #43371, #56926, #3838, #27640, #28893, #38247 ),
 .UNSPECIFIED., .F., .F. ) 
 B_SPLINE_CURVE_WITH_KNOTS ( ( 3, 2, 2, 2, 3 ),
 ( 0.7553571428571428381, 0.7559523809523809312, 0.7571428571428571175, 0.7583333333333333037, 0.7589285714285713969 ),
 .UNSPECIFIED. ) 
 CURVE ( )  GEOMETRIC_REPRESENTATION_ITEM ( )  RATIONAL_B_SPLINE_CURVE ( ( 0.9330127018922194093, 0.9330127018922194093, 1.000000000000000000, 0.8660254037844387076, 1.000000000000000000, 0.8660254037844387076, 1.000000000000000000, 0.9330127018922194093, 0.9330127018922194093 ) ) 
 REPRESENTATION_ITEM ( '' )  );
#18052 = CARTESIAN_POINT ( 'NONE',  ( -4.458734124999999437, 28.43750000136559208, 0.000000000000000000 ) ) ;
#18053 = EDGE_LOOP ( 'NONE', ( #53778, #46189, #6504, #59767 ) ) ;
#18054 = CARTESIAN_POINT ( 'NONE',  ( 4.458734124999999437, -93.81249999863440792, -5.460374474430324690E-16 ) ) ;
#18055 = CARTESIAN_POINT ( 'NONE',  ( -2.500000000000000444, -68.16666666666667140, -4.330127018922193649 ) ) ;
#18056 = CARTESIAN_POINT ( 'NONE',  ( -2.500000000000000444, -70.04166666393547303, -4.330127018922193649 ) ) ;
#18057 = CARTESIAN_POINT ( 'NONE',  ( 4.458734124999998549, -8.729166665301073991, -2.574251347313721627 ) ) ;
#18058 = LINE ( 'NONE', #47026, #10834 ) ;
#18059 = CARTESIAN_POINT ( 'NONE',  ( -9.184850993605147944E-16, -166.3750000027312126, 5.000000000000000000 ) ) ;
#18060 = CARTESIAN_POINT ( 'NONE',  ( -4.999999999999998224, 15.08333333333333215, 2.886751345948131764 ) ) ;
#18061 = CARTESIAN_POINT ( 'NONE',  ( -5.000000000000000000, -35.87499999726881583, 0.000000000000000000 ) ) ;
#18062 = FACE_OUTER_BOUND ( 'NONE', #47597, .T. ) ;
#18063 = CARTESIAN_POINT ( 'NONE',  ( -4.458734124999999437, 18.68750000136559564, 0.000000000000000000 ) ) ;
#18064 = CARTESIAN_POINT ( 'NONE',  ( -1.339745962155613812, -4.205341801261476498, -5.000000000000000000 ) ) ;
#18065 = CARTESIAN_POINT ( 'NONE',  ( 9.457646018065525792E-16, 21.93750000136559208, 5.148502694627439702 ) ) ;
#18066 = CARTESIAN_POINT ( 'NONE',  ( -3.152548672688508926E-16, -56.56249999863439371, -5.148502694627439702 ) ) ;
#18067 = CARTESIAN_POINT ( 'NONE',  ( 4.458734125000000326, -6.145833331967740953, 2.574251347313718519 ) ) ;
#18068 = CARTESIAN_POINT ( 'NONE',  ( 5.000000000000000888, 0.000000000000000000, -25.03750572909317285 ) ) ;
#18069 = CARTESIAN_POINT ( 'NONE',  ( 5.000000000000000000, 11.58333333333333570, -2.886751345948129988 ) ) ;
#18070 = CARTESIAN_POINT ( 'NONE',  ( 2.071067811865475505, -139.9375000027311842, -5.000000000000000888 ) ) ;
#18072 = AXIS2_PLACEMENT_3D ( 'NONE', #37069, #50901, #6843 ) ;
#18071 = DIRECTION ( 'NONE',  ( -0.000000000000000000, 1.000000000000000000, -0.000000000000000000 ) ) ;
#18073 = CARTESIAN_POINT ( 'NONE',  ( 4.458734124999999437, -48.81249999863440792, -5.460374474430324690E-16 ) ) ;
#18074 = CARTESIAN_POINT ( 'NONE',  ( -4.999999999999999112, -85.79166666393547303, 2.886751345948131764 ) ) ;
#18075 = EDGE_CURVE ( 'NONE', #55067, #60295, #586, .T. ) ;
#18076 = CARTESIAN_POINT ( 'NONE',  ( -50.40829686548195099, -137.2500000013656063, -1.485763867205728284 ) ) ;
#18077 = CARTESIAN_POINT ( 'NONE',  ( -1.339745962155613812, -87.20534180126148271, -5.000000000000000000 ) ) ;
#18078 = CARTESIAN_POINT ( 'NONE',  ( 1.339745962155557191, -36.70534180126148271, 5.000000000000032863 ) ) ;
#18079 = EDGE_CURVE ( 'NONE', #2056, #55022, #38262, .T. ) ;
#18080 = CARTESIAN_POINT ( 'NONE',  ( -4.458734124999997661, -89.47916666530105090, 2.574251347313722516 ) ) ;
#18081 = CARTESIAN_POINT ( 'NONE',  ( -4.458734124999999437, -156.2500000013656063, -1.846868145590735644 ) ) ;
#18082 = CARTESIAN_POINT ( 'NONE',  ( 5.000000000000000888, -30.58333333333332860, 2.886751345948126879 ) ) ;
#18083 = FILL_AREA_STYLE ('',( #47048 ) ) ;
#18084 = EDGE_LOOP ( 'NONE', ( #47365, #28050, #24174, #19116 ) ) ;
#18085 = CARTESIAN_POINT ( 'NONE',  ( -4.458734124999999437, 17.43750000136559208, 0.000000000000000000 ) ) ;
#18086 = VERTEX_POINT ( 'NONE', #33742 ) ;
#18087 = CARTESIAN_POINT ( 'NONE',  ( 2.229367062499998831, -98.64583333196773651, -3.861377020970580887 ) ) ;
#18088 = CARTESIAN_POINT ( 'NONE',  ( 4.458734124999998549, 10.02083333469892779, -2.574251347313721627 ) ) ;
#18089 = CARTESIAN_POINT ( 'NONE',  ( -5.000000000000000000, 10.12500000273118594, 0.000000000000000000 ) ) ;
#18090 = CARTESIAN_POINT ( 'NONE',  ( 5.000000000000000888, -16.58333333333333215, 2.886751345948126879 ) ) ;
#18091 = CARTESIAN_POINT ( 'NONE',  ( -5.000000000000000000, 4.916666666666666075, -2.886751345948128211 ) ) ;
#18092 = AXIS2_PLACEMENT_3D ( 'NONE', #8300, #47523, #41739 ) ;
#18093 = CARTESIAN_POINT ( 'NONE',  ( 9.457646018065525792E-16, -61.06249999863440081, 5.148502694627439702 ) ) ;
#18094 = CARTESIAN_POINT ( 'NONE',  ( -6.972266317189433020E-16, -40.24999999999999289, -5.000000000000000000 ) ) ;
#18095 = CARTESIAN_POINT ( 'NONE',  ( -3.535250795749689387E-16, -81.25000000000001421, -5.773502691896257311 ) ) ;
#18096 = CARTESIAN_POINT ( 'NONE',  ( -4.458734124999999437, -31.31249999863440436, 0.000000000000000000 ) ) ;
#18097 = CARTESIAN_POINT ( 'NONE',  ( 0.000000000000000000, -120.0000000000000000, 0.000000000000000000 ) ) ;
#18098 = DIRECTION ( 'NONE',  ( -0.000000000000000000, 1.000000000000000000, -0.000000000000000000 ) ) ;
#18099 = ADVANCED_FACE ( 'NONE', ( #53047 ), #28597, .T. ) ;
#18100 = CARTESIAN_POINT ( 'NONE',  ( 1.339745962155615144, -109.7053418012614685, 4.999999999999999112 ) ) ;
#18101 = CARTESIAN_POINT ( 'NONE',  ( 2.499999999999998668, -39.33333333333332860, -4.330127018922193649 ) ) ;
#18102 = CARTESIAN_POINT ( 'NONE',  ( 1.339745962155612702, -70.16965819600731891, -5.000000000000000000 ) ) ;
#18104 = CARTESIAN_POINT ( 'NONE',  ( 4.458734125000001214, -19.14583333196774007, 2.574251347313718519 ) ) ;
#18103 = CARTESIAN_POINT ( 'NONE',  ( 5.000000000000000888, 6.541666669397851130, 2.886751345948126879 ) ) ;
#18105 = CARTESIAN_POINT ( 'NONE',  ( -5.000000000000000000, -57.99999999999999289, 0.000000000000000000 ) ) ;
#18106 = CARTESIAN_POINT ( 'NONE',  ( -2.229367062500000163, -65.47916666530106511, -3.861377020970580443 ) ) ;
#18107 =( BOUNDED_CURVE ( )  B_SPLINE_CURVE ( 2, ( #8420, #51845, #47642, #23202, #31909, #42815, #62457, #18377, #22904 ),
 .UNSPECIFIED., .F., .F. ) 
 B_SPLINE_CURVE_WITH_KNOTS ( ( 3, 2, 2, 2, 3 ),
 ( 0.4339285714285714413, 0.4345238095238095344, 0.4357142857142857206, 0.4369047619047619069, 0.4375000000000000000 ),
 .UNSPECIFIED. ) 
 CURVE ( )  GEOMETRIC_REPRESENTATION_ITEM ( )  RATIONAL_B_SPLINE_CURVE ( ( 0.9330127018922194093, 0.9330127018922194093, 1.000000000000000000, 0.8660254037844387076, 1.000000000000000000, 0.8660254037844387076, 1.000000000000000000, 0.9330127018922194093, 0.9330127018922194093 ) ) 
 REPRESENTATION_ITEM ( '' )  );
#18108 = CARTESIAN_POINT ( 'NONE',  ( 1.846868145590736310, -148.8750000013655495, 4.458734124999999437 ) ) ;
#18109 = CARTESIAN_POINT ( 'NONE',  ( 2.229367062499998831, -77.64583333196773651, -3.861377020970580887 ) ) ;
#18110 = CARTESIAN_POINT ( 'NONE',  ( -50.55543936806279248, -143.3125000013656063, 0.3552334253322060320 ) ) ;
#18111 = CARTESIAN_POINT ( 'NONE',  ( 4.458734125000001214, -26.14583333196774007, 2.574251347313718519 ) ) ;
#18112 = CARTESIAN_POINT ( 'NONE',  ( 2.499999999999998668, -68.20833333060214443, -4.330127018922193649 ) ) ;
#18113 = ORIENTED_EDGE ( 'NONE', *, *, #2512, .F. ) ;
#18114 = CARTESIAN_POINT ( 'NONE',  ( -2.499999999999996447, -21.83333333333332860, 4.330127018922195425 ) ) ;
#18115 = ORIENTED_EDGE ( 'NONE', *, *, #42137, .F. ) ;
#18116 = CARTESIAN_POINT ( 'NONE',  ( 4.458734125000001214, -67.14583333196773651, 2.574251347313718519 ) ) ;
#18117 = CARTESIAN_POINT ( 'NONE',  ( 2.500000000000002220, -7.541666663935481907, 4.330127018922192761 ) ) ;
#18118 = CARTESIAN_POINT ( 'NONE',  ( 0.000000000000000000, 0.000000000000000000, -9.449444346342714240 ) ) ;
#18119 = ORIENTED_EDGE ( 'NONE', *, *, #49952, .T. ) ;
#18120 = CARTESIAN_POINT ( 'NONE',  ( 1.306442393143578906, 8.377108146505383601, -7.792327460285857654 ) ) ;
#18121 = CARTESIAN_POINT ( 'NONE',  ( -5.000000000000000000, -74.95833333060214443, -2.886751345948128211 ) ) ;
#18122 = CARTESIAN_POINT ( 'NONE',  ( 4.458734125000001214, -52.14583333196772941, 2.574251347313718519 ) ) ;
#18123 = ORIENTED_EDGE ( 'NONE', *, *, #10952, .T. ) ;
#18124 = DIRECTION ( 'NONE',  ( 0.000000000000000000, 0.000000000000000000, 1.000000000000000000 ) ) ;
#18125 = CARTESIAN_POINT ( 'NONE',  ( -4.458734124999998549, 10.77083333469892956, 2.574251347313722516 ) ) ;
#18126 = CARTESIAN_POINT ( 'NONE',  ( 9.457646018065525792E-16, 15.93750000136559564, 5.148502694627439702 ) ) ;
#18127 = CARTESIAN_POINT ( 'NONE',  ( -53.51423613279429503, -143.2500000013656063, 4.591703134518082763 ) ) ;
#18128 = DIRECTION ( 'NONE',  ( 0.000000000000000000, 1.000000000000000000, 0.000000000000000000 ) ) ;
#18129 = CARTESIAN_POINT ( 'NONE',  ( 4.458734124999999437, -169.3750000013656347, -1.846868145590734978 ) ) ;
#18130 = AXIS2_PLACEMENT_3D ( 'NONE', #13514, #53681, #63664 ) ;
#18131 = VERTEX_POINT ( 'NONE', #18940 ) ;
#18132 = CARTESIAN_POINT ( 'NONE',  ( 4.458734124999998549, -75.72916666530106511, -2.574251347313721627 ) ) ;
#18133 = CARTESIAN_POINT ( 'NONE',  ( -2.499999999999996447, -85.70833333060214443, 4.330127018922195425 ) ) ;
#18134 = CARTESIAN_POINT ( 'NONE',  ( -2.229367062500000163, 9.520833334698927786, -3.861377020970580443 ) ) ;
#18135 = VECTOR ( 'NONE', #15419, 1000.000000000000000 ) ;
#18136 = CARTESIAN_POINT ( 'NONE',  ( 0.000000000000000000, -170.0000000000000000, 5.000000000000000000 ) ) ;
#18137 = CARTESIAN_POINT ( 'NONE',  ( -2.229367062499996610, -62.39583333196774362, 3.861377020970582219 ) ) ;
#18138 = CARTESIAN_POINT ( 'NONE',  ( 5.000000000000000888, -22.45833333060214088, 2.886751345948126879 ) ) ;
#18139 = CARTESIAN_POINT ( 'NONE',  ( 5.000000000000000000, 4.500000000000000888, -6.123233995736766282E-16 ) ) ;
#18140 = DIRECTION ( 'NONE',  ( -0.000000000000000000, 1.000000000000000000, -0.000000000000000000 ) ) ;
#18141 = CARTESIAN_POINT ( 'NONE',  ( 2.500000000000002220, 19.45833333606451632, 4.330127018922192761 ) ) ;
#18142 = LINE ( 'NONE', #17831, #33690 ) ;
#18143 = CARTESIAN_POINT ( 'NONE',  ( -50.18089887299976937, -139.6875000000000000, 2.462841084822397164 ) ) ;
#18144 = CARTESIAN_POINT ( 'NONE',  ( -4.458734124999999437, -38.31249999863439371, 0.000000000000000000 ) ) ;
#18145 = CARTESIAN_POINT ( 'NONE',  ( 4.458734125000000326, -25.14583333196774007, 2.574251347313718519 ) ) ;
#18146 = CARTESIAN_POINT ( 'NONE',  ( -58.24261429053147765, -155.0000000000000284, -3.805975901505573411 ) ) ;
#18147 = CARTESIAN_POINT ( 'NONE',  ( -5.000000000000000000, 29.91666666666666430, -2.886751345948128211 ) ) ;
#18148 = CARTESIAN_POINT ( 'NONE',  ( 3.061616997868383141E-16, -154.8750000027311842, -5.000000000000000000 ) ) ;
#18149 = ORIENTED_EDGE ( 'NONE', *, *, #27611, .F. ) ;
#18150 = CARTESIAN_POINT ( 'NONE',  ( -2.229367062500000163, -106.7291666653010651, -3.861377020970580443 ) ) ;
#18151 = CARTESIAN_POINT ( 'NONE',  ( -2.229367062500000163, -29.47916666530107221, -3.861377020970580443 ) ) ;
#18152 = CARTESIAN_POINT ( 'NONE',  ( -4.999999999999999112, -69.79166666393547303, 2.886751345948131764 ) ) ;
#18153 = CARTESIAN_POINT ( 'NONE',  ( -53.51423613279429503, -149.5000000013655779, 4.591703134518082763 ) ) ;
#18154 = CARTESIAN_POINT ( 'NONE',  ( -3.535533905932737309, -146.6250000000000000, -3.535533905932738197 ) ) ;
#18155 = EDGE_CURVE ( 'NONE', #24664, #51343, #14115, .T. ) ;
#18156 = EDGE_CURVE ( 'NONE', #45293, #25630, #11649, .T. ) ;
#18157 = CARTESIAN_POINT ( 'NONE',  ( -4.458734124999999437, -31.31249999863440436, 0.000000000000000000 ) ) ;
#18158 = CARTESIAN_POINT ( 'NONE',  ( 4.458734124999999437, -69.06249999863439371, -5.460374474430324690E-16 ) ) ;
#18159 = CARTESIAN_POINT ( 'NONE',  ( -4.458734125000000326, -168.1250000013656063, 1.846868145590734089 ) ) ;
#18160 = CARTESIAN_POINT ( 'NONE',  ( -4.458734124999999437, -30.31249999863440436, 0.000000000000000000 ) ) ;
#18161 = EDGE_CURVE ( 'NONE', #20917, #57302, #11205, .T. ) ;
#18162 = CARTESIAN_POINT ( 'NONE',  ( 1.975475456537005874E-15, -106.7499999999999858, 5.000000000000000000 ) ) ;
#18163 = CARTESIAN_POINT ( 'NONE',  ( 2.499999999999998668, 18.79166666939785202, -4.330127018922193649 ) ) ;
#18164 = CARTESIAN_POINT ( 'NONE',  ( 5.000000000000000000, -18.41666666666666430, -2.886751345948129988 ) ) ;
#18165 = CARTESIAN_POINT ( 'NONE',  ( 4.458734124999999437, -148.5000000013656347, 1.846868145590737864 ) ) ;
#18166 = ORIENTED_EDGE ( 'NONE', *, *, #57567, .F. ) ;
#18167 = CARTESIAN_POINT ( 'NONE',  ( 1.975475456537005874E-15, -57.74999999999999289, 5.000000000000000000 ) ) ;
#18168 = CARTESIAN_POINT ( 'NONE',  ( -4.458734124999997661, -56.47916666530107221, 2.574251347313722516 ) ) ;
#18169 = CARTESIAN_POINT ( 'NONE',  ( 2.500000000000002220, 25.45833333606451987, 4.330127018922192761 ) ) ;
#18170 = DIRECTION ( 'NONE',  ( -0.000000000000000000, 1.000000000000000000, -0.000000000000000000 ) ) ;
#18171 = CARTESIAN_POINT ( 'NONE',  ( 5.000000000000000000, 26.50000000000000000, -6.123233995736766282E-16 ) ) ;
#18172 = EDGE_CURVE ( 'NONE', #61583, #17564, #13720, .T. ) ;
#18173 = EDGE_CURVE ( 'NONE', #52605, #60408, #48842, .T. ) ;
#18174 = CARTESIAN_POINT ( 'NONE',  ( -6.972266317189433020E-16, -44.25000000000000000, -5.000000000000000000 ) ) ;
#18175 = CARTESIAN_POINT ( 'NONE',  ( -2.229367062500000163, 0.5208333346989266754, -3.861377020970580443 ) ) ;
#18176 = CARTESIAN_POINT ( 'NONE',  ( 2.500000000000002220, -14.66666666666666785, 4.330127018922192761 ) ) ;
#18177 = CARTESIAN_POINT ( 'NONE',  ( 4.458734124999999437, 7.937500001365595637, -5.460374474430324690E-16 ) ) ;
#18179 = ORIENTED_EDGE ( 'NONE', *, *, #38613, .T. ) ;
#18178 = ADVANCED_FACE ( 'NONE', ( #5746 ), #34689, .F. ) ;
#18180 = CARTESIAN_POINT ( 'NONE',  ( 5.000000000000000888, 26.41666666666666430, 2.886751345948126879 ) ) ;
#18181 = VERTEX_POINT ( 'NONE', #40470 ) ;
#18182 = VECTOR ( 'NONE', #50911, 1000.000000000000000 ) ;
#18183 = CARTESIAN_POINT ( 'NONE',  ( 1.339745962155613146, 27.41965820146970145, 5.000000000000000888 ) ) ;
#18184 = CARTESIAN_POINT ( 'NONE',  ( 4.458734124999999437, -46.81249999863440792, -5.460374474430324690E-16 ) ) ;
#18185 = EDGE_CURVE ( 'NONE', #62764, #19443, #60110, .T. ) ;
#18186 = CARTESIAN_POINT ( 'NONE',  ( 1.846868145590736310, -161.8750000013656063, 4.458734124999999437 ) ) ;
#18187 = EDGE_CURVE ( 'NONE', #19422, #24361, #29531, .T. ) ;
#18188 = VECTOR ( 'NONE', #31287, 1000.000000000000000 ) ;
#18189 = VECTOR ( 'NONE', #53189, 1000.000000000000000 ) ;
#18190 =( BOUNDED_CURVE ( )  B_SPLINE_CURVE ( 2, ( #44306, #60083, #24383, #43984, #49137, #39482, #6052, #20195, #19868 ),
 .UNSPECIFIED., .F., .F. ) 
 B_SPLINE_CURVE_WITH_KNOTS ( ( 3, 2, 2, 2, 3 ),
 ( 0.2583333333333335813, 0.2625000000000002331, 0.2666666666666668850, 0.2708333333333335369, 0.2750000000000002442 ),
 .UNSPECIFIED. ) 
 CURVE ( )  GEOMETRIC_REPRESENTATION_ITEM ( )  RATIONAL_B_SPLINE_CURVE ( ( 0.9999999999999958922, 0.9238795325112908463, 1.000000000000000000, 0.9238795325112867385, 1.000000000000000000, 0.9238795325112867385, 1.000000000000000000, 0.9238795325112826307, 1.000000000000003997 ) ) 
 REPRESENTATION_ITEM ( '' )  );
#18191 = CARTESIAN_POINT ( 'NONE',  ( 1.060575238724906964E-15, -50.62499999726881583, 5.773502691896257311 ) ) ;
#18192 = ORIENTED_EDGE ( 'NONE', *, *, #11795, .T. ) ;
#18193 = CARTESIAN_POINT ( 'NONE',  ( -3.152548672688508926E-16, -24.56249999863440792, -5.148502694627439702 ) ) ;
#18194 = EDGE_LOOP ( 'NONE', ( #37258, #30608, #10923, #23192 ) ) ;
#18196 = CARTESIAN_POINT ( 'NONE',  ( 3.061616997868383141E-16, -142.8750000027312126, -5.000000000000000000 ) ) ;
#18195 = CARTESIAN_POINT ( 'NONE',  ( 6.123233995736766282E-16, -120.0000000000000000, -5.000000000000000000 ) ) ;
#18197 = CARTESIAN_POINT ( 'NONE',  ( 3.152801135295366208, -160.5625000013656063, 3.152801135295367985 ) ) ;
#18198 = CYLINDRICAL_SURFACE ( 'NONE', #14914, 5.000000000000000000 ) ;
#18199 = CARTESIAN_POINT ( 'NONE',  ( -58.24261429053147765, -136.2500000000000284, -3.805975901505573855 ) ) ;
#18200 = CARTESIAN_POINT ( 'NONE',  ( -4.458734124999998549, -40.47916666530107221, 2.574251347313722516 ) ) ;
#18201 = EDGE_LOOP ( 'NONE', ( #10644, #50862, #14999, #1630 ) ) ;
#18202 = CARTESIAN_POINT ( 'NONE',  ( 2.229367062500001939, -81.97916666530106511, 3.861377020970579999 ) ) ;
#18203 = CARTESIAN_POINT ( 'NONE',  ( -4.458734124999999437, 23.60416666803225993, -2.574251347313719407 ) ) ;
#18204 = CARTESIAN_POINT ( 'NONE',  ( 2.500000000000002220, -59.66666666666665719, 4.330127018922192761 ) ) ;
#18205 = ORIENTED_EDGE ( 'NONE', *, *, #31092, .T. ) ;
#18206 = CARTESIAN_POINT ( 'NONE',  ( 4.648177544792955347E-16, 28.87500000273118417, -5.000000000000000000 ) ) ;
#18207 = CARTESIAN_POINT ( 'NONE',  ( -52.10840900171896806, -139.4375000013656063, 3.393966926194110556 ) ) ;
#18208 = CARTESIAN_POINT ( 'NONE',  ( -4.458734124999999437, -83.64583333196773651, -2.574251347313719407 ) ) ;
#18209 = CARTESIAN_POINT ( 'NONE',  ( -51.75738570946856498, -128.8750000027312126, 3.805975901505576964 ) ) ;
#18210 = CARTESIAN_POINT ( 'NONE',  ( -1.339745962155613812, 24.91965820146970501, -5.000000000000000000 ) ) ;
#18211 = CARTESIAN_POINT ( 'NONE',  ( -5.000000000000000000, -83.08333333333332860, -2.886751345948128211 ) ) ;
#18212 = CARTESIAN_POINT ( 'NONE',  ( -5.000000000000000000, -44.87499999726880873, 0.000000000000000000 ) ) ;
#18213 = CARTESIAN_POINT ( 'NONE',  ( -4.458734124999997661, -56.22916666530107221, 2.574251347313722516 ) ) ;
#18214 = CARTESIAN_POINT ( 'NONE',  ( 5.000000000000000000, -37.41666666666666430, -2.886751345948130876 ) ) ;
#18215 = CARTESIAN_POINT ( 'NONE',  ( -4.458734124999999437, 21.60416666803225993, -2.574251347313719407 ) ) ;
#18216 = DIRECTION ( 'NONE',  ( -0.000000000000000000, 1.000000000000000000, -0.000000000000000000 ) ) ;
#18217 = CARTESIAN_POINT ( 'NONE',  ( -3.152548672688508926E-16, -41.81249999863440081, -5.148502694627439702 ) ) ;
#18218 = CARTESIAN_POINT ( 'NONE',  ( 5.000000000000000000, -5.374999997268811391, -6.123233995736766282E-16 ) ) ;
#18219 = DIRECTION ( 'NONE',  ( -0.000000000000000000, 1.000000000000000000, -0.000000000000000000 ) ) ;
#18220 = CARTESIAN_POINT ( 'NONE',  ( -54.64476657466781973, -126.8125000013655921, -4.444560631937228834 ) ) ;
#18221 = CARTESIAN_POINT ( 'NONE',  ( 4.458734125000001214, -84.14583333196772230, 2.574251347313718519 ) ) ;
#18222 = CARTESIAN_POINT ( 'NONE',  ( 4.458734124999999437, -103.8124999986344079, -5.460374474430324690E-16 ) ) ;
#18223 = CARTESIAN_POINT ( 'NONE',  ( -4.458734124999997661, -7.479166665301073991, 2.574251347313722516 ) ) ;
#18224 = VERTEX_POINT ( 'NONE', #5108 ) ;
#18225 = CARTESIAN_POINT ( 'NONE',  ( -6.972266317189433020E-16, 17.87500000273118417, -5.000000000000000000 ) ) ;
#18226 = CARTESIAN_POINT ( 'NONE',  ( 4.458734125000001214, -93.89583333196772230, 2.574251347313718519 ) ) ;
#18227 = CARTESIAN_POINT ( 'NONE',  ( 5.000000000000000000, -164.1250000027311842, 0.000000000000000000 ) ) ;
#18228 = CARTESIAN_POINT ( 'NONE',  ( -4.458734124999998549, -90.47916666530106511, 2.574251347313722516 ) ) ;
#18229 = AXIS2_PLACEMENT_3D ( 'NONE', #62383, #42739, #18305 ) ;
#18230 = CARTESIAN_POINT ( 'NONE',  ( -6.972266317189433020E-16, -16.25000000000000000, -5.000000000000000000 ) ) ;
#18231 = CARTESIAN_POINT ( 'NONE',  ( -50.55543936806279248, -130.0625000013656063, 0.3552334253322060320 ) ) ;
#18232 = VECTOR ( 'NONE', #15210, 1000.000000000000000 ) ;
#18233 = CARTESIAN_POINT ( 'NONE',  ( -3.152548672688508926E-16, -13.56249999863440259, -5.148502694627439702 ) ) ;
#18234 = CARTESIAN_POINT ( 'NONE',  ( 4.458734124999998549, 10.02083333469892779, -2.574251347313721627 ) ) ;
#18235 = CARTESIAN_POINT ( 'NONE',  ( 4.458734124999998549, -52.97916666530107932, -2.574251347313721627 ) ) ;
#18236 =( BOUNDED_CURVE ( )  B_SPLINE_CURVE ( 2, ( #4783, #19892, #44011, #59144, #39507, #950, #54637, #15076, #54314 ),
 .UNSPECIFIED., .F., .F. ) 
 B_SPLINE_CURVE_WITH_KNOTS ( ( 3, 2, 2, 2, 3 ),
 ( 0.6232142857142857206, 0.6238095238095238138, 0.6250000000000000000, 0.6261904761904761862, 0.6267857142857142794 ),
 .UNSPECIFIED. ) 
 CURVE ( )  GEOMETRIC_REPRESENTATION_ITEM ( )  RATIONAL_B_SPLINE_CURVE ( ( 0.9330127018922194093, 0.9330127018922194093, 1.000000000000000000, 0.8660254037844387076, 1.000000000000000000, 0.8660254037844387076, 1.000000000000000000, 0.9330127018922194093, 0.9330127018922194093 ) ) 
 REPRESENTATION_ITEM ( '' )  );
#18237 = CARTESIAN_POINT ( 'NONE',  ( -6.972266317189433020E-16, -86.12499999726880162, -5.000000000000000000 ) ) ;
#18238 = CARTESIAN_POINT ( 'NONE',  ( 1.975475456537005874E-15, 17.25000000000000000, 5.000000000000000000 ) ) ;
#18239 = CARTESIAN_POINT ( 'NONE',  ( 9.457646018065525792E-16, -11.06249999863440969, 5.148502694627439702 ) ) ;
#18240 = CARTESIAN_POINT ( 'NONE',  ( 1.339745962155615144, -84.70534180126146850, 4.999999999999999112 ) ) ;
#18241 = ORIENTED_EDGE ( 'NONE', *, *, #18020, .T. ) ;
#18242 = CARTESIAN_POINT ( 'NONE',  ( -3.152548672688508926E-16, -40.81249999863440081, -5.148502694627439702 ) ) ;
#18243 = UNCERTAINTY_MEASURE_WITH_UNIT (LENGTH_MEASURE( 1.000000000000000082E-05 ), #54126, 'distance_accuracy_value', 'NONE');
#18244 = CARTESIAN_POINT ( 'NONE',  ( -54.64476657466781973, -129.0625000013656063, -4.444560631937228834 ) ) ;
#18245 = CARTESIAN_POINT ( 'NONE',  ( 6.123233995736766282E-16, -170.0000000000000000, -5.000000000000000000 ) ) ;
#18246 = CARTESIAN_POINT ( 'NONE',  ( 4.458734124999998549, -80.72916666530106511, -2.574251347313721627 ) ) ;
#18247 = CARTESIAN_POINT ( 'NONE',  ( 4.458734124999998549, 25.02083333469892423, -2.574251347313721627 ) ) ;
#18248 = CARTESIAN_POINT ( 'NONE',  ( 4.458734124999999437, 17.18750000136559564, -5.460374474430324690E-16 ) ) ;
#18249 = CARTESIAN_POINT ( 'NONE',  ( 0.000000000000000000, -170.0000000000000000, 0.000000000000000000 ) ) ;
#18250 = CARTESIAN_POINT ( 'NONE',  ( 5.000000000000000000, -55.49999999999999289, -6.123233995736766282E-16 ) ) ;
#18251 = CARTESIAN_POINT ( 'NONE',  ( 2.229367062499998831, -84.89583333196773651, -3.861377020970580887 ) ) ;
#18252 = CARTESIAN_POINT ( 'NONE',  ( 2.499999999999998668, -72.33333333333332860, -4.330127018922193649 ) ) ;
#18253 = CARTESIAN_POINT ( 'NONE',  ( 2.499999999999998668, 15.79166666939785202, -4.330127018922193649 ) ) ;
#18254 = ORIENTED_EDGE ( 'NONE', *, *, #53403, .F. ) ;
#18255 = CARTESIAN_POINT ( 'NONE',  ( 2.499999999999998668, -35.33333333333332860, -4.330127018922193649 ) ) ;
#18256 = CARTESIAN_POINT ( 'NONE',  ( -5.000000000000000000, -90.08333333333332860, -2.886751345948128211 ) ) ;
#18258 = CARTESIAN_POINT ( 'NONE',  ( 5.000000000000000000, -27.49999999999999645, -6.123233995736766282E-16 ) ) ;
#18257 = CARTESIAN_POINT ( 'NONE',  ( 5.000000000000000888, -52.58333333333332860, 2.886751345948126879 ) ) ;
#18259 = CARTESIAN_POINT ( 'NONE',  ( 4.458734124999998549, -32.72916666530107221, -2.574251347313721627 ) ) ;
#18260 = FACE_OUTER_BOUND ( 'NONE', #38812, .T. ) ;
#18261 = EDGE_CURVE ( 'NONE', #49758, #41892, #18236, .T. ) ;
#18262 = CARTESIAN_POINT ( 'NONE',  ( 2.499999999999998668, -28.20833333060214798, -4.330127018922193649 ) ) ;
#18264 = ORIENTED_EDGE ( 'NONE', *, *, #21391, .F. ) ;
#18263 = CARTESIAN_POINT ( 'NONE',  ( 2.229367062500001939, -59.97916666530106511, 3.861377020970579999 ) ) ;
#18265 = PLANE ( 'NONE',  #20017 ) ;
#18267 = ORIENTED_EDGE ( 'NONE', *, *, #62976, .T. ) ;
#18266 = CARTESIAN_POINT ( 'NONE',  ( 2.229367062500001939, -8.229166665301073991, 3.861377020970579999 ) ) ;
#18268 = CARTESIAN_POINT ( 'NONE',  ( 2.500000000000002220, -75.66666666666665719, 4.330127018922192761 ) ) ;
#18269 = CARTESIAN_POINT ( 'NONE',  ( -50.75781946612335105, -135.0000000000005969, -1.372666862511563224 ) ) ;
#18270 = CARTESIAN_POINT ( 'NONE',  ( 4.458734124999999437, -52.06249999863440792, -5.460374474430324690E-16 ) ) ;
#18271 = VECTOR ( 'NONE', #20688, 1000.000000000000000 ) ;
#18272 = CARTESIAN_POINT ( 'NONE',  ( 5.000000000000000888, -78.45833333060214443, 2.886751345948126879 ) ) ;
#18274 = ORIENTED_EDGE ( 'NONE', *, *, #59361, .T. ) ;
#18273 = CARTESIAN_POINT ( 'NONE',  ( -2.500000000000000444, 9.958333336064519870, -4.330127018922193649 ) ) ;
#18275 = CARTESIAN_POINT ( 'NONE',  ( -58.80597590150559739, -148.0000000000000284, 3.242614290531460330 ) ) ;
#18276 = AXIS2_PLACEMENT_3D ( 'NONE', #48288, #23549, #13256 ) ;
#18277 = CARTESIAN_POINT ( 'NONE',  ( 4.458734124999999437, -23.06249999863440436, -5.460374474430324690E-16 ) ) ;
#18279 = ORIENTED_EDGE ( 'NONE', *, *, #23550, .T. ) ;
#18278 = CARTESIAN_POINT ( 'NONE',  ( -3.152548672688508926E-16, -54.81249999863440081, -5.148502694627439702 ) ) ;
#18280 = CARTESIAN_POINT ( 'NONE',  ( 0.000000000000000000, 0.000000000000000000, 0.000000000000000000 ) ) ;
#18281 = CARTESIAN_POINT ( 'NONE',  ( -4.458734125000001214, -169.1250000013656347, 1.846868145590734089 ) ) ;
#18282 = CARTESIAN_POINT ( 'NONE',  ( -4.458734124999998549, -100.4791666653010509, 2.574251347313722516 ) ) ;
#18283 = CARTESIAN_POINT ( 'NONE',  ( -57.46284108482265651, -135.0625000027312410, 4.819101127000238627 ) ) ;
#18284 = ORIENTED_EDGE ( 'NONE', *, *, #542, .F. ) ;
#18285 = CARTESIAN_POINT ( 'NONE',  ( -57.89159099828107458, -148.9375000013656063, -3.393966926194107447 ) ) ;
#18286 = CARTESIAN_POINT ( 'NONE',  ( -52.53715891517739323, -143.5625000027312126, -4.819101127000233298 ) ) ;
#18287 = VECTOR ( 'NONE', #22881, 1000.000000000000000 ) ;
#18288 =( BOUNDED_CURVE ( )  B_SPLINE_CURVE ( 2, ( #16476, #17437, #36411, #36733, #26765, #60867, #30946, #46063, #41860 ),
 .UNSPECIFIED., .F., .F. ) 
 B_SPLINE_CURVE_WITH_KNOTS ( ( 3, 2, 2, 2, 3 ),
 ( 0.6732142857142857650, 0.6738095238095238582, 0.6750000000000000444, 0.6761904761904762307, 0.6767857142857143238 ),
 .UNSPECIFIED. ) 
 CURVE ( )  GEOMETRIC_REPRESENTATION_ITEM ( )  RATIONAL_B_SPLINE_CURVE ( ( 0.9330127018922194093, 0.9330127018922194093, 1.000000000000000000, 0.8660254037844387076, 1.000000000000000000, 0.8660254037844387076, 1.000000000000000000, 0.9330127018922194093, 0.9330127018922194093 ) ) 
 REPRESENTATION_ITEM ( '' )  );
#18289 = CARTESIAN_POINT ( 'NONE',  ( -6.972266317189433020E-16, -86.25000000000001421, -5.000000000000000000 ) ) ;
#18290 = CARTESIAN_POINT ( 'NONE',  ( 2.229367062499998831, -8.645833331967736513, -3.861377020970580887 ) ) ;
#18291 = CARTESIAN_POINT ( 'NONE',  ( -2.229367062499996610, -97.39583333196773651, 3.861377020970582219 ) ) ;
#18292 = CARTESIAN_POINT ( 'NONE',  ( -1.846868145590734756, -143.3750000013656063, -4.458734125000000326 ) ) ;
#18293 = CARTESIAN_POINT ( 'NONE',  ( 2.229367062499998831, -29.89583333196773296, -3.861377020970580887 ) ) ;
#18294 = CARTESIAN_POINT ( 'NONE',  ( 0.000000000000000000, -170.0000000000000000, 0.000000000000000000 ) ) ;
#18295 = CARTESIAN_POINT ( 'NONE',  ( -57.89159099828107458, -138.6875000013656347, -3.393966926194107447 ) ) ;
#18296 = CARTESIAN_POINT ( 'NONE',  ( -2.229367062499996610, -69.39583333196773651, 3.861377020970582219 ) ) ;
#18297 = CARTESIAN_POINT ( 'NONE',  ( 1.975475456537005874E-15, -43.75000000000000000, 5.000000000000000000 ) ) ;
#18298 = CARTESIAN_POINT ( 'NONE',  ( -4.999999999999998224, -42.79166666393548013, 2.886751345948131764 ) ) ;
#18299 = CARTESIAN_POINT ( 'NONE',  ( 4.458734124999999437, -141.3750000013656063, -1.846868145590734978 ) ) ;
#18300 = CARTESIAN_POINT ( 'NONE',  ( -2.229367062500000163, 12.27083333469892601, -3.861377020970580443 ) ) ;
#18301 = ORIENTED_EDGE ( 'NONE', *, *, #60522, .F. ) ;
#18302 = CARTESIAN_POINT ( 'NONE',  ( -2.499999999999996447, -4.833333333333335702, 4.330127018922195425 ) ) ;
#18304 = CARTESIAN_POINT ( 'NONE',  ( 4.458734124999999437, -24.81249999863440436, -5.460374474430324690E-16 ) ) ;
#18303 = CARTESIAN_POINT ( 'NONE',  ( 2.499999999999998668, -90.33333333333332860, -4.330127018922193649 ) ) ;
#18305 = DIRECTION ( 'NONE',  ( -0.7611951803011147710, 0.000000000000000000, 0.6485228581062916220 ) ) ;
#18306 = CARTESIAN_POINT ( 'NONE',  ( -4.458734124999998549, -75.47916666530107932, 2.574251347313722516 ) ) ;
#18307 = CARTESIAN_POINT ( 'NONE',  ( 9.457646018065525792E-16, 24.68750000136559208, 5.148502694627439702 ) ) ;
#18308 = CYLINDRICAL_SURFACE ( 'NONE', #44804, 5.000000000000000000 ) ;
#18309 = CARTESIAN_POINT ( 'NONE',  ( -56.48576386720575471, -141.7500000013656063, -4.591703134518078322 ) ) ;
#18310 = CARTESIAN_POINT ( 'NONE',  ( 2.229367062500001939, 2.020833334698927786, 3.861377020970579999 ) ) ;
#18311 = CARTESIAN_POINT ( 'NONE',  ( 4.458734125000001214, 26.85416666803225993, 2.574251347313718519 ) ) ;
#18312 = CARTESIAN_POINT ( 'NONE',  ( 2.229367062500001939, -38.22916666530107221, 3.861377020970579999 ) ) ;
#18313 = CARTESIAN_POINT ( 'NONE',  ( 0.000000000000000000, -170.0000000000000000, 0.000000000000000000 ) ) ;
#18314 = CARTESIAN_POINT ( 'NONE',  ( -3.152548672688508926E-16, 6.437500001365592972, -5.148502694627439702 ) ) ;
#18315 = CARTESIAN_POINT ( 'NONE',  ( 9.457646018065525792E-16, -70.06249999863439371, 5.148502694627439702 ) ) ;
#18316 = CARTESIAN_POINT ( 'NONE',  ( -4.458734124999999437, -20.56249999863440081, 0.000000000000000000 ) ) ;
#18317 = CARTESIAN_POINT ( 'NONE',  ( 5.000000000000000888, -5.583333333333336590, 2.886751345948126879 ) ) ;
#18318 = CARTESIAN_POINT ( 'NONE',  ( -8.190561711645485556E-16, -160.6875000013655779, 4.458734124999999437 ) ) ;
#18319 = CARTESIAN_POINT ( 'NONE',  ( 5.000000000000000000, 23.58333333333333215, -2.886751345948130876 ) ) ;
#18320 = CARTESIAN_POINT ( 'NONE',  ( -4.458734124999999437, -63.39583333196772941, -2.574251347313719407 ) ) ;
#18321 = CARTESIAN_POINT ( 'NONE',  ( -5.000000000000000000, -99.95833333060213022, -2.886751345948128211 ) ) ;
#18322 = AXIS2_PLACEMENT_3D ( 'NONE', #49079, #19814, #48455 ) ;
#18323 = DIRECTION ( 'NONE',  ( -0.000000000000000000, 1.000000000000000000, -0.000000000000000000 ) ) ;
#18324 = CARTESIAN_POINT ( 'NONE',  ( 4.458734124999998549, -42.72916666530107932, -2.574251347313721627 ) ) ;
#18325 = CARTESIAN_POINT ( 'NONE',  ( 5.000000000000000000, 9.625000002731184168, -6.123233995736766282E-16 ) ) ;
#18326 = CARTESIAN_POINT ( 'NONE',  ( -3.152548672688508926E-16, -103.8124999986343937, -5.148502694627439702 ) ) ;
#18327 = CARTESIAN_POINT ( 'NONE',  ( -4.458734124999999437, -68.56249999863439371, 0.000000000000000000 ) ) ;
#18328 = CARTESIAN_POINT ( 'NONE',  ( 2.499999999999998668, -56.33333333333333570, -4.330127018922193649 ) ) ;
#18329 = DIRECTION ( 'NONE',  ( -0.6485228581062915110, 0.000000000000000000, -0.7611951803011149931 ) ) ;
#18330 = CARTESIAN_POINT ( 'NONE',  ( 2.500000000000002220, -89.66666666666665719, 4.330127018922192761 ) ) ;
#18331 = VERTEX_POINT ( 'NONE', #10252 ) ;
#18332 = LINE ( 'NONE', #61466, #4766 ) ;
#18333 = CARTESIAN_POINT ( 'NONE',  ( 5.000000000000000888, 2.541666669397851130, 2.886751345948126879 ) ) ;
#18334 = CARTESIAN_POINT ( 'NONE',  ( -2.499999999999996447, -13.83333333333333570, 4.330127018922195425 ) ) ;
#18335 = CARTESIAN_POINT ( 'NONE',  ( 4.458734124999998549, -18.72916666530106866, -2.574251347313721627 ) ) ;
#18336 = CARTESIAN_POINT ( 'NONE',  ( 2.229367062500001939, -77.97916666530106511, 3.861377020970579999 ) ) ;
#18337 = VECTOR ( 'NONE', #21396, 1000.000000000000000 ) ;
#18338 = FACE_OUTER_BOUND ( 'NONE', #50555, .T. ) ;
#18339 = CARTESIAN_POINT ( 'NONE',  ( 5.000000000000000888, -10.45833333060214621, 2.886751345948126879 ) ) ;
#18341 = ORIENTED_EDGE ( 'NONE', *, *, #39203, .T. ) ;
#18340 = CARTESIAN_POINT ( 'NONE',  ( 2.229367062499998831, -45.64583333196774362, -3.861377020970580887 ) ) ;
#18342 = CARTESIAN_POINT ( 'NONE',  ( 3.535533905932738197, -143.8750000000000000, -3.535533905932738197 ) ) ;
#18344 = ORIENTED_EDGE ( 'NONE', *, *, #12203, .T. ) ;
#18343 = CARTESIAN_POINT ( 'NONE',  ( -2.229367062500000163, 7.270833334698929562, -3.861377020970580443 ) ) ;
#18345 = CARTESIAN_POINT ( 'NONE',  ( 0.000000000000000000, -170.0000000000000000, 0.000000000000000000 ) ) ;
#18346 = CARTESIAN_POINT ( 'NONE',  ( 2.500000000000002220, -60.66666666666665719, 4.330127018922192761 ) ) ;
#18347 = CARTESIAN_POINT ( 'NONE',  ( 1.846868145590736310, -156.8750000013655779, 4.458734124999999437 ) ) ;
#18348 = CARTESIAN_POINT ( 'NONE',  ( 4.458734124999998549, -35.97916666530107221, -2.574251347313721627 ) ) ;
#18349 = CARTESIAN_POINT ( 'NONE',  ( -1.339745962155610925, -55.79465819873851729, 5.000000000000000000 ) ) ;
#18350 = CARTESIAN_POINT ( 'NONE',  ( 3.535533905932738197, -167.8750000000000284, -3.535533905932738197 ) ) ;
#18351 = LINE ( 'NONE', #37975, #31313 ) ;
#18352 = CARTESIAN_POINT ( 'NONE',  ( -51.60603307380591787, -131.1875000013656063, -2.891590998281053704 ) ) ;
#18353 = CARTESIAN_POINT ( 'NONE',  ( 4.458734124999998549, -5.979166665301073103, -2.574251347313721627 ) ) ;
#18354 = CARTESIAN_POINT ( 'NONE',  ( 4.458734124999998549, -42.97916666530107221, -2.574251347313721627 ) ) ;
#18355 = CARTESIAN_POINT ( 'NONE',  ( 2.499999999999998668, -54.33333333333332860, -4.330127018922193649 ) ) ;
#18356 = CARTESIAN_POINT ( 'NONE',  ( -2.229367062499996610, -85.39583333196773651, 3.861377020970582219 ) ) ;
#18357 = CARTESIAN_POINT ( 'NONE',  ( 5.000000000000000000, 8.500000000000000000, -6.123233995736766282E-16 ) ) ;
#18358 = EDGE_LOOP ( 'NONE', ( #49280, #53521, #35918, #3404 ) ) ;
#18359 = CARTESIAN_POINT ( 'NONE',  ( -50.01589407740564042, -152.7500000027312410, 0.3983568153799778022 ) ) ;
#18360 = AXIS2_PLACEMENT_3D ( 'NONE', #49266, #24821, #33528 ) ;
#18361 = CARTESIAN_POINT ( 'NONE',  ( -2.498395430326213474E-14, 21.37500000273118062, 5.000000000000000000 ) ) ;
#18363 = EDGE_CURVE ( 'NONE', #26556, #41789, #20690, .T. ) ;
#18362 = CARTESIAN_POINT ( 'NONE',  ( -2.229367062500000163, -69.72916666530107932, -3.861377020970580443 ) ) ;
#18364 = VECTOR ( 'NONE', #25790, 1000.000000000000000 ) ;
#18365 = CARTESIAN_POINT ( 'NONE',  ( 3.152801135295367541, -147.5625000013655779, -3.152801135295367541 ) ) ;
#18366 = ORIENTED_EDGE ( 'NONE', *, *, #33355, .T. ) ;
#18367 =( BOUNDED_CURVE ( )  B_SPLINE_CURVE ( 2, ( #11389, #31009, #35526, #26838, #60938, #40981, #60623, #16543, #36166 ),
 .UNSPECIFIED., .F., .F. ) 
 B_SPLINE_CURVE_WITH_KNOTS ( ( 3, 2, 2, 2, 3 ),
 ( 0.7020833333333332815, 0.7027777777777777235, 0.7041666666666667185, 0.7055555555555556024, 0.7062500000000000444 ),
 .UNSPECIFIED. ) 
 CURVE ( )  GEOMETRIC_REPRESENTATION_ITEM ( )  RATIONAL_B_SPLINE_CURVE ( ( 0.9330127018922194093, 0.9330127018922194093, 1.000000000000000000, 0.8660254037844387076, 1.000000000000000000, 0.8660254037844387076, 1.000000000000000000, 0.9330127018922194093, 0.9330127018922194093 ) ) 
 REPRESENTATION_ITEM ( '' )  );
#18368 = FACE_OUTER_BOUND ( 'NONE', #11309, .T. ) ;
#18369 = CARTESIAN_POINT ( 'NONE',  ( 4.458734124999999437, -10.06249999863440614, -5.460374474430324690E-16 ) ) ;
#18370 = CARTESIAN_POINT ( 'NONE',  ( 1.975475456537005874E-15, -79.62499999726881583, 5.000000000000000000 ) ) ;
#18371 = CARTESIAN_POINT ( 'NONE',  ( -2.229367062500000163, 0.5208333346989266754, -3.861377020970580443 ) ) ;
#18372 = CARTESIAN_POINT ( 'NONE',  ( -4.999999999999998224, -95.79166666393547303, 2.886751345948131764 ) ) ;
#18373 = CARTESIAN_POINT ( 'NONE',  ( -4.458734124999999437, -152.0000000013656063, -1.846868145590735644 ) ) ;
#18374 = CARTESIAN_POINT ( 'NONE',  ( -4.458734124999999437, 24.43750000136559208, 0.000000000000000000 ) ) ;
#18375 = ORIENTED_EDGE ( 'NONE', *, *, #12995, .T. ) ;
#18376 = CARTESIAN_POINT ( 'NONE',  ( -2.229367062499996610, -94.14583333196772230, 3.861377020970582219 ) ) ;
#18377 = CARTESIAN_POINT ( 'NONE',  ( -1.339745962155613812, -31.20534180126147916, -5.000000000000000000 ) ) ;
#18378 = CARTESIAN_POINT ( 'NONE',  ( 5.000000000000000888, -63.58333333333332860, 2.886751345948126879 ) ) ;
#18379 = CARTESIAN_POINT ( 'NONE',  ( 9.457646018065525792E-16, -8.062499998634404363, 5.148502694627439702 ) ) ;
#18380 = LINE ( 'NONE', #56689, #33427 ) ;
#18381 = AXIS2_PLACEMENT_3D ( 'NONE', #1811, #59700, #34591 ) ;
#18382 = FACE_OUTER_BOUND ( 'NONE', #21764, .T. ) ;
#18383 =( BOUNDED_CURVE ( )  B_SPLINE_CURVE ( 2, ( #39329, #50268, #25503, #34842, #29349, #30001, #58962, #11024, #761 ),
 .UNSPECIFIED., .F., .F. ) 
 B_SPLINE_CURVE_WITH_KNOTS ( ( 3, 2, 2, 2, 3 ),
 ( 0.7583333333333330817, 0.7624999999999997335, 0.7666666666666664964, 0.7708333333333331483, 0.7749999999999998002 ),
 .UNSPECIFIED. ) 
 CURVE ( )  GEOMETRIC_REPRESENTATION_ITEM ( )  RATIONAL_B_SPLINE_CURVE ( ( 1.000000000000003997, 0.9238795325112826307, 1.000000000000000000, 0.9238795325112867385, 1.000000000000000000, 0.9238795325112867385, 1.000000000000000000, 0.9238795325112908463, 0.9999999999999958922 ) ) 
 REPRESENTATION_ITEM ( '' )  );
#18384 = CARTESIAN_POINT ( 'NONE',  ( 5.000000000000000000, -87.41666666666667140, -2.886751345948130876 ) ) ;
#18385 = CARTESIAN_POINT ( 'NONE',  ( 5.000000000000000888, -37.45833333060213732, 2.886751345948126879 ) ) ;
#18386 = CARTESIAN_POINT ( 'NONE',  ( 5.000000000000000000, -49.29166666393547303, -2.886751345948130876 ) ) ;
#18387 = CARTESIAN_POINT ( 'NONE',  ( 4.458734124999999437, 21.18750000136559208, -5.460374474430324690E-16 ) ) ;
#18388 = CARTESIAN_POINT ( 'NONE',  ( -1.339745962155613812, -98.08034179853028434, -5.000000000000000000 ) ) ;
#18389 = CARTESIAN_POINT ( 'NONE',  ( 2.229367062499998831, 23.35416666803225993, -3.861377020970580887 ) ) ;
#18390 = CARTESIAN_POINT ( 'NONE',  ( -4.458734124999998549, -59.22916666530106511, 2.574251347313722516 ) ) ;
#18391 = CARTESIAN_POINT ( 'NONE',  ( -4.458734124999997661, -4.479166665301070438, 2.574251347313722516 ) ) ;
#18392 = CARTESIAN_POINT ( 'NONE',  ( -5.000000000000000000, -33.95833333060213732, -2.886751345948128211 ) ) ;
#18393 = CARTESIAN_POINT ( 'NONE',  ( -2.500000000000000444, 9.833333333333332149, -4.330127018922193649 ) ) ;
#18394 = CARTESIAN_POINT ( 'NONE',  ( -5.000000000000000000, -141.6250000027312126, -6.123233995736766282E-16 ) ) ;
#18395 = CARTESIAN_POINT ( 'NONE',  ( -1.339745962155660663, -20.66965819600733667, 4.999999999999972466 ) ) ;
#18396 = CARTESIAN_POINT ( 'NONE',  ( -2.229367062500000163, -49.47916666530107221, -3.861377020970580443 ) ) ;
#18397 = CARTESIAN_POINT ( 'NONE',  ( -5.000000000000000000, -84.95833333060215864, -2.886751345948128211 ) ) ;
#18398 = CARTESIAN_POINT ( 'NONE',  ( -55.35523342533222291, -135.5625000013656063, 4.444560631937231499 ) ) ;
#18399 = DIRECTION ( 'NONE',  ( 0.000000000000000000, 0.000000000000000000, 1.000000000000000000 ) ) ;
#18400 = CARTESIAN_POINT ( 'NONE',  ( -1.230605004983934782E-13, -36.75000000000000711, 5.000000000000000000 ) ) ;
#18401 = CARTESIAN_POINT ( 'NONE',  ( 9.457646018065525792E-16, -91.31249999863440792, 5.148502694627439702 ) ) ;
#18402 = CARTESIAN_POINT ( 'NONE',  ( 1.846868145590735200, -156.5000000013656347, -4.458734124999999437 ) ) ;
#18403 = CARTESIAN_POINT ( 'NONE',  ( 2.500000000000002220, -37.66666666666666430, 4.330127018922192761 ) ) ;
#18404 = CYLINDRICAL_SURFACE ( 'NONE', #8949, 5.000000000000000000 ) ;
#18405 = ORIENTED_EDGE ( 'NONE', *, *, #55792, .T. ) ;
#18406 = CARTESIAN_POINT ( 'NONE',  ( -2.229367062499996610, 16.60416666803225638, 3.861377020970582219 ) ) ;
#18407 = ORIENTED_EDGE ( 'NONE', *, *, #41590, .F. ) ;
#18408 = CARTESIAN_POINT ( 'NONE',  ( -4.458734124999999437, -95.31249999863440792, 0.000000000000000000 ) ) ;
#18409 = CARTESIAN_POINT ( 'NONE',  ( -4.458734124999999437, 9.437500001365593860, 0.000000000000000000 ) ) ;
#18410 = VECTOR ( 'NONE', #1344, 1000.000000000000000 ) ;
#18411 = CARTESIAN_POINT ( 'NONE',  ( 5.000000000000000000, 10.62500000273118594, -6.123233995736766282E-16 ) ) ;
#18412 = CARTESIAN_POINT ( 'NONE',  ( -2.500000000000000444, -88.04166666393548724, -4.330127018922193649 ) ) ;
#18413 = CARTESIAN_POINT ( 'NONE',  ( 2.500000000000002220, 5.333333333333332149, 4.330127018922192761 ) ) ;
#18414 = CARTESIAN_POINT ( 'NONE',  ( -4.458734124999999437, -59.31249999863440081, 0.000000000000000000 ) ) ;
#18415 = CARTESIAN_POINT ( 'NONE',  ( -4.999999999999999112, 4.208333336064518093, 2.886751345948131764 ) ) ;
#18416 = CARTESIAN_POINT ( 'NONE',  ( -4.458734124999999437, -26.39583333196773651, -2.574251347313719407 ) ) ;
#18417 = CARTESIAN_POINT ( 'NONE',  ( 1.339745962155612702, -40.16965819600733312, -5.000000000000000000 ) ) ;
#18418 = CARTESIAN_POINT ( 'NONE',  ( 1.339745962155615144, -63.70534180126147561, 4.999999999999999112 ) ) ;
#18419 = CARTESIAN_POINT ( 'NONE',  ( -2.071067811865308972, -151.4375000027312126, 5.000000000000169642 ) ) ;
#18420 = CARTESIAN_POINT ( 'NONE',  ( 5.000000000000000888, -44.58333333333333570, 2.886751345948126879 ) ) ;
#18422 = CARTESIAN_POINT ( 'NONE',  ( -4.458734124999998549, -18.47916666530106866, 2.574251347313722516 ) ) ;
#18421 = CARTESIAN_POINT ( 'NONE',  ( -1.339745962155618253, 24.33034180399266333, 4.999999999999996447 ) ) ;
#18423 = LINE ( 'NONE', #19360, #42967 ) ;
#18424 = CARTESIAN_POINT ( 'NONE',  ( -4.458734124999999437, -65.39583333196773651, -2.574251347313719407 ) ) ;
#18425 = CARTESIAN_POINT ( 'NONE',  ( 1.846868145590735200, -146.5000000013656347, -4.458734125000000326 ) ) ;
#18426 = CARTESIAN_POINT ( 'NONE',  ( -2.229367062499996610, -78.14583333196773651, 3.861377020970582219 ) ) ;
#18427 = CARTESIAN_POINT ( 'NONE',  ( -59.59170313451811296, -141.7500000013656063, 1.485763867205729394 ) ) ;
#18428 = CIRCLE ( 'NONE', #34866, 5.000000000000000000 ) ;
#18429 = CARTESIAN_POINT ( 'NONE',  ( -4.458734124999999437, -22.64583333196773296, -2.574251347313719407 ) ) ;
#18430 = CARTESIAN_POINT ( 'NONE',  ( 5.000000000000000000, -64.37499999726881583, -6.123233995736766282E-16 ) ) ;
#18431 = ORIENTED_EDGE ( 'NONE', *, *, #42428, .F. ) ;
#18432 = CARTESIAN_POINT ( 'NONE',  ( -2.071067811865686448, -152.8125000027312126, -4.999999999999789502 ) ) ;
#18433 = ORIENTED_EDGE ( 'NONE', *, *, #36761, .F. ) ;
#18434 = CARTESIAN_POINT ( 'NONE',  ( -4.458734124999998549, -67.47916666530106511, 2.574251347313722516 ) ) ;
#18435 = CARTESIAN_POINT ( 'NONE',  ( 3.061616997868383141E-16, -148.8750000027312126, -5.000000000000000000 ) ) ;
#18436 = CARTESIAN_POINT ( 'NONE',  ( 1.975475456537005874E-15, -12.74999999999999822, 5.000000000000000000 ) ) ;
#18437 = ORIENTED_EDGE ( 'NONE', *, *, #48806, .F. ) ;
#18438 =( BOUNDED_CURVE ( )  B_SPLINE_CURVE ( 2, ( #43827, #38383, #4597, #48348, #8803, #34180, #58324, #23607, #15205 ),
 .UNSPECIFIED., .F., .F. ) 
 B_SPLINE_CURVE_WITH_KNOTS ( ( 3, 2, 2, 2, 3 ),
 ( 0.2083333333333335091, 0.2125000000000001610, 0.2166666666666668406, 0.2208333333333335202, 0.2250000000000001998 ),
 .UNSPECIFIED. ) 
 CURVE ( )  GEOMETRIC_REPRESENTATION_ITEM ( )  RATIONAL_B_SPLINE_CURVE ( ( 0.9999999999999970024, 0.9238795325112897361, 1.000000000000000000, 0.9238795325112867385, 1.000000000000000000, 0.9238795325112867385, 1.000000000000000000, 0.9238795325112831858, 1.000000000000003553 ) ) 
 REPRESENTATION_ITEM ( '' )  );
#18439 = CARTESIAN_POINT ( 'NONE',  ( -5.000000000000000000, -3.000000000000002665, 0.000000000000000000 ) ) ;
#18441 = ADVANCED_FACE ( 'NONE', ( #40151 ), #59794, .T. ) ;
#18440 = CARTESIAN_POINT ( 'NONE',  ( -4.458734124999999437, -54.64583333196774362, -2.574251347313719407 ) ) ;
#18442 = CARTESIAN_POINT ( 'NONE',  ( 2.229367062500001939, 1.770833334698927786, 3.861377020970579999 ) ) ;
#18443 = EDGE_LOOP ( 'NONE', ( #38143, #38476, #30191, #22012 ) ) ;
#18444 = LINE ( 'NONE', #48025, #55293 ) ;
#18445 = CARTESIAN_POINT ( 'NONE',  ( -4.458734124999998549, 3.770833334698929562, 2.574251347313722516 ) ) ;
#18446 = CARTESIAN_POINT ( 'NONE',  ( -2.229367062499996610, 18.85416666803225993, 3.861377020970582219 ) ) ;
#18447 = CARTESIAN_POINT ( 'NONE',  ( -50.40829686548195099, -147.0000000013655779, -1.485763867205728284 ) ) ;
#18448 = CARTESIAN_POINT ( 'NONE',  ( 2.499999999999998668, -92.20833333060214443, -4.330127018922193649 ) ) ;
#18449 = CARTESIAN_POINT ( 'NONE',  ( 3.152801135295366208, -165.5625000013656063, 3.152801135295367985 ) ) ;
#18450 = EDGE_LOOP ( 'NONE', ( #7894, #50386, #39664, #10567 ) ) ;
#18451 = ORIENTED_EDGE ( 'NONE', *, *, #10688, .F. ) ;
#18452 = CARTESIAN_POINT ( 'NONE',  ( -4.458734124999997661, -77.22916666530106511, 2.574251347313722516 ) ) ;
#18453 = EDGE_CURVE ( 'NONE', #25022, #13616, #18611, .T. ) ;
#18454 = CARTESIAN_POINT ( 'NONE',  ( 1.975475456537005874E-15, -39.75000000000000000, 5.000000000000000000 ) ) ;
#18455 = CARTESIAN_POINT ( 'NONE',  ( -4.458734124999999437, 6.604166668032259047, -2.574251347313719407 ) ) ;
#18456 = AXIS2_PLACEMENT_3D ( 'NONE', #52894, #28127, #3701 ) ;
#18457 = FACE_OUTER_BOUND ( 'NONE', #35853, .T. ) ;
#18458 = CARTESIAN_POINT ( 'NONE',  ( -4.458734124999999437, -58.64583333196774362, -2.574251347313719407 ) ) ;
#18459 = CARTESIAN_POINT ( 'NONE',  ( -2.499999999999996447, -18.70833333060214798, 4.330127018922195425 ) ) ;
#18460 = EDGE_CURVE ( 'NONE', #29728, #13416, #56871, .T. ) ;
#18461 = CARTESIAN_POINT ( 'NONE',  ( 1.339745962155612702, -96.16965819600731891, -5.000000000000000000 ) ) ;
#18462 = CARTESIAN_POINT ( 'NONE',  ( 2.500000000000002220, -42.54166666393548013, 4.330127018922192761 ) ) ;
#18463 = CARTESIAN_POINT ( 'NONE',  ( -6.972266317189433020E-16, -15.12499999726881050, -5.000000000000000000 ) ) ;
#18464 = CARTESIAN_POINT ( 'NONE',  ( -9.184850993605147944E-16, -156.2500000000000000, 5.000000000000000000 ) ) ;
#18465 = CARTESIAN_POINT ( 'NONE',  ( -5.000000000000000888, -159.5625000000000853, -2.071067811865475949 ) ) ;
#18466 = CARTESIAN_POINT ( 'NONE',  ( 4.458734124999999437, -40.81249999863440081, -5.460374474430324690E-16 ) ) ;
#18467 =( BOUNDED_CURVE ( )  B_SPLINE_CURVE ( 2, ( #47062, #32899, #21986, #52524, #51575, #41579, #28066, #7513, #8148 ),
 .UNSPECIFIED., .F., .F. ) 
 B_SPLINE_CURVE_WITH_KNOTS ( ( 3, 2, 2, 2, 3 ),
 ( 0.5562500000000000222, 0.5569444444444444642, 0.5583333333333333481, 0.5597222222222222321, 0.5604166666666666741 ),
 .UNSPECIFIED. ) 
 CURVE ( )  GEOMETRIC_REPRESENTATION_ITEM ( )  RATIONAL_B_SPLINE_CURVE ( ( 0.9330127018922194093, 0.9330127018922194093, 1.000000000000000000, 0.8660254037844387076, 1.000000000000000000, 0.8660254037844387076, 1.000000000000000000, 0.9330127018922194093, 0.9330127018922194093 ) ) 
 REPRESENTATION_ITEM ( '' )  );
#18468 = CARTESIAN_POINT ( 'NONE',  ( -4.458734124999999437, -28.56249999863440081, 0.000000000000000000 ) ) ;
#18469 = DIRECTION ( 'NONE',  ( -0.000000000000000000, 1.000000000000000000, -0.000000000000000000 ) ) ;
#18470 = CARTESIAN_POINT ( 'NONE',  ( 5.000000000000000000, 25.50000000000000000, -6.123233995736766282E-16 ) ) ;
#18471 = CARTESIAN_POINT ( 'NONE',  ( 5.000000000000000888, -152.0625000027311842, -2.071067811865475505 ) ) ;
#18472 = ORIENTED_EDGE ( 'NONE', *, *, #10679, .T. ) ;
#18473 = CARTESIAN_POINT ( 'NONE',  ( -2.229367062500000163, -105.7291666653010651, -3.861377020970580443 ) ) ;
#18474 = CARTESIAN_POINT ( 'NONE',  ( 2.229367062499998831, -30.64583333196773651, -3.861377020970580887 ) ) ;
#18475 = CARTESIAN_POINT ( 'NONE',  ( 5.000000000000000888, -70.45833333060214443, 2.886751345948126879 ) ) ;
#18476 = CARTESIAN_POINT ( 'NONE',  ( -59.44456063193725015, -147.8125000013656063, -0.3552334253322034230 ) ) ;
#18477 = CARTESIAN_POINT ( 'NONE',  ( -2.071067811865478170, -143.3125000000000000, 5.000000000000000000 ) ) ;
#18478 = CARTESIAN_POINT ( 'NONE',  ( -4.458734124999999437, -28.31249999863440081, 0.000000000000000000 ) ) ;
#18479 = CARTESIAN_POINT ( 'NONE',  ( -3.152548672688508926E-16, -73.81249999863440792, -5.148502694627439702 ) ) ;
#18480 = CARTESIAN_POINT ( 'NONE',  ( -53.33387254593751692, -136.8125000000000284, 5.149110718188503633 ) ) ;
#18481 = CARTESIAN_POINT ( 'NONE',  ( -4.458734124999997661, -29.22916666530107221, 2.574251347313722516 ) ) ;
#18482 = CYLINDRICAL_SURFACE ( 'NONE', #47135, 5.000000000000000000 ) ;
#18483 = CARTESIAN_POINT ( 'NONE',  ( 5.000000000000000000, 22.70833333606451632, -2.886751345948130876 ) ) ;
#18484 = CARTESIAN_POINT ( 'NONE',  ( -2.499999999999996447, -21.83333333333332860, 4.330127018922195425 ) ) ;
#18485 = CARTESIAN_POINT ( 'NONE',  ( 1.846868145590735200, -146.2500000013656063, -4.458734125000000326 ) ) ;
#18486 = ORIENTED_EDGE ( 'NONE', *, *, #62834, .T. ) ;
#18487 = CARTESIAN_POINT ( 'NONE',  ( 1.975475456537005874E-15, -102.6249999972688158, 5.000000000000000000 ) ) ;
#18488 = CARTESIAN_POINT ( 'NONE',  ( 4.458734124999999437, -59.06249999863440081, -5.460374474430324690E-16 ) ) ;
#18489 = CARTESIAN_POINT ( 'NONE',  ( -5.000000000000000000, 25.04166666939785557, -2.886751345948128211 ) ) ;
#18490 =( BOUNDED_CURVE ( )  B_SPLINE_CURVE ( 2, ( #18454, #3046, #33247, #43200, #22664, #61903, #8491, #8181, #37759 ),
 .UNSPECIFIED., .F., .F. ) 
 B_SPLINE_CURVE_WITH_KNOTS ( ( 3, 2, 2, 2, 3 ),
 ( 0.5812500000000000444, 0.5819444444444444864, 0.5833333333333333703, 0.5847222222222222543, 0.5854166666666666963 ),
 .UNSPECIFIED. ) 
 CURVE ( )  GEOMETRIC_REPRESENTATION_ITEM ( )  RATIONAL_B_SPLINE_CURVE ( ( 0.9330127018922194093, 0.9330127018922194093, 1.000000000000000000, 0.8660254037844387076, 1.000000000000000000, 0.8660254037844387076, 1.000000000000000000, 0.9330127018922194093, 0.9330127018922194093 ) ) 
 REPRESENTATION_ITEM ( '' )  );
#18491 = CARTESIAN_POINT ( 'NONE',  ( -1.339745962155610925, -110.6696581960073189, 5.000000000000000000 ) ) ;
#18492 = CARTESIAN_POINT ( 'NONE',  ( -5.000000000000000000, 20.91666666666666785, -2.886751345948128211 ) ) ;
#18493 = EDGE_CURVE ( 'NONE', #42348, #61074, #42462, .T. ) ;
#18494 = DIRECTION ( 'NONE',  ( -0.000000000000000000, 1.000000000000000000, -0.000000000000000000 ) ) ;
#18495 = CARTESIAN_POINT ( 'NONE',  ( 2.229367062500001939, 0.02083333469892964529, 3.861377020970579999 ) ) ;
#18496 = CARTESIAN_POINT ( 'NONE',  ( 5.000000000000000888, 28.41666666666666430, 2.886751345948126879 ) ) ;
#18497 = DIRECTION ( 'NONE',  ( -0.000000000000000000, 1.000000000000000000, -0.000000000000000000 ) ) ;
#18498 = CARTESIAN_POINT ( 'NONE',  ( -4.458734124999999437, 8.354166668032261711, -2.574251347313719407 ) ) ;
#18499 = EDGE_CURVE ( 'NONE', #27206, #11807, #7665, .T. ) ;
#18500 = DIRECTION ( 'NONE',  ( 0.000000000000000000, 0.000000000000000000, 1.000000000000000000 ) ) ;
#18501 = ORIENTED_EDGE ( 'NONE', *, *, #50054, .T. ) ;
#18502 = CARTESIAN_POINT ( 'NONE',  ( -4.999999999999998224, -23.79166666393548368, 2.886751345948131764 ) ) ;
#18503 = CARTESIAN_POINT ( 'NONE',  ( -4.458734124999998549, -51.22916666530107221, 2.574251347313722516 ) ) ;
#18504 = CARTESIAN_POINT ( 'NONE',  ( 2.730187237215162345E-16, -158.4375000013655779, -4.458734124999999437 ) ) ;
#18505 = AXIS2_PLACEMENT_3D ( 'NONE', #50856, #6800, #42455 ) ;
#18506 = CARTESIAN_POINT ( 'NONE',  ( -2.500000000000000444, -50.04166666393547303, -4.330127018922193649 ) ) ;
#18507 = ORIENTED_EDGE ( 'NONE', *, *, #56408, .F. ) ;
#18508 = CARTESIAN_POINT ( 'NONE',  ( 9.457646018065525792E-16, -21.06249999863440436, 5.148502694627439702 ) ) ;
#18509 = ORIENTED_EDGE ( 'NONE', *, *, #20789, .T. ) ;
#18510 = CARTESIAN_POINT ( 'NONE',  ( 0.000000000000000000, -170.0000000000000000, 5.000000000000000000 ) ) ;
#18511 = CARTESIAN_POINT ( 'NONE',  ( -1.846868145590737420, -160.7500000013655779, 4.458734124999999437 ) ) ;
#18512 = ORIENTED_EDGE ( 'NONE', *, *, #50779, .T. ) ;
#18513 = CARTESIAN_POINT ( 'NONE',  ( -2.500000000000000444, -39.04166666393548013, -4.330127018922193649 ) ) ;
#18514 = CARTESIAN_POINT ( 'NONE',  ( -60.14911071818854538, -135.0625000000000284, 1.666127454062681368 ) ) ;
#18515 = CARTESIAN_POINT ( 'NONE',  ( -4.458734124999999437, -36.56249999863440792, 0.000000000000000000 ) ) ;
#18516 = VERTEX_POINT ( 'NONE', #36929 ) ;
#18517 = EDGE_CURVE ( 'NONE', #50534, #5841, #50765, .T. ) ;
#18518 = ADVANCED_FACE ( 'NONE', ( #30828 ), #35978, .F. ) ;
#18519 = CARTESIAN_POINT ( 'NONE',  ( 4.458734124999998549, -80.72916666530106511, -2.574251347313721627 ) ) ;
#18520 = CARTESIAN_POINT ( 'NONE',  ( 4.458734124999999437, 18.18750000136559564, -5.460374474430324690E-16 ) ) ;
#18521 = CARTESIAN_POINT ( 'NONE',  ( -5.000000000000000000, -17.95833333060214798, -2.886751345948128211 ) ) ;
#18522 = EDGE_CURVE ( 'NONE', #58767, #49758, #3412, .T. ) ;
#18523 = VERTEX_POINT ( 'NONE', #50457 ) ;
#18524 = CARTESIAN_POINT ( 'NONE',  ( -54.64476657466781973, -140.0625000013656063, -4.444560631937228834 ) ) ;
#18525 = CARTESIAN_POINT ( 'NONE',  ( -4.458734124999998549, -86.47916666530107932, 2.574251347313722516 ) ) ;
#18526 = CARTESIAN_POINT ( 'NONE',  ( -53.33387254593733928, -125.9375000027312268, 5.149110718188519620 ) ) ;
#18527 = CARTESIAN_POINT ( 'NONE',  ( 5.000000000000000888, -74.45833333060214443, 2.886751345948126879 ) ) ;
#18528 = CARTESIAN_POINT ( 'NONE',  ( -4.458734124999999437, -140.1875000013656063, -5.460374474430324690E-16 ) ) ;
#18529 = CARTESIAN_POINT ( 'NONE',  ( 5.000000000000000000, -145.1875000027312410, 2.071067811865478614 ) ) ;
#18530 = CARTESIAN_POINT ( 'NONE',  ( 9.457646018065525792E-16, -59.06249999863440792, 5.148502694627439702 ) ) ;
#18531 = CARTESIAN_POINT ( 'NONE',  ( -2.500000000000000444, -85.04166666393547303, -4.330127018922193649 ) ) ;
#18532 = CARTESIAN_POINT ( 'NONE',  ( -4.458734124999999437, 23.60416666803225993, -2.574251347313719407 ) ) ;
#18533 = EDGE_CURVE ( 'NONE', #1494, #49961, #31765, .T. ) ;
#18534 = FACE_OUTER_BOUND ( 'NONE', #29184, .T. ) ;
#18535 = DIRECTION ( 'NONE',  ( -0.000000000000000000, 1.000000000000000000, -0.000000000000000000 ) ) ;
#18536 = CARTESIAN_POINT ( 'NONE',  ( -2.229367062499996610, -44.39583333196774362, 3.861377020970582219 ) ) ;
#18537 = CARTESIAN_POINT ( 'NONE',  ( 2.500000000000002220, -5.541666663935480130, 4.330127018922192761 ) ) ;
#18538 = FACE_OUTER_BOUND ( 'NONE', #60438, .T. ) ;
#18539 = EDGE_CURVE ( 'NONE', #17257, #47088, #56236, .T. ) ;
#18540 = CYLINDRICAL_SURFACE ( 'NONE', #10106, 5.000000000000000000 ) ;
#18541 = CARTESIAN_POINT ( 'NONE',  ( 4.458734125000001214, -86.14583333196775072, 2.574251347313718519 ) ) ;
#18542 = CARTESIAN_POINT ( 'NONE',  ( 4.458734125000000326, -105.8958333319677365, 2.574251347313718519 ) ) ;
#18543 = CARTESIAN_POINT ( 'NONE',  ( 2.229367062499998831, -8.895833331967736513, -3.861377020970580887 ) ) ;
#18544 = ORIENTED_EDGE ( 'NONE', *, *, #50419, .F. ) ;
#18545 = CARTESIAN_POINT ( 'NONE',  ( -3.152548672688508926E-16, -99.56249999863440792, -5.148502694627439702 ) ) ;
#18546 = EDGE_CURVE ( 'NONE', #12070, #54038, #2839, .T. ) ;
#18547 = CARTESIAN_POINT ( 'NONE',  ( -9.184850993605147944E-16, -166.3750000027312126, 5.000000000000000000 ) ) ;
#18548 = CARTESIAN_POINT ( 'NONE',  ( -4.458734124999999437, -93.56249999863440792, 0.000000000000000000 ) ) ;
#18549 = CARTESIAN_POINT ( 'NONE',  ( -5.000000000000000000, -53.87499999726880162, 0.000000000000000000 ) ) ;
#18550 = CARTESIAN_POINT ( 'NONE',  ( -2.499999999999996447, 19.29166666939785202, 4.330127018922195425 ) ) ;
#18551 = CARTESIAN_POINT ( 'NONE',  ( -50.70258187064364108, -128.1250000013656347, 2.196230717870141014 ) ) ;
#18552 = CARTESIAN_POINT ( 'NONE',  ( -2.229367062499996610, -11.14583333196773829, 3.861377020970582219 ) ) ;
#18553 = CARTESIAN_POINT ( 'NONE',  ( 2.229367062499998831, 9.104166668032261711, -3.861377020970580887 ) ) ;
#18554 = CARTESIAN_POINT ( 'NONE',  ( 4.458734124999998549, -60.97916666530106511, -2.574251347313721627 ) ) ;
#18555 = CARTESIAN_POINT ( 'NONE',  ( -6.972266317189433020E-16, -69.24999999999998579, -5.000000000000000000 ) ) ;
#18556 = DIRECTION ( 'NONE',  ( -0.000000000000000000, 1.000000000000000000, -0.000000000000000000 ) ) ;
#18557 = CARTESIAN_POINT ( 'NONE',  ( -4.458734124999997661, -16.22916666530107577, 2.574251347313722516 ) ) ;
#18558 = CARTESIAN_POINT ( 'NONE',  ( -6.972266317189433020E-16, 18.87500000273118772, -5.000000000000000000 ) ) ;
#18559 = ORIENTED_EDGE ( 'NONE', *, *, #1280, .T. ) ;
#18560 = CARTESIAN_POINT ( 'NONE',  ( 9.457646018065525792E-16, -42.31249999863440081, 5.148502694627439702 ) ) ;
#18561 = CARTESIAN_POINT ( 'NONE',  ( -6.972266317189433020E-16, -83.12499999726878741, -5.000000000000000000 ) ) ;
#18562 = CARTESIAN_POINT ( 'NONE',  ( 5.000000000000000000, 0.7083333360645185373, -2.886751345948130876 ) ) ;
#18563 = CARTESIAN_POINT ( 'NONE',  ( -1.339745962155613812, 26.91965820146970501, -5.000000000000000000 ) ) ;
#18564 = CARTESIAN_POINT ( 'NONE',  ( 4.458734125000001214, -86.89583333196773651, 2.574251347313718519 ) ) ;
#18565 = CARTESIAN_POINT ( 'NONE',  ( 4.458734125000001214, 26.85416666803225993, 2.574251347313718519 ) ) ;
#18566 =( BOUNDED_CURVE ( )  B_SPLINE_CURVE ( 2, ( #52466, #3886, #33459, #43418, #52145, #58220, #8403, #42797, #9017 ),
 .UNSPECIFIED., .F., .F. ) 
 B_SPLINE_CURVE_WITH_KNOTS ( ( 3, 2, 2, 2, 3 ),
 ( 0.3839285714285714524, 0.3845238095238095455, 0.3857142857142857317, 0.3869047619047619180, 0.3875000000000000111 ),
 .UNSPECIFIED. ) 
 CURVE ( )  GEOMETRIC_REPRESENTATION_ITEM ( )  RATIONAL_B_SPLINE_CURVE ( ( 0.9330127018922194093, 0.9330127018922194093, 1.000000000000000000, 0.8660254037844387076, 1.000000000000000000, 0.8660254037844387076, 1.000000000000000000, 0.9330127018922194093, 0.9330127018922194093 ) ) 
 REPRESENTATION_ITEM ( '' )  );
#18567 = CARTESIAN_POINT ( 'NONE',  ( -4.458734124999998549, 16.77083333469892779, 2.574251347313722516 ) ) ;
#18568 = LINE ( 'NONE', #33357, #21589 ) ;
#18569 = CARTESIAN_POINT ( 'NONE',  ( 0.000000000000000000, -120.0000000000000000, 0.000000000000000000 ) ) ;
#18570 = CARTESIAN_POINT ( 'NONE',  ( 9.457646018065525792E-16, -89.31249999863440792, 5.148502694627439702 ) ) ;
#18571 = CARTESIAN_POINT ( 'NONE',  ( 2.500000000000002220, -71.66666666666667140, 4.330127018922192761 ) ) ;
#18572 = CARTESIAN_POINT ( 'NONE',  ( -2.499999999999996447, 11.29166666939785202, 4.330127018922195425 ) ) ;
#18573 = ORIENTED_EDGE ( 'NONE', *, *, #30109, .T. ) ;
#18574 = CARTESIAN_POINT ( 'NONE',  ( 1.975475456537005874E-15, -79.74999999999998579, 5.000000000000000000 ) ) ;
#18575 = CARTESIAN_POINT ( 'NONE',  ( -52.53715891517739323, -144.5625000027311842, -4.819101127000233298 ) ) ;
#18577 = CARTESIAN_POINT ( 'NONE',  ( 5.000000000000000000, -26.41666666666666430, -2.886751345948129988 ) ) ;
#18576 = CARTESIAN_POINT ( 'NONE',  ( -9.184850993605147944E-16, -159.3750000027311842, 5.000000000000000000 ) ) ;
#18578 = CARTESIAN_POINT ( 'NONE',  ( 2.229367062499998831, -34.64583333196772941, -3.861377020970580887 ) ) ;
#18579 = CARTESIAN_POINT ( 'NONE',  ( -5.000000000000000000, -31.87499999726880873, 0.000000000000000000 ) ) ;
#18581 = ORIENTED_EDGE ( 'NONE', *, *, #767, .T. ) ;
#18580 = CARTESIAN_POINT ( 'NONE',  ( 2.229367062499998831, -62.64583333196774362, -3.861377020970580887 ) ) ;
#18582 = CARTESIAN_POINT ( 'NONE',  ( -59.44456063193725015, -150.8125000013656063, -0.3552334253322034230 ) ) ;
#18584 = ORIENTED_EDGE ( 'NONE', *, *, #4027, .F. ) ;
#18583 = CARTESIAN_POINT ( 'NONE',  ( -3.152548672688508926E-16, -7.812499998634405252, -5.148502694627439702 ) ) ;
#18585 = CARTESIAN_POINT ( 'NONE',  ( 5.000000000000000000, -74.50000000000000000, -6.123233995736766282E-16 ) ) ;
#18586 = CARTESIAN_POINT ( 'NONE',  ( 5.000000000000000000, 28.62500000273118417, -6.123233995736766282E-16 ) ) ;
#18587 = CARTESIAN_POINT ( 'NONE',  ( 4.458734124999998549, -56.97916666530107932, -2.574251347313721627 ) ) ;
#18588 = CARTESIAN_POINT ( 'NONE',  ( 2.499999999999998668, -81.20833333060213022, -4.330127018922193649 ) ) ;
#18590 = EDGE_LOOP ( 'NONE', ( #17025, #18809, #26900, #24521 ) ) ;
#18589 = CARTESIAN_POINT ( 'NONE',  ( 1.975475456537005874E-15, -58.62499999726880162, 5.000000000000000000 ) ) ;
#18591 = VECTOR ( 'NONE', #32891, 1000.000000000000000 ) ;
#18592 = CARTESIAN_POINT ( 'NONE',  ( -59.81910112700025905, -150.1875000000000284, -2.462841084822630311 ) ) ;
#18593 = CARTESIAN_POINT ( 'NONE',  ( -4.458734124999999437, -20.56249999863440081, 0.000000000000000000 ) ) ;
#18595 = EDGE_LOOP ( 'NONE', ( #23586, #50215, #30090, #21841 ) ) ;
#18594 = CARTESIAN_POINT ( 'NONE',  ( 9.457646018065525792E-16, -57.31249999863440081, 5.148502694627439702 ) ) ;
#18596 = ADVANCED_FACE ( 'NONE', ( #33668 ), #32410, .T. ) ;
#18597 = DIRECTION ( 'NONE',  ( 0.000000000000000000, 0.000000000000000000, 1.000000000000000000 ) ) ;
#18598 = CARTESIAN_POINT ( 'NONE',  ( -1.846868145590734756, -166.3750000013655779, -4.458734125000000326 ) ) ;
#18599 = CARTESIAN_POINT ( 'NONE',  ( 9.457646018065525792E-16, -98.31249999863440792, 5.148502694627439702 ) ) ;
#18600 = CARTESIAN_POINT ( 'NONE',  ( 1.339745962155615144, -50.58034179853029144, 4.999999999999999112 ) ) ;
#18601 = VERTEX_POINT ( 'NONE', #13424 ) ;
#18602 = CARTESIAN_POINT ( 'NONE',  ( -59.29741812935640155, -151.8750000013655779, -2.196230717870135685 ) ) ;
#18603 = CARTESIAN_POINT ( 'NONE',  ( -58.24261429053147765, -139.3750000027312126, -3.805975901505573855 ) ) ;
#18604 = CARTESIAN_POINT ( 'NONE',  ( 1.339745962155612702, -83.29465819873851729, -5.000000000000000000 ) ) ;
#18605 = CARTESIAN_POINT ( 'NONE',  ( 4.458734124999998549, -7.729166665301073103, -2.574251347313721627 ) ) ;
#18606 = CARTESIAN_POINT ( 'NONE',  ( -4.458734124999999437, -100.6458333319677365, -2.574251347313719407 ) ) ;
#18607 = CARTESIAN_POINT ( 'NONE',  ( 1.846868145590735200, -143.5000000013656063, -4.458734125000000326 ) ) ;
#18608 = CARTESIAN_POINT ( 'NONE',  ( 9.457646018065525792E-16, -27.31249999863440436, 5.148502694627439702 ) ) ;
#18609 = LINE ( 'NONE', #24699, #21129 ) ;
#18610 = CARTESIAN_POINT ( 'NONE',  ( -53.51423613279429503, -137.2500000013656063, 4.591703134518082763 ) ) ;
#18611 =( BOUNDED_CURVE ( )  B_SPLINE_CURVE ( 2, ( #1578, #26316, #46898, #2217, #40785, #51091, #42055, #60432, #12158 ),
 .UNSPECIFIED., .F., .F. ) 
 B_SPLINE_CURVE_WITH_KNOTS ( ( 3, 2, 2, 2, 3 ),
 ( 0.6937499999999999778, 0.6944444444444444198, 0.6958333333333333037, 0.6972222222222221877, 0.6979166666666666297 ),
 .UNSPECIFIED. ) 
 CURVE ( )  GEOMETRIC_REPRESENTATION_ITEM ( )  RATIONAL_B_SPLINE_CURVE ( ( 0.9330127018922194093, 0.9330127018922194093, 1.000000000000000000, 0.8660254037844387076, 1.000000000000000000, 0.8660254037844387076, 1.000000000000000000, 0.9330127018922194093, 0.9330127018922194093 ) ) 
 REPRESENTATION_ITEM ( '' )  );
#18612 = CARTESIAN_POINT ( 'NONE',  ( 4.458734125000001214, -71.14583333196773651, 2.574251347313718519 ) ) ;
#18613 = EDGE_CURVE ( 'NONE', #24693, #29631, #20303, .T. ) ;
#18614 = CARTESIAN_POINT ( 'NONE',  ( 2.499999999999998668, -21.20833333060214798, -4.330127018922193649 ) ) ;
#18615 = CARTESIAN_POINT ( 'NONE',  ( -2.500000000000000444, 16.83333333333333215, -4.330127018922193649 ) ) ;
#18616 = CARTESIAN_POINT ( 'NONE',  ( 2.499999999999998668, -68.33333333333332860, -4.330127018922193649 ) ) ;
#18617 = CARTESIAN_POINT ( 'NONE',  ( -4.458734124999999437, 4.354166668032260823, -2.574251347313719407 ) ) ;
#18618 = ORIENTED_EDGE ( 'NONE', *, *, #18015, .F. ) ;
#18619 = CARTESIAN_POINT ( 'NONE',  ( -6.972266317189433020E-16, -71.12499999726878741, -5.000000000000000000 ) ) ;
#18620 = EDGE_CURVE ( 'NONE', #43870, #18978, #38335, .T. ) ;
#18621 = CARTESIAN_POINT ( 'NONE',  ( -75.00000000000002842, 15.00000000000000000, -5.000000000000000000 ) ) ;
#18623 = CARTESIAN_POINT ( 'NONE',  ( -2.229367062499996610, -32.14583333196773651, 3.861377020970582219 ) ) ;
#18622 = CARTESIAN_POINT ( 'NONE',  ( 2.500000000000002220, -92.66666666666665719, 4.330127018922192761 ) ) ;
#18624 = LINE ( 'NONE', #58168, #58268 ) ;
#18625 = CARTESIAN_POINT ( 'NONE',  ( -4.458734124999998549, -77.47916666530106511, 2.574251347313722516 ) ) ;
#18626 = CARTESIAN_POINT ( 'NONE',  ( 4.458734124999999437, 24.93750000136559208, -5.460374474430324690E-16 ) ) ;
#18627 = CARTESIAN_POINT ( 'NONE',  ( -1.339745962155610925, -101.6696581960073473, 5.000000000000000000 ) ) ;
#18628 = CARTESIAN_POINT ( 'NONE',  ( -50.70258187064364108, -143.1250000013656063, 2.196230717870141014 ) ) ;
#18629 = EDGE_CURVE ( 'NONE', #29232, #3859, #32728, .T. ) ;
#18630 = CARTESIAN_POINT ( 'NONE',  ( -4.458734124999999437, 1.604166668032262155, -2.574251347313719407 ) ) ;
#18631 = CARTESIAN_POINT ( 'NONE',  ( 4.458734124999998549, 26.02083333469892779, -2.574251347313721627 ) ) ;
#18632 = CARTESIAN_POINT ( 'NONE',  ( 2.229367062500001939, -40.22916666530107221, 3.861377020970579999 ) ) ;
#18633 = CARTESIAN_POINT ( 'NONE',  ( 2.500000000000002220, -60.54166666393547303, 4.330127018922192761 ) ) ;
#18634 = CARTESIAN_POINT ( 'NONE',  ( -2.229367062500000163, -0.4791666653010707710, -3.861377020970580443 ) ) ;
#18635 = CARTESIAN_POINT ( 'NONE',  ( 4.458734125000000326, -25.14583333196774007, 2.574251347313718519 ) ) ;
#18636 = CARTESIAN_POINT ( 'NONE',  ( 3.152801135295367541, -154.3125000013656063, -3.152801135295367541 ) ) ;
#18637 = CARTESIAN_POINT ( 'NONE',  ( -4.458734124999998549, -69.22916666530107932, 2.574251347313722516 ) ) ;
#18638 = CARTESIAN_POINT ( 'NONE',  ( 1.060575238724906964E-15, -101.6249999972688158, 5.773502691896257311 ) ) ;
#18639 = DIRECTION ( 'NONE',  ( -0.000000000000000000, 1.000000000000000000, -0.000000000000000000 ) ) ;
#18640 = CARTESIAN_POINT ( 'NONE',  ( -5.000000000000000000, -64.08333333333332860, -2.886751345948128211 ) ) ;
#18641 = CARTESIAN_POINT ( 'NONE',  ( -2.229367062500000163, -106.7291666653010651, -3.861377020970580443 ) ) ;
#18642 = CARTESIAN_POINT ( 'NONE',  ( 4.458734124999998549, -69.97916666530107932, -2.574251347313721627 ) ) ;
#18643 = CARTESIAN_POINT ( 'NONE',  ( 2.500000000000002220, -53.66666666666667140, 4.330127018922192761 ) ) ;
#18644 = FACE_OUTER_BOUND ( 'NONE', #34297, .T. ) ;
#18645 = CARTESIAN_POINT ( 'NONE',  ( -2.499999999999996447, 27.29166666939785202, 4.330127018922195425 ) ) ;
#18646 = ORIENTED_EDGE ( 'NONE', *, *, #43284, .F. ) ;
#18647 = AXIS2_PLACEMENT_3D ( 'NONE', #12738, #51983, #7925 ) ;
#18648 = CARTESIAN_POINT ( 'NONE',  ( -5.000000000000000000, -110.4374999986343937, 0.000000000000000000 ) ) ;
#18649 = CARTESIAN_POINT ( 'NONE',  ( 5.000000000000000888, -10.58333333333333393, 2.886751345948126879 ) ) ;
#18650 = CARTESIAN_POINT ( 'NONE',  ( 2.229367062500001939, -16.97916666530106866, 3.861377020970579999 ) ) ;
#18651 = CARTESIAN_POINT ( 'NONE',  ( 4.458734124999999437, -76.81249999863440792, -5.460374474430324690E-16 ) ) ;
#18652 = CARTESIAN_POINT ( 'NONE',  ( 1.339745962155615144, -59.58034179853028434, 4.999999999999999112 ) ) ;
#18653 = CARTESIAN_POINT ( 'NONE',  ( 5.000000000000000888, -17.45833333060214443, 2.886751345948126879 ) ) ;
#18655 = ORIENTED_EDGE ( 'NONE', *, *, #54347, .F. ) ;
#18654 = CARTESIAN_POINT ( 'NONE',  ( -4.458734124999999437, -46.39583333196774362, -2.574251347313719407 ) ) ;
#18656 = CARTESIAN_POINT ( 'NONE',  ( 5.000000000000000000, -15.37499999726881228, -6.123233995736766282E-16 ) ) ;
#18658 = ORIENTED_EDGE ( 'NONE', *, *, #51133, .T. ) ;
#18657 = CARTESIAN_POINT ( 'NONE',  ( 2.229367062500001939, 6.770833334698928674, 3.861377020970579999 ) ) ;
#18659 = CARTESIAN_POINT ( 'NONE',  ( -54.64476657466781973, -151.8125000013656063, -4.444560631937228834 ) ) ;
#18660 = CARTESIAN_POINT ( 'NONE',  ( 2.500000000000002220, -61.66666666666666430, 4.330127018922192761 ) ) ;
#18661 = CARTESIAN_POINT ( 'NONE',  ( 2.730187237215162345E-16, -155.4375000013655779, -4.458734124999999437 ) ) ;
#18662 = CARTESIAN_POINT ( 'NONE',  ( -4.458734124999999437, -38.64583333196772941, -2.574251347313719407 ) ) ;
#18663 =( BOUNDED_CURVE ( )  B_SPLINE_CURVE ( 2, ( #61592, #17195, #37145, #32621, #52247, #12375, #27790, #7556, #46471 ),
 .UNSPECIFIED., .F., .F. ) 
 B_SPLINE_CURVE_WITH_KNOTS ( ( 3, 2, 2, 2, 3 ),
 ( 0.2916666666666669072, 0.2958333333333335591, 0.3000000000000002665, 0.3041666666666669183, 0.3083333333333336257 ),
 .UNSPECIFIED. ) 
 CURVE ( )  GEOMETRIC_REPRESENTATION_ITEM ( )  RATIONAL_B_SPLINE_CURVE ( ( 0.9999999999999958922, 0.9238795325112908463, 1.000000000000000000, 0.9238795325112867385, 1.000000000000000000, 0.9238795325112867385, 1.000000000000000000, 0.9238795325112816315, 1.000000000000005107 ) ) 
 REPRESENTATION_ITEM ( '' )  );
#18664 = CARTESIAN_POINT ( 'NONE',  ( 5.000000000000000888, -165.9375000000000000, -2.071067811865475505 ) ) ;
#18665 = CARTESIAN_POINT ( 'NONE',  ( 2.500000000000002220, -11.66666666666666607, 4.330127018922192761 ) ) ;
#18666 = CARTESIAN_POINT ( 'NONE',  ( -54.64476657466781973, -131.0625000013656063, -4.444560631937228834 ) ) ;
#18667 = CARTESIAN_POINT ( 'NONE',  ( -4.458734124999998549, -6.479166665301073103, 2.574251347313722516 ) ) ;
#18668 = CARTESIAN_POINT ( 'NONE',  ( -4.458734124999998549, -40.47916666530107221, 2.574251347313722516 ) ) ;
#18669 = ADVANCED_FACE ( 'NONE', ( #27895 ), #63262, .T. ) ;
#18670 = CARTESIAN_POINT ( 'NONE',  ( -3.152801135295367985, -149.8125000013655779, 3.152801135295367096 ) ) ;
#18671 = CARTESIAN_POINT ( 'NONE',  ( -2.229367062500000163, -85.72916666530107932, -3.861377020970580443 ) ) ;
#18672 = CARTESIAN_POINT ( 'NONE',  ( 1.339745962155612702, -34.16965819600732601, -5.000000000000000000 ) ) ;
#18673 = ORIENTED_EDGE ( 'NONE', *, *, #51136, .F. ) ;
#18674 = CARTESIAN_POINT ( 'NONE',  ( 5.000000000000000000, -43.41666666666666430, -2.886751345948130876 ) ) ;
#18675 = CARTESIAN_POINT ( 'NONE',  ( 4.458734125000001214, -74.14583333196773651, 2.574251347313718519 ) ) ;
#18676 = ORIENTED_EDGE ( 'NONE', *, *, #24057, .F. ) ;
#18677 = DIRECTION ( 'NONE',  ( 0.000000000000000000, 0.000000000000000000, -1.000000000000000000 ) ) ;
#18678 = CARTESIAN_POINT ( 'NONE',  ( -4.458734124999999437, -11.56249999863440792, 0.000000000000000000 ) ) ;
#18679 = DIRECTION ( 'NONE',  ( 0.000000000000000000, 0.000000000000000000, 1.000000000000000000 ) ) ;
#18680 = CARTESIAN_POINT ( 'NONE',  ( -2.229367062499996610, 1.854166668032262377, 3.861377020970582219 ) ) ;
#18681 = CARTESIAN_POINT ( 'NONE',  ( -1.339745962155610925, -42.79465819873851729, 5.000000000000000000 ) ) ;
#18682 = CARTESIAN_POINT ( 'NONE',  ( 3.152801135295367541, -151.3125000013655779, -3.152801135295367541 ) ) ;
#18683 = CARTESIAN_POINT ( 'NONE',  ( 9.457646018065525792E-16, 23.68750000136559564, 5.148502694627439702 ) ) ;
#18684 = VERTEX_POINT ( 'NONE', #23719 ) ;
#18685 = CARTESIAN_POINT ( 'NONE',  ( -4.458734124999999437, -92.39583333196773651, -2.574251347313719407 ) ) ;
#18686 = CARTESIAN_POINT ( 'NONE',  ( -1.339745962155613812, -47.20534180126147561, -5.000000000000000000 ) ) ;
#18687 = CARTESIAN_POINT ( 'NONE',  ( 7.922281120364393914, -4.573931137438282057, -8.047472243342932430 ) ) ;
#18688 = CARTESIAN_POINT ( 'NONE',  ( -4.458734124999999437, -8.312499998634406140, 0.000000000000000000 ) ) ;
#18689 = CARTESIAN_POINT ( 'NONE',  ( 5.000000000000000888, -39.45833333060214443, 2.886751345948126879 ) ) ;
#18690 = CARTESIAN_POINT ( 'NONE',  ( 2.499999999999998668, -23.20833333060214443, -4.330127018922193649 ) ) ;
#18691 = CARTESIAN_POINT ( 'NONE',  ( -59.59170313451811296, -152.5000000013655779, 1.485763867205729394 ) ) ;
#18692 = CARTESIAN_POINT ( 'NONE',  ( -2.499999999999996447, -38.70833333060213732, 4.330127018922195425 ) ) ;
#18693 = CARTESIAN_POINT ( 'NONE',  ( -6.972266317189433020E-16, -64.12499999726880162, -5.000000000000000000 ) ) ;
#18694 = CARTESIAN_POINT ( 'NONE',  ( -2.229367062500000163, 19.52083333469893134, -3.861377020970580443 ) ) ;
#18695 = CARTESIAN_POINT ( 'NONE',  ( 1.249999999999999112, -7.938566201357367902, -7.198902722707431145 ) ) ;
#18696 = CARTESIAN_POINT ( 'NONE',  ( 4.458734125000000326, 24.10416666803225993, 2.574251347313718519 ) ) ;
#18697 = CARTESIAN_POINT ( 'NONE',  ( 4.458734125000001214, -57.89583333196773651, 2.574251347313718519 ) ) ;
#18698 = CARTESIAN_POINT ( 'NONE',  ( 4.458734125000000326, -11.14583333196773829, 2.574251347313718519 ) ) ;
#18699 = DIRECTION ( 'NONE',  ( -0.000000000000000000, 1.000000000000000000, -0.000000000000000000 ) ) ;
#18700 = CARTESIAN_POINT ( 'NONE',  ( -5.000000000000000000, 10.91666666666666607, -2.886751345948128211 ) ) ;
#18701 = CARTESIAN_POINT ( 'NONE',  ( 1.846868145590735200, -168.2500000013656063, -4.458734125000000326 ) ) ;
#18702 = CARTESIAN_POINT ( 'NONE',  ( 2.499999999999998668, -69.33333333333332860, -4.330127018922193649 ) ) ;
#18703 = CARTESIAN_POINT ( 'NONE',  ( 2.229367062499998831, -46.64583333196774362, -3.861377020970580887 ) ) ;
#18704 = CARTESIAN_POINT ( 'NONE',  ( -5.000000000000000000, -82.87499999726881583, 0.000000000000000000 ) ) ;
#18705 = CARTESIAN_POINT ( 'NONE',  ( -54.64476657466781973, -134.0625000013656063, -4.444560631937228834 ) ) ;
#18706 = CARTESIAN_POINT ( 'NONE',  ( -6.972266317189433020E-16, -17.25000000000000000, -5.000000000000000000 ) ) ;
#18707 = CARTESIAN_POINT ( 'NONE',  ( -1.339745962155610925, -91.79465819873853150, 5.000000000000000000 ) ) ;
#18708 = CARTESIAN_POINT ( 'NONE',  ( 4.458734124999999437, -91.06249999863440792, -5.460374474430324690E-16 ) ) ;
#18709 = CARTESIAN_POINT ( 'NONE',  ( -4.458734124999999437, -158.1875000013655779, -5.460374474430324690E-16 ) ) ;
#18710 = CARTESIAN_POINT ( 'NONE',  ( 1.060575238724906964E-15, -40.74999999999999289, 5.773502691896257311 ) ) ;
#18711 = SURFACE_SIDE_STYLE ('',( #32884 ) ) ;
#18712 = ORIENTED_EDGE ( 'NONE', *, *, #12228, .F. ) ;
#18713 = CARTESIAN_POINT ( 'NONE',  ( -59.54425679209026612, -135.0000000000000284, 1.880628494755099522 ) ) ;
#18714 = ORIENTED_EDGE ( 'NONE', *, *, #37498, .F. ) ;
#18715 = CARTESIAN_POINT ( 'NONE',  ( -3.152548672688508926E-16, -94.56249999863440792, -5.148502694627439702 ) ) ;
#18716 = CARTESIAN_POINT ( 'NONE',  ( -4.458734124999999437, 10.43750000136559386, 0.000000000000000000 ) ) ;
#18717 = CARTESIAN_POINT ( 'NONE',  ( -5.000000000000000000, 11.12500000273118594, 0.000000000000000000 ) ) ;
#18718 = CARTESIAN_POINT ( 'NONE',  ( 2.500000000000002220, -80.66666666666665719, 4.330127018922192761 ) ) ;
#18719 = CARTESIAN_POINT ( 'NONE',  ( -5.000000000000000000, 3.916666666666665630, -2.886751345948128211 ) ) ;
#18720 = ADVANCED_FACE ( 'NONE', ( #33050 ), #3468, .T. ) ;
#18721 = CARTESIAN_POINT ( 'NONE',  ( 2.229367062500001939, -60.97916666530106511, 3.861377020970579999 ) ) ;
#18722 = CARTESIAN_POINT ( 'NONE',  ( -1.339745962155610925, -39.79465819873851729, 5.000000000000000000 ) ) ;
#18723 = CARTESIAN_POINT ( 'NONE',  ( 5.000000000000000000, 1.625000002731184834, -6.123233995736766282E-16 ) ) ;
#18724 = CARTESIAN_POINT ( 'NONE',  ( 4.458734124999998549, -29.72916666530107221, -2.574251347313721627 ) ) ;
#18725 = CARTESIAN_POINT ( 'NONE',  ( -2.499999999999996447, -41.83333333333333570, 4.330127018922195425 ) ) ;
#18726 = CARTESIAN_POINT ( 'NONE',  ( 2.500000000000002220, -19.66666666666666430, 4.330127018922192761 ) ) ;
#18727 = CARTESIAN_POINT ( 'NONE',  ( -4.999999999999999112, -42.91666666666665719, 2.886751345948131764 ) ) ;
#18729 = CARTESIAN_POINT ( 'NONE',  ( 4.458734125000001214, -21.14583333196774362, 2.574251347313718519 ) ) ;
#18728 = CARTESIAN_POINT ( 'NONE',  ( -6.972266317189433020E-16, -19.12499999726880873, -5.000000000000000000 ) ) ;
#18730 = CARTESIAN_POINT ( 'NONE',  ( -1.339745962155606929, 21.91965820146970501, -5.000000000000004441 ) ) ;
#18731 = CARTESIAN_POINT ( 'NONE',  ( -3.152548672688508926E-16, -70.56249999863439371, -5.148502694627439702 ) ) ;
#18732 = CARTESIAN_POINT ( 'NONE',  ( 3.152801135295366208, -149.8125000013655779, 3.152801135295367985 ) ) ;
#18733 = CARTESIAN_POINT ( 'NONE',  ( 4.458734124999998549, -77.72916666530106511, -2.574251347313721627 ) ) ;
#18734 = CARTESIAN_POINT ( 'NONE',  ( -55.35523342533222291, -141.5625000013656063, 4.444560631937231499 ) ) ;
#18735 =( BOUNDED_CURVE ( )  B_SPLINE_CURVE ( 2, ( #34397, #35697, #49205, #11239, #30863, #24444, #15441, #5145, #39860 ),
 .UNSPECIFIED., .F., .F. ) 
 B_SPLINE_CURVE_WITH_KNOTS ( ( 3, 2, 2, 2, 3 ),
 ( 0.1053571428571428575, 0.1059523809523809507, 0.1071428571428571369, 0.1083333333333333370, 0.1089285714285714302 ),
 .UNSPECIFIED. ) 
 CURVE ( )  GEOMETRIC_REPRESENTATION_ITEM ( )  RATIONAL_B_SPLINE_CURVE ( ( 0.9330127018922194093, 0.9330127018922194093, 1.000000000000000000, 0.8660254037844387076, 1.000000000000000000, 0.8660254037844387076, 1.000000000000000000, 0.9330127018922194093, 0.9330127018922194093 ) ) 
 REPRESENTATION_ITEM ( '' )  );
#18736 = CARTESIAN_POINT ( 'NONE',  ( 4.458734125000001214, -23.14583333196773651, 2.574251347313718519 ) ) ;
#18737 = CARTESIAN_POINT ( 'NONE',  ( 2.500000000000002220, -66.54166666393547303, 4.330127018922192761 ) ) ;
#18738 = ORIENTED_EDGE ( 'NONE', *, *, #60858, .F. ) ;
#18739 = CARTESIAN_POINT ( 'NONE',  ( -1.339745962155610925, -21.79465819873851729, 5.000000000000000000 ) ) ;
#18740 = VERTEX_POINT ( 'NONE', #19181 ) ;
#18741 = CARTESIAN_POINT ( 'NONE',  ( 4.458734124999998549, -66.97916666530107932, -2.574251347313721627 ) ) ;
#18742 = CARTESIAN_POINT ( 'NONE',  ( 1.975475456537005874E-15, 8.375000002731187720, 5.000000000000000000 ) ) ;
#18743 = ORIENTED_EDGE ( 'NONE', *, *, #32681, .F. ) ;
#18744 = FACE_OUTER_BOUND ( 'NONE', #40475, .T. ) ;
#18745 = CARTESIAN_POINT ( 'NONE',  ( -4.458734124999998549, -55.47916666530107221, 2.574251347313722516 ) ) ;
#18746 = CARTESIAN_POINT ( 'NONE',  ( 4.458734124999999437, 1.937500001365593416, -5.460374474430324690E-16 ) ) ;
#18747 = VERTEX_POINT ( 'NONE', #38794 ) ;
#18748 =( BOUNDED_CURVE ( )  B_SPLINE_CURVE ( 2, ( #20834, #7632, #61345, #27547, #17597, #16956, #56199, #22425, #12756 ),
 .UNSPECIFIED., .F., .F. ) 
 B_SPLINE_CURVE_WITH_KNOTS ( ( 3, 2, 2, 2, 3 ),
 ( 0.2145833333333333481, 0.2152777777777777901, 0.2166666666666666741, 0.2180555555555555580, 0.2187500000000000000 ),
 .UNSPECIFIED. ) 
 CURVE ( )  GEOMETRIC_REPRESENTATION_ITEM ( )  RATIONAL_B_SPLINE_CURVE ( ( 0.9330127018922194093, 0.9330127018922207416, 1.000000000000000000, 0.8660254037844387076, 1.000000000000000000, 0.8660254037844387076, 1.000000000000000000, 0.9330127018922194093, 0.9330127018922194093 ) ) 
 REPRESENTATION_ITEM ( '' )  );
#18749 = CARTESIAN_POINT ( 'NONE',  ( 2.493747252781420335E-13, -55.24999999999999289, -5.000000000000000000 ) ) ;
#18750 = CARTESIAN_POINT ( 'NONE',  ( -2.229367062500000163, 19.52083333469893134, -3.861377020970580443 ) ) ;
#18751 = CARTESIAN_POINT ( 'NONE',  ( -51.60603307380591787, -146.9375000013656063, -2.891590998281053704 ) ) ;
#18752 = CARTESIAN_POINT ( 'NONE',  ( -51.75738570946856498, -155.0000000000000284, 3.805975901505577408 ) ) ;
#18753 = CARTESIAN_POINT ( 'NONE',  ( 3.152801135295367541, -164.3125000013656063, -3.152801135295367541 ) ) ;
#18754 = VERTEX_POINT ( 'NONE', #52663 ) ;
#18755 = CARTESIAN_POINT ( 'NONE',  ( -3.152548672688508926E-16, -77.56249999863440792, -5.148502694627439702 ) ) ;
#18756 = CARTESIAN_POINT ( 'NONE',  ( 0.000000000000000000, -120.0000000000000000, 0.000000000000000000 ) ) ;
#18757 = CARTESIAN_POINT ( 'NONE',  ( 2.229367062500001939, 8.020833334698926009, 3.861377020970579999 ) ) ;
#18758 = CARTESIAN_POINT ( 'NONE',  ( 1.975475456537005874E-15, -40.62499999726879452, 5.000000000000000000 ) ) ;
#18759 = CARTESIAN_POINT ( 'NONE',  ( -2.229367062500000163, -57.72916666530107932, -3.861377020970580443 ) ) ;
#18760 = CARTESIAN_POINT ( 'NONE',  ( -3.535250795749689387E-16, -22.12499999726881228, -5.773502691896257311 ) ) ;
#18761 = CARTESIAN_POINT ( 'NONE',  ( -60.14911071818854538, -142.0625000000000000, 1.666127454062681146 ) ) ;
#18762 = CARTESIAN_POINT ( 'NONE',  ( 1.975475456537005874E-15, -58.75000000000000000, 5.000000000000000000 ) ) ;
#18763 = CARTESIAN_POINT ( 'NONE',  ( -4.999999999999998224, -105.7916666639354588, 2.886751345948131764 ) ) ;
#18764 = CARTESIAN_POINT ( 'NONE',  ( -50.01589407740564042, -146.6250000000000284, 0.3983568153799778022 ) ) ;
#18765 = CARTESIAN_POINT ( 'NONE',  ( -4.458734124999999437, -40.31249999863440081, 0.000000000000000000 ) ) ;
#18766 = CARTESIAN_POINT ( 'NONE',  ( -4.458734124999997661, -24.47916666530107577, 2.574251347313722516 ) ) ;
#18767 = CYLINDRICAL_SURFACE ( 'NONE', #55662, 5.000000000000000000 ) ;
#18768 = CARTESIAN_POINT ( 'NONE',  ( 1.060575238724906964E-15, 27.25000000000000000, 5.773502691896257311 ) ) ;
#18769 = CARTESIAN_POINT ( 'NONE',  ( -5.000000000000000000, -154.6250000027311842, -6.123233995736766282E-16 ) ) ;
#18770 = ORIENTED_EDGE ( 'NONE', *, *, #44085, .F. ) ;
#18771 = CARTESIAN_POINT ( 'NONE',  ( 2.229367062499998831, -105.8958333319677365, -3.861377020970580887 ) ) ;
#18772 = CARTESIAN_POINT ( 'NONE',  ( 4.458734124999998549, -32.72916666530107221, -2.574251347313721627 ) ) ;
#18773 = CARTESIAN_POINT ( 'NONE',  ( -3.535250795749689387E-16, -67.12499999726881583, -5.773502691896257311 ) ) ;
#18774 = CARTESIAN_POINT ( 'NONE',  ( -50.55543936806279248, -148.3125000013656063, 0.3552334253322060320 ) ) ;
#18775 = CARTESIAN_POINT ( 'NONE',  ( -5.000000000000000888, -144.4375000000000284, 2.071067811865474617 ) ) ;
#18776 = CARTESIAN_POINT ( 'NONE',  ( -2.229367062500000163, -75.72916666530106511, -3.861377020970580443 ) ) ;
#18777 = CARTESIAN_POINT ( 'NONE',  ( 3.152801135295367541, -169.5625000013656063, -3.152801135295367541 ) ) ;
#18778 = CARTESIAN_POINT ( 'NONE',  ( 4.458734124999999437, -29.81249999863440436, -5.460374474430324690E-16 ) ) ;
#18779 = DIRECTION ( 'NONE',  ( -1.000000000000000000, 0.000000000000000000, -0.000000000000000000 ) ) ;
#18780 = CARTESIAN_POINT ( 'NONE',  ( 5.000000000000000888, -5.458333330602148870, 2.886751345948126879 ) ) ;
#18781 = CARTESIAN_POINT ( 'NONE',  ( 5.000000000000000888, -23.58333333333333215, 2.886751345948126879 ) ) ;
#18782 = CARTESIAN_POINT ( 'NONE',  ( -3.152801135295367985, -146.8125000013655779, 3.152801135295367096 ) ) ;
#18783 = ORIENTED_EDGE ( 'NONE', *, *, #449, .T. ) ;
#18784 = CARTESIAN_POINT ( 'NONE',  ( -4.458734124999999437, -57.56249999863440081, 0.000000000000000000 ) ) ;
#18785 = CARTESIAN_POINT ( 'NONE',  ( 5.000000000000000000, 24.62500000273118417, -6.123233995736766282E-16 ) ) ;
#18786 = CARTESIAN_POINT ( 'NONE',  ( 2.499999999999998668, -48.20833333060215153, -4.330127018922193649 ) ) ;
#18787 = CARTESIAN_POINT ( 'NONE',  ( -5.000000000000000000, 16.91666666666666430, -2.886751345948128211 ) ) ;
#18788 = EDGE_CURVE ( 'NONE', #19094, #63269, #3155, .T. ) ;
#18789 = CARTESIAN_POINT ( 'NONE',  ( -6.972266317189433020E-16, -84.12499999726880162, -5.000000000000000000 ) ) ;
#18790 = CARTESIAN_POINT ( 'NONE',  ( -2.229367062499996610, -6.145833331967740953, 3.861377020970582219 ) ) ;
#18791 = CARTESIAN_POINT ( 'NONE',  ( -1.975475456537005874E-15, 28.25000000000000000, 5.000000000000000000 ) ) ;
#18792 = FACE_OUTER_BOUND ( 'NONE', #49989, .T. ) ;
#18793 = CARTESIAN_POINT ( 'NONE',  ( -4.458734124999998549, 12.52083333469892779, 2.574251347313722516 ) ) ;
#18794 = CARTESIAN_POINT ( 'NONE',  ( 0.000000000000000000, -120.0000000000000000, 5.000000000000000000 ) ) ;
#18795 = ORIENTED_EDGE ( 'NONE', *, *, #28315, .F. ) ;
#18796 =( BOUNDED_CURVE ( )  B_SPLINE_CURVE ( 2, ( #48590, #13568, #43448, #34421, #23535, #354, #24470, #29599, #8737 ),
 .UNSPECIFIED., .F., .F. ) 
 B_SPLINE_CURVE_WITH_KNOTS ( ( 3, 2, 2, 2, 3 ),
 ( 0.5732142857142856762, 0.5738095238095237693, 0.5749999999999999556, 0.5761904761904761418, 0.5767857142857142350 ),
 .UNSPECIFIED. ) 
 CURVE ( )  GEOMETRIC_REPRESENTATION_ITEM ( )  RATIONAL_B_SPLINE_CURVE ( ( 0.9330127018922194093, 0.9330127018922194093, 1.000000000000000000, 0.8660254037844387076, 1.000000000000000000, 0.8660254037844387076, 1.000000000000000000, 0.9330127018922194093, 0.9330127018922194093 ) ) 
 REPRESENTATION_ITEM ( '' )  );
#18797 = CARTESIAN_POINT ( 'NONE',  ( -1.339745962155610925, -71.66965819600733312, 5.000000000000000000 ) ) ;
#18798 = CARTESIAN_POINT ( 'NONE',  ( 2.229367062500001939, -46.97916666530106511, 3.861377020970579999 ) ) ;
#18799 = CARTESIAN_POINT ( 'NONE',  ( -8.190561711645485556E-16, -160.9375000013655779, 4.458734124999999437 ) ) ;
#18800 = EDGE_CURVE ( 'NONE', #63519, #41293, #27726, .T. ) ;
#18801 = CARTESIAN_POINT ( 'NONE',  ( 5.000000000000000000, -49.37499999726880873, -6.123233995736766282E-16 ) ) ;
#18802 = ORIENTED_EDGE ( 'NONE', *, *, #39652, .F. ) ;
#18804 = EDGE_CURVE ( 'NONE', #24403, #58682, #18568, .T. ) ;
#18803 = CARTESIAN_POINT ( 'NONE',  ( 4.458734124999998549, -23.72916666530107221, -2.574251347313721627 ) ) ;
#18805 = ORIENTED_EDGE ( 'NONE', *, *, #13105, .T. ) ;
#18807 = CARTESIAN_POINT ( 'NONE',  ( 5.000000000000000000, -170.0000000000000000, 0.000000000000000000 ) ) ;
#18806 = DIRECTION ( 'NONE',  ( -0.000000000000000000, 1.000000000000000000, -0.000000000000000000 ) ) ;
#18808 = CARTESIAN_POINT ( 'NONE',  ( -1.846868145590734756, -159.1250000013656063, -4.458734125000000326 ) ) ;
#18809 = ORIENTED_EDGE ( 'NONE', *, *, #32997, .F. ) ;
#18810 = CARTESIAN_POINT ( 'NONE',  ( -5.000000000000000000, -38.87499999726880162, 0.000000000000000000 ) ) ;
#18811 = CARTESIAN_POINT ( 'NONE',  ( -51.19402409849444524, -133.5000000000000284, -3.242614290531456334 ) ) ;
#18812 = CARTESIAN_POINT ( 'NONE',  ( -2.500000000000000444, -59.04166666393546592, -4.330127018922193649 ) ) ;
#18813 = CARTESIAN_POINT ( 'NONE',  ( 2.229367062500001939, -37.22916666530107221, 3.861377020970579999 ) ) ;
#18814 = ORIENTED_EDGE ( 'NONE', *, *, #45086, .T. ) ;
#18815 = EDGE_CURVE ( 'NONE', #50284, #62586, #47822, .T. ) ;
#18816 = CIRCLE ( 'NONE', #53758, 7.500000000000001776 ) ;
#18817 = CARTESIAN_POINT ( 'NONE',  ( -4.458734124999999437, -84.31249999863439371, 0.000000000000000000 ) ) ;
#18818 = CARTESIAN_POINT ( 'NONE',  ( -4.458734124999998549, 16.77083333469892779, 2.574251347313722516 ) ) ;
#18819 = DIRECTION ( 'NONE',  ( 0.000000000000000000, 1.000000000000000000, 0.000000000000000000 ) ) ;
#18820 = ORIENTED_EDGE ( 'NONE', *, *, #7570, .T. ) ;
#18821 = CARTESIAN_POINT ( 'NONE',  ( -50.40829686548195099, -137.2500000013656063, -1.485763867205728284 ) ) ;
#18822 = CARTESIAN_POINT ( 'NONE',  ( -2.229367062499996610, -87.39583333196773651, 3.861377020970582219 ) ) ;
#18823 = CARTESIAN_POINT ( 'NONE',  ( -51.75738570946856498, -124.8750000027312126, 3.805975901505576964 ) ) ;
#18824 = CARTESIAN_POINT ( 'NONE',  ( 2.500000000000002220, -74.54166666393547303, 4.330127018922192761 ) ) ;
#18825 = CARTESIAN_POINT ( 'NONE',  ( -50.51982268314063873, -135.0000000000000000, 1.105932492512590404 ) ) ;
#18826 = CARTESIAN_POINT ( 'NONE',  ( 1.975475456537005874E-15, -13.62499999726881228, 5.000000000000000000 ) ) ;
#18827 = CARTESIAN_POINT ( 'NONE',  ( -4.458734124999999437, -62.31249999863440792, 0.000000000000000000 ) ) ;
#18828 = LINE ( 'NONE', #29101, #37656 ) ;
#18829 = CARTESIAN_POINT ( 'NONE',  ( 4.458734124999999437, 25.18750000136559208, -5.460374474430324690E-16 ) ) ;
#18830 = CARTESIAN_POINT ( 'NONE',  ( -2.499999999999996447, -109.8333333333333428, 4.330127018922195425 ) ) ;
#18831 = CARTESIAN_POINT ( 'NONE',  ( 0.000000000000000000, 0.000000000000000000, 0.000000000000000000 ) ) ;
#18832 = CARTESIAN_POINT ( 'NONE',  ( 4.458734124999999437, -42.06249999863440081, -5.460374474430324690E-16 ) ) ;
#18833 = EDGE_CURVE ( 'NONE', #4271, #50284, #51872, .T. ) ;
#18834 = CARTESIAN_POINT ( 'NONE',  ( -2.499999999999996447, -1.708333330602145761, 4.330127018922195425 ) ) ;
#18835 = CARTESIAN_POINT ( 'NONE',  ( -1.127183054612291972E-14, 25.24999999999999645, 4.999999999999999112 ) ) ;
#18836 = FACE_OUTER_BOUND ( 'NONE', #23353, .T. ) ;
#18837 = CARTESIAN_POINT ( 'NONE',  ( -2.229367062500000163, -83.72916666530106511, -3.861377020970580443 ) ) ;
#18838 = CARTESIAN_POINT ( 'NONE',  ( -2.229367062499996610, -109.1458333319677365, 3.861377020970582219 ) ) ;
#18839 = CARTESIAN_POINT ( 'NONE',  ( 4.458734125000000326, -9.145833331967736513, 2.574251347313718519 ) ) ;
#18840 = ORIENTED_EDGE ( 'NONE', *, *, #32707, .F. ) ;
#18841 = CARTESIAN_POINT ( 'NONE',  ( 3.061616997868383141E-16, -163.8750000027311842, -5.000000000000000000 ) ) ;
#18842 = CARTESIAN_POINT ( 'NONE',  ( 2.229367062499998831, -96.64583333196773651, -3.861377020970580887 ) ) ;
#18843 = CARTESIAN_POINT ( 'NONE',  ( -2.071067811865475061, -163.8125000027311842, -5.000000000000000888 ) ) ;
#18844 = CARTESIAN_POINT ( 'NONE',  ( 4.458734124999999437, -92.06249999863440792, -5.460374474430324690E-16 ) ) ;
#18845 = CARTESIAN_POINT ( 'NONE',  ( 2.500000000000002220, -53.54166666393548013, 4.330127018922192761 ) ) ;
#18846 = CARTESIAN_POINT ( 'NONE',  ( 0.000000000000000000, -120.0000000000000000, 0.000000000000000000 ) ) ;
#18847 = CARTESIAN_POINT ( 'NONE',  ( -50.40829686548195099, -131.0000000013656063, -1.485763867205728284 ) ) ;
#18848 = CARTESIAN_POINT ( 'NONE',  ( -52.10840900171896806, -146.1875000013656063, 3.393966926194110556 ) ) ;
#18849 = CARTESIAN_POINT ( 'NONE',  ( 9.457646018065525792E-16, -14.06249999863440436, 5.148502694627439702 ) ) ;
#18850 = CARTESIAN_POINT ( 'NONE',  ( 2.229367062499998831, 13.10416666803226171, -3.861377020970580887 ) ) ;
#18851 = CARTESIAN_POINT ( 'NONE',  ( 4.458734124999998549, -59.97916666530106511, -2.574251347313721627 ) ) ;
#18852 = DIRECTION ( 'NONE',  ( 0.000000000000000000, 0.000000000000000000, 1.000000000000000000 ) ) ;
#18853 = CARTESIAN_POINT ( 'NONE',  ( 5.000000000000000000, 3.583333333333333925, -2.886751345948130876 ) ) ;
#18854 = CARTESIAN_POINT ( 'NONE',  ( -3.152548672688508926E-16, -13.56249999863440259, -5.148502694627439702 ) ) ;
#18855 = DIRECTION ( 'NONE',  ( 0.000000000000000000, 0.000000000000000000, 1.000000000000000000 ) ) ;
#18856 = ORIENTED_EDGE ( 'NONE', *, *, #18517, .T. ) ;
#18857 = CARTESIAN_POINT ( 'NONE',  ( -4.458734124999999437, -42.64583333196773651, -2.574251347313719407 ) ) ;
#18858 = CARTESIAN_POINT ( 'NONE',  ( 0.000000000000000000, -170.0000000000000000, 5.000000000000000000 ) ) ;
#18859 = FACE_OUTER_BOUND ( 'NONE', #5811, .T. ) ;
#18860 = CARTESIAN_POINT ( 'NONE',  ( -1.339745962155613812, -67.08034179853029855, -5.000000000000000000 ) ) ;
#18861 = CARTESIAN_POINT ( 'NONE',  ( 4.458734125000001214, -87.89583333196773651, 2.574251347313718519 ) ) ;
#18862 = CARTESIAN_POINT ( 'NONE',  ( -2.229367062499996610, 17.60416666803225993, 3.861377020970582219 ) ) ;
#18863 = EDGE_CURVE ( 'NONE', #30019, #51834, #44914, .T. ) ;
#18864 = AXIS2_PLACEMENT_3D ( 'NONE', #5721, #270, #588 ) ;
#18865 = CARTESIAN_POINT ( 'NONE',  ( -2.229367062499996610, 14.85416666803226171, 3.861377020970582219 ) ) ;
#18866 = EDGE_CURVE ( 'NONE', #20917, #1494, #984, .T. ) ;
#18867 = EDGE_CURVE ( 'NONE', #61933, #5022, #1189, .T. ) ;
#18868 = CARTESIAN_POINT ( 'NONE',  ( 0.000000000000000000, -170.0000000000000000, 5.000000000000000000 ) ) ;
#18869 = CARTESIAN_POINT ( 'NONE',  ( -51.75738570946856498, -137.8750000027312126, 3.805975901505576964 ) ) ;
#18870 = CARTESIAN_POINT ( 'NONE',  ( -4.458734124999999437, -86.64583333196773651, -2.574251347313719407 ) ) ;
#18871 = CARTESIAN_POINT ( 'NONE',  ( 5.000000000000000888, -69.58333333333332860, 2.886751345948126879 ) ) ;
#18872 = CARTESIAN_POINT ( 'NONE',  ( 2.499999999999998668, 13.79166666939785202, -4.330127018922193649 ) ) ;
#18873 = VERTEX_POINT ( 'NONE', #20148 ) ;
#18874 = LINE ( 'NONE', #38491, #37654 ) ;
#18875 = PRODUCT ( 'crossbar', 'crossbar', '', ( #566 ) ) ;
#18876 = ORIENTED_EDGE ( 'NONE', *, *, #54347, .T. ) ;
#18877 = CARTESIAN_POINT ( 'NONE',  ( 5.000000000000000000, -167.0000000000000000, 0.000000000000000000 ) ) ;
#18879 = CARTESIAN_POINT ( 'NONE',  ( -2.500000000000000444, -31.16666666666666785, -4.330127018922193649 ) ) ;
#18878 = FACE_OUTER_BOUND ( 'NONE', #31348, .T. ) ;
#18880 = CARTESIAN_POINT ( 'NONE',  ( 2.229367062499998831, -33.64583333196772941, -3.861377020970580887 ) ) ;
#18881 = EDGE_CURVE ( 'NONE', #34481, #13658, #9958, .T. ) ;
#18882 = CARTESIAN_POINT ( 'NONE',  ( -5.000000000000000000, -35.87499999726881583, 0.000000000000000000 ) ) ;
#18884 = ORIENTED_EDGE ( 'NONE', *, *, #16667, .T. ) ;
#18883 = CARTESIAN_POINT ( 'NONE',  ( -2.229367062499996610, -58.14583333196773651, 3.861377020970582219 ) ) ;
#18885 = CARTESIAN_POINT ( 'NONE',  ( -55.35523342533222291, -150.5625000013656063, 4.444560631937231499 ) ) ;
#18886 = EDGE_CURVE ( 'NONE', #57924, #42260, #7542, .T. ) ;
#18888 = VERTEX_POINT ( 'NONE', #5031 ) ;
#18887 = CARTESIAN_POINT ( 'NONE',  ( -4.458734124999999437, -14.64583333196773474, -2.574251347313719407 ) ) ;
#18889 = CARTESIAN_POINT ( 'NONE',  ( -5.000000000000000000, -79.08333333333331439, -2.886751345948128211 ) ) ;
#18890 = CARTESIAN_POINT ( 'NONE',  ( -75.00000000000000000, 0.000000000000000000, 8.999999999999998224 ) ) ;
#18891 = CARTESIAN_POINT ( 'NONE',  ( 4.458734124999999437, -57.06249999863440081, -5.460374474430324690E-16 ) ) ;
#18892 = CARTESIAN_POINT ( 'NONE',  ( 2.500000000000002220, -83.54166666393547303, 4.330127018922192761 ) ) ;
#18894 = ORIENTED_EDGE ( 'NONE', *, *, #32619, .T. ) ;
#18893 = CARTESIAN_POINT ( 'NONE',  ( 5.000000000000000888, -13.58333333333333570, 2.886751345948126879 ) ) ;
#18895 = CARTESIAN_POINT ( 'NONE',  ( -51.19402409849444524, -144.5000000000000284, -3.242614290531456334 ) ) ;
#18896 = CARTESIAN_POINT ( 'NONE',  ( -2.229367062499996610, -23.39583333196773651, 3.861377020970582219 ) ) ;
#18898 = ORIENTED_EDGE ( 'NONE', *, *, #27101, .F. ) ;
#18897 = CARTESIAN_POINT ( 'NONE',  ( -4.458734124999999437, -60.56249999863440081, 0.000000000000000000 ) ) ;
#18899 = DIRECTION ( 'NONE',  ( -0.6485228581062916220, 0.000000000000000000, 0.7611951803011147710 ) ) ;
#18900 = CARTESIAN_POINT ( 'NONE',  ( -1.846868145590737420, -165.0000000013655779, 4.458734124999999437 ) ) ;
#18901 = CARTESIAN_POINT ( 'NONE',  ( -4.458734124999999437, -102.6458333319677507, -2.574251347313719407 ) ) ;
#18902 = CARTESIAN_POINT ( 'NONE',  ( -2.500000000000000444, 17.83333333333333215, -4.330127018922193649 ) ) ;
#18903 = ORIENTED_EDGE ( 'NONE', *, *, #44439, .T. ) ;
#18904 = CARTESIAN_POINT ( 'NONE',  ( -59.29741812935640155, -150.8750000013656063, -2.196230717870135685 ) ) ;
#18905 = CARTESIAN_POINT ( 'NONE',  ( -51.19402409849444524, -140.6250000027312126, -3.242614290531456334 ) ) ;
#18906 = CARTESIAN_POINT ( 'NONE',  ( 9.457646018065525792E-16, -40.06249999863440081, 5.148502694627439702 ) ) ;
#18907 = LINE ( 'NONE', #38522, #43474 ) ;
#18908 = CARTESIAN_POINT ( 'NONE',  ( 4.458734124999999437, -13.81249999863440259, -5.460374474430324690E-16 ) ) ;
#18909 = CARTESIAN_POINT ( 'NONE',  ( -2.229367062499996610, -100.3958333319677365, 3.861377020970582219 ) ) ;
#18910 = CIRCLE ( 'NONE', #17870, 5.000000000000000888 ) ;
#18911 = CARTESIAN_POINT ( 'NONE',  ( 4.458734125000000326, -142.6250000013655779, -1.846868145590734978 ) ) ;
#18912 = CARTESIAN_POINT ( 'NONE',  ( -3.152548672688508926E-16, -30.81249999863440436, -5.148502694627439702 ) ) ;
#18913 = DIRECTION ( 'NONE',  ( -0.000000000000000000, 1.000000000000000000, -0.000000000000000000 ) ) ;
#18914 = CARTESIAN_POINT ( 'NONE',  ( -59.44456063193725015, -131.5625000013656063, -0.3552334253322034230 ) ) ;
#18915 = CARTESIAN_POINT ( 'NONE',  ( -4.458734124999999437, -67.64583333196773651, -2.574251347313719407 ) ) ;
#18916 = DIRECTION ( 'NONE',  ( -0.000000000000000000, 1.000000000000000000, -0.000000000000000000 ) ) ;
#18917 = CARTESIAN_POINT ( 'NONE',  ( 1.975475456537005874E-15, 7.375000002731185944, 5.000000000000000000 ) ) ;
#18918 = CARTESIAN_POINT ( 'NONE',  ( 4.458734124999997661, -141.5000000013655779, 1.846868145590737864 ) ) ;
#18919 = CARTESIAN_POINT ( 'NONE',  ( -4.458734124999997661, 3.520833334698929118, 2.574251347313722516 ) ) ;
#18920 = ORIENTED_EDGE ( 'NONE', *, *, #54966, .F. ) ;
#18921 = CARTESIAN_POINT ( 'NONE',  ( 3.061616997868383141E-16, -159.7500000000000000, -5.000000000000000000 ) ) ;
#18923 = CARTESIAN_POINT ( 'NONE',  ( -4.458734124999999437, -29.31249999863440436, 0.000000000000000000 ) ) ;
#18922 = CARTESIAN_POINT ( 'NONE',  ( -2.500000000000000444, -96.16666666666665719, -4.330127018922193649 ) ) ;
#18924 = CARTESIAN_POINT ( 'NONE',  ( -5.000000000000000000, 7.041666669397852019, -2.886751345948128211 ) ) ;
#18925 = CARTESIAN_POINT ( 'NONE',  ( -4.458734124999999437, -76.56249999863440792, 0.000000000000000000 ) ) ;
#18926 = CARTESIAN_POINT ( 'NONE',  ( -3.152548672688508926E-16, 25.18750000136558853, -5.148502694627439702 ) ) ;
#18927 =( BOUNDED_CURVE ( )  B_SPLINE_CURVE ( 2, ( #63457, #48331, #29324, #9407, #18439, #4906, #9719, #19376, #53786 ),
 .UNSPECIFIED., .F., .F. ) 
 B_SPLINE_CURVE_WITH_KNOTS ( ( 3, 2, 2, 2, 3 ),
 ( 0.2729166666666666963, 0.2736111111111111382, 0.2750000000000000222, 0.2763888888888889062, 0.2770833333333333481 ),
 .UNSPECIFIED. ) 
 CURVE ( )  GEOMETRIC_REPRESENTATION_ITEM ( )  RATIONAL_B_SPLINE_CURVE ( ( 0.9330127018922194093, 0.9330127018922220739, 1.000000000000000000, 0.8660254037844387076, 1.000000000000000000, 0.8660254037844387076, 1.000000000000000000, 0.9330127018922194093, 0.9330127018922194093 ) ) 
 REPRESENTATION_ITEM ( '' )  );
#18928 = CARTESIAN_POINT ( 'NONE',  ( -50.55543936806279248, -143.0625000013656063, 0.3552334253322060320 ) ) ;
#18929 = CARTESIAN_POINT ( 'NONE',  ( -4.458734124999999437, 3.687500001365594748, 0.000000000000000000 ) ) ;
#18930 = CARTESIAN_POINT ( 'NONE',  ( -4.458734124999999437, 26.35416666803226349, -2.574251347313719407 ) ) ;
#18931 = CARTESIAN_POINT ( 'NONE',  ( -4.458734124999997661, -44.47916666530106511, 2.574251347313722516 ) ) ;
#18932 = CARTESIAN_POINT ( 'NONE',  ( 5.000000000000000000, -80.50000000000000000, -6.123233995736766282E-16 ) ) ;
#18933 = CARTESIAN_POINT ( 'NONE',  ( 4.458734125000000326, 1.104166668032261711, 2.574251347313718519 ) ) ;
#18934 = CARTESIAN_POINT ( 'NONE',  ( 4.458734124999998549, -26.97916666530107221, -2.574251347313721627 ) ) ;
#18935 = CARTESIAN_POINT ( 'NONE',  ( 1.846868145590736310, -156.6250000013655779, 4.458734124999999437 ) ) ;
#18936 = CARTESIAN_POINT ( 'NONE',  ( -2.229367062499996610, -69.14583333196773651, 3.861377020970582219 ) ) ;
#18937 = CARTESIAN_POINT ( 'NONE',  ( -5.000000000000000000, -103.8749999972688158, 0.000000000000000000 ) ) ;
#18938 = CARTESIAN_POINT ( 'NONE',  ( -51.75738570946856498, -148.7500000000000284, 3.805975901505576964 ) ) ;
#18939 = EDGE_CURVE ( 'NONE', #24503, #31719, #25284, .T. ) ;
#18940 = CARTESIAN_POINT ( 'NONE',  ( -6.972266317189433020E-16, -92.12499999726878741, -5.000000000000000000 ) ) ;
#18941 = CARTESIAN_POINT ( 'NONE',  ( 2.229367062500001939, -107.2291666653010651, 3.861377020970579999 ) ) ;
#18942 = CARTESIAN_POINT ( 'NONE',  ( 2.229367062500001939, -73.22916666530107932, 3.861377020970579999 ) ) ;
#18943 = CARTESIAN_POINT ( 'NONE',  ( -5.000000000000000000, -55.99999999999999289, 0.000000000000000000 ) ) ;
#18944 = FACE_OUTER_BOUND ( 'NONE', #39615, .T. ) ;
#18945 = ORIENTED_EDGE ( 'NONE', *, *, #30823, .F. ) ;
#18946 = DIRECTION ( 'NONE',  ( -0.000000000000000000, 1.000000000000000000, -0.000000000000000000 ) ) ;
#18947 = EDGE_CURVE ( 'NONE', #5972, #50310, #40396, .T. ) ;
#18948 = CARTESIAN_POINT ( 'NONE',  ( 2.499999999999998668, -27.20833333060214798, -4.330127018922193649 ) ) ;
#18949 = CARTESIAN_POINT ( 'NONE',  ( -3.535250795749689387E-16, -14.25000000000000178, -5.773502691896257311 ) ) ;
#18950 = CARTESIAN_POINT ( 'NONE',  ( -4.458734124999999437, -19.31249999863440081, 0.000000000000000000 ) ) ;
#18951 = ADVANCED_FACE ( 'NONE', ( #40070 ), #59712, .T. ) ;
#18952 = CARTESIAN_POINT ( 'NONE',  ( 4.458734124999998549, -75.72916666530106511, -2.574251347313721627 ) ) ;
#18953 = EDGE_CURVE ( 'NONE', #11945, #10944, #22763, .T. ) ;
#18954 = CARTESIAN_POINT ( 'NONE',  ( 2.730187237215162345E-16, -169.4375000013656063, -4.458734124999999437 ) ) ;
#18955 = CARTESIAN_POINT ( 'NONE',  ( 5.000000000000000000, -19.29166666393548013, -2.886751345948129988 ) ) ;
#18957 = ORIENTED_EDGE ( 'NONE', *, *, #10548, .T. ) ;
#18956 = CARTESIAN_POINT ( 'NONE',  ( -4.458734124999998549, -43.22916666530105800, 2.574251347313722516 ) ) ;
#18958 = CARTESIAN_POINT ( 'NONE',  ( 5.000000000000000888, -98.58333333333332860, 2.886751345948126879 ) ) ;
#18960 = ORIENTED_EDGE ( 'NONE', *, *, #44729, .T. ) ;
#18959 = CARTESIAN_POINT ( 'NONE',  ( 2.229367062500001939, 2.770833334698928674, 3.861377020970579999 ) ) ;
#18961 = CARTESIAN_POINT ( 'NONE',  ( -51.60603307380591787, -153.9375000013656063, -2.891590998281053704 ) ) ;
#18962 = CARTESIAN_POINT ( 'NONE',  ( -5.000000000000000000, -62.00000000000000000, 0.000000000000000000 ) ) ;
#18963 = EDGE_CURVE ( 'NONE', #7158, #24525, #16597, .T. ) ;
#18964 = CARTESIAN_POINT ( 'NONE',  ( -4.458734125000001214, -155.1250000013655779, 1.846868145590734089 ) ) ;
#18965 = CARTESIAN_POINT ( 'NONE',  ( -2.229367062500000163, -41.72916666530107932, -3.861377020970580443 ) ) ;
#18966 = CARTESIAN_POINT ( 'NONE',  ( -4.999999999999998224, -55.91666666666667140, 2.886751345948131764 ) ) ;
#18967 = CARTESIAN_POINT ( 'NONE',  ( 3.535533905932738197, -163.8750000000000284, -3.535533905932738197 ) ) ;
#18968 = EDGE_CURVE ( 'NONE', #26333, #25814, #29290, .T. ) ;
#18969 = CARTESIAN_POINT ( 'NONE',  ( -51.60603307380591787, -127.1875000013656063, -2.891590998281053704 ) ) ;
#18970 = CARTESIAN_POINT ( 'NONE',  ( 4.458734125000001214, -6.145833331967741842, 2.574251347313718519 ) ) ;
#18971 = CARTESIAN_POINT ( 'NONE',  ( -2.229367062500000163, -38.72916666530107221, -3.861377020970580443 ) ) ;
#18972 = EDGE_CURVE ( 'NONE', #38824, #28871, #35903, .T. ) ;
#18973 = CARTESIAN_POINT ( 'NONE',  ( 3.061616997868383141E-16, -151.8750000027311842, -5.000000000000000000 ) ) ;
#18974 = CARTESIAN_POINT ( 'NONE',  ( 2.730187237215162345E-16, -149.1875000013656063, -4.458734124999999437 ) ) ;
#18975 = CARTESIAN_POINT ( 'NONE',  ( 2.229367062499998831, -90.89583333196773651, -3.861377020970580887 ) ) ;
#18976 = CARTESIAN_POINT ( 'NONE',  ( -58.24261429053147765, -143.2500000000000284, -3.805975901505573855 ) ) ;
#18977 =( BOUNDED_CURVE ( )  B_SPLINE_CURVE ( 2, ( #39300, #63454, #19372, #45093, #50236, #21614, #25470, #20664, #35768 ),
 .UNSPECIFIED., .F., .F. ) 
 B_SPLINE_CURVE_WITH_KNOTS ( ( 3, 2, 2, 2, 3 ),
 ( 0.05625000000000000139, 0.05694444444444444337, 0.05833333333333333426, 0.05972222222222222515, 0.06041666666666666713 ),
 .UNSPECIFIED. ) 
 CURVE ( )  GEOMETRIC_REPRESENTATION_ITEM ( )  RATIONAL_B_SPLINE_CURVE ( ( 0.9330127018922192983, 0.9330127018922196314, 1.000000000000000000, 0.8660254037844387076, 1.000000000000000000, 0.8660254037844387076, 1.000000000000000000, 0.9330127018922194093, 0.9330127018922194093 ) ) 
 REPRESENTATION_ITEM ( '' )  );
#18978 = VERTEX_POINT ( 'NONE', #60675 ) ;
#18979 = CARTESIAN_POINT ( 'NONE',  ( 3.061616997868383141E-16, -154.8750000027311842, -5.000000000000000000 ) ) ;
#18980 = CARTESIAN_POINT ( 'NONE',  ( -54.60164318462004474, -149.5000000027312126, -4.984105922594373794 ) ) ;
#18981 =( BOUNDED_CURVE ( )  B_SPLINE_CURVE ( 2, ( #13282, #57050, #42546, #62185, #18105, #36462, #56089, #47690, #48626 ),
 .UNSPECIFIED., .F., .F. ) 
 B_SPLINE_CURVE_WITH_KNOTS ( ( 3, 2, 2, 2, 3 ),
 ( 0.6267857142857142794, 0.6273809523809523725, 0.6285714285714285587, 0.6297619047619047450, 0.6303571428571428381 ),
 .UNSPECIFIED. ) 
 CURVE ( )  GEOMETRIC_REPRESENTATION_ITEM ( )  RATIONAL_B_SPLINE_CURVE ( ( 0.9330127018922194093, 0.9330127018922194093, 1.000000000000000000, 0.8660254037844387076, 1.000000000000000000, 0.8660254037844387076, 1.000000000000000000, 0.9330127018922194093, 0.9330127018922194093 ) ) 
 REPRESENTATION_ITEM ( '' )  );
#18982 = CARTESIAN_POINT ( 'NONE',  ( -1.339745962155613812, -12.08034179853029322, -5.000000000000000000 ) ) ;
#18983 = CARTESIAN_POINT ( 'NONE',  ( 2.229367062500001939, -74.22916666530106511, 3.861377020970579999 ) ) ;
#18984 = ORIENTED_EDGE ( 'NONE', *, *, #30109, .F. ) ;
#18985 = LINE ( 'NONE', #48255, #41099 ) ;
#18986 = CARTESIAN_POINT ( 'NONE',  ( -4.458734124999999437, -13.56249999863440259, 0.000000000000000000 ) ) ;
#18987 = CARTESIAN_POINT ( 'NONE',  ( -2.229367062500000163, -0.4791666653010707710, -3.861377020970580443 ) ) ;
#18988 = CARTESIAN_POINT ( 'NONE',  ( -1.339745962155727277, -95.66965819600733312, 4.999999999999933387 ) ) ;
#18989 = CARTESIAN_POINT ( 'NONE',  ( 3.152801135295366208, -154.5625000013656063, 3.152801135295367985 ) ) ;
#18990 = CARTESIAN_POINT ( 'NONE',  ( 4.458734124999998549, 23.02083333469892423, -2.574251347313721627 ) ) ;
#18991 = ORIENTED_EDGE ( 'NONE', *, *, #16582, .F. ) ;
#18992 = CARTESIAN_POINT ( 'NONE',  ( -4.458734124999999437, -90.39583333196772230, -2.574251347313719407 ) ) ;
#18993 = CARTESIAN_POINT ( 'NONE',  ( -58.24261429053147765, -137.3750000027312126, -3.805975901505573855 ) ) ;
#18994 = CARTESIAN_POINT ( 'NONE',  ( 6.601567268551444378, -5.319966374295973743, -7.792327460285856766 ) ) ;
#18995 = CARTESIAN_POINT ( 'NONE',  ( -4.458734124999999437, -16.39583333196773651, -2.574251347313719407 ) ) ;
#18996 = CARTESIAN_POINT ( 'NONE',  ( 5.000000000000000000, -39.37499999726880162, -6.123233995736766282E-16 ) ) ;
#18997 = CARTESIAN_POINT ( 'NONE',  ( -1.339745962155613812, -73.20534180126146850, -5.000000000000000000 ) ) ;
#18998 = VECTOR ( 'NONE', #43958, 1000.000000000000000 ) ;
#18999 = CARTESIAN_POINT ( 'NONE',  ( -58.39396692619412477, -154.4375000013656063, 2.891590998281057701 ) ) ;
#19000 = CARTESIAN_POINT ( 'NONE',  ( -2.499999999999996447, -39.70833333060214443, 4.330127018922195425 ) ) ;
#19001 = DIRECTION ( 'NONE',  ( 0.000000000000000000, -0.000000000000000000, -1.000000000000000000 ) ) ;
#19002 = CARTESIAN_POINT ( 'NONE',  ( 4.458734124999998549, 18.27083333469893134, -2.574251347313721627 ) ) ;
#19003 = CARTESIAN_POINT ( 'NONE',  ( 1.339745962155615144, -44.70534180126146850, 4.999999999999999112 ) ) ;
#19004 =( BOUNDED_CURVE ( )  B_SPLINE_CURVE ( 2, ( #54875, #20784, #862, #40388, #35895, #35255, #12075, #46179, #40065 ),
 .UNSPECIFIED., .F., .F. ) 
 B_SPLINE_CURVE_WITH_KNOTS ( ( 3, 2, 2, 2, 3 ),
 ( 0.4803571428571428714, 0.4809523809523809645, 0.4821428571428571508, 0.4833333333333333370, 0.4839285714285714302 ),
 .UNSPECIFIED. ) 
 CURVE ( )  GEOMETRIC_REPRESENTATION_ITEM ( )  RATIONAL_B_SPLINE_CURVE ( ( 0.9330127018922194093, 0.9330127018922194093, 1.000000000000000000, 0.8660254037844387076, 1.000000000000000000, 0.8660254037844387076, 1.000000000000000000, 0.9330127018922194093, 0.9330127018922194093 ) ) 
 REPRESENTATION_ITEM ( '' )  );
#19005 = ORIENTED_EDGE ( 'NONE', *, *, #59025, .T. ) ;
#19006 = CARTESIAN_POINT ( 'NONE',  ( -4.458734124999999437, 18.68750000136559564, 0.000000000000000000 ) ) ;
#19007 = CARTESIAN_POINT ( 'NONE',  ( -3.152548672688508926E-16, -63.56249999863440792, -5.148502694627439702 ) ) ;
#19008 = CARTESIAN_POINT ( 'NONE',  ( 4.458734125000000326, -9.145833331967736513, 2.574251347313718519 ) ) ;
#19009 = DIRECTION ( 'NONE',  ( 1.000000000000000000, 0.000000000000000000, -0.000000000000000000 ) ) ;
#19010 = CARTESIAN_POINT ( 'NONE',  ( 5.000000000000000000, 10.49999999999999822, -6.123233995736766282E-16 ) ) ;
#19011 = CARTESIAN_POINT ( 'NONE',  ( -4.458734125000001214, -166.8750000013655779, 1.846868145590734089 ) ) ;
#19012 = CARTESIAN_POINT ( 'NONE',  ( -6.972266317189433020E-16, -9.250000000000000000, -5.000000000000000000 ) ) ;
#19013 = CARTESIAN_POINT ( 'NONE',  ( 4.458734124999998549, -55.72916666530107221, -2.574251347313721627 ) ) ;
#19014 = CARTESIAN_POINT ( 'NONE',  ( -3.535250795749689387E-16, -82.12499999726883004, -5.773502691896257311 ) ) ;
#19015 = CARTESIAN_POINT ( 'NONE',  ( -59.29741812935640155, -136.8750000013656063, -2.196230717870135685 ) ) ;
#19016 = CYLINDRICAL_SURFACE ( 'NONE', #39052, 5.000000000000000000 ) ;
#19017 = DIRECTION ( 'NONE',  ( -0.000000000000000000, 1.000000000000000000, -0.000000000000000000 ) ) ;
#19018 = CARTESIAN_POINT ( 'NONE',  ( 2.229367062499998831, -88.89583333196773651, -3.861377020970580887 ) ) ;
#19019 = CARTESIAN_POINT ( 'NONE',  ( 2.730187237215162345E-16, -155.4375000013655779, -4.458734124999999437 ) ) ;
#19020 = CARTESIAN_POINT ( 'NONE',  ( 5.000000000000000888, -38.58333333333332860, 2.886751345948126879 ) ) ;
#19021 = CARTESIAN_POINT ( 'NONE',  ( 5.000000000000000000, -98.37499999726881583, -6.123233995736766282E-16 ) ) ;
#19022 = CARTESIAN_POINT ( 'NONE',  ( 5.000000000000000000, -163.0000000000000000, 0.000000000000000000 ) ) ;
#19023 = ORIENTED_EDGE ( 'NONE', *, *, #58229, .T. ) ;
#19024 = CARTESIAN_POINT ( 'NONE',  ( -4.458734124999999437, -100.3958333319677365, -2.574251347313719407 ) ) ;
#19025 = CARTESIAN_POINT ( 'NONE',  ( 4.458734124999999437, 7.937500001365595637, -5.460374474430324690E-16 ) ) ;
#19026 = CARTESIAN_POINT ( 'NONE',  ( 5.000000000000000888, 12.54166666939785202, 2.886751345948126879 ) ) ;
#19027 =( BOUNDED_CURVE ( )  B_SPLINE_CURVE ( 2, ( #29221, #52747, #48847, #63347, #14750, #53364, #13815, #33434, #24415 ),
 .UNSPECIFIED., .F., .F. ) 
 B_SPLINE_CURVE_WITH_KNOTS ( ( 3, 2, 2, 2, 3 ),
 ( 0.4250000000000003220, 0.4291666666666669738, 0.4333333333333336812, 0.4375000000000003886, 0.4416666666666670404 ),
 .UNSPECIFIED. ) 
 CURVE ( )  GEOMETRIC_REPRESENTATION_ITEM ( )  RATIONAL_B_SPLINE_CURVE ( ( 0.9999999999999938938, 0.9238795325112928447, 1.000000000000000000, 0.9238795325112867385, 1.000000000000000000, 0.9238795325112867385, 1.000000000000000000, 0.9238795325112796331, 1.000000000000007105 ) ) 
 REPRESENTATION_ITEM ( '' )  );
#19028 = CARTESIAN_POINT ( 'NONE',  ( -2.499999999999996447, -87.70833333060214443, 4.330127018922195425 ) ) ;
#19029 = CARTESIAN_POINT ( 'NONE',  ( 5.000000000000000888, 0.4166666666666659080, 2.886751345948126879 ) ) ;
#19030 = CARTESIAN_POINT ( 'NONE',  ( -4.458734124999997661, -59.22916666530106511, 2.574251347313722516 ) ) ;
#19031 = PLANE ( 'NONE',  #2 ) ;
#19032 = CARTESIAN_POINT ( 'NONE',  ( -2.499999999999996447, -4.708333330602147981, 4.330127018922195425 ) ) ;
#19033 = CARTESIAN_POINT ( 'NONE',  ( 4.458734124999998549, -27.72916666530107221, -2.574251347313721627 ) ) ;
#19034 = CARTESIAN_POINT ( 'NONE',  ( -6.972266317189433020E-16, -42.24999999999998579, -5.000000000000000000 ) ) ;
#19035 = CARTESIAN_POINT ( 'NONE',  ( 0.000000000000000000, -120.0000000000000000, 5.000000000000000000 ) ) ;
#19036 = CARTESIAN_POINT ( 'NONE',  ( -49.85088928181150436, -136.5625000000000284, -1.666127454062680480 ) ) ;
#19037 = CARTESIAN_POINT ( 'NONE',  ( -2.500000000000000444, -43.16666666666665719, -4.330127018922193649 ) ) ;
#19039 = CARTESIAN_POINT ( 'NONE',  ( 4.458734124999998549, -26.97916666530107221, -2.574251347313721627 ) ) ;
#19038 = CARTESIAN_POINT ( 'NONE',  ( -5.000000000000000000, 24.12500000273118417, 0.000000000000000000 ) ) ;
#19040 = CARTESIAN_POINT ( 'NONE',  ( 5.000000000000000000, -4.291666663935479242, -2.886751345948130876 ) ) ;
#19041 = CARTESIAN_POINT ( 'NONE',  ( 4.458734124999999437, -67.81249999863440792, -5.460374474430324690E-16 ) ) ;
#19042 = CARTESIAN_POINT ( 'NONE',  ( -8.190561711645485556E-16, -143.9375000013656063, 4.458734124999999437 ) ) ;
#19043 = CARTESIAN_POINT ( 'NONE',  ( -3.152548672688508926E-16, -78.56249999863440792, -5.148502694627439702 ) ) ;
#19044 = CARTESIAN_POINT ( 'NONE',  ( -50.40829686548195099, -137.2500000013656063, -1.485763867205728284 ) ) ;
#19045 = VECTOR ( 'NONE', #12976, 1000.000000000000000 ) ;
#19046 = CARTESIAN_POINT ( 'NONE',  ( -4.458734124999998549, -23.47916666530107577, 2.574251347313722516 ) ) ;
#19047 = CARTESIAN_POINT ( 'NONE',  ( 5.000000000000000000, -66.37499999726881583, -6.123233995736766282E-16 ) ) ;
#19048 = EDGE_CURVE ( 'NONE', #59664, #58377, #31372, .T. ) ;
#19049 = VERTEX_POINT ( 'NONE', #30750 ) ;
#19050 = CARTESIAN_POINT ( 'NONE',  ( -53.33387254593725402, -147.9375000027312126, 5.149110718188524949 ) ) ;
#19051 = ORIENTED_EDGE ( 'NONE', *, *, #12950, .F. ) ;
#19052 = CARTESIAN_POINT ( 'NONE',  ( -4.458734124999999437, -71.64583333196773651, -2.574251347313719407 ) ) ;
#19053 = CARTESIAN_POINT ( 'NONE',  ( 5.000000000000000000, -166.0625000000000000, 2.071067811865478614 ) ) ;
#19054 = VERTEX_POINT ( 'NONE', #2451 ) ;
#19055 = CARTESIAN_POINT ( 'NONE',  ( -2.229367062499996610, -58.39583333196773651, 3.861377020970582219 ) ) ;
#19056 = CARTESIAN_POINT ( 'NONE',  ( 4.458734124999998549, -0.9791666653010713262, -2.574251347313721627 ) ) ;
#19057 = ORIENTED_EDGE ( 'NONE', *, *, #12302, .T. ) ;
#19058 = CYLINDRICAL_SURFACE ( 'NONE', #12166, 5.000000000000000000 ) ;
#19059 = CARTESIAN_POINT ( 'NONE',  ( -3.152548672688508926E-16, 14.43750000136559386, -5.148502694627439702 ) ) ;
#19060 = CARTESIAN_POINT ( 'NONE',  ( -50.55543936806279248, -146.0625000013656063, 0.3552334253322060320 ) ) ;
#19061 = CARTESIAN_POINT ( 'NONE',  ( 1.339745962155615144, -92.58034179853028434, 4.999999999999999112 ) ) ;
#19062 = CARTESIAN_POINT ( 'NONE',  ( 2.730187237215162345E-16, -163.1875000013655779, -4.458734124999999437 ) ) ;
#19063 = VERTEX_POINT ( 'NONE', #55533 ) ;
#19064 = CARTESIAN_POINT ( 'NONE',  ( -3.152548672688508926E-16, -78.56249999863440792, -5.148502694627439702 ) ) ;
#19065 = CARTESIAN_POINT ( 'NONE',  ( -5.000000000000000000, -51.95833333060214443, -2.886751345948128211 ) ) ;
#19066 = CARTESIAN_POINT ( 'NONE',  ( 2.229367062499998831, 2.354166668032262599, -3.861377020970580887 ) ) ;
#19067 = CARTESIAN_POINT ( 'NONE',  ( 1.339745962155615144, -19.58034179853029499, 4.999999999999999112 ) ) ;
#19068 = CARTESIAN_POINT ( 'NONE',  ( 4.458734124999998549, -67.97916666530107932, -2.574251347313721627 ) ) ;
#19069 = CARTESIAN_POINT ( 'NONE',  ( 5.000000000000000888, -20.45833333060214798, 2.886751345948126879 ) ) ;
#19070 = CARTESIAN_POINT ( 'NONE',  ( -53.33387254593711901, -141.8124999999999432, 5.149110718188534719 ) ) ;
#19071 = CARTESIAN_POINT ( 'NONE',  ( 2.500000000000002220, -44.54166666393547303, 4.330127018922192761 ) ) ;
#19072 = CARTESIAN_POINT ( 'NONE',  ( -5.000000000000000000, -59.08333333333332860, -2.886751345948128211 ) ) ;
#19073 = CARTESIAN_POINT ( 'NONE',  ( 1.975475456537005874E-15, 14.37500000273118417, 5.000000000000000000 ) ) ;
#19074 = CYLINDRICAL_SURFACE ( 'NONE', #31594, 5.000000000000000000 ) ;
#19075 = CARTESIAN_POINT ( 'NONE',  ( -2.229367062499996610, -41.14583333196773651, 3.861377020970582219 ) ) ;
#19076 = CARTESIAN_POINT ( 'NONE',  ( -4.458734124999999437, -24.56249999863440436, 0.000000000000000000 ) ) ;
#19077 = CARTESIAN_POINT ( 'NONE',  ( -4.458734124999999437, 6.354166668032259047, -2.574251347313719407 ) ) ;
#19078 = CARTESIAN_POINT ( 'NONE',  ( -59.98410592259440222, -144.1250000000000284, -0.3983568153799752487 ) ) ;
#19079 = CARTESIAN_POINT ( 'NONE',  ( -2.500000000000000444, 23.83333333333333215, -4.330127018922193649 ) ) ;
#19080 = CARTESIAN_POINT ( 'NONE',  ( -5.000000000000000000, -147.6250000027312126, -6.123233995736766282E-16 ) ) ;
#19081 = CARTESIAN_POINT ( 'NONE',  ( 4.458734124999999437, -107.0624999986343937, -5.460374474430324690E-16 ) ) ;
#19082 = CARTESIAN_POINT ( 'NONE',  ( 4.458734124999998549, -36.72916666530107221, -2.574251347313721627 ) ) ;
#19083 = CARTESIAN_POINT ( 'NONE',  ( -5.000000000000000000, -65.95833333060213022, -2.886751345948128211 ) ) ;
#19084 = AXIS2_PLACEMENT_3D ( 'NONE', #54770, #30634, #25170 ) ;
#19085 = CARTESIAN_POINT ( 'NONE',  ( -57.19623071787017210, -146.6250000013656063, 4.297418129356382899 ) ) ;
#19086 = CARTESIAN_POINT ( 'NONE',  ( 5.000000000000000000, -145.0000000000000284, 0.000000000000000000 ) ) ;
#19087 = CARTESIAN_POINT ( 'NONE',  ( 2.229367062500001939, -75.22916666530106511, 3.861377020970579999 ) ) ;
#19088 = CARTESIAN_POINT ( 'NONE',  ( 7.499999999999999112, -4.330127018922205195, -1.000000000000000888 ) ) ;
#19089 = CARTESIAN_POINT ( 'NONE',  ( -4.458734124999999437, -28.39583333196773651, -2.574251347313719407 ) ) ;
#19090 = DIRECTION ( 'NONE',  ( -0.000000000000000000, 1.000000000000000000, -0.000000000000000000 ) ) ;
#19091 = DIRECTION ( 'NONE',  ( 0.000000000000000000, 0.000000000000000000, 1.000000000000000000 ) ) ;
#19092 = CARTESIAN_POINT ( 'NONE',  ( -3.535250795749689387E-16, -21.24999999999999645, -5.773502691896257311 ) ) ;
#19093 = CARTESIAN_POINT ( 'NONE',  ( 1.846868145590736310, -143.6250000013655779, 4.458734124999999437 ) ) ;
#19094 = VERTEX_POINT ( 'NONE', #17228 ) ;
#19095 = CARTESIAN_POINT ( 'NONE',  ( -4.458734124999998549, 26.52083333469892779, 2.574251347313722516 ) ) ;
#19096 = CARTESIAN_POINT ( 'NONE',  ( -5.000000000000000000, -49.08333333333332860, -2.886751345948128211 ) ) ;
#19097 = CARTESIAN_POINT ( 'NONE',  ( -4.458734124999999437, -56.64583333196773651, -2.574251347313719407 ) ) ;
#19098 = CARTESIAN_POINT ( 'NONE',  ( 5.000000000000000000, 27.70833333606451987, -2.886751345948129988 ) ) ;
#19099 = LINE ( 'NONE', #48687, #50415 ) ;
#19100 = CARTESIAN_POINT ( 'NONE',  ( 5.000000000000000000, 18.50000000000000000, -6.123233995736766282E-16 ) ) ;
#19101 =( BOUNDED_CURVE ( )  B_SPLINE_CURVE ( 2, ( #44348, #14132, #14449, #10269, #311, #18958, #58205, #48548, #63359 ),
 .UNSPECIFIED., .F., .F. ) 
 B_SPLINE_CURVE_WITH_KNOTS ( ( 3, 2, 2, 2, 3 ),
 ( 0.9160714285714285365, 0.9166666666666666297, 0.9178571428571428159, 0.9190476190476190022, 0.9196428571428570953 ),
 .UNSPECIFIED. ) 
 CURVE ( )  GEOMETRIC_REPRESENTATION_ITEM ( )  RATIONAL_B_SPLINE_CURVE ( ( 0.9330127018922194093, 0.9330127018922194093, 1.000000000000000000, 0.8660254037844387076, 1.000000000000000000, 0.8660254037844387076, 1.000000000000000000, 0.9330127018922194093, 0.9330127018922194093 ) ) 
 REPRESENTATION_ITEM ( '' )  );
#19102 = DIRECTION ( 'NONE',  ( -0.000000000000000000, 1.000000000000000000, -0.000000000000000000 ) ) ;
#19103 = CARTESIAN_POINT ( 'NONE',  ( -4.458734124999999437, -4.395833331967740065, -2.574251347313719407 ) ) ;
#19104 = LINE ( 'NONE', #14597, #58536 ) ;
#19105 = CARTESIAN_POINT ( 'NONE',  ( 1.975475456537005874E-15, -76.75000000000000000, 5.000000000000000000 ) ) ;
#19106 = CARTESIAN_POINT ( 'NONE',  ( 7.499999999999999112, -4.330127018922205195, -1.000000000000000888 ) ) ;
#19107 = CARTESIAN_POINT ( 'NONE',  ( -1.339745962155610925, -87.66965819600731891, 5.000000000000000000 ) ) ;
#19108 = CARTESIAN_POINT ( 'NONE',  ( -4.458734124999998549, -19.22916666530106866, 2.574251347313722516 ) ) ;
#19109 = CARTESIAN_POINT ( 'NONE',  ( -6.972266317189433020E-16, -72.12499999726878741, -5.000000000000000000 ) ) ;
#19110 = CARTESIAN_POINT ( 'NONE',  ( 4.458734124999998549, -54.72916666530107932, -2.574251347313721627 ) ) ;
#19111 = CARTESIAN_POINT ( 'NONE',  ( 3.152801135295366208, -161.8125000013656063, 3.152801135295367985 ) ) ;
#19112 =( BOUNDED_CURVE ( )  B_SPLINE_CURVE ( 2, ( #13893, #19661, #29297, #48926, #38343, #24495, #18718, #54074, #14830 ),
 .UNSPECIFIED., .F., .F. ) 
 B_SPLINE_CURVE_WITH_KNOTS ( ( 3, 2, 2, 2, 3 ),
 ( 0.7874999999999999778, 0.7880952380952380709, 0.7892857142857142572, 0.7904761904761904434, 0.7910714285714285365 ),
 .UNSPECIFIED. ) 
 CURVE ( )  GEOMETRIC_REPRESENTATION_ITEM ( )  RATIONAL_B_SPLINE_CURVE ( ( 0.9330127018922194093, 0.9330127018922194093, 1.000000000000000000, 0.8660254037844387076, 1.000000000000000000, 0.8660254037844387076, 1.000000000000000000, 0.9330127018922194093, 0.9330127018922194093 ) ) 
 REPRESENTATION_ITEM ( '' )  );
#19113 = CARTESIAN_POINT ( 'NONE',  ( 5.000000000000000888, -49.45833333060213732, 2.886751345948126879 ) ) ;
#19114 = ORIENTED_EDGE ( 'NONE', *, *, #30448, .F. ) ;
#19115 = CARTESIAN_POINT ( 'NONE',  ( 2.229367062500001939, 4.770833334698926897, 3.861377020970579999 ) ) ;
#19116 = ORIENTED_EDGE ( 'NONE', *, *, #1270, .F. ) ;
#19118 = CARTESIAN_POINT ( 'NONE',  ( -2.499999999999996447, -67.70833333060214443, 4.330127018922195425 ) ) ;
#19117 = CARTESIAN_POINT ( 'NONE',  ( 5.000000000000000000, -87.50000000000000000, -6.123233995736766282E-16 ) ) ;
#19119 = CARTESIAN_POINT ( 'NONE',  ( 4.458734124999999437, -160.4375000013655779, 0.000000000000000000 ) ) ;
#19120 = ORIENTED_EDGE ( 'NONE', *, *, #1962, .F. ) ;
#19121 = UNCERTAINTY_MEASURE_WITH_UNIT (LENGTH_MEASURE( 1.000000000000000082E-05 ), #4901, 'distance_accuracy_value', 'NONE');
#19122 = VECTOR ( 'NONE', #44572, 1000.000000000000000 ) ;
#19123 = FACE_OUTER_BOUND ( 'NONE', #58926, .T. ) ;
#19124 = CARTESIAN_POINT ( 'NONE',  ( -58.80597590150559739, -135.0000000000000284, 3.242614290531460330 ) ) ;
#19125 = CARTESIAN_POINT ( 'NONE',  ( -6.972266317189433020E-16, -53.12499999726880162, -5.000000000000000000 ) ) ;
#19126 = CARTESIAN_POINT ( 'NONE',  ( -2.229367062500000163, -41.72916666530107932, -3.861377020970580443 ) ) ;
#19127 = VECTOR ( 'NONE', #17707, 1000.000000000000000 ) ;
#19128 = ORIENTED_EDGE ( 'NONE', *, *, #38843, .T. ) ;
#19129 = AXIS2_PLACEMENT_3D ( 'NONE', #2189, #41701, #16959 ) ;
#19130 = CARTESIAN_POINT ( 'NONE',  ( 2.500000000000002220, -103.5416666639354730, 4.330127018922192761 ) ) ;
#19131 = CARTESIAN_POINT ( 'NONE',  ( -2.229367062500000163, 18.52083333469892779, -3.861377020970580443 ) ) ;
#19132 = CARTESIAN_POINT ( 'NONE',  ( 2.499999999999998668, -24.20833333060214443, -4.330127018922193649 ) ) ;
#19133 = VERTEX_POINT ( 'NONE', #2761 ) ;
#19134 = CARTESIAN_POINT ( 'NONE',  ( 2.229367062500001939, -84.22916666530107932, 3.861377020970579999 ) ) ;
#19135 = CARTESIAN_POINT ( 'NONE',  ( -54.60164318462004474, -127.5000000027312126, -4.984105922594373794 ) ) ;
#19136 = CARTESIAN_POINT ( 'NONE',  ( 1.339745962155612702, -35.16965819600734022, -5.000000000000000000 ) ) ;
#19137 = CARTESIAN_POINT ( 'NONE',  ( 2.499999999999998668, -39.33333333333332860, -4.330127018922193649 ) ) ;
#19138 = CARTESIAN_POINT ( 'NONE',  ( 5.000000000000000000, -52.29166666393547303, -2.886751345948130876 ) ) ;
#19139 = CARTESIAN_POINT ( 'NONE',  ( -4.458734124999997661, -59.22916666530106511, 2.574251347313722516 ) ) ;
#19140 = CARTESIAN_POINT ( 'NONE',  ( -1.339745962155610925, 10.33034180399266333, 5.000000000000000000 ) ) ;
#19141 = CARTESIAN_POINT ( 'NONE',  ( 4.458734124999998549, 25.27083333469892779, -2.574251347313721627 ) ) ;
#19142 = ADVANCED_FACE ( 'NONE', ( #16910 ), #41344, .F. ) ;
#19143 = CARTESIAN_POINT ( 'NONE',  ( 2.499999999999998668, -109.3333333333333428, -4.330127018922193649 ) ) ;
#19144 = CARTESIAN_POINT ( 'NONE',  ( -4.458734124999999437, -48.64583333196773651, -2.574251347313719407 ) ) ;
#19145 = CARTESIAN_POINT ( 'NONE',  ( 2.500000000000002220, -2.541666663935477466, 4.330127018922192761 ) ) ;
#19146 = CARTESIAN_POINT ( 'NONE',  ( -1.049326080737009628E-13, -17.75000000000000355, 5.000000000000000000 ) ) ;
#19147 = DIRECTION ( 'NONE',  ( -0.000000000000000000, 1.000000000000000000, -0.000000000000000000 ) ) ;
#19148 = CARTESIAN_POINT ( 'NONE',  ( -4.458734124999999437, -85.64583333196773651, -2.574251347313719407 ) ) ;
#19149 = CARTESIAN_POINT ( 'NONE',  ( 2.229367062500001939, -107.9791666653010651, 3.861377020970579999 ) ) ;
#19150 = CARTESIAN_POINT ( 'NONE',  ( 4.458734125000000326, -13.14583333196774184, 2.574251347313718519 ) ) ;
#19151 = ORIENTED_EDGE ( 'NONE', *, *, #16307, .T. ) ;
#19152 = CARTESIAN_POINT ( 'NONE',  ( -1.339745962155610925, 18.33034180399266333, 5.000000000000000000 ) ) ;
#19153 = CARTESIAN_POINT ( 'NONE',  ( 4.458734125000001214, -99.89583333196772230, 2.574251347313718519 ) ) ;
#19154 = CARTESIAN_POINT ( 'NONE',  ( -3.535533905932738641, -162.5000000027312126, 3.535533905932737309 ) ) ;
#19155 = CARTESIAN_POINT ( 'NONE',  ( -2.229367062499996610, -93.39583333196773651, 3.861377020970582219 ) ) ;
#19156 = CARTESIAN_POINT ( 'NONE',  ( -4.999999999999999112, -49.79166666393547303, 2.886751345948131764 ) ) ;
#19157 = CARTESIAN_POINT ( 'NONE',  ( -7.907996613752304782, -3.055722423191990611, -7.792112796859422374 ) ) ;
#19158 = CARTESIAN_POINT ( 'NONE',  ( -58.39396692619412477, -131.4375000013656063, 2.891590998281057701 ) ) ;
#19159 = EDGE_CURVE ( 'NONE', #47541, #39239, #31377, .T. ) ;
#19160 = CARTESIAN_POINT ( 'NONE',  ( -52.10840900171896806, -145.1875000013656063, 3.393966926194110556 ) ) ;
#19161 = CARTESIAN_POINT ( 'NONE',  ( -3.152548672688508926E-16, -15.56249999863440614, -5.148502694627439702 ) ) ;
#19162 = CARTESIAN_POINT ( 'NONE',  ( -3.152548672688508926E-16, 13.18750000136559208, -5.148502694627439702 ) ) ;
#19163 = EDGE_CURVE ( 'NONE', #62831, #49893, #37967, .T. ) ;
#19164 = CARTESIAN_POINT ( 'NONE',  ( -2.229367062500000163, -56.72916666530107221, -3.861377020970580443 ) ) ;
#19165 = DIRECTION ( 'NONE',  ( -0.000000000000000000, 1.000000000000000000, -0.000000000000000000 ) ) ;
#19166 = CARTESIAN_POINT ( 'NONE',  ( -4.458734124999997661, -13.22916666530107399, 2.574251347313722516 ) ) ;
#19167 = CARTESIAN_POINT ( 'NONE',  ( 1.339745962155612702, -8.169658196007333117, -5.000000000000000000 ) ) ;
#19168 = CARTESIAN_POINT ( 'NONE',  ( -2.071067811865475061, -153.6875000000000000, -5.000000000000000888 ) ) ;
#19169 = ORIENTED_EDGE ( 'NONE', *, *, #1696, .F. ) ;
#19170 = CARTESIAN_POINT ( 'NONE',  ( 2.229367062500001939, -41.22916666530107932, 3.861377020970579999 ) ) ;
#19171 =( BOUNDED_CURVE ( )  B_SPLINE_CURVE ( 2, ( #37725, #29552, #8462, #35041, #24744, #54653, #30188, #5761, #49816 ),
 .UNSPECIFIED., .F., .F. ) 
 B_SPLINE_CURVE_WITH_KNOTS ( ( 3, 2, 2, 2, 3 ),
 ( 0.7482142857142857206, 0.7488095238095238138, 0.7500000000000000000, 0.7511904761904761862, 0.7517857142857142794 ),
 .UNSPECIFIED. ) 
 CURVE ( )  GEOMETRIC_REPRESENTATION_ITEM ( )  RATIONAL_B_SPLINE_CURVE ( ( 0.9330127018922194093, 0.9330127018922194093, 1.000000000000000000, 0.8660254037844387076, 1.000000000000000000, 0.8660254037844387076, 1.000000000000000000, 0.9330127018922194093, 0.9330127018922194093 ) ) 
 REPRESENTATION_ITEM ( '' )  );
#19172 = VECTOR ( 'NONE', #17258, 1000.000000000000000 ) ;
#19173 = CARTESIAN_POINT ( 'NONE',  ( 1.339745962155615144, -83.58034179853031276, 4.999999999999999112 ) ) ;
#19174 = CARTESIAN_POINT ( 'NONE',  ( -5.000000000000000000, -91.95833333060214443, -2.886751345948128211 ) ) ;
#19175 = DIRECTION ( 'NONE',  ( -0.000000000000000000, 1.000000000000000000, -0.000000000000000000 ) ) ;
#19176 = CARTESIAN_POINT ( 'NONE',  ( -2.229367062500000163, -86.47916666530107932, -3.861377020970580443 ) ) ;
#19177 = CARTESIAN_POINT ( 'NONE',  ( -4.458734124999998549, 20.52083333469892423, 2.574251347313722516 ) ) ;
#19178 = VECTOR ( 'NONE', #14602, 1000.000000000000000 ) ;
#19179 = AXIS2_PLACEMENT_3D ( 'NONE', #57489, #7647, #57174 ) ;
#19180 = CARTESIAN_POINT ( 'NONE',  ( 4.458734124999998549, 11.27083333469892779, -2.574251347313721627 ) ) ;
#19181 = CARTESIAN_POINT ( 'NONE',  ( -9.184850993605147944E-16, -167.2500000000000000, 5.000000000000000000 ) ) ;
#19182 = CARTESIAN_POINT ( 'NONE',  ( 0.000000000000000000, -120.0000000000000000, 5.000000000000000000 ) ) ;
#19183 = CARTESIAN_POINT ( 'NONE',  ( 4.458734124999998549, -87.97916666530107932, -2.574251347313721627 ) ) ;
#19184 = CARTESIAN_POINT ( 'NONE',  ( 5.000000000000000888, -71.58333333333332860, 2.886751345948126879 ) ) ;
#19185 = CARTESIAN_POINT ( 'NONE',  ( -5.000000000000000000, 16.12500000273118417, 0.000000000000000000 ) ) ;
#19186 = ORIENTED_EDGE ( 'NONE', *, *, #16566, .F. ) ;
#19187 = CARTESIAN_POINT ( 'NONE',  ( 5.000000000000000000, -102.4166666666666572, -2.886751345948130876 ) ) ;
#19188 = ORIENTED_EDGE ( 'NONE', *, *, #39340, .T. ) ;
#19189 = CARTESIAN_POINT ( 'NONE',  ( 2.626220312808019583E-14, 15.74999999999999645, -5.000000000000000000 ) ) ;
#19191 = CARTESIAN_POINT ( 'NONE',  ( -5.000000000000000000, -37.00000000000000711, 0.000000000000000000 ) ) ;
#19190 = CYLINDRICAL_SURFACE ( 'NONE', #38822, 5.000000000000000000 ) ;
#19192 = CARTESIAN_POINT ( 'NONE',  ( -2.229367062500000163, -36.47916666530107221, -3.861377020970580443 ) ) ;
#19193 = CARTESIAN_POINT ( 'NONE',  ( -3.535250795749689387E-16, -36.12499999726880873, -5.773502691896257311 ) ) ;
#19195 = VERTEX_POINT ( 'NONE', #48386 ) ;
#19194 = CARTESIAN_POINT ( 'NONE',  ( -4.458734124999999437, -66.39583333196773651, -2.574251347313719407 ) ) ;
#19196 = CARTESIAN_POINT ( 'NONE',  ( -59.59170313451811296, -152.7500000013655779, 1.485763867205729394 ) ) ;
#19197 = CARTESIAN_POINT ( 'NONE',  ( -4.458734124999999437, -14.39583333196773474, -2.574251347313719407 ) ) ;
#19199 = VERTEX_POINT ( 'NONE', #41983 ) ;
#19198 = CARTESIAN_POINT ( 'NONE',  ( 4.458734124999999437, -15.06249999863440436, -5.460374474430324690E-16 ) ) ;
#19200 = CARTESIAN_POINT ( 'NONE',  ( 2.499999999999998668, -76.33333333333334281, -4.330127018922193649 ) ) ;
#19201 = CYLINDRICAL_SURFACE ( 'NONE', #43276, 5.000000000000000000 ) ;
#19202 = CARTESIAN_POINT ( 'NONE',  ( 9.457646018065525792E-16, -55.31249999863439371, 5.148502694627439702 ) ) ;
#19203 = CARTESIAN_POINT ( 'NONE',  ( -4.999999999999999112, -79.79166666393545881, 2.886751345948131764 ) ) ;
#19205 = VERTEX_POINT ( 'NONE', #12718 ) ;
#19204 = DIRECTION ( 'NONE',  ( -0.000000000000000000, 1.000000000000000000, -0.000000000000000000 ) ) ;
#19206 = CARTESIAN_POINT ( 'NONE',  ( -54.60164318462004474, -145.3750000000000284, -4.984105922594373794 ) ) ;
#19207 = CARTESIAN_POINT ( 'NONE',  ( 2.229367062500001939, -24.22916666530107577, 3.861377020970579999 ) ) ;
#19208 = ORIENTED_EDGE ( 'NONE', *, *, #57738, .F. ) ;
#19209 = DIRECTION ( 'NONE',  ( 0.000000000000000000, 0.000000000000000000, -1.000000000000000000 ) ) ;
#19210 = CARTESIAN_POINT ( 'NONE',  ( -4.458734125000000326, -166.2500000013656347, -1.846868145590735644 ) ) ;
#19211 = CARTESIAN_POINT ( 'NONE',  ( 9.457646018065525792E-16, -104.3124999986344221, 5.148502694627439702 ) ) ;
#19212 = CARTESIAN_POINT ( 'NONE',  ( -3.535533905932738641, -167.5000000027312126, 3.535533905932737309 ) ) ;
#19213 = VERTEX_POINT ( 'NONE', #43237 ) ;
#19214 = CARTESIAN_POINT ( 'NONE',  ( -52.80376928212989185, -149.1250000013656063, -4.297418129356378458 ) ) ;
#19215 = CARTESIAN_POINT ( 'NONE',  ( -57.46284108482265651, -139.0625000027312126, 4.819101127000239515 ) ) ;
#19216 = CARTESIAN_POINT ( 'NONE',  ( -3.152548672688508926E-16, -40.56249999863440081, -5.148502694627439702 ) ) ;
#19217 = VECTOR ( 'NONE', #23281, 1000.000000000000000 ) ;
#19218 = CARTESIAN_POINT ( 'NONE',  ( -5.007715329123872641E-16, -8.660254037844399733, -10.00000000000000000 ) ) ;
#19219 = CARTESIAN_POINT ( 'NONE',  ( -9.184850993605147944E-16, -146.3750000027312126, 5.000000000000000000 ) ) ;
#19220 = EDGE_CURVE ( 'NONE', #43789, #60902, #43241, .T. ) ;
#19221 = AXIS2_PLACEMENT_3D ( 'NONE', #43152, #8447, #51874 ) ;
#19222 = CARTESIAN_POINT ( 'NONE',  ( 2.229367062499998831, -14.64583333196773474, -3.861377020970580887 ) ) ;
#19223 = VECTOR ( 'NONE', #14725, 1000.000000000000000 ) ;
#19224 = CARTESIAN_POINT ( 'NONE',  ( 2.229367062500001939, -100.2291666653010651, 3.861377020970579999 ) ) ;
#19225 = EDGE_LOOP ( 'NONE', ( #5829, #24964, #30700, #36093 ) ) ;
#19226 = CARTESIAN_POINT ( 'NONE',  ( -1.846868145590734756, -144.3750000013656063, -4.458734125000000326 ) ) ;
#19227 = CARTESIAN_POINT ( 'NONE',  ( 2.229367062499998831, -26.89583333196774007, -3.861377020970580887 ) ) ;
#19228 = CARTESIAN_POINT ( 'NONE',  ( -4.999999999999998224, 12.08333333333333215, 2.886751345948131764 ) ) ;
#19229 = CARTESIAN_POINT ( 'NONE',  ( -51.60603307380591787, -134.9375000013656063, -2.891590998281053704 ) ) ;
#19230 = CARTESIAN_POINT ( 'NONE',  ( -4.458734124999999437, -69.64583333196773651, -2.574251347313719407 ) ) ;
#19231 = CARTESIAN_POINT ( 'NONE',  ( 1.975475456537005874E-15, -15.75000000000000000, 5.000000000000000000 ) ) ;
#19232 = CARTESIAN_POINT ( 'NONE',  ( -2.500000000000000444, -1.041666663935479686, -4.330127018922193649 ) ) ;
#19233 = CARTESIAN_POINT ( 'NONE',  ( -4.458734125000000326, -139.8750000013656063, 1.846868145590734089 ) ) ;
#19234 = CARTESIAN_POINT ( 'NONE',  ( -3.152548672688508926E-16, 4.187500001365595637, -5.148502694627439702 ) ) ;
#19235 = ORIENTED_EDGE ( 'NONE', *, *, #35914, .F. ) ;
#19236 = CARTESIAN_POINT ( 'NONE',  ( 1.975475456537005874E-15, -59.74999999999999289, 5.000000000000000000 ) ) ;
#19238 = CARTESIAN_POINT ( 'NONE',  ( 4.458734125000001214, -30.89583333196773296, 2.574251347313718519 ) ) ;
#19237 = CARTESIAN_POINT ( 'NONE',  ( -2.500000000000000444, -98.16666666666665719, -4.330127018922193649 ) ) ;
#19239 = EDGE_CURVE ( 'NONE', #22662, #8603, #43605, .T. ) ;
#19240 = CARTESIAN_POINT ( 'NONE',  ( 1.975475456537005874E-15, -22.62499999726880873, 5.000000000000000000 ) ) ;
#19241 = CARTESIAN_POINT ( 'NONE',  ( 4.458734125000001214, -75.14583333196775072, 2.574251347313718519 ) ) ;
#19242 = CARTESIAN_POINT ( 'NONE',  ( 2.229367062499998831, 22.10416666803225993, -3.861377020970580887 ) ) ;
#19243 = DIRECTION ( 'NONE',  ( -0.000000000000000000, 1.000000000000000000, -0.000000000000000000 ) ) ;
#19244 = CARTESIAN_POINT ( 'NONE',  ( -56.48576386720575471, -142.7500000013656063, -4.591703134518078322 ) ) ;
#19245 = CARTESIAN_POINT ( 'NONE',  ( -4.458734124999999437, -4.395833331967740065, -2.574251347313719407 ) ) ;
#19246 = CARTESIAN_POINT ( 'NONE',  ( -2.229367062500000163, 28.27083333469892779, -3.861377020970580443 ) ) ;
#19247 = EDGE_CURVE ( 'NONE', #27844, #49754, #25594, .T. ) ;
#19248 = CARTESIAN_POINT ( 'NONE',  ( 4.458734125000000326, -44.14583333196774362, 2.574251347313718519 ) ) ;
#19249 = CARTESIAN_POINT ( 'NONE',  ( 5.000000000000000888, -60.45833333060213732, 2.886751345948126879 ) ) ;
#19250 = CARTESIAN_POINT ( 'NONE',  ( 9.457646018065525792E-16, 0.9375000013655959696, 5.148502694627439702 ) ) ;
#19251 = EDGE_CURVE ( 'NONE', #22002, #43496, #47759, .T. ) ;
#19252 = CARTESIAN_POINT ( 'NONE',  ( -4.458734124999999437, -25.56249999863440792, 0.000000000000000000 ) ) ;
#19253 = CARTESIAN_POINT ( 'NONE',  ( 4.458734125000001214, -71.89583333196773651, 2.574251347313718519 ) ) ;
#19254 = CARTESIAN_POINT ( 'NONE',  ( -5.000000000000000000, -106.9583333306021302, -2.886751345948128211 ) ) ;
#19255 = CARTESIAN_POINT ( 'NONE',  ( 2.229367062500001939, 26.02083333469892779, 3.861377020970579999 ) ) ;
#19256 = DIRECTION ( 'NONE',  ( -0.000000000000000000, 1.000000000000000000, -0.000000000000000000 ) ) ;
#19257 = CARTESIAN_POINT ( 'NONE',  ( -53.33387254593731086, -152.9375000027312126, 5.149110718188520508 ) ) ;
#19258 = CARTESIAN_POINT ( 'NONE',  ( -3.152548672688508926E-16, -73.81249999863440792, -5.148502694627439702 ) ) ;
#19259 = CARTESIAN_POINT ( 'NONE',  ( -2.500000000000000444, -53.16666666666666430, -4.330127018922193649 ) ) ;
#19260 = CARTESIAN_POINT ( 'NONE',  ( -1.339745962155610925, -65.66965819600733312, 5.000000000000000000 ) ) ;
#19261 = CARTESIAN_POINT ( 'NONE',  ( -1.339745962155610925, -10.66965819600733312, 5.000000000000000000 ) ) ;
#19262 = ORIENTED_EDGE ( 'NONE', *, *, #62480, .F. ) ;
#19263 = CARTESIAN_POINT ( 'NONE',  ( -2.071067811865520358, -140.3125000000000284, 4.999999999999957367 ) ) ;
#19264 = LINE ( 'NONE', #1587, #11378 ) ;
#19265 = CARTESIAN_POINT ( 'NONE',  ( -5.000000000000000000, -12.08333333333333393, -2.886751345948128211 ) ) ;
#19266 = CARTESIAN_POINT ( 'NONE',  ( 9.457646018065525792E-16, -15.06249999863440259, 5.148502694627439702 ) ) ;
#19267 = EDGE_CURVE ( 'NONE', #16051, #17071, #57432, .T. ) ;
#19268 = VECTOR ( 'NONE', #61212, 1000.000000000000000 ) ;
#19269 = CARTESIAN_POINT ( 'NONE',  ( -3.152548672688508926E-16, -81.56249999863440792, -5.148502694627439702 ) ) ;
#19270 = CARTESIAN_POINT ( 'NONE',  ( -4.458734124999999437, -167.1875000013655779, -5.460374474430324690E-16 ) ) ;
#19271 = CARTESIAN_POINT ( 'NONE',  ( -2.500000000000000444, -17.04166666393548368, -4.330127018922193649 ) ) ;
#19273 = ORIENTED_EDGE ( 'NONE', *, *, #50161, .F. ) ;
#19272 = CARTESIAN_POINT ( 'NONE',  ( 2.229367062499998831, -50.64583333196772941, -3.861377020970580887 ) ) ;
#19274 = CARTESIAN_POINT ( 'NONE',  ( 1.975475456537005874E-15, 5.250000000000000000, 5.000000000000000000 ) ) ;
#19275 = CARTESIAN_POINT ( 'NONE',  ( 1.975475456537005874E-15, -45.62499999726880873, 5.000000000000000000 ) ) ;
#19277 = ORIENTED_EDGE ( 'NONE', *, *, #12203, .F. ) ;
#19276 = CARTESIAN_POINT ( 'NONE',  ( -4.458734124999999437, 3.437500001365594748, 0.000000000000000000 ) ) ;
#19278 = CARTESIAN_POINT ( 'NONE',  ( -55.35523342533222291, -152.3125000013656063, 4.444560631937231499 ) ) ;
#19279 = CARTESIAN_POINT ( 'NONE',  ( 5.000000000000000888, -62.58333333333333570, 2.886751345948126879 ) ) ;
#19280 = CARTESIAN_POINT ( 'NONE',  ( -3.152801135295367096, -154.3125000013656063, -3.152801135295367541 ) ) ;
#19281 = CARTESIAN_POINT ( 'NONE',  ( 9.457646018065525792E-16, -40.31249999863440081, 5.148502694627439702 ) ) ;
#19282 = VECTOR ( 'NONE', #57920, 1000.000000000000000 ) ;
#19283 = CARTESIAN_POINT ( 'NONE',  ( -6.972266317189433020E-16, -56.25000000000000000, -5.000000000000000000 ) ) ;
#19284 = CARTESIAN_POINT ( 'NONE',  ( -5.000000000000000888, -161.4375000000000000, 2.071067811865474617 ) ) ;
#19285 = DIRECTION ( 'NONE',  ( -0.000000000000000000, 1.000000000000000000, -0.000000000000000000 ) ) ;
#19286 = CARTESIAN_POINT ( 'NONE',  ( -53.51423613279429503, -127.5000000013656347, 4.591703134518082763 ) ) ;
#19287 = CARTESIAN_POINT ( 'NONE',  ( -4.458734124999999437, -6.645833331967741842, -2.574251347313719407 ) ) ;
#19288 = CARTESIAN_POINT ( 'NONE',  ( 9.457646018065525792E-16, -46.31249999863440792, 5.148502694627439702 ) ) ;
#19289 = CARTESIAN_POINT ( 'NONE',  ( 3.061616997868383141E-16, -150.8750000027312126, -5.000000000000000000 ) ) ;
#19290 = CARTESIAN_POINT ( 'NONE',  ( 1.846868145590736310, -149.6250000013655779, 4.458734124999999437 ) ) ;
#19291 = CARTESIAN_POINT ( 'NONE',  ( -2.229367062500000163, -89.72916666530106511, -3.861377020970580443 ) ) ;
#19292 = CARTESIAN_POINT ( 'NONE',  ( -60.14911071818854538, -143.0625000000000284, 1.666127454062681146 ) ) ;
#19293 = ORIENTED_EDGE ( 'NONE', *, *, #2696, .T. ) ;
#19294 = CARTESIAN_POINT ( 'NONE',  ( -1.339745962155636017, 3.330341803992664218, 4.999999999999985789 ) ) ;
#19295 = CARTESIAN_POINT ( 'NONE',  ( 2.229367062499998831, 29.10416666803225993, -3.861377020970580887 ) ) ;
#19296 = CARTESIAN_POINT ( 'NONE',  ( -51.75738570946856498, -149.8750000027312126, 3.805975901505576964 ) ) ;
#19297 = CARTESIAN_POINT ( 'NONE',  ( -5.000000000000000000, -105.0833333333333286, -2.886751345948128211 ) ) ;
#19298 = VERTEX_POINT ( 'NONE', #52595 ) ;
#19299 =( BOUNDED_CURVE ( )  B_SPLINE_CURVE ( 2, ( #4387, #52963, #209, #58423, #33660, #23708, #28516, #59054, #43305 ),
 .UNSPECIFIED., .F., .F. ) 
 B_SPLINE_CURVE_WITH_KNOTS ( ( 3, 2, 2, 2, 3 ),
 ( 0.8437500000000000000, 0.8444444444444444420, 0.8458333333333333259, 0.8472222222222222099, 0.8479166666666666519 ),
 .UNSPECIFIED. ) 
 CURVE ( )  GEOMETRIC_REPRESENTATION_ITEM ( )  RATIONAL_B_SPLINE_CURVE ( ( 0.9330127018922194093, 0.9330127018922194093, 1.000000000000000000, 0.8660254037844387076, 1.000000000000000000, 0.8660254037844387076, 1.000000000000000000, 0.9330127018922194093, 0.9330127018922194093 ) ) 
 REPRESENTATION_ITEM ( '' )  );
#19300 = EDGE_CURVE ( 'NONE', #15327, #38362, #4190, .T. ) ;
#19301 = EDGE_CURVE ( 'NONE', #5022, #29389, #8802, .T. ) ;
#19302 = DIRECTION ( 'NONE',  ( 0.000000000000000000, 0.000000000000000000, 1.000000000000000000 ) ) ;
#19303 = CARTESIAN_POINT ( 'NONE',  ( 2.229367062499998831, -9.895833331967738289, -3.861377020970580887 ) ) ;
#19304 = EDGE_CURVE ( 'NONE', #32533, #47984, #63362, .T. ) ;
#19305 = CYLINDRICAL_SURFACE ( 'NONE', #39425, 5.000000000000000000 ) ;
#19306 = CARTESIAN_POINT ( 'NONE',  ( 4.458734124999999437, -0.8124999986344055847, -5.460374474430324690E-16 ) ) ;
#19307 = CARTESIAN_POINT ( 'NONE',  ( -2.500000000000000444, -74.04166666393547303, -4.330127018922193649 ) ) ;
#19308 = CARTESIAN_POINT ( 'NONE',  ( -4.458734124999999437, -154.9375000013655779, -5.460374474430324690E-16 ) ) ;
#19309 = CARTESIAN_POINT ( 'NONE',  ( -4.458734124999997661, 22.52083333469892423, 2.574251347313722516 ) ) ;
#19310 = VERTEX_POINT ( 'NONE', #44824 ) ;
#19311 = CARTESIAN_POINT ( 'NONE',  ( 4.458734124999998549, -92.72916666530106511, -2.574251347313721627 ) ) ;
#19312 = CARTESIAN_POINT ( 'NONE',  ( -3.535533905932737309, -148.6250000000000000, -3.535533905932738197 ) ) ;
#19313 = CARTESIAN_POINT ( 'NONE',  ( -1.339745962155610925, -103.6696581960073331, 5.000000000000000000 ) ) ;
#19314 = CARTESIAN_POINT ( 'NONE',  ( -2.229367062500000163, -16.47916666530107577, -3.861377020970580443 ) ) ;
#19316 = ADVANCED_FACE ( 'NONE', ( #14288 ), #4957, .T. ) ;
#19315 = CARTESIAN_POINT ( 'NONE',  ( -5.000000000000000000, -109.9999999999999858, 0.000000000000000000 ) ) ;
#19317 = CARTESIAN_POINT ( 'NONE',  ( 5.000000000000000000, -42.37499999726880873, -6.123233995736766282E-16 ) ) ;
#19318 = CARTESIAN_POINT ( 'NONE',  ( 5.000000000000000000, -64.29166666393547303, -2.886751345948130876 ) ) ;
#19319 = CARTESIAN_POINT ( 'NONE',  ( 9.457646018065525792E-16, 18.93750000136559564, 5.148502694627439702 ) ) ;
#19320 = CARTESIAN_POINT ( 'NONE',  ( -2.916731409357579869E-14, 12.37500000273118594, 5.000000000000000888 ) ) ;
#19321 = EDGE_CURVE ( 'NONE', #1448, #33786, #19104, .T. ) ;
#19322 = ORIENTED_EDGE ( 'NONE', *, *, #25943, .T. ) ;
#19323 = CARTESIAN_POINT ( 'NONE',  ( -4.458734124999997661, 18.77083333469892779, 2.574251347313722516 ) ) ;
#19324 = EDGE_CURVE ( 'NONE', #29404, #32980, #10869, .T. ) ;
#19325 = CARTESIAN_POINT ( 'NONE',  ( -4.458734124999999437, -61.31249999863440081, 0.000000000000000000 ) ) ;
#19326 = CARTESIAN_POINT ( 'NONE',  ( -4.458734124999999437, -6.645833331967741842, -2.574251347313719407 ) ) ;
#19327 =( NAMED_UNIT ( * ) PLANE_ANGLE_UNIT ( ) SI_UNIT ( $, .RADIAN. ) );
#19328 = CARTESIAN_POINT ( 'NONE',  ( 5.000000000000000888, 12.41666666666666607, 2.886751345948126879 ) ) ;
#19329 = CARTESIAN_POINT ( 'NONE',  ( 2.071067811865476394, -139.3125000027312126, 5.000000000000000000 ) ) ;
#19331 = EDGE_CURVE ( 'NONE', #871, #51921, #12823, .T. ) ;
#19330 = CARTESIAN_POINT ( 'NONE',  ( -51.75738570946856498, -149.7500000000000284, 3.805975901505576964 ) ) ;
#19332 = CARTESIAN_POINT ( 'NONE',  ( -3.152548672688508926E-16, -54.56249999863439371, -5.148502694627439702 ) ) ;
#19333 = CARTESIAN_POINT ( 'NONE',  ( -4.999999999999999112, -90.79166666393545881, 2.886751345948131764 ) ) ;
#19334 = VECTOR ( 'NONE', #40293, 1000.000000000000000 ) ;
#19335 = DIRECTION ( 'NONE',  ( -0.000000000000000000, 1.000000000000000000, -0.000000000000000000 ) ) ;
#19336 = FACE_OUTER_BOUND ( 'NONE', #19452, .T. ) ;
#19337 = CARTESIAN_POINT ( 'NONE',  ( -2.229367062499996610, -89.39583333196773651, 3.861377020970582219 ) ) ;
#19338 = CARTESIAN_POINT ( 'NONE',  ( 3.152801135295366208, -152.8125000013656063, 3.152801135295367985 ) ) ;
#19339 = CARTESIAN_POINT ( 'NONE',  ( -2.500000000000000444, -39.16666666666667140, -4.330127018922193649 ) ) ;
#19340 = CARTESIAN_POINT ( 'NONE',  ( -60.14911071818854538, -140.0625000000000000, 1.666127454062681146 ) ) ;
#19341 = CARTESIAN_POINT ( 'NONE',  ( 2.071067811865550556, -163.1875000000000000, 4.999999999999925393 ) ) ;
#19342 = ORIENTED_EDGE ( 'NONE', *, *, #17948, .F. ) ;
#19343 = CARTESIAN_POINT ( 'NONE',  ( -4.458734124999999437, -101.3124999986344079, 0.000000000000000000 ) ) ;
#19344 = CARTESIAN_POINT ( 'NONE',  ( -4.458734124999999437, 5.437500001365592972, 0.000000000000000000 ) ) ;
#19345 = DIRECTION ( 'NONE',  ( 0.000000000000000000, 1.000000000000000000, 0.000000000000000000 ) ) ;
#19346 = CARTESIAN_POINT ( 'NONE',  ( 2.500000000000002220, 0.3333333333333348136, 4.330127018922192761 ) ) ;
#19347 = CARTESIAN_POINT ( 'NONE',  ( -4.458734124999997661, -60.22916666530105800, 2.574251347313722516 ) ) ;
#19348 = DIRECTION ( 'NONE',  ( -0.8660254037844387076, 0.000000000000000000, -0.4999999999999997780 ) ) ;
#19349 = CARTESIAN_POINT ( 'NONE',  ( -2.500000000000000444, -3.041666663935477910, -4.330127018922193649 ) ) ;
#19351 = ORIENTED_EDGE ( 'NONE', *, *, #34157, .T. ) ;
#19350 = CARTESIAN_POINT ( 'NONE',  ( -3.152548672688508926E-16, -35.56249999863440792, -5.148502694627439702 ) ) ;
#19352 = CARTESIAN_POINT ( 'NONE',  ( 1.975475456537005874E-15, 17.37500000273118417, 5.000000000000000000 ) ) ;
#19353 = CARTESIAN_POINT ( 'NONE',  ( 1.975475456537005874E-15, -78.62499999726881583, 5.000000000000000000 ) ) ;
#19354 =( BOUNDED_CURVE ( )  B_SPLINE_CURVE ( 2, ( #318, #54979, #19916, #39530, #45326, #15100, #45646, #5449, #34387 ),
 .UNSPECIFIED., .F., .F. ) 
 B_SPLINE_CURVE_WITH_KNOTS ( ( 3, 2, 2, 2, 3 ),
 ( 0.6946428571428571175, 0.6952380952380952106, 0.6964285714285713969, 0.6976190476190475831, 0.6982142857142856762 ),
 .UNSPECIFIED. ) 
 CURVE ( )  GEOMETRIC_REPRESENTATION_ITEM ( )  RATIONAL_B_SPLINE_CURVE ( ( 0.9330127018922194093, 0.9330127018922194093, 1.000000000000000000, 0.8660254037844387076, 1.000000000000000000, 0.8660254037844387076, 1.000000000000000000, 0.9330127018922194093, 0.9330127018922194093 ) ) 
 REPRESENTATION_ITEM ( '' )  );
#19355 = CARTESIAN_POINT ( 'NONE',  ( -4.999999999999998224, 25.08333333333333215, 2.886751345948131764 ) ) ;
#19356 = CARTESIAN_POINT ( 'NONE',  ( 2.500000000000002220, -43.66666666666665719, 4.330127018922192761 ) ) ;
#19359 = CARTESIAN_POINT ( 'NONE',  ( -4.458734124999999437, -26.56249999863440792, 0.000000000000000000 ) ) ;
#19358 =( BOUNDED_CURVE ( )  B_SPLINE_CURVE ( 2, ( #55031, #45697, #46013, #31530, #57504, #47512, #1976, #21577, #8593 ),
 .UNSPECIFIED., .F., .F. ) 
 B_SPLINE_CURVE_WITH_KNOTS ( ( 3, 2, 2, 2, 3 ),
 ( 0.4812500000000000111, 0.4819444444444444531, 0.4833333333333333370, 0.4847222222222222210, 0.4854166666666666630 ),
 .UNSPECIFIED. ) 
 CURVE ( )  GEOMETRIC_REPRESENTATION_ITEM ( )  RATIONAL_B_SPLINE_CURVE ( ( 0.9330127018922194093, 0.9330127018922194093, 1.000000000000000000, 0.8660254037844387076, 1.000000000000000000, 0.8660254037844387076, 1.000000000000000000, 0.9330127018922194093, 0.9330127018922194093 ) ) 
 REPRESENTATION_ITEM ( '' )  );
#19357 = DIRECTION ( 'NONE',  ( 0.000000000000000000, 0.000000000000000000, -1.000000000000000000 ) ) ;
#19360 = CARTESIAN_POINT ( 'NONE',  ( 0.000000000000000000, -120.0000000000000000, 5.000000000000000000 ) ) ;
#19361 = CARTESIAN_POINT ( 'NONE',  ( 2.229367062499998831, -72.64583333196773651, -3.861377020970580887 ) ) ;
#19362 = CARTESIAN_POINT ( 'NONE',  ( -3.152801135295367985, -144.0625000013655779, 3.152801135295367096 ) ) ;
#19363 = CARTESIAN_POINT ( 'NONE',  ( -4.458734124999998549, -79.22916666530107932, 2.574251347313722516 ) ) ;
#19364 = AXIS2_PLACEMENT_3D ( 'NONE', #21758, #11452, #60041 ) ;
#19365 = CARTESIAN_POINT ( 'NONE',  ( -59.44456063193725015, -139.8125000013656063, -0.3552334253322034230 ) ) ;
#19366 = CARTESIAN_POINT ( 'NONE',  ( -4.458734124999998549, -32.47916666530107221, 2.574251347313722516 ) ) ;
#19367 = CARTESIAN_POINT ( 'NONE',  ( -5.000000000000000000, -67.95833333060214443, -2.886751345948128211 ) ) ;
#19368 = ORIENTED_EDGE ( 'NONE', *, *, #27165, .F. ) ;
#19369 = B_SPLINE_CURVE_WITH_KNOTS ( 'NONE', 3,
 ( #16006, #9898, #39800, #39167, #10536, #19553, #44960, #58792, #34997, #29507 ),
 .UNSPECIFIED., .F., .F.,
 ( 4, 2, 2, 2, 4 ),
 ( 0.000000000000000000, 0.002305503304226489900, 0.004611006608452982401, 0.006916509912679474036, 0.009222013216905966537 ),
 .UNSPECIFIED. ) ;
#19370 = EDGE_LOOP ( 'NONE', ( #43248, #59510, #14687, #19051 ) ) ;
#19371 = CARTESIAN_POINT ( 'NONE',  ( 2.229367062500001939, -73.22916666530107932, 3.861377020970579999 ) ) ;
#19372 = CARTESIAN_POINT ( 'NONE',  ( -2.499999999999996447, 22.29166666939785202, 4.330127018922195425 ) ) ;
#19373 =( NAMED_UNIT ( * ) PLANE_ANGLE_UNIT ( ) SI_UNIT ( $, .RADIAN. ) );
#19374 = EDGE_LOOP ( 'NONE', ( #22006, #38675, #19529, #12195 ) ) ;
#19375 = CARTESIAN_POINT ( 'NONE',  ( -4.764381983412779477E-15, 27.25000000000000000, 5.000000000000000000 ) ) ;
#19376 = CARTESIAN_POINT ( 'NONE',  ( -1.339745962155613812, -3.205341801261480938, -5.000000000000000000 ) ) ;
#19377 = CARTESIAN_POINT ( 'NONE',  ( 2.229367062499998831, -60.89583333196774362, -3.861377020970580887 ) ) ;
#19378 = CARTESIAN_POINT ( 'NONE',  ( -4.458734124999998549, 1.520833334698927342, 2.574251347313722516 ) ) ;
#19379 = VERTEX_POINT ( 'NONE', #24257 ) ;
#19380 = VECTOR ( 'NONE', #30015, 1000.000000000000000 ) ;
#19381 = CARTESIAN_POINT ( 'NONE',  ( -3.535533905932738641, -146.3750000000000000, 3.535533905932737309 ) ) ;
#19382 =( BOUNDED_CURVE ( )  B_SPLINE_CURVE ( 2, ( #61155, #37019, #61470, #17404, #3866, #41502, #17078, #31866, #23165 ),
 .UNSPECIFIED., .F., .F. ) 
 B_SPLINE_CURVE_WITH_KNOTS ( ( 3, 2, 2, 2, 3 ),
 ( 0.4267857142857142683, 0.4273809523809523614, 0.4285714285714285476, 0.4297619047619047894, 0.4303571428571428825 ),
 .UNSPECIFIED. ) 
 CURVE ( )  GEOMETRIC_REPRESENTATION_ITEM ( )  RATIONAL_B_SPLINE_CURVE ( ( 0.9330127018922194093, 0.9330127018922194093, 1.000000000000000000, 0.8660254037844387076, 1.000000000000000000, 0.8660254037844387076, 1.000000000000000000, 0.9330127018922194093, 0.9330127018922194093 ) ) 
 REPRESENTATION_ITEM ( '' )  );
#19383 = CARTESIAN_POINT ( 'NONE',  ( -3.152548672688508926E-16, 15.43750000136559564, -5.148502694627439702 ) ) ;
#19384 = CARTESIAN_POINT ( 'NONE',  ( -56.48576386720575471, -143.7500000013656063, -4.591703134518078322 ) ) ;
#19385 = CARTESIAN_POINT ( 'NONE',  ( 2.500000000000002220, -92.54166666393547303, 4.330127018922192761 ) ) ;
#19386 = CARTESIAN_POINT ( 'NONE',  ( -4.458734124999999437, -166.9375000013655779, -5.460374474430324690E-16 ) ) ;
#19387 = ORIENTED_EDGE ( 'NONE', *, *, #60987, .T. ) ;
#19388 = CARTESIAN_POINT ( 'NONE',  ( 2.229367062499998831, -74.64583333196773651, -3.861377020970580887 ) ) ;
#19389 = CARTESIAN_POINT ( 'NONE',  ( -9.184850993605147944E-16, -153.2500000000000000, 5.000000000000000000 ) ) ;
#19390 = CARTESIAN_POINT ( 'NONE',  ( -4.458734124999998549, 2.770833334698928674, 2.574251347313722516 ) ) ;
#19391 = CARTESIAN_POINT ( 'NONE',  ( 2.500000000000002220, -40.54166666393548013, 4.330127018922192761 ) ) ;
#19392 = CARTESIAN_POINT ( 'NONE',  ( -4.458734124999998549, -64.47916666530106511, 2.574251347313722516 ) ) ;
#19393 = CARTESIAN_POINT ( 'NONE',  ( -5.000000000000000000, -23.87499999726881228, 0.000000000000000000 ) ) ;
#19394 = CARTESIAN_POINT ( 'NONE',  ( 1.975475456537005874E-15, -96.62499999726880162, 5.000000000000000000 ) ) ;
#19395 = CARTESIAN_POINT ( 'NONE',  ( 1.339745962155612702, -28.16965819600733312, -5.000000000000000000 ) ) ;
#19396 = CARTESIAN_POINT ( 'NONE',  ( -1.339745962155610925, -64.66965819600733312, 5.000000000000000000 ) ) ;
#19397 = ADVANCED_FACE ( 'NONE', ( #29068 ), #59308, .T. ) ;
#19398 = CARTESIAN_POINT ( 'NONE',  ( 4.458734124999999437, -46.81249999863440792, -5.460374474430324690E-16 ) ) ;
#19399 = PRODUCT ( 'coupler', 'coupler', '', ( #6032 ) ) ;
#19400 = CARTESIAN_POINT ( 'NONE',  ( 4.458734124999998549, -24.97916666530106511, -2.574251347313721627 ) ) ;
#19401 = CARTESIAN_POINT ( 'NONE',  ( 2.229367062499998831, 5.104166668032261711, -3.861377020970580887 ) ) ;
#19402 = VECTOR ( 'NONE', #20149, 1000.000000000000000 ) ;
#19403 =( BOUNDED_CURVE ( )  B_SPLINE_CURVE ( 2, ( #20293, #49, #15475, #59540, #34766, #14816, #29609, #49239, #39894 ),
 .UNSPECIFIED., .F., .F. ) 
 B_SPLINE_CURVE_WITH_KNOTS ( ( 3, 2, 2, 2, 3 ),
 ( 0.7687500000000000444, 0.7694444444444444864, 0.7708333333333333703, 0.7722222222222222543, 0.7729166666666666963 ),
 .UNSPECIFIED. ) 
 CURVE ( )  GEOMETRIC_REPRESENTATION_ITEM ( )  RATIONAL_B_SPLINE_CURVE ( ( 0.9330127018922194093, 0.9330127018922194093, 1.000000000000000000, 0.8660254037844387076, 1.000000000000000000, 0.8660254037844387076, 1.000000000000000000, 0.9330127018922194093, 0.9330127018922194093 ) ) 
 REPRESENTATION_ITEM ( '' )  );
#19404 = CARTESIAN_POINT ( 'NONE',  ( -57.46284108482265651, -143.9375000000000000, 4.819101127000238627 ) ) ;
#19405 = CARTESIAN_POINT ( 'NONE',  ( -3.535250795749689387E-16, 27.75000000000000000, -5.773502691896257311 ) ) ;
#19406 = EDGE_CURVE ( 'NONE', #56532, #58923, #48692, .T. ) ;
#19407 = CARTESIAN_POINT ( 'NONE',  ( -5.000000000000000888, -148.6875000027311842, -2.071067811865475949 ) ) ;
#19408 = DIRECTION ( 'NONE',  ( -0.8660254037844410391, -0.4999999999999958367, -0.000000000000000000 ) ) ;
#19409 = VECTOR ( 'NONE', #63217, 1000.000000000000000 ) ;
#19410 = CARTESIAN_POINT ( 'NONE',  ( -4.458734124999999437, -39.31249999863440081, 0.000000000000000000 ) ) ;
#19411 = CARTESIAN_POINT ( 'NONE',  ( 5.000000000000000000, -74.29166666393547303, -2.886751345948129988 ) ) ;
#19412 = CARTESIAN_POINT ( 'NONE',  ( -50.55543936806279248, -143.3125000013656063, 0.3552334253322060320 ) ) ;
#19413 = CARTESIAN_POINT ( 'NONE',  ( 5.000000000000000888, -143.9375000000000000, -2.071067811865475505 ) ) ;
#19414 = EDGE_CURVE ( 'NONE', #46250, #34014, #14867, .T. ) ;
#19415 = CARTESIAN_POINT ( 'NONE',  ( 4.458734124999998549, -74.97916666530106511, -2.574251347313721627 ) ) ;
#19416 = CARTESIAN_POINT ( 'NONE',  ( 4.458734124999999437, -167.6250000013656347, -1.846868145590734978 ) ) ;
#19417 = CARTESIAN_POINT ( 'NONE',  ( -2.229367062500000163, -31.47916666530107577, -3.861377020970580443 ) ) ;
#19418 = CARTESIAN_POINT ( 'NONE',  ( 0.000000000000000000, -170.0000000000000000, 0.000000000000000000 ) ) ;
#19419 = CARTESIAN_POINT ( 'NONE',  ( 7.500000000000000000, 4.330127018922190096, -10.00000000000000000 ) ) ;
#19420 = CARTESIAN_POINT ( 'NONE',  ( 1.060575238724906964E-15, -23.75000000000000000, 5.773502691896257311 ) ) ;
#19421 = CARTESIAN_POINT ( 'NONE',  ( 3.152801135295366208, -143.5625000013655779, 3.152801135295367985 ) ) ;
#19422 = VERTEX_POINT ( 'NONE', #1432 ) ;
#19423 = CARTESIAN_POINT ( 'NONE',  ( 4.458734125000001214, 25.85416666803225638, 2.574251347313718519 ) ) ;
#19424 = CARTESIAN_POINT ( 'NONE',  ( -58.80597590150559739, -141.0000000000000000, 3.242614290531460330 ) ) ;
#19425 = CARTESIAN_POINT ( 'NONE',  ( -2.229367062499996610, -54.39583333196773651, 3.861377020970582219 ) ) ;
#19426 = CARTESIAN_POINT ( 'NONE',  ( -55.00000000000002132, -155.0000000000000284, 1.734723475976807094E-15 ) ) ;
#19427 = CARTESIAN_POINT ( 'NONE',  ( 1.339745962155615144, -48.58034179853029855, 4.999999999999999112 ) ) ;
#19428 = CARTESIAN_POINT ( 'NONE',  ( -3.535250795749689387E-16, 18.75000000000000000, -5.773502691896257311 ) ) ;
#19429 = CARTESIAN_POINT ( 'NONE',  ( -55.00000000000001421, -135.0000000000000284, -8.082903768654752241 ) ) ;
#19430 = CARTESIAN_POINT ( 'NONE',  ( 4.458734125000001214, -6.895833331967734736, 2.574251347313718519 ) ) ;
#19431 = CARTESIAN_POINT ( 'NONE',  ( -6.972266317189433020E-16, -23.24999999999999645, -5.000000000000000000 ) ) ;
#19432 = CARTESIAN_POINT ( 'NONE',  ( -51.75738570946856498, -145.8750000027312126, 3.805975901505576964 ) ) ;
#19433 = DIRECTION ( 'NONE',  ( -0.000000000000000000, 1.000000000000000000, -0.000000000000000000 ) ) ;
#19434 = CARTESIAN_POINT ( 'NONE',  ( -2.500000000000000444, -88.04166666393548724, -4.330127018922193649 ) ) ;
#19436 = CARTESIAN_POINT ( 'NONE',  ( 9.457646018065525792E-16, -22.06249999863440436, 5.148502694627439702 ) ) ;
#19435 = CARTESIAN_POINT ( 'NONE',  ( 1.339745962155627135, 18.70534180126147916, -4.999999999999991118 ) ) ;
#19437 = LINE ( 'NONE', #44191, #3959 ) ;
#19438 = CARTESIAN_POINT ( 'NONE',  ( -4.458734124999999437, -54.31249999863440081, 0.000000000000000000 ) ) ;
#19439 = CARTESIAN_POINT ( 'NONE',  ( 2.730187237215162345E-16, -154.4375000013655779, -4.458734124999999437 ) ) ;
#19440 = CARTESIAN_POINT ( 'NONE',  ( 5.000000000000000888, -51.45833333060214443, 2.886751345948126879 ) ) ;
#19441 = ORIENTED_EDGE ( 'NONE', *, *, #30734, .F. ) ;
#19442 = CARTESIAN_POINT ( 'NONE',  ( -4.458734124999999437, 7.354166668032259935, -2.574251347313719407 ) ) ;
#19443 = VERTEX_POINT ( 'NONE', #60600 ) ;
#19445 = CARTESIAN_POINT ( 'NONE',  ( -5.000000000000000000, -3.000000000000002665, 0.000000000000000000 ) ) ;
#19444 = CARTESIAN_POINT ( 'NONE',  ( 1.339745962155615144, -87.70534180126146850, 4.999999999999999112 ) ) ;
#19446 = CARTESIAN_POINT ( 'NONE',  ( 1.846868145590735200, -157.2500000013656063, -4.458734125000000326 ) ) ;
#19447 = ORIENTED_EDGE ( 'NONE', *, *, #7146, .T. ) ;
#19448 = CARTESIAN_POINT ( 'NONE',  ( -60.14911071818854538, -133.0625000000000284, 1.666127454062681368 ) ) ;
#19450 = AXIS2_PLACEMENT_3D ( 'NONE', #63341, #32807, #34054 ) ;
#19449 = CYLINDRICAL_SURFACE ( 'NONE', #31256, 5.000000000000000000 ) ;
#19451 = CARTESIAN_POINT ( 'NONE',  ( -2.229367062500000163, -42.72916666530107932, -3.861377020970580443 ) ) ;
#19452 = EDGE_LOOP ( 'NONE', ( #15596, #45547, #9686, #21300 ) ) ;
#19453 = ADVANCED_FACE ( 'NONE', ( #2065 ), #21031, .T. ) ;
#19454 = CARTESIAN_POINT ( 'NONE',  ( 5.000000000000000000, -103.2916666639354730, -2.886751345948130876 ) ) ;
#19455 = CARTESIAN_POINT ( 'NONE',  ( -4.458734124999999437, 19.68750000136559208, 0.000000000000000000 ) ) ;
#19456 = CARTESIAN_POINT ( 'NONE',  ( -56.66612745406278151, -149.3125000000000284, -5.149110718188523173 ) ) ;
#19457 = ORIENTED_EDGE ( 'NONE', *, *, #13894, .F. ) ;
#19458 = CARTESIAN_POINT ( 'NONE',  ( 9.457646018065525792E-16, 28.93750000136559564, 5.148502694627439702 ) ) ;
#19459 = CARTESIAN_POINT ( 'NONE',  ( -49.85088928181150436, -127.6875000027312126, -1.666127454062680702 ) ) ;
#19460 = CARTESIAN_POINT ( 'NONE',  ( 1.975475456537005874E-15, -39.75000000000000000, 5.000000000000000000 ) ) ;
#19461 = CARTESIAN_POINT ( 'NONE',  ( -6.972266317189433020E-16, -36.25000000000000000, -5.000000000000000000 ) ) ;
#19462 = CARTESIAN_POINT ( 'NONE',  ( -2.229367062500000163, -58.47916666530106511, -3.861377020970580443 ) ) ;
#19463 = CARTESIAN_POINT ( 'NONE',  ( 3.093533885183100018, 6.874201416487501604, -7.446478553995813598 ) ) ;
#19464 = CARTESIAN_POINT ( 'NONE',  ( 2.229367062500001939, 16.02083333469892779, 3.861377020970579999 ) ) ;
#19465 = CARTESIAN_POINT ( 'NONE',  ( -6.972266317189433020E-16, 6.750000000000000000, -5.000000000000000000 ) ) ;
#19466 = CARTESIAN_POINT ( 'NONE',  ( 9.457646018065525792E-16, -48.31249999863440081, 5.148502694627439702 ) ) ;
#19467 = CARTESIAN_POINT ( 'NONE',  ( -2.500000000000000444, -8.041666663935481907, -4.330127018922193649 ) ) ;
#19468 = CARTESIAN_POINT ( 'NONE',  ( 1.339745962155615144, -31.70534180126147916, 4.999999999999999112 ) ) ;
#19469 = PLANE ( 'NONE',  #41934 ) ;
#19470 = CARTESIAN_POINT ( 'NONE',  ( 0.000000000000000000, -120.0000000000000000, 0.000000000000000000 ) ) ;
#19471 = CARTESIAN_POINT ( 'NONE',  ( 9.457646018065525792E-16, -106.0624999986343937, 5.148502694627439702 ) ) ;
#19472 = CARTESIAN_POINT ( 'NONE',  ( -4.458734124999999437, -9.562499998634406140, 0.000000000000000000 ) ) ;
#19473 = ORIENTED_EDGE ( 'NONE', *, *, #5906, .T. ) ;
#19474 = CARTESIAN_POINT ( 'NONE',  ( 1.975475456537005874E-15, -16.62499999726881583, 5.000000000000000000 ) ) ;
#19475 = CARTESIAN_POINT ( 'NONE',  ( 4.458734124999999437, -96.81249999863440792, -5.460374474430324690E-16 ) ) ;
#19476 = CARTESIAN_POINT ( 'NONE',  ( 5.000000000000000000, -160.1875000027311842, 2.071067811865478614 ) ) ;
#19477 = B_SPLINE_CURVE_WITH_KNOTS ( 'NONE', 3,
 ( #47646, #27087, #8109, #36742, #2340, #13562 ),
 .UNSPECIFIED., .F., .F.,
 ( 4, 2, 4 ),
 ( 0.004444412883774346255, 0.006655097293744437204, 0.008865781703714529019 ),
 .UNSPECIFIED. ) ;
#19478 = CARTESIAN_POINT ( 'NONE',  ( 4.458734124999998549, -97.97916666530105090, -2.574251347313721627 ) ) ;
#19479 = CARTESIAN_POINT ( 'NONE',  ( 2.500000000000002220, -49.54166666393547303, 4.330127018922192761 ) ) ;
#19480 = CARTESIAN_POINT ( 'NONE',  ( 1.060575238724906964E-15, -49.62499999726880873, 5.773502691896257311 ) ) ;
#19481 = CARTESIAN_POINT ( 'NONE',  ( -4.406842699996122548, 6.115962218725288224, 1.165517335421917267E-15 ) ) ;
#19482 =( BOUNDED_CURVE ( )  B_SPLINE_CURVE ( 2, ( #22320, #37425, #17498, #21691, #47079, #32275, #51282, #56425, #36160 ),
 .UNSPECIFIED., .F., .F. ) 
 B_SPLINE_CURVE_WITH_KNOTS ( ( 3, 2, 2, 2, 3 ),
 ( 0.8160714285714285587, 0.8166666666666666519, 0.8178571428571428381, 0.8190476190476190244, 0.8196428571428571175 ),
 .UNSPECIFIED. ) 
 CURVE ( )  GEOMETRIC_REPRESENTATION_ITEM ( )  RATIONAL_B_SPLINE_CURVE ( ( 0.9330127018922194093, 0.9330127018922194093, 1.000000000000000000, 0.8660254037844387076, 1.000000000000000000, 0.8660254037844387076, 1.000000000000000000, 0.9330127018922194093, 0.9330127018922194093 ) ) 
 REPRESENTATION_ITEM ( '' )  );
#19483 = CARTESIAN_POINT ( 'NONE',  ( -56.48576386720575471, -129.7500000013656063, -4.591703134518078322 ) ) ;
#19484 = CARTESIAN_POINT ( 'NONE',  ( -59.29741812935640155, -148.6250000013656063, -2.196230717870135685 ) ) ;
#19485 = CARTESIAN_POINT ( 'NONE',  ( 2.229367062499998831, -20.64583333196774007, -3.861377020970580887 ) ) ;
#19486 = CARTESIAN_POINT ( 'NONE',  ( -4.458734124999999437, 9.437500001365593860, 0.000000000000000000 ) ) ;
#19487 = CARTESIAN_POINT ( 'NONE',  ( -2.229367062500000163, -60.72916666530106511, -3.861377020970580443 ) ) ;
#19488 = CARTESIAN_POINT ( 'NONE',  ( -6.972266317189433020E-16, -94.12499999726880162, -5.000000000000000000 ) ) ;
#19489 = CARTESIAN_POINT ( 'NONE',  ( 2.229367062500001939, -15.97916666530107399, 3.861377020970579999 ) ) ;
#19490 = CARTESIAN_POINT ( 'NONE',  ( 5.000000000000000000, -156.0625000000000284, 2.071067811865478614 ) ) ;
#19491 = CARTESIAN_POINT ( 'NONE',  ( 5.000000000000000888, -7.583333333333330373, 2.886751345948126879 ) ) ;
#19492 = ORIENTED_EDGE ( 'NONE', *, *, #12505, .F. ) ;
#19493 = CARTESIAN_POINT ( 'NONE',  ( 4.458734125000000326, -41.14583333196773651, 2.574251347313718519 ) ) ;
#19494 = PRESENTATION_LAYER_ASSIGNMENT (  '', '', ( #31814 ) ) ;
#19495 = CARTESIAN_POINT ( 'NONE',  ( -2.558993250147282073, 7.638875775587784744, -7.593821156097241065 ) ) ;
#19496 = CARTESIAN_POINT ( 'NONE',  ( 1.975475456537005874E-15, -66.62499999726881583, 5.000000000000000000 ) ) ;
#19497 = CARTESIAN_POINT ( 'NONE',  ( 2.229367062499998831, -87.64583333196773651, -3.861377020970580887 ) ) ;
#19498 = CARTESIAN_POINT ( 'NONE',  ( -2.229367062499996610, 20.60416666803225993, 3.861377020970582219 ) ) ;
#19499 = VECTOR ( 'NONE', #45467, 1000.000000000000000 ) ;
#19500 = CARTESIAN_POINT ( 'NONE',  ( 2.229367062499998831, 8.354166668032261711, -3.861377020970580887 ) ) ;
#19501 =( BOUNDED_CURVE ( )  B_SPLINE_CURVE ( 2, ( #38281, #54011, #43717, #38577, #28618, #53066, #44351, #47917, #29237 ),
 .UNSPECIFIED., .F., .F. ) 
 B_SPLINE_CURVE_WITH_KNOTS ( ( 3, 2, 2, 2, 3 ),
 ( 0.9645833333333333481, 0.9652777777777777901, 0.9666666666666666741, 0.9680555555555555580, 0.9687500000000000000 ),
 .UNSPECIFIED. ) 
 CURVE ( )  GEOMETRIC_REPRESENTATION_ITEM ( )  RATIONAL_B_SPLINE_CURVE ( ( 0.9330127018922194093, 0.9330127018922194093, 1.000000000000000000, 0.8660254037844387076, 1.000000000000000000, 0.8660254037844387076, 1.000000000000000000, 0.9330127018922194093, 0.9330127018922194093 ) ) 
 REPRESENTATION_ITEM ( '' )  );
#19502 = DIRECTION ( 'NONE',  ( -0.000000000000000000, 1.000000000000000000, -0.000000000000000000 ) ) ;
#19503 = CARTESIAN_POINT ( 'NONE',  ( -5.000000000000000000, -7.083333333333330373, -2.886751345948128211 ) ) ;
#19504 = CARTESIAN_POINT ( 'NONE',  ( -4.458734124999997661, -89.47916666530105090, 2.574251347313722516 ) ) ;
#19505 = CARTESIAN_POINT ( 'NONE',  ( 4.458734125000001214, 21.85416666803225993, 2.574251347313718519 ) ) ;
#19506 = CARTESIAN_POINT ( 'NONE',  ( 5.000000000000000000, -74.50000000000000000, -6.123233995736766282E-16 ) ) ;
#19507 = CARTESIAN_POINT ( 'NONE',  ( 5.000000000000000000, 11.62500000273118594, -6.123233995736766282E-16 ) ) ;
#19508 = ORIENTED_EDGE ( 'NONE', *, *, #42212, .T. ) ;
#19509 = DIRECTION ( 'NONE',  ( 0.000000000000000000, 0.000000000000000000, 1.000000000000000000 ) ) ;
#19510 = VERTEX_POINT ( 'NONE', #11680 ) ;
#19511 = CARTESIAN_POINT ( 'NONE',  ( -5.000000000000000000, -34.00000000000000000, 0.000000000000000000 ) ) ;
#19512 = CARTESIAN_POINT ( 'NONE',  ( -4.458734124999999437, -37.31249999863440792, 0.000000000000000000 ) ) ;
#19513 = EDGE_CURVE ( 'NONE', #45731, #13785, #28034, .T. ) ;
#19514 = CARTESIAN_POINT ( 'NONE',  ( -2.499999999999996447, -33.70833333060213732, 4.330127018922195425 ) ) ;
#19516 = VERTEX_POINT ( 'NONE', #2374 ) ;
#19515 = CARTESIAN_POINT ( 'NONE',  ( 4.458734124999999437, -67.81249999863440792, -5.460374474430324690E-16 ) ) ;
#19517 = CARTESIAN_POINT ( 'NONE',  ( -57.19623071787017210, -151.6250000013656063, 4.297418129356382899 ) ) ;
#19518 = CARTESIAN_POINT ( 'NONE',  ( 4.458734124999998549, -10.72916666530106866, -2.574251347313721627 ) ) ;
#19520 = ORIENTED_EDGE ( 'NONE', *, *, #15680, .F. ) ;
#19519 = CARTESIAN_POINT ( 'NONE',  ( 4.458734124999998549, -14.97916666530107221, -2.574251347313721627 ) ) ;
#19521 = CARTESIAN_POINT ( 'NONE',  ( 5.000000000000000888, -81.58333333333332860, 2.886751345948126879 ) ) ;
#19522 = CARTESIAN_POINT ( 'NONE',  ( 1.975475456537005874E-15, -93.62499999726881583, 5.000000000000000000 ) ) ;
#19523 = CARTESIAN_POINT ( 'NONE',  ( 2.229367062500001939, -58.22916666530107932, 3.861377020970579999 ) ) ;
#19524 = CARTESIAN_POINT ( 'NONE',  ( 5.000000000000000888, -81.45833333060213022, 2.886751345948126879 ) ) ;
#19526 = ORIENTED_EDGE ( 'NONE', *, *, #27490, .F. ) ;
#19525 = DIRECTION ( 'NONE',  ( -0.000000000000000000, 1.000000000000000000, -0.000000000000000000 ) ) ;
#19527 = CARTESIAN_POINT ( 'NONE',  ( -59.81910112700025905, -145.1875000000000000, -2.462841084822630311 ) ) ;
#19528 = CARTESIAN_POINT ( 'NONE',  ( 2.229367062499998831, -28.89583333196774007, -3.861377020970580887 ) ) ;
#19529 = ORIENTED_EDGE ( 'NONE', *, *, #24137, .T. ) ;
#19530 = DIRECTION ( 'NONE',  ( 0.000000000000000000, 0.000000000000000000, 1.000000000000000000 ) ) ;
#19531 = CARTESIAN_POINT ( 'NONE',  ( 4.458734124999999437, -166.6875000013655779, 0.000000000000000000 ) ) ;
#19532 = CARTESIAN_POINT ( 'NONE',  ( -4.458734124999999437, -107.6458333319677365, -2.574251347313719407 ) ) ;
#19533 = CARTESIAN_POINT ( 'NONE',  ( -5.000000000000000000, -68.95833333060214443, -2.886751345948128211 ) ) ;
#19534 = EDGE_LOOP ( 'NONE', ( #27212, #10730, #21631, #37474 ) ) ;
#19535 = CARTESIAN_POINT ( 'NONE',  ( -59.59170313451810586, -147.7500000013656063, 1.485763867205729394 ) ) ;
#19536 = AXIS2_PLACEMENT_3D ( 'NONE', #3520, #41791, #27322 ) ;
#19537 = CARTESIAN_POINT ( 'NONE',  ( -51.75738570946856498, -138.8750000027312126, 3.805975901505576964 ) ) ;
#19538 = CARTESIAN_POINT ( 'NONE',  ( -2.229367062499996610, -37.14583333196773651, 3.861377020970582219 ) ) ;
#19539 = CARTESIAN_POINT ( 'NONE',  ( 4.458734124999997661, -145.7500000013656063, 1.846868145590737864 ) ) ;
#19540 = CARTESIAN_POINT ( 'NONE',  ( -2.500000000000000444, 22.83333333333333215, -4.330127018922193649 ) ) ;
#19541 = AXIS2_PLACEMENT_3D ( 'NONE', #31928, #12935, #51245 ) ;
#19542 = DIRECTION ( 'NONE',  ( -0.000000000000000000, 1.000000000000000000, -0.000000000000000000 ) ) ;
#19543 = CARTESIAN_POINT ( 'NONE',  ( 9.457646018065525792E-16, -14.06249999863440259, 5.148502694627439702 ) ) ;
#19544 = CARTESIAN_POINT ( 'NONE',  ( 4.458734124999998549, -98.97916666530105090, -2.574251347313721627 ) ) ;
#19545 = EDGE_LOOP ( 'NONE', ( #55115, #3209, #13159, #19861, #21837, #28676 ) ) ;
#19546 = CARTESIAN_POINT ( 'NONE',  ( -1.846868145590737420, -144.0000000013655779, 4.458734124999999437 ) ) ;
#19547 = CARTESIAN_POINT ( 'NONE',  ( 4.458734124999999437, -32.06249999863440792, -5.460374474430324690E-16 ) ) ;
#19548 = CARTESIAN_POINT ( 'NONE',  ( -56.66612745406273888, -153.3125000000000284, -5.149110718188518732 ) ) ;
#19549 = CARTESIAN_POINT ( 'NONE',  ( -59.44456063193725015, -134.5625000013656063, -0.3552334253322034230 ) ) ;
#19550 = CARTESIAN_POINT ( 'NONE',  ( -3.152548672688508926E-16, -69.81249999863439371, -5.148502694627439702 ) ) ;
#19551 = CARTESIAN_POINT ( 'NONE',  ( 1.975475456537005874E-15, -17.75000000000000355, 5.000000000000000000 ) ) ;
#19552 = DIRECTION ( 'NONE',  ( -0.000000000000000000, 1.000000000000000000, -0.000000000000000000 ) ) ;
#19553 = CARTESIAN_POINT ( 'NONE',  ( -4.606548227981510202, -6.456511556909259930, -7.591235721156638583 ) ) ;
#19554 = CARTESIAN_POINT ( 'NONE',  ( 4.458734124999998549, 7.020833334698928674, -2.574251347313721627 ) ) ;
#19555 =( BOUNDED_CURVE ( )  B_SPLINE_CURVE ( 2, ( #16420, #36038, #49231, #5173, #50185, #25751, #59533, #24790, #54704 ),
 .UNSPECIFIED., .F., .F. ) 
 B_SPLINE_CURVE_WITH_KNOTS ( ( 3, 2, 2, 2, 3 ),
 ( 0.1687500000000000111, 0.1694444444444444531, 0.1708333333333333370, 0.1722222222222222210, 0.1729166666666666630 ),
 .UNSPECIFIED. ) 
 CURVE ( )  GEOMETRIC_REPRESENTATION_ITEM ( )  RATIONAL_B_SPLINE_CURVE ( ( 0.9330127018922194093, 0.9330127018922194093, 1.000000000000000000, 0.8660254037844387076, 1.000000000000000000, 0.8660254037844387076, 1.000000000000000000, 0.9330127018922194093, 0.9330127018922194093 ) ) 
 REPRESENTATION_ITEM ( '' )  );
#19556 = ORIENTED_EDGE ( 'NONE', *, *, #11474, .T. ) ;
#19557 =( NAMED_UNIT ( * ) SI_UNIT ( $, .STERADIAN. ) SOLID_ANGLE_UNIT ( ) );
#19558 = CARTESIAN_POINT ( 'NONE',  ( 0.000000000000000000, -170.0000000000000000, 0.000000000000000000 ) ) ;
#19560 = CARTESIAN_POINT ( 'NONE',  ( -2.229367062500000163, -29.47916666530107221, -3.861377020970580443 ) ) ;
#19559 = CARTESIAN_POINT ( 'NONE',  ( -5.000000000000000000, -97.08333333333332860, -2.886751345948128211 ) ) ;
#19561 = CARTESIAN_POINT ( 'NONE',  ( -6.972266317189433020E-16, -95.25000000000000000, -5.000000000000000000 ) ) ;
#19562 = CARTESIAN_POINT ( 'NONE',  ( 2.229367062500001939, -77.22916666530106511, 3.861377020970579999 ) ) ;
#19563 = CARTESIAN_POINT ( 'NONE',  ( -4.458734124999997661, 23.52083333469892779, 2.574251347313722516 ) ) ;
#19564 = CARTESIAN_POINT ( 'NONE',  ( 6.042630808230842148E-15, 26.75000000000000000, -4.999999999999999112 ) ) ;
#19565 = CARTESIAN_POINT ( 'NONE',  ( -50.40829686548195099, -143.0000000013655779, -1.485763867205728284 ) ) ;
#19566 = CARTESIAN_POINT ( 'NONE',  ( 9.457646018065525792E-16, -1.062499998634405696, 5.148502694627439702 ) ) ;
#19567 = CARTESIAN_POINT ( 'NONE',  ( 4.458734125000001214, 27.85416666803225993, 2.574251347313718519 ) ) ;
#19568 = CARTESIAN_POINT ( 'NONE',  ( -4.458734124999999437, -45.56249999863440081, 0.000000000000000000 ) ) ;
#19569 = CARTESIAN_POINT ( 'NONE',  ( 5.000000000000000888, -43.45833333060214443, 2.886751345948126879 ) ) ;
#19570 = CARTESIAN_POINT ( 'NONE',  ( 4.458734124999998549, 1.270833334698927342, -2.574251347313721627 ) ) ;
#19571 = VERTEX_POINT ( 'NONE', #1113 ) ;
#19572 = CARTESIAN_POINT ( 'NONE',  ( 2.229367062500001939, -23.22916666530107221, 3.861377020970579999 ) ) ;
#19573 = CARTESIAN_POINT ( 'NONE',  ( -4.458734124999999437, -69.39583333196773651, -2.574251347313719407 ) ) ;
#19574 = CARTESIAN_POINT ( 'NONE',  ( -2.500000000000000444, -105.0416666639354730, -4.330127018922193649 ) ) ;
#19575 = CARTESIAN_POINT ( 'NONE',  ( -2.229367062499996610, 25.85416666803225993, 3.861377020970582219 ) ) ;
#19576 = CARTESIAN_POINT ( 'NONE',  ( -5.000000000000000000, 9.999999999999998224, 0.000000000000000000 ) ) ;
#19577 = CARTESIAN_POINT ( 'NONE',  ( 2.229367062500001939, -110.2291666653010651, 3.861377020970579999 ) ) ;
#19578 = CARTESIAN_POINT ( 'NONE',  ( -4.458734124999997661, -73.47916666530106511, 2.574251347313722516 ) ) ;
#19579 = CARTESIAN_POINT ( 'NONE',  ( -4.999999999999999112, -59.91666666666665719, 2.886751345948131764 ) ) ;
#19580 = DIRECTION ( 'NONE',  ( -0.000000000000000000, 1.000000000000000000, -0.000000000000000000 ) ) ;
#19581 = FACE_OUTER_BOUND ( 'NONE', #21774, .T. ) ;
#19582 = VERTEX_POINT ( 'NONE', #20720 ) ;
#19583 = CARTESIAN_POINT ( 'NONE',  ( -2.071067811865432873, -140.6875000000000284, -5.000000000000041744 ) ) ;
#19584 =( BOUNDED_CURVE ( )  B_SPLINE_CURVE ( 2, ( #50888, #45743, #10686, #16152, #6830, #31579, #46380, #50568, #35778 ),
 .UNSPECIFIED., .F., .F. ) 
 B_SPLINE_CURVE_WITH_KNOTS ( ( 3, 2, 2, 2, 3 ),
 ( 0.1839285714285714413, 0.1845238095238095344, 0.1857142857142857206, 0.1869047619047619069, 0.1875000000000000000 ),
 .UNSPECIFIED. ) 
 CURVE ( )  GEOMETRIC_REPRESENTATION_ITEM ( )  RATIONAL_B_SPLINE_CURVE ( ( 0.9330127018922194093, 0.9330127018922209636, 1.000000000000000000, 0.8660254037844387076, 1.000000000000000000, 0.8660254037844387076, 1.000000000000000000, 0.9330127018922194093, 0.9330127018922194093 ) ) 
 REPRESENTATION_ITEM ( '' )  );
#19585 = CARTESIAN_POINT ( 'NONE',  ( -1.339745962155599601, 12.79465819873851906, -5.000000000000007994 ) ) ;
#19586 = CARTESIAN_POINT ( 'NONE',  ( -5.000000000000000000, -20.08333333333333215, -2.886751345948128211 ) ) ;
#19587 = CARTESIAN_POINT ( 'NONE',  ( 9.457646018065525792E-16, -24.06249999863440436, 5.148502694627439702 ) ) ;
#19588 = VECTOR ( 'NONE', #30340, 1000.000000000000000 ) ;
#19589 = ADVANCED_FACE ( 'NONE', ( #31627 ), #49970, .F. ) ;
#19590 = CARTESIAN_POINT ( 'NONE',  ( 4.458734124999999437, -83.81249999863439371, -5.460374474430324690E-16 ) ) ;
#19591 = CARTESIAN_POINT ( 'NONE',  ( -4.458734125000000326, -169.2500000013655779, -1.846868145590735644 ) ) ;
#19592 = CARTESIAN_POINT ( 'NONE',  ( 5.000000000000000000, -18.29166666393548013, -2.886751345948129988 ) ) ;
#19594 = ORIENTED_EDGE ( 'NONE', *, *, #58893, .F. ) ;
#19593 = CARTESIAN_POINT ( 'NONE',  ( 4.458734125000001214, -49.89583333196772941, 2.574251347313718519 ) ) ;
#19595 = CARTESIAN_POINT ( 'NONE',  ( 2.500000000000002220, 5.333333333333332149, 4.330127018922192761 ) ) ;
#19596 = CARTESIAN_POINT ( 'NONE',  ( 6.123233995736766282E-16, -120.0000000000000000, -5.000000000000000000 ) ) ;
#19598 = ORIENTED_EDGE ( 'NONE', *, *, #16874, .F. ) ;
#19597 = CARTESIAN_POINT ( 'NONE',  ( -4.458734124999998549, 2.520833334698928674, 2.574251347313722516 ) ) ;
#19599 = FACE_OUTER_BOUND ( 'NONE', #47407, .T. ) ;
#19600 = CARTESIAN_POINT ( 'NONE',  ( -2.499999999999996447, -68.83333333333332860, 4.330127018922195425 ) ) ;
#19601 = CARTESIAN_POINT ( 'NONE',  ( 3.152801135295366208, -154.8125000013656063, 3.152801135295367985 ) ) ;
#19602 = CARTESIAN_POINT ( 'NONE',  ( -4.458734124999998549, -39.47916666530107932, 2.574251347313722516 ) ) ;
#19603 = CARTESIAN_POINT ( 'NONE',  ( 2.499999999999998668, -14.33333333333333037, -4.330127018922193649 ) ) ;
#19604 = CARTESIAN_POINT ( 'NONE',  ( -9.184850993605147944E-16, -164.2500000000000000, 5.000000000000000000 ) ) ;
#19605 = CARTESIAN_POINT ( 'NONE',  ( -4.999999999999998224, 11.08333333333333393, 2.886751345948131764 ) ) ;
#19606 = CARTESIAN_POINT ( 'NONE',  ( -59.59170313451811296, -128.7500000013656063, 1.485763867205729394 ) ) ;
#19607 = CARTESIAN_POINT ( 'NONE',  ( -2.229367062500000163, -10.72916666530106866, -3.861377020970580443 ) ) ;
#19608 = CARTESIAN_POINT ( 'NONE',  ( -3.152548672688508926E-16, -47.81249999863440792, -5.148502694627439702 ) ) ;
#19609 = CARTESIAN_POINT ( 'NONE',  ( -5.000000000000000000, -7.958333330602144429, -2.886751345948128211 ) ) ;
#19610 = CARTESIAN_POINT ( 'NONE',  ( -4.458734125000001214, -146.8750000013656063, 1.846868145590734089 ) ) ;
#19611 = EDGE_CURVE ( 'NONE', #7250, #23647, #16198, .T. ) ;
#19612 = CARTESIAN_POINT ( 'NONE',  ( 4.458734124999999437, -87.06249999863439371, -5.460374474430324690E-16 ) ) ;
#19613 = CARTESIAN_POINT ( 'NONE',  ( -59.98410592259440222, -143.1250000000000284, -0.3983568153799752487 ) ) ;
#19614 = ORIENTED_EDGE ( 'NONE', *, *, #33496, .F. ) ;
#19615 = CARTESIAN_POINT ( 'NONE',  ( 5.000000000000000000, -19.29166666393548013, -2.886751345948130876 ) ) ;
#19616 = CYLINDRICAL_SURFACE ( 'NONE', #28238, 5.000000000000000000 ) ;
#19617 = CARTESIAN_POINT ( 'NONE',  ( -53.33387254593733928, -150.9375000027311842, 5.149110718188519620 ) ) ;
#19618 = CARTESIAN_POINT ( 'NONE',  ( 2.499999999999998668, -38.33333333333332860, -4.330127018922193649 ) ) ;
#19619 = EDGE_LOOP ( 'NONE', ( #57068, #41829, #42609, #42185 ) ) ;
#19620 = ADVANCED_FACE ( 'NONE', ( #36453 ), #45701, .F. ) ;
#19621 = CARTESIAN_POINT ( 'NONE',  ( -4.458734124999998549, 0.7708333346989267865, 2.574251347313722516 ) ) ;
#19622 = CARTESIAN_POINT ( 'NONE',  ( 5.000000000000000888, -78.58333333333334281, 2.886751345948126879 ) ) ;
#19623 = CARTESIAN_POINT ( 'NONE',  ( -2.229367062499996610, -15.39583333196773651, 3.861377020970582219 ) ) ;
#19624 = CARTESIAN_POINT ( 'NONE',  ( -2.500000000000000444, -51.16666666666666430, -4.330127018922193649 ) ) ;
#19625 = CARTESIAN_POINT ( 'NONE',  ( 2.229367062500001939, -1.979166665301068662, 3.861377020970579999 ) ) ;
#19626 = FACE_OUTER_BOUND ( 'NONE', #15975, .T. ) ;
#19627 = CARTESIAN_POINT ( 'NONE',  ( -3.152801135295367985, -151.8125000013655779, 3.152801135295367096 ) ) ;
#19628 = CARTESIAN_POINT ( 'NONE',  ( 4.458734124999998549, 19.02083333469892779, -2.574251347313721627 ) ) ;
#19629 = EDGE_LOOP ( 'NONE', ( #14448, #23109, #40407, #34517 ) ) ;
#19630 = CARTESIAN_POINT ( 'NONE',  ( 4.458734124999998549, -97.72916666530105090, -2.574251347313721627 ) ) ;
#19631 = FACE_OUTER_BOUND ( 'NONE', #11634, .T. ) ;
#19632 = CARTESIAN_POINT ( 'NONE',  ( -2.229367062499996610, -14.14583333196774184, 3.861377020970582219 ) ) ;
#19633 = CARTESIAN_POINT ( 'NONE',  ( -6.972266317189433020E-16, -99.12499999726880162, -5.000000000000000000 ) ) ;
#19634 = CARTESIAN_POINT ( 'NONE',  ( 5.000000000000000000, 29.58333333333332860, -2.886751345948130876 ) ) ;
#19635 = CARTESIAN_POINT ( 'NONE',  ( -50.55543936806279248, -154.0625000013656347, 0.3552334253322060320 ) ) ;
#19636 = EDGE_CURVE ( 'NONE', #38838, #13440, #35506, .T. ) ;
#19637 = CARTESIAN_POINT ( 'NONE',  ( 5.000000000000000888, -42.45833333060214443, 2.886751345948126879 ) ) ;
#19638 = CARTESIAN_POINT ( 'NONE',  ( 1.975475456537005874E-15, -67.62499999726881583, 5.000000000000000000 ) ) ;
#19639 = CARTESIAN_POINT ( 'NONE',  ( -3.152548672688508926E-16, 16.43750000136559564, -5.148502694627439702 ) ) ;
#19640 = CARTESIAN_POINT ( 'NONE',  ( -1.339745962155613812, -95.20534180126148271, -5.000000000000000000 ) ) ;
#19641 = EDGE_LOOP ( 'NONE', ( #20274, #60937, #30621, #10673 ) ) ;
#19642 = CARTESIAN_POINT ( 'NONE',  ( -2.229367062499996610, 17.85416666803225993, 3.861377020970582219 ) ) ;
#19643 = CARTESIAN_POINT ( 'NONE',  ( -4.458734124999999437, -63.31249999863440792, 0.000000000000000000 ) ) ;
#19644 = CARTESIAN_POINT ( 'NONE',  ( -2.229367062500000163, -9.729166665301068662, -3.861377020970580443 ) ) ;
#19645 = FACE_OUTER_BOUND ( 'NONE', #41957, .T. ) ;
#19646 = CARTESIAN_POINT ( 'NONE',  ( -5.000000000000000000, 6.916666666666664298, -2.886751345948128211 ) ) ;
#19647 = CARTESIAN_POINT ( 'NONE',  ( 2.730187237215162345E-16, -169.1875000013656063, -4.458734124999999437 ) ) ;
#19648 = CARTESIAN_POINT ( 'NONE',  ( -4.999999999999998224, -59.79166666393547303, 2.886751345948131764 ) ) ;
#19649 = CARTESIAN_POINT ( 'NONE',  ( -4.458734124999999437, -53.39583333196773651, -2.574251347313719407 ) ) ;
#19650 = CARTESIAN_POINT ( 'NONE',  ( -5.000000000000000000, -88.87499999726880162, 0.000000000000000000 ) ) ;
#19651 = CARTESIAN_POINT ( 'NONE',  ( 4.458734125000000326, -31.89583333196773651, 2.574251347313718519 ) ) ;
#19652 = CARTESIAN_POINT ( 'NONE',  ( -4.174999999999999822, 5.112900386440199535E-16, -0.5776712190230133270 ) ) ;
#19653 = FACE_OUTER_BOUND ( 'NONE', #6391, .T. ) ;
#19654 = CARTESIAN_POINT ( 'NONE',  ( 1.846868145590736310, -151.8750000013655779, 4.458734124999997661 ) ) ;
#19655 = CARTESIAN_POINT ( 'NONE',  ( -2.500000000000000444, -40.16666666666667140, -4.330127018922193649 ) ) ;
#19656 = CYLINDRICAL_SURFACE ( 'NONE', #32604, 5.000000000000000000 ) ;
#19657 = LINE ( 'NONE', #39269, #20200 ) ;
#19658 = ORIENTED_EDGE ( 'NONE', *, *, #5512, .F. ) ;
#19659 = CARTESIAN_POINT ( 'NONE',  ( 2.229367062499998831, -103.6458333319677365, -3.861377020970580887 ) ) ;
#19660 = CARTESIAN_POINT ( 'NONE',  ( 2.229367062500001939, 0.7708333346989268975, 3.861377020970579999 ) ) ;
#19661 = CARTESIAN_POINT ( 'NONE',  ( 1.339745962155612702, -80.29465819873850307, -5.000000000000000000 ) ) ;
#19662 = CARTESIAN_POINT ( 'NONE',  ( -2.500000000000000444, -3.166666666666664742, -4.330127018922193649 ) ) ;
#19663 = EDGE_CURVE ( 'NONE', #20660, #54885, #32545, .T. ) ;
#19664 = CARTESIAN_POINT ( 'NONE',  ( 4.458734124999999437, -66.81249999863440792, -5.460374474430324690E-16 ) ) ;
#19665 = CARTESIAN_POINT ( 'NONE',  ( -4.999999999999998224, 20.08333333333333925, 2.886751345948131764 ) ) ;
#19666 = EDGE_CURVE ( 'NONE', #16025, #34977, #32164, .T. ) ;
#19667 = EDGE_CURVE ( 'NONE', #52091, #26939, #21967, .T. ) ;
#19668 = CARTESIAN_POINT ( 'NONE',  ( -2.499999999999996447, -0.7083333306021483144, 4.330127018922195425 ) ) ;
#19670 = ORIENTED_EDGE ( 'NONE', *, *, #12639, .F. ) ;
#19669 = CARTESIAN_POINT ( 'NONE',  ( 4.458734124999999437, -34.81249999863440792, -5.460374474430324690E-16 ) ) ;
#19671 = CARTESIAN_POINT ( 'NONE',  ( 1.339745962155612702, 17.83034180399266688, -5.000000000000000000 ) ) ;
#19672 = DIRECTION ( 'NONE',  ( 1.000000000000000000, 0.000000000000000000, 0.000000000000000000 ) ) ;
#19673 = FACE_OUTER_BOUND ( 'NONE', #52638, .T. ) ;
#19674 = CARTESIAN_POINT ( 'NONE',  ( 5.000000000000000000, -43.41666666666666430, -2.886751345948129988 ) ) ;
#19676 = CARTESIAN_POINT ( 'NONE',  ( 4.458734124999998549, -22.97916666530107221, -2.574251347313721627 ) ) ;
#19675 = FACE_OUTER_BOUND ( 'NONE', #51505, .T. ) ;
#19677 = CARTESIAN_POINT ( 'NONE',  ( 5.000000000000000000, -64.41666666666665719, -2.886751345948130876 ) ) ;
#19678 = CARTESIAN_POINT ( 'NONE',  ( 4.458734124999998549, -71.72916666530107932, -2.574251347313721627 ) ) ;
#19679 = CARTESIAN_POINT ( 'NONE',  ( 1.846868145590735200, -144.5000000013656063, -4.458734125000000326 ) ) ;
#19680 = CARTESIAN_POINT ( 'NONE',  ( -4.458734124999998549, -80.22916666530106511, 2.574251347313722516 ) ) ;
#19681 = CARTESIAN_POINT ( 'NONE',  ( -50.40829686548195099, -138.2500000013656063, -1.485763867205728284 ) ) ;
#19682 = EDGE_CURVE ( 'NONE', #15117, #12901, #31943, .T. ) ;
#19683 = CARTESIAN_POINT ( 'NONE',  ( 4.458734125000001214, -30.14583333196773296, 2.574251347313718519 ) ) ;
#19684 =( BOUNDED_CURVE ( )  B_SPLINE_CURVE ( 2, ( #5470, #39866, #25407, #45347, #1314, #15119, #993, #50498, #19936 ),
 .UNSPECIFIED., .F., .F. ) 
 B_SPLINE_CURVE_WITH_KNOTS ( ( 3, 2, 2, 2, 3 ),
 ( 0.5660714285714285587, 0.5666666666666666519, 0.5678571428571428381, 0.5690476190476190244, 0.5696428571428571175 ),
 .UNSPECIFIED. ) 
 CURVE ( )  GEOMETRIC_REPRESENTATION_ITEM ( )  RATIONAL_B_SPLINE_CURVE ( ( 0.9330127018922194093, 0.9330127018922194093, 1.000000000000000000, 0.8660254037844387076, 1.000000000000000000, 0.8660254037844387076, 1.000000000000000000, 0.9330127018922194093, 0.9330127018922194093 ) ) 
 REPRESENTATION_ITEM ( '' )  );
#19685 = CARTESIAN_POINT ( 'NONE',  ( -2.500000000000000444, -72.04166666393548724, -4.330127018922193649 ) ) ;
#19686 = ORIENTED_EDGE ( 'NONE', *, *, #46687, .T. ) ;
#19687 = CARTESIAN_POINT ( 'NONE',  ( -5.000000000000000000, -82.95833333060214443, -2.886751345948128211 ) ) ;
#19689 = ORIENTED_EDGE ( 'NONE', *, *, #21290, .T. ) ;
#19688 = ADVANCED_FACE ( 'NONE', ( #62497 ), #42222, .T. ) ;
#19690 = CARTESIAN_POINT ( 'NONE',  ( -3.152548672688508926E-16, -75.81249999863440792, -5.148502694627439702 ) ) ;
#19691 = CARTESIAN_POINT ( 'NONE',  ( -50.18089887299978358, -150.6875000000000000, 2.462841084822575688 ) ) ;
#19692 = PRESENTATION_STYLE_ASSIGNMENT (( #29653 ) ) ;
#19693 = ORIENTED_EDGE ( 'NONE', *, *, #11189, .F. ) ;
#19694 = CARTESIAN_POINT ( 'NONE',  ( 5.000000000000000000, 12.58333333333333215, -2.886751345948130876 ) ) ;
#19695 = CARTESIAN_POINT ( 'NONE',  ( 0.000000000000000000, -120.0000000000000000, 5.000000000000000000 ) ) ;
#19696 = CARTESIAN_POINT ( 'NONE',  ( -2.229367062500000163, -58.72916666530106511, -3.861377020970580443 ) ) ;
#19697 = CARTESIAN_POINT ( 'NONE',  ( 9.457646018065525792E-16, 2.687500001365594304, 5.148502694627439702 ) ) ;
#19698 = VERTEX_POINT ( 'NONE', #61867 ) ;
#19699 = CARTESIAN_POINT ( 'NONE',  ( 6.123233995736766282E-16, -120.0000000000000000, -5.000000000000000000 ) ) ;
#19700 = CARTESIAN_POINT ( 'NONE',  ( -2.480964764533239819E-13, -107.7500000000000000, 5.000000000000000000 ) ) ;
#19701 = CARTESIAN_POINT ( 'NONE',  ( -2.229367062500000163, 12.52083333469892601, -3.861377020970580443 ) ) ;
#19702 = CARTESIAN_POINT ( 'NONE',  ( -57.19623071787017210, -142.3750000013656063, 4.297418129356382899 ) ) ;
#19703 = CARTESIAN_POINT ( 'NONE',  ( 5.000000000000000888, -47.45833333060215153, 2.886751345948126879 ) ) ;
#19704 = CARTESIAN_POINT ( 'NONE',  ( 2.730187237215162345E-16, -165.1875000013655779, -4.458734124999999437 ) ) ;
#19705 = VERTEX_POINT ( 'NONE', #28063 ) ;
#19706 = CARTESIAN_POINT ( 'NONE',  ( -4.458734124999999437, -83.31249999863439371, 0.000000000000000000 ) ) ;
#19707 = CARTESIAN_POINT ( 'NONE',  ( 1.339745962155612702, -39.29465819873851729, -5.000000000000000000 ) ) ;
#19708 = CARTESIAN_POINT ( 'NONE',  ( -3.152548672688508926E-16, 3.437500001365594748, -5.148502694627439702 ) ) ;
#19709 = CARTESIAN_POINT ( 'NONE',  ( -2.499999999999996447, -85.83333333333332860, 4.330127018922195425 ) ) ;
#19710 = CARTESIAN_POINT ( 'NONE',  ( 5.000000000000000888, -19.45833333060214798, 2.886751345948126879 ) ) ;
#19711 = CARTESIAN_POINT ( 'NONE',  ( -2.229367062500000163, -64.72916666530106511, -3.861377020970580443 ) ) ;
#19712 = CARTESIAN_POINT ( 'NONE',  ( -2.499999999999996447, -25.70833333060214798, 4.330127018922195425 ) ) ;
#19713 = CARTESIAN_POINT ( 'NONE',  ( 2.493747252781420335E-13, -42.25000000000000711, -5.000000000000000000 ) ) ;
#19714 = CARTESIAN_POINT ( 'NONE',  ( 2.229367062500001939, 28.02083333469892779, 3.861377020970579999 ) ) ;
#19715 = CARTESIAN_POINT ( 'NONE',  ( -6.972266317189433020E-16, 4.749999999999999112, -5.000000000000000000 ) ) ;
#19716 = CARTESIAN_POINT ( 'NONE',  ( 2.500000000000002220, -3.541666663935478354, 4.330127018922192761 ) ) ;
#19717 = CARTESIAN_POINT ( 'NONE',  ( 4.458734124999998549, -44.72916666530106511, -2.574251347313721627 ) ) ;
#19718 = CARTESIAN_POINT ( 'NONE',  ( 9.457646018065525792E-16, -33.31249999863440792, 5.148502694627439702 ) ) ;
#19719 = CARTESIAN_POINT ( 'NONE',  ( 2.229367062499998831, 7.104166668032259935, -3.861377020970580887 ) ) ;
#19720 = DIRECTION ( 'NONE',  ( -0.000000000000000000, 1.000000000000000000, -0.000000000000000000 ) ) ;
#19721 = CARTESIAN_POINT ( 'NONE',  ( -5.000000000000000000, 24.91666666666666430, -2.886751345948128211 ) ) ;
#19722 = CARTESIAN_POINT ( 'NONE',  ( 3.535533905932738197, -150.0000000027312126, -3.535533905932738197 ) ) ;
#19723 = CARTESIAN_POINT ( 'NONE',  ( 1.975475456537005874E-15, -14.62499999726881228, 5.000000000000000000 ) ) ;
#19724 = CARTESIAN_POINT ( 'NONE',  ( -2.229367062500000163, -35.47916666530107221, -3.861377020970580443 ) ) ;
#19725 = CARTESIAN_POINT ( 'NONE',  ( 2.499999999999998668, -74.20833333060214443, -4.330127018922193649 ) ) ;
#19726 = CARTESIAN_POINT ( 'NONE',  ( -52.80376928212989185, -145.1250000013655779, -4.297418129356379346 ) ) ;
#19727 = CARTESIAN_POINT ( 'NONE',  ( -5.000000000000000888, -144.5625000000000000, -2.071067811865475949 ) ) ;
#19728 = CARTESIAN_POINT ( 'NONE',  ( 4.458734124999999437, -75.06249999863440792, -5.460374474430324690E-16 ) ) ;
#19729 = CARTESIAN_POINT ( 'NONE',  ( -1.846868145590734756, -165.3750000013656347, -4.458734124999999437 ) ) ;
#19731 =( BOUNDED_CURVE ( )  B_SPLINE_CURVE ( 2, ( #61090, #52916, #17012, #31799, #60456, #62270, #12185, #32990, #8542 ),
 .UNSPECIFIED., .F., .F. ) 
 B_SPLINE_CURVE_WITH_KNOTS ( ( 3, 2, 2, 2, 3 ),
 ( 0.2053571428571428492, 0.2059523809523809423, 0.2071428571428571563, 0.2083333333333333426, 0.2089285714285714357 ),
 .UNSPECIFIED. ) 
 CURVE ( )  GEOMETRIC_REPRESENTATION_ITEM ( )  RATIONAL_B_SPLINE_CURVE ( ( 0.9330127018922194093, 0.9330127018922194093, 1.000000000000000000, 0.8660254037844387076, 1.000000000000000000, 0.8660254037844387076, 1.000000000000000000, 0.9330127018922194093, 0.9330127018922194093 ) ) 
 REPRESENTATION_ITEM ( '' )  );
#19730 = CARTESIAN_POINT ( 'NONE',  ( -4.458734124999997661, -36.22916666530106511, 2.574251347313722516 ) ) ;
#19732 = CARTESIAN_POINT ( 'NONE',  ( 0.000000000000000000, -170.0000000000000000, 0.000000000000000000 ) ) ;
#19733 = CARTESIAN_POINT ( 'NONE',  ( 2.499999999999998668, -24.33333333333333215, -4.330127018922193649 ) ) ;
#19734 = CARTESIAN_POINT ( 'NONE',  ( -1.846868145590737420, -142.7500000013656063, 4.458734124999999437 ) ) ;
#19735 = EDGE_LOOP ( 'NONE', ( #33645, #3689, #2137, #40723 ) ) ;
#19736 = CARTESIAN_POINT ( 'NONE',  ( -2.229367062499996610, 28.60416666803226349, 3.861377020970582219 ) ) ;
#19737 = ORIENTED_EDGE ( 'NONE', *, *, #13729, .F. ) ;
#19738 = CARTESIAN_POINT ( 'NONE',  ( 4.458734124999998549, -60.97916666530106511, -2.574251347313721627 ) ) ;
#19739 =( BOUNDED_CURVE ( )  B_SPLINE_CURVE ( 2, ( #14302, #4971, #19118, #53548, #9472, #39373, #59004, #14932, #34539 ),
 .UNSPECIFIED., .F., .F. ) 
 B_SPLINE_CURVE_WITH_KNOTS ( ( 3, 2, 2, 2, 3 ),
 ( 0.6910714285714285587, 0.6916666666666666519, 0.6928571428571428381, 0.6940476190476190244, 0.6946428571428571175 ),
 .UNSPECIFIED. ) 
 CURVE ( )  GEOMETRIC_REPRESENTATION_ITEM ( )  RATIONAL_B_SPLINE_CURVE ( ( 0.9330127018922194093, 0.9330127018922194093, 1.000000000000000000, 0.8660254037844387076, 1.000000000000000000, 0.8660254037844387076, 1.000000000000000000, 0.9330127018922194093, 0.9330127018922194093 ) ) 
 REPRESENTATION_ITEM ( '' )  );
#19740 = CARTESIAN_POINT ( 'NONE',  ( 2.499999999999998668, 23.79166666939785202, -4.330127018922193649 ) ) ;
#19741 = LINE ( 'NONE', #44820, #10365 ) ;
#19742 = CARTESIAN_POINT ( 'NONE',  ( -2.500000000000000444, 16.83333333333333215, -4.330127018922193649 ) ) ;
#19743 = CARTESIAN_POINT ( 'NONE',  ( 2.229367062500001939, -52.97916666530107221, 3.861377020970579999 ) ) ;
#19744 = CARTESIAN_POINT ( 'NONE',  ( 2.229367062499998831, -6.645833331967741842, -3.861377020970580887 ) ) ;
#19745 = DIRECTION ( 'NONE',  ( -0.000000000000000000, -1.000000000000000000, -0.000000000000000000 ) ) ;
#19746 = EDGE_CURVE ( 'NONE', #1698, #63455, #47991, .T. ) ;
#19747 = CARTESIAN_POINT ( 'NONE',  ( 6.123233995736766282E-16, -170.0000000000000000, -5.000000000000000000 ) ) ;
#19748 = CARTESIAN_POINT ( 'NONE',  ( 6.123233995736766282E-16, -120.0000000000000000, -5.000000000000000000 ) ) ;
#19749 = CARTESIAN_POINT ( 'NONE',  ( 1.975475456537005874E-15, -53.62499999726880162, 5.000000000000000000 ) ) ;
#19751 = CARTESIAN_POINT ( 'NONE',  ( -2.229367062499996610, -19.14583333196774007, 3.861377020970582219 ) ) ;
#19750 = CARTESIAN_POINT ( 'NONE',  ( -1.339745962155610925, 5.205341801261479162, 5.000000000000000000 ) ) ;
#19752 = CARTESIAN_POINT ( 'NONE',  ( -56.66612745406251861, -135.3125000000000284, -5.149110718188501856 ) ) ;
#19753 = CARTESIAN_POINT ( 'NONE',  ( -3.152548672688508926E-16, -52.56249999863440792, -5.148502694627439702 ) ) ;
#19754 = CARTESIAN_POINT ( 'NONE',  ( 3.152801135295367541, -156.5625000013656063, -3.152801135295367541 ) ) ;
#19755 = EDGE_CURVE ( 'NONE', #1513, #26750, #30469, .T. ) ;
#19756 = CARTESIAN_POINT ( 'NONE',  ( -3.535250795749689387E-16, -53.12499999726881583, -5.773502691896257311 ) ) ;
#19757 = ORIENTED_EDGE ( 'NONE', *, *, #1109, .F. ) ;
#19758 = CARTESIAN_POINT ( 'NONE',  ( 2.499999999999998668, -26.33333333333333215, -4.330127018922193649 ) ) ;
#19759 = CARTESIAN_POINT ( 'NONE',  ( -2.229367062499996610, 5.604166668032261711, 3.861377020970582219 ) ) ;
#19760 = ORIENTED_EDGE ( 'NONE', *, *, #54778, .F. ) ;
#19762 = CARTESIAN_POINT ( 'NONE',  ( 0.000000000000000000, -170.0000000000000000, 0.000000000000000000 ) ) ;
#19761 = CARTESIAN_POINT ( 'NONE',  ( -6.972266317189433020E-16, -7.124999997268814056, -5.000000000000000000 ) ) ;
#19763 = CARTESIAN_POINT ( 'NONE',  ( 4.458734125000000326, -155.3750000013656347, -1.846868145590734978 ) ) ;
#19764 = EDGE_CURVE ( 'NONE', #14049, #57389, #17464, .T. ) ;
#19765 = ORIENTED_EDGE ( 'NONE', *, *, #59330, .T. ) ;
#19766 = ADVANCED_FACE ( 'NONE', ( #13272 ), #32896, .T. ) ;
#19767 = CARTESIAN_POINT ( 'NONE',  ( -2.500000000000000444, 10.83333333333333393, -4.330127018922193649 ) ) ;
#19768 = CARTESIAN_POINT ( 'NONE',  ( -56.66612745406270335, -133.3125000000000284, -5.149110718188516067 ) ) ;
#19769 = FACE_OUTER_BOUND ( 'NONE', #13062, .T. ) ;
#19770 = CARTESIAN_POINT ( 'NONE',  ( -4.458734124999999437, -45.64583333196774362, -2.574251347313719407 ) ) ;
#19771 = ORIENTED_EDGE ( 'NONE', *, *, #51233, .F. ) ;
#19772 = ADVANCED_FACE ( 'NONE', ( #49573 ), #29948, .T. ) ;
#19773 = CARTESIAN_POINT ( 'NONE',  ( 0.000000000000000000, -120.0000000000000000, 5.000000000000000000 ) ) ;
#19774 = CARTESIAN_POINT ( 'NONE',  ( -4.458734124999998549, 17.77083333469892779, 2.574251347313722516 ) ) ;
#19775 = CARTESIAN_POINT ( 'NONE',  ( -6.972266317189433020E-16, -10.12499999726881406, -5.000000000000000000 ) ) ;
#19776 = VERTEX_POINT ( 'NONE', #39594 ) ;
#19777 = CARTESIAN_POINT ( 'NONE',  ( -4.458734124999999437, 29.60416666803225993, -2.574251347313719407 ) ) ;
#19778 = CARTESIAN_POINT ( 'NONE',  ( -56.66612745406270335, -126.4375000027312410, -5.149110718188516067 ) ) ;
#19779 = DIRECTION ( 'NONE',  ( -0.000000000000000000, 1.000000000000000000, -0.000000000000000000 ) ) ;
#19780 = CARTESIAN_POINT ( 'NONE',  ( -53.50031669685712643, -135.0000000000000000, 4.660752013197171806 ) ) ;
#19781 =( BOUNDED_CURVE ( )  B_SPLINE_CURVE ( 2, ( #30033, #59312, #5927, #6560, #16207, #10421, #59645, #55456, #30995 ),
 .UNSPECIFIED., .F., .F. ) 
 B_SPLINE_CURVE_WITH_KNOTS ( ( 3, 2, 2, 2, 3 ),
 ( 0.7395833333333333703, 0.7402777777777778123, 0.7416666666666666963, 0.7430555555555555802, 0.7437500000000000222 ),
 .UNSPECIFIED. ) 
 CURVE ( )  GEOMETRIC_REPRESENTATION_ITEM ( )  RATIONAL_B_SPLINE_CURVE ( ( 0.9330127018922194093, 0.9330127018922194093, 1.000000000000000000, 0.8660254037844387076, 1.000000000000000000, 0.8660254037844387076, 1.000000000000000000, 0.9330127018922194093, 0.9330127018922194093 ) ) 
 REPRESENTATION_ITEM ( '' )  );
#19782 = CARTESIAN_POINT ( 'NONE',  ( -2.229367062500000163, -59.47916666530106511, -3.861377020970580443 ) ) ;
#19783 = LINE ( 'NONE', #29739, #40720 ) ;
#19784 = CARTESIAN_POINT ( 'NONE',  ( -2.229367062500000163, 15.52083333469892779, -3.861377020970580443 ) ) ;
#19785 = DIRECTION ( 'NONE',  ( -0.000000000000000000, 1.000000000000000000, -0.000000000000000000 ) ) ;
#19786 = CARTESIAN_POINT ( 'NONE',  ( 4.458734124999998549, -46.97916666530106511, -2.574251347313721627 ) ) ;
#19787 = CARTESIAN_POINT ( 'NONE',  ( 5.000000000000000888, -11.45833333060214798, 2.886751345948126879 ) ) ;
#19788 = CARTESIAN_POINT ( 'NONE',  ( 5.000000000000000888, -25.45833333060214443, 2.886751345948126879 ) ) ;
#19789 = DIRECTION ( 'NONE',  ( 0.000000000000000000, 0.000000000000000000, 1.000000000000000000 ) ) ;
#19790 = CARTESIAN_POINT ( 'NONE',  ( -6.972266317189433020E-16, -74.25000000000000000, -5.000000000000000000 ) ) ;
#19791 = CARTESIAN_POINT ( 'NONE',  ( -4.458734124999999437, -109.3958333319677365, -2.574251347313719407 ) ) ;
#19792 = CARTESIAN_POINT ( 'NONE',  ( 2.229367062500001939, -9.229166665301075767, 3.861377020970579999 ) ) ;
#19793 = VERTEX_POINT ( 'NONE', #53451 ) ;
#19794 = CARTESIAN_POINT ( 'NONE',  ( 4.458734125000001214, -98.89583333196775072, 2.574251347313718519 ) ) ;
#19795 = CARTESIAN_POINT ( 'NONE',  ( 3.535533905932736864, -161.2500000027312126, 3.535533905932738641 ) ) ;
#19796 = CARTESIAN_POINT ( 'NONE',  ( 4.458734124999999437, -95.06249999863440792, -5.460374474430324690E-16 ) ) ;
#19797 = CARTESIAN_POINT ( 'NONE',  ( 1.339745962155615144, -49.58034179853029144, 4.999999999999999112 ) ) ;
#19798 = CARTESIAN_POINT ( 'NONE',  ( -5.000000000000000000, -56.95833333060214443, -2.886751345948128211 ) ) ;
#19799 = CARTESIAN_POINT ( 'NONE',  ( 1.339745962155612702, -5.294658198738519950, -5.000000000000000000 ) ) ;
#19800 = CARTESIAN_POINT ( 'NONE',  ( -50.70258187064364108, -125.1250000013656205, 2.196230717870141014 ) ) ;
#19801 = CARTESIAN_POINT ( 'NONE',  ( -52.10840900171896806, -148.1875000013656063, 3.393966926194110556 ) ) ;
#19802 = CARTESIAN_POINT ( 'NONE',  ( 2.229367062500001939, -17.97916666530106866, 3.861377020970579999 ) ) ;
#19803 = CARTESIAN_POINT ( 'NONE',  ( -4.458734124999998549, 7.520833334698926009, 2.574251347313722516 ) ) ;
#19804 = CARTESIAN_POINT ( 'NONE',  ( -2.229367062499996610, -58.39583333196773651, 3.861377020970582219 ) ) ;
#19805 = CARTESIAN_POINT ( 'NONE',  ( 2.499999999999998668, -48.20833333060215153, -4.330127018922193649 ) ) ;
#19806 = CARTESIAN_POINT ( 'NONE',  ( -2.229367062500000163, -16.47916666530107577, -3.861377020970580443 ) ) ;
#19807 = DIRECTION ( 'NONE',  ( 0.000000000000000000, 0.000000000000000000, 1.000000000000000000 ) ) ;
#19808 = CARTESIAN_POINT ( 'NONE',  ( 2.071067811865476394, -153.1875000000000284, 5.000000000000000000 ) ) ;
#19809 = CARTESIAN_POINT ( 'NONE',  ( -5.000000000000000000, -4.999999999999997335, 0.000000000000000000 ) ) ;
#19810 = ORIENTED_EDGE ( 'NONE', *, *, #7146, .F. ) ;
#19811 = CARTESIAN_POINT ( 'NONE',  ( -2.229367062500000163, -47.72916666530106511, -3.861377020970580443 ) ) ;
#19812 = CARTESIAN_POINT ( 'NONE',  ( 0.000000000000000000, -170.0000000000000000, 5.000000000000000000 ) ) ;
#19813 = CARTESIAN_POINT ( 'NONE',  ( -6.972266317189433020E-16, -9.250000000000000000, -5.000000000000000000 ) ) ;
#19814 = DIRECTION ( 'NONE',  ( -0.000000000000000000, 1.000000000000000000, -0.000000000000000000 ) ) ;
#19815 = CARTESIAN_POINT ( 'NONE',  ( 4.458734125000001214, -82.89583333196772230, 2.574251347313718519 ) ) ;
#19816 = CARTESIAN_POINT ( 'NONE',  ( 2.229367062500001939, 19.77083333469892779, 3.861377020970579999 ) ) ;
#19817 = CARTESIAN_POINT ( 'NONE',  ( 4.458734125000001214, 11.10416666803225993, 2.574251347313718519 ) ) ;
#19818 = CARTESIAN_POINT ( 'NONE',  ( -5.000000000000000000, -88.87499999726880162, 0.000000000000000000 ) ) ;
#19819 = CARTESIAN_POINT ( 'NONE',  ( 5.000000000000000000, -37.37499999726881583, -6.123233995736766282E-16 ) ) ;
#19820 = CARTESIAN_POINT ( 'NONE',  ( 5.000000000000000000, 20.62500000273118772, -6.123233995736766282E-16 ) ) ;
#19821 = CARTESIAN_POINT ( 'NONE',  ( -3.152548672688508926E-16, 22.18750000136559564, -5.148502694627439702 ) ) ;
#19822 = CARTESIAN_POINT ( 'NONE',  ( -5.000000000000000000, -78.08333333333332860, -2.886751345948128211 ) ) ;
#19823 = CARTESIAN_POINT ( 'NONE',  ( -3.535250795749689387E-16, 7.875000002731186832, -5.773502691896257311 ) ) ;
#19824 = VERTEX_POINT ( 'NONE', #58906 ) ;
#19825 = CARTESIAN_POINT ( 'NONE',  ( -7.500000000000000000, 4.330127018922191873, -7.422398894150032511 ) ) ;
#19826 = ORIENTED_EDGE ( 'NONE', *, *, #39005, .T. ) ;
#19828 = CARTESIAN_POINT ( 'NONE',  ( -5.000000000000000000, -32.00000000000000000, 0.000000000000000000 ) ) ;
#19827 = CARTESIAN_POINT ( 'NONE',  ( -5.000000000000000000, -104.0833333333333428, -2.886751345948128211 ) ) ;
#19829 = CARTESIAN_POINT ( 'NONE',  ( 9.457646018065525792E-16, -40.06249999863439371, 5.148502694627439702 ) ) ;
#19830 = CARTESIAN_POINT ( 'NONE',  ( 5.000000000000000000, -33.29166666393547303, -2.886751345948129988 ) ) ;
#19832 = ORIENTED_EDGE ( 'NONE', *, *, #31168, .T. ) ;
#19831 = CARTESIAN_POINT ( 'NONE',  ( -4.458734124999999437, -64.39583333196772230, -2.574251347313719407 ) ) ;
#19833 = CARTESIAN_POINT ( 'NONE',  ( -50.40829686548195099, -151.2500000013656063, -1.485763867205728284 ) ) ;
#19834 = CARTESIAN_POINT ( 'NONE',  ( -4.458734124999998549, -15.22916666530107754, 2.574251347313722516 ) ) ;
#19836 = ORIENTED_EDGE ( 'NONE', *, *, #24849, .F. ) ;
#19835 = CARTESIAN_POINT ( 'NONE',  ( -4.458734124999998549, -14.47916666530107221, 2.574251347313722516 ) ) ;
#19837 = CARTESIAN_POINT ( 'NONE',  ( -4.999999999999999112, -79.91666666666667140, 2.886751345948131764 ) ) ;
#19838 = CARTESIAN_POINT ( 'NONE',  ( -4.458734125000001214, -166.8750000013655779, 1.846868145590734089 ) ) ;
#19839 = CARTESIAN_POINT ( 'NONE',  ( 9.457646018065525792E-16, -56.31249999863440081, 5.148502694627439702 ) ) ;
#19840 = CARTESIAN_POINT ( 'NONE',  ( -4.999999999999999112, -81.79166666393547303, 2.886751345948131764 ) ) ;
#19842 = ORIENTED_EDGE ( 'NONE', *, *, #59431, .T. ) ;
#19841 = DIRECTION ( 'NONE',  ( 0.000000000000000000, 0.000000000000000000, 1.000000000000000000 ) ) ;
#19843 = CARTESIAN_POINT ( 'NONE',  ( -59.98410592259440222, -146.1250000000000284, -0.3983568153799752487 ) ) ;
#19844 = CARTESIAN_POINT ( 'NONE',  ( -3.152548672688508926E-16, -29.81249999863440436, -5.148502694627439702 ) ) ;
#19845 = CARTESIAN_POINT ( 'NONE',  ( 0.000000000000000000, -120.0000000000000000, 0.000000000000000000 ) ) ;
#19846 = ORIENTED_EDGE ( 'NONE', *, *, #26810, .T. ) ;
#19847 = APPLICATION_PROTOCOL_DEFINITION ( 'draft international standard', 'automotive_design', 1998, #56132 ) ;
#19848 = CARTESIAN_POINT ( 'NONE',  ( 3.152801135295367541, -167.5625000013656063, -3.152801135295367541 ) ) ;
#19849 = CARTESIAN_POINT ( 'NONE',  ( -4.458734124999999437, -105.5624999986344221, 0.000000000000000000 ) ) ;
#19850 = CARTESIAN_POINT ( 'NONE',  ( -9.184850993605147944E-16, -148.2500000000000284, 5.000000000000000000 ) ) ;
#19851 = ORIENTED_EDGE ( 'NONE', *, *, #5250, .T. ) ;
#19852 = CARTESIAN_POINT ( 'NONE',  ( -56.48576386720575471, -148.0000000013656063, -4.591703134518078322 ) ) ;
#19853 = CARTESIAN_POINT ( 'NONE',  ( -50.18089887299979068, -139.8125000027312126, 2.462841084822635640 ) ) ;
#19854 = CARTESIAN_POINT ( 'NONE',  ( -2.229367062500000163, -38.47916666530107221, -3.861377020970580443 ) ) ;
#19855 = CARTESIAN_POINT ( 'NONE',  ( 2.730187237215162345E-16, -144.4375000013656063, -4.458734124999999437 ) ) ;
#19856 = LINE ( 'NONE', #54274, #32195 ) ;
#19857 = CARTESIAN_POINT ( 'NONE',  ( -58.80597590150559739, -135.0000000000000284, 3.242614290531460330 ) ) ;
#19858 = CARTESIAN_POINT ( 'NONE',  ( 4.458734124999999437, -11.81249999863440081, -5.460374474430324690E-16 ) ) ;
#19859 =( BOUNDED_CURVE ( )  B_SPLINE_CURVE ( 2, ( #9186, #52935, #52320, #43273, #13069, #62913, #17591, #42963, #18826 ),
 .UNSPECIFIED., .F., .F. ) 
 B_SPLINE_CURVE_WITH_KNOTS ( ( 3, 2, 2, 2, 3 ),
 ( 0.3017857142857142683, 0.3023809523809523614, 0.3035714285714285476, 0.3047619047619047894, 0.3053571428571428825 ),
 .UNSPECIFIED. ) 
 CURVE ( )  GEOMETRIC_REPRESENTATION_ITEM ( )  RATIONAL_B_SPLINE_CURVE ( ( 0.9330127018922194093, 0.9330127018922194093, 1.000000000000000000, 0.8660254037844387076, 1.000000000000000000, 0.8660254037844387076, 1.000000000000000000, 0.9330127018922194093, 0.9330127018922194093 ) ) 
 REPRESENTATION_ITEM ( '' )  );
#19860 = CARTESIAN_POINT ( 'NONE',  ( -5.000000000000000000, -101.0833333333333286, -2.886751345948128211 ) ) ;
#19861 = ORIENTED_EDGE ( 'NONE', *, *, #48785, .F. ) ;
#19862 = CARTESIAN_POINT ( 'NONE',  ( 1.846868145590736310, -140.8750000013656063, 4.458734124999999437 ) ) ;
#19863 = CARTESIAN_POINT ( 'NONE',  ( -3.152548672688508926E-16, -33.81249999863440792, -5.148502694627439702 ) ) ;
#19864 = CARTESIAN_POINT ( 'NONE',  ( 2.500000000000002220, 5.458333336064518981, 4.330127018922192761 ) ) ;
#19865 = CYLINDRICAL_SURFACE ( 'NONE', #37564, 5.000000000000000000 ) ;
#19866 = CARTESIAN_POINT ( 'NONE',  ( -50.70258187064364108, -134.1250000013656347, 2.196230717870141014 ) ) ;
#19867 = CARTESIAN_POINT ( 'NONE',  ( 9.457646018065525792E-16, -75.31249999863440792, 5.148502694627439702 ) ) ;
#19868 = CARTESIAN_POINT ( 'NONE',  ( -51.75738570946856498, -145.8750000027312126, 3.805975901505576964 ) ) ;
#19869 = CARTESIAN_POINT ( 'NONE',  ( -2.499999999999996447, -69.83333333333332860, 4.330127018922195425 ) ) ;
#19870 = CARTESIAN_POINT ( 'NONE',  ( 0.000000000000000000, -120.0000000000000000, 0.000000000000000000 ) ) ;
#19871 = CARTESIAN_POINT ( 'NONE',  ( 2.229367062500001939, 5.770833334698927786, 3.861377020970579999 ) ) ;
#19872 = VERTEX_POINT ( 'NONE', #48304 ) ;
#19873 = CARTESIAN_POINT ( 'NONE',  ( 0.000000000000000000, -120.0000000000000000, 5.000000000000000000 ) ) ;
#19874 = CARTESIAN_POINT ( 'NONE',  ( 2.500000000000002220, 2.333333333333333037, 4.330127018922192761 ) ) ;
#19876 = CARTESIAN_POINT ( 'NONE',  ( -2.229367062500000163, -28.47916666530107221, -3.861377020970580443 ) ) ;
#19875 = CARTESIAN_POINT ( 'NONE',  ( -4.999999999999999112, -95.91666666666664298, 2.886751345948131764 ) ) ;
#19877 = CARTESIAN_POINT ( 'NONE',  ( -56.66612745406286678, -143.4375000027312410, -5.149110718188528502 ) ) ;
#19878 = CARTESIAN_POINT ( 'NONE',  ( 2.229367062500001939, -81.22916666530106511, 3.861377020970579999 ) ) ;
#19879 = CARTESIAN_POINT ( 'NONE',  ( 4.458734125000000326, 19.85416666803226349, 2.574251347313718519 ) ) ;
#19880 = CARTESIAN_POINT ( 'NONE',  ( 2.499999999999998668, -18.33333333333333215, -4.330127018922193649 ) ) ;
#19881 = CIRCLE ( 'NONE', #26049, 5.000000000000000000 ) ;
#19882 = CARTESIAN_POINT ( 'NONE',  ( -54.64476657466781973, -138.8125000013656063, -4.444560631937228834 ) ) ;
#19883 = CARTESIAN_POINT ( 'NONE',  ( 2.229367062500001939, -0.9791666653010712151, 3.861377020970579999 ) ) ;
#19884 = CARTESIAN_POINT ( 'NONE',  ( 4.458734124999998549, 21.02083333469892779, -2.574251347313721627 ) ) ;
#19885 = CARTESIAN_POINT ( 'NONE',  ( -4.458734124999999437, -42.56249999863440081, 0.000000000000000000 ) ) ;
#19886 = DIRECTION ( 'NONE',  ( -0.000000000000000000, 1.000000000000000000, -0.000000000000000000 ) ) ;
#19887 = CARTESIAN_POINT ( 'NONE',  ( 2.229367062500001939, 0.02083333469892964529, 3.861377020970579999 ) ) ;
#19888 = CARTESIAN_POINT ( 'NONE',  ( 2.229367062500001939, -26.22916666530106866, 3.861377020970579999 ) ) ;
#19889 = CARTESIAN_POINT ( 'NONE',  ( -3.152548672688508926E-16, -67.56249999863440792, -5.148502694627439702 ) ) ;
#19890 = CARTESIAN_POINT ( 'NONE',  ( -2.499999999999996447, -105.7083333306021444, 4.330127018922195425 ) ) ;
#19891 = CARTESIAN_POINT ( 'NONE',  ( 4.458734124999998549, 25.27083333469892779, -2.574251347313721627 ) ) ;
#19892 = CARTESIAN_POINT ( 'NONE',  ( 1.339745962155612702, -58.16965819600732601, -5.000000000000000000 ) ) ;
#19893 = CARTESIAN_POINT ( 'NONE',  ( 0.000000000000000000, -120.0000000000000000, 0.000000000000000000 ) ) ;
#19894 = CARTESIAN_POINT ( 'NONE',  ( -4.458734124999999437, -74.64583333196773651, -2.574251347313719407 ) ) ;
#19895 = CARTESIAN_POINT ( 'NONE',  ( -4.999999999999999112, -56.91666666666667140, 2.886751345948131764 ) ) ;
#19896 = CARTESIAN_POINT ( 'NONE',  ( 1.975475456537005874E-15, -31.62499999726880873, 5.000000000000000000 ) ) ;
#19897 = CARTESIAN_POINT ( 'NONE',  ( 5.000000000000000000, 27.70833333606451987, -2.886751345948129988 ) ) ;
#19898 = VERTEX_POINT ( 'NONE', #54409 ) ;
#19899 = CARTESIAN_POINT ( 'NONE',  ( -6.972266317189433020E-16, -27.24999999999999645, -5.000000000000000000 ) ) ;
#19900 = CARTESIAN_POINT ( 'NONE',  ( -5.000000000000000000, -56.95833333060214443, -2.886751345948128211 ) ) ;
#19901 = CARTESIAN_POINT ( 'NONE',  ( -5.000000000000000000, -17.08333333333333215, -2.886751345948128211 ) ) ;
#19902 = CARTESIAN_POINT ( 'NONE',  ( 4.458734124999999437, -23.81249999863440436, -5.460374474430324690E-16 ) ) ;
#19903 = CARTESIAN_POINT ( 'NONE',  ( -2.229367062499996610, -81.14583333196773651, 3.861377020970582219 ) ) ;
#19904 = CARTESIAN_POINT ( 'NONE',  ( -1.846868145590734756, -166.3750000013655779, -4.458734125000000326 ) ) ;
#19905 = CARTESIAN_POINT ( 'NONE',  ( 2.499999999999998668, -20.20833333060214798, -4.330127018922193649 ) ) ;
#19907 = ORIENTED_EDGE ( 'NONE', *, *, #55157, .T. ) ;
#19906 = CARTESIAN_POINT ( 'NONE',  ( 4.458734125000001214, -48.89583333196772941, 2.574251347313718519 ) ) ;
#19908 = CARTESIAN_POINT ( 'NONE',  ( -4.999999999999998224, -23.91666666666666785, 2.886751345948131764 ) ) ;
#19909 = CARTESIAN_POINT ( 'NONE',  ( 0.000000000000000000, -170.0000000000000000, 5.000000000000000000 ) ) ;
#19911 = ORIENTED_EDGE ( 'NONE', *, *, #37272, .F. ) ;
#19910 = CARTESIAN_POINT ( 'NONE',  ( 4.458734125000001214, 0.8541666680322613781, 2.574251347313718519 ) ) ;
#19912 = CARTESIAN_POINT ( 'NONE',  ( -59.59170313451810586, -150.5000000013655779, 1.485763867205729394 ) ) ;
#19913 = CARTESIAN_POINT ( 'NONE',  ( 1.060575238724906964E-15, -65.75000000000000000, 5.773502691896257311 ) ) ;
#19914 = CARTESIAN_POINT ( 'NONE',  ( 1.846868145590735200, -151.5000000013655779, -4.458734125000000326 ) ) ;
#19915 = CARTESIAN_POINT ( 'NONE',  ( 2.229367062499998831, -39.89583333196773651, -3.861377020970580887 ) ) ;
#19916 = CARTESIAN_POINT ( 'NONE',  ( 2.499999999999998668, -68.20833333060214443, -4.330127018922193649 ) ) ;
#19917 = CARTESIAN_POINT ( 'NONE',  ( -3.535533905932737309, -163.6250000000000284, -3.535533905932738197 ) ) ;
#19918 = CARTESIAN_POINT ( 'NONE',  ( 0.000000000000000000, -170.0000000000000000, 0.000000000000000000 ) ) ;
#19919 = CARTESIAN_POINT ( 'NONE',  ( -52.80376928212989185, -128.1250000013656347, -4.297418129356379346 ) ) ;
#19920 = CARTESIAN_POINT ( 'NONE',  ( -4.458734124999999437, -11.56249999863440792, 0.000000000000000000 ) ) ;
#19921 = CARTESIAN_POINT ( 'NONE',  ( -2.229367062499996610, -46.39583333196774362, 3.861377020970582219 ) ) ;
#19922 = AXIS2_PLACEMENT_3D ( 'NONE', #5955, #42179, #40352 ) ;
#19923 = CARTESIAN_POINT ( 'NONE',  ( -58.24261429053147765, -136.3750000027312126, -3.805975901505573855 ) ) ;
#19924 = CARTESIAN_POINT ( 'NONE',  ( 3.152801135295367541, -149.3125000013655779, -3.152801135295367541 ) ) ;
#19925 = CARTESIAN_POINT ( 'NONE',  ( -4.458734124999999437, -90.56249999863440792, 0.000000000000000000 ) ) ;
#19926 = DIRECTION ( 'NONE',  ( -0.000000000000000000, 1.000000000000000000, -0.000000000000000000 ) ) ;
#19927 = ORIENTED_EDGE ( 'NONE', *, *, #43975, .T. ) ;
#19928 = CARTESIAN_POINT ( 'NONE',  ( 5.000000000000000888, -19.45833333060214798, 2.886751345948126879 ) ) ;
#19929 = CARTESIAN_POINT ( 'NONE',  ( 0.000000000000000000, -170.0000000000000000, 0.000000000000000000 ) ) ;
#19930 = PRODUCT ( 'hex flange nut gradea_iso_ISO - 4161 - M10 - N', 'hex flange nut gradea_iso_ISO - 4161 - M10 - N', '', ( #249 ) ) ;
#19931 = CARTESIAN_POINT ( 'NONE',  ( -49.85088928181150436, -148.6875000027311842, -1.666127454062680702 ) ) ;
#19932 =( BOUNDED_CURVE ( )  B_SPLINE_CURVE ( 2, ( #2798, #62605, #36886, #42648, #38148, #51685, #33314, #62289, #22417 ),
 .UNSPECIFIED., .F., .F. ) 
 B_SPLINE_CURVE_WITH_KNOTS ( ( 3, 2, 2, 2, 3 ),
 ( 0.3270833333333333370, 0.3277777777777777790, 0.3291666666666666630, 0.3305555555555555469, 0.3312499999999999889 ),
 .UNSPECIFIED. ) 
 CURVE ( )  GEOMETRIC_REPRESENTATION_ITEM ( )  RATIONAL_B_SPLINE_CURVE ( ( 0.9330127018922194093, 0.9330127018922194093, 1.000000000000000000, 0.8660254037844387076, 1.000000000000000000, 0.8660254037844387076, 1.000000000000000000, 0.9330127018922194093, 0.9330127018922194093 ) ) 
 REPRESENTATION_ITEM ( '' )  );
#19933 = CARTESIAN_POINT ( 'NONE',  ( 5.000000000000000888, -38.58333333333332149, 2.886751345948126879 ) ) ;
#19934 = ORIENTED_EDGE ( 'NONE', *, *, #62817, .T. ) ;
#19935 = CARTESIAN_POINT ( 'NONE',  ( -2.229367062499996610, 1.854166668032262377, 3.861377020970582219 ) ) ;
#19936 = CARTESIAN_POINT ( 'NONE',  ( 1.975475456537005874E-15, -50.62499999726881583, 5.000000000000000000 ) ) ;
#19937 = CARTESIAN_POINT ( 'NONE',  ( 9.457646018065525792E-16, -15.31249999863440436, 5.148502694627439702 ) ) ;
#19938 = CARTESIAN_POINT ( 'NONE',  ( -2.499999999999996447, 9.166666666666666075, 4.330127018922195425 ) ) ;
#19939 = CARTESIAN_POINT ( 'NONE',  ( -2.229367062500000163, -1.479166665301071770, -3.861377020970580443 ) ) ;
#19940 = LINE ( 'NONE', #34742, #55198 ) ;
#19941 = CARTESIAN_POINT ( 'NONE',  ( 3.152801135295366208, -150.5625000013655779, 3.152801135295367985 ) ) ;
#19942 = CARTESIAN_POINT ( 'NONE',  ( 4.458734125000000326, 20.85416666803226349, 2.574251347313718519 ) ) ;
#19943 = EDGE_LOOP ( 'NONE', ( #51812, #48328, #29909, #4622 ) ) ;
#19944 = CARTESIAN_POINT ( 'NONE',  ( 2.229367062499998831, -99.64583333196773651, -3.861377020970580887 ) ) ;
#19945 = CARTESIAN_POINT ( 'NONE',  ( -2.499999999999996447, -33.70833333060213732, 4.330127018922195425 ) ) ;
#19946 =( REPRESENTATION_RELATIONSHIP ('NONE','NONE', #27855, #3639 ) REPRESENTATION_RELATIONSHIP_WITH_TRANSFORMATION ( #20815 )SHAPE_REPRESENTATION_RELATIONSHIP( ) );
#19947 = CARTESIAN_POINT ( 'NONE',  ( 0.000000000000000000, -120.0000000000000000, 5.000000000000000000 ) ) ;
#19948 = CARTESIAN_POINT ( 'NONE',  ( -3.152548672688508926E-16, -12.56249999863440081, -5.148502694627439702 ) ) ;
#19949 = EDGE_CURVE ( 'NONE', #63218, #44248, #60626, .T. ) ;
#19950 = CARTESIAN_POINT ( 'NONE',  ( -1.339745962155612480, 27.91965820146970856, -5.000000000000000888 ) ) ;
#19951 = DIRECTION ( 'NONE',  ( -0.000000000000000000, -1.000000000000000000, 0.000000000000000000 ) ) ;
#19952 = CARTESIAN_POINT ( 'NONE',  ( -4.999999999999998224, -87.91666666666667140, 2.886751345948131764 ) ) ;
#19953 = CARTESIAN_POINT ( 'NONE',  ( -4.999999999999999112, -40.79166666393548724, 2.886751345948131764 ) ) ;
#19954 = FACE_OUTER_BOUND ( 'NONE', #23284, .T. ) ;
#19955 = CARTESIAN_POINT ( 'NONE',  ( -3.152548672688508926E-16, 11.43750000136559564, -5.148502694627439702 ) ) ;
#19956 = CARTESIAN_POINT ( 'NONE',  ( -5.000000000000000000, -8.874999997268814056, 0.000000000000000000 ) ) ;
#19957 = CARTESIAN_POINT ( 'NONE',  ( 0.000000000000000000, -170.0000000000000000, 0.000000000000000000 ) ) ;
#19958 = CARTESIAN_POINT ( 'NONE',  ( -4.458734124999999437, 17.60416666803225993, -2.574251347313719407 ) ) ;
#19959 = CARTESIAN_POINT ( 'NONE',  ( -4.458734124999999437, -61.39583333196774362, -2.574251347313719407 ) ) ;
#19960 = VERTEX_POINT ( 'NONE', #67 ) ;
#19961 = CARTESIAN_POINT ( 'NONE',  ( 4.458734124999998549, -9.979166665301068662, -2.574251347313721627 ) ) ;
#19962 =( BOUNDED_CURVE ( )  B_SPLINE_CURVE ( 2, ( #11639, #31260, #36736, #56367, #59922, #15845, #37995, #37057, #27081, #52789, #32213, #32855, #18052, #56684, #12600, #57315, #27388, #42812, #3285, #46696, #7785, #52161, #51842, #13232, #42496, #47021, #38309, #52484, #37365, #32532, #2970, #31905, #51534, #22587, #2644, #17439, #57627, #42184, #7471, #17748, #22263, #61824, #56996, #12910, #8417, #41863, #8104, #27708, #47335, #61510, #28020, #22901, #47639, #23522, #62133, #8722, #37673, #3594, #62454, #23199, #18374, #13556, #33174, #28335, #47950, #3903, #12290, #43123, #62763, #18683, #5476, #33793, #49218, #5158, #49535, #54037, #29908, #18990, #14796, #29587, #28, #23833, #57937, #19309, #9035, #24778, #53724, #9975, #44382, #44699, #48893, #4519, #24144, #44062, #33479, #58558, #39238, #342, #38924, #43436, #15124, #38605, #4837, #19942, #43747, #39554, #34408, #59196, #34745, #63391, #53410, #54372, #20273, #28955, #28646, #9655, #48578, #25091, #10299, #9341, #63080, #664, #58238, #13855, #53100, #19628, #48261, #58864, #4219, #29264, #14166, #14478, #24457, #34099, #25413, #26369, #10932, #50819, #45671, #10611, #16084, #1629, #40207, #11570, #15454, #26693, #35071, #45353, #35708, #11252, #50173, #30547, #55336, #45031, #999, #5795, #20916, #40836, #36024, #30877, #55970, #59843, #50504, #36339, #16723, #46310, #2267, #6756, #40519, #45987, #1320, #6125, #41151, #6447, #31190, #54689, #1953, #20603, #30224, #11882, #15768, #60163, #60481, #49849, #60797, #26056, #31500, #51145, #35385, #21230, #7080, #16407, #55004, #55656, #21554, #25739, #39874, #59519, #46949, #42103, #36980, #32137, #47566, #61117, #46625, #8345, #18300, #21871, #17676, #27006, #57555, #51772, #2571, #27320, #3208, #41788, #17041, #8646, #27943, #22828, #17358, #13158, #36658, #3517, #22187, #56286, #62377, #61432, #42418, #27635, #56608, #12525, #62061, #7716, #52413, #12839, #12213, #2896, #22509, #47871, #17974, #52090, #61749, #41466, #37598, #37291, #56920, #32458, #31830, #51461, #8028, #7399, #47263, #23128, #57242, #32780, #42732, #37923, #13481, #33097, #52712, #28259, #23450, #63011, #14093, #9271, #13784, #63635, #62693, #19554, #15051, #38243, #44309, #48193, #58485, #34343, #33719, #39168, #24386, #29508, #24705, #273, #33406, #3832, #19871, #63312, #57862, #34669, #43364, #58793, #14723, #59121, #53969, #39485, #28572, #43987, #9899, #9588, #54288, #29194, #43055, #18617, #49140, #19234, #5084, #10227, #29832, #53021, #8962, #4146, #23765, #18919, #38533, #48820, #58161, #53338, #28887, #48508, #4446, #24075, #43671, #38850, #14410, #34032, #53653, #4757, #49778, #6054, #6682, #59766, #49465, #60407, #6372, #20198, #40444, #40759, #59445, #5404, #60085, #1551, #30801, #15692, #35312, #35631, #25021, #50099, #50430, #21154, #10858, #34998, #26289, #11806, #44631, #11178, #39801, #54932, #30473, #35955, #20841, #1874, #45911, #21479, #591, #20527, #15375, #1241, #40125, #41077, #11500, #44962, #54613, #60722, #16007, #16333, #55260, #50738, #25664, #10537, #30149, #45275, #5724, #55581, #25978, #16645, #25338, #31116, #45593, #36268, #55893, #922, #7640, #42347, #23057, #37849, #22434, #27244, #62301, #21798, #51061, #32063, #47186, #22113, #46869, #16965, #36576, #61042, #12452, #32386, #27554, #2812, #47489, #61985, #31752, #42030, #27869, #8267, #57482, #31423, #17905, #51699, #37526, #57167, #12763, #26938, #56206, #52011, #61671, #22749, #17604, #13082, #7953, #56846, #36901, #3129, #41393, #32703, #37220, #3442, #52332, #51385, #42662, #12130, #7005, #18223, #26614, #46231, #2194, #7327, #46554, #2497, #41706, #61354, #17277, #56531, #52637, #38163, #63554, #9812, #13400, #9198, #18543, #43288, #57787, #18839, #19792, #39399, #43904, #14016, #19472, #38457, #4069, #14642, #28810, #4678, #28182, #39086, #13707, #47798, #53887, #33329, #33955, #53576, #23377, #34259, #58085, #29422, #49053, #52948, #63236, #5002, #53263, #8885, #14334, #43593, #28498, #33021, #9503, #33643, #48429, #48117, #8571, #58716, #3755, #23688, #24621, #44228, #42977, #4373, #62924, #193, #23989, #19150, #38767, #58406, #62619, #29112, #48735, #24300, #5326, #55177, #54204, #20441, #44550, #16253, #21398, #59035, #20759, #49382, #44874, #25256, #45513, #30394, #11416, #35873, #24944, #14965, #55501, #54851, #506, #6599, #34912, #21077, #54535, #20114, #31035, #50017, #50344, #5970, #60327, #15614, #39718, #34573, #40040, #10142, #30721, #10784, #11096, #6291, #45834, #50660, #26214, #1160, #29749, #35232, #25896, #1796, #59355, #25580, #45193, #15290, #10455, #30070, #59682, #1475, #49699, #5643, #836, #40365, #60005, #15929, #35552, #40682, #17198, #57086, #7876, #41315, #36825, #37455, #17833, #2420, #61276, #56128, #60645, #16568, #16883, #31343, #46157, #22674, #51311, #36190, #46473, #13005, #7249, #2119, #22032, #22354, #55811, #36499, #26861, #41623, #50985, #37148, #11727, #56772, #52252, #6925, #32625, #21720, #31991, #27479, #56456, #12378, #47107, #51625, #8192, #27794, #26534, #41003, #47419, #7559, #60963, #3371, #12051, #32305, #51934, #31675, #12692, #27171, #46788, #61596, #3056, #2734, #41951, #17530, #42273, #61913, #58333, #18766, #19076, #14259, #9742, #58647, #63480, #19400, #23299, #18145, #24228, #28732, #42899, #33881, #62227, #53812, #13325, #42589, #23616, #38696, #32945, #29347, #52878, #28428, #62547, #43212, #43834, #33260, #22988, #53501, #43521, #57404, #13945, #9431, #52569, #48981, #37773, #29041, #62853, #48664, #48042, #13639, #39018, #38393, #4605, #8502, #14567, #47728, #28112, #34189, #18468, #63165, #48358, #3685, #38088, #3993, #57714, #8813, #58017, #9124, #33572, #53191, #4302, #23919, #35164, #44474, #30963, #5894, #10389, #49939, #24549, #433, #15213, #29999, #14886, #25501, #20693, #49631, #54128, #25826, #4930, #44153, #30318, #58960, #54463, #34839, #55096, #39966, #21006, #45441, #34493, #124, #1404, #759, #10066, #59282, #60255, #30643, #20039, #29679, #40611, #59612, #59936, #15544, #6213, #25181, #49309, #19718, #5567, #39327, #40298, #20367, #1085, #15858, #55422, #16174, #35799, #5251, #24873, #11340, #10711, #39643, #35480, #44795, #54780, #45120, #11022, #50265, #21955, #60882, #41235, #26780, #36113, #55736, #16492, #8659, #16807, #50588, #62391, #7482, #21323, #41551, #42748, #60567, #6528, #61202, #3531, #6848, #45761, #38254, #37937, #31919, #46079, #11652, #27095, #13495, #31272, #1715, #28272, #26462, #47580, #56380, #50906, #2037, #51546, #21642, #18312, #17124, #40924, #36427, #56055, #13799, #23140, #51235, #57570, #26142, #33111, #11971, #7171, #31601, #46398, #2347, #36750, #12304, #52727, #47887, #3845, #23465, #43068, #62706, #18632, #57875, #59134, #54301, #63330, #63024, #33420, #29847, #29208, #23777, #44644, #9285, #24718, #44322, #25034, #29521, #5417, #58178, #53984, #5100, #39180, #10243, #58805, #53038, #4773, #286, #48833, #49155, #19885, #20214, #604, #49479, #39816, #33732, #28586, #34682, #14737, #53350, #39498, #8976, #59457, #48207, #38863, #9600, #24400, #43379, #4160, #19248, #58499, #28901, #53667, #18931, #43684, #38547, #15070, #9913, #14107, #44002, #48521, #4462, #24089, #63649, #14423, #34045, #19568, #34354, #6066, #16657, #11192, #6696, #30162, #41089, #40138, #49791, #55906, #35324, #35967, #21167, #59782, #15707, #60420, #30489, #45925, #6386, #5737, #36282, #55273, #54945, #16345, #45610, #10872, #41405, #55593, #40460, #35647, #50111, #35014, #54628, #25680, #25355, #20541, #60736, #45288, #10552, #20857, #51079, #1254, #60099, #16020, #11512, #44973, #30814, #50446, #25991, #938, #31128, #1566, #50751, #26625, #40774, #11817, #26302, #1888, #21491, #31436, #7017, #46245, #2206, #21810, #15389, #7652, #23067, #36588, #22125, #47503, #57493, #61057, #56857, #2507, #33033, #27255, #41717, #2826, #42358, #16977, #46882, #47198, #56224, #61684, #61997, #13096, #22445, #46567, #18235, #23390, #12145, #22762, #51397, #42042, #17615, #3453, #32397, #13412, #37860, #26950, #31764, #32074, #7339, #12775, #51711, #52649, #42672, #56544, #61368, #8584, #52023, #52343, #7967, #62311, #37231, #17289, #36914, #27565, #12463, #32715, #3142, #28194, #17917, #47809, #37539, #8277, #57178, #27881, #3766, #53900, #34588, #49396, #33969, #19164, #10157, #33344, #62632, #43606, #58729, #52959, #38781, #28512, #48130, #8897, #24003, #43920, #39101, #58420, #59051, #9825, #43301, #14347, #39413, #19804, #5340, #42990, #29436, #63249, #49069, #4384, #44242, #53589, #34274, #57798, #5016, #4081, #13719, #14979, #62937, #63567, #48749, #23704, #18851, #24313, #58099, #24635, #9519, #38472, #14028, #33657, #53275, #19487, #29126, #9210, #18554, #14655, #38176, #4691, #206, #54219, #29762, #28823, #48444, #11430, #59698, #35886, #30735, #59370, #1174, #55516, #25271, #60339, #521, #11739, #20131, #30408, #20774, #60020, #35246, #15629, #40379, #10470, #30083, #54547, #5990, #25908, #21090, #15943, #41015, #31048, #35565, #16267, #34926, #44563, #55189, #40694, #44892, #39731, #31357, #50672, #6304, #20456, #49713, #45526, #11110, #6613, #50356, #26226, #1487, #45846, #1808, #5658, #852, #21412, #40054, #60659, #16583, #15304, #54865, #10796, #50998, #36202, #25595, #55824, #24958, #50032, #45208, #7888, #57101, #3069, #46169, #46487, #60975, #12063, #52267, #17211, #2131, #12390, #21733, #22686, #27807, #22044, #22366, #61608, #36838, #56468, #56785, #41329, #7572, #51949, #42286, #18158, #16896, #47432, #51323, #17542, #37468, #32004, #61926, #27492, #32637, #3384, #51638, #2435, #23001, #32957, #41637, #36512, #41966, #61289, #17845, #13019, #62239, #8204, #42602, #31688, #47121, #37786, #12704, #57416, #32318, #13337, #6938, #26549, #56143, #7261, #27185, #46800, #26874, #37162, #2747, #28440, #48992, #14899, #23628, #3697, #4311, #43223, #44167, #14578, #48054, #57725, #4939, #23931, #43844, #43532, #53823, #9135, #18479, #52582, #63176, #53513, #39029, #48369, #134, #38101, #58656, #62864, #63490, #58344, #23311, #28743, #19415, #19728, #58972, #19087, #38706, #39341, #42912, #8513, #14272, #18776, #38403, #33891, #13651, #33271, #52890, #33582, #9442, #48675, #29051, #24562, #34200, #8826, #4615, #28123, #29359, #47741, #62560, #9752, #4007, #58026, #13955, #24240, #53201, #39656, #55109, #25514, #25836, #1096, #60267, #11034, #59948, #39978, #30657, #44485, #35812, #15556, #11352, #55436, #5264, #30013, #59293, #60584, #50279, #35176, #45452, #20705, #6224, #10401, #35491, #21017, #1418, #44809, #16185, #10078, #15224, #40624, #30974, #34508, #59624, #49320, #50598, #6540, #49641, #49955, #45132, #771, #20378, #40310, #29689, #54794, #15871, #26153, #10722, #20052, #45772, #30329, #1730, #24884, #34853, #21334, #5907, #446, #40934, #54474, #54139, #5578, #25194, #31930, #7497, #26791, #46411, #2667, #55747, #17139, #61534, #32241, #41562, #2049, #42523, #16504, #41888, #6860, #2360, #21969, #2995, #51558, #32562, #57024, #46089, #36125, #12939, #12319, #26475, #27732, #56067, #7812, #27414, #8129, #52184, #27109, #47045, #46722, #17770, #36763, #21657, #11664, #61213, #31283, #51870, #22289, #12625, #22612, #3308, #47360, #22929, #50918, #16818, #41248, #42207, #60894, #36437, #17466, #56391, #11986, #31612, #51248, #37088, #61853, #7183, #56706, #37389, #52814, #3619, #3932, #33818, #13580, #62160, #19018, #38631, #42840, #43149, #28982, #9371, #19337, #18080, #58274, #23551, #14193, #47978, #33199, #48605, #62789, #53438, #32881, #4544, #23226, #52509, #24169, #9061, #28357, #4243, #8444, #43773, #18708, #63419, #37703, #18401, #53129, #57341, #38333, #38022, #23858, #28671, #57654, #13257, #28047, #57962, #48291, #47667, #62483, #8752, #13883, #33511, #43461, #63107, #3505, #41457, #42408, #26997, #3199, #61738, #26685, #32127, #22817, #47557, #62367, #46938, #51763, #31491, #61423, #7707, #27311, #2562, #46616, #2886, #61107, #17031, #21862, #36969, #56910, #52081, #22499, #8335, #62050, #56277, #42095, #52403, #32769, #17667, #8019, #12201, #51135, #42723, #17965, #37282, #51453, #36646, #12829, #32449, #47254, #27624, #37589, #57232, #13149, #17347, #27934, #2258, #23119, #7390, #18291, #55961, #46301, #22176, #31820, #11873, #7070, #56598, #41777, #12516, #9576, #13774, #38837, #24376, #34022, #48184, #63622, #13472, #62685, #19544, #4137, #33088, #43353, #52702, #53643, #58782, #53010, #53329, #28878, #23758, #63001, #24065, #8637, #38524, #19224, #29183, #18909, #23443, #14712, #18606, #48499, #4748, #58152, #48810, #58474, #39157, #34330, #14082, #33397, #53956, #262, #8952, #28248, #9263, #28563, #29497, #9888, #33710, #43045, #49129, #38234, #14400, #43977, #43661, #5072, #3822, #37914, #24692, #4436, #47862, #44298, #63302, #57544, #57854, #47287, #32808, #42762, #18326, #57583, #28286, #43388, #47898, #22537, #13510, #23475, #8986, #37950, #33743, #8057, #28598, #57267, #33430, #3854, #56945, #62404, #53049, #14117, #28910, #33126, #9294, #61774, #27972, #52743, #8672, #52437, #13185, #43078, #27659, #3237, #52113, #3545, #62716, #18641, #38263, #38559, #48216, #22853, #57885, #18941, #42133, #13811, #4171, #42444, #17701, #48533, #23786, #63033, #18003, #62086, #58188, #53360, #37315, #12866, #32484, #37626, #8371, #47593, #23153, #14432, #49169, #44985, #25365, #4784, #54315, #5747, #44330, #24411, #5426, #34690, #44012, #30501, #25043, #29532, #24728, #19577, #24099, #43695, #63660, #58508 ),
 .UNSPECIFIED., .F., .F. ) 
 B_SPLINE_CURVE_WITH_KNOTS ( ( 3, 2, 2, 2, 2, 2, 2, 2, 2, 2, 2, 2, 2, 2, 2, 2, 2, 2, 2, 2, 2, 2, 2, 2, 2, 2, 2, 2, 2, 2, 2, 2, 2, 2, 2, 2, 2, 2, 2, 2, 2, 2, 2, 2, 2, 2, 2, 2, 2, 2, 2, 2, 2, 2, 2, 2, 2, 2, 2, 2, 2, 2, 2, 2, 2, 2, 2, 2, 2, 2, 2, 2, 2, 2, 2, 2, 2, 2, 2, 2, 2, 2, 2, 2, 2, 2, 2, 2, 2, 2, 2, 2, 2, 2, 2, 2, 2, 2, 2, 2, 2, 2, 2, 2, 2, 2, 2, 2, 2, 2, 2, 2, 2, 2, 2, 2, 2, 2, 2, 2, 2, 2, 2, 2, 2, 2, 2, 2, 2, 2, 2, 2, 2, 2, 2, 2, 2, 2, 2, 2, 2, 2, 2, 2, 2, 2, 2, 2, 2, 2, 2, 2, 2, 2, 2, 2, 2, 2, 2, 2, 2, 2, 2, 2, 2, 2, 2, 2, 2, 2, 2, 2, 2, 2, 2, 2, 2, 2, 2, 2, 2, 2, 2, 2, 2, 2, 2, 2, 2, 2, 2, 2, 2, 2, 2, 2, 2, 2, 2, 2, 2, 2, 2, 2, 2, 2, 2, 2, 2, 2, 2, 2, 2, 2, 2, 2, 2, 2, 2, 2, 2, 2, 2, 2, 2, 2, 2, 2, 2, 2, 2, 2, 2, 2, 2, 2, 2, 2, 2, 2, 2, 2, 2, 2, 2, 2, 2, 2, 2, 2, 2, 2, 2, 2, 2, 2, 2, 2, 2, 2, 2, 2, 2, 2, 2, 2, 2, 2, 2, 2, 2, 2, 2, 2, 2, 2, 2, 2, 2, 2, 2, 2, 2, 2, 2, 2, 2, 2, 2, 2, 2, 2, 2, 2, 2, 2, 2, 2, 2, 2, 2, 2, 2, 2, 2, 2, 2, 2, 2, 2, 2, 2, 2, 2, 2, 2, 2, 2, 2, 2, 2, 2, 2, 2, 2, 2, 2, 2, 2, 2, 2, 2, 2, 2, 2, 2, 2, 2, 2, 2, 2, 2, 2, 2, 2, 2, 2, 2, 2, 2, 2, 2, 2, 2, 2, 2, 2, 2, 2, 2, 2, 2, 2, 2, 2, 2, 2, 2, 2, 2, 2, 2, 2, 2, 2, 2, 2, 2, 2, 2, 2, 2, 2, 2, 2, 2, 2, 2, 2, 2, 2, 2, 2, 2, 2, 2, 2, 2, 2, 2, 2, 2, 2, 2, 2, 2, 2, 2, 2, 2, 2, 2, 2, 2, 2, 2, 2, 2, 2, 2, 2, 2, 2, 2, 2, 2, 2, 2, 2, 2, 2, 2, 2, 2, 2, 2, 2, 2, 2, 2, 2, 2, 2, 2, 2, 2, 2, 2, 2, 2, 2, 2, 2, 2, 2, 2, 2, 2, 2, 2, 2, 2, 2, 2, 2, 2, 2, 2, 2, 2, 2, 2, 2, 2, 2, 2, 2, 2, 2, 2, 2, 2, 2, 2, 2, 2, 2, 2, 2, 2, 2, 2, 2, 2, 2, 2, 2, 2, 2, 2, 2, 2, 2, 2, 2, 2, 2, 2, 2, 2, 2, 2, 2, 2, 2, 2, 2, 2, 2, 2, 2, 2, 2, 2, 2, 2, 2, 2, 2, 2, 2, 2, 2, 2, 2, 2, 2, 2, 2, 2, 2, 2, 2, 2, 2, 2, 2, 2, 2, 2, 2, 2, 2, 2, 2, 2, 2, 2, 2, 2, 2, 2, 2, 2, 2, 2, 2, 2, 2, 2, 2, 2, 2, 2, 2, 2, 2, 2, 2, 2, 2, 2, 2, 2, 2, 2, 2, 2, 2, 2, 2, 2, 2, 2, 2, 2, 2, 2, 2, 2, 2, 2, 2, 2, 2, 2, 2, 2, 2, 2, 2, 2, 2, 2, 2, 2, 2, 2, 2, 2, 2, 2, 2, 2, 2, 2, 2, 2, 2, 2, 2, 2, 2, 2, 2, 2, 2, 2, 2, 2, 2, 2, 2, 2, 2, 2, 2, 2, 2, 2, 2, 2, 2, 2, 2, 2, 2, 2, 2, 2, 2, 2, 2, 2, 2, 2, 2, 2, 2, 2, 2, 2, 2, 2, 2, 2, 2, 2, 2, 2, 2, 2, 2, 2, 2, 2, 2, 2, 2, 2, 2, 2, 2, 2, 2, 2, 2, 2, 2, 2, 2, 2, 2, 2, 2, 2, 2, 2, 2, 2, 2, 2, 2, 2, 2, 2, 2, 2, 2, 2, 2, 2, 2, 2, 2, 2, 2, 2, 2, 2, 2, 2, 2, 2, 2, 2, 2, 2, 2, 2, 2, 2, 2, 2, 2, 2, 2, 2, 2, 2, 2, 2, 2, 2, 2, 2, 2, 2, 2, 2, 2, 2, 2, 2, 2, 2, 2, 2, 2, 2, 2, 2, 2, 2, 2, 2, 2, 2, 2, 2, 2, 2, 2, 2, 2, 2, 2, 2, 2, 2, 2, 2, 2, 2, 2, 2, 2, 2, 2, 2, 2, 2, 2, 2, 2, 2, 2, 2, 2, 2, 2, 2, 2, 2, 2, 2, 2, 2, 2, 2, 2, 2, 2, 2, 2, 2, 2, 2, 2, 2, 2, 2, 2, 2, 2, 2, 2, 2, 2, 2, 3 ),
 ( 0.000000000000000000, 0.001190476190476190584, 0.002380952380952381167, 0.003571428571428571317, 0.004761904761904762334, 0.005952380952380952051, 0.007142857142857142634, 0.008333333333333333218, 0.009523809523809524669, 0.01071428571428571438, 0.01190476190476190410, 0.01309523809523809555, 0.01428571428571428527, 0.01547619047619047672, 0.01666666666666666644, 0.01785714285714285615, 0.01904761904761904934, 0.02023809523809523905, 0.02142857142857142877, 0.02261904761904761849, 0.02380952380952380820, 0.02500000000000000139, 0.02619047619047619110, 0.02738095238095238082, 0.02857142857142857054, 0.02976190476190476025, 0.03095238095238095344, 0.03214285714285713969, 0.03333333333333333287, 0.03452380952380952606, 0.03571428571428571230, 0.03690476190476190549, 0.03809523809523809867, 0.03928571428571428492, 0.04047619047619047811, 0.04166666666666666435, 0.04285714285714285754, 0.04404761904761905073, 0.04523809523809523697, 0.04642857142857143016, 0.04761904761904761640, 0.04880952380952380959, 0.05000000000000000278, 0.05119047619047618902, 0.05238095238095238221, 0.05357142857142856845, 0.05476190476190476164, 0.05595238095238095483, 0.05714285714285714107, 0.05833333333333333426, 0.05952380952380952051, 0.06071428571428571369, 0.06190476190476190688, 0.06309523809523809312, 0.06428571428571427937, 0.06547619047619047949, 0.06666666666666666574, 0.06785714285714285199, 0.06904761904761905211, 0.07023809523809523836, 0.07142857142857142461, 0.07261904761904762473, 0.07380952380952381098, 0.07499999999999999722, 0.07619047619047619735, 0.07738095238095238360, 0.07857142857142856984, 0.07976190476190475609, 0.08095238095238095621, 0.08214285714285714246, 0.08333333333333332871, 0.08452380952380952883, 0.08571428571428571508, 0.08690476190476190133, 0.08809523809523810145, 0.08928571428571428770, 0.09047619047619047394, 0.09166666666666666019, 0.09285714285714286031, 0.09404761904761904656, 0.09523809523809523281, 0.09642857142857143293, 0.09761904761904761918, 0.09880952380952380543, 0.1000000000000000056, 0.1011904761904761918, 0.1023809523809523780, 0.1035714285714285782, 0.1047619047619047644, 0.1059523809523809507, 0.1071428571428571369, 0.1083333333333333370, 0.1095238095238095233, 0.1107142857142857095, 0.1119047619047619097, 0.1130952380952380959, 0.1142857142857142821, 0.1154761904761904823, 0.1166666666666666685, 0.1178571428571428548, 0.1190476190476190410, 0.1202380952380952411, 0.1214285714285714274, 0.1226190476190476136, 0.1238095238095238138, 0.1250000000000000000, 0.1261904761904761862, 0.1273809523809523725, 0.1285714285714285587, 0.1297619047619047727, 0.1309523809523809590, 0.1321428571428571452, 0.1333333333333333315, 0.1345238095238095177, 0.1357142857142857040, 0.1369047619047619180, 0.1380952380952381042, 0.1392857142857142905, 0.1404761904761904767, 0.1416666666666666630, 0.1428571428571428492, 0.1440476190476190355, 0.1452380952380952495, 0.1464285714285714357, 0.1476190476190476220, 0.1488095238095238082, 0.1499999999999999944, 0.1511904761904761807, 0.1523809523809523947, 0.1535714285714285809, 0.1547619047619047672, 0.1559523809523809534, 0.1571428571428571397, 0.1583333333333333259, 0.1595238095238095122, 0.1607142857142857262, 0.1619047619047619124, 0.1630952380952380987, 0.1642857142857142849, 0.1654761904761904712, 0.1666666666666666574, 0.1678571428571428437, 0.1690476190476190577, 0.1702380952380952439, 0.1714285714285714302, 0.1726190476190476164, 0.1738095238095238027, 0.1749999999999999889, 0.1761904761904762029, 0.1773809523809523891, 0.1785714285714285754, 0.1797619047619047616, 0.1809523809523809479, 0.1821428571428571341, 0.1833333333333333204, 0.1845238095238095344, 0.1857142857142857206, 0.1869047619047619069, 0.1880952380952380931, 0.1892857142857142794, 0.1904761904761904656, 0.1916666666666666796, 0.1928571428571428659, 0.1940476190476190521, 0.1952380952380952384, 0.1964285714285714246, 0.1976190476190476109, 0.1988095238095237971, 0.2000000000000000111, 0.2011904761904761973, 0.2023809523809523836, 0.2035714285714285698, 0.2047619047619047561, 0.2059523809523809423, 0.2071428571428571563, 0.2083333333333333426, 0.2095238095238095288, 0.2107142857142857151, 0.2119047619047619013, 0.2130952380952380876, 0.2142857142857142738, 0.2154761904761904878, 0.2166666666666666741, 0.2178571428571428603, 0.2190476190476190466, 0.2202380952380952328, 0.2214285714285714191, 0.2226190476190476053, 0.2238095238095238193, 0.2250000000000000056, 0.2261904761904761918, 0.2273809523809523780, 0.2285714285714285643, 0.2297619047619047505, 0.2309523809523809645, 0.2321428571428571508, 0.2333333333333333370, 0.2345238095238095233, 0.2357142857142857095, 0.2369047619047618958, 0.2380952380952380820, 0.2392857142857142960, 0.2404761904761904823, 0.2416666666666666685, 0.2428571428571428548, 0.2440476190476190410, 0.2452380952380952273, 0.2464285714285714413, 0.2476190476190476275, 0.2488095238095238138, 0.2500000000000000000, 0.2511904761904761862, 0.2523809523809523725, 0.2535714285714285587, 0.2547619047619047450, 0.2559523809523809312, 0.2571428571428571175, 0.2583333333333333592, 0.2595238095238095455, 0.2607142857142857317, 0.2619047619047619180, 0.2630952380952381042, 0.2642857142857142905, 0.2654761904761904767, 0.2666666666666666630, 0.2678571428571428492, 0.2690476190476190355, 0.2702380952380952217, 0.2714285714285714080, 0.2726190476190475942, 0.2738095238095238360, 0.2750000000000000222, 0.2761904761904762085, 0.2773809523809523947, 0.2785714285714285809, 0.2797619047619047672, 0.2809523809523809534, 0.2821428571428571397, 0.2833333333333333259, 0.2845238095238095122, 0.2857142857142856984, 0.2869047619047618847, 0.2880952380952380709, 0.2892857142857143127, 0.2904761904761904989, 0.2916666666666666852, 0.2928571428571428714, 0.2940476190476190577, 0.2952380952380952439, 0.2964285714285714302, 0.2976190476190476164, 0.2988095238095238027, 0.2999999999999999889, 0.3011904761904761751, 0.3023809523809523614, 0.3035714285714285476, 0.3047619047619047894, 0.3059523809523809756, 0.3071428571428571619, 0.3083333333333333481, 0.3095238095238095344, 0.3107142857142857206, 0.3119047619047619069, 0.3130952380952380931, 0.3142857142857142794, 0.3154761904761904656, 0.3166666666666666519, 0.3178571428571428381, 0.3190476190476190244, 0.3202380952380952106, 0.3214285714285714524, 0.3226190476190476386, 0.3238095238095238249, 0.3250000000000000111, 0.3261904761904761973, 0.3273809523809523836, 0.3285714285714285698, 0.3297619047619047561, 0.3309523809523809423, 0.3321428571428571286, 0.3333333333333333148, 0.3345238095238095011, 0.3357142857142856873, 0.3369047619047619291, 0.3380952380952381153, 0.3392857142857143016, 0.3404761904761904878, 0.3416666666666666741, 0.3428571428571428603, 0.3440476190476190466, 0.3452380952380952328, 0.3464285714285714191, 0.3476190476190476053, 0.3488095238095237915, 0.3499999999999999778, 0.3511904761904761640, 0.3523809523809524058, 0.3535714285714285920, 0.3547619047619047783, 0.3559523809523809645, 0.3571428571428571508, 0.3583333333333333370, 0.3595238095238095233, 0.3607142857142857095, 0.3619047619047618958, 0.3630952380952380820, 0.3642857142857142683, 0.3654761904761904545, 0.3666666666666666408, 0.3678571428571428825, 0.3690476190476190688, 0.3702380952380952550, 0.3714285714285714413, 0.3726190476190476275, 0.3738095238095238138, 0.3750000000000000000, 0.3761904761904761862, 0.3773809523809523725, 0.3785714285714285587, 0.3797619047619047450, 0.3809523809523809312, 0.3821428571428571175, 0.3833333333333333592, 0.3845238095238095455, 0.3857142857142857317, 0.3869047619047619180, 0.3880952380952381042, 0.3892857142857142905, 0.3904761904761904767, 0.3916666666666666630, 0.3928571428571428492, 0.3940476190476190355, 0.3952380952380952217, 0.3964285714285714080, 0.3976190476190475942, 0.3988095238095238360, 0.4000000000000000222, 0.4011904761904762085, 0.4023809523809523947, 0.4035714285714285809, 0.4047619047619047672, 0.4059523809523809534, 0.4071428571428571397, 0.4083333333333333259, 0.4095238095238095122, 0.4107142857142856984, 0.4119047619047618847, 0.4130952380952380709, 0.4142857142857143127, 0.4154761904761904989, 0.4166666666666666852, 0.4178571428571428714, 0.4190476190476190577, 0.4202380952380952439, 0.4214285714285714302, 0.4226190476190476164, 0.4238095238095238027, 0.4249999999999999889, 0.4261904761904761751, 0.4273809523809523614, 0.4285714285714285476, 0.4297619047619047894, 0.4309523809523809756, 0.4321428571428571619, 0.4333333333333333481, 0.4345238095238095344, 0.4357142857142857206, 0.4369047619047619069, 0.4380952380952380931, 0.4392857142857142794, 0.4404761904761904656, 0.4416666666666666519, 0.4428571428571428381, 0.4440476190476190244, 0.4452380952380952106, 0.4464285714285714524, 0.4476190476190476386, 0.4488095238095238249, 0.4500000000000000111, 0.4511904761904761973, 0.4523809523809523836, 0.4535714285714285698, 0.4547619047619047561, 0.4559523809523809423, 0.4571428571428571286, 0.4583333333333333148, 0.4595238095238095011, 0.4607142857142856873, 0.4619047619047619291, 0.4630952380952381153, 0.4642857142857143016, 0.4654761904761904878, 0.4666666666666666741, 0.4678571428571428603, 0.4690476190476190466, 0.4702380952380952328, 0.4714285714285714191, 0.4726190476190476053, 0.4738095238095237915, 0.4749999999999999778, 0.4761904761904761640, 0.4773809523809524058, 0.4785714285714285920, 0.4797619047619047783, 0.4809523809523809645, 0.4821428571428571508, 0.4833333333333333370, 0.4845238095238095233, 0.4857142857142857095, 0.4869047619047618958, 0.4880952380952380820, 0.4892857142857142683, 0.4904761904761904545, 0.4916666666666666408, 0.4928571428571428825, 0.4940476190476190688, 0.4952380952380952550, 0.4964285714285714413, 0.4976190476190476275, 0.4988095238095238138, 0.5000000000000000000, 0.5011904761904761862, 0.5023809523809523725, 0.5035714285714285587, 0.5047619047619047450, 0.5059523809523809312, 0.5071428571428571175, 0.5083333333333333037, 0.5095238095238094900, 0.5107142857142856762, 0.5119047619047618625, 0.5130952380952380487, 0.5142857142857142350, 0.5154761904761904212, 0.5166666666666667185, 0.5178571428571429047, 0.5190476190476190910, 0.5202380952380952772, 0.5214285714285714635, 0.5226190476190476497, 0.5238095238095238360, 0.5250000000000000222, 0.5261904761904762085, 0.5273809523809523947, 0.5285714285714285809, 0.5297619047619047672, 0.5309523809523809534, 0.5321428571428571397, 0.5333333333333333259, 0.5345238095238095122, 0.5357142857142856984, 0.5369047619047618847, 0.5380952380952380709, 0.5392857142857142572, 0.5404761904761904434, 0.5416666666666666297, 0.5428571428571428159, 0.5440476190476190022, 0.5452380952380951884, 0.5464285714285713746, 0.5476190476190476719, 0.5488095238095238582, 0.5500000000000000444, 0.5511904761904762307, 0.5523809523809524169, 0.5535714285714286031, 0.5547619047619047894, 0.5559523809523809756, 0.5571428571428571619, 0.5583333333333333481, 0.5595238095238095344, 0.5607142857142857206, 0.5619047619047619069, 0.5630952380952380931, 0.5642857142857142794, 0.5654761904761904656, 0.5666666666666666519, 0.5678571428571428381, 0.5690476190476190244, 0.5702380952380952106, 0.5714285714285713969, 0.5726190476190475831, 0.5738095238095237693, 0.5749999999999999556, 0.5761904761904761418, 0.5773809523809523281, 0.5785714285714286254, 0.5797619047619048116, 0.5809523809523809978, 0.5821428571428571841, 0.5833333333333333703, 0.5845238095238095566, 0.5857142857142857428, 0.5869047619047619291, 0.5880952380952381153, 0.5892857142857143016, 0.5904761904761904878, 0.5916666666666666741, 0.5928571428571428603, 0.5940476190476190466, 0.5952380952380952328, 0.5964285714285714191, 0.5976190476190476053, 0.5988095238095237915, 0.5999999999999999778, 0.6011904761904761640, 0.6023809523809523503, 0.6035714285714285365, 0.6047619047619047228, 0.6059523809523809090, 0.6071428571428570953, 0.6083333333333332815, 0.6095238095238095788, 0.6107142857142857650, 0.6119047619047619513, 0.6130952380952381375, 0.6142857142857143238, 0.6154761904761905100, 0.6166666666666666963, 0.6178571428571428825, 0.6190476190476190688, 0.6202380952380952550, 0.6214285714285714413, 0.6226190476190476275, 0.6238095238095238138, 0.6250000000000000000, 0.6261904761904761862, 0.6273809523809523725, 0.6285714285714285587, 0.6297619047619047450, 0.6309523809523809312, 0.6321428571428571175, 0.6333333333333333037, 0.6345238095238094900, 0.6357142857142856762, 0.6369047619047618625, 0.6380952380952380487, 0.6392857142857142350, 0.6404761904761904212, 0.6416666666666667185, 0.6428571428571429047, 0.6440476190476190910, 0.6452380952380952772, 0.6464285714285714635, 0.6476190476190476497, 0.6488095238095238360, 0.6500000000000000222, 0.6511904761904762085, 0.6523809523809523947, 0.6535714285714285809, 0.6547619047619047672, 0.6559523809523809534, 0.6571428571428571397, 0.6583333333333333259, 0.6595238095238095122, 0.6607142857142856984, 0.6619047619047618847, 0.6630952380952380709, 0.6642857142857142572, 0.6654761904761904434, 0.6666666666666666297, 0.6678571428571428159, 0.6690476190476190022, 0.6702380952380951884, 0.6714285714285713746, 0.6726190476190476719, 0.6738095238095238582, 0.6750000000000000444, 0.6761904761904762307, 0.6773809523809524169, 0.6785714285714286031, 0.6797619047619047894, 0.6809523809523809756, 0.6821428571428571619, 0.6833333333333333481, 0.6845238095238095344, 0.6857142857142857206, 0.6869047619047619069, 0.6880952380952380931, 0.6892857142857142794, 0.6904761904761904656, 0.6916666666666666519, 0.6928571428571428381, 0.6940476190476190244, 0.6952380952380952106, 0.6964285714285713969, 0.6976190476190475831, 0.6988095238095237693, 0.6999999999999999556, 0.7011904761904761418, 0.7023809523809523281, 0.7035714285714286254, 0.7047619047619048116, 0.7059523809523809978, 0.7071428571428571841, 0.7083333333333333703, 0.7095238095238095566, 0.7107142857142857428, 0.7119047619047619291, 0.7130952380952381153, 0.7142857142857143016, 0.7154761904761904878, 0.7166666666666666741, 0.7178571428571428603, 0.7190476190476190466, 0.7202380952380952328, 0.7214285714285714191, 0.7226190476190476053, 0.7238095238095237915, 0.7249999999999999778, 0.7261904761904761640, 0.7273809523809523503, 0.7285714285714285365, 0.7297619047619047228, 0.7309523809523809090, 0.7321428571428570953, 0.7333333333333332815, 0.7345238095238095788, 0.7357142857142857650, 0.7369047619047619513, 0.7380952380952381375, 0.7392857142857143238, 0.7404761904761905100, 0.7416666666666666963, 0.7428571428571428825, 0.7440476190476190688, 0.7452380952380952550, 0.7464285714285714413, 0.7476190476190476275, 0.7488095238095238138, 0.7500000000000000000, 0.7511904761904761862, 0.7523809523809523725, 0.7535714285714285587, 0.7547619047619047450, 0.7559523809523809312, 0.7571428571428571175, 0.7583333333333333037, 0.7595238095238094900, 0.7607142857142856762, 0.7619047619047618625, 0.7630952380952380487, 0.7642857142857142350, 0.7654761904761904212, 0.7666666666666667185, 0.7678571428571429047, 0.7690476190476190910, 0.7702380952380952772, 0.7714285714285714635, 0.7726190476190476497, 0.7738095238095238360, 0.7750000000000000222, 0.7761904761904762085, 0.7773809523809523947, 0.7785714285714285809, 0.7797619047619047672, 0.7809523809523809534, 0.7821428571428571397, 0.7833333333333333259, 0.7845238095238095122, 0.7857142857142856984, 0.7869047619047618847, 0.7880952380952380709, 0.7892857142857142572, 0.7904761904761904434, 0.7916666666666666297, 0.7928571428571428159, 0.7940476190476190022, 0.7952380952380951884, 0.7964285714285713746, 0.7976190476190476719, 0.7988095238095238582, 0.8000000000000000444, 0.8011904761904762307, 0.8023809523809524169, 0.8035714285714286031, 0.8047619047619047894, 0.8059523809523809756, 0.8071428571428571619, 0.8083333333333333481, 0.8095238095238095344, 0.8107142857142857206, 0.8119047619047619069, 0.8130952380952380931, 0.8142857142857142794, 0.8154761904761904656, 0.8166666666666666519, 0.8178571428571428381, 0.8190476190476190244, 0.8202380952380952106, 0.8214285714285713969, 0.8226190476190475831, 0.8238095238095237693, 0.8249999999999999556, 0.8261904761904761418, 0.8273809523809523281, 0.8285714285714286254, 0.8297619047619048116, 0.8309523809523809978, 0.8321428571428571841, 0.8333333333333333703, 0.8345238095238095566, 0.8357142857142857428, 0.8369047619047619291, 0.8380952380952381153, 0.8392857142857143016, 0.8404761904761904878, 0.8416666666666666741, 0.8428571428571428603, 0.8440476190476190466, 0.8452380952380952328, 0.8464285714285714191, 0.8476190476190476053, 0.8488095238095237915, 0.8499999999999999778, 0.8511904761904761640, 0.8523809523809523503, 0.8535714285714285365, 0.8547619047619047228, 0.8559523809523809090, 0.8571428571428570953, 0.8583333333333332815, 0.8595238095238095788, 0.8607142857142857650, 0.8619047619047619513, 0.8630952380952381375, 0.8642857142857143238, 0.8654761904761905100, 0.8666666666666666963, 0.8678571428571428825, 0.8690476190476190688, 0.8702380952380952550, 0.8714285714285714413, 0.8726190476190476275, 0.8738095238095238138, 0.8750000000000000000, 0.8761904761904761862, 0.8773809523809523725, 0.8785714285714285587, 0.8797619047619047450, 0.8809523809523809312, 0.8821428571428571175, 0.8833333333333333037, 0.8845238095238094900, 0.8857142857142856762, 0.8869047619047618625, 0.8880952380952380487, 0.8892857142857142350, 0.8904761904761904212, 0.8916666666666667185, 0.8928571428571429047, 0.8940476190476190910, 0.8952380952380952772, 0.8964285714285714635, 0.8976190476190476497, 0.8988095238095238360, 0.9000000000000000222, 0.9011904761904762085, 0.9023809523809523947, 0.9035714285714285809, 0.9047619047619047672, 0.9059523809523809534, 0.9071428571428571397, 0.9083333333333333259, 0.9095238095238095122, 0.9107142857142856984, 0.9119047619047618847, 0.9130952380952380709, 0.9142857142857142572, 0.9154761904761904434, 0.9166666666666666297, 0.9178571428571428159, 0.9190476190476190022, 0.9202380952380951884, 0.9214285714285713746, 0.9226190476190476719, 0.9238095238095238582, 0.9250000000000000444, 0.9261904761904762307, 0.9273809523809524169, 0.9285714285714286031, 0.9297619047619047894, 0.9309523809523809756, 0.9321428571428571619, 0.9333333333333333481, 0.9345238095238095344, 0.9357142857142857206, 0.9369047619047619069, 0.9380952380952380931, 0.9392857142857142794, 0.9404761904761904656, 0.9416666666666666519, 0.9428571428571428381, 0.9440476190476190244, 0.9452380952380952106, 0.9464285714285713969, 0.9476190476190475831, 0.9488095238095237693, 0.9499999999999999556, 0.9511904761904761418, 0.9523809523809523281, 0.9535714285714286254, 0.9547619047619048116, 0.9559523809523809978, 0.9571428571428571841, 0.9583333333333333703, 0.9595238095238095566, 0.9607142857142857428, 0.9619047619047619291, 0.9630952380952381153, 0.9642857142857143016, 0.9654761904761904878, 0.9666666666666666741, 0.9678571428571428603, 0.9690476190476190466, 0.9702380952380952328, 0.9714285714285714191, 0.9726190476190476053, 0.9738095238095237915, 0.9749999999999999778, 0.9761904761904761640, 0.9773809523809523503, 0.9785714285714285365, 0.9797619047619047228, 0.9809523809523809090, 0.9821428571428570953, 0.9833333333333332815, 0.9845238095238095788, 0.9857142857142857650, 0.9869047619047619513, 0.9880952380952381375, 0.9892857142857143238, 0.9904761904761905100, 0.9916666666666666963, 0.9928571428571428825, 0.9940476190476190688, 0.9952380952380952550, 0.9964285714285714413, 0.9976190476190476275, 0.9988095238095238138, 1.000000000000000000 ),
 .UNSPECIFIED. ) 
 CURVE ( )  GEOMETRIC_REPRESENTATION_ITEM ( )  RATIONAL_B_SPLINE_CURVE ( ( 1.000000000000000000, 0.8660254037844387076, 1.000000000000000000, 0.8660254037844387076, 1.000000000000000000, 0.8660254037844387076, 1.000000000000000000, 0.8660254037844387076, 1.000000000000000000, 0.8660254037844387076, 1.000000000000000000, 0.8660254037844387076, 1.000000000000000000, 0.8660254037844387076, 1.000000000000000000, 0.8660254037844387076, 1.000000000000000000, 0.8660254037844387076, 1.000000000000000000, 0.8660254037844387076, 1.000000000000000000, 0.8660254037844387076, 1.000000000000000000, 0.8660254037844387076, 1.000000000000000000, 0.8660254037844387076, 1.000000000000000000, 0.8660254037844387076, 1.000000000000000000, 0.8660254037844387076, 1.000000000000000000, 0.8660254037844387076, 1.000000000000000000, 0.8660254037844387076, 1.000000000000000000, 0.8660254037844387076, 1.000000000000000000, 0.8660254037844387076, 1.000000000000000000, 0.8660254037844387076, 1.000000000000000000, 0.8660254037844387076, 1.000000000000000000, 0.8660254037844387076, 1.000000000000000000, 0.8660254037844387076, 1.000000000000000000, 0.8660254037844387076, 1.000000000000000000, 0.8660254037844387076, 1.000000000000000000, 0.8660254037844387076, 1.000000000000000000, 0.8660254037844387076, 1.000000000000000000, 0.8660254037844387076, 1.000000000000000000, 0.8660254037844387076, 1.000000000000000000, 0.8660254037844387076, 1.000000000000000000, 0.8660254037844387076, 1.000000000000000000, 0.8660254037844387076, 1.000000000000000000, 0.8660254037844387076, 1.000000000000000000, 0.8660254037844387076, 1.000000000000000000, 0.8660254037844387076, 1.000000000000000000, 0.8660254037844387076, 1.000000000000000000, 0.8660254037844387076, 1.000000000000000000, 0.8660254037844387076, 1.000000000000000000, 0.8660254037844387076, 1.000000000000000000, 0.8660254037844387076, 1.000000000000000000, 0.8660254037844387076, 1.000000000000000000, 0.8660254037844387076, 1.000000000000000000, 0.8660254037844387076, 1.000000000000000000, 0.8660254037844387076, 1.000000000000000000, 0.8660254037844387076, 1.000000000000000000, 0.8660254037844387076, 1.000000000000000000, 0.8660254037844387076, 1.000000000000000000, 0.8660254037844387076, 1.000000000000000000, 0.8660254037844387076, 1.000000000000000000, 0.8660254037844387076, 1.000000000000000000, 0.8660254037844387076, 1.000000000000000000, 0.8660254037844387076, 1.000000000000000000, 0.8660254037844387076, 1.000000000000000000, 0.8660254037844387076, 1.000000000000000000, 0.8660254037844387076, 1.000000000000000000, 0.8660254037844387076, 1.000000000000000000, 0.8660254037844387076, 1.000000000000000000, 0.8660254037844387076, 1.000000000000000000, 0.8660254037844387076, 1.000000000000000000, 0.8660254037844387076, 1.000000000000000000, 0.8660254037844387076, 1.000000000000000000, 0.8660254037844387076, 1.000000000000000000, 0.8660254037844387076, 1.000000000000000000, 0.8660254037844387076, 1.000000000000000000, 0.8660254037844387076, 1.000000000000000000, 0.8660254037844387076, 1.000000000000000000, 0.8660254037844387076, 1.000000000000000000, 0.8660254037844387076, 1.000000000000000000, 0.8660254037844387076, 1.000000000000000000, 0.8660254037844387076, 1.000000000000000000, 0.8660254037844387076, 1.000000000000000000, 0.8660254037844387076, 1.000000000000000000, 0.8660254037844387076, 1.000000000000000000, 0.8660254037844387076, 1.000000000000000000, 0.8660254037844387076, 1.000000000000000000, 0.8660254037844387076, 1.000000000000000000, 0.8660254037844387076, 1.000000000000000000, 0.8660254037844387076, 1.000000000000000000, 0.8660254037844387076, 1.000000000000000000, 0.8660254037844387076, 1.000000000000000000, 0.8660254037844387076, 1.000000000000000000, 0.8660254037844387076, 1.000000000000000000, 0.8660254037844387076, 1.000000000000000000, 0.8660254037844387076, 1.000000000000000000, 0.8660254037844387076, 1.000000000000000000, 0.8660254037844387076, 1.000000000000000000, 0.8660254037844387076, 1.000000000000000000, 0.8660254037844387076, 1.000000000000000000, 0.8660254037844387076, 1.000000000000000000, 0.8660254037844387076, 1.000000000000000000, 0.8660254037844387076, 1.000000000000000000, 0.8660254037844387076, 1.000000000000000000, 0.8660254037844387076, 1.000000000000000000, 0.8660254037844387076, 1.000000000000000000, 0.8660254037844387076, 1.000000000000000000, 0.8660254037844387076, 1.000000000000000000, 0.8660254037844387076, 1.000000000000000000, 0.8660254037844387076, 1.000000000000000000, 0.8660254037844387076, 1.000000000000000000, 0.8660254037844387076, 1.000000000000000000, 0.8660254037844387076, 1.000000000000000000, 0.8660254037844387076, 1.000000000000000000, 0.8660254037844387076, 1.000000000000000000, 0.8660254037844387076, 1.000000000000000000, 0.8660254037844387076, 1.000000000000000000, 0.8660254037844387076, 1.000000000000000000, 0.8660254037844387076, 1.000000000000000000, 0.8660254037844387076, 1.000000000000000000, 0.8660254037844387076, 1.000000000000000000, 0.8660254037844387076, 1.000000000000000000, 0.8660254037844387076, 1.000000000000000000, 0.8660254037844387076, 1.000000000000000000, 0.8660254037844387076, 1.000000000000000000, 0.8660254037844387076, 1.000000000000000000, 0.8660254037844387076, 1.000000000000000000, 0.8660254037844387076, 1.000000000000000000, 0.8660254037844387076, 1.000000000000000000, 0.8660254037844387076, 1.000000000000000000, 0.8660254037844387076, 1.000000000000000000, 0.8660254037844387076, 1.000000000000000000, 0.8660254037844387076, 1.000000000000000000, 0.8660254037844387076, 1.000000000000000000, 0.8660254037844387076, 1.000000000000000000, 0.8660254037844387076, 1.000000000000000000, 0.8660254037844387076, 1.000000000000000000, 0.8660254037844387076, 1.000000000000000000, 0.8660254037844387076, 1.000000000000000000, 0.8660254037844387076, 1.000000000000000000, 0.8660254037844387076, 1.000000000000000000, 0.8660254037844387076, 1.000000000000000000, 0.8660254037844387076, 1.000000000000000000, 0.8660254037844387076, 1.000000000000000000, 0.8660254037844387076, 1.000000000000000000, 0.8660254037844387076, 1.000000000000000000, 0.8660254037844387076, 1.000000000000000000, 0.8660254037844387076, 1.000000000000000000, 0.8660254037844387076, 1.000000000000000000, 0.8660254037844387076, 1.000000000000000000, 0.8660254037844387076, 1.000000000000000000, 0.8660254037844387076, 1.000000000000000000, 0.8660254037844387076, 1.000000000000000000, 0.8660254037844387076, 1.000000000000000000, 0.8660254037844387076, 1.000000000000000000, 0.8660254037844387076, 1.000000000000000000, 0.8660254037844387076, 1.000000000000000000, 0.8660254037844387076, 1.000000000000000000, 0.8660254037844387076, 1.000000000000000000, 0.8660254037844387076, 1.000000000000000000, 0.8660254037844387076, 1.000000000000000000, 0.8660254037844387076, 1.000000000000000000, 0.8660254037844387076, 1.000000000000000000, 0.8660254037844387076, 1.000000000000000000, 0.8660254037844387076, 1.000000000000000000, 0.8660254037844387076, 1.000000000000000000, 0.8660254037844387076, 1.000000000000000000, 0.8660254037844387076, 1.000000000000000000, 0.8660254037844387076, 1.000000000000000000, 0.8660254037844387076, 1.000000000000000000, 0.8660254037844387076, 1.000000000000000000, 0.8660254037844387076, 1.000000000000000000, 0.8660254037844387076, 1.000000000000000000, 0.8660254037844387076, 1.000000000000000000, 0.8660254037844387076, 1.000000000000000000, 0.8660254037844387076, 1.000000000000000000, 0.8660254037844387076, 1.000000000000000000, 0.8660254037844387076, 1.000000000000000000, 0.8660254037844387076, 1.000000000000000000, 0.8660254037844387076, 1.000000000000000000, 0.8660254037844387076, 1.000000000000000000, 0.8660254037844387076, 1.000000000000000000, 0.8660254037844387076, 1.000000000000000000, 0.8660254037844387076, 1.000000000000000000, 0.8660254037844387076, 1.000000000000000000, 0.8660254037844387076, 1.000000000000000000, 0.8660254037844387076, 1.000000000000000000, 0.8660254037844387076, 1.000000000000000000, 0.8660254037844387076, 1.000000000000000000, 0.8660254037844387076, 1.000000000000000000, 0.8660254037844387076, 1.000000000000000000, 0.8660254037844387076, 1.000000000000000000, 0.8660254037844387076, 1.000000000000000000, 0.8660254037844387076, 1.000000000000000000, 0.8660254037844387076, 1.000000000000000000, 0.8660254037844387076, 1.000000000000000000, 0.8660254037844387076, 1.000000000000000000, 0.8660254037844387076, 1.000000000000000000, 0.8660254037844387076, 1.000000000000000000, 0.8660254037844387076, 1.000000000000000000, 0.8660254037844387076, 1.000000000000000000, 0.8660254037844387076, 1.000000000000000000, 0.8660254037844387076, 1.000000000000000000, 0.8660254037844387076, 1.000000000000000000, 0.8660254037844387076, 1.000000000000000000, 0.8660254037844387076, 1.000000000000000000, 0.8660254037844387076, 1.000000000000000000, 0.8660254037844387076, 1.000000000000000000, 0.8660254037844387076, 1.000000000000000000, 0.8660254037844387076, 1.000000000000000000, 0.8660254037844387076, 1.000000000000000000, 0.8660254037844387076, 1.000000000000000000, 0.8660254037844387076, 1.000000000000000000, 0.8660254037844387076, 1.000000000000000000, 0.8660254037844387076, 1.000000000000000000, 0.8660254037844387076, 1.000000000000000000, 0.8660254037844387076, 1.000000000000000000, 0.8660254037844387076, 1.000000000000000000, 0.8660254037844387076, 1.000000000000000000, 0.8660254037844387076, 1.000000000000000000, 0.8660254037844387076, 1.000000000000000000, 0.8660254037844387076, 1.000000000000000000, 0.8660254037844387076, 1.000000000000000000, 0.8660254037844387076, 1.000000000000000000, 0.8660254037844387076, 1.000000000000000000, 0.8660254037844387076, 1.000000000000000000, 0.8660254037844387076, 1.000000000000000000, 0.8660254037844387076, 1.000000000000000000, 0.8660254037844387076, 1.000000000000000000, 0.8660254037844387076, 1.000000000000000000, 0.8660254037844387076, 1.000000000000000000, 0.8660254037844387076, 1.000000000000000000, 0.8660254037844387076, 1.000000000000000000, 0.8660254037844387076, 1.000000000000000000, 0.8660254037844387076, 1.000000000000000000, 0.8660254037844387076, 1.000000000000000000, 0.8660254037844387076, 1.000000000000000000, 0.8660254037844387076, 1.000000000000000000, 0.8660254037844387076, 1.000000000000000000, 0.8660254037844387076, 1.000000000000000000, 0.8660254037844387076, 1.000000000000000000, 0.8660254037844387076, 1.000000000000000000, 0.8660254037844387076, 1.000000000000000000, 0.8660254037844387076, 1.000000000000000000, 0.8660254037844387076, 1.000000000000000000, 0.8660254037844387076, 1.000000000000000000, 0.8660254037844387076, 1.000000000000000000, 0.8660254037844387076, 1.000000000000000000, 0.8660254037844387076, 1.000000000000000000, 0.8660254037844387076, 1.000000000000000000, 0.8660254037844387076, 1.000000000000000000, 0.8660254037844387076, 1.000000000000000000, 0.8660254037844387076, 1.000000000000000000, 0.8660254037844387076, 1.000000000000000000, 0.8660254037844387076, 1.000000000000000000, 0.8660254037844387076, 1.000000000000000000, 0.8660254037844387076, 1.000000000000000000, 0.8660254037844387076, 1.000000000000000000, 0.8660254037844387076, 1.000000000000000000, 0.8660254037844387076, 1.000000000000000000, 0.8660254037844387076, 1.000000000000000000, 0.8660254037844387076, 1.000000000000000000, 0.8660254037844387076, 1.000000000000000000, 0.8660254037844387076, 1.000000000000000000, 0.8660254037844387076, 1.000000000000000000, 0.8660254037844387076, 1.000000000000000000, 0.8660254037844387076, 1.000000000000000000, 0.8660254037844387076, 1.000000000000000000, 0.8660254037844387076, 1.000000000000000000, 0.8660254037844387076, 1.000000000000000000, 0.8660254037844387076, 1.000000000000000000, 0.8660254037844387076, 1.000000000000000000, 0.8660254037844387076, 1.000000000000000000, 0.8660254037844387076, 1.000000000000000000, 0.8660254037844387076, 1.000000000000000000, 0.8660254037844387076, 1.000000000000000000, 0.8660254037844387076, 1.000000000000000000, 0.8660254037844387076, 1.000000000000000000, 0.8660254037844387076, 1.000000000000000000, 0.8660254037844387076, 1.000000000000000000, 0.8660254037844387076, 1.000000000000000000, 0.8660254037844387076, 1.000000000000000000, 0.8660254037844387076, 1.000000000000000000, 0.8660254037844387076, 1.000000000000000000, 0.8660254037844387076, 1.000000000000000000, 0.8660254037844387076, 1.000000000000000000, 0.8660254037844387076, 1.000000000000000000, 0.8660254037844387076, 1.000000000000000000, 0.8660254037844387076, 1.000000000000000000, 0.8660254037844387076, 1.000000000000000000, 0.8660254037844387076, 1.000000000000000000, 0.8660254037844387076, 1.000000000000000000, 0.8660254037844387076, 1.000000000000000000, 0.8660254037844387076, 1.000000000000000000, 0.8660254037844387076, 1.000000000000000000, 0.8660254037844387076, 1.000000000000000000, 0.8660254037844387076, 1.000000000000000000, 0.8660254037844387076, 1.000000000000000000, 0.8660254037844387076, 1.000000000000000000, 0.8660254037844387076, 1.000000000000000000, 0.8660254037844387076, 1.000000000000000000, 0.8660254037844387076, 1.000000000000000000, 0.8660254037844387076, 1.000000000000000000, 0.8660254037844387076, 1.000000000000000000, 0.8660254037844387076, 1.000000000000000000, 0.8660254037844387076, 1.000000000000000000, 0.8660254037844387076, 1.000000000000000000, 0.8660254037844387076, 1.000000000000000000, 0.8660254037844387076, 1.000000000000000000, 0.8660254037844387076, 1.000000000000000000, 0.8660254037844387076, 1.000000000000000000, 0.8660254037844387076, 1.000000000000000000, 0.8660254037844387076, 1.000000000000000000, 0.8660254037844387076, 1.000000000000000000, 0.8660254037844387076, 1.000000000000000000, 0.8660254037844387076, 1.000000000000000000, 0.8660254037844387076, 1.000000000000000000, 0.8660254037844387076, 1.000000000000000000, 0.8660254037844387076, 1.000000000000000000, 0.8660254037844387076, 1.000000000000000000, 0.8660254037844387076, 1.000000000000000000, 0.8660254037844387076, 1.000000000000000000, 0.8660254037844387076, 1.000000000000000000, 0.8660254037844387076, 1.000000000000000000, 0.8660254037844387076, 1.000000000000000000, 0.8660254037844387076, 1.000000000000000000, 0.8660254037844387076, 1.000000000000000000, 0.8660254037844387076, 1.000000000000000000, 0.8660254037844387076, 1.000000000000000000, 0.8660254037844387076, 1.000000000000000000, 0.8660254037844387076, 1.000000000000000000, 0.8660254037844387076, 1.000000000000000000, 0.8660254037844387076, 1.000000000000000000, 0.8660254037844387076, 1.000000000000000000, 0.8660254037844387076, 1.000000000000000000, 0.8660254037844387076, 1.000000000000000000, 0.8660254037844387076, 1.000000000000000000, 0.8660254037844387076, 1.000000000000000000, 0.8660254037844387076, 1.000000000000000000, 0.8660254037844387076, 1.000000000000000000, 0.8660254037844387076, 1.000000000000000000, 0.8660254037844387076, 1.000000000000000000, 0.8660254037844387076, 1.000000000000000000, 0.8660254037844387076, 1.000000000000000000, 0.8660254037844387076, 1.000000000000000000, 0.8660254037844387076, 1.000000000000000000, 0.8660254037844387076, 1.000000000000000000, 0.8660254037844387076, 1.000000000000000000, 0.8660254037844387076, 1.000000000000000000, 0.8660254037844387076, 1.000000000000000000, 0.8660254037844387076, 1.000000000000000000, 0.8660254037844387076, 1.000000000000000000, 0.8660254037844387076, 1.000000000000000000, 0.8660254037844387076, 1.000000000000000000, 0.8660254037844387076, 1.000000000000000000, 0.8660254037844387076, 1.000000000000000000, 0.8660254037844387076, 1.000000000000000000, 0.8660254037844387076, 1.000000000000000000, 0.8660254037844387076, 1.000000000000000000, 0.8660254037844387076, 1.000000000000000000, 0.8660254037844387076, 1.000000000000000000, 0.8660254037844387076, 1.000000000000000000, 0.8660254037844387076, 1.000000000000000000, 0.8660254037844387076, 1.000000000000000000, 0.8660254037844387076, 1.000000000000000000, 0.8660254037844387076, 1.000000000000000000, 0.8660254037844387076, 1.000000000000000000, 0.8660254037844387076, 1.000000000000000000, 0.8660254037844387076, 1.000000000000000000, 0.8660254037844387076, 1.000000000000000000, 0.8660254037844387076, 1.000000000000000000, 0.8660254037844387076, 1.000000000000000000, 0.8660254037844387076, 1.000000000000000000, 0.8660254037844387076, 1.000000000000000000, 0.8660254037844387076, 1.000000000000000000, 0.8660254037844387076, 1.000000000000000000, 0.8660254037844387076, 1.000000000000000000, 0.8660254037844387076, 1.000000000000000000, 0.8660254037844387076, 1.000000000000000000, 0.8660254037844387076, 1.000000000000000000, 0.8660254037844387076, 1.000000000000000000, 0.8660254037844387076, 1.000000000000000000, 0.8660254037844387076, 1.000000000000000000, 0.8660254037844387076, 1.000000000000000000, 0.8660254037844387076, 1.000000000000000000, 0.8660254037844387076, 1.000000000000000000, 0.8660254037844387076, 1.000000000000000000, 0.8660254037844387076, 1.000000000000000000, 0.8660254037844387076, 1.000000000000000000, 0.8660254037844387076, 1.000000000000000000, 0.8660254037844387076, 1.000000000000000000, 0.8660254037844387076, 1.000000000000000000, 0.8660254037844387076, 1.000000000000000000, 0.8660254037844387076, 1.000000000000000000, 0.8660254037844387076, 1.000000000000000000, 0.8660254037844387076, 1.000000000000000000, 0.8660254037844387076, 1.000000000000000000, 0.8660254037844387076, 1.000000000000000000, 0.8660254037844387076, 1.000000000000000000, 0.8660254037844387076, 1.000000000000000000, 0.8660254037844387076, 1.000000000000000000, 0.8660254037844387076, 1.000000000000000000, 0.8660254037844387076, 1.000000000000000000, 0.8660254037844387076, 1.000000000000000000, 0.8660254037844387076, 1.000000000000000000, 0.8660254037844387076, 1.000000000000000000, 0.8660254037844387076, 1.000000000000000000, 0.8660254037844387076, 1.000000000000000000, 0.8660254037844387076, 1.000000000000000000, 0.8660254037844387076, 1.000000000000000000, 0.8660254037844387076, 1.000000000000000000, 0.8660254037844387076, 1.000000000000000000, 0.8660254037844387076, 1.000000000000000000, 0.8660254037844387076, 1.000000000000000000, 0.8660254037844387076, 1.000000000000000000, 0.8660254037844387076, 1.000000000000000000, 0.8660254037844387076, 1.000000000000000000, 0.8660254037844387076, 1.000000000000000000, 0.8660254037844387076, 1.000000000000000000, 0.8660254037844387076, 1.000000000000000000, 0.8660254037844387076, 1.000000000000000000, 0.8660254037844387076, 1.000000000000000000, 0.8660254037844387076, 1.000000000000000000, 0.8660254037844387076, 1.000000000000000000, 0.8660254037844387076, 1.000000000000000000, 0.8660254037844387076, 1.000000000000000000, 0.8660254037844387076, 1.000000000000000000, 0.8660254037844387076, 1.000000000000000000, 0.8660254037844387076, 1.000000000000000000, 0.8660254037844387076, 1.000000000000000000, 0.8660254037844387076, 1.000000000000000000, 0.8660254037844387076, 1.000000000000000000, 0.8660254037844387076, 1.000000000000000000, 0.8660254037844387076, 1.000000000000000000, 0.8660254037844387076, 1.000000000000000000, 0.8660254037844387076, 1.000000000000000000, 0.8660254037844387076, 1.000000000000000000, 0.8660254037844387076, 1.000000000000000000, 0.8660254037844387076, 1.000000000000000000, 0.8660254037844387076, 1.000000000000000000, 0.8660254037844387076, 1.000000000000000000, 0.8660254037844387076, 1.000000000000000000, 0.8660254037844387076, 1.000000000000000000, 0.8660254037844387076, 1.000000000000000000, 0.8660254037844387076, 1.000000000000000000, 0.8660254037844387076, 1.000000000000000000, 0.8660254037844387076, 1.000000000000000000, 0.8660254037844387076, 1.000000000000000000, 0.8660254037844387076, 1.000000000000000000, 0.8660254037844387076, 1.000000000000000000, 0.8660254037844387076, 1.000000000000000000, 0.8660254037844387076, 1.000000000000000000, 0.8660254037844387076, 1.000000000000000000, 0.8660254037844387076, 1.000000000000000000, 0.8660254037844387076, 1.000000000000000000, 0.8660254037844387076, 1.000000000000000000, 0.8660254037844387076, 1.000000000000000000, 0.8660254037844387076, 1.000000000000000000, 0.8660254037844387076, 1.000000000000000000, 0.8660254037844387076, 1.000000000000000000, 0.8660254037844387076, 1.000000000000000000, 0.8660254037844387076, 1.000000000000000000, 0.8660254037844387076, 1.000000000000000000, 0.8660254037844387076, 1.000000000000000000, 0.8660254037844387076, 1.000000000000000000, 0.8660254037844387076, 1.000000000000000000, 0.8660254037844387076, 1.000000000000000000, 0.8660254037844387076, 1.000000000000000000, 0.8660254037844387076, 1.000000000000000000, 0.8660254037844387076, 1.000000000000000000, 0.8660254037844387076, 1.000000000000000000, 0.8660254037844387076, 1.000000000000000000, 0.8660254037844387076, 1.000000000000000000, 0.8660254037844387076, 1.000000000000000000, 0.8660254037844387076, 1.000000000000000000, 0.8660254037844387076, 1.000000000000000000, 0.8660254037844387076, 1.000000000000000000, 0.8660254037844387076, 1.000000000000000000, 0.8660254037844387076, 1.000000000000000000, 0.8660254037844387076, 1.000000000000000000, 0.8660254037844387076, 1.000000000000000000, 0.8660254037844387076, 1.000000000000000000, 0.8660254037844387076, 1.000000000000000000, 0.8660254037844387076, 1.000000000000000000, 0.8660254037844387076, 1.000000000000000000, 0.8660254037844387076, 1.000000000000000000, 0.8660254037844387076, 1.000000000000000000, 0.8660254037844387076, 1.000000000000000000, 0.8660254037844387076, 1.000000000000000000, 0.8660254037844387076, 1.000000000000000000, 0.8660254037844387076, 1.000000000000000000, 0.8660254037844387076, 1.000000000000000000, 0.8660254037844387076, 1.000000000000000000, 0.8660254037844387076, 1.000000000000000000, 0.8660254037844387076, 1.000000000000000000, 0.8660254037844387076, 1.000000000000000000, 0.8660254037844387076, 1.000000000000000000, 0.8660254037844387076, 1.000000000000000000, 0.8660254037844387076, 1.000000000000000000, 0.8660254037844387076, 1.000000000000000000, 0.8660254037844387076, 1.000000000000000000, 0.8660254037844387076, 1.000000000000000000, 0.8660254037844387076, 1.000000000000000000, 0.8660254037844387076, 1.000000000000000000, 0.8660254037844387076, 1.000000000000000000, 0.8660254037844387076, 1.000000000000000000, 0.8660254037844387076, 1.000000000000000000, 0.8660254037844387076, 1.000000000000000000, 0.8660254037844387076, 1.000000000000000000, 0.8660254037844387076, 1.000000000000000000, 0.8660254037844387076, 1.000000000000000000, 0.8660254037844387076, 1.000000000000000000, 0.8660254037844387076, 1.000000000000000000, 0.8660254037844387076, 1.000000000000000000, 0.8660254037844387076, 1.000000000000000000, 0.8660254037844387076, 1.000000000000000000, 0.8660254037844387076, 1.000000000000000000, 0.8660254037844387076, 1.000000000000000000, 0.8660254037844387076, 1.000000000000000000, 0.8660254037844387076, 1.000000000000000000, 0.8660254037844387076, 1.000000000000000000, 0.8660254037844387076, 1.000000000000000000, 0.8660254037844387076, 1.000000000000000000, 0.8660254037844387076, 1.000000000000000000, 0.8660254037844387076, 1.000000000000000000, 0.8660254037844387076, 1.000000000000000000, 0.8660254037844387076, 1.000000000000000000, 0.8660254037844387076, 1.000000000000000000, 0.8660254037844387076, 1.000000000000000000, 0.8660254037844387076, 1.000000000000000000, 0.8660254037844387076, 1.000000000000000000, 0.8660254037844387076, 1.000000000000000000, 0.8660254037844387076, 1.000000000000000000, 0.8660254037844387076, 1.000000000000000000, 0.8660254037844387076, 1.000000000000000000, 0.8660254037844387076, 1.000000000000000000, 0.8660254037844387076, 1.000000000000000000, 0.8660254037844387076, 1.000000000000000000, 0.8660254037844387076, 1.000000000000000000, 0.8660254037844387076, 1.000000000000000000, 0.8660254037844387076, 1.000000000000000000, 0.8660254037844387076, 1.000000000000000000, 0.8660254037844387076, 1.000000000000000000, 0.8660254037844387076, 1.000000000000000000, 0.8660254037844387076, 1.000000000000000000, 0.8660254037844387076, 1.000000000000000000, 0.8660254037844387076, 1.000000000000000000, 0.8660254037844387076, 1.000000000000000000, 0.8660254037844387076, 1.000000000000000000, 0.8660254037844387076, 1.000000000000000000, 0.8660254037844387076, 1.000000000000000000, 0.8660254037844387076, 1.000000000000000000, 0.8660254037844387076, 1.000000000000000000, 0.8660254037844387076, 1.000000000000000000, 0.8660254037844387076, 1.000000000000000000, 0.8660254037844387076, 1.000000000000000000, 0.8660254037844387076, 1.000000000000000000, 0.8660254037844387076, 1.000000000000000000, 0.8660254037844387076, 1.000000000000000000, 0.8660254037844387076, 1.000000000000000000, 0.8660254037844387076, 1.000000000000000000, 0.8660254037844387076, 1.000000000000000000, 0.8660254037844387076, 1.000000000000000000, 0.8660254037844387076, 1.000000000000000000, 0.8660254037844387076, 1.000000000000000000, 0.8660254037844387076, 1.000000000000000000, 0.8660254037844387076, 1.000000000000000000, 0.8660254037844387076, 1.000000000000000000, 0.8660254037844387076, 1.000000000000000000, 0.8660254037844387076, 1.000000000000000000, 0.8660254037844387076, 1.000000000000000000, 0.8660254037844387076, 1.000000000000000000, 0.8660254037844387076, 1.000000000000000000, 0.8660254037844387076, 1.000000000000000000, 0.8660254037844387076, 1.000000000000000000, 0.8660254037844387076, 1.000000000000000000, 0.8660254037844387076, 1.000000000000000000, 0.8660254037844387076, 1.000000000000000000, 0.8660254037844387076, 1.000000000000000000, 0.8660254037844387076, 1.000000000000000000, 0.8660254037844387076, 1.000000000000000000, 0.8660254037844387076, 1.000000000000000000, 0.8660254037844387076, 1.000000000000000000, 0.8660254037844387076, 1.000000000000000000, 0.8660254037844387076, 1.000000000000000000, 0.8660254037844387076, 1.000000000000000000, 0.8660254037844387076, 1.000000000000000000, 0.8660254037844387076, 1.000000000000000000, 0.8660254037844387076, 1.000000000000000000, 0.8660254037844387076, 1.000000000000000000, 0.8660254037844387076, 1.000000000000000000, 0.8660254037844387076, 1.000000000000000000, 0.8660254037844387076, 1.000000000000000000, 0.8660254037844387076, 1.000000000000000000, 0.8660254037844387076, 1.000000000000000000, 0.8660254037844387076, 1.000000000000000000, 0.8660254037844387076, 1.000000000000000000, 0.8660254037844387076, 1.000000000000000000, 0.8660254037844387076, 1.000000000000000000, 0.8660254037844387076, 1.000000000000000000, 0.8660254037844387076, 1.000000000000000000, 0.8660254037844387076, 1.000000000000000000, 0.8660254037844387076, 1.000000000000000000, 0.8660254037844387076, 1.000000000000000000, 0.8660254037844387076, 1.000000000000000000, 0.8660254037844387076, 1.000000000000000000, 0.8660254037844387076, 1.000000000000000000, 0.8660254037844387076, 1.000000000000000000, 0.8660254037844387076, 1.000000000000000000, 0.8660254037844387076, 1.000000000000000000, 0.8660254037844387076, 1.000000000000000000, 0.8660254037844387076, 1.000000000000000000, 0.8660254037844387076, 1.000000000000000000, 0.8660254037844387076, 1.000000000000000000, 0.8660254037844387076, 1.000000000000000000, 0.8660254037844387076, 1.000000000000000000, 0.8660254037844387076, 1.000000000000000000, 0.8660254037844387076, 1.000000000000000000, 0.8660254037844387076, 1.000000000000000000, 0.8660254037844387076, 1.000000000000000000, 0.8660254037844387076, 1.000000000000000000, 0.8660254037844387076, 1.000000000000000000, 0.8660254037844387076, 1.000000000000000000, 0.8660254037844387076, 1.000000000000000000, 0.8660254037844387076, 1.000000000000000000, 0.8660254037844387076, 1.000000000000000000, 0.8660254037844387076, 1.000000000000000000, 0.8660254037844387076, 1.000000000000000000, 0.8660254037844387076, 1.000000000000000000, 0.8660254037844387076, 1.000000000000000000, 0.8660254037844387076, 1.000000000000000000, 0.8660254037844387076, 1.000000000000000000, 0.8660254037844387076, 1.000000000000000000, 0.8660254037844387076, 1.000000000000000000, 0.8660254037844387076, 1.000000000000000000, 0.8660254037844387076, 1.000000000000000000, 0.8660254037844387076, 1.000000000000000000, 0.8660254037844387076, 1.000000000000000000, 0.8660254037844387076, 1.000000000000000000, 0.8660254037844387076, 1.000000000000000000, 0.8660254037844387076, 1.000000000000000000, 0.8660254037844387076, 1.000000000000000000, 0.8660254037844387076, 1.000000000000000000, 0.8660254037844387076, 1.000000000000000000, 0.8660254037844387076, 1.000000000000000000, 0.8660254037844387076, 1.000000000000000000, 0.8660254037844387076, 1.000000000000000000, 0.8660254037844387076, 1.000000000000000000, 0.8660254037844387076, 1.000000000000000000, 0.8660254037844387076, 1.000000000000000000, 0.8660254037844387076, 1.000000000000000000, 0.8660254037844387076, 1.000000000000000000, 0.8660254037844387076, 1.000000000000000000, 0.8660254037844387076, 1.000000000000000000, 0.8660254037844387076, 1.000000000000000000, 0.8660254037844387076, 1.000000000000000000, 0.8660254037844387076, 1.000000000000000000, 0.8660254037844387076, 1.000000000000000000, 0.8660254037844387076, 1.000000000000000000, 0.8660254037844387076, 1.000000000000000000, 0.8660254037844387076, 1.000000000000000000, 0.8660254037844387076, 1.000000000000000000, 0.8660254037844387076, 1.000000000000000000, 0.8660254037844387076, 1.000000000000000000, 0.8660254037844387076, 1.000000000000000000, 0.8660254037844387076, 1.000000000000000000, 0.8660254037844387076, 1.000000000000000000, 0.8660254037844387076, 1.000000000000000000, 0.8660254037844387076, 1.000000000000000000, 0.8660254037844387076, 1.000000000000000000, 0.8660254037844387076, 1.000000000000000000, 0.8660254037844387076, 1.000000000000000000, 0.8660254037844387076, 1.000000000000000000, 0.8660254037844387076, 1.000000000000000000, 0.8660254037844387076, 1.000000000000000000, 0.8660254037844387076, 1.000000000000000000, 0.8660254037844387076, 1.000000000000000000, 0.8660254037844387076, 1.000000000000000000, 0.8660254037844387076, 1.000000000000000000, 0.8660254037844387076, 1.000000000000000000, 0.8660254037844387076, 1.000000000000000000, 0.8660254037844387076, 1.000000000000000000, 0.8660254037844387076, 1.000000000000000000, 0.8660254037844387076, 1.000000000000000000, 0.8660254037844387076, 1.000000000000000000, 0.8660254037844387076, 1.000000000000000000, 0.8660254037844387076, 1.000000000000000000, 0.8660254037844387076, 1.000000000000000000, 0.8660254037844387076, 1.000000000000000000, 0.8660254037844387076, 1.000000000000000000, 0.8660254037844387076, 1.000000000000000000, 0.8660254037844387076, 1.000000000000000000, 0.8660254037844387076, 1.000000000000000000, 0.8660254037844387076, 1.000000000000000000, 0.8660254037844387076, 1.000000000000000000, 0.8660254037844387076, 1.000000000000000000, 0.8660254037844387076, 1.000000000000000000, 0.8660254037844387076, 1.000000000000000000, 0.8660254037844387076, 1.000000000000000000, 0.8660254037844387076, 1.000000000000000000, 0.8660254037844387076, 1.000000000000000000, 0.8660254037844387076, 1.000000000000000000, 0.8660254037844387076, 1.000000000000000000, 0.8660254037844387076, 1.000000000000000000, 0.8660254037844387076, 1.000000000000000000, 0.8660254037844387076, 1.000000000000000000, 0.8660254037844387076, 1.000000000000000000, 0.8660254037844387076, 1.000000000000000000, 0.8660254037844387076, 1.000000000000000000, 0.8660254037844387076, 1.000000000000000000, 0.8660254037844387076, 1.000000000000000000, 0.8660254037844387076, 1.000000000000000000, 0.8660254037844387076, 1.000000000000000000, 0.8660254037844387076, 1.000000000000000000, 0.8660254037844387076, 1.000000000000000000, 0.8660254037844387076, 1.000000000000000000, 0.8660254037844387076, 1.000000000000000000, 0.8660254037844387076, 1.000000000000000000, 0.8660254037844387076, 1.000000000000000000, 0.8660254037844387076, 1.000000000000000000, 0.8660254037844387076, 1.000000000000000000, 0.8660254037844387076, 1.000000000000000000, 0.8660254037844387076, 1.000000000000000000, 0.8660254037844387076, 1.000000000000000000, 0.8660254037844387076, 1.000000000000000000, 0.8660254037844387076, 1.000000000000000000, 0.8660254037844387076, 1.000000000000000000, 0.8660254037844387076, 1.000000000000000000, 0.8660254037844387076, 1.000000000000000000, 0.8660254037844387076, 1.000000000000000000, 0.8660254037844387076, 1.000000000000000000, 0.8660254037844387076, 1.000000000000000000, 0.8660254037844387076, 1.000000000000000000, 0.8660254037844387076, 1.000000000000000000, 0.8660254037844387076, 1.000000000000000000, 0.8660254037844387076, 1.000000000000000000, 0.8660254037844387076, 1.000000000000000000, 0.8660254037844387076, 1.000000000000000000, 0.8660254037844387076, 1.000000000000000000, 0.8660254037844387076, 1.000000000000000000, 0.8660254037844387076, 1.000000000000000000, 0.8660254037844387076, 1.000000000000000000, 0.8660254037844387076, 1.000000000000000000, 0.8660254037844387076, 1.000000000000000000, 0.8660254037844387076, 1.000000000000000000, 0.8660254037844387076, 1.000000000000000000, 0.8660254037844387076, 1.000000000000000000, 0.8660254037844387076, 1.000000000000000000, 0.8660254037844387076, 1.000000000000000000, 0.8660254037844387076, 1.000000000000000000, 0.8660254037844387076, 1.000000000000000000, 0.8660254037844387076, 1.000000000000000000, 0.8660254037844387076, 1.000000000000000000, 0.8660254037844387076, 1.000000000000000000, 0.8660254037844387076, 1.000000000000000000, 0.8660254037844387076, 1.000000000000000000, 0.8660254037844387076, 1.000000000000000000, 0.8660254037844387076, 1.000000000000000000, 0.8660254037844387076, 1.000000000000000000, 0.8660254037844387076, 1.000000000000000000, 0.8660254037844387076, 1.000000000000000000, 0.8660254037844387076, 1.000000000000000000, 0.8660254037844387076, 1.000000000000000000, 0.8660254037844387076, 1.000000000000000000, 0.8660254037844387076, 1.000000000000000000, 0.8660254037844387076, 1.000000000000000000, 0.8660254037844387076, 1.000000000000000000, 0.8660254037844387076, 1.000000000000000000, 0.8660254037844387076, 1.000000000000000000, 0.8660254037844387076, 1.000000000000000000, 0.8660254037844387076, 1.000000000000000000, 0.8660254037844387076, 1.000000000000000000, 0.8660254037844387076, 1.000000000000000000, 0.8660254037844387076, 1.000000000000000000, 0.8660254037844387076, 1.000000000000000000, 0.8660254037844387076, 1.000000000000000000, 0.8660254037844387076, 1.000000000000000000, 0.8660254037844387076, 1.000000000000000000, 0.8660254037844387076, 1.000000000000000000, 0.8660254037844387076, 1.000000000000000000, 0.8660254037844387076, 1.000000000000000000, 0.8660254037844387076, 1.000000000000000000, 0.8660254037844387076, 1.000000000000000000, 0.8660254037844387076, 1.000000000000000000, 0.8660254037844387076, 1.000000000000000000, 0.8660254037844387076, 1.000000000000000000, 0.8660254037844387076, 1.000000000000000000, 0.8660254037844387076, 1.000000000000000000, 0.8660254037844387076, 1.000000000000000000, 0.8660254037844387076, 1.000000000000000000, 0.8660254037844387076, 1.000000000000000000, 0.8660254037844387076, 1.000000000000000000, 0.8660254037844387076, 1.000000000000000000, 0.8660254037844387076, 1.000000000000000000, 0.8660254037844387076, 1.000000000000000000, 0.8660254037844387076, 1.000000000000000000, 0.8660254037844387076, 1.000000000000000000, 0.8660254037844387076, 1.000000000000000000, 0.8660254037844387076, 1.000000000000000000, 0.8660254037844387076, 1.000000000000000000, 0.8660254037844387076, 1.000000000000000000, 0.8660254037844387076, 1.000000000000000000, 0.8660254037844387076, 1.000000000000000000, 0.8660254037844387076, 1.000000000000000000, 0.8660254037844387076, 1.000000000000000000, 0.8660254037844387076, 1.000000000000000000, 0.8660254037844387076, 1.000000000000000000, 0.8660254037844387076, 1.000000000000000000, 0.8660254037844387076, 1.000000000000000000, 0.8660254037844387076, 1.000000000000000000, 0.8660254037844387076, 1.000000000000000000, 0.8660254037844387076, 1.000000000000000000, 0.8660254037844387076, 1.000000000000000000, 0.8660254037844387076, 1.000000000000000000, 0.8660254037844387076, 1.000000000000000000, 0.8660254037844387076, 1.000000000000000000, 0.8660254037844387076, 1.000000000000000000, 0.8660254037844387076, 1.000000000000000000, 0.8660254037844387076, 1.000000000000000000, 0.8660254037844387076, 1.000000000000000000, 0.8660254037844387076, 1.000000000000000000, 0.8660254037844387076, 1.000000000000000000, 0.8660254037844387076, 1.000000000000000000, 0.8660254037844387076, 1.000000000000000000, 0.8660254037844387076, 1.000000000000000000, 0.8660254037844387076, 1.000000000000000000, 0.8660254037844387076, 1.000000000000000000, 0.8660254037844387076, 1.000000000000000000, 0.8660254037844387076, 1.000000000000000000, 0.8660254037844387076, 1.000000000000000000, 0.8660254037844387076, 1.000000000000000000, 0.8660254037844387076, 1.000000000000000000, 0.8660254037844387076, 1.000000000000000000, 0.8660254037844387076, 1.000000000000000000, 0.8660254037844387076, 1.000000000000000000, 0.8660254037844387076, 1.000000000000000000, 0.8660254037844387076, 1.000000000000000000, 0.8660254037844387076, 1.000000000000000000, 0.8660254037844387076, 1.000000000000000000, 0.8660254037844387076, 1.000000000000000000, 0.8660254037844387076, 1.000000000000000000, 0.8660254037844387076, 1.000000000000000000, 0.8660254037844387076, 1.000000000000000000, 0.8660254037844387076, 1.000000000000000000, 0.8660254037844387076, 1.000000000000000000, 0.8660254037844387076, 1.000000000000000000, 0.8660254037844387076, 1.000000000000000000, 0.8660254037844387076, 1.000000000000000000, 0.8660254037844387076, 1.000000000000000000, 0.8660254037844387076, 1.000000000000000000, 0.8660254037844387076, 1.000000000000000000, 0.8660254037844387076, 1.000000000000000000 ) ) 
 REPRESENTATION_ITEM ( '' )  );
#19963 = FILL_AREA_STYLE ('',( #16661 ) ) ;
#19964 = CARTESIAN_POINT ( 'NONE',  ( -2.500000000000000444, 6.833333333333333925, -4.330127018922193649 ) ) ;
#19965 = CARTESIAN_POINT ( 'NONE',  ( -9.184850993605147944E-16, -139.3750000027312126, 5.000000000000000000 ) ) ;
#19966 = CARTESIAN_POINT ( 'NONE',  ( -1.339745962155613812, -60.08034179853027723, -5.000000000000000000 ) ) ;
#19967 = CARTESIAN_POINT ( 'NONE',  ( -3.152548672688508926E-16, -52.56249999863440792, -5.148502694627439702 ) ) ;
#19968 = CARTESIAN_POINT ( 'NONE',  ( -2.500000000000000444, -89.04166666393547303, -4.330127018922193649 ) ) ;
#19969 = CARTESIAN_POINT ( 'NONE',  ( 2.229367062499998831, -35.64583333196772941, -3.861377020970580887 ) ) ;
#19970 = VECTOR ( 'NONE', #54008, 1000.000000000000000 ) ;
#19971 = CARTESIAN_POINT ( 'NONE',  ( -2.500000000000000444, 19.95833333606451987, -4.330127018922193649 ) ) ;
#19972 = EDGE_CURVE ( 'NONE', #45194, #47814, #38962, .T. ) ;
#19973 = CARTESIAN_POINT ( 'NONE',  ( 5.000000000000000000, -142.1250000027312126, 0.000000000000000000 ) ) ;
#19974 = CARTESIAN_POINT ( 'NONE',  ( -50.01589407740564042, -151.7500000027312410, 0.3983568153799778022 ) ) ;
#19975 = EDGE_CURVE ( 'NONE', #31318, #4973, #22606, .T. ) ;
#19976 = CARTESIAN_POINT ( 'NONE',  ( 3.152801135295367541, -153.5625000013656063, -3.152801135295367541 ) ) ;
#19977 = CARTESIAN_POINT ( 'NONE',  ( -2.500000000000000444, -41.16666666666667140, -4.330127018922193649 ) ) ;
#19978 = CARTESIAN_POINT ( 'NONE',  ( -59.71086361768055184, -135.0000000000000000, -0.7912278194080049065 ) ) ;
#19979 = ORIENTED_EDGE ( 'NONE', *, *, #39441, .F. ) ;
#19980 = CARTESIAN_POINT ( 'NONE',  ( -3.152548672688508926E-16, -103.5624999986344221, -5.148502694627439702 ) ) ;
#19981 = CARTESIAN_POINT ( 'NONE',  ( 4.458734124999999437, 2.937500001365594304, -5.460374474430324690E-16 ) ) ;
#19982 = CYLINDRICAL_SURFACE ( 'NONE', #1124, 5.000000000000000000 ) ;
#19983 = CARTESIAN_POINT ( 'NONE',  ( -2.499999999999996447, -2.833333333333333481, 4.330127018922195425 ) ) ;
#19984 = EDGE_CURVE ( 'NONE', #32825, #29058, #3096, .T. ) ;
#19985 = CARTESIAN_POINT ( 'NONE',  ( -2.229367062499996610, -68.14583333196773651, 3.861377020970582219 ) ) ;
#19986 = CARTESIAN_POINT ( 'NONE',  ( -1.339745962155610925, -30.66965819600732956, 5.000000000000000000 ) ) ;
#19987 = CARTESIAN_POINT ( 'NONE',  ( 5.000000000000000000, -1.374999997268814500, -6.123233995736766282E-16 ) ) ;
#19989 = VERTEX_POINT ( 'NONE', #34140 ) ;
#19988 = CARTESIAN_POINT ( 'NONE',  ( 2.229367062500001939, -32.97916666530106511, 3.861377020970579999 ) ) ;
#19990 = CARTESIAN_POINT ( 'NONE',  ( -6.972266317189433020E-16, 17.87500000273118417, -5.000000000000000000 ) ) ;
#19991 = CARTESIAN_POINT ( 'NONE',  ( 1.975475456537005874E-15, 19.25000000000000000, 5.000000000000000000 ) ) ;
#19992 = ORIENTED_EDGE ( 'NONE', *, *, #10952, .F. ) ;
#19993 = CARTESIAN_POINT ( 'NONE',  ( 1.339745962155615144, 5.294658198738519950, 4.999999999999999112 ) ) ;
#19994 = CARTESIAN_POINT ( 'NONE',  ( -3.535250795749689387E-16, -50.25000000000000711, -5.773502691896257311 ) ) ;
#19996 = CARTESIAN_POINT ( 'NONE',  ( -4.458734124999999437, -23.56249999863440436, 0.000000000000000000 ) ) ;
#19995 = CARTESIAN_POINT ( 'NONE',  ( 1.339745962155612702, -17.16965819600733312, -5.000000000000000000 ) ) ;
#19997 = CARTESIAN_POINT ( 'NONE',  ( -2.500000000000000444, -4.166666666666666075, -4.330127018922193649 ) ) ;
#19998 = CARTESIAN_POINT ( 'NONE',  ( 4.458734124999999437, -72.81249999863439371, -5.460374474430324690E-16 ) ) ;
#19999 = CARTESIAN_POINT ( 'NONE',  ( -4.458734125000001214, -143.1250000013656063, 1.846868145590734089 ) ) ;
#20000 = CARTESIAN_POINT ( 'NONE',  ( 2.229367062499998831, -83.64583333196773651, -3.861377020970580887 ) ) ;
#20001 = CARTESIAN_POINT ( 'NONE',  ( -59.59170313451811296, -140.7500000013655779, 1.485763867205729394 ) ) ;
#20002 = CARTESIAN_POINT ( 'NONE',  ( -2.229367062500000163, -31.72916666530107577, -3.861377020970580443 ) ) ;
#20003 = CARTESIAN_POINT ( 'NONE',  ( -5.000000000000000000, -71.87499999726880162, 0.000000000000000000 ) ) ;
#20004 = ORIENTED_EDGE ( 'NONE', *, *, #62997, .T. ) ;
#20005 = EDGE_CURVE ( 'NONE', #62925, #45741, #30591, .T. ) ;
#20006 = CARTESIAN_POINT ( 'NONE',  ( 0.000000000000000000, -170.0000000000000000, 5.000000000000000000 ) ) ;
#20007 = ORIENTED_EDGE ( 'NONE', *, *, #22457, .T. ) ;
#20008 = CARTESIAN_POINT ( 'NONE',  ( 2.229367062499998831, -70.89583333196773651, -3.861377020970580887 ) ) ;
#20009 = CARTESIAN_POINT ( 'NONE',  ( 1.339745962155613146, 28.29465819873852084, 5.000000000000000888 ) ) ;
#20010 =( LENGTH_UNIT ( ) NAMED_UNIT ( * ) SI_UNIT ( .MILLI., .METRE. ) );
#20011 = VERTEX_POINT ( 'NONE', #44741 ) ;
#20012 = CARTESIAN_POINT ( 'NONE',  ( -2.500000000000000444, -39.16666666666667140, -4.330127018922193649 ) ) ;
#20013 = CARTESIAN_POINT ( 'NONE',  ( -51.75738570946856498, -142.8750000027312126, 3.805975901505576964 ) ) ;
#20014 = CARTESIAN_POINT ( 'NONE',  ( 4.458734124999999437, -58.06249999863440081, -5.460374474430324690E-16 ) ) ;
#20015 = CARTESIAN_POINT ( 'NONE',  ( -4.458734124999999437, -5.562499998634402587, 0.000000000000000000 ) ) ;
#20016 = EDGE_LOOP ( 'NONE', ( #7290, #28433, #6643, #46526 ) ) ;
#20017 = AXIS2_PLACEMENT_3D ( 'NONE', #26658, #7683, #27289 ) ;
#20018 = CARTESIAN_POINT ( 'NONE',  ( -5.000000000000000888, -146.4375000000000000, 2.071067811865474617 ) ) ;
#20019 = CARTESIAN_POINT ( 'NONE',  ( -6.972266317189433020E-16, -2.124999997268814056, -5.000000000000000000 ) ) ;
#20020 = CARTESIAN_POINT ( 'NONE',  ( -2.229367062499996610, 12.85416666803226171, 3.861377020970582219 ) ) ;
#20021 = CARTESIAN_POINT ( 'NONE',  ( -50.70258187064364108, -139.1250000013656063, 2.196230717870141014 ) ) ;
#20022 = CARTESIAN_POINT ( 'NONE',  ( -6.972266317189433020E-16, -24.24999999999999645, -5.000000000000000000 ) ) ;
#20023 = CARTESIAN_POINT ( 'NONE',  ( -8.190561711645485556E-16, -161.6875000013655779, 4.458734124999999437 ) ) ;
#20024 = VERTEX_POINT ( 'NONE', #58286 ) ;
#20025 = CARTESIAN_POINT ( 'NONE',  ( -4.458734124999997661, -82.22916666530106511, 2.574251347313722516 ) ) ;
#20026 = CARTESIAN_POINT ( 'NONE',  ( 5.000000000000000000, -39.41666666666667851, -2.886751345948130876 ) ) ;
#20027 = CARTESIAN_POINT ( 'NONE',  ( -3.152548672688508926E-16, 2.437500001365594304, -5.148502694627439702 ) ) ;
#20028 = EDGE_CURVE ( 'NONE', #48755, #30395, #10371, .T. ) ;
#20029 = CARTESIAN_POINT ( 'NONE',  ( 1.060575238724906964E-15, -82.75000000000001421, 5.773502691896257311 ) ) ;
#20030 = CARTESIAN_POINT ( 'NONE',  ( 1.339745962155615144, -40.58034179853029144, 4.999999999999999112 ) ) ;
#20031 = CARTESIAN_POINT ( 'NONE',  ( 4.458734125000001214, -64.14583333196773651, 2.574251347313718519 ) ) ;
#20033 = B_SPLINE_CURVE_WITH_KNOTS ( 'NONE', 3,
 ( #44703, #668, #5798, #45990, #1322, #39878, #50176, #41153, #50507 ),
 .UNSPECIFIED., .F., .F.,
 ( 4, 2, 1, 2, 4 ),
 ( 0.000000000000000000, 0.002165063509461097498, 0.004330127018922194995, 0.006495190528383292493, 0.008660254037844389990 ),
 .UNSPECIFIED. ) ;
#20032 = CARTESIAN_POINT ( 'NONE',  ( 5.000000000000000888, -27.45833333060214798, 2.886751345948126879 ) ) ;
#20034 = CARTESIAN_POINT ( 'NONE',  ( -6.972266317189433020E-16, 12.87500000273118417, -5.000000000000000000 ) ) ;
#20035 = CARTESIAN_POINT ( 'NONE',  ( 2.500000000000002220, -78.54166666393547303, 4.330127018922192761 ) ) ;
#20036 = CARTESIAN_POINT ( 'NONE',  ( 1.975475456537005874E-15, -64.62499999726880162, 5.000000000000000000 ) ) ;
#20037 = SURFACE_SIDE_STYLE ('',( #58957 ) ) ;
#20038 = CARTESIAN_POINT ( 'NONE',  ( -4.458734124999999437, -46.31249999863440792, 0.000000000000000000 ) ) ;
#20039 = CARTESIAN_POINT ( 'NONE',  ( -4.458734124999999437, -32.56249999863440792, 0.000000000000000000 ) ) ;
#20040 = CARTESIAN_POINT ( 'NONE',  ( -2.229367062500000163, 5.270833334698927786, -3.861377020970580443 ) ) ;
#20041 = CARTESIAN_POINT ( 'NONE',  ( -5.000000000000000000, -9.958333330602144429, -2.886751345948128211 ) ) ;
#20042 = CARTESIAN_POINT ( 'NONE',  ( 5.000000000000000000, 18.58333333333333215, -2.886751345948129988 ) ) ;
#20043 = CARTESIAN_POINT ( 'NONE',  ( 3.535533905932736864, -151.2500000027312126, 3.535533905932738641 ) ) ;
#20044 = CARTESIAN_POINT ( 'NONE',  ( 1.339745962155612702, -54.16965819600732601, -5.000000000000000000 ) ) ;
#20045 = CARTESIAN_POINT ( 'NONE',  ( 9.457646018065525792E-16, -36.06249999863441502, 5.148502694627439702 ) ) ;
#20046 = CARTESIAN_POINT ( 'NONE',  ( -5.000000000000000000, -75.95833333060215864, -2.886751345948128211 ) ) ;
#20047 =( BOUNDED_CURVE ( )  B_SPLINE_CURVE ( 2, ( #62463, #24784, #671, #29270, #48900, #4844, #58247, #29917, #9349 ),
 .UNSPECIFIED., .F., .F. ) 
 B_SPLINE_CURVE_WITH_KNOTS ( ( 3, 2, 2, 2, 3 ),
 ( 0.1687500000000000111, 0.1694444444444444531, 0.1708333333333333370, 0.1722222222222222210, 0.1729166666666666630 ),
 .UNSPECIFIED. ) 
 CURVE ( )  GEOMETRIC_REPRESENTATION_ITEM ( )  RATIONAL_B_SPLINE_CURVE ( ( 0.9330127018922194093, 0.9330127018922194093, 1.000000000000000000, 0.8660254037844387076, 1.000000000000000000, 0.8660254037844387076, 1.000000000000000000, 0.9330127018922194093, 0.9330127018922194093 ) ) 
 REPRESENTATION_ITEM ( '' )  );
#20048 = CARTESIAN_POINT ( 'NONE',  ( -50.40829686548195099, -143.2500000013656063, -1.485763867205728284 ) ) ;
#20049 = FACE_OUTER_BOUND ( 'NONE', #48229, .T. ) ;
#20050 = CARTESIAN_POINT ( 'NONE',  ( 2.459698528280935825, -7.240146430416073642, -0.09933465333851955459 ) ) ;
#20051 = EDGE_CURVE ( 'NONE', #7918, #62831, #5872, .T. ) ;
#20052 = CARTESIAN_POINT ( 'NONE',  ( 2.229367062499998831, -81.89583333196773651, -3.861377020970580887 ) ) ;
#20053 = CARTESIAN_POINT ( 'NONE',  ( -4.458734124999999437, -166.1875000013655779, -5.460374474430324690E-16 ) ) ;
#20054 = CARTESIAN_POINT ( 'NONE',  ( -6.972266317189433020E-16, 18.87500000273119127, -5.000000000000000000 ) ) ;
#20055 = PLANE ( 'NONE',  #3048 ) ;
#20056 = CARTESIAN_POINT ( 'NONE',  ( 1.060575238724906964E-15, -25.75000000000000000, 5.773502691896257311 ) ) ;
#20057 = CARTESIAN_POINT ( 'NONE',  ( 3.152801135295367541, -145.3125000013655779, -3.152801135295367541 ) ) ;
#20058 = ORIENTED_EDGE ( 'NONE', *, *, #30369, .F. ) ;
#20059 = CARTESIAN_POINT ( 'NONE',  ( -2.499999999999996447, -90.70833333060214443, 4.330127018922195425 ) ) ;
#20060 = ORIENTED_EDGE ( 'NONE', *, *, #56942, .F. ) ;
#20061 = CARTESIAN_POINT ( 'NONE',  ( 4.458734124999999437, -61.06249999863440081, -5.460374474430324690E-16 ) ) ;
#20062 = CARTESIAN_POINT ( 'NONE',  ( -2.499999999999996447, 22.29166666939785202, 4.330127018922195425 ) ) ;
#20063 = CARTESIAN_POINT ( 'NONE',  ( -2.499999999999996447, 15.16666666666666607, 4.330127018922195425 ) ) ;
#20064 = CARTESIAN_POINT ( 'NONE',  ( -2.229367062499996610, -50.14583333196772941, 3.861377020970582219 ) ) ;
#20065 = VECTOR ( 'NONE', #45338, 1000.000000000000000 ) ;
#20066 = CARTESIAN_POINT ( 'NONE',  ( -4.458734124999999437, -4.312499998634401699, 0.000000000000000000 ) ) ;
#20067 =( BOUNDED_CURVE ( )  B_SPLINE_CURVE ( 2, ( #5019, #19167, #39416, #23394, #24638, #63570, #14031, #47813, #43609 ),
 .UNSPECIFIED., .F., .F. ) 
 B_SPLINE_CURVE_WITH_KNOTS ( ( 3, 2, 2, 2, 3 ),
 ( 0.2660714285714285698, 0.2666666666666666630, 0.2678571428571428492, 0.2690476190476190355, 0.2696428571428571286 ),
 .UNSPECIFIED. ) 
 CURVE ( )  GEOMETRIC_REPRESENTATION_ITEM ( )  RATIONAL_B_SPLINE_CURVE ( ( 0.9330127018922194093, 0.9330127018922194093, 1.000000000000000000, 0.8660254037844387076, 1.000000000000000000, 0.8660254037844387076, 1.000000000000000000, 0.9330127018922194093, 0.9330127018922194093 ) ) 
 REPRESENTATION_ITEM ( '' )  );
#20068 = CARTESIAN_POINT ( 'NONE',  ( -1.339745962155613812, -23.20534180126147916, -5.000000000000000000 ) ) ;
#20069 = CARTESIAN_POINT ( 'NONE',  ( 3.061616997868383141E-16, -164.8750000027311842, -5.000000000000000000 ) ) ;
#20070 = FACE_OUTER_BOUND ( 'NONE', #12780, .T. ) ;
#20072 = CARTESIAN_POINT ( 'NONE',  ( -4.458734124999999437, -22.39583333196773651, -2.574251347313719407 ) ) ;
#20071 = CARTESIAN_POINT ( 'NONE',  ( -57.46284108482265651, -150.9375000000000000, 4.819101127000238627 ) ) ;
#20073 = CARTESIAN_POINT ( 'NONE',  ( -5.000000000000000000, -31.87499999726880873, 0.000000000000000000 ) ) ;
#20074 = CARTESIAN_POINT ( 'NONE',  ( 4.458734124999998549, -52.72916666530107221, -2.574251347313721627 ) ) ;
#20075 = CARTESIAN_POINT ( 'NONE',  ( 4.458734125000000326, -156.6250000013655779, -1.846868145590734978 ) ) ;
#20076 = EDGE_CURVE ( 'NONE', #25951, #34696, #39278, .T. ) ;
#20077 = CARTESIAN_POINT ( 'NONE',  ( -5.000000000000000000, -57.87499999726880873, 0.000000000000000000 ) ) ;
#20078 = VERTEX_POINT ( 'NONE', #49261 ) ;
#20079 = CARTESIAN_POINT ( 'NONE',  ( 5.000000000000000888, -26.58333333333333215, 2.886751345948126879 ) ) ;
#20080 = CARTESIAN_POINT ( 'NONE',  ( 4.458734125000001214, 5.854166668032262599, 2.574251347313718519 ) ) ;
#20081 = VERTEX_POINT ( 'NONE', #24817 ) ;
#20083 = CARTESIAN_POINT ( 'NONE',  ( -1.339745962155613812, -29.20534180126147916, -5.000000000000000000 ) ) ;
#20082 = CARTESIAN_POINT ( 'NONE',  ( 1.339745962155612702, -4.294658198738519062, -5.000000000000000000 ) ) ;
#20084 = CARTESIAN_POINT ( 'NONE',  ( -4.458734125000000326, -156.0000000013656063, -1.846868145590735644 ) ) ;
#20085 = ORIENTED_EDGE ( 'NONE', *, *, #4279, .T. ) ;
#20086 = CARTESIAN_POINT ( 'NONE',  ( 1.339745962155615144, -87.58034179853028434, 4.999999999999999112 ) ) ;
#20087 = CARTESIAN_POINT ( 'NONE',  ( -59.81910112700025905, -130.1875000000000568, -2.462841084822630311 ) ) ;
#20088 = CARTESIAN_POINT ( 'NONE',  ( 5.000000000000000000, -86.41666666666667140, -2.886751345948130876 ) ) ;
#20089 = CARTESIAN_POINT ( 'NONE',  ( 4.458734124999998549, -42.97916666530107221, -2.574251347313721627 ) ) ;
#20090 = ORIENTED_EDGE ( 'NONE', *, *, #56503, .F. ) ;
#20091 = CARTESIAN_POINT ( 'NONE',  ( 5.000000000000000888, -143.0625000027312126, -2.071067811865475505 ) ) ;
#20092 = CARTESIAN_POINT ( 'NONE',  ( -4.458734124999999437, 12.60416666803225993, -2.574251347313719407 ) ) ;
#20093 = CARTESIAN_POINT ( 'NONE',  ( 2.499999999999998668, 3.791666669397852019, -4.330127018922193649 ) ) ;
#20094 = ORIENTED_EDGE ( 'NONE', *, *, #19636, .T. ) ;
#20095 = CARTESIAN_POINT ( 'NONE',  ( -3.152548672688508926E-16, -89.81249999863439371, -5.148502694627439702 ) ) ;
#20096 = CARTESIAN_POINT ( 'NONE',  ( -59.29741812935640155, -151.6250000013656063, -2.196230717870135685 ) ) ;
#20097 = CARTESIAN_POINT ( 'NONE',  ( -5.000000000000000888, -165.5625000000000568, -2.071067811865475949 ) ) ;
#20098 = CARTESIAN_POINT ( 'NONE',  ( -6.972266317189433020E-16, -39.25000000000000000, -5.000000000000000000 ) ) ;
#20099 = CARTESIAN_POINT ( 'NONE',  ( -2.500000000000000444, 23.83333333333333215, -4.330127018922193649 ) ) ;
#20100 = CARTESIAN_POINT ( 'NONE',  ( -2.229367062500000163, -67.47916666530106511, -3.861377020970580443 ) ) ;
#20101 = CARTESIAN_POINT ( 'NONE',  ( -58.24261429053147765, -146.2500000000000284, -3.805975901505573855 ) ) ;
#20102 = CARTESIAN_POINT ( 'NONE',  ( -3.152548672688508926E-16, 19.43750000136559208, -5.148502694627439702 ) ) ;
#20103 = AXIS2_PLACEMENT_3D ( 'NONE', #43981, #14717, #8956 ) ;
#20104 = CARTESIAN_POINT ( 'NONE',  ( -5.000000000000000000, 18.00000000000000000, 0.000000000000000000 ) ) ;
#20105 = ADVANCED_FACE ( 'NONE', ( #383, #63120 ), #19031, .F. ) ;
#20106 = EDGE_CURVE ( 'NONE', #27694, #30611, #54833, .T. ) ;
#20107 = CARTESIAN_POINT ( 'NONE',  ( -2.229367062500000163, -50.72916666530107221, -3.861377020970580443 ) ) ;
#20108 = CARTESIAN_POINT ( 'NONE',  ( 1.060575238724906964E-15, -10.62499999726881583, 5.773502691896257311 ) ) ;
#20109 = CARTESIAN_POINT ( 'NONE',  ( -1.339745962155613812, 4.794658198738519950, -5.000000000000000000 ) ) ;
#20110 = CARTESIAN_POINT ( 'NONE',  ( 7.500000000000000000, -2.571118828324946648, -0.3627527587569098766 ) ) ;
#20111 = CARTESIAN_POINT ( 'NONE',  ( 4.458734124999998549, -89.97916666530105090, -2.574251347313721627 ) ) ;
#20112 = ADVANCED_FACE ( 'NONE', ( #11920 ), #30590, .T. ) ;
#20113 = CARTESIAN_POINT ( 'NONE',  ( 1.975475456537005874E-15, 11.37500000273118239, 5.000000000000000000 ) ) ;
#20114 = CARTESIAN_POINT ( 'NONE',  ( -3.152548672688508926E-16, -15.81249999863440436, -5.148502694627439702 ) ) ;
#20115 =( BOUNDED_CURVE ( )  B_SPLINE_CURVE ( 2, ( #22978, #38079, #8184, #2728, #37448, #22347, #51618, #17825, #23290 ),
 .UNSPECIFIED., .F., .F. ) 
 B_SPLINE_CURVE_WITH_KNOTS ( ( 3, 2, 2, 2, 3 ),
 ( 0.8187499999999999778, 0.8194444444444444198, 0.8208333333333333037, 0.8222222222222221877, 0.8229166666666666297 ),
 .UNSPECIFIED. ) 
 CURVE ( )  GEOMETRIC_REPRESENTATION_ITEM ( )  RATIONAL_B_SPLINE_CURVE ( ( 0.9330127018922194093, 0.9330127018922194093, 1.000000000000000000, 0.8660254037844387076, 1.000000000000000000, 0.8660254037844387076, 1.000000000000000000, 0.9330127018922194093, 0.9330127018922194093 ) ) 
 REPRESENTATION_ITEM ( '' )  );
#20117 = ORIENTED_EDGE ( 'NONE', *, *, #13898, .T. ) ;
#20116 = ADVANCED_FACE ( 'NONE', ( #41188 ), #36376, .T. ) ;
#20118 = CARTESIAN_POINT ( 'NONE',  ( 5.000000000000000000, -31.41666666666667140, -2.886751345948130876 ) ) ;
#20119 = CARTESIAN_POINT ( 'NONE',  ( 2.229367062500001939, -104.9791666653010651, 3.861377020970579999 ) ) ;
#20120 = CARTESIAN_POINT ( 'NONE',  ( -5.000000000000000888, -162.6875000027311557, -2.071067811865475949 ) ) ;
#20121 = CARTESIAN_POINT ( 'NONE',  ( -2.229367062499996610, -96.39583333196773651, 3.861377020970582219 ) ) ;
#20122 = CARTESIAN_POINT ( 'NONE',  ( -2.499999999999996447, -7.833333333333331261, 4.330127018922195425 ) ) ;
#20124 = EDGE_CURVE ( 'NONE', #48949, #14934, #51905, .T. ) ;
#20123 = CARTESIAN_POINT ( 'NONE',  ( -2.500000000000000444, -56.04166666393548013, -4.330127018922193649 ) ) ;
#20125 = DIRECTION ( 'NONE',  ( -0.000000000000000000, 1.000000000000000000, -0.000000000000000000 ) ) ;
#20126 = EDGE_CURVE ( 'NONE', #5147, #49482, #58835, .T. ) ;
#20127 = CARTESIAN_POINT ( 'NONE',  ( -50.55543936806279248, -154.3125000013656347, 0.3552334253322060320 ) ) ;
#20128 = CARTESIAN_POINT ( 'NONE',  ( -58.39396692619412477, -148.4375000013656063, 2.891590998281057701 ) ) ;
#20129 = CARTESIAN_POINT ( 'NONE',  ( 2.229367062499998831, -17.64583333196773651, -3.861377020970580887 ) ) ;
#20130 = CARTESIAN_POINT ( 'NONE',  ( 4.458734124999999437, 4.937500001365595637, -5.460374474430324690E-16 ) ) ;
#20131 = CARTESIAN_POINT ( 'NONE',  ( -4.458734124999999437, -62.64583333196774362, -2.574251347313719407 ) ) ;
#20132 = CARTESIAN_POINT ( 'NONE',  ( -5.000000000000000888, -141.6875000027311842, -2.071067811865475949 ) ) ;
#20133 = CARTESIAN_POINT ( 'NONE',  ( 4.458734125000000326, -18.89583333196774362, 2.574251347313718519 ) ) ;
#20134 = CARTESIAN_POINT ( 'NONE',  ( -5.000000000000000888, -154.4375000000000284, 2.071067811865474617 ) ) ;
#20135 = CARTESIAN_POINT ( 'NONE',  ( -4.999999999999999112, -6.916666666666667851, 2.886751345948131764 ) ) ;
#20136 = EDGE_CURVE ( 'NONE', #32525, #39907, #12448, .T. ) ;
#20137 = CARTESIAN_POINT ( 'NONE',  ( -8.190561711645485556E-16, -157.6875000013655779, 4.458734124999999437 ) ) ;
#20138 = ORIENTED_EDGE ( 'NONE', *, *, #17387, .T. ) ;
#20139 = CARTESIAN_POINT ( 'NONE',  ( 4.458734125000000326, -44.14583333196774362, 2.574251347313718519 ) ) ;
#20140 = CARTESIAN_POINT ( 'NONE',  ( -1.336351044127974539E-14, 21.37500000273118417, 5.000000000000000000 ) ) ;
#20141 = EDGE_CURVE ( 'NONE', #21367, #31465, #30913, .T. ) ;
#20142 = CARTESIAN_POINT ( 'NONE',  ( -4.999999999999998224, -11.91666666666666607, 2.886751345948131764 ) ) ;
#20143 = EDGE_CURVE ( 'NONE', #5292, #7216, #21268, .T. ) ;
#20144 = CARTESIAN_POINT ( 'NONE',  ( 2.500000000000002220, 27.33333333333333215, 4.330127018922192761 ) ) ;
#20145 = CARTESIAN_POINT ( 'NONE',  ( -4.458734124999999437, -93.39583333196773651, -2.574251347313719407 ) ) ;
#20146 = CARTESIAN_POINT ( 'NONE',  ( 4.458734124999999437, 17.93750000136559208, -5.460374474430324690E-16 ) ) ;
#20147 = CARTESIAN_POINT ( 'NONE',  ( 4.458734125000001214, 9.104166668032261711, 2.574251347313718519 ) ) ;
#20148 = CARTESIAN_POINT ( 'NONE',  ( 1.975475456537005874E-15, -81.74999999999998579, 5.000000000000000000 ) ) ;
#20149 = DIRECTION ( 'NONE',  ( -0.000000000000000000, 1.000000000000000000, -0.000000000000000000 ) ) ;
#20150 = CARTESIAN_POINT ( 'NONE',  ( -3.152548672688508926E-16, 23.18750000136559208, -5.148502694627439702 ) ) ;
#20151 = CARTESIAN_POINT ( 'NONE',  ( 2.499999999999998668, -73.33333333333332860, -4.330127018922193649 ) ) ;
#20152 = CARTESIAN_POINT ( 'NONE',  ( 5.000000000000000000, 6.625000002731185944, -6.123233995736766282E-16 ) ) ;
#20153 = ORIENTED_EDGE ( 'NONE', *, *, #43546, .F. ) ;
#20154 = CARTESIAN_POINT ( 'NONE',  ( 0.000000000000000000, -170.0000000000000000, 5.000000000000000000 ) ) ;
#20155 = ORIENTED_EDGE ( 'NONE', *, *, #58619, .T. ) ;
#20156 = CARTESIAN_POINT ( 'NONE',  ( -6.972266317189433020E-16, -104.2500000000000000, -5.000000000000000000 ) ) ;
#20157 = CARTESIAN_POINT ( 'NONE',  ( 9.457646018065525792E-16, -36.06249999863441502, 5.148502694627439702 ) ) ;
#20158 = AXIS2_PLACEMENT_3D ( 'NONE', #2585, #56932, #1965 ) ;
#20159 = CARTESIAN_POINT ( 'NONE',  ( -2.499999999999996447, -40.70833333060214443, 4.330127018922195425 ) ) ;
#20160 = EDGE_LOOP ( 'NONE', ( #58127, #14401, #15186, #4147 ) ) ;
#20161 = CARTESIAN_POINT ( 'NONE',  ( -52.80376928212989185, -146.1250000013656063, -4.297418129356379346 ) ) ;
#20162 = CARTESIAN_POINT ( 'NONE',  ( 9.457646018065525792E-16, -12.06249999863440081, 5.148502694627439702 ) ) ;
#20164 = ORIENTED_EDGE ( 'NONE', *, *, #1565, .T. ) ;
#20163 = CARTESIAN_POINT ( 'NONE',  ( -4.458734124999999437, -13.56249999863440259, 0.000000000000000000 ) ) ;
#20165 = CARTESIAN_POINT ( 'NONE',  ( -2.500000000000000444, -80.16666666666665719, -4.330127018922193649 ) ) ;
#20166 = CARTESIAN_POINT ( 'NONE',  ( -2.229367062499996610, -64.39583333196773651, 3.861377020970582219 ) ) ;
#20167 =( BOUNDED_CURVE ( )  B_SPLINE_CURVE ( 2, ( #50586, #20691, #11969, #11020, #40296, #17122, #12301, #16172, #35797 ),
 .UNSPECIFIED., .F., .F. ) 
 B_SPLINE_CURVE_WITH_KNOTS ( ( 3, 2, 2, 2, 3 ),
 ( 0.9270833333333333703, 0.9277777777777778123, 0.9291666666666666963, 0.9305555555555555802, 0.9312500000000000222 ),
 .UNSPECIFIED. ) 
 CURVE ( )  GEOMETRIC_REPRESENTATION_ITEM ( )  RATIONAL_B_SPLINE_CURVE ( ( 0.9330127018922194093, 0.9330127018922194093, 1.000000000000000000, 0.8660254037844387076, 1.000000000000000000, 0.8660254037844387076, 1.000000000000000000, 0.9330127018922194093, 0.9330127018922194093 ) ) 
 REPRESENTATION_ITEM ( '' )  );
#20168 = CARTESIAN_POINT ( 'NONE',  ( -4.999999999999999112, -87.79166666393550145, 2.886751345948131764 ) ) ;
#20170 = ORIENTED_EDGE ( 'NONE', *, *, #58688, .F. ) ;
#20169 = CARTESIAN_POINT ( 'NONE',  ( 2.500000000000002220, 3.458333336064517205, 4.330127018922192761 ) ) ;
#20171 = CARTESIAN_POINT ( 'NONE',  ( -58.80597590150559739, -140.0000000000000284, 3.242614290531460330 ) ) ;
#20172 = CARTESIAN_POINT ( 'NONE',  ( 4.458734124999999437, -29.06249999863440436, -5.460374474430324690E-16 ) ) ;
#20173 = CARTESIAN_POINT ( 'NONE',  ( -5.000000000000000000, -83.99999999999998579, 0.000000000000000000 ) ) ;
#20174 = VERTEX_POINT ( 'NONE', #60516 ) ;
#20175 = APPLICATION_PROTOCOL_DEFINITION ( 'draft international standard', 'automotive_design', 1998, #48689 ) ;
#20176 = CARTESIAN_POINT ( 'NONE',  ( -4.458734125000000326, -163.2500000013655495, -1.846868145590735644 ) ) ;
#20177 = CARTESIAN_POINT ( 'NONE',  ( -4.458734124999998549, -110.4791666653010793, 2.574251347313722516 ) ) ;
#20178 = CARTESIAN_POINT ( 'NONE',  ( 2.500000000000002220, 20.33333333333333215, 4.330127018922192761 ) ) ;
#20179 = ORIENTED_EDGE ( 'NONE', *, *, #47645, .T. ) ;
#20180 = CARTESIAN_POINT ( 'NONE',  ( -58.39396692619412477, -144.6875000013656063, 2.891590998281057701 ) ) ;
#20181 = CARTESIAN_POINT ( 'NONE',  ( 4.458734124999998549, -75.97916666530106511, -2.574251347313721627 ) ) ;
#20182 = CARTESIAN_POINT ( 'NONE',  ( -52.53715891517739323, -135.5625000027311842, -4.819101127000233298 ) ) ;
#20183 = CARTESIAN_POINT ( 'NONE',  ( -4.458734124999999437, -46.39583333196774362, -2.574251347313719407 ) ) ;
#20184 = CARTESIAN_POINT ( 'NONE',  ( -1.846868145590737420, -148.0000000013656063, 4.458734124999997661 ) ) ;
#20185 = CARTESIAN_POINT ( 'NONE',  ( -7.500000000000000000, -3.882691789160215290, -7.781695678273567118 ) ) ;
#20186 = CARTESIAN_POINT ( 'NONE',  ( -2.229367062499996610, -48.14583333196772941, 3.861377020970582219 ) ) ;
#20187 = DIRECTION ( 'NONE',  ( 0.000000000000000000, 0.000000000000000000, 1.000000000000000000 ) ) ;
#20188 = CARTESIAN_POINT ( 'NONE',  ( 2.229367062500001939, -14.97916666530107399, 3.861377020970579999 ) ) ;
#20189 = CARTESIAN_POINT ( 'NONE',  ( 5.000000000000000000, -100.4166666666666572, -2.886751345948129988 ) ) ;
#20190 = CARTESIAN_POINT ( 'NONE',  ( -4.458734124999999437, -142.1875000013656063, -5.460374474430324690E-16 ) ) ;
#20191 = CARTESIAN_POINT ( 'NONE',  ( -4.458734124999998549, -34.47916666530107221, 2.574251347313722516 ) ) ;
#20192 = CARTESIAN_POINT ( 'NONE',  ( -5.000000000000000000, 8.041666669397852019, -2.886751345948128211 ) ) ;
#20193 = CARTESIAN_POINT ( 'NONE',  ( -52.10840900171896806, -132.1875000013656063, 3.393966926194110556 ) ) ;
#20194 = CARTESIAN_POINT ( 'NONE',  ( -2.229367062499996610, -74.39583333196773651, 3.861377020970582219 ) ) ;
#20195 = CARTESIAN_POINT ( 'NONE',  ( -53.33387254593723270, -145.9375000027312410, 5.149110718188528502 ) ) ;
#20196 = FACE_OUTER_BOUND ( 'NONE', #29147, .T. ) ;
#20197 = CYLINDRICAL_SURFACE ( 'NONE', #28467, 5.000000000000000000 ) ;
#20198 = CARTESIAN_POINT ( 'NONE',  ( 9.457646018065525792E-16, 1.687500001365593194, 5.148502694627439702 ) ) ;
#20199 = ORIENTED_EDGE ( 'NONE', *, *, #17013, .T. ) ;
#20200 = VECTOR ( 'NONE', #13888, 1000.000000000000000 ) ;
#20201 = CARTESIAN_POINT ( 'NONE',  ( 2.499999999999998668, 16.79166666939785202, -4.330127018922193649 ) ) ;
#20203 = CARTESIAN_POINT ( 'NONE',  ( -4.458734124999999437, -37.39583333196773651, -2.574251347313719407 ) ) ;
#20202 = CARTESIAN_POINT ( 'NONE',  ( -4.999999999999999112, -93.91666666666667140, 2.886751345948131764 ) ) ;
#20204 = CARTESIAN_POINT ( 'NONE',  ( -2.500000000000000444, -36.16666666666666430, -4.330127018922193649 ) ) ;
#20205 = CARTESIAN_POINT ( 'NONE',  ( 4.458734125000001214, -79.14583333196772230, 2.574251347313718519 ) ) ;
#20206 = CONICAL_SURFACE ( 'NONE', #31488, 7.500000000000001776, 0.8594454914424796144 ) ;
#20207 = CARTESIAN_POINT ( 'NONE',  ( -3.152548672688508926E-16, 18.18750000136559564, -5.148502694627439702 ) ) ;
#20208 = CARTESIAN_POINT ( 'NONE',  ( 1.975475456537005874E-15, -77.62499999726881583, 5.000000000000000000 ) ) ;
#20209 = AXIS2_PLACEMENT_3D ( 'NONE', #18846, #23997, #43600 ) ;
#20210 = CARTESIAN_POINT ( 'NONE',  ( -50.55543936806279248, -137.0625000013656063, 0.3552334253322060320 ) ) ;
#20211 = VECTOR ( 'NONE', #4463, 1000.000000000000000 ) ;
#20212 = CARTESIAN_POINT ( 'NONE',  ( 9.457646018065525792E-16, -4.062499998634408804, 5.148502694627439702 ) ) ;
#20213 = CARTESIAN_POINT ( 'NONE',  ( 2.229367062500001939, 20.77083333469892779, 3.861377020970579999 ) ) ;
#20214 = CARTESIAN_POINT ( 'NONE',  ( -4.458734124999999437, -42.64583333196773651, -2.574251347313719407 ) ) ;
#20215 = LINE ( 'NONE', #10873, #37701 ) ;
#20216 = CARTESIAN_POINT ( 'NONE',  ( -4.458734124999999437, -2.312499998634407028, 0.000000000000000000 ) ) ;
#20217 = ADVANCED_FACE ( 'NONE', ( #31226 ), #46026, .F. ) ;
#20218 = CARTESIAN_POINT ( 'NONE',  ( -2.229367062500000163, -29.72916666530107221, -3.861377020970580443 ) ) ;
#20219 = CARTESIAN_POINT ( 'NONE',  ( -57.89159099828107458, -133.9375000013656063, -3.393966926194107447 ) ) ;
#20220 = CARTESIAN_POINT ( 'NONE',  ( -2.229367062499996610, -74.14583333196773651, 3.861377020970582219 ) ) ;
#20221 = CARTESIAN_POINT ( 'NONE',  ( 2.500000000000002220, -107.5416666639354730, 4.330127018922192761 ) ) ;
#20222 = CARTESIAN_POINT ( 'NONE',  ( 4.458734124999999437, 24.18750000136559564, -5.460374474430324690E-16 ) ) ;
#20223 = EDGE_CURVE ( 'NONE', #23230, #8786, #19382, .T. ) ;
#20224 = CARTESIAN_POINT ( 'NONE',  ( -1.339745962155585168, 9.794658198738519062, -5.000000000000015987 ) ) ;
#20225 = LINE ( 'NONE', #5109, #35771 ) ;
#20226 = CARTESIAN_POINT ( 'NONE',  ( 4.458734125000000326, -76.14583333196773651, 2.574251347313718519 ) ) ;
#20227 = CARTESIAN_POINT ( 'NONE',  ( 5.000000000000000000, -57.49999999999999289, -6.123233995736766282E-16 ) ) ;
#20228 = CARTESIAN_POINT ( 'NONE',  ( -6.972266317189433020E-16, -32.12499999726880873, -5.000000000000000000 ) ) ;
#20229 = CARTESIAN_POINT ( 'NONE',  ( 5.000000000000000888, 25.54166666939784847, 2.886751345948126879 ) ) ;
#20230 = EDGE_LOOP ( 'NONE', ( #20587, #54388, #41048, #2548 ) ) ;
#20231 = DIRECTION ( 'NONE',  ( -0.000000000000000000, 1.000000000000000000, -0.000000000000000000 ) ) ;
#20232 = DIRECTION ( 'NONE',  ( -0.000000000000000000, 1.000000000000000000, -0.000000000000000000 ) ) ;
#20233 = CARTESIAN_POINT ( 'NONE',  ( 1.060575238724906964E-15, -15.75000000000000178, 5.773502691896257311 ) ) ;
#20234 = CARTESIAN_POINT ( 'NONE',  ( -2.229367062500000163, -21.47916666530107221, -3.861377020970580443 ) ) ;
#20235 = CARTESIAN_POINT ( 'NONE',  ( -4.458734124999997661, -83.22916666530106511, 2.574251347313722516 ) ) ;
#20236 = CARTESIAN_POINT ( 'NONE',  ( 5.000000000000000888, -23.45833333060214443, 2.886751345948126879 ) ) ;
#20238 = ORIENTED_EDGE ( 'NONE', *, *, #26111, .T. ) ;
#20237 = CARTESIAN_POINT ( 'NONE',  ( 4.458734124999998549, -51.72916666530107221, -2.574251347313721627 ) ) ;
#20239 = CARTESIAN_POINT ( 'NONE',  ( 5.000000000000000000, 5.500000000000001776, -6.123233995736766282E-16 ) ) ;
#20240 = CARTESIAN_POINT ( 'NONE',  ( 5.000000000000000888, -74.45833333060214443, 2.886751345948126879 ) ) ;
#20242 = ORIENTED_EDGE ( 'NONE', *, *, #21391, .T. ) ;
#20241 = CARTESIAN_POINT ( 'NONE',  ( -4.458734124999998549, 3.520833334698929118, 2.574251347313722516 ) ) ;
#20243 = CARTESIAN_POINT ( 'NONE',  ( -51.60603307380591787, -150.9375000013656063, -2.891590998281053704 ) ) ;
#20244 = CARTESIAN_POINT ( 'NONE',  ( -4.999999999999999112, -68.91666666666667140, 2.886751345948131764 ) ) ;
#20245 = CARTESIAN_POINT ( 'NONE',  ( 1.846868145590736310, -151.8750000013655779, 4.458734124999999437 ) ) ;
#20246 = CARTESIAN_POINT ( 'NONE',  ( -2.229367062500000163, -46.72916666530106511, -3.861377020970580443 ) ) ;
#20247 = CARTESIAN_POINT ( 'NONE',  ( 0.000000000000000000, -120.0000000000000000, 5.000000000000000000 ) ) ;
#20248 = CARTESIAN_POINT ( 'NONE',  ( 2.071067811865476394, -162.1875000000000000, 5.000000000000000000 ) ) ;
#20249 = FACE_OUTER_BOUND ( 'NONE', #25996, .T. ) ;
#20250 = CARTESIAN_POINT ( 'NONE',  ( -59.59170313451811296, -126.7500000013655921, 1.485763867205729394 ) ) ;
#20251 = AXIS2_PLACEMENT_3D ( 'NONE', #22118, #11505, #16013 ) ;
#20252 = CARTESIAN_POINT ( 'NONE',  ( -3.152548672688508926E-16, -10.81249999863440792, -5.148502694627439702 ) ) ;
#20253 = VECTOR ( 'NONE', #4222, 1000.000000000000000 ) ;
#20254 = CARTESIAN_POINT ( 'NONE',  ( 4.458734124999998549, -46.97916666530106511, -2.574251347313721627 ) ) ;
#20255 =( BOUNDED_CURVE ( )  B_SPLINE_CURVE ( 2, ( #20428, #4665, #48414, #58393, #5314, #43891, #33942, #24610, #63540 ),
 .UNSPECIFIED., .F., .F. ) 
 B_SPLINE_CURVE_WITH_KNOTS ( ( 3, 2, 2, 2, 3 ),
 ( 0.02500000000000002220, 0.02916666666666669488, 0.03333333333333336757, 0.03750000000000003331, 0.04166666666666670599 ),
 .UNSPECIFIED. ) 
 CURVE ( )  GEOMETRIC_REPRESENTATION_ITEM ( )  RATIONAL_B_SPLINE_CURVE ( ( 0.9999999999999996669, 0.9238795325112870716, 1.000000000000000000, 0.9238795325112867385, 1.000000000000000000, 0.9238795325112867385, 1.000000000000000000, 0.9238795325112859613, 1.000000000000000666 ) ) 
 REPRESENTATION_ITEM ( '' )  );
#20256 = CARTESIAN_POINT ( 'NONE',  ( -50.18089887299976937, -136.8125000027311842, 2.462841084822337656 ) ) ;
#20257 = CARTESIAN_POINT ( 'NONE',  ( 2.730187237215162345E-16, -145.1875000013656063, -4.458734124999999437 ) ) ;
#20258 = VECTOR ( 'NONE', #42585, 1000.000000000000000 ) ;
#20259 = CARTESIAN_POINT ( 'NONE',  ( -4.458734124999999437, -87.56249999863439371, 0.000000000000000000 ) ) ;
#20260 = CARTESIAN_POINT ( 'NONE',  ( -6.972266317189433020E-16, -3.250000000000001332, -5.000000000000000000 ) ) ;
#20261 = ORIENTED_EDGE ( 'NONE', *, *, #59361, .F. ) ;
#20262 = CARTESIAN_POINT ( 'NONE',  ( -4.458734124999999437, 28.43750000136559208, 0.000000000000000000 ) ) ;
#20263 = CARTESIAN_POINT ( 'NONE',  ( -58.24261429053147765, -150.3750000027312126, -3.805975901505573855 ) ) ;
#20264 = CARTESIAN_POINT ( 'NONE',  ( -2.498395430326213474E-14, 21.24999999999999289, 5.000000000000000000 ) ) ;
#20265 = ORIENTED_EDGE ( 'NONE', *, *, #1264, .T. ) ;
#20266 = CARTESIAN_POINT ( 'NONE',  ( -2.229367062500000163, 5.520833334698927786, -3.861377020970580443 ) ) ;
#20267 = CARTESIAN_POINT ( 'NONE',  ( 5.000000000000000888, -106.5833333333333286, 2.886751345948126879 ) ) ;
#20268 = CARTESIAN_POINT ( 'NONE',  ( 2.229367062499998831, -14.89583333196773474, -3.861377020970580887 ) ) ;
#20269 = CARTESIAN_POINT ( 'NONE',  ( -6.972266317189433020E-16, 8.750000000000000000, -5.000000000000000000 ) ) ;
#20270 = CARTESIAN_POINT ( 'NONE',  ( -4.458734124999999437, -5.312499998634402587, 0.000000000000000000 ) ) ;
#20271 = DIRECTION ( 'NONE',  ( 0.000000000000000000, 0.000000000000000000, 1.000000000000000000 ) ) ;
#20272 = CARTESIAN_POINT ( 'NONE',  ( -1.846868145590737420, -149.7500000013656063, 4.458734124999997661 ) ) ;
#20273 = CARTESIAN_POINT ( 'NONE',  ( 2.229367062499998831, 20.10416666803225993, -3.861377020970580887 ) ) ;
#20274 = ORIENTED_EDGE ( 'NONE', *, *, #24500, .F. ) ;
#20275 = CARTESIAN_POINT ( 'NONE',  ( -4.458734124999997661, -97.22916666530105090, 2.574251347313722516 ) ) ;
#20276 = DIRECTION ( 'NONE',  ( -0.000000000000000000, 1.000000000000000000, -0.000000000000000000 ) ) ;
#20277 = CARTESIAN_POINT ( 'NONE',  ( 5.000000000000000000, -57.29166666393548013, -2.886751345948130876 ) ) ;
#20278 = CARTESIAN_POINT ( 'NONE',  ( -2.229367062500000163, -12.47916666530107044, -3.861377020970580443 ) ) ;
#20279 = CARTESIAN_POINT ( 'NONE',  ( -51.75738570946856498, -143.7500000000000284, 3.805975901505576964 ) ) ;
#20280 = CARTESIAN_POINT ( 'NONE',  ( -1.339745962155610925, -12.79465819873851906, 5.000000000000000000 ) ) ;
#20281 = CARTESIAN_POINT ( 'NONE',  ( -59.44456063193725015, -149.5625000013656063, -0.3552334253322034230 ) ) ;
#20282 = CARTESIAN_POINT ( 'NONE',  ( 5.000000000000000000, -43.29166666393548724, -2.886751345948129988 ) ) ;
#20283 = CARTESIAN_POINT ( 'NONE',  ( -49.85088928181150436, -148.5625000000000000, -1.666127454062680480 ) ) ;
#20284 = CARTESIAN_POINT ( 'NONE',  ( -2.229367062499996610, 11.85416666803225993, 3.861377020970582219 ) ) ;
#20285 = CARTESIAN_POINT ( 'NONE',  ( 5.000000000000000888, -35.58333333333332860, 2.886751345948126879 ) ) ;
#20286 = CARTESIAN_POINT ( 'NONE',  ( -6.972266317189433020E-16, -48.12499999726880873, -5.000000000000000000 ) ) ;
#20287 = CARTESIAN_POINT ( 'NONE',  ( 4.458734124999998549, 15.27083333469893134, -2.574251347313721627 ) ) ;
#20288 = CARTESIAN_POINT ( 'NONE',  ( 4.458734124999999437, -59.81249999863440081, -5.460374474430324690E-16 ) ) ;
#20289 = ORIENTED_EDGE ( 'NONE', *, *, #8713, .T. ) ;
#20290 = CARTESIAN_POINT ( 'NONE',  ( -4.458734124999997661, -15.47916666530107399, 2.574251347313722516 ) ) ;
#20291 = CARTESIAN_POINT ( 'NONE',  ( 5.000000000000000000, 4.500000000000000888, -6.123233995736766282E-16 ) ) ;
#20292 = CARTESIAN_POINT ( 'NONE',  ( 2.730187237215162345E-16, -165.1875000013655779, -4.458734124999999437 ) ) ;
#20293 = CARTESIAN_POINT ( 'NONE',  ( -6.972266317189433020E-16, -63.12499999726880162, -5.000000000000000000 ) ) ;
#20294 = CARTESIAN_POINT ( 'NONE',  ( -4.458734124999999437, -55.31249999863440081, 0.000000000000000000 ) ) ;
#20295 = CARTESIAN_POINT ( 'NONE',  ( 1.060575238724906964E-15, -88.62499999726880162, 5.773502691896257311 ) ) ;
#20296 = AXIS2_PLACEMENT_3D ( 'NONE', #32093, #51729, #7669 ) ;
#20297 = CARTESIAN_POINT ( 'NONE',  ( -2.229367062499996610, -34.14583333196772941, 3.861377020970582219 ) ) ;
#20298 = VECTOR ( 'NONE', #9701, 1000.000000000000000 ) ;
#20299 = CARTESIAN_POINT ( 'NONE',  ( -4.999999999999998224, 20.20833333606451987, 2.886751345948131764 ) ) ;
#20300 = CARTESIAN_POINT ( 'NONE',  ( -1.230605004983934782E-13, -26.62499999726881583, 5.000000000000000000 ) ) ;
#20301 = CARTESIAN_POINT ( 'NONE',  ( -51.19402409849444524, -151.6250000027312126, -3.242614290531456334 ) ) ;
#20302 = CARTESIAN_POINT ( 'NONE',  ( -1.846868145590737420, -153.0000000013656063, 4.458734124999997661 ) ) ;
#20303 =( BOUNDED_CURVE ( )  B_SPLINE_CURVE ( 2, ( #24018, #42370, #57814, #62328, #28836, #62649, #57508, #8293, #13112 ),
 .UNSPECIFIED., .F., .F. ) 
 B_SPLINE_CURVE_WITH_KNOTS ( ( 3, 2, 2, 2, 3 ),
 ( 0.1625000000000000056, 0.1630952380952380987, 0.1642857142857142849, 0.1654761904761904712, 0.1660714285714285643 ),
 .UNSPECIFIED. ) 
 CURVE ( )  GEOMETRIC_REPRESENTATION_ITEM ( )  RATIONAL_B_SPLINE_CURVE ( ( 0.9330127018922194093, 0.9330127018922194093, 1.000000000000000000, 0.8660254037844387076, 1.000000000000000000, 0.8660254037844387076, 1.000000000000000000, 0.9330127018922194093, 0.9330127018922194093 ) ) 
 REPRESENTATION_ITEM ( '' )  );
#20304 = CARTESIAN_POINT ( 'NONE',  ( -2.500000000000000444, -43.16666666666665719, -4.330127018922193649 ) ) ;
#20305 = CARTESIAN_POINT ( 'NONE',  ( -5.000000000000000000, -19.95833333060214798, -2.886751345948128211 ) ) ;
#20306 = CYLINDRICAL_SURFACE ( 'NONE', #24273, 5.000000000000000000 ) ;
#20307 = EDGE_LOOP ( 'NONE', ( #59006, #21941, #52073, #33861 ) ) ;
#20308 = CARTESIAN_POINT ( 'NONE',  ( -2.229367062499996610, -101.1458333319677365, 3.861377020970582219 ) ) ;
#20309 = CARTESIAN_POINT ( 'NONE',  ( 4.458734124999998549, 4.020833334698926009, -2.574251347313721627 ) ) ;
#20310 = CARTESIAN_POINT ( 'NONE',  ( -6.972266317189433020E-16, -59.25000000000000000, -5.000000000000000000 ) ) ;
#20311 = CARTESIAN_POINT ( 'NONE',  ( 5.000000000000000000, -4.499999999999997335, -6.123233995736766282E-16 ) ) ;
#20312 = CARTESIAN_POINT ( 'NONE',  ( -4.458734124999997661, -66.22916666530106511, 2.574251347313722516 ) ) ;
#20313 = CARTESIAN_POINT ( 'NONE',  ( 5.000000000000000888, -4.458333330602148870, 2.886751345948126879 ) ) ;
#20315 = EDGE_LOOP ( 'NONE', ( #14335, #21271, #26880, #31552 ) ) ;
#20314 = CARTESIAN_POINT ( 'NONE',  ( -4.458734124999999437, -35.31249999863440792, 0.000000000000000000 ) ) ;
#20316 = CARTESIAN_POINT ( 'NONE',  ( 1.975475456537005874E-15, -81.74999999999998579, 5.000000000000000000 ) ) ;
#20317 = DIRECTION ( 'NONE',  ( -0.000000000000000000, 1.000000000000000000, -0.000000000000000000 ) ) ;
#20318 = ORIENTED_EDGE ( 'NONE', *, *, #36967, .F. ) ;
#20319 = CARTESIAN_POINT ( 'NONE',  ( 1.975475456537005874E-15, -48.62499999726880162, 5.000000000000000000 ) ) ;
#20320 = CARTESIAN_POINT ( 'NONE',  ( -4.999999999999999112, -49.91666666666666430, 2.886751345948131764 ) ) ;
#20322 = CARTESIAN_POINT ( 'NONE',  ( 4.458734125000001214, -23.14583333196773651, 2.574251347313718519 ) ) ;
#20321 = CARTESIAN_POINT ( 'NONE',  ( 4.330127018922258486, 30.00000000000000000, 7.499999999999910294 ) ) ;
#20323 = CARTESIAN_POINT ( 'NONE',  ( 1.339745962155612702, -32.16965819600733312, -5.000000000000000000 ) ) ;
#20324 = CARTESIAN_POINT ( 'NONE',  ( 9.457646018065525792E-16, -74.06249999863440792, 5.148502694627439702 ) ) ;
#20325 = CARTESIAN_POINT ( 'NONE',  ( -4.458734124999999437, -142.1875000013656063, -5.460374474430324690E-16 ) ) ;
#20327 = EDGE_CURVE ( 'NONE', #12526, #52748, #37326, .T. ) ;
#20326 = CARTESIAN_POINT ( 'NONE',  ( -4.458734124999999437, -83.31249999863439371, 0.000000000000000000 ) ) ;
#20328 = CARTESIAN_POINT ( 'NONE',  ( -58.39396692619412477, -138.6875000013656347, 2.891590998281057701 ) ) ;
#20329 = CARTESIAN_POINT ( 'NONE',  ( 2.229367062499998831, -30.89583333196773651, -3.861377020970580887 ) ) ;
#20330 = CARTESIAN_POINT ( 'NONE',  ( -3.535250795749689387E-16, -73.12499999726881583, -5.773502691896257311 ) ) ;
#20331 = ORIENTED_EDGE ( 'NONE', *, *, #23213, .T. ) ;
#20332 = DIRECTION ( 'NONE',  ( -0.5000000000000009992, 0.000000000000000000, -0.8660254037844380415 ) ) ;
#20333 = ORIENTED_EDGE ( 'NONE', *, *, #11412, .T. ) ;
#20334 = CARTESIAN_POINT ( 'NONE',  ( 4.458734125000001214, -73.14583333196773651, 2.574251347313718519 ) ) ;
#20335 = CARTESIAN_POINT ( 'NONE',  ( -50.96713099277813797, -135.0000000000000568, -1.923792341520001115 ) ) ;
#20336 = SHAPE_REPRESENTATION_RELATIONSHIP ( 'NONE' , 'NONE' ,  #21293, #24770 ) ;
#20337 = VERTEX_POINT ( 'NONE', #42773 ) ;
#20338 = DIRECTION ( 'NONE',  ( 0.000000000000000000, 1.000000000000000000, 0.000000000000000000 ) ) ;
#20339 = VECTOR ( 'NONE', #14312, 1000.000000000000000 ) ;
#20340 = CARTESIAN_POINT ( 'NONE',  ( -7.922281120364393914, 4.573931137438271399, -8.047472243342930653 ) ) ;
#20341 = CARTESIAN_POINT ( 'NONE',  ( 4.458734125000001214, -57.14583333196773651, 2.574251347313718519 ) ) ;
#20342 = CARTESIAN_POINT ( 'NONE',  ( 2.229367062499998831, -3.895833331967739177, -3.861377020970580887 ) ) ;
#20343 = ORIENTED_EDGE ( 'NONE', *, *, #35745, .T. ) ;
#20344 = CARTESIAN_POINT ( 'NONE',  ( 2.071067811865517694, -141.8125000000000000, -4.999999999999958256 ) ) ;
#20345 = CYLINDRICAL_SURFACE ( 'NONE', #56209, 5.000000000000000000 ) ;
#20346 = CARTESIAN_POINT ( 'NONE',  ( 4.458734124999999437, 13.18750000136559208, -5.460374474430324690E-16 ) ) ;
#20347 = CARTESIAN_POINT ( 'NONE',  ( -50.55543936806279248, -142.0625000013656063, 0.3552334253322060320 ) ) ;
#20348 = CARTESIAN_POINT ( 'NONE',  ( -6.972266317189433020E-16, -27.12499999726881228, -5.000000000000000000 ) ) ;
#20349 = CARTESIAN_POINT ( 'NONE',  ( -4.458734124999999437, -162.9375000013655779, -5.460374474430324690E-16 ) ) ;
#20350 =( BOUNDED_CURVE ( )  B_SPLINE_CURVE ( 2, ( #11083, #40025, #5631, #54190, #10128, #50330, #59343, #44214, #29735 ),
 .UNSPECIFIED., .F., .F. ) 
 B_SPLINE_CURVE_WITH_KNOTS ( ( 3, 2, 2, 2, 3 ),
 ( 0.1160714285714285754, 0.1166666666666666685, 0.1178571428571428548, 0.1190476190476190410, 0.1196428571428571480 ),
 .UNSPECIFIED. ) 
 CURVE ( )  GEOMETRIC_REPRESENTATION_ITEM ( )  RATIONAL_B_SPLINE_CURVE ( ( 0.9330127018922194093, 0.9330127018922194093, 1.000000000000000000, 0.8660254037844387076, 1.000000000000000000, 0.8660254037844387076, 1.000000000000000000, 0.9330127018922185211, 0.9330127018922192983 ) ) 
 REPRESENTATION_ITEM ( '' )  );
#20351 = DIRECTION ( 'NONE',  ( -0.000000000000000000, 1.000000000000000000, -0.000000000000000000 ) ) ;
#20352 = ORIENTED_EDGE ( 'NONE', *, *, #58619, .F. ) ;
#20353 = CARTESIAN_POINT ( 'NONE',  ( 4.458734125000000326, -78.89583333196775072, 2.574251347313718519 ) ) ;
#20354 = CARTESIAN_POINT ( 'NONE',  ( 0.000000000000000000, -170.0000000000000000, 5.000000000000000000 ) ) ;
#20355 = CARTESIAN_POINT ( 'NONE',  ( -4.458734124999999437, 3.604166668032260379, -2.574251347313719407 ) ) ;
#20356 = CARTESIAN_POINT ( 'NONE',  ( 1.975475456537005874E-15, -71.75000000000000000, 5.000000000000000000 ) ) ;
#20357 = VECTOR ( 'NONE', #61806, 1000.000000000000000 ) ;
#20358 = CARTESIAN_POINT ( 'NONE',  ( -2.500000000000000444, -87.16666666666667140, -4.330127018922193649 ) ) ;
#20359 = CARTESIAN_POINT ( 'NONE',  ( -7.500000000000000888, 2.886751345948126435, -7.198902722707427593 ) ) ;
#20360 = CARTESIAN_POINT ( 'NONE',  ( -4.458734124999998549, -67.47916666530106511, 2.574251347313722516 ) ) ;
#20361 = CARTESIAN_POINT ( 'NONE',  ( 2.500000000000002220, -23.54166666393548368, 4.330127018922192761 ) ) ;
#20362 = CARTESIAN_POINT ( 'NONE',  ( 1.975475456537005874E-15, -14.74999999999999822, 5.000000000000000000 ) ) ;
#20363 = CARTESIAN_POINT ( 'NONE',  ( 9.457646018065525792E-16, 28.93750000136558853, 5.148502694627439702 ) ) ;
#20364 = CARTESIAN_POINT ( 'NONE',  ( -6.972266317189433020E-16, -38.12499999726880873, -5.000000000000000000 ) ) ;
#20365 = CARTESIAN_POINT ( 'NONE',  ( 1.339745962155615144, -43.58034179853029144, 4.999999999999999112 ) ) ;
#20366 = CARTESIAN_POINT ( 'NONE',  ( 2.229367062499998831, -46.64583333196774362, -3.861377020970580887 ) ) ;
#20367 = CARTESIAN_POINT ( 'NONE',  ( -4.458734124999999437, -33.64583333196772941, -2.574251347313719407 ) ) ;
#20368 = CARTESIAN_POINT ( 'NONE',  ( 4.458734124999999437, 8.937500001365592084, -5.460374474430324690E-16 ) ) ;
#20369 = CARTESIAN_POINT ( 'NONE',  ( -1.339745962155610925, -9.669658196007334894, 5.000000000000000000 ) ) ;
#20370 = CARTESIAN_POINT ( 'NONE',  ( -5.000000000000000000, 18.00000000000000000, 0.000000000000000000 ) ) ;
#20371 = CARTESIAN_POINT ( 'NONE',  ( -9.184850993605147944E-16, -144.3750000027312126, 5.000000000000000000 ) ) ;
#20372 = CYLINDRICAL_SURFACE ( 'NONE', #46933, 5.000000000000000000 ) ;
#20373 = CARTESIAN_POINT ( 'NONE',  ( -4.458734124999999437, -38.39583333196773651, -2.574251347313719407 ) ) ;
#20374 = CARTESIAN_POINT ( 'NONE',  ( -4.999999999999999112, -73.79166666393547303, 2.886751345948131764 ) ) ;
#20375 = CARTESIAN_POINT ( 'NONE',  ( -53.51423613279429503, -144.5000000013656063, 4.591703134518082763 ) ) ;
#20376 = CARTESIAN_POINT ( 'NONE',  ( 5.000000000000000888, -140.9375000000000284, -2.071067811865475505 ) ) ;
#20377 = CARTESIAN_POINT ( 'NONE',  ( -6.972266317189433020E-16, -15.12499999726881050, -5.000000000000000000 ) ) ;
#20378 = CARTESIAN_POINT ( 'NONE',  ( 9.457646018065525792E-16, -81.31249999863440792, 5.148502694627439702 ) ) ;
#20379 = CARTESIAN_POINT ( 'NONE',  ( 4.458734124999997661, -164.7500000013655779, 1.846868145590737864 ) ) ;
#20380 = CARTESIAN_POINT ( 'NONE',  ( 0.000000000000000000, -170.0000000000000000, 5.000000000000000000 ) ) ;
#20381 = CYLINDRICAL_SURFACE ( 'NONE', #50272, 5.000000000000000000 ) ;
#20382 = CARTESIAN_POINT ( 'NONE',  ( 5.000000000000000000, -27.49999999999999645, -6.123233995736766282E-16 ) ) ;
#20383 = CARTESIAN_POINT ( 'NONE',  ( 1.846868145590735200, -142.2500000013656063, -4.458734125000000326 ) ) ;
#20384 = EDGE_LOOP ( 'NONE', ( #26426, #29537, #45460, #7751 ) ) ;
#20385 = CARTESIAN_POINT ( 'NONE',  ( 2.229367062500001939, 26.77083333469892423, 3.861377020970579999 ) ) ;
#20386 = ORIENTED_EDGE ( 'NONE', *, *, #34178, .F. ) ;
#20387 = CARTESIAN_POINT ( 'NONE',  ( -4.458734124999999437, -64.64583333196773651, -2.574251347313719407 ) ) ;
#20388 = CARTESIAN_POINT ( 'NONE',  ( -2.500000000000000444, 23.95833333606451987, -4.330127018922193649 ) ) ;
#20389 = CARTESIAN_POINT ( 'NONE',  ( -58.24261429053147765, -138.3750000027312126, -3.805975901505573855 ) ) ;
#20390 = CARTESIAN_POINT ( 'NONE',  ( -3.535250795749689387E-16, 15.75000000000000178, -5.773502691896257311 ) ) ;
#20391 = VECTOR ( 'NONE', #16056, 1000.000000000000000 ) ;
#20392 = CARTESIAN_POINT ( 'NONE',  ( 4.458734124999999437, -48.81249999863440792, -5.460374474430324690E-16 ) ) ;
#20393 = CARTESIAN_POINT ( 'NONE',  ( -2.229367062499996610, -11.14583333196773829, 3.861377020970582219 ) ) ;
#20394 = CARTESIAN_POINT ( 'NONE',  ( -1.339745962155640457, 4.205341801261477386, 4.999999999999984901 ) ) ;
#20395 = CARTESIAN_POINT ( 'NONE',  ( -5.000000000000000000, 13.91666666666666785, -2.886751345948128211 ) ) ;
#20396 = CARTESIAN_POINT ( 'NONE',  ( 6.123233995736766282E-16, 30.00000000000000000, -5.000000000000000000 ) ) ;
#20397 = FACE_OUTER_BOUND ( 'NONE', #19619, .T. ) ;
#20398 = CARTESIAN_POINT ( 'NONE',  ( -2.499999999999996447, -9.833333333333332149, 4.330127018922195425 ) ) ;
#20400 = CARTESIAN_POINT ( 'NONE',  ( 4.458734125000001214, -19.89583333196773651, 2.574251347313718519 ) ) ;
#20399 = CARTESIAN_POINT ( 'NONE',  ( -58.24261429053147765, -151.2500000000000284, -3.805975901505573855 ) ) ;
#20401 = CARTESIAN_POINT ( 'NONE',  ( -5.000000000000000888, -140.6875000027311842, -2.071067811865475949 ) ) ;
#20402 = CARTESIAN_POINT ( 'NONE',  ( 2.229367062499998831, -52.64583333196773651, -3.861377020970580887 ) ) ;
#20403 = CARTESIAN_POINT ( 'NONE',  ( -4.458734124999999437, -156.1875000013655779, -5.460374474430324690E-16 ) ) ;
#20404 = EDGE_CURVE ( 'NONE', #57091, #29555, #36697, .T. ) ;
#20405 = CARTESIAN_POINT ( 'NONE',  ( 5.000000000000000888, -53.45833333060213732, 2.886751345948126879 ) ) ;
#20406 = ORIENTED_EDGE ( 'NONE', *, *, #48721, .T. ) ;
#20407 = CARTESIAN_POINT ( 'NONE',  ( -51.75738570946856498, -137.7500000000000000, 3.805975901505576964 ) ) ;
#20408 = CARTESIAN_POINT ( 'NONE',  ( -3.152548672688508926E-16, 2.187500001365593416, -5.148502694627439702 ) ) ;
#20409 = EDGE_LOOP ( 'NONE', ( #56510, #17005, #2513, #60104 ) ) ;
#20411 = DIRECTION ( 'NONE',  ( 0.000000000000000000, 0.000000000000000000, 1.000000000000000000 ) ) ;
#20410 = CARTESIAN_POINT ( 'NONE',  ( -5.000000000000000888, -157.6875000027312126, -2.071067811865475949 ) ) ;
#20412 = CARTESIAN_POINT ( 'NONE',  ( -3.152801135295367985, -154.8125000013656063, 3.152801135295367096 ) ) ;
#20413 = ORIENTED_EDGE ( 'NONE', *, *, #35730, .T. ) ;
#20414 = ADVANCED_FACE ( 'NONE', ( #61784 ), #13522, .T. ) ;
#20415 = CARTESIAN_POINT ( 'NONE',  ( 2.500000000000002220, -83.66666666666667140, 4.330127018922192761 ) ) ;
#20416 = CARTESIAN_POINT ( 'NONE',  ( -50.18089887299979068, -129.6875000000000568, 2.462841084822635640 ) ) ;
#20417 = CARTESIAN_POINT ( 'NONE',  ( 1.975475456537005874E-15, 15.25000000000000000, 5.000000000000000000 ) ) ;
#20418 = CARTESIAN_POINT ( 'NONE',  ( 4.458734124999999437, -44.06249999863440081, -5.460374474430324690E-16 ) ) ;
#20419 = VERTEX_POINT ( 'NONE', #22864 ) ;
#20420 = LINE ( 'NONE', #19773, #2913 ) ;
#20421 = EDGE_CURVE ( 'NONE', #26096, #19049, #56332, .T. ) ;
#20422 = CARTESIAN_POINT ( 'NONE',  ( -3.152548672688508926E-16, 14.43750000136559386, -5.148502694627439702 ) ) ;
#20423 = CARTESIAN_POINT ( 'NONE',  ( 9.457646018065525792E-16, -90.31249999863439371, 5.148502694627439702 ) ) ;
#20424 = CARTESIAN_POINT ( 'NONE',  ( -52.80376928212989185, -152.8750000013656063, -4.297418129356379346 ) ) ;
#20425 = CARTESIAN_POINT ( 'NONE',  ( -9.184850993605147944E-16, -165.2500000000000000, 5.000000000000000000 ) ) ;
#20426 = LINE ( 'NONE', #59993, #33611 ) ;
#20427 = AXIS2_PLACEMENT_3D ( 'NONE', #46428, #38038, #37104 ) ;
#20428 = CARTESIAN_POINT ( 'NONE',  ( -9.184850993605147944E-16, -169.2500000000000000, 5.000000000000000000 ) ) ;
#20429 = CARTESIAN_POINT ( 'NONE',  ( -4.458734124999997661, -67.22916666530106511, 2.574251347313722516 ) ) ;
#20430 = CARTESIAN_POINT ( 'NONE',  ( -5.000000000000000000, -61.95833333060213732, -2.886751345948128211 ) ) ;
#20431 = CARTESIAN_POINT ( 'NONE',  ( -4.458734124999999437, 17.60416666803225993, -2.574251347313719407 ) ) ;
#20432 = VECTOR ( 'NONE', #6429, 1000.000000000000000 ) ;
#20433 =( BOUNDED_CURVE ( )  B_SPLINE_CURVE ( 2, ( #36664, #41472, #51151, #51780, #42112, #51467, #26699, #17366, #56291, #31506, #32790, #7723, #52420, #7085, #46633, #27327, #8352, #2579, #41796, #47270, #2904, #61123, #22518, #56928, #61757, #27951, #12849, #60802, #3525, #17684, #46316, #2274, #32466, #37299, #37609, #47574, #22836, #36345, #8037, #55976, #57250, #21877, #13166, #23135, #11888, #38249, #24393, #39175, #33414, #13489, #38857, #18926, #63019, #29203, #18626, #34349, #62386, #18307, #38540, #62701, #14417, #28895, #57870, #9595, #43373, #63322, #4455, #14731, #43996, #23772, #63643, #19563, #8654, #28581, #34040, #53978, #33106, #58494, #42742, #28267, #48828, #4155, #37932, #58171, #57564, #52720, #58800, #13791, #19242, #47881, #3840, #29516, #14101, #4767, #53031, #8970, #43063, #9906, #49148, #33727, #53345, #53661, #9280, #48202, #23459, #48516, #5094, #24084, #43679, #30157, #20850, #55268, #11507, #29841, #15701, #19879, #16015, #25674, #44639, #5411, #15063, #6062, #15383, #54296, #25347, #598, #59129, #60415, #931, #16340, #34677, #35007, #44968, #35962, #59452, #20207, #11186, #54622, #10866, #10546, #39810, #49786, #55587, #40453, #24712, #31123, #50106, #10236, #49473, #60093, #45283, #6380, #50745, #50439, #44317, #5732, #281, #1249, #25028, #20536, #40133, #39493, #59775, #35320, #54940, #30482, #35641, #30809, #25986, #45602, #1560, #21162, #40769, #7960, #7646, #56217, #61992, #47193, #41400, #55900, #22440, #21486, #57173, #7334, #37226, #61051, #21805, #7012, #42353, #32392, #31759, #26945, #41712, #27250, #61361, #31431, #6690, #17610, #46877, #41084, #37532, #2820, #56852, #13089, #11812, #17284, #1881, #61677, #42036, #26620, #51069, #60730, #46561, #51706, #16972, #36277, #2502, #46239, #16652, #17911, #22120, #12769, #27560, #12458, #36907, #45919, #36583, #56538, #32069, #52017, #2201, #3136, #22755, #12137, #32710, #26295, #51392, #59613, #14887, #43522, #63166, #59283, #47495, #58334, #9743, #44475, #20368, #48982, #4931, #24550, #14260, #58648, #34494, #8272, #48665, #9432, #4606, #125, #33882, #29680, #44154, #53502, #34840, #49632, #43835, #23920, #49310, #29348, #19719, #39644, #29042, #44796, #27876, #3448, #39328, #24229, #24874, #19077, #58961, #434, #38697, #10067, #54129, #25182, #54464, #34190, #10390, #30000, #63481, #39019, #20040, #760, #19401, #5252, #52338, #14568, #5568, #15214, #53813, #39967, #15545, #11023, #55737, #45121, #49940, #21956, #35800, #2038, #25827, #50266, #35481, #7172, #60883, #60256, #55423, #6529, #36114, #26143, #59937, #35165, #46080, #21643, #55097, #40612, #31273, #41236, #41552, #40299, #45762, #30319, #26463, #11653, #30644, #15859, #25502, #11341, #16493, #45442, #1086, #30964, #6214, #1716, #50907, #11972, #16808, #36428, #40925, #50589, #10712, #1405, #21324, #60568, #56056, #21007, #6849, #31602, #16175, #46399, #51236, #54781, #61203, #26781, #2348, #5895, #20694, #12305, #22276, #37378, #8433, #47965, #12926, #32548, #52174, #41877, #22601, #62149, #36751, #12614, #37076, #32227, #27722, #52804, #61524, #28037, #17454, #62471, #13571, #7801, #51547, #13247, #57011, #8118, #3608, #56698, #8741, #56381, #31920, #47349, #51858, #52499, #7483, #27403, #47655, #17761, #37689, #42511, #28348, #18391, #61841, #38010, #57643, #46712, #2984, #23216, #3920, #27096, #32870, #17125, #2657, #42826, #33189, #47034, #42198, #57331, #3298, #23539, #22919, #18067, #43138, #29605, #5178, #57952, #4233, #19326, #54055, #29927, #58576, #14495, #34117, #23848, #4535, #53738, #9359, #14182, #9671, #44400, #29279, #34763, #43451, #9992, #63096, #359, #59212, #53426, #33498, #58881, #38940, #48909, #49235, #38621, #54389, #4854, #28971, #19008, #48594, #33809, #24474, #58258, #24795, #63408, #19644, #44081, #10315, #19961, #43763, #39572, #15141, #28661, #24160, #34426, #49552, #45, #39255, #14812, #5494, #48277, #25108, #18698, #62778, #13873, #38323, #53115, #9051, #1646, #54708, #59537, #31520, #45369, #11587, #35401, #59860, #31206, #15471, #35088, #20619, #60814, #21245, #35723, #40225, #30241, #20932, #16739, #50836, #45048, #50189, #40852, #6776, #51163, #49864, #55353, #39891, #6141, #50522, #7096, #10628, #25756, #26387, #36356, #5812, #46004, #44718, #1335, #11267, #60495, #21570, #1969, #41167, #6462, #40537, #20290, #10945, #55986, #15785, #30892, #30564, #36042, #55023, #11900, #681, #60178, #26071, #25429, #1015, #16100, #45689, #16423, #55672, #57258, #33115, #32153, #56936, #2912, #62395, #36674, #37000, #46967, #37941, #61450, #22207, #13175, #17380, #12857, #12540, #46643, #26710, #56304, #47278, #7415, #62077, #51789, #27025, #17057, #17991, #3227, #8360, #57573, #52428, #46325, #7731, #2284, #22845, #2588, #41806, #42123, #17692, #56626, #27336, #61765, #27961, #37307, #18316, #22527, #8046, #47584, #12232, #21887, #32476, #52732, #41483, #13499, #52105, #27651, #42435, #37617, #32799, #3535, #23144, #42752, #61134, #31846, #51478, #28277, #23468, #43071, #63653, #62709, #15072, #44006, #4777, #38550, #24404, #34048, #19572, #9288, #58503, #28589, #14426, #39184, #57878, #33735, #47891, #58182, #290, #49159, #43382, #13803, #58810, #63334, #34357, #5104, #14741, #9915, #4164, #53671, #53987, #18635, #38257, #48210, #24722, #48837, #19252, #33423, #8664, #29524, #29212, #53041, #39502, #44326, #19888, #59138, #14110, #34685, #3847, #63027, #8979, #23780, #38866, #18934, #53353, #28905, #48525, #4466, #24093, #43688, #9604, #15711, #54949, #25685, #55279, #45294, #15393, #54305, #1572, #11198, #25036, #21497, #30821, #50452, #1893, #45616, #49795, #49483, #21172, #6392, #10555, #35017, #44648, #30494, #35653, #44978, #20218, #10878, #30166, #609, #26308, #50116, #45930, #39819, #943, #6072, #41095, #5740, #40780, #25359, #40465, #40143, #20546, #10247, #59460, #25997, #54631, #60426, #35329, #59787, #35973, #16351, #55600, #5421, #1259, #20862, #11518, #60105, #29850, #31133, #16026, #50757, #6702, #60742, #16665, #51402, #51717, #17922, #7658, #8283, #41412, #47204, #36594, #37544, #32720, #26955, #7023, #55911, #23073, #2514, #27263, #46888, #2832, #22450, #22130, #56230, #46573, #7344, #42047, #12151, #3148, #36919, #56863, #61690, #27887, #57183, #17294, #32403, #41723, #52030, #17621, #22768, #56549, #37237, #31770, #12781, #42364, #21815, #61373, #11823, #62003, #36288, #12469, #31441, #7972, #32080, #27571, #13103, #51085, #52348, #47509, #3459, #42677, #61063, #62317, #26631, #46251, #2212, #16982, #13417, #4390, #44249, #37867, #5023, #48136, #53280, #9215, #57499, #33039, #58104, #38182, #53595, #52655, #28829, #9527, #8590, #28200, #47815, #29133, #3772, #24642, #48756, #14353, #4087, #33975, #43612, #4698, #23396, #24320, #18242, #42996, #43927, #63574, #19493, #19170, #23711, #9832, #58736, #52965, #62639, #39108, #48451, #14662, #34282, #53906, #29443, #13726, #18560, #49075, #57804, #43307, #18857, #24009, #38787, #63254, #33350, #8902, #28518, #58426, #62943, #38477, #14033, #33662, #11438, #55197, #59378, #21098, #11117, #1182, #20139, #44570, #54226, #40062, #45217, #54555, #29769, #860, #39738, #34595, #35894, #59705, #55526, #10164, #10478, #20463, #31056, #34934, #50040, #54873, #45534, #528, #10804, #60028, #30091, #50679, #15951, #213, #6621, #25603, #49403, #5347, #35573, #20782, #1495, #26234, #5666, #40387, #49721, #15312, #15637, #40702, #35253, #19811, #24965, #30744, #25279, #60347, #16275, #44901, #30416, #50365, #5999, #6312, #25916, #39420, #59059, #14986, #12072, #46177, #36520, #60983, #32013, #2138, #12712, #46496, #2755, #7581, #17854, #47130, #26882, #27501, #3078, #11747, #31697, #17551, #37476, #16590, #21741, #51647, #56794, #31365, #7270, #1816, #2444, #60667, #21420, #42294, #41337, #22375, #55832, #36210, #32645, #22053, #32328, #56150, #16904, #51331, #51006, #6946, #41646, #61935, #41975, #36847, #61298, #26557, #17220, #57111, #51958, #56477, #12399, #61617, #7896, #52276, #27193, #46809, #41023, #37171, #22696, #8213, #13028, #45854, #33901, #19425, #32967, #58354, #34208, #33279, #58035, #23941, #4625, #53524, #29061, #33592, #48063, #3393, #57734, #13965, #9452, #28132, #38411, #43542, #62569, #39038, #63186, #27816, #53833, #53211, #18168, #37795, #19097, #48379, #48685, #58665, #24250, #47441, #52899, #23010, #23637, #52590, #38715, #18784, #43854, #63500, #14282, #14588, #23321, #9145, #42611, #62249, #57425, #3706, #13346, #4321, #28754, #42922, #8522, #4015, #47750, #18488, #38111, #13660, #8835, #28448, #43231, #62873, #30667, #15880, #15234, #15565, #36685, #4949, #34862, #35500, #1426, #14910, #40319, #17067, #44177, #45461, #49650, #21025, #19738, #20061, #30022, #40632, #44495, #5273, #59957, #457, #59632, #59302, #29699, #9762, #39352, #30338, #54149, #45141, #35185, #144, #58982, #1105, #49964, #55118, #61145, #11043, #29369, #54483, #49002, #5917, #10088, #24894, #25204, #780, #39665, #10410, #44818, #50287, #34518, #25523, #5587, #54803, #6234, #49330, #24572, #10731, #20387, #39987, #20714, #25844, #27660, #47288, #3238, #22854, #22538, #56637, #46975, #7740, #42445, #27973, #12242, #7426, #27035, #47594, #46652, #62717, #3546, #52438, #42134, #8372, #18004, #23154, #56946, #62087, #12551, #37627, #42763, #41814, #57584, #57268, #61775, #47899, #33127, #27344, #61461, #3855, #31855, #51488, #32485, #32163, #62405, #2597, #13186, #18327, #22217, #17393, #37008, #37951, #13511, #37316, #52744, #8673, #51798, #17702, #28287, #23476, #2923, #43079, #56319, #12867, #18642, #52114, #8058, #32809, #24100, #29856, #15078, #9295, #58817, #48217, #53050, #25044, #38875, #5110, #28911, #53361, #38560, #10255, #297, #63344, #58509, #9611, #39192, #29218, #63034, #38264, #49170, #14747, #58189, #43696, #34364, #24729, #44655, #43389, #48844, #33431, #29533, #53994, #14118, #18942, #28599, #14433, #19578, #48534, #44331, #616, #19258, #4785, #34056, #49489, #4172, #4473, #53678, #5427, #24412, #33744, #19894, #44013, #63661, #9921, #39509, #57886, #23787, #59146, #34691, #54316, #13812, #8987, #10563, #55609, #40787, #1900, #31452, #45937, #20226, #25691, #39826, #60434, #20552, #35337, #35662, #11207, #30502, #54956, #55287, #21507, #30830, #55918, #16033, #1580, #41104, #5748, #15402, #6399, #46260, #59469, #7030, #50124, #50459, #26007, #45625, #11832, #25366, #31141, #40153, #60749, #16674, #10886, #35027, #54639, #26641, #6081, #21180, #16359, #35980, #11525, #45301, #59797, #1268, #20870, #50767, #15718, #6710, #40472, #26318, #36295, #51093, #30173, #49803, #44986, #952, #60112, #37553, #57510, #36607, #62011, #2219, #31779, #32730, #13113, #3470, #3158, #51727, #13426, #42686, #36931, #51410, #17929, #16991, #52666, #2841, #52357, #56557, #17304, #2524, #37878, #27898, #27274, #22461, #37246, #22777, #56873, #26963, #21822, #8295, #42372, #56239, #33052, #57193, #47519, #8600, #7353, #12791, #61070, #23083, #62330, #22139, #46582, #12160, #18251, #28210, #41734, #41421, #42058, #61384, #12478, #32091, #61700, #7667, #46900, #7982, #17629, #32412, #52043, #27580, #47215, #29456, #48146, #58434, #43936, #18870, #59070, #63583, #47824, #54235, #9539, #38191, #57816, #53915, #43005, #52974, #4399, #39117, #14995, #43623, #63265, #19183, #8915, #53289, #29143, #3783, #43317, #4098, #62952, #23721, #222, #24335, #38796, #28528, #23406, #58744, #4710, #18570, #34608, #19504, #14672, #10176, #34293, #38487, #5033, #9841, #9225, #53605, #62651, #13738, #14362, #33359, #58114 ),
 .UNSPECIFIED., .F., .F. ) 
 B_SPLINE_CURVE_WITH_KNOTS ( ( 3, 2, 2, 2, 2, 2, 2, 2, 2, 2, 2, 2, 2, 2, 2, 2, 2, 2, 2, 2, 2, 2, 2, 2, 2, 2, 2, 2, 2, 2, 2, 2, 2, 2, 2, 2, 2, 2, 2, 2, 2, 2, 2, 2, 2, 2, 2, 2, 2, 2, 2, 2, 2, 2, 2, 2, 2, 2, 2, 2, 2, 2, 2, 2, 2, 2, 2, 2, 2, 2, 2, 2, 2, 2, 2, 2, 2, 2, 2, 2, 2, 2, 2, 2, 2, 2, 2, 2, 2, 2, 2, 2, 2, 2, 2, 2, 2, 2, 2, 2, 2, 2, 2, 2, 2, 2, 2, 2, 2, 2, 2, 2, 2, 2, 2, 2, 2, 2, 2, 2, 2, 2, 2, 2, 2, 2, 2, 2, 2, 2, 2, 2, 2, 2, 2, 2, 2, 2, 2, 2, 2, 2, 2, 2, 2, 2, 2, 2, 2, 2, 2, 2, 2, 2, 2, 2, 2, 2, 2, 2, 2, 2, 2, 2, 2, 2, 2, 2, 2, 2, 2, 2, 2, 2, 2, 2, 2, 2, 2, 2, 2, 2, 2, 2, 2, 2, 2, 2, 2, 2, 2, 2, 2, 2, 2, 2, 2, 2, 2, 2, 2, 2, 2, 2, 2, 2, 2, 2, 2, 2, 2, 2, 2, 2, 2, 2, 2, 2, 2, 2, 2, 2, 2, 2, 2, 2, 2, 2, 2, 2, 2, 2, 2, 2, 2, 2, 2, 2, 2, 2, 2, 2, 2, 2, 2, 2, 2, 2, 2, 2, 2, 2, 2, 2, 2, 2, 2, 2, 2, 2, 2, 2, 2, 2, 2, 2, 2, 2, 2, 2, 2, 2, 2, 2, 2, 2, 2, 2, 2, 2, 2, 2, 2, 2, 2, 2, 2, 2, 2, 2, 2, 2, 2, 2, 2, 2, 2, 2, 2, 2, 2, 2, 2, 2, 2, 2, 2, 2, 2, 2, 2, 2, 2, 2, 2, 2, 2, 2, 2, 2, 2, 2, 2, 2, 2, 2, 2, 2, 2, 2, 2, 2, 2, 2, 2, 2, 2, 2, 2, 2, 2, 2, 2, 2, 2, 2, 2, 2, 2, 2, 2, 2, 2, 2, 2, 2, 2, 2, 2, 2, 2, 2, 2, 2, 2, 2, 2, 2, 2, 2, 2, 2, 2, 2, 2, 2, 2, 2, 2, 2, 2, 2, 2, 2, 2, 2, 2, 2, 2, 2, 2, 2, 2, 2, 2, 2, 2, 2, 2, 2, 2, 2, 2, 2, 2, 2, 2, 2, 2, 2, 2, 2, 2, 2, 2, 2, 2, 2, 2, 2, 2, 2, 2, 2, 2, 2, 2, 2, 2, 2, 2, 2, 2, 2, 2, 2, 2, 2, 2, 2, 2, 2, 2, 2, 2, 2, 2, 2, 2, 2, 2, 2, 2, 2, 2, 2, 2, 2, 2, 2, 2, 2, 2, 2, 2, 2, 2, 2, 2, 2, 2, 2, 2, 2, 2, 2, 2, 2, 2, 2, 2, 2, 2, 2, 2, 2, 2, 2, 2, 2, 2, 2, 2, 2, 2, 2, 2, 2, 2, 2, 2, 2, 2, 2, 2, 2, 2, 2, 2, 2, 2, 2, 2, 2, 2, 2, 2, 2, 2, 2, 2, 2, 2, 2, 2, 2, 2, 2, 2, 2, 2, 2, 2, 2, 2, 2, 2, 2, 2, 2, 2, 2, 2, 2, 2, 2, 2, 2, 2, 2, 2, 2, 2, 2, 2, 2, 2, 2, 2, 2, 2, 2, 2, 2, 2, 2, 2, 2, 2, 2, 2, 2, 2, 2, 2, 2, 2, 2, 2, 2, 2, 2, 2, 2, 2, 2, 2, 2, 2, 2, 2, 2, 2, 2, 2, 2, 2, 2, 2, 2, 2, 2, 2, 2, 2, 2, 2, 2, 2, 2, 2, 2, 2, 2, 2, 2, 2, 2, 2, 2, 2, 2, 2, 2, 2, 2, 2, 2, 2, 2, 2, 2, 2, 2, 2, 2, 2, 2, 2, 2, 2, 2, 2, 2, 2, 2, 2, 2, 2, 2, 2, 2, 2, 2, 2, 2, 2, 2, 2, 2, 2, 2, 2, 2, 2, 2, 2, 2, 2, 2, 2, 2, 2, 2, 2, 2, 2, 2, 2, 2, 2, 2, 2, 2, 2, 2, 2, 2, 2, 2, 2, 2, 2, 2, 2, 2, 2, 2, 2, 2, 2, 2, 2, 2, 2, 2, 2, 2, 2, 2, 2, 2, 2, 2, 2, 2, 2, 2, 2, 2, 3 ),
 ( 0.000000000000000000, 0.001388888888888888942, 0.002777777777777777884, 0.004166666666666666609, 0.005555555555555555768, 0.006944444444444444059, 0.008333333333333333218, 0.009722222222222222376, 0.01111111111111111154, 0.01250000000000000069, 0.01388888888888888812, 0.01527777777777777728, 0.01666666666666666644, 0.01805555555555555386, 0.01944444444444444475, 0.02083333333333333218, 0.02222222222222222307, 0.02361111111111111049, 0.02500000000000000139, 0.02638888888888888881, 0.02777777777777777624, 0.02916666666666666713, 0.03055555555555555455, 0.03194444444444444198, 0.03333333333333333287, 0.03472222222222222376, 0.03611111111111110772, 0.03749999999999999861, 0.03888888888888888951, 0.04027777777777778040, 0.04166666666666666435, 0.04305555555555555525, 0.04444444444444444614, 0.04583333333333333010, 0.04722222222222222099, 0.04861111111111111188, 0.05000000000000000278, 0.05138888888888888673, 0.05277777777777777762, 0.05416666666666666852, 0.05555555555555555247, 0.05694444444444444337, 0.05833333333333333426, 0.05972222222222222515, 0.06111111111111110911, 0.06250000000000000000, 0.06388888888888888395, 0.06527777777777778179, 0.06666666666666666574, 0.06805555555555554970, 0.06944444444444444753, 0.07083333333333333148, 0.07222222222222221544, 0.07361111111111111327, 0.07499999999999999722, 0.07638888888888889506, 0.07777777777777777901, 0.07916666666666666297, 0.08055555555555556080, 0.08194444444444444475, 0.08333333333333332871, 0.08472222222222222654, 0.08611111111111111049, 0.08749999999999999445, 0.08888888888888889228, 0.09027777777777777624, 0.09166666666666666019, 0.09305555555555555802, 0.09444444444444444198, 0.09583333333333333981, 0.09722222222222222376, 0.09861111111111110772, 0.1000000000000000056, 0.1013888888888888895, 0.1027777777777777735, 0.1041666666666666713, 0.1055555555555555552, 0.1069444444444444392, 0.1083333333333333370, 0.1097222222222222210, 0.1111111111111111049, 0.1125000000000000028, 0.1138888888888888867, 0.1152777777777777846, 0.1166666666666666685, 0.1180555555555555525, 0.1194444444444444503, 0.1208333333333333343, 0.1222222222222222182, 0.1236111111111111160, 0.1250000000000000000, 0.1263888888888888840, 0.1277777777777777679, 0.1291666666666666796, 0.1305555555555555636, 0.1319444444444444475, 0.1333333333333333315, 0.1347222222222222154, 0.1361111111111110994, 0.1375000000000000111, 0.1388888888888888951, 0.1402777777777777790, 0.1416666666666666630, 0.1430555555555555469, 0.1444444444444444309, 0.1458333333333333426, 0.1472222222222222265, 0.1486111111111111105, 0.1499999999999999944, 0.1513888888888888784, 0.1527777777777777901, 0.1541666666666666741, 0.1555555555555555580, 0.1569444444444444420, 0.1583333333333333259, 0.1597222222222222099, 0.1611111111111111216, 0.1625000000000000056, 0.1638888888888888895, 0.1652777777777777735, 0.1666666666666666574, 0.1680555555555555691, 0.1694444444444444531, 0.1708333333333333370, 0.1722222222222222210, 0.1736111111111111049, 0.1749999999999999889, 0.1763888888888889006, 0.1777777777777777846, 0.1791666666666666685, 0.1805555555555555525, 0.1819444444444444364, 0.1833333333333333204, 0.1847222222222222321, 0.1861111111111111160, 0.1875000000000000000, 0.1888888888888888840, 0.1902777777777777679, 0.1916666666666666796, 0.1930555555555555636, 0.1944444444444444475, 0.1958333333333333315, 0.1972222222222222154, 0.1986111111111110994, 0.2000000000000000111, 0.2013888888888888951, 0.2027777777777777790, 0.2041666666666666630, 0.2055555555555555469, 0.2069444444444444309, 0.2083333333333333426, 0.2097222222222222265, 0.2111111111111111105, 0.2124999999999999944, 0.2138888888888888784, 0.2152777777777777901, 0.2166666666666666741, 0.2180555555555555580, 0.2194444444444444420, 0.2208333333333333259, 0.2222222222222222099, 0.2236111111111111216, 0.2250000000000000056, 0.2263888888888888895, 0.2277777777777777735, 0.2291666666666666574, 0.2305555555555555691, 0.2319444444444444531, 0.2333333333333333370, 0.2347222222222222210, 0.2361111111111111049, 0.2374999999999999889, 0.2388888888888889006, 0.2402777777777777846, 0.2416666666666666685, 0.2430555555555555525, 0.2444444444444444364, 0.2458333333333333204, 0.2472222222222222321, 0.2486111111111111160, 0.2500000000000000000, 0.2513888888888888840, 0.2527777777777777679, 0.2541666666666666519, 0.2555555555555555358, 0.2569444444444444198, 0.2583333333333333592, 0.2597222222222222432, 0.2611111111111111271, 0.2625000000000000111, 0.2638888888888888951, 0.2652777777777777790, 0.2666666666666666630, 0.2680555555555555469, 0.2694444444444444309, 0.2708333333333333148, 0.2722222222222221988, 0.2736111111111111382, 0.2750000000000000222, 0.2763888888888889062, 0.2777777777777777901, 0.2791666666666666741, 0.2805555555555555580, 0.2819444444444444420, 0.2833333333333333259, 0.2847222222222222099, 0.2861111111111110938, 0.2874999999999999778, 0.2888888888888888618, 0.2902777777777778012, 0.2916666666666666852, 0.2930555555555555691, 0.2944444444444444531, 0.2958333333333333370, 0.2972222222222222210, 0.2986111111111111049, 0.2999999999999999889, 0.3013888888888888729, 0.3027777777777777568, 0.3041666666666666408, 0.3055555555555555802, 0.3069444444444444642, 0.3083333333333333481, 0.3097222222222222321, 0.3111111111111111160, 0.3125000000000000000, 0.3138888888888888840, 0.3152777777777777679, 0.3166666666666666519, 0.3180555555555555358, 0.3194444444444444198, 0.3208333333333333592, 0.3222222222222222432, 0.3236111111111111271, 0.3250000000000000111, 0.3263888888888888951, 0.3277777777777777790, 0.3291666666666666630, 0.3305555555555555469, 0.3319444444444444309, 0.3333333333333333148, 0.3347222222222221988, 0.3361111111111111382, 0.3375000000000000222, 0.3388888888888889062, 0.3402777777777777901, 0.3416666666666666741, 0.3430555555555555580, 0.3444444444444444420, 0.3458333333333333259, 0.3472222222222222099, 0.3486111111111110938, 0.3499999999999999778, 0.3513888888888888618, 0.3527777777777778012, 0.3541666666666666852, 0.3555555555555555691, 0.3569444444444444531, 0.3583333333333333370, 0.3597222222222222210, 0.3611111111111111049, 0.3624999999999999889, 0.3638888888888888729, 0.3652777777777777568, 0.3666666666666666408, 0.3680555555555555802, 0.3694444444444444642, 0.3708333333333333481, 0.3722222222222222321, 0.3736111111111111160, 0.3750000000000000000, 0.3763888888888888840, 0.3777777777777777679, 0.3791666666666666519, 0.3805555555555555358, 0.3819444444444444198, 0.3833333333333333592, 0.3847222222222222432, 0.3861111111111111271, 0.3875000000000000111, 0.3888888888888888951, 0.3902777777777777790, 0.3916666666666666630, 0.3930555555555555469, 0.3944444444444444309, 0.3958333333333333148, 0.3972222222222221988, 0.3986111111111111382, 0.4000000000000000222, 0.4013888888888889062, 0.4027777777777777901, 0.4041666666666666741, 0.4055555555555555580, 0.4069444444444444420, 0.4083333333333333259, 0.4097222222222222099, 0.4111111111111110938, 0.4124999999999999778, 0.4138888888888888618, 0.4152777777777778012, 0.4166666666666666852, 0.4180555555555555691, 0.4194444444444444531, 0.4208333333333333370, 0.4222222222222222210, 0.4236111111111111049, 0.4249999999999999889, 0.4263888888888888729, 0.4277777777777777568, 0.4291666666666666408, 0.4305555555555555802, 0.4319444444444444642, 0.4333333333333333481, 0.4347222222222222321, 0.4361111111111111160, 0.4375000000000000000, 0.4388888888888888840, 0.4402777777777777679, 0.4416666666666666519, 0.4430555555555555358, 0.4444444444444444198, 0.4458333333333333592, 0.4472222222222222432, 0.4486111111111111271, 0.4500000000000000111, 0.4513888888888888951, 0.4527777777777777790, 0.4541666666666666630, 0.4555555555555555469, 0.4569444444444444309, 0.4583333333333333148, 0.4597222222222221988, 0.4611111111111111382, 0.4625000000000000222, 0.4638888888888889062, 0.4652777777777777901, 0.4666666666666666741, 0.4680555555555555580, 0.4694444444444444420, 0.4708333333333333259, 0.4722222222222222099, 0.4736111111111110938, 0.4749999999999999778, 0.4763888888888888618, 0.4777777777777778012, 0.4791666666666666852, 0.4805555555555555691, 0.4819444444444444531, 0.4833333333333333370, 0.4847222222222222210, 0.4861111111111111049, 0.4874999999999999889, 0.4888888888888888729, 0.4902777777777777568, 0.4916666666666666408, 0.4930555555555555802, 0.4944444444444444642, 0.4958333333333333481, 0.4972222222222222321, 0.4986111111111111160, 0.5000000000000000000, 0.5013888888888888840, 0.5027777777777777679, 0.5041666666666666519, 0.5055555555555555358, 0.5069444444444444198, 0.5083333333333333037, 0.5097222222222221877, 0.5111111111111110716, 0.5124999999999999556, 0.5138888888888888395, 0.5152777777777777235, 0.5166666666666667185, 0.5180555555555556024, 0.5194444444444444864, 0.5208333333333333703, 0.5222222222222222543, 0.5236111111111111382, 0.5250000000000000222, 0.5263888888888889062, 0.5277777777777777901, 0.5291666666666666741, 0.5305555555555555580, 0.5319444444444444420, 0.5333333333333333259, 0.5347222222222222099, 0.5361111111111110938, 0.5374999999999999778, 0.5388888888888888618, 0.5402777777777777457, 0.5416666666666666297, 0.5430555555555555136, 0.5444444444444443976, 0.5458333333333332815, 0.5472222222222222765, 0.5486111111111111605, 0.5500000000000000444, 0.5513888888888889284, 0.5527777777777778123, 0.5541666666666666963, 0.5555555555555555802, 0.5569444444444444642, 0.5583333333333333481, 0.5597222222222222321, 0.5611111111111111160, 0.5625000000000000000, 0.5638888888888888840, 0.5652777777777777679, 0.5666666666666666519, 0.5680555555555555358, 0.5694444444444444198, 0.5708333333333333037, 0.5722222222222221877, 0.5736111111111110716, 0.5749999999999999556, 0.5763888888888888395, 0.5777777777777777235, 0.5791666666666667185, 0.5805555555555556024, 0.5819444444444444864, 0.5833333333333333703, 0.5847222222222222543, 0.5861111111111111382, 0.5875000000000000222, 0.5888888888888889062, 0.5902777777777777901, 0.5916666666666666741, 0.5930555555555555580, 0.5944444444444444420, 0.5958333333333333259, 0.5972222222222222099, 0.5986111111111110938, 0.5999999999999999778, 0.6013888888888888618, 0.6027777777777777457, 0.6041666666666666297, 0.6055555555555555136, 0.6069444444444443976, 0.6083333333333332815, 0.6097222222222222765, 0.6111111111111111605, 0.6125000000000000444, 0.6138888888888889284, 0.6152777777777778123, 0.6166666666666666963, 0.6180555555555555802, 0.6194444444444444642, 0.6208333333333333481, 0.6222222222222222321, 0.6236111111111111160, 0.6250000000000000000, 0.6263888888888888840, 0.6277777777777777679, 0.6291666666666666519, 0.6305555555555555358, 0.6319444444444444198, 0.6333333333333333037, 0.6347222222222221877, 0.6361111111111110716, 0.6374999999999999556, 0.6388888888888888395, 0.6402777777777777235, 0.6416666666666667185, 0.6430555555555556024, 0.6444444444444444864, 0.6458333333333333703, 0.6472222222222222543, 0.6486111111111111382, 0.6500000000000000222, 0.6513888888888889062, 0.6527777777777777901, 0.6541666666666666741, 0.6555555555555555580, 0.6569444444444444420, 0.6583333333333333259, 0.6597222222222222099, 0.6611111111111110938, 0.6624999999999999778, 0.6638888888888888618, 0.6652777777777777457, 0.6666666666666666297, 0.6680555555555555136, 0.6694444444444443976, 0.6708333333333332815, 0.6722222222222222765, 0.6736111111111111605, 0.6750000000000000444, 0.6763888888888889284, 0.6777777777777778123, 0.6791666666666666963, 0.6805555555555555802, 0.6819444444444444642, 0.6833333333333333481, 0.6847222222222222321, 0.6861111111111111160, 0.6875000000000000000, 0.6888888888888888840, 0.6902777777777777679, 0.6916666666666666519, 0.6930555555555555358, 0.6944444444444444198, 0.6958333333333333037, 0.6972222222222221877, 0.6986111111111110716, 0.6999999999999999556, 0.7013888888888888395, 0.7027777777777777235, 0.7041666666666667185, 0.7055555555555556024, 0.7069444444444444864, 0.7083333333333333703, 0.7097222222222222543, 0.7111111111111111382, 0.7125000000000000222, 0.7138888888888889062, 0.7152777777777777901, 0.7166666666666666741, 0.7180555555555555580, 0.7194444444444444420, 0.7208333333333333259, 0.7222222222222222099, 0.7236111111111110938, 0.7249999999999999778, 0.7263888888888888618, 0.7277777777777777457, 0.7291666666666666297, 0.7305555555555555136, 0.7319444444444443976, 0.7333333333333332815, 0.7347222222222222765, 0.7361111111111111605, 0.7375000000000000444, 0.7388888888888889284, 0.7402777777777778123, 0.7416666666666666963, 0.7430555555555555802, 0.7444444444444444642, 0.7458333333333333481, 0.7472222222222222321, 0.7486111111111111160, 0.7500000000000000000, 0.7513888888888888840, 0.7527777777777777679, 0.7541666666666666519, 0.7555555555555555358, 0.7569444444444444198, 0.7583333333333333037, 0.7597222222222221877, 0.7611111111111110716, 0.7624999999999999556, 0.7638888888888888395, 0.7652777777777777235, 0.7666666666666667185, 0.7680555555555556024, 0.7694444444444444864, 0.7708333333333333703, 0.7722222222222222543, 0.7736111111111111382, 0.7750000000000000222, 0.7763888888888889062, 0.7777777777777777901, 0.7791666666666666741, 0.7805555555555555580, 0.7819444444444444420, 0.7833333333333333259, 0.7847222222222222099, 0.7861111111111110938, 0.7874999999999999778, 0.7888888888888888618, 0.7902777777777777457, 0.7916666666666666297, 0.7930555555555555136, 0.7944444444444443976, 0.7958333333333332815, 0.7972222222222222765, 0.7986111111111111605, 0.8000000000000000444, 0.8013888888888889284, 0.8027777777777778123, 0.8041666666666666963, 0.8055555555555555802, 0.8069444444444444642, 0.8083333333333333481, 0.8097222222222222321, 0.8111111111111111160, 0.8125000000000000000, 0.8138888888888888840, 0.8152777777777777679, 0.8166666666666666519, 0.8180555555555555358, 0.8194444444444444198, 0.8208333333333333037, 0.8222222222222221877, 0.8236111111111110716, 0.8249999999999999556, 0.8263888888888888395, 0.8277777777777777235, 0.8291666666666667185, 0.8305555555555556024, 0.8319444444444444864, 0.8333333333333333703, 0.8347222222222222543, 0.8361111111111111382, 0.8375000000000000222, 0.8388888888888889062, 0.8402777777777777901, 0.8416666666666666741, 0.8430555555555555580, 0.8444444444444444420, 0.8458333333333333259, 0.8472222222222222099, 0.8486111111111110938, 0.8499999999999999778, 0.8513888888888888618, 0.8527777777777777457, 0.8541666666666666297, 0.8555555555555555136, 0.8569444444444443976, 0.8583333333333332815, 0.8597222222222222765, 0.8611111111111111605, 0.8625000000000000444, 0.8638888888888889284, 0.8652777777777778123, 0.8666666666666666963, 0.8680555555555555802, 0.8694444444444444642, 0.8708333333333333481, 0.8722222222222222321, 0.8736111111111111160, 0.8750000000000000000, 0.8763888888888888840, 0.8777777777777777679, 0.8791666666666666519, 0.8805555555555555358, 0.8819444444444444198, 0.8833333333333333037, 0.8847222222222221877, 0.8861111111111110716, 0.8874999999999999556, 0.8888888888888888395, 0.8902777777777777235, 0.8916666666666667185, 0.8930555555555556024, 0.8944444444444444864, 0.8958333333333333703, 0.8972222222222222543, 0.8986111111111111382, 0.9000000000000000222, 0.9013888888888889062, 0.9027777777777777901, 0.9041666666666666741, 0.9055555555555555580, 0.9069444444444444420, 0.9083333333333333259, 0.9097222222222222099, 0.9111111111111110938, 0.9124999999999999778, 0.9138888888888888618, 0.9152777777777777457, 0.9166666666666666297, 0.9180555555555555136, 0.9194444444444443976, 0.9208333333333332815, 0.9222222222222222765, 0.9236111111111111605, 0.9250000000000000444, 0.9263888888888889284, 0.9277777777777778123, 0.9291666666666666963, 0.9305555555555555802, 0.9319444444444444642, 0.9333333333333333481, 0.9347222222222222321, 0.9361111111111111160, 0.9375000000000000000, 0.9388888888888888840, 0.9402777777777777679, 0.9416666666666666519, 0.9430555555555555358, 0.9444444444444444198, 0.9458333333333333037, 0.9472222222222221877, 0.9486111111111110716, 0.9499999999999999556, 0.9513888888888888395, 0.9527777777777777235, 0.9541666666666667185, 0.9555555555555556024, 0.9569444444444444864, 0.9583333333333333703, 0.9597222222222222543, 0.9611111111111111382, 0.9625000000000000222, 0.9638888888888889062, 0.9652777777777777901, 0.9666666666666666741, 0.9680555555555555580, 0.9694444444444444420, 0.9708333333333333259, 0.9722222222222222099, 0.9736111111111110938, 0.9749999999999999778, 0.9763888888888888618, 0.9777777777777777457, 0.9791666666666666297, 0.9805555555555555136, 0.9819444444444443976, 0.9833333333333332815, 0.9847222222222222765, 0.9861111111111111605, 0.9875000000000000444, 0.9888888888888889284, 0.9902777777777778123, 0.9916666666666666963, 0.9930555555555555802, 0.9944444444444444642, 0.9958333333333333481, 0.9972222222222222321, 0.9986111111111111160, 1.000000000000000000 ),
 .UNSPECIFIED. ) 
 CURVE ( )  GEOMETRIC_REPRESENTATION_ITEM ( )  RATIONAL_B_SPLINE_CURVE ( ( 1.000000000000000000, 0.8660254037844387076, 1.000000000000000000, 0.8660254037844387076, 1.000000000000000000, 0.8660254037844387076, 1.000000000000000000, 0.8660254037844387076, 1.000000000000000000, 0.8660254037844387076, 1.000000000000000000, 0.8660254037844387076, 1.000000000000000000, 0.8660254037844387076, 1.000000000000000000, 0.8660254037844387076, 1.000000000000000000, 0.8660254037844387076, 1.000000000000000000, 0.8660254037844387076, 1.000000000000000000, 0.8660254037844387076, 1.000000000000000000, 0.8660254037844387076, 1.000000000000000000, 0.8660254037844387076, 1.000000000000000000, 0.8660254037844387076, 1.000000000000000000, 0.8660254037844387076, 1.000000000000000000, 0.8660254037844387076, 1.000000000000000000, 0.8660254037844387076, 1.000000000000000000, 0.8660254037844387076, 1.000000000000000000, 0.8660254037844387076, 1.000000000000000000, 0.8660254037844387076, 1.000000000000000000, 0.8660254037844387076, 1.000000000000000000, 0.8660254037844387076, 1.000000000000000000, 0.8660254037844387076, 1.000000000000000000, 0.8660254037844387076, 1.000000000000000000, 0.8660254037844387076, 1.000000000000000000, 0.8660254037844387076, 1.000000000000000000, 0.8660254037844387076, 1.000000000000000000, 0.8660254037844387076, 1.000000000000000000, 0.8660254037844387076, 1.000000000000000000, 0.8660254037844387076, 1.000000000000000000, 0.8660254037844387076, 1.000000000000000000, 0.8660254037844387076, 1.000000000000000000, 0.8660254037844387076, 1.000000000000000000, 0.8660254037844387076, 1.000000000000000000, 0.8660254037844387076, 1.000000000000000000, 0.8660254037844387076, 1.000000000000000000, 0.8660254037844387076, 1.000000000000000000, 0.8660254037844387076, 1.000000000000000000, 0.8660254037844387076, 1.000000000000000000, 0.8660254037844387076, 1.000000000000000000, 0.8660254037844387076, 1.000000000000000000, 0.8660254037844387076, 1.000000000000000000, 0.8660254037844387076, 1.000000000000000000, 0.8660254037844387076, 1.000000000000000000, 0.8660254037844387076, 1.000000000000000000, 0.8660254037844387076, 1.000000000000000000, 0.8660254037844387076, 1.000000000000000000, 0.8660254037844387076, 1.000000000000000000, 0.8660254037844387076, 1.000000000000000000, 0.8660254037844387076, 1.000000000000000000, 0.8660254037844387076, 1.000000000000000000, 0.8660254037844387076, 1.000000000000000000, 0.8660254037844387076, 1.000000000000000000, 0.8660254037844387076, 1.000000000000000000, 0.8660254037844387076, 1.000000000000000000, 0.8660254037844387076, 1.000000000000000000, 0.8660254037844387076, 1.000000000000000000, 0.8660254037844387076, 1.000000000000000000, 0.8660254037844387076, 1.000000000000000000, 0.8660254037844387076, 1.000000000000000000, 0.8660254037844387076, 1.000000000000000000, 0.8660254037844387076, 1.000000000000000000, 0.8660254037844387076, 1.000000000000000000, 0.8660254037844387076, 1.000000000000000000, 0.8660254037844387076, 1.000000000000000000, 0.8660254037844387076, 1.000000000000000000, 0.8660254037844387076, 1.000000000000000000, 0.8660254037844387076, 1.000000000000000000, 0.8660254037844387076, 1.000000000000000000, 0.8660254037844387076, 1.000000000000000000, 0.8660254037844387076, 1.000000000000000000, 0.8660254037844387076, 1.000000000000000000, 0.8660254037844387076, 1.000000000000000000, 0.8660254037844387076, 1.000000000000000000, 0.8660254037844387076, 1.000000000000000000, 0.8660254037844387076, 1.000000000000000000, 0.8660254037844387076, 1.000000000000000000, 0.8660254037844387076, 1.000000000000000000, 0.8660254037844387076, 1.000000000000000000, 0.8660254037844387076, 1.000000000000000000, 0.8660254037844387076, 1.000000000000000000, 0.8660254037844387076, 1.000000000000000000, 0.8660254037844387076, 1.000000000000000000, 0.8660254037844387076, 1.000000000000000000, 0.8660254037844387076, 1.000000000000000000, 0.8660254037844387076, 1.000000000000000000, 0.8660254037844387076, 1.000000000000000000, 0.8660254037844387076, 1.000000000000000000, 0.8660254037844387076, 1.000000000000000000, 0.8660254037844387076, 1.000000000000000000, 0.8660254037844387076, 1.000000000000000000, 0.8660254037844387076, 1.000000000000000000, 0.8660254037844387076, 1.000000000000000000, 0.8660254037844387076, 1.000000000000000000, 0.8660254037844387076, 1.000000000000000000, 0.8660254037844387076, 1.000000000000000000, 0.8660254037844387076, 1.000000000000000000, 0.8660254037844387076, 1.000000000000000000, 0.8660254037844387076, 1.000000000000000000, 0.8660254037844387076, 1.000000000000000000, 0.8660254037844387076, 1.000000000000000000, 0.8660254037844387076, 1.000000000000000000, 0.8660254037844387076, 1.000000000000000000, 0.8660254037844387076, 1.000000000000000000, 0.8660254037844387076, 1.000000000000000000, 0.8660254037844387076, 1.000000000000000000, 0.8660254037844387076, 1.000000000000000000, 0.8660254037844387076, 1.000000000000000000, 0.8660254037844387076, 1.000000000000000000, 0.8660254037844387076, 1.000000000000000000, 0.8660254037844387076, 1.000000000000000000, 0.8660254037844387076, 1.000000000000000000, 0.8660254037844387076, 1.000000000000000000, 0.8660254037844387076, 1.000000000000000000, 0.8660254037844387076, 1.000000000000000000, 0.8660254037844387076, 1.000000000000000000, 0.8660254037844387076, 1.000000000000000000, 0.8660254037844387076, 1.000000000000000000, 0.8660254037844387076, 1.000000000000000000, 0.8660254037844387076, 1.000000000000000000, 0.8660254037844387076, 1.000000000000000000, 0.8660254037844387076, 1.000000000000000000, 0.8660254037844387076, 1.000000000000000000, 0.8660254037844387076, 1.000000000000000000, 0.8660254037844387076, 1.000000000000000000, 0.8660254037844387076, 1.000000000000000000, 0.8660254037844387076, 1.000000000000000000, 0.8660254037844387076, 1.000000000000000000, 0.8660254037844387076, 1.000000000000000000, 0.8660254037844387076, 1.000000000000000000, 0.8660254037844387076, 1.000000000000000000, 0.8660254037844387076, 1.000000000000000000, 0.8660254037844387076, 1.000000000000000000, 0.8660254037844387076, 1.000000000000000000, 0.8660254037844387076, 1.000000000000000000, 0.8660254037844387076, 1.000000000000000000, 0.8660254037844387076, 1.000000000000000000, 0.8660254037844387076, 1.000000000000000000, 0.8660254037844387076, 1.000000000000000000, 0.8660254037844387076, 1.000000000000000000, 0.8660254037844387076, 1.000000000000000000, 0.8660254037844387076, 1.000000000000000000, 0.8660254037844387076, 1.000000000000000000, 0.8660254037844387076, 1.000000000000000000, 0.8660254037844387076, 1.000000000000000000, 0.8660254037844387076, 1.000000000000000000, 0.8660254037844387076, 1.000000000000000000, 0.8660254037844387076, 1.000000000000000000, 0.8660254037844387076, 1.000000000000000000, 0.8660254037844387076, 1.000000000000000000, 0.8660254037844387076, 1.000000000000000000, 0.8660254037844387076, 1.000000000000000000, 0.8660254037844387076, 1.000000000000000000, 0.8660254037844387076, 1.000000000000000000, 0.8660254037844387076, 1.000000000000000000, 0.8660254037844387076, 1.000000000000000000, 0.8660254037844387076, 1.000000000000000000, 0.8660254037844387076, 1.000000000000000000, 0.8660254037844387076, 1.000000000000000000, 0.8660254037844387076, 1.000000000000000000, 0.8660254037844387076, 1.000000000000000000, 0.8660254037844387076, 1.000000000000000000, 0.8660254037844387076, 1.000000000000000000, 0.8660254037844387076, 1.000000000000000000, 0.8660254037844387076, 1.000000000000000000, 0.8660254037844387076, 1.000000000000000000, 0.8660254037844387076, 1.000000000000000000, 0.8660254037844387076, 1.000000000000000000, 0.8660254037844387076, 1.000000000000000000, 0.8660254037844387076, 1.000000000000000000, 0.8660254037844387076, 1.000000000000000000, 0.8660254037844387076, 1.000000000000000000, 0.8660254037844387076, 1.000000000000000000, 0.8660254037844387076, 1.000000000000000000, 0.8660254037844387076, 1.000000000000000000, 0.8660254037844387076, 1.000000000000000000, 0.8660254037844387076, 1.000000000000000000, 0.8660254037844387076, 1.000000000000000000, 0.8660254037844387076, 1.000000000000000000, 0.8660254037844387076, 1.000000000000000000, 0.8660254037844387076, 1.000000000000000000, 0.8660254037844387076, 1.000000000000000000, 0.8660254037844387076, 1.000000000000000000, 0.8660254037844387076, 1.000000000000000000, 0.8660254037844387076, 1.000000000000000000, 0.8660254037844387076, 1.000000000000000000, 0.8660254037844387076, 1.000000000000000000, 0.8660254037844387076, 1.000000000000000000, 0.8660254037844387076, 1.000000000000000000, 0.8660254037844387076, 1.000000000000000000, 0.8660254037844387076, 1.000000000000000000, 0.8660254037844387076, 1.000000000000000000, 0.8660254037844387076, 1.000000000000000000, 0.8660254037844387076, 1.000000000000000000, 0.8660254037844387076, 1.000000000000000000, 0.8660254037844387076, 1.000000000000000000, 0.8660254037844387076, 1.000000000000000000, 0.8660254037844387076, 1.000000000000000000, 0.8660254037844387076, 1.000000000000000000, 0.8660254037844387076, 1.000000000000000000, 0.8660254037844387076, 1.000000000000000000, 0.8660254037844387076, 1.000000000000000000, 0.8660254037844387076, 1.000000000000000000, 0.8660254037844387076, 1.000000000000000000, 0.8660254037844387076, 1.000000000000000000, 0.8660254037844387076, 1.000000000000000000, 0.8660254037844387076, 1.000000000000000000, 0.8660254037844387076, 1.000000000000000000, 0.8660254037844387076, 1.000000000000000000, 0.8660254037844387076, 1.000000000000000000, 0.8660254037844387076, 1.000000000000000000, 0.8660254037844387076, 1.000000000000000000, 0.8660254037844387076, 1.000000000000000000, 0.8660254037844387076, 1.000000000000000000, 0.8660254037844387076, 1.000000000000000000, 0.8660254037844387076, 1.000000000000000000, 0.8660254037844387076, 1.000000000000000000, 0.8660254037844387076, 1.000000000000000000, 0.8660254037844387076, 1.000000000000000000, 0.8660254037844387076, 1.000000000000000000, 0.8660254037844387076, 1.000000000000000000, 0.8660254037844387076, 1.000000000000000000, 0.8660254037844387076, 1.000000000000000000, 0.8660254037844387076, 1.000000000000000000, 0.8660254037844387076, 1.000000000000000000, 0.8660254037844387076, 1.000000000000000000, 0.8660254037844387076, 1.000000000000000000, 0.8660254037844387076, 1.000000000000000000, 0.8660254037844387076, 1.000000000000000000, 0.8660254037844387076, 1.000000000000000000, 0.8660254037844387076, 1.000000000000000000, 0.8660254037844387076, 1.000000000000000000, 0.8660254037844387076, 1.000000000000000000, 0.8660254037844387076, 1.000000000000000000, 0.8660254037844387076, 1.000000000000000000, 0.8660254037844387076, 1.000000000000000000, 0.8660254037844387076, 1.000000000000000000, 0.8660254037844387076, 1.000000000000000000, 0.8660254037844387076, 1.000000000000000000, 0.8660254037844387076, 1.000000000000000000, 0.8660254037844387076, 1.000000000000000000, 0.8660254037844387076, 1.000000000000000000, 0.8660254037844387076, 1.000000000000000000, 0.8660254037844387076, 1.000000000000000000, 0.8660254037844387076, 1.000000000000000000, 0.8660254037844387076, 1.000000000000000000, 0.8660254037844387076, 1.000000000000000000, 0.8660254037844387076, 1.000000000000000000, 0.8660254037844387076, 1.000000000000000000, 0.8660254037844387076, 1.000000000000000000, 0.8660254037844387076, 1.000000000000000000, 0.8660254037844387076, 1.000000000000000000, 0.8660254037844387076, 1.000000000000000000, 0.8660254037844387076, 1.000000000000000000, 0.8660254037844387076, 1.000000000000000000, 0.8660254037844387076, 1.000000000000000000, 0.8660254037844387076, 1.000000000000000000, 0.8660254037844387076, 1.000000000000000000, 0.8660254037844387076, 1.000000000000000000, 0.8660254037844387076, 1.000000000000000000, 0.8660254037844387076, 1.000000000000000000, 0.8660254037844387076, 1.000000000000000000, 0.8660254037844387076, 1.000000000000000000, 0.8660254037844387076, 1.000000000000000000, 0.8660254037844387076, 1.000000000000000000, 0.8660254037844387076, 1.000000000000000000, 0.8660254037844387076, 1.000000000000000000, 0.8660254037844387076, 1.000000000000000000, 0.8660254037844387076, 1.000000000000000000, 0.8660254037844387076, 1.000000000000000000, 0.8660254037844387076, 1.000000000000000000, 0.8660254037844387076, 1.000000000000000000, 0.8660254037844387076, 1.000000000000000000, 0.8660254037844387076, 1.000000000000000000, 0.8660254037844387076, 1.000000000000000000, 0.8660254037844387076, 1.000000000000000000, 0.8660254037844387076, 1.000000000000000000, 0.8660254037844387076, 1.000000000000000000, 0.8660254037844387076, 1.000000000000000000, 0.8660254037844387076, 1.000000000000000000, 0.8660254037844387076, 1.000000000000000000, 0.8660254037844387076, 1.000000000000000000, 0.8660254037844387076, 1.000000000000000000, 0.8660254037844387076, 1.000000000000000000, 0.8660254037844387076, 1.000000000000000000, 0.8660254037844387076, 1.000000000000000000, 0.8660254037844387076, 1.000000000000000000, 0.8660254037844387076, 1.000000000000000000, 0.8660254037844387076, 1.000000000000000000, 0.8660254037844387076, 1.000000000000000000, 0.8660254037844387076, 1.000000000000000000, 0.8660254037844387076, 1.000000000000000000, 0.8660254037844387076, 1.000000000000000000, 0.8660254037844387076, 1.000000000000000000, 0.8660254037844387076, 1.000000000000000000, 0.8660254037844387076, 1.000000000000000000, 0.8660254037844387076, 1.000000000000000000, 0.8660254037844387076, 1.000000000000000000, 0.8660254037844387076, 1.000000000000000000, 0.8660254037844387076, 1.000000000000000000, 0.8660254037844387076, 1.000000000000000000, 0.8660254037844387076, 1.000000000000000000, 0.8660254037844387076, 1.000000000000000000, 0.8660254037844387076, 1.000000000000000000, 0.8660254037844387076, 1.000000000000000000, 0.8660254037844387076, 1.000000000000000000, 0.8660254037844387076, 1.000000000000000000, 0.8660254037844387076, 1.000000000000000000, 0.8660254037844387076, 1.000000000000000000, 0.8660254037844387076, 1.000000000000000000, 0.8660254037844387076, 1.000000000000000000, 0.8660254037844387076, 1.000000000000000000, 0.8660254037844387076, 1.000000000000000000, 0.8660254037844387076, 1.000000000000000000, 0.8660254037844387076, 1.000000000000000000, 0.8660254037844387076, 1.000000000000000000, 0.8660254037844387076, 1.000000000000000000, 0.8660254037844387076, 1.000000000000000000, 0.8660254037844387076, 1.000000000000000000, 0.8660254037844387076, 1.000000000000000000, 0.8660254037844387076, 1.000000000000000000, 0.8660254037844387076, 1.000000000000000000, 0.8660254037844387076, 1.000000000000000000, 0.8660254037844387076, 1.000000000000000000, 0.8660254037844387076, 1.000000000000000000, 0.8660254037844387076, 1.000000000000000000, 0.8660254037844387076, 1.000000000000000000, 0.8660254037844387076, 1.000000000000000000, 0.8660254037844387076, 1.000000000000000000, 0.8660254037844387076, 1.000000000000000000, 0.8660254037844387076, 1.000000000000000000, 0.8660254037844387076, 1.000000000000000000, 0.8660254037844387076, 1.000000000000000000, 0.8660254037844387076, 1.000000000000000000, 0.8660254037844387076, 1.000000000000000000, 0.8660254037844387076, 1.000000000000000000, 0.8660254037844387076, 1.000000000000000000, 0.8660254037844387076, 1.000000000000000000, 0.8660254037844387076, 1.000000000000000000, 0.8660254037844387076, 1.000000000000000000, 0.8660254037844387076, 1.000000000000000000, 0.8660254037844387076, 1.000000000000000000, 0.8660254037844387076, 1.000000000000000000, 0.8660254037844387076, 1.000000000000000000, 0.8660254037844387076, 1.000000000000000000, 0.8660254037844387076, 1.000000000000000000, 0.8660254037844387076, 1.000000000000000000, 0.8660254037844387076, 1.000000000000000000, 0.8660254037844387076, 1.000000000000000000, 0.8660254037844387076, 1.000000000000000000, 0.8660254037844387076, 1.000000000000000000, 0.8660254037844387076, 1.000000000000000000, 0.8660254037844387076, 1.000000000000000000, 0.8660254037844387076, 1.000000000000000000, 0.8660254037844387076, 1.000000000000000000, 0.8660254037844387076, 1.000000000000000000, 0.8660254037844387076, 1.000000000000000000, 0.8660254037844387076, 1.000000000000000000, 0.8660254037844387076, 1.000000000000000000, 0.8660254037844387076, 1.000000000000000000, 0.8660254037844387076, 1.000000000000000000, 0.8660254037844387076, 1.000000000000000000, 0.8660254037844387076, 1.000000000000000000, 0.8660254037844387076, 1.000000000000000000, 0.8660254037844387076, 1.000000000000000000, 0.8660254037844387076, 1.000000000000000000, 0.8660254037844387076, 1.000000000000000000, 0.8660254037844387076, 1.000000000000000000, 0.8660254037844387076, 1.000000000000000000, 0.8660254037844387076, 1.000000000000000000, 0.8660254037844387076, 1.000000000000000000, 0.8660254037844387076, 1.000000000000000000, 0.8660254037844387076, 1.000000000000000000, 0.8660254037844387076, 1.000000000000000000, 0.8660254037844387076, 1.000000000000000000, 0.8660254037844387076, 1.000000000000000000, 0.8660254037844387076, 1.000000000000000000, 0.8660254037844387076, 1.000000000000000000, 0.8660254037844387076, 1.000000000000000000, 0.8660254037844387076, 1.000000000000000000, 0.8660254037844387076, 1.000000000000000000, 0.8660254037844387076, 1.000000000000000000, 0.8660254037844387076, 1.000000000000000000, 0.8660254037844387076, 1.000000000000000000, 0.8660254037844387076, 1.000000000000000000, 0.8660254037844387076, 1.000000000000000000, 0.8660254037844387076, 1.000000000000000000, 0.8660254037844387076, 1.000000000000000000, 0.8660254037844387076, 1.000000000000000000, 0.8660254037844387076, 1.000000000000000000, 0.8660254037844387076, 1.000000000000000000, 0.8660254037844387076, 1.000000000000000000, 0.8660254037844387076, 1.000000000000000000, 0.8660254037844387076, 1.000000000000000000, 0.8660254037844387076, 1.000000000000000000, 0.8660254037844387076, 1.000000000000000000, 0.8660254037844387076, 1.000000000000000000, 0.8660254037844387076, 1.000000000000000000, 0.8660254037844387076, 1.000000000000000000, 0.8660254037844387076, 1.000000000000000000, 0.8660254037844387076, 1.000000000000000000, 0.8660254037844387076, 1.000000000000000000, 0.8660254037844387076, 1.000000000000000000, 0.8660254037844387076, 1.000000000000000000, 0.8660254037844387076, 1.000000000000000000, 0.8660254037844387076, 1.000000000000000000, 0.8660254037844387076, 1.000000000000000000, 0.8660254037844387076, 1.000000000000000000, 0.8660254037844387076, 1.000000000000000000, 0.8660254037844387076, 1.000000000000000000, 0.8660254037844387076, 1.000000000000000000, 0.8660254037844387076, 1.000000000000000000, 0.8660254037844387076, 1.000000000000000000, 0.8660254037844387076, 1.000000000000000000, 0.8660254037844387076, 1.000000000000000000, 0.8660254037844387076, 1.000000000000000000, 0.8660254037844387076, 1.000000000000000000, 0.8660254037844387076, 1.000000000000000000, 0.8660254037844387076, 1.000000000000000000, 0.8660254037844387076, 1.000000000000000000, 0.8660254037844387076, 1.000000000000000000, 0.8660254037844387076, 1.000000000000000000, 0.8660254037844387076, 1.000000000000000000, 0.8660254037844387076, 1.000000000000000000, 0.8660254037844387076, 1.000000000000000000, 0.8660254037844387076, 1.000000000000000000, 0.8660254037844387076, 1.000000000000000000, 0.8660254037844387076, 1.000000000000000000, 0.8660254037844387076, 1.000000000000000000, 0.8660254037844387076, 1.000000000000000000, 0.8660254037844387076, 1.000000000000000000, 0.8660254037844387076, 1.000000000000000000, 0.8660254037844387076, 1.000000000000000000, 0.8660254037844387076, 1.000000000000000000, 0.8660254037844387076, 1.000000000000000000, 0.8660254037844387076, 1.000000000000000000, 0.8660254037844387076, 1.000000000000000000, 0.8660254037844387076, 1.000000000000000000, 0.8660254037844387076, 1.000000000000000000, 0.8660254037844387076, 1.000000000000000000, 0.8660254037844387076, 1.000000000000000000, 0.8660254037844387076, 1.000000000000000000, 0.8660254037844387076, 1.000000000000000000, 0.8660254037844387076, 1.000000000000000000, 0.8660254037844387076, 1.000000000000000000, 0.8660254037844387076, 1.000000000000000000, 0.8660254037844387076, 1.000000000000000000, 0.8660254037844387076, 1.000000000000000000, 0.8660254037844387076, 1.000000000000000000, 0.8660254037844387076, 1.000000000000000000, 0.8660254037844387076, 1.000000000000000000, 0.8660254037844387076, 1.000000000000000000, 0.8660254037844387076, 1.000000000000000000, 0.8660254037844387076, 1.000000000000000000, 0.8660254037844387076, 1.000000000000000000, 0.8660254037844387076, 1.000000000000000000, 0.8660254037844387076, 1.000000000000000000, 0.8660254037844387076, 1.000000000000000000, 0.8660254037844387076, 1.000000000000000000, 0.8660254037844387076, 1.000000000000000000, 0.8660254037844387076, 1.000000000000000000, 0.8660254037844387076, 1.000000000000000000, 0.8660254037844387076, 1.000000000000000000, 0.8660254037844387076, 1.000000000000000000, 0.8660254037844387076, 1.000000000000000000, 0.8660254037844387076, 1.000000000000000000, 0.8660254037844387076, 1.000000000000000000, 0.8660254037844387076, 1.000000000000000000, 0.8660254037844387076, 1.000000000000000000, 0.8660254037844387076, 1.000000000000000000, 0.8660254037844387076, 1.000000000000000000, 0.8660254037844387076, 1.000000000000000000, 0.8660254037844387076, 1.000000000000000000, 0.8660254037844387076, 1.000000000000000000, 0.8660254037844387076, 1.000000000000000000, 0.8660254037844387076, 1.000000000000000000, 0.8660254037844387076, 1.000000000000000000, 0.8660254037844387076, 1.000000000000000000, 0.8660254037844387076, 1.000000000000000000, 0.8660254037844387076, 1.000000000000000000, 0.8660254037844387076, 1.000000000000000000, 0.8660254037844387076, 1.000000000000000000, 0.8660254037844387076, 1.000000000000000000, 0.8660254037844387076, 1.000000000000000000, 0.8660254037844387076, 1.000000000000000000, 0.8660254037844387076, 1.000000000000000000, 0.8660254037844387076, 1.000000000000000000, 0.8660254037844387076, 1.000000000000000000, 0.8660254037844387076, 1.000000000000000000, 0.8660254037844387076, 1.000000000000000000, 0.8660254037844387076, 1.000000000000000000, 0.8660254037844387076, 1.000000000000000000, 0.8660254037844387076, 1.000000000000000000, 0.8660254037844387076, 1.000000000000000000, 0.8660254037844387076, 1.000000000000000000, 0.8660254037844387076, 1.000000000000000000, 0.8660254037844387076, 1.000000000000000000, 0.8660254037844387076, 1.000000000000000000, 0.8660254037844387076, 1.000000000000000000, 0.8660254037844387076, 1.000000000000000000, 0.8660254037844387076, 1.000000000000000000, 0.8660254037844387076, 1.000000000000000000, 0.8660254037844387076, 1.000000000000000000, 0.8660254037844387076, 1.000000000000000000, 0.8660254037844387076, 1.000000000000000000, 0.8660254037844387076, 1.000000000000000000, 0.8660254037844387076, 1.000000000000000000, 0.8660254037844387076, 1.000000000000000000, 0.8660254037844387076, 1.000000000000000000, 0.8660254037844387076, 1.000000000000000000, 0.8660254037844387076, 1.000000000000000000, 0.8660254037844387076, 1.000000000000000000, 0.8660254037844387076, 1.000000000000000000, 0.8660254037844387076, 1.000000000000000000, 0.8660254037844387076, 1.000000000000000000, 0.8660254037844387076, 1.000000000000000000, 0.8660254037844387076, 1.000000000000000000, 0.8660254037844387076, 1.000000000000000000, 0.8660254037844387076, 1.000000000000000000, 0.8660254037844387076, 1.000000000000000000, 0.8660254037844387076, 1.000000000000000000, 0.8660254037844387076, 1.000000000000000000, 0.8660254037844387076, 1.000000000000000000, 0.8660254037844387076, 1.000000000000000000, 0.8660254037844387076, 1.000000000000000000, 0.8660254037844387076, 1.000000000000000000, 0.8660254037844387076, 1.000000000000000000, 0.8660254037844387076, 1.000000000000000000, 0.8660254037844387076, 1.000000000000000000, 0.8660254037844387076, 1.000000000000000000, 0.8660254037844387076, 1.000000000000000000, 0.8660254037844387076, 1.000000000000000000, 0.8660254037844387076, 1.000000000000000000, 0.8660254037844387076, 1.000000000000000000, 0.8660254037844387076, 1.000000000000000000, 0.8660254037844387076, 1.000000000000000000, 0.8660254037844387076, 1.000000000000000000, 0.8660254037844387076, 1.000000000000000000, 0.8660254037844387076, 1.000000000000000000, 0.8660254037844387076, 1.000000000000000000, 0.8660254037844387076, 1.000000000000000000, 0.8660254037844387076, 1.000000000000000000, 0.8660254037844387076, 1.000000000000000000, 0.8660254037844387076, 1.000000000000000000, 0.8660254037844387076, 1.000000000000000000, 0.8660254037844387076, 1.000000000000000000, 0.8660254037844387076, 1.000000000000000000, 0.8660254037844387076, 1.000000000000000000, 0.8660254037844387076, 1.000000000000000000, 0.8660254037844387076, 1.000000000000000000, 0.8660254037844387076, 1.000000000000000000, 0.8660254037844387076, 1.000000000000000000, 0.8660254037844387076, 1.000000000000000000, 0.8660254037844387076, 1.000000000000000000, 0.8660254037844387076, 1.000000000000000000, 0.8660254037844387076, 1.000000000000000000, 0.8660254037844387076, 1.000000000000000000, 0.8660254037844387076, 1.000000000000000000, 0.8660254037844387076, 1.000000000000000000, 0.8660254037844387076, 1.000000000000000000, 0.8660254037844387076, 1.000000000000000000, 0.8660254037844387076, 1.000000000000000000, 0.8660254037844387076, 1.000000000000000000, 0.8660254037844387076, 1.000000000000000000, 0.8660254037844387076, 1.000000000000000000, 0.8660254037844387076, 1.000000000000000000, 0.8660254037844387076, 1.000000000000000000, 0.8660254037844387076, 1.000000000000000000, 0.8660254037844387076, 1.000000000000000000, 0.8660254037844387076, 1.000000000000000000, 0.8660254037844387076, 1.000000000000000000, 0.8660254037844387076, 1.000000000000000000, 0.8660254037844387076, 1.000000000000000000, 0.8660254037844387076, 1.000000000000000000, 0.8660254037844387076, 1.000000000000000000, 0.8660254037844387076, 1.000000000000000000, 0.8660254037844387076, 1.000000000000000000, 0.8660254037844387076, 1.000000000000000000, 0.8660254037844387076, 1.000000000000000000, 0.8660254037844387076, 1.000000000000000000, 0.8660254037844387076, 1.000000000000000000, 0.8660254037844387076, 1.000000000000000000, 0.8660254037844387076, 1.000000000000000000, 0.8660254037844387076, 1.000000000000000000, 0.8660254037844387076, 1.000000000000000000, 0.8660254037844387076, 1.000000000000000000, 0.8660254037844387076, 1.000000000000000000, 0.8660254037844387076, 1.000000000000000000, 0.8660254037844387076, 1.000000000000000000, 0.8660254037844387076, 1.000000000000000000, 0.8660254037844387076, 1.000000000000000000, 0.8660254037844387076, 1.000000000000000000, 0.8660254037844387076, 1.000000000000000000, 0.8660254037844387076, 1.000000000000000000, 0.8660254037844387076, 1.000000000000000000, 0.8660254037844387076, 1.000000000000000000, 0.8660254037844387076, 1.000000000000000000, 0.8660254037844387076, 1.000000000000000000, 0.8660254037844387076, 1.000000000000000000, 0.8660254037844387076, 1.000000000000000000, 0.8660254037844387076, 1.000000000000000000, 0.8660254037844387076, 1.000000000000000000, 0.8660254037844387076, 1.000000000000000000, 0.8660254037844387076, 1.000000000000000000, 0.8660254037844387076, 1.000000000000000000, 0.8660254037844387076, 1.000000000000000000, 0.8660254037844387076, 1.000000000000000000, 0.8660254037844387076, 1.000000000000000000, 0.8660254037844387076, 1.000000000000000000, 0.8660254037844387076, 1.000000000000000000, 0.8660254037844387076, 1.000000000000000000, 0.8660254037844387076, 1.000000000000000000, 0.8660254037844387076, 1.000000000000000000, 0.8660254037844387076, 1.000000000000000000, 0.8660254037844387076, 1.000000000000000000, 0.8660254037844387076, 1.000000000000000000, 0.8660254037844387076, 1.000000000000000000, 0.8660254037844387076, 1.000000000000000000, 0.8660254037844387076, 1.000000000000000000, 0.8660254037844387076, 1.000000000000000000, 0.8660254037844387076, 1.000000000000000000, 0.8660254037844387076, 1.000000000000000000, 0.8660254037844387076, 1.000000000000000000, 0.8660254037844387076, 1.000000000000000000, 0.8660254037844387076, 1.000000000000000000, 0.8660254037844387076, 1.000000000000000000, 0.8660254037844387076, 1.000000000000000000, 0.8660254037844387076, 1.000000000000000000, 0.8660254037844387076, 1.000000000000000000, 0.8660254037844387076, 1.000000000000000000, 0.8660254037844387076, 1.000000000000000000, 0.8660254037844387076, 1.000000000000000000, 0.8660254037844387076, 1.000000000000000000, 0.8660254037844387076, 1.000000000000000000, 0.8660254037844387076, 1.000000000000000000, 0.8660254037844387076, 1.000000000000000000, 0.8660254037844387076, 1.000000000000000000, 0.8660254037844387076, 1.000000000000000000, 0.8660254037844387076, 1.000000000000000000, 0.8660254037844387076, 1.000000000000000000, 0.8660254037844387076, 1.000000000000000000, 0.8660254037844387076, 1.000000000000000000, 0.8660254037844387076, 1.000000000000000000, 0.8660254037844387076, 1.000000000000000000, 0.8660254037844387076, 1.000000000000000000, 0.8660254037844387076, 1.000000000000000000, 0.8660254037844387076, 1.000000000000000000, 0.8660254037844387076, 1.000000000000000000, 0.8660254037844387076, 1.000000000000000000, 0.8660254037844387076, 1.000000000000000000, 0.8660254037844387076, 1.000000000000000000, 0.8660254037844387076, 1.000000000000000000, 0.8660254037844387076, 1.000000000000000000, 0.8660254037844387076, 1.000000000000000000, 0.8660254037844387076, 1.000000000000000000, 0.8660254037844387076, 1.000000000000000000, 0.8660254037844387076, 1.000000000000000000, 0.8660254037844387076, 1.000000000000000000, 0.8660254037844387076, 1.000000000000000000, 0.8660254037844387076, 1.000000000000000000, 0.8660254037844387076, 1.000000000000000000, 0.8660254037844387076, 1.000000000000000000, 0.8660254037844387076, 1.000000000000000000, 0.8660254037844387076, 1.000000000000000000, 0.8660254037844387076, 1.000000000000000000, 0.8660254037844387076, 1.000000000000000000, 0.8660254037844387076, 1.000000000000000000, 0.8660254037844387076, 1.000000000000000000, 0.8660254037844387076, 1.000000000000000000, 0.8660254037844387076, 1.000000000000000000, 0.8660254037844387076, 1.000000000000000000, 0.8660254037844387076, 1.000000000000000000, 0.8660254037844387076, 1.000000000000000000, 0.8660254037844387076, 1.000000000000000000, 0.8660254037844387076, 1.000000000000000000, 0.8660254037844387076, 1.000000000000000000, 0.8660254037844387076, 1.000000000000000000, 0.8660254037844387076, 1.000000000000000000, 0.8660254037844387076, 1.000000000000000000, 0.8660254037844387076, 1.000000000000000000, 0.8660254037844387076, 1.000000000000000000, 0.8660254037844387076, 1.000000000000000000, 0.8660254037844387076, 1.000000000000000000, 0.8660254037844387076, 1.000000000000000000, 0.8660254037844387076, 1.000000000000000000, 0.8660254037844387076, 1.000000000000000000, 0.8660254037844387076, 1.000000000000000000, 0.8660254037844387076, 1.000000000000000000, 0.8660254037844387076, 1.000000000000000000, 0.8660254037844387076, 1.000000000000000000, 0.8660254037844387076, 1.000000000000000000, 0.8660254037844387076, 1.000000000000000000, 0.8660254037844387076, 1.000000000000000000, 0.8660254037844387076, 1.000000000000000000, 0.8660254037844387076, 1.000000000000000000, 0.8660254037844387076, 1.000000000000000000, 0.8660254037844387076, 1.000000000000000000, 0.8660254037844387076, 1.000000000000000000, 0.8660254037844387076, 1.000000000000000000, 0.8660254037844387076, 1.000000000000000000, 0.8660254037844387076, 1.000000000000000000, 0.8660254037844387076, 1.000000000000000000, 0.8660254037844387076, 1.000000000000000000, 0.8660254037844387076, 1.000000000000000000, 0.8660254037844387076, 1.000000000000000000, 0.8660254037844387076, 1.000000000000000000, 0.8660254037844387076, 1.000000000000000000, 0.8660254037844387076, 1.000000000000000000, 0.8660254037844387076, 1.000000000000000000, 0.8660254037844387076, 1.000000000000000000, 0.8660254037844387076, 1.000000000000000000, 0.8660254037844387076, 1.000000000000000000, 0.8660254037844387076, 1.000000000000000000, 0.8660254037844387076, 1.000000000000000000, 0.8660254037844387076, 1.000000000000000000, 0.8660254037844387076, 1.000000000000000000, 0.8660254037844387076, 1.000000000000000000, 0.8660254037844387076, 1.000000000000000000, 0.8660254037844387076, 1.000000000000000000, 0.8660254037844387076, 1.000000000000000000 ) ) 
 REPRESENTATION_ITEM ( '' )  );
#20434 = CARTESIAN_POINT ( 'NONE',  ( 3.044556291839386294E-14, 17.75000000000000355, -5.000000000000000000 ) ) ;
#20435 = CARTESIAN_POINT ( 'NONE',  ( -2.500000000000000444, -27.16666666666666430, -4.330127018922193649 ) ) ;
#20436 = CARTESIAN_POINT ( 'NONE',  ( 4.458734125000001214, -51.14583333196772941, 2.574251347313718519 ) ) ;
#20437 = CARTESIAN_POINT ( 'NONE',  ( 5.000000000000000000, -10.29166666393547835, -2.886751345948129988 ) ) ;
#20438 = CARTESIAN_POINT ( 'NONE',  ( -4.999999999999998224, -65.79166666393547303, 2.886751345948131764 ) ) ;
#20439 = CARTESIAN_POINT ( 'NONE',  ( 4.458734124999999437, -89.06249999863439371, -5.460374474430324690E-16 ) ) ;
#20440 = CARTESIAN_POINT ( 'NONE',  ( 6.123233995736766282E-16, -170.0000000000000000, -5.000000000000000000 ) ) ;
#20441 = CARTESIAN_POINT ( 'NONE',  ( 4.458734124999998549, -13.97916666530107221, -2.574251347313721627 ) ) ;
#20442 = ORIENTED_EDGE ( 'NONE', *, *, #47502, .T. ) ;
#20443 = CARTESIAN_POINT ( 'NONE',  ( 1.339745962155612702, 23.70534180126148271, -5.000000000000000000 ) ) ;
#20444 = CARTESIAN_POINT ( 'NONE',  ( -4.458734124999999437, -102.3124999986344079, 0.000000000000000000 ) ) ;
#20445 = CARTESIAN_POINT ( 'NONE',  ( -3.535533905932738641, -161.5000000027312126, 3.535533905932737309 ) ) ;
#20446 = ORIENTED_EDGE ( 'NONE', *, *, #45342, .T. ) ;
#20447 = CARTESIAN_POINT ( 'NONE',  ( 2.229367062500001939, -96.22916666530105090, 3.861377020970579999 ) ) ;
#20448 = DIRECTION ( 'NONE',  ( -0.000000000000000000, 1.000000000000000000, -0.000000000000000000 ) ) ;
#20449 = CARTESIAN_POINT ( 'NONE',  ( -2.500000000000000444, -58.04166666393548013, -4.330127018922193649 ) ) ;
#20450 = CARTESIAN_POINT ( 'NONE',  ( -54.64476657466781973, -126.8125000013655921, -4.444560631937228834 ) ) ;
#20451 =( BOUNDED_CURVE ( )  B_SPLINE_CURVE ( 2, ( #55885, #7944, #17269, #12122, #46223, #6997, #61978, #2186, #60714 ),
 .UNSPECIFIED., .F., .F. ) 
 B_SPLINE_CURVE_WITH_KNOTS ( ( 3, 2, 2, 2, 3 ),
 ( 0.2770833333333333481, 0.2777777777777777901, 0.2791666666666666741, 0.2805555555555555580, 0.2812500000000000000 ),
 .UNSPECIFIED. ) 
 CURVE ( )  GEOMETRIC_REPRESENTATION_ITEM ( )  RATIONAL_B_SPLINE_CURVE ( ( 0.9330127018922194093, 0.9330127018922194093, 1.000000000000000000, 0.8660254037844387076, 1.000000000000000000, 0.8660254037844387076, 1.000000000000000000, 0.9330127018922194093, 0.9330127018922194093 ) ) 
 REPRESENTATION_ITEM ( '' )  );
#20452 = CARTESIAN_POINT ( 'NONE',  ( -54.64476657466781973, -141.8125000013656063, -4.444560631937228834 ) ) ;
#20453 = EDGE_CURVE ( 'NONE', #19054, #1919, #41178, .T. ) ;
#20454 = CARTESIAN_POINT ( 'NONE',  ( -4.458734124999999437, -16.39583333196773651, -2.574251347313719407 ) ) ;
#20455 = CARTESIAN_POINT ( 'NONE',  ( -2.229367062500000163, 5.270833334698927786, -3.861377020970580443 ) ) ;
#20456 = CARTESIAN_POINT ( 'NONE',  ( 2.229367062499998831, -64.89583333196773651, -3.861377020970580887 ) ) ;
#20457 = CARTESIAN_POINT ( 'NONE',  ( -2.229367062499996610, -22.14583333196773651, 3.861377020970582219 ) ) ;
#20458 = LINE ( 'NONE', #40057, #54330 ) ;
#20459 = CARTESIAN_POINT ( 'NONE',  ( -5.000000000000000888, -155.4375000000000000, 2.071067811865474617 ) ) ;
#20460 = CARTESIAN_POINT ( 'NONE',  ( -5.000000000000000000, -11.99999999999999645, 0.000000000000000000 ) ) ;
#20461 = CARTESIAN_POINT ( 'NONE',  ( -8.190561711645485556E-16, -154.6875000013655779, 4.458734124999999437 ) ) ;
#20462 = ORIENTED_EDGE ( 'NONE', *, *, #35544, .F. ) ;
#20463 = CARTESIAN_POINT ( 'NONE',  ( -2.229367062499996610, -45.39583333196774362, 3.861377020970582219 ) ) ;
#20464 = CARTESIAN_POINT ( 'NONE',  ( 1.339745962155612702, -2.294658198738521282, -5.000000000000000000 ) ) ;
#20465 = DIRECTION ( 'NONE',  ( 0.000000000000000000, 1.000000000000000000, 0.000000000000000000 ) ) ;
#20466 = CARTESIAN_POINT ( 'NONE',  ( -2.500000000000000444, 29.83333333333333215, -4.330127018922193649 ) ) ;
#20467 = CARTESIAN_POINT ( 'NONE',  ( 4.458734125000001214, 12.10416666803226171, 2.574251347313718519 ) ) ;
#20468 = CARTESIAN_POINT ( 'NONE',  ( 2.499999999999998668, -93.33333333333332860, -4.330127018922193649 ) ) ;
#20469 = CARTESIAN_POINT ( 'NONE',  ( 2.499999999999998668, -37.20833333060213732, -4.330127018922193649 ) ) ;
#20470 = CARTESIAN_POINT ( 'NONE',  ( 1.975475456537005874E-15, -73.75000000000000000, 5.000000000000000000 ) ) ;
#20471 = CARTESIAN_POINT ( 'NONE',  ( -4.458734124999999437, 19.43750000136559208, 0.000000000000000000 ) ) ;
#20472 = CARTESIAN_POINT ( 'NONE',  ( 2.500000000000002220, -75.66666666666665719, 4.330127018922192761 ) ) ;
#20473 = CARTESIAN_POINT ( 'NONE',  ( -4.999999999999999112, 6.208333336064520758, 2.886751345948131764 ) ) ;
#20474 = ORIENTED_EDGE ( 'NONE', *, *, #2745, .T. ) ;
#20475 = CARTESIAN_POINT ( 'NONE',  ( -2.499999999999996447, 8.166666666666666075, 4.330127018922195425 ) ) ;
#20476 = ORIENTED_EDGE ( 'NONE', *, *, #10323, .F. ) ;
#20477 = VECTOR ( 'NONE', #46974, 1000.000000000000000 ) ;
#20478 = DIRECTION ( 'NONE',  ( -0.000000000000000000, 1.000000000000000000, -0.000000000000000000 ) ) ;
#20479 = CARTESIAN_POINT ( 'NONE',  ( 4.458734124999998549, -40.72916666530107221, -2.574251347313721627 ) ) ;
#20480 = VECTOR ( 'NONE', #47328, 1000.000000000000000 ) ;
#20481 = ADVANCED_FACE ( 'NONE', ( #18338 ), #22226, .F. ) ;
#20482 = CARTESIAN_POINT ( 'NONE',  ( 5.000000000000000888, -38.45833333060213732, 2.886751345948126879 ) ) ;
#20483 = EDGE_CURVE ( 'NONE', #34023, #19443, #61424, .T. ) ;
#20484 = VERTEX_POINT ( 'NONE', #57281 ) ;
#20485 = CARTESIAN_POINT ( 'NONE',  ( 4.458734124999998549, -12.72916666530107044, -2.574251347313721627 ) ) ;
#20487 = VERTEX_POINT ( 'NONE', #52127 ) ;
#20486 = CARTESIAN_POINT ( 'NONE',  ( -2.229367062499996610, -18.39583333196774007, 3.861377020970582219 ) ) ;
#20488 = EDGE_CURVE ( 'NONE', #2611, #38204, #8069, .T. ) ;
#20489 = CARTESIAN_POINT ( 'NONE',  ( 2.500000000000002220, -80.66666666666665719, 4.330127018922192761 ) ) ;
#20490 = CARTESIAN_POINT ( 'NONE',  ( 1.846868145590736310, -166.6250000013656063, 4.458734124999999437 ) ) ;
#20491 = CARTESIAN_POINT ( 'NONE',  ( 9.457646018065525792E-16, -60.31249999863440792, 5.148502694627439702 ) ) ;
#20492 = CARTESIAN_POINT ( 'NONE',  ( -2.500000000000000444, -88.04166666393548724, -4.330127018922193649 ) ) ;
#20494 = ORIENTED_EDGE ( 'NONE', *, *, #39203, .F. ) ;
#20493 = CARTESIAN_POINT ( 'NONE',  ( -4.999999999999998224, -17.91666666666666430, 2.886751345948131764 ) ) ;
#20495 = CARTESIAN_POINT ( 'NONE',  ( -50.01589407740564042, -142.6250000000000284, 0.3983568153799778022 ) ) ;
#20496 = CARTESIAN_POINT ( 'NONE',  ( -3.152548672688508926E-16, -24.81249999863440436, -5.148502694627439702 ) ) ;
#20497 = EDGE_CURVE ( 'NONE', #16762, #17838, #28526, .T. ) ;
#20498 = ORIENTED_EDGE ( 'NONE', *, *, #47180, .F. ) ;
#20499 = SHAPE_DEFINITION_REPRESENTATION ( #29149, #27855 ) ;
#20500 = CARTESIAN_POINT ( 'NONE',  ( -1.846868145590734756, -163.3750000013656347, -4.458734125000000326 ) ) ;
#20501 = ADVANCED_FACE ( 'NONE', ( #38274 ), #59336, .T. ) ;
#20502 = CARTESIAN_POINT ( 'NONE',  ( -4.458734124999999437, -108.6458333319677365, -2.574251347313719407 ) ) ;
#20503 = CARTESIAN_POINT ( 'NONE',  ( 5.000000000000000000, -156.0000000000000000, 0.000000000000000000 ) ) ;
#20504 = ORIENTED_EDGE ( 'NONE', *, *, #62976, .F. ) ;
#20505 = CARTESIAN_POINT ( 'NONE',  ( -59.29741812935640155, -145.8750000013655779, -2.196230717870135685 ) ) ;
#20506 = CARTESIAN_POINT ( 'NONE',  ( 4.458734125000001214, -73.14583333196773651, 2.574251347313718519 ) ) ;
#20507 = CARTESIAN_POINT ( 'NONE',  ( -59.81910112700025905, -133.3125000027312410, -2.462841084822630311 ) ) ;
#20508 = CARTESIAN_POINT ( 'NONE',  ( -2.229367062499996610, -43.14583333196773651, 3.861377020970582219 ) ) ;
#20509 = CARTESIAN_POINT ( 'NONE',  ( 3.152801135295366208, -140.8125000013655779, 3.152801135295367985 ) ) ;
#20510 =( BOUNDED_CURVE ( )  B_SPLINE_CURVE ( 2, ( #49706, #14648, #35239, #49389, #5008, #4684, #24628, #44882, #45200 ),
 .UNSPECIFIED., .F., .F. ) 
 B_SPLINE_CURVE_WITH_KNOTS ( ( 3, 2, 2, 2, 3 ),
 ( 0.1916666666666668462, 0.1958333333333334980, 0.2000000000000001776, 0.2041666666666668295, 0.2083333333333335091 ),
 .UNSPECIFIED. ) 
 CURVE ( )  GEOMETRIC_REPRESENTATION_ITEM ( )  RATIONAL_B_SPLINE_CURVE ( ( 0.9999999999999970024, 0.9238795325112897361, 1.000000000000000000, 0.9238795325112867385, 1.000000000000000000, 0.9238795325112867385, 1.000000000000000000, 0.9238795325112837409, 1.000000000000003109 ) ) 
 REPRESENTATION_ITEM ( '' )  );
#20511 = ADVANCED_FACE ( 'NONE', ( #25834 ), #45450, .T. ) ;
#20512 = CARTESIAN_POINT ( 'NONE',  ( -7.500000000000000000, -4.732323933430407692, -7.493854309896101462 ) ) ;
#20513 = CARTESIAN_POINT ( 'NONE',  ( -4.458734124999999437, -50.31249999863440792, 0.000000000000000000 ) ) ;
#20514 = CARTESIAN_POINT ( 'NONE',  ( 2.499999999999998668, 29.66666666666666430, -4.330127018922193649 ) ) ;
#20515 = CARTESIAN_POINT ( 'NONE',  ( 9.457646018065525792E-16, -16.06249999863440436, 5.148502694627439702 ) ) ;
#20516 = CARTESIAN_POINT ( 'NONE',  ( -5.000000000000000000, -99.08333333333332860, -2.886751345948128211 ) ) ;
#20517 = CARTESIAN_POINT ( 'NONE',  ( 3.061616997868383141E-16, -152.8750000027311842, -5.000000000000000000 ) ) ;
#20518 = CARTESIAN_POINT ( 'NONE',  ( 2.229367062499998831, -32.89583333196773651, -3.861377020970580887 ) ) ;
#20519 = CARTESIAN_POINT ( 'NONE',  ( -4.999999999999999112, 8.208333336064518093, 2.886751345948131764 ) ) ;
#20520 = CARTESIAN_POINT ( 'NONE',  ( 5.000000000000000888, -50.58333333333332860, 2.886751345948126879 ) ) ;
#20521 = CARTESIAN_POINT ( 'NONE',  ( -50.55543936806279248, -129.0625000013656063, 0.3552334253322060320 ) ) ;
#20522 = CARTESIAN_POINT ( 'NONE',  ( -4.458734124999999437, -76.56249999863440792, 0.000000000000000000 ) ) ;
#20523 = CARTESIAN_POINT ( 'NONE',  ( 0.000000000000000000, 0.000000000000000000, -10.00000000000000000 ) ) ;
#20524 = LINE ( 'NONE', #34996, #15142 ) ;
#20525 = FACE_OUTER_BOUND ( 'NONE', #32611, .T. ) ;
#20526 = PRODUCT_DEFINITION_FORMATION_WITH_SPECIFIED_SOURCE ( 'ANY', '', #21005, .NOT_KNOWN. ) ;
#20527 = CARTESIAN_POINT ( 'NONE',  ( -3.152548672688508926E-16, -0.8124999986344056957, -5.148502694627439702 ) ) ;
#20528 = ORIENTED_EDGE ( 'NONE', *, *, #8234, .T. ) ;
#20529 = CARTESIAN_POINT ( 'NONE',  ( -9.184850993605147944E-16, -146.2500000000000284, 5.000000000000000000 ) ) ;
#20530 = CARTESIAN_POINT ( 'NONE',  ( -2.500000000000000444, -60.16666666666665719, -4.330127018922193649 ) ) ;
#20532 = CARTESIAN_POINT ( 'NONE',  ( 9.457646018065525792E-16, -37.06249999863440792, 5.148502694627439702 ) ) ;
#20531 = CARTESIAN_POINT ( 'NONE',  ( 4.458734124999999437, -88.81249999863439371, -5.460374474430324690E-16 ) ) ;
#20533 = CARTESIAN_POINT ( 'NONE',  ( -6.972266317189433020E-16, -9.250000000000000000, -5.000000000000000000 ) ) ;
#20534 = CARTESIAN_POINT ( 'NONE',  ( 4.458734124999998549, -78.97916666530106511, -2.574251347313721627 ) ) ;
#20535 = AXIS2_PLACEMENT_3D ( 'NONE', #150, #19745, #58988 ) ;
#20536 = CARTESIAN_POINT ( 'NONE',  ( -3.152548672688508926E-16, 16.18750000136559564, -5.148502694627439702 ) ) ;
#20537 = CYLINDRICAL_SURFACE ( 'NONE', #44851, 5.000000000000000000 ) ;
#20538 = CARTESIAN_POINT ( 'NONE',  ( -50.70258187064364108, -139.1250000013656063, 2.196230717870141014 ) ) ;
#20539 = CARTESIAN_POINT ( 'NONE',  ( 2.229367062500001939, 0.02083333469892964529, 3.861377020970579999 ) ) ;
#20540 = CARTESIAN_POINT ( 'NONE',  ( -4.458734124999999437, 23.43750000136559564, 0.000000000000000000 ) ) ;
#20541 = CARTESIAN_POINT ( 'NONE',  ( -4.458734124999999437, -48.56249999863440792, 0.000000000000000000 ) ) ;
#20542 = CARTESIAN_POINT ( 'NONE',  ( -6.972266317189433020E-16, -14.24999999999999822, -5.000000000000000000 ) ) ;
#20543 = CARTESIAN_POINT ( 'NONE',  ( -3.152548672688508926E-16, -85.56249999863439371, -5.148502694627439702 ) ) ;
#20544 = CARTESIAN_POINT ( 'NONE',  ( -4.458734124999999437, -3.395833331967739177, -2.574251347313719407 ) ) ;
#20545 = VERTEX_POINT ( 'NONE', #34851 ) ;
#20546 = CARTESIAN_POINT ( 'NONE',  ( 4.458734124999999437, -31.06249999863440436, -5.460374474430324690E-16 ) ) ;
#20547 = CARTESIAN_POINT ( 'NONE',  ( -55.35523342533222291, -132.5625000013656063, 4.444560631937231499 ) ) ;
#20548 = CARTESIAN_POINT ( 'NONE',  ( -4.458734124999999437, -74.39583333196775072, -2.574251347313719407 ) ) ;
#20549 = CARTESIAN_POINT ( 'NONE',  ( -2.500000000000000444, -110.0416666639354730, -4.330127018922193649 ) ) ;
#20550 = CARTESIAN_POINT ( 'NONE',  ( 2.229367062499998831, 23.35416666803225993, -3.861377020970580887 ) ) ;
#20551 = CARTESIAN_POINT ( 'NONE',  ( -4.764381983412779477E-15, 26.37500000273118417, 5.000000000000000000 ) ) ;
#20552 = CARTESIAN_POINT ( 'NONE',  ( -4.458734124999997661, -76.47916666530105090, 2.574251347313722516 ) ) ;
#20553 = CARTESIAN_POINT ( 'NONE',  ( -3.535250795749689387E-16, -60.25000000000000000, -5.773502691896257311 ) ) ;
#20554 = CARTESIAN_POINT ( 'NONE',  ( -1.339745962155613812, -75.20534180126148271, -5.000000000000000000 ) ) ;
#20555 = CARTESIAN_POINT ( 'NONE',  ( -2.499999999999996447, 26.29166666939785202, 4.330127018922195425 ) ) ;
#20556 = ORIENTED_EDGE ( 'NONE', *, *, #54985, .F. ) ;
#20557 = CYLINDRICAL_SURFACE ( 'NONE', #56119, 5.000000000000000000 ) ;
#20558 = CARTESIAN_POINT ( 'NONE',  ( -5.000000000000000000, -99.08333333333332860, -2.886751345948128211 ) ) ;
#20559 =( BOUNDED_CURVE ( )  B_SPLINE_CURVE ( 2, ( #13408, #33028, #16973, #13714, #58092, #33963, #8578, #48124, #8892 ),
 .UNSPECIFIED., .F., .F. ) 
 B_SPLINE_CURVE_WITH_KNOTS ( ( 3, 2, 2, 2, 3 ),
 ( 0.4979166666666666741, 0.4986111111111111160, 0.5000000000000000000, 0.5013888888888888840, 0.5020833333333333259 ),
 .UNSPECIFIED. ) 
 CURVE ( )  GEOMETRIC_REPRESENTATION_ITEM ( )  RATIONAL_B_SPLINE_CURVE ( ( 0.9330127018922194093, 0.9330127018922194093, 1.000000000000000000, 0.8660254037844387076, 1.000000000000000000, 0.8660254037844387076, 1.000000000000000000, 0.9330127018922194093, 0.9330127018922194093 ) ) 
 REPRESENTATION_ITEM ( '' )  );
#20561 = CARTESIAN_POINT ( 'NONE',  ( 1.060575238724906964E-15, -18.75000000000000000, 5.773502691896257311 ) ) ;
#20560 = DIRECTION ( 'NONE',  ( 0.000000000000000000, 0.000000000000000000, 1.000000000000000000 ) ) ;
#20562 = CARTESIAN_POINT ( 'NONE',  ( 4.458734124999998549, -22.72916666530107221, -2.574251347313721627 ) ) ;
#20563 = CARTESIAN_POINT ( 'NONE',  ( -3.152548672688508926E-16, -83.56249999863440792, -5.148502694627439702 ) ) ;
#20564 = ADVANCED_FACE ( 'NONE', ( #49951 ), #21015, .F. ) ;
#20565 = CARTESIAN_POINT ( 'NONE',  ( 5.000000000000000000, -23.37499999726881228, -6.123233995736766282E-16 ) ) ;
#20567 = ORIENTED_EDGE ( 'NONE', *, *, #47530, .F. ) ;
#20566 = CARTESIAN_POINT ( 'NONE',  ( -2.229367062500000163, -50.47916666530107221, -3.861377020970580443 ) ) ;
#20568 = DIRECTION ( 'NONE',  ( 0.000000000000000000, 0.000000000000000000, 1.000000000000000000 ) ) ;
#20569 = DIRECTION ( 'NONE',  ( -0.000000000000000000, 1.000000000000000000, -0.000000000000000000 ) ) ;
#20571 = ORIENTED_EDGE ( 'NONE', *, *, #5537, .T. ) ;
#20570 = CARTESIAN_POINT ( 'NONE',  ( -4.458734124999998549, -3.479166665301069994, 2.574251347313722516 ) ) ;
#20572 = CARTESIAN_POINT ( 'NONE',  ( -56.48576386720575471, -149.7500000013656063, -4.591703134518078322 ) ) ;
#20573 = CARTESIAN_POINT ( 'NONE',  ( 5.000000000000000000, -65.41666666666665719, -2.886751345948129988 ) ) ;
#20574 = CARTESIAN_POINT ( 'NONE',  ( 3.152801135295367541, -150.5625000013655779, -3.152801135295367541 ) ) ;
#20575 = CARTESIAN_POINT ( 'NONE',  ( 4.458734124999999437, -45.06249999863440081, -5.460374474430324690E-16 ) ) ;
#20576 = CARTESIAN_POINT ( 'NONE',  ( 1.975475456537005874E-15, -15.62499999726881406, 5.000000000000000000 ) ) ;
#20577 = CARTESIAN_POINT ( 'NONE',  ( 3.061616997868383141E-16, -157.7500000000000000, -5.000000000000000000 ) ) ;
#20578 = FACE_OUTER_BOUND ( 'NONE', #32518, .T. ) ;
#20579 = AXIS2_PLACEMENT_3D ( 'NONE', #33816, #57960, #62787 ) ;
#20580 = CARTESIAN_POINT ( 'NONE',  ( -50.18089887299979068, -152.6875000000000284, 2.462841084822635640 ) ) ;
#20581 = CARTESIAN_POINT ( 'NONE',  ( 4.458734124999999437, -13.06249999863440259, -5.460374474430324690E-16 ) ) ;
#20582 = CARTESIAN_POINT ( 'NONE',  ( -4.458734124999999437, -47.64583333196775072, -2.574251347313719407 ) ) ;
#20583 = DIRECTION ( 'NONE',  ( -0.000000000000000000, 1.000000000000000000, -0.000000000000000000 ) ) ;
#20584 = CARTESIAN_POINT ( 'NONE',  ( -1.846868145590734756, -144.1250000013655779, -4.458734125000000326 ) ) ;
#20585 = CARTESIAN_POINT ( 'NONE',  ( 4.458734124999998549, -94.97916666530106511, -2.574251347313721627 ) ) ;
#20586 = LINE ( 'NONE', #60145, #36873 ) ;
#20587 = ORIENTED_EDGE ( 'NONE', *, *, #63552, .F. ) ;
#20588 = ADVANCED_FACE ( 'NONE', ( #24882 ), #35174, .T. ) ;
#20589 = CARTESIAN_POINT ( 'NONE',  ( -55.00000000000002132, -155.0000000000000284, 1.734723475976807094E-15 ) ) ;
#20590 = CARTESIAN_POINT ( 'NONE',  ( -6.972266317189433020E-16, -64.24999999999998579, -5.000000000000000000 ) ) ;
#20591 = CARTESIAN_POINT ( 'NONE',  ( -50.01589407740564042, -145.7500000027312126, 0.3983568153799778022 ) ) ;
#20592 = ADVANCED_FACE ( 'NONE', ( #5904 ), #442, .T. ) ;
#20593 = CARTESIAN_POINT ( 'NONE',  ( 2.499999999999998668, -30.33333333333332860, -4.330127018922193649 ) ) ;
#20594 = ORIENTED_EDGE ( 'NONE', *, *, #12639, .T. ) ;
#20595 = CARTESIAN_POINT ( 'NONE',  ( 4.458734125000001214, 4.104166668032260823, 2.574251347313718519 ) ) ;
#20596 = EDGE_CURVE ( 'NONE', #33989, #29077, #52285, .T. ) ;
#20597 = CARTESIAN_POINT ( 'NONE',  ( -6.972266317189433020E-16, 8.875000002731184168, -5.000000000000000000 ) ) ;
#20598 = CARTESIAN_POINT ( 'NONE',  ( -2.229367062500000163, -15.72916666530107399, -3.861377020970580443 ) ) ;
#20599 = CARTESIAN_POINT ( 'NONE',  ( -5.000000000000000000, -101.0000000000000000, 0.000000000000000000 ) ) ;
#20600 = CARTESIAN_POINT ( 'NONE',  ( 2.229367062499998831, -9.645833331967738289, -3.861377020970580887 ) ) ;
#20601 = CARTESIAN_POINT ( 'NONE',  ( 1.975475456537005874E-15, -73.62499999726878741, 5.000000000000000000 ) ) ;
#20602 = CARTESIAN_POINT ( 'NONE',  ( -4.458734124999999437, -149.0000000013656063, -1.846868145590735644 ) ) ;
#20603 = CARTESIAN_POINT ( 'NONE',  ( 9.457646018065525792E-16, 14.68750000136559564, 5.148502694627439702 ) ) ;
#20604 = ORIENTED_EDGE ( 'NONE', *, *, #19666, .F. ) ;
#20605 = DIRECTION ( 'NONE',  ( -0.000000000000000000, 1.000000000000000000, -0.000000000000000000 ) ) ;
#20606 = LINE ( 'NONE', #40210, #29812 ) ;
#20607 = CARTESIAN_POINT ( 'NONE',  ( 2.229367062499998831, -21.64583333196774007, -3.861377020970580887 ) ) ;
#20608 = LINE ( 'NONE', #59848, #32423 ) ;
#20609 = CARTESIAN_POINT ( 'NONE',  ( -53.33387254593703375, -137.8124999999999716, 5.149110718188541824 ) ) ;
#20610 = CARTESIAN_POINT ( 'NONE',  ( -53.51423613279429503, -148.2500000013656063, 4.591703134518082763 ) ) ;
#20611 = CARTESIAN_POINT ( 'NONE',  ( -5.000000000000000000, -47.95833333060214443, -2.886751345948128211 ) ) ;
#20612 = CARTESIAN_POINT ( 'NONE',  ( -6.972266317189433020E-16, -74.25000000000000000, -5.000000000000000000 ) ) ;
#20613 = CARTESIAN_POINT ( 'NONE',  ( 9.457646018065525792E-16, 14.93750000136559386, 5.148502694627439702 ) ) ;
#20614 = CYLINDRICAL_SURFACE ( 'NONE', #1778, 5.000000000000000000 ) ;
#20615 = CARTESIAN_POINT ( 'NONE',  ( -3.152548672688508926E-16, 12.43750000136559208, -5.148502694627439702 ) ) ;
#20616 = CARTESIAN_POINT ( 'NONE',  ( -2.229367062500000163, -68.47916666530107932, -3.861377020970580443 ) ) ;
#20617 = ORIENTED_EDGE ( 'NONE', *, *, #51497, .F. ) ;
#20618 =( GEOMETRIC_REPRESENTATION_CONTEXT ( 3 ) GLOBAL_UNCERTAINTY_ASSIGNED_CONTEXT ( ( #28519 ) ) GLOBAL_UNIT_ASSIGNED_CONTEXT ( ( #41093, #19327, #53740 ) ) REPRESENTATION_CONTEXT ( 'NONE', 'WORKASPACE' ) );
#20619 = CARTESIAN_POINT ( 'NONE',  ( -4.458734124999999437, -12.56249999863440259, 0.000000000000000000 ) ) ;
#20620 = CARTESIAN_POINT ( 'NONE',  ( -3.535250795749689387E-16, 2.749999999999999112, -5.773502691896257311 ) ) ;
#20621 = CARTESIAN_POINT ( 'NONE',  ( -1.846868145590737420, -162.7500000013655779, 4.458734124999999437 ) ) ;
#20622 = LINE ( 'NONE', #36359, #41820 ) ;
#20623 = AXIS2_PLACEMENT_3D ( 'NONE', #52825, #49256, #64 ) ;
#20624 = CARTESIAN_POINT ( 'NONE',  ( 2.229367062499998831, -56.64583333196773651, -3.861377020970580887 ) ) ;
#20625 = CARTESIAN_POINT ( 'NONE',  ( -3.535250795749689387E-16, -91.12499999726878741, -5.773502691896257311 ) ) ;
#20626 = CARTESIAN_POINT ( 'NONE',  ( -3.152548672688508926E-16, -34.56249999863440792, -5.148502694627439702 ) ) ;
#20627 = CARTESIAN_POINT ( 'NONE',  ( 0.000000000000000000, -120.0000000000000000, 0.000000000000000000 ) ) ;
#20628 = CYLINDRICAL_SURFACE ( 'NONE', #4954, 5.000000000000000000 ) ;
#20629 = DIRECTION ( 'NONE',  ( -0.000000000000000000, -0.000000000000000000, 1.000000000000000000 ) ) ;
#20630 = CARTESIAN_POINT ( 'NONE',  ( 5.000000000000000000, 1.500000000000001332, -6.123233995736766282E-16 ) ) ;
#20631 = CARTESIAN_POINT ( 'NONE',  ( 3.152801135295367541, -150.5625000013655779, -3.152801135295367541 ) ) ;
#20632 = CARTESIAN_POINT ( 'NONE',  ( -2.500000000000000444, -45.16666666666665719, -4.330127018922193649 ) ) ;
#20633 = CARTESIAN_POINT ( 'NONE',  ( 1.975475456537005874E-15, -57.62499999726880873, 5.000000000000000000 ) ) ;
#20634 = CARTESIAN_POINT ( 'NONE',  ( 5.000000000000000888, -86.45833333060213022, 2.886751345948126879 ) ) ;
#20635 = EDGE_LOOP ( 'NONE', ( #35273, #46789, #54960, #20386 ) ) ;
#20636 = CARTESIAN_POINT ( 'NONE',  ( -4.458734124999998549, -107.2291666653010509, 2.574251347313722516 ) ) ;
#20637 = CARTESIAN_POINT ( 'NONE',  ( -3.152548672688508926E-16, 3.187500001365594748, -5.148502694627439702 ) ) ;
#20638 = CARTESIAN_POINT ( 'NONE',  ( 1.975475456537005874E-15, -96.62499999726880162, 5.000000000000000000 ) ) ;
#20639 = CARTESIAN_POINT ( 'NONE',  ( -5.000000000000000000, -2.000000000000001776, 0.000000000000000000 ) ) ;
#20640 = CARTESIAN_POINT ( 'NONE',  ( 9.457646018065525792E-16, -65.06249999863440792, 5.148502694627439702 ) ) ;
#20641 =( BOUNDED_CURVE ( )  B_SPLINE_CURVE ( 2, ( #11243, #40826, #31817, #31181, #60471, #31487, #50810, #7068, #45661 ),
 .UNSPECIFIED., .F., .F. ) 
 B_SPLINE_CURVE_WITH_KNOTS ( ( 3, 2, 2, 2, 3 ),
 ( 0.6687499999999999556, 0.6694444444444443976, 0.6708333333333332815, 0.6722222222222222765, 0.6729166666666667185 ),
 .UNSPECIFIED. ) 
 CURVE ( )  GEOMETRIC_REPRESENTATION_ITEM ( )  RATIONAL_B_SPLINE_CURVE ( ( 0.9330127018922194093, 0.9330127018922194093, 1.000000000000000000, 0.8660254037844387076, 1.000000000000000000, 0.8660254037844387076, 1.000000000000000000, 0.9330127018922194093, 0.9330127018922194093 ) ) 
 REPRESENTATION_ITEM ( '' )  );
#20642 = ADVANCED_FACE ( 'NONE', ( #20049 ), #31281, .T. ) ;
#20643 = DIRECTION ( 'NONE',  ( -0.000000000000000000, 1.000000000000000000, -0.000000000000000000 ) ) ;
#20644 = CARTESIAN_POINT ( 'NONE',  ( -5.000000000000000000, -9.874999997268815832, 0.000000000000000000 ) ) ;
#20646 = VERTEX_POINT ( 'NONE', #20703 ) ;
#20645 = CARTESIAN_POINT ( 'NONE',  ( -4.458734124999998549, -34.22916666530107221, 2.574251347313722516 ) ) ;
#20647 = CARTESIAN_POINT ( 'NONE',  ( -6.972266317189433020E-16, -5.249999999999998224, -5.000000000000000000 ) ) ;
#20648 = CARTESIAN_POINT ( 'NONE',  ( 5.000000000000000000, -6.416666666666667851, -2.886751345948130876 ) ) ;
#20649 = ORIENTED_EDGE ( 'NONE', *, *, #53861, .F. ) ;
#20650 = LINE ( 'NONE', #45721, #27859 ) ;
#20651 = CARTESIAN_POINT ( 'NONE',  ( 5.000000000000000888, -52.58333333333332860, 2.886751345948126879 ) ) ;
#20653 = CARTESIAN_POINT ( 'NONE',  ( -4.458734124999998549, -31.47916666530107221, 2.574251347313722516 ) ) ;
#20652 = CARTESIAN_POINT ( 'NONE',  ( 1.975475456537005874E-15, -46.62499999726880873, 5.000000000000000000 ) ) ;
#20654 = DIRECTION ( 'NONE',  ( 0.000000000000000000, 0.000000000000000000, 1.000000000000000000 ) ) ;
#20655 = CARTESIAN_POINT ( 'NONE',  ( 2.229367062499998831, -73.64583333196773651, -3.861377020970580887 ) ) ;
#20656 = CARTESIAN_POINT ( 'NONE',  ( 4.458734125000000326, -141.6250000013656631, -1.846868145590734978 ) ) ;
#20657 = CARTESIAN_POINT ( 'NONE',  ( 4.458734124999998549, -82.72916666530106511, -2.574251347313721627 ) ) ;
#20658 = CARTESIAN_POINT ( 'NONE',  ( -55.35523342533222291, -135.5625000013656063, 4.444560631937231499 ) ) ;
#20659 = CARTESIAN_POINT ( 'NONE',  ( -4.458734124999999437, -32.56249999863440792, 0.000000000000000000 ) ) ;
#20660 = VERTEX_POINT ( 'NONE', #30010 ) ;
#20661 = FACE_OUTER_BOUND ( 'NONE', #50603, .T. ) ;
#20662 = ORIENTED_EDGE ( 'NONE', *, *, #31889, .F. ) ;
#20663 = CARTESIAN_POINT ( 'NONE',  ( 4.458734125000001214, -78.14583333196775072, 2.574251347313718519 ) ) ;
#20664 = CARTESIAN_POINT ( 'NONE',  ( -1.339745962155613812, 21.91965820146970856, -5.000000000000000000 ) ) ;
#20665 = EDGE_LOOP ( 'NONE', ( #17645, #24358, #60274, #42497 ) ) ;
#20666 = CARTESIAN_POINT ( 'NONE',  ( 0.000000000000000000, -120.0000000000000000, 5.000000000000000000 ) ) ;
#20668 = VECTOR ( 'NONE', #3080, 1000.000000000000000 ) ;
#20667 = CARTESIAN_POINT ( 'NONE',  ( -6.972266317189433020E-16, -76.12499999726880162, -5.000000000000000000 ) ) ;
#20669 = CARTESIAN_POINT ( 'NONE',  ( 2.229367062499998831, -64.89583333196773651, -3.861377020970580887 ) ) ;
#20670 = CARTESIAN_POINT ( 'NONE',  ( 9.457646018065525792E-16, -3.312499998634407472, 5.148502694627439702 ) ) ;
#20671 = VERTEX_POINT ( 'NONE', #40307 ) ;
#20672 = CARTESIAN_POINT ( 'NONE',  ( 1.975475456537005874E-15, 5.375000002731185944, 5.000000000000000000 ) ) ;
#20673 = DIRECTION ( 'NONE',  ( -0.000000000000000000, 1.000000000000000000, -0.000000000000000000 ) ) ;
#20674 = CARTESIAN_POINT ( 'NONE',  ( -2.229367062499996610, 6.854166668032259935, 3.861377020970582219 ) ) ;
#20675 = CARTESIAN_POINT ( 'NONE',  ( -52.80376928212989185, -141.8750000013655779, -4.297418129356379346 ) ) ;
#20676 = CARTESIAN_POINT ( 'NONE',  ( 5.000000000000000000, -47.29166666393547303, -2.886751345948130876 ) ) ;
#20677 = CARTESIAN_POINT ( 'NONE',  ( 4.458734124999999437, -161.3750000013656063, -1.846868145590734978 ) ) ;
#20678 = CARTESIAN_POINT ( 'NONE',  ( 0.000000000000000000, -120.0000000000000000, 0.000000000000000000 ) ) ;
#20679 = ORIENTED_EDGE ( 'NONE', *, *, #54526, .F. ) ;
#20680 = CARTESIAN_POINT ( 'NONE',  ( 4.458734124999999437, -81.81249999863440792, -5.460374474430324690E-16 ) ) ;
#20681 = DIRECTION ( 'NONE',  ( 0.000000000000000000, 0.000000000000000000, 1.000000000000000000 ) ) ;
#20682 = CARTESIAN_POINT ( 'NONE',  ( 4.458734125000001214, -1.895833331967737623, 2.574251347313718519 ) ) ;
#20683 = CARTESIAN_POINT ( 'NONE',  ( -49.85088928181150436, -147.5625000000000000, -1.666127454062680480 ) ) ;
#20684 = FACE_OUTER_BOUND ( 'NONE', #54169, .T. ) ;
#20685 = CARTESIAN_POINT ( 'NONE',  ( 4.458734124999998549, -68.97916666530106511, -2.574251347313721627 ) ) ;
#20686 = CARTESIAN_POINT ( 'NONE',  ( -2.500000000000000444, -28.04166666393548013, -4.330127018922193649 ) ) ;
#20687 = CARTESIAN_POINT ( 'NONE',  ( 5.000000000000000000, 12.70833333606451809, -2.886751345948130876 ) ) ;
#20688 = DIRECTION ( 'NONE',  ( -0.000000000000000000, 1.000000000000000000, -0.000000000000000000 ) ) ;
#20689 = CARTESIAN_POINT ( 'NONE',  ( -1.339745962155610925, -3.794658198738523058, 5.000000000000000000 ) ) ;
#20690 =( BOUNDED_CURVE ( )  B_SPLINE_CURVE ( 2, ( #25042, #44653, #614, #15400, #10560, #30171, #49802, #25364, #20551 ),
 .UNSPECIFIED., .F., .F. ) 
 B_SPLINE_CURVE_WITH_KNOTS ( ( 3, 2, 2, 2, 3 ),
 ( 0.01874999999999999931, 0.01944444444444444475, 0.02083333333333333218, 0.02222222222222222307, 0.02291666666666666852 ),
 .UNSPECIFIED. ) 
 CURVE ( )  GEOMETRIC_REPRESENTATION_ITEM ( )  RATIONAL_B_SPLINE_CURVE ( ( 0.9330127018922194093, 0.9330127018922194093, 1.000000000000000000, 0.8660254037844387076, 1.000000000000000000, 0.8660254037844387076, 1.000000000000000000, 0.9330127018922191873, 0.9330127018922194093 ) ) 
 REPRESENTATION_ITEM ( '' )  );
#20691 = CARTESIAN_POINT ( 'NONE',  ( 1.339745962155612702, -82.16965819600734733, -5.000000000000000000 ) ) ;
#20692 = CARTESIAN_POINT ( 'NONE',  ( 4.458734124999998549, -43.72916666530106511, -2.574251347313721627 ) ) ;
#20693 = CARTESIAN_POINT ( 'NONE',  ( -2.229367062500000163, -30.72916666530107221, -3.861377020970580443 ) ) ;
#20694 = CARTESIAN_POINT ( 'NONE',  ( 2.229367062499998831, -0.8958333319677401763, -3.861377020970580887 ) ) ;
#20695 = FACE_OUTER_BOUND ( 'NONE', #44106, .T. ) ;
#20696 = CARTESIAN_POINT ( 'NONE',  ( 1.060575238724906964E-15, 18.24999999999999645, 5.773502691896257311 ) ) ;
#20697 = CARTESIAN_POINT ( 'NONE',  ( -5.000000000000000888, -144.5625000027311842, 2.071067811865474617 ) ) ;
#20698 = CARTESIAN_POINT ( 'NONE',  ( -1.339745962155612480, 28.79465819873852439, -5.000000000000000888 ) ) ;
#20699 = EDGE_CURVE ( 'NONE', #33480, #55181, #59946, .T. ) ;
#20700 = CARTESIAN_POINT ( 'NONE',  ( -4.458734124999999437, -42.31249999863440081, 0.000000000000000000 ) ) ;
#20701 = CARTESIAN_POINT ( 'NONE',  ( 5.000000000000000888, -74.45833333060214443, 2.886751345948126879 ) ) ;
#20702 = CARTESIAN_POINT ( 'NONE',  ( -52.80376928212989185, -143.1250000013656063, -4.297418129356379346 ) ) ;
#20703 = CARTESIAN_POINT ( 'NONE',  ( 3.061616997868383141E-16, -161.7500000000000000, -5.000000000000000000 ) ) ;
#20704 = CARTESIAN_POINT ( 'NONE',  ( -5.000000000000000000, -5.773502691896264416, -7.063244554130003294 ) ) ;
#20705 = CARTESIAN_POINT ( 'NONE',  ( -4.458734124999999437, -79.56249999863440792, 0.000000000000000000 ) ) ;
#20706 = CARTESIAN_POINT ( 'NONE',  ( 2.730187237215162345E-16, -165.4375000013655779, -4.458734124999999437 ) ) ;
#20707 = CARTESIAN_POINT ( 'NONE',  ( -5.000000000000000000, -160.5000000000000000, -6.123233995736766282E-16 ) ) ;
#20708 = CARTESIAN_POINT ( 'NONE',  ( -5.147825380260782957, -5.688155668810408017, -7.450218641351304960 ) ) ;
#20709 = CARTESIAN_POINT ( 'NONE',  ( 5.000000000000000000, -26.41666666666666430, -2.886751345948129988 ) ) ;
#20710 = CARTESIAN_POINT ( 'NONE',  ( -8.190561711645485556E-16, -139.6875000013656063, 4.458734124999999437 ) ) ;
#20711 = ORIENTED_EDGE ( 'NONE', *, *, #41156, .F. ) ;
#20712 = CARTESIAN_POINT ( 'NONE',  ( 2.229367062500001939, 20.77083333469892779, 3.861377020970579999 ) ) ;
#20713 = ORIENTED_EDGE ( 'NONE', *, *, #22478, .F. ) ;
#20714 = CARTESIAN_POINT ( 'NONE',  ( -3.152548672688508926E-16, -64.81249999863440792, -5.148502694627439702 ) ) ;
#20715 = CARTESIAN_POINT ( 'NONE',  ( 5.000000000000000888, 21.54166666939785202, 2.886751345948126879 ) ) ;
#20716 = CARTESIAN_POINT ( 'NONE',  ( 5.000000000000000888, 2.416666666666667851, 2.886751345948126879 ) ) ;
#20717 = CARTESIAN_POINT ( 'NONE',  ( 1.060575238724906964E-15, 12.25000000000000000, 5.773502691896257311 ) ) ;
#20718 = CARTESIAN_POINT ( 'NONE',  ( 4.458734124999998549, -50.72916666530106511, -2.574251347313721627 ) ) ;
#20719 = CARTESIAN_POINT ( 'NONE',  ( 4.458734124999998549, -11.72916666530107044, -2.574251347313721627 ) ) ;
#20720 = CARTESIAN_POINT ( 'NONE',  ( 1.975475456537005874E-15, -6.749999999999999112, 5.000000000000000000 ) ) ;
#20721 = CARTESIAN_POINT ( 'NONE',  ( 2.500000000000002220, 15.45833333606451987, 4.330127018922192761 ) ) ;
#20722 = CARTESIAN_POINT ( 'NONE',  ( -1.339745962155613812, -62.20534180126146850, -5.000000000000000000 ) ) ;
#20723 = LINE ( 'NONE', #10420, #1774 ) ;
#20724 = CARTESIAN_POINT ( 'NONE',  ( -3.152548672688508926E-16, -15.81249999863440436, -5.148502694627439702 ) ) ;
#20725 = CARTESIAN_POINT ( 'NONE',  ( 1.975475456537005874E-15, -79.74999999999998579, 5.000000000000000000 ) ) ;
#20726 = CARTESIAN_POINT ( 'NONE',  ( -4.458734124999998549, -57.22916666530107932, 2.574251347313722516 ) ) ;
#20727 = CARTESIAN_POINT ( 'NONE',  ( 3.152801135295366208, -155.8125000013656063, 3.152801135295367985 ) ) ;
#20728 = CARTESIAN_POINT ( 'NONE',  ( -2.499999999999996447, -56.70833333060214443, 4.330127018922195425 ) ) ;
#20729 = ORIENTED_EDGE ( 'NONE', *, *, #19746, .T. ) ;
#20730 = DIRECTION ( 'NONE',  ( -0.000000000000000000, 1.000000000000000000, -0.000000000000000000 ) ) ;
#20731 = CARTESIAN_POINT ( 'NONE',  ( -2.229367062499996610, -0.3958333319677397322, 3.861377020970582219 ) ) ;
#20732 = ORIENTED_EDGE ( 'NONE', *, *, #61016, .F. ) ;
#20733 = CARTESIAN_POINT ( 'NONE',  ( -2.500000000000000444, -86.16666666666667140, -4.330127018922193649 ) ) ;
#20734 = CARTESIAN_POINT ( 'NONE',  ( 4.458734124999999437, -155.4375000013655779, 0.000000000000000000 ) ) ;
#20735 = ORIENTED_EDGE ( 'NONE', *, *, #61016, .T. ) ;
#20736 =( BOUNDED_CURVE ( )  B_SPLINE_CURVE ( 2, ( #8644, #57553, #46947, #37921, #3515, #38241, #13156, #8960, #53019 ),
 .UNSPECIFIED., .F., .F. ) 
 B_SPLINE_CURVE_WITH_KNOTS ( ( 3, 2, 2, 2, 3 ),
 ( 0.4553571428571428492, 0.4559523809523809423, 0.4571428571428571286, 0.4583333333333333148, 0.4589285714285714080 ),
 .UNSPECIFIED. ) 
 CURVE ( )  GEOMETRIC_REPRESENTATION_ITEM ( )  RATIONAL_B_SPLINE_CURVE ( ( 0.9330127018922194093, 0.9330127018922194093, 1.000000000000000000, 0.8660254037844387076, 1.000000000000000000, 0.8660254037844387076, 1.000000000000000000, 0.9330127018922194093, 0.9330127018922194093 ) ) 
 REPRESENTATION_ITEM ( '' )  );
#20737 = DIRECTION ( 'NONE',  ( 0.000000000000000000, 0.000000000000000000, 1.000000000000000000 ) ) ;
#20738 = CARTESIAN_POINT ( 'NONE',  ( -52.53715891517739323, -130.4375000000000284, -4.819101127000233298 ) ) ;
#20739 = CARTESIAN_POINT ( 'NONE',  ( -9.184850993605147944E-16, -153.2500000000000000, 5.000000000000000000 ) ) ;
#20740 = CARTESIAN_POINT ( 'NONE',  ( 4.458734124999998549, -48.97916666530107221, -2.574251347313721627 ) ) ;
#20741 = VERTEX_POINT ( 'NONE', #11030 ) ;
#20742 = CARTESIAN_POINT ( 'NONE',  ( -6.972266317189433020E-16, -87.12499999726880162, -5.000000000000000000 ) ) ;
#20743 = CARTESIAN_POINT ( 'NONE',  ( -4.458734124999999437, 15.60416666803225993, -2.574251347313719407 ) ) ;
#20744 = CARTESIAN_POINT ( 'NONE',  ( 2.229367062500001939, 29.02083333469892779, 3.861377020970579999 ) ) ;
#20745 = CARTESIAN_POINT ( 'NONE',  ( -58.24261429053147765, -124.3750000027312126, -3.805975901505573855 ) ) ;
#20746 = CARTESIAN_POINT ( 'NONE',  ( -3.535533905932738641, -165.3750000000000284, 3.535533905932737309 ) ) ;
#20747 = LINE ( 'NONE', #26523, #36701 ) ;
#20748 = CARTESIAN_POINT ( 'NONE',  ( 4.458734124999999437, -66.81249999863440792, -5.460374474430324690E-16 ) ) ;
#20749 = CARTESIAN_POINT ( 'NONE',  ( -2.500000000000000444, 0.8333333333333317050, -4.330127018922193649 ) ) ;
#20750 = CARTESIAN_POINT ( 'NONE',  ( 4.458734125000001214, 17.10416666803225993, 2.574251347313718519 ) ) ;
#20751 = CYLINDRICAL_SURFACE ( 'NONE', #37014, 5.000000000000000000 ) ;
#20752 = CYLINDRICAL_SURFACE ( 'NONE', #1862, 5.000000000000000000 ) ;
#20753 = CARTESIAN_POINT ( 'NONE',  ( 2.229367062499998831, -52.89583333196773651, -3.861377020970580887 ) ) ;
#20754 = CARTESIAN_POINT ( 'NONE',  ( -3.535250795749689387E-16, -11.12499999726881761, -5.773502691896257311 ) ) ;
#20755 = CARTESIAN_POINT ( 'NONE',  ( -5.000000000000000000, 24.91666666666666785, -2.886751345948128211 ) ) ;
#20756 = LINE ( 'NONE', #40362, #18337 ) ;
#20757 = CARTESIAN_POINT ( 'NONE',  ( -4.458734124999998549, -90.47916666530106511, 2.574251347313722516 ) ) ;
#20758 = LINE ( 'NONE', #60004, #43906 ) ;
#20759 = CARTESIAN_POINT ( 'NONE',  ( -2.229367062499996610, -14.39583333196774184, 3.861377020970582219 ) ) ;
#20760 = VERTEX_POINT ( 'NONE', #30654 ) ;
#20761 = CARTESIAN_POINT ( 'NONE',  ( 1.339745962155612702, -31.29465819873851373, -5.000000000000000000 ) ) ;
#20762 = CARTESIAN_POINT ( 'NONE',  ( 4.458734125000001214, -103.8958333319677365, 2.574251347313718519 ) ) ;
#20763 = CARTESIAN_POINT ( 'NONE',  ( -2.071067811865478170, -156.4375000027311842, 5.000000000000000000 ) ) ;
#20764 = VERTEX_POINT ( 'NONE', #50277 ) ;
#20765 = CARTESIAN_POINT ( 'NONE',  ( -4.458734124999999437, -96.64583333196773651, -2.574251347313719407 ) ) ;
#20766 = EDGE_CURVE ( 'NONE', #33720, #53313, #6222, .T. ) ;
#20767 = CARTESIAN_POINT ( 'NONE',  ( -2.498395430326213474E-14, 22.25000000000000000, 5.000000000000000000 ) ) ;
#20768 = CARTESIAN_POINT ( 'NONE',  ( -5.000000000000000000, -56.87499999726880162, 0.000000000000000000 ) ) ;
#20769 = CARTESIAN_POINT ( 'NONE',  ( -2.500000000000000444, -67.16666666666667140, -4.330127018922193649 ) ) ;
#20770 = CARTESIAN_POINT ( 'NONE',  ( -52.10840900171896806, -126.1875000013656063, 3.393966926194110556 ) ) ;
#20771 = CARTESIAN_POINT ( 'NONE',  ( -52.10840900171896806, -141.1875000013656063, 3.393966926194110556 ) ) ;
#20772 = CARTESIAN_POINT ( 'NONE',  ( 4.458734125000000326, -22.89583333196773651, 2.574251347313718519 ) ) ;
#20773 = CARTESIAN_POINT ( 'NONE',  ( 2.229367062499998831, 6.104166668032262599, -3.861377020970580887 ) ) ;
#20774 = CARTESIAN_POINT ( 'NONE',  ( -3.152548672688508926E-16, -62.81249999863440792, -5.148502694627439702 ) ) ;
#20775 = CARTESIAN_POINT ( 'NONE',  ( 2.499999999999998668, -94.20833333060213022, -4.330127018922193649 ) ) ;
#20776 = CARTESIAN_POINT ( 'NONE',  ( 4.458734124999998549, -17.72916666530106866, -2.574251347313721627 ) ) ;
#20777 = FACE_OUTER_BOUND ( 'NONE', #52687, .T. ) ;
#20778 = CARTESIAN_POINT ( 'NONE',  ( 5.000000000000000888, -152.9375000000000000, -2.071067811865475505 ) ) ;
#20779 = CARTESIAN_POINT ( 'NONE',  ( -2.499999999999996447, -13.83333333333333570, 4.330127018922195425 ) ) ;
#20780 = CARTESIAN_POINT ( 'NONE',  ( -4.458734125000001214, -156.8750000013655779, 1.846868145590734089 ) ) ;
#20781 = EDGE_LOOP ( 'NONE', ( #45047, #53086, #33997, #2462 ) ) ;
#20782 = CARTESIAN_POINT ( 'NONE',  ( 2.229367062499998831, -46.89583333196774362, -3.861377020970580887 ) ) ;
#20783 = CARTESIAN_POINT ( 'NONE',  ( -1.339745962155613812, -38.20534180126147561, -5.000000000000000000 ) ) ;
#20784 = CARTESIAN_POINT ( 'NONE',  ( 1.339745962155612702, -38.16965819600732601, -5.000000000000000000 ) ) ;
#20785 = CARTESIAN_POINT ( 'NONE',  ( -4.458734124999998549, -90.22916666530106511, 2.574251347313722516 ) ) ;
#20786 = CARTESIAN_POINT ( 'NONE',  ( 4.458734125000001214, 5.104166668032261711, 2.574251347313718519 ) ) ;
#20787 = EDGE_CURVE ( 'NONE', #14134, #35143, #23536, .T. ) ;
#20788 = DIRECTION ( 'NONE',  ( -0.000000000000000000, 1.000000000000000000, -0.000000000000000000 ) ) ;
#20789 = EDGE_CURVE ( 'NONE', #41833, #15263, #27730, .T. ) ;
#20790 = CYLINDRICAL_SURFACE ( 'NONE', #59461, 5.000000000000000000 ) ;
#20791 = CARTESIAN_POINT ( 'NONE',  ( 1.975475456537005874E-15, 20.37500000273118417, 5.000000000000000000 ) ) ;
#20792 = CARTESIAN_POINT ( 'NONE',  ( -4.458734124999999437, 18.35416666803225993, -2.574251347313719407 ) ) ;
#20793 = CARTESIAN_POINT ( 'NONE',  ( -5.000000000000000000, -75.00000000000000000, 0.000000000000000000 ) ) ;
#20794 = CARTESIAN_POINT ( 'NONE',  ( -5.000000000000000000, 11.04166666939785202, -2.886751345948128211 ) ) ;
#20795 = ORIENTED_EDGE ( 'NONE', *, *, #18453, .F. ) ;
#20796 = CARTESIAN_POINT ( 'NONE',  ( -1.339745962155610925, -97.79465819873851729, 5.000000000000000000 ) ) ;
#20797 = ORIENTED_EDGE ( 'NONE', *, *, #27967, .T. ) ;
#20798 = CARTESIAN_POINT ( 'NONE',  ( -5.000000000000000000, -53.95833333060214443, -2.886751345948128211 ) ) ;
#20799 = CARTESIAN_POINT ( 'NONE',  ( 4.458734124999998549, -44.72916666530106511, -2.574251347313721627 ) ) ;
#20800 = ADVANCED_FACE ( 'NONE', ( #47357 ), #32559, .T. ) ;
#20801 = CARTESIAN_POINT ( 'NONE',  ( 2.499999999999998668, -41.20833333060214443, -4.330127018922193649 ) ) ;
#20802 = EDGE_LOOP ( 'NONE', ( #40445, #17562, #36902, #55721 ) ) ;
#20803 = CARTESIAN_POINT ( 'NONE',  ( -4.458734124999999437, -17.31249999863440792, 0.000000000000000000 ) ) ;
#20804 = ORIENTED_EDGE ( 'NONE', *, *, #57825, .F. ) ;
#20805 = CARTESIAN_POINT ( 'NONE',  ( 5.000000000000000000, -80.41666666666667140, -2.886751345948129988 ) ) ;
#20806 = CARTESIAN_POINT ( 'NONE',  ( 3.152801135295366208, -167.5625000013656063, 3.152801135295367985 ) ) ;
#20807 = CARTESIAN_POINT ( 'NONE',  ( -2.500000000000000444, -86.04166666393547303, -4.330127018922193649 ) ) ;
#20809 = ORIENTED_EDGE ( 'NONE', *, *, #49475, .F. ) ;
#20808 = CARTESIAN_POINT ( 'NONE',  ( 5.000000000000000000, -55.41666666666667140, -2.886751345948130876 ) ) ;
#20810 = CARTESIAN_POINT ( 'NONE',  ( -55.39835681537999790, -139.8750000000000284, 4.984105922594378235 ) ) ;
#20811 = CARTESIAN_POINT ( 'NONE',  ( 2.229367062500001939, -28.22916666530107221, 3.861377020970579999 ) ) ;
#20812 = DIRECTION ( 'NONE',  ( -0.000000000000000000, 1.000000000000000000, -0.000000000000000000 ) ) ;
#20813 = ORIENTED_EDGE ( 'NONE', *, *, #61024, .T. ) ;
#20814 =( BOUNDED_CURVE ( )  B_SPLINE_CURVE ( 2, ( #17651, #28231, #37267, #47846, #23741, #18893, #3804, #32435, #23427 ),
 .UNSPECIFIED., .F., .F. ) 
 B_SPLINE_CURVE_WITH_KNOTS ( ( 3, 2, 2, 2, 3 ),
 ( 0.3604166666666666630, 0.3611111111111111049, 0.3624999999999999889, 0.3638888888888888729, 0.3645833333333333148 ),
 .UNSPECIFIED. ) 
 CURVE ( )  GEOMETRIC_REPRESENTATION_ITEM ( )  RATIONAL_B_SPLINE_CURVE ( ( 0.9330127018922194093, 0.9330127018922194093, 1.000000000000000000, 0.8660254037844387076, 1.000000000000000000, 0.8660254037844387076, 1.000000000000000000, 0.9330127018922194093, 0.9330127018922194093 ) ) 
 REPRESENTATION_ITEM ( '' )  );
#20815 = ITEM_DEFINED_TRANSFORMATION ( 'NONE', 'NONE', #50315,  #43054 ) ;
#20816 = CARTESIAN_POINT ( 'NONE',  ( -8.190561711645485556E-16, -163.9375000013655779, 4.458734124999999437 ) ) ;
#20817 = EDGE_CURVE ( 'NONE', #33932, #38122, #16816, .T. ) ;
#20818 = CARTESIAN_POINT ( 'NONE',  ( 4.458734124999998549, -77.72916666530106511, -2.574251347313721627 ) ) ;
#20819 = CARTESIAN_POINT ( 'NONE',  ( -4.458734124999999437, 29.68750000136559208, 0.000000000000000000 ) ) ;
#20820 = ORIENTED_EDGE ( 'NONE', *, *, #33138, .T. ) ;
#20821 = CARTESIAN_POINT ( 'NONE',  ( -5.000000000000000000, -26.00000000000000355, 0.000000000000000000 ) ) ;
#20822 = CARTESIAN_POINT ( 'NONE',  ( -59.29741812935640155, -146.8750000013656063, -2.196230717870135685 ) ) ;
#20823 = CARTESIAN_POINT ( 'NONE',  ( -3.152548672688508926E-16, -72.81249999863439371, -5.148502694627439702 ) ) ;
#20824 = CARTESIAN_POINT ( 'NONE',  ( -54.60164318462004474, -135.5000000027312126, -4.984105922594373794 ) ) ;
#20825 = CARTESIAN_POINT ( 'NONE',  ( 2.229367062500001939, -42.97916666530107932, 3.861377020970579999 ) ) ;
#20826 = CARTESIAN_POINT ( 'NONE',  ( -3.152801135295367096, -142.3125000013655779, -3.152801135295367541 ) ) ;
#20827 = CARTESIAN_POINT ( 'NONE',  ( 1.975475456537005874E-15, -57.74999999999999289, 5.000000000000000000 ) ) ;
#20828 = CARTESIAN_POINT ( 'NONE',  ( -2.229367062500000163, -47.47916666530106511, -3.861377020970580443 ) ) ;
#20829 = CARTESIAN_POINT ( 'NONE',  ( -2.229367062499996610, -48.14583333196772941, 3.861377020970582219 ) ) ;
#20830 = CARTESIAN_POINT ( 'NONE',  ( -6.031010364368858512E-14, 2.375000002731183280, 5.000000000000000000 ) ) ;
#20831 = CARTESIAN_POINT ( 'NONE',  ( 2.229367062499998831, -17.64583333196773651, -3.861377020970580887 ) ) ;
#20832 = CARTESIAN_POINT ( 'NONE',  ( -2.499999999999996447, -101.8333333333333286, 4.330127018922195425 ) ) ;
#20833 =( BOUNDED_CURVE ( )  B_SPLINE_CURVE ( 2, ( #54207, #49384, #16256, #10144, #59684, #29751, #35875, #5973, #11418 ),
 .UNSPECIFIED., .F., .F. ) 
 B_SPLINE_CURVE_WITH_KNOTS ( ( 3, 2, 2, 2, 3 ),
 ( 0.8416666666666664520, 0.8458333333333331039, 0.8499999999999997558, 0.8541666666666664076, 0.8583333333333330595 ),
 .UNSPECIFIED. ) 
 CURVE ( )  GEOMETRIC_REPRESENTATION_ITEM ( )  RATIONAL_B_SPLINE_CURVE ( ( 1.000000000000003997, 0.9238795325112826307, 1.000000000000000000, 0.9238795325112867385, 1.000000000000000000, 0.9238795325112867385, 1.000000000000000000, 0.9238795325112908463, 0.9999999999999958922 ) ) 
 REPRESENTATION_ITEM ( '' )  );
#20834 = CARTESIAN_POINT ( 'NONE',  ( -5.147856630858197489E-14, 4.249999999999996447, 5.000000000000000000 ) ) ;
#20835 = CARTESIAN_POINT ( 'NONE',  ( -3.152548672688508926E-16, -35.81249999863440792, -5.148502694627439702 ) ) ;
#20836 = CARTESIAN_POINT ( 'NONE',  ( -5.000000000000000000, 4.041666669397852019, -2.886751345948128211 ) ) ;
#20837 = CARTESIAN_POINT ( 'NONE',  ( -59.59170313451811296, -130.5000000013656063, 1.485763867205729394 ) ) ;
#20838 = CARTESIAN_POINT ( 'NONE',  ( 4.458734124999999437, -72.06249999863439371, -5.460374474430324690E-16 ) ) ;
#20839 = CARTESIAN_POINT ( 'NONE',  ( 0.000000000000000000, -170.0000000000000000, 0.000000000000000000 ) ) ;
#20840 = CARTESIAN_POINT ( 'NONE',  ( 1.975475456537005874E-15, -18.74999999999999645, 5.000000000000000000 ) ) ;
#20841 = CARTESIAN_POINT ( 'NONE',  ( -2.229367062499996610, -0.3958333319677397322, 3.861377020970582219 ) ) ;
#20842 = ORIENTED_EDGE ( 'NONE', *, *, #35105, .F. ) ;
#20843 = CARTESIAN_POINT ( 'NONE',  ( 5.000000000000000888, -145.9375000000000000, -2.071067811865475505 ) ) ;
#20844 = CARTESIAN_POINT ( 'NONE',  ( 1.339745962155618697, 23.83034180399267044, -4.999999999999998224 ) ) ;
#20846 = CARTESIAN_POINT ( 'NONE',  ( 4.458734124999998549, -34.72916666530107221, -2.574251347313721627 ) ) ;
#20845 = CARTESIAN_POINT ( 'NONE',  ( -2.229367062499996610, -86.14583333196773651, 3.861377020970582219 ) ) ;
#20847 = CARTESIAN_POINT ( 'NONE',  ( -5.000000000000000000, -167.6250000027312126, -6.123233995736766282E-16 ) ) ;
#20848 = CARTESIAN_POINT ( 'NONE',  ( 9.457646018065525792E-16, -81.31249999863440792, 5.148502694627439702 ) ) ;
#20849 = ADVANCED_FACE ( 'NONE', ( #46087 ), #13255, .T. ) ;
#20850 = CARTESIAN_POINT ( 'NONE',  ( -2.229367062500000163, 20.27083333469892779, -3.861377020970580443 ) ) ;
#20851 = CARTESIAN_POINT ( 'NONE',  ( 0.000000000000000000, -170.0000000000000000, 5.000000000000000000 ) ) ;
#20852 = CARTESIAN_POINT ( 'NONE',  ( -59.44456063193725015, -137.5625000013656063, -0.3552334253322034230 ) ) ;
#20853 = EDGE_CURVE ( 'NONE', #55791, #21047, #2259, .T. ) ;
#20854 = EDGE_CURVE ( 'NONE', #32825, #26290, #61211, .T. ) ;
#20855 = CARTESIAN_POINT ( 'NONE',  ( -3.152548672688508926E-16, -8.562499998634406140, -5.148502694627439702 ) ) ;
#20856 = CARTESIAN_POINT ( 'NONE',  ( -4.458734124999999437, 21.43750000136559208, 0.000000000000000000 ) ) ;
#20857 = CARTESIAN_POINT ( 'NONE',  ( 2.229367062499998831, -48.89583333196772941, -3.861377020970580887 ) ) ;
#20858 = CARTESIAN_POINT ( 'NONE',  ( 5.000000000000000000, -11.41666666666666607, -2.886751345948130876 ) ) ;
#20859 = CARTESIAN_POINT ( 'NONE',  ( -2.229367062499996610, -83.14583333196773651, 3.861377020970582219 ) ) ;
#20860 = CARTESIAN_POINT ( 'NONE',  ( -3.152548672688508926E-16, -2.562499998634407028, -5.148502694627439702 ) ) ;
#20861 = VERTEX_POINT ( 'NONE', #17137 ) ;
#20862 = CARTESIAN_POINT ( 'NONE',  ( 4.458734125000000326, -32.14583333196773651, 2.574251347313718519 ) ) ;
#20863 = CARTESIAN_POINT ( 'NONE',  ( -50.55543936806279248, -131.3125000013656063, 0.3552334253322060320 ) ) ;
#20864 = CARTESIAN_POINT ( 'NONE',  ( -4.458734124999999437, -77.31249999863440792, 0.000000000000000000 ) ) ;
#20865 = CARTESIAN_POINT ( 'NONE',  ( 5.000000000000000000, -109.3749999972688016, -6.123233995736766282E-16 ) ) ;
#20866 = CARTESIAN_POINT ( 'NONE',  ( 4.458734125000001214, 19.10416666803225638, 2.574251347313718519 ) ) ;
#20867 = DIRECTION ( 'NONE',  ( -0.000000000000000000, 1.000000000000000000, -0.000000000000000000 ) ) ;
#20868 = EDGE_CURVE ( 'NONE', #25022, #34977, #56065, .T. ) ;
#20869 = CARTESIAN_POINT ( 'NONE',  ( 0.000000000000000000, -170.0000000000000000, 0.000000000000000000 ) ) ;
#20870 = CARTESIAN_POINT ( 'NONE',  ( 2.229367062499998831, -79.89583333196773651, -3.861377020970580887 ) ) ;
#20871 = CARTESIAN_POINT ( 'NONE',  ( -2.499999999999996447, -57.83333333333333570, 4.330127018922195425 ) ) ;
#20872 = CARTESIAN_POINT ( 'NONE',  ( 1.975475456537005874E-15, -80.74999999999998579, 5.000000000000000000 ) ) ;
#20873 = CARTESIAN_POINT ( 'NONE',  ( 5.000000000000000888, 26.54166666939785202, 2.886751345948126879 ) ) ;
#20874 = EDGE_LOOP ( 'NONE', ( #38596, #62827, #9094, #26243 ) ) ;
#20875 = DIRECTION ( 'NONE',  ( -0.000000000000000000, 1.000000000000000000, -0.000000000000000000 ) ) ;
#20877 = CARTESIAN_POINT ( 'NONE',  ( -3.535250795749689387E-16, -18.25000000000000355, -5.773502691896257311 ) ) ;
#20876 = CARTESIAN_POINT ( 'NONE',  ( 1.975475456537005874E-15, -71.75000000000000000, 5.000000000000000000 ) ) ;
#20878 = CARTESIAN_POINT ( 'NONE',  ( -4.458734124999998549, -20.22916666530107221, 2.574251347313722516 ) ) ;
#20879 = CARTESIAN_POINT ( 'NONE',  ( 4.458734124999998549, -86.72916666530107932, -2.574251347313721627 ) ) ;
#20880 = CARTESIAN_POINT ( 'NONE',  ( 2.499999999999998668, -23.20833333060214443, -4.330127018922193649 ) ) ;
#20882 = ORIENTED_EDGE ( 'NONE', *, *, #19667, .F. ) ;
#20881 = CARTESIAN_POINT ( 'NONE',  ( -3.152548672688508926E-16, -57.56249999863439371, -5.148502694627439702 ) ) ;
#20883 = CARTESIAN_POINT ( 'NONE',  ( 2.500000000000002220, -27.66666666666666430, 4.330127018922192761 ) ) ;
#20884 = CARTESIAN_POINT ( 'NONE',  ( 1.975475456537005874E-15, -59.62499999726880873, 5.000000000000000000 ) ) ;
#20886 = ORIENTED_EDGE ( 'NONE', *, *, #29530, .F. ) ;
#20885 = CARTESIAN_POINT ( 'NONE',  ( 2.229367062500001939, -6.229166665301072214, 3.861377020970579999 ) ) ;
#20887 = CARTESIAN_POINT ( 'NONE',  ( -50.55543936806279248, -149.0625000013656063, 0.3552334253322060320 ) ) ;
#20888 = CARTESIAN_POINT ( 'NONE',  ( -4.999999999999999112, -66.91666666666667140, 2.886751345948131764 ) ) ;
#20889 = CARTESIAN_POINT ( 'NONE',  ( -4.458734125000001214, -154.1250000013656063, 1.846868145590734089 ) ) ;
#20890 = CARTESIAN_POINT ( 'NONE',  ( -2.229367062499996610, -48.39583333196772941, 3.861377020970582219 ) ) ;
#20891 = CARTESIAN_POINT ( 'NONE',  ( -5.000000000000000000, -15.87499999726881406, 0.000000000000000000 ) ) ;
#20892 =( BOUNDED_CURVE ( )  B_SPLINE_CURVE ( 2, ( #12300, #62468, #22915, #7479, #2654, #62145, #31916, #51543, #27092 ),
 .UNSPECIFIED., .F., .F. ) 
 B_SPLINE_CURVE_WITH_KNOTS ( ( 3, 2, 2, 2, 3 ),
 ( 0.2660714285714285698, 0.2666666666666666630, 0.2678571428571428492, 0.2690476190476190355, 0.2696428571428571286 ),
 .UNSPECIFIED. ) 
 CURVE ( )  GEOMETRIC_REPRESENTATION_ITEM ( )  RATIONAL_B_SPLINE_CURVE ( ( 0.9330127018922194093, 0.9330127018922194093, 1.000000000000000000, 0.8660254037844387076, 1.000000000000000000, 0.8660254037844387076, 1.000000000000000000, 0.9330127018922194093, 0.9330127018922194093 ) ) 
 REPRESENTATION_ITEM ( '' )  );
#20893 = CARTESIAN_POINT ( 'NONE',  ( -3.535533905932737309, -159.6250000000000284, -3.535533905932738197 ) ) ;
#20894 = CARTESIAN_POINT ( 'NONE',  ( -5.000000000000000000, -56.87499999726880162, 0.000000000000000000 ) ) ;
#20895 = CARTESIAN_POINT ( 'NONE',  ( -57.89159099828107458, -124.9375000013656063, -3.393966926194107447 ) ) ;
#20896 = CARTESIAN_POINT ( 'NONE',  ( -4.458734124999998549, -13.47916666530107221, 2.574251347313722516 ) ) ;
#20897 = CARTESIAN_POINT ( 'NONE',  ( -4.458734124999998549, -52.47916666530107221, 2.574251347313722516 ) ) ;
#20898 = CYLINDRICAL_SURFACE ( 'NONE', #10876, 5.000000000000000000 ) ;
#20899 = CARTESIAN_POINT ( 'NONE',  ( -8.190561711645485556E-16, -143.6875000013656063, 4.458734124999999437 ) ) ;
#20900 = CARTESIAN_POINT ( 'NONE',  ( -4.458734124999998549, -92.47916666530106511, 2.574251347313722516 ) ) ;
#20901 = LINE ( 'NONE', #25076, #49210 ) ;
#20902 = EDGE_LOOP ( 'NONE', ( #59211, #41996, #47233, #41675 ) ) ;
#20903 = CARTESIAN_POINT ( 'NONE',  ( 0.000000000000000000, -120.0000000000000000, 0.000000000000000000 ) ) ;
#20904 = CARTESIAN_POINT ( 'NONE',  ( -2.229367062499996610, 26.60416666803225993, 3.861377020970582219 ) ) ;
#20905 = CARTESIAN_POINT ( 'NONE',  ( -58.24261429053147765, -148.3750000027312126, -3.805975901505573855 ) ) ;
#20906 = CARTESIAN_POINT ( 'NONE',  ( 5.000000000000000000, -29.29166666393548013, -2.886751345948130876 ) ) ;
#20907 = EDGE_LOOP ( 'NONE', ( #7145, #25939, #45988, #56561 ) ) ;
#20908 = CARTESIAN_POINT ( 'NONE',  ( -2.229367062500000163, -4.479166665301070438, -3.861377020970580443 ) ) ;
#20909 = CARTESIAN_POINT ( 'NONE',  ( 5.000000000000000888, -1.458333330602148870, 2.886751345948126879 ) ) ;
#20910 = CARTESIAN_POINT ( 'NONE',  ( 4.458734124999999437, -16.06249999863440436, -5.460374474430324690E-16 ) ) ;
#20911 = CARTESIAN_POINT ( 'NONE',  ( 1.975475456537005874E-15, -100.6249999972688016, 5.000000000000000000 ) ) ;
#20912 = CARTESIAN_POINT ( 'NONE',  ( -4.458734124999999437, -6.312499998634403475, 0.000000000000000000 ) ) ;
#20913 = DIRECTION ( 'NONE',  ( -0.000000000000000000, 1.000000000000000000, -0.000000000000000000 ) ) ;
#20914 = CARTESIAN_POINT ( 'NONE',  ( -8.190561711645485556E-16, -148.6875000013656063, 4.458734124999999437 ) ) ;
#20915 =( BOUNDED_CURVE ( )  B_SPLINE_CURVE ( 2, ( #20316, #39917, #3077, #3392, #42293, #37794, #52275, #37475, #17550 ),
 .UNSPECIFIED., .F., .F. ) 
 B_SPLINE_CURVE_WITH_KNOTS ( ( 3, 2, 2, 2, 3 ),
 ( 0.7982142857142857650, 0.7988095238095238582, 0.8000000000000000444, 0.8011904761904762307, 0.8017857142857143238 ),
 .UNSPECIFIED. ) 
 CURVE ( )  GEOMETRIC_REPRESENTATION_ITEM ( )  RATIONAL_B_SPLINE_CURVE ( ( 0.9330127018922194093, 0.9330127018922194093, 1.000000000000000000, 0.8660254037844387076, 1.000000000000000000, 0.8660254037844387076, 1.000000000000000000, 0.9330127018922194093, 0.9330127018922194093 ) ) 
 REPRESENTATION_ITEM ( '' )  );
#20916 = CARTESIAN_POINT ( 'NONE',  ( -4.458734124999999437, 16.43750000136559564, 0.000000000000000000 ) ) ;
#20917 = VERTEX_POINT ( 'NONE', #41245 ) ;
#20918 = CARTESIAN_POINT ( 'NONE',  ( -4.999999999999998224, -62.79166666393546592, 2.886751345948131764 ) ) ;
#20919 = CARTESIAN_POINT ( 'NONE',  ( -6.972266317189433020E-16, -71.12499999726878741, -5.000000000000000000 ) ) ;
#20920 = CARTESIAN_POINT ( 'NONE',  ( -2.229367062500000163, -17.47916666530106866, -3.861377020970580443 ) ) ;
#20921 = CARTESIAN_POINT ( 'NONE',  ( 1.975475456537005874E-15, -80.74999999999998579, 5.000000000000000000 ) ) ;
#20922 = CARTESIAN_POINT ( 'NONE',  ( -4.999999999999998224, -5.916666666666666963, 2.886751345948131764 ) ) ;
#20923 = CARTESIAN_POINT ( 'NONE',  ( -52.80376928212989185, -150.8750000013656063, -4.297418129356379346 ) ) ;
#20924 = EDGE_CURVE ( 'NONE', #48046, #51146, #60892, .T. ) ;
#20925 = CARTESIAN_POINT ( 'NONE',  ( -2.500000000000000444, -49.04166666393547303, -4.330127018922193649 ) ) ;
#20926 = CARTESIAN_POINT ( 'NONE',  ( -5.000000000000000000, 21.04166666939784847, -2.886751345948128211 ) ) ;
#20927 = CARTESIAN_POINT ( 'NONE',  ( -2.229367062500000163, 15.52083333469892779, -3.861377020970580443 ) ) ;
#20928 = CARTESIAN_POINT ( 'NONE',  ( 5.000000000000000000, -35.41666666666666430, -2.886751345948130876 ) ) ;
#20929 = EDGE_CURVE ( 'NONE', #46416, #36547, #36760, .T. ) ;
#20930 = CARTESIAN_POINT ( 'NONE',  ( -4.458734124999997661, 12.77083333469892779, 2.574251347313722516 ) ) ;
#20931 = CARTESIAN_POINT ( 'NONE',  ( 2.229367062500001939, -65.97916666530106511, 3.861377020970579999 ) ) ;
#20932 = CARTESIAN_POINT ( 'NONE',  ( 4.458734124999999437, -13.06249999863440259, -5.460374474430324690E-16 ) ) ;
#20933 = EDGE_CURVE ( 'NONE', #28539, #21365, #27772, .T. ) ;
#20934 = CARTESIAN_POINT ( 'NONE',  ( -2.499999999999996447, 4.166666666666666075, 4.330127018922195425 ) ) ;
#20935 = CARTESIAN_POINT ( 'NONE',  ( 3.152801135295367541, -165.3125000013656063, -3.152801135295367541 ) ) ;
#20936 = CARTESIAN_POINT ( 'NONE',  ( -2.500000000000000444, 21.83333333333333215, -4.330127018922193649 ) ) ;
#20937 = CARTESIAN_POINT ( 'NONE',  ( 4.458734124999998549, -56.72916666530107932, -2.574251347313721627 ) ) ;
#20938 = CARTESIAN_POINT ( 'NONE',  ( -5.000000000000000000, -95.87499999726881583, 0.000000000000000000 ) ) ;
#20939 = CARTESIAN_POINT ( 'NONE',  ( 4.458734124999998549, -32.72916666530106511, -2.574251347313721627 ) ) ;
#20940 = EDGE_CURVE ( 'NONE', #5665, #15117, #61531, .T. ) ;
#20941 = EDGE_CURVE ( 'NONE', #60646, #41255, #8329, .T. ) ;
#20942 = CARTESIAN_POINT ( 'NONE',  ( -2.500000000000000444, -42.04166666393548013, -4.330127018922193649 ) ) ;
#20943 = CARTESIAN_POINT ( 'NONE',  ( -58.24261429053147765, -153.3750000027312126, -3.805975901505573855 ) ) ;
#20944 = CARTESIAN_POINT ( 'NONE',  ( -4.999999999999998224, -88.79166666393548724, 2.886751345948131764 ) ) ;
#20945 = CARTESIAN_POINT ( 'NONE',  ( -4.458734124999999437, -38.31249999863439371, 0.000000000000000000 ) ) ;
#20946 = CARTESIAN_POINT ( 'NONE',  ( -4.999999999999998224, -48.91666666666666430, 2.886751345948131764 ) ) ;
#20947 = CARTESIAN_POINT ( 'NONE',  ( 4.458734124999999437, -148.6875000013656063, 0.000000000000000000 ) ) ;
#20948 = CARTESIAN_POINT ( 'NONE',  ( -5.000000000000000000, -40.99999999999999289, 0.000000000000000000 ) ) ;
#20949 = CARTESIAN_POINT ( 'NONE',  ( 1.975475456537005874E-15, -53.74999999999999289, 5.000000000000000000 ) ) ;
#20950 = EDGE_CURVE ( 'NONE', #24283, #46979, #9679, .T. ) ;
#20951 = VERTEX_POINT ( 'NONE', #29286 ) ;
#20952 = CARTESIAN_POINT ( 'NONE',  ( -2.229367062499996610, -107.1458333319677365, 3.861377020970582219 ) ) ;
#20953 = CARTESIAN_POINT ( 'NONE',  ( 9.457646018065525792E-16, -2.312499998634407028, 5.148502694627439702 ) ) ;
#20954 = CARTESIAN_POINT ( 'NONE',  ( -6.972266317189433020E-16, -97.12499999726880162, -5.000000000000000000 ) ) ;
#20955 = ADVANCED_FACE ( 'NONE', ( #53436 ), #47975, .T. ) ;
#20956 = CARTESIAN_POINT ( 'NONE',  ( 5.000000000000000888, -3.583333333333333925, 2.886751345948126879 ) ) ;
#20957 = CARTESIAN_POINT ( 'NONE',  ( 4.458734125000000326, -67.89583333196773651, 2.574251347313718519 ) ) ;
#20958 = CARTESIAN_POINT ( 'NONE',  ( 5.000000000000000888, -22.45833333060214443, 2.886751345948126879 ) ) ;
#20959 = EDGE_CURVE ( 'NONE', #32214, #54588, #45321, .T. ) ;
#20960 = CARTESIAN_POINT ( 'NONE',  ( 2.499999999999998668, -10.20833333060214621, -4.330127018922193649 ) ) ;
#20962 = ORIENTED_EDGE ( 'NONE', *, *, #11984, .T. ) ;
#20961 = CARTESIAN_POINT ( 'NONE',  ( -4.458734124999999437, -37.31249999863440792, 0.000000000000000000 ) ) ;
#20963 = CARTESIAN_POINT ( 'NONE',  ( 0.000000000000000000, -170.0000000000000000, 0.000000000000000000 ) ) ;
#20964 = DIRECTION ( 'NONE',  ( -0.000000000000000000, 1.000000000000000000, -0.000000000000000000 ) ) ;
#20966 = ORIENTED_EDGE ( 'NONE', *, *, #57018, .T. ) ;
#20965 = CARTESIAN_POINT ( 'NONE',  ( -4.458734124999998549, 11.52083333469892779, 2.574251347313722516 ) ) ;
#20967 = DIRECTION ( 'NONE',  ( -0.000000000000000000, 1.000000000000000000, -0.000000000000000000 ) ) ;
#20968 = CARTESIAN_POINT ( 'NONE',  ( -4.999999999999999112, -52.91666666666666430, 2.886751345948131764 ) ) ;
#20969 = CARTESIAN_POINT ( 'NONE',  ( 4.458734124999998549, -32.97916666530106511, -2.574251347313721627 ) ) ;
#20970 = CARTESIAN_POINT ( 'NONE',  ( 9.457646018065525792E-16, -75.06249999863439371, 5.148502694627439702 ) ) ;
#20971 = CARTESIAN_POINT ( 'NONE',  ( -8.190561711645485556E-16, -141.9375000013656063, 4.458734124999999437 ) ) ;
#20972 = CARTESIAN_POINT ( 'NONE',  ( -4.458734124999999437, -81.39583333196773651, -2.574251347313719407 ) ) ;
#20973 = CARTESIAN_POINT ( 'NONE',  ( -52.10840900171896806, -133.4375000013656063, 3.393966926194110556 ) ) ;
#20974 = CARTESIAN_POINT ( 'NONE',  ( 9.457646018065525792E-16, -36.31249999863440792, 5.148502694627439702 ) ) ;
#20975 = VERTEX_POINT ( 'NONE', #58584 ) ;
#20976 = CARTESIAN_POINT ( 'NONE',  ( -2.500000000000000444, -83.04166666393547303, -4.330127018922193649 ) ) ;
#20977 = ORIENTED_EDGE ( 'NONE', *, *, #19667, .T. ) ;
#20978 = CARTESIAN_POINT ( 'NONE',  ( 4.458734124999998549, -76.97916666530106511, -2.574251347313721627 ) ) ;
#20979 = CARTESIAN_POINT ( 'NONE',  ( -54.06206593695552698, -135.0000000000000284, -4.368617065816306599 ) ) ;
#20980 = ORIENTED_EDGE ( 'NONE', *, *, #39621, .T. ) ;
#20981 = CARTESIAN_POINT ( 'NONE',  ( 2.500000000000002220, -16.66666666666666430, 4.330127018922192761 ) ) ;
#20982 = CARTESIAN_POINT ( 'NONE',  ( 0.000000000000000000, -120.0000000000000000, 0.000000000000000000 ) ) ;
#20983 = CARTESIAN_POINT ( 'NONE',  ( -2.229367062500000163, -64.72916666530106511, -3.861377020970580443 ) ) ;
#20984 = CARTESIAN_POINT ( 'NONE',  ( -4.458734124999999437, -4.562499998634401699, 0.000000000000000000 ) ) ;
#20985 = ORIENTED_EDGE ( 'NONE', *, *, #20421, .T. ) ;
#20986 = CARTESIAN_POINT ( 'NONE',  ( 2.500000000000002220, -62.66666666666666430, 4.330127018922192761 ) ) ;
#20987 = CARTESIAN_POINT ( 'NONE',  ( -6.972266317189433020E-16, -27.24999999999999645, -5.000000000000000000 ) ) ;
#20988 = CARTESIAN_POINT ( 'NONE',  ( 9.457646018065525792E-16, 5.937500001365592972, 5.148502694627439702 ) ) ;
#20989 = CARTESIAN_POINT ( 'NONE',  ( -50.70258187064364108, -142.1250000013656063, 2.196230717870141014 ) ) ;
#20990 = CARTESIAN_POINT ( 'NONE',  ( -1.846868145590737420, -159.7500000013656063, 4.458734124999997661 ) ) ;
#20991 = DIRECTION ( 'NONE',  ( 0.000000000000000000, 0.000000000000000000, 1.000000000000000000 ) ) ;
#20992 = ORIENTED_EDGE ( 'NONE', *, *, #18947, .T. ) ;
#20993 = CARTESIAN_POINT ( 'NONE',  ( -2.229367062499996610, -82.14583333196773651, 3.861377020970582219 ) ) ;
#20994 = CARTESIAN_POINT ( 'NONE',  ( -6.972266317189433020E-16, -17.12499999726881583, -5.000000000000000000 ) ) ;
#20995 = CARTESIAN_POINT ( 'NONE',  ( -4.458734124999999437, -4.395833331967740065, -2.574251347313719407 ) ) ;
#20996 = CARTESIAN_POINT ( 'NONE',  ( -51.75738570946856498, -147.7500000000000284, 3.805975901505576964 ) ) ;
#20997 = CARTESIAN_POINT ( 'NONE',  ( -4.999999999999998224, -67.91666666666667140, 2.886751345948131764 ) ) ;
#20998 = CARTESIAN_POINT ( 'NONE',  ( 4.458734124999998549, -70.97916666530107932, -2.574251347313721627 ) ) ;
#20999 = CARTESIAN_POINT ( 'NONE',  ( -3.535250795749689387E-16, -30.12499999726881228, -5.773502691896257311 ) ) ;
#21000 = CARTESIAN_POINT ( 'NONE',  ( -6.972266317189433020E-16, -15.25000000000000000, -5.000000000000000000 ) ) ;
#21001 = CARTESIAN_POINT ( 'NONE',  ( -6.972266317189433020E-16, -78.12499999726881583, -5.000000000000000000 ) ) ;
#21002 = CARTESIAN_POINT ( 'NONE',  ( -5.000000000000000000, -56.08333333333332860, -2.886751345948128211 ) ) ;
#21003 = CARTESIAN_POINT ( 'NONE',  ( -4.458734124999999437, 26.68750000136559564, 0.000000000000000000 ) ) ;
#21004 = CARTESIAN_POINT ( 'NONE',  ( -4.458734124999998549, -53.22916666530107932, 2.574251347313722516 ) ) ;
#21005 = PRODUCT ( 'MAS-184', 'MAS-184', '', ( #59741 ) ) ;
#21006 = CARTESIAN_POINT ( 'NONE',  ( -2.229367062500000163, -31.72916666530107577, -3.861377020970580443 ) ) ;
#21007 = CARTESIAN_POINT ( 'NONE',  ( 4.458734124999998549, 0.02083333469892617584, -2.574251347313721627 ) ) ;
#21008 = CARTESIAN_POINT ( 'NONE',  ( 2.500000000000002220, 19.33333333333333570, 4.330127018922192761 ) ) ;
#21009 = CARTESIAN_POINT ( 'NONE',  ( -3.535533905932737309, -143.7500000027311842, -3.535533905932738197 ) ) ;
#21010 = DIRECTION ( 'NONE',  ( -0.000000000000000000, 1.000000000000000000, -0.000000000000000000 ) ) ;
#21011 = CARTESIAN_POINT ( 'NONE',  ( 2.229367062499998831, -42.64583333196773651, -3.861377020970580887 ) ) ;
#21012 = CARTESIAN_POINT ( 'NONE',  ( -4.999999999999999112, -79.79166666393545881, 2.886751345948131764 ) ) ;
#21013 = CARTESIAN_POINT ( 'NONE',  ( -53.51423613279429503, -141.5000000013656063, 4.591703134518082763 ) ) ;
#21014 =( BOUNDED_CURVE ( )  B_SPLINE_CURVE ( 2, ( #15134, #44711, #674, #20283, #15463, #45682, #41800, #17372, #16733 ),
 .UNSPECIFIED., .F., .F. ) 
 B_SPLINE_CURVE_WITH_KNOTS ( ( 3, 2, 2, 2, 3 ),
 ( 0.2083333333333335091, 0.2125000000000001610, 0.2166666666666668406, 0.2208333333333335202, 0.2250000000000001998 ),
 .UNSPECIFIED. ) 
 CURVE ( )  GEOMETRIC_REPRESENTATION_ITEM ( )  RATIONAL_B_SPLINE_CURVE ( ( 0.9999999999999970024, 0.9238795325112897361, 1.000000000000000000, 0.9238795325112867385, 1.000000000000000000, 0.9238795325112867385, 1.000000000000000000, 0.9238795325112831858, 1.000000000000003553 ) ) 
 REPRESENTATION_ITEM ( '' )  );
#21015 = CYLINDRICAL_SURFACE ( 'NONE', #37017, 5.000000000000000000 ) ;
#21016 = CARTESIAN_POINT ( 'NONE',  ( -6.972266317189433020E-16, -59.12499999726880873, -5.000000000000000000 ) ) ;
#21017 = CARTESIAN_POINT ( 'NONE',  ( 2.229367062499998831, -79.89583333196773651, -3.861377020970580887 ) ) ;
#21018 = CARTESIAN_POINT ( 'NONE',  ( 1.846868145590736310, -162.8750000013655779, 4.458734124999997661 ) ) ;
#21019 = CARTESIAN_POINT ( 'NONE',  ( 1.464175926609780648E-14, 21.87500000273118062, -5.000000000000000000 ) ) ;
#21020 = CARTESIAN_POINT ( 'NONE',  ( -2.499999999999996447, -26.83333333333333570, 4.330127018922195425 ) ) ;
#21021 = CARTESIAN_POINT ( 'NONE',  ( 55.00000000000002132, 15.00000000000000000, -5.000000000000000000 ) ) ;
#21022 = VERTEX_POINT ( 'NONE', #48916 ) ;
#21023 = CARTESIAN_POINT ( 'NONE',  ( 4.458734124999998549, 25.02083333469892423, -2.574251347313721627 ) ) ;
#21024 = ORIENTED_EDGE ( 'NONE', *, *, #48019, .T. ) ;
#21025 = CARTESIAN_POINT ( 'NONE',  ( 2.229367062499998831, -60.89583333196774362, -3.861377020970580887 ) ) ;
#21026 = CARTESIAN_POINT ( 'NONE',  ( 5.000000000000000888, 23.54166666939785202, 2.886751345948126879 ) ) ;
#21027 = CARTESIAN_POINT ( 'NONE',  ( -6.972266317189433020E-16, -61.12499999726880162, -5.000000000000000000 ) ) ;
#21028 = CARTESIAN_POINT ( 'NONE',  ( -5.000000000000000000, 13.99999999999999822, 0.000000000000000000 ) ) ;
#21029 = CARTESIAN_POINT ( 'NONE',  ( -4.458734124999999437, -49.31249999863440792, 0.000000000000000000 ) ) ;
#21030 = CARTESIAN_POINT ( 'NONE',  ( 2.229367062499998831, -11.64583333196774007, -3.861377020970580887 ) ) ;
#21031 = CYLINDRICAL_SURFACE ( 'NONE', #4094, 5.000000000000000000 ) ;
#21033 = ADVANCED_FACE ( 'NONE', ( #3929 ), #23547, .T. ) ;
#21032 = AXIS2_PLACEMENT_3D ( 'NONE', #40846, #26065, #21881 ) ;
#21034 = CARTESIAN_POINT ( 'NONE',  ( 1.975475456537005874E-15, -63.62499999726880873, 5.000000000000000000 ) ) ;
#21035 = DIRECTION ( 'NONE',  ( 0.000000000000000000, 0.000000000000000000, 1.000000000000000000 ) ) ;
#21036 = CARTESIAN_POINT ( 'NONE',  ( 1.339745962155612702, -11.16965819600733667, -5.000000000000000000 ) ) ;
#21037 = CARTESIAN_POINT ( 'NONE',  ( 5.000000000000000000, -35.41666666666667140, -2.886751345948129988 ) ) ;
#21038 = DIRECTION ( 'NONE',  ( -0.000000000000000000, 1.000000000000000000, -0.000000000000000000 ) ) ;
#21040 = CARTESIAN_POINT ( 'NONE',  ( 2.229367062500001939, -14.22916666530107221, 3.861377020970579999 ) ) ;
#21039 = CARTESIAN_POINT ( 'NONE',  ( 5.000000000000000888, 21.54166666939785202, 2.886751345948126879 ) ) ;
#21041 = CARTESIAN_POINT ( 'NONE',  ( -4.999999999999998224, -31.79166666393548724, 2.886751345948131764 ) ) ;
#21042 = CARTESIAN_POINT ( 'NONE',  ( -2.229367062499996610, -61.14583333196774362, 3.861377020970582219 ) ) ;
#21043 = CARTESIAN_POINT ( 'NONE',  ( -1.846868145590734756, -153.3750000013656347, -4.458734125000000326 ) ) ;
#21044 = CARTESIAN_POINT ( 'NONE',  ( 4.458734124999998549, -65.72916666530106511, -2.574251347313721627 ) ) ;
#21045 = AXIS2_PLACEMENT_3D ( 'NONE', #36871, #12424, #36546 ) ;
#21046 = CARTESIAN_POINT ( 'NONE',  ( -2.500000000000000444, -57.04166666393548013, -4.330127018922193649 ) ) ;
#21047 = VERTEX_POINT ( 'NONE', #4241 ) ;
#21048 = CARTESIAN_POINT ( 'NONE',  ( -50.18089887299976937, -137.6875000000000284, 2.462841084822337656 ) ) ;
#21049 = ORIENTED_EDGE ( 'NONE', *, *, #54696, .T. ) ;
#21050 = CARTESIAN_POINT ( 'NONE',  ( 2.499999999999998668, -58.33333333333333570, -4.330127018922193649 ) ) ;
#21051 = CARTESIAN_POINT ( 'NONE',  ( -8.190561711645485556E-16, -152.6875000013656063, 4.458734124999999437 ) ) ;
#21052 = VERTEX_POINT ( 'NONE', #54 ) ;
#21053 = CARTESIAN_POINT ( 'NONE',  ( -2.500000000000000444, -10.16666666666666430, -4.330127018922193649 ) ) ;
#21054 = CARTESIAN_POINT ( 'NONE',  ( -56.66612745406270335, -129.3125000000000284, -5.149110718188516067 ) ) ;
#21055 = CARTESIAN_POINT ( 'NONE',  ( 3.535533905932736864, -153.1250000000000000, 3.535533905932738641 ) ) ;
#21056 = CARTESIAN_POINT ( 'NONE',  ( 2.229367062500001939, -49.22916666530107221, 3.861377020970579999 ) ) ;
#21057 = ORIENTED_EDGE ( 'NONE', *, *, #19406, .T. ) ;
#21058 = CARTESIAN_POINT ( 'NONE',  ( 5.000000000000000000, 11.50000000000000000, -6.123233995736766282E-16 ) ) ;
#21059 = CARTESIAN_POINT ( 'NONE',  ( -2.229367062499996610, 15.85416666803226171, 3.861377020970582219 ) ) ;
#21060 =( BOUNDED_CURVE ( )  B_SPLINE_CURVE ( 2, ( #43967, #8328, #63294, #28556, #62360, #19533, #38829, #39147, #13766 ),
 .UNSPECIFIED., .F., .F. ) 
 B_SPLINE_CURVE_WITH_KNOTS ( ( 3, 2, 2, 2, 3 ),
 ( 0.6982142857142856762, 0.6988095238095237693, 0.6999999999999999556, 0.7011904761904761418, 0.7017857142857142350 ),
 .UNSPECIFIED. ) 
 CURVE ( )  GEOMETRIC_REPRESENTATION_ITEM ( )  RATIONAL_B_SPLINE_CURVE ( ( 0.9330127018922194093, 0.9330127018922194093, 1.000000000000000000, 0.8660254037844387076, 1.000000000000000000, 0.8660254037844387076, 1.000000000000000000, 0.9330127018922194093, 0.9330127018922194093 ) ) 
 REPRESENTATION_ITEM ( '' )  );
#21061 = CARTESIAN_POINT ( 'NONE',  ( 4.458734124999999437, 26.18750000136559564, -5.460374474430324690E-16 ) ) ;
#21062 = CARTESIAN_POINT ( 'NONE',  ( -55.35523342533222291, -152.3125000013656063, 4.444560631937231499 ) ) ;
#21063 = DIRECTION ( 'NONE',  ( -0.000000000000000000, 1.000000000000000000, -0.000000000000000000 ) ) ;
#21064 = DIRECTION ( 'NONE',  ( -0.000000000000000000, 1.000000000000000000, -0.000000000000000000 ) ) ;
#21065 = ORIENTED_EDGE ( 'NONE', *, *, #32650, .F. ) ;
#21066 = CARTESIAN_POINT ( 'NONE',  ( -2.229367062500000163, -63.47916666530106511, -3.861377020970580443 ) ) ;
#21067 = CARTESIAN_POINT ( 'NONE',  ( 2.500000000000002220, -28.54166666393548013, 4.330127018922192761 ) ) ;
#21068 = CARTESIAN_POINT ( 'NONE',  ( 4.458734124999998549, 12.27083333469892423, -2.574251347313721627 ) ) ;
#21069 = CARTESIAN_POINT ( 'NONE',  ( 1.339745962155612702, -60.16965819600731891, -5.000000000000000000 ) ) ;
#21070 = CARTESIAN_POINT ( 'NONE',  ( -9.184850993605147944E-16, -161.3750000027311842, 5.000000000000000000 ) ) ;
#21071 = CARTESIAN_POINT ( 'NONE',  ( -2.229367062500000163, -56.72916666530107221, -3.861377020970580443 ) ) ;
#21072 = CARTESIAN_POINT ( 'NONE',  ( 5.000000000000000000, -16.29166666393548368, -2.886751345948129988 ) ) ;
#21073 = DIRECTION ( 'NONE',  ( 0.000000000000000000, 0.000000000000000000, 1.000000000000000000 ) ) ;
#21074 = CARTESIAN_POINT ( 'NONE',  ( -59.81910112700026616, -147.1874999999999716, -2.462841084822510851 ) ) ;
#21075 = CARTESIAN_POINT ( 'NONE',  ( -6.972266317189433020E-16, -10.24999999999999822, -5.000000000000000000 ) ) ;
#21076 = CARTESIAN_POINT ( 'NONE',  ( -58.80597590150559739, -154.5625000013656347, 3.242614290531460330 ) ) ;
#21077 = CARTESIAN_POINT ( 'NONE',  ( -4.458734124999999437, -15.64583333196773829, -2.574251347313719407 ) ) ;
#21078 = ORIENTED_EDGE ( 'NONE', *, *, #49227, .F. ) ;
#21079 = CARTESIAN_POINT ( 'NONE',  ( 3.061616997868383141E-16, -169.7500000000000000, -5.000000000000000000 ) ) ;
#21080 = CARTESIAN_POINT ( 'NONE',  ( 4.458734125000001214, -104.8958333319677365, 2.574251347313718519 ) ) ;
#21081 = CARTESIAN_POINT ( 'NONE',  ( 3.535533905932736864, -159.2500000027312126, 3.535533905932738641 ) ) ;
#21082 = ORIENTED_EDGE ( 'NONE', *, *, #33847, .T. ) ;
#21083 = CARTESIAN_POINT ( 'NONE',  ( -2.229367062499996610, -101.3958333319677365, 3.861377020970582219 ) ) ;
#21084 = CARTESIAN_POINT ( 'NONE',  ( -4.458734124999999437, -26.39583333196773651, -2.574251347313719407 ) ) ;
#21085 = CARTESIAN_POINT ( 'NONE',  ( 2.499999999999998668, -57.20833333060214443, -4.330127018922193649 ) ) ;
#21086 = AXIS2_PLACEMENT_3D ( 'NONE', #34544, #44524, #4652 ) ;
#21087 = CARTESIAN_POINT ( 'NONE',  ( -51.60603307380591787, -124.9375000013656063, -2.891590998281053704 ) ) ;
#21088 = CARTESIAN_POINT ( 'NONE',  ( -57.89159099828107458, -142.6875000013656063, -3.393966926194107447 ) ) ;
#21089 = CARTESIAN_POINT ( 'NONE',  ( -4.458734124999999437, -22.31249999863440436, 0.000000000000000000 ) ) ;
#21090 = CARTESIAN_POINT ( 'NONE',  ( -4.458734124999999437, -63.64583333196773651, -2.574251347313719407 ) ) ;
#21091 = CARTESIAN_POINT ( 'NONE',  ( 1.339745962155615144, 8.294658198738519062, 4.999999999999999112 ) ) ;
#21092 = CARTESIAN_POINT ( 'NONE',  ( -2.229367062500000163, -19.47916666530106866, -3.861377020970580443 ) ) ;
#21093 = CARTESIAN_POINT ( 'NONE',  ( 5.000000000000000000, -75.41666666666667140, -2.886751345948130876 ) ) ;
#21094 = CARTESIAN_POINT ( 'NONE',  ( -5.000000000000000888, -151.5625000000000568, -2.071067811865475949 ) ) ;
#21095 = CARTESIAN_POINT ( 'NONE',  ( -2.499999999999996447, -12.83333333333333570, 4.330127018922195425 ) ) ;
#21096 = CARTESIAN_POINT ( 'NONE',  ( -3.152801135295367985, -153.8125000013656063, 3.152801135295367096 ) ) ;
#21097 = VERTEX_POINT ( 'NONE', #53126 ) ;
#21098 = CARTESIAN_POINT ( 'NONE',  ( 2.229367062499998831, -43.89583333196774362, -3.861377020970580887 ) ) ;
#21099 = CARTESIAN_POINT ( 'NONE',  ( -2.500000000000000444, -38.16666666666667140, -4.330127018922193649 ) ) ;
#21100 = CARTESIAN_POINT ( 'NONE',  ( 2.229367062500001939, -88.97916666530106511, 3.861377020970579999 ) ) ;
#21101 = CARTESIAN_POINT ( 'NONE',  ( 4.458734124999998549, 5.270833334698926897, -2.574251347313721627 ) ) ;
#21102 = CARTESIAN_POINT ( 'NONE',  ( -3.535533905932737309, -142.6250000000000000, -3.535533905932738197 ) ) ;
#21103 = DIRECTION ( 'NONE',  ( -0.000000000000000000, 1.000000000000000000, -0.000000000000000000 ) ) ;
#21104 = DIRECTION ( 'NONE',  ( 0.000000000000000000, 0.000000000000000000, 1.000000000000000000 ) ) ;
#21105 = CARTESIAN_POINT ( 'NONE',  ( 2.229367062499998831, 18.10416666803225993, -3.861377020970580887 ) ) ;
#21106 = CARTESIAN_POINT ( 'NONE',  ( 5.000000000000000000, -79.41666666666665719, -2.886751345948129988 ) ) ;
#21107 = CARTESIAN_POINT ( 'NONE',  ( 2.500000000000002220, 9.458333336064519870, 4.330127018922192761 ) ) ;
#21108 = ORIENTED_EDGE ( 'NONE', *, *, #51078, .T. ) ;
#21109 = CARTESIAN_POINT ( 'NONE',  ( 1.975475456537005874E-15, -97.74999999999998579, 5.000000000000000000 ) ) ;
#21110 = ORIENTED_EDGE ( 'NONE', *, *, #40828, .T. ) ;
#21111 =( BOUNDED_CURVE ( )  B_SPLINE_CURVE ( 2, ( #56061, #31606, #22605, #38015, #57647, #33193, #13575, #62153, #12930 ),
 .UNSPECIFIED., .F., .F. ) 
 B_SPLINE_CURVE_WITH_KNOTS ( ( 3, 2, 2, 2, 3 ),
 ( 0.8687500000000000222, 0.8694444444444444642, 0.8708333333333333481, 0.8722222222222222321, 0.8729166666666666741 ),
 .UNSPECIFIED. ) 
 CURVE ( )  GEOMETRIC_REPRESENTATION_ITEM ( )  RATIONAL_B_SPLINE_CURVE ( ( 0.9330127018922194093, 0.9330127018922194093, 1.000000000000000000, 0.8660254037844387076, 1.000000000000000000, 0.8660254037844387076, 1.000000000000000000, 0.9330127018922194093, 0.9330127018922194093 ) ) 
 REPRESENTATION_ITEM ( '' )  );
#21112 = CARTESIAN_POINT ( 'NONE',  ( -4.999999999999998224, -53.79166666393548013, 2.886751345948131764 ) ) ;
#21113 = CARTESIAN_POINT ( 'NONE',  ( -3.152548672688508926E-16, -44.56249999863440081, -5.148502694627439702 ) ) ;
#21114 = CARTESIAN_POINT ( 'NONE',  ( -3.152801135295367985, -165.0625000013656063, 3.152801135295367096 ) ) ;
#21115 = CARTESIAN_POINT ( 'NONE',  ( -5.000000000000000000, -37.87499999726881583, 0.000000000000000000 ) ) ;
#21116 = ORIENTED_EDGE ( 'NONE', *, *, #9862, .F. ) ;
#21117 = CARTESIAN_POINT ( 'NONE',  ( -4.458734124999999437, -16.39583333196773651, -2.574251347313719407 ) ) ;
#21118 = VERTEX_POINT ( 'NONE', #57652 ) ;
#21119 = CARTESIAN_POINT ( 'NONE',  ( 5.000000000000000000, -88.41666666666665719, -2.886751345948129988 ) ) ;
#21120 = CARTESIAN_POINT ( 'NONE',  ( 2.730187237215162345E-16, -169.1875000013656063, -4.458734124999999437 ) ) ;
#21121 = CARTESIAN_POINT ( 'NONE',  ( -5.000000000000000000, -86.95833333060214443, -2.886751345948128211 ) ) ;
#21123 = ORIENTED_EDGE ( 'NONE', *, *, #12668, .F. ) ;
#21122 = CARTESIAN_POINT ( 'NONE',  ( -5.000000000000000000, -19.08333333333333570, -2.886751345948128211 ) ) ;
#21124 = CARTESIAN_POINT ( 'NONE',  ( -49.85088928181150436, -143.5625000000000568, -1.666127454062680702 ) ) ;
#21125 = EDGE_CURVE ( 'NONE', #29058, #37707, #9367, .T. ) ;
#21126 = CARTESIAN_POINT ( 'NONE',  ( 4.458734124999998549, -34.97916666530107221, -2.574251347313721627 ) ) ;
#21127 = CARTESIAN_POINT ( 'NONE',  ( 2.500000000000002220, -29.66666666666666785, 4.330127018922192761 ) ) ;
#21128 = VERTEX_POINT ( 'NONE', #9059 ) ;
#21129 = VECTOR ( 'NONE', #4752, 1000.000000000000000 ) ;
#21130 = CARTESIAN_POINT ( 'NONE',  ( -4.458734124999999437, -79.39583333196773651, -2.574251347313719407 ) ) ;
#21131 = CARTESIAN_POINT ( 'NONE',  ( 2.229367062499998831, -107.8958333319677365, -3.861377020970580887 ) ) ;
#21132 = CARTESIAN_POINT ( 'NONE',  ( 1.975475456537005874E-15, 20.24999999999999289, 5.000000000000000000 ) ) ;
#21133 = ORIENTED_EDGE ( 'NONE', *, *, #62637, .T. ) ;
#21134 = CARTESIAN_POINT ( 'NONE',  ( -9.184850993605147944E-16, -166.3750000027312126, 5.000000000000000000 ) ) ;
#21135 = CARTESIAN_POINT ( 'NONE',  ( -59.59170313451810586, -140.7500000013655779, 1.485763867205729394 ) ) ;
#21136 = CARTESIAN_POINT ( 'NONE',  ( -2.229367062499996610, -81.39583333196773651, 3.861377020970582219 ) ) ;
#21137 = CARTESIAN_POINT ( 'NONE',  ( -58.24261429053147765, -135.3750000027312410, -3.805975901505573855 ) ) ;
#21138 = CARTESIAN_POINT ( 'NONE',  ( -4.458734124999997661, -44.22916666530106511, 2.574251347313722516 ) ) ;
#21139 = CARTESIAN_POINT ( 'NONE',  ( -8.190561711645485556E-16, -143.9375000013656063, 4.458734124999999437 ) ) ;
#21140 = CARTESIAN_POINT ( 'NONE',  ( -5.000000000000000000, -58.08333333333333570, -2.886751345948128211 ) ) ;
#21141 = CARTESIAN_POINT ( 'NONE',  ( -3.152548672688508926E-16, -47.56249999863442213, -5.148502694627439702 ) ) ;
#21142 = CARTESIAN_POINT ( 'NONE',  ( 4.458734125000000326, -46.89583333196773651, 2.574251347313718519 ) ) ;
#21143 = CARTESIAN_POINT ( 'NONE',  ( -1.339745962155613812, 27.79465819873851729, -5.000000000000000000 ) ) ;
#21144 = CARTESIAN_POINT ( 'NONE',  ( 4.458734125000001214, -15.89583333196773651, 2.574251347313718519 ) ) ;
#21145 = CARTESIAN_POINT ( 'NONE',  ( 5.000000000000000000, -99.41666666666664298, -2.886751345948129988 ) ) ;
#21146 = EDGE_CURVE ( 'NONE', #969, #15028, #1765, .T. ) ;
#21147 = CARTESIAN_POINT ( 'NONE',  ( -8.190561711645485556E-16, -139.9375000013656063, 4.458734124999999437 ) ) ;
#21148 = CARTESIAN_POINT ( 'NONE',  ( -4.458734124999999437, -40.56249999863440081, 0.000000000000000000 ) ) ;
#21149 = CARTESIAN_POINT ( 'NONE',  ( 5.000000000000000000, 1.625000002731184834, -6.123233995736766282E-16 ) ) ;
#21150 = CARTESIAN_POINT ( 'NONE',  ( -2.499999999999996447, -6.708333330602149758, 4.330127018922195425 ) ) ;
#21151 = CARTESIAN_POINT ( 'NONE',  ( -58.39396692619412477, -129.4375000013656063, 2.891590998281057701 ) ) ;
#21152 = CARTESIAN_POINT ( 'NONE',  ( 4.458734124999998549, -72.97916666530107932, -2.574251347313721627 ) ) ;
#21153 = CARTESIAN_POINT ( 'NONE',  ( 5.000000000000000000, -34.41666666666666430, -2.886751345948130876 ) ) ;
#21154 = CARTESIAN_POINT ( 'NONE',  ( -4.458734124999997661, 0.5208333346989266754, 2.574251347313722516 ) ) ;
#21155 = VERTEX_POINT ( 'NONE', #28980 ) ;
#21156 = CARTESIAN_POINT ( 'NONE',  ( -6.972266317189433020E-16, -48.24999999999999289, -5.000000000000000000 ) ) ;
#21157 = CARTESIAN_POINT ( 'NONE',  ( 5.000000000000000000, -57.49999999999999289, -6.123233995736766282E-16 ) ) ;
#21159 = CARTESIAN_POINT ( 'NONE',  ( -4.458734124999999437, -33.39583333196772941, -2.574251347313719407 ) ) ;
#21158 = CARTESIAN_POINT ( 'NONE',  ( -2.229367062500000163, -89.47916666530106511, -3.861377020970580443 ) ) ;
#21160 = CARTESIAN_POINT ( 'NONE',  ( -4.999999999999998224, -4.916666666666666075, 2.886751345948131764 ) ) ;
#21161 = CARTESIAN_POINT ( 'NONE',  ( 9.457646018065525792E-16, -84.31249999863437949, 5.148502694627439702 ) ) ;
#21162 = CARTESIAN_POINT ( 'NONE',  ( -3.152548672688508926E-16, 15.18750000136559564, -5.148502694627439702 ) ) ;
#21163 = DIRECTION ( 'NONE',  ( -0.000000000000000000, 1.000000000000000000, -0.000000000000000000 ) ) ;
#21164 = CARTESIAN_POINT ( 'NONE',  ( -54.64476657466781973, -136.8125000013656063, -4.444560631937228834 ) ) ;
#21165 = CARTESIAN_POINT ( 'NONE',  ( 4.458734124999999437, -7.812499998634405252, -5.460374474430324690E-16 ) ) ;
#21166 = CARTESIAN_POINT ( 'NONE',  ( 2.229367062500001939, 23.77083333469892779, 3.861377020970579999 ) ) ;
#21167 = CARTESIAN_POINT ( 'NONE',  ( -4.458734124999999437, -46.64583333196774362, -2.574251347313719407 ) ) ;
#21168 = CARTESIAN_POINT ( 'NONE',  ( -2.229367062500000163, -86.47916666530107932, -3.861377020970580443 ) ) ;
#21169 = CARTESIAN_POINT ( 'NONE',  ( -2.229367062500000163, -4.479166665301070438, -3.861377020970580443 ) ) ;
#21170 = SURFACE_STYLE_USAGE ( .BOTH. , #39256 ) ;
#21171 = EDGE_LOOP ( 'NONE', ( #34323, #26057, #60964 ) ) ;
#21172 = CARTESIAN_POINT ( 'NONE',  ( 4.458734124999999437, -29.06249999863440436, -5.460374474430324690E-16 ) ) ;
#21173 = CARTESIAN_POINT ( 'NONE',  ( -55.35523342533222291, -131.5625000013656063, 4.444560631937231499 ) ) ;
#21174 = CARTESIAN_POINT ( 'NONE',  ( 4.458734124999998549, -72.72916666530106511, -2.574251347313721627 ) ) ;
#21175 = CARTESIAN_POINT ( 'NONE',  ( 5.000000000000000000, -110.2916666639354588, -2.886751345948129988 ) ) ;
#21176 = AXIS2_PLACEMENT_3D ( 'NONE', #2107, #50969, #5954 ) ;
#21177 = VECTOR ( 'NONE', #45994, 1000.000000000000000 ) ;
#21178 = CARTESIAN_POINT ( 'NONE',  ( -3.152548672688508926E-16, 21.43750000136559564, -5.148502694627439702 ) ) ;
#21179 = CARTESIAN_POINT ( 'NONE',  ( 1.339745962155615144, 1.294658198738520172, 4.999999999999999112 ) ) ;
#21180 = CARTESIAN_POINT ( 'NONE',  ( 9.457646018065525792E-16, -79.31249999863440792, 5.148502694627439702 ) ) ;
#21181 = CARTESIAN_POINT ( 'NONE',  ( -5.000000000000000000, -67.00000000000000000, 0.000000000000000000 ) ) ;
#21182 = CARTESIAN_POINT ( 'NONE',  ( -51.75738570946856498, -151.7500000000000284, 3.805975901505576964 ) ) ;
#21183 = CARTESIAN_POINT ( 'NONE',  ( 5.000000000000000000, 22.70833333606451632, -2.886751345948129988 ) ) ;
#21184 = ORIENTED_EDGE ( 'NONE', *, *, #34954, .T. ) ;
#21185 = CARTESIAN_POINT ( 'NONE',  ( -5.000000000000000000, -66.00000000000000000, 0.000000000000000000 ) ) ;
#21186 = DIRECTION ( 'NONE',  ( -0.000000000000000000, 1.000000000000000000, -0.000000000000000000 ) ) ;
#21188 = CARTESIAN_POINT ( 'NONE',  ( -2.499999999999996447, -21.83333333333332860, 4.330127018922195425 ) ) ;
#21187 = CARTESIAN_POINT ( 'NONE',  ( 6.123233995736766282E-16, -120.0000000000000000, -5.000000000000000000 ) ) ;
#21189 = CARTESIAN_POINT ( 'NONE',  ( 2.229367062499998831, -28.64583333196774007, -3.861377020970580887 ) ) ;
#21190 = CARTESIAN_POINT ( 'NONE',  ( 2.229367062500001939, -86.97916666530107932, 3.861377020970579999 ) ) ;
#21191 =( BOUNDED_CURVE ( )  B_SPLINE_CURVE ( 2, ( #29166, #25946, #1519, #6973, #16932, #21122, #41674, #21769, #46202 ),
 .UNSPECIFIED., .F., .F. ) 
 B_SPLINE_CURVE_WITH_KNOTS ( ( 3, 2, 2, 2, 3 ),
 ( 0.4062500000000000000, 0.4069444444444444420, 0.4083333333333333259, 0.4097222222222222099, 0.4104166666666666519 ),
 .UNSPECIFIED. ) 
 CURVE ( )  GEOMETRIC_REPRESENTATION_ITEM ( )  RATIONAL_B_SPLINE_CURVE ( ( 0.9330127018922194093, 0.9330127018922194093, 1.000000000000000000, 0.8660254037844387076, 1.000000000000000000, 0.8660254037844387076, 1.000000000000000000, 0.9330127018922194093, 0.9330127018922194093 ) ) 
 REPRESENTATION_ITEM ( '' )  );
#21192 = CARTESIAN_POINT ( 'NONE',  ( 5.000000000000000000, -24.37499999726881228, -6.123233995736766282E-16 ) ) ;
#21194 = VERTEX_POINT ( 'NONE', #43459 ) ;
#21193 = CARTESIAN_POINT ( 'NONE',  ( 9.457646018065525792E-16, -57.06249999863440081, 5.148502694627439702 ) ) ;
#21195 = CARTESIAN_POINT ( 'NONE',  ( 1.339745962155615144, -35.58034179853028434, 4.999999999999999112 ) ) ;
#21196 = CYLINDRICAL_SURFACE ( 'NONE', #36467, 5.000000000000000000 ) ;
#21198 = ORIENTED_EDGE ( 'NONE', *, *, #46687, .F. ) ;
#21197 = CARTESIAN_POINT ( 'NONE',  ( -2.229367062500000163, -4.729166665301071326, -3.861377020970580443 ) ) ;
#21199 = CARTESIAN_POINT ( 'NONE',  ( -5.000000000000000000, -72.00000000000000000, 0.000000000000000000 ) ) ;
#21200 = CARTESIAN_POINT ( 'NONE',  ( -3.152801135295367096, -152.3125000013655779, -3.152801135295367541 ) ) ;
#21201 = CARTESIAN_POINT ( 'NONE',  ( 4.458734125000001214, -47.14583333196774362, 2.574251347313718519 ) ) ;
#21202 = CARTESIAN_POINT ( 'NONE',  ( -75.00000000000000000, 15.00000000000000000, 8.999999999999998224 ) ) ;
#21203 = CARTESIAN_POINT ( 'NONE',  ( 3.535533905932736864, -158.1250000000000284, 3.535533905932738641 ) ) ;
#21204 = CARTESIAN_POINT ( 'NONE',  ( -6.972266317189433020E-16, -22.12499999726881228, -5.000000000000000000 ) ) ;
#21205 = CARTESIAN_POINT ( 'NONE',  ( -55.39835681537999790, -153.8750000000000284, 4.984105922594378235 ) ) ;
#21206 = EDGE_CURVE ( 'NONE', #4973, #14179, #7274, .T. ) ;
#21207 = CARTESIAN_POINT ( 'NONE',  ( 2.229367062499998831, -14.89583333196773474, -3.861377020970580887 ) ) ;
#21208 = CARTESIAN_POINT ( 'NONE',  ( 2.229367062499998831, -52.89583333196773651, -3.861377020970580887 ) ) ;
#21209 =( BOUNDED_CURVE ( )  B_SPLINE_CURVE ( 2, ( #391, #43480, #4884, #24185, #53766, #58291, #15170, #19993, #72 ),
 .UNSPECIFIED., .F., .F. ) 
 B_SPLINE_CURVE_WITH_KNOTS ( ( 3, 2, 2, 2, 3 ),
 ( 0.2020833333333333370, 0.2027777777777777790, 0.2041666666666666630, 0.2055555555555555469, 0.2062499999999999889 ),
 .UNSPECIFIED. ) 
 CURVE ( )  GEOMETRIC_REPRESENTATION_ITEM ( )  RATIONAL_B_SPLINE_CURVE ( ( 0.9330127018922194093, 0.9330127018922194093, 1.000000000000000000, 0.8660254037844387076, 1.000000000000000000, 0.8660254037844387076, 1.000000000000000000, 0.9330127018922194093, 0.9330127018922194093 ) ) 
 REPRESENTATION_ITEM ( '' )  );
#21210 = CARTESIAN_POINT ( 'NONE',  ( 1.975475456537005874E-15, -58.62499999726879452, 5.000000000000000000 ) ) ;
#21211 = CARTESIAN_POINT ( 'NONE',  ( -1.846868145590734756, -143.1250000013656063, -4.458734125000000326 ) ) ;
#21212 = CARTESIAN_POINT ( 'NONE',  ( 9.457646018065525792E-16, -93.31249999863439371, 5.148502694627439702 ) ) ;
#21213 = ORIENTED_EDGE ( 'NONE', *, *, #37851, .F. ) ;
#21214 = CARTESIAN_POINT ( 'NONE',  ( -56.48576386720575471, -154.0000000013656063, -4.591703134518078322 ) ) ;
#21215 = CARTESIAN_POINT ( 'NONE',  ( 2.229367062499998831, 26.10416666803225993, -3.861377020970580887 ) ) ;
#21216 = CARTESIAN_POINT ( 'NONE',  ( -56.66612745406270335, -147.4375000027311842, -5.149110718188516067 ) ) ;
#21217 = CIRCLE ( 'NONE', #1717, 5.000000000000000000 ) ;
#21218 = ADVANCED_FACE ( 'NONE', ( #39264 ), #19016, .T. ) ;
#21219 = DIRECTION ( 'NONE',  ( 7.709882115452476194E-16, -0.000000000000000000, 1.000000000000000000 ) ) ;
#21220 = ORIENTED_EDGE ( 'NONE', *, *, #43993, .F. ) ;
#21221 = AXIS2_PLACEMENT_3D ( 'NONE', #24417, #5432, #4791 ) ;
#21222 = CARTESIAN_POINT ( 'NONE',  ( -4.458734124999998549, -4.229166665301070438, 2.574251347313722516 ) ) ;
#21223 = AXIS2_PLACEMENT_3D ( 'NONE', #10867, #47496, #26946 ) ;
#21224 = CARTESIAN_POINT ( 'NONE',  ( 4.458734124999999437, -23.06249999863440436, -5.460374474430324690E-16 ) ) ;
#21225 = ADVANCED_FACE ( 'NONE', ( #38020 ), #34123, .F. ) ;
#21226 = DIRECTION ( 'NONE',  ( -0.000000000000000000, 1.000000000000000000, -0.000000000000000000 ) ) ;
#21227 = CARTESIAN_POINT ( 'NONE',  ( 4.458734125000001214, -6.895833331967734736, 2.574251347313718519 ) ) ;
#21228 = CARTESIAN_POINT ( 'NONE',  ( 6.625705691649528717, -5.306270977113132226, -7.795653906408932521 ) ) ;
#21229 = CARTESIAN_POINT ( 'NONE',  ( 1.846868145590735200, -150.2500000013656347, -4.458734124999999437 ) ) ;
#21230 = CARTESIAN_POINT ( 'NONE',  ( 9.457646018065525792E-16, 13.68750000136559386, 5.148502694627439702 ) ) ;
#21231 = ORIENTED_EDGE ( 'NONE', *, *, #36622, .F. ) ;
#21232 = CARTESIAN_POINT ( 'NONE',  ( -5.000000000000000000, -62.87499999726880873, 0.000000000000000000 ) ) ;
#21233 = CARTESIAN_POINT ( 'NONE',  ( -6.972266317189433020E-16, 26.87500000273118417, -5.000000000000000000 ) ) ;
#21234 = CARTESIAN_POINT ( 'NONE',  ( 2.229367062500001939, -16.97916666530106866, 3.861377020970579999 ) ) ;
#21235 = CARTESIAN_POINT ( 'NONE',  ( 2.500000000000002220, -85.54166666393547303, 4.330127018922192761 ) ) ;
#21236 = CARTESIAN_POINT ( 'NONE',  ( -2.500000000000000444, -6.166666666666667851, -4.330127018922193649 ) ) ;
#21237 = CARTESIAN_POINT ( 'NONE',  ( -57.19623071787017210, -149.3750000013656347, 4.297418129356382899 ) ) ;
#21238 = CARTESIAN_POINT ( 'NONE',  ( 5.000000000000000000, -44.37499999726880873, -6.123233995736766282E-16 ) ) ;
#21239 = LINE ( 'NONE', #22201, #61991 ) ;
#21240 = CARTESIAN_POINT ( 'NONE',  ( 9.457646018065525792E-16, 6.937500001365595637, 5.148502694627439702 ) ) ;
#21241 = CARTESIAN_POINT ( 'NONE',  ( 1.975475456537005874E-15, -8.624999997268812280, 5.000000000000000000 ) ) ;
#21242 = ORIENTED_EDGE ( 'NONE', *, *, #50256, .F. ) ;
#21243 = CARTESIAN_POINT ( 'NONE',  ( 4.458734125000000326, 11.10416666803225993, 2.574251347313718519 ) ) ;
#21244 = CARTESIAN_POINT ( 'NONE',  ( 4.458734124999999437, -68.81249999863439371, -5.460374474430324690E-16 ) ) ;
#21245 = CARTESIAN_POINT ( 'NONE',  ( -2.229367062500000163, -12.72916666530107044, -3.861377020970580443 ) ) ;
#21246 = CARTESIAN_POINT ( 'NONE',  ( -5.000000000000000000, -1.000000000000000888, 0.000000000000000000 ) ) ;
#21247 = CARTESIAN_POINT ( 'NONE',  ( -1.846868145590737420, -164.7500000013656063, 4.458734124999999437 ) ) ;
#21248 = CARTESIAN_POINT ( 'NONE',  ( -5.000000000000000000, 26.12500000273118417, 0.000000000000000000 ) ) ;
#21249 = CARTESIAN_POINT ( 'NONE',  ( 2.229367062499998831, -58.64583333196773651, -3.861377020970580887 ) ) ;
#21250 = CARTESIAN_POINT ( 'NONE',  ( -2.500000000000000444, -94.04166666393547303, -4.330127018922193649 ) ) ;
#21251 = EDGE_CURVE ( 'NONE', #11078, #58699, #21474, .T. ) ;
#21252 = CARTESIAN_POINT ( 'NONE',  ( -2.499999999999996447, 20.29166666939784847, 4.330127018922195425 ) ) ;
#21253 = CARTESIAN_POINT ( 'NONE',  ( -9.184850993605147944E-16, -165.3750000027312126, 5.000000000000000000 ) ) ;
#21254 = CARTESIAN_POINT ( 'NONE',  ( 5.000000000000000000, -139.1875000027312126, 2.071067811865478614 ) ) ;
#21255 = CARTESIAN_POINT ( 'NONE',  ( -2.229367062499996610, -34.14583333196772941, 3.861377020970582219 ) ) ;
#21256 = CARTESIAN_POINT ( 'NONE',  ( 5.000000000000000000, -45.50000000000000000, -6.123233995736766282E-16 ) ) ;
#21257 = LINE ( 'NONE', #30582, #43868 ) ;
#21258 = CARTESIAN_POINT ( 'NONE',  ( 0.000000000000000000, 0.000000000000000000, -8.499999999999998224 ) ) ;
#21259 = EDGE_LOOP ( 'NONE', ( #14017, #33991, #40412, #873 ) ) ;
#21260 = CARTESIAN_POINT ( 'NONE',  ( -4.458734124999998549, -108.2291666653010651, 2.574251347313722516 ) ) ;
#21261 = CARTESIAN_POINT ( 'NONE',  ( -4.458734124999999437, -1.645833331967737401, -2.574251347313719407 ) ) ;
#21262 =( BOUNDED_CURVE ( )  B_SPLINE_CURVE ( 2, ( #20767, #5650, #24307, #54541, #43912, #33961, #15622, #49062, #14340 ),
 .UNSPECIFIED., .F., .F. ) 
 B_SPLINE_CURVE_WITH_KNOTS ( ( 3, 2, 2, 2, 3 ),
 ( 0.06458333333333333981, 0.06527777777777778179, 0.06666666666666666574, 0.06805555555555554970, 0.06875000000000000555 ),
 .UNSPECIFIED. ) 
 CURVE ( )  GEOMETRIC_REPRESENTATION_ITEM ( )  RATIONAL_B_SPLINE_CURVE ( ( 0.9330127018922194093, 0.9330127018922200755, 1.000000000000000000, 0.8660254037844387076, 1.000000000000000000, 0.8660254037844387076, 1.000000000000000000, 0.9330127018922187432, 0.9330127018922194093 ) ) 
 REPRESENTATION_ITEM ( '' )  );
#21263 = VECTOR ( 'NONE', #50570, 1000.000000000000114 ) ;
#21264 = CARTESIAN_POINT ( 'NONE',  ( 1.339745962155612702, -73.16965819600734733, -5.000000000000000000 ) ) ;
#21265 = CARTESIAN_POINT ( 'NONE',  ( -3.535250795749689387E-16, -6.249999999999998224, -5.773502691896257311 ) ) ;
#21266 = CARTESIAN_POINT ( 'NONE',  ( -2.229367062500000163, -73.47916666530106511, -3.861377020970580443 ) ) ;
#21267 = VECTOR ( 'NONE', #17360, 1000.000000000000000 ) ;
#21268 = LINE ( 'NONE', #40873, #5136 ) ;
#21269 = CARTESIAN_POINT ( 'NONE',  ( 5.000000000000000000, -5.374999997268811391, -6.123233995736766282E-16 ) ) ;
#21271 = ORIENTED_EDGE ( 'NONE', *, *, #6302, .T. ) ;
#21270 = CARTESIAN_POINT ( 'NONE',  ( -2.229367062500000163, -37.47916666530107221, -3.861377020970580443 ) ) ;
#21272 = AXIS2_PLACEMENT_3D ( 'NONE', #30560, #6137, #49548 ) ;
#21274 = EDGE_LOOP ( 'NONE', ( #60968, #24267, #49835, #22655 ) ) ;
#21273 = CARTESIAN_POINT ( 'NONE',  ( 4.458734125000001214, 9.854166668032263487, 2.574251347313718519 ) ) ;
#21275 = CARTESIAN_POINT ( 'NONE',  ( 5.000000000000000000, -101.5000000000000000, -6.123233995736766282E-16 ) ) ;
#21276 = CARTESIAN_POINT ( 'NONE',  ( -2.499999999999996447, -48.83333333333332860, 4.330127018922195425 ) ) ;
#21277 = CARTESIAN_POINT ( 'NONE',  ( -4.458734124999999437, -28.56249999863440081, 0.000000000000000000 ) ) ;
#21278 = CARTESIAN_POINT ( 'NONE',  ( -5.000000000000000000, 14.12500000273118594, 0.000000000000000000 ) ) ;
#21279 = CARTESIAN_POINT ( 'NONE',  ( -4.458734124999998549, -77.22916666530106511, 2.574251347313722516 ) ) ;
#21280 = CARTESIAN_POINT ( 'NONE',  ( -3.152801135295367985, -140.0625000013655779, 3.152801135295367096 ) ) ;
#21281 = CARTESIAN_POINT ( 'NONE',  ( 9.457646018065525792E-16, -87.06249999863440792, 5.148502694627439702 ) ) ;
#21282 = CARTESIAN_POINT ( 'NONE',  ( -50.70258187064364108, -133.3750000013656063, 2.196230717870141014 ) ) ;
#21283 = CARTESIAN_POINT ( 'NONE',  ( -3.152548672688508926E-16, -37.81249999863440792, -5.148502694627439702 ) ) ;
#21284 = EDGE_CURVE ( 'NONE', #23096, #46264, #34587, .T. ) ;
#21285 = EDGE_CURVE ( 'NONE', #248, #20337, #37072, .T. ) ;
#21286 = CARTESIAN_POINT ( 'NONE',  ( -2.500000000000000444, -94.04166666393547303, -4.330127018922193649 ) ) ;
#21287 = ORIENTED_EDGE ( 'NONE', *, *, #9501, .F. ) ;
#21288 = CARTESIAN_POINT ( 'NONE',  ( -2.229367062500000163, -80.72916666530106511, -3.861377020970580443 ) ) ;
#21289 = DIRECTION ( 'NONE',  ( 0.000000000000000000, 0.000000000000000000, 1.000000000000000000 ) ) ;
#21290 = EDGE_CURVE ( 'NONE', #61986, #56964, #30899, .T. ) ;
#21291 = ORIENTED_EDGE ( 'NONE', *, *, #39010, .T. ) ;
#21292 = CARTESIAN_POINT ( 'NONE',  ( -1.339745962155660663, -3.669658196007337558, 4.999999999999972466 ) ) ;
#21293 = SHAPE_REPRESENTATION ( 'crossbar', ( #43054 ), #21498 ) ;
#21294 = DIRECTION ( 'NONE',  ( -0.000000000000000000, 1.000000000000000000, -0.000000000000000000 ) ) ;
#21295 = CARTESIAN_POINT ( 'NONE',  ( -4.458734124999998549, -65.47916666530107932, 2.574251347313722516 ) ) ;
#21296 = CARTESIAN_POINT ( 'NONE',  ( -2.229367062499996610, -3.395833331967738733, 3.861377020970582219 ) ) ;
#21297 = VERTEX_POINT ( 'NONE', #54396 ) ;
#21298 = ADVANCED_FACE ( 'NONE', ( #15479 ), #49560, .T. ) ;
#21299 = CARTESIAN_POINT ( 'NONE',  ( -5.000000000000000000, 5.041666669397853795, -2.886751345948128211 ) ) ;
#21300 = ORIENTED_EDGE ( 'NONE', *, *, #6436, .F. ) ;
#21301 = CARTESIAN_POINT ( 'NONE',  ( 1.975475456537005874E-15, -44.74999999999999289, 5.000000000000000000 ) ) ;
#21302 = ADVANCED_FACE ( 'NONE', ( #39899 ), #35098, .T. ) ;
#21303 = ADVANCED_FACE ( 'NONE', ( #40233 ), #54716, .T. ) ;
#21304 = CARTESIAN_POINT ( 'NONE',  ( 2.229367062500001939, 10.02083333469892779, 3.861377020970579999 ) ) ;
#21305 = CARTESIAN_POINT ( 'NONE',  ( -3.152801135295367096, -163.0625000013656063, -3.152801135295367541 ) ) ;
#21306 = AXIS2_PLACEMENT_3D ( 'NONE', #30379, #50002, #24608 ) ;
#21307 = DIRECTION ( 'NONE',  ( -0.000000000000000000, 1.000000000000000000, -0.000000000000000000 ) ) ;
#21308 = ORIENTED_EDGE ( 'NONE', *, *, #56294, .T. ) ;
#21309 = CARTESIAN_POINT ( 'NONE',  ( -3.152548672688508926E-16, -84.56249999863439371, -5.148502694627439702 ) ) ;
#21310 = EDGE_CURVE ( 'NONE', #9578, #15905, #1341, .T. ) ;
#21311 = FACE_OUTER_BOUND ( 'NONE', #61296, .T. ) ;
#21312 = CARTESIAN_POINT ( 'NONE',  ( 2.229367062499998831, -4.645833331967740065, -3.861377020970580887 ) ) ;
#21313 = VECTOR ( 'NONE', #48219, 1000.000000000000000 ) ;
#21314 = CARTESIAN_POINT ( 'NONE',  ( 2.499999999999998668, 25.79166666939785202, -4.330127018922193649 ) ) ;
#21315 = VECTOR ( 'NONE', #29677, 1000.000000000000000 ) ;
#21316 = AXIS2_PLACEMENT_3D ( 'NONE', #24870, #58645, #28424 ) ;
#21317 = CARTESIAN_POINT ( 'NONE',  ( 1.060575238724906964E-15, -29.62499999726881228, 5.773502691896257311 ) ) ;
#21318 = CARTESIAN_POINT ( 'NONE',  ( -1.339745962155610925, -28.79465819873852084, 5.000000000000000000 ) ) ;
#21319 = CARTESIAN_POINT ( 'NONE',  ( 4.458734124999998549, 25.27083333469892779, -2.574251347313721627 ) ) ;
#21320 = CARTESIAN_POINT ( 'NONE',  ( -6.972266317189433020E-16, -0.1249999972688142225, -5.000000000000000000 ) ) ;
#21321 = CARTESIAN_POINT ( 'NONE',  ( 4.458734125000000326, 26.10416666803225993, 2.574251347313718519 ) ) ;
#21322 = CARTESIAN_POINT ( 'NONE',  ( 9.457646018065525792E-16, -53.06249999863441502, 5.148502694627439702 ) ) ;
#21323 = CARTESIAN_POINT ( 'NONE',  ( 4.458734124999999437, -36.06249999863440792, -5.460374474430324690E-16 ) ) ;
#21324 = CARTESIAN_POINT ( 'NONE',  ( -2.229367062500000163, 0.2708333346989263979, -3.861377020970580443 ) ) ;
#21325 = CARTESIAN_POINT ( 'NONE',  ( -3.535533905932737309, -149.7500000027312126, -3.535533905932738197 ) ) ;
#21326 = CARTESIAN_POINT ( 'NONE',  ( -2.500000000000000444, 20.83333333333333215, -4.330127018922193649 ) ) ;
#21327 = CARTESIAN_POINT ( 'NONE',  ( -3.535533905932738641, -145.5000000027311842, 3.535533905932737309 ) ) ;
#21328 = CARTESIAN_POINT ( 'NONE',  ( 3.061616997868383141E-16, -158.7500000000000000, -5.000000000000000000 ) ) ;
#21329 = CARTESIAN_POINT ( 'NONE',  ( 9.457646018065525792E-16, -44.06249999863439371, 5.148502694627439702 ) ) ;
#21330 = CARTESIAN_POINT ( 'NONE',  ( -2.500000000000000444, -78.04166666393547303, -4.330127018922193649 ) ) ;
#21331 = CARTESIAN_POINT ( 'NONE',  ( -55.35523342533222291, -138.5625000013656063, 4.444560631937231499 ) ) ;
#21332 = CARTESIAN_POINT ( 'NONE',  ( -5.000000000000000000, -140.5000000000000000, -6.123233995736766282E-16 ) ) ;
#21333 = CARTESIAN_POINT ( 'NONE',  ( 1.975475456537005874E-15, -88.74999999999998579, 5.000000000000000000 ) ) ;
#21334 = CARTESIAN_POINT ( 'NONE',  ( -2.229367062499996610, -82.39583333196773651, 3.861377020970582219 ) ) ;
#21335 = CARTESIAN_POINT ( 'NONE',  ( -4.458734125000000326, -163.1250000013656347, 1.846868145590734089 ) ) ;
#21336 = CARTESIAN_POINT ( 'NONE',  ( 0.000000000000000000, -120.0000000000000000, 0.000000000000000000 ) ) ;
#21337 = CARTESIAN_POINT ( 'NONE',  ( 5.000000000000000000, -26.49999999999999645, -6.123233995736766282E-16 ) ) ;
#21338 = CARTESIAN_POINT ( 'NONE',  ( -4.458734124999999437, -139.9375000013656063, -5.460374474430324690E-16 ) ) ;
#21339 = EDGE_LOOP ( 'NONE', ( #13889, #33305, #29804, #17942 ) ) ;
#21340 = CARTESIAN_POINT ( 'NONE',  ( -4.458734124999999437, 24.43750000136559208, 0.000000000000000000 ) ) ;
#21341 = ORIENTED_EDGE ( 'NONE', *, *, #54601, .T. ) ;
#21342 = CARTESIAN_POINT ( 'NONE',  ( -4.458734124999998549, -88.22916666530107932, 2.574251347313722516 ) ) ;
#21343 = CARTESIAN_POINT ( 'NONE',  ( 9.457646018065525792E-16, 12.68750000136559208, 5.148502694627439702 ) ) ;
#21344 = CARTESIAN_POINT ( 'NONE',  ( -5.000000000000000000, 16.04166666939785202, -2.886751345948128211 ) ) ;
#21345 = CARTESIAN_POINT ( 'NONE',  ( 5.000000000000000000, 11.50000000000000000, -6.123233995736766282E-16 ) ) ;
#21346 = CARTESIAN_POINT ( 'NONE',  ( 2.229367062499998831, -53.64583333196773651, -3.861377020970580887 ) ) ;
#21347 = CARTESIAN_POINT ( 'NONE',  ( -2.229367062500000163, -11.47916666530107044, -3.861377020970580443 ) ) ;
#21348 = CARTESIAN_POINT ( 'NONE',  ( 3.061616997868383141E-16, -165.8750000027312126, -5.000000000000000000 ) ) ;
#21349 = CARTESIAN_POINT ( 'NONE',  ( -54.64476657466781973, -136.0625000013656063, -4.444560631937228834 ) ) ;
#21350 = CARTESIAN_POINT ( 'NONE',  ( -6.972266317189433020E-16, 15.87500000273118417, -5.000000000000000000 ) ) ;
#21351 = CARTESIAN_POINT ( 'NONE',  ( -5.000000000000000000, -64.08333333333332860, -2.886751345948128211 ) ) ;
#21352 = CARTESIAN_POINT ( 'NONE',  ( -2.499999999999996447, -61.83333333333333570, 4.330127018922195425 ) ) ;
#21353 = CARTESIAN_POINT ( 'NONE',  ( 2.499999999999998668, -36.33333333333332860, -4.330127018922193649 ) ) ;
#21354 = LINE ( 'NONE', #10742, #46934 ) ;
#21356 = CARTESIAN_POINT ( 'NONE',  ( -4.458734124999998549, -16.47916666530107577, 2.574251347313722516 ) ) ;
#21355 = LINE ( 'NONE', #10743, #44950 ) ;
#21357 = VECTOR ( 'NONE', #6907, 1000.000000000000000 ) ;
#21358 = CARTESIAN_POINT ( 'NONE',  ( -2.500000000000000444, -32.04166666393548724, -4.330127018922193649 ) ) ;
#21359 = CARTESIAN_POINT ( 'NONE',  ( 4.458734124999999437, -57.81249999863440081, -5.460374474430324690E-16 ) ) ;
#21360 = CARTESIAN_POINT ( 'NONE',  ( 3.152801135295366208, -150.8125000013655779, 3.152801135295367985 ) ) ;
#21361 = CARTESIAN_POINT ( 'NONE',  ( -4.458734124999999437, -72.31249999863439371, 0.000000000000000000 ) ) ;
#21362 = VECTOR ( 'NONE', #40860, 1000.000000000000000 ) ;
#21363 = CARTESIAN_POINT ( 'NONE',  ( -57.19623071787017210, -148.6250000013656063, 4.297418129356382899 ) ) ;
#21364 = CARTESIAN_POINT ( 'NONE',  ( 5.000000000000000888, -59.45833333060214443, 2.886751345948126879 ) ) ;
#21365 = VERTEX_POINT ( 'NONE', #49872 ) ;
#21366 = CARTESIAN_POINT ( 'NONE',  ( 0.000000000000000000, -120.0000000000000000, 0.000000000000000000 ) ) ;
#21367 = VERTEX_POINT ( 'NONE', #5819 ) ;
#21369 = CARTESIAN_POINT ( 'NONE',  ( 6.123233995736766282E-16, -120.0000000000000000, -5.000000000000000000 ) ) ;
#21368 = DIRECTION ( 'NONE',  ( -0.000000000000000000, 1.000000000000000000, -0.000000000000000000 ) ) ;
#21370 = CARTESIAN_POINT ( 'NONE',  ( 4.458734124999999437, -151.4375000013655779, 0.000000000000000000 ) ) ;
#21371 = ORIENTED_EDGE ( 'NONE', *, *, #2715, .F. ) ;
#21372 = CARTESIAN_POINT ( 'NONE',  ( -6.972266317189433020E-16, -10.24999999999999822, -5.000000000000000000 ) ) ;
#21373 = CARTESIAN_POINT ( 'NONE',  ( -59.98410592259440222, -130.1250000000000284, -0.3983568153799752487 ) ) ;
#21374 = CARTESIAN_POINT ( 'NONE',  ( 5.000000000000000888, -86.58333333333332860, 2.886751345948126879 ) ) ;
#21375 = CARTESIAN_POINT ( 'NONE',  ( 4.458734124999999437, -50.06249999863440792, -5.460374474430324690E-16 ) ) ;
#21376 = ORIENTED_EDGE ( 'NONE', *, *, #23713, .F. ) ;
#21377 = CARTESIAN_POINT ( 'NONE',  ( -6.972266317189433020E-16, 11.74999999999999645, -5.000000000000000000 ) ) ;
#21378 = CARTESIAN_POINT ( 'NONE',  ( 4.458734124999999437, 13.18750000136559208, -5.460374474430324690E-16 ) ) ;
#21379 = EDGE_CURVE ( 'NONE', #32387, #47937, #35114, .T. ) ;
#21380 = CARTESIAN_POINT ( 'NONE',  ( -3.152548672688508926E-16, 24.43750000136559564, -5.148502694627439702 ) ) ;
#21381 = CARTESIAN_POINT ( 'NONE',  ( -57.89159099828107458, -152.6875000013656063, -3.393966926194107447 ) ) ;
#21382 = CARTESIAN_POINT ( 'NONE',  ( 2.500000000000002220, -13.54166666393548013, 4.330127018922192761 ) ) ;
#21383 = CARTESIAN_POINT ( 'NONE',  ( -6.972266317189433020E-16, -61.12499999726880162, -5.000000000000000000 ) ) ;
#21385 = EDGE_CURVE ( 'NONE', #45889, #51535, #55359, .T. ) ;
#21384 = ORIENTED_EDGE ( 'NONE', *, *, #39262, .T. ) ;
#21386 = CARTESIAN_POINT ( 'NONE',  ( 2.229367062500001939, -63.97916666530106511, 3.861377020970579999 ) ) ;
#21387 = CARTESIAN_POINT ( 'NONE',  ( -0.3483149870578547969, 8.861353789385022495, -7.493854785173811983 ) ) ;
#21388 = CARTESIAN_POINT ( 'NONE',  ( 4.458734125000001214, 12.10416666803226171, 2.574251347313718519 ) ) ;
#21389 =( BOUNDED_CURVE ( )  B_SPLINE_CURVE ( 2, ( #1376, #24838, #59906, #48948, #44761, #59580, #15514, #25467, #4897 ),
 .UNSPECIFIED., .F., .F. ) 
 B_SPLINE_CURVE_WITH_KNOTS ( ( 3, 2, 2, 2, 3 ),
 ( 0.6770833333333333703, 0.6777777777777778123, 0.6791666666666666963, 0.6805555555555555802, 0.6812500000000000222 ),
 .UNSPECIFIED. ) 
 CURVE ( )  GEOMETRIC_REPRESENTATION_ITEM ( )  RATIONAL_B_SPLINE_CURVE ( ( 0.9330127018922194093, 0.9330127018922194093, 1.000000000000000000, 0.8660254037844387076, 1.000000000000000000, 0.8660254037844387076, 1.000000000000000000, 0.9330127018922194093, 0.9330127018922194093 ) ) 
 REPRESENTATION_ITEM ( '' )  );
#21390 = CARTESIAN_POINT ( 'NONE',  ( -6.972266317189433020E-16, -63.25000000000000000, -5.000000000000000000 ) ) ;
#21391 = EDGE_CURVE ( 'NONE', #59111, #62654, #54338, .T. ) ;
#21392 = CARTESIAN_POINT ( 'NONE',  ( -5.000000000000000888, -157.4375000000000000, 2.071067811865474617 ) ) ;
#21393 = CARTESIAN_POINT ( 'NONE',  ( -2.229367062499996610, -55.39583333196773651, 3.861377020970582219 ) ) ;
#21394 = CARTESIAN_POINT ( 'NONE',  ( -4.999999999999999112, -16.79166666393548368, 2.886751345948131764 ) ) ;
#21395 = CARTESIAN_POINT ( 'NONE',  ( 5.000000000000000000, -48.50000000000000000, -6.123233995736766282E-16 ) ) ;
#21396 = DIRECTION ( 'NONE',  ( -1.000000000000000000, -0.000000000000000000, -3.614007241618347908E-17 ) ) ;
#21397 = DIRECTION ( 'NONE',  ( 0.000000000000000000, 0.000000000000000000, 1.000000000000000000 ) ) ;
#21398 = CARTESIAN_POINT ( 'NONE',  ( 2.229367062500001939, -14.22916666530107221, 3.861377020970579999 ) ) ;
#21399 = ORIENTED_EDGE ( 'NONE', *, *, #8292, .T. ) ;
#21400 = VECTOR ( 'NONE', #13926, 1000.000000000000000 ) ;
#21401 = PLANE ( 'NONE',  #44 ) ;
#21402 = CARTESIAN_POINT ( 'NONE',  ( 4.458734124999999437, -101.8124999986344079, -5.460374474430324690E-16 ) ) ;
#21403 = CARTESIAN_POINT ( 'NONE',  ( 5.000000000000000000, -159.1250000027311842, 0.000000000000000000 ) ) ;
#21404 = ORIENTED_EDGE ( 'NONE', *, *, #18453, .T. ) ;
#21405 = CARTESIAN_POINT ( 'NONE',  ( 2.229367062499998831, -103.8958333319677365, -3.861377020970580887 ) ) ;
#21406 = VECTOR ( 'NONE', #3463, 1000.000000000000000 ) ;
#21407 = CARTESIAN_POINT ( 'NONE',  ( -4.458734124999998549, -29.22916666530107221, 2.574251347313722516 ) ) ;
#21408 = CARTESIAN_POINT ( 'NONE',  ( -5.000000000000000000, -63.87499999726880873, 0.000000000000000000 ) ) ;
#21409 = CARTESIAN_POINT ( 'NONE',  ( -59.29741812935640155, -150.8750000013656063, -2.196230717870135685 ) ) ;
#21410 = CARTESIAN_POINT ( 'NONE',  ( -53.51423613279429503, -141.2500000013656063, 4.591703134518083651 ) ) ;
#21411 = CARTESIAN_POINT ( 'NONE',  ( -4.458734124999999437, -22.39583333196773651, -2.574251347313719407 ) ) ;
#21412 = CARTESIAN_POINT ( 'NONE',  ( 2.229367062499998831, -65.89583333196773651, -3.861377020970580887 ) ) ;
#21413 = CARTESIAN_POINT ( 'NONE',  ( 6.158835246850667461E-14, 8.749999999999998224, -4.999999999999999112 ) ) ;
#21414 = CARTESIAN_POINT ( 'NONE',  ( -3.152548672688508926E-16, -19.56249999863440081, -5.148502694627439702 ) ) ;
#21415 = DIRECTION ( 'NONE',  ( 1.000000000000000000, 0.000000000000000000, 0.000000000000000000 ) ) ;
#21416 = CARTESIAN_POINT ( 'NONE',  ( 3.535533905932738197, -151.8750000000000000, -3.535533905932738197 ) ) ;
#21417 = CARTESIAN_POINT ( 'NONE',  ( -5.000000000000000000, -11.00000000000000355, 0.000000000000000000 ) ) ;
#21418 = CARTESIAN_POINT ( 'NONE',  ( 4.458734125000000326, -153.3750000013656347, -1.846868145590734978 ) ) ;
#21419 = ORIENTED_EDGE ( 'NONE', *, *, #58890, .T. ) ;
#21420 = CARTESIAN_POINT ( 'NONE',  ( 9.457646018065525792E-16, -51.31249999863440792, 5.148502694627439702 ) ) ;
#21421 = DIRECTION ( 'NONE',  ( -0.000000000000000000, 1.000000000000000000, -0.000000000000000000 ) ) ;
#21422 = CARTESIAN_POINT ( 'NONE',  ( -59.81910112700024484, -136.1875000000000284, -2.462841084822808835 ) ) ;
#21423 = CARTESIAN_POINT ( 'NONE',  ( -2.229367062500000163, -89.47916666530106511, -3.861377020970580443 ) ) ;
#21424 = AXIS2_PLACEMENT_3D ( 'NONE', #39083, #28495, #19789 ) ;
#21425 = CARTESIAN_POINT ( 'NONE',  ( 2.229367062500001939, 2.020833334698927786, 3.861377020970579999 ) ) ;
#21426 = CARTESIAN_POINT ( 'NONE',  ( 1.339745962155499015, -95.58034179853029855, 5.000000000000065725 ) ) ;
#21427 = CARTESIAN_POINT ( 'NONE',  ( 1.339745962155612702, -17.29465819873852084, -5.000000000000000000 ) ) ;
#21428 = CARTESIAN_POINT ( 'NONE',  ( 4.458734125000001214, 14.85416666803225993, 2.574251347313718519 ) ) ;
#21429 = CARTESIAN_POINT ( 'NONE',  ( 1.060575238724906964E-15, 2.375000002731185500, 5.773502691896257311 ) ) ;
#21430 = EDGE_LOOP ( 'NONE', ( #23129, #36220, #9228, #22829 ) ) ;
#21431 = CARTESIAN_POINT ( 'NONE',  ( -1.339745962155613812, 7.794658198738521726, -5.000000000000000000 ) ) ;
#21432 = ORIENTED_EDGE ( 'NONE', *, *, #38998, .T. ) ;
#21433 = CARTESIAN_POINT ( 'NONE',  ( 2.499999999999998668, 26.66666666666666430, -4.330127018922193649 ) ) ;
#21434 = CARTESIAN_POINT ( 'NONE',  ( 2.229367062500001939, -45.97916666530106511, 3.861377020970579999 ) ) ;
#21435 = CARTESIAN_POINT ( 'NONE',  ( -3.152801135295367985, -164.0625000013656063, 3.152801135295367096 ) ) ;
#21436 = EDGE_CURVE ( 'NONE', #28232, #8173, #56551, .T. ) ;
#21437 = CARTESIAN_POINT ( 'NONE',  ( -2.500000000000000444, -40.04166666393548013, -4.330127018922193649 ) ) ;
#21438 = ORIENTED_EDGE ( 'NONE', *, *, #63327, .F. ) ;
#21439 = CARTESIAN_POINT ( 'NONE',  ( -2.229367062500000163, -16.47916666530107577, -3.861377020970580443 ) ) ;
#21440 = ORIENTED_EDGE ( 'NONE', *, *, #22095, .T. ) ;
#21441 =( BOUNDED_CURVE ( )  B_SPLINE_CURVE ( 2, ( #13679, #38131, #55631, #47769, #1923, #37817, #55940, #57756, #26982 ),
 .UNSPECIFIED., .F., .F. ) 
 B_SPLINE_CURVE_WITH_KNOTS ( ( 3, 2, 2, 2, 3 ),
 ( 0.8982142857142857428, 0.8988095238095238360, 0.9000000000000000222, 0.9011904761904762085, 0.9017857142857143016 ),
 .UNSPECIFIED. ) 
 CURVE ( )  GEOMETRIC_REPRESENTATION_ITEM ( )  RATIONAL_B_SPLINE_CURVE ( ( 0.9330127018922194093, 0.9330127018922194093, 1.000000000000000000, 0.8660254037844387076, 1.000000000000000000, 0.8660254037844387076, 1.000000000000000000, 0.9330127018922194093, 0.9330127018922194093 ) ) 
 REPRESENTATION_ITEM ( '' )  );
#21442 = CYLINDRICAL_SURFACE ( 'NONE', #32692, 5.000000000000000000 ) ;
#21443 = CARTESIAN_POINT ( 'NONE',  ( -3.152801135295367096, -164.0625000013656063, -3.152801135295367541 ) ) ;
#21444 =( BOUNDED_CURVE ( )  B_SPLINE_CURVE ( 2, ( #18807, #13680, #13369, #42315, #61955 ),
 .UNSPECIFIED., .F., .F. ) 
 B_SPLINE_CURVE_WITH_KNOTS ( ( 3, 2, 3 ),
 ( 0.000000000000000000, 0.004166666666666670078, 0.008333333333333340157 ),
 .UNSPECIFIED. ) 
 CURVE ( )  GEOMETRIC_REPRESENTATION_ITEM ( )  RATIONAL_B_SPLINE_CURVE ( ( 1.000000000000000000, 0.9238795325112867385, 1.000000000000000000, 0.9238795325112866275, 1.000000000000000222 ) ) 
 REPRESENTATION_ITEM ( '' )  );
#21445 = AXIS2_PLACEMENT_3D ( 'NONE', #47518, #32411, #33051 ) ;
#21446 = CARTESIAN_POINT ( 'NONE',  ( -5.000000000000000000, -84.95833333060215864, -2.886751345948128211 ) ) ;
#21448 = ORIENTED_EDGE ( 'NONE', *, *, #59503, .F. ) ;
#21447 = CARTESIAN_POINT ( 'NONE',  ( -6.972266317189433020E-16, -61.12499999726880162, -5.000000000000000000 ) ) ;
#21449 = CARTESIAN_POINT ( 'NONE',  ( -51.19402409849444524, -141.5000000000000284, -3.242614290531456334 ) ) ;
#21450 = AXIS2_PLACEMENT_3D ( 'NONE', #56730, #21993, #8465 ) ;
#21451 = CARTESIAN_POINT ( 'NONE',  ( -4.458734124999998549, -31.47916666530107221, 2.574251347313722516 ) ) ;
#21452 = CARTESIAN_POINT ( 'NONE',  ( -1.339745962155613812, 19.91965820146970501, -5.000000000000000000 ) ) ;
#21453 = ORIENTED_EDGE ( 'NONE', *, *, #22568, .T. ) ;
#21454 = CARTESIAN_POINT ( 'NONE',  ( 4.458734124999999437, -79.81249999863440792, -5.460374474430324690E-16 ) ) ;
#21455 = CARTESIAN_POINT ( 'NONE',  ( 4.458734124999998549, 29.27083333469892423, -2.574251347313721627 ) ) ;
#21456 = CARTESIAN_POINT ( 'NONE',  ( -1.127183054612291972E-14, 24.37500000273118417, 4.999999999999999112 ) ) ;
#21457 = EDGE_LOOP ( 'NONE', ( #30693, #24022, #11883, #31068 ) ) ;
#21458 = DIRECTION ( 'NONE',  ( -0.000000000000000000, 1.000000000000000000, -0.000000000000000000 ) ) ;
#21459 = CARTESIAN_POINT ( 'NONE',  ( -55.35523342533222291, -142.5625000013656063, 4.444560631937231499 ) ) ;
#21460 = CARTESIAN_POINT ( 'NONE',  ( -2.229367062499996610, -82.39583333196773651, 3.861377020970582219 ) ) ;
#21461 = CARTESIAN_POINT ( 'NONE',  ( -58.80597590150559739, -135.1250000027312410, 3.242614290531460330 ) ) ;
#21462 = CARTESIAN_POINT ( 'NONE',  ( 1.339745962155612702, 0.8303418039926664385, -5.000000000000000000 ) ) ;
#21463 = CARTESIAN_POINT ( 'NONE',  ( 1.846868145590736310, -142.8750000013656063, 4.458734124999997661 ) ) ;
#21464 = CARTESIAN_POINT ( 'NONE',  ( -9.184850993605147944E-16, -145.3750000027312126, 5.000000000000000000 ) ) ;
#21465 = CARTESIAN_POINT ( 'NONE',  ( -3.152548672688508926E-16, -49.56249999863441502, -5.148502694627439702 ) ) ;
#21466 = CARTESIAN_POINT ( 'NONE',  ( -4.458734124999999437, -46.39583333196774362, -2.574251347313719407 ) ) ;
#21467 = CARTESIAN_POINT ( 'NONE',  ( 2.229367062500001939, 29.02083333469892779, 3.861377020970579999 ) ) ;
#21468 = CARTESIAN_POINT ( 'NONE',  ( 5.000000000000000000, -108.4166666666666572, -2.886751345948129988 ) ) ;
#21469 = CARTESIAN_POINT ( 'NONE',  ( -6.972266317189433020E-16, 18.74999999999999645, -5.000000000000000000 ) ) ;
#21470 = CARTESIAN_POINT ( 'NONE',  ( 4.458734125000001214, -38.14583333196773651, 2.574251347313718519 ) ) ;
#21471 = CARTESIAN_POINT ( 'NONE',  ( 2.499999999999998668, 3.791666669397852019, -4.330127018922193649 ) ) ;
#21472 = CARTESIAN_POINT ( 'NONE',  ( 5.000000000000000000, -50.50000000000000000, -6.123233995736766282E-16 ) ) ;
#21473 = CARTESIAN_POINT ( 'NONE',  ( -57.89159099828107458, -130.6875000013656063, -3.393966926194107447 ) ) ;
#21474 =( BOUNDED_CURVE ( )  B_SPLINE_CURVE ( 2, ( #38947, #34434, #10324, #59544, #5187, #6469, #16106, #54062, #24803 ),
 .UNSPECIFIED., .F., .F. ) 
 B_SPLINE_CURVE_WITH_KNOTS ( ( 3, 2, 2, 2, 3 ),
 ( 0.5687499999999999778, 0.5694444444444444198, 0.5708333333333333037, 0.5722222222222221877, 0.5729166666666666297 ),
 .UNSPECIFIED. ) 
 CURVE ( )  GEOMETRIC_REPRESENTATION_ITEM ( )  RATIONAL_B_SPLINE_CURVE ( ( 0.9330127018922194093, 0.9330127018922194093, 1.000000000000000000, 0.8660254037844387076, 1.000000000000000000, 0.8660254037844387076, 1.000000000000000000, 0.9330127018922194093, 0.9330127018922194093 ) ) 
 REPRESENTATION_ITEM ( '' )  );
#21475 = CARTESIAN_POINT ( 'NONE',  ( 4.458734124999998549, -80.97916666530106511, -2.574251347313721627 ) ) ;
#21476 = CARTESIAN_POINT ( 'NONE',  ( -58.80597590150559739, -142.1250000027312126, 3.242614290531460330 ) ) ;
#21477 = CARTESIAN_POINT ( 'NONE',  ( 9.457646018065525792E-16, -95.06249999863440792, 5.148502694627439702 ) ) ;
#21478 = FACE_OUTER_BOUND ( 'NONE', #880, .T. ) ;
#21479 = CARTESIAN_POINT ( 'NONE',  ( -4.458734124999999437, -0.6458333319677399542, -2.574251347313719407 ) ) ;
#21480 = ORIENTED_EDGE ( 'NONE', *, *, #38543, .T. ) ;
#21481 = CARTESIAN_POINT ( 'NONE',  ( 0.000000000000000000, -170.0000000000000000, 5.000000000000000000 ) ) ;
#21482 = CARTESIAN_POINT ( 'NONE',  ( 2.500000000000002220, -47.66666666666666430, 4.330127018922192761 ) ) ;
#21483 = CARTESIAN_POINT ( 'NONE',  ( -4.458734124999999437, -89.31249999863440792, 0.000000000000000000 ) ) ;
#21484 = CARTESIAN_POINT ( 'NONE',  ( -3.535533905932737309, -167.7500000027312126, -3.535533905932738197 ) ) ;
#21485 = CARTESIAN_POINT ( 'NONE',  ( -2.229367062500000163, -86.72916666530107932, -3.861377020970580443 ) ) ;
#21486 = CARTESIAN_POINT ( 'NONE',  ( -4.458734124999999437, 14.35416666803226171, -2.574251347313719407 ) ) ;
#21487 = CARTESIAN_POINT ( 'NONE',  ( 5.000000000000000000, -77.37499999726881583, -6.123233995736766282E-16 ) ) ;
#21488 = CARTESIAN_POINT ( 'NONE',  ( -59.59170313451811296, -133.5000000013656347, 1.485763867205729394 ) ) ;
#21489 = CARTESIAN_POINT ( 'NONE',  ( 4.458734125000000326, -4.895833331967740065, 2.574251347313718519 ) ) ;
#21490 = CARTESIAN_POINT ( 'NONE',  ( -4.458734124999999437, 18.43750000136559564, 0.000000000000000000 ) ) ;
#21491 = CARTESIAN_POINT ( 'NONE',  ( -4.458734124999997661, -50.47916666530107221, 2.574251347313722516 ) ) ;
#21492 = CARTESIAN_POINT ( 'NONE',  ( 1.975475456537005874E-15, -7.624999997268812280, 5.000000000000000000 ) ) ;
#21493 = CARTESIAN_POINT ( 'NONE',  ( -4.458734124999999437, -84.39583333196773651, -2.574251347313719407 ) ) ;
#21494 = CARTESIAN_POINT ( 'NONE',  ( -4.458734124999997661, -2.229166665301068662, 2.574251347313722516 ) ) ;
#21495 = CARTESIAN_POINT ( 'NONE',  ( 1.975475456537005874E-15, -43.62499999726880873, 5.000000000000000000 ) ) ;
#21496 = VERTEX_POINT ( 'NONE', #62005 ) ;
#21497 = CARTESIAN_POINT ( 'NONE',  ( -4.458734124999997661, -28.47916666530107221, 2.574251347313722516 ) ) ;
#21498 =( GEOMETRIC_REPRESENTATION_CONTEXT ( 3 ) GLOBAL_UNCERTAINTY_ASSIGNED_CONTEXT ( ( #14618 ) ) GLOBAL_UNIT_ASSIGNED_CONTEXT ( ( #20010, #19373, #58929 ) ) REPRESENTATION_CONTEXT ( 'NONE', 'WORKASPACE' ) );
#21499 =( BOUNDED_CURVE ( )  B_SPLINE_CURVE ( 2, ( #9675, #10319, #63413, #10631, #38625, #38944, #58580, #45051, #26714 ),
 .UNSPECIFIED., .F., .F. ) 
 B_SPLINE_CURVE_WITH_KNOTS ( ( 3, 2, 2, 2, 3 ),
 ( 0.9124999999999999778, 0.9130952380952380709, 0.9142857142857142572, 0.9154761904761904434, 0.9160714285714285365 ),
 .UNSPECIFIED. ) 
 CURVE ( )  GEOMETRIC_REPRESENTATION_ITEM ( )  RATIONAL_B_SPLINE_CURVE ( ( 0.9330127018922194093, 0.9330127018922194093, 1.000000000000000000, 0.8660254037844387076, 1.000000000000000000, 0.8660254037844387076, 1.000000000000000000, 0.9330127018922194093, 0.9330127018922194093 ) ) 
 REPRESENTATION_ITEM ( '' )  );
#21500 = CARTESIAN_POINT ( 'NONE',  ( -51.60603307380591787, -133.1875000013656063, -2.891590998281053704 ) ) ;
#21501 = CARTESIAN_POINT ( 'NONE',  ( -2.229367062500000163, -76.47916666530106511, -3.861377020970580443 ) ) ;
#21502 = CARTESIAN_POINT ( 'NONE',  ( 4.458734124999998549, 29.02083333469893134, -2.574251347313721627 ) ) ;
#21503 = ADVANCED_FACE ( 'NONE', ( #52033 ), #52967, .T. ) ;
#21504 = AXIS2_PLACEMENT_3D ( 'NONE', #1220, #34976, #45254 ) ;
#21505 = CARTESIAN_POINT ( 'NONE',  ( 4.458734125000001214, 21.10416666803226349, 2.574251347313718519 ) ) ;
#21506 = CARTESIAN_POINT ( 'NONE',  ( -5.000000000000000000, -43.95833333060214443, -2.886751345948128211 ) ) ;
#21507 = CARTESIAN_POINT ( 'NONE',  ( 4.458734124999999437, -77.06249999863440792, -5.460374474430324690E-16 ) ) ;
#21508 = CARTESIAN_POINT ( 'NONE',  ( 5.000000000000000000, -64.41666666666667140, -2.886751345948129988 ) ) ;
#21509 = CARTESIAN_POINT ( 'NONE',  ( 5.000000000000000888, -36.45833333060213732, 2.886751345948126879 ) ) ;
#21510 = CARTESIAN_POINT ( 'NONE',  ( -3.535250795749689387E-16, 23.87500000273118417, -5.773502691896257311 ) ) ;
#21511 = VERTEX_POINT ( 'NONE', #27573 ) ;
#21512 = DIRECTION ( 'NONE',  ( -0.000000000000000000, 1.000000000000000000, -0.000000000000000000 ) ) ;
#21513 = CARTESIAN_POINT ( 'NONE',  ( -2.499999999999996447, 9.166666666666666075, 4.330127018922195425 ) ) ;
#21515 = CARTESIAN_POINT ( 'NONE',  ( -3.535250795749689387E-16, -21.24999999999999645, -5.773502691896257311 ) ) ;
#21514 = CARTESIAN_POINT ( 'NONE',  ( 2.500000000000002220, -0.6666666666666660745, 4.330127018922192761 ) ) ;
#21516 = CARTESIAN_POINT ( 'NONE',  ( 2.229367062500001939, -26.97916666530106866, 3.861377020970579999 ) ) ;
#21517 = CARTESIAN_POINT ( 'NONE',  ( 2.229367062499998831, -87.64583333196773651, -3.861377020970580887 ) ) ;
#21518 = CARTESIAN_POINT ( 'NONE',  ( 5.000000000000000000, -25.37499999726881583, -6.123233995736766282E-16 ) ) ;
#21520 = ORIENTED_EDGE ( 'NONE', *, *, #3507, .T. ) ;
#21519 = CARTESIAN_POINT ( 'NONE',  ( -3.152548672688508926E-16, -54.56249999863439371, -5.148502694627439702 ) ) ;
#21521 = DIRECTION ( 'NONE',  ( -0.000000000000000000, 1.000000000000000000, -0.000000000000000000 ) ) ;
#21522 = CARTESIAN_POINT ( 'NONE',  ( -1.975475456537005874E-15, 27.37500000273118417, 5.000000000000000000 ) ) ;
#21524 = VERTEX_POINT ( 'NONE', #61375 ) ;
#21523 = CARTESIAN_POINT ( 'NONE',  ( 4.458734124999999437, -2.062499998634406584, -5.460374474430324690E-16 ) ) ;
#21525 = CARTESIAN_POINT ( 'NONE',  ( 5.000000000000000000, -72.50000000000000000, -6.123233995736766282E-16 ) ) ;
#21526 = CARTESIAN_POINT ( 'NONE',  ( -51.60603307380591787, -139.9375000013656063, -2.891590998281053704 ) ) ;
#21527 = CARTESIAN_POINT ( 'NONE',  ( -4.458734124999998549, -47.47916666530106511, 2.574251347313722516 ) ) ;
#21528 = CARTESIAN_POINT ( 'NONE',  ( 5.000000000000000000, -34.41666666666666430, -2.886751345948130876 ) ) ;
#21529 = CARTESIAN_POINT ( 'NONE',  ( 2.071067811865476394, -160.1875000000000000, 5.000000000000000000 ) ) ;
#21530 = CARTESIAN_POINT ( 'NONE',  ( -5.000000000000000000, -70.95833333060214443, -2.886751345948128211 ) ) ;
#21531 = CARTESIAN_POINT ( 'NONE',  ( -4.999999999999998224, -21.79166666393548368, 2.886751345948131764 ) ) ;
#21532 = CARTESIAN_POINT ( 'NONE',  ( -56.66612745406270335, -153.3125000000000000, -5.149110718188516067 ) ) ;
#21533 = CARTESIAN_POINT ( 'NONE',  ( -2.229367062499996610, -15.39583333196773651, 3.861377020970582219 ) ) ;
#21534 = CARTESIAN_POINT ( 'NONE',  ( -3.152548672688508926E-16, -52.81249999863440792, -5.148502694627439702 ) ) ;
#21535 = CARTESIAN_POINT ( 'NONE',  ( 1.975475456537005874E-15, -65.62499999726881583, 5.000000000000000000 ) ) ;
#21536 = SHAPE_REPRESENTATION_RELATIONSHIP ( 'NONE' , 'NONE' ,  #49651, #60912 ) ;
#21537 = CARTESIAN_POINT ( 'NONE',  ( -1.846868145590734756, -145.1250000013655779, -4.458734125000000326 ) ) ;
#21538 = CARTESIAN_POINT ( 'NONE',  ( -4.458734124999999437, -92.64583333196773651, -2.574251347313719407 ) ) ;
#21539 = FACE_OUTER_BOUND ( 'NONE', #32704, .T. ) ;
#21540 = ORIENTED_EDGE ( 'NONE', *, *, #58971, .F. ) ;
#21541 = CARTESIAN_POINT ( 'NONE',  ( -3.535533905932738641, -155.3750000000000000, 3.535533905932737309 ) ) ;
#21542 = CARTESIAN_POINT ( 'NONE',  ( 9.457646018065525792E-16, 26.68750000136559564, 5.148502694627439702 ) ) ;
#21543 = CARTESIAN_POINT ( 'NONE',  ( -53.33387254593733928, -144.9375000027312126, 5.149110718188519620 ) ) ;
#21544 = FACE_OUTER_BOUND ( 'NONE', #43116, .T. ) ;
#21545 = VECTOR ( 'NONE', #55438, 1000.000000000000000 ) ;
#21546 = CARTESIAN_POINT ( 'NONE',  ( 4.458734124999999437, -2.812499998634407472, -5.460374474430324690E-16 ) ) ;
#21547 = CARTESIAN_POINT ( 'NONE',  ( 2.730187237215162345E-16, -149.4375000013656063, -4.458734124999999437 ) ) ;
#21548 = CARTESIAN_POINT ( 'NONE',  ( 9.457646018065525792E-16, -23.31249999863440436, 5.148502694627439702 ) ) ;
#21549 = CARTESIAN_POINT ( 'NONE',  ( 4.458734125000001214, -65.14583333196773651, 2.574251347313718519 ) ) ;
#21550 = CARTESIAN_POINT ( 'NONE',  ( -5.000000000000000000, -83.87499999726880162, 0.000000000000000000 ) ) ;
#21551 = CARTESIAN_POINT ( 'NONE',  ( -4.458734124999998549, -9.229166665301068662, 2.574251347313722516 ) ) ;
#21552 = CARTESIAN_POINT ( 'NONE',  ( 2.500000000000002220, 6.458333336064519870, 4.330127018922192761 ) ) ;
#21553 = CARTESIAN_POINT ( 'NONE',  ( -1.846868145590734756, -144.1250000013655779, -4.458734124999999437 ) ) ;
#21554 = CARTESIAN_POINT ( 'NONE',  ( -2.229367062500000163, 13.27083333469892779, -3.861377020970580443 ) ) ;
#21555 = VERTEX_POINT ( 'NONE', #42049 ) ;
#21556 = CARTESIAN_POINT ( 'NONE',  ( 0.000000000000000000, -170.0000000000000000, 0.000000000000000000 ) ) ;
#21557 = DIRECTION ( 'NONE',  ( -0.000000000000000000, 1.000000000000000000, -0.000000000000000000 ) ) ;
#21559 = CARTESIAN_POINT ( 'NONE',  ( 2.229367062500001939, -17.97916666530106866, 3.861377020970579999 ) ) ;
#21558 = CARTESIAN_POINT ( 'NONE',  ( 2.499999999999998668, -84.33333333333332860, -4.330127018922193649 ) ) ;
#21560 = CARTESIAN_POINT ( 'NONE',  ( 6.123233995736766282E-16, -120.0000000000000000, -5.000000000000000000 ) ) ;
#21561 = CARTESIAN_POINT ( 'NONE',  ( -58.24261429053147765, -138.2500000000000000, -3.805975901505573855 ) ) ;
#21562 = CARTESIAN_POINT ( 'NONE',  ( -59.44456063193725015, -148.5625000013656063, -0.3552334253322034230 ) ) ;
#21563 = CARTESIAN_POINT ( 'NONE',  ( 2.499999999999998668, -44.20833333060214443, -4.330127018922193649 ) ) ;
#21564 = CARTESIAN_POINT ( 'NONE',  ( 2.500000000000002220, -24.66666666666666430, 4.330127018922192761 ) ) ;
#21565 = CARTESIAN_POINT ( 'NONE',  ( -2.229367062499996610, 9.854166668032261711, 3.861377020970582219 ) ) ;
#21566 = CARTESIAN_POINT ( 'NONE',  ( -2.500000000000000444, -63.04166666393547303, -4.330127018922193649 ) ) ;
#21567 = CARTESIAN_POINT ( 'NONE',  ( -6.972266317189433020E-16, -15.25000000000000000, -5.000000000000000000 ) ) ;
#21568 = CARTESIAN_POINT ( 'NONE',  ( -4.458734124999999437, 12.60416666803226349, -2.574251347313719407 ) ) ;
#21569 = CARTESIAN_POINT ( 'NONE',  ( -2.229367062499996610, -66.14583333196773651, 3.861377020970582219 ) ) ;
#21570 = CARTESIAN_POINT ( 'NONE',  ( 4.458734124999999437, -15.06249999863440436, -5.460374474430324690E-16 ) ) ;
#21571 = CARTESIAN_POINT ( 'NONE',  ( 5.000000000000000888, -0.5833333333333350357, 2.886751345948126879 ) ) ;
#21572 = CARTESIAN_POINT ( 'NONE',  ( 1.846868145590735200, -162.2500000013656347, -4.458734125000000326 ) ) ;
#21573 = CARTESIAN_POINT ( 'NONE',  ( 2.229367062500001939, -56.97916666530107932, 3.861377020970579999 ) ) ;
#21574 = CARTESIAN_POINT ( 'NONE',  ( 2.499999999999998668, -97.20833333060213022, -4.330127018922193649 ) ) ;
#21575 = EDGE_CURVE ( 'NONE', #7616, #1762, #10754, .T. ) ;
#21576 =( BOUNDED_CURVE ( )  B_SPLINE_CURVE ( 2, ( #23264, #18432, #63137, #48635, #57989, #48323, #38053, #4574, #43805 ),
 .UNSPECIFIED., .F., .F. ) 
 B_SPLINE_CURVE_WITH_KNOTS ( ( 3, 2, 2, 2, 3 ),
 ( 0.5416666666666671848, 0.5458333333333338366, 0.5500000000000004885, 0.5541666666666671404, 0.5583333333333337922 ),
 .UNSPECIFIED. ) 
 CURVE ( )  GEOMETRIC_REPRESENTATION_ITEM ( )  RATIONAL_B_SPLINE_CURVE ( ( 0.9999999999999898970, 0.9238795325112968415, 1.000000000000000000, 0.9238795325112867385, 1.000000000000000000, 0.9238795325112867385, 1.000000000000000000, 0.9238795325112786339, 1.000000000000008216 ) ) 
 REPRESENTATION_ITEM ( '' )  );
#21577 = CARTESIAN_POINT ( 'NONE',  ( -1.339745962155613812, -28.20534180126147916, -5.000000000000000000 ) ) ;
#21578 = CARTESIAN_POINT ( 'NONE',  ( -5.000000000000000000, -88.95833333060214443, -2.886751345948128211 ) ) ;
#21579 = CARTESIAN_POINT ( 'NONE',  ( -3.152548672688508926E-16, -34.56249999863440792, -5.148502694627439702 ) ) ;
#21580 = CARTESIAN_POINT ( 'NONE',  ( 5.000000000000000888, -60.58333333333332860, 2.886751345948126879 ) ) ;
#21581 = CARTESIAN_POINT ( 'NONE',  ( -4.999999999999999112, -49.91666666666666430, 2.886751345948131764 ) ) ;
#21582 = CARTESIAN_POINT ( 'NONE',  ( 6.123233995736766282E-16, -170.0000000000000000, -5.000000000000000000 ) ) ;
#21583 = CARTESIAN_POINT ( 'NONE',  ( 2.499999999999998668, -17.20833333060214443, -4.330127018922193649 ) ) ;
#21584 = ORIENTED_EDGE ( 'NONE', *, *, #32699, .F. ) ;
#21585 = CARTESIAN_POINT ( 'NONE',  ( -4.458734124999999437, -107.3958333319677365, -2.574251347313719407 ) ) ;
#21586 = CARTESIAN_POINT ( 'NONE',  ( -3.152548672688508926E-16, -0.8124999986344055847, -5.148502694627439702 ) ) ;
#21587 = CARTESIAN_POINT ( 'NONE',  ( 5.000000000000000000, -89.29166666393547303, -2.886751345948130876 ) ) ;
#21588 = CARTESIAN_POINT ( 'NONE',  ( -3.535250795749689387E-16, -8.250000000000000000, -5.773502691896257311 ) ) ;
#21589 = VECTOR ( 'NONE', #28208, 1000.000000000000000 ) ;
#21590 = CARTESIAN_POINT ( 'NONE',  ( 9.457646018065525792E-16, -74.06249999863440792, 5.148502694627439702 ) ) ;
#21592 = DIRECTION ( 'NONE',  ( 0.000000000000000000, 0.000000000000000000, 1.000000000000000000 ) ) ;
#21591 =( BOUNDED_CURVE ( )  B_SPLINE_CURVE ( 2, ( #27119, #16829, #2678, #17476, #21980, #27424, #42850, #28059, #7507 ),
 .UNSPECIFIED., .F., .F. ) 
 B_SPLINE_CURVE_WITH_KNOTS ( ( 3, 2, 2, 2, 3 ),
 ( 0.4553571428571428492, 0.4559523809523809423, 0.4571428571428571286, 0.4583333333333333148, 0.4589285714285714080 ),
 .UNSPECIFIED. ) 
 CURVE ( )  GEOMETRIC_REPRESENTATION_ITEM ( )  RATIONAL_B_SPLINE_CURVE ( ( 0.9330127018922194093, 0.9330127018922194093, 1.000000000000000000, 0.8660254037844387076, 1.000000000000000000, 0.8660254037844387076, 1.000000000000000000, 0.9330127018922194093, 0.9330127018922194093 ) ) 
 REPRESENTATION_ITEM ( '' )  );
#21593 = EDGE_CURVE ( 'NONE', #14094, #38980, #41665, .T. ) ;
#21594 = CARTESIAN_POINT ( 'NONE',  ( -2.499999999999996447, -9.708333330602146205, 4.330127018922195425 ) ) ;
#21596 = ORIENTED_EDGE ( 'NONE', *, *, #62196, .T. ) ;
#21595 = CARTESIAN_POINT ( 'NONE',  ( 2.229367062499998831, -40.64583333196773651, -3.861377020970580887 ) ) ;
#21597 = CARTESIAN_POINT ( 'NONE',  ( -5.000000000000000000, 28.04166666939785202, -2.886751345948128211 ) ) ;
#21598 = ADVANCED_FACE ( 'NONE', ( #27266 ), #3462, .T. ) ;
#21600 = ORIENTED_EDGE ( 'NONE', *, *, #16225, .T. ) ;
#21599 = CARTESIAN_POINT ( 'NONE',  ( 4.458734124999999437, 13.93750000136559386, -5.460374474430324690E-16 ) ) ;
#21601 = CARTESIAN_POINT ( 'NONE',  ( -4.999999999999998224, -55.79166666393548013, 2.886751345948131764 ) ) ;
#21602 = CARTESIAN_POINT ( 'NONE',  ( -4.999999999999999112, -54.91666666666667140, 2.886751345948131764 ) ) ;
#21603 = CARTESIAN_POINT ( 'NONE',  ( -3.152548672688508926E-16, -30.81249999863440436, -5.148502694627439702 ) ) ;
#21604 = CARTESIAN_POINT ( 'NONE',  ( 1.975475456537005874E-15, -86.75000000000001421, 5.000000000000000000 ) ) ;
#21605 = CARTESIAN_POINT ( 'NONE',  ( 4.458734124999999437, -75.81249999863440792, -5.460374474430324690E-16 ) ) ;
#21606 = CARTESIAN_POINT ( 'NONE',  ( 4.458734125000000326, -140.6250000013656063, -1.846868145590734978 ) ) ;
#21607 = CARTESIAN_POINT ( 'NONE',  ( 4.458734125000001214, -86.89583333196773651, 2.574251347313718519 ) ) ;
#21608 = CARTESIAN_POINT ( 'NONE',  ( -59.29741812935640155, -135.8750000013655779, -2.196230717870135685 ) ) ;
#21609 = EDGE_CURVE ( 'NONE', #42590, #2645, #48138, .T. ) ;
#21610 = CARTESIAN_POINT ( 'NONE',  ( -3.152548672688508926E-16, -33.81249999863440792, -5.148502694627439702 ) ) ;
#21611 = CARTESIAN_POINT ( 'NONE',  ( 5.000000000000000000, -16.37499999726881228, -6.123233995736766282E-16 ) ) ;
#21612 = ORIENTED_EDGE ( 'NONE', *, *, #27440, .F. ) ;
#21613 = CARTESIAN_POINT ( 'NONE',  ( -2.229367062500000163, -79.72916666530106511, -3.861377020970580443 ) ) ;
#21614 = CARTESIAN_POINT ( 'NONE',  ( -5.000000000000000000, 22.04166666939785202, -2.886751345948128211 ) ) ;
#21615 = ORIENTED_EDGE ( 'NONE', *, *, #22761, .T. ) ;
#21616 = CARTESIAN_POINT ( 'NONE',  ( -1.049326080737009628E-13, -3.624999997268818053, 5.000000000000000000 ) ) ;
#21617 = CARTESIAN_POINT ( 'NONE',  ( -2.499999999999996447, -11.70833333060214798, 4.330127018922195425 ) ) ;
#21618 = CARTESIAN_POINT ( 'NONE',  ( 4.458734124999999437, -66.06249999863440792, -5.460374474430324690E-16 ) ) ;
#21619 = CARTESIAN_POINT ( 'NONE',  ( -4.458734124999999437, -11.56249999863440792, 0.000000000000000000 ) ) ;
#21620 = ORIENTED_EDGE ( 'NONE', *, *, #22183, .T. ) ;
#21621 = CYLINDRICAL_SURFACE ( 'NONE', #27642, 5.000000000000000000 ) ;
#21622 = DIRECTION ( 'NONE',  ( -0.000000000000000000, 1.000000000000000000, -0.000000000000000000 ) ) ;
#21623 = VERTEX_POINT ( 'NONE', #23075 ) ;
#21624 = EDGE_CURVE ( 'NONE', #49905, #45912, #60932, .T. ) ;
#21625 = CARTESIAN_POINT ( 'NONE',  ( 2.229367062499998831, -7.895833331967735624, -3.861377020970580887 ) ) ;
#21626 = CARTESIAN_POINT ( 'NONE',  ( 2.229367062500001939, 8.020833334698926009, 3.861377020970579999 ) ) ;
#21627 = AXIS2_PLACEMENT_3D ( 'NONE', #10615, #21557, #60483 ) ;
#21628 = CARTESIAN_POINT ( 'NONE',  ( -6.972266317189433020E-16, -60.12499999726880162, -5.000000000000000000 ) ) ;
#21629 = CARTESIAN_POINT ( 'NONE',  ( 1.846868145590735200, -157.2500000013656063, -4.458734124999999437 ) ) ;
#21630 = CYLINDRICAL_SURFACE ( 'NONE', #14214, 5.000000000000000000 ) ;
#21631 = ORIENTED_EDGE ( 'NONE', *, *, #48877, .T. ) ;
#21632 = CARTESIAN_POINT ( 'NONE',  ( 9.457646018065525792E-16, -87.06249999863439371, 5.148502694627439702 ) ) ;
#21633 = CYLINDRICAL_SURFACE ( 'NONE', #9952, 5.000000000000000000 ) ;
#21634 = CARTESIAN_POINT ( 'NONE',  ( 4.458734125000001214, -2.895833331967738289, 2.574251347313718519 ) ) ;
#21635 = LINE ( 'NONE', #26134, #40638 ) ;
#21636 = CARTESIAN_POINT ( 'NONE',  ( -5.000000000000000000, -31.87499999726880873, 0.000000000000000000 ) ) ;
#21637 = CARTESIAN_POINT ( 'NONE',  ( -55.00000000000002132, 15.00000000000000000, 5.000000000000000000 ) ) ;
#21638 = CARTESIAN_POINT ( 'NONE',  ( -4.458734124999999437, 24.60416666803225993, -2.574251347313719407 ) ) ;
#21639 = CARTESIAN_POINT ( 'NONE',  ( -6.972266317189433020E-16, -56.25000000000000000, -5.000000000000000000 ) ) ;
#21640 = CARTESIAN_POINT ( 'NONE',  ( -3.152548672688508926E-16, 29.43750000136559564, -5.148502694627439702 ) ) ;
#21641 = CARTESIAN_POINT ( 'NONE',  ( -3.152548672688508926E-16, -53.56249999863439371, -5.148502694627439702 ) ) ;
#21642 = CARTESIAN_POINT ( 'NONE',  ( 4.458734125000000326, -38.14583333196773651, 2.574251347313718519 ) ) ;
#21643 = CARTESIAN_POINT ( 'NONE',  ( 9.457646018065525792E-16, 2.687500001365593860, 5.148502694627439702 ) ) ;
#21644 =( BOUNDED_CURVE ( )  B_SPLINE_CURVE ( 2, ( #35032, #50464, #40159, #55923, #7035, #59802, #30834, #35342, #21828 ),
 .UNSPECIFIED., .F., .F. ) 
 B_SPLINE_CURVE_WITH_KNOTS ( ( 3, 2, 2, 2, 3 ),
 ( 0.2520833333333333259, 0.2527777777777777679, 0.2541666666666666519, 0.2555555555555555358, 0.2562499999999999778 ),
 .UNSPECIFIED. ) 
 CURVE ( )  GEOMETRIC_REPRESENTATION_ITEM ( )  RATIONAL_B_SPLINE_CURVE ( ( 0.9330127018922194093, 0.9330127018922194093, 1.000000000000000000, 0.8660254037844387076, 1.000000000000000000, 0.8660254037844387076, 1.000000000000000000, 0.9330127018922194093, 0.9330127018922194093 ) ) 
 REPRESENTATION_ITEM ( '' )  );
#21645 = DIRECTION ( 'NONE',  ( -0.000000000000000000, -0.000000000000000000, 1.000000000000000000 ) ) ;
#21646 = CARTESIAN_POINT ( 'NONE',  ( -2.499999999999996447, 13.16666666666666607, 4.330127018922195425 ) ) ;
#21647 = CARTESIAN_POINT ( 'NONE',  ( 5.000000000000000000, -145.1250000027312126, 0.000000000000000000 ) ) ;
#21648 = CARTESIAN_POINT ( 'NONE',  ( 5.000000000000000888, -33.45833333060215153, 2.886751345948126879 ) ) ;
#21649 = CARTESIAN_POINT ( 'NONE',  ( 4.458734124999998549, -40.72916666530107221, -2.574251347313721627 ) ) ;
#21650 = CARTESIAN_POINT ( 'NONE',  ( -3.535250795749689387E-16, -78.12499999726880162, -5.773502691896257311 ) ) ;
#21651 = EDGE_CURVE ( 'NONE', #50712, #21367, #50202, .T. ) ;
#21652 = CARTESIAN_POINT ( 'NONE',  ( -57.19623071787017210, -140.6250000013656063, 4.297418129356382899 ) ) ;
#21653 = DIRECTION ( 'NONE',  ( -0.000000000000000000, 1.000000000000000000, -0.000000000000000000 ) ) ;
#21654 = EDGE_CURVE ( 'NONE', #37904, #62207, #3814, .T. ) ;
#21655 = LINE ( 'NONE', #60582, #23384 ) ;
#21656 = EDGE_CURVE ( 'NONE', #21511, #30690, #15386, .T. ) ;
#21657 = CARTESIAN_POINT ( 'NONE',  ( 4.458734125000000326, -86.14583333196775072, 2.574251347313718519 ) ) ;
#21658 = CARTESIAN_POINT ( 'NONE',  ( 4.458734124999999437, -161.6250000013656063, -1.846868145590734978 ) ) ;
#21659 = CARTESIAN_POINT ( 'NONE',  ( 2.499999999999998668, 7.666666666666665186, -4.330127018922193649 ) ) ;
#21660 = CARTESIAN_POINT ( 'NONE',  ( 5.000000000000000000, -30.41666666666666785, -2.886751345948129988 ) ) ;
#21661 = CARTESIAN_POINT ( 'NONE',  ( 4.458734124999999437, -140.5000000013656347, 1.846868145590737864 ) ) ;
#21662 = ORIENTED_EDGE ( 'NONE', *, *, #33067, .F. ) ;
#21663 = CARTESIAN_POINT ( 'NONE',  ( 4.458734124999999437, 21.93750000136559208, -5.460374474430324690E-16 ) ) ;
#21664 = ORIENTED_EDGE ( 'NONE', *, *, #38995, .T. ) ;
#21665 = CARTESIAN_POINT ( 'NONE',  ( -2.229367062499996610, -91.14583333196773651, 3.861377020970582219 ) ) ;
#21666 = CARTESIAN_POINT ( 'NONE',  ( 2.229367062500001939, 11.77083333469892601, 3.861377020970579999 ) ) ;
#21667 = CARTESIAN_POINT ( 'NONE',  ( -5.000000000000000000, 16.12500000273118417, 0.000000000000000000 ) ) ;
#21668 = CARTESIAN_POINT ( 'NONE',  ( 1.975475456537005874E-15, -89.74999999999998579, 5.000000000000000000 ) ) ;
#21669 = CARTESIAN_POINT ( 'NONE',  ( -5.000000000000000000, 7.916666666666665186, -2.886751345948128211 ) ) ;
#21670 = ADVANCED_FACE ( 'NONE', ( #18859 ), #38789, .T. ) ;
#21671 = CARTESIAN_POINT ( 'NONE',  ( -4.458734124999999437, -58.39583333196773651, -2.574251347313719407 ) ) ;
#21672 = CARTESIAN_POINT ( 'NONE',  ( 4.458734125000001214, -10.89583333196773651, 2.574251347313718519 ) ) ;
#21673 = CARTESIAN_POINT ( 'NONE',  ( 7.500000000000000000, -3.202733125947433201, -7.213074474936314928 ) ) ;
#21674 = CARTESIAN_POINT ( 'NONE',  ( -4.999999999999998224, -109.9166666666666572, 2.886751345948131764 ) ) ;
#21675 = CARTESIAN_POINT ( 'NONE',  ( 5.000000000000000000, -1.500000000000001332, -6.123233995736766282E-16 ) ) ;
#21676 = EDGE_CURVE ( 'NONE', #6165, #18131, #4292, .T. ) ;
#21677 = CARTESIAN_POINT ( 'NONE',  ( -1.339745962155613812, -75.08034179853029855, -5.000000000000000000 ) ) ;
#21678 = CARTESIAN_POINT ( 'NONE',  ( -4.999999999999999112, -40.91666666666667140, 2.886751345948131764 ) ) ;
#21679 = AXIS2_PLACEMENT_3D ( 'NONE', #57332, #38012, #57644 ) ;
#21680 =( BOUNDED_CURVE ( )  B_SPLINE_CURVE ( 2, ( #36092, #11633, #2327, #11952, #16788, #7149, #59917, #30298, #41216 ),
 .UNSPECIFIED., .F., .F. ) 
 B_SPLINE_CURVE_WITH_KNOTS ( ( 3, 2, 2, 2, 3 ),
 ( 0.8696428571428571619, 0.8702380952380952550, 0.8714285714285714413, 0.8726190476190476275, 0.8732142857142857206 ),
 .UNSPECIFIED. ) 
 CURVE ( )  GEOMETRIC_REPRESENTATION_ITEM ( )  RATIONAL_B_SPLINE_CURVE ( ( 0.9330127018922194093, 0.9330127018922194093, 1.000000000000000000, 0.8660254037844387076, 1.000000000000000000, 0.8660254037844387076, 1.000000000000000000, 0.9330127018922194093, 0.9330127018922194093 ) ) 
 REPRESENTATION_ITEM ( '' )  );
#21682 = CARTESIAN_POINT ( 'NONE',  ( -2.229367062500000163, -14.72916666530107221, -3.861377020970580443 ) ) ;
#21681 = CARTESIAN_POINT ( 'NONE',  ( 1.975475456537005874E-15, -42.75000000000000000, 5.000000000000000000 ) ) ;
#21683 = CARTESIAN_POINT ( 'NONE',  ( 0.000000000000000000, -170.0000000000000000, 0.000000000000000000 ) ) ;
#21684 = CARTESIAN_POINT ( 'NONE',  ( 4.458734125000001214, -60.89583333196774362, 2.574251347313718519 ) ) ;
#21685 = CARTESIAN_POINT ( 'NONE',  ( -4.458734125000000326, -153.2500000013655779, -1.846868145590735644 ) ) ;
#21686 = CARTESIAN_POINT ( 'NONE',  ( -3.152548672688508926E-16, -69.56249999863439371, -5.148502694627439702 ) ) ;
#21687 = CARTESIAN_POINT ( 'NONE',  ( -53.51423613279429503, -146.5000000013656347, 4.591703134518082763 ) ) ;
#21688 = CARTESIAN_POINT ( 'NONE',  ( -4.458734124999998549, -17.47916666530106866, 2.574251347313722516 ) ) ;
#21689 = CARTESIAN_POINT ( 'NONE',  ( 2.500000000000002220, -62.54166666393547303, 4.330127018922192761 ) ) ;
#21690 = ORIENTED_EDGE ( 'NONE', *, *, #47647, .T. ) ;
#21691 = CARTESIAN_POINT ( 'NONE',  ( 5.000000000000000000, -85.29166666393547303, -2.886751345948130876 ) ) ;
#21692 = VERTEX_POINT ( 'NONE', #9218 ) ;
#21693 = CARTESIAN_POINT ( 'NONE',  ( 4.458734125000001214, -61.14583333196773651, 2.574251347313718519 ) ) ;
#21695 = CARTESIAN_POINT ( 'NONE',  ( 5.000000000000000000, -58.41666666666665719, -2.886751345948130876 ) ) ;
#21694 = CARTESIAN_POINT ( 'NONE',  ( -9.184850993605147944E-16, -157.3750000027311842, 5.000000000000000000 ) ) ;
#21696 = CARTESIAN_POINT ( 'NONE',  ( -1.846868145590737420, -150.7500000013655779, 4.458734124999999437 ) ) ;
#21697 = VERTEX_POINT ( 'NONE', #48454 ) ;
#21698 = CARTESIAN_POINT ( 'NONE',  ( -6.972266317189433020E-16, -24.12499999726881228, -5.000000000000000000 ) ) ;
#21699 = CARTESIAN_POINT ( 'NONE',  ( -54.60164318462004474, -126.3750000000000142, -4.984105922594373794 ) ) ;
#21700 = DIRECTION ( 'NONE',  ( 0.000000000000000000, 0.000000000000000000, 1.000000000000000000 ) ) ;
#21701 = CARTESIAN_POINT ( 'NONE',  ( 9.457646018065525792E-16, -46.31249999863440792, 5.148502694627439702 ) ) ;
#21702 = ORIENTED_EDGE ( 'NONE', *, *, #14576, .F. ) ;
#21703 = CARTESIAN_POINT ( 'NONE',  ( 1.339745962155615144, 11.29465819873851906, 4.999999999999999112 ) ) ;
#21704 = CARTESIAN_POINT ( 'NONE',  ( 4.458734125000001214, 8.104166668032261711, 2.574251347313718519 ) ) ;
#21705 = CARTESIAN_POINT ( 'NONE',  ( 4.458734124999998549, 23.27083333469892423, -2.574251347313721627 ) ) ;
#21706 = CARTESIAN_POINT ( 'NONE',  ( -54.64476657466781973, -149.8125000013656063, -4.444560631937228834 ) ) ;
#21707 = CARTESIAN_POINT ( 'NONE',  ( -2.480964764533239819E-13, -108.6249999972688016, 5.000000000000000000 ) ) ;
#21708 = CARTESIAN_POINT ( 'NONE',  ( 7.500000000000000000, 4.330127018922190096, -7.422398894150032511 ) ) ;
#21709 = EDGE_LOOP ( 'NONE', ( #8520, #4909, #13557, #2159, #59036, #20261, #43393, #40659, #36100, #48118, #12565, #34887, #61947, #19594, #43564, #13459, #53851, #4651, #58351, #43024, #57437, #35984, #33794, #33295, #39719, #48173, #25048, #20679, #37584, #56712, #49649, #16849, #27151, #60040, #41624, #18945, #50708, #50631, #59907, #34396, #22332, #32326, #16933, #30114, #21856, #60467, #25225, #37329, #21740, #57523, #53682, #12291, #25158, #21612, #25092, #479, #32846, #61563, #9543, #31155, #48524, #3057, #45566, #63610, #24913, #46032, #54364, #61245, #27224, #8448, #51740, #15455, #48074, #27738, #18738, #18676, #38987, #39301, #4749, #10034, #16037, #60425, #26512, #58254, #57849, #32566, #40734, #14677, #34793, #25478, #21065, #56187, #50074, #15562, #42314, #40316, #3787, #29971, #26798, #57207, #36382, #43056, #17883, #32113, #4037, #43153, #44939, #32459, #54910, #36340, #61321, #18407, #25705, #56877, #27596, #41600, #20649, #2961, #7459, #45594, #21376, #44850, #45615, #28549, #38911, #25623, #44601, #36369, #56980, #40082, #17921, #18149, #49364, #42903, #17802, #33448, #48450, #37427, #45873, #8282, #28165, #5685, #10903, #54010, #59377, #8532, #21220, #51801, #7150, #35679, #16538, #57615, #53487, #37485, #14697, #10020, #22343, #16008, #6683, #26130, #51016, #45493, #358, #57990, #52713, #37444, #15830, #13686, #49680, #59905, #53869, #40687, #3737, #40009, #32436, #28927, #40076, #40126, #15800, #16888, #50206, #48342, #63183, #31243, #52549, #22157, #15407, #49281, #15193, #47188, #30368, #26351, #50391, #14679, #1358, #4336, #49001, #55085, #53053, #18802, #35572, #20060, #43713, #32986, #555, #17236, #62895, #28021, #12809, #62134, #15140, #48162, #39540, #6620, #11609, #28473, #29472, #3391, #46768, #40339, #33083, #18840, #34260, #27305, #30360, #2927, #29327, #41191, #6509, #21448, #1686, #54502, #35908, #12911, #44551, #29891, #60328, #38512, #16511, #32498, #6325, #44264, #6084, #956, #28130, #38606, #40102, #35350, #19992, #42385, #32306, #28469, #3411, #44383, #30780, #20882, #22232, #12347, #58228, #47327, #28363, #48321, #25358, #35284, #47872, #42713, #6757, #18743, #18254, #28012, #45941, #21662, #24721, #49671, #35709, #43009, #27007, #51288, #16765, #25639, #1161, #50065, #13976, #16305 ) ) ;
#21710 = CARTESIAN_POINT ( 'NONE',  ( 9.457646018065525792E-16, -70.06249999863439371, 5.148502694627439702 ) ) ;
#21711 = CARTESIAN_POINT ( 'NONE',  ( 3.061616997868383141E-16, -169.7500000000000000, -5.000000000000000000 ) ) ;
#21712 = CARTESIAN_POINT ( 'NONE',  ( 4.458734124999999437, 10.18750000136559386, -5.460374474430324690E-16 ) ) ;
#21713 = CARTESIAN_POINT ( 'NONE',  ( -5.000000000000000000, -69.87499999726880162, 0.000000000000000000 ) ) ;
#21714 = FACE_OUTER_BOUND ( 'NONE', #9097, .T. ) ;
#21715 = CARTESIAN_POINT ( 'NONE',  ( 9.457646018065525792E-16, -54.31249999863440081, 5.148502694627439702 ) ) ;
#21716 = CARTESIAN_POINT ( 'NONE',  ( 2.499999999999998668, -12.20833333060214798, -4.330127018922193649 ) ) ;
#21717 = DIRECTION ( 'NONE',  ( -0.000000000000000000, 1.000000000000000000, -0.000000000000000000 ) ) ;
#21718 = DIRECTION ( 'NONE',  ( -0.000000000000000000, 1.000000000000000000, -0.000000000000000000 ) ) ;
#21719 = CARTESIAN_POINT ( 'NONE',  ( 5.000000000000000888, -65.58333333333332860, 2.886751345948126879 ) ) ;
#21720 = CARTESIAN_POINT ( 'NONE',  ( 4.458734124999998549, -21.97916666530107221, -2.574251347313721627 ) ) ;
#21721 = EDGE_LOOP ( 'NONE', ( #60147, #13752, #34778, #12468 ) ) ;
#21722 = CARTESIAN_POINT ( 'NONE',  ( -1.339745962155613812, -102.2053418012614827, -5.000000000000000000 ) ) ;
#21723 = CARTESIAN_POINT ( 'NONE',  ( -4.458734124999999437, -107.3958333319677365, -2.574251347313719407 ) ) ;
#21724 = CARTESIAN_POINT ( 'NONE',  ( -5.000000000000000888, -157.6875000027312126, -2.071067811865475949 ) ) ;
#21725 = EDGE_LOOP ( 'NONE', ( #43230, #48061, #33703, #49347 ) ) ;
#21726 = CARTESIAN_POINT ( 'NONE',  ( 4.458734124999999437, -101.0624999986344079, -5.460374474430324690E-16 ) ) ;
#21727 = CARTESIAN_POINT ( 'NONE',  ( -3.152548672688508926E-16, -27.56249999863440081, -5.148502694627439702 ) ) ;
#21728 = CARTESIAN_POINT ( 'NONE',  ( 2.500000000000002220, -64.54166666393547303, 4.330127018922192761 ) ) ;
#21729 = CARTESIAN_POINT ( 'NONE',  ( -51.60603307380591787, -151.1875000013656063, -2.891590998281053704 ) ) ;
#21730 = CARTESIAN_POINT ( 'NONE',  ( -51.60603307380591787, -141.9375000013656063, -2.891590998281053704 ) ) ;
#21731 = ADVANCED_FACE ( 'NONE', ( #30093 ), #16961, .F. ) ;
#21732 = CARTESIAN_POINT ( 'NONE',  ( -4.458734124999999437, -21.39583333196774007, -2.574251347313719407 ) ) ;
#21733 = CARTESIAN_POINT ( 'NONE',  ( 4.458734124999998549, -67.97916666530106511, -2.574251347313721627 ) ) ;
#21734 = FACE_OUTER_BOUND ( 'NONE', #45672, .T. ) ;
#21735 = CARTESIAN_POINT ( 'NONE',  ( 4.458734124999998549, -26.72916666530106866, -2.574251347313721627 ) ) ;
#21736 = CARTESIAN_POINT ( 'NONE',  ( 2.071067811865560326, -146.8125000000000000, -4.999999999999914735 ) ) ;
#21737 = CARTESIAN_POINT ( 'NONE',  ( -2.071067811865475061, -149.6875000000000000, -5.000000000000000888 ) ) ;
#21738 = CARTESIAN_POINT ( 'NONE',  ( -4.999999999999999112, -12.91666666666666785, 2.886751345948131764 ) ) ;
#21739 = CARTESIAN_POINT ( 'NONE',  ( 2.730187237215162345E-16, -153.1875000013656063, -4.458734124999999437 ) ) ;
#21740 = ORIENTED_EDGE ( 'NONE', *, *, #57459, .F. ) ;
#21741 = CARTESIAN_POINT ( 'NONE',  ( -4.458734124999999437, -50.64583333196773651, -2.574251347313719407 ) ) ;
#21742 = EDGE_CURVE ( 'NONE', #38436, #62035, #30082, .T. ) ;
#21743 = FACE_OUTER_BOUND ( 'NONE', #1375, .T. ) ;
#21744 = DIRECTION ( 'NONE',  ( 0.000000000000000000, 0.000000000000000000, 1.000000000000000000 ) ) ;
#21745 = CARTESIAN_POINT ( 'NONE',  ( 1.060575238724906964E-15, 25.25000000000000355, 5.773502691896257311 ) ) ;
#21746 = EDGE_CURVE ( 'NONE', #24993, #53062, #48245, .T. ) ;
#21747 = CARTESIAN_POINT ( 'NONE',  ( 1.339745962155608039, 25.29465819873851729, 5.000000000000003553 ) ) ;
#21748 = CARTESIAN_POINT ( 'NONE',  ( 4.458734124999999437, 3.187500001365594304, -5.460374474430324690E-16 ) ) ;
#21749 = CARTESIAN_POINT ( 'NONE',  ( -5.000000000000000000, -142.5000000000000284, -6.123233995736766282E-16 ) ) ;
#21750 = CARTESIAN_POINT ( 'NONE',  ( 1.339745962155612702, -41.16965819600732601, -5.000000000000000000 ) ) ;
#21751 = DIRECTION ( 'NONE',  ( -0.000000000000000000, 1.000000000000000000, -0.000000000000000000 ) ) ;
#21752 = CARTESIAN_POINT ( 'NONE',  ( 2.229367062499998831, 14.10416666803226171, -3.861377020970580887 ) ) ;
#21753 = CARTESIAN_POINT ( 'NONE',  ( -2.499999999999996447, 2.291666669397850686, 4.330127018922195425 ) ) ;
#21755 = EDGE_LOOP ( 'NONE', ( #59184, #44605, #8780, #57994 ) ) ;
#21754 = EDGE_CURVE ( 'NONE', #26446, #41301, #25281, .T. ) ;
#21756 = LINE ( 'NONE', #18794, #56170 ) ;
#21757 = VERTEX_POINT ( 'NONE', #60351 ) ;
#21758 = CARTESIAN_POINT ( 'NONE',  ( 0.000000000000000000, -120.0000000000000000, 0.000000000000000000 ) ) ;
#21759 = CARTESIAN_POINT ( 'NONE',  ( -3.152548672688508926E-16, -43.56249999863440081, -5.148502694627439702 ) ) ;
#21760 = EDGE_CURVE ( 'NONE', #34735, #37487, #36522, .T. ) ;
#21761 = CARTESIAN_POINT ( 'NONE',  ( 3.152801135295367541, -162.5625000013656063, -3.152801135295367541 ) ) ;
#21762 = EDGE_CURVE ( 'NONE', #41671, #5841, #19004, .T. ) ;
#21763 = CARTESIAN_POINT ( 'NONE',  ( 5.000000000000000888, -45.45833333060214443, 2.886751345948126879 ) ) ;
#21764 = EDGE_LOOP ( 'NONE', ( #5380, #29460, #7282, #33203 ) ) ;
#21765 = CARTESIAN_POINT ( 'NONE',  ( -4.458734124999998549, -18.22916666530107221, 2.574251347313722516 ) ) ;
#21766 = ORIENTED_EDGE ( 'NONE', *, *, #51519, .T. ) ;
#21767 = CARTESIAN_POINT ( 'NONE',  ( -2.499999999999996447, -87.83333333333332860, 4.330127018922195425 ) ) ;
#21768 = CARTESIAN_POINT ( 'NONE',  ( 3.152801135295367541, -165.3125000013656063, -3.152801135295367541 ) ) ;
#21770 = VERTEX_POINT ( 'NONE', #31699 ) ;
#21769 = CARTESIAN_POINT ( 'NONE',  ( -1.339745962155613812, -19.20534180126147916, -5.000000000000000000 ) ) ;
#21771 = CARTESIAN_POINT ( 'NONE',  ( -53.33387254593733928, -137.8125000000000000, 5.149110718188519620 ) ) ;
#21772 = CARTESIAN_POINT ( 'NONE',  ( -2.229367062500000163, -33.72916666530107221, -3.861377020970580443 ) ) ;
#21773 = CARTESIAN_POINT ( 'NONE',  ( -4.999999999999998224, -38.91666666666667140, 2.886751345948131764 ) ) ;
#21774 = EDGE_LOOP ( 'NONE', ( #15112, #52162, #44595, #56960, #61007, #10595, #60510, #13627, #8705, #31538, #47624, #12358, #11775, #53630, #23620, #7564, #12349, #26578, #55307, #3402, #23891, #39737, #55894, #36228, #1704, #20886, #56037, #386, #17945, #49234, #36066, #5040, #4176, #12023, #48801, #3716, #61857, #5123, #11771, #5217, #31646, #38879, #43155, #24301, #22326, #36793, #35753, #20711, #23168, #4736, #17738, #6714, #51977, #8711, #41595, #27514, #37494, #30758, #18655, #60589, #15671, #2421, #39830, #33175, #53735, #44346, #2121, #8757, #37580, #56774, #40653, #13117, #43501, #5272, #60591, #54826, #18166, #56609, #49268, #20604, #60116, #18437, #10758, #12103, #15125, #7063, #53624, #37674, #8943, #50885, #32759, #24569, #45239, #24056, #35776, #35819, #39770, #27535, #8614, #50649, #25956, #63361, #41349, #51984, #47049, #9791, #6117, #43873, #25083, #41411, #23972, #13452, #58809, #61083, #3656, #56338, #15693, #31334, #28904, #34400, #37576, #46922, #2108, #843, #11449, #54101, #11698, #47322, #39546, #22552, #20090, #5939, #16153, #38851, #29156, #12739, #19186, #2406, #4189, #43021, #35557, #41094, #8197, #37543, #33055, #45736, #7400, #5764, #9900, #1030, #26571, #109, #8090, #22088, #60055, #19368, #8133, #28222, #63205, #33099, #12501, #20462, #54356, #3974, #44426, #6417, #48619, #40041, #35786, #1600, #19492, #33675, #9644, #40177, #1982, #48720, #55846, #57168, #17278, #20713, #56805, #705, #56000, #35400, #36414, #19979, #28517, #46295, #45562, #42139, #22993, #53177, #11437, #55855, #22801, #4506, #37492, #18433, #47080, #13515, #60370, #40664, #16646, #42702, #5554, #38982, #4041, #39384, #41604, #15344, #20662, #29604, #3965, #30434, #46666, #63573, #56812, #56368, #38458, #25077, #34167, #8790, #54259, #14061, #53294, #46418, #1954, #19520, #1283, #53223, #54509, #48906, #58865, #31323, #35430, #620, #15985, #57058, #61630, #34534, #31070, #46585, #52692, #22494 ) ) ;
#21775 =( BOUNDED_CURVE ( )  B_SPLINE_CURVE ( 2, ( #59188, #35376, #40830, #26361, #6441, #20909, #336, #50812, #5789 ),
 .UNSPECIFIED., .F., .F. ) 
 B_SPLINE_CURVE_WITH_KNOTS ( ( 3, 2, 2, 2, 3 ),
 ( 0.2160714285714285809, 0.2166666666666666741, 0.2178571428571428603, 0.2190476190476190466, 0.2196428571428571397 ),
 .UNSPECIFIED. ) 
 CURVE ( )  GEOMETRIC_REPRESENTATION_ITEM ( )  RATIONAL_B_SPLINE_CURVE ( ( 0.9330127018922194093, 0.9330127018922194093, 1.000000000000000000, 0.8660254037844387076, 1.000000000000000000, 0.8660254037844387076, 1.000000000000000000, 0.9330127018922194093, 0.9330127018922194093 ) ) 
 REPRESENTATION_ITEM ( '' )  );
#21776 = CARTESIAN_POINT ( 'NONE',  ( 4.458734125000001214, -77.89583333196773651, 2.574251347313718519 ) ) ;
#21777 = CARTESIAN_POINT ( 'NONE',  ( -4.458734124999999437, 26.60416666803225993, -2.574251347313719407 ) ) ;
#21778 = CARTESIAN_POINT ( 'NONE',  ( 2.500000000000002220, -18.66666666666666430, 4.330127018922192761 ) ) ;
#21779 = ORIENTED_EDGE ( 'NONE', *, *, #22892, .F. ) ;
#21780 = DIRECTION ( 'NONE',  ( -0.000000000000000000, 1.000000000000000000, -0.000000000000000000 ) ) ;
#21781 = CARTESIAN_POINT ( 'NONE',  ( -54.64476657466781973, -144.0625000013656063, -4.444560631937228834 ) ) ;
#21782 = CARTESIAN_POINT ( 'NONE',  ( 2.229367062500001939, -80.22916666530106511, 3.861377020970579999 ) ) ;
#21783 = CARTESIAN_POINT ( 'NONE',  ( -60.14911071818854538, -130.1875000027312410, 1.666127454062681368 ) ) ;
#21784 = CARTESIAN_POINT ( 'NONE',  ( -9.184850993605147944E-16, -143.2500000000000284, 5.000000000000000000 ) ) ;
#21785 = CARTESIAN_POINT ( 'NONE',  ( -3.152801135295367985, -142.0625000013655779, 3.152801135295367096 ) ) ;
#21786 = CARTESIAN_POINT ( 'NONE',  ( 2.229367062500001939, -56.97916666530107932, 3.861377020970579999 ) ) ;
#21787 = CARTESIAN_POINT ( 'NONE',  ( -2.229367062499996610, -47.14583333196774362, 3.861377020970582219 ) ) ;
#21788 = CARTESIAN_POINT ( 'NONE',  ( 4.458734125000001214, 27.10416666803225993, 2.574251347313718519 ) ) ;
#21789 = CARTESIAN_POINT ( 'NONE',  ( 2.500000000000002220, -108.6666666666666572, 4.330127018922192761 ) ) ;
#21790 = CARTESIAN_POINT ( 'NONE',  ( 1.975475456537005874E-15, 16.37500000273118417, 5.000000000000000000 ) ) ;
#21791 = CARTESIAN_POINT ( 'NONE',  ( -4.458734124999999437, -37.56249999863440792, 0.000000000000000000 ) ) ;
#21792 = CARTESIAN_POINT ( 'NONE',  ( 1.060575238724906964E-15, 1.375000002731184834, 5.773502691896257311 ) ) ;
#21793 = CARTESIAN_POINT ( 'NONE',  ( 3.061616997868383141E-16, -153.8750000027311842, -5.000000000000000000 ) ) ;
#21794 = CARTESIAN_POINT ( 'NONE',  ( -52.10840900171896806, -129.1875000013656063, 3.393966926194110556 ) ) ;
#21795 = CARTESIAN_POINT ( 'NONE',  ( -4.458734124999999437, -78.64583333196773651, -2.574251347313719407 ) ) ;
#21796 = CARTESIAN_POINT ( 'NONE',  ( 1.339745962155619807, 24.70534180126147916, -4.999999999999996447 ) ) ;
#21797 = CARTESIAN_POINT ( 'NONE',  ( 2.229367062500001939, -96.97916666530105090, 3.861377020970579999 ) ) ;
#21798 = CARTESIAN_POINT ( 'NONE',  ( -4.458734124999999437, -3.645833331967739177, -2.574251347313719407 ) ) ;
#21799 = ORIENTED_EDGE ( 'NONE', *, *, #5255, .T. ) ;
#21800 = DIRECTION ( 'NONE',  ( 0.000000000000000000, 0.000000000000000000, 1.000000000000000000 ) ) ;
#21801 = CYLINDRICAL_SURFACE ( 'NONE', #60666, 5.000000000000000000 ) ;
#21802 = CARTESIAN_POINT ( 'NONE',  ( 4.458734124999998549, -89.72916666530106511, -2.574251347313721627 ) ) ;
#21803 = CARTESIAN_POINT ( 'NONE',  ( -5.000000000000000888, -168.6875000027311842, -2.071067811865475949 ) ) ;
#21804 = CARTESIAN_POINT ( 'NONE',  ( 4.458734124999999437, -89.06249999863439371, -5.460374474430324690E-16 ) ) ;
#21805 = CARTESIAN_POINT ( 'NONE',  ( 4.458734124999999437, 13.93750000136559386, -5.460374474430324690E-16 ) ) ;
#21806 = CYLINDRICAL_SURFACE ( 'NONE', #19179, 5.000000000000000000 ) ;
#21807 = CARTESIAN_POINT ( 'NONE',  ( -50.40829686548195099, -134.0000000013656063, -1.485763867205728284 ) ) ;
#21808 = CARTESIAN_POINT ( 'NONE',  ( 4.458734125000000326, -8.895833331967736513, 2.574251347313718519 ) ) ;
#21809 = CARTESIAN_POINT ( 'NONE',  ( -2.229367062500000163, 19.27083333469892779, -3.861377020970580443 ) ) ;
#21810 = CARTESIAN_POINT ( 'NONE',  ( 2.229367062499998831, -50.89583333196772941, -3.861377020970580887 ) ) ;
#21811 = CARTESIAN_POINT ( 'NONE',  ( 1.975475456537005874E-15, -11.74999999999999645, 5.000000000000000000 ) ) ;
#21812 = CARTESIAN_POINT ( 'NONE',  ( -4.458734124999999437, -87.39583333196773651, -2.574251347313719407 ) ) ;
#21813 = CARTESIAN_POINT ( 'NONE',  ( 4.458734125000000326, -8.895833331967736513, 2.574251347313718519 ) ) ;
#21814 = ORIENTED_EDGE ( 'NONE', *, *, #44439, .F. ) ;
#21815 = CARTESIAN_POINT ( 'NONE',  ( -4.458734124999997661, -36.47916666530107221, 2.574251347313722516 ) ) ;
#21816 = CARTESIAN_POINT ( 'NONE',  ( -51.60603307380591787, -129.1875000013656063, -2.891590998281053704 ) ) ;
#21817 = CARTESIAN_POINT ( 'NONE',  ( 2.229367062500001939, -78.97916666530106511, 3.861377020970579999 ) ) ;
#21818 = CARTESIAN_POINT ( 'NONE',  ( 5.000000000000000000, -108.2916666639354730, -2.886751345948129988 ) ) ;
#21819 = CARTESIAN_POINT ( 'NONE',  ( -2.229367062499996610, 17.85416666803225993, 3.861377020970582219 ) ) ;
#21820 = CARTESIAN_POINT ( 'NONE',  ( -2.500000000000000444, -58.04166666393548013, -4.330127018922193649 ) ) ;
#21821 = FACE_OUTER_BOUND ( 'NONE', #24746, .T. ) ;
#21822 = CARTESIAN_POINT ( 'NONE',  ( -4.458734124999999437, -83.56249999863439371, 0.000000000000000000 ) ) ;
#21823 = CARTESIAN_POINT ( 'NONE',  ( -3.535250795749689387E-16, -67.25000000000000000, -5.773502691896257311 ) ) ;
#21824 =( BOUNDED_CURVE ( )  B_SPLINE_CURVE ( 2, ( #8695, #48866, #4811, #23175, #44036, #37973, #63367, #28307, #42786 ),
 .UNSPECIFIED., .F., .F. ) 
 B_SPLINE_CURVE_WITH_KNOTS ( ( 3, 2, 2, 2, 3 ),
 ( 0.1416666666666667740, 0.1458333333333334814, 0.1500000000000001332, 0.1541666666666668406, 0.1583333333333334925 ),
 .UNSPECIFIED. ) 
 CURVE ( )  GEOMETRIC_REPRESENTATION_ITEM ( )  RATIONAL_B_SPLINE_CURVE ( ( 0.9999999999999980016, 0.9238795325112887369, 1.000000000000000000, 0.9238795325112867385, 1.000000000000000000, 0.9238795325112867385, 1.000000000000000000, 0.9238795325112837409, 1.000000000000003109 ) ) 
 REPRESENTATION_ITEM ( '' )  );
#21825 = DIRECTION ( 'NONE',  ( -0.8660254037844384856, 0.000000000000000000, 0.5000000000000001110 ) ) ;
#21826 = CARTESIAN_POINT ( 'NONE',  ( 5.000000000000000000, 17.62500000273118417, -6.123233995736766282E-16 ) ) ;
#21827 = ORIENTED_EDGE ( 'NONE', *, *, #45248, .T. ) ;
#21828 = CARTESIAN_POINT ( 'NONE',  ( 1.975475456537005874E-15, -1.624999997268813834, 5.000000000000000000 ) ) ;
#21829 =( BOUNDED_CURVE ( )  B_SPLINE_CURVE ( 2, ( #62321, #55993, #50842, #13107, #11907, #6784, #26393, #27891, #42680 ),
 .UNSPECIFIED., .F., .F. ) 
 B_SPLINE_CURVE_WITH_KNOTS ( ( 3, 2, 2, 2, 3 ),
 ( 0.1645833333333333315, 0.1652777777777777735, 0.1666666666666666574, 0.1680555555555555691, 0.1687500000000000111 ),
 .UNSPECIFIED. ) 
 CURVE ( )  GEOMETRIC_REPRESENTATION_ITEM ( )  RATIONAL_B_SPLINE_CURVE ( ( 0.9330127018922194093, 0.9330127018922194093, 1.000000000000000000, 0.8660254037844387076, 1.000000000000000000, 0.8660254037844387076, 1.000000000000000000, 0.9330127018922194093, 0.9330127018922194093 ) ) 
 REPRESENTATION_ITEM ( '' )  );
#21830 = CARTESIAN_POINT ( 'NONE',  ( -2.500000000000000444, 8.833333333333332149, -4.330127018922193649 ) ) ;
#21832 = CARTESIAN_POINT ( 'NONE',  ( -2.500000000000000444, -26.16666666666666430, -4.330127018922193649 ) ) ;
#21831 = CARTESIAN_POINT ( 'NONE',  ( -1.339745962155610925, -106.6696581960073189, 5.000000000000000000 ) ) ;
#21833 = CARTESIAN_POINT ( 'NONE',  ( 4.458734124999998549, -26.72916666530106866, -2.574251347313721627 ) ) ;
#21834 = CARTESIAN_POINT ( 'NONE',  ( 9.457646018065525792E-16, -88.06249999863439371, 5.148502694627439702 ) ) ;
#21835 = CARTESIAN_POINT ( 'NONE',  ( -5.000000000000000000, -26.87499999726881583, 0.000000000000000000 ) ) ;
#21837 = ORIENTED_EDGE ( 'NONE', *, *, #61761, .T. ) ;
#21836 = CARTESIAN_POINT ( 'NONE',  ( 4.458734124999999437, -54.81249999863440081, -5.460374474430324690E-16 ) ) ;
#21838 = DIRECTION ( 'NONE',  ( 0.000000000000000000, 1.000000000000000000, 0.000000000000000000 ) ) ;
#21839 = CARTESIAN_POINT ( 'NONE',  ( 5.000000000000000000, -28.41666666666666430, -2.886751345948130876 ) ) ;
#21841 = ORIENTED_EDGE ( 'NONE', *, *, #42224, .T. ) ;
#21840 = CARTESIAN_POINT ( 'NONE',  ( 2.229367062500001939, -1.229166665301071548, 3.861377020970579999 ) ) ;
#21842 = CARTESIAN_POINT ( 'NONE',  ( -3.535250795749689387E-16, -73.25000000000000000, -5.773502691896257311 ) ) ;
#21843 = CARTESIAN_POINT ( 'NONE',  ( -52.80376928212989185, -137.8750000013655779, -4.297418129356378458 ) ) ;
#21844 = CARTESIAN_POINT ( 'NONE',  ( -4.458734124999999437, -53.56249999863439371, 0.000000000000000000 ) ) ;
#21845 = CARTESIAN_POINT ( 'NONE',  ( 2.500000000000002220, -34.66666666666666430, 4.330127018922192761 ) ) ;
#21846 = CARTESIAN_POINT ( 'NONE',  ( 2.499999999999998668, -71.20833333060214443, -4.330127018922193649 ) ) ;
#21847 = CYLINDRICAL_SURFACE ( 'NONE', #1542, 5.000000000000000000 ) ;
#21848 = CARTESIAN_POINT ( 'NONE',  ( -52.53715891517739323, -152.4375000000000284, -4.819101127000233298 ) ) ;
#21849 = CARTESIAN_POINT ( 'NONE',  ( 2.229367062500001939, -17.22916666530106866, 3.861377020970579999 ) ) ;
#21850 = CARTESIAN_POINT ( 'NONE',  ( 2.229367062500001939, -49.22916666530107221, 3.861377020970579999 ) ) ;
#21851 = DIRECTION ( 'NONE',  ( -0.8660254037844382635, 0.5000000000000005551, 0.000000000000000000 ) ) ;
#21852 =( NAMED_UNIT ( * ) SI_UNIT ( $, .STERADIAN. ) SOLID_ANGLE_UNIT ( ) );
#21853 = CARTESIAN_POINT ( 'NONE',  ( 1.846868145590735200, -140.2500000013656063, -4.458734125000000326 ) ) ;
#21854 = CARTESIAN_POINT ( 'NONE',  ( -2.229367062499996610, -96.39583333196773651, 3.861377020970582219 ) ) ;
#21855 = CARTESIAN_POINT ( 'NONE',  ( 5.000000000000000888, -157.9375000000000000, -2.071067811865475505 ) ) ;
#21856 = ORIENTED_EDGE ( 'NONE', *, *, #8596, .F. ) ;
#21857 = CARTESIAN_POINT ( 'NONE',  ( -52.10840900171896806, -154.4375000013656063, 3.393966926194110556 ) ) ;
#21858 = CARTESIAN_POINT ( 'NONE',  ( 2.229367062500001939, 26.77083333469892423, 3.861377020970579999 ) ) ;
#21859 = CARTESIAN_POINT ( 'NONE',  ( -50.18089887299979068, -141.8125000027311842, 2.462841084822635640 ) ) ;
#21860 = DIRECTION ( 'NONE',  ( 0.000000000000000000, 0.000000000000000000, 1.000000000000000000 ) ) ;
#21861 = CARTESIAN_POINT ( 'NONE',  ( -2.229367062499996610, -1.145833331967736957, 3.861377020970582219 ) ) ;
#21862 = CARTESIAN_POINT ( 'NONE',  ( -2.229367062500000163, -94.72916666530106511, -3.861377020970580443 ) ) ;
#21863 = CARTESIAN_POINT ( 'NONE',  ( -1.846868145590737420, -150.0000000013655779, 4.458734124999999437 ) ) ;
#21864 = CARTESIAN_POINT ( 'NONE',  ( -4.458734124999998549, -21.47916666530107221, 2.574251347313722516 ) ) ;
#21865 = CARTESIAN_POINT ( 'NONE',  ( -7.500000000000000000, 4.330127018922191873, -0.9999999999999970024 ) ) ;
#21866 = CARTESIAN_POINT ( 'NONE',  ( -3.152548672688508926E-16, -65.81249999863440792, -5.148502694627439702 ) ) ;
#21867 = CARTESIAN_POINT ( 'NONE',  ( -2.499999999999996447, -83.70833333060214443, 4.330127018922195425 ) ) ;
#21868 = CARTESIAN_POINT ( 'NONE',  ( -10.39117206796836257, 1.272551561242683764E-15, -8.499999999999998224 ) ) ;
#21869 = CARTESIAN_POINT ( 'NONE',  ( -1.846868145590734756, -146.1250000013655779, -4.458734124999999437 ) ) ;
#21870 =( BOUNDED_CURVE ( )  B_SPLINE_CURVE ( 2, ( #39922, #10660, #711, #74, #45079, #59570, #1046, #15503, #20652 ),
 .UNSPECIFIED., .F., .F. ) 
 B_SPLINE_CURVE_WITH_KNOTS ( ( 3, 2, 2, 2, 3 ),
 ( 0.6270833333333333259, 0.6277777777777777679, 0.6291666666666666519, 0.6305555555555555358, 0.6312499999999999778 ),
 .UNSPECIFIED. ) 
 CURVE ( )  GEOMETRIC_REPRESENTATION_ITEM ( )  RATIONAL_B_SPLINE_CURVE ( ( 0.9330127018922194093, 0.9330127018922194093, 1.000000000000000000, 0.8660254037844387076, 1.000000000000000000, 0.8660254037844387076, 1.000000000000000000, 0.9330127018922194093, 0.9330127018922194093 ) ) 
 REPRESENTATION_ITEM ( '' )  );
#21871 = CARTESIAN_POINT ( 'NONE',  ( -3.152548672688508926E-16, 12.18750000136559564, -5.148502694627439702 ) ) ;
#21872 = VERTEX_POINT ( 'NONE', #55528 ) ;
#21873 = CARTESIAN_POINT ( 'NONE',  ( -2.500000000000000444, -53.04166666393548013, -4.330127018922193649 ) ) ;
#21874 = CARTESIAN_POINT ( 'NONE',  ( -5.000000000000000888, -144.5625000000000000, -2.071067811865475949 ) ) ;
#21876 = CARTESIAN_POINT ( 'NONE',  ( -2.229367062499996610, -19.14583333196774007, 3.861377020970582219 ) ) ;
#21875 = CARTESIAN_POINT ( 'NONE',  ( 5.000000000000000000, -84.49999999999998579, -6.123233995736766282E-16 ) ) ;
#21877 = CARTESIAN_POINT ( 'NONE',  ( 4.458734124999998549, 26.02083333469892779, -2.574251347313721627 ) ) ;
#21878 = CARTESIAN_POINT ( 'NONE',  ( -2.499999999999996447, -5.833333333333336590, 4.330127018922195425 ) ) ;
#21879 = CARTESIAN_POINT ( 'NONE',  ( -59.29741812935640155, -147.6250000013655779, -2.196230717870135685 ) ) ;
#21880 = CARTESIAN_POINT ( 'NONE',  ( 1.060575238724906964E-15, -44.62499999726881583, 5.773502691896257311 ) ) ;
#21881 = DIRECTION ( 'NONE',  ( 0.000000000000000000, 0.000000000000000000, 1.000000000000000000 ) ) ;
#21882 = CARTESIAN_POINT ( 'NONE',  ( -2.229367062500000163, 8.520833334698926009, -3.861377020970580443 ) ) ;
#21883 = DIRECTION ( 'NONE',  ( -0.000000000000000000, 1.000000000000000000, -0.000000000000000000 ) ) ;
#21884 = CARTESIAN_POINT ( 'NONE',  ( -6.972266317189433020E-16, -60.12499999726880873, -5.000000000000000000 ) ) ;
#21885 = CARTESIAN_POINT ( 'NONE',  ( -2.229367062500000163, 10.52083333469892779, -3.861377020970580443 ) ) ;
#21886 = CARTESIAN_POINT ( 'NONE',  ( -2.229367062499996610, -65.14583333196773651, 3.861377020970582219 ) ) ;
#21887 = CARTESIAN_POINT ( 'NONE',  ( 4.458734124999998549, -20.97916666530107221, -2.574251347313721627 ) ) ;
#21888 = CARTESIAN_POINT ( 'NONE',  ( -4.999999999999999112, 0.08333333333333457771, 2.886751345948131764 ) ) ;
#21889 = CARTESIAN_POINT ( 'NONE',  ( 3.152801135295366208, -159.5625000013656063, 3.152801135295367985 ) ) ;
#21890 = DIRECTION ( 'NONE',  ( -0.000000000000000000, 1.000000000000000000, -0.000000000000000000 ) ) ;
#21891 = CARTESIAN_POINT ( 'NONE',  ( -4.458734124999999437, -59.31249999863440081, 0.000000000000000000 ) ) ;
#21892 = CARTESIAN_POINT ( 'NONE',  ( -3.535250795749689387E-16, -94.12499999726881583, -5.773502691896257311 ) ) ;
#21893 = CARTESIAN_POINT ( 'NONE',  ( 0.000000000000000000, -120.0000000000000000, 5.000000000000000000 ) ) ;
#21894 = CARTESIAN_POINT ( 'NONE',  ( -4.458734124999999437, -34.39583333196772941, -2.574251347313719407 ) ) ;
#21895 = CYLINDRICAL_SURFACE ( 'NONE', #16352, 5.000000000000000000 ) ;
#21896 = CARTESIAN_POINT ( 'NONE',  ( 5.000000000000000888, -49.58333333333332860, 2.886751345948126879 ) ) ;
#21897 = CARTESIAN_POINT ( 'NONE',  ( 1.975475456537005874E-15, -13.75000000000000000, 5.000000000000000000 ) ) ;
#21898 = CARTESIAN_POINT ( 'NONE',  ( -6.972266317189433020E-16, -89.24999999999998579, -5.000000000000000000 ) ) ;
#21899 = ORIENTED_EDGE ( 'NONE', *, *, #50975, .F. ) ;
#21900 = CARTESIAN_POINT ( 'NONE',  ( -3.152548672688508926E-16, -105.5624999986344079, -5.148502694627439702 ) ) ;
#21901 = CARTESIAN_POINT ( 'NONE',  ( -4.458734124999999437, -0.6458333319677399542, -2.574251347313719407 ) ) ;
#21902 = CARTESIAN_POINT ( 'NONE',  ( 2.071067811865560326, -143.9375000027311842, -4.999999999999914735 ) ) ;
#21903 = CARTESIAN_POINT ( 'NONE',  ( -2.499999999999996447, -8.833333333333332149, 4.330127018922195425 ) ) ;
#21904 = CARTESIAN_POINT ( 'NONE',  ( 4.458734124999999437, -74.81249999863440792, -5.460374474430324690E-16 ) ) ;
#21905 = CARTESIAN_POINT ( 'NONE',  ( -2.499999999999996447, -16.83333333333333215, 4.330127018922195425 ) ) ;
#21906 = CARTESIAN_POINT ( 'NONE',  ( -2.500000000000000444, -8.041666663935481907, -4.330127018922193649 ) ) ;
#21908 = ORIENTED_EDGE ( 'NONE', *, *, #654, .F. ) ;
#21907 = CARTESIAN_POINT ( 'NONE',  ( -3.152548672688508926E-16, -38.56249999863439371, -5.148502694627439702 ) ) ;
#21909 = CARTESIAN_POINT ( 'NONE',  ( -6.972266317189433020E-16, -81.24999999999998579, -5.000000000000000000 ) ) ;
#21911 = EDGE_LOOP ( 'NONE', ( #23341, #29167, #21057, #62524 ) ) ;
#21910 = CARTESIAN_POINT ( 'NONE',  ( 2.229367062499998831, 14.10416666803226171, -3.861377020970580887 ) ) ;
#21912 = CARTESIAN_POINT ( 'NONE',  ( 2.499999999999998668, -81.20833333060213022, -4.330127018922193649 ) ) ;
#21913 = CARTESIAN_POINT ( 'NONE',  ( 5.000000000000000000, -57.41666666666667140, -2.886751345948129988 ) ) ;
#21914 = CARTESIAN_POINT ( 'NONE',  ( 3.152801135295366208, -159.8125000013656063, 3.152801135295367985 ) ) ;
#21915 = CARTESIAN_POINT ( 'NONE',  ( -4.458734124999999437, -30.56249999863440436, 0.000000000000000000 ) ) ;
#21916 = CARTESIAN_POINT ( 'NONE',  ( -1.339745962155613812, -35.20534180126148271, -5.000000000000000000 ) ) ;
#21917 = CARTESIAN_POINT ( 'NONE',  ( 2.229367062500001939, -80.97916666530106511, 3.861377020970579999 ) ) ;
#21918 = CARTESIAN_POINT ( 'NONE',  ( 2.730187237215162345E-16, -141.4375000013656063, -4.458734124999999437 ) ) ;
#21919 = CARTESIAN_POINT ( 'NONE',  ( -4.458734124999998549, -85.22916666530107932, 2.574251347313722516 ) ) ;
#21920 = CARTESIAN_POINT ( 'NONE',  ( -52.10840900171896806, -135.4375000013656063, 3.393966926194110556 ) ) ;
#21921 = CARTESIAN_POINT ( 'NONE',  ( -4.458734124999998549, -0.4791666653010707710, 2.574251347313722516 ) ) ;
#21922 = CARTESIAN_POINT ( 'NONE',  ( -2.229367062499996610, -35.39583333196772941, 3.861377020970582219 ) ) ;
#21923 = CARTESIAN_POINT ( 'NONE',  ( 5.000000000000000000, -70.37499999726880162, -6.123233995736766282E-16 ) ) ;
#21924 = CARTESIAN_POINT ( 'NONE',  ( -4.458734124999999437, -77.64583333196773651, -2.574251347313719407 ) ) ;
#21925 = CARTESIAN_POINT ( 'NONE',  ( 6.123233995736766282E-16, -120.0000000000000000, -5.000000000000000000 ) ) ;
#21926 = ORIENTED_EDGE ( 'NONE', *, *, #37737, .T. ) ;
#21927 = DIRECTION ( 'NONE',  ( -0.000000000000000000, 1.000000000000000000, -0.000000000000000000 ) ) ;
#21928 = CARTESIAN_POINT ( 'NONE',  ( 5.000000000000000888, -151.9375000000000000, -2.071067811865475505 ) ) ;
#21930 = ADVANCED_FACE ( 'NONE', ( #10806 ), #6623, .T. ) ;
#21929 = CARTESIAN_POINT ( 'NONE',  ( -3.152548672688508926E-16, -66.81249999863442213, -5.148502694627439702 ) ) ;
#21931 = CARTESIAN_POINT ( 'NONE',  ( -3.152548672688508926E-16, -9.812499998634406140, -5.148502694627439702 ) ) ;
#21932 = VERTEX_POINT ( 'NONE', #11119 ) ;
#21933 = CARTESIAN_POINT ( 'NONE',  ( -6.972266317189433020E-16, -38.25000000000000000, -5.000000000000000000 ) ) ;
#21934 = CARTESIAN_POINT ( 'NONE',  ( 1.339745962155627135, 17.70534180126147916, -4.999999999999991118 ) ) ;
#21935 = CARTESIAN_POINT ( 'NONE',  ( -2.229367062500000163, -8.729166665301073991, -3.861377020970580443 ) ) ;
#21936 = CARTESIAN_POINT ( 'NONE',  ( 0.000000000000000000, -120.0000000000000000, 0.000000000000000000 ) ) ;
#21937 = CARTESIAN_POINT ( 'NONE',  ( -4.458734124999998549, 8.770833334698927786, 2.574251347313722516 ) ) ;
#21938 = CARTESIAN_POINT ( 'NONE',  ( -5.000000000000000000, -76.00000000000000000, 0.000000000000000000 ) ) ;
#21939 = CARTESIAN_POINT ( 'NONE',  ( -4.458734124999999437, -159.0000000013656063, -1.846868145590735644 ) ) ;
#21940 = DIRECTION ( 'NONE',  ( 0.000000000000000000, 1.000000000000000000, 0.000000000000000000 ) ) ;
#21941 = ORIENTED_EDGE ( 'NONE', *, *, #7587, .F. ) ;
#21942 = CARTESIAN_POINT ( 'NONE',  ( -2.229367062499996610, -84.14583333196773651, 3.861377020970582219 ) ) ;
#21943 = CARTESIAN_POINT ( 'NONE',  ( -1.339745962155610925, -67.79465819873851729, 5.000000000000000000 ) ) ;
#21944 = CARTESIAN_POINT ( 'NONE',  ( 9.457646018065525792E-16, -3.062499998634407472, 5.148502694627439702 ) ) ;
#21945 = FACE_OUTER_BOUND ( 'NONE', #27446, .T. ) ;
#21946 =( BOUNDED_CURVE ( )  B_SPLINE_CURVE ( 2, ( #9400, #29009, #58618, #34158, #33851, #32916, #8164, #19050, #8473 ),
 .UNSPECIFIED., .F., .F. ) 
 B_SPLINE_CURVE_WITH_KNOTS ( ( 3, 2, 2, 2, 3 ),
 ( 0.1916666666666668462, 0.1958333333333334980, 0.2000000000000001776, 0.2041666666666668295, 0.2083333333333335091 ),
 .UNSPECIFIED. ) 
 CURVE ( )  GEOMETRIC_REPRESENTATION_ITEM ( )  RATIONAL_B_SPLINE_CURVE ( ( 0.9999999999999970024, 0.9238795325112897361, 1.000000000000000000, 0.9238795325112867385, 1.000000000000000000, 0.9238795325112867385, 1.000000000000000000, 0.9238795325112837409, 1.000000000000003109 ) ) 
 REPRESENTATION_ITEM ( '' )  );
#21947 = ADVANCED_FACE ( 'NONE', ( #11440 ), #55200, .F. ) ;
#21948 = CARTESIAN_POINT ( 'NONE',  ( -5.000000000000000000, -29.87499999726881228, 0.000000000000000000 ) ) ;
#21949 = EDGE_CURVE ( 'NONE', #17633, #4656, #24017, .T. ) ;
#21950 = FACE_OUTER_BOUND ( 'NONE', #60332, .T. ) ;
#21951 = CARTESIAN_POINT ( 'NONE',  ( -4.458734124999999437, 22.60416666803225993, -2.574251347313719407 ) ) ;
#21952 = FACE_OUTER_BOUND ( 'NONE', #18201, .T. ) ;
#21953 = CARTESIAN_POINT ( 'NONE',  ( -4.458734124999999437, 27.60416666803226349, -2.574251347313719407 ) ) ;
#21954 = CARTESIAN_POINT ( 'NONE',  ( -2.229367062499996610, -49.14583333196772941, 3.861377020970582219 ) ) ;
#21955 = CARTESIAN_POINT ( 'NONE',  ( 4.458734124999999437, -35.06249999863440792, -5.460374474430324690E-16 ) ) ;
#21956 = CARTESIAN_POINT ( 'NONE',  ( 4.458734124999998549, 4.020833334698926009, -2.574251347313721627 ) ) ;
#21957 = CARTESIAN_POINT ( 'NONE',  ( -6.972266317189433020E-16, -0.1249999972688142363, -5.000000000000000000 ) ) ;
#21958 = CARTESIAN_POINT ( 'NONE',  ( 2.500000000000002220, 14.33333333333333393, 4.330127018922192761 ) ) ;
#21959 = CARTESIAN_POINT ( 'NONE',  ( -9.184850993605147944E-16, -141.3750000027312126, 5.000000000000000000 ) ) ;
#21960 = CARTESIAN_POINT ( 'NONE',  ( -6.972266317189433020E-16, -33.12499999726880873, -5.000000000000000000 ) ) ;
#21961 = CARTESIAN_POINT ( 'NONE',  ( -2.229367062499996610, -41.14583333196773651, 3.861377020970582219 ) ) ;
#21962 = CARTESIAN_POINT ( 'NONE',  ( 5.000000000000000888, -76.45833333060215864, 2.886751345948126879 ) ) ;
#21963 = ADVANCED_FACE ( 'NONE', ( #41977 ), #17222, .T. ) ;
#21964 = CARTESIAN_POINT ( 'NONE',  ( -56.48576386720575471, -140.0000000013656063, -4.591703134518078322 ) ) ;
#21965 = VECTOR ( 'NONE', #4277, 1000.000000000000000 ) ;
#21966 = CARTESIAN_POINT ( 'NONE',  ( 0.000000000000000000, -170.0000000000000000, 0.000000000000000000 ) ) ;
#21967 =( BOUNDED_CURVE ( )  B_SPLINE_CURVE ( 2, ( #13593, #32576, #8764, #28372, #7511, #47059, #46736, #2682, #22625 ),
 .UNSPECIFIED., .F., .F. ) 
 B_SPLINE_CURVE_WITH_KNOTS ( ( 3, 2, 2, 2, 3 ),
 ( 0.09821428571428571230, 0.09880952380952380543, 0.1000000000000000056, 0.1011904761904761918, 0.1017857142857142849 ),
 .UNSPECIFIED. ) 
 CURVE ( )  GEOMETRIC_REPRESENTATION_ITEM ( )  RATIONAL_B_SPLINE_CURVE ( ( 0.9330127018922194093, 0.9330127018922194093, 1.000000000000000000, 0.8660254037844387076, 1.000000000000000000, 0.8660254037844387076, 1.000000000000000000, 0.9330127018922194093, 0.9330127018922194093 ) ) 
 REPRESENTATION_ITEM ( '' )  );
#21968 = CARTESIAN_POINT ( 'NONE',  ( -6.972266317189433020E-16, -64.12499999726880162, -5.000000000000000000 ) ) ;
#21969 = CARTESIAN_POINT ( 'NONE',  ( -2.229367062499996610, -84.39583333196773651, 3.861377020970582219 ) ) ;
#21970 = CARTESIAN_POINT ( 'NONE',  ( -3.152801135295367096, -161.3125000013656063, -3.152801135295367541 ) ) ;
#21971 = CARTESIAN_POINT ( 'NONE',  ( 1.975475456537005874E-15, -63.74999999999998579, 5.000000000000000000 ) ) ;
#21972 = CARTESIAN_POINT ( 'NONE',  ( 5.000000000000000888, -34.58333333333332860, 2.886751345948126879 ) ) ;
#21973 = CARTESIAN_POINT ( 'NONE',  ( -51.75738570946856498, -146.7500000000000284, 3.805975901505576964 ) ) ;
#21974 = ORIENTED_EDGE ( 'NONE', *, *, #62146, .F. ) ;
#21975 = CARTESIAN_POINT ( 'NONE',  ( -2.229367062499996610, 17.60416666803225993, 3.861377020970582219 ) ) ;
#21976 = ORIENTED_EDGE ( 'NONE', *, *, #20136, .F. ) ;
#21977 = CARTESIAN_POINT ( 'NONE',  ( -2.229367062499996610, -93.14583333196773651, 3.861377020970582219 ) ) ;
#21978 = CARTESIAN_POINT ( 'NONE',  ( -3.152548672688508926E-16, 11.18750000136559564, -5.148502694627439702 ) ) ;
#21979 = CARTESIAN_POINT ( 'NONE',  ( -5.000000000000000000, 14.12500000273118594, 0.000000000000000000 ) ) ;
#21980 = CARTESIAN_POINT ( 'NONE',  ( -5.000000000000000000, -34.87499999726881583, 0.000000000000000000 ) ) ;
#21981 = CARTESIAN_POINT ( 'NONE',  ( -5.000000000000000000, 8.000000000000000000, 0.000000000000000000 ) ) ;
#21982 = CARTESIAN_POINT ( 'NONE',  ( -2.229367062500000163, -58.47916666530106511, -3.861377020970580443 ) ) ;
#21983 = CARTESIAN_POINT ( 'NONE',  ( 7.922798488042200660, -4.627419312545550056, -8.057411459260041653 ) ) ;
#21984 = EDGE_CURVE ( 'NONE', #24823, #54905, #37799, .T. ) ;
#21985 = CARTESIAN_POINT ( 'NONE',  ( -59.29741812935640155, -136.8750000013656063, -2.196230717870135685 ) ) ;
#21986 = CARTESIAN_POINT ( 'NONE',  ( -2.499999999999996447, -37.70833333060213732, 4.330127018922195425 ) ) ;
#21987 = CARTESIAN_POINT ( 'NONE',  ( -2.499999999999996447, -63.83333333333332860, 4.330127018922195425 ) ) ;
#21988 = CARTESIAN_POINT ( 'NONE',  ( -1.339745962155610925, -24.66965819600733667, 5.000000000000000000 ) ) ;
#21989 = CARTESIAN_POINT ( 'NONE',  ( -4.999999999999999112, -37.91666666666666430, 2.886751345948131764 ) ) ;
#21990 = CARTESIAN_POINT ( 'NONE',  ( 5.000000000000000888, -96.58333333333332860, 2.886751345948126879 ) ) ;
#21992 = CARTESIAN_POINT ( 'NONE',  ( 2.229367062499998831, -14.89583333196773474, -3.861377020970580887 ) ) ;
#21991 = CARTESIAN_POINT ( 'NONE',  ( -5.000000000000000000, -45.00000000000000000, 0.000000000000000000 ) ) ;
#21993 = DIRECTION ( 'NONE',  ( -0.000000000000000000, 1.000000000000000000, -0.000000000000000000 ) ) ;
#21994 = CARTESIAN_POINT ( 'NONE',  ( -2.229367062500000163, -57.47916666530107932, -3.861377020970580443 ) ) ;
#21995 = CARTESIAN_POINT ( 'NONE',  ( 1.846868145590736310, -151.8750000013655779, 4.458734124999999437 ) ) ;
#21996 = CARTESIAN_POINT ( 'NONE',  ( -2.229367062499996610, -72.14583333196773651, 3.861377020970582219 ) ) ;
#21997 = CARTESIAN_POINT ( 'NONE',  ( -57.89159099828107458, -147.9375000013656063, -3.393966926194107447 ) ) ;
#21998 = CARTESIAN_POINT ( 'NONE',  ( 4.458734124999998549, -21.97916666530107221, -2.574251347313721627 ) ) ;
#21999 = CARTESIAN_POINT ( 'NONE',  ( -2.499999999999996447, -60.70833333060214443, 4.330127018922195425 ) ) ;
#22000 = ORIENTED_EDGE ( 'NONE', *, *, #52040, .F. ) ;
#22001 = CARTESIAN_POINT ( 'NONE',  ( -2.499999999999996447, -48.83333333333332860, 4.330127018922195425 ) ) ;
#22002 = VERTEX_POINT ( 'NONE', #61619 ) ;
#22003 = CARTESIAN_POINT ( 'NONE',  ( 9.457646018065525792E-16, -62.31249999863440792, 5.148502694627439702 ) ) ;
#22004 = CARTESIAN_POINT ( 'NONE',  ( 1.975475456537005874E-15, -64.74999999999998579, 5.000000000000000000 ) ) ;
#22005 = CARTESIAN_POINT ( 'NONE',  ( -1.846868145590737420, -152.7500000013656063, 4.458734124999999437 ) ) ;
#22006 = ORIENTED_EDGE ( 'NONE', *, *, #50294, .F. ) ;
#22007 = CARTESIAN_POINT ( 'NONE',  ( 2.500000000000002220, 25.33333333333333215, 4.330127018922192761 ) ) ;
#22008 = CARTESIAN_POINT ( 'NONE',  ( 6.602753909532903087, 5.319290460493537154, -7.792447862505332168 ) ) ;
#22009 = DIRECTION ( 'NONE',  ( 0.000000000000000000, 0.000000000000000000, 1.000000000000000000 ) ) ;
#22011 = EDGE_CURVE ( 'NONE', #25520, #5760, #8525, .T. ) ;
#22010 = CARTESIAN_POINT ( 'NONE',  ( 2.229367062500001939, -50.22916666530107221, 3.861377020970579999 ) ) ;
#22012 = ORIENTED_EDGE ( 'NONE', *, *, #27238, .T. ) ;
#22013 = CARTESIAN_POINT ( 'NONE',  ( 2.626220312808019583E-14, 15.74999999999999645, -5.000000000000000000 ) ) ;
#22014 = CARTESIAN_POINT ( 'NONE',  ( -3.152548672688508926E-16, 10.43750000136559386, -5.148502694627439702 ) ) ;
#22015 = CARTESIAN_POINT ( 'NONE',  ( -2.229367062500000163, 24.52083333469892779, -3.861377020970580443 ) ) ;
#22016 = CARTESIAN_POINT ( 'NONE',  ( -51.60603307380591787, -147.9375000013656063, -2.891590998281053704 ) ) ;
#22017 = CARTESIAN_POINT ( 'NONE',  ( 2.499999999999998668, -13.20833333060214976, -4.330127018922193649 ) ) ;
#22018 = CARTESIAN_POINT ( 'NONE',  ( 5.000000000000000888, -164.9375000000000284, -2.071067811865475505 ) ) ;
#22019 =( BOUNDED_CURVE ( )  B_SPLINE_CURVE ( 2, ( #55190, #54220, #4692, #58730, #24314, #43921, #63568, #14656, #10158 ),
 .UNSPECIFIED., .F., .F. ) 
 B_SPLINE_CURVE_WITH_KNOTS ( ( 3, 2, 2, 2, 3 ),
 ( 0.6979166666666666297, 0.6986111111111110716, 0.6999999999999999556, 0.7013888888888888395, 0.7020833333333332815 ),
 .UNSPECIFIED. ) 
 CURVE ( )  GEOMETRIC_REPRESENTATION_ITEM ( )  RATIONAL_B_SPLINE_CURVE ( ( 0.9330127018922194093, 0.9330127018922194093, 1.000000000000000000, 0.8660254037844387076, 1.000000000000000000, 0.8660254037844387076, 1.000000000000000000, 0.9330127018922194093, 0.9330127018922194093 ) ) 
 REPRESENTATION_ITEM ( '' )  );
#22020 = ORIENTED_EDGE ( 'NONE', *, *, #37785, .T. ) ;
#22021 = CARTESIAN_POINT ( 'NONE',  ( 4.458734124999998549, -70.72916666530107932, -2.574251347313721627 ) ) ;
#22022 = CARTESIAN_POINT ( 'NONE',  ( -5.000000000000000000, 0.9166666666666664076, -2.886751345948128211 ) ) ;
#22023 = CARTESIAN_POINT ( 'NONE',  ( 2.229367062500001939, 13.02083333469892779, 3.861377020970579999 ) ) ;
#22024 = CARTESIAN_POINT ( 'NONE',  ( 5.000000000000000000, -60.37499999726880873, -6.123233995736766282E-16 ) ) ;
#22025 = LINE ( 'NONE', #61905, #36741 ) ;
#22026 = CARTESIAN_POINT ( 'NONE',  ( 4.458734125000001214, -55.14583333196772941, 2.574251347313718519 ) ) ;
#22027 = CARTESIAN_POINT ( 'NONE',  ( 5.000000000000000888, -15.45833333060214265, 2.886751345948126879 ) ) ;
#22028 = EDGE_CURVE ( 'NONE', #2572, #3938, #39100, .T. ) ;
#22029 = CARTESIAN_POINT ( 'NONE',  ( 0.000000000000000000, -120.0000000000000000, 0.000000000000000000 ) ) ;
#22030 = CARTESIAN_POINT ( 'NONE',  ( -3.535533905932738641, -139.5000000027311842, 3.535533905932737309 ) ) ;
#22031 = CARTESIAN_POINT ( 'NONE',  ( -1.339745962155613812, -84.08034179853027013, -5.000000000000000000 ) ) ;
#22032 = CARTESIAN_POINT ( 'NONE',  ( 2.229367062499998831, -20.89583333196774007, -3.861377020970580887 ) ) ;
#22033 = ORIENTED_EDGE ( 'NONE', *, *, #25556, .F. ) ;
#22034 = CARTESIAN_POINT ( 'NONE',  ( -5.000000000000000000, -102.0833333333333286, -2.886751345948128211 ) ) ;
#22035 = CARTESIAN_POINT ( 'NONE',  ( 1.060575238724906964E-15, 29.25000000000000000, 5.773502691896257311 ) ) ;
#22036 = CARTESIAN_POINT ( 'NONE',  ( -9.184850993605147944E-16, -156.3750000027311842, 5.000000000000000000 ) ) ;
#22037 = VERTEX_POINT ( 'NONE', #2757 ) ;
#22038 = CARTESIAN_POINT ( 'NONE',  ( -2.229367062500000163, -102.7291666653010651, -3.861377020970580443 ) ) ;
#22039 = CARTESIAN_POINT ( 'NONE',  ( -4.458734124999999437, -24.31249999863440436, 0.000000000000000000 ) ) ;
#22040 = CARTESIAN_POINT ( 'NONE',  ( 5.000000000000000000, -65.29166666393548724, -2.886751345948129988 ) ) ;
#22041 = CARTESIAN_POINT ( 'NONE',  ( -56.48576386720575471, -153.0000000013656063, -4.591703134518078322 ) ) ;
#22042 = CARTESIAN_POINT ( 'NONE',  ( 5.000000000000000000, -147.0625000000000000, 2.071067811865478614 ) ) ;
#22043 = CARTESIAN_POINT ( 'NONE',  ( -2.229367062499996610, -25.14583333196773651, 3.861377020970582219 ) ) ;
#22044 = CARTESIAN_POINT ( 'NONE',  ( 2.229367062500001939, -68.22916666530106511, 3.861377020970579999 ) ) ;
#22045 = CARTESIAN_POINT ( 'NONE',  ( 5.000000000000000888, 8.416666666666666075, 2.886751345948126879 ) ) ;
#22046 = CARTESIAN_POINT ( 'NONE',  ( -3.152548672688508926E-16, -23.56249999863440436, -5.148502694627439702 ) ) ;
#22047 = DIRECTION ( 'NONE',  ( -0.000000000000000000, -1.000000000000000000, -0.000000000000000000 ) ) ;
#22048 = CARTESIAN_POINT ( 'NONE',  ( -2.071067811865478170, -151.3125000000000284, 5.000000000000000000 ) ) ;
#22049 = CARTESIAN_POINT ( 'NONE',  ( -4.999999999999999112, -17.91666666666666430, 2.886751345948131764 ) ) ;
#22050 = CARTESIAN_POINT ( 'NONE',  ( 4.458734124999999437, -150.4375000013656063, 0.000000000000000000 ) ) ;
#22051 = ORIENTED_EDGE ( 'NONE', *, *, #47579, .T. ) ;
#22052 = CARTESIAN_POINT ( 'NONE',  ( -4.458734124999999437, 29.68750000136559208, 0.000000000000000000 ) ) ;
#22053 = CARTESIAN_POINT ( 'NONE',  ( 2.229367062499998831, -51.89583333196773651, -3.861377020970580887 ) ) ;
#22054 =( BOUNDED_CURVE ( )  B_SPLINE_CURVE ( 2, ( #20113, #39717, #59354, #1474, #25579, #15289, #10454, #30069, #49698 ),
 .UNSPECIFIED., .F., .F. ) 
 B_SPLINE_CURVE_WITH_KNOTS ( ( 3, 2, 2, 2, 3 ),
 ( 0.1479166666666666685, 0.1486111111111111105, 0.1499999999999999944, 0.1513888888888888784, 0.1520833333333333481 ),
 .UNSPECIFIED. ) 
 CURVE ( )  GEOMETRIC_REPRESENTATION_ITEM ( )  RATIONAL_B_SPLINE_CURVE ( ( 0.9330127018922194093, 0.9330127018922194093, 1.000000000000000000, 0.8660254037844387076, 1.000000000000000000, 0.8660254037844387076, 1.000000000000000000, 0.9330127018922180770, 0.9330127018922194093 ) ) 
 REPRESENTATION_ITEM ( '' )  );
#22055 = CARTESIAN_POINT ( 'NONE',  ( 0.000000000000000000, -170.0000000000000000, 0.000000000000000000 ) ) ;
#22056 = CARTESIAN_POINT ( 'NONE',  ( -55.39835681537999790, -135.8750000000000284, 4.984105922594378235 ) ) ;
#22057 = CARTESIAN_POINT ( 'NONE',  ( 5.000000000000000000, 23.58333333333333215, -2.886751345948129988 ) ) ;
#22058 = EDGE_CURVE ( 'NONE', #42260, #40791, #61308, .T. ) ;
#22059 = CARTESIAN_POINT ( 'NONE',  ( 8.660254037844342889, 30.00000000000000000, 0.000000000000000000 ) ) ;
#22060 = AXIS2_PLACEMENT_3D ( 'NONE', #21366, #37120, #51903 ) ;
#22061 = CARTESIAN_POINT ( 'NONE',  ( -4.458734124999998549, -3.229166665301069994, 2.574251347313722516 ) ) ;
#22062 = CARTESIAN_POINT ( 'NONE',  ( 0.000000000000000000, -170.0000000000000000, 0.000000000000000000 ) ) ;
#22063 = CARTESIAN_POINT ( 'NONE',  ( -6.972266317189433020E-16, -87.12499999726880162, -5.000000000000000000 ) ) ;
#22064 = CARTESIAN_POINT ( 'NONE',  ( 2.229367062500001939, 15.77083333469892601, 3.861377020970579999 ) ) ;
#22065 = CARTESIAN_POINT ( 'NONE',  ( 2.499999999999998668, 0.7916666693978530178, -4.330127018922193649 ) ) ;
#22066 = ORIENTED_EDGE ( 'NONE', *, *, #9960, .T. ) ;
#22067 = CARTESIAN_POINT ( 'NONE',  ( -2.499999999999996447, -29.70833333060215153, 4.330127018922195425 ) ) ;
#22068 = ORIENTED_EDGE ( 'NONE', *, *, #57897, .F. ) ;
#22069 = CARTESIAN_POINT ( 'NONE',  ( -6.972266317189433020E-16, -24.12499999726881228, -5.000000000000000000 ) ) ;
#22070 = CARTESIAN_POINT ( 'NONE',  ( 2.229367062500001939, -42.97916666530107932, 3.861377020970579999 ) ) ;
#22071 = CARTESIAN_POINT ( 'NONE',  ( 3.152801135295367541, -164.5625000013656063, -3.152801135295367541 ) ) ;
#22072 = CARTESIAN_POINT ( 'NONE',  ( 1.060575238724906964E-15, -42.62499999726880162, 5.773502691896257311 ) ) ;
#22073 = VERTEX_POINT ( 'NONE', #51649 ) ;
#22074 = CARTESIAN_POINT ( 'NONE',  ( 4.458734124999999437, -19.81249999863440081, -5.460374474430324690E-16 ) ) ;
#22075 = ORIENTED_EDGE ( 'NONE', *, *, #19321, .T. ) ;
#22076 = CARTESIAN_POINT ( 'NONE',  ( 5.000000000000000888, -87.58333333333332860, 2.886751345948126879 ) ) ;
#22077 = CARTESIAN_POINT ( 'NONE',  ( -4.458734124999999437, -163.9375000013655779, -5.460374474430324690E-16 ) ) ;
#22078 = VERTEX_POINT ( 'NONE', #26884 ) ;
#22079 = CARTESIAN_POINT ( 'NONE',  ( -55.39835681537999790, -137.8750000000000284, 4.984105922594378235 ) ) ;
#22080 = CARTESIAN_POINT ( 'NONE',  ( 4.458734125000001214, -33.14583333196774362, 2.574251347313718519 ) ) ;
#22081 = CARTESIAN_POINT ( 'NONE',  ( -5.000000000000000000, 20.99999999999999645, 0.000000000000000000 ) ) ;
#22082 = ORIENTED_EDGE ( 'NONE', *, *, #48092, .T. ) ;
#22083 = ADVANCED_FACE ( 'NONE', ( #37173 ), #57736, .T. ) ;
#22084 = ADVANCED_FACE ( 'NONE', ( #47752 ), #47132, .T. ) ;
#22085 = CARTESIAN_POINT ( 'NONE',  ( 2.229367062500001939, -78.97916666530106511, 3.861377020970579999 ) ) ;
#22086 = CARTESIAN_POINT ( 'NONE',  ( -2.229367062500000163, 23.52083333469892779, -3.861377020970580443 ) ) ;
#22087 = ADVANCED_FACE ( 'NONE', ( #47444 ), #23012, .T. ) ;
#22088 = ORIENTED_EDGE ( 'NONE', *, *, #812, .F. ) ;
#22089 = CARTESIAN_POINT ( 'NONE',  ( 1.975475456537005874E-15, -83.74999999999998579, 5.000000000000000000 ) ) ;
#22090 = CARTESIAN_POINT ( 'NONE',  ( -56.48576386720575471, -141.0000000013655779, -4.591703134518078322 ) ) ;
#22091 = CARTESIAN_POINT ( 'NONE',  ( 2.229367062500001939, -78.22916666530106511, 3.861377020970579999 ) ) ;
#22092 = CARTESIAN_POINT ( 'NONE',  ( -60.14911071818854538, -132.1875000027312410, 1.666127454062681368 ) ) ;
#22093 = CARTESIAN_POINT ( 'NONE',  ( 2.499999999999998668, 0.7916666693978530178, -4.330127018922193649 ) ) ;
#22094 = CARTESIAN_POINT ( 'NONE',  ( -5.000000000000000000, -82.99999999999998579, 0.000000000000000000 ) ) ;
#22095 = EDGE_CURVE ( 'NONE', #8165, #34549, #56581, .T. ) ;
#22096 = CARTESIAN_POINT ( 'NONE',  ( 0.000000000000000000, -120.0000000000000000, 0.000000000000000000 ) ) ;
#22097 = CARTESIAN_POINT ( 'NONE',  ( -4.458734124999997661, -53.22916666530107932, 2.574251347313722516 ) ) ;
#22098 = CARTESIAN_POINT ( 'NONE',  ( -2.229367062500000163, -45.47916666530106511, -3.861377020970580443 ) ) ;
#22099 = CARTESIAN_POINT ( 'NONE',  ( 2.229367062500001939, 27.02083333469892423, 3.861377020970579999 ) ) ;
#22100 = EDGE_CURVE ( 'NONE', #19824, #28539, #32969, .T. ) ;
#22101 = EDGE_CURVE ( 'NONE', #34069, #7844, #38724, .T. ) ;
#22102 = CARTESIAN_POINT ( 'NONE',  ( -5.000000000000000000, -108.0833333333333428, -2.886751345948128211 ) ) ;
#22103 = AXIS2_PLACEMENT_3D ( 'NONE', #60137, #16058, #55315 ) ;
#22104 = CARTESIAN_POINT ( 'NONE',  ( 5.000000000000000000, -169.5625000013656063, 0.000000000000000000 ) ) ;
#22105 = CARTESIAN_POINT ( 'NONE',  ( 2.229367062499998831, -38.89583333196773651, -3.861377020970580887 ) ) ;
#22106 = CARTESIAN_POINT ( 'NONE',  ( -5.000000000000000000, -0.8749999972688139449, 0.000000000000000000 ) ) ;
#22107 = PLANE ( 'NONE',  #19129 ) ;
#22108 = EDGE_CURVE ( 'NONE', #57819, #19872, #17341, .T. ) ;
#22109 = CARTESIAN_POINT ( 'NONE',  ( -58.39396692619412477, -124.4375000013656063, 2.891590998281057701 ) ) ;
#22110 = CARTESIAN_POINT ( 'NONE',  ( -4.458734124999999437, -78.56249999863440792, 0.000000000000000000 ) ) ;
#22111 = EDGE_CURVE ( 'NONE', #27444, #44174, #43856, .T. ) ;
#22112 = CARTESIAN_POINT ( 'NONE',  ( -2.229367062500000163, -103.4791666653010651, -3.861377020970580443 ) ) ;
#22113 = CARTESIAN_POINT ( 'NONE',  ( 4.458734124999998549, -3.979166665301070438, -2.574251347313721627 ) ) ;
#22114 = ORIENTED_EDGE ( 'NONE', *, *, #55706, .T. ) ;
#22115 = EDGE_CURVE ( 'NONE', #50115, #39210, #23902, .T. ) ;
#22116 = CARTESIAN_POINT ( 'NONE',  ( 4.458734124999998549, -91.72916666530106511, -2.574251347313721627 ) ) ;
#22117 = EDGE_CURVE ( 'NONE', #32533, #30611, #19099, .T. ) ;
#22118 = CARTESIAN_POINT ( 'NONE',  ( 0.000000000000000000, -170.0000000000000000, 0.000000000000000000 ) ) ;
#22119 = CARTESIAN_POINT ( 'NONE',  ( -4.458734124999998549, -89.47916666530106511, 2.574251347313722516 ) ) ;
#22120 = CARTESIAN_POINT ( 'NONE',  ( 2.229367062499998831, 11.10416666803225993, -3.861377020970580887 ) ) ;
#22121 = CARTESIAN_POINT ( 'NONE',  ( 0.000000000000000000, -120.0000000000000000, 5.000000000000000000 ) ) ;
#22122 = CARTESIAN_POINT ( 'NONE',  ( -50.70258187064364108, -134.1250000013656347, 2.196230717870141014 ) ) ;
#22123 = CARTESIAN_POINT ( 'NONE',  ( -2.229367062499996610, -7.145833331967735624, 3.861377020970582219 ) ) ;
#22124 = CARTESIAN_POINT ( 'NONE',  ( 4.458734124999998549, 14.02083333469892779, -2.574251347313721627 ) ) ;
#22125 = CARTESIAN_POINT ( 'NONE',  ( 9.457646018065525792E-16, -51.31249999863440792, 5.148502694627439702 ) ) ;
#22126 = CARTESIAN_POINT ( 'NONE',  ( -5.000000000000000000, -15.95833333060214443, -2.886751345948128211 ) ) ;
#22127 = CARTESIAN_POINT ( 'NONE',  ( -2.229367062499996610, -7.145833331967735624, 3.861377020970582219 ) ) ;
#22128 = FILL_AREA_STYLE_COLOUR ( '', #44227 ) ;
#22129 = ORIENTED_EDGE ( 'NONE', *, *, #25509, .T. ) ;
#22130 = CARTESIAN_POINT ( 'NONE',  ( -4.458734124999999437, -34.56249999863440792, 0.000000000000000000 ) ) ;
#22131 = CARTESIAN_POINT ( 'NONE',  ( -54.64476657466781973, -128.0625000013656063, -4.444560631937228834 ) ) ;
#22132 = CARTESIAN_POINT ( 'NONE',  ( -2.229367062500000163, -82.47916666530106511, -3.861377020970580443 ) ) ;
#22133 = CARTESIAN_POINT ( 'NONE',  ( -4.458734124999998549, 26.52083333469892779, 2.574251347313722516 ) ) ;
#22134 =( BOUNDED_CURVE ( )  B_SPLINE_CURVE ( 2, ( #15286, #44869, #49695, #40036, #23530, #52796, #32538, #33181, #8731 ),
 .UNSPECIFIED., .F., .F. ) 
 B_SPLINE_CURVE_WITH_KNOTS ( ( 3, 2, 2, 2, 3 ),
 ( 0.3250000000000002887, 0.3291666666666669405, 0.3333333333333335924, 0.3375000000000002998, 0.3416666666666669516 ),
 .UNSPECIFIED. ) 
 CURVE ( )  GEOMETRIC_REPRESENTATION_ITEM ( )  RATIONAL_B_SPLINE_CURVE ( ( 0.9999999999999948930, 0.9238795325112918455, 1.000000000000000000, 0.9238795325112867385, 1.000000000000000000, 0.9238795325112867385, 1.000000000000000000, 0.9238795325112816315, 1.000000000000005107 ) ) 
 REPRESENTATION_ITEM ( '' )  );
#22135 = CARTESIAN_POINT ( 'NONE',  ( -1.846868145590734756, -148.3750000013655779, -4.458734124999999437 ) ) ;
#22136 = CARTESIAN_POINT ( 'NONE',  ( 2.229367062500001939, 22.02083333469892779, 3.861377020970579999 ) ) ;
#22137 = CARTESIAN_POINT ( 'NONE',  ( -75.00000000000001421, 0.000000000000000000, -9.000000000000001776 ) ) ;
#22138 = CARTESIAN_POINT ( 'NONE',  ( 1.975475456537005874E-15, -66.74999999999998579, 5.000000000000000000 ) ) ;
#22139 = CARTESIAN_POINT ( 'NONE',  ( -4.458734124999999437, -84.64583333196773651, -2.574251347313719407 ) ) ;
#22140 = CARTESIAN_POINT ( 'NONE',  ( -5.000000000000000000, -66.08333333333332860, -2.886751345948128211 ) ) ;
#22141 = CARTESIAN_POINT ( 'NONE',  ( -1.339745962155613368, 29.79465819873851729, -5.000000000000000000 ) ) ;
#22142 = CARTESIAN_POINT ( 'NONE',  ( 5.000000000000000000, 21.62500000273118417, -6.123233995736766282E-16 ) ) ;
#22143 = ORIENTED_EDGE ( 'NONE', *, *, #60217, .T. ) ;
#22144 = CARTESIAN_POINT ( 'NONE',  ( 1.975475456537005874E-15, -61.62499999726880873, 5.000000000000000000 ) ) ;
#22145 = CARTESIAN_POINT ( 'NONE',  ( 5.000000000000000888, 7.416666666666665186, 2.886751345948126879 ) ) ;
#22147 = CARTESIAN_POINT ( 'NONE',  ( -5.000000000000000000, -23.00000000000000000, 0.000000000000000000 ) ) ;
#22146 = CARTESIAN_POINT ( 'NONE',  ( 2.500000000000002220, -40.66666666666667140, 4.330127018922192761 ) ) ;
#22148 = CARTESIAN_POINT ( 'NONE',  ( -4.458734124999999437, -26.39583333196773651, -2.574251347313719407 ) ) ;
#22149 = CARTESIAN_POINT ( 'NONE',  ( 4.458734125000000326, -85.89583333196775072, 2.574251347313718519 ) ) ;
#22150 = VECTOR ( 'NONE', #41869, 1000.000000000000000 ) ;
#22151 =( BOUNDED_CURVE ( )  B_SPLINE_CURVE ( 2, ( #42893, #18461, #13939, #63160, #57708, #9426, #33253, #13634, #19394 ),
 .UNSPECIFIED., .F., .F. ) 
 B_SPLINE_CURVE_WITH_KNOTS ( ( 3, 2, 2, 2, 3 ),
 ( 0.8946428571428571841, 0.8952380952380952772, 0.8964285714285714635, 0.8976190476190476497, 0.8982142857142857428 ),
 .UNSPECIFIED. ) 
 CURVE ( )  GEOMETRIC_REPRESENTATION_ITEM ( )  RATIONAL_B_SPLINE_CURVE ( ( 0.9330127018922194093, 0.9330127018922194093, 1.000000000000000000, 0.8660254037844387076, 1.000000000000000000, 0.8660254037844387076, 1.000000000000000000, 0.9330127018922194093, 0.9330127018922194093 ) ) 
 REPRESENTATION_ITEM ( '' )  );
#22152 = CARTESIAN_POINT ( 'NONE',  ( 5.000000000000000000, -31.29166666393548368, -2.886751345948129988 ) ) ;
#22154 = ORIENTED_EDGE ( 'NONE', *, *, #30741, .T. ) ;
#22153 = CARTESIAN_POINT ( 'NONE',  ( -4.458734124999999437, -55.31249999863440081, 0.000000000000000000 ) ) ;
#22155 = CARTESIAN_POINT ( 'NONE',  ( -58.39396692619412477, -154.6875000013656063, 2.891590998281057701 ) ) ;
#22157 = ORIENTED_EDGE ( 'NONE', *, *, #7863, .F. ) ;
#22156 = CARTESIAN_POINT ( 'NONE',  ( -4.458734124999998549, -9.479166665301070438, 2.574251347313722516 ) ) ;
#22158 = CARTESIAN_POINT ( 'NONE',  ( -5.000000000000000000, -74.00000000000000000, 0.000000000000000000 ) ) ;
#22159 = CARTESIAN_POINT ( 'NONE',  ( -58.39396692619412477, -137.4375000013656063, 2.891590998281057701 ) ) ;
#22160 = CARTESIAN_POINT ( 'NONE',  ( -4.458734124999999437, -50.64583333196773651, -2.574251347313719407 ) ) ;
#22161 = CARTESIAN_POINT ( 'NONE',  ( -4.999999999999999112, -78.79166666393547303, 2.886751345948131764 ) ) ;
#22163 = EDGE_LOOP ( 'NONE', ( #54205, #58051, #54412, #3175 ) ) ;
#22162 = CARTESIAN_POINT ( 'NONE',  ( -2.499999999999996447, -21.70833333060214798, 4.330127018922195425 ) ) ;
#22164 = CARTESIAN_POINT ( 'NONE',  ( -53.33387254593733928, -148.8125000000000284, 5.149110718188519620 ) ) ;
#22165 = CARTESIAN_POINT ( 'NONE',  ( -2.229367062500000163, -18.72916666530106866, -3.861377020970580443 ) ) ;
#22166 = CARTESIAN_POINT ( 'NONE',  ( -2.229367062500000163, -51.72916666530107221, -3.861377020970580443 ) ) ;
#22167 = CARTESIAN_POINT ( 'NONE',  ( -2.499999999999996447, -58.70833333060214443, 4.330127018922195425 ) ) ;
#22168 = CARTESIAN_POINT ( 'NONE',  ( -1.846868145590737420, -140.7500000013655779, 4.458734124999999437 ) ) ;
#22169 = CARTESIAN_POINT ( 'NONE',  ( 4.458734125000001214, -101.1458333319677365, 2.574251347313718519 ) ) ;
#22170 = CARTESIAN_POINT ( 'NONE',  ( 1.975475456537005874E-15, 10.24999999999999822, 5.000000000000000000 ) ) ;
#22171 = ORIENTED_EDGE ( 'NONE', *, *, #6331, .T. ) ;
#22172 = CARTESIAN_POINT ( 'NONE',  ( -57.89159099828107458, -153.9375000013656063, -3.393966926194107447 ) ) ;
#22173 = CARTESIAN_POINT ( 'NONE',  ( -51.75738570946856498, -143.8750000027312126, 3.805975901505576964 ) ) ;
#22174 = CARTESIAN_POINT ( 'NONE',  ( 5.000000000000000000, 18.58333333333333215, -2.886751345948130876 ) ) ;
#22175 = CARTESIAN_POINT ( 'NONE',  ( 9.457646018065525792E-16, -5.062499998634401699, 5.148502694627439702 ) ) ;
#22176 = CARTESIAN_POINT ( 'NONE',  ( -4.458734124999999437, -97.64583333196773651, -2.574251347313719407 ) ) ;
#22177 = CARTESIAN_POINT ( 'NONE',  ( 3.152801135295366208, -147.8125000013655779, 3.152801135295367985 ) ) ;
#22178 = CARTESIAN_POINT ( 'NONE',  ( -2.229367062499996610, -23.39583333196773651, 3.861377020970582219 ) ) ;
#22179 = CARTESIAN_POINT ( 'NONE',  ( 1.975475456537005874E-15, -74.62499999726880162, 5.000000000000000000 ) ) ;
#22180 = CARTESIAN_POINT ( 'NONE',  ( -59.44456063193725015, -138.5625000013656063, -0.3552334253322034230 ) ) ;
#22181 = CARTESIAN_POINT ( 'NONE',  ( -4.458734124999999437, -61.56249999863440081, 0.000000000000000000 ) ) ;
#22182 = AXIS2_PLACEMENT_3D ( 'NONE', #49517, #29887, #35364 ) ;
#22183 = EDGE_CURVE ( 'NONE', #62586, #36804, #56804, .T. ) ;
#22184 = CARTESIAN_POINT ( 'NONE',  ( 5.000000000000000000, -72.41666666666665719, -2.886751345948130876 ) ) ;
#22185 = CARTESIAN_POINT ( 'NONE',  ( 6.486836893983020325, -4.915077010914103539, -7.231838333420563814 ) ) ;
#22186 = CARTESIAN_POINT ( 'NONE',  ( -3.152801135295367985, -144.8125000013655779, 3.152801135295367096 ) ) ;
#22187 = CARTESIAN_POINT ( 'NONE',  ( 2.229367062500001939, 10.77083333469892956, 3.861377020970579999 ) ) ;
#22188 = EDGE_LOOP ( 'NONE', ( #54024, #60044, #44780, #36737 ) ) ;
#22189 = CARTESIAN_POINT ( 'NONE',  ( -2.500000000000000444, -5.166666666666666963, -4.330127018922193649 ) ) ;
#22190 = CARTESIAN_POINT ( 'NONE',  ( 5.000000000000000000, -61.41666666666665719, -2.886751345948130876 ) ) ;
#22192 = CARTESIAN_POINT ( 'NONE',  ( -3.152548672688508926E-16, -25.56249999863440436, -5.148502694627439702 ) ) ;
#22191 = CARTESIAN_POINT ( 'NONE',  ( -5.000000000000000000, -90.00000000000000000, 0.000000000000000000 ) ) ;
#22193 = CARTESIAN_POINT ( 'NONE',  ( -7.500000000000000000, 3.608439182435158710, -7.298562697733104621 ) ) ;
#22194 = CARTESIAN_POINT ( 'NONE',  ( 9.457646018065525792E-16, -70.31249999863439371, 5.148502694627439702 ) ) ;
#22195 = CARTESIAN_POINT ( 'NONE',  ( 1.975475456537005874E-15, 16.37500000273118417, 5.000000000000000000 ) ) ;
#22196 = CARTESIAN_POINT ( 'NONE',  ( -1.339745962155610925, -17.66965819600733312, 5.000000000000000000 ) ) ;
#22197 = VECTOR ( 'NONE', #6631, 1000.000000000000000 ) ;
#22198 = CARTESIAN_POINT ( 'NONE',  ( -59.59170313451811296, -147.5000000013656063, 1.485763867205729394 ) ) ;
#22199 = EDGE_CURVE ( 'NONE', #6259, #20545, #6260, .T. ) ;
#22200 = CARTESIAN_POINT ( 'NONE',  ( 5.000000000000000000, -52.29166666393548013, -2.886751345948129988 ) ) ;
#22201 = CARTESIAN_POINT ( 'NONE',  ( -48.00000000000002132, -155.0000000000000284, -4.041451884327376121 ) ) ;
#22202 = CARTESIAN_POINT ( 'NONE',  ( -2.229367062499996610, 6.854166668032259935, 3.861377020970582219 ) ) ;
#22203 = CYLINDRICAL_SURFACE ( 'NONE', #60263, 5.000000000000000000 ) ;
#22204 = CARTESIAN_POINT ( 'NONE',  ( 5.000000000000000000, 21.58333333333333215, -2.886751345948130876 ) ) ;
#22205 = CARTESIAN_POINT ( 'NONE',  ( 9.457646018065525792E-16, 8.937500001365595637, 5.148502694627439702 ) ) ;
#22206 = CARTESIAN_POINT ( 'NONE',  ( -2.229367062499996610, -71.14583333196773651, 3.861377020970582219 ) ) ;
#22207 = CARTESIAN_POINT ( 'NONE',  ( 2.229367062499998831, -17.89583333196773651, -3.861377020970580887 ) ) ;
#22208 =( BOUNDED_CURVE ( )  B_SPLINE_CURVE ( 2, ( #27883, #62634, #57800, #12465, #47505, #41719, #33346, #32076, #17291 ),
 .UNSPECIFIED., .F., .F. ) 
 B_SPLINE_CURVE_WITH_KNOTS ( ( 3, 2, 2, 2, 3 ),
 ( 0.4767857142857143127, 0.4773809523809524058, 0.4785714285714285920, 0.4797619047619047783, 0.4803571428571428714 ),
 .UNSPECIFIED. ) 
 CURVE ( )  GEOMETRIC_REPRESENTATION_ITEM ( )  RATIONAL_B_SPLINE_CURVE ( ( 0.9330127018922194093, 0.9330127018922225179, 1.000000000000000000, 0.8660254037844387076, 1.000000000000000000, 0.8660254037844387076, 1.000000000000000000, 0.9330127018922194093, 0.9330127018922194093 ) ) 
 REPRESENTATION_ITEM ( '' )  );
#22209 = CARTESIAN_POINT ( 'NONE',  ( -4.999999999999999112, -0.9166666666666664076, 2.886751345948131764 ) ) ;
#22210 = CARTESIAN_POINT ( 'NONE',  ( 4.458734124999999437, -159.4375000013655779, 0.000000000000000000 ) ) ;
#22211 = DIRECTION ( 'NONE',  ( 1.000000000000000000, -0.000000000000000000, -0.000000000000000000 ) ) ;
#22212 = CARTESIAN_POINT ( 'NONE',  ( -2.229367062500000163, -65.47916666530106511, -3.861377020970580443 ) ) ;
#22213 = CARTESIAN_POINT ( 'NONE',  ( 5.000000000000000000, -94.37499999726881583, -6.123233995736766282E-16 ) ) ;
#22214 = CARTESIAN_POINT ( 'NONE',  ( 1.339745962155612702, 5.830341803992665106, -5.000000000000000000 ) ) ;
#22215 = CARTESIAN_POINT ( 'NONE',  ( 4.458734124999999437, -42.81249999863440081, -5.460374474430324690E-16 ) ) ;
#22216 = CARTESIAN_POINT ( 'NONE',  ( 1.339745962155615144, 19.41965820146970501, 4.999999999999999112 ) ) ;
#22217 = CARTESIAN_POINT ( 'NONE',  ( -4.458734124999999437, -68.64583333196773651, -2.574251347313719407 ) ) ;
#22218 = CARTESIAN_POINT ( 'NONE',  ( -4.999999999999999112, -46.91666666666665719, 2.886751345948131764 ) ) ;
#22219 = CARTESIAN_POINT ( 'NONE',  ( -6.972266317189433020E-16, -57.12499999726879452, -5.000000000000000000 ) ) ;
#22220 = CARTESIAN_POINT ( 'NONE',  ( -6.972266317189433020E-16, -41.24999999999999289, -5.000000000000000000 ) ) ;
#22221 = VERTEX_POINT ( 'NONE', #54151 ) ;
#22222 = CARTESIAN_POINT ( 'NONE',  ( -4.458734124999999437, -110.3124999986343937, 0.000000000000000000 ) ) ;
#22223 = DIRECTION ( 'NONE',  ( -0.000000000000000000, 1.000000000000000000, -0.000000000000000000 ) ) ;
#22224 = CARTESIAN_POINT ( 'NONE',  ( 5.000000000000000000, -7.500000000000000000, -6.123233995736766282E-16 ) ) ;
#22225 = CARTESIAN_POINT ( 'NONE',  ( -3.152548672688508926E-16, -71.56249999863439371, -5.148502694627439702 ) ) ;
#22226 = CYLINDRICAL_SURFACE ( 'NONE', #46286, 5.000000000000000000 ) ;
#22227 = CARTESIAN_POINT ( 'NONE',  ( -5.000000000000000000, -13.95833333060215153, -2.886751345948128211 ) ) ;
#22229 = ORIENTED_EDGE ( 'NONE', *, *, #38648, .F. ) ;
#22228 = CARTESIAN_POINT ( 'NONE',  ( -2.229367062500000163, -39.47916666530107221, -3.861377020970580443 ) ) ;
#22230 = CARTESIAN_POINT ( 'NONE',  ( 1.975475456537005874E-15, -100.6249999972688016, 5.000000000000000000 ) ) ;
#22232 = ORIENTED_EDGE ( 'NONE', *, *, #62203, .F. ) ;
#22231 = CARTESIAN_POINT ( 'NONE',  ( 2.229367062500001939, 9.770833334698927786, 3.861377020970579999 ) ) ;
#22233 = CARTESIAN_POINT ( 'NONE',  ( -3.535533905932737309, -151.6250000000000000, -3.535533905932738197 ) ) ;
#22234 = CARTESIAN_POINT ( 'NONE',  ( 5.000000000000000888, -56.58333333333332860, 2.886751345948126879 ) ) ;
#22235 = CARTESIAN_POINT ( 'NONE',  ( -3.152801135295367096, -160.3125000013656063, -3.152801135295367541 ) ) ;
#22236 = CARTESIAN_POINT ( 'NONE',  ( 4.458734124999999437, -35.06249999863440792, -5.460374474430324690E-16 ) ) ;
#22237 = CARTESIAN_POINT ( 'NONE',  ( 0.000000000000000000, -170.0000000000000000, 5.000000000000000000 ) ) ;
#22238 = CARTESIAN_POINT ( 'NONE',  ( 4.458734125000001214, -80.89583333196773651, 2.574251347313718519 ) ) ;
#22239 = CARTESIAN_POINT ( 'NONE',  ( 3.535533905932738197, -164.8750000000000284, -3.535533905932738197 ) ) ;
#22240 = CARTESIAN_POINT ( 'NONE',  ( 4.458734124999998549, -84.72916666530106511, -2.574251347313721627 ) ) ;
#22241 = CARTESIAN_POINT ( 'NONE',  ( -54.64476657466781973, -130.0625000013656063, -4.444560631937228834 ) ) ;
#22242 = VECTOR ( 'NONE', #47904, 1000.000000000000000 ) ;
#22243 = CARTESIAN_POINT ( 'NONE',  ( 4.458734124999998549, -0.9791666653010713262, -2.574251347313721627 ) ) ;
#22244 = AXIS2_PLACEMENT_3D ( 'NONE', #37845, #43283, #53572 ) ;
#22245 = CARTESIAN_POINT ( 'NONE',  ( 4.458734125000001214, -37.14583333196773651, 2.574251347313718519 ) ) ;
#22246 = EDGE_CURVE ( 'NONE', #11915, #27774, #52901, .T. ) ;
#22247 = CARTESIAN_POINT ( 'NONE',  ( 2.499999999999998668, -16.20833333060214443, -4.330127018922193649 ) ) ;
#22248 = CARTESIAN_POINT ( 'NONE',  ( -3.152548672688508926E-16, -83.81249999863439371, -5.148502694627439702 ) ) ;
#22249 = VERTEX_POINT ( 'NONE', #53835 ) ;
#22250 = CARTESIAN_POINT ( 'NONE',  ( 6.123233995736766282E-16, -120.0000000000000000, -5.000000000000000000 ) ) ;
#22251 =( BOUNDED_CURVE ( )  B_SPLINE_CURVE ( 2, ( #20529, #31118, #26291, #1243, #35000, #20843, #50740, #15055, #10540 ),
 .UNSPECIFIED., .F., .F. ) 
 B_SPLINE_CURVE_WITH_KNOTS ( ( 3, 2, 2, 2, 3 ),
 ( 0.7916666666666664076, 0.7958333333333330595, 0.7999999999999998224, 0.8041666666666664742, 0.8083333333333331261 ),
 .UNSPECIFIED. ) 
 CURVE ( )  GEOMETRIC_REPRESENTATION_ITEM ( )  RATIONAL_B_SPLINE_CURVE ( ( 1.000000000000003997, 0.9238795325112826307, 1.000000000000000000, 0.9238795325112867385, 1.000000000000000000, 0.9238795325112867385, 1.000000000000000000, 0.9238795325112908463, 0.9999999999999958922 ) ) 
 REPRESENTATION_ITEM ( '' )  );
#22252 = CARTESIAN_POINT ( 'NONE',  ( -5.000000000000000000, -11.87499999726881761, 0.000000000000000000 ) ) ;
#22253 = CARTESIAN_POINT ( 'NONE',  ( 2.229367062500001939, -67.22916666530106511, 3.861377020970579999 ) ) ;
#22254 = CARTESIAN_POINT ( 'NONE',  ( 4.458734124999999437, -10.06249999863440614, -5.460374474430324690E-16 ) ) ;
#22255 = ORIENTED_EDGE ( 'NONE', *, *, #29108, .F. ) ;
#22256 = CARTESIAN_POINT ( 'NONE',  ( 1.975475456537005874E-15, -84.74999999999998579, 5.000000000000000000 ) ) ;
#22257 = DIRECTION ( 'NONE',  ( -0.000000000000000000, 1.000000000000000000, -0.000000000000000000 ) ) ;
#22258 = CARTESIAN_POINT ( 'NONE',  ( 2.229367062500001939, -9.229166665301075767, 3.861377020970579999 ) ) ;
#22259 = CARTESIAN_POINT ( 'NONE',  ( 6.158835246850666199E-14, 8.875000002731182391, -4.999999999999999112 ) ) ;
#22260 = CARTESIAN_POINT ( 'NONE',  ( 9.457646018065525792E-16, 3.937500001365595192, 5.148502694627439702 ) ) ;
#22261 = CARTESIAN_POINT ( 'NONE',  ( -5.000000000000000000, -76.08333333333334281, -2.886751345948128211 ) ) ;
#22262 = CARTESIAN_POINT ( 'NONE',  ( 1.846868145590736310, -157.6250000013655779, 4.458734124999997661 ) ) ;
#22263 = CARTESIAN_POINT ( 'NONE',  ( 2.229367062499998831, 26.10416666803225993, -3.861377020970580887 ) ) ;
#22264 = ORIENTED_EDGE ( 'NONE', *, *, #5596, .T. ) ;
#22265 = CARTESIAN_POINT ( 'NONE',  ( 4.458734125000000326, -84.89583333196773651, 2.574251347313718519 ) ) ;
#22266 = CARTESIAN_POINT ( 'NONE',  ( 0.000000000000000000, -170.0000000000000000, 0.000000000000000000 ) ) ;
#22267 = CARTESIAN_POINT ( 'NONE',  ( 4.458734124999999437, -9.812499998634406140, -5.460374474430324690E-16 ) ) ;
#22268 = DIRECTION ( 'NONE',  ( 0.000000000000000000, 0.000000000000000000, 1.000000000000000000 ) ) ;
#22269 = CYLINDRICAL_SURFACE ( 'NONE', #44844, 5.000000000000000000 ) ;
#22270 = CARTESIAN_POINT ( 'NONE',  ( -5.000000000000000000, -36.95833333060213732, -2.886751345948128211 ) ) ;
#22271 = DIRECTION ( 'NONE',  ( 0.000000000000000000, -0.000000000000000000, -1.000000000000000000 ) ) ;
#22272 = CARTESIAN_POINT ( 'NONE',  ( 4.458734124999998549, 24.27083333469892779, -2.574251347313721627 ) ) ;
#22273 = CARTESIAN_POINT ( 'NONE',  ( -5.000000000000000000, -20.87499999726881228, 0.000000000000000000 ) ) ;
#22274 = CARTESIAN_POINT ( 'NONE',  ( 2.229367062500001939, 22.02083333469892779, 3.861377020970579999 ) ) ;
#22275 = CARTESIAN_POINT ( 'NONE',  ( -2.229367062499996610, -52.14583333196773651, 3.861377020970582219 ) ) ;
#22276 = CARTESIAN_POINT ( 'NONE',  ( 4.458734124999999437, -1.062499998634405696, -5.460374474430324690E-16 ) ) ;
#22277 = VECTOR ( 'NONE', #6313, 1000.000000000000000 ) ;
#22278 = CARTESIAN_POINT ( 'NONE',  ( 2.071067811865561215, -160.3125000027312126, 4.999999999999913847 ) ) ;
#22279 = CARTESIAN_POINT ( 'NONE',  ( -3.535250795749689387E-16, 16.75000000000000355, -5.773502691896257311 ) ) ;
#22280 = CARTESIAN_POINT ( 'NONE',  ( 5.000000000000000000, -142.1875000027312126, 2.071067811865478614 ) ) ;
#22281 = CYLINDRICAL_SURFACE ( 'NONE', #48964, 5.000000000000000000 ) ;
#22282 = CARTESIAN_POINT ( 'NONE',  ( -4.458734124999998549, -46.22916666530106511, 2.574251347313722516 ) ) ;
#22283 = CARTESIAN_POINT ( 'NONE',  ( 2.499999999999998668, -81.20833333060213022, -4.330127018922193649 ) ) ;
#22284 = AXIS2_PLACEMENT_3D ( 'NONE', #43242, #4960, #18500 ) ;
#22285 = CARTESIAN_POINT ( 'NONE',  ( -50.70258187064364108, -139.3750000013656063, 2.196230717870141014 ) ) ;
#22286 = DIRECTION ( 'NONE',  ( -0.000000000000000000, -0.000000000000000000, 1.000000000000000000 ) ) ;
#22287 = CARTESIAN_POINT ( 'NONE',  ( 5.000000000000000888, -22.58333333333332860, 2.886751345948126879 ) ) ;
#22288 = AXIS2_PLACEMENT_3D ( 'NONE', #19957, #34759, #29601 ) ;
#22289 = CARTESIAN_POINT ( 'NONE',  ( -4.458734124999999437, -86.56249999863439371, 0.000000000000000000 ) ) ;
#22290 = CARTESIAN_POINT ( 'NONE',  ( 4.458734124999999437, -157.6250000013655779, -1.846868145590734978 ) ) ;
#22291 = CARTESIAN_POINT ( 'NONE',  ( -2.500000000000000444, -32.16666666666666430, -4.330127018922193649 ) ) ;
#22292 = CARTESIAN_POINT ( 'NONE',  ( -2.500000000000000444, 23.83333333333333215, -4.330127018922193649 ) ) ;
#22293 = VERTEX_POINT ( 'NONE', #4019 ) ;
#22294 = CARTESIAN_POINT ( 'NONE',  ( -3.152548672688508926E-16, 20.18750000136559208, -5.148502694627439702 ) ) ;
#22295 = ORIENTED_EDGE ( 'NONE', *, *, #59480, .F. ) ;
#22296 = CARTESIAN_POINT ( 'NONE',  ( -4.458734124999999437, -90.31249999863440792, 0.000000000000000000 ) ) ;
#22297 = CARTESIAN_POINT ( 'NONE',  ( -2.229367062499996610, 14.60416666803226171, 3.861377020970582219 ) ) ;
#22298 = CARTESIAN_POINT ( 'NONE',  ( 2.499999999999998668, 15.79166666939785202, -4.330127018922193649 ) ) ;
#22299 = CARTESIAN_POINT ( 'NONE',  ( -5.000000000000000000, 6.999999999999999112, 0.000000000000000000 ) ) ;
#22300 = EDGE_CURVE ( 'NONE', #12016, #15518, #25974, .T. ) ;
#22301 = CARTESIAN_POINT ( 'NONE',  ( -2.229367062500000163, -57.47916666530107932, -3.861377020970580443 ) ) ;
#22302 = CARTESIAN_POINT ( 'NONE',  ( -1.339745962155613812, -8.205341801261480938, -5.000000000000000000 ) ) ;
#22303 = CARTESIAN_POINT ( 'NONE',  ( 5.000000000000000000, -80.50000000000000000, -6.123233995736766282E-16 ) ) ;
#22304 = CARTESIAN_POINT ( 'NONE',  ( -59.29741812935640155, -135.8750000013655779, -2.196230717870135685 ) ) ;
#22305 = CARTESIAN_POINT ( 'NONE',  ( 1.975475456537005874E-15, 7.375000002731186832, 5.000000000000000000 ) ) ;
#22306 = CARTESIAN_POINT ( 'NONE',  ( 0.000000000000000000, -170.0000000000000000, 0.000000000000000000 ) ) ;
#22307 = DIRECTION ( 'NONE',  ( 0.000000000000000000, 0.000000000000000000, 1.000000000000000000 ) ) ;
#22308 = CARTESIAN_POINT ( 'NONE',  ( 5.000000000000000000, -41.41666666666667140, -2.886751345948129988 ) ) ;
#22309 = CARTESIAN_POINT ( 'NONE',  ( 1.975475456537005874E-15, 13.37500000273118417, 5.000000000000000000 ) ) ;
#22311 = CARTESIAN_POINT ( 'NONE',  ( 2.229367062500001939, -20.22916666530107221, 3.861377020970579999 ) ) ;
#22310 = CARTESIAN_POINT ( 'NONE',  ( -2.499999999999996447, -42.83333333333333570, 4.330127018922195425 ) ) ;
#22312 = LINE ( 'NONE', #31637, #6028 ) ;
#22313 = CARTESIAN_POINT ( 'NONE',  ( -4.458734124999999437, -64.39583333196772230, -2.574251347313719407 ) ) ;
#22314 = CARTESIAN_POINT ( 'NONE',  ( 1.846868145590735200, -150.5000000013656347, -4.458734125000000326 ) ) ;
#22315 = CARTESIAN_POINT ( 'NONE',  ( 2.229367062500001939, -68.97916666530107932, 3.861377020970579999 ) ) ;
#22316 = CARTESIAN_POINT ( 'NONE',  ( -59.29741812935640155, -146.8750000013656063, -2.196230717870135685 ) ) ;
#22317 = CARTESIAN_POINT ( 'NONE',  ( 9.457646018065525792E-16, -18.31249999863440436, 5.148502694627439702 ) ) ;
#22318 = CARTESIAN_POINT ( 'NONE',  ( 5.000000000000000000, -61.29166666393548013, -2.886751345948129988 ) ) ;
#22319 = ORIENTED_EDGE ( 'NONE', *, *, #29322, .F. ) ;
#22320 = CARTESIAN_POINT ( 'NONE',  ( -6.972266317189433020E-16, -85.12499999726880162, -5.000000000000000000 ) ) ;
#22321 = ORIENTED_EDGE ( 'NONE', *, *, #18546, .F. ) ;
#22322 = CARTESIAN_POINT ( 'NONE',  ( -4.458734124999998549, -62.47916666530106511, 2.574251347313722516 ) ) ;
#22323 = FACE_OUTER_BOUND ( 'NONE', #57075, .T. ) ;
#22324 = CARTESIAN_POINT ( 'NONE',  ( 6.123233995736766282E-16, -170.0000000000000000, -5.000000000000000000 ) ) ;
#22325 = CARTESIAN_POINT ( 'NONE',  ( 3.152801135295367541, -151.3125000013655779, -3.152801135295367541 ) ) ;
#22326 = ORIENTED_EDGE ( 'NONE', *, *, #6001, .F. ) ;
#22327 = VECTOR ( 'NONE', #48986, 1000.000000000000000 ) ;
#22328 = CARTESIAN_POINT ( 'NONE',  ( -5.000000000000000000, 27.04166666939785202, -2.886751345948128211 ) ) ;
#22329 = CARTESIAN_POINT ( 'NONE',  ( -52.53715891517739323, -126.4375000000000426, -4.819101127000233298 ) ) ;
#22330 = CARTESIAN_POINT ( 'NONE',  ( -6.972266317189433020E-16, -8.249999999999998224, -5.000000000000000000 ) ) ;
#22331 = CARTESIAN_POINT ( 'NONE',  ( 2.229367062500001939, -53.22916666530107221, 3.861377020970579999 ) ) ;
#22332 = ORIENTED_EDGE ( 'NONE', *, *, #56313, .F. ) ;
#22333 = VECTOR ( 'NONE', #58944, 1000.000000000000000 ) ;
#22334 =( BOUNDED_CURVE ( )  B_SPLINE_CURVE ( 2, ( #12198, #26995, #46614, #22174, #61421, #14078, #24063, #56908, #37587 ),
 .UNSPECIFIED., .F., .F. ) 
 B_SPLINE_CURVE_WITH_KNOTS ( ( 3, 2, 2, 2, 3 ),
 ( 0.09375000000000000000, 0.09444444444444444198, 0.09583333333333333981, 0.09722222222222222376, 0.09791666666666666574 ),
 .UNSPECIFIED. ) 
 CURVE ( )  GEOMETRIC_REPRESENTATION_ITEM ( )  RATIONAL_B_SPLINE_CURVE ( ( 0.9330127018922194093, 0.9330127018922194093, 1.000000000000000000, 0.8660254037844387076, 1.000000000000000000, 0.8660254037844387076, 1.000000000000000000, 0.9330127018922194093, 0.9330127018922194093 ) ) 
 REPRESENTATION_ITEM ( '' )  );
#22335 = DIRECTION ( 'NONE',  ( 0.000000000000000000, 0.000000000000000000, 1.000000000000000000 ) ) ;
#22336 = VECTOR ( 'NONE', #38404, 1000.000000000000000 ) ;
#22337 = B_SPLINE_CURVE_WITH_KNOTS ( 'NONE', 3,
 ( #18687, #54041, #18994, #29267, #59200, #3907, #34103, #29591, #63084, #43751 ),
 .UNSPECIFIED., .F., .F.,
 ( 4, 2, 2, 2, 4 ),
 ( 0.000000000000000000, 0.002305503304226490767, 0.004611006608452981534, 0.006916509912679473168, 0.009222013216905964803 ),
 .UNSPECIFIED. ) ;
#22338 = CARTESIAN_POINT ( 'NONE',  ( -4.458734124999999437, 8.687500001365595637, 0.000000000000000000 ) ) ;
#22339 = CARTESIAN_POINT ( 'NONE',  ( 2.229367062499998831, 21.35416666803226349, -3.861377020970580887 ) ) ;
#22340 = CARTESIAN_POINT ( 'NONE',  ( -52.80376928212989185, -147.8750000013656063, -4.297418129356379346 ) ) ;
#22341 = CARTESIAN_POINT ( 'NONE',  ( 1.975475456537005874E-15, -23.62499999726880873, 5.000000000000000000 ) ) ;
#22342 = CARTESIAN_POINT ( 'NONE',  ( 4.458734124999997661, -168.5000000013655779, 1.846868145590737864 ) ) ;
#22343 = ORIENTED_EDGE ( 'NONE', *, *, #15502, .F. ) ;
#22344 = CARTESIAN_POINT ( 'NONE',  ( -2.229367062500000163, -69.47916666530107932, -3.861377020970580443 ) ) ;
#22345 = CARTESIAN_POINT ( 'NONE',  ( 1.975475456537005874E-15, -10.62499999726881228, 5.000000000000000000 ) ) ;
#22346 = CARTESIAN_POINT ( 'NONE',  ( 4.458734125000001214, 11.10416666803225993, 2.574251347313718519 ) ) ;
#22347 = CARTESIAN_POINT ( 'NONE',  ( 5.000000000000000888, -69.45833333060214443, 2.886751345948126879 ) ) ;
#22348 = CARTESIAN_POINT ( 'NONE',  ( -4.458734124999998549, -60.47916666530105800, 2.574251347313722516 ) ) ;
#22349 = CARTESIAN_POINT ( 'NONE',  ( -2.499999999999996447, -16.70833333060214443, 4.330127018922195425 ) ) ;
#22350 = CARTESIAN_POINT ( 'NONE',  ( 1.975475456537005874E-15, -32.62499999726880873, 5.000000000000000000 ) ) ;
#22351 = CARTESIAN_POINT ( 'NONE',  ( 4.729367062499999719, -169.8437500006828031, 0.000000000000000000 ) ) ;
#22352 = CARTESIAN_POINT ( 'NONE',  ( 0.000000000000000000, -170.0000000000000000, 0.000000000000000000 ) ) ;
#22353 = CARTESIAN_POINT ( 'NONE',  ( 2.229367062499998831, -34.64583333196772941, -3.861377020970580887 ) ) ;
#22354 = CARTESIAN_POINT ( 'NONE',  ( 4.458734124999998549, -20.97916666530107221, -2.574251347313721627 ) ) ;
#22355 = ORIENTED_EDGE ( 'NONE', *, *, #57552, .T. ) ;
#22356 = CARTESIAN_POINT ( 'NONE',  ( -6.972266317189433020E-16, -48.24999999999999289, -5.000000000000000000 ) ) ;
#22357 = CARTESIAN_POINT ( 'NONE',  ( -4.458734124999999437, -110.3124999986343937, 0.000000000000000000 ) ) ;
#22358 = CARTESIAN_POINT ( 'NONE',  ( 5.000000000000000000, -155.1250000027311842, 0.000000000000000000 ) ) ;
#22359 = ORIENTED_EDGE ( 'NONE', *, *, #16199, .T. ) ;
#22360 = CARTESIAN_POINT ( 'NONE',  ( 4.458734124999999437, -104.0624999986344079, -5.460374474430324690E-16 ) ) ;
#22361 = CARTESIAN_POINT ( 'NONE',  ( -4.458734124999999437, -32.39583333196773651, -2.574251347313719407 ) ) ;
#22362 = CARTESIAN_POINT ( 'NONE',  ( -3.535250795749689387E-16, -64.12499999726881583, -5.773502691896257311 ) ) ;
#22363 = CARTESIAN_POINT ( 'NONE',  ( -59.29741812935640155, -153.8750000013655779, -2.196230717870135685 ) ) ;
#22364 = CARTESIAN_POINT ( 'NONE',  ( -2.071067811865478170, -147.3125000000000000, 5.000000000000000000 ) ) ;
#22365 = CARTESIAN_POINT ( 'NONE',  ( -4.458734124999997661, -31.22916666530106866, 2.574251347313722516 ) ) ;
#22366 = CARTESIAN_POINT ( 'NONE',  ( 9.457646018065525792E-16, -68.31249999863440792, 5.148502694627439702 ) ) ;
#22367 = LINE ( 'NONE', #55517, #56221 ) ;
#22368 = CARTESIAN_POINT ( 'NONE',  ( -4.458734124999997661, -25.22916666530106866, 2.574251347313722516 ) ) ;
#22369 = CARTESIAN_POINT ( 'NONE',  ( 1.975475456537005874E-15, -32.62499999726880873, 5.000000000000000000 ) ) ;
#22370 = CARTESIAN_POINT ( 'NONE',  ( 75.00000000000000000, 15.00000000000000000, 8.999999999999998224 ) ) ;
#22371 = CARTESIAN_POINT ( 'NONE',  ( 2.500000000000002220, -15.66666666666666963, 4.330127018922192761 ) ) ;
#22372 = CARTESIAN_POINT ( 'NONE',  ( -3.152801135295367985, -148.8125000013655779, 3.152801135295367096 ) ) ;
#22373 = EDGE_LOOP ( 'NONE', ( #26585, #57752, #5361, #55627 ) ) ;
#22374 = CARTESIAN_POINT ( 'NONE',  ( 5.000000000000000000, -150.0000000000000284, 0.000000000000000000 ) ) ;
#22375 = CARTESIAN_POINT ( 'NONE',  ( -4.458734124999999437, -51.56249999863440792, 0.000000000000000000 ) ) ;
#22376 = VECTOR ( 'NONE', #57240, 1000.000000000000000 ) ;
#22377 = LINE ( 'NONE', #13030, #55098 ) ;
#22378 = CARTESIAN_POINT ( 'NONE',  ( -5.000000000000000000, -1.083333333333331927, -2.886751345948128211 ) ) ;
#22379 = CARTESIAN_POINT ( 'NONE',  ( 2.499999999999998668, 23.66666666666666430, -4.330127018922193649 ) ) ;
#22380 = EDGE_CURVE ( 'NONE', #41, #25378, #19741, .T. ) ;
#22381 = AXIS2_PLACEMENT_3D ( 'NONE', #49246, #29937, #14505 ) ;
#22382 = CARTESIAN_POINT ( 'NONE',  ( 2.229367062499998831, -0.6458333319677399542, -3.861377020970580887 ) ) ;
#22383 = CARTESIAN_POINT ( 'NONE',  ( 1.975475456537005874E-15, 4.375000002731185056, 5.000000000000000000 ) ) ;
#22384 = LINE ( 'NONE', #51655, #47156 ) ;
#22385 = CARTESIAN_POINT ( 'NONE',  ( -5.000000000000000000, -74.08333333333330017, -2.886751345948128211 ) ) ;
#22386 = CARTESIAN_POINT ( 'NONE',  ( 4.458734124999999437, 14.93750000136559386, -5.460374474430324690E-16 ) ) ;
#22387 = CARTESIAN_POINT ( 'NONE',  ( -4.999999999999999112, 3.208333336064520758, 2.886751345948131764 ) ) ;
#22388 = EDGE_LOOP ( 'NONE', ( #61387, #17173, #12323, #20004 ) ) ;
#22389 = CARTESIAN_POINT ( 'NONE',  ( 5.000000000000000000, 26.50000000000000000, -6.123233995736766282E-16 ) ) ;
#22390 = ORIENTED_EDGE ( 'NONE', *, *, #22398, .T. ) ;
#22391 = CARTESIAN_POINT ( 'NONE',  ( 1.975475456537005874E-15, -70.75000000000000000, 5.000000000000000000 ) ) ;
#22392 = CARTESIAN_POINT ( 'NONE',  ( 4.458734124999998549, -50.72916666530107932, -2.574251347313721627 ) ) ;
#22393 = CARTESIAN_POINT ( 'NONE',  ( 4.458734124999999437, -162.6875000013655779, 0.000000000000000000 ) ) ;
#22394 = EDGE_CURVE ( 'NONE', #5037, #43748, #26486, .T. ) ;
#22395 = CARTESIAN_POINT ( 'NONE',  ( 5.000000000000000888, -47.45833333060214443, 2.886751345948126879 ) ) ;
#22396 = ORIENTED_EDGE ( 'NONE', *, *, #58946, .F. ) ;
#22398 = EDGE_CURVE ( 'NONE', #58460, #19793, #11675, .T. ) ;
#22397 = CARTESIAN_POINT ( 'NONE',  ( -2.229367062499996610, -25.14583333196773651, 3.861377020970582219 ) ) ;
#22399 = ORIENTED_EDGE ( 'NONE', *, *, #28102, .T. ) ;
#22400 = CARTESIAN_POINT ( 'NONE',  ( -5.000000000000000000, -87.00000000000000000, 0.000000000000000000 ) ) ;
#22401 = CARTESIAN_POINT ( 'NONE',  ( -1.846868145590734756, -166.1250000013655779, -4.458734125000000326 ) ) ;
#22402 =( BOUNDED_CURVE ( )  B_SPLINE_CURVE ( 2, ( #35311, #49139, #5723, #5082, #24704, #59444, #35630, #6053, #6371 ),
 .UNSPECIFIED., .F., .F. ) 
 B_SPLINE_CURVE_WITH_KNOTS ( ( 3, 2, 2, 2, 3 ),
 ( 0.1187500000000000083, 0.1194444444444444503, 0.1208333333333333343, 0.1222222222222222182, 0.1229166666666666741 ),
 .UNSPECIFIED. ) 
 CURVE ( )  GEOMETRIC_REPRESENTATION_ITEM ( )  RATIONAL_B_SPLINE_CURVE ( ( 0.9330127018922194093, 0.9330127018922200755, 1.000000000000000000, 0.8660254037844387076, 1.000000000000000000, 0.8660254037844387076, 1.000000000000000000, 0.9330127018922187432, 0.9330127018922194093 ) ) 
 REPRESENTATION_ITEM ( '' )  );
#22403 = CARTESIAN_POINT ( 'NONE',  ( 1.975475456537005874E-15, -42.74999999999999289, 5.000000000000000000 ) ) ;
#22404 = CARTESIAN_POINT ( 'NONE',  ( -60.14911071818854538, -136.0625000000000284, 1.666127454062681368 ) ) ;
#22405 = CARTESIAN_POINT ( 'NONE',  ( 4.458734124999999437, -31.06249999863440436, -5.460374474430324690E-16 ) ) ;
#22406 = FACE_OUTER_BOUND ( 'NONE', #46029, .T. ) ;
#22407 = ORIENTED_EDGE ( 'NONE', *, *, #3927, .T. ) ;
#22408 = CARTESIAN_POINT ( 'NONE',  ( -3.152548672688508926E-16, -80.56249999863440792, -5.148502694627439702 ) ) ;
#22409 = CARTESIAN_POINT ( 'NONE',  ( -2.229367062499996610, 21.85416666803226349, 3.861377020970582219 ) ) ;
#22410 = CARTESIAN_POINT ( 'NONE',  ( -1.339745962155613812, -29.08034179853029144, -5.000000000000000000 ) ) ;
#22411 = EDGE_LOOP ( 'NONE', ( #19658, #18192, #46371, #35893 ) ) ;
#22412 = CARTESIAN_POINT ( 'NONE',  ( -6.972266317189433020E-16, -23.12499999726880873, -5.000000000000000000 ) ) ;
#22413 = CARTESIAN_POINT ( 'NONE',  ( -52.10840900171896806, -143.4375000013656063, 3.393966926194110556 ) ) ;
#22414 = CARTESIAN_POINT ( 'NONE',  ( 2.229367062499998831, -79.89583333196773651, -3.861377020970580887 ) ) ;
#22415 = CARTESIAN_POINT ( 'NONE',  ( -56.66612745406270335, -130.4375000027312410, -5.149110718188516067 ) ) ;
#22416 = CARTESIAN_POINT ( 'NONE',  ( 0.000000000000000000, -120.0000000000000000, 0.000000000000000000 ) ) ;
#22417 = CARTESIAN_POINT ( 'NONE',  ( 1.975475456537005874E-15, -9.750000000000000000, 5.000000000000000000 ) ) ;
#22418 = VECTOR ( 'NONE', #37451, 1000.000000000000000 ) ;
#22419 = CARTESIAN_POINT ( 'NONE',  ( -6.972266317189433020E-16, -20.24999999999999645, -5.000000000000000000 ) ) ;
#22420 = CARTESIAN_POINT ( 'NONE',  ( 4.458734125000000326, -53.89583333196773651, 2.574251347313718519 ) ) ;
#22421 = DIRECTION ( 'NONE',  ( -0.000000000000000000, 1.000000000000000000, -0.000000000000000000 ) ) ;
#22422 = CARTESIAN_POINT ( 'NONE',  ( -4.458734124999998549, 27.77083333469892423, 2.574251347313722516 ) ) ;
#22423 = AXIS2_PLACEMENT_3D ( 'NONE', #16431, #55994, #6471 ) ;
#22424 = CARTESIAN_POINT ( 'NONE',  ( 5.000000000000000000, -104.4166666666666572, -2.886751345948129988 ) ) ;
#22425 = CARTESIAN_POINT ( 'NONE',  ( -1.339745962155613812, 3.794658198738521282, -5.000000000000000000 ) ) ;
#22426 = CARTESIAN_POINT ( 'NONE',  ( -2.229367062500000163, -38.72916666530107221, -3.861377020970580443 ) ) ;
#22427 = EDGE_CURVE ( 'NONE', #32079, #24403, #36686, .T. ) ;
#22428 = CARTESIAN_POINT ( 'NONE',  ( 2.499999999999998668, 1.791666669397853795, -4.330127018922193649 ) ) ;
#22429 = FACE_OUTER_BOUND ( 'NONE', #8755, .T. ) ;
#22430 = CARTESIAN_POINT ( 'NONE',  ( 1.255007937094098239E-14, 24.75000000000000000, -4.999999999999999112 ) ) ;
#22431 = CARTESIAN_POINT ( 'NONE',  ( 9.457646018065525792E-16, -80.31249999863440792, 5.148502694627439702 ) ) ;
#22432 = CARTESIAN_POINT ( 'NONE',  ( -4.458734124999999437, -101.3124999986344079, 0.000000000000000000 ) ) ;
#22433 =( BOUNDED_CURVE ( )  B_SPLINE_CURVE ( 2, ( #20022, #39947, #14553, #54111, #5235, #39628, #4914, #54764, #25483 ),
 .UNSPECIFIED., .F., .F. ) 
 B_SPLINE_CURVE_WITH_KNOTS ( ( 3, 2, 2, 2, 3 ),
 ( 0.4520833333333333370, 0.4527777777777777790, 0.4541666666666666630, 0.4555555555555555469, 0.4562499999999999889 ),
 .UNSPECIFIED. ) 
 CURVE ( )  GEOMETRIC_REPRESENTATION_ITEM ( )  RATIONAL_B_SPLINE_CURVE ( ( 0.9330127018922194093, 0.9330127018922194093, 1.000000000000000000, 0.8660254037844387076, 1.000000000000000000, 0.8660254037844387076, 1.000000000000000000, 0.9330127018922194093, 0.9330127018922194093 ) ) 
 REPRESENTATION_ITEM ( '' )  );
#22434 = CARTESIAN_POINT ( 'NONE',  ( -2.229367062499996610, -3.395833331967738733, 3.861377020970582219 ) ) ;
#22435 = VERTEX_POINT ( 'NONE', #21668 ) ;
#22436 = CARTESIAN_POINT ( 'NONE',  ( 1.975475456537005874E-15, -82.74999999999998579, 5.000000000000000000 ) ) ;
#22437 = CARTESIAN_POINT ( 'NONE',  ( -2.229367062499996610, -91.14583333196773651, 3.861377020970582219 ) ) ;
#22438 = CARTESIAN_POINT ( 'NONE',  ( 3.061616997868383141E-16, -163.8750000027311842, -5.000000000000000000 ) ) ;
#22439 = CARTESIAN_POINT ( 'NONE',  ( 2.229367062499998831, -88.89583333196773651, -3.861377020970580887 ) ) ;
#22440 = CARTESIAN_POINT ( 'NONE',  ( -4.458734124999999437, 14.43750000136559386, 0.000000000000000000 ) ) ;
#22441 = CARTESIAN_POINT ( 'NONE',  ( 1.339745962155641346, -2.169658196007335338, -4.999999999999983125 ) ) ;
#22442 = CARTESIAN_POINT ( 'NONE',  ( -54.64476657466781973, -134.8125000013656063, -4.444560631937228834 ) ) ;
#22443 = CARTESIAN_POINT ( 'NONE',  ( -2.229367062500000163, -12.47916666530107044, -3.861377020970580443 ) ) ;
#22444 = CARTESIAN_POINT ( 'NONE',  ( -3.152548672688508926E-16, 19.18750000136559208, -5.148502694627439702 ) ) ;
#22445 = CARTESIAN_POINT ( 'NONE',  ( -3.152548672688508926E-16, -52.81249999863440792, -5.148502694627439702 ) ) ;
#22446 = CARTESIAN_POINT ( 'NONE',  ( -5.000000000000000000, -15.87499999726881406, 0.000000000000000000 ) ) ;
#22447 = CARTESIAN_POINT ( 'NONE',  ( -2.229367062499996610, -8.145833331967736513, 3.861377020970582219 ) ) ;
#22448 = CARTESIAN_POINT ( 'NONE',  ( 5.000000000000000000, -84.49999999999998579, -6.123233995736766282E-16 ) ) ;
#22449 = ORIENTED_EDGE ( 'NONE', *, *, #25496, .T. ) ;
#22450 = CARTESIAN_POINT ( 'NONE',  ( -4.458734124999997661, -34.47916666530107221, 2.574251347313722516 ) ) ;
#22451 = CARTESIAN_POINT ( 'NONE',  ( -50.40829686548195099, -126.2500000013656063, -1.485763867205728284 ) ) ;
#22452 = CARTESIAN_POINT ( 'NONE',  ( 5.000000000000000000, 26.62500000273118772, -6.123233995736766282E-16 ) ) ;
#22453 = CARTESIAN_POINT ( 'NONE',  ( -2.229367062500000163, -78.47916666530106511, -3.861377020970580443 ) ) ;
#22454 = CARTESIAN_POINT ( 'NONE',  ( 9.457646018065525792E-16, 26.68750000136559564, 5.148502694627439702 ) ) ;
#22455 = CARTESIAN_POINT ( 'NONE',  ( 4.458734124999999437, -151.6250000013655779, -1.846868145590734978 ) ) ;
#22456 = CARTESIAN_POINT ( 'NONE',  ( 4.458734124999998549, 17.27083333469892779, -2.574251347313721627 ) ) ;
#22457 = EDGE_CURVE ( 'NONE', #7439, #12164, #49820, .T. ) ;
#22458 = EDGE_CURVE ( 'NONE', #58717, #20660, #56427, .T. ) ;
#22459 = CARTESIAN_POINT ( 'NONE',  ( -4.999999999999998224, -43.79166666393546592, 2.886751345948131764 ) ) ;
#22460 = DIRECTION ( 'NONE',  ( -0.000000000000000000, 1.000000000000000000, -0.000000000000000000 ) ) ;
#22461 = CARTESIAN_POINT ( 'NONE',  ( 4.458734125000000326, -83.14583333196773651, 2.574251347313718519 ) ) ;
#22462 = CARTESIAN_POINT ( 'NONE',  ( 5.000000000000000000, -64.50000000000000000, -6.123233995736766282E-16 ) ) ;
#22463 = DIRECTION ( 'NONE',  ( -0.000000000000000000, 1.000000000000000000, -0.000000000000000000 ) ) ;
#22464 = CARTESIAN_POINT ( 'NONE',  ( 5.000000000000000000, 16.62500000273118417, -6.123233995736766282E-16 ) ) ;
#22465 = ORIENTED_EDGE ( 'NONE', *, *, #48881, .T. ) ;
#22466 = CARTESIAN_POINT ( 'NONE',  ( -2.480964764533239819E-13, -94.75000000000000000, 5.000000000000000000 ) ) ;
#22467 = VECTOR ( 'NONE', #17433, 1000.000000000000000 ) ;
#22468 = CARTESIAN_POINT ( 'NONE',  ( -2.500000000000000444, 27.83333333333333215, -4.330127018922193649 ) ) ;
#22470 = CARTESIAN_POINT ( 'NONE',  ( 2.499999999999998668, -25.33333333333333215, -4.330127018922193649 ) ) ;
#22469 = CARTESIAN_POINT ( 'NONE',  ( -1.339745962155613812, -109.0803417985302843, -5.000000000000000000 ) ) ;
#22471 = CARTESIAN_POINT ( 'NONE',  ( 2.229367062499998831, -25.64583333196773651, -3.861377020970580887 ) ) ;
#22472 = VECTOR ( 'NONE', #51195, 1000.000000000000000 ) ;
#22473 = ADVANCED_FACE ( 'NONE', ( #41259 ), #40945, .T. ) ;
#22474 = CARTESIAN_POINT ( 'NONE',  ( -2.500000000000000444, -30.04166666393548013, -4.330127018922193649 ) ) ;
#22475 = B_SPLINE_CURVE_WITH_KNOTS ( 'NONE', 3,
 ( #24789, #5171, #18695, #44395, #40, #43759, #58876, #14807, #34112 ),
 .UNSPECIFIED., .F., .F.,
 ( 4, 2, 1, 2, 4 ),
 ( 6.245710625686469831E-20, 0.002165063509461098365, 0.004330127018922195863, 0.006495190528383293360, 0.008660254037844389990 ),
 .UNSPECIFIED. ) ;
#22477 = VERTEX_POINT ( 'NONE', #35187 ) ;
#22476 = CARTESIAN_POINT ( 'NONE',  ( -2.229367062499996610, -62.14583333196774362, 3.861377020970582219 ) ) ;
#22478 = EDGE_CURVE ( 'NONE', #37963, #14479, #62991, .T. ) ;
#22480 = ORIENTED_EDGE ( 'NONE', *, *, #61048, .T. ) ;
#22479 = CARTESIAN_POINT ( 'NONE',  ( 2.229367062499998831, -10.89583333196773829, -3.861377020970580887 ) ) ;
#22481 = CARTESIAN_POINT ( 'NONE',  ( 2.500000000000002220, -69.66666666666667140, 4.330127018922192761 ) ) ;
#22482 = CARTESIAN_POINT ( 'NONE',  ( -51.60603307380591787, -137.9375000013656063, -2.891590998281053704 ) ) ;
#22483 = CARTESIAN_POINT ( 'NONE',  ( 9.457646018065525792E-16, -49.31249999863441502, 5.148502694627439702 ) ) ;
#22484 = CARTESIAN_POINT ( 'NONE',  ( 2.499999999999998668, -76.20833333060214443, -4.330127018922193649 ) ) ;
#22486 = ORIENTED_EDGE ( 'NONE', *, *, #16075, .F. ) ;
#22485 = CARTESIAN_POINT ( 'NONE',  ( 1.975475456537005874E-15, -65.62499999726881583, 5.000000000000000000 ) ) ;
#22487 = CARTESIAN_POINT ( 'NONE',  ( -58.80597590150559739, -151.0000000000000284, 3.242614290531460330 ) ) ;
#22488 = CARTESIAN_POINT ( 'NONE',  ( 4.458734125000001214, -15.14583333196773651, 2.574251347313718519 ) ) ;
#22489 = CARTESIAN_POINT ( 'NONE',  ( -2.229367062499996610, -58.39583333196773651, 3.861377020970582219 ) ) ;
#22490 = CARTESIAN_POINT ( 'NONE',  ( -1.339745962155610925, -23.79465819873851729, 5.000000000000000000 ) ) ;
#22491 = CARTESIAN_POINT ( 'NONE',  ( 2.730187237215162345E-16, -141.1875000013656063, -4.458734124999999437 ) ) ;
#22492 = CARTESIAN_POINT ( 'NONE',  ( -2.229367062500000163, -100.7291666653010651, -3.861377020970580443 ) ) ;
#22493 = CARTESIAN_POINT ( 'NONE',  ( -6.972266317189433020E-16, 10.75000000000000000, -5.000000000000000000 ) ) ;
#22494 = ORIENTED_EDGE ( 'NONE', *, *, #54891, .F. ) ;
#22495 = CARTESIAN_POINT ( 'NONE',  ( -52.80376928212989185, -153.1250000013656063, -4.297418129356378458 ) ) ;
#22496 = CARTESIAN_POINT ( 'NONE',  ( -59.98410592259440222, -143.2500000027312126, -0.3983568153799752487 ) ) ;
#22497 = CARTESIAN_POINT ( 'NONE',  ( 2.500000000000002220, -60.66666666666665719, 4.330127018922192761 ) ) ;
#22498 = CARTESIAN_POINT ( 'NONE',  ( -2.229367062500000163, -8.479166665301073991, -3.861377020970580443 ) ) ;
#22499 = CARTESIAN_POINT ( 'NONE',  ( 4.458734124999999437, -95.06249999863440792, -5.460374474430324690E-16 ) ) ;
#22500 = CARTESIAN_POINT ( 'NONE',  ( 4.458734124999999437, -149.7500000013656063, 1.846868145590737864 ) ) ;
#22501 = CARTESIAN_POINT ( 'NONE',  ( 2.229367062500001939, -22.22916666530107221, 3.861377020970579999 ) ) ;
#22502 = CARTESIAN_POINT ( 'NONE',  ( -7.500000000000000000, 1.854554393013821745, -0.1880126015361722192 ) ) ;
#22503 = CARTESIAN_POINT ( 'NONE',  ( -51.60603307380591787, -136.9375000013655779, -2.891590998281053704 ) ) ;
#22504 = CARTESIAN_POINT ( 'NONE',  ( 2.229367062499998831, -63.89583333196772941, -3.861377020970580887 ) ) ;
#22505 = CARTESIAN_POINT ( 'NONE',  ( 7.922281120364393914, 4.573931137438269623, -8.047472243342930653 ) ) ;
#22506 = CARTESIAN_POINT ( 'NONE',  ( -2.500000000000000444, -43.04166666393548013, -4.330127018922193649 ) ) ;
#22507 = CARTESIAN_POINT ( 'NONE',  ( 4.458734124999999437, -146.4375000013656063, 0.000000000000000000 ) ) ;
#22508 = VECTOR ( 'NONE', #34451, 1000.000000000000000 ) ;
#22509 = CARTESIAN_POINT ( 'NONE',  ( -2.229367062499996610, 9.604166668032261711, 3.861377020970582219 ) ) ;
#22510 = ORIENTED_EDGE ( 'NONE', *, *, #47211, .T. ) ;
#22511 = CARTESIAN_POINT ( 'NONE',  ( -4.999999999999998224, -80.91666666666667140, 2.886751345948131764 ) ) ;
#22512 = CARTESIAN_POINT ( 'NONE',  ( -6.972266317189433020E-16, -61.25000000000000000, -5.000000000000000000 ) ) ;
#22514 = CARTESIAN_POINT ( 'NONE',  ( -3.152548672688508926E-16, -23.56249999863440436, -5.148502694627439702 ) ) ;
#22513 = CARTESIAN_POINT ( 'NONE',  ( -5.000000000000000000, -93.08333333333331439, -2.886751345948128211 ) ) ;
#22515 = CARTESIAN_POINT ( 'NONE',  ( 0.000000000000000000, -170.0000000000000000, 0.000000000000000000 ) ) ;
#22516 = CARTESIAN_POINT ( 'NONE',  ( 2.229367062500001939, -70.22916666530107932, 3.861377020970579999 ) ) ;
#22517 = CIRCLE ( 'NONE', #32789, 5.000000000000000888 ) ;
#22518 = CARTESIAN_POINT ( 'NONE',  ( -2.229367062499996610, 27.60416666803225993, 3.861377020970582219 ) ) ;
#22519 = LINE ( 'NONE', #46958, #42744 ) ;
#22520 =( BOUNDED_CURVE ( )  B_SPLINE_CURVE ( 2, ( #48743, #4686, #38776, #4379, #29430, #28505, #58414, #63562, #38172 ),
 .UNSPECIFIED., .F., .F. ) 
 B_SPLINE_CURVE_WITH_KNOTS ( ( 3, 2, 2, 2, 3 ),
 ( 0.4696428571428571397, 0.4702380952380952328, 0.4714285714285714191, 0.4726190476190476053, 0.4732142857142856984 ),
 .UNSPECIFIED. ) 
 CURVE ( )  GEOMETRIC_REPRESENTATION_ITEM ( )  RATIONAL_B_SPLINE_CURVE ( ( 0.9330127018922194093, 0.9330127018922194093, 1.000000000000000000, 0.8660254037844387076, 1.000000000000000000, 0.8660254037844387076, 1.000000000000000000, 0.9330127018922194093, 0.9330127018922194093 ) ) 
 REPRESENTATION_ITEM ( '' )  );
#22521 = CARTESIAN_POINT ( 'NONE',  ( -55.35523342533222291, -146.3125000013656063, 4.444560631937231499 ) ) ;
#22522 = CARTESIAN_POINT ( 'NONE',  ( 2.229367062500001939, 6.020833334698927786, 3.861377020970579999 ) ) ;
#22523 = CARTESIAN_POINT ( 'NONE',  ( -5.000000000000000000, -62.87499999726880873, 0.000000000000000000 ) ) ;
#22524 = CARTESIAN_POINT ( 'NONE',  ( 6.123233995736766282E-16, -170.0000000000000000, -5.000000000000000000 ) ) ;
#22525 = CARTESIAN_POINT ( 'NONE',  ( 2.229367062500001939, 8.020833334698926009, 3.861377020970579999 ) ) ;
#22526 = CARTESIAN_POINT ( 'NONE',  ( 4.458734124999999437, -70.81249999863439371, -5.460374474430324690E-16 ) ) ;
#22527 = CARTESIAN_POINT ( 'NONE',  ( -4.458734124999999437, -20.64583333196774007, -2.574251347313719407 ) ) ;
#22528 = CARTESIAN_POINT ( 'NONE',  ( 1.060575238724906964E-15, 0.2500000000000002220, 5.773502691896257311 ) ) ;
#22529 = CARTESIAN_POINT ( 'NONE',  ( 3.152801135295366208, -158.5625000013656063, 3.152801135295367985 ) ) ;
#22530 = CARTESIAN_POINT ( 'NONE',  ( -5.000000000000000000, 29.12500000273118417, 0.000000000000000000 ) ) ;
#22531 = CARTESIAN_POINT ( 'NONE',  ( -2.229367062500000163, -66.47916666530106511, -3.861377020970580443 ) ) ;
#22532 = CARTESIAN_POINT ( 'NONE',  ( 5.000000000000000000, -102.3749999972688158, -6.123233995736766282E-16 ) ) ;
#22533 =( BOUNDED_CURVE ( )  B_SPLINE_CURVE ( 2, ( #55973, #31193, #49539, #20277, #55659, #29912, #25095, #59523, #1956 ),
 .UNSPECIFIED., .F., .F. ) 
 B_SPLINE_CURVE_WITH_KNOTS ( ( 3, 2, 2, 2, 3 ),
 ( 0.6160714285714286031, 0.6166666666666666963, 0.6178571428571428825, 0.6190476190476190688, 0.6196428571428571619 ),
 .UNSPECIFIED. ) 
 CURVE ( )  GEOMETRIC_REPRESENTATION_ITEM ( )  RATIONAL_B_SPLINE_CURVE ( ( 0.9330127018922194093, 0.9330127018922194093, 1.000000000000000000, 0.8660254037844387076, 1.000000000000000000, 0.8660254037844387076, 1.000000000000000000, 0.9330127018922194093, 0.9330127018922194093 ) ) 
 REPRESENTATION_ITEM ( '' )  );
#22534 = CARTESIAN_POINT ( 'NONE',  ( -6.972266317189433020E-16, -41.24999999999998579, -5.000000000000000000 ) ) ;
#22535 = CARTESIAN_POINT ( 'NONE',  ( -4.458734124999999437, -38.39583333196773651, -2.574251347313719407 ) ) ;
#22536 = EDGE_CURVE ( 'NONE', #7188, #54337, #26164, .T. ) ;
#22537 = CARTESIAN_POINT ( 'NONE',  ( 2.229367062500001939, -104.2291666653010651, 3.861377020970579999 ) ) ;
#22538 = CARTESIAN_POINT ( 'NONE',  ( 9.457646018065525792E-16, -65.31249999863440792, 5.148502694627439702 ) ) ;
#22539 = CARTESIAN_POINT ( 'NONE',  ( -2.499999999999996447, -47.83333333333332149, 4.330127018922195425 ) ) ;
#22540 = CARTESIAN_POINT ( 'NONE',  ( -5.000000000000000000, -23.08333333333333215, -2.886751345948128211 ) ) ;
#22541 = CARTESIAN_POINT ( 'NONE',  ( 3.535533905932736864, -152.2500000027312126, 3.535533905932738641 ) ) ;
#22542 = ORIENTED_EDGE ( 'NONE', *, *, #6070, .F. ) ;
#22543 = CARTESIAN_POINT ( 'NONE',  ( -1.339745962155613812, -68.08034179853028434, -5.000000000000000000 ) ) ;
#22544 = CARTESIAN_POINT ( 'NONE',  ( 2.499999999999998668, -6.333333333333336590, -4.330127018922193649 ) ) ;
#22545 = CARTESIAN_POINT ( 'NONE',  ( 4.458734124999998549, -72.72916666530107932, -2.574251347313721627 ) ) ;
#22546 = CARTESIAN_POINT ( 'NONE',  ( -5.000000000000000000, -6.083333333333336590, -2.886751345948128211 ) ) ;
#22547 = CARTESIAN_POINT ( 'NONE',  ( -5.000000000000000000, -14.95833333060214265, -2.886751345948128211 ) ) ;
#22549 = ORIENTED_EDGE ( 'NONE', *, *, #45248, .F. ) ;
#22548 = CARTESIAN_POINT ( 'NONE',  ( -4.458734124999999437, -47.31249999863440792, 0.000000000000000000 ) ) ;
#22550 = CARTESIAN_POINT ( 'NONE',  ( -5.000000000000000000, 30.00000000000000000, 0.000000000000000000 ) ) ;
#22552 = ORIENTED_EDGE ( 'NONE', *, *, #40483, .F. ) ;
#22551 = CARTESIAN_POINT ( 'NONE',  ( 4.458734124999998549, 5.020833334698926897, -2.574251347313721627 ) ) ;
#22553 = CARTESIAN_POINT ( 'NONE',  ( 5.000000000000000888, -34.45833333060213732, 2.886751345948126879 ) ) ;
#22554 = CARTESIAN_POINT ( 'NONE',  ( -2.500000000000000444, -58.16666666666665719, -4.330127018922193649 ) ) ;
#22555 = ADVANCED_FACE ( 'NONE', ( #36137 ), #54485, .T. ) ;
#22556 = CARTESIAN_POINT ( 'NONE',  ( -4.458734125000001214, -161.1250000013656063, 1.846868145590734089 ) ) ;
#22557 = CARTESIAN_POINT ( 'NONE',  ( 4.458734125000001214, -37.14583333196773651, 2.574251347313718519 ) ) ;
#22558 = MECHANICAL_DESIGN_GEOMETRIC_PRESENTATION_REPRESENTATION (  '', ( #14305 ), #9169 ) ;
#22559 = CARTESIAN_POINT ( 'NONE',  ( 1.975475456537005874E-15, -82.74999999999998579, 5.000000000000000000 ) ) ;
#22560 = CARTESIAN_POINT ( 'NONE',  ( 4.458734124999999437, -78.81249999863440792, -5.460374474430324690E-16 ) ) ;
#22561 = CARTESIAN_POINT ( 'NONE',  ( -9.184850993605147944E-16, -167.2500000000000000, 5.000000000000000000 ) ) ;
#22562 = EDGE_CURVE ( 'NONE', #16286, #38301, #25206, .T. ) ;
#22563 = CARTESIAN_POINT ( 'NONE',  ( 2.229367062499998831, -89.64583333196773651, -3.861377020970580887 ) ) ;
#22564 = VECTOR ( 'NONE', #14431, 1000.000000000000000 ) ;
#22565 = CARTESIAN_POINT ( 'NONE',  ( -59.29741812935640155, -131.8750000013656347, -2.196230717870135685 ) ) ;
#22566 = CARTESIAN_POINT ( 'NONE',  ( 2.229367062499998831, -1.895833331967737623, -3.861377020970580887 ) ) ;
#22567 = CARTESIAN_POINT ( 'NONE',  ( 4.458734125000001214, -40.14583333196772941, 2.574251347313718519 ) ) ;
#22568 = EDGE_CURVE ( 'NONE', #5292, #48949, #49930, .T. ) ;
#22569 = CARTESIAN_POINT ( 'NONE',  ( -5.000000000000000000, -93.95833333060213022, -2.886751345948128211 ) ) ;
#22570 = CARTESIAN_POINT ( 'NONE',  ( -4.458734124999999437, -81.64583333196773651, -2.574251347313719407 ) ) ;
#22571 = CARTESIAN_POINT ( 'NONE',  ( 1.339745962155615144, -84.70534180126146850, 4.999999999999999112 ) ) ;
#22572 = ORIENTED_EDGE ( 'NONE', *, *, #59503, .T. ) ;
#22573 = CARTESIAN_POINT ( 'NONE',  ( 3.061616997868383141E-16, -148.8750000027312126, -5.000000000000000000 ) ) ;
#22574 = DIRECTION ( 'NONE',  ( 0.000000000000000000, 0.000000000000000000, 1.000000000000000000 ) ) ;
#22575 = CARTESIAN_POINT ( 'NONE',  ( -4.458734124999998549, -70.47916666530107932, 2.574251347313722516 ) ) ;
#22576 = CARTESIAN_POINT ( 'NONE',  ( 4.458734124999998549, -40.72916666530107221, -2.574251347313721627 ) ) ;
#22577 = CARTESIAN_POINT ( 'NONE',  ( -4.458734124999999437, -9.562499998634406140, 0.000000000000000000 ) ) ;
#22578 = ORIENTED_EDGE ( 'NONE', *, *, #62482, .F. ) ;
#22579 = FACE_OUTER_BOUND ( 'NONE', #10817, .T. ) ;
#22580 = CARTESIAN_POINT ( 'NONE',  ( -2.499999999999996447, -1.833333333333332593, 4.330127018922195425 ) ) ;
#22581 = CARTESIAN_POINT ( 'NONE',  ( 2.229367062500001939, -5.229166665301071326, 3.861377020970579999 ) ) ;
#22582 = CARTESIAN_POINT ( 'NONE',  ( -1.339745962155613812, 2.794658198738520394, -5.000000000000000000 ) ) ;
#22583 = CARTESIAN_POINT ( 'NONE',  ( -3.152548672688508926E-16, 2.437500001365594304, -5.148502694627439702 ) ) ;
#22584 = DIRECTION ( 'NONE',  ( -0.000000000000000000, 1.000000000000000000, -0.000000000000000000 ) ) ;
#22585 = CARTESIAN_POINT ( 'NONE',  ( -1.846868145590737420, -158.7500000013656063, 4.458734124999997661 ) ) ;
#22586 =( BOUNDED_CURVE ( )  B_SPLINE_CURVE ( 2, ( #59041, #59363, #14971, #54212, #3985, #19710, #38686, #19067, #53492 ),
 .UNSPECIFIED., .F., .F. ) 
 B_SPLINE_CURVE_WITH_KNOTS ( ( 3, 2, 2, 2, 3 ),
 ( 0.4020833333333333481, 0.4027777777777777901, 0.4041666666666666741, 0.4055555555555555580, 0.4062500000000000000 ),
 .UNSPECIFIED. ) 
 CURVE ( )  GEOMETRIC_REPRESENTATION_ITEM ( )  RATIONAL_B_SPLINE_CURVE ( ( 0.9330127018922194093, 0.9330127018922194093, 1.000000000000000000, 0.8660254037844387076, 1.000000000000000000, 0.8660254037844387076, 1.000000000000000000, 0.9330127018922194093, 0.9330127018922194093 ) ) 
 REPRESENTATION_ITEM ( '' )  );
#22587 = CARTESIAN_POINT ( 'NONE',  ( 9.457646018065525792E-16, 26.68750000136559564, 5.148502694627439702 ) ) ;
#22588 = VERTEX_POINT ( 'NONE', #41574 ) ;
#22589 = CARTESIAN_POINT ( 'NONE',  ( -2.229367062500000163, -88.47916666530106511, -3.861377020970580443 ) ) ;
#22590 = CARTESIAN_POINT ( 'NONE',  ( -6.972266317189433020E-16, -78.24999999999998579, -5.000000000000000000 ) ) ;
#22591 = CARTESIAN_POINT ( 'NONE',  ( -3.152548672688508926E-16, -9.562499998634406140, -5.148502694627439702 ) ) ;
#22592 = CARTESIAN_POINT ( 'NONE',  ( -1.339745962155613812, 19.79465819873851729, -5.000000000000000000 ) ) ;
#22593 = CARTESIAN_POINT ( 'NONE',  ( -9.184850993605147944E-16, -142.3750000027312126, 5.000000000000000000 ) ) ;
#22594 = CARTESIAN_POINT ( 'NONE',  ( 5.000000000000000888, -67.58333333333332860, 2.886751345948126879 ) ) ;
#22595 = CARTESIAN_POINT ( 'NONE',  ( -5.000000000000000000, -35.95833333060213732, -2.886751345948128211 ) ) ;
#22596 = CARTESIAN_POINT ( 'NONE',  ( -6.972266317189433020E-16, 5.875000002731185056, -5.000000000000000000 ) ) ;
#22597 = CARTESIAN_POINT ( 'NONE',  ( 4.458734125000000326, 27.10416666803225993, 2.574251347313718519 ) ) ;
#22598 = CARTESIAN_POINT ( 'NONE',  ( -5.000000000000000000, -97.87499999726881583, 0.000000000000000000 ) ) ;
#22599 = CARTESIAN_POINT ( 'NONE',  ( 4.458734124999999437, 21.18750000136559208, -5.460374474430324690E-16 ) ) ;
#22600 = CARTESIAN_POINT ( 'NONE',  ( 9.457646018065525792E-16, -57.06249999863440081, 5.148502694627439702 ) ) ;
#22601 = CARTESIAN_POINT ( 'NONE',  ( -2.229367062500000163, -1.729166665301071992, -3.861377020970580443 ) ) ;
#22602 = AXIS2_PLACEMENT_3D ( 'NONE', #53319, #4737, #28867 ) ;
#22603 = CARTESIAN_POINT ( 'NONE',  ( -3.535250795749689387E-16, 14.75000000000000000, -5.773502691896257311 ) ) ;
#22604 = CARTESIAN_POINT ( 'NONE',  ( 3.535533905932736864, -140.2500000027311842, 3.535533905932738641 ) ) ;
#22605 = CARTESIAN_POINT ( 'NONE',  ( 2.499999999999998668, -75.20833333060214443, -4.330127018922193649 ) ) ;
#22606 = CIRCLE ( 'NONE', #30808, 7.500000000000001776 ) ;
#22607 = CARTESIAN_POINT ( 'NONE',  ( 4.458734125000001214, -49.89583333196772941, 2.574251347313718519 ) ) ;
#22608 = CARTESIAN_POINT ( 'NONE',  ( -4.999999999999999112, -84.79166666393547303, 2.886751345948131764 ) ) ;
#22609 = CARTESIAN_POINT ( 'NONE',  ( -50.40829686548195099, -136.2500000013656063, -1.485763867205728284 ) ) ;
#22610 = CARTESIAN_POINT ( 'NONE',  ( 5.000000000000000888, -37.45833333060213732, 2.886751345948126879 ) ) ;
#22611 = CARTESIAN_POINT ( 'NONE',  ( -5.000000000000000000, -63.95833333060213732, -2.886751345948128211 ) ) ;
#22612 = CARTESIAN_POINT ( 'NONE',  ( -2.229367062500000163, -86.72916666530107932, -3.861377020970580443 ) ) ;
#22613 = CARTESIAN_POINT ( 'NONE',  ( -1.846868145590734756, -158.3750000013655779, -4.458734124999999437 ) ) ;
#22614 = CARTESIAN_POINT ( 'NONE',  ( 5.000000000000000000, -34.41666666666666430, -2.886751345948129988 ) ) ;
#22615 = CARTESIAN_POINT ( 'NONE',  ( 2.500000000000002220, 8.458333336064518093, 4.330127018922192761 ) ) ;
#22616 = EDGE_LOOP ( 'NONE', ( #570, #21291, #56738, #49647 ) ) ;
#22617 = CARTESIAN_POINT ( 'NONE',  ( -2.229367062499996610, 19.60416666803225993, 3.861377020970582219 ) ) ;
#22618 = EDGE_LOOP ( 'NONE', ( #18714, #40485, #33806, #59419 ) ) ;
#22619 = CARTESIAN_POINT ( 'NONE',  ( -2.229367062500000163, -95.47916666530107932, -3.861377020970580443 ) ) ;
#22620 = CARTESIAN_POINT ( 'NONE',  ( 4.458734125000001214, 14.85416666803225993, 2.574251347313718519 ) ) ;
#22621 = CARTESIAN_POINT ( 'NONE',  ( -3.535250795749689387E-16, 17.87500000273118417, -5.773502691896257311 ) ) ;
#22622 = CARTESIAN_POINT ( 'NONE',  ( -58.24261429053147765, -155.0000000000000284, -3.805975901505573411 ) ) ;
#22623 = CARTESIAN_POINT ( 'NONE',  ( 5.000000000000000888, 6.416666666666666963, 2.886751345948126879 ) ) ;
#22624 = CARTESIAN_POINT ( 'NONE',  ( 2.229367062499998831, -54.64583333196773651, -3.861377020970580887 ) ) ;
#22625 = CARTESIAN_POINT ( 'NONE',  ( -6.972266317189433020E-16, 14.87500000273118594, -5.000000000000000000 ) ) ;
#22626 = CARTESIAN_POINT ( 'NONE',  ( -2.500000000000000444, -82.16666666666667140, -4.330127018922193649 ) ) ;
#22627 = CARTESIAN_POINT ( 'NONE',  ( 0.000000000000000000, -170.0000000000000000, 0.000000000000000000 ) ) ;
#22628 = CARTESIAN_POINT ( 'NONE',  ( -9.184850993605147944E-16, -153.3750000027311842, 5.000000000000000000 ) ) ;
#22629 = DIRECTION ( 'NONE',  ( 0.000000000000000000, 0.000000000000000000, 1.000000000000000000 ) ) ;
#22630 = CARTESIAN_POINT ( 'NONE',  ( -5.000000000000000000, -37.08333333333332860, -2.886751345948128211 ) ) ;
#22631 = CARTESIAN_POINT ( 'NONE',  ( -2.500000000000000444, 12.95833333606451809, -4.330127018922193649 ) ) ;
#22633 = CARTESIAN_POINT ( 'NONE',  ( -4.458734124999999437, -21.56249999863440436, 0.000000000000000000 ) ) ;
#22632 = CARTESIAN_POINT ( 'NONE',  ( -5.000000000000000000, -43.08333333333333570, -2.886751345948128211 ) ) ;
#22634 = CARTESIAN_POINT ( 'NONE',  ( -5.000000000000000888, -143.4375000000000284, 2.071067811865474617 ) ) ;
#22635 = CARTESIAN_POINT ( 'NONE',  ( 2.229367062500001939, -62.97916666530106511, 3.861377020970579999 ) ) ;
#22636 =( BOUNDED_CURVE ( )  B_SPLINE_CURVE ( 2, ( #34483, #19707, #14874, #20026, #43509, #53180, #54117, #33558, #9113 ),
 .UNSPECIFIED., .F., .F. ) 
 B_SPLINE_CURVE_WITH_KNOTS ( ( 3, 2, 2, 2, 3 ),
 ( 0.5770833333333332815, 0.5777777777777777235, 0.5791666666666667185, 0.5805555555555556024, 0.5812500000000000444 ),
 .UNSPECIFIED. ) 
 CURVE ( )  GEOMETRIC_REPRESENTATION_ITEM ( )  RATIONAL_B_SPLINE_CURVE ( ( 0.9330127018922194093, 0.9330127018922194093, 1.000000000000000000, 0.8660254037844387076, 1.000000000000000000, 0.8660254037844387076, 1.000000000000000000, 0.9330127018922194093, 0.9330127018922194093 ) ) 
 REPRESENTATION_ITEM ( '' )  );
#22637 = CARTESIAN_POINT ( 'NONE',  ( 4.458734124999999437, -146.6875000013656063, 0.000000000000000000 ) ) ;
#22638 = CARTESIAN_POINT ( 'NONE',  ( 4.458734124999998549, -71.72916666530107932, -2.574251347313721627 ) ) ;
#22639 = CARTESIAN_POINT ( 'NONE',  ( -59.59170313451811296, -142.7500000013656063, 1.485763867205729394 ) ) ;
#22640 = CARTESIAN_POINT ( 'NONE',  ( -4.458734124999999437, -18.64583333196774007, -2.574251347313719407 ) ) ;
#22641 = CARTESIAN_POINT ( 'NONE',  ( -5.000000000000000000, -62.87499999726880873, 0.000000000000000000 ) ) ;
#22642 = ORIENTED_EDGE ( 'NONE', *, *, #56295, .F. ) ;
#22643 = CARTESIAN_POINT ( 'NONE',  ( -3.535533905932738641, -150.3750000000000000, 3.535533905932737309 ) ) ;
#22644 = ORIENTED_EDGE ( 'NONE', *, *, #26730, .T. ) ;
#22645 = CARTESIAN_POINT ( 'NONE',  ( -4.458734124999998549, -68.47916666530106511, 2.574251347313722516 ) ) ;
#22646 = CARTESIAN_POINT ( 'NONE',  ( 2.499999999999998668, -21.20833333060214798, -4.330127018922193649 ) ) ;
#22647 = CARTESIAN_POINT ( 'NONE',  ( -4.769696007084728073, -120.0000000000000000, 1.499999999999999556 ) ) ;
#22648 = ORIENTED_EDGE ( 'NONE', *, *, #48778, .T. ) ;
#22649 = VECTOR ( 'NONE', #63316, 1000.000000000000000 ) ;
#22650 = LINE ( 'NONE', #17506, #19045 ) ;
#22651 = CARTESIAN_POINT ( 'NONE',  ( -59.81910112700025905, -127.1875000000000426, -2.462841084822630311 ) ) ;
#22653 = VECTOR ( 'NONE', #27106, 1000.000000000000000 ) ;
#22652 = CARTESIAN_POINT ( 'NONE',  ( 5.000000000000000000, -8.500000000000000000, -6.123233995736766282E-16 ) ) ;
#22654 = CARTESIAN_POINT ( 'NONE',  ( -3.152548672688508926E-16, -51.81249999863440792, -5.148502694627439702 ) ) ;
#22655 = ORIENTED_EDGE ( 'NONE', *, *, #56976, .T. ) ;
#22656 = CARTESIAN_POINT ( 'NONE',  ( -5.000000000000000000, 2.041666669397854239, -2.886751345948128211 ) ) ;
#22657 = CARTESIAN_POINT ( 'NONE',  ( 4.458734124999998549, 10.27083333469892779, -2.574251347313721627 ) ) ;
#22658 = CARTESIAN_POINT ( 'NONE',  ( 9.457646018065525792E-16, 18.93750000136559208, 5.148502694627439702 ) ) ;
#22659 = CARTESIAN_POINT ( 'NONE',  ( -59.44456063193725015, -148.5625000013656063, -0.3552334253322034230 ) ) ;
#22660 = CARTESIAN_POINT ( 'NONE',  ( -6.972266317189433020E-16, -1.124999997268814278, -5.000000000000000000 ) ) ;
#22661 = CARTESIAN_POINT ( 'NONE',  ( 2.071067811865412445, -164.8125000000000284, -5.000000000000063949 ) ) ;
#22662 = VERTEX_POINT ( 'NONE', #61544 ) ;
#22663 = CARTESIAN_POINT ( 'NONE',  ( -2.229367062500000163, -71.47916666530107932, -3.861377020970580443 ) ) ;
#22664 = CARTESIAN_POINT ( 'NONE',  ( -5.000000000000000000, -39.99999999999999289, 0.000000000000000000 ) ) ;
#22665 = CARTESIAN_POINT ( 'NONE',  ( -4.458734124999998549, 6.770833334698928674, 2.574251347313722516 ) ) ;
#22666 = CARTESIAN_POINT ( 'NONE',  ( -4.999999999999998224, -41.91666666666667140, 2.886751345948131764 ) ) ;
#22667 = CARTESIAN_POINT ( 'NONE',  ( -4.458734124999999437, -60.56249999863440081, 0.000000000000000000 ) ) ;
#22668 = CARTESIAN_POINT ( 'NONE',  ( -5.000000000000000000, -20.87499999726881228, 0.000000000000000000 ) ) ;
#22669 = CARTESIAN_POINT ( 'NONE',  ( -1.339745962155610925, -18.79465819873852084, 5.000000000000000000 ) ) ;
#22670 = DIRECTION ( 'NONE',  ( -0.000000000000000000, 1.000000000000000000, -0.000000000000000000 ) ) ;
#22671 = CARTESIAN_POINT ( 'NONE',  ( 0.000000000000000000, -170.0000000000000000, 5.000000000000000000 ) ) ;
#22672 = LINE ( 'NONE', #12690, #12114 ) ;
#22673 = CARTESIAN_POINT ( 'NONE',  ( 2.229367062500001939, -41.97916666530107932, 3.861377020970579999 ) ) ;
#22674 = CARTESIAN_POINT ( 'NONE',  ( 9.457646018065525792E-16, -20.31249999863439726, 5.148502694627439702 ) ) ;
#22675 = ORIENTED_EDGE ( 'NONE', *, *, #63400, .T. ) ;
#22676 = CARTESIAN_POINT ( 'NONE',  ( 0.000000000000000000, -170.0000000000000000, 0.000000000000000000 ) ) ;
#22677 = CARTESIAN_POINT ( 'NONE',  ( -4.458734124999998549, -110.2291666653010651, 2.574251347313722516 ) ) ;
#22678 = CARTESIAN_POINT ( 'NONE',  ( -2.071067811865475061, -154.8125000027312126, -5.000000000000000888 ) ) ;
#22679 = ORIENTED_EDGE ( 'NONE', *, *, #47661, .T. ) ;
#22680 = CARTESIAN_POINT ( 'NONE',  ( 4.458734124999998549, -108.9791666653010651, -2.574251347313721627 ) ) ;
#22681 = CARTESIAN_POINT ( 'NONE',  ( -4.458734124999999437, -30.39583333196773651, -2.574251347313719407 ) ) ;
#22682 = CARTESIAN_POINT ( 'NONE',  ( -4.999999999999999112, -60.79166666393547303, 2.886751345948131764 ) ) ;
#22683 = CARTESIAN_POINT ( 'NONE',  ( -51.60603307380591787, -150.1875000013656063, -2.891590998281053704 ) ) ;
#22684 = CARTESIAN_POINT ( 'NONE',  ( -2.071067811865478170, -145.3125000000000000, 5.000000000000000000 ) ) ;
#22685 = CARTESIAN_POINT ( 'NONE',  ( 2.229367062500001939, -30.97916666530107221, 3.861377020970579999 ) ) ;
#22686 = CARTESIAN_POINT ( 'NONE',  ( 4.458734124999999437, -68.06249999863440792, -5.460374474430324690E-16 ) ) ;
#22687 = CARTESIAN_POINT ( 'NONE',  ( 1.339745962155609149, 22.41965820146970501, 5.000000000000003553 ) ) ;
#22688 = CARTESIAN_POINT ( 'NONE',  ( 4.458734124999999437, -25.81249999863440792, -5.460374474430324690E-16 ) ) ;
#22689 = CARTESIAN_POINT ( 'NONE',  ( 5.000000000000000888, -146.9375000000000000, -2.071067811865475505 ) ) ;
#22690 = DIRECTION ( 'NONE',  ( -0.000000000000000000, -1.000000000000000000, -0.000000000000000000 ) ) ;
#22691 = CARTESIAN_POINT ( 'NONE',  ( -5.000000000000000000, -19.08333333333333570, -2.886751345948128211 ) ) ;
#22692 = CARTESIAN_POINT ( 'NONE',  ( 4.458734125000000326, -147.3750000013656063, -1.846868145590734978 ) ) ;
#22693 = VERTEX_POINT ( 'NONE', #51568 ) ;
#22694 = AXIS2_PLACEMENT_3D ( 'NONE', #62941, #14350, #33972 ) ;
#22695 = CARTESIAN_POINT ( 'NONE',  ( -53.33387254593731086, -152.8125000000000284, 5.149110718188520508 ) ) ;
#22696 = CARTESIAN_POINT ( 'NONE',  ( 4.458734124999998549, -53.97916666530107221, -2.574251347313721627 ) ) ;
#22697 = EDGE_CURVE ( 'NONE', #52288, #18740, #3629, .T. ) ;
#22698 = CARTESIAN_POINT ( 'NONE',  ( -6.972266317189433020E-16, -87.12499999726880162, -5.000000000000000000 ) ) ;
#22699 = CARTESIAN_POINT ( 'NONE',  ( 0.000000000000000000, -170.0000000000000000, 0.000000000000000000 ) ) ;
#22700 = CARTESIAN_POINT ( 'NONE',  ( 2.499999999999998668, 22.66666666666666430, -4.330127018922193649 ) ) ;
#22701 = VECTOR ( 'NONE', #48065, 1000.000000000000000 ) ;
#22702 = CARTESIAN_POINT ( 'NONE',  ( 1.339745962155615144, -17.58034179853029499, 4.999999999999999112 ) ) ;
#22703 = CARTESIAN_POINT ( 'NONE',  ( 4.458734125000001214, -2.895833331967738289, 2.574251347313718519 ) ) ;
#22704 = CARTESIAN_POINT ( 'NONE',  ( 5.000000000000000000, 28.58333333333333215, -2.886751345948130876 ) ) ;
#22705 = DIRECTION ( 'NONE',  ( -0.000000000000000000, 1.000000000000000000, -0.000000000000000000 ) ) ;
#22706 = CARTESIAN_POINT ( 'NONE',  ( -2.229367062499996610, 7.604166668032260823, 3.861377020970582219 ) ) ;
#22707 = ORIENTED_EDGE ( 'NONE', *, *, #25848, .T. ) ;
#22708 = CARTESIAN_POINT ( 'NONE',  ( 2.499999999999998668, -42.33333333333333570, -4.330127018922193649 ) ) ;
#22709 = ORIENTED_EDGE ( 'NONE', *, *, #56962, .F. ) ;
#22710 = CARTESIAN_POINT ( 'NONE',  ( -5.000000000000000000, -23.95833333060214443, -2.886751345948128211 ) ) ;
#22711 = CARTESIAN_POINT ( 'NONE',  ( -4.458734124999999437, -47.39583333196774362, -2.574251347313719407 ) ) ;
#22712 = CARTESIAN_POINT ( 'NONE',  ( 3.152801135295366208, -158.8125000013656063, 3.152801135295367985 ) ) ;
#22713 =( BOUNDED_CURVE ( )  B_SPLINE_CURVE ( 2, ( #24767, #14785, #5783, #29577, #45343, #35063, #44371, #34734, #25403 ),
 .UNSPECIFIED., .F., .F. ) 
 B_SPLINE_CURVE_WITH_KNOTS ( ( 3, 2, 2, 2, 3 ),
 ( 0.7645833333333332815, 0.7652777777777777235, 0.7666666666666667185, 0.7680555555555556024, 0.7687500000000000444 ),
 .UNSPECIFIED. ) 
 CURVE ( )  GEOMETRIC_REPRESENTATION_ITEM ( )  RATIONAL_B_SPLINE_CURVE ( ( 0.9330127018922194093, 0.9330127018922194093, 1.000000000000000000, 0.8660254037844387076, 1.000000000000000000, 0.8660254037844387076, 1.000000000000000000, 0.9330127018922194093, 0.9330127018922194093 ) ) 
 REPRESENTATION_ITEM ( '' )  );
#22714 = CARTESIAN_POINT ( 'NONE',  ( 1.060575238724906964E-15, -43.62499999726880873, 5.773502691896257311 ) ) ;
#22715 = VERTEX_POINT ( 'NONE', #56077 ) ;
#22716 = CARTESIAN_POINT ( 'NONE',  ( -2.229367062499996610, -21.14583333196774007, 3.861377020970582219 ) ) ;
#22717 = EDGE_LOOP ( 'NONE', ( #61787, #11042, #61191, #47903 ) ) ;
#22718 = CARTESIAN_POINT ( 'NONE',  ( 1.975475456537005874E-15, -13.62499999726881228, 5.000000000000000000 ) ) ;
#22719 = CARTESIAN_POINT ( 'NONE',  ( -8.190561711645485556E-16, -164.6875000013655779, 4.458734124999999437 ) ) ;
#22720 = CARTESIAN_POINT ( 'NONE',  ( -6.972266317189433020E-16, -72.12499999726878741, -5.000000000000000000 ) ) ;
#22721 = CARTESIAN_POINT ( 'NONE',  ( -50.18089887299979068, -137.6875000000000000, 2.462841084822635640 ) ) ;
#22722 = CARTESIAN_POINT ( 'NONE',  ( 9.457646018065525792E-16, -36.31249999863440792, 5.148502694627439702 ) ) ;
#22723 = CARTESIAN_POINT ( 'NONE',  ( 1.975475456537005874E-15, 23.37500000273118417, 5.000000000000000000 ) ) ;
#22724 = ORIENTED_EDGE ( 'NONE', *, *, #53156, .F. ) ;
#22725 = CARTESIAN_POINT ( 'NONE',  ( -4.458734124999999437, -82.31249999863440792, 0.000000000000000000 ) ) ;
#22726 = CARTESIAN_POINT ( 'NONE',  ( 2.229367062500001939, 26.02083333469892779, 3.861377020970579999 ) ) ;
#22727 = CARTESIAN_POINT ( 'NONE',  ( 3.061616997868383141E-16, -155.7500000000000000, -5.000000000000000000 ) ) ;
#22728 = ORIENTED_EDGE ( 'NONE', *, *, #58256, .T. ) ;
#22729 = CARTESIAN_POINT ( 'NONE',  ( -2.499999999999996447, -22.70833333060214443, 4.330127018922195425 ) ) ;
#22730 = CARTESIAN_POINT ( 'NONE',  ( -50.40829686548195099, -140.2500000013656063, -1.485763867205728284 ) ) ;
#22731 = CARTESIAN_POINT ( 'NONE',  ( -2.229367062499996610, -84.39583333196773651, 3.861377020970582219 ) ) ;
#22732 = CARTESIAN_POINT ( 'NONE',  ( -54.60164318462004474, -130.5000000027312126, -4.984105922594373794 ) ) ;
#22733 = CYLINDRICAL_SURFACE ( 'NONE', #16115, 5.000000000000000000 ) ;
#22734 = DIRECTION ( 'NONE',  ( 1.000000000000000000, 0.000000000000000000, 0.000000000000000000 ) ) ;
#22735 = CARTESIAN_POINT ( 'NONE',  ( 3.535533905932738197, -145.0000000027311842, -3.535533905932738197 ) ) ;
#22736 = CARTESIAN_POINT ( 'NONE',  ( 4.458734124999998549, -52.72916666530107221, -2.574251347313721627 ) ) ;
#22737 = CARTESIAN_POINT ( 'NONE',  ( -1.339745962155610925, -84.66965819600731891, 5.000000000000000000 ) ) ;
#22738 = AXIS2_PLACEMENT_3D ( 'NONE', #46546, #45903, #1865 ) ;
#22739 = CARTESIAN_POINT ( 'NONE',  ( 9.457646018065525792E-16, 20.93750000136558853, 5.148502694627439702 ) ) ;
#22740 = EDGE_CURVE ( 'NONE', #32214, #10009, #51881, .T. ) ;
#22741 = CARTESIAN_POINT ( 'NONE',  ( 5.000000000000000888, -104.5833333333333286, 2.886751345948126879 ) ) ;
#22742 = CARTESIAN_POINT ( 'NONE',  ( 3.535533905932736864, -159.2500000027312126, 3.535533905932738641 ) ) ;
#22743 = CARTESIAN_POINT ( 'NONE',  ( 4.458734124999999437, -46.06249999863440081, -5.460374474430324690E-16 ) ) ;
#22744 = CARTESIAN_POINT ( 'NONE',  ( -5.000000000000000000, -3.874999997268816720, 0.000000000000000000 ) ) ;
#22745 = CARTESIAN_POINT ( 'NONE',  ( -5.000000000000000000, -153.6250000027312126, -6.123233995736766282E-16 ) ) ;
#22746 = CARTESIAN_POINT ( 'NONE',  ( -59.29741812935640155, -124.6250000013656347, -2.196230717870135685 ) ) ;
#22747 = CARTESIAN_POINT ( 'NONE',  ( -2.229367062499996610, -78.39583333196773651, 3.861377020970582219 ) ) ;
#22748 = CARTESIAN_POINT ( 'NONE',  ( 2.229367062500001939, -102.9791666653010651, 3.861377020970579999 ) ) ;
#22749 = CARTESIAN_POINT ( 'NONE',  ( 4.458734125000000326, -6.145833331967740953, 2.574251347313718519 ) ) ;
#22750 = ORIENTED_EDGE ( 'NONE', *, *, #27921, .T. ) ;
#22751 = CARTESIAN_POINT ( 'NONE',  ( 1.975475456537005874E-15, -51.75000000000000711, 5.000000000000000000 ) ) ;
#22752 = CARTESIAN_POINT ( 'NONE',  ( 4.458734124999999437, -95.81249999863440792, -5.460374474430324690E-16 ) ) ;
#22753 = CARTESIAN_POINT ( 'NONE',  ( 5.000000000000000000, -166.1875000027311842, 2.071067811865478614 ) ) ;
#22754 = CARTESIAN_POINT ( 'NONE',  ( -2.229367062499996610, -90.39583333196773651, 3.861377020970582219 ) ) ;
#22755 = CARTESIAN_POINT ( 'NONE',  ( 2.229367062499998831, 10.10416666803225993, -3.861377020970580887 ) ) ;
#22756 = FACE_OUTER_BOUND ( 'NONE', #34708, .T. ) ;
#22757 = CARTESIAN_POINT ( 'NONE',  ( -50.40829686548195099, -133.0000000013656063, -1.485763867205728284 ) ) ;
#22758 = EDGE_CURVE ( 'NONE', #16611, #55752, #42533, .T. ) ;
#22759 = CARTESIAN_POINT ( 'NONE',  ( -2.229367062500000163, -14.47916666530107221, -3.861377020970580443 ) ) ;
#22760 = CARTESIAN_POINT ( 'NONE',  ( -4.458734124999999437, 15.43750000136559386, 0.000000000000000000 ) ) ;
#22761 = EDGE_CURVE ( 'NONE', #29335, #19698, #21591, .T. ) ;
#22762 = CARTESIAN_POINT ( 'NONE',  ( 2.229367062500001939, -53.22916666530107221, 3.861377020970579999 ) ) ;
#22763 =( BOUNDED_CURVE ( )  B_SPLINE_CURVE ( 2, ( #31062, #7591, #51654, #12406, #41028, #50370, #46184, #27199, #11443 ),
 .UNSPECIFIED., .F., .F. ) 
 B_SPLINE_CURVE_WITH_KNOTS ( ( 3, 2, 2, 2, 3 ),
 ( 0.2750000000000002442, 0.2791666666666668961, 0.2833333333333335480, 0.2875000000000001998, 0.2916666666666669072 ),
 .UNSPECIFIED. ) 
 CURVE ( )  GEOMETRIC_REPRESENTATION_ITEM ( )  RATIONAL_B_SPLINE_CURVE ( ( 0.9999999999999958922, 0.9238795325112908463, 1.000000000000000000, 0.9238795325112867385, 1.000000000000000000, 0.9238795325112867385, 1.000000000000000000, 0.9238795325112826307, 1.000000000000003997 ) ) 
 REPRESENTATION_ITEM ( '' )  );
#22764 = CARTESIAN_POINT ( 'NONE',  ( -2.500000000000000444, -69.16666666666667140, -4.330127018922193649 ) ) ;
#22765 = CARTESIAN_POINT ( 'NONE',  ( -4.999999999999998224, -21.79166666393548368, 2.886751345948131764 ) ) ;
#22766 = CARTESIAN_POINT ( 'NONE',  ( 4.458734124999999437, -6.812499998634404363, -5.460374474430324690E-16 ) ) ;
#22767 = ORIENTED_EDGE ( 'NONE', *, *, #13810, .T. ) ;
#22768 = CARTESIAN_POINT ( 'NONE',  ( 4.458734124999998549, -35.97916666530107221, -2.574251347313721627 ) ) ;
#22769 = CARTESIAN_POINT ( 'NONE',  ( -59.44456063193725015, -127.8125000013655921, -0.3552334253322034230 ) ) ;
#22770 = CARTESIAN_POINT ( 'NONE',  ( 6.123233995736766282E-16, -170.0000000000000000, -5.000000000000000000 ) ) ;
#22771 = CARTESIAN_POINT ( 'NONE',  ( 4.458734124999998549, -77.72916666530106511, -2.574251347313721627 ) ) ;
#22772 = CARTESIAN_POINT ( 'NONE',  ( 2.229367062500001939, 22.77083333469892423, 3.861377020970579999 ) ) ;
#22773 = EDGE_CURVE ( 'NONE', #32181, #49141, #56541, .T. ) ;
#22774 = CARTESIAN_POINT ( 'NONE',  ( -4.458734124999999437, 13.68750000136559386, 0.000000000000000000 ) ) ;
#22775 = CARTESIAN_POINT ( 'NONE',  ( 0.000000000000000000, 0.000000000000000000, -10.00000000000000000 ) ) ;
#22776 = CARTESIAN_POINT ( 'NONE',  ( 1.975475456537005874E-15, -87.75000000000001421, 5.000000000000000000 ) ) ;
#22777 = CARTESIAN_POINT ( 'NONE',  ( 9.457646018065525792E-16, -83.31249999863440792, 5.148502694627439702 ) ) ;
#22778 = CARTESIAN_POINT ( 'NONE',  ( -5.000000000000000000, -67.99999999999998579, 0.000000000000000000 ) ) ;
#22779 = CARTESIAN_POINT ( 'NONE',  ( 5.000000000000000000, -72.37499999726880162, -6.123233995736766282E-16 ) ) ;
#22780 = CARTESIAN_POINT ( 'NONE',  ( 1.060575238724906964E-15, 17.37500000273118417, 5.773502691896257311 ) ) ;
#22781 = ORIENTED_EDGE ( 'NONE', *, *, #58534, .F. ) ;
#22782 = CARTESIAN_POINT ( 'NONE',  ( 1.339745962155612702, -18.16965819600733312, -5.000000000000000000 ) ) ;
#22783 = CARTESIAN_POINT ( 'NONE',  ( -59.98410592259440222, -139.2500000027312126, -0.3983568153799752487 ) ) ;
#22785 = CARTESIAN_POINT ( 'NONE',  ( -4.999999999999999112, -27.91666666666666430, 2.886751345948131764 ) ) ;
#22784 = CARTESIAN_POINT ( 'NONE',  ( 1.975475456537005874E-15, -40.74999999999999289, 5.000000000000000000 ) ) ;
#22786 = CARTESIAN_POINT ( 'NONE',  ( -2.229367062500000163, -30.47916666530107221, -3.861377020970580443 ) ) ;
#22787 = VECTOR ( 'NONE', #50335, 1000.000000000000000 ) ;
#22788 = CARTESIAN_POINT ( 'NONE',  ( -6.972266317189433020E-16, -107.1249999972687874, -5.000000000000000000 ) ) ;
#22789 = CARTESIAN_POINT ( 'NONE',  ( 2.500000000000002220, -29.54166666393548013, 4.330127018922192761 ) ) ;
#22790 = EDGE_CURVE ( 'NONE', #11153, #37277, #6383, .T. ) ;
#22792 = ORIENTED_EDGE ( 'NONE', *, *, #25492, .T. ) ;
#22791 = CARTESIAN_POINT ( 'NONE',  ( -2.229367062499996610, -61.14583333196774362, 3.861377020970582219 ) ) ;
#22793 = CARTESIAN_POINT ( 'NONE',  ( 5.000000000000000888, -62.45833333060213732, 2.886751345948126879 ) ) ;
#22795 = ORIENTED_EDGE ( 'NONE', *, *, #57754, .T. ) ;
#22794 = CARTESIAN_POINT ( 'NONE',  ( -2.229367062499996610, -9.395833331967736513, 3.861377020970582219 ) ) ;
#22796 = CARTESIAN_POINT ( 'NONE',  ( -3.535250795749689387E-16, -78.25000000000001421, -5.773502691896257311 ) ) ;
#22797 = CARTESIAN_POINT ( 'NONE',  ( -50.70258187064364108, -138.1250000013656063, 2.196230717870141014 ) ) ;
#22798 = CARTESIAN_POINT ( 'NONE',  ( 2.229367062499998831, -49.89583333196772941, -3.861377020970580887 ) ) ;
#22799 = CARTESIAN_POINT ( 'NONE',  ( -5.000000000000000000, -76.87499999726880162, 0.000000000000000000 ) ) ;
#22801 = ORIENTED_EDGE ( 'NONE', *, *, #6782, .F. ) ;
#22800 = CARTESIAN_POINT ( 'NONE',  ( -4.999999999999998224, 10.20833333606451987, 2.886751345948131764 ) ) ;
#22802 = CARTESIAN_POINT ( 'NONE',  ( -59.98410592259440222, -150.1250000000000284, -0.3983568153799752487 ) ) ;
#22803 = CARTESIAN_POINT ( 'NONE',  ( 9.457646018065525792E-16, -19.31249999863440792, 5.148502694627439702 ) ) ;
#22805 = ORIENTED_EDGE ( 'NONE', *, *, #18185, .T. ) ;
#22804 = CARTESIAN_POINT ( 'NONE',  ( 9.457646018065525792E-16, -55.31249999863439371, 5.148502694627439702 ) ) ;
#22806 = SHAPE_REPRESENTATION_RELATIONSHIP ( 'NONE' , 'NONE' ,  #25037, #3382 ) ;
#22807 = CARTESIAN_POINT ( 'NONE',  ( -1.846868145590737420, -169.0000000013655779, 4.458734124999999437 ) ) ;
#22808 = CARTESIAN_POINT ( 'NONE',  ( -4.458734124999999437, -98.64583333196773651, -2.574251347313719407 ) ) ;
#22809 = CARTESIAN_POINT ( 'NONE',  ( 5.000000000000000888, -148.0625000027312126, -2.071067811865475505 ) ) ;
#22810 = VERTEX_POINT ( 'NONE', #7194 ) ;
#22811 = CARTESIAN_POINT ( 'NONE',  ( -56.48576386720575471, -151.0000000013656063, -4.591703134518078322 ) ) ;
#22812 = CARTESIAN_POINT ( 'NONE',  ( -54.60164318462004474, -143.5000000027312126, -4.984105922594373794 ) ) ;
#22813 =( BOUNDED_CURVE ( )  B_SPLINE_CURVE ( 2, ( #20348, #15528, #44137, #48962, #35461, #14870, #35148, #49295, #30626 ),
 .UNSPECIFIED., .F., .F. ) 
 B_SPLINE_CURVE_WITH_KNOTS ( ( 3, 2, 2, 2, 3 ),
 ( 0.4687500000000000000, 0.4694444444444444420, 0.4708333333333333259, 0.4722222222222222099, 0.4729166666666666519 ),
 .UNSPECIFIED. ) 
 CURVE ( )  GEOMETRIC_REPRESENTATION_ITEM ( )  RATIONAL_B_SPLINE_CURVE ( ( 0.9330127018922194093, 0.9330127018922194093, 1.000000000000000000, 0.8660254037844387076, 1.000000000000000000, 0.8660254037844387076, 1.000000000000000000, 0.9330127018922194093, 0.9330127018922194093 ) ) 
 REPRESENTATION_ITEM ( '' )  );
#22814 = CARTESIAN_POINT ( 'NONE',  ( 1.975475456537005874E-15, -29.74999999999999645, 5.000000000000000000 ) ) ;
#22815 = EDGE_CURVE ( 'NONE', #28751, #62202, #43729, .T. ) ;
#22816 = CARTESIAN_POINT ( 'NONE',  ( 4.458734125000001214, -4.895833331967740065, 2.574251347313718519 ) ) ;
#22817 = CARTESIAN_POINT ( 'NONE',  ( -4.458734124999999437, -93.56249999863440792, 0.000000000000000000 ) ) ;
#22818 = EDGE_CURVE ( 'NONE', #45276, #44207, #19112, .T. ) ;
#22819 = EDGE_CURVE ( 'NONE', #9785, #28712, #4252, .T. ) ;
#22820 = CARTESIAN_POINT ( 'NONE',  ( 3.152801135295367541, -149.5625000013655779, -3.152801135295367541 ) ) ;
#22821 = CARTESIAN_POINT ( 'NONE',  ( 4.458734124999999437, -27.06249999863440081, -5.460374474430324690E-16 ) ) ;
#22822 = DIRECTION ( 'NONE',  ( -0.000000000000000000, 1.000000000000000000, -0.000000000000000000 ) ) ;
#22823 = CARTESIAN_POINT ( 'NONE',  ( -59.59170313451811296, -138.5000000013656347, 1.485763867205729394 ) ) ;
#22824 = CARTESIAN_POINT ( 'NONE',  ( -3.152548672688508926E-16, -61.81249999863440081, -5.148502694627439702 ) ) ;
#22825 = CARTESIAN_POINT ( 'NONE',  ( -1.339745962155613812, -91.20534180126146850, -5.000000000000000000 ) ) ;
#22826 = CARTESIAN_POINT ( 'NONE',  ( 1.975475456537005874E-15, -42.62499999726880873, 5.000000000000000000 ) ) ;
#22827 = CARTESIAN_POINT ( 'NONE',  ( -4.458734124999999437, -147.0000000013656063, -1.846868145590735644 ) ) ;
#22828 = CARTESIAN_POINT ( 'NONE',  ( -3.152548672688508926E-16, 11.18750000136559386, -5.148502694627439702 ) ) ;
#22829 = ORIENTED_EDGE ( 'NONE', *, *, #33502, .F. ) ;
#22830 = CARTESIAN_POINT ( 'NONE',  ( -6.972266317189433020E-16, -53.12499999726880162, -5.000000000000000000 ) ) ;
#22831 = LINE ( 'NONE', #18621, #3275 ) ;
#22833 = CARTESIAN_POINT ( 'NONE',  ( -4.458734124999998549, -27.22916666530107221, 2.574251347313722516 ) ) ;
#22832 = CARTESIAN_POINT ( 'NONE',  ( -4.999999999999999112, -91.91666666666667140, 2.886751345948131764 ) ) ;
#22834 = CARTESIAN_POINT ( 'NONE',  ( 2.499999999999998668, -73.33333333333332860, -4.330127018922193649 ) ) ;
#22835 = CARTESIAN_POINT ( 'NONE',  ( -2.229367062499996610, -69.39583333196773651, 3.861377020970582219 ) ) ;
#22836 = CARTESIAN_POINT ( 'NONE',  ( -4.458734124999999437, 26.43750000136559564, 0.000000000000000000 ) ) ;
#22837 = DIRECTION ( 'NONE',  ( 0.000000000000000000, 0.000000000000000000, 1.000000000000000000 ) ) ;
#22838 = CARTESIAN_POINT ( 'NONE',  ( -50.70258187064364108, -145.1250000013655779, 2.196230717870141014 ) ) ;
#22839 = CARTESIAN_POINT ( 'NONE',  ( -2.229367062500000163, 3.520833334698929118, -3.861377020970580443 ) ) ;
#22840 = DIRECTION ( 'NONE',  ( -0.000000000000000000, 1.000000000000000000, -0.000000000000000000 ) ) ;
#22841 = EDGE_CURVE ( 'NONE', #15636, #44762, #26092, .T. ) ;
#22842 = CARTESIAN_POINT ( 'NONE',  ( -51.19402409849444524, -141.6250000027312126, -3.242614290531456334 ) ) ;
#22843 = CARTESIAN_POINT ( 'NONE',  ( -2.229367062500000163, 9.520833334698927786, -3.861377020970580443 ) ) ;
#22844 = CARTESIAN_POINT ( 'NONE',  ( 2.229367062500001939, -71.97916666530107932, 3.861377020970579999 ) ) ;
#22845 = CARTESIAN_POINT ( 'NONE',  ( -2.229367062500000163, -19.72916666530107221, -3.861377020970580443 ) ) ;
#22846 = CARTESIAN_POINT ( 'NONE',  ( -2.499999999999996447, -3.833333333333334370, 4.330127018922195425 ) ) ;
#22847 = CARTESIAN_POINT ( 'NONE',  ( -3.152801135295367096, -160.0625000013656063, -3.152801135295367541 ) ) ;
#22848 = CARTESIAN_POINT ( 'NONE',  ( 1.975475456537005874E-15, -67.62499999726881583, 5.000000000000000000 ) ) ;
#22849 = CARTESIAN_POINT ( 'NONE',  ( 2.229367062500001939, -62.97916666530106511, 3.861377020970579999 ) ) ;
#22850 = CARTESIAN_POINT ( 'NONE',  ( -4.999999999999999112, -98.79166666393547303, 2.886751345948131764 ) ) ;
#22851 = CARTESIAN_POINT ( 'NONE',  ( -57.46284108482265651, -148.9375000000000000, 4.819101127000238627 ) ) ;
#22852 = CARTESIAN_POINT ( 'NONE',  ( -4.458734124999999437, -42.31249999863440081, 0.000000000000000000 ) ) ;
#22853 = CARTESIAN_POINT ( 'NONE',  ( 4.458734124999999437, -107.0624999986343937, -5.460374474430324690E-16 ) ) ;
#22854 = CARTESIAN_POINT ( 'NONE',  ( 2.229367062500001939, -65.22916666530106511, 3.861377020970579999 ) ) ;
#22855 = CARTESIAN_POINT ( 'NONE',  ( -3.535250795749689387E-16, -48.25000000000000000, -5.773502691896257311 ) ) ;
#22856 = CARTESIAN_POINT ( 'NONE',  ( -2.499999999999996447, -22.83333333333333215, 4.330127018922195425 ) ) ;
#22857 = CARTESIAN_POINT ( 'NONE',  ( -4.330127018922205195, 45.00000000000000000, -7.499999999999943157 ) ) ;
#22858 = VERTEX_POINT ( 'NONE', #48300 ) ;
#22859 = LINE ( 'NONE', #27978, #26312 ) ;
#22860 = CARTESIAN_POINT ( 'NONE',  ( 1.975475456537005874E-15, -99.62499999726880162, 5.000000000000000000 ) ) ;
#22861 = CARTESIAN_POINT ( 'NONE',  ( -5.000000000000000000, -11.08333333333333393, -2.886751345948128211 ) ) ;
#22862 = CARTESIAN_POINT ( 'NONE',  ( -4.458734124999999437, -16.39583333196773651, -2.574251347313719407 ) ) ;
#22863 = CARTESIAN_POINT ( 'NONE',  ( -4.458734124999999437, -78.39583333196772230, -2.574251347313719407 ) ) ;
#22864 = CARTESIAN_POINT ( 'NONE',  ( 1.975475456537005874E-15, 12.24999999999999822, 5.000000000000000000 ) ) ;
#22865 = CARTESIAN_POINT ( 'NONE',  ( 2.500000000000002220, -11.54166666393547835, 4.330127018922192761 ) ) ;
#22867 = ORIENTED_EDGE ( 'NONE', *, *, #59743, .F. ) ;
#22866 = CARTESIAN_POINT ( 'NONE',  ( 2.229367062499998831, -42.64583333196773651, -3.861377020970580887 ) ) ;
#22869 = ORIENTED_EDGE ( 'NONE', *, *, #57115, .T. ) ;
#22868 = CARTESIAN_POINT ( 'NONE',  ( 2.229367062499998831, 9.104166668032261711, -3.861377020970580887 ) ) ;
#22870 = CARTESIAN_POINT ( 'NONE',  ( 2.493747252781420335E-13, -90.25000000000000000, -5.000000000000000000 ) ) ;
#22871 = CARTESIAN_POINT ( 'NONE',  ( 5.000000000000000000, -55.49999999999999289, -6.123233995736766282E-16 ) ) ;
#22872 = CARTESIAN_POINT ( 'NONE',  ( -8.190561711645485556E-16, -159.9375000013655779, 4.458734124999999437 ) ) ;
#22873 = CARTESIAN_POINT ( 'NONE',  ( 2.229367062499998831, -35.89583333196773651, -3.861377020970580887 ) ) ;
#22874 = PLANE ( 'NONE',  #53254 ) ;
#22875 = CARTESIAN_POINT ( 'NONE',  ( -3.152548672688508926E-16, -81.56249999863440792, -5.148502694627439702 ) ) ;
#22876 = CARTESIAN_POINT ( 'NONE',  ( 2.071067811865476394, -165.1875000000000000, 5.000000000000000000 ) ) ;
#22877 = CARTESIAN_POINT ( 'NONE',  ( 5.000000000000000888, 5.541666669397853795, 2.886751345948126879 ) ) ;
#22878 = CARTESIAN_POINT ( 'NONE',  ( -56.48576386720575471, -130.0000000013656063, -4.591703134518078322 ) ) ;
#22879 = CARTESIAN_POINT ( 'NONE',  ( -2.229367062500000163, -1.729166665301071992, -3.861377020970580443 ) ) ;
#22880 = CARTESIAN_POINT ( 'NONE',  ( -3.152548672688508926E-16, -42.81249999863440081, -5.148502694627439702 ) ) ;
#22881 = DIRECTION ( 'NONE',  ( 0.000000000000000000, 1.000000000000000000, 0.000000000000000000 ) ) ;
#22882 = CARTESIAN_POINT ( 'NONE',  ( 2.229367062500001939, -84.22916666530107932, 3.861377020970579999 ) ) ;
#22883 = CARTESIAN_POINT ( 'NONE',  ( 2.499999999999998668, -84.33333333333332860, -4.330127018922193649 ) ) ;
#22884 = ORIENTED_EDGE ( 'NONE', *, *, #8025, .T. ) ;
#22885 = CARTESIAN_POINT ( 'NONE',  ( -9.184850993605147944E-16, -141.2500000000000284, 5.000000000000000000 ) ) ;
#22886 = CARTESIAN_POINT ( 'NONE',  ( -7.908030677224553884, 3.059924800338342799, -7.792662696733364314 ) ) ;
#22887 = CARTESIAN_POINT ( 'NONE',  ( 2.229367062500001939, -71.22916666530107932, 3.861377020970579999 ) ) ;
#22888 = CARTESIAN_POINT ( 'NONE',  ( 4.458734125000001214, -9.145833331967736513, 2.574251347313718519 ) ) ;
#22889 = VERTEX_POINT ( 'NONE', #8761 ) ;
#22890 =( BOUNDED_CURVE ( )  B_SPLINE_CURVE ( 2, ( #745, #45754, #31593, #44785, #56048, #25818, #60561, #31264, #16800 ),
 .UNSPECIFIED., .F., .F. ) 
 B_SPLINE_CURVE_WITH_KNOTS ( ( 3, 2, 2, 2, 3 ),
 ( 0.8354166666666666963, 0.8361111111111111382, 0.8375000000000000222, 0.8388888888888889062, 0.8395833333333333481 ),
 .UNSPECIFIED. ) 
 CURVE ( )  GEOMETRIC_REPRESENTATION_ITEM ( )  RATIONAL_B_SPLINE_CURVE ( ( 0.9330127018922194093, 0.9330127018922194093, 1.000000000000000000, 0.8660254037844387076, 1.000000000000000000, 0.8660254037844387076, 1.000000000000000000, 0.9330127018922194093, 0.9330127018922194093 ) ) 
 REPRESENTATION_ITEM ( '' )  );
#22891 = CARTESIAN_POINT ( 'NONE',  ( 2.499999999999998668, -5.333333333333335702, -4.330127018922193649 ) ) ;
#22892 = EDGE_CURVE ( 'NONE', #24529, #31402, #10013, .T. ) ;
#22893 = EDGE_CURVE ( 'NONE', #16274, #48010, #28680, .T. ) ;
#22894 = CARTESIAN_POINT ( 'NONE',  ( 5.000000000000000000, -3.374999997268816276, -6.123233995736766282E-16 ) ) ;
#22895 = CARTESIAN_POINT ( 'NONE',  ( 9.457646018065525792E-16, -5.312499998634402587, 5.148502694627439702 ) ) ;
#22896 = EDGE_CURVE ( 'NONE', #6296, #34224, #63428, .T. ) ;
#22897 = CARTESIAN_POINT ( 'NONE',  ( -51.75738570946856498, -150.8750000027312126, 3.805975901505576964 ) ) ;
#22898 = CARTESIAN_POINT ( 'NONE',  ( 9.457646018065525792E-16, 1.937500001365593416, 5.148502694627439702 ) ) ;
#22899 = CARTESIAN_POINT ( 'NONE',  ( -2.500000000000000444, -80.16666666666665719, -4.330127018922193649 ) ) ;
#22900 = CARTESIAN_POINT ( 'NONE',  ( 2.730187237215162345E-16, -158.1875000013655779, -4.458734124999999437 ) ) ;
#22901 = CARTESIAN_POINT ( 'NONE',  ( -3.152548672688508926E-16, 25.18750000136558853, -5.148502694627439702 ) ) ;
#22902 = EDGE_LOOP ( 'NONE', ( #36308, #3194, #12492, #63405 ) ) ;
#22903 = CARTESIAN_POINT ( 'NONE',  ( 4.458734125000000326, -92.89583333196773651, 2.574251347313718519 ) ) ;
#22904 = CARTESIAN_POINT ( 'NONE',  ( -6.972266317189433020E-16, -31.24999999999999645, -5.000000000000000000 ) ) ;
#22905 = CARTESIAN_POINT ( 'NONE',  ( -2.229367062499996610, -7.145833331967735624, 3.861377020970582219 ) ) ;
#22906 = ADVANCED_FACE ( 'NONE', ( #34135 ), #43470, .T. ) ;
#22908 = ADVANCED_FACE ( 'NONE', ( #23867 ), #43159, .T. ) ;
#22907 = FACE_OUTER_BOUND ( 'NONE', #38534, .T. ) ;
#22909 = CARTESIAN_POINT ( 'NONE',  ( 5.000000000000000888, -48.58333333333333570, 2.886751345948126879 ) ) ;
#22910 =( BOUNDED_CURVE ( )  B_SPLINE_CURVE ( 2, ( #43674, #8965, #14726, #28262, #28576, #38852, #9901, #276, #9274 ),
 .UNSPECIFIED., .F., .F. ) 
 B_SPLINE_CURVE_WITH_KNOTS ( ( 3, 2, 2, 2, 3 ),
 ( 0.1446428571428571563, 0.1452380952380952495, 0.1464285714285714357, 0.1476190476190476220, 0.1482142857142857151 ),
 .UNSPECIFIED. ) 
 CURVE ( )  GEOMETRIC_REPRESENTATION_ITEM ( )  RATIONAL_B_SPLINE_CURVE ( ( 0.9330127018922194093, 0.9330127018922209636, 1.000000000000000000, 0.8660254037844387076, 1.000000000000000000, 0.8660254037844387076, 1.000000000000000000, 0.9330127018922194093, 0.9330127018922194093 ) ) 
 REPRESENTATION_ITEM ( '' )  );
#22911 = CARTESIAN_POINT ( 'NONE',  ( -2.499999999999996447, 15.16666666666666607, 4.330127018922195425 ) ) ;
#22912 = CARTESIAN_POINT ( 'NONE',  ( 5.000000000000000888, -34.45833333060213732, 2.886751345948126879 ) ) ;
#22913 = DIRECTION ( 'NONE',  ( -0.000000000000000000, 1.000000000000000000, -0.000000000000000000 ) ) ;
#22914 = CARTESIAN_POINT ( 'NONE',  ( -3.152548672688508926E-16, 18.43750000136559564, -5.148502694627439702 ) ) ;
#22915 = CARTESIAN_POINT ( 'NONE',  ( 2.499999999999998668, -7.333333333333330373, -4.330127018922193649 ) ) ;
#22916 = CARTESIAN_POINT ( 'NONE',  ( -3.152548672688508926E-16, 21.43750000136559208, -5.148502694627439702 ) ) ;
#22917 = EDGE_CURVE ( 'NONE', #19872, #20646, #52020, .T. ) ;
#22918 = CARTESIAN_POINT ( 'NONE',  ( -4.458734124999999437, -54.39583333196773651, -2.574251347313719407 ) ) ;
#22919 = CARTESIAN_POINT ( 'NONE',  ( 4.458734124999999437, -6.062499998634403475, -5.460374474430324690E-16 ) ) ;
#22920 = FACE_OUTER_BOUND ( 'NONE', #43636, .T. ) ;
#22921 = CARTESIAN_POINT ( 'NONE',  ( 5.000000000000000000, 15.50000000000000000, -6.123233995736766282E-16 ) ) ;
#22922 = EDGE_CURVE ( 'NONE', #39751, #27115, #47498, .T. ) ;
#22923 = CARTESIAN_POINT ( 'NONE',  ( 3.535533905932738197, -143.0000000027311842, -3.535533905932738197 ) ) ;
#22924 = CARTESIAN_POINT ( 'NONE',  ( -2.499999999999996447, -51.83333333333332860, 4.330127018922195425 ) ) ;
#22925 = CARTESIAN_POINT ( 'NONE',  ( 2.229367062499998831, -47.64583333196774362, -3.861377020970580887 ) ) ;
#22926 = CARTESIAN_POINT ( 'NONE',  ( -2.499999999999996447, -85.70833333060214443, 4.330127018922195425 ) ) ;
#22927 = CARTESIAN_POINT ( 'NONE',  ( -59.59170313451811296, -136.7500000013655779, 1.485763867205729394 ) ) ;
#22928 = LINE ( 'NONE', #53437, #37801 ) ;
#22929 = CARTESIAN_POINT ( 'NONE',  ( 4.458734124999998549, -86.97916666530107932, -2.574251347313721627 ) ) ;
#22930 = CARTESIAN_POINT ( 'NONE',  ( 4.458734124999999437, -157.6875000013655779, 0.000000000000000000 ) ) ;
#22931 = CARTESIAN_POINT ( 'NONE',  ( -2.500000000000000444, -35.16666666666666430, -4.330127018922193649 ) ) ;
#22932 =( LENGTH_UNIT ( ) NAMED_UNIT ( * ) SI_UNIT ( .MILLI., .METRE. ) );
#22933 = ORIENTED_EDGE ( 'NONE', *, *, #10676, .F. ) ;
#22934 = CARTESIAN_POINT ( 'NONE',  ( -4.458734124999999437, 17.35416666803225993, -2.574251347313719407 ) ) ;
#22935 = ORIENTED_EDGE ( 'NONE', *, *, #28051, .T. ) ;
#22936 = CARTESIAN_POINT ( 'NONE',  ( -2.229367062500000163, -98.47916666530105090, -3.861377020970580443 ) ) ;
#22937 = CARTESIAN_POINT ( 'NONE',  ( 4.458734124999998549, 7.020833334698929562, -2.574251347313721627 ) ) ;
#22938 = CARTESIAN_POINT ( 'NONE',  ( 2.499999999999998668, 10.79166666939785202, -4.330127018922193649 ) ) ;
#22939 = CARTESIAN_POINT ( 'NONE',  ( 0.000000000000000000, -170.0000000000000000, 5.000000000000000000 ) ) ;
#22940 = CARTESIAN_POINT ( 'NONE',  ( 2.499999999999998668, 3.666666666666665186, -4.330127018922193649 ) ) ;
#22941 = CARTESIAN_POINT ( 'NONE',  ( 4.458734125000000326, -61.89583333196774362, 2.574251347313718519 ) ) ;
#22942 = CARTESIAN_POINT ( 'NONE',  ( -2.500000000000000444, -8.166666666666669627, -4.330127018922193649 ) ) ;
#22943 = CARTESIAN_POINT ( 'NONE',  ( -5.000000000000000000, -81.00000000000000000, 0.000000000000000000 ) ) ;
#22944 = CARTESIAN_POINT ( 'NONE',  ( -4.458734124999998549, -31.22916666530107221, 2.574251347313722516 ) ) ;
#22945 = CARTESIAN_POINT ( 'NONE',  ( 1.339745962155615144, 7.419658201469705894, 4.999999999999999112 ) ) ;
#22946 = CARTESIAN_POINT ( 'NONE',  ( -5.000000000000000888, -151.5625000027311842, 2.071067811865474617 ) ) ;
#22947 = CARTESIAN_POINT ( 'NONE',  ( 5.000000000000000000, -37.50000000000000711, -6.123233995736766282E-16 ) ) ;
#22948 = DIRECTION ( 'NONE',  ( -0.000000000000000000, 1.000000000000000000, -0.000000000000000000 ) ) ;
#22949 = CARTESIAN_POINT ( 'NONE',  ( 4.458734124999998549, -19.97916666530106866, -2.574251347313721627 ) ) ;
#22950 = CARTESIAN_POINT ( 'NONE',  ( 5.000000000000000000, -107.3749999972687874, -6.123233995736766282E-16 ) ) ;
#22951 = CARTESIAN_POINT ( 'NONE',  ( -2.229367062499996610, -63.14583333196774362, 3.861377020970582219 ) ) ;
#22952 = CARTESIAN_POINT ( 'NONE',  ( 2.730187237215162345E-16, -148.4375000013656063, -4.458734124999999437 ) ) ;
#22953 = CARTESIAN_POINT ( 'NONE',  ( -4.458734124999999437, -77.39583333196772230, -2.574251347313719407 ) ) ;
#22954 = CARTESIAN_POINT ( 'NONE',  ( -50.70258187064364108, -143.3750000013656063, 2.196230717870141014 ) ) ;
#22955 = CARTESIAN_POINT ( 'NONE',  ( -2.229367062499996610, -26.39583333196774007, 3.861377020970582219 ) ) ;
#22956 = CARTESIAN_POINT ( 'NONE',  ( 5.000000000000000000, -65.37499999726881583, -6.123233995736766282E-16 ) ) ;
#22957 = ORIENTED_EDGE ( 'NONE', *, *, #38515, .T. ) ;
#22958 = FACE_OUTER_BOUND ( 'NONE', #45720, .T. ) ;
#22959 = VERTEX_POINT ( 'NONE', #45709 ) ;
#22960 = CARTESIAN_POINT ( 'NONE',  ( 2.229367062500001939, -68.22916666530106511, 3.861377020970579999 ) ) ;
#22961 = CARTESIAN_POINT ( 'NONE',  ( -6.972266317189433020E-16, 10.87500000273118417, -5.000000000000000000 ) ) ;
#22962 = EDGE_LOOP ( 'NONE', ( #23409, #31003, #21766, #23490 ) ) ;
#22963 =( BOUNDED_CURVE ( )  B_SPLINE_CURVE ( 2, ( #38025, #47670, #27417, #38337, #37392, #2998, #22615, #3622, #13583 ),
 .UNSPECIFIED., .F., .F. ) 
 B_SPLINE_CURVE_WITH_KNOTS ( ( 3, 2, 2, 2, 3 ),
 ( 0.1446428571428571563, 0.1452380952380952495, 0.1464285714285714357, 0.1476190476190476220, 0.1482142857142857151 ),
 .UNSPECIFIED. ) 
 CURVE ( )  GEOMETRIC_REPRESENTATION_ITEM ( )  RATIONAL_B_SPLINE_CURVE ( ( 0.9330127018922194093, 0.9330127018922209636, 1.000000000000000000, 0.8660254037844387076, 1.000000000000000000, 0.8660254037844387076, 1.000000000000000000, 0.9330127018922194093, 0.9330127018922194093 ) ) 
 REPRESENTATION_ITEM ( '' )  );
#22964 = CARTESIAN_POINT ( 'NONE',  ( -53.33387254593733928, -126.8125000000000568, 5.149110718188519620 ) ) ;
#22965 = CARTESIAN_POINT ( 'NONE',  ( -2.500000000000000444, -56.04166666393548013, -4.330127018922193649 ) ) ;
#22966 = CARTESIAN_POINT ( 'NONE',  ( 2.229367062500001939, -51.22916666530107221, 3.861377020970579999 ) ) ;
#22967 = ORIENTED_EDGE ( 'NONE', *, *, #26905, .T. ) ;
#22968 = DIRECTION ( 'NONE',  ( -0.000000000000000000, 1.000000000000000000, -0.000000000000000000 ) ) ;
#22969 = CARTESIAN_POINT ( 'NONE',  ( 9.457646018065525792E-16, 6.937500001365594748, 5.148502694627439702 ) ) ;
#22970 = CARTESIAN_POINT ( 'NONE',  ( 4.458734124999998549, 19.27083333469893134, -2.574251347313721627 ) ) ;
#22971 = CARTESIAN_POINT ( 'NONE',  ( -59.59170313451811296, -143.5000000013656347, 1.485763867205729394 ) ) ;
#22972 = CARTESIAN_POINT ( 'NONE',  ( -5.000000000000000000, 6.041666669397852019, -2.886751345948128211 ) ) ;
#22973 = DIRECTION ( 'NONE',  ( -0.000000000000000000, 1.000000000000000000, -0.000000000000000000 ) ) ;
#22974 = ORIENTED_EDGE ( 'NONE', *, *, #38515, .F. ) ;
#22975 = CARTESIAN_POINT ( 'NONE',  ( -2.229367062500000163, -72.47916666530107932, -3.861377020970580443 ) ) ;
#22976 = CARTESIAN_POINT ( 'NONE',  ( 1.975475456537005874E-15, 14.37500000273118417, 5.000000000000000000 ) ) ;
#22977 = CARTESIAN_POINT ( 'NONE',  ( -4.458734124999998549, 9.770833334698927786, 2.574251347313722516 ) ) ;
#22978 = CARTESIAN_POINT ( 'NONE',  ( -6.972266317189433020E-16, -69.12499999726880162, -5.000000000000000000 ) ) ;
#22979 = CARTESIAN_POINT ( 'NONE',  ( -2.229367062500000163, -58.72916666530106511, -3.861377020970580443 ) ) ;
#22980 = CARTESIAN_POINT ( 'NONE',  ( -4.999999999999999112, -19.79166666393547658, 2.886751345948131764 ) ) ;
#22981 = CARTESIAN_POINT ( 'NONE',  ( -4.999999999999998224, -99.91666666666665719, 2.886751345948131764 ) ) ;
#22982 = CARTESIAN_POINT ( 'NONE',  ( -6.972266317189433020E-16, -45.12499999726880162, -5.000000000000000000 ) ) ;
#22983 = CARTESIAN_POINT ( 'NONE',  ( -50.18089887299976937, -140.8125000027311557, 2.462841084822427362 ) ) ;
#22984 = CARTESIAN_POINT ( 'NONE',  ( 1.975475456537005874E-15, -83.62499999726878741, 5.000000000000000000 ) ) ;
#22985 = CYLINDRICAL_SURFACE ( 'NONE', #26407, 5.000000000000000000 ) ;
#22986 = CARTESIAN_POINT ( 'NONE',  ( 4.458734124999999437, -38.81249999863440081, -5.460374474430324690E-16 ) ) ;
#22987 =( BOUNDED_CURVE ( )  B_SPLINE_CURVE ( 2, ( #19432, #34870, #43550, #15244, #58363, #10418, #49009, #14289, #39044 ),
 .UNSPECIFIED., .F., .F. ) 
 B_SPLINE_CURVE_WITH_KNOTS ( ( 3, 2, 2, 2, 3 ),
 ( 0.2750000000000002442, 0.2791666666666668961, 0.2833333333333335480, 0.2875000000000001998, 0.2916666666666669072 ),
 .UNSPECIFIED. ) 
 CURVE ( )  GEOMETRIC_REPRESENTATION_ITEM ( )  RATIONAL_B_SPLINE_CURVE ( ( 0.9999999999999958922, 0.9238795325112908463, 1.000000000000000000, 0.9238795325112867385, 1.000000000000000000, 0.9238795325112867385, 1.000000000000000000, 0.9238795325112826307, 1.000000000000003997 ) ) 
 REPRESENTATION_ITEM ( '' )  );
#22988 = CARTESIAN_POINT ( 'NONE',  ( -2.229367062500000163, -26.72916666530106866, -3.861377020970580443 ) ) ;
#22989 = ORIENTED_EDGE ( 'NONE', *, *, #9420, .T. ) ;
#22990 = CARTESIAN_POINT ( 'NONE',  ( -60.14911071818854538, -140.1875000027312126, 1.666127454062681146 ) ) ;
#22991 = CARTESIAN_POINT ( 'NONE',  ( 9.457646018065525792E-16, -107.0624999986343937, 5.148502694627439702 ) ) ;
#22992 = CARTESIAN_POINT ( 'NONE',  ( -5.000000000000000888, -152.5625000027312126, 2.071067811865474617 ) ) ;
#22993 = ORIENTED_EDGE ( 'NONE', *, *, #23566, .F. ) ;
#22994 = CARTESIAN_POINT ( 'NONE',  ( -3.152548672688508926E-16, -109.8124999986343795, -5.148502694627439702 ) ) ;
#22995 = CARTESIAN_POINT ( 'NONE',  ( 4.458734124999999437, -33.81249999863440792, -5.460374474430324690E-16 ) ) ;
#22996 = CARTESIAN_POINT ( 'NONE',  ( 1.060575238724906964E-15, -69.62499999726880162, 5.773502691896257311 ) ) ;
#22997 = CARTESIAN_POINT ( 'NONE',  ( -56.48576386720575471, -149.0000000013656063, -4.591703134518078322 ) ) ;
#22998 = CARTESIAN_POINT ( 'NONE',  ( 5.000000000000000000, -145.0625000000000284, 2.071067811865478614 ) ) ;
#22999 = EDGE_CURVE ( 'NONE', #9589, #32181, #54063, .T. ) ;
#23000 = CARTESIAN_POINT ( 'NONE',  ( -2.229367062499996610, -29.14583333196774007, 3.861377020970582219 ) ) ;
#23001 = CARTESIAN_POINT ( 'NONE',  ( 4.458734125000000326, -70.14583333196773651, 2.574251347313718519 ) ) ;
#23002 = CARTESIAN_POINT ( 'NONE',  ( 1.846868145590735200, -168.5000000013655779, -4.458734124999999437 ) ) ;
#23003 = CARTESIAN_POINT ( 'NONE',  ( 2.229367062500001939, -26.97916666530106866, 3.861377020970579999 ) ) ;
#23004 = CARTESIAN_POINT ( 'NONE',  ( 2.500000000000002220, -32.66666666666666430, 4.330127018922192761 ) ) ;
#23005 = CARTESIAN_POINT ( 'NONE',  ( 1.339745962155612702, 22.83034180399266333, -5.000000000000000000 ) ) ;
#23006 = CARTESIAN_POINT ( 'NONE',  ( 2.499999999999998668, -16.33333333333333215, -4.330127018922193649 ) ) ;
#23007 = CARTESIAN_POINT ( 'NONE',  ( -4.458734124999999437, -148.9375000013656063, -5.460374474430324690E-16 ) ) ;
#23008 = ORIENTED_EDGE ( 'NONE', *, *, #9494, .T. ) ;
#23009 = CARTESIAN_POINT ( 'NONE',  ( 3.535533905932738197, -149.8750000000000000, -3.535533905932738197 ) ) ;
#23010 = CARTESIAN_POINT ( 'NONE',  ( 2.229367062500001939, -57.22916666530107932, 3.861377020970579999 ) ) ;
#23011 = CARTESIAN_POINT ( 'NONE',  ( 1.060575238724906964E-15, 27.37500000273118062, 5.773502691896257311 ) ) ;
#23012 = CYLINDRICAL_SURFACE ( 'NONE', #59689, 5.000000000000000000 ) ;
#23013 = CARTESIAN_POINT ( 'NONE',  ( -4.999999999999999112, 26.08333333333333215, 2.886751345948131764 ) ) ;
#23014 = DIRECTION ( 'NONE',  ( -0.000000000000000000, 1.000000000000000000, -0.000000000000000000 ) ) ;
#23015 = CARTESIAN_POINT ( 'NONE',  ( -2.229367062500000163, 1.520833334698927564, -3.861377020970580443 ) ) ;
#23016 = CARTESIAN_POINT ( 'NONE',  ( -5.000000000000000888, -164.4375000000000284, 2.071067811865474617 ) ) ;
#23017 = CARTESIAN_POINT ( 'NONE',  ( -2.229367062500000163, 11.27083333469892601, -3.861377020970580443 ) ) ;
#23018 = EDGE_LOOP ( 'NONE', ( #60784, #6892, #29659, #30931 ) ) ;
#23019 = CARTESIAN_POINT ( 'NONE',  ( -6.972266317189433020E-16, -16.25000000000000000, -5.000000000000000000 ) ) ;
#23020 = VERTEX_POINT ( 'NONE', #34782 ) ;
#23021 = CARTESIAN_POINT ( 'NONE',  ( 5.000000000000000888, 27.54166666939785557, 2.886751345948126879 ) ) ;
#23022 = CARTESIAN_POINT ( 'NONE',  ( -2.229367062499996610, -51.14583333196772941, 3.861377020970582219 ) ) ;
#23023 = CARTESIAN_POINT ( 'NONE',  ( -4.458734125000000326, -158.2500000013656063, -1.846868145590735644 ) ) ;
#23024 = CARTESIAN_POINT ( 'NONE',  ( -2.499999999999996447, -45.70833333060214443, 4.330127018922195425 ) ) ;
#23025 = ORIENTED_EDGE ( 'NONE', *, *, #27958, .F. ) ;
#23026 = CARTESIAN_POINT ( 'NONE',  ( 2.229367062500001939, -20.97916666530107221, 3.861377020970579999 ) ) ;
#23027 = ORIENTED_EDGE ( 'NONE', *, *, #4580, .T. ) ;
#23029 = CARTESIAN_POINT ( 'NONE',  ( -58.24261429053147765, -155.0000000000000284, -3.805975901505573411 ) ) ;
#23028 = DIRECTION ( 'NONE',  ( -1.000000000000000000, 0.000000000000000000, -0.000000000000000000 ) ) ;
#23030 = CARTESIAN_POINT ( 'NONE',  ( 2.730187237215162345E-16, -160.1875000013655779, -4.458734124999999437 ) ) ;
#23031 = DIRECTION ( 'NONE',  ( 0.000000000000000000, 0.000000000000000000, 1.000000000000000000 ) ) ;
#23032 = CARTESIAN_POINT ( 'NONE',  ( -58.80597590150559739, -139.0000000000000284, 3.242614290531460330 ) ) ;
#23033 = CARTESIAN_POINT ( 'NONE',  ( 2.229367062499998831, -35.89583333196773651, -3.861377020970580887 ) ) ;
#23034 = CARTESIAN_POINT ( 'NONE',  ( -4.999999999999998224, 17.08333333333333215, 2.886751345948131764 ) ) ;
#23035 = EDGE_LOOP ( 'NONE', ( #42574, #44528, #25585, #57600 ) ) ;
#23036 = CARTESIAN_POINT ( 'NONE',  ( -4.458734124999998549, -81.22916666530106511, 2.574251347313722516 ) ) ;
#23037 = CARTESIAN_POINT ( 'NONE',  ( -4.458734124999998549, 26.77083333469893134, 2.574251347313722516 ) ) ;
#23038 = CARTESIAN_POINT ( 'NONE',  ( 5.000000000000000000, -59.50000000000000000, -6.123233995736766282E-16 ) ) ;
#23039 = ORIENTED_EDGE ( 'NONE', *, *, #53434, .T. ) ;
#23040 = CARTESIAN_POINT ( 'NONE',  ( 5.000000000000000888, -69.45833333060214443, 2.886751345948126879 ) ) ;
#23041 = CARTESIAN_POINT ( 'NONE',  ( -52.80376928212989185, -140.1250000013656347, -4.297418129356378458 ) ) ;
#23042 = CARTESIAN_POINT ( 'NONE',  ( 2.229367062499998831, -83.89583333196773651, -3.861377020970580887 ) ) ;
#23043 = CARTESIAN_POINT ( 'NONE',  ( -54.60164318462004474, -129.5000000027312126, -4.984105922594373794 ) ) ;
#23044 = CARTESIAN_POINT ( 'NONE',  ( 0.000000000000000000, 15.00000000000000000, 0.000000000000000000 ) ) ;
#23045 = CARTESIAN_POINT ( 'NONE',  ( 0.000000000000000000, -170.0000000000000000, 0.000000000000000000 ) ) ;
#23046 = CARTESIAN_POINT ( 'NONE',  ( -4.458734124999999437, -53.39583333196773651, -2.574251347313719407 ) ) ;
#23047 = CARTESIAN_POINT ( 'NONE',  ( 5.000000000000000000, 10.49999999999999822, -6.123233995736766282E-16 ) ) ;
#23048 = CARTESIAN_POINT ( 'NONE',  ( 9.457646018065525792E-16, 25.93750000136559564, 5.148502694627439702 ) ) ;
#23049 = CARTESIAN_POINT ( 'NONE',  ( 5.000000000000000000, -109.4166666666666572, -2.886751345948129988 ) ) ;
#23050 = CARTESIAN_POINT ( 'NONE',  ( -4.999999999999998224, -81.91666666666667140, 2.886751345948131764 ) ) ;
#23051 = CARTESIAN_POINT ( 'NONE',  ( 4.458734124999998549, -42.97916666530107221, -2.574251347313721627 ) ) ;
#23052 = CARTESIAN_POINT ( 'NONE',  ( 1.060575238724906964E-15, -3.624999997268816276, 5.773502691896257311 ) ) ;
#23053 = CYLINDRICAL_SURFACE ( 'NONE', #22244, 5.000000000000000000 ) ;
#23054 = CARTESIAN_POINT ( 'NONE',  ( -51.60603307380591787, -126.9375000013656063, -2.891590998281053704 ) ) ;
#23055 = CARTESIAN_POINT ( 'NONE',  ( -2.229367062499996610, -82.39583333196773651, 3.861377020970582219 ) ) ;
#23056 = CARTESIAN_POINT ( 'NONE',  ( 2.229367062500001939, -101.9791666653010651, 3.861377020970579999 ) ) ;
#23057 = CARTESIAN_POINT ( 'NONE',  ( 2.229367062500001939, -3.229166665301069550, 3.861377020970579999 ) ) ;
#23058 = ORIENTED_EDGE ( 'NONE', *, *, #1366, .F. ) ;
#23059 = CARTESIAN_POINT ( 'NONE',  ( -5.000000000000000000, -155.6250000027311842, -6.123233995736766282E-16 ) ) ;
#23060 = CARTESIAN_POINT ( 'NONE',  ( 2.229367062499998831, -91.64583333196773651, -3.861377020970580887 ) ) ;
#23061 = CARTESIAN_POINT ( 'NONE',  ( -5.000000000000000888, -163.5625000027312126, 2.071067811865474617 ) ) ;
#23062 = CARTESIAN_POINT ( 'NONE',  ( 4.458734124999999437, -94.06249999863440792, -5.460374474430324690E-16 ) ) ;
#23063 = CARTESIAN_POINT ( 'NONE',  ( -5.000000000000000000, -16.08333333333333215, -2.886751345948128211 ) ) ;
#23064 = CARTESIAN_POINT ( 'NONE',  ( -56.48576386720575471, -130.7500000013656063, -4.591703134518078322 ) ) ;
#23065 = CARTESIAN_POINT ( 'NONE',  ( -4.458734124999997661, -14.22916666530107221, 2.574251347313722516 ) ) ;
#23066 = CARTESIAN_POINT ( 'NONE',  ( 4.458734124999998549, 13.02083333469892779, -2.574251347313721627 ) ) ;
#23067 = CARTESIAN_POINT ( 'NONE',  ( 4.458734125000000326, -51.14583333196772941, 2.574251347313718519 ) ) ;
#23068 = CARTESIAN_POINT ( 'NONE',  ( -2.499999999999996447, -19.83333333333333570, 4.330127018922195425 ) ) ;
#23069 = CARTESIAN_POINT ( 'NONE',  ( -5.000000000000000888, -152.4375000000000000, 2.071067811865474617 ) ) ;
#23070 = CARTESIAN_POINT ( 'NONE',  ( 4.458734124999998549, -10.72916666530106866, -2.574251347313721627 ) ) ;
#23071 =( NAMED_UNIT ( * ) PLANE_ANGLE_UNIT ( ) SI_UNIT ( $, .RADIAN. ) );
#23072 = EDGE_LOOP ( 'NONE', ( #2739, #6018, #40224, #2157 ) ) ;
#23073 = CARTESIAN_POINT ( 'NONE',  ( 4.458734124999999437, -34.06249999863440792, -5.460374474430324690E-16 ) ) ;
#23074 = CARTESIAN_POINT ( 'NONE',  ( -52.80376928212989185, -128.1250000013656347, -4.297418129356379346 ) ) ;
#23075 = CARTESIAN_POINT ( 'NONE',  ( 1.062108568985190270E-13, -26.12499999726881583, -4.999999999999999112 ) ) ;
#23076 = CARTESIAN_POINT ( 'NONE',  ( -2.500000000000000444, -70.16666666666667140, -4.330127018922193649 ) ) ;
#23077 = CARTESIAN_POINT ( 'NONE',  ( 4.458734124999998549, -81.72916666530106511, -2.574251347313721627 ) ) ;
#23078 = CARTESIAN_POINT ( 'NONE',  ( 2.229367062499998831, 25.10416666803225993, -3.861377020970580887 ) ) ;
#23079 =( BOUNDED_CURVE ( )  B_SPLINE_CURVE ( 2, ( #2874, #22490, #42086, #38434, #61728, #17657, #37273, #56900, #12819 ),
 .UNSPECIFIED., .F., .F. ) 
 B_SPLINE_CURVE_WITH_KNOTS ( ( 3, 2, 2, 2, 3 ),
 ( 0.4479166666666666852, 0.4486111111111111271, 0.4500000000000000111, 0.4513888888888888951, 0.4520833333333333370 ),
 .UNSPECIFIED. ) 
 CURVE ( )  GEOMETRIC_REPRESENTATION_ITEM ( )  RATIONAL_B_SPLINE_CURVE ( ( 0.9330127018922194093, 0.9330127018922194093, 1.000000000000000000, 0.8660254037844387076, 1.000000000000000000, 0.8660254037844387076, 1.000000000000000000, 0.9330127018922194093, 0.9330127018922194093 ) ) 
 REPRESENTATION_ITEM ( '' )  );
#23080 = CARTESIAN_POINT ( 'NONE',  ( 4.458734124999999437, 13.18750000136559208, -5.460374474430324690E-16 ) ) ;
#23081 = DIRECTION ( 'NONE',  ( -0.000000000000000000, 1.000000000000000000, -0.000000000000000000 ) ) ;
#23082 = CARTESIAN_POINT ( 'NONE',  ( 1.339745962155612702, -55.29465819873852439, -5.000000000000000000 ) ) ;
#23083 = CARTESIAN_POINT ( 'NONE',  ( -4.458734124999997661, -84.47916666530107932, 2.574251347313722516 ) ) ;
#23084 = CARTESIAN_POINT ( 'NONE',  ( 2.500000000000002220, -70.66666666666667140, 4.330127018922192761 ) ) ;
#23085 = CARTESIAN_POINT ( 'NONE',  ( -2.500000000000000444, 12.95833333606451809, -4.330127018922193649 ) ) ;
#23086 = ORIENTED_EDGE ( 'NONE', *, *, #909, .F. ) ;
#23087 = CARTESIAN_POINT ( 'NONE',  ( 5.000000000000000888, -25.58333333333333215, 2.886751345948126879 ) ) ;
#23088 = DIRECTION ( 'NONE',  ( -0.000000000000000000, 1.000000000000000000, -0.000000000000000000 ) ) ;
#23090 = CARTESIAN_POINT ( 'NONE',  ( -2.499999999999996447, -26.83333333333333570, 4.330127018922195425 ) ) ;
#23089 = CARTESIAN_POINT ( 'NONE',  ( 1.339745962155615144, -52.70534180126147561, 4.999999999999999112 ) ) ;
#23091 = CARTESIAN_POINT ( 'NONE',  ( -4.458734124999999437, -31.31249999863440436, 0.000000000000000000 ) ) ;
#23092 = ADVANCED_FACE ( 'NONE', ( #6480 ), #19982, .T. ) ;
#23093 = CARTESIAN_POINT ( 'NONE',  ( 0.000000000000000000, -120.0000000000000000, 0.000000000000000000 ) ) ;
#23094 = CARTESIAN_POINT ( 'NONE',  ( 2.500000000000002220, -30.54166666393548013, 4.330127018922192761 ) ) ;
#23096 = VERTEX_POINT ( 'NONE', #39591 ) ;
#23095 = CARTESIAN_POINT ( 'NONE',  ( 4.458734124999998549, -59.72916666530106511, -2.574251347313721627 ) ) ;
#23097 = CARTESIAN_POINT ( 'NONE',  ( 2.500000000000002220, -28.66666666666666785, 4.330127018922192761 ) ) ;
#23099 = VERTEX_POINT ( 'NONE', #25124 ) ;
#23098 = CARTESIAN_POINT ( 'NONE',  ( -4.458734124999999437, -7.645833331967735624, -2.574251347313719407 ) ) ;
#23100 = CARTESIAN_POINT ( 'NONE',  ( 5.000000000000000000, -74.41666666666665719, -2.886751345948129988 ) ) ;
#23101 = CARTESIAN_POINT ( 'NONE',  ( -59.59170313451810586, -135.5000000013656063, 1.485763867205729394 ) ) ;
#23102 = CARTESIAN_POINT ( 'NONE',  ( -4.458734124999999437, -51.64583333196773651, -2.574251347313719407 ) ) ;
#23103 = CARTESIAN_POINT ( 'NONE',  ( 5.000000000000000000, -76.37499999726880162, -6.123233995736766282E-16 ) ) ;
#23105 = ORIENTED_EDGE ( 'NONE', *, *, #1264, .F. ) ;
#23104 = CARTESIAN_POINT ( 'NONE',  ( -6.972266317189433020E-16, -55.12499999726880873, -5.000000000000000000 ) ) ;
#23106 = CARTESIAN_POINT ( 'NONE',  ( -51.19402409849444524, -151.5000000000000284, -3.242614290531456334 ) ) ;
#23107 = CARTESIAN_POINT ( 'NONE',  ( 4.458734124999998549, -22.97916666530107221, -2.574251347313721627 ) ) ;
#23109 = ORIENTED_EDGE ( 'NONE', *, *, #21125, .T. ) ;
#23108 = CARTESIAN_POINT ( 'NONE',  ( -4.458734124999998549, -59.47916666530106511, 2.574251347313722516 ) ) ;
#23110 = SURFACE_STYLE_USAGE ( .BOTH. , #13460 ) ;
#23111 = CARTESIAN_POINT ( 'NONE',  ( -1.846868145590734756, -140.1250000013655779, -4.458734125000000326 ) ) ;
#23112 = CARTESIAN_POINT ( 'NONE',  ( 2.229367062499998831, -99.89583333196773651, -3.861377020970580887 ) ) ;
#23113 = CARTESIAN_POINT ( 'NONE',  ( -4.999999999999998224, -26.79166666393547658, 2.886751345948131764 ) ) ;
#23114 = ORIENTED_EDGE ( 'NONE', *, *, #23349, .T. ) ;
#23115 = CARTESIAN_POINT ( 'NONE',  ( -52.10840900171896806, -150.4375000013656063, 3.393966926194110556 ) ) ;
#23116 = CARTESIAN_POINT ( 'NONE',  ( -52.53715891517739323, -142.5625000027312126, -4.819101127000233298 ) ) ;
#23117 = CYLINDRICAL_SURFACE ( 'NONE', #34236, 5.000000000000000000 ) ;
#23118 = CARTESIAN_POINT ( 'NONE',  ( 4.458734125000001214, -5.895833331967740953, 2.574251347313718519 ) ) ;
#23119 = CARTESIAN_POINT ( 'NONE',  ( 2.229367062500001939, -97.22916666530105090, 3.861377020970579999 ) ) ;
#23120 = CARTESIAN_POINT ( 'NONE',  ( 4.458734124999999437, -145.7500000013655779, 1.846868145590737864 ) ) ;
#23121 = CARTESIAN_POINT ( 'NONE',  ( -2.229367062499996610, -26.39583333196774007, 3.861377020970582219 ) ) ;
#23122 = CARTESIAN_POINT ( 'NONE',  ( 1.975475456537005874E-15, -74.75000000000000000, 5.000000000000000000 ) ) ;
#23123 = CARTESIAN_POINT ( 'NONE',  ( -55.35523342533222291, -135.3125000013656063, 4.444560631937231499 ) ) ;
#23124 =( BOUNDED_CURVE ( )  B_SPLINE_CURVE ( 2, ( #48177, #8942, #42717, #24365, #52393, #14390, #19212, #8630, #24055 ),
 .UNSPECIFIED., .F., .F. ) 
 B_SPLINE_CURVE_WITH_KNOTS ( ( 3, 2, 2, 2, 3 ),
 ( 0.04166666666666670599, 0.04583333333333337173, 0.05000000000000004441, 0.05416666666666671709, 0.05833333333333338283 ),
 .UNSPECIFIED. ) 
 CURVE ( )  GEOMETRIC_REPRESENTATION_ITEM ( )  RATIONAL_B_SPLINE_CURVE ( ( 0.9999999999999992228, 0.9238795325112875156, 1.000000000000000000, 0.9238795325112867385, 1.000000000000000000, 0.9238795325112867385, 1.000000000000000000, 0.9238795325112858503, 1.000000000000000888 ) ) 
 REPRESENTATION_ITEM ( '' )  );
#23125 = CARTESIAN_POINT ( 'NONE',  ( -4.458734124999999437, -67.56249999863440792, 0.000000000000000000 ) ) ;
#23126 = CARTESIAN_POINT ( 'NONE',  ( -4.999999999999998224, 17.08333333333333215, 2.886751345948131764 ) ) ;
#23127 = CARTESIAN_POINT ( 'NONE',  ( 4.458734124999997661, -142.5000000013656063, 1.846868145590737864 ) ) ;
#23128 = CARTESIAN_POINT ( 'NONE',  ( -4.458734124999999437, 8.354166668032261711, -2.574251347313719407 ) ) ;
#23129 = ORIENTED_EDGE ( 'NONE', *, *, #27955, .F. ) ;
#23130 = DIRECTION ( 'NONE',  ( -0.000000000000000000, 1.000000000000000000, -0.000000000000000000 ) ) ;
#23132 = CARTESIAN_POINT ( 'NONE',  ( -4.458734124999998549, -22.22916666530107221, 2.574251347313722516 ) ) ;
#23131 = CARTESIAN_POINT ( 'NONE',  ( -2.499999999999996447, -89.83333333333332860, 4.330127018922195425 ) ) ;
#23133 = PLANE ( 'NONE',  #18229 ) ;
#23134 = CARTESIAN_POINT ( 'NONE',  ( -2.229367062500000163, -78.72916666530106511, -3.861377020970580443 ) ) ;
#23135 = CARTESIAN_POINT ( 'NONE',  ( 4.458734125000000326, 25.85416666803225993, 2.574251347313718519 ) ) ;
#23136 = CARTESIAN_POINT ( 'NONE',  ( -5.000000000000000000, -17.95833333060214798, -2.886751345948128211 ) ) ;
#23137 = CARTESIAN_POINT ( 'NONE',  ( -50.40829686548195099, -144.0000000013656063, -1.485763867205728284 ) ) ;
#23138 = CARTESIAN_POINT ( 'NONE',  ( 4.458734124999998549, 4.270833334698926897, -2.574251347313721627 ) ) ;
#23139 = CARTESIAN_POINT ( 'NONE',  ( -3.152548672688508926E-16, 26.18750000136559564, -5.148502694627439702 ) ) ;
#23140 = CARTESIAN_POINT ( 'NONE',  ( -2.229367062500000163, -38.72916666530107221, -3.861377020970580443 ) ) ;
#23141 = CARTESIAN_POINT ( 'NONE',  ( -4.999999999999998224, -3.791666663935478798, 2.886751345948131764 ) ) ;
#23142 = CARTESIAN_POINT ( 'NONE',  ( 4.458734124999999437, 7.187500001365594748, -5.460374474430324690E-16 ) ) ;
#23143 = CARTESIAN_POINT ( 'NONE',  ( 2.229367062499998831, -70.64583333196773651, -3.861377020970580887 ) ) ;
#23144 = CARTESIAN_POINT ( 'NONE',  ( 2.229367062499998831, -21.89583333196774007, -3.861377020970580887 ) ) ;
#23145 = CARTESIAN_POINT ( 'NONE',  ( -5.000000000000000000, -8.083333333333330373, -2.886751345948128211 ) ) ;
#23146 = CARTESIAN_POINT ( 'NONE',  ( -4.458734124999999437, -160.9375000013655779, -5.460374474430324690E-16 ) ) ;
#23147 = CARTESIAN_POINT ( 'NONE',  ( -2.071067811865351604, -158.3125000000000284, 5.000000000000126121 ) ) ;
#23148 = CARTESIAN_POINT ( 'NONE',  ( -4.458734124999999437, -65.31249999863440792, 0.000000000000000000 ) ) ;
#23149 = CARTESIAN_POINT ( 'NONE',  ( -3.535250795749689387E-16, -101.1249999972688158, -5.773502691896257311 ) ) ;
#23150 = CARTESIAN_POINT ( 'NONE',  ( 2.229367062499998831, 29.35416666803225993, -3.861377020970580887 ) ) ;
#23151 = CARTESIAN_POINT ( 'NONE',  ( -4.458734124999997661, -42.22916666530107932, 2.574251347313722516 ) ) ;
#23152 = LINE ( 'NONE', #29216, #59558 ) ;
#23153 = CARTESIAN_POINT ( 'NONE',  ( -3.152548672688508926E-16, -108.8124999986343937, -5.148502694627439702 ) ) ;
#23154 = CARTESIAN_POINT ( 'NONE',  ( -2.229367062500000163, -66.72916666530106511, -3.861377020970580443 ) ) ;
#23155 = CARTESIAN_POINT ( 'NONE',  ( -3.535250795749689387E-16, -56.25000000000000000, -5.773502691896257311 ) ) ;
#23156 = CARTESIAN_POINT ( 'NONE',  ( -5.000000000000000000, 27.00000000000000000, 0.000000000000000000 ) ) ;
#23157 = CARTESIAN_POINT ( 'NONE',  ( 1.339745962155615144, -89.70534180126146850, 4.999999999999999112 ) ) ;
#23158 = ORIENTED_EDGE ( 'NONE', *, *, #54678, .T. ) ;
#23159 = CARTESIAN_POINT ( 'NONE',  ( 6.123233995736766282E-16, -120.0000000000000000, -5.000000000000000000 ) ) ;
#23160 = CARTESIAN_POINT ( 'NONE',  ( 1.339745962155612702, -6.169658196007334894, -5.000000000000000000 ) ) ;
#23161 = CARTESIAN_POINT ( 'NONE',  ( -4.999999999999999112, -13.91666666666666785, 2.886751345948131764 ) ) ;
#23162 = CARTESIAN_POINT ( 'NONE',  ( 9.457646018065525792E-16, -18.06249999863440436, 5.148502694627439702 ) ) ;
#23163 = EDGE_CURVE ( 'NONE', #17975, #26112, #59556, .T. ) ;
#23164 = CARTESIAN_POINT ( 'NONE',  ( -2.229367062500000163, -77.47916666530106511, -3.861377020970580443 ) ) ;
#23165 = CARTESIAN_POINT ( 'NONE',  ( -6.972266317189433020E-16, -31.12499999726880873, -5.000000000000000000 ) ) ;
#23166 = CARTESIAN_POINT ( 'NONE',  ( 5.000000000000000000, -11.37499999726881583, -6.123233995736766282E-16 ) ) ;
#23168 = ORIENTED_EDGE ( 'NONE', *, *, #52386, .F. ) ;
#23167 = CARTESIAN_POINT ( 'NONE',  ( -2.229367062499996610, -43.14583333196773651, 3.861377020970582219 ) ) ;
#23169 = CARTESIAN_POINT ( 'NONE',  ( 5.000000000000000000, -81.41666666666667140, -2.886751345948130876 ) ) ;
#23171 = ORIENTED_EDGE ( 'NONE', *, *, #1265, .F. ) ;
#23170 = CARTESIAN_POINT ( 'NONE',  ( -2.229367062499996610, 4.604166668032261711, 3.861377020970582219 ) ) ;
#23172 = CARTESIAN_POINT ( 'NONE',  ( -5.000000000000000000, -63.08333333333332860, -2.886751345948128211 ) ) ;
#23173 = CARTESIAN_POINT ( 'NONE',  ( -1.846868145590737420, -159.0000000013656063, 4.458734124999999437 ) ) ;
#23174 = CARTESIAN_POINT ( 'NONE',  ( 2.229367062499998831, -36.89583333196773651, -3.861377020970580887 ) ) ;
#23175 = CARTESIAN_POINT ( 'NONE',  ( -49.85088928181150436, -149.6875000027311842, -1.666127454062680480 ) ) ;
#23176 =( BOUNDED_CURVE ( )  B_SPLINE_CURVE ( 2, ( #5815, #45372, #35727, #55356, #15788, #46008, #55989, #41486, #60817 ),
 .UNSPECIFIED., .F., .F. ) 
 B_SPLINE_CURVE_WITH_KNOTS ( ( 3, 2, 2, 2, 3 ),
 ( 0.5812500000000000444, 0.5819444444444444864, 0.5833333333333333703, 0.5847222222222222543, 0.5854166666666666963 ),
 .UNSPECIFIED. ) 
 CURVE ( )  GEOMETRIC_REPRESENTATION_ITEM ( )  RATIONAL_B_SPLINE_CURVE ( ( 0.9330127018922194093, 0.9330127018922194093, 1.000000000000000000, 0.8660254037844387076, 1.000000000000000000, 0.8660254037844387076, 1.000000000000000000, 0.9330127018922194093, 0.9330127018922194093 ) ) 
 REPRESENTATION_ITEM ( '' )  );
#23177 = CARTESIAN_POINT ( 'NONE',  ( 3.061616997868383141E-16, -165.7500000000000000, -5.000000000000000000 ) ) ;
#23178 = EDGE_CURVE ( 'NONE', #1738, #31328, #8443, .T. ) ;
#23179 = LINE ( 'NONE', #42789, #32336 ) ;
#23180 = CARTESIAN_POINT ( 'NONE',  ( -56.48576386720575471, -132.0000000013656063, -4.591703134518078322 ) ) ;
#23181 = CARTESIAN_POINT ( 'NONE',  ( 4.458734125000001214, -7.145833331967734736, 2.574251347313718519 ) ) ;
#23182 = CARTESIAN_POINT ( 'NONE',  ( 2.229367062499998831, -42.89583333196773651, -3.861377020970580887 ) ) ;
#23183 = CARTESIAN_POINT ( 'NONE',  ( 5.000000000000000000, -67.29166666393547303, -2.886751345948130876 ) ) ;
#23184 = ADVANCED_FACE ( 'NONE', ( #10647 ), #45067, .T. ) ;
#23185 = CARTESIAN_POINT ( 'NONE',  ( -3.152548672688508926E-16, -85.81249999863440792, -5.148502694627439702 ) ) ;
#23186 = CARTESIAN_POINT ( 'NONE',  ( 2.500000000000002220, 8.333333333333332149, 4.330127018922192761 ) ) ;
#23187 = EDGE_LOOP ( 'NONE', ( #51600, #33626, #35064, #61017 ) ) ;
#23188 = CARTESIAN_POINT ( 'NONE',  ( -50.18089887299979068, -152.8125000027311842, 2.462841084822635640 ) ) ;
#23189 = CARTESIAN_POINT ( 'NONE',  ( -6.972266317189433020E-16, -43.25000000000000000, -5.000000000000000000 ) ) ;
#23190 = CARTESIAN_POINT ( 'NONE',  ( -4.458734124999999437, -69.56249999863439371, 0.000000000000000000 ) ) ;
#23191 = CARTESIAN_POINT ( 'NONE',  ( -4.458734124999999437, -148.1875000013656063, -5.460374474430324690E-16 ) ) ;
#23192 = ORIENTED_EDGE ( 'NONE', *, *, #39697, .T. ) ;
#23193 = CARTESIAN_POINT ( 'NONE',  ( -4.999999999999998224, -1.916666666666663854, 2.886751345948131764 ) ) ;
#23194 = CARTESIAN_POINT ( 'NONE',  ( 4.458734124999999437, -11.06249999863440792, -5.460374474430324690E-16 ) ) ;
#23195 = CARTESIAN_POINT ( 'NONE',  ( -51.19402409849444524, -150.6250000027312126, -3.242614290531456334 ) ) ;
#23196 = CARTESIAN_POINT ( 'NONE',  ( 4.458734124999998549, 2.270833334698928230, -2.574251347313721627 ) ) ;
#23197 = CARTESIAN_POINT ( 'NONE',  ( 2.499999999999998668, -77.20833333060214443, -4.330127018922193649 ) ) ;
#23198 = CARTESIAN_POINT ( 'NONE',  ( -1.846868145590737420, -154.7500000013656063, 4.458734124999997661 ) ) ;
#23199 = CARTESIAN_POINT ( 'NONE',  ( -4.458734124999997661, 24.52083333469892779, 2.574251347313722516 ) ) ;
#23200 = ORIENTED_EDGE ( 'NONE', *, *, #33487, .T. ) ;
#23201 = CARTESIAN_POINT ( 'NONE',  ( 9.457646018065525792E-16, -93.06249999863440792, 5.148502694627439702 ) ) ;
#23202 = CARTESIAN_POINT ( 'NONE',  ( -4.999999999999998224, -30.91666666666667140, 2.886751345948131764 ) ) ;
#23203 = CARTESIAN_POINT ( 'NONE',  ( 2.499999999999998668, -63.33333333333332149, -4.330127018922193649 ) ) ;
#23204 = CARTESIAN_POINT ( 'NONE',  ( 9.457646018065525792E-16, -7.062499998634404363, 5.148502694627439702 ) ) ;
#23205 = ADVANCED_FACE ( 'NONE', ( #30587 ), #55040, .T. ) ;
#23206 = CARTESIAN_POINT ( 'NONE',  ( -6.972266317189433020E-16, -34.25000000000000000, -5.000000000000000000 ) ) ;
#23207 = CARTESIAN_POINT ( 'NONE',  ( 2.500000000000002220, -23.54166666393548368, 4.330127018922192761 ) ) ;
#23208 = CARTESIAN_POINT ( 'NONE',  ( 2.499999999999998668, -87.33333333333332860, -4.330127018922193649 ) ) ;
#23209 = CARTESIAN_POINT ( 'NONE',  ( 2.500000000000002220, -36.54166666393547303, 4.330127018922192761 ) ) ;
#23210 = CARTESIAN_POINT ( 'NONE',  ( 1.339745962155615144, -64.58034179853029855, 4.999999999999999112 ) ) ;
#23211 = CARTESIAN_POINT ( 'NONE',  ( -4.458734124999999437, 18.60416666803225993, -2.574251347313719407 ) ) ;
#23212 = CARTESIAN_POINT ( 'NONE',  ( 5.000000000000000888, -10.58333333333333393, 2.886751345948126879 ) ) ;
#23213 = EDGE_CURVE ( 'NONE', #4881, #23583, #34333, .T. ) ;
#23214 = CARTESIAN_POINT ( 'NONE',  ( -2.229367062499996610, 23.85416666803225993, 3.861377020970582219 ) ) ;
#23215 = CARTESIAN_POINT ( 'NONE',  ( 2.229367062500001939, -57.97916666530107932, 3.861377020970579999 ) ) ;
#23216 = CARTESIAN_POINT ( 'NONE',  ( 4.458734124999998549, -4.979166665301071326, -2.574251347313721627 ) ) ;
#23217 = CARTESIAN_POINT ( 'NONE',  ( 1.975475456537005874E-15, -105.6249999972688016, 5.000000000000000000 ) ) ;
#23218 = CARTESIAN_POINT ( 'NONE',  ( 5.000000000000000000, 7.500000000000000000, -6.123233995736766282E-16 ) ) ;
#23219 = CARTESIAN_POINT ( 'NONE',  ( -5.000000000000000888, -139.6875000027312126, -2.071067811865475949 ) ) ;
#23220 = CARTESIAN_POINT ( 'NONE',  ( -1.049326080737009628E-13, -20.62499999726881583, 5.000000000000000000 ) ) ;
#23221 = CARTESIAN_POINT ( 'NONE',  ( -2.229367062500000163, -48.47916666530106511, -3.861377020970580443 ) ) ;
#23222 = CARTESIAN_POINT ( 'NONE',  ( 2.499999999999998668, -86.20833333060214443, -4.330127018922193649 ) ) ;
#23223 = CARTESIAN_POINT ( 'NONE',  ( -54.64476657466781973, -136.0625000013656063, -4.444560631937228834 ) ) ;
#23224 = CARTESIAN_POINT ( 'NONE',  ( -1.230605004983934782E-13, -37.62499999726881583, 5.000000000000000000 ) ) ;
#23225 = LINE ( 'NONE', #13882, #34654 ) ;
#23226 = CARTESIAN_POINT ( 'NONE',  ( -2.229367062499996610, -90.39583333196773651, 3.861377020970582219 ) ) ;
#23227 = CARTESIAN_POINT ( 'NONE',  ( 3.152801135295366208, -157.8125000013656063, 3.152801135295367985 ) ) ;
#23228 = CARTESIAN_POINT ( 'NONE',  ( -5.000000000000000000, -37.99999999999999289, 0.000000000000000000 ) ) ;
#23229 = SURFACE_STYLE_USAGE ( .BOTH. , #18711 ) ;
#23230 = VERTEX_POINT ( 'NONE', #16116 ) ;
#23231 = CARTESIAN_POINT ( 'NONE',  ( -4.458734124999999437, 19.35416666803225993, -2.574251347313719407 ) ) ;
#23232 = ORIENTED_EDGE ( 'NONE', *, *, #20051, .T. ) ;
#23233 = CARTESIAN_POINT ( 'NONE',  ( -4.458734124999999437, -96.31249999863440792, 0.000000000000000000 ) ) ;
#23234 = CARTESIAN_POINT ( 'NONE',  ( 4.458734124999999437, 9.937500001365593860, -5.460374474430324690E-16 ) ) ;
#23235 = CARTESIAN_POINT ( 'NONE',  ( 5.000000000000000000, 9.708333336064519870, -2.886751345948129988 ) ) ;
#23236 = AXIS2_PLACEMENT_3D ( 'NONE', #33569, #8810, #52567 ) ;
#23237 = CARTESIAN_POINT ( 'NONE',  ( -5.000000000000000000, 0.9166666666666664076, -2.886751345948128211 ) ) ;
#23238 = AXIS2_PLACEMENT_3D ( 'NONE', #44713, #40219, #6136 ) ;
#23239 = CARTESIAN_POINT ( 'NONE',  ( 2.229367062499998831, -63.64583333196772941, -3.861377020970580887 ) ) ;
#23240 = VECTOR ( 'NONE', #33639, 1000.000000000000000 ) ;
#23241 = CARTESIAN_POINT ( 'NONE',  ( 5.000000000000000000, -61.37499999726880873, -6.123233995736766282E-16 ) ) ;
#23242 = EDGE_CURVE ( 'NONE', #12417, #26245, #40556, .T. ) ;
#23243 = EDGE_CURVE ( 'NONE', #56096, #44174, #47863, .T. ) ;
#23244 = CARTESIAN_POINT ( 'NONE',  ( 4.458734124999999437, -29.81249999863440436, -5.460374474430324690E-16 ) ) ;
#23245 = CYLINDRICAL_SURFACE ( 'NONE', #20427, 5.000000000000000000 ) ;
#23246 = CYLINDRICAL_SURFACE ( 'NONE', #10748, 5.000000000000000000 ) ;
#23247 = ADVANCED_FACE ( 'NONE', ( #51181 ), #27666, .T. ) ;
#23248 = CARTESIAN_POINT ( 'NONE',  ( 0.000000000000000000, -120.0000000000000000, 0.000000000000000000 ) ) ;
#23249 = CARTESIAN_POINT ( 'NONE',  ( 2.500000000000002220, -44.66666666666665719, 4.330127018922192761 ) ) ;
#23250 = LINE ( 'NONE', #58831, #18135 ) ;
#23252 = CARTESIAN_POINT ( 'NONE',  ( -4.458734124999999437, -18.64583333196774007, -2.574251347313719407 ) ) ;
#23251 = CARTESIAN_POINT ( 'NONE',  ( -2.500000000000000444, -45.16666666666665719, -4.330127018922193649 ) ) ;
#23253 = CARTESIAN_POINT ( 'NONE',  ( 5.000000000000000000, -4.374999997268816720, -6.123233995736766282E-16 ) ) ;
#23254 = CARTESIAN_POINT ( 'NONE',  ( 4.458734125000001214, -63.89583333196772941, 2.574251347313718519 ) ) ;
#23255 = CARTESIAN_POINT ( 'NONE',  ( -8.190561711645485556E-16, -146.9375000013656063, 4.458734124999999437 ) ) ;
#23256 = APPLICATION_CONTEXT ( 'automotive_design' ) ;
#23257 = CARTESIAN_POINT ( 'NONE',  ( -4.458734124999999437, -75.31249999863440792, 0.000000000000000000 ) ) ;
#23258 = CARTESIAN_POINT ( 'NONE',  ( -50.70258187064364108, -142.3750000013656063, 2.196230717870141014 ) ) ;
#23259 = EDGE_CURVE ( 'NONE', #63455, #58748, #30896, .T. ) ;
#23260 =( BOUNDED_CURVE ( )  B_SPLINE_CURVE ( 2, ( #55551, #36233, #61006, #26906, #12099, #7295, #40729, #26256, #21447 ),
 .UNSPECIFIED., .F., .F. ) 
 B_SPLINE_CURVE_WITH_KNOTS ( ( 3, 2, 2, 2, 3 ),
 ( 0.7479166666666666741, 0.7486111111111111160, 0.7500000000000000000, 0.7513888888888888840, 0.7520833333333333259 ),
 .UNSPECIFIED. ) 
 CURVE ( )  GEOMETRIC_REPRESENTATION_ITEM ( )  RATIONAL_B_SPLINE_CURVE ( ( 0.9330127018922194093, 0.9330127018922194093, 1.000000000000000000, 0.8660254037844387076, 1.000000000000000000, 0.8660254037844387076, 1.000000000000000000, 0.9330127018922194093, 0.9330127018922194093 ) ) 
 REPRESENTATION_ITEM ( '' )  );
#23261 = CARTESIAN_POINT ( 'NONE',  ( 4.458734125000001214, -27.14583333196774717, 2.574251347313718519 ) ) ;
#23262 = CARTESIAN_POINT ( 'NONE',  ( -5.000000000000000000, -64.87499999726881583, 0.000000000000000000 ) ) ;
#23263 = ORIENTED_EDGE ( 'NONE', *, *, #814, .T. ) ;
#23264 = CARTESIAN_POINT ( 'NONE',  ( 3.061616997868383141E-16, -152.8750000027311842, -5.000000000000000000 ) ) ;
#23266 = ORIENTED_EDGE ( 'NONE', *, *, #29190, .T. ) ;
#23265 = ADVANCED_FACE ( 'NONE', ( #61152 ), #27348, .T. ) ;
#23267 = CARTESIAN_POINT ( 'NONE',  ( -4.458734124999999437, -65.56249999863440792, 0.000000000000000000 ) ) ;
#23268 = DIRECTION ( 'NONE',  ( -0.000000000000000000, 1.000000000000000000, -0.000000000000000000 ) ) ;
#23269 = LINE ( 'NONE', #38057, #39968 ) ;
#23270 = VERTEX_POINT ( 'NONE', #56643 ) ;
#23271 = EDGE_CURVE ( 'NONE', #454, #24668, #17077, .T. ) ;
#23272 = CARTESIAN_POINT ( 'NONE',  ( 1.975475456537005874E-15, -25.75000000000000355, 5.000000000000000000 ) ) ;
#23273 = CARTESIAN_POINT ( 'NONE',  ( 2.229367062499998831, -53.89583333196773651, -3.861377020970580887 ) ) ;
#23274 = CARTESIAN_POINT ( 'NONE',  ( 2.229367062499998831, 1.104166668032261711, -3.861377020970580887 ) ) ;
#23275 = ORIENTED_EDGE ( 'NONE', *, *, #57116, .T. ) ;
#23276 =( BOUNDED_CURVE ( )  B_SPLINE_CURVE ( 2, ( #46982, #37322, #32815, #21587, #16756, #36372, #9617, #4479, #27979 ),
 .UNSPECIFIED., .F., .F. ) 
 B_SPLINE_CURVE_WITH_KNOTS ( ( 3, 2, 2, 2, 3 ),
 ( 0.9854166666666667185, 0.9861111111111111605, 0.9875000000000000444, 0.9888888888888889284, 0.9895833333333333703 ),
 .UNSPECIFIED. ) 
 CURVE ( )  GEOMETRIC_REPRESENTATION_ITEM ( )  RATIONAL_B_SPLINE_CURVE ( ( 0.9330127018922194093, 0.9330127018922194093, 1.000000000000000000, 0.8660254037844387076, 1.000000000000000000, 0.8660254037844387076, 1.000000000000000000, 0.9330127018922194093, 0.9330127018922194093 ) ) 
 REPRESENTATION_ITEM ( '' )  );
#23277 = DIRECTION ( 'NONE',  ( -0.000000000000000000, 1.000000000000000000, -0.000000000000000000 ) ) ;
#23278 = CARTESIAN_POINT ( 'NONE',  ( 9.457646018065525792E-16, 4.937500001365596525, 5.148502694627439702 ) ) ;
#23279 = CARTESIAN_POINT ( 'NONE',  ( 4.458734124999998549, 20.27083333469892779, -2.574251347313721627 ) ) ;
#23280 = CARTESIAN_POINT ( 'NONE',  ( -52.10840900171896806, -143.1875000013656063, 3.393966926194110556 ) ) ;
#23281 = DIRECTION ( 'NONE',  ( -0.000000000000000000, 1.000000000000000000, -0.000000000000000000 ) ) ;
#23282 = CARTESIAN_POINT ( 'NONE',  ( 3.152801135295367541, -167.3125000013656063, -3.152801135295367541 ) ) ;
#23283 = VECTOR ( 'NONE', #13240, 1000.000000000000000 ) ;
#23284 = EDGE_LOOP ( 'NONE', ( #10477, #55278, #46197, #58005 ) ) ;
#23285 = CARTESIAN_POINT ( 'NONE',  ( -3.152548672688508926E-16, -73.56249999863439371, -5.148502694627439702 ) ) ;
#23286 = CARTESIAN_POINT ( 'NONE',  ( -4.999999999999998224, -85.79166666393547303, 2.886751345948131764 ) ) ;
#23287 = CARTESIAN_POINT ( 'NONE',  ( -4.458734124999999437, 4.687500001365595637, 0.000000000000000000 ) ) ;
#23288 = VECTOR ( 'NONE', #16603, 1000.000000000000000 ) ;
#23289 = AXIS2_PLACEMENT_3D ( 'NONE', #57703, #47409, #48032 ) ;
#23290 = CARTESIAN_POINT ( 'NONE',  ( 1.975475456537005874E-15, -69.62499999726880162, 5.000000000000000000 ) ) ;
#23291 = CARTESIAN_POINT ( 'NONE',  ( -4.458734124999999437, -60.64583333196774362, -2.574251347313719407 ) ) ;
#23292 = CARTESIAN_POINT ( 'NONE',  ( 2.500000000000002220, -18.54166666393547658, 4.330127018922192761 ) ) ;
#23293 = CARTESIAN_POINT ( 'NONE',  ( 2.499999999999998668, -20.33333333333333570, -4.330127018922193649 ) ) ;
#23294 = CARTESIAN_POINT ( 'NONE',  ( 5.000000000000000888, -42.45833333060214443, 2.886751345948126879 ) ) ;
#23295 = CARTESIAN_POINT ( 'NONE',  ( 5.000000000000000888, -76.58333333333335702, 2.886751345948126879 ) ) ;
#23296 = CARTESIAN_POINT ( 'NONE',  ( -5.000000000000000000, -156.5000000000000000, -6.123233995736766282E-16 ) ) ;
#23297 = CARTESIAN_POINT ( 'NONE',  ( -6.972266317189433020E-16, -89.12499999726880162, -5.000000000000000000 ) ) ;
#23298 = CARTESIAN_POINT ( 'NONE',  ( 4.458734125000001214, -38.89583333196773651, 2.574251347313718519 ) ) ;
#23299 = CARTESIAN_POINT ( 'NONE',  ( 4.458734124999999437, -25.06249999863440792, -5.460374474430324690E-16 ) ) ;
#23300 = CARTESIAN_POINT ( 'NONE',  ( 5.000000000000000000, 11.58333333333333393, -2.886751345948130876 ) ) ;
#23301 = CARTESIAN_POINT ( 'NONE',  ( -4.999999999999999112, 28.08333333333333570, 2.886751345948131764 ) ) ;
#23302 = CARTESIAN_POINT ( 'NONE',  ( -5.000000000000000000, -152.6250000027312126, -6.123233995736766282E-16 ) ) ;
#23303 = VERTEX_POINT ( 'NONE', #17074 ) ;
#23304 = CARTESIAN_POINT ( 'NONE',  ( -4.458734124999999437, -110.5624999986343937, 0.000000000000000000 ) ) ;
#23305 = CARTESIAN_POINT ( 'NONE',  ( -2.229367062499996610, -33.14583333196772941, 3.861377020970582219 ) ) ;
#23306 = CARTESIAN_POINT ( 'NONE',  ( 5.000000000000000000, -70.37499999726880162, -6.123233995736766282E-16 ) ) ;
#23307 = CARTESIAN_POINT ( 'NONE',  ( -51.60603307380591787, -146.1875000013656063, -2.891590998281053704 ) ) ;
#23308 = CARTESIAN_POINT ( 'NONE',  ( 5.000000000000000000, -143.0000000000000284, 0.000000000000000000 ) ) ;
#23309 = ADVANCED_BREP_SHAPE_REPRESENTATION ( '', ( #50626, #43054 ), #29681 ) ;
#23310 = CARTESIAN_POINT ( 'NONE',  ( 4.458734125000000326, -27.89583333196774007, 2.574251347313718519 ) ) ;
#23311 = CARTESIAN_POINT ( 'NONE',  ( -3.152548672688508926E-16, -74.81249999863439371, -5.148502694627439702 ) ) ;
#23312 = CARTESIAN_POINT ( 'NONE',  ( 1.464175926609780648E-14, 22.74999999999999645, -5.000000000000000000 ) ) ;
#23314 = CARTESIAN_POINT ( 'NONE',  ( -2.229367062499996610, -30.14583333196773651, 3.861377020970582219 ) ) ;
#23313 = PRODUCT_RELATED_PRODUCT_CATEGORY ( 'part', '', ( #19399 ) ) ;
#23315 = CARTESIAN_POINT ( 'NONE',  ( -55.39835681537999790, -147.8750000000000284, 4.984105922594378235 ) ) ;
#23316 = CARTESIAN_POINT ( 'NONE',  ( 2.500000000000002220, -5.541666663935480130, 4.330127018922192761 ) ) ;
#23317 = CARTESIAN_POINT ( 'NONE',  ( 2.499999999999998668, -19.33333333333333570, -4.330127018922193649 ) ) ;
#23318 = CARTESIAN_POINT ( 'NONE',  ( 3.152801135295367541, -147.3125000013655779, -3.152801135295367541 ) ) ;
#23319 = ORIENTED_EDGE ( 'NONE', *, *, #23242, .F. ) ;
#23320 = CARTESIAN_POINT ( 'NONE',  ( 0.000000000000000000, -170.0000000000000000, 0.000000000000000000 ) ) ;
#23321 = CARTESIAN_POINT ( 'NONE',  ( 4.458734124999998549, -57.97916666530107932, -2.574251347313721627 ) ) ;
#23322 = CARTESIAN_POINT ( 'NONE',  ( -4.999999999999999112, 25.20833333606451987, 2.886751345948131764 ) ) ;
#23323 = CARTESIAN_POINT ( 'NONE',  ( 1.975475456537005874E-15, -110.6249999972688158, 5.000000000000000000 ) ) ;
#23324 = CARTESIAN_POINT ( 'NONE',  ( -5.000000000000000000, 18.00000000000000000, 0.000000000000000000 ) ) ;
#23325 = CYLINDRICAL_SURFACE ( 'NONE', #35588, 5.000000000000000000 ) ;
#23326 = CARTESIAN_POINT ( 'NONE',  ( 9.457646018065525792E-16, -0.06249999863440491854, 5.148502694627439702 ) ) ;
#23327 = CARTESIAN_POINT ( 'NONE',  ( -1.339745962155613812, -52.08034179853028434, -5.000000000000000000 ) ) ;
#23328 = EDGE_CURVE ( 'NONE', #26895, #48046, #34723, .T. ) ;
#23329 = CARTESIAN_POINT ( 'NONE',  ( -1.339745962155610925, -80.66965819600734733, 5.000000000000000000 ) ) ;
#23330 = CARTESIAN_POINT ( 'NONE',  ( -4.458734124999999437, 11.43750000136559564, 0.000000000000000000 ) ) ;
#23331 = CARTESIAN_POINT ( 'NONE',  ( 2.499999999999998668, -12.33333333333333570, -4.330127018922193649 ) ) ;
#23332 = ORIENTED_EDGE ( 'NONE', *, *, #30448, .T. ) ;
#23333 =( BOUNDED_CURVE ( )  B_SPLINE_CURVE ( 2, ( #42858, #44028, #49186, #63358, #20239, #45168, #19595, #4802, #19274 ),
 .UNSPECIFIED., .F., .F. ) 
 B_SPLINE_CURVE_WITH_KNOTS ( ( 3, 2, 2, 2, 3 ),
 ( 0.1732142857142857095, 0.1738095238095238027, 0.1749999999999999889, 0.1761904761904762029, 0.1767857142857142960 ),
 .UNSPECIFIED. ) 
 CURVE ( )  GEOMETRIC_REPRESENTATION_ITEM ( )  RATIONAL_B_SPLINE_CURVE ( ( 0.9330127018922194093, 0.9330127018922194093, 1.000000000000000000, 0.8660254037844387076, 1.000000000000000000, 0.8660254037844387076, 1.000000000000000000, 0.9330127018922194093, 0.9330127018922194093 ) ) 
 REPRESENTATION_ITEM ( '' )  );
#23334 = VECTOR ( 'NONE', #5572, 1000.000000000000000 ) ;
#23335 = CARTESIAN_POINT ( 'NONE',  ( 1.975475456537005874E-15, -23.62499999726880873, 5.000000000000000000 ) ) ;
#23336 = CARTESIAN_POINT ( 'NONE',  ( -4.458734124999999437, -46.31249999863440792, 0.000000000000000000 ) ) ;
#23337 = CARTESIAN_POINT ( 'NONE',  ( 4.458734124999999437, -158.7500000013656063, 1.846868145590737864 ) ) ;
#23338 = AXIS2_PLACEMENT_3D ( 'NONE', #56395, #46415, #25840 ) ;
#23339 = AXIS2_PLACEMENT_3D ( 'NONE', #61119, #23130, #2898 ) ;
#23340 = CARTESIAN_POINT ( 'NONE',  ( -4.999999999999999112, -51.79166666393548013, 2.886751345948131764 ) ) ;
#23341 = ORIENTED_EDGE ( 'NONE', *, *, #32775, .F. ) ;
#23342 = VECTOR ( 'NONE', #355, 1000.000000000000000 ) ;
#23343 = CARTESIAN_POINT ( 'NONE',  ( 4.458734124999998549, -22.72916666530107221, -2.574251347313721627 ) ) ;
#23344 = ORIENTED_EDGE ( 'NONE', *, *, #50061, .F. ) ;
#23346 = CARTESIAN_POINT ( 'NONE',  ( 1.975475456537005874E-15, -53.74999999999999289, 5.000000000000000000 ) ) ;
#23345 = CARTESIAN_POINT ( 'NONE',  ( 1.339745962155615144, -34.70534180126148271, 4.999999999999999112 ) ) ;
#23347 = CARTESIAN_POINT ( 'NONE',  ( -8.190561711645485556E-16, -160.6875000013655779, 4.458734124999999437 ) ) ;
#23348 = EDGE_CURVE ( 'NONE', #46264, #57843, #12873, .T. ) ;
#23349 = EDGE_CURVE ( 'NONE', #54895, #61565, #45432, .T. ) ;
#23350 = LINE ( 'NONE', #8238, #55011 ) ;
#23351 = CARTESIAN_POINT ( 'NONE',  ( -55.39835681537999790, -134.8750000000000284, 4.984105922594378235 ) ) ;
#23352 = CARTESIAN_POINT ( 'NONE',  ( 4.458734124999999437, -39.06249999863440081, -5.460374474430324690E-16 ) ) ;
#23353 = EDGE_LOOP ( 'NONE', ( #8474, #24793, #36540, #48080 ) ) ;
#23354 = ADVANCED_FACE ( 'NONE', ( #61780 ), #41499, .T. ) ;
#23355 = CARTESIAN_POINT ( 'NONE',  ( 2.229367062499998831, -81.64583333196773651, -3.861377020970580887 ) ) ;
#23356 = CARTESIAN_POINT ( 'NONE',  ( -4.458734124999999437, 20.60416666803225993, -2.574251347313719407 ) ) ;
#23357 = CARTESIAN_POINT ( 'NONE',  ( 1.975475456537005874E-15, -24.62499999726881583, 5.000000000000000000 ) ) ;
#23358 = ORIENTED_EDGE ( 'NONE', *, *, #10968, .T. ) ;
#23359 = CARTESIAN_POINT ( 'NONE',  ( -50.70258187064364108, -140.3750000013656063, 2.196230717870141014 ) ) ;
#23360 = CARTESIAN_POINT ( 'NONE',  ( 4.458734124999998549, -83.97916666530107932, -2.574251347313721627 ) ) ;
#23361 = CARTESIAN_POINT ( 'NONE',  ( -58.24261429053147765, -126.3750000027312126, -3.805975901505573855 ) ) ;
#23362 = CARTESIAN_POINT ( 'NONE',  ( 5.000000000000000000, -35.37499999726881583, -6.123233995736766282E-16 ) ) ;
#23363 = CARTESIAN_POINT ( 'NONE',  ( -3.535533905932737309, -158.7500000027312126, -3.535533905932738197 ) ) ;
#23364 =( BOUNDED_CURVE ( )  B_SPLINE_CURVE ( 2, ( #2145, #21750, #41345, #12082, #25923, #35580, #51339, #60033, #30751 ),
 .UNSPECIFIED., .F., .F. ) 
 B_SPLINE_CURVE_WITH_KNOTS ( ( 3, 2, 2, 2, 3 ),
 ( 0.5854166666666666963, 0.5861111111111111382, 0.5875000000000000222, 0.5888888888888889062, 0.5895833333333333481 ),
 .UNSPECIFIED. ) 
 CURVE ( )  GEOMETRIC_REPRESENTATION_ITEM ( )  RATIONAL_B_SPLINE_CURVE ( ( 0.9330127018922194093, 0.9330127018922194093, 1.000000000000000000, 0.8660254037844387076, 1.000000000000000000, 0.8660254037844387076, 1.000000000000000000, 0.9330127018922194093, 0.9330127018922194093 ) ) 
 REPRESENTATION_ITEM ( '' )  );
#23365 = CARTESIAN_POINT ( 'NONE',  ( 1.339745962155615144, -57.70534180126147561, 4.999999999999999112 ) ) ;
#23366 = CARTESIAN_POINT ( 'NONE',  ( -2.229367062499996610, -58.14583333196773651, 3.861377020970582219 ) ) ;
#23367 = CARTESIAN_POINT ( 'NONE',  ( 2.500000000000002220, -37.66666666666666430, 4.330127018922192761 ) ) ;
#23368 = CARTESIAN_POINT ( 'NONE',  ( -4.458734124999999437, 25.60416666803225993, -2.574251347313719407 ) ) ;
#23369 = DIRECTION ( 'NONE',  ( -0.6485228581062915110, 0.000000000000000000, -0.7611951803011149931 ) ) ;
#23370 = CARTESIAN_POINT ( 'NONE',  ( -6.972266317189433020E-16, -18.12499999726881228, -5.000000000000000000 ) ) ;
#23371 = CARTESIAN_POINT ( 'NONE',  ( 4.458734124999999437, -43.06249999863440081, -5.460374474430324690E-16 ) ) ;
#23372 = CARTESIAN_POINT ( 'NONE',  ( -5.000000000000000000, -3.958333330602147537, -2.886751345948128211 ) ) ;
#23373 = CARTESIAN_POINT ( 'NONE',  ( 1.975475456537005874E-15, -31.75000000000000000, 5.000000000000000000 ) ) ;
#23374 = CARTESIAN_POINT ( 'NONE',  ( -59.44456063193725015, -125.5625000013655921, -0.3552334253322034230 ) ) ;
#23375 = CARTESIAN_POINT ( 'NONE',  ( -2.229367062500000163, -82.72916666530106511, -3.861377020970580443 ) ) ;
#23376 = CARTESIAN_POINT ( 'NONE',  ( 2.229367062500001939, -104.9791666653010651, 3.861377020970579999 ) ) ;
#23377 = CARTESIAN_POINT ( 'NONE',  ( -2.229367062500000163, -10.72916666530106866, -3.861377020970580443 ) ) ;
#23378 = ORIENTED_EDGE ( 'NONE', *, *, #15239, .T. ) ;
#23379 = AXIS2_PLACEMENT_3D ( 'NONE', #10224, #58482, #39799 ) ;
#23380 = CARTESIAN_POINT ( 'NONE',  ( -6.972266317189433020E-16, -52.25000000000000711, -5.000000000000000000 ) ) ;
#23381 = CARTESIAN_POINT ( 'NONE',  ( 2.229367062500001939, -92.97916666530106511, 3.861377020970579999 ) ) ;
#23382 = CARTESIAN_POINT ( 'NONE',  ( 5.000000000000000000, -165.1250000027311842, 0.000000000000000000 ) ) ;
#23383 = CARTESIAN_POINT ( 'NONE',  ( 2.229367062500001939, -90.22916666530106511, 3.861377020970579999 ) ) ;
#23384 = VECTOR ( 'NONE', #41246, 1000.000000000000000 ) ;
#23385 = CARTESIAN_POINT ( 'NONE',  ( -2.500000000000000444, -51.04166666393547303, -4.330127018922193649 ) ) ;
#23386 = COLOUR_RGB ( '',0.8941176470588234615, 0.8941176470588234615, 0.8941176470588234615 ) ;
#23387 = CARTESIAN_POINT ( 'NONE',  ( -52.80376928212989185, -127.8750000013656063, -4.297418129356379346 ) ) ;
#23388 = CARTESIAN_POINT ( 'NONE',  ( 4.458734124999999437, -11.81249999863440081, -5.460374474430324690E-16 ) ) ;
#23389 = CARTESIAN_POINT ( 'NONE',  ( 9.457646018065525792E-16, 11.68750000136559564, 5.148502694627439702 ) ) ;
#23390 = CARTESIAN_POINT ( 'NONE',  ( 4.458734124999999437, -53.06249999863440792, -5.460374474430324690E-16 ) ) ;
#23391 = DIRECTION ( 'NONE',  ( 0.000000000000000000, 0.000000000000000000, 1.000000000000000000 ) ) ;
#23392 = CARTESIAN_POINT ( 'NONE',  ( 5.000000000000000000, 17.58333333333333215, -2.886751345948130876 ) ) ;
#23393 = CARTESIAN_POINT ( 'NONE',  ( 9.457646018065525792E-16, -12.06249999863440081, 5.148502694627439702 ) ) ;
#23394 = CARTESIAN_POINT ( 'NONE',  ( 5.000000000000000000, -8.291666663935481907, -2.886751345948130876 ) ) ;
#23395 = ORIENTED_EDGE ( 'NONE', *, *, #39804, .F. ) ;
#23396 = CARTESIAN_POINT ( 'NONE',  ( -4.458734124999999437, -40.64583333196773651, -2.574251347313719407 ) ) ;
#23397 = CARTESIAN_POINT ( 'NONE',  ( 2.500000000000002220, -77.66666666666665719, 4.330127018922192761 ) ) ;
#23398 = CARTESIAN_POINT ( 'NONE',  ( 1.339745962155612702, -68.29465819873851729, -5.000000000000000000 ) ) ;
#23399 = CARTESIAN_POINT ( 'NONE',  ( -2.500000000000000444, -67.04166666393547303, -4.330127018922193649 ) ) ;
#23400 = CARTESIAN_POINT ( 'NONE',  ( -4.458734124999998549, -86.22916666530106511, 2.574251347313722516 ) ) ;
#23401 = CARTESIAN_POINT ( 'NONE',  ( -4.458734124999998549, 23.52083333469892779, 2.574251347313722516 ) ) ;
#23403 = EDGE_CURVE ( 'NONE', #50575, #57905, #23276, .T. ) ;
#23402 = CARTESIAN_POINT ( 'NONE',  ( 4.458734124999999437, 16.18750000136559564, -5.460374474430324690E-16 ) ) ;
#23404 = DIRECTION ( 'NONE',  ( -0.000000000000000000, 1.000000000000000000, -0.000000000000000000 ) ) ;
#23405 = FACE_OUTER_BOUND ( 'NONE', #50963, .T. ) ;
#23406 = CARTESIAN_POINT ( 'NONE',  ( 4.458734124999999437, -89.06249999863439371, -5.460374474430324690E-16 ) ) ;
#23407 = CARTESIAN_POINT ( 'NONE',  ( -5.000000000000000000, -71.00000000000000000, 0.000000000000000000 ) ) ;
#23408 = CARTESIAN_POINT ( 'NONE',  ( 5.000000000000000888, 15.54166666939785024, 2.886751345948126879 ) ) ;
#23409 = ORIENTED_EDGE ( 'NONE', *, *, #38635, .F. ) ;
#23410 = CARTESIAN_POINT ( 'NONE',  ( 5.000000000000000888, -18.45833333060214798, 2.886751345948126879 ) ) ;
#23411 = CARTESIAN_POINT ( 'NONE',  ( -5.000000000000000000, -79.95833333060213022, -2.886751345948128211 ) ) ;
#23413 = CARTESIAN_POINT ( 'NONE',  ( -5.000000000000000000, -31.00000000000000000, 0.000000000000000000 ) ) ;
#23412 = CARTESIAN_POINT ( 'NONE',  ( -75.00000000000002842, 15.00000000000000000, -5.000000000000000000 ) ) ;
#23414 = CARTESIAN_POINT ( 'NONE',  ( -3.152548672688508926E-16, -34.56249999863440792, -5.148502694627439702 ) ) ;
#23415 = CARTESIAN_POINT ( 'NONE',  ( 3.044556291839386294E-14, 18.75000000000000355, -5.000000000000000000 ) ) ;
#23416 = CARTESIAN_POINT ( 'NONE',  ( -5.000000000000000000, -34.95833333060213732, -2.886751345948128211 ) ) ;
#23418 = ORIENTED_EDGE ( 'NONE', *, *, #43916, .T. ) ;
#23417 = CARTESIAN_POINT ( 'NONE',  ( -2.229367062500000163, -62.47916666530106511, -3.861377020970580443 ) ) ;
#23419 = CARTESIAN_POINT ( 'NONE',  ( -59.44456063193725015, -152.8125000013656063, -0.3552334253322034230 ) ) ;
#23421 = ORIENTED_EDGE ( 'NONE', *, *, #17283, .F. ) ;
#23420 = CARTESIAN_POINT ( 'NONE',  ( -2.229367062499996610, -7.395833331967735624, 3.861377020970582219 ) ) ;
#23422 = CARTESIAN_POINT ( 'NONE',  ( 5.000000000000000000, -78.41666666666667140, -2.886751345948129988 ) ) ;
#23423 = CARTESIAN_POINT ( 'NONE',  ( -55.35523342533222291, -136.3125000013656063, 4.444560631937231499 ) ) ;
#23424 = CARTESIAN_POINT ( 'NONE',  ( -2.229367062500000163, -57.72916666530107932, -3.861377020970580443 ) ) ;
#23425 = VECTOR ( 'NONE', #30375, 1000.000000000000000 ) ;
#23426 = CARTESIAN_POINT ( 'NONE',  ( 5.000000000000000888, -76.45833333060215864, 2.886751345948126879 ) ) ;
#23428 = ORIENTED_EDGE ( 'NONE', *, *, #38231, .T. ) ;
#23427 = CARTESIAN_POINT ( 'NONE',  ( 1.975475456537005874E-15, -13.75000000000000000, 5.000000000000000000 ) ) ;
#23429 = CARTESIAN_POINT ( 'NONE',  ( -50.18089887299979068, -150.6875000000000284, 2.462841084822635640 ) ) ;
#23430 = VECTOR ( 'NONE', #27525, 1000.000000000000000 ) ;
#23431 = CARTESIAN_POINT ( 'NONE',  ( 4.458734124999998549, -19.97916666530106866, -2.574251347313721627 ) ) ;
#23433 = ORIENTED_EDGE ( 'NONE', *, *, #17283, .T. ) ;
#23432 = CARTESIAN_POINT ( 'NONE',  ( -2.229367062500000163, -55.72916666530107221, -3.861377020970580443 ) ) ;
#23434 = DIRECTION ( 'NONE',  ( 1.000000000000000000, 0.000000000000000000, 0.000000000000000000 ) ) ;
#23435 = CARTESIAN_POINT ( 'NONE',  ( 3.152801135295367541, -165.5625000013656063, -3.152801135295367541 ) ) ;
#23436 = CARTESIAN_POINT ( 'NONE',  ( 9.457646018065525792E-16, -97.31249999863440792, 5.148502694627439702 ) ) ;
#23437 = CARTESIAN_POINT ( 'NONE',  ( 1.339745962155612702, -50.16965819600732601, -5.000000000000000000 ) ) ;
#23438 = ORIENTED_EDGE ( 'NONE', *, *, #43261, .T. ) ;
#23439 = CARTESIAN_POINT ( 'NONE',  ( -59.59170313451810586, -148.7500000013655779, 1.485763867205729394 ) ) ;
#23440 = CARTESIAN_POINT ( 'NONE',  ( -59.98410592259440222, -140.2500000027312126, -0.3983568153799752487 ) ) ;
#23441 = CARTESIAN_POINT ( 'NONE',  ( 2.499999999999998668, -83.33333333333332860, -4.330127018922193649 ) ) ;
#23442 = CARTESIAN_POINT ( 'NONE',  ( 2.229367062500001939, -9.979166665301068662, 3.861377020970579999 ) ) ;
#23443 = CARTESIAN_POINT ( 'NONE',  ( -4.458734124999997661, -100.4791666653010651, 2.574251347313722516 ) ) ;
#23444 = CARTESIAN_POINT ( 'NONE',  ( -1.846868145590737420, -146.0000000013655779, 4.458734124999999437 ) ) ;
#23445 = CARTESIAN_POINT ( 'NONE',  ( -2.229367062500000163, -25.72916666530106866, -3.861377020970580443 ) ) ;
#23446 = CARTESIAN_POINT ( 'NONE',  ( -58.39396692619412477, -137.4375000013656063, 2.891590998281057701 ) ) ;
#23447 = CARTESIAN_POINT ( 'NONE',  ( -4.458734124999998549, -67.47916666530106511, 2.574251347313722516 ) ) ;
#23448 = CARTESIAN_POINT ( 'NONE',  ( 0.000000000000000000, -120.0000000000000000, 5.000000000000000000 ) ) ;
#23449 = CARTESIAN_POINT ( 'NONE',  ( 4.458734124999999437, -140.3750000013656063, -1.846868145590734978 ) ) ;
#23450 = CARTESIAN_POINT ( 'NONE',  ( -2.229367062499996610, 7.604166668032260823, 3.861377020970582219 ) ) ;
#23451 = EDGE_LOOP ( 'NONE', ( #26323, #59894, #39840, #6092 ) ) ;
#23452 = CARTESIAN_POINT ( 'NONE',  ( -5.000000000000000000, -70.87499999726880162, 0.000000000000000000 ) ) ;
#23453 = CYLINDRICAL_SURFACE ( 'NONE', #38059, 5.000000000000000000 ) ;
#23455 = CARTESIAN_POINT ( 'NONE',  ( 2.229367062499998831, -25.64583333196773651, -3.861377020970580887 ) ) ;
#23454 = CARTESIAN_POINT ( 'NONE',  ( -2.499999999999996447, -91.83333333333334281, 4.330127018922195425 ) ) ;
#23456 = CARTESIAN_POINT ( 'NONE',  ( -6.972266317189433020E-16, 6.875000002731185944, -5.000000000000000000 ) ) ;
#23457 = CARTESIAN_POINT ( 'NONE',  ( -2.229367062499996610, -76.39583333196773651, 3.861377020970582219 ) ) ;
#23458 = EDGE_CURVE ( 'NONE', #7844, #43959, #63350, .T. ) ;
#23459 = CARTESIAN_POINT ( 'NONE',  ( 2.229367062500001939, 20.77083333469892779, 3.861377020970579999 ) ) ;
#23460 = LINE ( 'NONE', #57251, #47883 ) ;
#23461 =( BOUNDED_CURVE ( )  B_SPLINE_CURVE ( 2, ( #13215, #38587, #23814, #37658, #53081, #57299, #32838, #13839, #4201 ),
 .UNSPECIFIED., .F., .F. ) 
 B_SPLINE_CURVE_WITH_KNOTS ( ( 3, 2, 2, 2, 3 ),
 ( 0.4017857142857143016, 0.4023809523809523947, 0.4035714285714285809, 0.4047619047619047672, 0.4053571428571428603 ),
 .UNSPECIFIED. ) 
 CURVE ( )  GEOMETRIC_REPRESENTATION_ITEM ( )  RATIONAL_B_SPLINE_CURVE ( ( 0.9330127018922194093, 0.9330127018922194093, 1.000000000000000000, 0.8660254037844387076, 1.000000000000000000, 0.8660254037844387076, 1.000000000000000000, 0.9330127018922194093, 0.9330127018922194093 ) ) 
 REPRESENTATION_ITEM ( '' )  );
#23462 = CARTESIAN_POINT ( 'NONE',  ( -55.35523342533222291, -140.3125000013656063, 4.444560631937231499 ) ) ;
#23463 = CARTESIAN_POINT ( 'NONE',  ( 4.458734124999999437, 3.187500001365594304, -5.460374474430324690E-16 ) ) ;
#23464 = CARTESIAN_POINT ( 'NONE',  ( -4.458734124999998549, 27.52083333469892779, 2.574251347313722516 ) ) ;
#23465 = CARTESIAN_POINT ( 'NONE',  ( 4.458734124999998549, -39.97916666530107221, -2.574251347313721627 ) ) ;
#23466 = CARTESIAN_POINT ( 'NONE',  ( 0.000000000000000000, -120.0000000000000000, 0.000000000000000000 ) ) ;
#23467 = CARTESIAN_POINT ( 'NONE',  ( 2.229367062499998831, 7.354166668032259935, -3.861377020970580887 ) ) ;
#23468 = CARTESIAN_POINT ( 'NONE',  ( -2.229367062499996610, -22.39583333196773651, 3.861377020970582219 ) ) ;
#23469 = CARTESIAN_POINT ( 'NONE',  ( 4.458734125000000326, -155.3750000013656347, -1.846868145590734978 ) ) ;
#23470 = CARTESIAN_POINT ( 'NONE',  ( 2.229367062499998831, -68.64583333196773651, -3.861377020970580887 ) ) ;
#23471 = CARTESIAN_POINT ( 'NONE',  ( -2.499999999999996447, -99.70833333060214443, 4.330127018922195425 ) ) ;
#23472 = AXIS2_PLACEMENT_3D ( 'NONE', #9546, #29151, #48772 ) ;
#23473 = CARTESIAN_POINT ( 'NONE',  ( -58.24261429053147765, -149.2500000000000284, -3.805975901505573855 ) ) ;
#23474 = CARTESIAN_POINT ( 'NONE',  ( 5.000000000000000000, 9.708333336064519870, -2.886751345948130876 ) ) ;
#23475 = CARTESIAN_POINT ( 'NONE',  ( -2.229367062499996610, -104.3958333319677365, 3.861377020970582219 ) ) ;
#23476 = CARTESIAN_POINT ( 'NONE',  ( -4.458734124999999437, -69.56249999863439371, 0.000000000000000000 ) ) ;
#23477 = CARTESIAN_POINT ( 'NONE',  ( -4.999999999999999112, -55.91666666666667140, 2.886751345948131764 ) ) ;
#23478 = CARTESIAN_POINT ( 'NONE',  ( 1.339745962155615144, -73.70534180126146850, 4.999999999999999112 ) ) ;
#23479 = CARTESIAN_POINT ( 'NONE',  ( 5.000000000000000888, 27.54166666939785557, 2.886751345948126879 ) ) ;
#23480 = VERTEX_POINT ( 'NONE', #24418 ) ;
#23481 = CARTESIAN_POINT ( 'NONE',  ( -1.339745962155601378, 14.91965820146970501, -5.000000000000007105 ) ) ;
#23482 = CARTESIAN_POINT ( 'NONE',  ( -4.999999999999998224, 12.20833333606451632, 2.886751345948131764 ) ) ;
#23483 = CARTESIAN_POINT ( 'NONE',  ( 2.500000000000002220, -12.66666666666666607, 4.330127018922192761 ) ) ;
#23484 = CARTESIAN_POINT ( 'NONE',  ( -4.458734124999999437, -18.39583333196774007, -2.574251347313719407 ) ) ;
#23485 = CARTESIAN_POINT ( 'NONE',  ( 4.458734125000000326, -79.89583333196773651, 2.574251347313718519 ) ) ;
#23486 = AXIS2_PLACEMENT_3D ( 'NONE', #22029, #41621, #4925 ) ;
#23487 = CARTESIAN_POINT ( 'NONE',  ( 1.846868145590735200, -168.5000000013656063, -4.458734125000000326 ) ) ;
#23488 = CARTESIAN_POINT ( 'NONE',  ( 5.000000000000000888, -15.45833333060214265, 2.886751345948126879 ) ) ;
#23490 = ORIENTED_EDGE ( 'NONE', *, *, #9223, .F. ) ;
#23489 = CARTESIAN_POINT ( 'NONE',  ( 4.458734124999999437, -42.81249999863440081, -5.460374474430324690E-16 ) ) ;
#23491 = CARTESIAN_POINT ( 'NONE',  ( -51.75738570946856498, -146.8750000027312126, 3.805975901505576964 ) ) ;
#23493 = VERTEX_POINT ( 'NONE', #33135 ) ;
#23492 = CARTESIAN_POINT ( 'NONE',  ( 4.458734125000001214, 7.854166668032260823, 2.574251347313718519 ) ) ;
#23494 = CARTESIAN_POINT ( 'NONE',  ( -52.80376928212989185, -152.8750000013656063, -4.297418129356378458 ) ) ;
#23495 = CARTESIAN_POINT ( 'NONE',  ( 5.000000000000000000, -61.50000000000000000, -6.123233995736766282E-16 ) ) ;
#23496 = CARTESIAN_POINT ( 'NONE',  ( 1.846868145590736310, -155.8750000013655779, 4.458734124999999437 ) ) ;
#23497 = CARTESIAN_POINT ( 'NONE',  ( -4.458734124999998549, -35.47916666530107221, 2.574251347313722516 ) ) ;
#23498 = CYLINDRICAL_SURFACE ( 'NONE', #58397, 5.000000000000000000 ) ;
#23499 = CARTESIAN_POINT ( 'NONE',  ( -5.000000000000000888, -166.5625000000000000, -2.071067811865475949 ) ) ;
#23500 = CARTESIAN_POINT ( 'NONE',  ( 2.071067811865495045, -168.1875000000000284, 4.999999999999981348 ) ) ;
#23501 = CARTESIAN_POINT ( 'NONE',  ( -50.40829686548195099, -130.2500000013656063, -1.485763867205728284 ) ) ;
#23502 = CARTESIAN_POINT ( 'NONE',  ( 9.457646018065525792E-16, -8.312499998634406140, 5.148502694627439702 ) ) ;
#23503 = CARTESIAN_POINT ( 'NONE',  ( 2.229367062499998831, -38.89583333196773651, -3.861377020970580887 ) ) ;
#23504 = CARTESIAN_POINT ( 'NONE',  ( -6.972266317189433020E-16, -67.12499999726881583, -5.000000000000000000 ) ) ;
#23505 = CARTESIAN_POINT ( 'NONE',  ( -4.458734125000000326, -150.0000000013655779, -1.846868145590735644 ) ) ;
#23506 = CARTESIAN_POINT ( 'NONE',  ( -4.458734124999998549, -81.47916666530106511, 2.574251347313722516 ) ) ;
#23507 =( BOUNDED_CURVE ( )  B_SPLINE_CURVE ( 2, ( #40570, #30922, #50549, #56656, #12264, #37336, #26743, #21916, #7127 ),
 .UNSPECIFIED., .F., .F. ) 
 B_SPLINE_CURVE_WITH_KNOTS ( ( 3, 2, 2, 2, 3 ),
 ( 0.5395833333333333037, 0.5402777777777777457, 0.5416666666666666297, 0.5430555555555555136, 0.5437499999999999556 ),
 .UNSPECIFIED. ) 
 CURVE ( )  GEOMETRIC_REPRESENTATION_ITEM ( )  RATIONAL_B_SPLINE_CURVE ( ( 0.9330127018922194093, 0.9330127018922194093, 1.000000000000000000, 0.8660254037844387076, 1.000000000000000000, 0.8660254037844387076, 1.000000000000000000, 0.9330127018922194093, 0.9330127018922194093 ) ) 
 REPRESENTATION_ITEM ( '' )  );
#23508 = ORIENTED_EDGE ( 'NONE', *, *, #49168, .T. ) ;
#23509 = PRODUCT_DEFINITION_SHAPE ( 'NONE', 'NONE',  #63675 ) ;
#23510 = CARTESIAN_POINT ( 'NONE',  ( -5.000000000000000888, -141.4375000000000284, 2.071067811865474617 ) ) ;
#23511 =( BOUNDED_CURVE ( )  B_SPLINE_CURVE ( 2, ( #43553, #54497, #45796, #26177, #35199, #55459, #25859, #45475, #11689 ),
 .UNSPECIFIED., .F., .F. ) 
 B_SPLINE_CURVE_WITH_KNOTS ( ( 3, 2, 2, 2, 3 ),
 ( 0.6083333333333329485, 0.6124999999999997113, 0.6166666666666663632, 0.6208333333333330151, 0.6249999999999996669 ),
 .UNSPECIFIED. ) 
 CURVE ( )  GEOMETRIC_REPRESENTATION_ITEM ( )  RATIONAL_B_SPLINE_CURVE ( ( 1.000000000000005995, 0.9238795325112806323, 1.000000000000000000, 0.9238795325112867385, 1.000000000000000000, 0.9238795325112867385, 1.000000000000000000, 0.9238795325112928447, 0.9999999999999938938 ) ) 
 REPRESENTATION_ITEM ( '' )  );
#23512 = CARTESIAN_POINT ( 'NONE',  ( -6.972266317189433020E-16, -105.2500000000000000, -5.000000000000000000 ) ) ;
#23513 = CARTESIAN_POINT ( 'NONE',  ( -2.229367062499996610, -70.39583333196773651, 3.861377020970582219 ) ) ;
#23514 = AXIS2_PLACEMENT_3D ( 'NONE', #58544, #54023, #4204 ) ;
#23515 = CARTESIAN_POINT ( 'NONE',  ( 3.152801135295367541, -146.5625000013655779, -3.152801135295367541 ) ) ;
#23516 = ORIENTED_EDGE ( 'NONE', *, *, #4795, .T. ) ;
#23517 = CARTESIAN_POINT ( 'NONE',  ( 5.000000000000000000, -78.50000000000000000, -6.123233995736766282E-16 ) ) ;
#23518 = CARTESIAN_POINT ( 'NONE',  ( -4.458734124999999437, -11.64583333196773829, -2.574251347313719407 ) ) ;
#23519 = CARTESIAN_POINT ( 'NONE',  ( -4.458734124999998549, 1.770833334698927786, 2.574251347313722516 ) ) ;
#23520 = CARTESIAN_POINT ( 'NONE',  ( 5.000000000000000000, -77.37499999726881583, -6.123233995736766282E-16 ) ) ;
#23521 = CARTESIAN_POINT ( 'NONE',  ( 3.152801135295366208, -151.5625000013655779, 3.152801135295367985 ) ) ;
#23522 = CARTESIAN_POINT ( 'NONE',  ( 4.458734124999998549, 25.02083333469892779, -2.574251347313721627 ) ) ;
#23523 = VERTEX_POINT ( 'NONE', #4178 ) ;
#23524 = CARTESIAN_POINT ( 'NONE',  ( -4.458734124999999437, -93.31249999863440792, 0.000000000000000000 ) ) ;
#23525 = CARTESIAN_POINT ( 'NONE',  ( 1.975475456537005874E-15, -74.75000000000000000, 5.000000000000000000 ) ) ;
#23526 = CARTESIAN_POINT ( 'NONE',  ( 1.339745962155615144, -12.58034179853029144, 4.999999999999999112 ) ) ;
#23527 = CARTESIAN_POINT ( 'NONE',  ( 4.458734124999998549, -7.729166665301073103, -2.574251347313721627 ) ) ;
#23528 = EDGE_CURVE ( 'NONE', #14852, #26724, #1885, .T. ) ;
#23529 = CARTESIAN_POINT ( 'NONE',  ( 0.000000000000000000, -170.0000000000000000, 5.000000000000000000 ) ) ;
#23530 = CARTESIAN_POINT ( 'NONE',  ( -58.80597590150559739, -145.0000000000000284, 3.242614290531460330 ) ) ;
#23531 = CARTESIAN_POINT ( 'NONE',  ( -2.499999999999996447, -87.83333333333332860, 4.330127018922195425 ) ) ;
#23532 = CARTESIAN_POINT ( 'NONE',  ( -5.000000000000000000, -36.87499999726881583, 0.000000000000000000 ) ) ;
#23533 = FACE_OUTER_BOUND ( 'NONE', #12258, .T. ) ;
#23534 = CARTESIAN_POINT ( 'NONE',  ( 4.458734124999998549, 19.27083333469893134, -2.574251347313721627 ) ) ;
#23535 = CARTESIAN_POINT ( 'NONE',  ( 5.000000000000000000, -51.37499999726881583, -6.123233995736766282E-16 ) ) ;
#23536 =( BOUNDED_CURVE ( )  B_SPLINE_CURVE ( 2, ( #11983, #7181, #26789, #57020, #46408, #51556, #41560, #2357, #57339 ),
 .UNSPECIFIED., .F., .F. ) 
 B_SPLINE_CURVE_WITH_KNOTS ( ( 3, 2, 2, 2, 3 ),
 ( 0.6732142857142857650, 0.6738095238095238582, 0.6750000000000000444, 0.6761904761904762307, 0.6767857142857143238 ),
 .UNSPECIFIED. ) 
 CURVE ( )  GEOMETRIC_REPRESENTATION_ITEM ( )  RATIONAL_B_SPLINE_CURVE ( ( 0.9330127018922194093, 0.9330127018922194093, 1.000000000000000000, 0.8660254037844387076, 1.000000000000000000, 0.8660254037844387076, 1.000000000000000000, 0.9330127018922194093, 0.9330127018922194093 ) ) 
 REPRESENTATION_ITEM ( '' )  );
#23537 = CARTESIAN_POINT ( 'NONE',  ( -2.229367062500000163, 24.52083333469892779, -3.861377020970580443 ) ) ;
#23538 = CARTESIAN_POINT ( 'NONE',  ( -2.229367062499996610, -58.14583333196773651, 3.861377020970582219 ) ) ;
#23539 = CARTESIAN_POINT ( 'NONE',  ( 4.458734124999998549, -5.979166665301071326, -2.574251347313721627 ) ) ;
#23540 = CARTESIAN_POINT ( 'NONE',  ( -1.339745962155610925, -62.79465819873851729, 5.000000000000000000 ) ) ;
#23541 = CARTESIAN_POINT ( 'NONE',  ( 2.499999999999998668, 7.666666666666665186, -4.330127018922193649 ) ) ;
#23542 = CARTESIAN_POINT ( 'NONE',  ( -3.152801135295367985, -167.8125000013656063, 3.152801135295367096 ) ) ;
#23543 = CARTESIAN_POINT ( 'NONE',  ( -5.000000000000000000, -52.00000000000000711, 0.000000000000000000 ) ) ;
#23544 = CARTESIAN_POINT ( 'NONE',  ( 4.458734124999998549, -46.72916666530106511, -2.574251347313721627 ) ) ;
#23545 = CARTESIAN_POINT ( 'NONE',  ( 1.060575238724906964E-15, -82.62499999726880162, 5.773502691896257311 ) ) ;
#23546 = CARTESIAN_POINT ( 'NONE',  ( -59.44456063193725015, -134.8125000013656063, -0.3552334253322034230 ) ) ;
#23547 = CYLINDRICAL_SURFACE ( 'NONE', #20579, 5.000000000000000000 ) ;
#23548 = EDGE_CURVE ( 'NONE', #30305, #59122, #28149, .T. ) ;
#23549 = DIRECTION ( 'NONE',  ( -0.000000000000000000, 1.000000000000000000, -0.000000000000000000 ) ) ;
#23550 = EDGE_CURVE ( 'NONE', #19195, #24536, #37186, .T. ) ;
#23551 = CARTESIAN_POINT ( 'NONE',  ( -4.458734124999999437, -89.64583333196773651, -2.574251347313719407 ) ) ;
#23552 = CARTESIAN_POINT ( 'NONE',  ( 1.846868145590736310, -157.8750000013655779, 4.458734124999997661 ) ) ;
#23553 = CARTESIAN_POINT ( 'NONE',  ( 5.000000000000000888, -37.58333333333332860, 2.886751345948126879 ) ) ;
#23554 = CARTESIAN_POINT ( 'NONE',  ( -6.972266317189433020E-16, 23.75000000000000000, -5.000000000000000000 ) ) ;
#23555 = EDGE_LOOP ( 'NONE', ( #38226, #55398, #20729, #53644 ) ) ;
#23556 = CARTESIAN_POINT ( 'NONE',  ( 0.000000000000000000, -170.0000000000000000, 0.000000000000000000 ) ) ;
#23557 = ORIENTED_EDGE ( 'NONE', *, *, #20005, .F. ) ;
#23558 = CARTESIAN_POINT ( 'NONE',  ( -3.152548672688508926E-16, -95.56249999863442213, -5.148502694627439702 ) ) ;
#23559 = CARTESIAN_POINT ( 'NONE',  ( 2.229367062500001939, 5.770833334698927786, 3.861377020970579999 ) ) ;
#23560 = COLOUR_RGB ( '',0.8941176470588234615, 0.8941176470588234615, 0.8941176470588234615 ) ;
#23561 = CARTESIAN_POINT ( 'NONE',  ( 2.500000000000002220, 9.458333336064519870, 4.330127018922192761 ) ) ;
#23562 =( BOUNDED_CURVE ( )  B_SPLINE_CURVE ( 2, ( #21898, #51491, #3549, #51176, #8375, #32167, #18330, #23157, #18007 ),
 .UNSPECIFIED., .F., .F. ) 
 B_SPLINE_CURVE_WITH_KNOTS ( ( 3, 2, 2, 2, 3 ),
 ( 0.9937500000000000222, 0.9944444444444444642, 0.9958333333333333481, 0.9972222222222222321, 0.9979166666666666741 ),
 .UNSPECIFIED. ) 
 CURVE ( )  GEOMETRIC_REPRESENTATION_ITEM ( )  RATIONAL_B_SPLINE_CURVE ( ( 0.9330127018922194093, 0.9330127018922194093, 1.000000000000000000, 0.8660254037844387076, 1.000000000000000000, 0.8660254037844387076, 1.000000000000000000, 0.9330127018922194093, 0.9330127018922194093 ) ) 
 REPRESENTATION_ITEM ( '' )  );
#23563 = CARTESIAN_POINT ( 'NONE',  ( -1.339745962155613812, -88.08034179853028434, -5.000000000000000000 ) ) ;
#23564 = CARTESIAN_POINT ( 'NONE',  ( -2.499999999999996447, 2.166666666666667407, 4.330127018922195425 ) ) ;
#23565 = VECTOR ( 'NONE', #55285, 1000.000000000000000 ) ;
#23566 = EDGE_CURVE ( 'NONE', #12840, #7641, #23652, .T. ) ;
#23567 = CARTESIAN_POINT ( 'NONE',  ( 2.229367062500001939, -63.97916666530106511, 3.861377020970579999 ) ) ;
#23568 = CARTESIAN_POINT ( 'NONE',  ( -1.339745962155610925, -7.794658198738519950, 5.000000000000000000 ) ) ;
#23569 = CARTESIAN_POINT ( 'NONE',  ( 5.000000000000000888, 1.541666669397853573, 2.886751345948126879 ) ) ;
#23570 = CARTESIAN_POINT ( 'NONE',  ( -2.229367062500000163, -27.47916666530107221, -3.861377020970580443 ) ) ;
#23571 = CARTESIAN_POINT ( 'NONE',  ( -1.339745962155613812, -42.20534180126148271, -5.000000000000000000 ) ) ;
#23572 = CARTESIAN_POINT ( 'NONE',  ( 0.000000000000000000, -170.0000000000000000, 0.000000000000000000 ) ) ;
#23573 = CARTESIAN_POINT ( 'NONE',  ( -6.972266317189433020E-16, -19.25000000000000000, -5.000000000000000000 ) ) ;
#23574 = CARTESIAN_POINT ( 'NONE',  ( -2.499999999999996447, -44.83333333333333570, 4.330127018922195425 ) ) ;
#23576 = CARTESIAN_POINT ( 'NONE',  ( -4.458734124999999437, -20.56249999863440081, 0.000000000000000000 ) ) ;
#23575 = CARTESIAN_POINT ( 'NONE',  ( -6.972266317189433020E-16, -45.24999999999999289, -5.000000000000000000 ) ) ;
#23577 = CARTESIAN_POINT ( 'NONE',  ( -4.458734124999998549, -64.22916666530107932, 2.574251347313722516 ) ) ;
#23578 = CARTESIAN_POINT ( 'NONE',  ( 4.458734125000000326, -146.6250000013655779, -1.846868145590734978 ) ) ;
#23579 = CARTESIAN_POINT ( 'NONE',  ( -3.152548672688508926E-16, -77.56249999863440792, -5.148502694627439702 ) ) ;
#23580 = CARTESIAN_POINT ( 'NONE',  ( -57.89159099828107458, -144.9375000013656063, -3.393966926194107447 ) ) ;
#23581 = CARTESIAN_POINT ( 'NONE',  ( -4.458734124999999437, -27.56249999863440081, 0.000000000000000000 ) ) ;
#23582 = CARTESIAN_POINT ( 'NONE',  ( -5.000000000000000000, -64.95833333060214443, -2.886751345948128211 ) ) ;
#23583 = VERTEX_POINT ( 'NONE', #62724 ) ;
#23584 = EDGE_CURVE ( 'NONE', #53594, #46354, #63105, .T. ) ;
#23585 = CARTESIAN_POINT ( 'NONE',  ( 0.000000000000000000, -120.0000000000000000, 0.000000000000000000 ) ) ;
#23586 = ORIENTED_EDGE ( 'NONE', *, *, #3867, .F. ) ;
#23587 = CARTESIAN_POINT ( 'NONE',  ( 9.457646018065525792E-16, -70.31249999863439371, 5.148502694627439702 ) ) ;
#23588 = DIRECTION ( 'NONE',  ( -0.000000000000000000, 1.000000000000000000, -0.000000000000000000 ) ) ;
#23589 = CARTESIAN_POINT ( 'NONE',  ( -2.500000000000000444, -6.041666663935481019, -4.330127018922193649 ) ) ;
#23590 = ORIENTED_EDGE ( 'NONE', *, *, #25667, .T. ) ;
#23591 = CARTESIAN_POINT ( 'NONE',  ( -59.81910112700026616, -143.3125000027312126, -2.462841084822481541 ) ) ;
#23592 = CARTESIAN_POINT ( 'NONE',  ( 4.458734125000001214, -55.14583333196772941, 2.574251347313718519 ) ) ;
#23593 = CARTESIAN_POINT ( 'NONE',  ( 4.458734124999999437, 2.937500001365594304, -5.460374474430324690E-16 ) ) ;
#23594 = ORIENTED_EDGE ( 'NONE', *, *, #40432, .F. ) ;
#23595 = CARTESIAN_POINT ( 'NONE',  ( -2.499999999999996447, -54.83333333333332860, 4.330127018922195425 ) ) ;
#23596 = CARTESIAN_POINT ( 'NONE',  ( 4.458734124999998549, 17.27083333469892779, -2.574251347313721627 ) ) ;
#23597 = CARTESIAN_POINT ( 'NONE',  ( -59.29741812935640155, -144.6250000013656063, -2.196230717870135685 ) ) ;
#23598 = LINE ( 'NONE', #62837, #26444 ) ;
#23599 = CARTESIAN_POINT ( 'NONE',  ( -4.458734125000000326, -165.8750000013656063, 1.846868145590734089 ) ) ;
#23600 = ORIENTED_EDGE ( 'NONE', *, *, #37869, .T. ) ;
#23601 = CARTESIAN_POINT ( 'NONE',  ( 9.457646018065525792E-16, -74.06249999863440792, 5.148502694627439702 ) ) ;
#23602 = DIRECTION ( 'NONE',  ( -0.000000000000000000, 1.000000000000000000, -0.000000000000000000 ) ) ;
#23603 = CARTESIAN_POINT ( 'NONE',  ( -4.458734124999999437, 8.604166668032261711, -2.574251347313719407 ) ) ;
#23604 = AXIS2_PLACEMENT_3D ( 'NONE', #36302, #31786, #45632 ) ;
#23605 = EDGE_CURVE ( 'NONE', #32079, #51190, #9302, .T. ) ;
#23606 = EDGE_CURVE ( 'NONE', #44494, #8541, #19264, .T. ) ;
#23607 = CARTESIAN_POINT ( 'NONE',  ( -2.071067811865404451, -162.4375000027311557, 5.000000000000073719 ) ) ;
#23608 = EDGE_CURVE ( 'NONE', #53065, #20011, #41294, .T. ) ;
#23609 = CARTESIAN_POINT ( 'NONE',  ( -4.458734124999999437, -59.64583333196773651, -2.574251347313719407 ) ) ;
#23610 = CARTESIAN_POINT ( 'NONE',  ( 5.000000000000000888, -18.45833333060214798, 2.886751345948126879 ) ) ;
#23611 = CARTESIAN_POINT ( 'NONE',  ( 1.975475456537005874E-15, -40.74999999999999289, 5.000000000000000000 ) ) ;
#23612 = CYLINDRICAL_SURFACE ( 'NONE', #24237, 5.000000000000000000 ) ;
#23613 = CARTESIAN_POINT ( 'NONE',  ( 2.499999999999998668, -18.20833333060214798, -4.330127018922193649 ) ) ;
#23614 = CARTESIAN_POINT ( 'NONE',  ( -9.184850993605147944E-16, -159.2500000000000000, 5.000000000000000000 ) ) ;
#23615 = CARTESIAN_POINT ( 'NONE',  ( -3.152548672688508926E-16, -39.56249999863440081, -5.148502694627439702 ) ) ;
#23616 = CARTESIAN_POINT ( 'NONE',  ( 2.229367062499998831, -25.89583333196773651, -3.861377020970580887 ) ) ;
#23617 = DIRECTION ( 'NONE',  ( -0.000000000000000000, 1.000000000000000000, -0.000000000000000000 ) ) ;
#23618 = CARTESIAN_POINT ( 'NONE',  ( -4.999999999999999112, 24.08333333333333215, 2.886751345948131764 ) ) ;
#23619 = CARTESIAN_POINT ( 'NONE',  ( -3.535533905932738641, -151.5000000027312126, 3.535533905932737309 ) ) ;
#23620 = ORIENTED_EDGE ( 'NONE', *, *, #44076, .F. ) ;
#23621 = CARTESIAN_POINT ( 'NONE',  ( 9.457646018065525792E-16, -110.3124999986343937, 5.148502694627439702 ) ) ;
#23622 = CARTESIAN_POINT ( 'NONE',  ( -4.458734124999999437, -30.31249999863440436, 0.000000000000000000 ) ) ;
#23623 = CARTESIAN_POINT ( 'NONE',  ( -3.535250795749689387E-16, -69.12499999726880162, -5.773502691896257311 ) ) ;
#23624 = ADVANCED_FACE ( 'NONE', ( #29541 ), #59803, .T. ) ;
#23625 = CARTESIAN_POINT ( 'NONE',  ( -59.44456063193725015, -149.8125000013656063, -0.3552334253322034230 ) ) ;
#23626 = CARTESIAN_POINT ( 'NONE',  ( -3.535533905932737309, -144.6250000000000000, -3.535533905932738197 ) ) ;
#23627 = ADVANCED_FACE ( 'NONE', ( #45631 ), #54324, .T. ) ;
#23628 = CARTESIAN_POINT ( 'NONE',  ( -4.458734124999999437, -72.64583333196773651, -2.574251347313719407 ) ) ;
#23629 = CARTESIAN_POINT ( 'NONE',  ( -2.500000000000000444, -55.16666666666667140, -4.330127018922193649 ) ) ;
#23630 = CARTESIAN_POINT ( 'NONE',  ( 2.229367062499998831, -29.64583333196773296, -3.861377020970580887 ) ) ;
#23631 = DIRECTION ( 'NONE',  ( 0.000000000000000000, 0.000000000000000000, 1.000000000000000000 ) ) ;
#23632 = CARTESIAN_POINT ( 'NONE',  ( 5.000000000000000000, 18.62500000273118772, -6.123233995736766282E-16 ) ) ;
#23633 = CARTESIAN_POINT ( 'NONE',  ( 2.500000000000002220, -19.66666666666666430, 4.330127018922192761 ) ) ;
#23634 = CARTESIAN_POINT ( 'NONE',  ( -4.458734124999999437, -145.9375000013656063, -5.460374474430324690E-16 ) ) ;
#23635 = ORIENTED_EDGE ( 'NONE', *, *, #9707, .T. ) ;
#23636 = CARTESIAN_POINT ( 'NONE',  ( -1.339745962155613812, -79.08034179853028434, -5.000000000000000000 ) ) ;
#23637 = CARTESIAN_POINT ( 'NONE',  ( 9.457646018065525792E-16, -57.31249999863440081, 5.148502694627439702 ) ) ;
#23638 = CARTESIAN_POINT ( 'NONE',  ( 5.000000000000000000, 24.70833333606451987, -2.886751345948129988 ) ) ;
#23639 = CARTESIAN_POINT ( 'NONE',  ( 5.000000000000000000, 4.708333336064518093, -2.886751345948130876 ) ) ;
#23640 = CARTESIAN_POINT ( 'NONE',  ( 5.000000000000000000, 17.58333333333333215, -2.886751345948129988 ) ) ;
#23641 =( BOUNDED_CURVE ( )  B_SPLINE_CURVE ( 2, ( #49206, #29254, #52545, #24445, #39228, #10288, #25079, #30212, #14469 ),
 .UNSPECIFIED., .F., .F. ) 
 B_SPLINE_CURVE_WITH_KNOTS ( ( 3, 2, 2, 2, 3 ),
 ( 0.2895833333333333592, 0.2902777777777778012, 0.2916666666666666852, 0.2930555555555555691, 0.2937500000000000111 ),
 .UNSPECIFIED. ) 
 CURVE ( )  GEOMETRIC_REPRESENTATION_ITEM ( )  RATIONAL_B_SPLINE_CURVE ( ( 0.9330127018922194093, 0.9330127018922220739, 1.000000000000000000, 0.8660254037844387076, 1.000000000000000000, 0.8660254037844387076, 1.000000000000000000, 0.9330127018922194093, 0.9330127018922194093 ) ) 
 REPRESENTATION_ITEM ( '' )  );
#23642 = CARTESIAN_POINT ( 'NONE',  ( -2.229367062500000163, -7.479166665301073991, -3.861377020970580443 ) ) ;
#23643 = CARTESIAN_POINT ( 'NONE',  ( 5.000000000000000000, 28.49999999999999645, -6.123233995736766282E-16 ) ) ;
#23644 = CARTESIAN_POINT ( 'NONE',  ( -1.339745962155610925, -40.66965819600732601, 5.000000000000000000 ) ) ;
#23645 = CARTESIAN_POINT ( 'NONE',  ( 9.457646018065525792E-16, 8.687500001365595637, 5.148502694627439702 ) ) ;
#23646 = CARTESIAN_POINT ( 'NONE',  ( 2.499999999999998668, -53.20833333060213732, -4.330127018922193649 ) ) ;
#23647 = VERTEX_POINT ( 'NONE', #622 ) ;
#23648 = CARTESIAN_POINT ( 'NONE',  ( -52.53715891517739323, -135.4375000000000284, -4.819101127000233298 ) ) ;
#23649 = CARTESIAN_POINT ( 'NONE',  ( -4.458734124999999437, -48.39583333196772941, -2.574251347313719407 ) ) ;
#23650 = CARTESIAN_POINT ( 'NONE',  ( -3.152801135295367096, -160.3125000013656063, -3.152801135295367541 ) ) ;
#23651 = VECTOR ( 'NONE', #23404, 1000.000000000000000 ) ;
#23652 =( BOUNDED_CURVE ( )  B_SPLINE_CURVE ( 2, ( #14753, #38881, #47905, #34370, #28293, #18333, #57590, #13518, #8679 ),
 .UNSPECIFIED., .F., .F. ) 
 B_SPLINE_CURVE_WITH_KNOTS ( ( 3, 2, 2, 2, 3 ),
 ( 0.2187500000000000000, 0.2194444444444444420, 0.2208333333333333259, 0.2222222222222222099, 0.2229166666666666796 ),
 .UNSPECIFIED. ) 
 CURVE ( )  GEOMETRIC_REPRESENTATION_ITEM ( )  RATIONAL_B_SPLINE_CURVE ( ( 0.9330127018922194093, 0.9330127018922194093, 1.000000000000000000, 0.8660254037844387076, 1.000000000000000000, 0.8660254037844387076, 1.000000000000000000, 0.9330127018922180770, 0.9330127018922194093 ) ) 
 REPRESENTATION_ITEM ( '' )  );
#23653 = CARTESIAN_POINT ( 'NONE',  ( 5.000000000000000888, -52.45833333060213732, 2.886751345948126879 ) ) ;
#23654 = VERTEX_POINT ( 'NONE', #16039 ) ;
#23655 = CARTESIAN_POINT ( 'NONE',  ( -4.458734124999999437, -23.39583333196773296, -2.574251347313719407 ) ) ;
#23656 = VERTEX_POINT ( 'NONE', #44993 ) ;
#23658 = LINE ( 'NONE', #62893, #5978 ) ;
#23657 = CARTESIAN_POINT ( 'NONE',  ( 1.975475456537005874E-15, -69.62499999726880162, 5.000000000000000000 ) ) ;
#23659 = CARTESIAN_POINT ( 'NONE',  ( 4.458734124999999437, -161.5000000013656063, 1.846868145590737864 ) ) ;
#23660 = ORIENTED_EDGE ( 'NONE', *, *, #36892, .T. ) ;
#23661 = CARTESIAN_POINT ( 'NONE',  ( -51.75738570946856498, -133.7500000000000284, 3.805975901505576964 ) ) ;
#23662 = CARTESIAN_POINT ( 'NONE',  ( 0.000000000000000000, -120.0000000000000000, 0.000000000000000000 ) ) ;
#23663 = CARTESIAN_POINT ( 'NONE',  ( 2.229367062500001939, -35.22916666530107221, 3.861377020970579999 ) ) ;
#23664 = AXIS2_PLACEMENT_3D ( 'NONE', #20, #34402, #43741 ) ;
#23665 = VERTEX_POINT ( 'NONE', #25050 ) ;
#23666 = CARTESIAN_POINT ( 'NONE',  ( -4.458734124999999437, -81.31249999863440792, 0.000000000000000000 ) ) ;
#23667 = CARTESIAN_POINT ( 'NONE',  ( 4.458734125000001214, 17.10416666803225993, 2.574251347313718519 ) ) ;
#23668 = LINE ( 'NONE', #38142, #19409 ) ;
#23669 = ORIENTED_EDGE ( 'NONE', *, *, #59330, .F. ) ;
#23670 = CARTESIAN_POINT ( 'NONE',  ( -52.10840900171896806, -137.4375000013656063, 3.393966926194110556 ) ) ;
#23671 = CARTESIAN_POINT ( 'NONE',  ( 4.458734124999999437, -87.06249999863439371, -5.460374474430324690E-16 ) ) ;
#23672 = CARTESIAN_POINT ( 'NONE',  ( -50.01589407740564042, -125.7500000027311984, 0.3983568153799778022 ) ) ;
#23673 = CARTESIAN_POINT ( 'NONE',  ( 1.975475456537005874E-15, 11.37500000273118239, 5.000000000000000000 ) ) ;
#23674 = LINE ( 'NONE', #15275, #16167 ) ;
#23675 = CARTESIAN_POINT ( 'NONE',  ( 5.000000000000000000, 4.500000000000000888, -6.123233995736766282E-16 ) ) ;
#23676 = CARTESIAN_POINT ( 'NONE',  ( 9.457646018065525792E-16, -62.06249999863440792, 5.148502694627439702 ) ) ;
#23677 = CARTESIAN_POINT ( 'NONE',  ( 1.975475456537005874E-15, -37.74999999999999289, 5.000000000000000000 ) ) ;
#23678 = CARTESIAN_POINT ( 'NONE',  ( -4.458734124999999437, 24.68750000136559208, 0.000000000000000000 ) ) ;
#23679 = CARTESIAN_POINT ( 'NONE',  ( 1.060575238724906964E-15, -109.7499999999999858, 5.773502691896257311 ) ) ;
#23680 = CARTESIAN_POINT ( 'NONE',  ( -6.972266317189433020E-16, -82.24999999999998579, -5.000000000000000000 ) ) ;
#23681 = EDGE_CURVE ( 'NONE', #49893, #551, #15410, .T. ) ;
#23682 = CARTESIAN_POINT ( 'NONE',  ( 4.458734124999998549, -44.97916666530107221, -2.574251347313721627 ) ) ;
#23683 = CARTESIAN_POINT ( 'NONE',  ( 5.000000000000000000, -6.374999997268812280, -6.123233995736766282E-16 ) ) ;
#23684 = CARTESIAN_POINT ( 'NONE',  ( -6.972266317189433020E-16, -93.24999999999998579, -5.000000000000000000 ) ) ;
#23685 = CARTESIAN_POINT ( 'NONE',  ( -6.972266317189433020E-16, -61.25000000000000000, -5.000000000000000000 ) ) ;
#23686 = CARTESIAN_POINT ( 'NONE',  ( -2.229367062499996610, -85.39583333196773651, 3.861377020970582219 ) ) ;
#23687 = CARTESIAN_POINT ( 'NONE',  ( -4.458734124999999437, -110.3124999986343937, 0.000000000000000000 ) ) ;
#23688 = CARTESIAN_POINT ( 'NONE',  ( -4.458734124999997661, -12.47916666530107044, 2.574251347313722516 ) ) ;
#23690 = VERTEX_POINT ( 'NONE', #16365 ) ;
#23689 = EDGE_CURVE ( 'NONE', #14909, #51364, #35344, .T. ) ;
#23691 = CARTESIAN_POINT ( 'NONE',  ( 2.500000000000002220, -52.66666666666666430, 4.330127018922192761 ) ) ;
#23692 = CARTESIAN_POINT ( 'NONE',  ( 4.458734125000001214, -95.89583333196773651, 2.574251347313718519 ) ) ;
#23693 = CARTESIAN_POINT ( 'NONE',  ( 2.071067811865476394, -165.3125000027312126, 5.000000000000000000 ) ) ;
#23694 = CARTESIAN_POINT ( 'NONE',  ( 2.229367062499998831, -91.89583333196773651, -3.861377020970580887 ) ) ;
#23695 = AXIS2_PLACEMENT_3D ( 'NONE', #5261, #1094, #10399 ) ;
#23697 = EDGE_CURVE ( 'NONE', #34811, #23480, #53999, .T. ) ;
#23696 = CARTESIAN_POINT ( 'NONE',  ( -4.999999999999999112, -52.79166666393547303, 2.886751345948131764 ) ) ;
#23698 = CARTESIAN_POINT ( 'NONE',  ( -6.293430271071534854, 5.026740376715094882, -0.4524126574264483169 ) ) ;
#23699 = EDGE_CURVE ( 'NONE', #7768, #58694, #58585, .T. ) ;
#23700 = CARTESIAN_POINT ( 'NONE',  ( -53.51423613279429503, -131.2500000013656347, 4.591703134518082763 ) ) ;
#23701 = CARTESIAN_POINT ( 'NONE',  ( -57.89159099828107458, -148.6875000013656063, -3.393966926194107447 ) ) ;
#23702 = CARTESIAN_POINT ( 'NONE',  ( -4.458734124999999437, -13.31249999863440259, 0.000000000000000000 ) ) ;
#23703 = CARTESIAN_POINT ( 'NONE',  ( 4.458734124999999437, 8.937500001365592084, -5.460374474430324690E-16 ) ) ;
#23704 = CARTESIAN_POINT ( 'NONE',  ( 2.229367062499998831, -59.89583333196774362, -3.861377020970580887 ) ) ;
#23705 = CARTESIAN_POINT ( 'NONE',  ( -6.972266317189433020E-16, -14.12499999726881228, -5.000000000000000000 ) ) ;
#23706 = CARTESIAN_POINT ( 'NONE',  ( 2.500000000000002220, -15.54166666393548191, 4.330127018922192761 ) ) ;
#23707 = CARTESIAN_POINT ( 'NONE',  ( -2.229367062500000163, -14.47916666530107221, -3.861377020970580443 ) ) ;
#23708 = CARTESIAN_POINT ( 'NONE',  ( 5.000000000000000888, -71.58333333333332860, 2.886751345948126879 ) ) ;
#23709 = EDGE_CURVE ( 'NONE', #26645, #8886, #56911, .T. ) ;
#23710 = ORIENTED_EDGE ( 'NONE', *, *, #46042, .T. ) ;
#23711 = CARTESIAN_POINT ( 'NONE',  ( 9.457646018065525792E-16, -41.31249999863440792, 5.148502694627439702 ) ) ;
#23712 =( BOUNDED_CURVE ( )  B_SPLINE_CURVE ( 2, ( #35195, #54811, #20398, #5283, #54493, #24903, #5926, #45793, #29708 ),
 .UNSPECIFIED., .F., .F. ) 
 B_SPLINE_CURVE_WITH_KNOTS ( ( 3, 2, 2, 2, 3 ),
 ( 0.3312499999999999889, 0.3319444444444444309, 0.3333333333333333148, 0.3347222222222221988, 0.3354166666666666963 ),
 .UNSPECIFIED. ) 
 CURVE ( )  GEOMETRIC_REPRESENTATION_ITEM ( )  RATIONAL_B_SPLINE_CURVE ( ( 0.9330127018922194093, 0.9330127018922194093, 1.000000000000000000, 0.8660254037844387076, 1.000000000000000000, 0.8660254037844387076, 1.000000000000000000, 0.9330127018922167448, 0.9330127018922194093 ) ) 
 REPRESENTATION_ITEM ( '' )  );
#23713 = EDGE_CURVE ( 'NONE', #43496, #32964, #36420, .T. ) ;
#23714 = CARTESIAN_POINT ( 'NONE',  ( 1.975475456537005874E-15, -24.74999999999999645, 5.000000000000000000 ) ) ;
#23715 = CARTESIAN_POINT ( 'NONE',  ( -4.458734124999999437, -87.39583333196773651, -2.574251347313719407 ) ) ;
#23716 = CARTESIAN_POINT ( 'NONE',  ( -4.458734124999998549, 18.52083333469892779, 2.574251347313722516 ) ) ;
#23717 = CARTESIAN_POINT ( 'NONE',  ( -2.229367062499996610, 12.85416666803226171, 3.861377020970582219 ) ) ;
#23718 = EDGE_CURVE ( 'NONE', #36394, #45194, #62017, .T. ) ;
#23719 = CARTESIAN_POINT ( 'NONE',  ( 3.061616997868383141E-16, -155.7500000000000000, -5.000000000000000000 ) ) ;
#23720 = CARTESIAN_POINT ( 'NONE',  ( -52.53715891517739323, -137.5625000027312126, -4.819101127000233298 ) ) ;
#23721 = CARTESIAN_POINT ( 'NONE',  ( -4.458734124999999437, -88.64583333196773651, -2.574251347313719407 ) ) ;
#23722 = CARTESIAN_POINT ( 'NONE',  ( -2.499999999999996447, -70.83333333333332860, 4.330127018922195425 ) ) ;
#23723 = CARTESIAN_POINT ( 'NONE',  ( 5.000000000000000888, 14.54166666939785024, 2.886751345948126879 ) ) ;
#23724 = ORIENTED_EDGE ( 'NONE', *, *, #11031, .F. ) ;
#23725 = CARTESIAN_POINT ( 'NONE',  ( 1.339745962155615144, -79.70534180126146850, 4.999999999999999112 ) ) ;
#23726 = CARTESIAN_POINT ( 'NONE',  ( -50.18089887299977647, -144.8125000027312126, 2.462841084822486426 ) ) ;
#23728 = CARTESIAN_POINT ( 'NONE',  ( -3.535250795749689387E-16, -30.24999999999999645, -5.773502691896257311 ) ) ;
#23727 = CARTESIAN_POINT ( 'NONE',  ( -5.000000000000000000, -104.0000000000000142, 0.000000000000000000 ) ) ;
#23729 = CARTESIAN_POINT ( 'NONE',  ( -3.152548672688508926E-16, -31.56249999863440436, -5.148502694627439702 ) ) ;
#23730 = CARTESIAN_POINT ( 'NONE',  ( 5.000000000000000000, -36.29166666393547303, -2.886751345948129988 ) ) ;
#23732 = EDGE_LOOP ( 'NONE', ( #41182, #11384, #25555, #22020 ) ) ;
#23731 = CARTESIAN_POINT ( 'NONE',  ( -2.229367062499996610, -63.14583333196774362, 3.861377020970582219 ) ) ;
#23733 = CARTESIAN_POINT ( 'NONE',  ( -50.55543936806279248, -152.3125000013656063, 0.3552334253322060320 ) ) ;
#23735 = ORIENTED_EDGE ( 'NONE', *, *, #42929, .F. ) ;
#23734 = CARTESIAN_POINT ( 'NONE',  ( 2.229367062500001939, -14.22916666530107221, 3.861377020970579999 ) ) ;
#23736 = CARTESIAN_POINT ( 'NONE',  ( -2.499999999999996447, -76.83333333333334281, 4.330127018922195425 ) ) ;
#23737 = CARTESIAN_POINT ( 'NONE',  ( -50.48477904491434742, -135.0324864422693736, -0.5288446712371500658 ) ) ;
#23738 = CARTESIAN_POINT ( 'NONE',  ( 4.458734124999999437, -58.06249999863440081, -5.460374474430324690E-16 ) ) ;
#23739 =( BOUNDED_CURVE ( )  B_SPLINE_CURVE ( 2, ( #27477, #47105, #31674, #61911, #61275, #17196, #41949, #36823, #56454 ),
 .UNSPECIFIED., .F., .F. ) 
 B_SPLINE_CURVE_WITH_KNOTS ( ( 3, 2, 2, 2, 3 ),
 ( 0.08958333333333333426, 0.09027777777777777624, 0.09166666666666666019, 0.09305555555555555802, 0.09375000000000000000 ),
 .UNSPECIFIED. ) 
 CURVE ( )  GEOMETRIC_REPRESENTATION_ITEM ( )  RATIONAL_B_SPLINE_CURVE ( ( 0.9330127018922194093, 0.9330127018922194093, 1.000000000000000000, 0.8660254037844387076, 1.000000000000000000, 0.8660254037844387076, 1.000000000000000000, 0.9330127018922194093, 0.9330127018922194093 ) ) 
 REPRESENTATION_ITEM ( '' )  );
#23740 = CARTESIAN_POINT ( 'NONE',  ( 5.000000000000000000, -80.29166666393545881, -2.886751345948129988 ) ) ;
#23742 = ORIENTED_EDGE ( 'NONE', *, *, #16593, .T. ) ;
#23741 = CARTESIAN_POINT ( 'NONE',  ( 5.000000000000000000, -13.49999999999999822, -6.123233995736766282E-16 ) ) ;
#23743 = AXIS2_PLACEMENT_3D ( 'NONE', #44661, #21186, #50465 ) ;
#23744 = CARTESIAN_POINT ( 'NONE',  ( -50.18089887299979068, -145.6875000000000000, 2.462841084822635640 ) ) ;
#23745 = CARTESIAN_POINT ( 'NONE',  ( -4.458734124999999437, -22.64583333196773296, -2.574251347313719407 ) ) ;
#23747 = ORIENTED_EDGE ( 'NONE', *, *, #48346, .T. ) ;
#23746 = CARTESIAN_POINT ( 'NONE',  ( -4.458734124999999437, -55.64583333196773651, -2.574251347313719407 ) ) ;
#23748 = DIRECTION ( 'NONE',  ( 0.000000000000000000, 0.000000000000000000, 1.000000000000000000 ) ) ;
#23749 = CARTESIAN_POINT ( 'NONE',  ( 3.152801135295366208, -168.8125000013656063, 3.152801135295367985 ) ) ;
#23750 = AXIS2_PLACEMENT_3D ( 'NONE', #9353, #63091, #19001 ) ;
#23751 = CARTESIAN_POINT ( 'NONE',  ( 4.458734125000001214, -106.1458333319677365, 2.574251347313718519 ) ) ;
#23752 = EDGE_LOOP ( 'NONE', ( #36299, #33699, #3409, #36700 ) ) ;
#23753 = CARTESIAN_POINT ( 'NONE',  ( -57.19623071787016499, -148.6250000013656063, 4.297418129356382899 ) ) ;
#23754 = CARTESIAN_POINT ( 'NONE',  ( -58.24261429053147765, -137.3750000027312126, -3.805975901505573855 ) ) ;
#23755 = CARTESIAN_POINT ( 'NONE',  ( -4.458734124999997661, -39.22916666530107221, 2.574251347313722516 ) ) ;
#23756 = CARTESIAN_POINT ( 'NONE',  ( 0.000000000000000000, -170.0000000000000000, 0.000000000000000000 ) ) ;
#23757 = CARTESIAN_POINT ( 'NONE',  ( 4.458734124999998549, -14.72916666530107399, -2.574251347313721627 ) ) ;
#23758 = CARTESIAN_POINT ( 'NONE',  ( -3.152548672688508926E-16, -99.81249999863440792, -5.148502694627439702 ) ) ;
#23759 = CARTESIAN_POINT ( 'NONE',  ( 3.152801135295367541, -144.5625000013655779, -3.152801135295367541 ) ) ;
#23760 = CARTESIAN_POINT ( 'NONE',  ( -2.229367062500000163, -26.72916666530106866, -3.861377020970580443 ) ) ;
#23761 = CARTESIAN_POINT ( 'NONE',  ( -56.48576386720575471, -133.7500000013656063, -4.591703134518078322 ) ) ;
#23762 = CARTESIAN_POINT ( 'NONE',  ( -2.229367062499996610, -67.39583333196773651, 3.861377020970582219 ) ) ;
#23763 = DIRECTION ( 'NONE',  ( -0.000000000000000000, 1.000000000000000000, -0.000000000000000000 ) ) ;
#23764 = CARTESIAN_POINT ( 'NONE',  ( 4.458734124999999437, -142.3750000013656063, -1.846868145590734978 ) ) ;
#23765 = CARTESIAN_POINT ( 'NONE',  ( -2.229367062499996610, 3.604166668032260379, 3.861377020970582219 ) ) ;
#23766 = ORIENTED_EDGE ( 'NONE', *, *, #50419, .T. ) ;
#23767 = CARTESIAN_POINT ( 'NONE',  ( -4.999999999999998224, -70.79166666393547303, 2.886751345948131764 ) ) ;
#23768 = CARTESIAN_POINT ( 'NONE',  ( -2.500000000000000444, 15.95833333606451809, -4.330127018922193649 ) ) ;
#23770 = CARTESIAN_POINT ( 'NONE',  ( -3.152548672688508926E-16, -28.56249999863440436, -5.148502694627439702 ) ) ;
#23769 = CARTESIAN_POINT ( 'NONE',  ( 5.000000000000000888, -96.58333333333332860, 2.886751345948126879 ) ) ;
#23771 = CARTESIAN_POINT ( 'NONE',  ( 4.458734124999999437, -74.06249999863440792, -5.460374474430324690E-16 ) ) ;
#23772 = CARTESIAN_POINT ( 'NONE',  ( 9.457646018065525792E-16, 23.68750000136559564, 5.148502694627439702 ) ) ;
#23773 = CARTESIAN_POINT ( 'NONE',  ( -6.972266317189433020E-16, -102.1249999972688158, -5.000000000000000000 ) ) ;
#23774 = CARTESIAN_POINT ( 'NONE',  ( -52.10840900171896806, -140.1875000013656063, 3.393966926194110556 ) ) ;
#23775 = CARTESIAN_POINT ( 'NONE',  ( -4.458734124999999437, 3.604166668032260379, -2.574251347313719407 ) ) ;
#23776 = CARTESIAN_POINT ( 'NONE',  ( -4.458734124999999437, 29.43750000136559208, 0.000000000000000000 ) ) ;
#23777 = CARTESIAN_POINT ( 'NONE',  ( 4.458734124999998549, -40.97916666530106511, -2.574251347313721627 ) ) ;
#23778 = CARTESIAN_POINT ( 'NONE',  ( 2.499999999999998668, -43.20833333060214443, -4.330127018922193649 ) ) ;
#23779 = CARTESIAN_POINT ( 'NONE',  ( -2.229367062499996610, 1.854166668032262377, 3.861377020970582219 ) ) ;
#23780 = CARTESIAN_POINT ( 'NONE',  ( -3.152548672688508926E-16, -26.81249999863440436, -5.148502694627439702 ) ) ;
#23781 = CARTESIAN_POINT ( 'NONE',  ( 1.846868145590735200, -155.2500000013656063, -4.458734125000000326 ) ) ;
#23782 = CARTESIAN_POINT ( 'NONE',  ( -4.458734124999999437, -68.31249999863439371, 0.000000000000000000 ) ) ;
#23783 = CARTESIAN_POINT ( 'NONE',  ( -4.999999999999999112, -101.7916666639354446, 2.886751345948131764 ) ) ;
#23784 = CARTESIAN_POINT ( 'NONE',  ( 5.000000000000000000, 15.58333333333332860, -2.886751345948130876 ) ) ;
#23785 = DIRECTION ( 'NONE',  ( -0.000000000000000000, 1.000000000000000000, -0.000000000000000000 ) ) ;
#23786 = CARTESIAN_POINT ( 'NONE',  ( -3.152548672688508926E-16, -107.8124999986343937, -5.148502694627439702 ) ) ;
#23787 = CARTESIAN_POINT ( 'NONE',  ( 4.458734125000000326, -75.14583333196775072, 2.574251347313718519 ) ) ;
#23788 = CARTESIAN_POINT ( 'NONE',  ( 2.500000000000002220, -56.66666666666667140, 4.330127018922192761 ) ) ;
#23789 = CARTESIAN_POINT ( 'NONE',  ( -5.000000000000000000, -22.00000000000000000, 0.000000000000000000 ) ) ;
#23790 = CARTESIAN_POINT ( 'NONE',  ( -2.500000000000000444, 28.95833333606451987, -4.330127018922193649 ) ) ;
#23791 = ORIENTED_EDGE ( 'NONE', *, *, #30578, .T. ) ;
#23792 = CARTESIAN_POINT ( 'NONE',  ( -1.339745962155610925, -26.79465819873852084, 5.000000000000000000 ) ) ;
#23793 = CARTESIAN_POINT ( 'NONE',  ( -4.999999999999998224, 13.08333333333333215, 2.886751345948131764 ) ) ;
#23794 = CARTESIAN_POINT ( 'NONE',  ( 1.060575238724906964E-15, -13.75000000000000000, 5.773502691896257311 ) ) ;
#23795 = CARTESIAN_POINT ( 'NONE',  ( -2.229367062500000163, -15.47916666530107399, -3.861377020970580443 ) ) ;
#23796 = CARTESIAN_POINT ( 'NONE',  ( -4.458734124999999437, -78.31249999863440792, 0.000000000000000000 ) ) ;
#23797 = CARTESIAN_POINT ( 'NONE',  ( -1.846868145590734756, -169.3750000013656347, -4.458734125000000326 ) ) ;
#23798 = CARTESIAN_POINT ( 'NONE',  ( -5.000000000000000000, -18.87499999726881583, 0.000000000000000000 ) ) ;
#23800 = VERTEX_POINT ( 'NONE', #3164 ) ;
#23799 = CARTESIAN_POINT ( 'NONE',  ( -2.229367062499996610, -47.14583333196774362, 3.861377020970582219 ) ) ;
#23801 = CARTESIAN_POINT ( 'NONE',  ( -1.339745962155610925, -27.66965819600733667, 5.000000000000000000 ) ) ;
#23803 = VERTEX_POINT ( 'NONE', #32097 ) ;
#23802 = CARTESIAN_POINT ( 'NONE',  ( 4.458734124999998549, 2.020833334698927786, -2.574251347313721627 ) ) ;
#23804 = CARTESIAN_POINT ( 'NONE',  ( -57.89159099828107458, -152.6875000013656063, -3.393966926194107447 ) ) ;
#23805 = CARTESIAN_POINT ( 'NONE',  ( -2.500000000000000444, -63.16666666666666430, -4.330127018922193649 ) ) ;
#23806 = CARTESIAN_POINT ( 'NONE',  ( 3.152801135295367541, -156.5625000013656063, -3.152801135295367541 ) ) ;
#23807 = CARTESIAN_POINT ( 'NONE',  ( -4.458734124999999437, -42.56249999863440081, 0.000000000000000000 ) ) ;
#23808 = CARTESIAN_POINT ( 'NONE',  ( -5.000000000000000000, -79.00000000000000000, 0.000000000000000000 ) ) ;
#23809 = CARTESIAN_POINT ( 'NONE',  ( -2.071067811865478170, -161.3125000000000284, 5.000000000000000000 ) ) ;
#23810 = CARTESIAN_POINT ( 'NONE',  ( 0.000000000000000000, -170.0000000000000000, 0.000000000000000000 ) ) ;
#23811 = CARTESIAN_POINT ( 'NONE',  ( -55.35523342533222291, -127.5625000013655921, 4.444560631937231499 ) ) ;
#23812 = CARTESIAN_POINT ( 'NONE',  ( 4.458734125000001214, -4.145833331967740065, 2.574251347313718519 ) ) ;
#23813 = CARTESIAN_POINT ( 'NONE',  ( -4.458734124999998549, -41.47916666530107221, 2.574251347313722516 ) ) ;
#23814 = CARTESIAN_POINT ( 'NONE',  ( 2.499999999999998668, -26.33333333333333215, -4.330127018922193649 ) ) ;
#23815 = CARTESIAN_POINT ( 'NONE',  ( -1.846868145590737420, -149.7500000013656063, 4.458734124999999437 ) ) ;
#23816 = CARTESIAN_POINT ( 'NONE',  ( -4.458734124999999437, -90.64583333196773651, -2.574251347313719407 ) ) ;
#23817 = CARTESIAN_POINT ( 'NONE',  ( 1.339745962155615144, 8.294658198738519062, 4.999999999999999112 ) ) ;
#23818 = VERTEX_POINT ( 'NONE', #61389 ) ;
#23819 = DIRECTION ( 'NONE',  ( -0.000000000000000000, 1.000000000000000000, -0.000000000000000000 ) ) ;
#23820 = CARTESIAN_POINT ( 'NONE',  ( -59.98410592259440222, -150.2500000027312126, -0.3983568153799752487 ) ) ;
#23821 = CARTESIAN_POINT ( 'NONE',  ( -4.999999999999998224, -104.9166666666666572, 2.886751345948131764 ) ) ;
#23822 = CARTESIAN_POINT ( 'NONE',  ( -2.229367062500000163, -77.72916666530106511, -3.861377020970580443 ) ) ;
#23823 = ORIENTED_EDGE ( 'NONE', *, *, #50790, .T. ) ;
#23824 =( BOUNDED_CURVE ( )  B_SPLINE_CURVE ( 2, ( #7575, #27810, #16899, #2750, #3387, #60978, #36515, #27187, #22369 ),
 .UNSPECIFIED., .F., .F. ) 
 B_SPLINE_CURVE_WITH_KNOTS ( ( 3, 2, 2, 2, 3 ),
 ( 0.4375000000000000000, 0.4380952380952380931, 0.4392857142857142794, 0.4404761904761904656, 0.4410714285714285587 ),
 .UNSPECIFIED. ) 
 CURVE ( )  GEOMETRIC_REPRESENTATION_ITEM ( )  RATIONAL_B_SPLINE_CURVE ( ( 0.9330127018922194093, 0.9330127018922194093, 1.000000000000000000, 0.8660254037844387076, 1.000000000000000000, 0.8660254037844387076, 1.000000000000000000, 0.9330127018922194093, 0.9330127018922194093 ) ) 
 REPRESENTATION_ITEM ( '' )  );
#23825 = CYLINDRICAL_SURFACE ( 'NONE', #37129, 11.00000000000000000 ) ;
#23826 = CARTESIAN_POINT ( 'NONE',  ( 2.229367062500001939, -12.22916666530107044, 3.861377020970579999 ) ) ;
#23827 = PRODUCT_DEFINITION_CONTEXT ( 'detailed design', #38816, 'design' ) ;
#23828 = CARTESIAN_POINT ( 'NONE',  ( -49.85088928181150436, -150.6875000027312126, -1.666127454062680480 ) ) ;
#23829 = CARTESIAN_POINT ( 'NONE',  ( -4.458734124999999437, -2.312499998634407028, 0.000000000000000000 ) ) ;
#23830 = VECTOR ( 'NONE', #25149, 1000.000000000000000 ) ;
#23832 = EDGE_CURVE ( 'NONE', #24115, #32079, #38839, .T. ) ;
#23831 = CARTESIAN_POINT ( 'NONE',  ( -4.458734124999999437, -151.9375000013655779, -5.460374474430324690E-16 ) ) ;
#23833 = CARTESIAN_POINT ( 'NONE',  ( 9.457646018065525792E-16, 22.68750000136559564, 5.148502694627439702 ) ) ;
#23834 = ORIENTED_EDGE ( 'NONE', *, *, #46844, .T. ) ;
#23835 = CARTESIAN_POINT ( 'NONE',  ( 4.458734124999998549, -89.72916666530106511, -2.574251347313721627 ) ) ;
#23836 = FACE_OUTER_BOUND ( 'NONE', #60798, .T. ) ;
#23837 = CARTESIAN_POINT ( 'NONE',  ( 2.499999999999998668, -12.20833333060214798, -4.330127018922193649 ) ) ;
#23838 = CARTESIAN_POINT ( 'NONE',  ( -3.152548672688508926E-16, -15.56249999863440614, -5.148502694627439702 ) ) ;
#23839 = CARTESIAN_POINT ( 'NONE',  ( -4.999999999999998224, -84.79166666393547303, 2.886751345948131764 ) ) ;
#23840 = CYLINDRICAL_SURFACE ( 'NONE', #35593, 5.000000000000000000 ) ;
#23841 = CARTESIAN_POINT ( 'NONE',  ( -59.29741812935640155, -153.6250000013655779, -2.196230717870135685 ) ) ;
#23842 = CARTESIAN_POINT ( 'NONE',  ( 2.499999999999998668, -39.20833333060214443, -4.330127018922193649 ) ) ;
#23843 = CARTESIAN_POINT ( 'NONE',  ( 2.499999999999998668, -64.20833333060213022, -4.330127018922193649 ) ) ;
#23844 = CARTESIAN_POINT ( 'NONE',  ( 4.458734124999998549, 17.27083333469892779, -2.574251347313721627 ) ) ;
#23845 = CARTESIAN_POINT ( 'NONE',  ( 2.500000000000002220, -46.54166666393547303, 4.330127018922192761 ) ) ;
#23846 = CARTESIAN_POINT ( 'NONE',  ( 9.457646018065525792E-16, 15.93750000136559564, 5.148502694627439702 ) ) ;
#23847 = CARTESIAN_POINT ( 'NONE',  ( -4.458734124999999437, -58.31249999863440081, 0.000000000000000000 ) ) ;
#23848 = CARTESIAN_POINT ( 'NONE',  ( 4.458734125000000326, -7.145833331967736513, 2.574251347313718519 ) ) ;
#23849 = LINE ( 'NONE', #14183, #8316 ) ;
#23850 = CARTESIAN_POINT ( 'NONE',  ( -3.535250795749689387E-16, 8.750000000000000000, -5.773502691896257311 ) ) ;
#23851 = CARTESIAN_POINT ( 'NONE',  ( 4.458734125000000326, -167.3750000013656347, -1.846868145590734978 ) ) ;
#23852 = CARTESIAN_POINT ( 'NONE',  ( -50.01589407740564042, -142.6250000000000284, 0.3983568153799778022 ) ) ;
#23853 = CARTESIAN_POINT ( 'NONE',  ( 9.457646018065525792E-16, -52.06249999863440792, 5.148502694627439702 ) ) ;
#23854 = CARTESIAN_POINT ( 'NONE',  ( -2.499999999999996447, -81.70833333060213022, 4.330127018922195425 ) ) ;
#23855 = CARTESIAN_POINT ( 'NONE',  ( -55.35523342533222291, -137.5625000013656063, 4.444560631937231499 ) ) ;
#23856 = CARTESIAN_POINT ( 'NONE',  ( 1.975475456537005874E-15, -14.62499999726881228, 5.000000000000000000 ) ) ;
#23857 = LINE ( 'NONE', #43460, #41868 ) ;
#23858 = CARTESIAN_POINT ( 'NONE',  ( -2.229367062500000163, -91.72916666530106511, -3.861377020970580443 ) ) ;
#23859 = CARTESIAN_POINT ( 'NONE',  ( -4.458734124999999437, -155.1875000013655779, -5.460374474430324690E-16 ) ) ;
#23860 = CARTESIAN_POINT ( 'NONE',  ( -3.535250795749689387E-16, -39.24999999999999289, -5.773502691896257311 ) ) ;
#23861 = CARTESIAN_POINT ( 'NONE',  ( -59.81910112700027327, -140.1875000000000284, -2.462841084822392279 ) ) ;
#23862 = CARTESIAN_POINT ( 'NONE',  ( 1.975475456537005874E-15, -85.62499999726880162, 5.000000000000000000 ) ) ;
#23863 = ORIENTED_EDGE ( 'NONE', *, *, #5603, .F. ) ;
#23864 = CARTESIAN_POINT ( 'NONE',  ( 9.457646018065525792E-16, -94.06249999863439371, 5.148502694627439702 ) ) ;
#23865 = CARTESIAN_POINT ( 'NONE',  ( -4.458734124999998549, 9.520833334698927786, 2.574251347313722516 ) ) ;
#23866 = CARTESIAN_POINT ( 'NONE',  ( -5.000000000000000000, 13.04166666939785379, -2.886751345948128211 ) ) ;
#23867 = FACE_OUTER_BOUND ( 'NONE', #28915, .T. ) ;
#23868 = CARTESIAN_POINT ( 'NONE',  ( -5.000000000000000000, 2.916666666666668739, -2.886751345948128211 ) ) ;
#23869 = CARTESIAN_POINT ( 'NONE',  ( 2.229367062499998831, -59.64583333196774362, -3.861377020970580887 ) ) ;
#23870 = CARTESIAN_POINT ( 'NONE',  ( -4.999999999999998224, 3.083333333333333925, 2.886751345948131764 ) ) ;
#23871 = CARTESIAN_POINT ( 'NONE',  ( 5.000000000000000000, -0.3749999972688135008, -6.123233995736766282E-16 ) ) ;
#23872 = CARTESIAN_POINT ( 'NONE',  ( -4.458734124999998549, -28.22916666530106866, 2.574251347313722516 ) ) ;
#23873 = CARTESIAN_POINT ( 'NONE',  ( 3.061616997868383141E-16, -152.8750000027311842, -5.000000000000000000 ) ) ;
#23874 = CARTESIAN_POINT ( 'NONE',  ( 5.000000000000000000, 19.50000000000000000, -6.123233995736766282E-16 ) ) ;
#23875 =( BOUNDED_CURVE ( )  B_SPLINE_CURVE ( 2, ( #3967, #406, #48951, #44447, #14228, #63140, #48014, #20009, #48326 ),
 .UNSPECIFIED., .F., .F. ) 
 B_SPLINE_CURVE_WITH_KNOTS ( ( 3, 2, 2, 2, 3 ),
 ( 0.01041666666666666782, 0.01111111111111111154, 0.01250000000000000069, 0.01388888888888888812, 0.01458333333333333356 ),
 .UNSPECIFIED. ) 
 CURVE ( )  GEOMETRIC_REPRESENTATION_ITEM ( )  RATIONAL_B_SPLINE_CURVE ( ( 0.9330127018922192983, 0.9330127018922194093, 1.000000000000000000, 0.8660254037844387076, 1.000000000000000000, 0.8660254037844387076, 1.000000000000000000, 0.9330127018922191873, 0.9330127018922192983 ) ) 
 REPRESENTATION_ITEM ( '' )  );
#23876 = DIRECTION ( 'NONE',  ( 0.000000000000000000, 0.000000000000000000, 1.000000000000000000 ) ) ;
#23877 = CARTESIAN_POINT ( 'NONE',  ( 5.000000000000000000, -45.41666666666666430, -2.886751345948129988 ) ) ;
#23880 = CARTESIAN_POINT ( 'NONE',  ( -4.458734124999999437, -26.64583333196773651, -2.574251347313719407 ) ) ;
#23879 =( BOUNDED_CURVE ( )  B_SPLINE_CURVE ( 2, ( #44727, #58891, #14821, #369, #19973, #689, #39582, #45057, #59545 ),
 .UNSPECIFIED., .F., .F. ) 
 B_SPLINE_CURVE_WITH_KNOTS ( ( 3, 2, 2, 2, 3 ),
 ( 0.8916666666666664964, 0.8958333333333331483, 0.8999999999999999112, 0.9041666666666665630, 0.9083333333333332149 ),
 .UNSPECIFIED. ) 
 CURVE ( )  GEOMETRIC_REPRESENTATION_ITEM ( )  RATIONAL_B_SPLINE_CURVE ( ( 1.000000000000003997, 0.9238795325112826307, 1.000000000000000000, 0.9238795325112867385, 1.000000000000000000, 0.9238795325112867385, 1.000000000000000000, 0.9238795325112887369, 0.9999999999999980016 ) ) 
 REPRESENTATION_ITEM ( '' )  );
#23878 = CARTESIAN_POINT ( 'NONE',  ( 3.061616997868383141E-16, -141.8750000027312126, -5.000000000000000000 ) ) ;
#23881 = CARTESIAN_POINT ( 'NONE',  ( -4.999999999999998224, 22.20833333606451987, 2.886751345948131764 ) ) ;
#23882 = CARTESIAN_POINT ( 'NONE',  ( 9.457646018065525792E-16, -71.06249999863440792, 5.148502694627439702 ) ) ;
#23883 = CARTESIAN_POINT ( 'NONE',  ( 1.846868145590736310, -146.8750000013656063, 4.458734124999999437 ) ) ;
#23885 = EDGE_CURVE ( 'NONE', #19213, #24693, #50323, .T. ) ;
#23884 = CARTESIAN_POINT ( 'NONE',  ( 4.458734125000001214, -74.89583333196773651, 2.574251347313718519 ) ) ;
#23886 = CARTESIAN_POINT ( 'NONE',  ( -59.29741812935640155, -144.8750000013655779, -2.196230717870135685 ) ) ;
#23887 = CARTESIAN_POINT ( 'NONE',  ( -2.229367062500000163, -24.72916666530106866, -3.861377020970580443 ) ) ;
#23888 = CARTESIAN_POINT ( 'NONE',  ( -4.999999999999999112, -65.79166666393547303, 2.886751345948131764 ) ) ;
#23889 = EDGE_LOOP ( 'NONE', ( #31290, #20735, #47851, #20804 ) ) ;
#23890 = CARTESIAN_POINT ( 'NONE',  ( -4.999999999999998224, -21.91666666666666785, 2.886751345948131764 ) ) ;
#23891 = ORIENTED_EDGE ( 'NONE', *, *, #50769, .F. ) ;
#23892 = CARTESIAN_POINT ( 'NONE',  ( -4.458734124999999437, -69.64583333196773651, -2.574251347313719407 ) ) ;
#23893 = CARTESIAN_POINT ( 'NONE',  ( -9.184850993605147944E-16, -166.2500000000000000, 5.000000000000000000 ) ) ;
#23894 = EDGE_LOOP ( 'NONE', ( #4414, #53612, #58979, #48488 ) ) ;
#23895 = LINE ( 'NONE', #38060, #11661 ) ;
#23896 = CARTESIAN_POINT ( 'NONE',  ( 4.458734124999999437, -57.06249999863440081, -5.460374474430324690E-16 ) ) ;
#23897 = CARTESIAN_POINT ( 'NONE',  ( 2.229367062499998831, -0.8958333319677401763, -3.861377020970580887 ) ) ;
#23898 = ORIENTED_EDGE ( 'NONE', *, *, #50417, .F. ) ;
#23899 = ADVANCED_FACE ( 'NONE', ( #12799 ), #50774, .T. ) ;
#23900 = CARTESIAN_POINT ( 'NONE',  ( -1.339745962155610925, -19.79465819873851729, 5.000000000000000000 ) ) ;
#23901 = EDGE_CURVE ( 'NONE', #7254, #3563, #54453, .T. ) ;
#23902 =( BOUNDED_CURVE ( )  B_SPLINE_CURVE ( 2, ( #14590, #9455, #43544, #23943, #59304, #62875, #44179, #63189, #29701 ),
 .UNSPECIFIED., .F., .F. ) 
 B_SPLINE_CURVE_WITH_KNOTS ( ( 3, 2, 2, 2, 3 ),
 ( 0.1270833333333333259, 0.1277777777777777679, 0.1291666666666666796, 0.1305555555555555636, 0.1312500000000000056 ),
 .UNSPECIFIED. ) 
 CURVE ( )  GEOMETRIC_REPRESENTATION_ITEM ( )  RATIONAL_B_SPLINE_CURVE ( ( 0.9330127018922194093, 0.9330127018922194093, 1.000000000000000000, 0.8660254037844387076, 1.000000000000000000, 0.8660254037844387076, 1.000000000000000000, 0.9330127018922194093, 0.9330127018922194093 ) ) 
 REPRESENTATION_ITEM ( '' )  );
#23903 = CARTESIAN_POINT ( 'NONE',  ( -2.229367062499996610, 17.85416666803225993, 3.861377020970582219 ) ) ;
#23904 = CARTESIAN_POINT ( 'NONE',  ( -52.10840900171896806, -146.1875000013656063, 3.393966926194110556 ) ) ;
#23905 = CARTESIAN_POINT ( 'NONE',  ( -8.190561711645485556E-16, -163.6875000013655779, 4.458734124999999437 ) ) ;
#23906 = VERTEX_POINT ( 'NONE', #17634 ) ;
#23907 = CARTESIAN_POINT ( 'NONE',  ( 4.458734124999999437, -75.81249999863440792, -5.460374474430324690E-16 ) ) ;
#23908 = CARTESIAN_POINT ( 'NONE',  ( -2.499999999999996447, -69.70833333060214443, 4.330127018922195425 ) ) ;
#23909 = CARTESIAN_POINT ( 'NONE',  ( -2.229367062500000163, 3.520833334698929118, -3.861377020970580443 ) ) ;
#23910 = DIRECTION ( 'NONE',  ( -0.000000000000000000, 1.000000000000000000, -0.000000000000000000 ) ) ;
#23911 = CARTESIAN_POINT ( 'NONE',  ( 2.229367062500001939, -65.22916666530106511, 3.861377020970579999 ) ) ;
#23912 = CARTESIAN_POINT ( 'NONE',  ( 1.060575238724906964E-15, -17.62499999726881583, 5.773502691896257311 ) ) ;
#23913 = CARTESIAN_POINT ( 'NONE',  ( -2.499999999999996447, 6.166666666666667851, 4.330127018922195425 ) ) ;
#23914 = CARTESIAN_POINT ( 'NONE',  ( 0.000000000000000000, -120.0000000000000000, 0.000000000000000000 ) ) ;
#23915 = DIRECTION ( 'NONE',  ( -0.000000000000000000, 1.000000000000000000, -0.000000000000000000 ) ) ;
#23916 = CARTESIAN_POINT ( 'NONE',  ( -5.000000000000000000, -105.8749999972688158, 0.000000000000000000 ) ) ;
#23917 = DIRECTION ( 'NONE',  ( -0.000000000000000000, 1.000000000000000000, -0.000000000000000000 ) ) ;
#23918 = CARTESIAN_POINT ( 'NONE',  ( -3.152548672688508926E-16, -40.56249999863440081, -5.148502694627439702 ) ) ;
#23919 = CARTESIAN_POINT ( 'NONE',  ( -4.458734124999999437, -29.64583333196773651, -2.574251347313719407 ) ) ;
#23920 = CARTESIAN_POINT ( 'NONE',  ( -4.458734124999999437, 7.354166668032259047, -2.574251347313719407 ) ) ;
#23921 =( BOUNDED_CURVE ( )  B_SPLINE_CURVE ( 2, ( #11159, #41688, #25640, #45256, #20821, #16312, #35933, #11476, #50717 ),
 .UNSPECIFIED., .F., .F. ) 
 B_SPLINE_CURVE_WITH_KNOTS ( ( 3, 2, 2, 2, 3 ),
 ( 0.4645833333333333481, 0.4652777777777777901, 0.4666666666666666741, 0.4680555555555555580, 0.4687500000000000000 ),
 .UNSPECIFIED. ) 
 CURVE ( )  GEOMETRIC_REPRESENTATION_ITEM ( )  RATIONAL_B_SPLINE_CURVE ( ( 0.9330127018922194093, 0.9330127018922194093, 1.000000000000000000, 0.8660254037844387076, 1.000000000000000000, 0.8660254037844387076, 1.000000000000000000, 0.9330127018922194093, 0.9330127018922194093 ) ) 
 REPRESENTATION_ITEM ( '' )  );
#23922 = LINE ( 'NONE', #28430, #58624 ) ;
#23923 = CARTESIAN_POINT ( 'NONE',  ( -2.499999999999996447, 26.16666666666666430, 4.330127018922195425 ) ) ;
#23924 = CARTESIAN_POINT ( 'NONE',  ( -3.535533905932737309, -147.7500000027311842, -3.535533905932738197 ) ) ;
#23925 = CARTESIAN_POINT ( 'NONE',  ( 4.458734124999998549, -107.9791666653010651, -2.574251347313721627 ) ) ;
#23926 = CARTESIAN_POINT ( 'NONE',  ( 9.457646018065525792E-16, -37.06249999863440792, 5.148502694627439702 ) ) ;
#23927 = CARTESIAN_POINT ( 'NONE',  ( 5.000000000000000000, -69.29166666393548724, -2.886751345948129988 ) ) ;
#23928 = CARTESIAN_POINT ( 'NONE',  ( -54.64476657466781973, -149.0625000013656063, -4.444560631937228834 ) ) ;
#23929 = CARTESIAN_POINT ( 'NONE',  ( 5.000000000000000888, -142.9375000000000284, -2.071067811865475505 ) ) ;
#23930 = EDGE_CURVE ( 'NONE', #26541, #40520, #63472, .T. ) ;
#23931 = CARTESIAN_POINT ( 'NONE',  ( -2.229367062499996610, -73.39583333196773651, 3.861377020970582219 ) ) ;
#23932 = CARTESIAN_POINT ( 'NONE',  ( 4.458734124999999437, -167.6875000013655779, 0.000000000000000000 ) ) ;
#23933 = CARTESIAN_POINT ( 'NONE',  ( -3.152548672688508926E-16, -29.56249999863440436, -5.148502694627439702 ) ) ;
#23934 = CARTESIAN_POINT ( 'NONE',  ( -1.339745962155613812, -28.08034179853028789, -5.000000000000000000 ) ) ;
#23935 = FACE_OUTER_BOUND ( 'NONE', #10407, .T. ) ;
#23936 = CARTESIAN_POINT ( 'NONE',  ( 5.000000000000000000, -20.49999999999999645, -6.123233995736766282E-16 ) ) ;
#23937 = CARTESIAN_POINT ( 'NONE',  ( 4.458734124999999437, -144.5000000013656063, 1.846868145590737864 ) ) ;
#23938 = ORIENTED_EDGE ( 'NONE', *, *, #5823, .F. ) ;
#23939 = CARTESIAN_POINT ( 'NONE',  ( -4.458734124999998549, 28.52083333469892423, 2.574251347313722516 ) ) ;
#23940 = CARTESIAN_POINT ( 'NONE',  ( -2.499999999999996447, -78.70833333060214443, 4.330127018922195425 ) ) ;
#23941 = CARTESIAN_POINT ( 'NONE',  ( 2.229367062499998831, -54.89583333196773651, -3.861377020970580887 ) ) ;
#23942 = CARTESIAN_POINT ( 'NONE',  ( -2.500000000000000444, 27.95833333606451987, -4.330127018922193649 ) ) ;
#23943 = CARTESIAN_POINT ( 'NONE',  ( 5.000000000000000000, 13.70833333606451987, -2.886751345948130876 ) ) ;
#23944 = CARTESIAN_POINT ( 'NONE',  ( -5.000000000000000000, 17.00000000000000000, 0.000000000000000000 ) ) ;
#23945 = DIRECTION ( 'NONE',  ( -0.000000000000000000, 1.000000000000000000, -0.000000000000000000 ) ) ;
#23946 = CARTESIAN_POINT ( 'NONE',  ( 4.458734125000001214, -3.895833331967739621, 2.574251347313718519 ) ) ;
#23947 = CARTESIAN_POINT ( 'NONE',  ( -2.499999999999996447, 4.291666669397852907, 4.330127018922195425 ) ) ;
#23948 = CARTESIAN_POINT ( 'NONE',  ( -2.229367062500000163, 10.27083333469892779, -3.861377020970580443 ) ) ;
#23949 = CARTESIAN_POINT ( 'NONE',  ( 5.000000000000000888, -12.58333333333333570, 2.886751345948126879 ) ) ;
#23950 = CARTESIAN_POINT ( 'NONE',  ( 4.458734125000001214, -53.89583333196773651, 2.574251347313718519 ) ) ;
#23951 = CARTESIAN_POINT ( 'NONE',  ( -8.190561711645485556E-16, -159.9375000013655779, 4.458734124999999437 ) ) ;
#23952 = EDGE_CURVE ( 'NONE', #60902, #20484, #61054, .T. ) ;
#23953 = CARTESIAN_POINT ( 'NONE',  ( 2.500000000000002220, -52.54166666393548013, 4.330127018922192761 ) ) ;
#23954 = VERTEX_POINT ( 'NONE', #13431 ) ;
#23955 = CARTESIAN_POINT ( 'NONE',  ( -4.458734124999999437, 2.437500001365593860, 0.000000000000000000 ) ) ;
#23956 = ORIENTED_EDGE ( 'NONE', *, *, #42064, .F. ) ;
#23958 = CARTESIAN_POINT ( 'NONE',  ( -2.500000000000000444, -12.16666666666666607, -4.330127018922193649 ) ) ;
#23957 = CYLINDRICAL_SURFACE ( 'NONE', #13223, 5.000000000000000000 ) ;
#23959 = CARTESIAN_POINT ( 'NONE',  ( 3.152801135295367541, -160.3125000013656063, -3.152801135295367541 ) ) ;
#23960 = ORIENTED_EDGE ( 'NONE', *, *, #4725, .T. ) ;
#23961 = EDGE_CURVE ( 'NONE', #26446, #32199, #6005, .T. ) ;
#23962 = CARTESIAN_POINT ( 'NONE',  ( 1.975475456537005874E-15, -83.74999999999998579, 5.000000000000000000 ) ) ;
#23963 = CARTESIAN_POINT ( 'NONE',  ( -54.60164318462004474, -133.3750000000000284, -4.984105922594373794 ) ) ;
#23964 = CARTESIAN_POINT ( 'NONE',  ( 2.499999999999998668, -53.20833333060213732, -4.330127018922193649 ) ) ;
#23965 = CARTESIAN_POINT ( 'NONE',  ( -4.458734124999999437, -38.56249999863440081, 0.000000000000000000 ) ) ;
#23966 = ORIENTED_EDGE ( 'NONE', *, *, #44808, .T. ) ;
#23967 = VECTOR ( 'NONE', #44946, 1000.000000000000114 ) ;
#23968 = CARTESIAN_POINT ( 'NONE',  ( 3.535533905932738197, -143.0000000027311842, -3.535533905932738197 ) ) ;
#23969 = EDGE_CURVE ( 'NONE', #22435, #24993, #3930, .T. ) ;
#23970 = CARTESIAN_POINT ( 'NONE',  ( 4.458734125000001214, 18.10416666803225638, 2.574251347313718519 ) ) ;
#23971 = CARTESIAN_POINT ( 'NONE',  ( 1.339745962155615144, -24.58034179853029499, 4.999999999999999112 ) ) ;
#23972 = ORIENTED_EDGE ( 'NONE', *, *, #61683, .F. ) ;
#23973 = EDGE_CURVE ( 'NONE', #55402, #59225, #14993, .T. ) ;
#23974 = CARTESIAN_POINT ( 'NONE',  ( -4.458734124999999437, -83.56249999863439371, 0.000000000000000000 ) ) ;
#23975 = CARTESIAN_POINT ( 'NONE',  ( -52.53715891517739323, -127.5625000027312552, -4.819101127000233298 ) ) ;
#23976 = CARTESIAN_POINT ( 'NONE',  ( 1.975475456537005874E-15, -40.74999999999999289, 5.000000000000000000 ) ) ;
#23977 = CARTESIAN_POINT ( 'NONE',  ( 1.975475456537005874E-15, -102.7499999999999858, 5.000000000000000000 ) ) ;
#23978 = CARTESIAN_POINT ( 'NONE',  ( 4.458734124999999437, -58.81249999863440081, -5.460374474430324690E-16 ) ) ;
#23979 = CARTESIAN_POINT ( 'NONE',  ( 1.975475456537005874E-15, -11.62499999726881406, 5.000000000000000000 ) ) ;
#23980 = CARTESIAN_POINT ( 'NONE',  ( 4.458734124999999437, 22.18750000136559564, -5.460374474430324690E-16 ) ) ;
#23981 = CARTESIAN_POINT ( 'NONE',  ( 5.000000000000000000, -102.2916666639354588, -2.886751345948130876 ) ) ;
#23982 = FACE_OUTER_BOUND ( 'NONE', #3111, .T. ) ;
#23983 = CARTESIAN_POINT ( 'NONE',  ( -4.458734124999999437, -46.64583333196774362, -2.574251347313719407 ) ) ;
#23984 = CARTESIAN_POINT ( 'NONE',  ( 1.060575238724906964E-15, -1.624999997268814500, 5.773502691896257311 ) ) ;
#23985 = CARTESIAN_POINT ( 'NONE',  ( 0.000000000000000000, -170.0000000000000000, 0.000000000000000000 ) ) ;
#23986 = DIRECTION ( 'NONE',  ( -0.000000000000000000, 1.000000000000000000, -0.000000000000000000 ) ) ;
#23987 = CARTESIAN_POINT ( 'NONE',  ( -4.458734124999998549, -82.47916666530106511, 2.574251347313722516 ) ) ;
#23988 = CARTESIAN_POINT ( 'NONE',  ( 2.229367062500001939, -109.9791666653010651, 3.861377020970579999 ) ) ;
#23989 = CARTESIAN_POINT ( 'NONE',  ( 4.458734124999999437, -13.06249999863440259, -5.460374474430324690E-16 ) ) ;
#23990 = ORIENTED_EDGE ( 'NONE', *, *, #91, .T. ) ;
#23991 = CARTESIAN_POINT ( 'NONE',  ( -1.339745962155610925, -16.66965819600733312, 5.000000000000000000 ) ) ;
#23992 = CARTESIAN_POINT ( 'NONE',  ( 4.458734124999999437, -97.81249999863440792, -5.460374474430324690E-16 ) ) ;
#23993 = CARTESIAN_POINT ( 'NONE',  ( -5.000000000000000888, -161.6875000027312126, -2.071067811865475949 ) ) ;
#23994 = CARTESIAN_POINT ( 'NONE',  ( 9.457646018065525792E-16, -92.31249999863439371, 5.148502694627439702 ) ) ;
#23995 = EDGE_CURVE ( 'NONE', #39107, #58623, #49561, .T. ) ;
#23996 = CARTESIAN_POINT ( 'NONE',  ( 5.000000000000000000, -53.37499999726881583, -6.123233995736766282E-16 ) ) ;
#23997 = DIRECTION ( 'NONE',  ( -0.000000000000000000, 1.000000000000000000, -0.000000000000000000 ) ) ;
#23998 =( BOUNDED_CURVE ( )  B_SPLINE_CURVE ( 2, ( #62102, #47301, #52452, #47607, #2937, #42778, #33144, #18019, #56336 ),
 .UNSPECIFIED., .F., .F. ) 
 B_SPLINE_CURVE_WITH_KNOTS ( ( 3, 2, 2, 2, 3 ),
 ( 0.5937500000000000000, 0.5944444444444444420, 0.5958333333333333259, 0.5972222222222222099, 0.5979166666666666519 ),
 .UNSPECIFIED. ) 
 CURVE ( )  GEOMETRIC_REPRESENTATION_ITEM ( )  RATIONAL_B_SPLINE_CURVE ( ( 0.9330127018922194093, 0.9330127018922194093, 1.000000000000000000, 0.8660254037844387076, 1.000000000000000000, 0.8660254037844387076, 1.000000000000000000, 0.9330127018922194093, 0.9330127018922194093 ) ) 
 REPRESENTATION_ITEM ( '' )  );
#23999 = CARTESIAN_POINT ( 'NONE',  ( -57.19623071787017210, -131.3750000013656347, 4.297418129356382899 ) ) ;
#24000 = CARTESIAN_POINT ( 'NONE',  ( -59.59170313451810586, -148.5000000013655779, 1.485763867205729394 ) ) ;
#24001 = CARTESIAN_POINT ( 'NONE',  ( 4.458734124999999437, -15.81249999863440436, -5.460374474430324690E-16 ) ) ;
#24002 = CARTESIAN_POINT ( 'NONE',  ( 4.458734124999999437, 13.93750000136559386, -5.460374474430324690E-16 ) ) ;
#24003 = CARTESIAN_POINT ( 'NONE',  ( -4.458734124999999437, -57.64583333196773651, -2.574251347313719407 ) ) ;
#24004 = CARTESIAN_POINT ( 'NONE',  ( -2.499999999999996447, -68.83333333333332860, 4.330127018922195425 ) ) ;
#24005 = CARTESIAN_POINT ( 'NONE',  ( -3.152548672688508926E-16, -15.56249999863440614, -5.148502694627439702 ) ) ;
#24006 = CARTESIAN_POINT ( 'NONE',  ( 0.000000000000000000, 0.000000000000000000, -0.5251556536572846712 ) ) ;
#24007 = CARTESIAN_POINT ( 'NONE',  ( 2.071067811865476394, -155.1875000000000000, 5.000000000000000000 ) ) ;
#24008 = ORIENTED_EDGE ( 'NONE', *, *, #6348, .T. ) ;
#24009 = CARTESIAN_POINT ( 'NONE',  ( -2.229367062500000163, -42.72916666530107932, -3.861377020970580443 ) ) ;
#24010 = CARTESIAN_POINT ( 'NONE',  ( 5.000000000000000000, -77.50000000000000000, -6.123233995736766282E-16 ) ) ;
#24011 = CARTESIAN_POINT ( 'NONE',  ( 1.975475456537005874E-15, -66.74999999999998579, 5.000000000000000000 ) ) ;
#24012 = CARTESIAN_POINT ( 'NONE',  ( -5.000000000000000000, 27.04166666939785202, -2.886751345948128211 ) ) ;
#24013 = CARTESIAN_POINT ( 'NONE',  ( -4.458734124999998549, -87.22916666530107932, 2.574251347313722516 ) ) ;
#24014 = CARTESIAN_POINT ( 'NONE',  ( -2.229367062499996610, 16.60416666803225638, 3.861377020970582219 ) ) ;
#24015 = AXIS2_PLACEMENT_3D ( 'NONE', #20839, #11176, #30799 ) ;
#24016 = CARTESIAN_POINT ( 'NONE',  ( -3.152548672688508926E-16, 8.437500001365595637, -5.148502694627439702 ) ) ;
#24017 =( BOUNDED_CURVE ( )  B_SPLINE_CURVE ( 2, ( #1818, #21422, #60669, #16592, #11749, #31367, #22056, #41648, #46812 ),
 .UNSPECIFIED., .F., .F. ) 
 B_SPLINE_CURVE_WITH_KNOTS ( ( 3, 2, 2, 2, 3 ),
 ( 0.6249999999999996669, 0.6291666666666663188, 0.6333333333333328596, 0.6374999999999995115, 0.6416666666666662744 ),
 .UNSPECIFIED. ) 
 CURVE ( )  GEOMETRIC_REPRESENTATION_ITEM ( )  RATIONAL_B_SPLINE_CURVE ( ( 1.000000000000005995, 0.9238795325112806323, 1.000000000000000000, 0.9238795325112867385, 1.000000000000000000, 0.9238795325112867385, 1.000000000000000000, 0.9238795325112948431, 0.9999999999999918954 ) ) 
 REPRESENTATION_ITEM ( '' )  );
#24018 = CARTESIAN_POINT ( 'NONE',  ( 1.975475456537005874E-15, 7.249999999999998224, 5.000000000000000000 ) ) ;
#24019 = CARTESIAN_POINT ( 'NONE',  ( -5.000000000000000000, 11.91666666666666607, -2.886751345948128211 ) ) ;
#24020 = CARTESIAN_POINT ( 'NONE',  ( -2.499999999999996447, -69.83333333333332860, 4.330127018922195425 ) ) ;
#24021 = CARTESIAN_POINT ( 'NONE',  ( 2.500000000000002220, 15.45833333606451987, 4.330127018922192761 ) ) ;
#24022 = ORIENTED_EDGE ( 'NONE', *, *, #38220, .F. ) ;
#24023 = CARTESIAN_POINT ( 'NONE',  ( 5.000000000000000888, -102.5833333333333286, 2.886751345948126879 ) ) ;
#24024 = PRODUCT_DEFINITION_SHAPE ( 'NONE', 'NONE',  #63680 ) ;
#24025 = EDGE_LOOP ( 'NONE', ( #53832, #35031, #420, #9310 ) ) ;
#24026 = CARTESIAN_POINT ( 'NONE',  ( -5.000000000000000000, -79.87499999726881583, 0.000000000000000000 ) ) ;
#24028 = CARTESIAN_POINT ( 'NONE',  ( -5.000000000000000000, -36.00000000000000711, 0.000000000000000000 ) ) ;
#24027 = DIRECTION ( 'NONE',  ( 0.000000000000000000, -0.000000000000000000, -1.000000000000000000 ) ) ;
#24029 = CARTESIAN_POINT ( 'NONE',  ( 9.457646018065525792E-16, -38.06249999863441502, 5.148502694627439702 ) ) ;
#24030 = ADVANCED_FACE ( 'NONE', ( #52979 ), #8920, .T. ) ;
#24031 = CARTESIAN_POINT ( 'NONE',  ( -5.000000000000000000, -34.87499999726881583, 0.000000000000000000 ) ) ;
#24032 = EDGE_CURVE ( 'NONE', #18740, #43422, #32664, .T. ) ;
#24034 = ORIENTED_EDGE ( 'NONE', *, *, #15413, .T. ) ;
#24033 = CARTESIAN_POINT ( 'NONE',  ( -2.229367062499996610, -65.14583333196773651, 3.861377020970582219 ) ) ;
#24035 = CARTESIAN_POINT ( 'NONE',  ( -59.29741812935640155, -149.8750000013655779, -2.196230717870135685 ) ) ;
#24036 = CARTESIAN_POINT ( 'NONE',  ( 2.229367062499998831, -13.64583333196774184, -3.861377020970580887 ) ) ;
#24038 = ORIENTED_EDGE ( 'NONE', *, *, #1270, .T. ) ;
#24037 = CARTESIAN_POINT ( 'NONE',  ( -4.458734124999998549, -12.47916666530107221, 2.574251347313722516 ) ) ;
#24039 = EDGE_CURVE ( 'NONE', #37137, #30949, #28845, .T. ) ;
#24040 = CARTESIAN_POINT ( 'NONE',  ( 5.000000000000000000, -77.41666666666665719, -2.886751345948129988 ) ) ;
#24041 = CARTESIAN_POINT ( 'NONE',  ( -50.70258187064364108, -136.1250000013656063, 2.196230717870141014 ) ) ;
#24042 = CARTESIAN_POINT ( 'NONE',  ( -4.458734124999998549, -59.47916666530106511, 2.574251347313722516 ) ) ;
#24043 = CARTESIAN_POINT ( 'NONE',  ( -4.999999999999999112, -82.79166666393547303, 2.886751345948131764 ) ) ;
#24045 = ORIENTED_EDGE ( 'NONE', *, *, #55494, .T. ) ;
#24044 = CARTESIAN_POINT ( 'NONE',  ( -6.031010364368858512E-14, 3.375000002731183280, 5.000000000000000000 ) ) ;
#24046 = CARTESIAN_POINT ( 'NONE',  ( -52.53715891517739323, -146.4375000000000000, -4.819101127000233298 ) ) ;
#24047 = ADVANCED_FACE ( 'NONE', ( #8302 ), #47524, .T. ) ;
#24048 = CARTESIAN_POINT ( 'NONE',  ( 4.458734125000001214, -24.14583333196773651, 2.574251347313718519 ) ) ;
#24049 = EDGE_CURVE ( 'NONE', #31719, #48295, #1501, .T. ) ;
#24051 = VERTEX_POINT ( 'NONE', #60605 ) ;
#24050 = CARTESIAN_POINT ( 'NONE',  ( -2.229367062499996610, -60.39583333196774362, 3.861377020970582219 ) ) ;
#24052 = CARTESIAN_POINT ( 'NONE',  ( 2.730187237215162345E-16, -165.4375000013655779, -4.458734124999999437 ) ) ;
#24053 = ADVANCED_FACE ( 'NONE', ( #20397 ), #789, .T. ) ;
#24054 = CARTESIAN_POINT ( 'NONE',  ( 4.458734124999998549, -104.9791666653010651, -2.574251347313721627 ) ) ;
#24055 = CARTESIAN_POINT ( 'NONE',  ( -9.184850993605147944E-16, -167.3750000027312126, 5.000000000000000000 ) ) ;
#24056 = ORIENTED_EDGE ( 'NONE', *, *, #31015, .F. ) ;
#24057 = EDGE_CURVE ( 'NONE', #44922, #45518, #39221, .T. ) ;
#24058 = CARTESIAN_POINT ( 'NONE',  ( -56.48576386720575471, -150.0000000013656063, -4.591703134518078322 ) ) ;
#24059 = CARTESIAN_POINT ( 'NONE',  ( -52.53715891517739323, -138.5625000027312126, -4.819101127000233298 ) ) ;
#24060 = CARTESIAN_POINT ( 'NONE',  ( 4.458734125000000326, -37.89583333196773651, 2.574251347313718519 ) ) ;
#24061 = EDGE_CURVE ( 'NONE', #33389, #40505, #5609, .T. ) ;
#24062 = EDGE_CURVE ( 'NONE', #4593, #25319, #8068, .T. ) ;
#24063 = CARTESIAN_POINT ( 'NONE',  ( 2.500000000000002220, 18.33333333333333215, 4.330127018922192761 ) ) ;
#24064 = CARTESIAN_POINT ( 'NONE',  ( 2.229367062500001939, -12.97916666530107221, 3.861377020970579999 ) ) ;
#24065 = CARTESIAN_POINT ( 'NONE',  ( 4.458734124999998549, -99.97916666530106511, -2.574251347313721627 ) ) ;
#24066 = AXIS2_PLACEMENT_3D ( 'NONE', #39918, #34144, #19672 ) ;
#24067 = CARTESIAN_POINT ( 'NONE',  ( -1.846868145590734756, -145.3750000013656347, -4.458734125000000326 ) ) ;
#24068 = CARTESIAN_POINT ( 'NONE',  ( -4.458734124999999437, -25.56249999863440792, 0.000000000000000000 ) ) ;
#24069 = CARTESIAN_POINT ( 'NONE',  ( -50.18089887299976937, -139.8125000027312126, 2.462841084822397164 ) ) ;
#24070 = CARTESIAN_POINT ( 'NONE',  ( -58.39396692619412477, -134.4375000013656063, 2.891590998281057701 ) ) ;
#24071 = CARTESIAN_POINT ( 'NONE',  ( -2.229367062499996610, -68.39583333196773651, 3.861377020970582219 ) ) ;
#24072 = CARTESIAN_POINT ( 'NONE',  ( 2.500000000000002220, -43.66666666666665719, 4.330127018922192761 ) ) ;
#24073 = CARTESIAN_POINT ( 'NONE',  ( -5.000000000000000000, -0.8749999972688139449, 0.000000000000000000 ) ) ;
#24074 = CARTESIAN_POINT ( 'NONE',  ( 4.458734124999999437, -140.4375000013656063, 0.000000000000000000 ) ) ;
#24075 = CARTESIAN_POINT ( 'NONE',  ( 4.458734125000000326, 2.854166668032259491, 2.574251347313718519 ) ) ;
#24076 =( BOUNDED_CURVE ( )  B_SPLINE_CURVE ( 2, ( #38548, #3532, #8977, #23141, #58179, #14424, #42749, #53039, #62392 ),
 .UNSPECIFIED., .F., .F. ) 
 B_SPLINE_CURVE_WITH_KNOTS ( ( 3, 2, 2, 2, 3 ),
 ( 0.2339285714285714302, 0.2345238095238095233, 0.2357142857142857095, 0.2369047619047618958, 0.2374999999999999889 ),
 .UNSPECIFIED. ) 
 CURVE ( )  GEOMETRIC_REPRESENTATION_ITEM ( )  RATIONAL_B_SPLINE_CURVE ( ( 0.9330127018922194093, 0.9330127018922194093, 1.000000000000000000, 0.8660254037844387076, 1.000000000000000000, 0.8660254037844387076, 1.000000000000000000, 0.9330127018922194093, 0.9330127018922194093 ) ) 
 REPRESENTATION_ITEM ( '' )  );
#24077 = VERTEX_POINT ( 'NONE', #1435 ) ;
#24078 = CARTESIAN_POINT ( 'NONE',  ( -4.999999999999998224, 2.083333333333333037, 2.886751345948131764 ) ) ;
#24079 = CARTESIAN_POINT ( 'NONE',  ( 1.975475456537005874E-15, 16.37500000273118417, 5.000000000000000000 ) ) ;
#24081 = CARTESIAN_POINT ( 'NONE',  ( -4.458734124999998549, -29.22916666530107221, 2.574251347313722516 ) ) ;
#24080 = CARTESIAN_POINT ( 'NONE',  ( -4.999999999999999112, -97.91666666666664298, 2.886751345948131764 ) ) ;
#24082 = CARTESIAN_POINT ( 'NONE',  ( 5.000000000000000888, -73.58333333333332860, 2.886751345948126879 ) ) ;
#24083 = CARTESIAN_POINT ( 'NONE',  ( -3.152548672688508926E-16, -74.81249999863439371, -5.148502694627439702 ) ) ;
#24084 = CARTESIAN_POINT ( 'NONE',  ( -4.458734124999997661, 20.52083333469892423, 2.574251347313722516 ) ) ;
#24085 = CARTESIAN_POINT ( 'NONE',  ( -2.500000000000000444, -102.0416666639354588, -4.330127018922193649 ) ) ;
#24086 = CARTESIAN_POINT ( 'NONE',  ( -58.39396692619412477, -141.4375000013656063, 2.891590998281057701 ) ) ;
#24087 = CARTESIAN_POINT ( 'NONE',  ( -2.229367062500000163, 2.520833334698928230, -3.861377020970580443 ) ) ;
#24088 = CARTESIAN_POINT ( 'NONE',  ( -3.152548672688508926E-16, 29.18750000136559208, -5.148502694627439702 ) ) ;
#24089 = CARTESIAN_POINT ( 'NONE',  ( 2.229367062500001939, -45.22916666530106511, 3.861377020970579999 ) ) ;
#24090 = CARTESIAN_POINT ( 'NONE',  ( 1.975475456537005874E-15, -55.74999999999999289, 5.000000000000000000 ) ) ;
#24091 = CARTESIAN_POINT ( 'NONE',  ( -2.229367062500000163, 1.520833334698927564, -3.861377020970580443 ) ) ;
#24092 = ORIENTED_EDGE ( 'NONE', *, *, #33834, .T. ) ;
#24093 = CARTESIAN_POINT ( 'NONE',  ( -2.229367062499996610, -27.39583333196774007, 3.861377020970582219 ) ) ;
#24094 = CARTESIAN_POINT ( 'NONE',  ( -3.152801135295367096, -157.0625000013656063, -3.152801135295367541 ) ) ;
#24095 = CARTESIAN_POINT ( 'NONE',  ( -4.458734124999999437, -71.39583333196773651, -2.574251347313719407 ) ) ;
#24096 = CARTESIAN_POINT ( 'NONE',  ( -4.999999999999999112, -105.7916666639354588, 2.886751345948131764 ) ) ;
#24097 = CARTESIAN_POINT ( 'NONE',  ( 4.458734124999998549, 27.27083333469892423, -2.574251347313721627 ) ) ;
#24098 = CARTESIAN_POINT ( 'NONE',  ( 0.04725809328185039127, -9.175759667312528123, -8.057670357645362103 ) ) ;
#24099 = CARTESIAN_POINT ( 'NONE',  ( 9.457646018065525792E-16, -110.3124999986343937, 5.148502694627439702 ) ) ;
#24100 = CARTESIAN_POINT ( 'NONE',  ( 9.457646018065525792E-16, -70.31249999863439371, 5.148502694627439702 ) ) ;
#24101 = CARTESIAN_POINT ( 'NONE',  ( 5.000000000000000000, -54.41666666666666430, -2.886751345948129988 ) ) ;
#24102 = CARTESIAN_POINT ( 'NONE',  ( -2.500000000000000444, -22.16666666666666785, -4.330127018922193649 ) ) ;
#24103 = CARTESIAN_POINT ( 'NONE',  ( -5.000000000000000000, 29.04166666939784847, -2.886751345948128211 ) ) ;
#24104 = ORIENTED_EDGE ( 'NONE', *, *, #35780, .F. ) ;
#24105 = CARTESIAN_POINT ( 'NONE',  ( 4.458734124999999437, -169.5625000013655779, 0.000000000000000000 ) ) ;
#24106 =( BOUNDED_CURVE ( )  B_SPLINE_CURVE ( 2, ( #906, #63620, #20514, #35620, #39155, #45264, #49127, #15361, #35298 ),
 .UNSPECIFIED., .F., .F. ) 
 B_SPLINE_CURVE_WITH_KNOTS ( ( 3, 2, 2, 2, 3 ),
 ( 0.001785714285714286092, 0.002380952380952381167, 0.003571428571428571317, 0.004761904761904762334, 0.005357142857142858060 ),
 .UNSPECIFIED. ) 
 CURVE ( )  GEOMETRIC_REPRESENTATION_ITEM ( )  RATIONAL_B_SPLINE_CURVE ( ( 0.9330127018922194093, 0.9330127018922194093, 1.000000000000000000, 0.8660254037844387076, 1.000000000000000000, 0.8660254037844387076, 1.000000000000000000, 0.9330127018922191873, 0.9330127018922192983 ) ) 
 REPRESENTATION_ITEM ( '' )  );
#24107 = CARTESIAN_POINT ( 'NONE',  ( 2.499999999999998668, -6.208333330602149758, -4.330127018922193649 ) ) ;
#24108 = CARTESIAN_POINT ( 'NONE',  ( -2.499999999999996447, -12.83333333333333570, 4.330127018922195425 ) ) ;
#24109 = CARTESIAN_POINT ( 'NONE',  ( 4.458734124999998549, -16.72916666530107577, -2.574251347313721627 ) ) ;
#24110 = CARTESIAN_POINT ( 'NONE',  ( -2.229367062500000163, -76.47916666530106511, -3.861377020970580443 ) ) ;
#24111 = AXIS2_PLACEMENT_3D ( 'NONE', #23810, #19285, #38287 ) ;
#24112 = CARTESIAN_POINT ( 'NONE',  ( 3.152801135295366208, -168.8125000013656063, 3.152801135295367985 ) ) ;
#24113 = CARTESIAN_POINT ( 'NONE',  ( 2.499999999999998668, -17.20833333060214443, -4.330127018922193649 ) ) ;
#24115 = VERTEX_POINT ( 'NONE', #49974 ) ;
#24114 = CARTESIAN_POINT ( 'NONE',  ( -4.458734124999999437, -49.39583333196773651, -2.574251347313719407 ) ) ;
#24117 = EDGE_LOOP ( 'NONE', ( #22542, #30415, #58304, #31811 ) ) ;
#24116 = CARTESIAN_POINT ( 'NONE',  ( -3.152548672688508926E-16, 2.187500001365593416, -5.148502694627439702 ) ) ;
#24118 = CARTESIAN_POINT ( 'NONE',  ( -52.80376928212989185, -151.8750000013655779, -4.297418129356378458 ) ) ;
#24119 = CARTESIAN_POINT ( 'NONE',  ( 5.000000000000000888, -58.58333333333333570, 2.886751345948126879 ) ) ;
#24120 = CARTESIAN_POINT ( 'NONE',  ( -4.458734124999999437, -158.1875000013655779, -5.460374474430324690E-16 ) ) ;
#24121 = CARTESIAN_POINT ( 'NONE',  ( -2.229367062500000163, -42.72916666530107932, -3.861377020970580443 ) ) ;
#24122 = CARTESIAN_POINT ( 'NONE',  ( -2.499999999999996447, -64.83333333333332860, 4.330127018922195425 ) ) ;
#24123 = CARTESIAN_POINT ( 'NONE',  ( 3.061616997868383141E-16, -160.7500000000000000, -5.000000000000000000 ) ) ;
#24124 = CARTESIAN_POINT ( 'NONE',  ( 1.339745962155615144, 5.419658201469705894, 4.999999999999999112 ) ) ;
#24125 = CARTESIAN_POINT ( 'NONE',  ( -54.64476657466781973, -128.0625000013656063, -4.444560631937228834 ) ) ;
#24126 = CARTESIAN_POINT ( 'NONE',  ( -4.458734124999998549, -3.479166665301069994, 2.574251347313722516 ) ) ;
#24127 = CARTESIAN_POINT ( 'NONE',  ( -4.458734124999999437, -45.64583333196774362, -2.574251347313719407 ) ) ;
#24128 = DIRECTION ( 'NONE',  ( -0.000000000000000000, 1.000000000000000000, -0.000000000000000000 ) ) ;
#24129 = CARTESIAN_POINT ( 'NONE',  ( -8.190561711645485556E-16, -148.6875000013656063, 4.458734124999999437 ) ) ;
#24130 = CARTESIAN_POINT ( 'NONE',  ( -4.458734124999998549, -87.47916666530107932, 2.574251347313722516 ) ) ;
#24131 = CARTESIAN_POINT ( 'NONE',  ( -51.75738570946856498, -142.7500000000000284, 3.805975901505576964 ) ) ;
#24132 = VERTEX_POINT ( 'NONE', #5925 ) ;
#24133 = EDGE_CURVE ( 'NONE', #51592, #39210, #6244, .T. ) ;
#24134 = CARTESIAN_POINT ( 'NONE',  ( -57.46284108482265651, -151.9375000000000284, 4.819101127000238627 ) ) ;
#24135 = CARTESIAN_POINT ( 'NONE',  ( -58.24261429053147765, -151.3750000027312126, -3.805975901505573855 ) ) ;
#24136 = VERTEX_POINT ( 'NONE', #16204 ) ;
#24137 = EDGE_CURVE ( 'NONE', #55402, #25522, #36146, .T. ) ;
#24138 = LINE ( 'NONE', #33471, #7147 ) ;
#24139 = CARTESIAN_POINT ( 'NONE',  ( 9.457646018065525792E-16, -13.31249999863440259, 5.148502694627439702 ) ) ;
#24140 = CARTESIAN_POINT ( 'NONE',  ( -1.339745962155610925, -34.79465819873851729, 5.000000000000000000 ) ) ;
#24141 = CARTESIAN_POINT ( 'NONE',  ( 2.229367062500001939, -2.979166665301069550, 3.861377020970579999 ) ) ;
#24142 = CARTESIAN_POINT ( 'NONE',  ( -2.499999999999996447, 4.291666669397852907, 4.330127018922195425 ) ) ;
#24143 = CARTESIAN_POINT ( 'NONE',  ( 4.458734124999999437, -152.4375000013655779, 0.000000000000000000 ) ) ;
#24144 = CARTESIAN_POINT ( 'NONE',  ( 2.229367062500001939, 21.77083333469892779, 3.861377020970579999 ) ) ;
#24145 = ORIENTED_EDGE ( 'NONE', *, *, #13935, .T. ) ;
#24146 = CARTESIAN_POINT ( 'NONE',  ( 4.458734124999998549, -91.72916666530106511, -2.574251347313721627 ) ) ;
#24147 = CARTESIAN_POINT ( 'NONE',  ( -6.972266317189433020E-16, -34.12499999726881583, -5.000000000000000000 ) ) ;
#24148 = CARTESIAN_POINT ( 'NONE',  ( -53.33387254593733218, -153.9375000027311842, 5.149110718188519620 ) ) ;
#24149 = CARTESIAN_POINT ( 'NONE',  ( 4.458734124999999437, -11.81249999863440081, -5.460374474430324690E-16 ) ) ;
#24150 = LINE ( 'NONE', #9042, #12863 ) ;
#24151 = CARTESIAN_POINT ( 'NONE',  ( -6.972266317189433020E-16, -73.25000000000000000, -5.000000000000000000 ) ) ;
#24152 = CARTESIAN_POINT ( 'NONE',  ( -56.48576386720575471, -151.7500000013655779, -4.591703134518078322 ) ) ;
#24153 = CARTESIAN_POINT ( 'NONE',  ( -2.499999999999996447, -40.70833333060214443, 4.330127018922195425 ) ) ;
#24154 = DIRECTION ( 'NONE',  ( -0.000000000000000000, 1.000000000000000000, -0.000000000000000000 ) ) ;
#24155 = CARTESIAN_POINT ( 'NONE',  ( -4.458734124999997661, 16.77083333469892779, 2.574251347313722516 ) ) ;
#24156 = CARTESIAN_POINT ( 'NONE',  ( 1.339745962155615144, -46.58034179853028434, 4.999999999999999112 ) ) ;
#24157 = EDGE_LOOP ( 'NONE', ( #38819, #51675, #51875, #63652, #6605 ) ) ;
#24158 = CARTESIAN_POINT ( 'NONE',  ( 2.229367062500001939, 15.02083333469892779, 3.861377020970579999 ) ) ;
#24159 = CARTESIAN_POINT ( 'NONE',  ( 9.457646018065525792E-16, -61.06249999863440081, 5.148502694627439702 ) ) ;
#24160 = CARTESIAN_POINT ( 'NONE',  ( -2.229367062499996610, -10.39583333196773829, 3.861377020970582219 ) ) ;
#24161 = DIRECTION ( 'NONE',  ( 0.000000000000000000, 1.000000000000000000, 0.000000000000000000 ) ) ;
#24162 = CARTESIAN_POINT ( 'NONE',  ( 5.000000000000000000, 12.50000000000000000, -6.123233995736766282E-16 ) ) ;
#24163 = CARTESIAN_POINT ( 'NONE',  ( -1.846868145590737420, -167.7500000013655779, 4.458734124999999437 ) ) ;
#24164 = CARTESIAN_POINT ( 'NONE',  ( -49.85088928181150436, -142.5625000000000284, -1.666127454062680480 ) ) ;
#24165 = CARTESIAN_POINT ( 'NONE',  ( 2.229367062499998831, -54.64583333196773651, -3.861377020970580887 ) ) ;
#24166 = CARTESIAN_POINT ( 'NONE',  ( -5.000000000000000000, -89.95833333060214443, -2.886751345948128211 ) ) ;
#24167 = CARTESIAN_POINT ( 'NONE',  ( -57.89159099828107458, -132.9375000013656063, -3.393966926194107447 ) ) ;
#24168 = CARTESIAN_POINT ( 'NONE',  ( -1.339745962155610925, -104.6696581960073331, 5.000000000000000000 ) ) ;
#24169 = CARTESIAN_POINT ( 'NONE',  ( -4.458734124999999437, -90.56249999863440792, 0.000000000000000000 ) ) ;
#24170 = CARTESIAN_POINT ( 'NONE',  ( -1.846868145590737420, -155.0000000013656063, 4.458734124999997661 ) ) ;
#24171 = CARTESIAN_POINT ( 'NONE',  ( 2.499999999999998668, -38.33333333333332860, -4.330127018922193649 ) ) ;
#24172 = DIRECTION ( 'NONE',  ( 0.000000000000000000, 0.000000000000000000, 1.000000000000000000 ) ) ;
#24173 = CARTESIAN_POINT ( 'NONE',  ( 5.000000000000000000, -22.50000000000000000, -6.123233995736766282E-16 ) ) ;
#24174 = ORIENTED_EDGE ( 'NONE', *, *, #54198, .T. ) ;
#24175 = CARTESIAN_POINT ( 'NONE',  ( 2.229367062500001939, -103.9791666653010651, 3.861377020970579999 ) ) ;
#24176 = CARTESIAN_POINT ( 'NONE',  ( 9.457646018065525792E-16, 9.687500001365593860, 5.148502694627439702 ) ) ;
#24177 = CARTESIAN_POINT ( 'NONE',  ( -3.535250795749689387E-16, 3.750000000000000000, -5.773502691896257311 ) ) ;
#24178 = CARTESIAN_POINT ( 'NONE',  ( 4.458734124999999437, -61.81249999863440081, -5.460374474430324690E-16 ) ) ;
#24179 = EDGE_CURVE ( 'NONE', #14365, #22959, #14609, .T. ) ;
#24180 = CARTESIAN_POINT ( 'NONE',  ( -5.000000000000000000, 19.91666666666666430, -2.886751345948128211 ) ) ;
#24181 = CARTESIAN_POINT ( 'NONE',  ( 2.500000000000002220, -1.541666663935480130, 4.330127018922192761 ) ) ;
#24183 = EDGE_LOOP ( 'NONE', ( #49074, #20494, #31078, #36876 ) ) ;
#24182 = CARTESIAN_POINT ( 'NONE',  ( 2.229367062499998831, -30.64583333196773651, -3.861377020970580887 ) ) ;
#24184 = DIRECTION ( 'NONE',  ( 0.000000000000000000, 0.000000000000000000, 1.000000000000000000 ) ) ;
#24185 = CARTESIAN_POINT ( 'NONE',  ( 5.000000000000000000, 5.583333333333332149, -2.886751345948130876 ) ) ;
#24186 = CARTESIAN_POINT ( 'NONE',  ( -5.000000000000000000, -43.00000000000000000, 0.000000000000000000 ) ) ;
#24188 = CARTESIAN_POINT ( 'NONE',  ( 2.229367062500001939, -27.22916666530106866, 3.861377020970579999 ) ) ;
#24187 = CARTESIAN_POINT ( 'NONE',  ( 6.123233995736766282E-16, -170.0000000000000000, -5.000000000000000000 ) ) ;
#24189 = LINE ( 'NONE', #14215, #16302 ) ;
#24190 = CARTESIAN_POINT ( 'NONE',  ( 2.229367062500001939, -70.97916666530107932, 3.861377020970579999 ) ) ;
#24191 = CARTESIAN_POINT ( 'NONE',  ( 4.458734124999999437, -144.6875000013656063, 0.000000000000000000 ) ) ;
#24192 = CARTESIAN_POINT ( 'NONE',  ( 2.229367062500001939, -78.97916666530106511, 3.861377020970579999 ) ) ;
#24193 = CARTESIAN_POINT ( 'NONE',  ( -52.80376928212989185, -139.1250000013656063, -4.297418129356379346 ) ) ;
#24194 = AXIS2_PLACEMENT_3D ( 'NONE', #29269, #53416, #47956 ) ;
#24195 = CARTESIAN_POINT ( 'NONE',  ( 2.229367062499998831, -23.89583333196773651, -3.861377020970580887 ) ) ;
#24196 =( BOUNDED_CURVE ( )  B_SPLINE_CURVE ( 2, ( #55329, #1623, #11246, #54366, #10294, #44694, #59514, #15448, #35066 ),
 .UNSPECIFIED., .F., .F. ) 
 B_SPLINE_CURVE_WITH_KNOTS ( ( 3, 2, 2, 2, 3 ),
 ( 0.4104166666666666519, 0.4111111111111110938, 0.4124999999999999778, 0.4138888888888888618, 0.4145833333333333592 ),
 .UNSPECIFIED. ) 
 CURVE ( )  GEOMETRIC_REPRESENTATION_ITEM ( )  RATIONAL_B_SPLINE_CURVE ( ( 0.9330127018922194093, 0.9330127018922194093, 1.000000000000000000, 0.8660254037844387076, 1.000000000000000000, 0.8660254037844387076, 1.000000000000000000, 0.9330127018922167448, 0.9330127018922194093 ) ) 
 REPRESENTATION_ITEM ( '' )  );
#24197 = CARTESIAN_POINT ( 'NONE',  ( -4.999999999999999112, -67.79166666393547303, 2.886751345948131764 ) ) ;
#24198 = ORIENTED_EDGE ( 'NONE', *, *, #9399, .T. ) ;
#24199 = CARTESIAN_POINT ( 'NONE',  ( 1.339745962155615144, -93.58034179853028434, 4.999999999999999112 ) ) ;
#24200 = ORIENTED_EDGE ( 'NONE', *, *, #7932, .T. ) ;
#24201 = CARTESIAN_POINT ( 'NONE',  ( -3.152548672688508926E-16, -74.81249999863439371, -5.148502694627439702 ) ) ;
#24202 = CARTESIAN_POINT ( 'NONE',  ( -6.972266317189433020E-16, -43.25000000000000000, -5.000000000000000000 ) ) ;
#24203 =( NAMED_UNIT ( * ) SI_UNIT ( $, .STERADIAN. ) SOLID_ANGLE_UNIT ( ) );
#24204 = EDGE_LOOP ( 'NONE', ( #54006, #58617, #2233 ) ) ;
#24205 = CARTESIAN_POINT ( 'NONE',  ( -55.00000000000001421, -135.0000000000000284, -8.082903768654752241 ) ) ;
#24206 = LINE ( 'NONE', #48954, #36332 ) ;
#24207 = CARTESIAN_POINT ( 'NONE',  ( 4.458734124999998549, -59.97916666530107221, -2.574251347313721627 ) ) ;
#24208 = CARTESIAN_POINT ( 'NONE',  ( -3.152548672688508926E-16, -0.8124999986344055847, -5.148502694627439702 ) ) ;
#24209 = ORIENTED_EDGE ( 'NONE', *, *, #62983, .F. ) ;
#24210 = DIRECTION ( 'NONE',  ( 0.000000000000000000, 0.000000000000000000, 1.000000000000000000 ) ) ;
#24211 = CYLINDRICAL_SURFACE ( 'NONE', #8947, 5.000000000000000000 ) ;
#24212 = CARTESIAN_POINT ( 'NONE',  ( -4.458734124999999437, 10.68750000136559386, 0.000000000000000000 ) ) ;
#24213 = CARTESIAN_POINT ( 'NONE',  ( -59.59170313451811296, -144.5000000013656063, 1.485763867205729394 ) ) ;
#24214 = CARTESIAN_POINT ( 'NONE',  ( -1.339745962155610925, 6.330341803992665106, 5.000000000000000000 ) ) ;
#24215 = CARTESIAN_POINT ( 'NONE',  ( 2.730187237215162345E-16, -164.1875000013655779, -4.458734124999999437 ) ) ;
#24216 = VERTEX_POINT ( 'NONE', #47685 ) ;
#24217 = CARTESIAN_POINT ( 'NONE',  ( 4.458734124999998549, -74.72916666530106511, -2.574251347313721627 ) ) ;
#24218 = CARTESIAN_POINT ( 'NONE',  ( -6.972266317189433020E-16, -0.1249999972688142363, -5.000000000000000000 ) ) ;
#24219 = CARTESIAN_POINT ( 'NONE',  ( 4.458734124999998549, 3.270833334698929118, -2.574251347313721627 ) ) ;
#24220 = CARTESIAN_POINT ( 'NONE',  ( -5.000000000000000000, -42.87499999726880873, 0.000000000000000000 ) ) ;
#24221 = CARTESIAN_POINT ( 'NONE',  ( -4.458734124999999437, -64.56249999863440792, 0.000000000000000000 ) ) ;
#24222 = CARTESIAN_POINT ( 'NONE',  ( 5.000000000000000000, -27.29166666393547658, -2.886751345948129988 ) ) ;
#24223 = CARTESIAN_POINT ( 'NONE',  ( -55.39835681537999790, -141.8750000000000284, 4.984105922594378235 ) ) ;
#24224 = CYLINDRICAL_SURFACE ( 'NONE', #34698, 5.000000000000000000 ) ;
#24225 = CARTESIAN_POINT ( 'NONE',  ( 1.975475456537005874E-15, -82.62499999726878741, 5.000000000000000000 ) ) ;
#24226 = LINE ( 'NONE', #9740, #21315 ) ;
#24227 = CARTESIAN_POINT ( 'NONE',  ( 9.457646018065525792E-16, -45.06249999863440792, 5.148502694627439702 ) ) ;
#24228 = CARTESIAN_POINT ( 'NONE',  ( 2.229367062500001939, -25.22916666530106866, 3.861377020970579999 ) ) ;
#24229 = CARTESIAN_POINT ( 'NONE',  ( -4.458734124999997661, 6.520833334698930450, 2.574251347313722516 ) ) ;
#24230 = CARTESIAN_POINT ( 'NONE',  ( -60.14911071818854538, -144.0625000000000000, 1.666127454062681146 ) ) ;
#24231 = CARTESIAN_POINT ( 'NONE',  ( 5.000000000000000000, 27.58333333333332860, -2.886751345948129988 ) ) ;
#24232 = CARTESIAN_POINT ( 'NONE',  ( -3.535533905932738641, -149.5000000027311842, 3.535533905932737309 ) ) ;
#24233 = CARTESIAN_POINT ( 'NONE',  ( 2.499999999999998668, -54.20833333060213732, -4.330127018922193649 ) ) ;
#24234 = EDGE_CURVE ( 'NONE', #50232, #45912, #46431, .T. ) ;
#24235 = CARTESIAN_POINT ( 'NONE',  ( -3.152548672688508926E-16, -38.56249999863439371, -5.148502694627439702 ) ) ;
#24236 = CARTESIAN_POINT ( 'NONE',  ( 5.000000000000000000, -73.37499999726880162, -6.123233995736766282E-16 ) ) ;
#24237 = AXIS2_PLACEMENT_3D ( 'NONE', #48038, #23915, #62849 ) ;
#24238 = CARTESIAN_POINT ( 'NONE',  ( -59.44456063193725015, -148.8125000013656063, -0.3552334253322034230 ) ) ;
#24239 = CARTESIAN_POINT ( 'NONE',  ( -3.535533905932738641, -144.3750000000000000, 3.535533905932737309 ) ) ;
#24240 = CARTESIAN_POINT ( 'NONE',  ( -4.458734124999999437, -77.56249999863440792, 0.000000000000000000 ) ) ;
#24241 = CARTESIAN_POINT ( 'NONE',  ( -3.152801135295367985, -164.0625000013656063, 3.152801135295367096 ) ) ;
#24242 = CARTESIAN_POINT ( 'NONE',  ( -4.458734124999999437, -31.39583333196773296, -2.574251347313719407 ) ) ;
#24243 = CARTESIAN_POINT ( 'NONE',  ( 0.000000000000000000, -120.0000000000000000, 5.000000000000000000 ) ) ;
#24244 = DIRECTION ( 'NONE',  ( 0.000000000000000000, 0.000000000000000000, 1.000000000000000000 ) ) ;
#24245 = CARTESIAN_POINT ( 'NONE',  ( -2.499999999999996447, -22.83333333333333215, 4.330127018922195425 ) ) ;
#24246 = CARTESIAN_POINT ( 'NONE',  ( 1.846868145590735200, -144.2500000013656063, -4.458734125000000326 ) ) ;
#24247 = ORIENTED_EDGE ( 'NONE', *, *, #4005, .F. ) ;
#24248 = CARTESIAN_POINT ( 'NONE',  ( -4.458734124999999437, 26.35416666803226349, -2.574251347313719407 ) ) ;
#24249 = CARTESIAN_POINT ( 'NONE',  ( -1.339745962155610925, -48.79465819873850307, 5.000000000000000000 ) ) ;
#24250 = CARTESIAN_POINT ( 'NONE',  ( 4.458734124999998549, -56.97916666530107932, -2.574251347313721627 ) ) ;
#24251 =( BOUNDED_CURVE ( )  B_SPLINE_CURVE ( 2, ( #56546, #42044, #32399, #22765, #61686, #37233, #37540, #42360, #61999 ),
 .UNSPECIFIED., .F., .F. ) 
 B_SPLINE_CURVE_WITH_KNOTS ( ( 3, 2, 2, 2, 3 ),
 ( 0.4229166666666666630, 0.4236111111111111049, 0.4249999999999999889, 0.4263888888888888729, 0.4270833333333333148 ),
 .UNSPECIFIED. ) 
 CURVE ( )  GEOMETRIC_REPRESENTATION_ITEM ( )  RATIONAL_B_SPLINE_CURVE ( ( 0.9330127018922194093, 0.9330127018922194093, 1.000000000000000000, 0.8660254037844387076, 1.000000000000000000, 0.8660254037844387076, 1.000000000000000000, 0.9330127018922194093, 0.9330127018922194093 ) ) 
 REPRESENTATION_ITEM ( '' )  );
#24252 = DIRECTION ( 'NONE',  ( -0.000000000000000000, -1.000000000000000000, 0.000000000000000000 ) ) ;
#24253 = CARTESIAN_POINT ( 'NONE',  ( 1.339745962155612702, -48.16965819600734022, -5.000000000000000000 ) ) ;
#24254 = CARTESIAN_POINT ( 'NONE',  ( -3.535250795749689387E-16, 20.74999999999999645, -5.773502691896257311 ) ) ;
#24255 = CARTESIAN_POINT ( 'NONE',  ( -5.000000000000000000, 8.041666669397852019, -2.886751345948128211 ) ) ;
#24256 = CARTESIAN_POINT ( 'NONE',  ( -3.152548672688508926E-16, -5.562499998634402587, -5.148502694627439702 ) ) ;
#24257 = CARTESIAN_POINT ( 'NONE',  ( 1.975475456537005874E-15, 15.25000000000000000, 5.000000000000000000 ) ) ;
#24258 = CARTESIAN_POINT ( 'NONE',  ( 0.000000000000000000, -120.0000000000000000, 5.000000000000000000 ) ) ;
#24259 = CARTESIAN_POINT ( 'NONE',  ( 5.000000000000000000, -89.37499999726880162, -6.123233995736766282E-16 ) ) ;
#24260 = CARTESIAN_POINT ( 'NONE',  ( -6.127431526422343306E-17, 9.147862274876549904, -8.047472243342932430 ) ) ;
#24261 = CARTESIAN_POINT ( 'NONE',  ( -2.229367062499996610, -23.14583333196773651, 3.861377020970582219 ) ) ;
#24262 = CARTESIAN_POINT ( 'NONE',  ( -3.152548672688508926E-16, -55.56249999863440081, -5.148502694627439702 ) ) ;
#24263 = CARTESIAN_POINT ( 'NONE',  ( 2.730187237215162345E-16, -156.4375000013655779, -4.458734124999999437 ) ) ;
#24264 = CARTESIAN_POINT ( 'NONE',  ( -2.500000000000000444, -51.04166666393547303, -4.330127018922193649 ) ) ;
#24265 = EDGE_LOOP ( 'NONE', ( #15231, #24377, #3315, #38490 ) ) ;
#24266 = CARTESIAN_POINT ( 'NONE',  ( -2.229367062500000163, 5.270833334698927786, -3.861377020970580443 ) ) ;
#24267 = ORIENTED_EDGE ( 'NONE', *, *, #14116, .F. ) ;
#24269 = CARTESIAN_POINT ( 'NONE',  ( 0.000000000000000000, -120.0000000000000000, 0.000000000000000000 ) ) ;
#24268 = CARTESIAN_POINT ( 'NONE',  ( 5.000000000000000000, -4.499999999999997335, -6.123233995736766282E-16 ) ) ;
#24270 = CARTESIAN_POINT ( 'NONE',  ( -3.152801135295367096, -159.0625000013656063, -3.152801135295367541 ) ) ;
#24271 = EDGE_LOOP ( 'NONE', ( #34450, #54187, #5541, #21615 ) ) ;
#24272 = UNCERTAINTY_MEASURE_WITH_UNIT (LENGTH_MEASURE( 1.000000000000000082E-05 ), #7698, 'distance_accuracy_value', 'NONE');
#24273 = AXIS2_PLACEMENT_3D ( 'NONE', #16751, #6476, #1659 ) ;
#24274 = CARTESIAN_POINT ( 'NONE',  ( -6.972266317189433020E-16, -87.12499999726880162, -5.000000000000000000 ) ) ;
#24275 = CARTESIAN_POINT ( 'NONE',  ( -50.01589407740564042, -134.6250000000000284, 0.3983568153799778022 ) ) ;
#24276 = DIRECTION ( 'NONE',  ( -0.000000000000000000, 1.000000000000000000, -0.000000000000000000 ) ) ;
#24277 = CARTESIAN_POINT ( 'NONE',  ( -3.152548672688508926E-16, -45.81249999863440081, -5.148502694627439702 ) ) ;
#24278 = AXIS2_PLACEMENT_3D ( 'NONE', #3222, #21883, #12853 ) ;
#24279 = ORIENTED_EDGE ( 'NONE', *, *, #44760, .F. ) ;
#24280 = AXIS2_PLACEMENT_3D ( 'NONE', #14173, #53417, #43754 ) ;
#24281 = CARTESIAN_POINT ( 'NONE',  ( 1.975475456537005874E-15, -45.74999999999999289, 5.000000000000000000 ) ) ;
#24282 = CARTESIAN_POINT ( 'NONE',  ( 2.229367062499998831, 21.35416666803226349, -3.861377020970580887 ) ) ;
#24283 = VERTEX_POINT ( 'NONE', #62501 ) ;
#24284 = CARTESIAN_POINT ( 'NONE',  ( -4.458734124999998549, 26.77083333469893134, 2.574251347313722516 ) ) ;
#24285 = CARTESIAN_POINT ( 'NONE',  ( -52.53715891517739323, -125.5625000027312552, -4.819101127000233298 ) ) ;
#24286 = CARTESIAN_POINT ( 'NONE',  ( -6.972266317189433020E-16, -88.25000000000000000, -5.000000000000000000 ) ) ;
#24287 = CARTESIAN_POINT ( 'NONE',  ( 1.339745962155612702, -100.2946581987385315, -5.000000000000000000 ) ) ;
#24288 =( BOUNDED_CURVE ( )  B_SPLINE_CURVE ( 2, ( #37726, #8463, #28071, #47688, #57674, #33219, #52837, #59239, #15172 ),
 .UNSPECIFIED., .F., .F. ) 
 B_SPLINE_CURVE_WITH_KNOTS ( ( 3, 2, 2, 2, 3 ),
 ( 0.4604166666666666963, 0.4611111111111111382, 0.4625000000000000222, 0.4638888888888889062, 0.4645833333333333481 ),
 .UNSPECIFIED. ) 
 CURVE ( )  GEOMETRIC_REPRESENTATION_ITEM ( )  RATIONAL_B_SPLINE_CURVE ( ( 0.9330127018922194093, 0.9330127018922220739, 1.000000000000000000, 0.8660254037844387076, 1.000000000000000000, 0.8660254037844387076, 1.000000000000000000, 0.9330127018922194093, 0.9330127018922194093 ) ) 
 REPRESENTATION_ITEM ( '' )  );
#24289 = CARTESIAN_POINT ( 'NONE',  ( 1.339745962155612702, -52.16965819600733312, -5.000000000000000000 ) ) ;
#24290 = CARTESIAN_POINT ( 'NONE',  ( 4.458734124999998549, -58.72916666530106511, -2.574251347313721627 ) ) ;
#24291 = CARTESIAN_POINT ( 'NONE',  ( -2.500000000000000444, 9.958333336064519870, -4.330127018922193649 ) ) ;
#24292 = CARTESIAN_POINT ( 'NONE',  ( 2.229367062500001939, 17.02083333469892779, 3.861377020970579999 ) ) ;
#24293 = CARTESIAN_POINT ( 'NONE',  ( -7.808218555863073007, -4.508077085118257443, -7.999534413642739317 ) ) ;
#24294 = CARTESIAN_POINT ( 'NONE',  ( 2.229367062500001939, -50.22916666530107221, 3.861377020970579999 ) ) ;
#24295 = CARTESIAN_POINT ( 'NONE',  ( 2.500000000000002220, -11.54166666393547835, 4.330127018922192761 ) ) ;
#24296 = CYLINDRICAL_SURFACE ( 'NONE', #32468, 5.000000000000000000 ) ;
#24297 = CARTESIAN_POINT ( 'NONE',  ( -1.339745962155610925, -19.66965819600733667, 5.000000000000000000 ) ) ;
#24298 = CARTESIAN_POINT ( 'NONE',  ( -4.458734124999999437, -89.56249999863440792, 0.000000000000000000 ) ) ;
#24299 = CARTESIAN_POINT ( 'NONE',  ( 4.458734124999999437, -105.8124999986344221, -5.460374474430324690E-16 ) ) ;
#24300 = CARTESIAN_POINT ( 'NONE',  ( -4.458734124999999437, -13.64583333196774184, -2.574251347313719407 ) ) ;
#24301 = ORIENTED_EDGE ( 'NONE', *, *, #49967, .F. ) ;
#24302 = CARTESIAN_POINT ( 'NONE',  ( -1.339745962155610925, -80.79465819873850307, 5.000000000000000000 ) ) ;
#24303 = CARTESIAN_POINT ( 'NONE',  ( 9.457646018065525792E-16, -101.0624999986344079, 5.148502694627439702 ) ) ;
#24304 = CARTESIAN_POINT ( 'NONE',  ( 5.000000000000000000, -161.1250000027311842, 0.000000000000000000 ) ) ;
#24305 = CARTESIAN_POINT ( 'NONE',  ( 2.229367062499998831, -94.89583333196773651, -3.861377020970580887 ) ) ;
#24306 = EDGE_CURVE ( 'NONE', #54724, #29833, #30203, .T. ) ;
#24307 = CARTESIAN_POINT ( 'NONE',  ( -2.499999999999996447, 22.16666666666666785, 4.330127018922195425 ) ) ;
#24308 = CARTESIAN_POINT ( 'NONE',  ( -3.535250795749689387E-16, -51.12499999726880873, -5.773502691896257311 ) ) ;
#24309 = CARTESIAN_POINT ( 'NONE',  ( -52.80376928212989185, -128.8750000013656063, -4.297418129356379346 ) ) ;
#24310 = CARTESIAN_POINT ( 'NONE',  ( -53.51423613279429503, -148.2500000013656347, 4.591703134518083651 ) ) ;
#24311 = CARTESIAN_POINT ( 'NONE',  ( -3.152548672688508926E-16, -20.56249999863440081, -5.148502694627439702 ) ) ;
#24312 = CARTESIAN_POINT ( 'NONE',  ( 9.457646018065525792E-16, 9.687500001365593860, 5.148502694627439702 ) ) ;
#24313 = CARTESIAN_POINT ( 'NONE',  ( 4.458734124999999437, -60.06249999863440081, -5.460374474430324690E-16 ) ) ;
#24314 = CARTESIAN_POINT ( 'NONE',  ( -5.000000000000000000, -53.99999999999999289, 0.000000000000000000 ) ) ;
#24315 = CARTESIAN_POINT ( 'NONE',  ( -4.458734124999999437, -15.39583333196773651, -2.574251347313719407 ) ) ;
#24316 = CARTESIAN_POINT ( 'NONE',  ( 6.123233995736766282E-16, -170.0000000000000000, -5.000000000000000000 ) ) ;
#24317 = CARTESIAN_POINT ( 'NONE',  ( -2.071067811865478170, -156.3125000000000284, 5.000000000000000000 ) ) ;
#24318 = CARTESIAN_POINT ( 'NONE',  ( 2.499999999999998668, -6.333333333333336590, -4.330127018922193649 ) ) ;
#24319 = ORIENTED_EDGE ( 'NONE', *, *, #4109, .F. ) ;
#24320 = CARTESIAN_POINT ( 'NONE',  ( -2.229367062500000163, -40.72916666530107221, -3.861377020970580443 ) ) ;
#24321 = VECTOR ( 'NONE', #34194, 1000.000000000000000 ) ;
#24322 = CARTESIAN_POINT ( 'NONE',  ( -58.39396692619412477, -124.6875000013656063, 2.891590998281057701 ) ) ;
#24323 = CARTESIAN_POINT ( 'NONE',  ( -1.339745962155613812, -9.205341801261479162, -5.000000000000000000 ) ) ;
#24324 = ADVANCED_FACE ( 'NONE', ( #33217 ), #32902, .T. ) ;
#24325 = CARTESIAN_POINT ( 'NONE',  ( 1.975475456537005874E-15, -102.7499999999999858, 5.000000000000000000 ) ) ;
#24326 = CARTESIAN_POINT ( 'NONE',  ( -2.229367062500000163, -87.47916666530107932, -3.861377020970580443 ) ) ;
#24327 = CARTESIAN_POINT ( 'NONE',  ( 4.458734125000001214, 16.85416666803225638, 2.574251347313718519 ) ) ;
#24328 = VECTOR ( 'NONE', #52528, 1000.000000000000000 ) ;
#24329 = VECTOR ( 'NONE', #17611, 1000.000000000000000 ) ;
#24330 = CARTESIAN_POINT ( 'NONE',  ( 9.457646018065525792E-16, 8.937500001365597413, 5.148502694627439702 ) ) ;
#24331 = B_SPLINE_CURVE_WITH_KNOTS ( 'NONE', 3,
 ( #31824, #2262, #2890, #32452, #22502, #56280, #31494, #42412, #52084, #21865 ),
 .UNSPECIFIED., .F., .F.,
 ( 4, 2, 2, 2, 4 ),
 ( 0.01051144076094934904, 0.01162027323572610918, 0.01272910571050286932, 0.01383793818527962946, 0.01494677066005638960 ),
 .UNSPECIFIED. ) ;
#24332 = CARTESIAN_POINT ( 'NONE',  ( -6.972266317189433020E-16, -44.25000000000000000, -5.000000000000000000 ) ) ;
#24333 = ADVANCED_FACE ( 'NONE', ( #42856 ), #17485, .T. ) ;
#24334 = CARTESIAN_POINT ( 'NONE',  ( -6.972266317189433020E-16, -7.249999999999998224, -5.000000000000000000 ) ) ;
#24335 = CARTESIAN_POINT ( 'NONE',  ( -3.152548672688508926E-16, -88.81249999863439371, -5.148502694627439702 ) ) ;
#24336 = CARTESIAN_POINT ( 'NONE',  ( 4.458734124999999437, 22.93750000136559564, -5.460374474430324690E-16 ) ) ;
#24337 = CARTESIAN_POINT ( 'NONE',  ( 2.499999999999998668, -76.33333333333334281, -4.330127018922193649 ) ) ;
#24338 = CARTESIAN_POINT ( 'NONE',  ( -2.499999999999996447, 14.29166666939785202, 4.330127018922195425 ) ) ;
#24339 = ORIENTED_EDGE ( 'NONE', *, *, #17205, .T. ) ;
#24340 = CARTESIAN_POINT ( 'NONE',  ( 0.000000000000000000, -170.0000000000000000, 0.000000000000000000 ) ) ;
#24341 = ORIENTED_EDGE ( 'NONE', *, *, #50324, .F. ) ;
#24343 = CARTESIAN_POINT ( 'NONE',  ( 5.000000000000000000, -32.50000000000000000, -6.123233995736766282E-16 ) ) ;
#24342 = CARTESIAN_POINT ( 'NONE',  ( 5.000000000000000000, -85.41666666666665719, -2.886751345948130876 ) ) ;
#24344 = CARTESIAN_POINT ( 'NONE',  ( -4.458734124999999437, -36.39583333196772941, -2.574251347313719407 ) ) ;
#24345 = EDGE_CURVE ( 'NONE', #29634, #34999, #30937, .T. ) ;
#24346 = CARTESIAN_POINT ( 'NONE',  ( -3.535250795749689387E-16, -33.12499999726881583, -5.773502691896257311 ) ) ;
#24348 = ORIENTED_EDGE ( 'NONE', *, *, #28064, .F. ) ;
#24347 = CARTESIAN_POINT ( 'NONE',  ( 2.229367062500001939, -67.97916666530106511, 3.861377020970579999 ) ) ;
#24349 = CARTESIAN_POINT ( 'NONE',  ( -50.55543936806279248, -151.3125000013656063, 0.3552334253322060320 ) ) ;
#24350 = CARTESIAN_POINT ( 'NONE',  ( -2.229367062500000163, -14.47916666530107221, -3.861377020970580443 ) ) ;
#24352 = VERTEX_POINT ( 'NONE', #27126 ) ;
#24351 = CARTESIAN_POINT ( 'NONE',  ( 4.458734125000001214, -14.14583333196774184, 2.574251347313718519 ) ) ;
#24353 = CARTESIAN_POINT ( 'NONE',  ( 2.500000000000002220, -81.66666666666667140, 4.330127018922192761 ) ) ;
#24354 = FACE_OUTER_BOUND ( 'NONE', #56287, .T. ) ;
#24355 = CARTESIAN_POINT ( 'NONE',  ( 4.458734124999999437, -55.06249999863440081, -5.460374474430324690E-16 ) ) ;
#24356 = CARTESIAN_POINT ( 'NONE',  ( -2.499999999999996447, -84.70833333060214443, 4.330127018922195425 ) ) ;
#24358 = ORIENTED_EDGE ( 'NONE', *, *, #9884, .F. ) ;
#24357 = CARTESIAN_POINT ( 'NONE',  ( 2.499999999999998668, 3.791666669397852019, -4.330127018922193649 ) ) ;
#24359 = CARTESIAN_POINT ( 'NONE',  ( -51.19402409849444524, -147.5000000000000284, -3.242614290531456334 ) ) ;
#24360 = CARTESIAN_POINT ( 'NONE',  ( -4.458734124999999437, -28.56249999863440081, 0.000000000000000000 ) ) ;
#24361 = VERTEX_POINT ( 'NONE', #37410 ) ;
#24362 = CARTESIAN_POINT ( 'NONE',  ( 2.730187237215162345E-16, -168.4375000013656063, -4.458734124999999437 ) ) ;
#24363 = EDGE_CURVE ( 'NONE', #33925, #15736, #10485, .T. ) ;
#24364 = CARTESIAN_POINT ( 'NONE',  ( -4.458734124999998549, -107.4791666653010651, 2.574251347313722516 ) ) ;
#24365 = CARTESIAN_POINT ( 'NONE',  ( -5.000000000000000888, -167.6875000027311842, -2.071067811865475949 ) ) ;
#24366 = ORIENTED_EDGE ( 'NONE', *, *, #55953, .T. ) ;
#24367 = CARTESIAN_POINT ( 'NONE',  ( -54.64476657466781973, -145.0625000013656063, -4.444560631937228834 ) ) ;
#24368 = CARTESIAN_POINT ( 'NONE',  ( -50.18089887299979068, -138.8125000027311842, 2.462841084822635640 ) ) ;
#24369 = CARTESIAN_POINT ( 'NONE',  ( 9.457646018065525792E-16, -38.06249999863440792, 5.148502694627439702 ) ) ;
#24370 = CARTESIAN_POINT ( 'NONE',  ( -7.499999999999653610, -1.545780083834116247, -7.491787297939224821 ) ) ;
#24371 = DIRECTION ( 'NONE',  ( 0.000000000000000000, 0.000000000000000000, 1.000000000000000000 ) ) ;
#24372 = VECTOR ( 'NONE', #13188, 1000.000000000000000 ) ;
#24373 = CARTESIAN_POINT ( 'NONE',  ( -4.458734124999999437, -11.39583333196774007, -2.574251347313719407 ) ) ;
#24374 = CIRCLE ( 'NONE', #61363, 10.12668159690567649 ) ;
#24375 =( BOUNDED_CURVE ( )  B_SPLINE_CURVE ( 2, ( #2884, #45978, #55958, #2560, #41140, #1943, #22497, #50495, #56275 ),
 .UNSPECIFIED., .F., .F. ) 
 B_SPLINE_CURVE_WITH_KNOTS ( ( 3, 2, 2, 2, 3 ),
 ( 0.6446428571428571841, 0.6452380952380952772, 0.6464285714285714635, 0.6476190476190476497, 0.6482142857142857428 ),
 .UNSPECIFIED. ) 
 CURVE ( )  GEOMETRIC_REPRESENTATION_ITEM ( )  RATIONAL_B_SPLINE_CURVE ( ( 0.9330127018922194093, 0.9330127018922194093, 1.000000000000000000, 0.8660254037844387076, 1.000000000000000000, 0.8660254037844387076, 1.000000000000000000, 0.9330127018922194093, 0.9330127018922194093 ) ) 
 REPRESENTATION_ITEM ( '' )  );
#24376 = CARTESIAN_POINT ( 'NONE',  ( -4.458734124999997661, -98.47916666530105090, 2.574251347313722516 ) ) ;
#24377 = ORIENTED_EDGE ( 'NONE', *, *, #11828, .F. ) ;
#24378 = CARTESIAN_POINT ( 'NONE',  ( -3.152801135295367985, -144.0625000013655779, 3.152801135295367096 ) ) ;
#24379 = CARTESIAN_POINT ( 'NONE',  ( -4.458734124999999437, -31.64583333196773651, -2.574251347313719407 ) ) ;
#24380 = AXIS2_PLACEMENT_3D ( 'NONE', #61998, #52960, #17918 ) ;
#24381 = CARTESIAN_POINT ( 'NONE',  ( -52.80376928212989185, -131.8750000013656347, -4.297418129356379346 ) ) ;
#24382 = CARTESIAN_POINT ( 'NONE',  ( 2.229367062500001939, -66.22916666530106511, 3.861377020970579999 ) ) ;
#24383 = CARTESIAN_POINT ( 'NONE',  ( -59.98410592259440222, -146.2500000027312126, -0.3983568153799752487 ) ) ;
#24384 = CYLINDRICAL_SURFACE ( 'NONE', #60392, 5.000000000000000000 ) ;
#24385 = CARTESIAN_POINT ( 'NONE',  ( -4.458734124999999437, -139.9375000013656063, -5.460374474430324690E-16 ) ) ;
#24386 = CARTESIAN_POINT ( 'NONE',  ( -2.229367062500000163, 6.270833334698928674, -3.861377020970580443 ) ) ;
#24387 = ORIENTED_EDGE ( 'NONE', *, *, #22917, .F. ) ;
#24388 = SURFACE_STYLE_USAGE ( .BOTH. , #63315 ) ;
#24390 = CARTESIAN_POINT ( 'NONE',  ( -3.152548672688508926E-16, -27.56249999863440081, -5.148502694627439702 ) ) ;
#24389 = CARTESIAN_POINT ( 'NONE',  ( 1.060575238724906964E-15, -95.75000000000000000, 5.773502691896257311 ) ) ;
#24391 = CARTESIAN_POINT ( 'NONE',  ( -52.53715891517739323, -143.5625000027312126, -4.819101127000233298 ) ) ;
#24392 = CARTESIAN_POINT ( 'NONE',  ( 2.229367062500001939, -78.22916666530106511, 3.861377020970579999 ) ) ;
#24393 = CARTESIAN_POINT ( 'NONE',  ( -2.229367062499996610, 25.60416666803225993, 3.861377020970582219 ) ) ;
#24394 = CARTESIAN_POINT ( 'NONE',  ( -5.000000000000000000, 26.91666666666666430, -2.886751345948128211 ) ) ;
#24395 = CARTESIAN_POINT ( 'NONE',  ( -59.44456063193725015, -141.5625000013656063, -0.3552334253322034230 ) ) ;
#24396 = EDGE_CURVE ( 'NONE', #44687, #30129, #60674, .T. ) ;
#24397 = ADVANCED_FACE ( 'NONE', ( #37723 ), #2687, .T. ) ;
#24398 = CARTESIAN_POINT ( 'NONE',  ( 4.458734124999999437, -4.812499998634402587, -5.460374474430324690E-16 ) ) ;
#24399 = CARTESIAN_POINT ( 'NONE',  ( 9.457646018065525792E-16, 28.68750000136559208, 5.148502694627439702 ) ) ;
#24400 = CARTESIAN_POINT ( 'NONE',  ( 2.229367062499998831, -43.89583333196774362, -3.861377020970580887 ) ) ;
#24401 = CYLINDRICAL_SURFACE ( 'NONE', #28420, 5.000000000000000000 ) ;
#24402 = CARTESIAN_POINT ( 'NONE',  ( 4.458734124999999437, 0.1875000013655953035, -5.460374474430324690E-16 ) ) ;
#24403 = VERTEX_POINT ( 'NONE', #52203 ) ;
#24404 = CARTESIAN_POINT ( 'NONE',  ( 4.458734124999999437, -23.06249999863440436, -5.460374474430324690E-16 ) ) ;
#24405 = CARTESIAN_POINT ( 'NONE',  ( 2.229367062500001939, -67.97916666530106511, 3.861377020970579999 ) ) ;
#24406 = CARTESIAN_POINT ( 'NONE',  ( -2.499999999999996447, -103.7083333306021444, 4.330127018922195425 ) ) ;
#24407 = ADVANCED_FACE ( 'NONE', ( #27750 ), #47378, .F. ) ;
#24408 = CARTESIAN_POINT ( 'NONE',  ( -4.458734124999999437, 26.68750000136559564, 0.000000000000000000 ) ) ;
#24409 = CARTESIAN_POINT ( 'NONE',  ( -1.339745962155610925, 10.20534180126147739, 5.000000000000000000 ) ) ;
#24410 = EDGE_CURVE ( 'NONE', #2425, #17633, #36806, .T. ) ;
#24411 = CARTESIAN_POINT ( 'NONE',  ( -4.458734124999999437, -109.5624999986343937, 0.000000000000000000 ) ) ;
#24412 = CARTESIAN_POINT ( 'NONE',  ( -4.458734124999997661, -74.47916666530106511, 2.574251347313722516 ) ) ;
#24413 = CARTESIAN_POINT ( 'NONE',  ( 5.000000000000000888, -54.58333333333332860, 2.886751345948126879 ) ) ;
#24414 = DIRECTION ( 'NONE',  ( -1.061635649774262822E-14, 0.000000000000000000, -1.000000000000000000 ) ) ;
#24415 = CARTESIAN_POINT ( 'NONE',  ( 3.061616997868383141E-16, -155.8750000027311842, -5.000000000000000000 ) ) ;
#24416 = ORIENTED_EDGE ( 'NONE', *, *, #42491, .F. ) ;
#24417 = CARTESIAN_POINT ( 'NONE',  ( 0.000000000000000000, -120.0000000000000000, 0.000000000000000000 ) ) ;
#24418 = CARTESIAN_POINT ( 'NONE',  ( -6.972266317189433020E-16, -43.12499999726880873, -5.000000000000000000 ) ) ;
#24419 = CARTESIAN_POINT ( 'NONE',  ( -5.000000000000000000, -17.00000000000000000, 0.000000000000000000 ) ) ;
#24420 = CARTESIAN_POINT ( 'NONE',  ( -4.458734124999998549, -21.22916666530107221, 2.574251347313722516 ) ) ;
#24421 = CARTESIAN_POINT ( 'NONE',  ( -4.458734124999997661, -84.22916666530107932, 2.574251347313722516 ) ) ;
#24422 = CARTESIAN_POINT ( 'NONE',  ( -4.458734125000001214, -169.1250000013656347, 1.846868145590734089 ) ) ;
#24423 = CARTESIAN_POINT ( 'NONE',  ( -5.000000000000000000, -16.95833333060214443, -2.886751345948128211 ) ) ;
#24425 = ORIENTED_EDGE ( 'NONE', *, *, #62998, .T. ) ;
#24424 = CARTESIAN_POINT ( 'NONE',  ( -2.229367062499996610, -50.14583333196772941, 3.861377020970582219 ) ) ;
#24426 = CARTESIAN_POINT ( 'NONE',  ( -1.339745962155613812, -24.20534180126147206, -5.000000000000000000 ) ) ;
#24427 = CARTESIAN_POINT ( 'NONE',  ( 3.061616997868383141E-16, -164.8750000027311842, -5.000000000000000000 ) ) ;
#24429 = ORIENTED_EDGE ( 'NONE', *, *, #59887, .T. ) ;
#24428 = CARTESIAN_POINT ( 'NONE',  ( -4.458734124999999437, -0.5624999986344053626, 0.000000000000000000 ) ) ;
#24430 = CARTESIAN_POINT ( 'NONE',  ( -50.70258187064364108, -153.1250000013656063, 2.196230717870141014 ) ) ;
#24431 = CARTESIAN_POINT ( 'NONE',  ( -4.999999999999999112, -60.91666666666666430, 2.886751345948131764 ) ) ;
#24432 = CARTESIAN_POINT ( 'NONE',  ( 4.458734124999999437, -157.7500000013656063, 1.846868145590737864 ) ) ;
#24433 = CARTESIAN_POINT ( 'NONE',  ( 2.229367062500001939, -39.22916666530107221, 3.861377020970579999 ) ) ;
#24434 = CARTESIAN_POINT ( 'NONE',  ( -5.000000000000000000, -65.00000000000000000, 0.000000000000000000 ) ) ;
#24435 = CARTESIAN_POINT ( 'NONE',  ( -5.000000000000000888, -160.5625000000000284, -2.071067811865475949 ) ) ;
#24436 = CARTESIAN_POINT ( 'NONE',  ( -57.19623071787017210, -126.6250000013656489, 4.297418129356382899 ) ) ;
#24437 = CARTESIAN_POINT ( 'NONE',  ( -4.458734124999999437, -9.562499998634406140, 0.000000000000000000 ) ) ;
#24438 = CARTESIAN_POINT ( 'NONE',  ( 2.229367062499998831, -48.89583333196772941, -3.861377020970580887 ) ) ;
#24439 = CARTESIAN_POINT ( 'NONE',  ( 1.339745962155612702, -89.29465819873851729, -5.000000000000000000 ) ) ;
#24440 = CARTESIAN_POINT ( 'NONE',  ( 1.846868145590735200, -148.2500000013656063, -4.458734125000000326 ) ) ;
#24441 = CARTESIAN_POINT ( 'NONE',  ( 2.229367062500001939, -90.22916666530106511, 3.861377020970579999 ) ) ;
#24442 = CARTESIAN_POINT ( 'NONE',  ( 5.000000000000000888, -108.5833333333333144, 2.886751345948126879 ) ) ;
#24443 = ORIENTED_EDGE ( 'NONE', *, *, #50294, .T. ) ;
#24444 = CARTESIAN_POINT ( 'NONE',  ( -5.000000000000000000, 14.04166666939785202, -2.886751345948128211 ) ) ;
#24445 = CARTESIAN_POINT ( 'NONE',  ( -4.999999999999998224, -5.791666663935480130, 2.886751345948131764 ) ) ;
#24446 = CARTESIAN_POINT ( 'NONE',  ( -57.46284108482265651, -152.0625000027311842, 4.819101127000239515 ) ) ;
#24447 = CARTESIAN_POINT ( 'NONE',  ( 2.499999999999998668, -29.20833333060214798, -4.330127018922193649 ) ) ;
#24448 = ORIENTED_EDGE ( 'NONE', *, *, #38544, .F. ) ;
#24449 = CARTESIAN_POINT ( 'NONE',  ( 4.458734125000001214, 5.104166668032261711, 2.574251347313718519 ) ) ;
#24450 = CARTESIAN_POINT ( 'NONE',  ( -4.999999999999998224, -70.79166666393547303, 2.886751345948131764 ) ) ;
#24451 = CARTESIAN_POINT ( 'NONE',  ( -4.458734124999998549, -14.47916666530107221, 2.574251347313722516 ) ) ;
#24452 = CARTESIAN_POINT ( 'NONE',  ( -4.999999999999998224, -50.91666666666666430, 2.886751345948131764 ) ) ;
#24453 = CARTESIAN_POINT ( 'NONE',  ( -4.458734124999999437, -2.395833331967737845, -2.574251347313719407 ) ) ;
#24454 = CARTESIAN_POINT ( 'NONE',  ( -4.999999999999998224, 4.208333336064518093, 2.886751345948131764 ) ) ;
#24455 = CARTESIAN_POINT ( 'NONE',  ( -1.846868145590734756, -152.1250000013655779, -4.458734124999999437 ) ) ;
#24456 = AXIS2_PLACEMENT_3D ( 'NONE', #41538, #6198, #16795 ) ;
#24457 = CARTESIAN_POINT ( 'NONE',  ( -4.458734124999999437, 18.43750000136559564, 0.000000000000000000 ) ) ;
#24458 = ORIENTED_EDGE ( 'NONE', *, *, #27271, .F. ) ;
#24459 = CARTESIAN_POINT ( 'NONE',  ( -4.458734124999999437, -96.39583333196773651, -2.574251347313719407 ) ) ;
#24460 = CARTESIAN_POINT ( 'NONE',  ( 0.000000000000000000, -170.0000000000000000, 5.000000000000000000 ) ) ;
#24461 = CARTESIAN_POINT ( 'NONE',  ( 2.500000000000002220, -12.54166666393548013, 4.330127018922192761 ) ) ;
#24462 = CARTESIAN_POINT ( 'NONE',  ( -2.229367062499996610, -12.14583333196774007, 3.861377020970582219 ) ) ;
#24463 = CARTESIAN_POINT ( 'NONE',  ( -2.500000000000000444, 27.95833333606451987, -4.330127018922193649 ) ) ;
#24464 = LINE ( 'NONE', #54044, #27368 ) ;
#24465 = CARTESIAN_POINT ( 'NONE',  ( -6.972266317189433020E-16, -88.25000000000000000, -5.000000000000000000 ) ) ;
#24466 = EDGE_CURVE ( 'NONE', #37025, #50637, #3557, .T. ) ;
#24467 = CARTESIAN_POINT ( 'NONE',  ( -5.000000000000000000, -42.95833333060214443, -2.886751345948128211 ) ) ;
#24468 = CARTESIAN_POINT ( 'NONE',  ( 0.000000000000000000, -120.0000000000000000, 0.000000000000000000 ) ) ;
#24469 = CARTESIAN_POINT ( 'NONE',  ( 9.457646018065525792E-16, 12.93750000136559208, 5.148502694627439702 ) ) ;
#24470 = CARTESIAN_POINT ( 'NONE',  ( 2.500000000000002220, -51.54166666393547303, 4.330127018922192761 ) ) ;
#24471 = ORIENTED_EDGE ( 'NONE', *, *, #37324, .T. ) ;
#24472 = CARTESIAN_POINT ( 'NONE',  ( -2.229367062499996610, 18.85416666803225993, 3.861377020970582219 ) ) ;
#24473 = CARTESIAN_POINT ( 'NONE',  ( -2.229367062500000163, -60.47916666530106511, -3.861377020970580443 ) ) ;
#24474 = CARTESIAN_POINT ( 'NONE',  ( -2.229367062499996610, -9.395833331967736513, 3.861377020970582219 ) ) ;
#24475 =( BOUNDED_CURVE ( )  B_SPLINE_CURVE ( 2, ( #27579, #49410, #53288, #866, #9224, #19503, #53914, #49086, #24334 ),
 .UNSPECIFIED., .F., .F. ) 
 B_SPLINE_CURVE_WITH_KNOTS ( ( 3, 2, 2, 2, 3 ),
 ( 0.2625000000000000111, 0.2630952380952381042, 0.2642857142857142905, 0.2654761904761904767, 0.2660714285714285698 ),
 .UNSPECIFIED. ) 
 CURVE ( )  GEOMETRIC_REPRESENTATION_ITEM ( )  RATIONAL_B_SPLINE_CURVE ( ( 0.9330127018922194093, 0.9330127018922194093, 1.000000000000000000, 0.8660254037844387076, 1.000000000000000000, 0.8660254037844387076, 1.000000000000000000, 0.9330127018922194093, 0.9330127018922194093 ) ) 
 REPRESENTATION_ITEM ( '' )  );
#24476 = CARTESIAN_POINT ( 'NONE',  ( 2.499999999999998668, -109.2083333306021444, -4.330127018922193649 ) ) ;
#24477 = CARTESIAN_POINT ( 'NONE',  ( 2.499999999999998668, 9.666666666666667851, -4.330127018922193649 ) ) ;
#24478 = CARTESIAN_POINT ( 'NONE',  ( -1.846868145590734756, -167.1250000013656063, -4.458734125000000326 ) ) ;
#24479 = CARTESIAN_POINT ( 'NONE',  ( -5.000000000000000000, -20.95833333060214798, -2.886751345948128211 ) ) ;
#24480 = CARTESIAN_POINT ( 'NONE',  ( -2.229367062499996610, -51.14583333196772941, 3.861377020970582219 ) ) ;
#24481 = CARTESIAN_POINT ( 'NONE',  ( 5.000000000000000888, -91.45833333060214443, 2.886751345948126879 ) ) ;
#24482 = CARTESIAN_POINT ( 'NONE',  ( 4.458734124999999437, -27.81249999863440081, -5.460374474430324690E-16 ) ) ;
#24483 = VECTOR ( 'NONE', #24544, 1000.000000000000000 ) ;
#24484 = CARTESIAN_POINT ( 'NONE',  ( 1.339745962155612702, -14.16965819600733312, -5.000000000000000000 ) ) ;
#24485 = CARTESIAN_POINT ( 'NONE',  ( -2.500000000000000444, -55.04166666393548013, -4.330127018922193649 ) ) ;
#24486 = CARTESIAN_POINT ( 'NONE',  ( 5.000000000000000888, -69.58333333333332860, 2.886751345948126879 ) ) ;
#24487 = CARTESIAN_POINT ( 'NONE',  ( 3.152801135295367541, -155.5625000013656063, -3.152801135295367541 ) ) ;
#24488 = CARTESIAN_POINT ( 'NONE',  ( 5.000000000000000000, -36.50000000000000711, -6.123233995736766282E-16 ) ) ;
#24489 = DIRECTION ( 'NONE',  ( 0.000000000000000000, 0.000000000000000000, 1.000000000000000000 ) ) ;
#24490 = ADVANCED_FACE ( 'NONE', ( #19673 ), #47999, .T. ) ;
#24491 = CARTESIAN_POINT ( 'NONE',  ( -9.184850993605147944E-16, -148.3750000027312126, 5.000000000000000000 ) ) ;
#24492 = ORIENTED_EDGE ( 'NONE', *, *, #31896, .T. ) ;
#24493 = CARTESIAN_POINT ( 'NONE',  ( 9.457646018065525792E-16, -103.0624999986344221, 5.148502694627439702 ) ) ;
#24494 = CARTESIAN_POINT ( 'NONE',  ( -2.229367062499996610, 1.604166668032262155, 3.861377020970582219 ) ) ;
#24495 = CARTESIAN_POINT ( 'NONE',  ( 5.000000000000000888, -80.58333333333332860, 2.886751345948126879 ) ) ;
#24496 = EDGE_CURVE ( 'NONE', #20741, #62531, #21209, .T. ) ;
#24497 = CARTESIAN_POINT ( 'NONE',  ( -5.000000000000000000, 0.000000000000000000, 0.000000000000000000 ) ) ;
#24498 = CARTESIAN_POINT ( 'NONE',  ( 2.229367062500001939, -64.97916666530106511, 3.861377020970579999 ) ) ;
#24499 = CARTESIAN_POINT ( 'NONE',  ( -2.500000000000000444, -31.04166666393548368, -4.330127018922193649 ) ) ;
#24500 = EDGE_CURVE ( 'NONE', #14071, #39231, #39601, .T. ) ;
#24501 = CARTESIAN_POINT ( 'NONE',  ( -5.000000000000000000, -2.874999997268815832, 0.000000000000000000 ) ) ;
#24503 = VERTEX_POINT ( 'NONE', #14840 ) ;
#24502 = CARTESIAN_POINT ( 'NONE',  ( -2.229367062499996610, -34.14583333196772941, 3.861377020970582219 ) ) ;
#24504 = CARTESIAN_POINT ( 'NONE',  ( 1.339745962155615144, 17.41965820146970145, 4.999999999999999112 ) ) ;
#24505 = CYLINDRICAL_SURFACE ( 'NONE', #48702, 5.000000000000000000 ) ;
#24506 = CARTESIAN_POINT ( 'NONE',  ( -56.66612745406251861, -136.3125000000000000, -5.149110718188501856 ) ) ;
#24507 = CARTESIAN_POINT ( 'NONE',  ( 5.000000000000000888, -46.58333333333334991, 2.886751345948126879 ) ) ;
#24509 = CARTESIAN_POINT ( 'NONE',  ( -4.458734124999998549, -26.47916666530107221, 2.574251347313722516 ) ) ;
#24508 = CARTESIAN_POINT ( 'NONE',  ( 3.061616997868383141E-16, -147.7500000000000284, -5.000000000000000000 ) ) ;
#24510 = VECTOR ( 'NONE', #13275, 1000.000000000000000 ) ;
#24511 = CARTESIAN_POINT ( 'NONE',  ( 2.499999999999998668, -4.208333330602147981, -4.330127018922193649 ) ) ;
#24512 = CARTESIAN_POINT ( 'NONE',  ( 2.229367062499998831, -70.64583333196773651, -3.861377020970580887 ) ) ;
#24513 = CARTESIAN_POINT ( 'NONE',  ( -4.458734125000000326, -145.2500000013655779, -1.846868145590735644 ) ) ;
#24514 = CARTESIAN_POINT ( 'NONE',  ( 2.229367062499998831, -84.64583333196773651, -3.861377020970580887 ) ) ;
#24515 = VECTOR ( 'NONE', #20478, 1000.000000000000000 ) ;
#24516 = CARTESIAN_POINT ( 'NONE',  ( -59.29741812935640155, -139.8750000013655779, -2.196230717870135685 ) ) ;
#24517 = CARTESIAN_POINT ( 'NONE',  ( -3.152548672688508926E-16, -32.81249999863440792, -5.148502694627439702 ) ) ;
#24518 = CARTESIAN_POINT ( 'NONE',  ( 5.000000000000000888, -70.45833333060214443, 2.886751345948126879 ) ) ;
#24519 = ORIENTED_EDGE ( 'NONE', *, *, #40264, .F. ) ;
#24520 = LINE ( 'NONE', #45408, #40271 ) ;
#24521 = ORIENTED_EDGE ( 'NONE', *, *, #58600, .T. ) ;
#24522 = CARTESIAN_POINT ( 'NONE',  ( 4.458734124999998549, -72.97916666530107932, -2.574251347313721627 ) ) ;
#24523 = CARTESIAN_POINT ( 'NONE',  ( 5.000000000000000000, -166.0000000000000000, 0.000000000000000000 ) ) ;
#24524 = FILL_AREA_STYLE ('',( #58306 ) ) ;
#24525 = VERTEX_POINT ( 'NONE', #9387 ) ;
#24526 = CARTESIAN_POINT ( 'NONE',  ( -51.19402409849444524, -140.5000000000000000, -3.242614290531456334 ) ) ;
#24527 = CARTESIAN_POINT ( 'NONE',  ( -4.458734124999999437, -56.64583333196773651, -2.574251347313719407 ) ) ;
#24528 = CARTESIAN_POINT ( 'NONE',  ( -3.152548672688508926E-16, 1.187500001365596081, -5.148502694627439702 ) ) ;
#24529 = VERTEX_POINT ( 'NONE', #54416 ) ;
#24530 = CARTESIAN_POINT ( 'NONE',  ( 3.061616997868383141E-16, -146.7500000000000284, -5.000000000000000000 ) ) ;
#24531 = CARTESIAN_POINT ( 'NONE',  ( 2.500000000000002220, -69.54166666393547303, 4.330127018922192761 ) ) ;
#24532 = CARTESIAN_POINT ( 'NONE',  ( -2.229367062500000163, 14.52083333469892779, -3.861377020970580443 ) ) ;
#24533 = CARTESIAN_POINT ( 'NONE',  ( -51.60603307380591787, -139.9375000013656063, -2.891590998281053704 ) ) ;
#24534 = CARTESIAN_POINT ( 'NONE',  ( -53.33387254593733218, -154.8125000000000000, 5.149110718188519620 ) ) ;
#24535 = CARTESIAN_POINT ( 'NONE',  ( -4.458734124999999437, -166.0000000013656063, -1.846868145590735644 ) ) ;
#24536 = VERTEX_POINT ( 'NONE', #34794 ) ;
#24537 = CARTESIAN_POINT ( 'NONE',  ( 2.229367062499998831, -75.64583333196773651, -3.861377020970580887 ) ) ;
#24538 = CARTESIAN_POINT ( 'NONE',  ( -3.535533905932738641, -153.3750000000000000, 3.535533905932737309 ) ) ;
#24539 = CARTESIAN_POINT ( 'NONE',  ( 4.458734124999998549, 1.270833334698927342, -2.574251347313721627 ) ) ;
#24540 = CARTESIAN_POINT ( 'NONE',  ( -2.499999999999996447, -82.83333333333332860, 4.330127018922195425 ) ) ;
#24541 = CARTESIAN_POINT ( 'NONE',  ( -1.339745962155610925, 2.205341801261479606, 5.000000000000000000 ) ) ;
#24542 = CARTESIAN_POINT ( 'NONE',  ( -2.229367062499996610, -64.39583333196773651, 3.861377020970582219 ) ) ;
#24543 = CARTESIAN_POINT ( 'NONE',  ( -4.999999999999999112, -24.79166666393548368, 2.886751345948131764 ) ) ;
#24544 = DIRECTION ( 'NONE',  ( -0.000000000000000000, 1.000000000000000000, -0.000000000000000000 ) ) ;
#24545 = CARTESIAN_POINT ( 'NONE',  ( -2.229367062500000163, 28.52083333469892779, -3.861377020970580443 ) ) ;
#24546 = CARTESIAN_POINT ( 'NONE',  ( -2.499999999999996447, -64.70833333060213022, 4.330127018922195425 ) ) ;
#24547 = CARTESIAN_POINT ( 'NONE',  ( 9.457646018065525792E-16, -48.06249999863440081, 5.148502694627439702 ) ) ;
#24548 = PRODUCT ( 'pulling arm', 'pulling arm', '', ( #15349 ) ) ;
#24549 = CARTESIAN_POINT ( 'NONE',  ( 2.229367062500001939, -30.22916666530107221, 3.861377020970579999 ) ) ;
#24550 = CARTESIAN_POINT ( 'NONE',  ( 9.457646018065525792E-16, 8.687500001365595637, 5.148502694627439702 ) ) ;
#24551 = STYLED_ITEM ( 'NONE', ( #4578 ), #23309 ) ;
#24552 = CARTESIAN_POINT ( 'NONE',  ( -6.972266317189433020E-16, -13.25000000000000000, -5.000000000000000000 ) ) ;
#24553 = CARTESIAN_POINT ( 'NONE',  ( -5.000000000000000000, 24.99999999999999645, 0.000000000000000000 ) ) ;
#24554 = CARTESIAN_POINT ( 'NONE',  ( 3.061616997868383141E-16, -149.8750000027312126, -5.000000000000000000 ) ) ;
#24555 = CARTESIAN_POINT ( 'NONE',  ( -1.339745962155613812, -50.20534180126148271, -5.000000000000000000 ) ) ;
#24556 = AXIS2_PLACEMENT_3D ( 'NONE', #49834, #19926, #15751 ) ;
#24557 = CARTESIAN_POINT ( 'NONE',  ( 4.458734124999998549, -39.72916666530107932, -2.574251347313721627 ) ) ;
#24558 = CARTESIAN_POINT ( 'NONE',  ( -5.000000000000000000, -72.87499999726880162, 0.000000000000000000 ) ) ;
#24559 =( BOUNDED_CURVE ( )  B_SPLINE_CURVE ( 2, ( #61660, #37210, #56836, #13697, #32375, #51999, #43275, #28172, #8560 ),
 .UNSPECIFIED., .F., .F. ) 
 B_SPLINE_CURVE_WITH_KNOTS ( ( 3, 2, 2, 2, 3 ),
 ( 0.09166666666666674346, 0.09583333333333342308, 0.1000000000000000888, 0.1041666666666667546, 0.1083333333333334203 ),
 .UNSPECIFIED. ) 
 CURVE ( )  GEOMETRIC_REPRESENTATION_ITEM ( )  RATIONAL_B_SPLINE_CURVE ( ( 0.9999999999999984457, 0.9238795325112882928, 1.000000000000000000, 0.9238795325112867385, 1.000000000000000000, 0.9238795325112867385, 1.000000000000000000, 0.9238795325112851842, 1.000000000000001554 ) ) 
 REPRESENTATION_ITEM ( '' )  );
#24560 = CARTESIAN_POINT ( 'NONE',  ( -52.80376928212989185, -144.1250000013656063, -4.297418129356379346 ) ) ;
#24561 = CARTESIAN_POINT ( 'NONE',  ( -5.000000000000000888, -141.4375000000000284, 2.071067811865474617 ) ) ;
#24562 = CARTESIAN_POINT ( 'NONE',  ( -4.458734124999999437, -76.56249999863440792, 0.000000000000000000 ) ) ;
#24563 = CARTESIAN_POINT ( 'NONE',  ( -4.458734124999999437, -167.1875000013655779, -5.460374474430324690E-16 ) ) ;
#24564 = CARTESIAN_POINT ( 'NONE',  ( 9.457646018065525792E-16, -28.06249999863440081, 5.148502694627439702 ) ) ;
#24565 = CARTESIAN_POINT ( 'NONE',  ( -1.339745962155610925, -32.79465819873851729, 5.000000000000000000 ) ) ;
#24566 = LINE ( 'NONE', #44812, #27687 ) ;
#24567 = CARTESIAN_POINT ( 'NONE',  ( -3.535250795749689387E-16, -24.24999999999999645, -5.773502691896257311 ) ) ;
#24568 = CARTESIAN_POINT ( 'NONE',  ( -1.846868145590737420, -143.7500000013655779, 4.458734124999999437 ) ) ;
#24569 = ORIENTED_EDGE ( 'NONE', *, *, #36971, .F. ) ;
#24570 = CARTESIAN_POINT ( 'NONE',  ( 1.060575238724906964E-15, -90.62499999726880162, 5.773502691896257311 ) ) ;
#24571 = ORIENTED_EDGE ( 'NONE', *, *, #10330, .T. ) ;
#24572 = CARTESIAN_POINT ( 'NONE',  ( -4.458734124999997661, -64.47916666530106511, 2.574251347313722516 ) ) ;
#24573 = CARTESIAN_POINT ( 'NONE',  ( 2.500000000000002220, 20.45833333606451987, 4.330127018922192761 ) ) ;
#24574 = CARTESIAN_POINT ( 'NONE',  ( 5.000000000000000888, 4.541666669397852019, 2.886751345948126879 ) ) ;
#24575 = CARTESIAN_POINT ( 'NONE',  ( -4.999999999999999112, 19.08333333333333570, 2.886751345948131764 ) ) ;
#24576 = CARTESIAN_POINT ( 'NONE',  ( -4.458734124999999437, -49.39583333196772230, -2.574251347313719407 ) ) ;
#24577 = CARTESIAN_POINT ( 'NONE',  ( -4.458734124999999437, -7.395833331967734736, -2.574251347313719407 ) ) ;
#24578 =( BOUNDED_CURVE ( )  B_SPLINE_CURVE ( 2, ( #45185, #6283, #35543, #29414, #11088, #185, #25249, #827, #10136 ),
 .UNSPECIFIED., .F., .F. ) 
 B_SPLINE_CURVE_WITH_KNOTS ( ( 3, 2, 2, 2, 3 ),
 ( 0.8979166666666666963, 0.8986111111111111382, 0.9000000000000000222, 0.9013888888888889062, 0.9020833333333333481 ),
 .UNSPECIFIED. ) 
 CURVE ( )  GEOMETRIC_REPRESENTATION_ITEM ( )  RATIONAL_B_SPLINE_CURVE ( ( 0.9330127018922194093, 0.9330127018922194093, 1.000000000000000000, 0.8660254037844387076, 1.000000000000000000, 0.8660254037844387076, 1.000000000000000000, 0.9330127018922194093, 0.9330127018922194093 ) ) 
 REPRESENTATION_ITEM ( '' )  );
#24579 = CARTESIAN_POINT ( 'NONE',  ( -5.000000000000000000, 4.000000000000000000, 0.000000000000000000 ) ) ;
#24580 = DIRECTION ( 'NONE',  ( 0.000000000000000000, 0.000000000000000000, 1.000000000000000000 ) ) ;
#24581 = CARTESIAN_POINT ( 'NONE',  ( 1.339745962155612702, -89.16965819600733312, -5.000000000000000000 ) ) ;
#24582 = CARTESIAN_POINT ( 'NONE',  ( 0.000000000000000000, -120.0000000000000000, 5.000000000000000000 ) ) ;
#24584 = CARTESIAN_POINT ( 'NONE',  ( 4.458734125000001214, -21.89583333196773296, 2.574251347313718519 ) ) ;
#24583 = CARTESIAN_POINT ( 'NONE',  ( 1.975475456537005874E-15, -62.74999999999998579, 5.000000000000000000 ) ) ;
#24585 = CARTESIAN_POINT ( 'NONE',  ( 5.000000000000000000, -97.37499999726881583, -6.123233995736766282E-16 ) ) ;
#24586 = CARTESIAN_POINT ( 'NONE',  ( -2.229367062500000163, -55.47916666530107221, -3.861377020970580443 ) ) ;
#24587 = CARTESIAN_POINT ( 'NONE',  ( 4.458734125000000326, -157.6250000013655779, -1.846868145590734978 ) ) ;
#24588 = CARTESIAN_POINT ( 'NONE',  ( -4.999999999999999112, -47.79166666393548013, 2.886751345948131764 ) ) ;
#24589 = ORIENTED_EDGE ( 'NONE', *, *, #55412, .F. ) ;
#24590 = CARTESIAN_POINT ( 'NONE',  ( 9.457646018065525792E-16, 6.687500001365594748, 5.148502694627439702 ) ) ;
#24591 = VERTEX_POINT ( 'NONE', #9080 ) ;
#24593 = CARTESIAN_POINT ( 'NONE',  ( -4.999999999999998224, -28.91666666666666430, 2.886751345948131764 ) ) ;
#24592 = CARTESIAN_POINT ( 'NONE',  ( 0.000000000000000000, -120.0000000000000000, 0.000000000000000000 ) ) ;
#24594 = CARTESIAN_POINT ( 'NONE',  ( -3.152801135295367985, -155.8125000013656063, 3.152801135295367096 ) ) ;
#24595 = VERTEX_POINT ( 'NONE', #63125 ) ;
#24596 =( GEOMETRIC_REPRESENTATION_CONTEXT ( 3 ) GLOBAL_UNCERTAINTY_ASSIGNED_CONTEXT ( ( #48711 ) ) GLOBAL_UNIT_ASSIGNED_CONTEXT ( ( #61097, #51123, #56901 ) ) REPRESENTATION_CONTEXT ( 'NONE', 'WORKASPACE' ) );
#24597 = DIRECTION ( 'NONE',  ( -0.000000000000000000, 1.000000000000000000, -0.000000000000000000 ) ) ;
#24598 = CARTESIAN_POINT ( 'NONE',  ( -52.53715891517739323, -134.4375000000000284, -4.819101127000233298 ) ) ;
#24599 = CARTESIAN_POINT ( 'NONE',  ( 5.000000000000000000, -53.29166666393548013, -2.886751345948130876 ) ) ;
#24600 = CARTESIAN_POINT ( 'NONE',  ( -2.229367062500000163, -44.72916666530106511, -3.861377020970580443 ) ) ;
#24601 = ORIENTED_EDGE ( 'NONE', *, *, #23832, .T. ) ;
#24602 = CARTESIAN_POINT ( 'NONE',  ( 1.339745962155615144, -103.5803417985302701, 4.999999999999999112 ) ) ;
#24603 = CARTESIAN_POINT ( 'NONE',  ( -2.229367062499996610, 20.85416666803226349, 3.861377020970582219 ) ) ;
#24604 = DIRECTION ( 'NONE',  ( -0.000000000000000000, 1.000000000000000000, -0.000000000000000000 ) ) ;
#24605 = ORIENTED_EDGE ( 'NONE', *, *, #46782, .T. ) ;
#24606 = CARTESIAN_POINT ( 'NONE',  ( 2.229367062499998831, -88.89583333196773651, -3.861377020970580887 ) ) ;
#24607 = CARTESIAN_POINT ( 'NONE',  ( -53.33387254593733928, -127.9375000027312126, 5.149110718188519620 ) ) ;
#24608 = DIRECTION ( 'NONE',  ( 0.000000000000000000, 0.000000000000000000, 1.000000000000000000 ) ) ;
#24609 = CARTESIAN_POINT ( 'NONE',  ( 1.339745962155615144, -100.7053418012614827, 4.999999999999999112 ) ) ;
#24610 = CARTESIAN_POINT ( 'NONE',  ( 2.071067811865459962, -168.8124999999999716, -5.000000000000015987 ) ) ;
#24611 = CARTESIAN_POINT ( 'NONE',  ( -4.458734124999999437, -59.39583333196773651, -2.574251347313719407 ) ) ;
#24612 = CARTESIAN_POINT ( 'NONE',  ( -4.999999999999998224, 10.20833333606451987, 2.886751345948131764 ) ) ;
#24613 = CARTESIAN_POINT ( 'NONE',  ( 4.458734124999998549, 16.27083333469892779, -2.574251347313721627 ) ) ;
#24614 = FACE_OUTER_BOUND ( 'NONE', #7609, .T. ) ;
#24615 = CARTESIAN_POINT ( 'NONE',  ( -3.152548672688508926E-16, -51.81249999863440792, -5.148502694627439702 ) ) ;
#24616 = CARTESIAN_POINT ( 'NONE',  ( 5.000000000000000000, -9.291666663935483683, -2.886751345948129988 ) ) ;
#24617 = DIRECTION ( 'NONE',  ( 0.000000000000000000, 0.000000000000000000, 1.000000000000000000 ) ) ;
#24618 = CARTESIAN_POINT ( 'NONE',  ( 0.000000000000000000, -120.0000000000000000, 0.000000000000000000 ) ) ;
#24619 = CARTESIAN_POINT ( 'NONE',  ( 2.229367062500001939, -90.22916666530106511, 3.861377020970579999 ) ) ;
#24620 = CARTESIAN_POINT ( 'NONE',  ( 2.229367062499998831, -108.6458333319677365, -3.861377020970580887 ) ) ;
#24621 = CARTESIAN_POINT ( 'NONE',  ( -4.458734124999999437, -12.56249999863440259, 0.000000000000000000 ) ) ;
#24622 =( BOUNDED_CURVE ( )  B_SPLINE_CURVE ( 2, ( #51066, #40451, #36275, #61359, #7010, #2199, #50437, #41082, #60091 ),
 .UNSPECIFIED., .F., .F. ) 
 B_SPLINE_CURVE_WITH_KNOTS ( ( 3, 2, 2, 2, 3 ),
 ( 0.01607142857142857331, 0.01666666666666666644, 0.01785714285714285615, 0.01904761904761904934, 0.01964285714285714593 ),
 .UNSPECIFIED. ) 
 CURVE ( )  GEOMETRIC_REPRESENTATION_ITEM ( )  RATIONAL_B_SPLINE_CURVE ( ( 0.9330127018922194093, 0.9330127018922195203, 1.000000000000000000, 0.8660254037844387076, 1.000000000000000000, 0.8660254037844387076, 1.000000000000000000, 0.9330127018922191873, 0.9330127018922194093 ) ) 
 REPRESENTATION_ITEM ( '' )  );
#24623 = VERTEX_POINT ( 'NONE', #10023 ) ;
#24624 = CARTESIAN_POINT ( 'NONE',  ( -9.184850993605147944E-16, -169.2500000000000000, 5.000000000000000000 ) ) ;
#24625 = CARTESIAN_POINT ( 'NONE',  ( -4.458734124999999437, -97.31249999863440792, 0.000000000000000000 ) ) ;
#24626 = CARTESIAN_POINT ( 'NONE',  ( -5.000000000000000888, -159.5625000027311842, 2.071067811865474617 ) ) ;
#24627 = CARTESIAN_POINT ( 'NONE',  ( 2.229367062499998831, -99.89583333196773651, -3.861377020970580887 ) ) ;
#24628 = CARTESIAN_POINT ( 'NONE',  ( 3.535533905932738197, -163.0000000027312126, -3.535533905932738197 ) ) ;
#24629 = CARTESIAN_POINT ( 'NONE',  ( 2.500000000000002220, -57.54166666393548013, 4.330127018922192761 ) ) ;
#24630 = CARTESIAN_POINT ( 'NONE',  ( -7.897836333153808397, -1.530409084195006653, -7.633857274177628938 ) ) ;
#24631 = CARTESIAN_POINT ( 'NONE',  ( -52.80376928212989185, -126.8750000013656205, -4.297418129356379346 ) ) ;
#24632 = CARTESIAN_POINT ( 'NONE',  ( -58.39396692619412477, -145.4375000013656063, 2.891590998281057701 ) ) ;
#24633 = CARTESIAN_POINT ( 'NONE',  ( -3.152548672688508926E-16, -19.56249999863440081, -5.148502694627439702 ) ) ;
#24634 = CARTESIAN_POINT ( 'NONE',  ( -4.458734124999999437, 4.354166668032260823, -2.574251347313719407 ) ) ;
#24635 = CARTESIAN_POINT ( 'NONE',  ( 2.229367062500001939, -60.22916666530106511, 3.861377020970579999 ) ) ;
#24636 = DIRECTION ( 'NONE',  ( 0.000000000000000000, 0.000000000000000000, 1.000000000000000000 ) ) ;
#24637 = CARTESIAN_POINT ( 'NONE',  ( 9.457646018065525792E-16, -13.06249999863440259, 5.148502694627439702 ) ) ;
#24638 = CARTESIAN_POINT ( 'NONE',  ( 5.000000000000000000, -8.374999997268814056, -6.123233995736766282E-16 ) ) ;
#24639 = CARTESIAN_POINT ( 'NONE',  ( 5.000000000000000000, -154.0000000000000284, 0.000000000000000000 ) ) ;
#24640 = CARTESIAN_POINT ( 'NONE',  ( -3.535250795749689387E-16, -6.249999999999998224, -5.773502691896257311 ) ) ;
#24641 = ORIENTED_EDGE ( 'NONE', *, *, #57552, .F. ) ;
#24642 = CARTESIAN_POINT ( 'NONE',  ( 4.458734124999999437, -40.06249999863440081, -5.460374474430324690E-16 ) ) ;
#24643 = CARTESIAN_POINT ( 'NONE',  ( 0.000000000000000000, -170.0000000000000000, 0.000000000000000000 ) ) ;
#24644 = CARTESIAN_POINT ( 'NONE',  ( -1.015826369459165157, 8.073766409993364590, -7.642786413619490737 ) ) ;
#24645 = CARTESIAN_POINT ( 'NONE',  ( -3.288228914120473245, 7.217643567644804747, -7.591235721156635030 ) ) ;
#24646 = CARTESIAN_POINT ( 'NONE',  ( 4.458734124999999437, -83.81249999863439371, -5.460374474430324690E-16 ) ) ;
#24647 = CARTESIAN_POINT ( 'NONE',  ( 2.229367062500001939, 20.77083333469892779, 3.861377020970579999 ) ) ;
#24648 = AXIS2_PLACEMENT_3D ( 'NONE', #14833, #44103, #10017 ) ;
#24649 = CARTESIAN_POINT ( 'NONE',  ( 4.458734125000001214, 10.10416666803226171, 2.574251347313718519 ) ) ;
#24650 = CARTESIAN_POINT ( 'NONE',  ( 1.975475456537005874E-15, -88.62499999726880162, 5.000000000000000000 ) ) ;
#24651 = CARTESIAN_POINT ( 'NONE',  ( -4.999999999999998224, 12.08333333333333215, 2.886751345948131764 ) ) ;
#24652 = CARTESIAN_POINT ( 'NONE',  ( 2.499999999999998668, 20.79166666939784847, -4.330127018922193649 ) ) ;
#24653 = CARTESIAN_POINT ( 'NONE',  ( -4.458734124999999437, 23.35416666803226349, -2.574251347313719407 ) ) ;
#24654 = CARTESIAN_POINT ( 'NONE',  ( -5.000000000000000000, -78.00000000000000000, 0.000000000000000000 ) ) ;
#24655 = CARTESIAN_POINT ( 'NONE',  ( 5.000000000000000000, 10.62500000273118594, -6.123233995736766282E-16 ) ) ;
#24656 = ORIENTED_EDGE ( 'NONE', *, *, #44166, .T. ) ;
#24657 = CARTESIAN_POINT ( 'NONE',  ( 0.000000000000000000, -120.0000000000000000, 0.000000000000000000 ) ) ;
#24658 = ORIENTED_EDGE ( 'NONE', *, *, #9525, .F. ) ;
#24660 = CARTESIAN_POINT ( 'NONE',  ( 5.000000000000000888, -36.58333333333332149, 2.886751345948126879 ) ) ;
#24659 = CARTESIAN_POINT ( 'NONE',  ( -2.499999999999996447, -103.8333333333333286, 4.330127018922195425 ) ) ;
#24661 = CARTESIAN_POINT ( 'NONE',  ( -3.152548672688508926E-16, -39.56249999863440081, -5.148502694627439702 ) ) ;
#24662 = CARTESIAN_POINT ( 'NONE',  ( -5.000000000000000000, -32.87499999726880873, 0.000000000000000000 ) ) ;
#24664 = VERTEX_POINT ( 'NONE', #23573 ) ;
#24663 = CARTESIAN_POINT ( 'NONE',  ( 4.458734124999998549, -67.72916666530107932, -2.574251347313721627 ) ) ;
#24665 = CARTESIAN_POINT ( 'NONE',  ( -56.48576386720575471, -150.0000000013655779, -4.591703134518078322 ) ) ;
#24666 = CARTESIAN_POINT ( 'NONE',  ( -4.458734124999999437, -15.31249999863440436, 0.000000000000000000 ) ) ;
#24668 = VERTEX_POINT ( 'NONE', #29635 ) ;
#24667 = CARTESIAN_POINT ( 'NONE',  ( -2.229367062500000163, -16.72916666530107577, -3.861377020970580443 ) ) ;
#24669 = CARTESIAN_POINT ( 'NONE',  ( 2.499999999999998668, -82.33333333333332860, -4.330127018922193649 ) ) ;
#24670 = CARTESIAN_POINT ( 'NONE',  ( 1.846868145590736310, -167.6250000013655779, 4.458734124999999437 ) ) ;
#24671 = CARTESIAN_POINT ( 'NONE',  ( -4.458734124999998549, -55.47916666530107221, 2.574251347313722516 ) ) ;
#24672 =( BOUNDED_CURVE ( )  B_SPLINE_CURVE ( 2, ( #25857, #30351, #26175, #10101, #11373, #21039, #49976, #44506, #40646 ),
 .UNSPECIFIED., .F., .F. ) 
 B_SPLINE_CURVE_WITH_KNOTS ( ( 3, 2, 2, 2, 3 ),
 ( 0.06041666666666666713, 0.06111111111111110911, 0.06250000000000000000, 0.06388888888888888395, 0.06458333333333333981 ),
 .UNSPECIFIED. ) 
 CURVE ( )  GEOMETRIC_REPRESENTATION_ITEM ( )  RATIONAL_B_SPLINE_CURVE ( ( 0.9330127018922194093, 0.9330127018922194093, 1.000000000000000000, 0.8660254037844387076, 1.000000000000000000, 0.8660254037844387076, 1.000000000000000000, 0.9330127018922187432, 0.9330127018922194093 ) ) 
 REPRESENTATION_ITEM ( '' )  );
#24673 = CARTESIAN_POINT ( 'NONE',  ( 2.499999999999998668, -80.20833333060213022, -4.330127018922193649 ) ) ;
#24675 = ORIENTED_EDGE ( 'NONE', *, *, #15761, .F. ) ;
#24674 = CARTESIAN_POINT ( 'NONE',  ( -5.000000000000000000, -48.87499999726880873, 0.000000000000000000 ) ) ;
#24676 = CARTESIAN_POINT ( 'NONE',  ( -50.18089887299979068, -146.6875000000000284, 2.462841084822635640 ) ) ;
#24677 = EDGE_CURVE ( 'NONE', #34132, #45305, #12936, .T. ) ;
#24678 = CARTESIAN_POINT ( 'NONE',  ( 2.229367062500001939, -26.22916666530106866, 3.861377020970579999 ) ) ;
#24679 = ORIENTED_EDGE ( 'NONE', *, *, #45606, .F. ) ;
#24680 = CARTESIAN_POINT ( 'NONE',  ( -4.458734124999999437, -165.1875000013655779, -5.460374474430324690E-16 ) ) ;
#24681 = CARTESIAN_POINT ( 'NONE',  ( -2.229367062499996610, -106.3958333319677365, 3.861377020970582219 ) ) ;
#24682 = ORIENTED_EDGE ( 'NONE', *, *, #36274, .T. ) ;
#24683 = CARTESIAN_POINT ( 'NONE',  ( -58.39396692619412477, -146.6875000013656063, 2.891590998281057701 ) ) ;
#24684 = AXIS2_PLACEMENT_3D ( 'NONE', #54844, #10775, #30386 ) ;
#24685 = CARTESIAN_POINT ( 'NONE',  ( -59.81910112700025905, -137.3125000027312126, -2.462841084822630311 ) ) ;
#24686 = CARTESIAN_POINT ( 'NONE',  ( -2.229367062499996610, -41.14583333196773651, 3.861377020970582219 ) ) ;
#24687 = CARTESIAN_POINT ( 'NONE',  ( 1.846868145590735200, -144.5000000013656063, -4.458734124999999437 ) ) ;
#24688 = DIRECTION ( 'NONE',  ( -0.000000000000000000, 1.000000000000000000, -0.000000000000000000 ) ) ;
#24689 = AXIS2_PLACEMENT_3D ( 'NONE', #32405, #7975, #57186 ) ;
#24690 = CARTESIAN_POINT ( 'NONE',  ( 1.975475456537005874E-15, 9.375000002731185944, 5.000000000000000000 ) ) ;
#24691 = CARTESIAN_POINT ( 'NONE',  ( -2.229367062500000163, -10.47916666530106866, -3.861377020970580443 ) ) ;
#24692 = CARTESIAN_POINT ( 'NONE',  ( 4.458734124999998549, -102.9791666653010651, -2.574251347313721627 ) ) ;
#24693 = VERTEX_POINT ( 'NONE', #33530 ) ;
#24694 = EDGE_CURVE ( 'NONE', #22715, #2538, #40917, .T. ) ;
#24695 = CARTESIAN_POINT ( 'NONE',  ( -5.000000000000000888, -167.4375000000000284, 2.071067811865474617 ) ) ;
#24696 = CARTESIAN_POINT ( 'NONE',  ( 9.457646018065525792E-16, -34.31249999863440792, 5.148502694627439702 ) ) ;
#24697 = EDGE_CURVE ( 'NONE', #6026, #22810, #27775, .T. ) ;
#24698 = CARTESIAN_POINT ( 'NONE',  ( 5.000000000000000000, 7.625000002731186832, -6.123233995736766282E-16 ) ) ;
#24699 = CARTESIAN_POINT ( 'NONE',  ( -6.000000000000000000, -114.9999999999999858, -1.500000000000000000 ) ) ;
#24700 = CARTESIAN_POINT ( 'NONE',  ( -55.35523342533222291, -132.3125000013656063, 4.444560631937231499 ) ) ;
#24701 = CARTESIAN_POINT ( 'NONE',  ( 2.229367062499998831, -72.89583333196773651, -3.861377020970580887 ) ) ;
#24702 = CARTESIAN_POINT ( 'NONE',  ( -3.535533905932738641, -144.5000000027311842, 3.535533905932737309 ) ) ;
#24703 = DIRECTION ( 'NONE',  ( -0.000000000000000000, 1.000000000000000000, -0.000000000000000000 ) ) ;
#24704 = CARTESIAN_POINT ( 'NONE',  ( 5.000000000000000000, 14.62500000273118594, -6.123233995736766282E-16 ) ) ;
#24705 = CARTESIAN_POINT ( 'NONE',  ( 2.229367062499998831, 6.104166668032262599, -3.861377020970580887 ) ) ;
#24706 = ORIENTED_EDGE ( 'NONE', *, *, #29108, .T. ) ;
#24707 = CARTESIAN_POINT ( 'NONE',  ( 0.000000000000000000, -120.0000000000000000, 5.000000000000000000 ) ) ;
#24708 = CARTESIAN_POINT ( 'NONE',  ( 5.000000000000000888, 2.416666666666667851, 2.886751345948126879 ) ) ;
#24710 = CARTESIAN_POINT ( 'NONE',  ( -4.458734124999998549, -31.22916666530107221, 2.574251347313722516 ) ) ;
#24709 = CARTESIAN_POINT ( 'NONE',  ( 1.060575238724906964E-15, -94.75000000000000000, 5.773502691896257311 ) ) ;
#24711 = CARTESIAN_POINT ( 'NONE',  ( -4.458734124999999437, -79.56249999863440792, 0.000000000000000000 ) ) ;
#24712 = CARTESIAN_POINT ( 'NONE',  ( -4.458734124999999437, 17.43750000136559208, 0.000000000000000000 ) ) ;
#24713 = CYLINDRICAL_SURFACE ( 'NONE', #49997, 5.000000000000000000 ) ;
#24714 = EDGE_CURVE ( 'NONE', #9036, #39802, #41195, .T. ) ;
#24715 = CARTESIAN_POINT ( 'NONE',  ( -58.39396692619412477, -143.4375000013656063, 2.891590998281057701 ) ) ;
#24716 = CARTESIAN_POINT ( 'NONE',  ( -2.229367062500000163, -0.4791666653010707710, -3.861377020970580443 ) ) ;
#24717 = CARTESIAN_POINT ( 'NONE',  ( 4.458734124999999437, 21.93750000136559208, -5.460374474430324690E-16 ) ) ;
#24718 = CARTESIAN_POINT ( 'NONE',  ( 2.229367062500001939, -41.22916666530107932, 3.861377020970579999 ) ) ;
#24719 = CARTESIAN_POINT ( 'NONE',  ( -6.972266317189433020E-16, -46.12499999726880873, -5.000000000000000000 ) ) ;
#24720 = CARTESIAN_POINT ( 'NONE',  ( -4.458734124999997661, 1.770833334698928008, 2.574251347313722516 ) ) ;
#24721 = ORIENTED_EDGE ( 'NONE', *, *, #57204, .F. ) ;
#24722 = CARTESIAN_POINT ( 'NONE',  ( -2.229367062499996610, -25.39583333196773651, 3.861377020970582219 ) ) ;
#24723 = CARTESIAN_POINT ( 'NONE',  ( 2.229367062499998831, -70.64583333196773651, -3.861377020970580887 ) ) ;
#24724 = CARTESIAN_POINT ( 'NONE',  ( 2.500000000000002220, -103.5416666639354730, 4.330127018922192761 ) ) ;
#24725 = CARTESIAN_POINT ( 'NONE',  ( 2.229367062499998831, 27.35416666803225993, -3.861377020970580887 ) ) ;
#24726 = CARTESIAN_POINT ( 'NONE',  ( -5.000000000000000000, 9.916666666666667851, -2.886751345948128211 ) ) ;
#24727 = EDGE_CURVE ( 'NONE', #36804, #29555, #10107, .T. ) ;
#24728 = CARTESIAN_POINT ( 'NONE',  ( 4.458734125000000326, -110.1458333319677365, 2.574251347313718519 ) ) ;
#24729 = CARTESIAN_POINT ( 'NONE',  ( -4.458734124999999437, -72.56249999863439371, 0.000000000000000000 ) ) ;
#24730 = CARTESIAN_POINT ( 'NONE',  ( -5.000000000000000000, -62.00000000000000000, 0.000000000000000000 ) ) ;
#24731 = CARTESIAN_POINT ( 'NONE',  ( -4.999999999999998224, -21.91666666666666785, 2.886751345948131764 ) ) ;
#24732 = CARTESIAN_POINT ( 'NONE',  ( -5.000000000000000000, 28.04166666939785202, -2.886751345948128211 ) ) ;
#24733 = ORIENTED_EDGE ( 'NONE', *, *, #53095, .F. ) ;
#24734 = FACE_OUTER_BOUND ( 'NONE', #13041, .T. ) ;
#24735 = DIRECTION ( 'NONE',  ( -0.000000000000000000, 1.000000000000000000, -0.000000000000000000 ) ) ;
#24736 = CARTESIAN_POINT ( 'NONE',  ( -4.999999999999999112, -17.91666666666666430, 2.886751345948131764 ) ) ;
#24737 = CARTESIAN_POINT ( 'NONE',  ( 4.458734124999998549, -19.72916666530107221, -2.574251347313721627 ) ) ;
#24738 = VECTOR ( 'NONE', #10091, 1000.000000000000000 ) ;
#24739 = CARTESIAN_POINT ( 'NONE',  ( -4.458734124999999437, -81.39583333196773651, -2.574251347313719407 ) ) ;
#24740 = CARTESIAN_POINT ( 'NONE',  ( -3.152801135295367096, -169.3125000013656063, -3.152801135295367541 ) ) ;
#24741 = CARTESIAN_POINT ( 'NONE',  ( -5.000000000000000000, -18.95833333060214443, -2.886751345948128211 ) ) ;
#24743 = ORIENTED_EDGE ( 'NONE', *, *, #61479, .T. ) ;
#24742 = CARTESIAN_POINT ( 'NONE',  ( -4.458734124999998549, -50.22916666530107221, 2.574251347313722516 ) ) ;
#24744 = CARTESIAN_POINT ( 'NONE',  ( -5.000000000000000000, -75.87499999726880162, 0.000000000000000000 ) ) ;
#24746 = EDGE_LOOP ( 'NONE', ( #16479, #24443, #48135, #34235 ) ) ;
#24745 = CARTESIAN_POINT ( 'NONE',  ( -3.152548672688508926E-16, 0.1875000013655953035, -5.148502694627439702 ) ) ;
#24747 = CARTESIAN_POINT ( 'NONE',  ( 2.500000000000002220, -65.66666666666667140, 4.330127018922192761 ) ) ;
#24748 = CARTESIAN_POINT ( 'NONE',  ( -1.846868145590737420, -158.0000000013655779, 4.458734124999999437 ) ) ;
#24749 = CARTESIAN_POINT ( 'NONE',  ( -2.229367062500000163, -43.72916666530106511, -3.861377020970580443 ) ) ;
#24750 = CARTESIAN_POINT ( 'NONE',  ( -2.499999999999996447, -15.70833333060214443, 4.330127018922195425 ) ) ;
#24751 = CARTESIAN_POINT ( 'NONE',  ( 5.000000000000000000, -162.0625000000000000, 2.071067811865478614 ) ) ;
#24752 = CYLINDRICAL_SURFACE ( 'NONE', #8732, 5.000000000000000000 ) ;
#24753 = CARTESIAN_POINT ( 'NONE',  ( -50.40829686548195099, -128.2500000013656063, -1.485763867205728284 ) ) ;
#24754 = EDGE_CURVE ( 'NONE', #62985, #58767, #10658, .T. ) ;
#24755 = CARTESIAN_POINT ( 'NONE',  ( 4.458734124999998549, -9.979166665301068662, -2.574251347313721627 ) ) ;
#24756 = CARTESIAN_POINT ( 'NONE',  ( 9.457646018065525792E-16, -45.31249999863440081, 5.148502694627439702 ) ) ;
#24757 =( BOUNDED_CURVE ( )  B_SPLINE_CURVE ( 2, ( #39798, #49775, #50098, #21153, #26286, #46229, #41391, #16643, #1871 ),
 .UNSPECIFIED., .F., .F. ) 
 B_SPLINE_CURVE_WITH_KNOTS ( ( 3, 2, 2, 2, 3 ),
 ( 0.5354166666666666519, 0.5361111111111110938, 0.5374999999999999778, 0.5388888888888888618, 0.5395833333333333037 ),
 .UNSPECIFIED. ) 
 CURVE ( )  GEOMETRIC_REPRESENTATION_ITEM ( )  RATIONAL_B_SPLINE_CURVE ( ( 0.9330127018922194093, 0.9330127018922194093, 1.000000000000000000, 0.8660254037844387076, 1.000000000000000000, 0.8660254037844387076, 1.000000000000000000, 0.9330127018922194093, 0.9330127018922194093 ) ) 
 REPRESENTATION_ITEM ( '' )  );
#24758 = EDGE_CURVE ( 'NONE', #44925, #1202, #16704, .T. ) ;
#24759 = DIRECTION ( 'NONE',  ( -0.000000000000000000, 1.000000000000000000, -0.000000000000000000 ) ) ;
#24760 = CARTESIAN_POINT ( 'NONE',  ( -1.846868145590734756, -150.1250000013655779, -4.458734125000000326 ) ) ;
#24761 = CARTESIAN_POINT ( 'NONE',  ( -2.229367062500000163, -87.72916666530107932, -3.861377020970580443 ) ) ;
#24762 = CARTESIAN_POINT ( 'NONE',  ( -3.750000000000007105, -6.495190528383289141, 0.000000000000000000 ) ) ;
#24763 = VERTEX_POINT ( 'NONE', #36383 ) ;
#24764 = CARTESIAN_POINT ( 'NONE',  ( 7.204675194429079505E-15, 26.87500000273118417, -5.000000000000000000 ) ) ;
#24765 = CARTESIAN_POINT ( 'NONE',  ( -2.499999999999996447, -68.70833333060214443, 4.330127018922195425 ) ) ;
#24766 = CARTESIAN_POINT ( 'NONE',  ( -50.01589407740564042, -151.7500000027312410, 0.3983568153799778022 ) ) ;
#24767 = CARTESIAN_POINT ( 'NONE',  ( 1.975475456537005874E-15, -61.74999999999999289, 5.000000000000000000 ) ) ;
#24768 = EDGE_LOOP ( 'NONE', ( #22642, #38058, #37826, #24034 ) ) ;
#24769 = CARTESIAN_POINT ( 'NONE',  ( -4.458734124999998549, 1.770833334698927786, 2.574251347313722516 ) ) ;
#24770 = ADVANCED_BREP_SHAPE_REPRESENTATION ( '', ( #29015, #43054 ), #21498 ) ;
#24771 = CARTESIAN_POINT ( 'NONE',  ( -2.500000000000000444, -14.16666666666666785, -4.330127018922193649 ) ) ;
#24772 = CARTESIAN_POINT ( 'NONE',  ( -4.458734124999998549, -15.47916666530107399, 2.574251347313722516 ) ) ;
#24773 = EDGE_CURVE ( 'NONE', #24693, #57442, #20650, .T. ) ;
#24774 = CARTESIAN_POINT ( 'NONE',  ( -4.999999999999998224, -100.9166666666666572, 2.886751345948131764 ) ) ;
#24775 = CARTESIAN_POINT ( 'NONE',  ( 4.458734125000001214, -3.895833331967739621, 2.574251347313718519 ) ) ;
#24776 = CARTESIAN_POINT ( 'NONE',  ( -5.000000000000000000, 4.125000002731186832, 0.000000000000000000 ) ) ;
#24777 = CARTESIAN_POINT ( 'NONE',  ( -4.458734124999999437, -151.0000000013656063, -1.846868145590735644 ) ) ;
#24778 = CARTESIAN_POINT ( 'NONE',  ( -4.458734124999999437, 22.35416666803225638, -2.574251347313719407 ) ) ;
#24779 = EDGE_LOOP ( 'NONE', ( #62015, #51283, #31288, #62378 ) ) ;
#24780 = CARTESIAN_POINT ( 'NONE',  ( -4.458734124999997661, -99.22916666530105090, 2.574251347313722516 ) ) ;
#24781 = CARTESIAN_POINT ( 'NONE',  ( -4.999999999999998224, -74.91666666666665719, 2.886751345948131764 ) ) ;
#24782 = CARTESIAN_POINT ( 'NONE',  ( 9.457646018065525792E-16, -13.06249999863440259, 5.148502694627439702 ) ) ;
#24783 = AXIS2_PLACEMENT_3D ( 'NONE', #50618, #26493, #15889 ) ;
#24784 = CARTESIAN_POINT ( 'NONE',  ( 1.339745962155612702, 8.830341803992666883, -5.000000000000000000 ) ) ;
#24785 = CARTESIAN_POINT ( 'NONE',  ( -59.29741812935640155, -152.6250000013656063, -2.196230717870135685 ) ) ;
#24786 = CARTESIAN_POINT ( 'NONE',  ( 2.499999999999998668, -43.20833333060214443, -4.330127018922193649 ) ) ;
#24787 = CARTESIAN_POINT ( 'NONE',  ( 1.339745962155615144, -67.58034179853029855, 4.999999999999999112 ) ) ;
#24788 = CARTESIAN_POINT ( 'NONE',  ( 2.229367062499998831, 13.35416666803226171, -3.861377020970580887 ) ) ;
#24789 = CARTESIAN_POINT ( 'NONE',  ( -5.007715329123872641E-16, -8.660254037844399733, -7.422398894150038728 ) ) ;
#24790 = CARTESIAN_POINT ( 'NONE',  ( 1.339745962155615144, 9.294658198738520838, 4.999999999999999112 ) ) ;
#24791 = CARTESIAN_POINT ( 'NONE',  ( 4.458734124999999437, 17.18750000136559564, -5.460374474430324690E-16 ) ) ;
#24792 = CARTESIAN_POINT ( 'NONE',  ( -2.229367062500000163, -64.47916666530106511, -3.861377020970580443 ) ) ;
#24793 = ORIENTED_EDGE ( 'NONE', *, *, #60942, .T. ) ;
#24794 = AXIS2_PLACEMENT_3D ( 'NONE', #26910, #46529, #51674 ) ;
#24795 = CARTESIAN_POINT ( 'NONE',  ( -4.458734124999999437, -9.562499998634406140, 0.000000000000000000 ) ) ;
#24796 = CARTESIAN_POINT ( 'NONE',  ( 2.071067811865472841, -168.9375000027311842, -5.000000000000002665 ) ) ;
#24797 = CARTESIAN_POINT ( 'NONE',  ( -4.999999999999999112, 3.083333333333333925, 2.886751345948131764 ) ) ;
#24798 = CARTESIAN_POINT ( 'NONE',  ( -3.152801135295367985, -166.8125000013656063, 3.152801135295367096 ) ) ;
#24799 = DIRECTION ( 'NONE',  ( 0.000000000000000000, 0.000000000000000000, 1.000000000000000000 ) ) ;
#24800 = CARTESIAN_POINT ( 'NONE',  ( -4.458734124999998549, -54.22916666530107221, 2.574251347313722516 ) ) ;
#24801 = CARTESIAN_POINT ( 'NONE',  ( 2.500000000000002220, -88.54166666393548724, 4.330127018922192761 ) ) ;
#24802 = CARTESIAN_POINT ( 'NONE',  ( -2.229367062500000163, -35.47916666530107221, -3.861377020970580443 ) ) ;
#24803 = CARTESIAN_POINT ( 'NONE',  ( 1.975475456537005874E-15, -38.75000000000000000, 5.000000000000000000 ) ) ;
#24804 = CARTESIAN_POINT ( 'NONE',  ( 1.975475456537005874E-15, -98.62499999726880162, 5.000000000000000000 ) ) ;
#24805 = CARTESIAN_POINT ( 'NONE',  ( 0.000000000000000000, -170.0000000000000000, 5.000000000000000000 ) ) ;
#24806 = CARTESIAN_POINT ( 'NONE',  ( 4.458734124999997661, -153.7500000013656063, 1.846868145590737864 ) ) ;
#24807 =( BOUNDED_CURVE ( )  B_SPLINE_CURVE ( 2, ( #61965, #28480, #52616, #62599, #42956, #18521, #58066, #48095, #4050 ),
 .UNSPECIFIED., .F., .F. ) 
 B_SPLINE_CURVE_WITH_KNOTS ( ( 3, 2, 2, 2, 3 ),
 ( 0.3339285714285714080, 0.3345238095238095011, 0.3357142857142856873, 0.3369047619047619291, 0.3375000000000000222 ),
 .UNSPECIFIED. ) 
 CURVE ( )  GEOMETRIC_REPRESENTATION_ITEM ( )  RATIONAL_B_SPLINE_CURVE ( ( 0.9330127018922194093, 0.9330127018922194093, 1.000000000000000000, 0.8660254037844387076, 1.000000000000000000, 0.8660254037844387076, 1.000000000000000000, 0.9330127018922194093, 0.9330127018922194093 ) ) 
 REPRESENTATION_ITEM ( '' )  );
#24808 = CARTESIAN_POINT ( 'NONE',  ( -2.500000000000000444, -44.16666666666665719, -4.330127018922193649 ) ) ;
#24809 = CARTESIAN_POINT ( 'NONE',  ( 2.500000000000002220, -98.54166666393545881, 4.330127018922192761 ) ) ;
#24810 = CARTESIAN_POINT ( 'NONE',  ( 3.535533905932738197, -162.8750000000000284, -3.535533905932738197 ) ) ;
#24811 = ORIENTED_EDGE ( 'NONE', *, *, #22011, .T. ) ;
#24812 = CARTESIAN_POINT ( 'NONE',  ( 2.229367062499998831, -100.6458333319677365, -3.861377020970580887 ) ) ;
#24813 = CARTESIAN_POINT ( 'NONE',  ( -3.152548672688508926E-16, 5.187500001365592972, -5.148502694627439702 ) ) ;
#24814 = CARTESIAN_POINT ( 'NONE',  ( -9.184850993605147944E-16, -162.2500000000000000, 5.000000000000000000 ) ) ;
#24815 = CARTESIAN_POINT ( 'NONE',  ( -5.000000000000000000, -2.083333333333333037, -2.886751345948128211 ) ) ;
#24816 = CARTESIAN_POINT ( 'NONE',  ( -4.458734124999997661, -69.22916666530107932, 2.574251347313722516 ) ) ;
#24817 = CARTESIAN_POINT ( 'NONE',  ( 1.975475456537005874E-15, -61.74999999999999289, 5.000000000000000000 ) ) ;
#24818 = CARTESIAN_POINT ( 'NONE',  ( -3.535250795749689387E-16, -1.124999997268814056, -5.773502691896257311 ) ) ;
#24820 = VERTEX_POINT ( 'NONE', #40882 ) ;
#24819 = CARTESIAN_POINT ( 'NONE',  ( 4.458734124999998549, -34.72916666530107221, -2.574251347313721627 ) ) ;
#24821 = DIRECTION ( 'NONE',  ( -0.000000000000000000, 1.000000000000000000, -0.000000000000000000 ) ) ;
#24822 = DIRECTION ( 'NONE',  ( 0.000000000000000000, 0.000000000000000000, 1.000000000000000000 ) ) ;
#24823 = VERTEX_POINT ( 'NONE', #709 ) ;
#24824 = CARTESIAN_POINT ( 'NONE',  ( -52.53715891517739323, -136.4375000000000000, -4.819101127000233298 ) ) ;
#24825 = CARTESIAN_POINT ( 'NONE',  ( -4.999999999999999112, -51.91666666666667140, 2.886751345948131764 ) ) ;
#24827 = CARTESIAN_POINT ( 'NONE',  ( -4.458734124999999437, -24.64583333196773651, -2.574251347313719407 ) ) ;
#24826 = CARTESIAN_POINT ( 'NONE',  ( 2.499999999999998668, -17.20833333060214443, -4.330127018922193649 ) ) ;
#24828 = CARTESIAN_POINT ( 'NONE',  ( 2.499999999999998668, -32.20833333060215153, -4.330127018922193649 ) ) ;
#24829 = CARTESIAN_POINT ( 'NONE',  ( -2.229367062500000163, -72.47916666530107932, -3.861377020970580443 ) ) ;
#24830 = CARTESIAN_POINT ( 'NONE',  ( -3.152801135295367096, -144.3125000013655779, -3.152801135295367541 ) ) ;
#24831 = CARTESIAN_POINT ( 'NONE',  ( 4.458734124999999437, -80.81249999863440792, -5.460374474430324690E-16 ) ) ;
#24832 = CARTESIAN_POINT ( 'NONE',  ( -54.64476657466781973, -140.0625000013656063, -4.444560631937228834 ) ) ;
#24833 = CARTESIAN_POINT ( 'NONE',  ( -4.458734124999998549, -30.47916666530107221, 2.574251347313722516 ) ) ;
#24834 = CARTESIAN_POINT ( 'NONE',  ( -5.000000000000000000, -73.95833333060214443, -2.886751345948128211 ) ) ;
#24836 = VERTEX_POINT ( 'NONE', #30599 ) ;
#24835 = EDGE_CURVE ( 'NONE', #13829, #18331, #56156, .T. ) ;
#24837 = EDGE_CURVE ( 'NONE', #16286, #42590, #29822, .T. ) ;
#24838 = CARTESIAN_POINT ( 'NONE',  ( 1.339745962155612702, -51.29465819873851729, -5.000000000000000000 ) ) ;
#24839 = ORIENTED_EDGE ( 'NONE', *, *, #25650, .F. ) ;
#24840 = CARTESIAN_POINT ( 'NONE',  ( -2.229367062500000163, -72.72916666530107932, -3.861377020970580443 ) ) ;
#24841 = CARTESIAN_POINT ( 'NONE',  ( -2.499999999999996447, 8.291666669397852019, 4.330127018922195425 ) ) ;
#24842 = ADVANCED_FACE ( 'NONE', ( #56965 ), #62815, .T. ) ;
#24843 = ORIENTED_EDGE ( 'NONE', *, *, #47934, .F. ) ;
#24844 = CARTESIAN_POINT ( 'NONE',  ( 1.975475456537005874E-15, 17.25000000000000000, 5.000000000000000000 ) ) ;
#24845 = CARTESIAN_POINT ( 'NONE',  ( 2.229367062499998831, -59.89583333196774362, -3.861377020970580887 ) ) ;
#24846 = EDGE_CURVE ( 'NONE', #14700, #43870, #43354, .T. ) ;
#24847 = CARTESIAN_POINT ( 'NONE',  ( 4.458734124999998549, -3.979166665301070438, -2.574251347313721627 ) ) ;
#24848 = ORIENTED_EDGE ( 'NONE', *, *, #10820, .T. ) ;
#24849 = EDGE_CURVE ( 'NONE', #2012, #1843, #3564, .T. ) ;
#24850 = LINE ( 'NONE', #53791, #27502 ) ;
#24851 = CARTESIAN_POINT ( 'NONE',  ( 0.000000000000000000, -170.0000000000000000, 0.000000000000000000 ) ) ;
#24852 = ADVANCED_FACE ( 'NONE', ( #62427 ), #37645, .T. ) ;
#24853 = CARTESIAN_POINT ( 'NONE',  ( -4.458734124999999437, 12.60416666803225993, -2.574251347313719407 ) ) ;
#24854 = CARTESIAN_POINT ( 'NONE',  ( -57.19623071787017210, -140.3750000013656063, 4.297418129356382899 ) ) ;
#24855 = DIRECTION ( 'NONE',  ( -0.000000000000000000, 1.000000000000000000, -0.000000000000000000 ) ) ;
#24856 = CARTESIAN_POINT ( 'NONE',  ( 4.458734124999999437, -165.4375000013655779, 0.000000000000000000 ) ) ;
#24857 =( BOUNDED_CURVE ( )  B_SPLINE_CURVE ( 2, ( #12678, #47094, #37442, #60633, #6911, #12037, #36177, #11715, #21707 ),
 .UNSPECIFIED., .F., .F. ) 
 B_SPLINE_CURVE_WITH_KNOTS ( ( 3, 2, 2, 2, 3 ),
 ( 0.9803571428571428159, 0.9809523809523809090, 0.9821428571428570953, 0.9833333333333332815, 0.9839285714285714857 ),
 .UNSPECIFIED. ) 
 CURVE ( )  GEOMETRIC_REPRESENTATION_ITEM ( )  RATIONAL_B_SPLINE_CURVE ( ( 0.9330127018922194093, 0.9330127018922194093, 1.000000000000000000, 0.8660254037844387076, 1.000000000000000000, 0.8660254037844387076, 1.000000000000000000, 0.9330127018922130810, 0.9330127018922194093 ) ) 
 REPRESENTATION_ITEM ( '' )  );
#24859 = ADVANCED_FACE ( 'NONE', ( #11926 ), #61791, .T. ) ;
#24858 = ORIENTED_EDGE ( 'NONE', *, *, #16862, .F. ) ;
#24860 = CARTESIAN_POINT ( 'NONE',  ( -3.152548672688508926E-16, -79.56249999863440792, -5.148502694627439702 ) ) ;
#24861 = EDGE_CURVE ( 'NONE', #32177, #8165, #42463, .T. ) ;
#24862 = CARTESIAN_POINT ( 'NONE',  ( 2.500000000000002220, -0.5416666639354792423, 4.330127018922192761 ) ) ;
#24863 = CARTESIAN_POINT ( 'NONE',  ( 9.457646018065525792E-16, 2.937500001365594304, 5.148502694627439702 ) ) ;
#24864 = CARTESIAN_POINT ( 'NONE',  ( -3.535250795749689387E-16, -86.25000000000000000, -5.773502691896257311 ) ) ;
#24865 = CARTESIAN_POINT ( 'NONE',  ( 5.000000000000000000, -40.29166666393548013, -2.886751345948130876 ) ) ;
#24866 = CARTESIAN_POINT ( 'NONE',  ( -4.458734124999998549, -63.47916666530106511, 2.574251347313722516 ) ) ;
#24867 = CARTESIAN_POINT ( 'NONE',  ( 5.000000000000000888, -26.45833333060214443, 2.886751345948126879 ) ) ;
#24868 = LINE ( 'NONE', #45436, #19334 ) ;
#24869 = CARTESIAN_POINT ( 'NONE',  ( -6.972266317189433020E-16, -41.24999999999998579, -5.000000000000000000 ) ) ;
#24870 = CARTESIAN_POINT ( 'NONE',  ( -55.00000000000002132, -155.0000000000000284, 1.734723475976807094E-15 ) ) ;
#24871 = CARTESIAN_POINT ( 'NONE',  ( 2.499999999999998668, -3.208333330602147093, -4.330127018922193649 ) ) ;
#24872 = CARTESIAN_POINT ( 'NONE',  ( -3.152548672688508926E-16, -48.56249999863440792, -5.148502694627439702 ) ) ;
#24873 = CARTESIAN_POINT ( 'NONE',  ( 2.229367062500001939, -34.22916666530107221, 3.861377020970579999 ) ) ;
#24874 = CARTESIAN_POINT ( 'NONE',  ( -4.458734124999999437, 6.437500001365593860, 0.000000000000000000 ) ) ;
#24875 = CARTESIAN_POINT ( 'NONE',  ( 5.000000000000000888, -150.9375000000000000, -2.071067811865475505 ) ) ;
#24876 = CARTESIAN_POINT ( 'NONE',  ( 5.000000000000000000, 22.50000000000000000, -6.123233995736766282E-16 ) ) ;
#24877 = CARTESIAN_POINT ( 'NONE',  ( -3.535533905932738641, -148.5000000027311842, 3.535533905932737309 ) ) ;
#24878 = CARTESIAN_POINT ( 'NONE',  ( -2.500000000000000444, -50.16666666666666430, -4.330127018922193649 ) ) ;
#24879 = CARTESIAN_POINT ( 'NONE',  ( -2.229367062499996610, -35.14583333196772941, 3.861377020970582219 ) ) ;
#24880 = CARTESIAN_POINT ( 'NONE',  ( 5.000000000000000000, -71.37499999726880162, -6.123233995736766282E-16 ) ) ;
#24881 = CARTESIAN_POINT ( 'NONE',  ( -59.29741812935640155, -142.8750000013656063, -2.196230717870135685 ) ) ;
#24882 = FACE_OUTER_BOUND ( 'NONE', #15018, .T. ) ;
#24883 = CARTESIAN_POINT ( 'NONE',  ( 2.499999999999998668, -37.33333333333332860, -4.330127018922193649 ) ) ;
#24884 = CARTESIAN_POINT ( 'NONE',  ( 2.229367062500001939, -82.22916666530106511, 3.861377020970579999 ) ) ;
#24885 = CARTESIAN_POINT ( 'NONE',  ( -1.846868145590737420, -164.0000000013656063, 4.458734124999997661 ) ) ;
#24886 = CARTESIAN_POINT ( 'NONE',  ( -2.229367062499996610, -38.14583333196773651, 3.861377020970582219 ) ) ;
#24887 = CARTESIAN_POINT ( 'NONE',  ( 1.975475456537005874E-15, -70.62499999726880162, 5.000000000000000000 ) ) ;
#24888 = DIRECTION ( 'NONE',  ( -1.000000000000000000, 0.000000000000000000, 0.000000000000000000 ) ) ;
#24889 = CARTESIAN_POINT ( 'NONE',  ( 5.000000000000000000, -24.50000000000000000, -6.123233995736766282E-16 ) ) ;
#24890 = CARTESIAN_POINT ( 'NONE',  ( -4.458734124999999437, -141.9375000013656063, -5.460374474430324690E-16 ) ) ;
#24891 = ORIENTED_EDGE ( 'NONE', *, *, #27618, .T. ) ;
#24892 = CARTESIAN_POINT ( 'NONE',  ( 4.458734124999999437, 27.93750000136559208, -5.460374474430324690E-16 ) ) ;
#24893 = ORIENTED_EDGE ( 'NONE', *, *, #36239, .F. ) ;
#24894 = CARTESIAN_POINT ( 'NONE',  ( -2.229367062499996610, -63.39583333196774362, 3.861377020970582219 ) ) ;
#24895 = CARTESIAN_POINT ( 'NONE',  ( 2.499999999999998668, 19.79166666939785202, -4.330127018922193649 ) ) ;
#24896 = CARTESIAN_POINT ( 'NONE',  ( 2.500000000000002220, -48.54166666393547303, 4.330127018922192761 ) ) ;
#24897 = CARTESIAN_POINT ( 'NONE',  ( -5.000000000000000000, 11.00000000000000000, 0.000000000000000000 ) ) ;
#24898 = CARTESIAN_POINT ( 'NONE',  ( -2.229367062499996610, -49.14583333196772941, 3.861377020970582219 ) ) ;
#24899 = CARTESIAN_POINT ( 'NONE',  ( -4.458734124999998549, -7.229166665301073103, 2.574251347313722516 ) ) ;
#24900 = CARTESIAN_POINT ( 'NONE',  ( -1.339745962155613812, -9.205341801261479162, -5.000000000000000000 ) ) ;
#24901 = CARTESIAN_POINT ( 'NONE',  ( 5.000000000000000000, -91.37499999726880162, -6.123233995736766282E-16 ) ) ;
#24902 = PRODUCT_DEFINITION ( 'UNKNOWN', '', #48237, #39061 ) ;
#24903 = CARTESIAN_POINT ( 'NONE',  ( -5.000000000000000000, -10.08333333333333393, -2.886751345948128211 ) ) ;
#24905 = CARTESIAN_POINT ( 'NONE',  ( -2.229367062500000163, -19.47916666530106866, -3.861377020970580443 ) ) ;
#24904 = CARTESIAN_POINT ( 'NONE',  ( -4.999999999999998224, -78.91666666666665719, 2.886751345948131764 ) ) ;
#24906 = CARTESIAN_POINT ( 'NONE',  ( 1.339745962155612702, 10.83034180399266511, -5.000000000000000000 ) ) ;
#24907 = CARTESIAN_POINT ( 'NONE',  ( -3.152548672688508926E-16, -56.56249999863439371, -5.148502694627439702 ) ) ;
#24908 = CARTESIAN_POINT ( 'NONE',  ( 1.846868145590736310, -155.8750000013655779, 4.458734124999999437 ) ) ;
#24909 = CARTESIAN_POINT ( 'NONE',  ( 2.499999999999998668, -58.20833333060214443, -4.330127018922193649 ) ) ;
#24910 = ORIENTED_EDGE ( 'NONE', *, *, #13894, .T. ) ;
#24911 = CARTESIAN_POINT ( 'NONE',  ( -6.972266317189433020E-16, -86.25000000000001421, -5.000000000000000000 ) ) ;
#24912 = CARTESIAN_POINT ( 'NONE',  ( -2.229367062500000163, 3.270833334698929118, -3.861377020970580443 ) ) ;
#24913 = ORIENTED_EDGE ( 'NONE', *, *, #5012, .F. ) ;
#24915 = CARTESIAN_POINT ( 'NONE',  ( 1.339745962155627135, 11.83034180399266333, -4.999999999999991118 ) ) ;
#24914 = CARTESIAN_POINT ( 'NONE',  ( 5.000000000000000000, -56.41666666666667140, -2.886751345948130876 ) ) ;
#24916 = CARTESIAN_POINT ( 'NONE',  ( -4.458734124999999437, -156.9375000013655779, -5.460374474430324690E-16 ) ) ;
#24917 = ORIENTED_EDGE ( 'NONE', *, *, #59143, .T. ) ;
#24918 = CARTESIAN_POINT ( 'NONE',  ( 1.339745962155612702, -83.29465819873851729, -5.000000000000000000 ) ) ;
#24919 = CARTESIAN_POINT ( 'NONE',  ( -51.19402409849444524, -131.5000000000000284, -3.242614290531456334 ) ) ;
#24920 = CARTESIAN_POINT ( 'NONE',  ( 5.000000000000000000, -161.1875000027312126, 2.071067811865478614 ) ) ;
#24921 = CARTESIAN_POINT ( 'NONE',  ( -2.229367062500000163, -45.72916666530106511, -3.861377020970580443 ) ) ;
#24922 = EDGE_LOOP ( 'NONE', ( #12724, #10456, #48736, #32764 ) ) ;
#24923 = CARTESIAN_POINT ( 'NONE',  ( -6.972266317189433020E-16, -54.24999999999999289, -5.000000000000000000 ) ) ;
#24924 = CARTESIAN_POINT ( 'NONE',  ( -2.229367062499996610, 11.85416666803225993, 3.861377020970582219 ) ) ;
#24925 = CARTESIAN_POINT ( 'NONE',  ( -5.000000000000000000, -9.958333330602144429, -2.886751345948128211 ) ) ;
#24926 = ORIENTED_EDGE ( 'NONE', *, *, #51902, .F. ) ;
#24927 = CARTESIAN_POINT ( 'NONE',  ( 2.229367062499998831, 28.35416666803225993, -3.861377020970580887 ) ) ;
#24928 = CARTESIAN_POINT ( 'NONE',  ( -60.14911071818854538, -124.1875000027312410, 1.666127454062681368 ) ) ;
#24929 = CYLINDRICAL_SURFACE ( 'NONE', #793, 5.000000000000000000 ) ;
#24930 = CARTESIAN_POINT ( 'NONE',  ( -50.75781946612335105, -135.0000000000005969, -1.372666862511563224 ) ) ;
#24931 = LINE ( 'NONE', #44216, #36375 ) ;
#24932 = CARTESIAN_POINT ( 'NONE',  ( 2.229367062499998831, -65.64583333196773651, -3.861377020970580887 ) ) ;
#24933 = CARTESIAN_POINT ( 'NONE',  ( -51.75738570946856498, -145.7500000000000284, 3.805975901505576964 ) ) ;
#24934 = CARTESIAN_POINT ( 'NONE',  ( -2.229367062500000163, 19.52083333469893134, -3.861377020970580443 ) ) ;
#24935 =( BOUNDED_CURVE ( )  B_SPLINE_CURVE ( 2, ( #30047, #24918, #484, #25234, #44845, #808, #20415, #13989, #23962 ),
 .UNSPECIFIED., .F., .F. ) 
 B_SPLINE_CURVE_WITH_KNOTS ( ( 3, 2, 2, 2, 3 ),
 ( 0.9437499999999999778, 0.9444444444444444198, 0.9458333333333333037, 0.9472222222222221877, 0.9479166666666666297 ),
 .UNSPECIFIED. ) 
 CURVE ( )  GEOMETRIC_REPRESENTATION_ITEM ( )  RATIONAL_B_SPLINE_CURVE ( ( 0.9330127018922194093, 0.9330127018922194093, 1.000000000000000000, 0.8660254037844387076, 1.000000000000000000, 0.8660254037844387076, 1.000000000000000000, 0.9330127018922194093, 0.9330127018922194093 ) ) 
 REPRESENTATION_ITEM ( '' )  );
#24936 = CARTESIAN_POINT ( 'NONE',  ( 2.499999999999998668, -33.33333333333332860, -4.330127018922193649 ) ) ;
#24937 = EDGE_CURVE ( 'NONE', #4579, #18873, #62729, .T. ) ;
#24938 = CARTESIAN_POINT ( 'NONE',  ( -4.458734124999998549, -47.47916666530106511, 2.574251347313722516 ) ) ;
#24939 = CARTESIAN_POINT ( 'NONE',  ( 5.000000000000000000, -11.29166666393547835, -2.886751345948129988 ) ) ;
#24940 = CARTESIAN_POINT ( 'NONE',  ( 1.975475456537005874E-15, -25.62499999726881228, 5.000000000000000000 ) ) ;
#24941 = CARTESIAN_POINT ( 'NONE',  ( -5.000000000000000000, -65.87499999726881583, 0.000000000000000000 ) ) ;
#24942 = CARTESIAN_POINT ( 'NONE',  ( 0.000000000000000000, -170.0000000000000000, 0.000000000000000000 ) ) ;
#24943 = CARTESIAN_POINT ( 'NONE',  ( 4.458734125000000326, -108.8958333319677365, 2.574251347313718519 ) ) ;
#24944 = CARTESIAN_POINT ( 'NONE',  ( 4.458734124999999437, -15.06249999863440436, -5.460374474430324690E-16 ) ) ;
#24945 = ORIENTED_EDGE ( 'NONE', *, *, #37160, .T. ) ;
#24946 = CARTESIAN_POINT ( 'NONE',  ( 2.499999999999998668, -31.33333333333333215, -4.330127018922193649 ) ) ;
#24947 = CARTESIAN_POINT ( 'NONE',  ( 4.458734124999999437, -103.8124999986344079, -5.460374474430324690E-16 ) ) ;
#24948 = CARTESIAN_POINT ( 'NONE',  ( -3.535533905932738641, -160.5000000027312126, 3.535533905932737309 ) ) ;
#24949 = CARTESIAN_POINT ( 'NONE',  ( -4.458734124999998549, -97.47916666530106511, 2.574251347313722516 ) ) ;
#24950 = CARTESIAN_POINT ( 'NONE',  ( 10.12668159690567649, 0.000000000000000000, -9.999999999999998224 ) ) ;
#24951 = CARTESIAN_POINT ( 'NONE',  ( 5.000000000000000000, -57.29166666393548013, -2.886751345948129988 ) ) ;
#24952 = CARTESIAN_POINT ( 'NONE',  ( -2.499999999999996447, -66.83333333333332860, 4.330127018922195425 ) ) ;
#24953 = CARTESIAN_POINT ( 'NONE',  ( -52.10840900171896806, -154.4375000013656063, 3.393966926194110556 ) ) ;
#24954 =( BOUNDED_CURVE ( )  B_SPLINE_CURVE ( 2, ( #9744, #20369, #59284, #435, #29682, #20041, #39646, #15215, #54465 ),
 .UNSPECIFIED., .F., .F. ) 
 B_SPLINE_CURVE_WITH_KNOTS ( ( 3, 2, 2, 2, 3 ),
 ( 0.3229166666666666852, 0.3236111111111111271, 0.3250000000000000111, 0.3263888888888888951, 0.3270833333333333370 ),
 .UNSPECIFIED. ) 
 CURVE ( )  GEOMETRIC_REPRESENTATION_ITEM ( )  RATIONAL_B_SPLINE_CURVE ( ( 0.9330127018922194093, 0.9330127018922194093, 1.000000000000000000, 0.8660254037844387076, 1.000000000000000000, 0.8660254037844387076, 1.000000000000000000, 0.9330127018922194093, 0.9330127018922194093 ) ) 
 REPRESENTATION_ITEM ( '' )  );
#24955 = CARTESIAN_POINT ( 'NONE',  ( -58.39396692619412477, -147.4375000013656063, 2.891590998281057701 ) ) ;
#24956 = CARTESIAN_POINT ( 'NONE',  ( 9.457646018065525792E-16, -20.06249999863440081, 5.148502694627439702 ) ) ;
#24957 = CARTESIAN_POINT ( 'NONE',  ( -4.458734124999998549, 5.520833334698927786, 2.574251347313722516 ) ) ;
#24958 = CARTESIAN_POINT ( 'NONE',  ( -3.152548672688508926E-16, -66.81249999863440792, -5.148502694627439702 ) ) ;
#24959 = CARTESIAN_POINT ( 'NONE',  ( 3.061616997868383141E-16, -141.8750000027312126, -5.000000000000000000 ) ) ;
#24960 = CARTESIAN_POINT ( 'NONE',  ( 9.457646018065525792E-16, -20.06249999863440081, 5.148502694627439702 ) ) ;
#24961 = CARTESIAN_POINT ( 'NONE',  ( -2.499999999999996447, -79.70833333060213022, 4.330127018922195425 ) ) ;
#24962 = CARTESIAN_POINT ( 'NONE',  ( 2.071067811865475505, -155.8125000000000284, -5.000000000000000888 ) ) ;
#24963 = CARTESIAN_POINT ( 'NONE',  ( 5.000000000000000000, -6.416666666666666963, -2.886751345948129988 ) ) ;
#24964 = ORIENTED_EDGE ( 'NONE', *, *, #12119, .F. ) ;
#24965 = CARTESIAN_POINT ( 'NONE',  ( -3.152548672688508926E-16, -47.81249999863440792, -5.148502694627439702 ) ) ;
#24966 = CARTESIAN_POINT ( 'NONE',  ( -6.972266317189433020E-16, -50.24999999999999289, -5.000000000000000000 ) ) ;
#24967 = CARTESIAN_POINT ( 'NONE',  ( 1.975475456537005874E-15, -11.74999999999999645, 5.000000000000000000 ) ) ;
#24968 = CARTESIAN_POINT ( 'NONE',  ( 2.500000000000002220, 28.33333333333333215, 4.330127018922192761 ) ) ;
#24969 = CARTESIAN_POINT ( 'NONE',  ( 9.457646018065525792E-16, -90.06249999863440792, 5.148502694627439702 ) ) ;
#24970 = CARTESIAN_POINT ( 'NONE',  ( -4.458734124999999437, 16.35416666803225993, -2.574251347313719407 ) ) ;
#24971 = CARTESIAN_POINT ( 'NONE',  ( -3.152548672688508926E-16, 7.437500001365594748, -5.148502694627439702 ) ) ;
#24972 = CARTESIAN_POINT ( 'NONE',  ( 5.000000000000000000, -93.50000000000000000, -6.123233995736766282E-16 ) ) ;
#24973 = CARTESIAN_POINT ( 'NONE',  ( 1.975475456537005874E-15, 12.24999999999999822, 5.000000000000000000 ) ) ;
#24974 = DIRECTION ( 'NONE',  ( -0.000000000000000000, 1.000000000000000000, -0.000000000000000000 ) ) ;
#24975 = CARTESIAN_POINT ( 'NONE',  ( -3.152548672688508926E-16, 19.18750000136559208, -5.148502694627439702 ) ) ;
#24976 = CARTESIAN_POINT ( 'NONE',  ( -4.999999999999999112, -76.91666666666667140, 2.886751345948131764 ) ) ;
#24977 = CARTESIAN_POINT ( 'NONE',  ( 5.000000000000000000, 7.708333336064517205, -2.886751345948129988 ) ) ;
#24978 = VERTEX_POINT ( 'NONE', #32826 ) ;
#24979 = DIRECTION ( 'NONE',  ( 0.000000000000000000, 0.000000000000000000, 1.000000000000000000 ) ) ;
#24980 = ORIENTED_EDGE ( 'NONE', *, *, #53080, .T. ) ;
#24981 = PLANE ( 'NONE',  #15191 ) ;
#24982 = CARTESIAN_POINT ( 'NONE',  ( -2.229367062500000163, -37.47916666530107221, -3.861377020970580443 ) ) ;
#24983 = CARTESIAN_POINT ( 'NONE',  ( 1.060575238724906964E-15, -40.62499999726880162, 5.773502691896257311 ) ) ;
#24984 = ORIENTED_EDGE ( 'NONE', *, *, #55822, .T. ) ;
#24985 = CARTESIAN_POINT ( 'NONE',  ( -50.40829686548195099, -147.2500000013656063, -1.485763867205728284 ) ) ;
#24986 = CARTESIAN_POINT ( 'NONE',  ( 4.458734124999998549, -11.72916666530107044, -2.574251347313721627 ) ) ;
#24988 = ORIENTED_EDGE ( 'NONE', *, *, #43639, .T. ) ;
#24987 = CARTESIAN_POINT ( 'NONE',  ( 2.229367062499998831, -11.89583333196774007, -3.861377020970580887 ) ) ;
#24989 = CARTESIAN_POINT ( 'NONE',  ( 5.000000000000000000, -82.41666666666665719, -2.886751345948129988 ) ) ;
#24990 = CARTESIAN_POINT ( 'NONE',  ( -1.846868145590734756, -168.1250000013656063, -4.458734125000000326 ) ) ;
#24991 = CARTESIAN_POINT ( 'NONE',  ( -2.229367062500000163, -61.72916666530106511, -3.861377020970580443 ) ) ;
#24992 = CARTESIAN_POINT ( 'NONE',  ( 2.500000000000002220, -80.54166666393547303, 4.330127018922192761 ) ) ;
#24993 = VERTEX_POINT ( 'NONE', #22870 ) ;
#24994 = CARTESIAN_POINT ( 'NONE',  ( -51.75738570946856498, -143.7500000000000284, 3.805975901505576964 ) ) ;
#24995 = CARTESIAN_POINT ( 'NONE',  ( 4.458734124999999437, -26.06249999863440792, -5.460374474430324690E-16 ) ) ;
#24996 = CARTESIAN_POINT ( 'NONE',  ( -58.24261429053147765, -155.0000000000000284, -3.805975901505573411 ) ) ;
#24997 = ORIENTED_EDGE ( 'NONE', *, *, #27165, .T. ) ;
#24998 = CARTESIAN_POINT ( 'NONE',  ( 4.458734124999999437, -164.7500000013656063, 1.846868145590737864 ) ) ;
#24999 = CARTESIAN_POINT ( 'NONE',  ( 2.229367062500001939, -103.2291666653010651, 3.861377020970579999 ) ) ;
#25000 = VERTEX_POINT ( 'NONE', #52455 ) ;
#25001 = CARTESIAN_POINT ( 'NONE',  ( -52.80376928212989185, -146.1250000013656063, -4.297418129356378458 ) ) ;
#25002 = CARTESIAN_POINT ( 'NONE',  ( 4.458734124999999437, -74.06249999863440792, -5.460374474430324690E-16 ) ) ;
#25003 = CARTESIAN_POINT ( 'NONE',  ( -53.33387254593733928, -135.9375000027311842, 5.149110718188519620 ) ) ;
#25004 = CARTESIAN_POINT ( 'NONE',  ( 4.458734124999999437, -44.81249999863440081, -5.460374474430324690E-16 ) ) ;
#25005 = CARTESIAN_POINT ( 'NONE',  ( -4.458734125000000326, -146.1250000013655779, 1.846868145590734089 ) ) ;
#25006 =( BOUNDED_CURVE ( )  B_SPLINE_CURVE ( 2, ( #48199, #57868, #13789, #62067, #4153, #52718, #37605, #8968, #12846 ),
 .UNSPECIFIED., .F., .F. ) 
 B_SPLINE_CURVE_WITH_KNOTS ( ( 3, 2, 2, 2, 3 ),
 ( 0.3604166666666666630, 0.3611111111111111049, 0.3624999999999999889, 0.3638888888888888729, 0.3645833333333333148 ),
 .UNSPECIFIED. ) 
 CURVE ( )  GEOMETRIC_REPRESENTATION_ITEM ( )  RATIONAL_B_SPLINE_CURVE ( ( 0.9330127018922194093, 0.9330127018922194093, 1.000000000000000000, 0.8660254037844387076, 1.000000000000000000, 0.8660254037844387076, 1.000000000000000000, 0.9330127018922194093, 0.9330127018922194093 ) ) 
 REPRESENTATION_ITEM ( '' )  );
#25007 = CARTESIAN_POINT ( 'NONE',  ( -7.500000000000000000, -0.7729939684941458111, -7.026407045654831762 ) ) ;
#25008 = CARTESIAN_POINT ( 'NONE',  ( -2.229367062499996610, -47.14583333196774362, 3.861377020970582219 ) ) ;
#25009 = CARTESIAN_POINT ( 'NONE',  ( -4.999999999999998224, 28.08333333333332860, 2.886751345948131764 ) ) ;
#25010 = CARTESIAN_POINT ( 'NONE',  ( -4.458734124999999437, -11.31249999863440792, 0.000000000000000000 ) ) ;
#25011 = CARTESIAN_POINT ( 'NONE',  ( 5.000000000000000000, -103.4166666666666430, -2.886751345948129988 ) ) ;
#25012 = CARTESIAN_POINT ( 'NONE',  ( -1.846868145590734756, -140.3750000013656063, -4.458734125000000326 ) ) ;
#25013 = CARTESIAN_POINT ( 'NONE',  ( -2.229367062499996610, -34.39583333196772941, 3.861377020970582219 ) ) ;
#25014 = CARTESIAN_POINT ( 'NONE',  ( 5.000000000000000000, 4.708333336064518093, -2.886751345948129988 ) ) ;
#25015 = CARTESIAN_POINT ( 'NONE',  ( -4.729367062499999719, 29.84375000068279604, 0.000000000000000000 ) ) ;
#25016 = CARTESIAN_POINT ( 'NONE',  ( -57.89159099828107458, -133.6875000013656063, -3.393966926194107447 ) ) ;
#25017 = CARTESIAN_POINT ( 'NONE',  ( -2.229367062500000163, -74.72916666530106511, -3.861377020970580443 ) ) ;
#25018 = CARTESIAN_POINT ( 'NONE',  ( -2.071067811865391128, -144.8125000027312410, -5.000000000000086153 ) ) ;
#25019 = CARTESIAN_POINT ( 'NONE',  ( -52.53715891517739323, -146.5625000027311842, -4.819101127000233298 ) ) ;
#25020 = CARTESIAN_POINT ( 'NONE',  ( 1.339745962155612702, -30.16965819600732956, -5.000000000000000000 ) ) ;
#25021 = CARTESIAN_POINT ( 'NONE',  ( 2.229367062500001939, 0.7708333346989268975, 3.861377020970579999 ) ) ;
#25022 = VERTEX_POINT ( 'NONE', #2615 ) ;
#25023 = CARTESIAN_POINT ( 'NONE',  ( 5.000000000000000888, -15.58333333333332860, 2.886751345948126879 ) ) ;
#25025 = CARTESIAN_POINT ( 'NONE',  ( -3.152548672688508926E-16, -36.56249999863441502, -5.148502694627439702 ) ) ;
#25024 = CARTESIAN_POINT ( 'NONE',  ( -4.999999999999999112, -94.91666666666667140, 2.886751345948131764 ) ) ;
#25026 = CARTESIAN_POINT ( 'NONE',  ( 2.499999999999998668, -95.33333333333332860, -4.330127018922193649 ) ) ;
#25027 = CARTESIAN_POINT ( 'NONE',  ( 4.458734124999999437, -82.06249999863440792, -5.460374474430324690E-16 ) ) ;
#25028 = CARTESIAN_POINT ( 'NONE',  ( -2.229367062500000163, 16.27083333469892779, -3.861377020970580443 ) ) ;
#25029 = CYLINDRICAL_SURFACE ( 'NONE', #53077, 5.000000000000000000 ) ;
#25030 = AXIS2_PLACEMENT_3D ( 'NONE', #48882, #4827, #21860 ) ;
#25031 = CARTESIAN_POINT ( 'NONE',  ( -57.19623071787017210, -137.3750000013656063, 4.297418129356382899 ) ) ;
#25032 = CARTESIAN_POINT ( 'NONE',  ( -4.458734124999999437, -3.312499998634407916, 0.000000000000000000 ) ) ;
#25033 = CARTESIAN_POINT ( 'NONE',  ( 4.458734124999998549, 23.02083333469892423, -2.574251347313721627 ) ) ;
#25034 = CARTESIAN_POINT ( 'NONE',  ( -2.229367062499996610, -41.39583333196773651, 3.861377020970582219 ) ) ;
#25035 = CARTESIAN_POINT ( 'NONE',  ( -2.229367062499996610, -3.145833331967738733, 3.861377020970582219 ) ) ;
#25036 = CARTESIAN_POINT ( 'NONE',  ( -2.229367062499996610, -28.39583333196774007, 3.861377020970582219 ) ) ;
#25037 = SHAPE_REPRESENTATION ( 'pulling arm', ( #43054 ), #38957 ) ;
#25038 = CARTESIAN_POINT ( 'NONE',  ( -4.458734124999999437, -75.31249999863440792, 0.000000000000000000 ) ) ;
#25039 = CARTESIAN_POINT ( 'NONE',  ( -5.000000000000000000, -105.8749999972688158, 0.000000000000000000 ) ) ;
#25040 = EDGE_CURVE ( 'NONE', #20951, #24591, #25722, .T. ) ;
#25041 = CARTESIAN_POINT ( 'NONE',  ( -4.458734124999998549, 27.77083333469892423, 2.574251347313722516 ) ) ;
#25042 = CARTESIAN_POINT ( 'NONE',  ( -6.972266317189433020E-16, 26.87500000273118417, -5.000000000000000000 ) ) ;
#25043 = CARTESIAN_POINT ( 'NONE',  ( 4.458734124999998549, -109.9791666653010509, -2.574251347313721627 ) ) ;
#25044 = CARTESIAN_POINT ( 'NONE',  ( 2.229367062499998831, -70.89583333196773651, -3.861377020970580887 ) ) ;
#25045 = CARTESIAN_POINT ( 'NONE',  ( 5.000000000000000888, -60.58333333333332860, 2.886751345948126879 ) ) ;
#25046 = CARTESIAN_POINT ( 'NONE',  ( 1.339745962155615144, -36.58034179853029855, 4.999999999999999112 ) ) ;
#25047 = CARTESIAN_POINT ( 'NONE',  ( 1.060575238724906964E-15, 23.37500000273118062, 5.773502691896257311 ) ) ;
#25048 = ORIENTED_EDGE ( 'NONE', *, *, #62274, .F. ) ;
#25049 = DIRECTION ( 'NONE',  ( -0.000000000000000000, 1.000000000000000000, -0.000000000000000000 ) ) ;
#25050 = CARTESIAN_POINT ( 'NONE',  ( 3.061616997868383141E-16, -162.8750000027311842, -5.000000000000000000 ) ) ;
#25051 =( BOUNDED_CURVE ( )  B_SPLINE_CURVE ( 2, ( #49299, #44782, #53799, #9733, #29337, #19065, #63470, #39316, #13933 ),
 .UNSPECIFIED., .F., .F. ) 
 B_SPLINE_CURVE_WITH_KNOTS ( ( 3, 2, 2, 2, 3 ),
 ( 0.6729166666666667185, 0.6736111111111111605, 0.6750000000000000444, 0.6763888888888889284, 0.6770833333333333703 ),
 .UNSPECIFIED. ) 
 CURVE ( )  GEOMETRIC_REPRESENTATION_ITEM ( )  RATIONAL_B_SPLINE_CURVE ( ( 0.9330127018922194093, 0.9330127018922194093, 1.000000000000000000, 0.8660254037844387076, 1.000000000000000000, 0.8660254037844387076, 1.000000000000000000, 0.9330127018922194093, 0.9330127018922194093 ) ) 
 REPRESENTATION_ITEM ( '' )  );
#25052 = CARTESIAN_POINT ( 'NONE',  ( -5.000000000000000000, -16.08333333333333215, -2.886751345948128211 ) ) ;
#25053 = CARTESIAN_POINT ( 'NONE',  ( -3.152548672688508926E-16, -23.56249999863440436, -5.148502694627439702 ) ) ;
#25054 = B_SPLINE_CURVE_WITH_KNOTS ( 'NONE', 3,
 ( #51273, #32908, #52531, #46437, #32586, #16841 ),
 .UNSPECIFIED., .F., .F.,
 ( 4, 2, 4 ),
 ( 0.000000000000000000, 0.0004189869898913735043, 0.0008379739797827470086 ),
 .UNSPECIFIED. ) ;
#25055 = CARTESIAN_POINT ( 'NONE',  ( -4.458734124999999437, -82.31249999863440792, 0.000000000000000000 ) ) ;
#25056 = CARTESIAN_POINT ( 'NONE',  ( -2.499999999999996447, -23.70833333060214443, 4.330127018922195425 ) ) ;
#25058 = ORIENTED_EDGE ( 'NONE', *, *, #38230, .T. ) ;
#25057 = CARTESIAN_POINT ( 'NONE',  ( -4.458734124999999437, -51.39583333196772941, -2.574251347313719407 ) ) ;
#25059 = CARTESIAN_POINT ( 'NONE',  ( 2.500000000000002220, -35.54166666393547303, 4.330127018922192761 ) ) ;
#25060 = DIRECTION ( 'NONE',  ( 0.000000000000000000, 1.000000000000000000, 0.000000000000000000 ) ) ;
#25062 = ORIENTED_EDGE ( 'NONE', *, *, #542, .T. ) ;
#25061 = CARTESIAN_POINT ( 'NONE',  ( 2.229367062500001939, -0.2291666653010705768, 3.861377020970579999 ) ) ;
#25063 = CARTESIAN_POINT ( 'NONE',  ( -54.64476657466781973, -148.8125000013656063, -4.444560631937228834 ) ) ;
#25064 = CARTESIAN_POINT ( 'NONE',  ( 2.499999999999998668, -68.33333333333332860, -4.330127018922193649 ) ) ;
#25065 = CARTESIAN_POINT ( 'NONE',  ( 1.846868145590736310, -150.8750000013655779, 4.458734124999999437 ) ) ;
#25066 = CARTESIAN_POINT ( 'NONE',  ( -4.458734124999999437, -41.56249999863440081, 0.000000000000000000 ) ) ;
#25067 = CARTESIAN_POINT ( 'NONE',  ( -2.499999999999996447, -80.70833333060213022, 4.330127018922195425 ) ) ;
#25068 = CARTESIAN_POINT ( 'NONE',  ( 5.000000000000000888, -163.9375000000000000, -2.071067811865475505 ) ) ;
#25069 = CARTESIAN_POINT ( 'NONE',  ( -5.000000000000000000, 7.125000002731185944, 0.000000000000000000 ) ) ;
#25070 = CARTESIAN_POINT ( 'NONE',  ( -52.10840900171896806, -126.4375000013656063, 3.393966926194110556 ) ) ;
#25071 = CARTESIAN_POINT ( 'NONE',  ( -4.458734124999998549, -10.47916666530107044, 2.574251347313722516 ) ) ;
#25072 = CARTESIAN_POINT ( 'NONE',  ( 4.458734125000001214, -44.14583333196773651, 2.574251347313718519 ) ) ;
#25073 = CARTESIAN_POINT ( 'NONE',  ( 5.000000000000000888, -151.0625000027311842, -2.071067811865475505 ) ) ;
#25074 = CARTESIAN_POINT ( 'NONE',  ( -1.846868145590737420, -145.7500000013655779, 4.458734124999999437 ) ) ;
#25075 = CARTESIAN_POINT ( 'NONE',  ( -4.458734124999999437, -88.56249999863439371, 0.000000000000000000 ) ) ;
#25076 = CARTESIAN_POINT ( 'NONE',  ( 6.123233995736766282E-16, -120.0000000000000000, -5.000000000000000000 ) ) ;
#25077 = ORIENTED_EDGE ( 'NONE', *, *, #59398, .F. ) ;
#25078 = CARTESIAN_POINT ( 'NONE',  ( 6.123233995736766282E-16, -170.0000000000000000, -5.000000000000000000 ) ) ;
#25079 = CARTESIAN_POINT ( 'NONE',  ( -2.500000000000000444, -6.041666663935481019, -4.330127018922193649 ) ) ;
#25080 = PRODUCT_DEFINITION_SHAPE ( 'NONE', 'NONE',  #63683 ) ;
#25081 = CARTESIAN_POINT ( 'NONE',  ( -51.75738570946856498, -150.8750000027312126, 3.805975901505576964 ) ) ;
#25082 = CARTESIAN_POINT ( 'NONE',  ( 1.975475456537005874E-15, -65.74999999999998579, 5.000000000000000000 ) ) ;
#25083 = ORIENTED_EDGE ( 'NONE', *, *, #826, .F. ) ;
#25084 = CARTESIAN_POINT ( 'NONE',  ( 9.457646018065525792E-16, 2.937500001365594304, 5.148502694627439702 ) ) ;
#25085 = CARTESIAN_POINT ( 'NONE',  ( 2.499999999999998668, 6.666666666666667851, -4.330127018922193649 ) ) ;
#25086 = CARTESIAN_POINT ( 'NONE',  ( -2.229367062499996610, -19.39583333196774007, 3.861377020970582219 ) ) ;
#25087 = CARTESIAN_POINT ( 'NONE',  ( 1.975475456537005874E-15, -100.7499999999999858, 5.000000000000000000 ) ) ;
#25088 = CARTESIAN_POINT ( 'NONE',  ( -2.229367062499996610, -5.145833331967740065, 3.861377020970582219 ) ) ;
#25089 = CARTESIAN_POINT ( 'NONE',  ( 3.061616997868383141E-16, -145.8750000027312126, -5.000000000000000000 ) ) ;
#25090 = CARTESIAN_POINT ( 'NONE',  ( -4.458734125000000326, -147.8750000013655779, 1.846868145590734089 ) ) ;
#25091 = CARTESIAN_POINT ( 'NONE',  ( 9.457646018065525792E-16, 19.68750000136559208, 5.148502694627439702 ) ) ;
#25092 = ORIENTED_EDGE ( 'NONE', *, *, #38859, .F. ) ;
#25093 = CARTESIAN_POINT ( 'NONE',  ( -2.229367062499996610, -97.14583333196773651, 3.861377020970582219 ) ) ;
#25094 = CARTESIAN_POINT ( 'NONE',  ( -2.499999999999996447, -18.70833333060214798, 4.330127018922195425 ) ) ;
#25095 = CARTESIAN_POINT ( 'NONE',  ( 2.500000000000002220, -57.54166666393548013, 4.330127018922192761 ) ) ;
#25096 = CARTESIAN_POINT ( 'NONE',  ( 4.458734125000001214, -14.89583333196773474, 2.574251347313718519 ) ) ;
#25097 = CARTESIAN_POINT ( 'NONE',  ( -6.972266317189433020E-16, -25.12499999726881228, -5.000000000000000000 ) ) ;
#25098 = CARTESIAN_POINT ( 'NONE',  ( -2.480964764533239819E-13, -72.75000000000000000, 5.000000000000000000 ) ) ;
#25099 = CARTESIAN_POINT ( 'NONE',  ( -51.60603307380591787, -150.9375000013656063, -2.891590998281053704 ) ) ;
#25100 = CARTESIAN_POINT ( 'NONE',  ( -4.999999999999999112, -41.79166666393548013, 2.886751345948131764 ) ) ;
#25101 = CARTESIAN_POINT ( 'NONE',  ( -2.500000000000000444, 20.95833333606451987, -4.330127018922193649 ) ) ;
#25102 = CARTESIAN_POINT ( 'NONE',  ( 9.457646018065525792E-16, 13.93750000136559564, 5.148502694627439702 ) ) ;
#25103 = CARTESIAN_POINT ( 'NONE',  ( -1.339745962155610925, -89.66965819600733312, 5.000000000000000000 ) ) ;
#25104 = CARTESIAN_POINT ( 'NONE',  ( -1.339745962155610925, -47.66965819600734022, 5.000000000000000000 ) ) ;
#25105 = CARTESIAN_POINT ( 'NONE',  ( 4.458734125000000326, 20.10416666803225638, 2.574251347313718519 ) ) ;
#25106 = CARTESIAN_POINT ( 'NONE',  ( -4.458734124999999437, -60.39583333196773651, -2.574251347313719407 ) ) ;
#25107 = ORIENTED_EDGE ( 'NONE', *, *, #36970, .T. ) ;
#25108 = CARTESIAN_POINT ( 'NONE',  ( 4.458734124999999437, -11.06249999863440792, -5.460374474430324690E-16 ) ) ;
#25109 = CARTESIAN_POINT ( 'NONE',  ( 1.060575238724906964E-15, 6.249999999999998224, 5.773502691896257311 ) ) ;
#25110 = CARTESIAN_POINT ( 'NONE',  ( -1.846868145590734756, -164.1250000013656063, -4.458734125000000326 ) ) ;
#25111 = CARTESIAN_POINT ( 'NONE',  ( -3.152548672688508926E-16, -51.56249999863441502, -5.148502694627439702 ) ) ;
#25112 = CARTESIAN_POINT ( 'NONE',  ( -4.999999999999999112, -91.79166666393547303, 2.886751345948131764 ) ) ;
#25113 = EDGE_CURVE ( 'NONE', #18601, #12246, #42987, .T. ) ;
#25114 = CARTESIAN_POINT ( 'NONE',  ( 4.458734124999999437, -33.81249999863440792, -5.460374474430324690E-16 ) ) ;
#25115 = DIRECTION ( 'NONE',  ( -0.000000000000000000, 1.000000000000000000, -0.000000000000000000 ) ) ;
#25116 = CARTESIAN_POINT ( 'NONE',  ( 2.499999999999998668, 25.79166666939785202, -4.330127018922193649 ) ) ;
#25117 = CARTESIAN_POINT ( 'NONE',  ( -1.339745962155610925, -88.66965819600733312, 5.000000000000000000 ) ) ;
#25118 = CARTESIAN_POINT ( 'NONE',  ( 1.846868145590736310, -152.8750000013655779, 4.458734124999997661 ) ) ;
#25119 = CARTESIAN_POINT ( 'NONE',  ( 5.000000000000000888, -42.58333333333334281, 2.886751345948126879 ) ) ;
#25120 = CARTESIAN_POINT ( 'NONE',  ( 5.000000000000000000, -86.29166666393547303, -2.886751345948130876 ) ) ;
#25121 = EDGE_LOOP ( 'NONE', ( #42081, #9782, #46831, #56822 ) ) ;
#25122 = CARTESIAN_POINT ( 'NONE',  ( 2.229367062500001939, -98.97916666530105090, 3.861377020970579999 ) ) ;
#25123 = CARTESIAN_POINT ( 'NONE',  ( 2.229367062499998831, 1.104166668032261711, -3.861377020970580887 ) ) ;
#25124 = CARTESIAN_POINT ( 'NONE',  ( 1.975475456537005874E-15, -79.74999999999998579, 5.000000000000000000 ) ) ;
#25125 = CARTESIAN_POINT ( 'NONE',  ( 2.500000000000002220, -4.666666666666666075, 4.330127018922192761 ) ) ;
#25126 = EDGE_CURVE ( 'NONE', #27450, #23493, #19501, .T. ) ;
#25127 = CARTESIAN_POINT ( 'NONE',  ( -4.458734124999997661, -67.22916666530106511, 2.574251347313722516 ) ) ;
#25128 =( BOUNDED_CURVE ( )  B_SPLINE_CURVE ( 2, ( #20612, #39885, #49229, #40217, #59853, #15777, #35394, #55016, #10308 ),
 .UNSPECIFIED., .F., .F. ) 
 B_SPLINE_CURVE_WITH_KNOTS ( ( 3, 2, 2, 2, 3 ),
 ( 0.8687500000000000222, 0.8694444444444444642, 0.8708333333333333481, 0.8722222222222222321, 0.8729166666666666741 ),
 .UNSPECIFIED. ) 
 CURVE ( )  GEOMETRIC_REPRESENTATION_ITEM ( )  RATIONAL_B_SPLINE_CURVE ( ( 0.9330127018922194093, 0.9330127018922194093, 1.000000000000000000, 0.8660254037844387076, 1.000000000000000000, 0.8660254037844387076, 1.000000000000000000, 0.9330127018922194093, 0.9330127018922194093 ) ) 
 REPRESENTATION_ITEM ( '' )  );
#25129 = CARTESIAN_POINT ( 'NONE',  ( -1.339745962155613812, 2.794658198738520394, -5.000000000000000000 ) ) ;
#25130 = CARTESIAN_POINT ( 'NONE',  ( 2.499999999999998668, -4.208333330602147981, -4.330127018922193649 ) ) ;
#25132 = ORIENTED_EDGE ( 'NONE', *, *, #1728, .F. ) ;
#25131 = CARTESIAN_POINT ( 'NONE',  ( -2.229367062500000163, -36.47916666530107221, -3.861377020970580443 ) ) ;
#25133 = CARTESIAN_POINT ( 'NONE',  ( -1.339745962155613812, -78.20534180126146850, -5.000000000000000000 ) ) ;
#25134 = CARTESIAN_POINT ( 'NONE',  ( 3.535533905932738197, -156.8750000000000284, -3.535533905932738197 ) ) ;
#25135 = ADVANCED_FACE ( 'NONE', ( #19599 ), #48233, .F. ) ;
#25136 = ORIENTED_EDGE ( 'NONE', *, *, #54792, .F. ) ;
#25137 = DIRECTION ( 'NONE',  ( -0.000000000000000000, 1.000000000000000000, -0.000000000000000000 ) ) ;
#25138 = CARTESIAN_POINT ( 'NONE',  ( -3.535250795749689387E-16, -49.25000000000000000, -5.773502691896257311 ) ) ;
#25140 = CARTESIAN_POINT ( 'NONE',  ( -4.458734124999999437, -25.64583333196773651, -2.574251347313719407 ) ) ;
#25139 = CARTESIAN_POINT ( 'NONE',  ( 2.500000000000002220, -17.54166666393547658, 4.330127018922192761 ) ) ;
#25141 = CARTESIAN_POINT ( 'NONE',  ( 5.000000000000000000, -32.29166666393548724, -2.886751345948130876 ) ) ;
#25142 = CARTESIAN_POINT ( 'NONE',  ( -2.229367062499996610, -73.14583333196773651, 3.861377020970582219 ) ) ;
#25143 = CARTESIAN_POINT ( 'NONE',  ( 3.152801135295367541, -144.5625000013655779, -3.152801135295367541 ) ) ;
#25144 = CARTESIAN_POINT ( 'NONE',  ( -4.458734124999999437, -81.31249999863440792, 0.000000000000000000 ) ) ;
#25145 = CARTESIAN_POINT ( 'NONE',  ( -58.39396692619412477, -140.6875000013656063, 2.891590998281057701 ) ) ;
#25146 = CARTESIAN_POINT ( 'NONE',  ( 4.458734124999999437, -29.06249999863440436, -5.460374474430324690E-16 ) ) ;
#25147 = CARTESIAN_POINT ( 'NONE',  ( 5.000000000000000000, -73.37499999726880162, -6.123233995736766282E-16 ) ) ;
#25148 = ORIENTED_EDGE ( 'NONE', *, *, #1467, .T. ) ;
#25149 = DIRECTION ( 'NONE',  ( -0.000000000000000000, -1.000000000000000000, -0.000000000000000000 ) ) ;
#25150 = EDGE_LOOP ( 'NONE', ( #37320, #47336, #20797, #57902 ) ) ;
#25151 = CARTESIAN_POINT ( 'NONE',  ( 4.458734124999999437, -74.06249999863440792, -5.460374474430324690E-16 ) ) ;
#25152 = CARTESIAN_POINT ( 'NONE',  ( -52.70900849189143855, -134.9999999999999432, -3.836432292133860944 ) ) ;
#25153 = ORIENTED_EDGE ( 'NONE', *, *, #35914, .T. ) ;
#25154 = CARTESIAN_POINT ( 'NONE',  ( -1.339745962155610925, 17.20534180126147916, 5.000000000000000000 ) ) ;
#25155 = CARTESIAN_POINT ( 'NONE',  ( -55.39835681537999790, -143.0000000027312126, 4.984105922594378235 ) ) ;
#25156 = CARTESIAN_POINT ( 'NONE',  ( 4.458734125000001214, -58.14583333196773651, 2.574251347313718519 ) ) ;
#25157 = CARTESIAN_POINT ( 'NONE',  ( 4.458734125000001214, -6.145833331967741842, 2.574251347313718519 ) ) ;
#25158 = ORIENTED_EDGE ( 'NONE', *, *, #52295, .F. ) ;
#25159 = DIRECTION ( 'NONE',  ( 0.000000000000000000, 0.000000000000000000, 1.000000000000000000 ) ) ;
#25160 = CARTESIAN_POINT ( 'NONE',  ( 0.000000000000000000, -170.0000000000000000, 0.000000000000000000 ) ) ;
#25161 = CARTESIAN_POINT ( 'NONE',  ( 2.229367062499998831, 11.35416666803225993, -3.861377020970580887 ) ) ;
#25162 = CARTESIAN_POINT ( 'NONE',  ( -59.44456063193725015, -141.5625000013656063, -0.3552334253322034230 ) ) ;
#25163 = CARTESIAN_POINT ( 'NONE',  ( -5.000000000000000000, -1.083333333333331927, -2.886751345948128211 ) ) ;
#25164 = CARTESIAN_POINT ( 'NONE',  ( -8.190561711645485556E-16, -160.6875000013655779, 4.458734124999999437 ) ) ;
#25165 = DIRECTION ( 'NONE',  ( 0.000000000000000000, 0.000000000000000000, 1.000000000000000000 ) ) ;
#25166 = ORIENTED_EDGE ( 'NONE', *, *, #36910, .T. ) ;
#25167 = CARTESIAN_POINT ( 'NONE',  ( -4.458734124999997661, -80.22916666530107932, 2.574251347313722516 ) ) ;
#25168 = CARTESIAN_POINT ( 'NONE',  ( 6.123233995736766282E-16, -170.0000000000000000, -5.000000000000000000 ) ) ;
#25169 = CARTESIAN_POINT ( 'NONE',  ( -2.229367062499996610, -0.1458333319677394824, 3.861377020970582219 ) ) ;
#25170 = DIRECTION ( 'NONE',  ( 0.000000000000000000, 0.000000000000000000, 1.000000000000000000 ) ) ;
#25171 = CARTESIAN_POINT ( 'NONE',  ( -3.535250795749689387E-16, -85.24999999999998579, -5.773502691896257311 ) ) ;
#25172 = CARTESIAN_POINT ( 'NONE',  ( 1.339745962155612702, -36.29465819873852439, -5.000000000000000000 ) ) ;
#25173 = CARTESIAN_POINT ( 'NONE',  ( 4.458734125000001214, -67.14583333196773651, 2.574251347313718519 ) ) ;
#25174 = CARTESIAN_POINT ( 'NONE',  ( 5.000000000000000888, -25.45833333060214443, 2.886751345948126879 ) ) ;
#25175 = CARTESIAN_POINT ( 'NONE',  ( -2.500000000000000444, -21.16666666666666785, -4.330127018922193649 ) ) ;
#25176 = CARTESIAN_POINT ( 'NONE',  ( -5.000000000000000000, -0.9583333306021485365, -2.886751345948128211 ) ) ;
#25177 = CARTESIAN_POINT ( 'NONE',  ( -1.339745962155610925, -55.79465819873851729, 5.000000000000000000 ) ) ;
#25178 =( BOUNDED_CURVE ( )  B_SPLINE_CURVE ( 2, ( #9568, #53003, #4129, #43346, #47549, #62990, #18902, #3499, #13463 ),
 .UNSPECIFIED., .F., .F. ) 
 B_SPLINE_CURVE_WITH_KNOTS ( ( 3, 2, 2, 2, 3 ),
 ( 0.09791666666666666574, 0.09861111111111110772, 0.1000000000000000056, 0.1013888888888888895, 0.1020833333333333315 ),
 .UNSPECIFIED. ) 
 CURVE ( )  GEOMETRIC_REPRESENTATION_ITEM ( )  RATIONAL_B_SPLINE_CURVE ( ( 0.9330127018922194093, 0.9330127018922194093, 1.000000000000000000, 0.8660254037844387076, 1.000000000000000000, 0.8660254037844387076, 1.000000000000000000, 0.9330127018922194093, 0.9330127018922194093 ) ) 
 REPRESENTATION_ITEM ( '' )  );
#25179 = FILL_AREA_STYLE ('',( #15211 ) ) ;
#25180 = CARTESIAN_POINT ( 'NONE',  ( -3.152548672688508926E-16, -45.56249999863439371, -5.148502694627439702 ) ) ;
#25181 = CARTESIAN_POINT ( 'NONE',  ( 4.458734125000000326, -33.14583333196774362, 2.574251347313718519 ) ) ;
#25182 = CARTESIAN_POINT ( 'NONE',  ( 4.458734125000000326, 5.854166668032262599, 2.574251347313718519 ) ) ;
#25183 = CARTESIAN_POINT ( 'NONE',  ( 2.071067811865349828, -151.1875000000000000, 5.000000000000126121 ) ) ;
#25184 = CARTESIAN_POINT ( 'NONE',  ( 5.000000000000000888, 22.41666666666666785, 2.886751345948126879 ) ) ;
#25185 = CARTESIAN_POINT ( 'NONE',  ( 3.061616997868383141E-16, -150.8750000027312126, -5.000000000000000000 ) ) ;
#25186 = LINE ( 'NONE', #39332, #23334 ) ;
#25187 = CARTESIAN_POINT ( 'NONE',  ( -2.229367062500000163, -36.47916666530107221, -3.861377020970580443 ) ) ;
#25188 = CARTESIAN_POINT ( 'NONE',  ( 5.000000000000000888, -75.45833333060214443, 2.886751345948126879 ) ) ;
#25189 = CARTESIAN_POINT ( 'NONE',  ( -57.89159099828107458, -145.9375000013656063, -3.393966926194107447 ) ) ;
#25190 = CARTESIAN_POINT ( 'NONE',  ( -3.535533905932737309, -140.6250000000000000, -3.535533905932738197 ) ) ;
#25191 = EDGE_CURVE ( 'NONE', #24595, #35208, #12561, .T. ) ;
#25192 = CARTESIAN_POINT ( 'NONE',  ( -0.6249999999999991118, -8.299410119600880265, -7.298562697733108173 ) ) ;
#25193 = EDGE_CURVE ( 'NONE', #5493, #11807, #52404, .T. ) ;
#25194 = CARTESIAN_POINT ( 'NONE',  ( 4.458734124999998549, -82.97916666530106511, -2.574251347313721627 ) ) ;
#25195 = CARTESIAN_POINT ( 'NONE',  ( -1.846868145590734756, -167.3750000013656347, -4.458734124999999437 ) ) ;
#25196 = EDGE_CURVE ( 'NONE', #36723, #26676, #9243, .T. ) ;
#25197 = LINE ( 'NONE', #30659, #38885 ) ;
#25198 = CARTESIAN_POINT ( 'NONE',  ( 5.000000000000000888, 22.54166666939785202, 2.886751345948126879 ) ) ;
#25199 = CARTESIAN_POINT ( 'NONE',  ( -2.499999999999996447, -29.83333333333332860, 4.330127018922195425 ) ) ;
#25200 = CARTESIAN_POINT ( 'NONE',  ( 4.458734124999999437, -142.5000000013656347, 1.846868145590737864 ) ) ;
#25201 = VERTEX_POINT ( 'NONE', #34003 ) ;
#25202 = CARTESIAN_POINT ( 'NONE',  ( -4.458734124999999437, 27.35416666803225993, -2.574251347313719407 ) ) ;
#25203 = VERTEX_POINT ( 'NONE', #53309 ) ;
#25204 = CARTESIAN_POINT ( 'NONE',  ( -4.458734124999997661, -63.47916666530106511, 2.574251347313722516 ) ) ;
#25205 = CARTESIAN_POINT ( 'NONE',  ( -2.499999999999996447, 20.29166666939784847, 4.330127018922195425 ) ) ;
#25206 = LINE ( 'NONE', #22622, #4225 ) ;
#25207 = CARTESIAN_POINT ( 'NONE',  ( -2.500000000000000444, 11.83333333333333037, -4.330127018922193649 ) ) ;
#25208 = ADVANCED_FACE ( 'NONE', ( #37896 ), #19201, .T. ) ;
#25209 = CARTESIAN_POINT ( 'NONE',  ( -2.229367062499996610, -51.14583333196772941, 3.861377020970582219 ) ) ;
#25210 = AXIS2_PLACEMENT_3D ( 'NONE', #20903, #54025, #29892 ) ;
#25211 = CARTESIAN_POINT ( 'NONE',  ( 2.229367062500001939, -9.979166665301068662, 3.861377020970579999 ) ) ;
#25212 = DIRECTION ( 'NONE',  ( -0.000000000000000000, 1.000000000000000000, -0.000000000000000000 ) ) ;
#25213 = CARTESIAN_POINT ( 'NONE',  ( -1.339745962155613812, -64.08034179853029855, -5.000000000000000000 ) ) ;
#25214 = CARTESIAN_POINT ( 'NONE',  ( 5.047120108843200725, -5.746297884371399434, -0.1007566405101860824 ) ) ;
#25215 = EDGE_CURVE ( 'NONE', #34626, #12016, #58456, .T. ) ;
#25216 = CARTESIAN_POINT ( 'NONE',  ( 6.123233995736766282E-16, -120.0000000000000000, -5.000000000000000000 ) ) ;
#25217 = CARTESIAN_POINT ( 'NONE',  ( 1.339745962155612702, -66.16965819600733312, -5.000000000000000000 ) ) ;
#25219 = CARTESIAN_POINT ( 'NONE',  ( 4.458734124999998549, -23.72916666530107221, -2.574251347313721627 ) ) ;
#25218 = CARTESIAN_POINT ( 'NONE',  ( -51.75738570946856498, -150.7500000000000284, 3.805975901505576964 ) ) ;
#25220 = CARTESIAN_POINT ( 'NONE',  ( 5.000000000000000000, 17.62500000273118417, -6.123233995736766282E-16 ) ) ;
#25221 = CARTESIAN_POINT ( 'NONE',  ( 9.457646018065525792E-16, -53.06249999863441502, 5.148502694627439702 ) ) ;
#25222 = CARTESIAN_POINT ( 'NONE',  ( -1.846868145590734756, -157.3750000013656347, -4.458734125000000326 ) ) ;
#25223 = ADVANCED_FACE ( 'NONE', ( #24354 ), #48787, .T. ) ;
#25224 = CARTESIAN_POINT ( 'NONE',  ( -2.500000000000000444, -55.04166666393548013, -4.330127018922193649 ) ) ;
#25225 = ORIENTED_EDGE ( 'NONE', *, *, #39355, .F. ) ;
#25226 = CARTESIAN_POINT ( 'NONE',  ( -1.339745962155614700, 25.33034180399266333, 4.999999999999999112 ) ) ;
#25227 = CARTESIAN_POINT ( 'NONE',  ( -4.458734124999999437, 2.354166668032262599, -2.574251347313719407 ) ) ;
#25228 = ORIENTED_EDGE ( 'NONE', *, *, #20223, .T. ) ;
#25230 = DIRECTION ( 'NONE',  ( 0.000000000000000000, 0.000000000000000000, -1.000000000000000000 ) ) ;
#25229 = CARTESIAN_POINT ( 'NONE',  ( -57.46284108482265651, -149.0625000027312126, 4.819101127000238627 ) ) ;
#25231 = CARTESIAN_POINT ( 'NONE',  ( -1.846868145590737420, -156.7500000013656063, 4.458734124999999437 ) ) ;
#25232 = ORIENTED_EDGE ( 'NONE', *, *, #56679, .F. ) ;
#25233 =( BOUNDED_CURVE ( )  B_SPLINE_CURVE ( 2, ( #3978, #52554, #48339, #58318, #9414, #27780, #8796, #4286, #8486 ),
 .UNSPECIFIED., .F., .F. ) 
 B_SPLINE_CURVE_WITH_KNOTS ( ( 3, 2, 2, 2, 3 ),
 ( 0.09464285714285713969, 0.09523809523809523281, 0.09642857142857143293, 0.09761904761904761918, 0.09821428571428571230 ),
 .UNSPECIFIED. ) 
 CURVE ( )  GEOMETRIC_REPRESENTATION_ITEM ( )  RATIONAL_B_SPLINE_CURVE ( ( 0.9330127018922194093, 0.9330127018922194093, 1.000000000000000000, 0.8660254037844387076, 1.000000000000000000, 0.8660254037844387076, 1.000000000000000000, 0.9330127018922194093, 0.9330127018922194093 ) ) 
 REPRESENTATION_ITEM ( '' )  );
#25234 = CARTESIAN_POINT ( 'NONE',  ( 5.000000000000000000, -83.41666666666667140, -2.886751345948130876 ) ) ;
#25235 = CARTESIAN_POINT ( 'NONE',  ( -50.18089887299979068, -130.6875000000000284, 2.462841084822635640 ) ) ;
#25236 = CARTESIAN_POINT ( 'NONE',  ( 4.458734124999999437, -42.06249999863440081, -5.460374474430324690E-16 ) ) ;
#25237 = VERTEX_POINT ( 'NONE', #19522 ) ;
#25238 = LINE ( 'NONE', #39067, #14165 ) ;
#25239 = CARTESIAN_POINT ( 'NONE',  ( -4.458734124999999437, 13.60416666803226349, -2.574251347313719407 ) ) ;
#25240 = CARTESIAN_POINT ( 'NONE',  ( -2.229367062500000163, -89.72916666530106511, -3.861377020970580443 ) ) ;
#25241 = CARTESIAN_POINT ( 'NONE',  ( -52.10840900171896806, -153.1875000013656063, 3.393966926194110556 ) ) ;
#25242 = CARTESIAN_POINT ( 'NONE',  ( -2.071067811865517250, -165.6875000000000000, -4.999999999999958256 ) ) ;
#25243 = DIRECTION ( 'NONE',  ( -0.000000000000000000, 1.000000000000000000, -0.000000000000000000 ) ) ;
#25244 = DIRECTION ( 'NONE',  ( 0.000000000000000000, -1.000000000000000000, 0.000000000000000000 ) ) ;
#25245 = CARTESIAN_POINT ( 'NONE',  ( -2.229367062500000163, -66.47916666530106511, -3.861377020970580443 ) ) ;
#25246 = CARTESIAN_POINT ( 'NONE',  ( 0.000000000000000000, -120.0000000000000000, 0.000000000000000000 ) ) ;
#25247 = CARTESIAN_POINT ( 'NONE',  ( 4.458734125000001214, 20.10416666803225993, 2.574251347313718519 ) ) ;
#25248 = AXIS2_PLACEMENT_3D ( 'NONE', #36104, #25490, #11012 ) ;
#25249 = CARTESIAN_POINT ( 'NONE',  ( -2.500000000000000444, -79.04166666393547303, -4.330127018922193649 ) ) ;
#25250 = CARTESIAN_POINT ( 'NONE',  ( 2.229367062499998831, -50.89583333196772941, -3.861377020970580887 ) ) ;
#25251 = CARTESIAN_POINT ( 'NONE',  ( -5.000000000000000000, -8.874999997268814056, 0.000000000000000000 ) ) ;
#25252 = CARTESIAN_POINT ( 'NONE',  ( -1.339745962155610925, 5.205341801261479162, 5.000000000000000000 ) ) ;
#25253 = DIRECTION ( 'NONE',  ( 0.000000000000000000, 0.000000000000000000, 1.000000000000000000 ) ) ;
#25254 = CARTESIAN_POINT ( 'NONE',  ( -2.229367062499996610, -88.39583333196773651, 3.861377020970582219 ) ) ;
#25255 = CARTESIAN_POINT ( 'NONE',  ( 2.493747252781420335E-13, -55.24999999999999289, -5.000000000000000000 ) ) ;
#25256 = CARTESIAN_POINT ( 'NONE',  ( -4.458734124999999437, -14.64583333196773474, -2.574251347313719407 ) ) ;
#25257 = ORIENTED_EDGE ( 'NONE', *, *, #12317, .F. ) ;
#25258 = CYLINDRICAL_SURFACE ( 'NONE', #17505, 5.000000000000000000 ) ;
#25259 = CARTESIAN_POINT ( 'NONE',  ( -3.152548672688508926E-16, -103.5624999986344221, -5.148502694627439702 ) ) ;
#25260 = CARTESIAN_POINT ( 'NONE',  ( 2.071067811865476394, -162.3125000027312694, 5.000000000000000000 ) ) ;
#25261 = VERTEX_POINT ( 'NONE', #58763 ) ;
#25262 = CARTESIAN_POINT ( 'NONE',  ( 9.457646018065525792E-16, -98.31249999863440792, 5.148502694627439702 ) ) ;
#25263 = CARTESIAN_POINT ( 'NONE',  ( 5.000000000000000888, -49.45833333060213732, 2.886751345948126879 ) ) ;
#25264 = CARTESIAN_POINT ( 'NONE',  ( -4.999999999999999112, -55.79166666393548013, 2.886751345948131764 ) ) ;
#25265 = CARTESIAN_POINT ( 'NONE',  ( -2.499999999999996447, -71.70833333060214443, 4.330127018922195425 ) ) ;
#25266 = CARTESIAN_POINT ( 'NONE',  ( -58.39396692619412477, -126.4375000013656063, 2.891590998281057701 ) ) ;
#25267 = CARTESIAN_POINT ( 'NONE',  ( -59.59170313451810586, -143.5000000013656063, 1.485763867205729394 ) ) ;
#25268 = EDGE_CURVE ( 'NONE', #31680, #7616, #45815, .T. ) ;
#25269 = CARTESIAN_POINT ( 'NONE',  ( -2.229367062499996610, -19.14583333196774007, 3.861377020970582219 ) ) ;
#25270 = CARTESIAN_POINT ( 'NONE',  ( 4.458734124999999437, 7.937500001365595637, -5.460374474430324690E-16 ) ) ;
#25271 = CARTESIAN_POINT ( 'NONE',  ( 9.457646018065525792E-16, -62.31249999863440792, 5.148502694627439702 ) ) ;
#25272 = CARTESIAN_POINT ( 'NONE',  ( 5.000000000000000000, -94.37499999726881583, -6.123233995736766282E-16 ) ) ;
#25273 = CARTESIAN_POINT ( 'NONE',  ( -4.458734124999999437, -18.31249999863440792, 0.000000000000000000 ) ) ;
#25274 = LINE ( 'NONE', #55519, #56824 ) ;
#25275 = CARTESIAN_POINT ( 'NONE',  ( 5.000000000000000888, -155.9375000000000000, -2.071067811865475505 ) ) ;
#25276 = CARTESIAN_POINT ( 'NONE',  ( -4.999999999999999112, -8.916666666666664298, 2.886751345948131764 ) ) ;
#25277 = CARTESIAN_POINT ( 'NONE',  ( -4.458734125000000326, -155.0000000013656063, -1.846868145590735644 ) ) ;
#25278 = ORIENTED_EDGE ( 'NONE', *, *, #41458, .F. ) ;
#25279 = CARTESIAN_POINT ( 'NONE',  ( 4.458734124999998549, -47.97916666530106511, -2.574251347313721627 ) ) ;
#25280 = CARTESIAN_POINT ( 'NONE',  ( 1.975475456537005874E-15, -44.62499999726880162, 5.000000000000000000 ) ) ;
#25281 = LINE ( 'NONE', #15639, #32923 ) ;
#25282 = CARTESIAN_POINT ( 'NONE',  ( -2.499999999999996447, 27.16666666666666430, 4.330127018922195425 ) ) ;
#25283 = CARTESIAN_POINT ( 'NONE',  ( 2.229367062499998831, 12.35416666803226171, -3.861377020970580887 ) ) ;
#25284 = LINE ( 'NONE', #33983, #42093 ) ;
#25285 = CARTESIAN_POINT ( 'NONE',  ( 1.975475456537005874E-15, -64.74999999999998579, 5.000000000000000000 ) ) ;
#25286 = DIRECTION ( 'NONE',  ( -0.000000000000000000, 1.000000000000000000, -0.000000000000000000 ) ) ;
#25287 = CARTESIAN_POINT ( 'NONE',  ( 9.457646018065525792E-16, 19.68750000136559208, 5.148502694627439702 ) ) ;
#25288 = CARTESIAN_POINT ( 'NONE',  ( -4.999999999999999112, -75.91666666666667140, 2.886751345948131764 ) ) ;
#25289 = CARTESIAN_POINT ( 'NONE',  ( 1.060575238724906964E-15, 8.375000002731187720, 5.773502691896257311 ) ) ;
#25291 = VERTEX_POINT ( 'NONE', #59731 ) ;
#25290 = ADVANCED_FACE ( 'NONE', ( #44927 ), #15657, .T. ) ;
#25292 = ORIENTED_EDGE ( 'NONE', *, *, #42145, .F. ) ;
#25293 = CONICAL_SURFACE ( 'NONE', #31442, 7.500000000000001776, 0.8594454914424796144 ) ;
#25294 = CARTESIAN_POINT ( 'NONE',  ( -1.339745962155610925, -50.79465819873851018, 5.000000000000000000 ) ) ;
#25295 = CARTESIAN_POINT ( 'NONE',  ( 2.229367062500001939, -39.97916666530107221, 3.861377020970579999 ) ) ;
#25296 = EDGE_CURVE ( 'NONE', #33278, #18086, #54254, .T. ) ;
#25297 = VECTOR ( 'NONE', #58572, 1000.000000000000000 ) ;
#25298 = AXIS2_PLACEMENT_3D ( 'NONE', #45270, #5718, #30143 ) ;
#25299 = ADVANCED_FACE ( 'NONE', ( #40409 ), #32287, .T. ) ;
#25300 = CARTESIAN_POINT ( 'NONE',  ( -2.500000000000000444, -41.04166666393548013, -4.330127018922193649 ) ) ;
#25301 = ORIENTED_EDGE ( 'NONE', *, *, #13438, .T. ) ;
#25302 = CARTESIAN_POINT ( 'NONE',  ( -4.458734124999999437, -12.39583333196774184, -2.574251347313719407 ) ) ;
#25304 = ORIENTED_EDGE ( 'NONE', *, *, #20141, .T. ) ;
#25303 = CARTESIAN_POINT ( 'NONE',  ( 4.458734124999998549, -18.97916666530107221, -2.574251347313721627 ) ) ;
#25305 = CARTESIAN_POINT ( 'NONE',  ( -5.000000000000000000, -80.00000000000000000, 0.000000000000000000 ) ) ;
#25306 = CARTESIAN_POINT ( 'NONE',  ( -8.190561711645485556E-16, -166.6875000013655779, 4.458734124999999437 ) ) ;
#25307 = CARTESIAN_POINT ( 'NONE',  ( -2.229367062500000163, -60.72916666530106511, -3.861377020970580443 ) ) ;
#25308 = CARTESIAN_POINT ( 'NONE',  ( -4.999999999999999112, -88.79166666393547303, 2.886751345948131764 ) ) ;
#25310 = VERTEX_POINT ( 'NONE', #25969 ) ;
#25309 = CARTESIAN_POINT ( 'NONE',  ( 1.339745962155612702, 3.830341803992665550, -5.000000000000000000 ) ) ;
#25311 = CARTESIAN_POINT ( 'NONE',  ( -59.81910112700025905, -140.1875000000000000, -2.462841084822630311 ) ) ;
#25312 = CARTESIAN_POINT ( 'NONE',  ( -3.152548672688508926E-16, -27.81249999863440436, -5.148502694627439702 ) ) ;
#25313 = CARTESIAN_POINT ( 'NONE',  ( -1.339745962155613812, -84.20534180126149693, -5.000000000000000000 ) ) ;
#25314 = ORIENTED_EDGE ( 'NONE', *, *, #57883, .T. ) ;
#25315 =( BOUNDED_CURVE ( )  B_SPLINE_CURVE ( 2, ( #33985, #48765, #24652, #44258, #19820, #5675, #45860, #6319, #20791 ),
 .UNSPECIFIED., .F., .F. ) 
 B_SPLINE_CURVE_WITH_KNOTS ( ( 3, 2, 2, 2, 3 ),
 ( 0.05892857142857142738, 0.05952380952380952051, 0.06071428571428571369, 0.06190476190476190688, 0.06250000000000000000 ),
 .UNSPECIFIED. ) 
 CURVE ( )  GEOMETRIC_REPRESENTATION_ITEM ( )  RATIONAL_B_SPLINE_CURVE ( ( 0.9330127018922194093, 0.9330127018922194093, 1.000000000000000000, 0.8660254037844387076, 1.000000000000000000, 0.8660254037844387076, 1.000000000000000000, 0.9330127018922194093, 0.9330127018922194093 ) ) 
 REPRESENTATION_ITEM ( '' )  );
#25316 = CARTESIAN_POINT ( 'NONE',  ( 2.730187237215162345E-16, -162.4375000013655779, -4.458734124999999437 ) ) ;
#25317 = CARTESIAN_POINT ( 'NONE',  ( 2.229367062500001939, 28.02083333469892779, 3.861377020970579999 ) ) ;
#25318 = CARTESIAN_POINT ( 'NONE',  ( -2.499999999999996447, -38.70833333060213732, 4.330127018922195425 ) ) ;
#25319 = VERTEX_POINT ( 'NONE', #15041 ) ;
#25320 = CARTESIAN_POINT ( 'NONE',  ( -50.55543936806279248, -145.3125000013656063, 0.3552334253322060320 ) ) ;
#25321 = CARTESIAN_POINT ( 'NONE',  ( -3.152548672688508926E-16, -75.81249999863440792, -5.148502694627439702 ) ) ;
#25322 = CARTESIAN_POINT ( 'NONE',  ( -52.53715891517739323, -134.5625000027312126, -4.819101127000233298 ) ) ;
#25323 = CARTESIAN_POINT ( 'NONE',  ( 2.229367062500001939, -41.97916666530107932, 3.861377020970579999 ) ) ;
#25324 = CARTESIAN_POINT ( 'NONE',  ( -4.458734124999999437, -144.1875000013656063, -5.460374474430324690E-16 ) ) ;
#25325 = CARTESIAN_POINT ( 'NONE',  ( -1.127183054612291972E-14, 23.25000000000000000, 4.999999999999999112 ) ) ;
#25326 = CARTESIAN_POINT ( 'NONE',  ( -4.458734124999999437, -48.39583333196772941, -2.574251347313719407 ) ) ;
#25327 = CARTESIAN_POINT ( 'NONE',  ( -4.458734124999998549, -16.22916666530107577, 2.574251347313722516 ) ) ;
#25328 = CARTESIAN_POINT ( 'NONE',  ( 2.500000000000002220, -102.6666666666666572, 4.330127018922192761 ) ) ;
#25329 =( BOUNDED_CURVE ( )  B_SPLINE_CURVE ( 2, ( #14326, #38760, #13074, #52630, #52325, #8259, #13391, #53569, #28491 ),
 .UNSPECIFIED., .F., .F. ) 
 B_SPLINE_CURVE_WITH_KNOTS ( ( 3, 2, 2, 2, 3 ),
 ( 0.5267857142857143016, 0.5273809523809523947, 0.5285714285714285809, 0.5297619047619047672, 0.5303571428571428603 ),
 .UNSPECIFIED. ) 
 CURVE ( )  GEOMETRIC_REPRESENTATION_ITEM ( )  RATIONAL_B_SPLINE_CURVE ( ( 0.9330127018922194093, 0.9330127018922194093, 1.000000000000000000, 0.8660254037844387076, 1.000000000000000000, 0.8660254037844387076, 1.000000000000000000, 0.9330127018922194093, 0.9330127018922194093 ) ) 
 REPRESENTATION_ITEM ( '' )  );
#25330 = CARTESIAN_POINT ( 'NONE',  ( -1.846868145590737420, -140.0000000013655779, 4.458734124999999437 ) ) ;
#25331 = CARTESIAN_POINT ( 'NONE',  ( -2.229367062500000163, -32.72916666530106511, -3.861377020970580443 ) ) ;
#25332 = CARTESIAN_POINT ( 'NONE',  ( 5.000000000000000888, 8.541666669397853795, 2.886751345948126879 ) ) ;
#25333 = DIRECTION ( 'NONE',  ( -0.000000000000000000, 1.000000000000000000, -0.000000000000000000 ) ) ;
#25334 = CARTESIAN_POINT ( 'NONE',  ( -50.70258187064364108, -128.1250000013656347, 2.196230717870141014 ) ) ;
#25335 = CARTESIAN_POINT ( 'NONE',  ( 9.457646018065525792E-16, -76.31249999863439371, 5.148502694627439702 ) ) ;
#25336 = DIRECTION ( 'NONE',  ( -0.000000000000000000, 1.000000000000000000, -0.000000000000000000 ) ) ;
#25337 = CARTESIAN_POINT ( 'NONE',  ( 0.000000000000000000, -170.0000000000000000, 5.000000000000000000 ) ) ;
#25338 = CARTESIAN_POINT ( 'NONE',  ( -4.458734124999999437, -2.562499998634407028, 0.000000000000000000 ) ) ;
#25339 = VERTEX_POINT ( 'NONE', #20517 ) ;
#25340 = DIRECTION ( 'NONE',  ( -0.000000000000000000, 1.000000000000000000, -0.000000000000000000 ) ) ;
#25341 = CARTESIAN_POINT ( 'NONE',  ( 5.000000000000000888, 23.54166666939785202, 2.886751345948126879 ) ) ;
#25343 = CARTESIAN_POINT ( 'NONE',  ( 4.458734124999998549, -33.72916666530106511, -2.574251347313721627 ) ) ;
#25342 = CARTESIAN_POINT ( 'NONE',  ( 2.229367062499998831, -86.64583333196773651, -3.861377020970580887 ) ) ;
#25344 = CARTESIAN_POINT ( 'NONE',  ( 5.000000000000000000, -95.50000000000000000, -6.123233995736766282E-16 ) ) ;
#25345 = CARTESIAN_POINT ( 'NONE',  ( 2.229367062499998831, -80.89583333196773651, -3.861377020970580887 ) ) ;
#25346 = VECTOR ( 'NONE', #54858, 1000.000000000000000 ) ;
#25347 = CARTESIAN_POINT ( 'NONE',  ( 2.229367062499998831, 19.10416666803225993, -3.861377020970580887 ) ) ;
#25348 = CYLINDRICAL_SURFACE ( 'NONE', #31490, 5.000000000000000000 ) ;
#25349 = VECTOR ( 'NONE', #46146, 1000.000000000000000 ) ;
#25351 = EDGE_CURVE ( 'NONE', #25405, #18740, #58948, .T. ) ;
#25350 = CARTESIAN_POINT ( 'NONE',  ( -51.60603307380591787, -138.9375000013656063, -2.891590998281053704 ) ) ;
#25352 = CLOSED_SHELL ( 'NONE', ( #10016, #19397, #29448, #21947, #26816, #32085, #40968, #34918, #45695, #28741, #14234, #51439, #17381, #30357, #29838, #44373, #11910, #13468, #16845, #14445, #55014 ) ) ;
#25353 = CARTESIAN_POINT ( 'NONE',  ( 4.458734125000000326, -2.895833331967738289, 2.574251347313718519 ) ) ;
#25354 = CARTESIAN_POINT ( 'NONE',  ( -2.229367062500000163, 20.27083333469892779, -3.861377020970580443 ) ) ;
#25355 = CARTESIAN_POINT ( 'NONE',  ( -4.458734124999997661, -48.47916666530106511, 2.574251347313722516 ) ) ;
#25356 = CARTESIAN_POINT ( 'NONE',  ( 1.975475456537005874E-15, -15.75000000000000000, 5.000000000000000000 ) ) ;
#25357 = CARTESIAN_POINT ( 'NONE',  ( 4.458734125000000326, -1.895833331967737623, 2.574251347313718519 ) ) ;
#25358 = ORIENTED_EDGE ( 'NONE', *, *, #29978, .F. ) ;
#25359 = CARTESIAN_POINT ( 'NONE',  ( -3.152548672688508926E-16, -30.81249999863440436, -5.148502694627439702 ) ) ;
#25360 = CARTESIAN_POINT ( 'NONE',  ( -54.64476657466781973, -133.0625000013656063, -4.444560631937228834 ) ) ;
#25361 = CARTESIAN_POINT ( 'NONE',  ( -3.152548672688508926E-16, -74.56249999863440792, -5.148502694627439702 ) ) ;
#25362 = CARTESIAN_POINT ( 'NONE',  ( -3.535250795749689387E-16, -108.1249999972688016, -5.773502691896257311 ) ) ;
#25363 = CARTESIAN_POINT ( 'NONE',  ( -2.229367062499996610, 26.85416666803225993, 3.861377020970582219 ) ) ;
#25364 = CARTESIAN_POINT ( 'NONE',  ( 1.339745962155612258, 26.41965820146970501, 5.000000000000000888 ) ) ;
#25365 = CARTESIAN_POINT ( 'NONE',  ( 4.458734125000000326, -109.1458333319677365, 2.574251347313718519 ) ) ;
#25366 = CARTESIAN_POINT ( 'NONE',  ( -4.458734124999997661, -78.47916666530106511, 2.574251347313722516 ) ) ;
#25367 = CARTESIAN_POINT ( 'NONE',  ( 2.500000000000002220, -58.66666666666665719, 4.330127018922192761 ) ) ;
#25368 = CARTESIAN_POINT ( 'NONE',  ( -50.18089887299978358, -151.6875000000000284, 2.462841084822590787 ) ) ;
#25369 = CARTESIAN_POINT ( 'NONE',  ( 1.060575238724906964E-15, 25.37500000273118417, 5.773502691896257311 ) ) ;
#25370 = ORIENTED_EDGE ( 'NONE', *, *, #9075, .F. ) ;
#25371 = CARTESIAN_POINT ( 'NONE',  ( -5.000000000000000000, -72.95833333060214443, -2.886751345948128211 ) ) ;
#25372 = CARTESIAN_POINT ( 'NONE',  ( -5.000000000000000000, -99.00000000000000000, 0.000000000000000000 ) ) ;
#25373 = CARTESIAN_POINT ( 'NONE',  ( 5.000000000000000000, -20.49999999999999645, -6.123233995736766282E-16 ) ) ;
#25374 = CARTESIAN_POINT ( 'NONE',  ( -3.152548672688508926E-16, -21.56249999863440081, -5.148502694627439702 ) ) ;
#25375 = CARTESIAN_POINT ( 'NONE',  ( 2.229367062499998831, -82.64583333196773651, -3.861377020970580887 ) ) ;
#25376 = CARTESIAN_POINT ( 'NONE',  ( -2.499999999999996447, -22.70833333060214443, 4.330127018922195425 ) ) ;
#25378 = VERTEX_POINT ( 'NONE', #29823 ) ;
#25377 = CARTESIAN_POINT ( 'NONE',  ( 4.458734124999999437, -49.81249999863440792, -5.460374474430324690E-16 ) ) ;
#25379 = CARTESIAN_POINT ( 'NONE',  ( -6.972266317189433020E-16, -70.12499999726880162, -5.000000000000000000 ) ) ;
#25380 = CARTESIAN_POINT ( 'NONE',  ( -2.500000000000000444, 10.95833333606451632, -4.330127018922193649 ) ) ;
#25382 = ORIENTED_EDGE ( 'NONE', *, *, #24345, .T. ) ;
#25381 = CARTESIAN_POINT ( 'NONE',  ( -4.458734124999999437, -2.562499998634407028, 0.000000000000000000 ) ) ;
#25383 = CARTESIAN_POINT ( 'NONE',  ( -51.60603307380591787, -149.9375000013656063, -2.891590998281053704 ) ) ;
#25384 = CARTESIAN_POINT ( 'NONE',  ( -5.000000000000000000, -67.00000000000000000, 0.000000000000000000 ) ) ;
#25385 = CARTESIAN_POINT ( 'NONE',  ( -4.458734125000000326, -151.2500000013656063, -1.846868145590735644 ) ) ;
#25386 = CARTESIAN_POINT ( 'NONE',  ( 2.229367062499998831, -48.89583333196772941, -3.861377020970580887 ) ) ;
#25387 =( BOUNDED_CURVE ( )  B_SPLINE_CURVE ( 2, ( #53611, #33363, #48466, #58749, #52978, #10181, #14678, #9846, #39122 ),
 .UNSPECIFIED., .F., .F. ) 
 B_SPLINE_CURVE_WITH_KNOTS ( ( 3, 2, 2, 2, 3 ),
 ( 0.2979166666666666630, 0.2986111111111111049, 0.2999999999999999889, 0.3013888888888888729, 0.3020833333333333148 ),
 .UNSPECIFIED. ) 
 CURVE ( )  GEOMETRIC_REPRESENTATION_ITEM ( )  RATIONAL_B_SPLINE_CURVE ( ( 0.9330127018922194093, 0.9330127018922194093, 1.000000000000000000, 0.8660254037844387076, 1.000000000000000000, 0.8660254037844387076, 1.000000000000000000, 0.9330127018922194093, 0.9330127018922194093 ) ) 
 REPRESENTATION_ITEM ( '' )  );
#25388 = CARTESIAN_POINT ( 'NONE',  ( -5.000000000000000888, -158.5625000000000000, -2.071067811865475949 ) ) ;
#25389 = CARTESIAN_POINT ( 'NONE',  ( -1.339745962155610925, 11.20534180126147739, 5.000000000000000000 ) ) ;
#25390 = CARTESIAN_POINT ( 'NONE',  ( -60.14911071818854538, -153.0625000000000000, 1.666127454062681368 ) ) ;
#25391 = AXIS2_PLACEMENT_3D ( 'NONE', #2577, #6205, #56614 ) ;
#25392 = CARTESIAN_POINT ( 'NONE',  ( 4.458734124999998549, -10.97916666530107044, -2.574251347313721627 ) ) ;
#25393 = AXIS2_PLACEMENT_3D ( 'NONE', #2337, #55410, #16161 ) ;
#25394 = CARTESIAN_POINT ( 'NONE',  ( 9.457646018065525792E-16, -47.31249999863440792, 5.148502694627439702 ) ) ;
#25395 = DIRECTION ( 'NONE',  ( 7.709882115452476194E-16, -0.000000000000000000, 1.000000000000000000 ) ) ;
#25396 = CARTESIAN_POINT ( 'NONE',  ( 2.730187237215162345E-16, -146.1875000013656063, -4.458734124999999437 ) ) ;
#25397 = AXIS2_PLACEMENT_3D ( 'NONE', #47172, #3116, #22734 ) ;
#25398 = CARTESIAN_POINT ( 'NONE',  ( -2.229367062499996610, -94.39583333196773651, 3.861377020970582219 ) ) ;
#25399 = CARTESIAN_POINT ( 'NONE',  ( -51.75738570946856498, -149.7500000000000284, 3.805975901505576964 ) ) ;
#25400 = VERTEX_POINT ( 'NONE', #50421 ) ;
#25401 = CARTESIAN_POINT ( 'NONE',  ( -1.230605004983934782E-13, -37.62499999726881583, 5.000000000000000000 ) ) ;
#25402 = CARTESIAN_POINT ( 'NONE',  ( -54.60164318462004474, -148.5000000027312126, -4.984105922594373794 ) ) ;
#25403 = CARTESIAN_POINT ( 'NONE',  ( -6.972266317189433020E-16, -62.24999999999999289, -5.000000000000000000 ) ) ;
#25404 = EDGE_CURVE ( 'NONE', #34999, #13547, #6365, .T. ) ;
#25405 = VERTEX_POINT ( 'NONE', #25654 ) ;
#25406 = CARTESIAN_POINT ( 'NONE',  ( -4.458734124999998549, 5.770833334698927786, 2.574251347313722516 ) ) ;
#25407 = CARTESIAN_POINT ( 'NONE',  ( 2.499999999999998668, -50.20833333060213732, -4.330127018922193649 ) ) ;
#25408 = CARTESIAN_POINT ( 'NONE',  ( -4.458734124999998549, -18.47916666530106866, 2.574251347313722516 ) ) ;
#25409 = CARTESIAN_POINT ( 'NONE',  ( 4.458734124999999437, -6.812499998634404363, -5.460374474430324690E-16 ) ) ;
#25410 = CARTESIAN_POINT ( 'NONE',  ( 1.339745962155615144, -77.58034179853028434, 4.999999999999999112 ) ) ;
#25411 = CARTESIAN_POINT ( 'NONE',  ( 4.458734124999999437, -147.4375000013656063, 0.000000000000000000 ) ) ;
#25412 =( BOUNDED_CURVE ( )  B_SPLINE_CURVE ( 2, ( #8767, #28375, #9078, #43166, #57975, #14837, #43478, #62805, #38651 ),
 .UNSPECIFIED., .F., .F. ) 
 B_SPLINE_CURVE_WITH_KNOTS ( ( 3, 2, 2, 2, 3 ),
 ( 0.3250000000000002887, 0.3291666666666669405, 0.3333333333333335924, 0.3375000000000002998, 0.3416666666666669516 ),
 .UNSPECIFIED. ) 
 CURVE ( )  GEOMETRIC_REPRESENTATION_ITEM ( )  RATIONAL_B_SPLINE_CURVE ( ( 0.9999999999999948930, 0.9238795325112918455, 1.000000000000000000, 0.9238795325112867385, 1.000000000000000000, 0.9238795325112867385, 1.000000000000000000, 0.9238795325112816315, 1.000000000000005107 ) ) 
 REPRESENTATION_ITEM ( '' )  );
#25413 = CARTESIAN_POINT ( 'NONE',  ( -2.229367062500000163, 18.27083333469892779, -3.861377020970580443 ) ) ;
#25414 = ORIENTED_EDGE ( 'NONE', *, *, #53478, .F. ) ;
#25415 = FACE_OUTER_BOUND ( 'NONE', #31906, .T. ) ;
#25416 = CARTESIAN_POINT ( 'NONE',  ( 5.000000000000000888, -71.45833333060214443, 2.886751345948126879 ) ) ;
#25417 = CARTESIAN_POINT ( 'NONE',  ( 9.457646018065525792E-16, -21.06249999863440436, 5.148502694627439702 ) ) ;
#25418 = CARTESIAN_POINT ( 'NONE',  ( -52.53715891517739323, -143.4375000000000284, -4.819101127000233298 ) ) ;
#25419 = CARTESIAN_POINT ( 'NONE',  ( 0.000000000000000000, -170.0000000000000000, 5.000000000000000000 ) ) ;
#25420 = CARTESIAN_POINT ( 'NONE',  ( -50.40829686548195099, -151.0000000013656063, -1.485763867205728284 ) ) ;
#25421 = CARTESIAN_POINT ( 'NONE',  ( 2.500000000000002220, -45.54166666393547303, 4.330127018922192761 ) ) ;
#25422 = CARTESIAN_POINT ( 'NONE',  ( 5.000000000000000000, -67.29166666393547303, -2.886751345948130876 ) ) ;
#25423 = CARTESIAN_POINT ( 'NONE',  ( -2.229367062500000163, 14.52083333469892779, -3.861377020970580443 ) ) ;
#25424 = CYLINDRICAL_SURFACE ( 'NONE', #36599, 5.000000000000000000 ) ;
#25425 = ORIENTED_EDGE ( 'NONE', *, *, #9724, .T. ) ;
#25426 = CARTESIAN_POINT ( 'NONE',  ( 4.458734124999999437, 11.18750000136559386, -5.460374474430324690E-16 ) ) ;
#25427 = CARTESIAN_POINT ( 'NONE',  ( -4.458734124999999437, -62.31249999863440792, 0.000000000000000000 ) ) ;
#25428 = ORIENTED_EDGE ( 'NONE', *, *, #19764, .F. ) ;
#25429 = CARTESIAN_POINT ( 'NONE',  ( -4.458734124999997661, -16.47916666530107577, 2.574251347313722516 ) ) ;
#25430 = VECTOR ( 'NONE', #14949, 1000.000000000000000 ) ;
#25431 = CARTESIAN_POINT ( 'NONE',  ( 2.500000000000002220, 5.333333333333332149, 4.330127018922192761 ) ) ;
#25432 = CARTESIAN_POINT ( 'NONE',  ( -4.458734125000000326, -165.0000000013655779, -1.846868145590735644 ) ) ;
#25433 = CARTESIAN_POINT ( 'NONE',  ( -5.926426369611017623E-15, 26.37500000273118417, 5.000000000000000000 ) ) ;
#25434 = CARTESIAN_POINT ( 'NONE',  ( 4.458734125000001214, -58.89583333196773651, 2.574251347313718519 ) ) ;
#25435 = CARTESIAN_POINT ( 'NONE',  ( -3.535250795749689387E-16, -88.12499999726878741, -5.773502691896257311 ) ) ;
#25436 = CARTESIAN_POINT ( 'NONE',  ( 4.458734124999998549, -33.72916666530107221, -2.574251347313721627 ) ) ;
#25437 = CARTESIAN_POINT ( 'NONE',  ( 1.339745962155615144, -8.705341801261482715, 4.999999999999999112 ) ) ;
#25438 = CARTESIAN_POINT ( 'NONE',  ( 5.000000000000000000, -69.49999999999998579, -6.123233995736766282E-16 ) ) ;
#25439 = CARTESIAN_POINT ( 'NONE',  ( 2.499999999999998668, -16.20833333060214443, -4.330127018922193649 ) ) ;
#25440 = CARTESIAN_POINT ( 'NONE',  ( -1.846868145590737420, -150.0000000013656063, 4.458734124999997661 ) ) ;
#25441 = CARTESIAN_POINT ( 'NONE',  ( 1.060575238724906964E-15, -43.75000000000000000, 5.773502691896257311 ) ) ;
#25442 = DIRECTION ( 'NONE',  ( -0.000000000000000000, 1.000000000000000000, -0.000000000000000000 ) ) ;
#25443 = CARTESIAN_POINT ( 'NONE',  ( 5.000000000000000000, -17.37499999726881583, -6.123233995736766282E-16 ) ) ;
#25444 = ORIENTED_EDGE ( 'NONE', *, *, #19251, .T. ) ;
#25445 = CARTESIAN_POINT ( 'NONE',  ( 2.229367062499998831, -106.6458333319677365, -3.861377020970580887 ) ) ;
#25446 = CARTESIAN_POINT ( 'NONE',  ( -3.152548672688508926E-16, 4.187500001365595637, -5.148502694627439702 ) ) ;
#25447 = DIRECTION ( 'NONE',  ( 0.000000000000000000, 0.000000000000000000, 1.000000000000000000 ) ) ;
#25448 = CARTESIAN_POINT ( 'NONE',  ( -4.999999999999999112, -1.916666666666663854, 2.886751345948131764 ) ) ;
#25449 = CARTESIAN_POINT ( 'NONE',  ( -4.458734124999999437, -64.31249999863440792, 0.000000000000000000 ) ) ;
#25450 = CARTESIAN_POINT ( 'NONE',  ( -58.24261429053147765, -147.3750000027312126, -3.805975901505573855 ) ) ;
#25451 = CARTESIAN_POINT ( 'NONE',  ( -2.500000000000000444, -6.041666663935481019, -4.330127018922193649 ) ) ;
#25453 = VERTEX_POINT ( 'NONE', #49455 ) ;
#25452 = CARTESIAN_POINT ( 'NONE',  ( 4.458734125000001214, -33.89583333196773651, 2.574251347313718519 ) ) ;
#25454 = CARTESIAN_POINT ( 'NONE',  ( -1.339745962155610925, -77.79465819873853150, 5.000000000000000000 ) ) ;
#25455 = CARTESIAN_POINT ( 'NONE',  ( 1.339745962155612702, -22.16965819600733312, -5.000000000000000000 ) ) ;
#25456 = ORIENTED_EDGE ( 'NONE', *, *, #37409, .F. ) ;
#25457 = CARTESIAN_POINT ( 'NONE',  ( -4.999999999999998224, -48.79166666393547303, 2.886751345948131764 ) ) ;
#25458 = CARTESIAN_POINT ( 'NONE',  ( 5.000000000000000888, -49.58333333333332860, 2.886751345948126879 ) ) ;
#25459 = CARTESIAN_POINT ( 'NONE',  ( -4.458734124999998549, -28.47916666530107221, 2.574251347313722516 ) ) ;
#25460 = CARTESIAN_POINT ( 'NONE',  ( -2.499999999999996447, -41.70833333060214443, 4.330127018922195425 ) ) ;
#25461 = CARTESIAN_POINT ( 'NONE',  ( 4.458734125000001214, -75.89583333196775072, 2.574251347313718519 ) ) ;
#25462 = CARTESIAN_POINT ( 'NONE',  ( 5.000000000000000000, -169.0625000000000000, 2.071067811865478614 ) ) ;
#25463 = CARTESIAN_POINT ( 'NONE',  ( 2.229367062500001939, -80.97916666530106511, 3.861377020970579999 ) ) ;
#25464 = CARTESIAN_POINT ( 'NONE',  ( -50.55543936806279248, -137.3125000013656063, 0.3552334253322060320 ) ) ;
#25465 = CARTESIAN_POINT ( 'NONE',  ( 4.458734124999998549, -30.97916666530107577, -2.574251347313721627 ) ) ;
#25466 = ORIENTED_EDGE ( 'NONE', *, *, #5182, .T. ) ;
#25467 = CARTESIAN_POINT ( 'NONE',  ( 1.339745962155615144, -51.70534180126148271, 4.999999999999999112 ) ) ;
#25468 = ORIENTED_EDGE ( 'NONE', *, *, #47134, .F. ) ;
#25469 = CARTESIAN_POINT ( 'NONE',  ( -4.458734124999998549, -72.47916666530107932, 2.574251347313722516 ) ) ;
#25470 = CARTESIAN_POINT ( 'NONE',  ( -2.500000000000000444, 21.95833333606451987, -4.330127018922193649 ) ) ;
#25471 = ORIENTED_EDGE ( 'NONE', *, *, #20421, .F. ) ;
#25472 = AXIS2_PLACEMENT_3D ( 'NONE', #30393, #40681, #21397 ) ;
#25473 = DIRECTION ( 'NONE',  ( 0.000000000000000000, 0.000000000000000000, 1.000000000000000000 ) ) ;
#25475 = EDGE_CURVE ( 'NONE', #61933, #30240, #18748, .T. ) ;
#25474 = CARTESIAN_POINT ( 'NONE',  ( -2.229367062500000163, -63.72916666530106511, -3.861377020970580443 ) ) ;
#25476 = VECTOR ( 'NONE', #60820, 1000.000000000000000 ) ;
#25477 = CARTESIAN_POINT ( 'NONE',  ( -2.229367062499996610, -1.395833331967737179, 3.861377020970582219 ) ) ;
#25478 = ORIENTED_EDGE ( 'NONE', *, *, #10882, .F. ) ;
#25479 = CARTESIAN_POINT ( 'NONE',  ( 3.044556291839386294E-14, 17.75000000000000000, -5.000000000000000000 ) ) ;
#25480 = CARTESIAN_POINT ( 'NONE',  ( -6.972266317189433020E-16, -21.12499999726881228, -5.000000000000000000 ) ) ;
#25481 = CARTESIAN_POINT ( 'NONE',  ( 9.457646018065525792E-16, 14.93750000136559564, 5.148502694627439702 ) ) ;
#25482 = CARTESIAN_POINT ( 'NONE',  ( -56.48576386720575471, -140.7500000013655779, -4.591703134518078322 ) ) ;
#25483 = CARTESIAN_POINT ( 'NONE',  ( 1.975475456537005874E-15, -24.74999999999999645, 5.000000000000000000 ) ) ;
#25484 = CARTESIAN_POINT ( 'NONE',  ( -4.458734125000000326, -161.8750000013656063, 1.846868145590734089 ) ) ;
#25485 = CARTESIAN_POINT ( 'NONE',  ( 5.000000000000000000, -75.29166666393548724, -2.886751345948130876 ) ) ;
#25486 = ORIENTED_EDGE ( 'NONE', *, *, #46381, .F. ) ;
#25487 = CARTESIAN_POINT ( 'NONE',  ( -3.152548672688508926E-16, -81.56249999863440792, -5.148502694627439702 ) ) ;
#25488 = CARTESIAN_POINT ( 'NONE',  ( 1.975475456537005874E-15, -75.74999999999998579, 5.000000000000000000 ) ) ;
#25489 = CARTESIAN_POINT ( 'NONE',  ( 4.458734125000001214, -4.895833331967740065, 2.574251347313718519 ) ) ;
#25490 = DIRECTION ( 'NONE',  ( -0.000000000000000000, 1.000000000000000000, -0.000000000000000000 ) ) ;
#25491 = VECTOR ( 'NONE', #50013, 1000.000000000000000 ) ;
#25492 = EDGE_CURVE ( 'NONE', #46232, #28871, #37213, .T. ) ;
#25493 = CARTESIAN_POINT ( 'NONE',  ( 5.000000000000000000, 4.708333336064518093, -2.886751345948130876 ) ) ;
#25494 = CARTESIAN_POINT ( 'NONE',  ( 2.229367062500001939, -71.22916666530107932, 3.861377020970579999 ) ) ;
#25495 = CARTESIAN_POINT ( 'NONE',  ( -3.535250795749689387E-16, -26.12499999726881583, -5.773502691896257311 ) ) ;
#25496 = EDGE_CURVE ( 'NONE', #11953, #3491, #20451, .T. ) ;
#25497 = CARTESIAN_POINT ( 'NONE',  ( -1.339745962155610925, -14.79465819873851729, 5.000000000000000000 ) ) ;
#25498 = CARTESIAN_POINT ( 'NONE',  ( -4.458734124999999437, 28.60416666803226349, -2.574251347313719407 ) ) ;
#25499 = CARTESIAN_POINT ( 'NONE',  ( 2.229367062500001939, 29.02083333469892779, 3.861377020970579999 ) ) ;
#25500 = CARTESIAN_POINT ( 'NONE',  ( 4.458734124999998549, -47.72916666530106511, -2.574251347313721627 ) ) ;
#25501 = CARTESIAN_POINT ( 'NONE',  ( -4.458734124999999437, -30.64583333196774007, -2.574251347313719407 ) ) ;
#25502 = CARTESIAN_POINT ( 'NONE',  ( -2.229367062499996610, 1.604166668032262155, 3.861377020970582219 ) ) ;
#25503 = CARTESIAN_POINT ( 'NONE',  ( 3.535533905932736864, -146.2500000027311842, 3.535533905932738641 ) ) ;
#25504 = CARTESIAN_POINT ( 'NONE',  ( 2.499999999999998668, 22.66666666666666430, -4.330127018922193649 ) ) ;
#25505 = CARTESIAN_POINT ( 'NONE',  ( -5.000000000000000888, -145.5625000027311842, 2.071067811865474617 ) ) ;
#25506 = CARTESIAN_POINT ( 'NONE',  ( 6.158835246850666199E-14, 7.875000002731183280, -4.999999999999999112 ) ) ;
#25507 = CARTESIAN_POINT ( 'NONE',  ( -3.152548672688508926E-16, -42.56249999863440792, -5.148502694627439702 ) ) ;
#25508 = CARTESIAN_POINT ( 'NONE',  ( -2.499999999999996447, -75.70833333060214443, 4.330127018922195425 ) ) ;
#25509 = EDGE_CURVE ( 'NONE', #11915, #41425, #13864, .T. ) ;
#25510 = CARTESIAN_POINT ( 'NONE',  ( -51.60603307380591787, -143.1875000013656063, -2.891590998281053704 ) ) ;
#25511 =( BOUNDED_CURVE ( )  B_SPLINE_CURVE ( 2, ( #54382, #29597, #39248, #25422, #6456, #45041, #1008, #24787, #19638 ),
 .UNSPECIFIED., .F., .F. ) 
 B_SPLINE_CURVE_WITH_KNOTS ( ( 3, 2, 2, 2, 3 ),
 ( 0.6875000000000000000, 0.6880952380952380931, 0.6892857142857142794, 0.6904761904761904656, 0.6910714285714285587 ),
 .UNSPECIFIED. ) 
 CURVE ( )  GEOMETRIC_REPRESENTATION_ITEM ( )  RATIONAL_B_SPLINE_CURVE ( ( 0.9330127018922194093, 0.9330127018922194093, 1.000000000000000000, 0.8660254037844387076, 1.000000000000000000, 0.8660254037844387076, 1.000000000000000000, 0.9330127018922194093, 0.9330127018922194093 ) ) 
 REPRESENTATION_ITEM ( '' )  );
#25512 = DIRECTION ( 'NONE',  ( -0.000000000000000000, 1.000000000000000000, -0.000000000000000000 ) ) ;
#25513 = CARTESIAN_POINT ( 'NONE',  ( -75.00000000000001421, 0.000000000000000000, -9.000000000000001776 ) ) ;
#25514 = CARTESIAN_POINT ( 'NONE',  ( 2.229367062499998831, -77.89583333196773651, -3.861377020970580887 ) ) ;
#25515 = CARTESIAN_POINT ( 'NONE',  ( -3.152801135295367985, -166.0625000013656063, 3.152801135295367096 ) ) ;
#25516 = LINE ( 'NONE', #45134, #19380 ) ;
#25517 = CARTESIAN_POINT ( 'NONE',  ( 5.000000000000000888, 13.54166666939785202, 2.886751345948126879 ) ) ;
#25518 = CARTESIAN_POINT ( 'NONE',  ( -5.000000000000000000, -30.08333333333333215, -2.886751345948128211 ) ) ;
#25519 = CARTESIAN_POINT ( 'NONE',  ( 4.458734124999999437, -141.5000000013655779, 1.846868145590737864 ) ) ;
#25520 = VERTEX_POINT ( 'NONE', #2488 ) ;
#25521 = CARTESIAN_POINT ( 'NONE',  ( -4.458734124999999437, 22.43750000136559564, 0.000000000000000000 ) ) ;
#25522 = VERTEX_POINT ( 'NONE', #21790 ) ;
#25523 = CARTESIAN_POINT ( 'NONE',  ( 4.458734124999999437, -64.06249999863440792, -5.460374474430324690E-16 ) ) ;
#25524 = AXIS2_PLACEMENT_3D ( 'NONE', #49924, #36413, #6837 ) ;
#25525 = CARTESIAN_POINT ( 'NONE',  ( 5.000000000000000000, 21.70833333606451987, -2.886751345948129988 ) ) ;
#25526 = CARTESIAN_POINT ( 'NONE',  ( 5.000000000000000000, 2.583333333333333481, -2.886751345948130876 ) ) ;
#25527 = CARTESIAN_POINT ( 'NONE',  ( -5.000000000000000000, 14.91666666666666607, -2.886751345948128211 ) ) ;
#25528 = AXIS2_PLACEMENT_3D ( 'NONE', #3724, #31473, #51114 ) ;
#25529 = CARTESIAN_POINT ( 'NONE',  ( -4.458734124999999437, -48.39583333196772941, -2.574251347313719407 ) ) ;
#25530 = CARTESIAN_POINT ( 'NONE',  ( 4.458734124999999437, -10.81249999863440792, -5.460374474430324690E-16 ) ) ;
#25531 = CARTESIAN_POINT ( 'NONE',  ( 7.500000000000000000, 3.948247735265829395, -7.349893093595813554 ) ) ;
#25532 = EDGE_CURVE ( 'NONE', #54505, #39380, #27031, .T. ) ;
#25533 = CARTESIAN_POINT ( 'NONE',  ( -5.000000000000000000, 0.1250000027311869155, 0.000000000000000000 ) ) ;
#25534 = CARTESIAN_POINT ( 'NONE',  ( -4.999999999999998224, -74.79166666393547303, 2.886751345948131764 ) ) ;
#25535 = CYLINDRICAL_SURFACE ( 'NONE', #38685, 5.000000000000000000 ) ;
#25537 = CARTESIAN_POINT ( 'NONE',  ( 2.229367062500001939, -12.22916666530107044, 3.861377020970579999 ) ) ;
#25536 = CARTESIAN_POINT ( 'NONE',  ( -6.972266317189433020E-16, -5.249999999999998224, -5.000000000000000000 ) ) ;
#25538 = CARTESIAN_POINT ( 'NONE',  ( 1.975475456537005874E-15, -12.62499999726881050, 5.000000000000000000 ) ) ;
#25539 = CARTESIAN_POINT ( 'NONE',  ( 2.229367062499998831, -59.64583333196774362, -3.861377020970580887 ) ) ;
#25540 = CARTESIAN_POINT ( 'NONE',  ( -8.190561711645485556E-16, -156.9375000013655779, 4.458734124999999437 ) ) ;
#25541 = CARTESIAN_POINT ( 'NONE',  ( 5.000000000000000000, -56.29166666393548013, -2.886751345948129988 ) ) ;
#25542 = ORIENTED_EDGE ( 'NONE', *, *, #10174, .F. ) ;
#25543 = CYLINDRICAL_SURFACE ( 'NONE', #37386, 5.000000000000000000 ) ;
#25544 = CARTESIAN_POINT ( 'NONE',  ( -4.458734124999999437, 0.3541666680322609340, -2.574251347313719407 ) ) ;
#25545 = EDGE_LOOP ( 'NONE', ( #15970, #60870 ) ) ;
#25547 = CARTESIAN_POINT ( 'NONE',  ( 5.000000000000000000, -9.291666663935483683, -2.886751345948130876 ) ) ;
#25546 = CARTESIAN_POINT ( 'NONE',  ( -2.071067811865351604, -157.4375000027312126, 5.000000000000126121 ) ) ;
#25548 = CARTESIAN_POINT ( 'NONE',  ( -1.846868145590734756, -158.1250000013656063, -4.458734125000000326 ) ) ;
#25549 = ORIENTED_EDGE ( 'NONE', *, *, #18788, .F. ) ;
#25550 = CARTESIAN_POINT ( 'NONE',  ( 2.499999999999998668, -99.33333333333332860, -4.330127018922193649 ) ) ;
#25551 = CARTESIAN_POINT ( 'NONE',  ( -59.98410592259440222, -129.1250000000000284, -0.3983568153799752487 ) ) ;
#25552 = DIRECTION ( 'NONE',  ( -0.000000000000000000, 1.000000000000000000, -0.000000000000000000 ) ) ;
#25554 = EDGE_CURVE ( 'NONE', #42628, #42363, #31414, .T. ) ;
#25553 = CARTESIAN_POINT ( 'NONE',  ( -4.458734124999999437, -47.64583333196775072, -2.574251347313719407 ) ) ;
#25555 = ORIENTED_EDGE ( 'NONE', *, *, #58971, .T. ) ;
#25556 = EDGE_CURVE ( 'NONE', #17081, #8963, #17897, .T. ) ;
#25557 = ADVANCED_FACE ( 'NONE', ( #16636 ), #11491, .T. ) ;
#25558 = CARTESIAN_POINT ( 'NONE',  ( 1.339745962155637349, 10.83034180399266333, -4.999999999999985789 ) ) ;
#25559 = CARTESIAN_POINT ( 'NONE',  ( 9.457646018065525792E-16, 12.93750000136559386, 5.148502694627439702 ) ) ;
#25560 =( BOUNDED_CURVE ( )  B_SPLINE_CURVE ( 2, ( #13842, #53710, #48875, #14465, #18357, #9643, #23186, #23817, #58849 ),
 .UNSPECIFIED., .F., .F. ) 
 B_SPLINE_CURVE_WITH_KNOTS ( ( 3, 2, 2, 2, 3 ),
 ( 0.1770833333333333426, 0.1777777777777777846, 0.1791666666666666685, 0.1805555555555555525, 0.1812499999999999944 ),
 .UNSPECIFIED. ) 
 CURVE ( )  GEOMETRIC_REPRESENTATION_ITEM ( )  RATIONAL_B_SPLINE_CURVE ( ( 0.9330127018922194093, 0.9330127018922194093, 1.000000000000000000, 0.8660254037844387076, 1.000000000000000000, 0.8660254037844387076, 1.000000000000000000, 0.9330127018922194093, 0.9330127018922194093 ) ) 
 REPRESENTATION_ITEM ( '' )  );
#25561 = CARTESIAN_POINT ( 'NONE',  ( 4.458734125000001214, 27.10416666803225993, 2.574251347313718519 ) ) ;
#25562 = CARTESIAN_POINT ( 'NONE',  ( -51.19402409849444524, -124.6250000027312126, -3.242614290531456334 ) ) ;
#25563 = CARTESIAN_POINT ( 'NONE',  ( 1.975475456537005874E-15, -17.75000000000000355, 5.000000000000000000 ) ) ;
#25564 = CARTESIAN_POINT ( 'NONE',  ( 1.339745962155612702, -25.29465819873852439, -5.000000000000000000 ) ) ;
#25565 =( BOUNDED_CURVE ( )  B_SPLINE_CURVE ( 2, ( #38421, #29711, #9775, #58047, #24585, #13977, #38728, #4638, #49342 ),
 .UNSPECIFIED., .F., .F. ) 
 B_SPLINE_CURVE_WITH_KNOTS ( ( 3, 2, 2, 2, 3 ),
 ( 0.9017857142857143016, 0.9023809523809523947, 0.9035714285714285809, 0.9047619047619047672, 0.9053571428571428603 ),
 .UNSPECIFIED. ) 
 CURVE ( )  GEOMETRIC_REPRESENTATION_ITEM ( )  RATIONAL_B_SPLINE_CURVE ( ( 0.9330127018922194093, 0.9330127018922194093, 1.000000000000000000, 0.8660254037844387076, 1.000000000000000000, 0.8660254037844387076, 1.000000000000000000, 0.9330127018922194093, 0.9330127018922194093 ) ) 
 REPRESENTATION_ITEM ( '' )  );
#25566 = CYLINDRICAL_SURFACE ( 'NONE', #3506, 5.000000000000000000 ) ;
#25567 = CARTESIAN_POINT ( 'NONE',  ( -3.152548672688508926E-16, -63.56249999863440792, -5.148502694627439702 ) ) ;
#25568 = LINE ( 'NONE', #60317, #45871 ) ;
#25569 = CARTESIAN_POINT ( 'NONE',  ( 4.458734124999998549, 19.27083333469893134, -2.574251347313721627 ) ) ;
#25570 = AXIS2_PLACEMENT_3D ( 'NONE', #36960, #12510, #51757 ) ;
#25571 = CARTESIAN_POINT ( 'NONE',  ( -2.500000000000000444, 6.833333333333333925, -4.330127018922193649 ) ) ;
#25572 = CARTESIAN_POINT ( 'NONE',  ( -6.972266317189433020E-16, -31.12499999726880873, -5.000000000000000000 ) ) ;
#25573 = CARTESIAN_POINT ( 'NONE',  ( 2.229367062500001939, -49.22916666530107221, 3.861377020970579999 ) ) ;
#25574 = CARTESIAN_POINT ( 'NONE',  ( 2.500000000000002220, -9.541666663935483683, 4.330127018922192761 ) ) ;
#25575 = CARTESIAN_POINT ( 'NONE',  ( 1.339745962155615144, -25.58034179853029144, 4.999999999999999112 ) ) ;
#25576 = ADVANCED_FACE ( 'NONE', ( #61033 ), #26929, .T. ) ;
#25577 = CARTESIAN_POINT ( 'NONE',  ( -1.339745962155610925, -65.66965819600733312, 5.000000000000000000 ) ) ;
#25578 = CARTESIAN_POINT ( 'NONE',  ( -2.229367062500000163, -88.72916666530106511, -3.861377020970580443 ) ) ;
#25579 = CARTESIAN_POINT ( 'NONE',  ( -5.000000000000000000, 11.12500000273118594, 0.000000000000000000 ) ) ;
#25580 = CARTESIAN_POINT ( 'NONE',  ( -3.152548672688508926E-16, -17.81249999863440792, -5.148502694627439702 ) ) ;
#25581 = ORIENTED_EDGE ( 'NONE', *, *, #59025, .F. ) ;
#25582 = CARTESIAN_POINT ( 'NONE',  ( -9.184850993605147944E-16, -163.3750000027311842, 5.000000000000000000 ) ) ;
#25583 = CARTESIAN_POINT ( 'NONE',  ( 4.458734124999998549, -104.7291666653010509, -2.574251347313721627 ) ) ;
#25584 = CARTESIAN_POINT ( 'NONE',  ( -2.071067811865475061, -158.8125000027312126, -5.000000000000000888 ) ) ;
#25585 = ORIENTED_EDGE ( 'NONE', *, *, #52292, .F. ) ;
#25586 = CARTESIAN_POINT ( 'NONE',  ( -4.458734124999999437, -98.64583333196773651, -2.574251347313719407 ) ) ;
#25587 = CARTESIAN_POINT ( 'NONE',  ( 1.243387493232115550E-13, -8.250000000000003553, -5.000000000000000000 ) ) ;
#25588 = CARTESIAN_POINT ( 'NONE',  ( -2.500000000000000444, -55.04166666393548013, -4.330127018922193649 ) ) ;
#25589 = CARTESIAN_POINT ( 'NONE',  ( -5.000000000000000000, -67.08333333333332860, -2.886751345948128211 ) ) ;
#25590 = CARTESIAN_POINT ( 'NONE',  ( -53.51423613279429503, -127.2500000013656347, 4.591703134518082763 ) ) ;
#25591 = CARTESIAN_POINT ( 'NONE',  ( -58.39396692619412477, -141.4375000013656063, 2.891590998281057701 ) ) ;
#25592 = CARTESIAN_POINT ( 'NONE',  ( -3.152548672688508926E-16, -24.56249999863440792, -5.148502694627439702 ) ) ;
#25593 = CARTESIAN_POINT ( 'NONE',  ( 4.458734125000001214, 5.854166668032262599, 2.574251347313718519 ) ) ;
#25594 =( BOUNDED_CURVE ( )  B_SPLINE_CURVE ( 2, ( #32338, #62255, #33599, #51964, #3712, #52282, #58042, #28139, #3399 ),
 .UNSPECIFIED., .F., .F. ) 
 B_SPLINE_CURVE_WITH_KNOTS ( ( 3, 2, 2, 2, 3 ),
 ( 0.6520833333333333481, 0.6527777777777777901, 0.6541666666666666741, 0.6555555555555555580, 0.6562500000000000000 ),
 .UNSPECIFIED. ) 
 CURVE ( )  GEOMETRIC_REPRESENTATION_ITEM ( )  RATIONAL_B_SPLINE_CURVE ( ( 0.9330127018922194093, 0.9330127018922194093, 1.000000000000000000, 0.8660254037844387076, 1.000000000000000000, 0.8660254037844387076, 1.000000000000000000, 0.9330127018922194093, 0.9330127018922194093 ) ) 
 REPRESENTATION_ITEM ( '' )  );
#25595 = CARTESIAN_POINT ( 'NONE',  ( -4.458734124999999437, -66.64583333196773651, -2.574251347313719407 ) ) ;
#25596 = CARTESIAN_POINT ( 'NONE',  ( 1.339745962155612702, -48.16965819600734022, -5.000000000000000000 ) ) ;
#25597 = CARTESIAN_POINT ( 'NONE',  ( 2.229367062500001939, -17.97916666530106866, 3.861377020970579999 ) ) ;
#25598 = CARTESIAN_POINT ( 'NONE',  ( 2.499999999999998668, -75.33333333333332860, -4.330127018922193649 ) ) ;
#25599 = CARTESIAN_POINT ( 'NONE',  ( 5.000000000000000888, -151.9375000000000000, -2.071067811865475505 ) ) ;
#25600 = CARTESIAN_POINT ( 'NONE',  ( 1.060575238724906964E-15, -13.75000000000000000, 5.773502691896257311 ) ) ;
#25601 = CARTESIAN_POINT ( 'NONE',  ( -3.152801135295367985, -155.8125000013656063, 3.152801135295367096 ) ) ;
#25602 = EDGE_LOOP ( 'NONE', ( #56757, #24658, #33131, #2936 ) ) ;
#25603 = CARTESIAN_POINT ( 'NONE',  ( -4.458734124999999437, -46.56249999863440792, 0.000000000000000000 ) ) ;
#25604 = CARTESIAN_POINT ( 'NONE',  ( -1.339745962155613812, 25.79465819873851729, -5.000000000000000000 ) ) ;
#25605 = CARTESIAN_POINT ( 'NONE',  ( 0.000000000000000000, -170.0000000000000000, 0.000000000000000000 ) ) ;
#25606 = CARTESIAN_POINT ( 'NONE',  ( 2.500000000000002220, 29.33333333333333215, 4.330127018922192761 ) ) ;
#25607 = CARTESIAN_POINT ( 'NONE',  ( 4.458734125000001214, 3.104166668032260379, 2.574251347313718519 ) ) ;
#25608 = CARTESIAN_POINT ( 'NONE',  ( 1.339745962155615144, -93.70534180126149693, 4.999999999999999112 ) ) ;
#25609 = LINE ( 'NONE', #26566, #43012 ) ;
#25610 = CARTESIAN_POINT ( 'NONE',  ( -6.288404560131954923, -5.029641972278938944, -0.4504974108212008721 ) ) ;
#25611 = CARTESIAN_POINT ( 'NONE',  ( 4.458734124999999437, 20.93750000136559208, -5.460374474430324690E-16 ) ) ;
#25612 = CARTESIAN_POINT ( 'NONE',  ( -5.000000000000000000, -73.00000000000000000, 0.000000000000000000 ) ) ;
#25613 = CARTESIAN_POINT ( 'NONE',  ( 5.000000000000000000, 9.708333336064519870, -2.886751345948129988 ) ) ;
#25614 = EDGE_LOOP ( 'NONE', ( #17834, #25456, #43988, #13741 ) ) ;
#25615 = CARTESIAN_POINT ( 'NONE',  ( -6.972266317189433020E-16, -98.24999999999998579, -5.000000000000000000 ) ) ;
#25616 = ORIENTED_EDGE ( 'NONE', *, *, #20817, .T. ) ;
#25617 = AXIS2_PLACEMENT_3D ( 'NONE', #47083, #42247, #28085 ) ;
#25618 =( BOUNDED_CURVE ( )  B_SPLINE_CURVE ( 2, ( #32647, #61299, #17221, #17855, #31698, #2139, #51959, #61936, #1817 ),
 .UNSPECIFIED., .F., .F. ) 
 B_SPLINE_CURVE_WITH_KNOTS ( ( 3, 2, 2, 2, 3 ),
 ( 0.8089285714285714413, 0.8095238095238095344, 0.8107142857142857206, 0.8119047619047619069, 0.8125000000000000000 ),
 .UNSPECIFIED. ) 
 CURVE ( )  GEOMETRIC_REPRESENTATION_ITEM ( )  RATIONAL_B_SPLINE_CURVE ( ( 0.9330127018922194093, 0.9330127018922194093, 1.000000000000000000, 0.8660254037844387076, 1.000000000000000000, 0.8660254037844387076, 1.000000000000000000, 0.9330127018922194093, 0.9330127018922194093 ) ) 
 REPRESENTATION_ITEM ( '' )  );
#25619 = CYLINDRICAL_SURFACE ( 'NONE', #15240, 5.000000000000000000 ) ;
#25620 = CARTESIAN_POINT ( 'NONE',  ( -3.152548672688508926E-16, -41.56249999863439371, -5.148502694627439702 ) ) ;
#25621 = AXIS2_PLACEMENT_3D ( 'NONE', #32961, #8830, #33275 ) ;
#25622 = CARTESIAN_POINT ( 'NONE',  ( 2.500000000000002220, -39.54166666393548013, 4.330127018922192761 ) ) ;
#25623 = ORIENTED_EDGE ( 'NONE', *, *, #48453, .F. ) ;
#25624 = CARTESIAN_POINT ( 'NONE',  ( 4.458734124999998549, -16.72916666530107577, -2.574251347313721627 ) ) ;
#25625 = VERTEX_POINT ( 'NONE', #21469 ) ;
#25626 = CARTESIAN_POINT ( 'NONE',  ( 5.000000000000000888, -83.58333333333332860, 2.886751345948126879 ) ) ;
#25627 = CARTESIAN_POINT ( 'NONE',  ( 3.152801135295367541, -169.3125000013656063, -3.152801135295367541 ) ) ;
#25628 = CARTESIAN_POINT ( 'NONE',  ( 5.000000000000000000, -85.37499999726880162, -6.123233995736766282E-16 ) ) ;
#25630 = VERTEX_POINT ( 'NONE', #41068 ) ;
#25629 = CARTESIAN_POINT ( 'NONE',  ( -2.500000000000000444, -35.04166666393547303, -4.330127018922193649 ) ) ;
#25631 = CARTESIAN_POINT ( 'NONE',  ( -51.19402409849444524, -142.5000000000000284, -3.242614290531456334 ) ) ;
#25632 = CARTESIAN_POINT ( 'NONE',  ( 4.458734124999999437, -28.06249999863440081, -5.460374474430324690E-16 ) ) ;
#25633 = VERTEX_POINT ( 'NONE', #36259 ) ;
#25634 = EDGE_CURVE ( 'NONE', #18331, #22810, #46860, .T. ) ;
#25635 = APPLICATION_PROTOCOL_DEFINITION ( 'draft international standard', 'automotive_design', 1998, #5591 ) ;
#25636 = CARTESIAN_POINT ( 'NONE',  ( -3.152801135295367096, -164.3125000013656063, -3.152801135295367541 ) ) ;
#25637 = CARTESIAN_POINT ( 'NONE',  ( -3.152548672688508926E-16, 27.43750000136559564, -5.148502694627439702 ) ) ;
#25638 = CARTESIAN_POINT ( 'NONE',  ( -2.500000000000000444, -39.04166666393548013, -4.330127018922193649 ) ) ;
#25639 = ORIENTED_EDGE ( 'NONE', *, *, #43115, .F. ) ;
#25640 = CARTESIAN_POINT ( 'NONE',  ( -2.499999999999996447, -25.83333333333333215, 4.330127018922195425 ) ) ;
#25641 = CARTESIAN_POINT ( 'NONE',  ( -50.40829686548195099, -147.2500000013656063, -1.485763867205728284 ) ) ;
#25642 = CARTESIAN_POINT ( 'NONE',  ( 9.457646018065525792E-16, -76.31249999863439371, 5.148502694627439702 ) ) ;
#25643 = CARTESIAN_POINT ( 'NONE',  ( -51.19402409849444524, -135.6250000027312410, -3.242614290531456334 ) ) ;
#25644 = CARTESIAN_POINT ( 'NONE',  ( -4.458734124999999437, -43.39583333196773651, -2.574251347313719407 ) ) ;
#25645 = CARTESIAN_POINT ( 'NONE',  ( -4.458734125000000326, -142.1250000013656063, 1.846868145590734089 ) ) ;
#25646 = EDGE_CURVE ( 'NONE', #25453, #7221, #58399, .T. ) ;
#25647 = CARTESIAN_POINT ( 'NONE',  ( -58.24261429053147765, -155.0000000000000284, -3.805975901505573411 ) ) ;
#25648 = CARTESIAN_POINT ( 'NONE',  ( -3.152548672688508926E-16, -50.56249999863440792, -5.148502694627439702 ) ) ;
#25649 = DIRECTION ( 'NONE',  ( -0.000000000000000000, 1.000000000000000000, -0.000000000000000000 ) ) ;
#25650 = EDGE_CURVE ( 'NONE', #11315, #35606, #25329, .T. ) ;
#25651 = CARTESIAN_POINT ( 'NONE',  ( 4.458734124999999437, -16.81249999863440436, -5.460374474430324690E-16 ) ) ;
#25652 = EDGE_CURVE ( 'NONE', #15950, #40878, #9493, .T. ) ;
#25653 = CARTESIAN_POINT ( 'NONE',  ( -3.535250795749689387E-16, -100.2500000000000142, -5.773502691896257311 ) ) ;
#25654 = CARTESIAN_POINT ( 'NONE',  ( 3.061616997868383141E-16, -167.7500000000000000, -5.000000000000000000 ) ) ;
#25655 = CARTESIAN_POINT ( 'NONE',  ( 9.457646018065525792E-16, -35.31249999863440792, 5.148502694627439702 ) ) ;
#25656 = CARTESIAN_POINT ( 'NONE',  ( -2.499999999999996447, 4.291666669397852907, 4.330127018922195425 ) ) ;
#25657 = CARTESIAN_POINT ( 'NONE',  ( -6.972266317189433020E-16, -53.24999999999999289, -5.000000000000000000 ) ) ;
#25658 = CARTESIAN_POINT ( 'NONE',  ( -55.35523342533222291, -129.3125000013656063, 4.444560631937231499 ) ) ;
#25659 = CARTESIAN_POINT ( 'NONE',  ( 2.229367062500001939, -75.22916666530106511, 3.861377020970579999 ) ) ;
#25660 = EDGE_CURVE ( 'NONE', #40464, #31318, #25803, .T. ) ;
#25661 = CARTESIAN_POINT ( 'NONE',  ( -2.071067811865435981, -166.3124999999999716, 5.000000000000041744 ) ) ;
#25662 = DIRECTION ( 'NONE',  ( -0.8660254037844313801, 0.5000000000000125455, -0.000000000000000000 ) ) ;
#25663 = AXIS2_PLACEMENT_3D ( 'NONE', #48174, #47853, #32760 ) ;
#25664 = CARTESIAN_POINT ( 'NONE',  ( 2.229367062499998831, -1.895833331967737623, -3.861377020970580887 ) ) ;
#25665 = VERTEX_POINT ( 'NONE', #62611 ) ;
#25666 = CYLINDRICAL_SURFACE ( 'NONE', #4863, 5.000000000000000000 ) ;
#25667 = EDGE_CURVE ( 'NONE', #7439, #12840, #58079, .T. ) ;
#25668 = CARTESIAN_POINT ( 'NONE',  ( 2.499999999999998668, 23.79166666939785202, -4.330127018922193649 ) ) ;
#25670 = CARTESIAN_POINT ( 'NONE',  ( -4.458734124999999437, -34.31249999863440792, 0.000000000000000000 ) ) ;
#25669 = CARTESIAN_POINT ( 'NONE',  ( -2.229367062500000163, -86.47916666530107932, -3.861377020970580443 ) ) ;
#25671 = CARTESIAN_POINT ( 'NONE',  ( 2.500000000000002220, -9.666666666666664298, 4.330127018922192761 ) ) ;
#25672 = CARTESIAN_POINT ( 'NONE',  ( -4.458734124999999437, -83.56249999863439371, 0.000000000000000000 ) ) ;
#25673 = VECTOR ( 'NONE', #42684, 1000.000000000000000 ) ;
#25674 = CARTESIAN_POINT ( 'NONE',  ( 9.457646018065525792E-16, 19.68750000136559208, 5.148502694627439702 ) ) ;
#25675 = CARTESIAN_POINT ( 'NONE',  ( -6.972266317189433020E-16, -30.12499999726880873, -5.000000000000000000 ) ) ;
#25676 = CARTESIAN_POINT ( 'NONE',  ( -50.55543936806279248, -139.0625000013656063, 0.3552334253322060320 ) ) ;
#25677 = EDGE_CURVE ( 'NONE', #40725, #25930, #27862, .T. ) ;
#25678 = CARTESIAN_POINT ( 'NONE',  ( -4.458734124999999437, -6.395833331967741842, -2.574251347313719407 ) ) ;
#25679 = CARTESIAN_POINT ( 'NONE',  ( 2.229367062500001939, 22.77083333469892423, 3.861377020970579999 ) ) ;
#25680 = CARTESIAN_POINT ( 'NONE',  ( -2.229367062499996610, -48.39583333196772941, 3.861377020970582219 ) ) ;
#25681 = CARTESIAN_POINT ( 'NONE',  ( 2.500000000000002220, -105.6666666666666572, 4.330127018922192761 ) ) ;
#25682 = CARTESIAN_POINT ( 'NONE',  ( -4.458734124999998549, -85.22916666530107932, 2.574251347313722516 ) ) ;
#25683 = CARTESIAN_POINT ( 'NONE',  ( 4.458734125000000326, -4.895833331967740065, 2.574251347313718519 ) ) ;
#25684 = VERTEX_POINT ( 'NONE', #29104 ) ;
#25685 = CARTESIAN_POINT ( 'NONE',  ( -3.152548672688508926E-16, -27.81249999863440436, -5.148502694627439702 ) ) ;
#25686 = CARTESIAN_POINT ( 'NONE',  ( -54.64476657466781973, -131.0625000013656063, -4.444560631937228834 ) ) ;
#25687 = CARTESIAN_POINT ( 'NONE',  ( 9.457646018065525792E-16, -77.06249999863440792, 5.148502694627439702 ) ) ;
#25688 = CARTESIAN_POINT ( 'NONE',  ( 2.500000000000002220, -110.5416666639354730, 4.330127018922192761 ) ) ;
#25689 = CARTESIAN_POINT ( 'NONE',  ( -2.229367062499996610, 20.85416666803226349, 3.861377020970582219 ) ) ;
#25690 = CARTESIAN_POINT ( 'NONE',  ( -6.972266317189433020E-16, -28.25000000000000000, -5.000000000000000000 ) ) ;
#25691 = CARTESIAN_POINT ( 'NONE',  ( 2.229367062500001939, -76.22916666530106511, 3.861377020970579999 ) ) ;
#25692 = CARTESIAN_POINT ( 'NONE',  ( 5.000000000000000000, -57.41666666666667140, -2.886751345948129988 ) ) ;
#25693 = CARTESIAN_POINT ( 'NONE',  ( 2.499999999999998668, -36.20833333060213732, -4.330127018922193649 ) ) ;
#25694 = CARTESIAN_POINT ( 'NONE',  ( -2.500000000000000444, 25.95833333606451632, -4.330127018922193649 ) ) ;
#25695 = ORIENTED_EDGE ( 'NONE', *, *, #13801, .F. ) ;
#25696 = LINE ( 'NONE', #16038, #8861 ) ;
#25697 = CARTESIAN_POINT ( 'NONE',  ( 1.339745962155612702, -52.16965819600733312, -5.000000000000000000 ) ) ;
#25699 = CARTESIAN_POINT ( 'NONE',  ( -5.000000000000000000, -18.08333333333333570, -2.886751345948128211 ) ) ;
#25698 = CARTESIAN_POINT ( 'NONE',  ( -9.184850993605147944E-16, -149.2500000000000284, 5.000000000000000000 ) ) ;
#25700 = CARTESIAN_POINT ( 'NONE',  ( 4.458734124999998549, -23.72916666530107221, -2.574251347313721627 ) ) ;
#25701 = CARTESIAN_POINT ( 'NONE',  ( 4.458734124999998549, -85.72916666530107932, -2.574251347313721627 ) ) ;
#25702 =( BOUNDED_CURVE ( )  B_SPLINE_CURVE ( 2, ( #9770, #53842, #15575, #63196, #24901, #10099, #15245, #10419, #49010 ),
 .UNSPECIFIED., .F., .F. ) 
 B_SPLINE_CURVE_WITH_KNOTS ( ( 3, 2, 2, 2, 3 ),
 ( 0.8589285714285714857, 0.8595238095238095788, 0.8607142857142857650, 0.8619047619047619513, 0.8625000000000000444 ),
 .UNSPECIFIED. ) 
 CURVE ( )  GEOMETRIC_REPRESENTATION_ITEM ( )  RATIONAL_B_SPLINE_CURVE ( ( 0.9330127018922194093, 0.9330127018922256266, 1.000000000000000000, 0.8660254037844387076, 1.000000000000000000, 0.8660254037844387076, 1.000000000000000000, 0.9330127018922194093, 0.9330127018922194093 ) ) 
 REPRESENTATION_ITEM ( '' )  );
#25703 = CARTESIAN_POINT ( 'NONE',  ( -2.500000000000000444, -21.04166666393548013, -4.330127018922193649 ) ) ;
#25705 = ORIENTED_EDGE ( 'NONE', *, *, #5596, .F. ) ;
#25704 = CARTESIAN_POINT ( 'NONE',  ( -2.229367062499996610, -53.14583333196773651, 3.861377020970582219 ) ) ;
#25706 = CARTESIAN_POINT ( 'NONE',  ( 5.000000000000000000, -65.41666666666667140, -2.886751345948130876 ) ) ;
#25707 = DIRECTION ( 'NONE',  ( -0.000000000000000000, 1.000000000000000000, -0.000000000000000000 ) ) ;
#25709 = ORIENTED_EDGE ( 'NONE', *, *, #4707, .T. ) ;
#25708 = CARTESIAN_POINT ( 'NONE',  ( 4.458734125000001214, -2.145833331967737845, 2.574251347313718519 ) ) ;
#25710 = CARTESIAN_POINT ( 'NONE',  ( -53.51423613279429503, -151.2500000013656063, 4.591703134518083651 ) ) ;
#25711 = CARTESIAN_POINT ( 'NONE',  ( 5.000000000000000000, -67.50000000000000000, -6.123233995736766282E-16 ) ) ;
#25712 = CARTESIAN_POINT ( 'NONE',  ( -1.846868145590734756, -151.3750000013656063, -4.458734125000000326 ) ) ;
#25713 = AXIS2_PLACEMENT_3D ( 'NONE', #58335, #38089, #13640 ) ;
#25714 = CARTESIAN_POINT ( 'NONE',  ( -4.458734124999999437, -44.56249999863440081, 0.000000000000000000 ) ) ;
#25715 = CARTESIAN_POINT ( 'NONE',  ( -2.499999999999996447, -76.70833333060214443, 4.330127018922195425 ) ) ;
#25716 = CARTESIAN_POINT ( 'NONE',  ( -2.071067811865478170, -158.3125000000000284, 5.000000000000000000 ) ) ;
#25717 = CYLINDRICAL_SURFACE ( 'NONE', #34374, 5.000000000000000000 ) ;
#25718 = VECTOR ( 'NONE', #27351, 1000.000000000000000 ) ;
#25719 = CARTESIAN_POINT ( 'NONE',  ( -52.80376928212989185, -125.1250000013656205, -4.297418129356379346 ) ) ;
#25720 = CARTESIAN_POINT ( 'NONE',  ( -2.229367062499996610, -13.39583333196774007, 3.861377020970582219 ) ) ;
#25721 = CARTESIAN_POINT ( 'NONE',  ( 4.458734124999999437, -52.06249999863440792, -5.460374474430324690E-16 ) ) ;
#25722 =( BOUNDED_CURVE ( )  B_SPLINE_CURVE ( 2, ( #2940, #56339, #22233, #61477, #8076, #17411, #46992, #3258, #37026 ),
 .UNSPECIFIED., .F., .F. ) 
 B_SPLINE_CURVE_WITH_KNOTS ( ( 3, 2, 2, 2, 3 ),
 ( 0.6083333333333329485, 0.6124999999999997113, 0.6166666666666663632, 0.6208333333333330151, 0.6249999999999996669 ),
 .UNSPECIFIED. ) 
 CURVE ( )  GEOMETRIC_REPRESENTATION_ITEM ( )  RATIONAL_B_SPLINE_CURVE ( ( 1.000000000000005995, 0.9238795325112806323, 1.000000000000000000, 0.9238795325112867385, 1.000000000000000000, 0.9238795325112867385, 1.000000000000000000, 0.9238795325112928447, 0.9999999999999938938 ) ) 
 REPRESENTATION_ITEM ( '' )  );
#25723 = CARTESIAN_POINT ( 'NONE',  ( 4.458734124999999437, -144.5000000013656063, 1.846868145590737864 ) ) ;
#25724 = CARTESIAN_POINT ( 'NONE',  ( 4.458734124999999437, -96.06249999863440792, -5.460374474430324690E-16 ) ) ;
#25725 = CARTESIAN_POINT ( 'NONE',  ( -1.339745962155601378, 20.91965820146970501, -5.000000000000007105 ) ) ;
#25726 = ORIENTED_EDGE ( 'NONE', *, *, #48430, .F. ) ;
#25727 = CYLINDRICAL_SURFACE ( 'NONE', #25210, 5.000000000000000000 ) ;
#25728 = CARTESIAN_POINT ( 'NONE',  ( 4.458734124999998549, 26.02083333469892779, -2.574251347313721627 ) ) ;
#25729 = CARTESIAN_POINT ( 'NONE',  ( -51.19402409849444524, -147.6250000027312126, -3.242614290531456334 ) ) ;
#25730 = CYLINDRICAL_SURFACE ( 'NONE', #25030, 5.000000000000000000 ) ;
#25731 = ORIENTED_EDGE ( 'NONE', *, *, #38859, .T. ) ;
#25732 = CARTESIAN_POINT ( 'NONE',  ( -4.458734124999999437, -3.395833331967739177, -2.574251347313719407 ) ) ;
#25733 = CARTESIAN_POINT ( 'NONE',  ( 1.975475456537005874E-15, -106.7499999999999858, 5.000000000000000000 ) ) ;
#25734 = CARTESIAN_POINT ( 'NONE',  ( -4.458734124999999437, -19.56249999863440081, 0.000000000000000000 ) ) ;
#25735 = CYLINDRICAL_SURFACE ( 'NONE', #7604, 5.000000000000000000 ) ;
#25736 = CARTESIAN_POINT ( 'NONE',  ( 4.458734124999999437, -5.812499998634403475, -5.460374474430324690E-16 ) ) ;
#25737 = CARTESIAN_POINT ( 'NONE',  ( 7.848314987057850800, -4.129027267381569999, -7.493854785173811095 ) ) ;
#25738 = CARTESIAN_POINT ( 'NONE',  ( -1.846868145590734756, -149.1250000013656063, -4.458734124999999437 ) ) ;
#25739 = CARTESIAN_POINT ( 'NONE',  ( -3.152548672688508926E-16, 13.18750000136559208, -5.148502694627439702 ) ) ;
#25740 = VERTEX_POINT ( 'NONE', #9191 ) ;
#25741 = CARTESIAN_POINT ( 'NONE',  ( -2.500000000000000444, -27.04166666393548013, -4.330127018922193649 ) ) ;
#25742 = CARTESIAN_POINT ( 'NONE',  ( -2.499999999999996447, -12.83333333333333570, 4.330127018922195425 ) ) ;
#25743 = CARTESIAN_POINT ( 'NONE',  ( 4.458734124999998549, -17.72916666530106866, -2.574251347313721627 ) ) ;
#25744 = CARTESIAN_POINT ( 'NONE',  ( 1.339745962155612702, 1.830341803992665772, -5.000000000000000000 ) ) ;
#25745 = CARTESIAN_POINT ( 'NONE',  ( -50.55543936806279248, -151.0625000013656063, 0.3552334253322060320 ) ) ;
#25746 = EDGE_CURVE ( 'NONE', #18873, #12181, #3189, .T. ) ;
#25747 = CARTESIAN_POINT ( 'NONE',  ( -5.000000000000000000, -48.95833333060213732, -2.886751345948128211 ) ) ;
#25748 = CYLINDRICAL_SURFACE ( 'NONE', #50780, 5.000000000000000000 ) ;
#25749 = CARTESIAN_POINT ( 'NONE',  ( 2.229367062500001939, 14.02083333469892779, 3.861377020970579999 ) ) ;
#25750 = CARTESIAN_POINT ( 'NONE',  ( 0.000000000000000000, -120.0000000000000000, 0.000000000000000000 ) ) ;
#25751 = CARTESIAN_POINT ( 'NONE',  ( 5.000000000000000888, 9.416666666666666075, 2.886751345948126879 ) ) ;
#25752 = CARTESIAN_POINT ( 'NONE',  ( 2.229367062500001939, 10.02083333469892779, 3.861377020970579999 ) ) ;
#25753 = CARTESIAN_POINT ( 'NONE',  ( -4.458734124999998549, -65.22916666530106511, 2.574251347313722516 ) ) ;
#25754 = ORIENTED_EDGE ( 'NONE', *, *, #55138, .T. ) ;
#25755 = VECTOR ( 'NONE', #63251, 1000.000000000000000 ) ;
#25756 = CARTESIAN_POINT ( 'NONE',  ( 9.457646018065525792E-16, -14.31249999863440614, 5.148502694627439702 ) ) ;
#25757 = CARTESIAN_POINT ( 'NONE',  ( 5.000000000000000000, 6.583333333333333037, -2.886751345948129988 ) ) ;
#25758 = CARTESIAN_POINT ( 'NONE',  ( 1.846868145590735200, -165.2500000013655779, -4.458734125000000326 ) ) ;
#25759 = CARTESIAN_POINT ( 'NONE',  ( -6.972266317189433020E-16, 21.75000000000000000, -5.000000000000000000 ) ) ;
#25760 = VECTOR ( 'NONE', #29224, 1000.000000000000000 ) ;
#25761 = CARTESIAN_POINT ( 'NONE',  ( -4.458734124999998549, -57.22916666530107932, 2.574251347313722516 ) ) ;
#25762 = CARTESIAN_POINT ( 'NONE',  ( 1.060575238724906964E-15, -95.62499999726881583, 5.773502691896257311 ) ) ;
#25763 = CARTESIAN_POINT ( 'NONE',  ( -4.458734124999999437, -33.39583333196772941, -2.574251347313719407 ) ) ;
#25764 = CARTESIAN_POINT ( 'NONE',  ( -5.000000000000000000, -41.95833333060214443, -2.886751345948128211 ) ) ;
#25765 = DIRECTION ( 'NONE',  ( 0.8660254037844385966, 0.5000000000000001110, 0.000000000000000000 ) ) ;
#25766 = CARTESIAN_POINT ( 'NONE',  ( 6.123233995736766282E-16, -170.0000000000000000, -5.000000000000000000 ) ) ;
#25767 = CARTESIAN_POINT ( 'NONE',  ( -75.00000000000001421, 15.00000000000000000, -9.000000000000001776 ) ) ;
#25768 = CARTESIAN_POINT ( 'NONE',  ( 1.846868145590736310, -149.8750000013655779, 4.458734124999997661 ) ) ;
#25769 = CARTESIAN_POINT ( 'NONE',  ( -5.000000000000000000, -42.08333333333333570, -2.886751345948128211 ) ) ;
#25770 = CARTESIAN_POINT ( 'NONE',  ( -2.500000000000000444, -14.16666666666666785, -4.330127018922193649 ) ) ;
#25771 = CARTESIAN_POINT ( 'NONE',  ( -9.184850993605147944E-16, -156.3750000027311842, 5.000000000000000000 ) ) ;
#25772 = ORIENTED_EDGE ( 'NONE', *, *, #38200, .T. ) ;
#25773 = CARTESIAN_POINT ( 'NONE',  ( -4.458734124999999437, -106.3124999986343937, 0.000000000000000000 ) ) ;
#25774 = CARTESIAN_POINT ( 'NONE',  ( 4.458734124999998549, 3.020833334698928674, -2.574251347313721627 ) ) ;
#25775 =( BOUNDED_CURVE ( )  B_SPLINE_CURVE ( 2, ( #34070, #9625, #29233, #19908, #39841, #59484, #310, #24426, #39207 ),
 .UNSPECIFIED., .F., .F. ) 
 B_SPLINE_CURVE_WITH_KNOTS ( ( 3, 2, 2, 2, 3 ),
 ( 0.3839285714285714524, 0.3845238095238095455, 0.3857142857142857317, 0.3869047619047619180, 0.3875000000000000111 ),
 .UNSPECIFIED. ) 
 CURVE ( )  GEOMETRIC_REPRESENTATION_ITEM ( )  RATIONAL_B_SPLINE_CURVE ( ( 0.9330127018922194093, 0.9330127018922194093, 1.000000000000000000, 0.8660254037844387076, 1.000000000000000000, 0.8660254037844387076, 1.000000000000000000, 0.9330127018922194093, 0.9330127018922194093 ) ) 
 REPRESENTATION_ITEM ( '' )  );
#25776 = CARTESIAN_POINT ( 'NONE',  ( -2.500000000000000444, -97.04166666393545881, -4.330127018922193649 ) ) ;
#25777 = CARTESIAN_POINT ( 'NONE',  ( -2.499999999999996447, -3.833333333333334370, 4.330127018922195425 ) ) ;
#25778 = CARTESIAN_POINT ( 'NONE',  ( 9.457646018065525792E-16, -67.06249999863440792, 5.148502694627439702 ) ) ;
#25779 = CARTESIAN_POINT ( 'NONE',  ( 5.000000000000000000, -22.29166666393548013, -2.886751345948130876 ) ) ;
#25780 = CARTESIAN_POINT ( 'NONE',  ( 2.500000000000002220, -9.541666663935483683, 4.330127018922192761 ) ) ;
#25782 = ORIENTED_EDGE ( 'NONE', *, *, #33982, .T. ) ;
#25781 = CARTESIAN_POINT ( 'NONE',  ( -2.229367062500000163, -33.47916666530107221, -3.861377020970580443 ) ) ;
#25783 = CARTESIAN_POINT ( 'NONE',  ( -4.999999999999998224, -77.91666666666665719, 2.886751345948131764 ) ) ;
#25784 = CYLINDRICAL_SURFACE ( 'NONE', #54922, 5.000000000000000000 ) ;
#25786 = VERTEX_POINT ( 'NONE', #57779 ) ;
#25785 = CARTESIAN_POINT ( 'NONE',  ( -2.229367062499996610, 11.60416666803225993, 3.861377020970582219 ) ) ;
#25787 = CARTESIAN_POINT ( 'NONE',  ( -58.80597590150559739, -141.1250000027312126, 3.242614290531460330 ) ) ;
#25788 = CARTESIAN_POINT ( 'NONE',  ( 1.060575238724906964E-15, -52.75000000000000000, 5.773502691896257311 ) ) ;
#25789 = CARTESIAN_POINT ( 'NONE',  ( -4.458734124999999437, -32.64583333196774362, -2.574251347313719407 ) ) ;
#25790 = DIRECTION ( 'NONE',  ( -0.000000000000000000, 1.000000000000000000, -0.000000000000000000 ) ) ;
#25791 = CARTESIAN_POINT ( 'NONE',  ( -4.458734124999999437, -73.31249999863439371, 0.000000000000000000 ) ) ;
#25792 = CARTESIAN_POINT ( 'NONE',  ( 4.458734124999999437, -139.7500000013655779, 1.846868145590737864 ) ) ;
#25793 = CARTESIAN_POINT ( 'NONE',  ( 2.229367062500001939, -83.97916666530106511, 3.861377020970579999 ) ) ;
#25794 = CARTESIAN_POINT ( 'NONE',  ( -52.80376928212989185, -135.1250000013656063, -4.297418129356379346 ) ) ;
#25795 = CARTESIAN_POINT ( 'NONE',  ( -2.229367062499996610, -37.39583333196773651, 3.861377020970582219 ) ) ;
#25796 = ORIENTED_EDGE ( 'NONE', *, *, #62983, .T. ) ;
#25797 = CARTESIAN_POINT ( 'NONE',  ( -4.999999999999998224, -82.79166666393547303, 2.886751345948131764 ) ) ;
#25798 = EDGE_LOOP ( 'NONE', ( #17774, #46669, #26954, #40837 ) ) ;
#25799 = CARTESIAN_POINT ( 'NONE',  ( 9.457646018065525792E-16, -78.31249999863442213, 5.148502694627439702 ) ) ;
#25800 = EDGE_LOOP ( 'NONE', ( #29951, #37130, #18876, #56641 ) ) ;
#25801 = CARTESIAN_POINT ( 'NONE',  ( -1.339745962155613812, -15.08034179853029322, -5.000000000000000000 ) ) ;
#25802 =( BOUNDED_CURVE ( )  B_SPLINE_CURVE ( 2, ( #62872, #15795, #13964, #63185, #19424, #38714, #58353, #53523, #1025 ),
 .UNSPECIFIED., .F., .F. ) 
 B_SPLINE_CURVE_WITH_KNOTS ( ( 3, 2, 2, 2, 3 ),
 ( 0.4583333333333337589, 0.4625000000000004663, 0.4666666666666671182, 0.4708333333333337700, 0.4750000000000004219 ),
 .UNSPECIFIED. ) 
 CURVE ( )  GEOMETRIC_REPRESENTATION_ITEM ( )  RATIONAL_B_SPLINE_CURVE ( ( 0.9999999999999918954, 0.9238795325112948431, 1.000000000000000000, 0.9238795325112867385, 1.000000000000000000, 0.9238795325112867385, 1.000000000000000000, 0.9238795325112786339, 1.000000000000008216 ) ) 
 REPRESENTATION_ITEM ( '' )  );
#25803 = CIRCLE ( 'NONE', #46374, 7.500000000000001776 ) ;
#25804 = CARTESIAN_POINT ( 'NONE',  ( -4.458734124999999437, -62.64583333196774362, -2.574251347313719407 ) ) ;
#25805 = CARTESIAN_POINT ( 'NONE',  ( -4.458734124999998549, -3.479166665301069994, 2.574251347313722516 ) ) ;
#25806 = ORIENTED_EDGE ( 'NONE', *, *, #58253, .T. ) ;
#25807 = CARTESIAN_POINT ( 'NONE',  ( -6.972266317189433020E-16, 4.875000002731184168, -5.000000000000000000 ) ) ;
#25808 = CARTESIAN_POINT ( 'NONE',  ( -2.498395430326213474E-14, 16.24999999999999645, 5.000000000000000000 ) ) ;
#25809 = CARTESIAN_POINT ( 'NONE',  ( 4.458734124999998549, 8.270833334698926009, -2.574251347313721627 ) ) ;
#25810 = CARTESIAN_POINT ( 'NONE',  ( -57.89159099828107458, -139.6875000013656063, -3.393966926194107447 ) ) ;
#25811 = CARTESIAN_POINT ( 'NONE',  ( -6.972266317189433020E-16, -1.250000000000000000, -5.000000000000000000 ) ) ;
#25812 = CARTESIAN_POINT ( 'NONE',  ( 1.846868145590736310, -159.6250000013655779, 4.458734124999997661 ) ) ;
#25813 = CARTESIAN_POINT ( 'NONE',  ( 6.123233995736766282E-16, -170.0000000000000000, -5.000000000000000000 ) ) ;
#25814 = VERTEX_POINT ( 'NONE', #37841 ) ;
#25815 = CARTESIAN_POINT ( 'NONE',  ( 2.229367062499998831, -79.64583333196773651, -3.861377020970580887 ) ) ;
#25816 = CARTESIAN_POINT ( 'NONE',  ( -4.999999999999998224, -96.91666666666665719, 2.886751345948131764 ) ) ;
#25817 = CARTESIAN_POINT ( 'NONE',  ( -3.152548672688508926E-16, -1.562499998634406140, -5.148502694627439702 ) ) ;
#25818 = CARTESIAN_POINT ( 'NONE',  ( 5.000000000000000888, -71.45833333060214443, 2.886751345948126879 ) ) ;
#25819 = FACE_OUTER_BOUND ( 'NONE', #39196, .T. ) ;
#25820 = CARTESIAN_POINT ( 'NONE',  ( -4.458734124999999437, -68.56249999863439371, 0.000000000000000000 ) ) ;
#25821 = CARTESIAN_POINT ( 'NONE',  ( 5.000000000000000000, -33.37499999726880873, -6.123233995736766282E-16 ) ) ;
#25822 = CARTESIAN_POINT ( 'NONE',  ( -5.000000000000000000, -20.99999999999999645, 0.000000000000000000 ) ) ;
#25823 = CARTESIAN_POINT ( 'NONE',  ( 5.000000000000000000, -78.29166666393547303, -2.886751345948130876 ) ) ;
#25824 = CARTESIAN_POINT ( 'NONE',  ( -2.229367062499996610, 26.85416666803225993, 3.861377020970582219 ) ) ;
#25825 = CARTESIAN_POINT ( 'NONE',  ( -4.458734124999999437, -52.31249999863440792, 0.000000000000000000 ) ) ;
#25826 = CARTESIAN_POINT ( 'NONE',  ( 4.458734124999998549, -30.97916666530106866, -2.574251347313721627 ) ) ;
#25827 = CARTESIAN_POINT ( 'NONE',  ( 2.229367062500001939, 3.770833334698926009, 3.861377020970579999 ) ) ;
#25828 = CARTESIAN_POINT ( 'NONE',  ( -2.500000000000000444, 21.83333333333333215, -4.330127018922193649 ) ) ;
#25829 = CARTESIAN_POINT ( 'NONE',  ( -3.535533905932738641, -144.5000000027311842, 3.535533905932737309 ) ) ;
#25830 = FACE_OUTER_BOUND ( 'NONE', #61689, .T. ) ;
#25831 = CARTESIAN_POINT ( 'NONE',  ( -4.458734124999998549, -42.22916666530107932, 2.574251347313722516 ) ) ;
#25832 = CARTESIAN_POINT ( 'NONE',  ( 2.500000000000002220, -79.54166666393547303, 4.330127018922192761 ) ) ;
#25833 = CARTESIAN_POINT ( 'NONE',  ( -54.64476657466781973, -143.0625000013656063, -4.444560631937228834 ) ) ;
#25834 = FACE_OUTER_BOUND ( 'NONE', #15499, .T. ) ;
#25835 = CARTESIAN_POINT ( 'NONE',  ( 5.000000000000000000, 3.499999999999999556, -6.123233995736766282E-16 ) ) ;
#25836 = CARTESIAN_POINT ( 'NONE',  ( 4.458734124999998549, -77.97916666530106511, -2.574251347313721627 ) ) ;
#25837 = CARTESIAN_POINT ( 'NONE',  ( 3.152801135295366208, -161.8125000013656063, 3.152801135295367985 ) ) ;
#25838 = CARTESIAN_POINT ( 'NONE',  ( 2.500000000000002220, 7.333333333333333925, 4.330127018922192761 ) ) ;
#25839 = CARTESIAN_POINT ( 'NONE',  ( 5.000000000000000888, -28.58333333333333570, 2.886751345948126879 ) ) ;
#25840 = DIRECTION ( 'NONE',  ( -0.6485228581062915110, 0.000000000000000000, -0.7611951803011149931 ) ) ;
#25841 = VERTEX_POINT ( 'NONE', #57474 ) ;
#25842 = CARTESIAN_POINT ( 'NONE',  ( 4.458734124999998549, 24.02083333469892423, -2.574251347313721627 ) ) ;
#25843 = ORIENTED_EDGE ( 'NONE', *, *, #24937, .F. ) ;
#25844 = CARTESIAN_POINT ( 'NONE',  ( 2.229367062499998831, -64.89583333196773651, -3.861377020970580887 ) ) ;
#25845 = CARTESIAN_POINT ( 'NONE',  ( 2.499999999999998668, 20.79166666939784847, -4.330127018922193649 ) ) ;
#25846 = CARTESIAN_POINT ( 'NONE',  ( 2.500000000000002220, 2.333333333333333037, 4.330127018922192761 ) ) ;
#25847 = CARTESIAN_POINT ( 'NONE',  ( 5.000000000000000888, 14.41666666666666785, 2.886751345948126879 ) ) ;
#25848 = EDGE_CURVE ( 'NONE', #50923, #38994, #31555, .T. ) ;
#25849 = CARTESIAN_POINT ( 'NONE',  ( 4.458734124999999437, -51.81249999863440792, -5.460374474430324690E-16 ) ) ;
#25850 = CARTESIAN_POINT ( 'NONE',  ( 4.458734125000001214, -9.895833331967736513, 2.574251347313718519 ) ) ;
#25851 = CARTESIAN_POINT ( 'NONE',  ( 7.500000000000000000, 0.7723602884954153813, -7.026388801733942202 ) ) ;
#25852 = DIRECTION ( 'NONE',  ( 0.000000000000000000, 0.000000000000000000, 1.000000000000000000 ) ) ;
#25853 = CARTESIAN_POINT ( 'NONE',  ( -1.339745962155610925, -63.79465819873851729, 5.000000000000000000 ) ) ;
#25854 = CARTESIAN_POINT ( 'NONE',  ( 0.000000000000000000, -170.0000000000000000, 5.000000000000000000 ) ) ;
#25855 = CARTESIAN_POINT ( 'NONE',  ( -2.500000000000000444, -32.16666666666666430, -4.330127018922193649 ) ) ;
#25856 = CARTESIAN_POINT ( 'NONE',  ( 1.339745962155615144, -66.58034179853028434, 4.999999999999999112 ) ) ;
#25858 = CARTESIAN_POINT ( 'NONE',  ( -4.458734124999999437, -12.56249999863440259, 0.000000000000000000 ) ) ;
#25857 = CARTESIAN_POINT ( 'NONE',  ( -6.972266317189433020E-16, 21.87500000273118417, -5.000000000000000000 ) ) ;
#25859 = CARTESIAN_POINT ( 'NONE',  ( -54.60164318462004474, -135.5000000027312126, -4.984105922594373794 ) ) ;
#25860 = CARTESIAN_POINT ( 'NONE',  ( 9.457646018065525792E-16, -58.06249999863440081, 5.148502694627439702 ) ) ;
#25861 = CARTESIAN_POINT ( 'NONE',  ( -3.152801135295367985, -150.0625000013655779, 3.152801135295367096 ) ) ;
#25862 = CARTESIAN_POINT ( 'NONE',  ( -2.229367062500000163, -64.47916666530106511, -3.861377020970580443 ) ) ;
#25863 = ADVANCED_FACE ( 'NONE', ( #63545 ), #47791, .F. ) ;
#25864 = CARTESIAN_POINT ( 'NONE',  ( -2.499999999999996447, -54.70833333060213732, 4.330127018922195425 ) ) ;
#25865 = ORIENTED_EDGE ( 'NONE', *, *, #49593, .F. ) ;
#25866 = CARTESIAN_POINT ( 'NONE',  ( -5.926426369611017623E-15, 25.37500000273118062, 5.000000000000000000 ) ) ;
#25867 = CARTESIAN_POINT ( 'NONE',  ( -3.152548672688508926E-16, -1.812499998634406362, -5.148502694627439702 ) ) ;
#25868 = VERTEX_POINT ( 'NONE', #32695 ) ;
#25870 = DIRECTION ( 'NONE',  ( -0.000000000000000000, 1.000000000000000000, -0.000000000000000000 ) ) ;
#25869 = CARTESIAN_POINT ( 'NONE',  ( -6.972266317189433020E-16, -21.24999999999999289, -5.000000000000000000 ) ) ;
#25871 = CARTESIAN_POINT ( 'NONE',  ( 4.458734125000000326, -158.3750000013655779, -1.846868145590734978 ) ) ;
#25872 = ORIENTED_EDGE ( 'NONE', *, *, #55147, .T. ) ;
#25873 = FACE_OUTER_BOUND ( 'NONE', #61043, .T. ) ;
#25874 = CARTESIAN_POINT ( 'NONE',  ( -52.53715891517739323, -129.4375000000000568, -4.819101127000233298 ) ) ;
#25875 = LINE ( 'NONE', #45491, #49844 ) ;
#25876 = CARTESIAN_POINT ( 'NONE',  ( 4.458734125000001214, -46.14583333196773651, 2.574251347313718519 ) ) ;
#25877 = ORIENTED_EDGE ( 'NONE', *, *, #22246, .F. ) ;
#25878 = CARTESIAN_POINT ( 'NONE',  ( -2.500000000000000444, 16.95833333606451987, -4.330127018922193649 ) ) ;
#25879 = CARTESIAN_POINT ( 'NONE',  ( -4.458734124999999437, 15.68750000136559564, 0.000000000000000000 ) ) ;
#25880 = CARTESIAN_POINT ( 'NONE',  ( 2.229367062499998831, 25.35416666803225993, -3.861377020970580887 ) ) ;
#25881 = CARTESIAN_POINT ( 'NONE',  ( -57.89159099828107458, -153.6875000013656063, -3.393966926194107447 ) ) ;
#25882 = DIRECTION ( 'NONE',  ( -0.000000000000000000, 1.000000000000000000, -0.000000000000000000 ) ) ;
#25883 = CARTESIAN_POINT ( 'NONE',  ( -1.339745962155613812, -36.08034179853029144, -5.000000000000000000 ) ) ;
#25884 = ORIENTED_EDGE ( 'NONE', *, *, #27958, .T. ) ;
#25885 = CARTESIAN_POINT ( 'NONE',  ( 2.229367062499998831, -63.64583333196772941, -3.861377020970580887 ) ) ;
#25886 = CARTESIAN_POINT ( 'NONE',  ( 5.000000000000000000, -28.37499999726881228, -6.123233995736766282E-16 ) ) ;
#25887 = CARTESIAN_POINT ( 'NONE',  ( 2.229367062500001939, 12.02083333469892601, 3.861377020970579999 ) ) ;
#25888 =( BOUNDED_CURVE ( )  B_SPLINE_CURVE ( 2, ( #19125, #43258, #23964, #24599, #43567, #34546, #39064, #13992, #44205 ),
 .UNSPECIFIED., .F., .F. ) 
 B_SPLINE_CURVE_WITH_KNOTS ( ( 3, 2, 2, 2, 3 ),
 ( 0.5875000000000000222, 0.5880952380952381153, 0.5892857142857143016, 0.5904761904761904878, 0.5910714285714285809 ),
 .UNSPECIFIED. ) 
 CURVE ( )  GEOMETRIC_REPRESENTATION_ITEM ( )  RATIONAL_B_SPLINE_CURVE ( ( 0.9330127018922194093, 0.9330127018922194093, 1.000000000000000000, 0.8660254037844387076, 1.000000000000000000, 0.8660254037844387076, 1.000000000000000000, 0.9330127018922194093, 0.9330127018922194093 ) ) 
 REPRESENTATION_ITEM ( '' )  );
#25889 = FACE_OUTER_BOUND ( 'NONE', #31424, .T. ) ;
#25890 = CARTESIAN_POINT ( 'NONE',  ( -4.458734124999999437, -56.56249999863440081, 0.000000000000000000 ) ) ;
#25891 = CARTESIAN_POINT ( 'NONE',  ( -2.499999999999996447, -12.70833333060214798, 4.330127018922195425 ) ) ;
#25892 = CYLINDRICAL_SURFACE ( 'NONE', #28371, 5.000000000000000000 ) ;
#25893 = DIRECTION ( 'NONE',  ( -0.000000000000000000, 1.000000000000000000, -0.000000000000000000 ) ) ;
#25894 = CARTESIAN_POINT ( 'NONE',  ( -1.339745962155613812, 14.79465819873851906, -5.000000000000000000 ) ) ;
#25895 = LINE ( 'NONE', #21076, #54206 ) ;
#25896 = CARTESIAN_POINT ( 'NONE',  ( -4.458734124999999437, -17.56249999863440792, 0.000000000000000000 ) ) ;
#25897 = VERTEX_POINT ( 'NONE', #37519 ) ;
#25898 = CARTESIAN_POINT ( 'NONE',  ( 5.000000000000000888, 23.41666666666666430, 2.886751345948126879 ) ) ;
#25899 = CARTESIAN_POINT ( 'NONE',  ( -4.458734124999999437, -104.3958333319677365, -2.574251347313719407 ) ) ;
#25900 = CARTESIAN_POINT ( 'NONE',  ( 5.000000000000000000, -156.1250000027311842, 0.000000000000000000 ) ) ;
#25901 = ORIENTED_EDGE ( 'NONE', *, *, #26824, .T. ) ;
#25902 = CARTESIAN_POINT ( 'NONE',  ( 9.457646018065525792E-16, -101.3124999986344079, 5.148502694627439702 ) ) ;
#25903 = CARTESIAN_POINT ( 'NONE',  ( 4.458734124999999437, -24.81249999863440436, -5.460374474430324690E-16 ) ) ;
#25904 = CARTESIAN_POINT ( 'NONE',  ( 5.000000000000000888, -56.45833333060213732, 2.886751345948126879 ) ) ;
#25905 = CARTESIAN_POINT ( 'NONE',  ( -52.10840900171896806, -125.1875000013656063, 3.393966926194110556 ) ) ;
#25906 = CARTESIAN_POINT ( 'NONE',  ( -52.10840900171896806, -143.1875000013656063, 3.393966926194110556 ) ) ;
#25907 = CARTESIAN_POINT ( 'NONE',  ( 9.457646018065525792E-16, -26.06249999863440792, 5.148502694627439702 ) ) ;
#25908 = CARTESIAN_POINT ( 'NONE',  ( -4.458734124999999437, -63.56249999863440792, 0.000000000000000000 ) ) ;
#25909 = CARTESIAN_POINT ( 'NONE',  ( 1.339745962155641346, 8.705341801261479162, -4.999999999999983125 ) ) ;
#25910 = CARTESIAN_POINT ( 'NONE',  ( 4.458734125000000326, -19.89583333196774007, 2.574251347313718519 ) ) ;
#25911 = CARTESIAN_POINT ( 'NONE',  ( 1.975475456537005874E-15, -79.62499999726881583, 5.000000000000000000 ) ) ;
#25912 = CARTESIAN_POINT ( 'NONE',  ( 2.071067811865475505, -152.8125000000000284, -5.000000000000000888 ) ) ;
#25913 = CARTESIAN_POINT ( 'NONE',  ( -2.500000000000000444, -9.166666666666662522, -4.330127018922193649 ) ) ;
#25914 = CARTESIAN_POINT ( 'NONE',  ( 2.730187237215162345E-16, -150.1875000013656063, -4.458734124999999437 ) ) ;
#25915 = ORIENTED_EDGE ( 'NONE', *, *, #25532, .F. ) ;
#25916 = CARTESIAN_POINT ( 'NONE',  ( -4.458734124999999437, -48.64583333196773651, -2.574251347313719407 ) ) ;
#25917 = DIRECTION ( 'NONE',  ( -0.000000000000000000, 1.000000000000000000, -0.000000000000000000 ) ) ;
#25918 = CARTESIAN_POINT ( 'NONE',  ( -7.298354728638373423, 4.926141412641537265, -7.913704048100170141 ) ) ;
#25919 = CARTESIAN_POINT ( 'NONE',  ( 5.000000000000000000, 27.58333333333332860, -2.886751345948129988 ) ) ;
#25920 = EDGE_CURVE ( 'NONE', #51356, #53696, #62294, .T. ) ;
#25921 = CARTESIAN_POINT ( 'NONE',  ( 4.458734125000001214, 2.104166668032262599, 2.574251347313718519 ) ) ;
#25922 = CARTESIAN_POINT ( 'NONE',  ( -5.000000000000000000, -73.87499999726880162, 0.000000000000000000 ) ) ;
#25923 = CARTESIAN_POINT ( 'NONE',  ( 5.000000000000000000, -41.37499999726880162, -6.123233995736766282E-16 ) ) ;
#25924 = CARTESIAN_POINT ( 'NONE',  ( -6.972266317189433020E-16, -86.12499999726880162, -5.000000000000000000 ) ) ;
#25925 = CARTESIAN_POINT ( 'NONE',  ( -4.458734124999999437, 13.43750000136559386, 0.000000000000000000 ) ) ;
#25926 = CARTESIAN_POINT ( 'NONE',  ( -2.500000000000000444, -80.16666666666665719, -4.330127018922193649 ) ) ;
#25927 = CARTESIAN_POINT ( 'NONE',  ( 1.060575238724906964E-15, 10.37500000273118594, 5.773502691896257311 ) ) ;
#25928 = ORIENTED_EDGE ( 'NONE', *, *, #62273, .F. ) ;
#25929 = CARTESIAN_POINT ( 'NONE',  ( -5.000000000000000000, 8.000000000000000000, 0.000000000000000000 ) ) ;
#25930 = VERTEX_POINT ( 'NONE', #23370 ) ;
#25931 = CARTESIAN_POINT ( 'NONE',  ( 2.500000000000002220, -85.66666666666667140, 4.330127018922192761 ) ) ;
#25932 = CARTESIAN_POINT ( 'NONE',  ( 4.458734125000001214, -43.89583333196775072, 2.574251347313718519 ) ) ;
#25933 = CARTESIAN_POINT ( 'NONE',  ( -8.190561711645485556E-16, -165.9375000013655779, 4.458734124999999437 ) ) ;
#25934 = ADVANCED_FACE ( 'NONE', ( #23982 ), #33322, .F. ) ;
#25935 = CARTESIAN_POINT ( 'NONE',  ( -5.000000000000000000, -41.87499999726880873, 0.000000000000000000 ) ) ;
#25936 = VERTEX_POINT ( 'NONE', #55169 ) ;
#25938 = EDGE_CURVE ( 'NONE', #22889, #61790, #17999, .T. ) ;
#25937 = CARTESIAN_POINT ( 'NONE',  ( 4.458734124999998549, -17.72916666530106866, -2.574251347313721627 ) ) ;
#25939 = ORIENTED_EDGE ( 'NONE', *, *, #53972, .F. ) ;
#25940 =( BOUNDED_CURVE ( )  B_SPLINE_CURVE ( 2, ( #18742, #14541, #24841, #28395, #43183, #38366, #28706, #33545, #48638 ),
 .UNSPECIFIED., .F., .F. ) 
 B_SPLINE_CURVE_WITH_KNOTS ( ( 3, 2, 2, 2, 3 ),
 ( 0.1729166666666666630, 0.1736111111111111049, 0.1749999999999999889, 0.1763888888888889006, 0.1770833333333333426 ),
 .UNSPECIFIED. ) 
 CURVE ( )  GEOMETRIC_REPRESENTATION_ITEM ( )  RATIONAL_B_SPLINE_CURVE ( ( 0.9330127018922194093, 0.9330127018922194093, 1.000000000000000000, 0.8660254037844387076, 1.000000000000000000, 0.8660254037844387076, 1.000000000000000000, 0.9330127018922194093, 0.9330127018922194093 ) ) 
 REPRESENTATION_ITEM ( '' )  );
#25941 = FACE_OUTER_BOUND ( 'NONE', #11768, .T. ) ;
#25942 = CARTESIAN_POINT ( 'NONE',  ( -3.152801135295367096, -168.0625000013656063, -3.152801135295367541 ) ) ;
#25943 = EDGE_CURVE ( 'NONE', #39802, #13190, #24578, .T. ) ;
#25944 =( BOUNDED_CURVE ( )  B_SPLINE_CURVE ( 2, ( #58056, #3725, #57136, #8543, #37495, #9165, #13052, #43252, #42947 ),
 .UNSPECIFIED., .F., .F. ) 
 B_SPLINE_CURVE_WITH_KNOTS ( ( 3, 2, 2, 2, 3 ),
 ( 0.9410714285714285587, 0.9416666666666666519, 0.9428571428571428381, 0.9440476190476190244, 0.9446428571428571175 ),
 .UNSPECIFIED. ) 
 CURVE ( )  GEOMETRIC_REPRESENTATION_ITEM ( )  RATIONAL_B_SPLINE_CURVE ( ( 0.9330127018922194093, 0.9330127018922194093, 1.000000000000000000, 0.8660254037844387076, 1.000000000000000000, 0.8660254037844387076, 1.000000000000000000, 0.9330127018922194093, 0.9330127018922194093 ) ) 
 REPRESENTATION_ITEM ( '' )  );
#25945 = CARTESIAN_POINT ( 'NONE',  ( -5.000000000000000000, -86.87499999726880162, 0.000000000000000000 ) ) ;
#25947 = EDGE_LOOP ( 'NONE', ( #62269, #16678, #42623, #7136 ) ) ;
#25946 = CARTESIAN_POINT ( 'NONE',  ( -1.339745962155610925, -18.79465819873852084, 5.000000000000000000 ) ) ;
#25948 = CARTESIAN_POINT ( 'NONE',  ( -55.39835681537999790, -142.8750000000000284, 4.984105922594378235 ) ) ;
#25949 = CARTESIAN_POINT ( 'NONE',  ( -2.229367062500000163, -34.72916666530107221, -3.861377020970580443 ) ) ;
#25950 = CARTESIAN_POINT ( 'NONE',  ( 2.499999999999998668, -29.33333333333332860, -4.330127018922193649 ) ) ;
#25951 = VERTEX_POINT ( 'NONE', #58709 ) ;
#25952 = CONTEXT_DEPENDENT_SHAPE_REPRESENTATION ( #26539, #38392 ) ;
#25953 = CARTESIAN_POINT ( 'NONE',  ( -4.458734124999999437, -79.31249999863440792, 0.000000000000000000 ) ) ;
#25954 = CARTESIAN_POINT ( 'NONE',  ( -2.229367062499996610, -110.3958333319677507, 3.861377020970582219 ) ) ;
#25955 = CARTESIAN_POINT ( 'NONE',  ( 5.000000000000000000, 20.58333333333333215, -2.886751345948130876 ) ) ;
#25956 = ORIENTED_EDGE ( 'NONE', *, *, #46056, .F. ) ;
#25957 = CARTESIAN_POINT ( 'NONE',  ( -50.40829686548195099, -141.2500000013656063, -1.485763867205728284 ) ) ;
#25958 = CARTESIAN_POINT ( 'NONE',  ( -2.229367062500000163, -75.72916666530106511, -3.861377020970580443 ) ) ;
#25959 = CARTESIAN_POINT ( 'NONE',  ( -59.98410592259440222, -135.2500000027312126, -0.3983568153799752487 ) ) ;
#25960 = CARTESIAN_POINT ( 'NONE',  ( 2.229367062499998831, -41.64583333196773651, -3.861377020970580887 ) ) ;
#25961 = CARTESIAN_POINT ( 'NONE',  ( 2.730187237215162345E-16, -140.4375000013656063, -4.458734124999999437 ) ) ;
#25962 = CARTESIAN_POINT ( 'NONE',  ( 5.000000000000000000, -84.37499999726880162, -6.123233995736766282E-16 ) ) ;
#25963 = CARTESIAN_POINT ( 'NONE',  ( 2.229367062500001939, -51.97916666530107221, 3.861377020970579999 ) ) ;
#25964 = CARTESIAN_POINT ( 'NONE',  ( 4.458734125000000326, -42.89583333196773651, 2.574251347313718519 ) ) ;
#25965 = CARTESIAN_POINT ( 'NONE',  ( 4.458734125000001214, 28.10416666803225993, 2.574251347313718519 ) ) ;
#25966 = EDGE_CURVE ( 'NONE', #51908, #63455, #15607, .T. ) ;
#25967 = CARTESIAN_POINT ( 'NONE',  ( -2.229367062500000163, -16.47916666530107577, -3.861377020970580443 ) ) ;
#25968 = CARTESIAN_POINT ( 'NONE',  ( 2.500000000000002220, -100.6666666666666572, 4.330127018922192761 ) ) ;
#25969 = CARTESIAN_POINT ( 'NONE',  ( 1.975475456537005874E-15, -66.62499999726881583, 5.000000000000000000 ) ) ;
#25970 = CARTESIAN_POINT ( 'NONE',  ( 2.229367062499998831, -39.89583333196773651, -3.861377020970580887 ) ) ;
#25971 = CARTESIAN_POINT ( 'NONE',  ( 5.000000000000000888, 6.541666669397851130, 2.886751345948126879 ) ) ;
#25972 = CARTESIAN_POINT ( 'NONE',  ( -5.000000000000000000, -6.874999997268812280, 0.000000000000000000 ) ) ;
#25973 = CARTESIAN_POINT ( 'NONE',  ( -50.70258187064364108, -130.1250000013656347, 2.196230717870141014 ) ) ;
#25974 =( BOUNDED_CURVE ( )  B_SPLINE_CURVE ( 2, ( #29371, #49004, #33594, #23639, #58037, #24574, #13968, #28758, #146 ),
 .UNSPECIFIED., .F., .F. ) 
 B_SPLINE_CURVE_WITH_KNOTS ( ( 3, 2, 2, 2, 3 ),
 ( 0.1732142857142857095, 0.1738095238095238027, 0.1749999999999999889, 0.1761904761904762029, 0.1767857142857142960 ),
 .UNSPECIFIED. ) 
 CURVE ( )  GEOMETRIC_REPRESENTATION_ITEM ( )  RATIONAL_B_SPLINE_CURVE ( ( 0.9330127018922194093, 0.9330127018922194093, 1.000000000000000000, 0.8660254037844387076, 1.000000000000000000, 0.8660254037844387076, 1.000000000000000000, 0.9330127018922194093, 0.9330127018922194093 ) ) 
 REPRESENTATION_ITEM ( '' )  );
#25975 = CARTESIAN_POINT ( 'NONE',  ( -3.152548672688508926E-16, -72.81249999863439371, -5.148502694627439702 ) ) ;
#25976 = CARTESIAN_POINT ( 'NONE',  ( -2.500000000000000444, 5.833333333333333037, -4.330127018922193649 ) ) ;
#25977 = CARTESIAN_POINT ( 'NONE',  ( 5.000000000000000000, -68.49999999999998579, -6.123233995736766282E-16 ) ) ;
#25978 = CARTESIAN_POINT ( 'NONE',  ( -2.229367062499996610, -2.395833331967737845, 3.861377020970582219 ) ) ;
#25979 = ORIENTED_EDGE ( 'NONE', *, *, #57550, .T. ) ;
#25980 = CARTESIAN_POINT ( 'NONE',  ( 1.339745962155608039, 24.41965820146970145, 5.000000000000003553 ) ) ;
#25981 = CARTESIAN_POINT ( 'NONE',  ( 5.000000000000000000, -15.41666666666666963, -2.886751345948130876 ) ) ;
#25983 = CARTESIAN_POINT ( 'NONE',  ( -4.458734124999999437, -33.31249999863440792, 0.000000000000000000 ) ) ;
#25982 = CARTESIAN_POINT ( 'NONE',  ( -4.458734124999998549, -88.22916666530107932, 2.574251347313722516 ) ) ;
#25984 = FACE_OUTER_BOUND ( 'NONE', #4741, .T. ) ;
#25985 = CARTESIAN_POINT ( 'NONE',  ( -4.458734124999999437, -81.56249999863440792, 0.000000000000000000 ) ) ;
#25986 = CARTESIAN_POINT ( 'NONE',  ( -4.458734124999999437, 15.43750000136559386, 0.000000000000000000 ) ) ;
#25987 = CARTESIAN_POINT ( 'NONE',  ( -5.000000000000000000, -53.08333333333332860, -2.886751345948128211 ) ) ;
#25988 = CARTESIAN_POINT ( 'NONE',  ( -55.35523342533222291, -137.3125000013656063, 4.444560631937231499 ) ) ;
#25989 = CARTESIAN_POINT ( 'NONE',  ( 9.457646018065525792E-16, -5.062499998634402587, 5.148502694627439702 ) ) ;
#25990 = CARTESIAN_POINT ( 'NONE',  ( -2.229367062499996610, 24.60416666803225993, 3.861377020970582219 ) ) ;
#25991 = CARTESIAN_POINT ( 'NONE',  ( -4.458734124999999437, -49.64583333196772941, -2.574251347313719407 ) ) ;
#25992 = CARTESIAN_POINT ( 'NONE',  ( 5.000000000000000000, -105.4166666666666572, -2.886751345948130876 ) ) ;
#25993 = CARTESIAN_POINT ( 'NONE',  ( 2.229367062499998831, -84.64583333196773651, -3.861377020970580887 ) ) ;
#25994 = CARTESIAN_POINT ( 'NONE',  ( 2.229367062500001939, -4.979166665301071326, 3.861377020970579999 ) ) ;
#25995 = CARTESIAN_POINT ( 'NONE',  ( -4.999999999999998224, -30.91666666666667140, 2.886751345948131764 ) ) ;
#25996 = EDGE_LOOP ( 'NONE', ( #12018, #14058, #10217, #1571 ) ) ;
#25997 = CARTESIAN_POINT ( 'NONE',  ( 9.457646018065525792E-16, -31.31249999863440436, 5.148502694627439702 ) ) ;
#25998 =( BOUNDED_CURVE ( )  B_SPLINE_CURVE ( 2, ( #27038, #26723, #56949, #8061, #31537, #36689, #13189, #41817, #2296 ),
 .UNSPECIFIED., .F., .F. ) 
 B_SPLINE_CURVE_WITH_KNOTS ( ( 3, 2, 2, 2, 3 ),
 ( 0.5437499999999999556, 0.5444444444444443976, 0.5458333333333332815, 0.5472222222222222765, 0.5479166666666667185 ),
 .UNSPECIFIED. ) 
 CURVE ( )  GEOMETRIC_REPRESENTATION_ITEM ( )  RATIONAL_B_SPLINE_CURVE ( ( 0.9330127018922194093, 0.9330127018922194093, 1.000000000000000000, 0.8660254037844387076, 1.000000000000000000, 0.8660254037844387076, 1.000000000000000000, 0.9330127018922194093, 0.9330127018922194093 ) ) 
 REPRESENTATION_ITEM ( '' )  );
#25999 = CARTESIAN_POINT ( 'NONE',  ( -56.48576386720575471, -134.0000000013656063, -4.591703134518078322 ) ) ;
#26000 = CARTESIAN_POINT ( 'NONE',  ( -2.229367062500000163, -73.47916666530106511, -3.861377020970580443 ) ) ;
#26001 = CARTESIAN_POINT ( 'NONE',  ( -2.229367062499996610, 27.60416666803225993, 3.861377020970582219 ) ) ;
#26002 = CARTESIAN_POINT ( 'NONE',  ( 4.458734124999998549, 21.27083333469892779, -2.574251347313721627 ) ) ;
#26003 = EDGE_CURVE ( 'NONE', #35107, #17257, #54196, .T. ) ;
#26004 = ADVANCED_FACE ( 'NONE', ( #25889 ), #34566, .T. ) ;
#26005 = CARTESIAN_POINT ( 'NONE',  ( 1.975475456537005874E-15, -43.62499999726880873, 5.000000000000000000 ) ) ;
#26006 = FACE_OUTER_BOUND ( 'NONE', #53555, .T. ) ;
#26007 = CARTESIAN_POINT ( 'NONE',  ( 2.229367062500001939, -78.22916666530106511, 3.861377020970579999 ) ) ;
#26008 = CARTESIAN_POINT ( 'NONE',  ( 2.499999999999998668, -57.33333333333333570, -4.330127018922193649 ) ) ;
#26009 = EDGE_CURVE ( 'NONE', #51626, #59975, #44287, .T. ) ;
#26010 = CARTESIAN_POINT ( 'NONE',  ( 5.000000000000000000, -90.37499999726880162, -6.123233995736766282E-16 ) ) ;
#26011 = CARTESIAN_POINT ( 'NONE',  ( -2.500000000000000444, 22.95833333606451632, -4.330127018922193649 ) ) ;
#26012 = ORIENTED_EDGE ( 'NONE', *, *, #19220, .F. ) ;
#26013 = CARTESIAN_POINT ( 'NONE',  ( -6.972266317189433020E-16, -57.25000000000000000, -5.000000000000000000 ) ) ;
#26014 = CARTESIAN_POINT ( 'NONE',  ( 5.000000000000000000, -67.41666666666667140, -2.886751345948130876 ) ) ;
#26016 = CARTESIAN_POINT ( 'NONE',  ( -4.999999999999999112, -24.91666666666666075, 2.886751345948131764 ) ) ;
#26015 = CARTESIAN_POINT ( 'NONE',  ( 3.061616997868383141E-16, -149.7500000000000284, -5.000000000000000000 ) ) ;
#26017 = CARTESIAN_POINT ( 'NONE',  ( 2.229367062500001939, -24.97916666530106866, 3.861377020970579999 ) ) ;
#26018 = CARTESIAN_POINT ( 'NONE',  ( -2.229367062499996610, -87.14583333196773651, 3.861377020970582219 ) ) ;
#26019 = ADVANCED_FACE ( 'NONE', ( #24614 ), #20751, .T. ) ;
#26020 = CARTESIAN_POINT ( 'NONE',  ( -5.000000000000000000, -24.87499999726881583, 0.000000000000000000 ) ) ;
#26022 = VERTEX_POINT ( 'NONE', #39710 ) ;
#26021 = CARTESIAN_POINT ( 'NONE',  ( 4.458734125000001214, -53.89583333196773651, 2.574251347313718519 ) ) ;
#26023 = CARTESIAN_POINT ( 'NONE',  ( 1.975475456537005874E-15, -65.74999999999998579, 5.000000000000000000 ) ) ;
#26024 = EDGE_CURVE ( 'NONE', #51028, #5037, #37734, .T. ) ;
#26026 = EDGE_LOOP ( 'NONE', ( #2306, #7786, #41991, #24893 ) ) ;
#26025 = CARTESIAN_POINT ( 'NONE',  ( -2.229367062499996610, -1.395833331967737179, 3.861377020970582219 ) ) ;
#26027 = CARTESIAN_POINT ( 'NONE',  ( -4.999999999999999112, -71.91666666666667140, 2.886751345948131764 ) ) ;
#26028 = ADVANCED_FACE ( 'NONE', ( #49691 ), #30063, .T. ) ;
#26029 = CARTESIAN_POINT ( 'NONE',  ( 3.152801135295367541, -152.5625000013655779, -3.152801135295367541 ) ) ;
#26030 = CARTESIAN_POINT ( 'NONE',  ( 4.458734124999998549, -46.97916666530106511, -2.574251347313721627 ) ) ;
#26031 = CARTESIAN_POINT ( 'NONE',  ( 1.975475456537005874E-15, -13.75000000000000000, 5.000000000000000000 ) ) ;
#26032 = CARTESIAN_POINT ( 'NONE',  ( 2.071067811865475505, -159.8125000000000284, -5.000000000000000888 ) ) ;
#26033 = EDGE_CURVE ( 'NONE', #21872, #28553, #7696, .T. ) ;
#26034 = DIRECTION ( 'NONE',  ( -0.000000000000000000, 1.000000000000000000, -0.000000000000000000 ) ) ;
#26035 = CARTESIAN_POINT ( 'NONE',  ( -54.64476657466781973, -125.0625000013655921, -4.444560631937228834 ) ) ;
#26036 = CARTESIAN_POINT ( 'NONE',  ( 4.458734124999999437, -19.06249999863440792, -5.460374474430324690E-16 ) ) ;
#26037 = CARTESIAN_POINT ( 'NONE',  ( 9.457646018065525792E-16, -50.31249999863440792, 5.148502694627439702 ) ) ;
#26038 = DIRECTION ( 'NONE',  ( 0.5000000000000006661, 0.8660254037844383745, -0.000000000000000000 ) ) ;
#26039 = CARTESIAN_POINT ( 'NONE',  ( 4.458734124999999437, -146.4375000013656063, 0.000000000000000000 ) ) ;
#26040 = CARTESIAN_POINT ( 'NONE',  ( 4.458734125000001214, -94.14583333196773651, 2.574251347313718519 ) ) ;
#26041 = CARTESIAN_POINT ( 'NONE',  ( -1.206569728928481577, -7.963640680051488729, -0.4524126574264552558 ) ) ;
#26042 = VERTEX_POINT ( 'NONE', #26854 ) ;
#26043 = CARTESIAN_POINT ( 'NONE',  ( -59.29741812935640155, -153.8750000013655779, -2.196230717870135685 ) ) ;
#26044 = CARTESIAN_POINT ( 'NONE',  ( -4.458734124999999437, 26.43750000136559564, 0.000000000000000000 ) ) ;
#26045 = CARTESIAN_POINT ( 'NONE',  ( -59.81910112700025905, -147.3125000027312410, -2.462841084822630311 ) ) ;
#26046 = CYLINDRICAL_SURFACE ( 'NONE', #39381, 5.000000000000000000 ) ;
#26047 = EDGE_LOOP ( 'NONE', ( #14787, #55872, #62002 ) ) ;
#26048 = CARTESIAN_POINT ( 'NONE',  ( 4.458734125000001214, -1.895833331967737623, 2.574251347313718519 ) ) ;
#26049 = AXIS2_PLACEMENT_3D ( 'NONE', #54437, #6506, #25473 ) ;
#26050 = CARTESIAN_POINT ( 'NONE',  ( 2.500000000000002220, 6.333333333333333037, 4.330127018922192761 ) ) ;
#26051 = CARTESIAN_POINT ( 'NONE',  ( 4.458734124999999437, -17.06249999863440792, -5.460374474430324690E-16 ) ) ;
#26052 = CARTESIAN_POINT ( 'NONE',  ( 5.000000000000000000, 11.70833333606451809, -2.886751345948130876 ) ) ;
#26053 = CARTESIAN_POINT ( 'NONE',  ( -4.458734124999999437, -8.395833331967736513, -2.574251347313719407 ) ) ;
#26054 = CARTESIAN_POINT ( 'NONE',  ( 5.112021521198788498, -5.708827036477115868, -7.069802615102037890 ) ) ;
#26055 = CARTESIAN_POINT ( 'NONE',  ( 4.458734124999999437, -149.4375000013656063, 0.000000000000000000 ) ) ;
#26056 = CARTESIAN_POINT ( 'NONE',  ( 4.458734124999998549, 14.02083333469892779, -2.574251347313721627 ) ) ;
#26057 = ORIENTED_EDGE ( 'NONE', *, *, #35360, .T. ) ;
#26058 = CARTESIAN_POINT ( 'NONE',  ( -1.339745962155610925, -62.66965819600734022, 5.000000000000000000 ) ) ;
#26059 = CARTESIAN_POINT ( 'NONE',  ( -5.000000000000000000, -21.08333333333333570, -2.886751345948128211 ) ) ;
#26060 = CARTESIAN_POINT ( 'NONE',  ( 2.229367062500001939, -20.97916666530107221, 3.861377020970579999 ) ) ;
#26061 = CARTESIAN_POINT ( 'NONE',  ( 7.499999999999999112, 1.854554393013827296, -0.1880126015361732184 ) ) ;
#26062 = CARTESIAN_POINT ( 'NONE',  ( 5.000000000000000000, -88.29166666393548724, -2.886751345948130876 ) ) ;
#26063 = CARTESIAN_POINT ( 'NONE',  ( -55.35523342533222291, -150.3125000013656063, 4.444560631937231499 ) ) ;
#26064 = CARTESIAN_POINT ( 'NONE',  ( -2.499999999999996447, -46.70833333060214443, 4.330127018922195425 ) ) ;
#26065 = DIRECTION ( 'NONE',  ( -0.000000000000000000, 1.000000000000000000, -0.000000000000000000 ) ) ;
#26066 = CARTESIAN_POINT ( 'NONE',  ( 4.458734125000000326, 7.104166668032259935, 2.574251347313718519 ) ) ;
#26067 = CYLINDRICAL_SURFACE ( 'NONE', #23238, 5.000000000000000000 ) ;
#26068 = CARTESIAN_POINT ( 'NONE',  ( 1.975475456537005874E-15, -47.62499999726880873, 5.000000000000000000 ) ) ;
#26069 = CARTESIAN_POINT ( 'NONE',  ( 4.458734124999998549, 13.27083333469892779, -2.574251347313721627 ) ) ;
#26070 = CARTESIAN_POINT ( 'NONE',  ( -2.229367062499996610, -67.14583333196773651, 3.861377020970582219 ) ) ;
#26071 = CARTESIAN_POINT ( 'NONE',  ( -2.229367062499996610, -16.39583333196773651, 3.861377020970582219 ) ) ;
#26072 = CARTESIAN_POINT ( 'NONE',  ( -2.499999999999996447, 0.1666666666666656582, 4.330127018922195425 ) ) ;
#26073 = CARTESIAN_POINT ( 'NONE',  ( -1.846868145590734756, -163.1250000013656063, -4.458734125000000326 ) ) ;
#26074 = CARTESIAN_POINT ( 'NONE',  ( -4.999999999999998224, -37.91666666666667851, 2.886751345948131764 ) ) ;
#26075 = CARTESIAN_POINT ( 'NONE',  ( -2.229367062500000163, -60.47916666530106511, -3.861377020970580443 ) ) ;
#26076 = CARTESIAN_POINT ( 'NONE',  ( 2.499999999999998668, -93.20833333060214443, -4.330127018922193649 ) ) ;
#26077 =( BOUNDED_CURVE ( )  B_SPLINE_CURVE ( 2, ( #51888, #3328, #7829, #46741, #62500, #8768, #37722, #18418, #37408 ),
 .UNSPECIFIED., .F., .F. ) 
 B_SPLINE_CURVE_WITH_KNOTS ( ( 3, 2, 2, 2, 3 ),
 ( 0.6660714285714285365, 0.6666666666666666297, 0.6678571428571428159, 0.6690476190476190022, 0.6696428571428570953 ),
 .UNSPECIFIED. ) 
 CURVE ( )  GEOMETRIC_REPRESENTATION_ITEM ( )  RATIONAL_B_SPLINE_CURVE ( ( 0.9330127018922194093, 0.9330127018922194093, 1.000000000000000000, 0.8660254037844387076, 1.000000000000000000, 0.8660254037844387076, 1.000000000000000000, 0.9330127018922194093, 0.9330127018922194093 ) ) 
 REPRESENTATION_ITEM ( '' )  );
#26078 = CARTESIAN_POINT ( 'NONE',  ( -5.000000000000000000, -77.08333333333334281, -2.886751345948128211 ) ) ;
#26079 = CARTESIAN_POINT ( 'NONE',  ( 1.339745962155612702, -56.29465819873852439, -5.000000000000000000 ) ) ;
#26080 = CARTESIAN_POINT ( 'NONE',  ( 2.229367062500001939, -36.97916666530107221, 3.861377020970579999 ) ) ;
#26081 = CARTESIAN_POINT ( 'NONE',  ( -6.972266317189433020E-16, -71.25000000000000000, -5.000000000000000000 ) ) ;
#26082 = CARTESIAN_POINT ( 'NONE',  ( 2.500000000000002220, -44.66666666666665719, 4.330127018922192761 ) ) ;
#26083 = CARTESIAN_POINT ( 'NONE',  ( 7.922281120364393914, -4.573931137438282057, -8.047472243342932430 ) ) ;
#26084 = CARTESIAN_POINT ( 'NONE',  ( 5.000000000000000000, -6.374999997268812280, -6.123233995736766282E-16 ) ) ;
#26085 = VERTEX_POINT ( 'NONE', #40995 ) ;
#26086 = CARTESIAN_POINT ( 'NONE',  ( 2.229367062499998831, -104.6458333319677365, -3.861377020970580887 ) ) ;
#26087 = CARTESIAN_POINT ( 'NONE',  ( 9.457646018065525792E-16, -1.312499998634405918, 5.148502694627439702 ) ) ;
#26088 = CARTESIAN_POINT ( 'NONE',  ( -2.480964764533239819E-13, -59.75000000000000711, 5.000000000000000000 ) ) ;
#26089 = CARTESIAN_POINT ( 'NONE',  ( 2.500000000000002220, -5.666666666666666963, 4.330127018922192761 ) ) ;
#26090 = CARTESIAN_POINT ( 'NONE',  ( 2.229367062500001939, -72.97916666530107932, 3.861377020970579999 ) ) ;
#26091 = CONICAL_SURFACE ( 'NONE', #7648, 4.174999999999999822, 0.9599310885968795892 ) ;
#26093 = CARTESIAN_POINT ( 'NONE',  ( -1.339745962155610925, -16.79465819873852084, 5.000000000000000000 ) ) ;
#26092 =( BOUNDED_CURVE ( )  B_SPLINE_CURVE ( 2, ( #4875, #62493, #19028, #34444, #44100, #9689, #18412, #23563, #57970 ),
 .UNSPECIFIED., .F., .F. ) 
 B_SPLINE_CURVE_WITH_KNOTS ( ( 3, 2, 2, 2, 3 ),
 ( 0.9729166666666666519, 0.9736111111111110938, 0.9749999999999999778, 0.9763888888888888618, 0.9770833333333333037 ),
 .UNSPECIFIED. ) 
 CURVE ( )  GEOMETRIC_REPRESENTATION_ITEM ( )  RATIONAL_B_SPLINE_CURVE ( ( 0.9330127018922194093, 0.9330127018922194093, 1.000000000000000000, 0.8660254037844387076, 1.000000000000000000, 0.8660254037844387076, 1.000000000000000000, 0.9330127018922194093, 0.9330127018922194093 ) ) 
 REPRESENTATION_ITEM ( '' )  );
#26094 = CARTESIAN_POINT ( 'NONE',  ( 5.000000000000000000, -7.374999997268813168, -6.123233995736766282E-16 ) ) ;
#26096 = VERTEX_POINT ( 'NONE', #60639 ) ;
#26095 = CARTESIAN_POINT ( 'NONE',  ( 9.457646018065525792E-16, -37.06249999863440792, 5.148502694627439702 ) ) ;
#26097 = CARTESIAN_POINT ( 'NONE',  ( 5.000000000000000888, -6.583333333333329485, 2.886751345948126879 ) ) ;
#26099 = ORIENTED_EDGE ( 'NONE', *, *, #27896, .F. ) ;
#26098 = CARTESIAN_POINT ( 'NONE',  ( 4.458734124999999437, 10.93750000136559386, -5.460374474430324690E-16 ) ) ;
#26100 = CARTESIAN_POINT ( 'NONE',  ( 5.000000000000000888, -101.4583333306021302, 2.886751345948126879 ) ) ;
#26101 = CARTESIAN_POINT ( 'NONE',  ( 2.500000000000002220, -48.66666666666666430, 4.330127018922192761 ) ) ;
#26102 = EDGE_CURVE ( 'NONE', #56905, #58717, #53318, .T. ) ;
#26103 = CARTESIAN_POINT ( 'NONE',  ( 2.229367062500001939, -29.22916666530107221, 3.861377020970579999 ) ) ;
#26104 = CARTESIAN_POINT ( 'NONE',  ( 2.499999999999998668, -4.333333333333334814, -4.330127018922193649 ) ) ;
#26105 = CARTESIAN_POINT ( 'NONE',  ( 4.458734124999998549, -76.72916666530106511, -2.574251347313721627 ) ) ;
#26106 = CARTESIAN_POINT ( 'NONE',  ( 5.000000000000000888, -169.9375000000000000, -2.071067811865475505 ) ) ;
#26107 = EDGE_CURVE ( 'NONE', #53853, #57442, #33965, .T. ) ;
#26108 = CARTESIAN_POINT ( 'NONE',  ( -3.152548672688508926E-16, -85.56249999863439371, -5.148502694627439702 ) ) ;
#26109 = CARTESIAN_POINT ( 'NONE',  ( -57.19623071787017210, -135.6250000013655779, 4.297418129356382899 ) ) ;
#26110 = CARTESIAN_POINT ( 'NONE',  ( -2.229367062500000163, -34.72916666530107221, -3.861377020970580443 ) ) ;
#26111 = EDGE_CURVE ( 'NONE', #14367, #30949, #12191, .T. ) ;
#26112 = VERTEX_POINT ( 'NONE', #37677 ) ;
#26113 = CARTESIAN_POINT ( 'NONE',  ( 1.975475456537005874E-15, -93.62499999726881583, 5.000000000000000000 ) ) ;
#26114 = ORIENTED_EDGE ( 'NONE', *, *, #7436, .T. ) ;
#26115 = CARTESIAN_POINT ( 'NONE',  ( 4.458734125000001214, -76.14583333196773651, 2.574251347313718519 ) ) ;
#26116 = CARTESIAN_POINT ( 'NONE',  ( -51.79594014233510535, -135.0000000000000000, -3.114416876829539937 ) ) ;
#26117 = ORIENTED_EDGE ( 'NONE', *, *, #51226, .T. ) ;
#26118 = CARTESIAN_POINT ( 'NONE',  ( -5.000000000000000000, -75.95833333060214443, -2.886751345948128211 ) ) ;
#26119 = CARTESIAN_POINT ( 'NONE',  ( 4.458734125000001214, -64.14583333196773651, 2.574251347313718519 ) ) ;
#26120 = CARTESIAN_POINT ( 'NONE',  ( -4.458734124999998549, -5.479166665301072214, 2.574251347313722516 ) ) ;
#26121 = ORIENTED_EDGE ( 'NONE', *, *, #1204, .F. ) ;
#26122 = CARTESIAN_POINT ( 'NONE',  ( 1.975475456537005874E-15, -84.74999999999998579, 5.000000000000000000 ) ) ;
#26123 = DIRECTION ( 'NONE',  ( 0.000000000000000000, 0.000000000000000000, 1.000000000000000000 ) ) ;
#26124 = ORIENTED_EDGE ( 'NONE', *, *, #49381, .T. ) ;
#26125 = CARTESIAN_POINT ( 'NONE',  ( 75.00000000000002842, 15.00000000000000000, 5.000000000000000000 ) ) ;
#26126 = CARTESIAN_POINT ( 'NONE',  ( -4.458734124999999437, 8.687500001365595637, 0.000000000000000000 ) ) ;
#26127 = CYLINDRICAL_SURFACE ( 'NONE', #12073, 5.000000000000000000 ) ;
#26128 = CARTESIAN_POINT ( 'NONE',  ( -4.458734124999999437, -161.9375000013655779, -5.460374474430324690E-16 ) ) ;
#26129 = CARTESIAN_POINT ( 'NONE',  ( 5.000000000000000888, -75.45833333060214443, 2.886751345948126879 ) ) ;
#26130 = ORIENTED_EDGE ( 'NONE', *, *, #31521, .F. ) ;
#26131 = CARTESIAN_POINT ( 'NONE',  ( -3.152548672688508926E-16, -88.56249999863439371, -5.148502694627439702 ) ) ;
#26132 = CARTESIAN_POINT ( 'NONE',  ( -9.184850993605147944E-16, -140.3750000027312126, 5.000000000000000000 ) ) ;
#26133 = CARTESIAN_POINT ( 'NONE',  ( -4.458734124999998549, -5.229166665301072214, 2.574251347313722516 ) ) ;
#26134 = CARTESIAN_POINT ( 'NONE',  ( 6.123233995736766282E-16, -170.0000000000000000, -5.000000000000000000 ) ) ;
#26135 = CARTESIAN_POINT ( 'NONE',  ( -1.339745962155613812, -68.20534180126148271, -5.000000000000000000 ) ) ;
#26136 = CARTESIAN_POINT ( 'NONE',  ( -4.999999999999999112, -30.79166666393548013, 2.886751345948131764 ) ) ;
#26137 = CARTESIAN_POINT ( 'NONE',  ( -1.339745962155613812, -21.20534180126147561, -5.000000000000000000 ) ) ;
#26138 = CARTESIAN_POINT ( 'NONE',  ( 4.458734125000000326, 23.10416666803225993, 2.574251347313718519 ) ) ;
#26139 = CARTESIAN_POINT ( 'NONE',  ( -4.999999999999998224, -37.79166666393548724, 2.886751345948131764 ) ) ;
#26140 = CARTESIAN_POINT ( 'NONE',  ( -4.458734124999997661, 26.77083333469892779, 2.574251347313722516 ) ) ;
#26141 = CARTESIAN_POINT ( 'NONE',  ( 4.458734124999999437, -50.81249999863440792, -5.460374474430324690E-16 ) ) ;
#26142 = CARTESIAN_POINT ( 'NONE',  ( 4.458734124999998549, -38.97916666530107221, -2.574251347313721627 ) ) ;
#26143 = CARTESIAN_POINT ( 'NONE',  ( 4.458734124999998549, 3.020833334698928674, -2.574251347313721627 ) ) ;
#26144 = CARTESIAN_POINT ( 'NONE',  ( 3.535533905932738197, -160.0000000027312126, -3.535533905932738197 ) ) ;
#26145 = CARTESIAN_POINT ( 'NONE',  ( 2.500000000000002220, 22.33333333333333215, 4.330127018922192761 ) ) ;
#26146 = CARTESIAN_POINT ( 'NONE',  ( -9.184850993605147944E-16, -147.3750000027312126, 5.000000000000000000 ) ) ;
#26147 = CARTESIAN_POINT ( 'NONE',  ( 5.000000000000000888, -26.45833333060214798, 2.886751345948126879 ) ) ;
#26148 = CARTESIAN_POINT ( 'NONE',  ( -4.458734124999999437, -44.31249999863440081, 0.000000000000000000 ) ) ;
#26149 = CARTESIAN_POINT ( 'NONE',  ( 5.000000000000000000, -76.37499999726880162, -6.123233995736766282E-16 ) ) ;
#26150 = CARTESIAN_POINT ( 'NONE',  ( -50.55543936806279248, -138.3125000013656063, 0.3552334253322060320 ) ) ;
#26151 = CARTESIAN_POINT ( 'NONE',  ( 3.535533905932738197, -140.8750000000000000, -3.535533905932738197 ) ) ;
#26152 = CARTESIAN_POINT ( 'NONE',  ( -5.147856630858197489E-14, 3.249999999999997335, 5.000000000000000000 ) ) ;
#26153 = CARTESIAN_POINT ( 'NONE',  ( -2.229367062500000163, -81.72916666530106511, -3.861377020970580443 ) ) ;
#26154 = CARTESIAN_POINT ( 'NONE',  ( 1.846868145590736310, -160.8750000013656063, 4.458734124999997661 ) ) ;
#26155 = CARTESIAN_POINT ( 'NONE',  ( -6.658902113226115027, -5.287118297636088649, -7.776713651266535798 ) ) ;
#26156 = CARTESIAN_POINT ( 'NONE',  ( 5.000000000000000000, -28.41666666666666430, -2.886751345948129988 ) ) ;
#26157 = CARTESIAN_POINT ( 'NONE',  ( 4.458734124999999437, -141.4375000013656063, 0.000000000000000000 ) ) ;
#26158 = ORIENTED_EDGE ( 'NONE', *, *, #10253, .T. ) ;
#26159 = CARTESIAN_POINT ( 'NONE',  ( -4.458734124999999437, 25.43750000136559208, 0.000000000000000000 ) ) ;
#26160 = EDGE_LOOP ( 'NONE', ( #26850, #29150, #9181, #14623 ) ) ;
#26161 = CARTESIAN_POINT ( 'NONE',  ( 2.229367062500001939, -88.97916666530106511, 3.861377020970579999 ) ) ;
#26162 = CARTESIAN_POINT ( 'NONE',  ( 4.458734125000001214, 12.85416666803226171, 2.574251347313718519 ) ) ;
#26163 = CARTESIAN_POINT ( 'NONE',  ( 1.060575238724906964E-15, 18.37500000273118772, 5.773502691896257311 ) ) ;
#26164 = LINE ( 'NONE', #34864, #39092 ) ;
#26165 = CARTESIAN_POINT ( 'NONE',  ( 2.500000000000002220, 13.33333333333333215, 4.330127018922192761 ) ) ;
#26166 = CARTESIAN_POINT ( 'NONE',  ( 4.458734125000000326, -53.89583333196773651, 2.574251347313718519 ) ) ;
#26167 = CARTESIAN_POINT ( 'NONE',  ( -2.229367062500000163, -9.479166665301068662, -3.861377020970580443 ) ) ;
#26168 = CARTESIAN_POINT ( 'NONE',  ( -56.48576386720575471, -136.0000000013656063, -4.591703134518078322 ) ) ;
#26169 = CARTESIAN_POINT ( 'NONE',  ( 1.975475456537005874E-15, 15.37500000273118417, 5.000000000000000000 ) ) ;
#26170 = CARTESIAN_POINT ( 'NONE',  ( 0.000000000000000000, -120.0000000000000000, 0.000000000000000000 ) ) ;
#26171 = DIRECTION ( 'NONE',  ( -0.000000000000000000, 1.000000000000000000, -0.000000000000000000 ) ) ;
#26172 = CARTESIAN_POINT ( 'NONE',  ( -5.000000000000000000, -32.08333333333333570, -2.886751345948128211 ) ) ;
#26173 = DIRECTION ( 'NONE',  ( -0.000000000000000000, 1.000000000000000000, -0.000000000000000000 ) ) ;
#26174 =( BOUNDED_CURVE ( )  B_SPLINE_CURVE ( 2, ( #35463, #51221, #16158, #25485, #55084, #26129, #35785, #46065, #45426 ),
 .UNSPECIFIED., .F., .F. ) 
 B_SPLINE_CURVE_WITH_KNOTS ( ( 3, 2, 2, 2, 3 ),
 ( 0.7446428571428571619, 0.7452380952380952550, 0.7464285714285714413, 0.7476190476190476275, 0.7482142857142857206 ),
 .UNSPECIFIED. ) 
 CURVE ( )  GEOMETRIC_REPRESENTATION_ITEM ( )  RATIONAL_B_SPLINE_CURVE ( ( 0.9330127018922194093, 0.9330127018922194093, 1.000000000000000000, 0.8660254037844387076, 1.000000000000000000, 0.8660254037844387076, 1.000000000000000000, 0.9330127018922194093, 0.9330127018922194093 ) ) 
 REPRESENTATION_ITEM ( '' )  );
#26176 = CARTESIAN_POINT ( 'NONE',  ( 2.229367062500001939, -13.22916666530107221, 3.861377020970579999 ) ) ;
#26175 = CARTESIAN_POINT ( 'NONE',  ( 2.499999999999998668, 21.79166666939785202, -4.330127018922193649 ) ) ;
#26177 = CARTESIAN_POINT ( 'NONE',  ( -49.85088928181150436, -135.6875000027311842, -1.666127454062680480 ) ) ;
#26178 = CARTESIAN_POINT ( 'NONE',  ( -4.458734124999999437, -59.39583333196773651, -2.574251347313719407 ) ) ;
#26179 = CARTESIAN_POINT ( 'NONE',  ( 2.730187237215162345E-16, -153.4375000013655779, -4.458734124999999437 ) ) ;
#26180 = CARTESIAN_POINT ( 'NONE',  ( 4.458734125000001214, -63.89583333196772941, 2.574251347313718519 ) ) ;
#26181 = CARTESIAN_POINT ( 'NONE',  ( -51.60603307380591787, -148.1875000013656063, -2.891590998281053704 ) ) ;
#26182 = AXIS2_PLACEMENT_3D ( 'NONE', #16857, #61253, #17507 ) ;
#26183 = CARTESIAN_POINT ( 'NONE',  ( 5.000000000000000000, -63.29166666393547303, -2.886751345948129988 ) ) ;
#26184 = ORIENTED_EDGE ( 'NONE', *, *, #49243, .T. ) ;
#26185 = CARTESIAN_POINT ( 'NONE',  ( 2.499999999999998668, -31.20833333060214443, -4.330127018922193649 ) ) ;
#26186 = EDGE_LOOP ( 'NONE', ( #45533, #43034, #228, #62752 ) ) ;
#26188 = CARTESIAN_POINT ( 'NONE',  ( -58.24261429053147765, -140.2500000000000000, -3.805975901505573855 ) ) ;
#26187 = FACE_OUTER_BOUND ( 'NONE', #41335, .T. ) ;
#26189 = CARTESIAN_POINT ( 'NONE',  ( 4.458734124999999437, -152.5000000013656347, 1.846868145590737864 ) ) ;
#26190 = VERTEX_POINT ( 'NONE', #36183 ) ;
#26191 = CARTESIAN_POINT ( 'NONE',  ( -1.339745962155613812, -8.080341798530294994, -5.000000000000000000 ) ) ;
#26192 = CARTESIAN_POINT ( 'NONE',  ( -58.80597590150559739, -128.0000000000000284, 3.242614290531460330 ) ) ;
#26193 = CARTESIAN_POINT ( 'NONE',  ( 2.500000000000002220, -80.54166666393547303, 4.330127018922192761 ) ) ;
#26194 = CARTESIAN_POINT ( 'NONE',  ( 2.229367062499998831, -49.89583333196772941, -3.861377020970580887 ) ) ;
#26195 = VERTEX_POINT ( 'NONE', #37999 ) ;
#26196 = CARTESIAN_POINT ( 'NONE',  ( 2.500000000000002220, 11.33333333333333393, 4.330127018922192761 ) ) ;
#26197 = CARTESIAN_POINT ( 'NONE',  ( -4.458734124999999437, 11.60416666803225993, -2.574251347313719407 ) ) ;
#26198 = CARTESIAN_POINT ( 'NONE',  ( -2.229367062499996610, 24.85416666803225993, 3.861377020970582219 ) ) ;
#26199 = CARTESIAN_POINT ( 'NONE',  ( -59.59170313451811296, -152.5000000013655779, 1.485763867205729394 ) ) ;
#26200 = CARTESIAN_POINT ( 'NONE',  ( 5.000000000000000888, -13.45833333060214976, 2.886751345948126879 ) ) ;
#26201 = CARTESIAN_POINT ( 'NONE',  ( 7.500000000000000888, 3.608439182435154269, -7.298562697733103732 ) ) ;
#26202 = VERTEX_POINT ( 'NONE', #6918 ) ;
#26203 = CARTESIAN_POINT ( 'NONE',  ( 4.458734125000000326, -66.89583333196773651, 2.574251347313718519 ) ) ;
#26204 = CARTESIAN_POINT ( 'NONE',  ( -6.972266317189433020E-16, -50.12499999726881583, -5.000000000000000000 ) ) ;
#26205 = CARTESIAN_POINT ( 'NONE',  ( 2.229367062500001939, 14.02083333469892779, 3.861377020970579999 ) ) ;
#26206 = EDGE_CURVE ( 'NONE', #4115, #36130, #9350, .T. ) ;
#26207 = CARTESIAN_POINT ( 'NONE',  ( 2.500000000000002220, -63.66666666666666430, 4.330127018922192761 ) ) ;
#26208 = CARTESIAN_POINT ( 'NONE',  ( 3.535533905932736864, -157.2500000027312126, 3.535533905932738641 ) ) ;
#26209 = CARTESIAN_POINT ( 'NONE',  ( 4.458734125000001214, -53.14583333196773651, 2.574251347313718519 ) ) ;
#26210 = CARTESIAN_POINT ( 'NONE',  ( 2.500000000000002220, -16.54166666393548368, 4.330127018922192761 ) ) ;
#26211 = CARTESIAN_POINT ( 'NONE',  ( 5.000000000000000000, -23.29166666393548368, -2.886751345948130876 ) ) ;
#26212 = CARTESIAN_POINT ( 'NONE',  ( 0.000000000000000000, -170.0000000000000000, 0.000000000000000000 ) ) ;
#26213 = CARTESIAN_POINT ( 'NONE',  ( 2.499999999999998668, -64.20833333060213022, -4.330127018922193649 ) ) ;
#26214 = CARTESIAN_POINT ( 'NONE',  ( 2.229367062500001939, -17.22916666530106866, 3.861377020970579999 ) ) ;
#26215 = VERTEX_POINT ( 'NONE', #41305 ) ;
#26216 = PLANE ( 'NONE',  #11464 ) ;
#26217 = CARTESIAN_POINT ( 'NONE',  ( 4.458734125000001214, -105.8958333319677365, 2.574251347313718519 ) ) ;
#26218 = CARTESIAN_POINT ( 'NONE',  ( -5.000000000000000000, -157.6250000027311842, -6.123233995736766282E-16 ) ) ;
#26219 = ORIENTED_EDGE ( 'NONE', *, *, #12505, .T. ) ;
#26220 = CARTESIAN_POINT ( 'NONE',  ( 4.458734124999998549, -103.9791666653010509, -2.574251347313721627 ) ) ;
#26221 = CARTESIAN_POINT ( 'NONE',  ( 2.229367062500001939, -28.97916666530107221, 3.861377020970579999 ) ) ;
#26222 = CARTESIAN_POINT ( 'NONE',  ( 2.499999999999998668, -62.20833333060214443, -4.330127018922193649 ) ) ;
#26223 = CARTESIAN_POINT ( 'NONE',  ( -57.89159099828107458, -153.9375000013656063, -3.393966926194107447 ) ) ;
#26224 = CARTESIAN_POINT ( 'NONE',  ( -59.44456063193725015, -144.5625000013656063, -0.3552334253322034230 ) ) ;
#26225 = CARTESIAN_POINT ( 'NONE',  ( -2.229367062499996610, -22.14583333196773651, 3.861377020970582219 ) ) ;
#26226 = CARTESIAN_POINT ( 'NONE',  ( -2.229367062499996610, -65.39583333196773651, 3.861377020970582219 ) ) ;
#26227 = CARTESIAN_POINT ( 'NONE',  ( -59.81910112700027327, -137.1875000000000000, -2.462841084822392279 ) ) ;
#26228 = CARTESIAN_POINT ( 'NONE',  ( -2.229367062500000163, -17.47916666530106866, -3.861377020970580443 ) ) ;
#26229 = CARTESIAN_POINT ( 'NONE',  ( 5.000000000000000888, -75.58333333333334281, 2.886751345948126879 ) ) ;
#26230 = CARTESIAN_POINT ( 'NONE',  ( -5.000000000000000888, -149.4375000000000000, 2.071067811865474617 ) ) ;
#26231 = CARTESIAN_POINT ( 'NONE',  ( -4.999999999999999112, -9.916666666666662522, 2.886751345948131764 ) ) ;
#26232 = CARTESIAN_POINT ( 'NONE',  ( -1.846868145590737420, -150.7500000013655779, 4.458734124999999437 ) ) ;
#26233 = ORIENTED_EDGE ( 'NONE', *, *, #35453, .F. ) ;
#26234 = CARTESIAN_POINT ( 'NONE',  ( 4.458734124999999437, -47.06249999863440792, -5.460374474430324690E-16 ) ) ;
#26235 = CARTESIAN_POINT ( 'NONE',  ( 1.464175926609780648E-14, 21.87500000273118062, -5.000000000000000000 ) ) ;
#26236 = DIRECTION ( 'NONE',  ( -7.709882115452477180E-16, 0.000000000000000000, 1.000000000000000000 ) ) ;
#26237 = CARTESIAN_POINT ( 'NONE',  ( -2.229367062499996610, -88.14583333196773651, 3.861377020970582219 ) ) ;
#26238 = CARTESIAN_POINT ( 'NONE',  ( -3.152548672688508926E-16, 6.437500001365592972, -5.148502694627439702 ) ) ;
#26239 = CARTESIAN_POINT ( 'NONE',  ( 0.000000000000000000, -170.0000000000000000, 5.000000000000000000 ) ) ;
#26240 = LINE ( 'NONE', #30423, #22197 ) ;
#26241 = CARTESIAN_POINT ( 'NONE',  ( -4.458734124999998549, 13.52083333469892779, 2.574251347313722516 ) ) ;
#26242 = CARTESIAN_POINT ( 'NONE',  ( -2.500000000000000444, 1.958333336064519647, -4.330127018922193649 ) ) ;
#26243 = ORIENTED_EDGE ( 'NONE', *, *, #42116, .T. ) ;
#26244 = CARTESIAN_POINT ( 'NONE',  ( 2.071067811865401787, -161.9375000027311842, -5.000000000000074607 ) ) ;
#26245 = VERTEX_POINT ( 'NONE', #8421 ) ;
#26246 = CARTESIAN_POINT ( 'NONE',  ( 1.975475456537005874E-15, -53.62499999726880162, 5.000000000000000000 ) ) ;
#26247 = CARTESIAN_POINT ( 'NONE',  ( 4.458734125000001214, -45.89583333196774362, 2.574251347313718519 ) ) ;
#26248 = CARTESIAN_POINT ( 'NONE',  ( -1.846868145590734756, -163.3750000013656347, -4.458734125000000326 ) ) ;
#26249 = CARTESIAN_POINT ( 'NONE',  ( 5.000000000000000000, -37.37499999726881583, -6.123233995736766282E-16 ) ) ;
#26250 = ORIENTED_EDGE ( 'NONE', *, *, #13469, .T. ) ;
#26251 = CARTESIAN_POINT ( 'NONE',  ( 9.457646018065525792E-16, -18.06249999863440436, 5.148502694627439702 ) ) ;
#26252 = ORIENTED_EDGE ( 'NONE', *, *, #601, .F. ) ;
#26253 = CARTESIAN_POINT ( 'NONE',  ( -2.500000000000000444, -89.16666666666665719, -4.330127018922193649 ) ) ;
#26254 = CARTESIAN_POINT ( 'NONE',  ( -4.458734125000000326, -166.0000000013656063, -1.846868145590735644 ) ) ;
#26255 = CARTESIAN_POINT ( 'NONE',  ( -4.999999999999999112, -85.79166666393547303, 2.886751345948131764 ) ) ;
#26257 = ORIENTED_EDGE ( 'NONE', *, *, #18075, .T. ) ;
#26256 = CARTESIAN_POINT ( 'NONE',  ( -1.339745962155613812, -61.08034179853027723, -5.000000000000000000 ) ) ;
#26258 = CARTESIAN_POINT ( 'NONE',  ( -51.19402409849444524, -143.5000000000000284, -3.242614290531456334 ) ) ;
#26259 = CARTESIAN_POINT ( 'NONE',  ( -2.229367062499996610, -31.39583333196773651, 3.861377020970582219 ) ) ;
#26260 = CARTESIAN_POINT ( 'NONE',  ( 1.975475456537005874E-15, -29.74999999999999645, 5.000000000000000000 ) ) ;
#26261 = ORIENTED_EDGE ( 'NONE', *, *, #6177, .T. ) ;
#26262 = VECTOR ( 'NONE', #53015, 1000.000000000000114 ) ;
#26263 =( BOUNDED_CURVE ( )  B_SPLINE_CURVE ( 2, ( #39345, #15227, #5580, #59295, #20707, #40312, #49643, #58975, #59950 ),
 .UNSPECIFIED., .F., .F. ) 
 B_SPLINE_CURVE_WITH_KNOTS ( ( 3, 2, 2, 2, 3 ),
 ( 0.3083333333333336257, 0.3125000000000002776, 0.3166666666666669294, 0.3208333333333336368, 0.3250000000000002887 ),
 .UNSPECIFIED. ) 
 CURVE ( )  GEOMETRIC_REPRESENTATION_ITEM ( )  RATIONAL_B_SPLINE_CURVE ( ( 0.9999999999999948930, 0.9238795325112918455, 1.000000000000000000, 0.9238795325112867385, 1.000000000000000000, 0.9238795325112867385, 1.000000000000000000, 0.9238795325112816315, 1.000000000000005107 ) ) 
 REPRESENTATION_ITEM ( '' )  );
#26264 = CARTESIAN_POINT ( 'NONE',  ( 4.458734124999999437, -74.81249999863440792, -5.460374474430324690E-16 ) ) ;
#26265 = CARTESIAN_POINT ( 'NONE',  ( -4.458734124999999437, 29.60416666803225993, -2.574251347313719407 ) ) ;
#26266 = CARTESIAN_POINT ( 'NONE',  ( 1.975475456537005874E-15, -18.74999999999999645, 5.000000000000000000 ) ) ;
#26267 = ORIENTED_EDGE ( 'NONE', *, *, #10187, .F. ) ;
#26268 = CARTESIAN_POINT ( 'NONE',  ( -2.071067811865394237, -161.3125000000000284, 5.000000000000084377 ) ) ;
#26269 = CARTESIAN_POINT ( 'NONE',  ( -57.89159099828107458, -141.9375000013656063, -3.393966926194107447 ) ) ;
#26270 = CARTESIAN_POINT ( 'NONE',  ( 4.458734124999999437, -83.06249999863440792, -5.460374474430324690E-16 ) ) ;
#26271 = CARTESIAN_POINT ( 'NONE',  ( -59.81910112700025905, -136.3125000027312126, -2.462841084822630311 ) ) ;
#26272 = CARTESIAN_POINT ( 'NONE',  ( 9.457646018065525792E-16, -44.06249999863439371, 5.148502694627439702 ) ) ;
#26273 = CARTESIAN_POINT ( 'NONE',  ( -4.458734124999999437, -142.2500000013656063, -1.846868145590735644 ) ) ;
#26274 = DIRECTION ( 'NONE',  ( -0.000000000000000000, 1.000000000000000000, -0.000000000000000000 ) ) ;
#26275 = CARTESIAN_POINT ( 'NONE',  ( -4.458734124999997661, -48.22916666530106511, 2.574251347313722516 ) ) ;
#26276 = CARTESIAN_POINT ( 'NONE',  ( -4.458734124999999437, -43.39583333196773651, -2.574251347313719407 ) ) ;
#26277 = CARTESIAN_POINT ( 'NONE',  ( -2.229367062500000163, 28.52083333469892779, -3.861377020970580443 ) ) ;
#26278 = ADVANCED_FACE ( 'NONE', ( #56121 ), #12044, .T. ) ;
#26279 = CARTESIAN_POINT ( 'NONE',  ( -2.499999999999996447, -98.83333333333332860, 4.330127018922195425 ) ) ;
#26280 = CARTESIAN_POINT ( 'NONE',  ( 3.535533905932738197, -159.0000000027312126, -3.535533905932738197 ) ) ;
#26281 = CARTESIAN_POINT ( 'NONE',  ( 2.229367062499998831, -40.89583333196773651, -3.861377020970580887 ) ) ;
#26282 = CARTESIAN_POINT ( 'NONE',  ( -2.499999999999996447, 0.2916666693978525737, 4.330127018922195425 ) ) ;
#26283 = CARTESIAN_POINT ( 'NONE',  ( 0.000000000000000000, -120.0000000000000000, 0.000000000000000000 ) ) ;
#26284 = CARTESIAN_POINT ( 'NONE',  ( -50.70258187064364108, -127.1250000013656205, 2.196230717870141014 ) ) ;
#26285 = CARTESIAN_POINT ( 'NONE',  ( -4.458734124999998549, -81.47916666530106511, 2.574251347313722516 ) ) ;
#26286 = CARTESIAN_POINT ( 'NONE',  ( 5.000000000000000000, -34.50000000000000000, -6.123233995736766282E-16 ) ) ;
#26287 = CARTESIAN_POINT ( 'NONE',  ( 2.229367062500001939, -97.97916666530105090, 3.861377020970579999 ) ) ;
#26288 = CARTESIAN_POINT ( 'NONE',  ( 2.499999999999998668, -76.33333333333334281, -4.330127018922193649 ) ) ;
#26289 = CARTESIAN_POINT ( 'NONE',  ( -2.229367062500000163, 0.2708333346989263979, -3.861377020970580443 ) ) ;
#26290 = VERTEX_POINT ( 'NONE', #43440 ) ;
#26291 = CARTESIAN_POINT ( 'NONE',  ( 3.535533905932736864, -146.1250000000000000, 3.535533905932738641 ) ) ;
#26292 = CARTESIAN_POINT ( 'NONE',  ( 9.457646018065525792E-16, -89.06249999863439371, 5.148502694627439702 ) ) ;
#26293 = CARTESIAN_POINT ( 'NONE',  ( 1.975475456537005874E-15, -62.62499999726880873, 5.000000000000000000 ) ) ;
#26294 = CARTESIAN_POINT ( 'NONE',  ( 4.458734124999999437, -88.06249999863439371, -5.460374474430324690E-16 ) ) ;
#26295 = CARTESIAN_POINT ( 'NONE',  ( 4.458734125000000326, 9.854166668032261711, 2.574251347313718519 ) ) ;
#26296 = FACE_OUTER_BOUND ( 'NONE', #40405, .T. ) ;
#26297 = CARTESIAN_POINT ( 'NONE',  ( -56.48576386720575471, -133.7500000013656063, -4.591703134518078322 ) ) ;
#26298 = EDGE_CURVE ( 'NONE', #59631, #2425, #47954, .T. ) ;
#26299 = CARTESIAN_POINT ( 'NONE',  ( 4.458734124999999437, -5.812499998634403475, -5.460374474430324690E-16 ) ) ;
#26300 = CARTESIAN_POINT ( 'NONE',  ( 4.458734124999998549, 18.02083333469892779, -2.574251347313721627 ) ) ;
#26301 = EDGE_CURVE ( 'NONE', #3756, #23656, #22337, .T. ) ;
#26302 = CARTESIAN_POINT ( 'NONE',  ( 9.457646018065525792E-16, -50.31249999863440792, 5.148502694627439702 ) ) ;
#26303 = CARTESIAN_POINT ( 'NONE',  ( -5.000000000000000000, -13.87499999726881228, 0.000000000000000000 ) ) ;
#26304 = CARTESIAN_POINT ( 'NONE',  ( -4.458734124999999437, -87.31249999863439371, 0.000000000000000000 ) ) ;
#26305 = CARTESIAN_POINT ( 'NONE',  ( 4.458734124999998549, -1.729166665301068440, -2.574251347313721627 ) ) ;
#26306 = CYLINDRICAL_SURFACE ( 'NONE', #46281, 5.000000000000000000 ) ;
#26307 = ORIENTED_EDGE ( 'NONE', *, *, #47442, .F. ) ;
#26308 = CARTESIAN_POINT ( 'NONE',  ( 4.458734124999999437, -30.06249999863440436, -5.460374474430324690E-16 ) ) ;
#26309 = CARTESIAN_POINT ( 'NONE',  ( -59.44456063193725015, -130.8125000013656063, -0.3552334253322034230 ) ) ;
#26310 = CARTESIAN_POINT ( 'NONE',  ( -2.229367062499996610, -72.14583333196773651, 3.861377020970582219 ) ) ;
#26311 = CARTESIAN_POINT ( 'NONE',  ( 4.458734124999998549, 27.02083333469892423, -2.574251347313721627 ) ) ;
#26312 = VECTOR ( 'NONE', #42768, 1000.000000000000000 ) ;
#26313 = EDGE_CURVE ( 'NONE', #41008, #12871, #40545, .T. ) ;
#26314 = AXIS2_PLACEMENT_3D ( 'NONE', #33107, #2580, #8353 ) ;
#26315 = CARTESIAN_POINT ( 'NONE',  ( -2.229367062499996610, 19.85416666803225993, 3.861377020970582219 ) ) ;
#26316 = CARTESIAN_POINT ( 'NONE',  ( 1.339745962155612702, -53.29465819873850307, -5.000000000000000000 ) ) ;
#26317 = CARTESIAN_POINT ( 'NONE',  ( 5.000000000000000000, 1.500000000000001332, -6.123233995736766282E-16 ) ) ;
#26318 = CARTESIAN_POINT ( 'NONE',  ( 9.457646018065525792E-16, -80.31249999863440792, 5.148502694627439702 ) ) ;
#26319 = CARTESIAN_POINT ( 'NONE',  ( 1.060575238724906964E-15, -65.75000000000000000, 5.773502691896257311 ) ) ;
#26320 =( BOUNDED_CURVE ( )  B_SPLINE_CURVE ( 2, ( #39372, #38428, #5296, #24914, #34227, #53854, #9783, #59003, #10430 ),
 .UNSPECIFIED., .F., .F. ) 
 B_SPLINE_CURVE_WITH_KNOTS ( ( 3, 2, 2, 2, 3 ),
 ( 0.7187500000000000000, 0.7194444444444444420, 0.7208333333333333259, 0.7222222222222222099, 0.7229166666666666519 ),
 .UNSPECIFIED. ) 
 CURVE ( )  GEOMETRIC_REPRESENTATION_ITEM ( )  RATIONAL_B_SPLINE_CURVE ( ( 0.9330127018922194093, 0.9330127018922194093, 1.000000000000000000, 0.8660254037844387076, 1.000000000000000000, 0.8660254037844387076, 1.000000000000000000, 0.9330127018922194093, 0.9330127018922194093 ) ) 
 REPRESENTATION_ITEM ( '' )  );
#26321 = CARTESIAN_POINT ( 'NONE',  ( -6.972266317189433020E-16, -11.25000000000000178, -5.000000000000000000 ) ) ;
#26322 = CARTESIAN_POINT ( 'NONE',  ( 2.499999999999998668, 24.79166666939785202, -4.330127018922193649 ) ) ;
#26323 = ORIENTED_EDGE ( 'NONE', *, *, #42923, .F. ) ;
#26324 = CARTESIAN_POINT ( 'NONE',  ( -6.972266317189433020E-16, -73.12499999726878741, -5.000000000000000000 ) ) ;
#26325 =( BOUNDED_CURVE ( )  B_SPLINE_CURVE ( 2, ( #11593, #27032, #16108, #32160, #1977, #11908, #60821, #55362, #12864 ),
 .UNSPECIFIED., .F., .F. ) 
 B_SPLINE_CURVE_WITH_KNOTS ( ( 3, 2, 2, 2, 3 ),
 ( 0.05833333333333338283, 0.06250000000000005551, 0.06666666666666672125, 0.07083333333333338699, 0.07500000000000005274 ),
 .UNSPECIFIED. ) 
 CURVE ( )  GEOMETRIC_REPRESENTATION_ITEM ( )  RATIONAL_B_SPLINE_CURVE ( ( 0.9999999999999991118, 0.9238795325112876267, 1.000000000000000000, 0.9238795325112867385, 1.000000000000000000, 0.9238795325112867385, 1.000000000000000000, 0.9238795325112857393, 1.000000000000001110 ) ) 
 REPRESENTATION_ITEM ( '' )  );
#26326 = CARTESIAN_POINT ( 'NONE',  ( 3.061616997868383141E-16, -168.8750000027312126, -5.000000000000000000 ) ) ;
#26327 = CARTESIAN_POINT ( 'NONE',  ( -4.999999999999999112, -25.91666666666666430, 2.886751345948131764 ) ) ;
#26328 = CARTESIAN_POINT ( 'NONE',  ( -2.229367062499996610, -28.14583333196774007, 3.861377020970582219 ) ) ;
#26329 = CARTESIAN_POINT ( 'NONE',  ( -2.229367062500000163, -89.47916666530106511, -3.861377020970580443 ) ) ;
#26330 = CARTESIAN_POINT ( 'NONE',  ( 2.500000000000002220, -22.54166666393548013, 4.330127018922192761 ) ) ;
#26331 = ADVANCED_FACE ( 'NONE', ( #14482 ), #15128, .T. ) ;
#26333 = VERTEX_POINT ( 'NONE', #14170 ) ;
#26332 = CARTESIAN_POINT ( 'NONE',  ( 2.229367062500001939, -57.97916666530107932, 3.861377020970579999 ) ) ;
#26334 = CARTESIAN_POINT ( 'NONE',  ( 5.000000000000000000, -27.41666666666666430, -2.886751345948130876 ) ) ;
#26335 = LINE ( 'NONE', #16691, #11797 ) ;
#26337 = ORIENTED_EDGE ( 'NONE', *, *, #61736, .F. ) ;
#26336 = CARTESIAN_POINT ( 'NONE',  ( 4.458734124999998549, -3.979166665301070438, -2.574251347313721627 ) ) ;
#26338 = CARTESIAN_POINT ( 'NONE',  ( -2.500000000000000444, -73.16666666666665719, -4.330127018922193649 ) ) ;
#26339 = CARTESIAN_POINT ( 'NONE',  ( -8.190561711645485556E-16, -152.9375000013655779, 4.458734124999999437 ) ) ;
#26340 = CARTESIAN_POINT ( 'NONE',  ( 9.457646018065525792E-16, -45.31249999863440081, 5.148502694627439702 ) ) ;
#26341 = CARTESIAN_POINT ( 'NONE',  ( 5.000000000000000000, -160.0000000000000000, 0.000000000000000000 ) ) ;
#26342 = CARTESIAN_POINT ( 'NONE',  ( -4.999999999999999112, -72.79166666393547303, 2.886751345948131764 ) ) ;
#26343 = CARTESIAN_POINT ( 'NONE',  ( -5.000000000000000000, -86.00000000000000000, 0.000000000000000000 ) ) ;
#26344 = CARTESIAN_POINT ( 'NONE',  ( -57.46284108482265651, -153.9375000000000284, 4.819101127000239515 ) ) ;
#26345 = CARTESIAN_POINT ( 'NONE',  ( 9.457646018065525792E-16, -17.31249999863440436, 5.148502694627439702 ) ) ;
#26346 = CARTESIAN_POINT ( 'NONE',  ( -4.458734124999999437, -52.56249999863440792, 0.000000000000000000 ) ) ;
#26347 = CARTESIAN_POINT ( 'NONE',  ( 5.000000000000000000, 22.50000000000000000, -6.123233995736766282E-16 ) ) ;
#26348 = CARTESIAN_POINT ( 'NONE',  ( -3.152801135295367985, -142.8125000013655779, 3.152801135295367096 ) ) ;
#26349 = CARTESIAN_POINT ( 'NONE',  ( -4.458734124999999437, -94.64583333196773651, -2.574251347313719407 ) ) ;
#26350 = CARTESIAN_POINT ( 'NONE',  ( 5.000000000000000000, -2.416666666666663410, -2.886751345948130876 ) ) ;
#26351 = ORIENTED_EDGE ( 'NONE', *, *, #40084, .F. ) ;
#26352 = CARTESIAN_POINT ( 'NONE',  ( -3.535533905932737309, -155.6250000000000000, -3.535533905932738197 ) ) ;
#26353 = CARTESIAN_POINT ( 'NONE',  ( -4.458734124999999437, 25.35416666803225993, -2.574251347313719407 ) ) ;
#26354 = CARTESIAN_POINT ( 'NONE',  ( -51.19402409849444524, -148.6250000027312126, -3.242614290531456334 ) ) ;
#26355 = VECTOR ( 'NONE', #58512, 1000.000000000000000 ) ;
#26356 = DIRECTION ( 'NONE',  ( -0.000000000000000000, 1.000000000000000000, -0.000000000000000000 ) ) ;
#26357 = EDGE_CURVE ( 'NONE', #43968, #19989, #15940, .T. ) ;
#26358 = CARTESIAN_POINT ( 'NONE',  ( 4.458734124999998549, -1.729166665301068440, -2.574251347313721627 ) ) ;
#26359 = EDGE_CURVE ( 'NONE', #8589, #56396, #45056, .T. ) ;
#26360 = EDGE_CURVE ( 'NONE', #35996, #16789, #38609, .T. ) ;
#26361 = CARTESIAN_POINT ( 'NONE',  ( 5.000000000000000000, -1.291666663935479908, -2.886751345948130876 ) ) ;
#26362 = CARTESIAN_POINT ( 'NONE',  ( 2.229367062500001939, -24.22916666530107577, 3.861377020970579999 ) ) ;
#26363 = CARTESIAN_POINT ( 'NONE',  ( -2.229367062500000163, -62.72916666530106511, -3.861377020970580443 ) ) ;
#26364 = CARTESIAN_POINT ( 'NONE',  ( 1.975475456537005874E-15, -2.624999997268813168, 5.000000000000000000 ) ) ;
#26365 = CARTESIAN_POINT ( 'NONE',  ( 9.457646018065525792E-16, -6.062499998634403475, 5.148502694627439702 ) ) ;
#26366 = CARTESIAN_POINT ( 'NONE',  ( 5.000000000000000000, 23.70833333606451632, -2.886751345948130876 ) ) ;
#26367 = CARTESIAN_POINT ( 'NONE',  ( -3.152801135295367096, -147.0625000013655779, -3.152801135295367541 ) ) ;
#26368 =( BOUNDED_CURVE ( )  B_SPLINE_CURVE ( 2, ( #20399, #50621, #40960, #470, #5285, #20071, #34874, #5601, #25218 ),
 .UNSPECIFIED., .F., .F. ) 
 B_SPLINE_CURVE_WITH_KNOTS ( ( 3, 2, 2, 2, 3 ),
 ( 0.1250000000000001110, 0.1291666666666667906, 0.1333333333333334425, 0.1375000000000001221, 0.1416666666666667740 ),
 .UNSPECIFIED. ) 
 CURVE ( )  GEOMETRIC_REPRESENTATION_ITEM ( )  RATIONAL_B_SPLINE_CURVE ( ( 0.9999999999999980016, 0.9238795325112887369, 1.000000000000000000, 0.9238795325112867385, 1.000000000000000000, 0.9238795325112867385, 1.000000000000000000, 0.9238795325112847401, 1.000000000000001998 ) ) 
 REPRESENTATION_ITEM ( '' )  );
#26369 = CARTESIAN_POINT ( 'NONE',  ( -3.152548672688508926E-16, 18.18750000136559564, -5.148502694627439702 ) ) ;
#26370 = ORIENTED_EDGE ( 'NONE', *, *, #34199, .T. ) ;
#26371 = CARTESIAN_POINT ( 'NONE',  ( 6.123233995736766282E-16, -120.0000000000000000, -5.000000000000000000 ) ) ;
#26372 = CARTESIAN_POINT ( 'NONE',  ( 1.339745962155615144, -71.58034179853027013, 4.999999999999999112 ) ) ;
#26374 = CARTESIAN_POINT ( 'NONE',  ( 4.458734124999999437, -19.81249999863440081, -5.460374474430324690E-16 ) ) ;
#26373 = CARTESIAN_POINT ( 'NONE',  ( 2.499999999999998668, -86.33333333333332860, -4.330127018922193649 ) ) ;
#26376 = EDGE_CURVE ( 'NONE', #27636, #40984, #4223, .T. ) ;
#26375 = CARTESIAN_POINT ( 'NONE',  ( 7.499999999999999112, 0.3744244963005059490, 1.526918059583750369E-15 ) ) ;
#26377 = CARTESIAN_POINT ( 'NONE',  ( 5.000000000000000000, 1.708333336064519425, -2.886751345948130876 ) ) ;
#26378 = CARTESIAN_POINT ( 'NONE',  ( -54.64476657466781973, -148.8125000013656063, -4.444560631937228834 ) ) ;
#26379 = CARTESIAN_POINT ( 'NONE',  ( 5.000000000000000000, -47.37499999726880873, -6.123233995736766282E-16 ) ) ;
#26380 = DIRECTION ( 'NONE',  ( -0.000000000000000000, 1.000000000000000000, -0.000000000000000000 ) ) ;
#26381 = CARTESIAN_POINT ( 'NONE',  ( -4.458734124999999437, 7.604166668032259935, -2.574251347313719407 ) ) ;
#26382 = CARTESIAN_POINT ( 'NONE',  ( -2.500000000000000444, -90.04166666393547303, -4.330127018922193649 ) ) ;
#26383 = EDGE_CURVE ( 'NONE', #25740, #1775, #16325, .T. ) ;
#26384 = CARTESIAN_POINT ( 'NONE',  ( -4.999999999999998224, -14.91666666666666785, 2.886751345948131764 ) ) ;
#26385 = CARTESIAN_POINT ( 'NONE',  ( -2.229367062500000163, 14.52083333469892779, -3.861377020970580443 ) ) ;
#26386 = CARTESIAN_POINT ( 'NONE',  ( 2.229367062500001939, -69.97916666530107932, 3.861377020970579999 ) ) ;
#26387 = CARTESIAN_POINT ( 'NONE',  ( -2.229367062499996610, -14.39583333196774184, 3.861377020970582219 ) ) ;
#26388 = CARTESIAN_POINT ( 'NONE',  ( -5.000000000000000000, -0.08333333333333457771, -2.886751345948128211 ) ) ;
#26389 = CARTESIAN_POINT ( 'NONE',  ( -1.846868145590734756, -162.1250000013655779, -4.458734125000000326 ) ) ;
#26390 = CARTESIAN_POINT ( 'NONE',  ( 1.975475456537005874E-15, -37.74999999999999289, 5.000000000000000000 ) ) ;
#26391 = CARTESIAN_POINT ( 'NONE',  ( -3.152548672688508926E-16, -56.56249999863439371, -5.148502694627439702 ) ) ;
#26392 = CARTESIAN_POINT ( 'NONE',  ( -2.500000000000000444, -97.04166666393545881, -4.330127018922193649 ) ) ;
#26393 = CARTESIAN_POINT ( 'NONE',  ( -2.500000000000000444, 9.833333333333332149, -4.330127018922193649 ) ) ;
#26394 = CARTESIAN_POINT ( 'NONE',  ( -6.972266317189433020E-16, -36.25000000000000000, -5.000000000000000000 ) ) ;
#26395 = CARTESIAN_POINT ( 'NONE',  ( -4.458734124999999437, -37.31249999863440792, 0.000000000000000000 ) ) ;
#26396 = CARTESIAN_POINT ( 'NONE',  ( 2.493747252781420335E-13, -91.12499999726880162, -5.000000000000000000 ) ) ;
#26397 = CARTESIAN_POINT ( 'NONE',  ( -5.000000000000000000, -48.00000000000000000, 0.000000000000000000 ) ) ;
#26398 = CARTESIAN_POINT ( 'NONE',  ( -2.500000000000000444, 18.83333333333333215, -4.330127018922193649 ) ) ;
#26399 = CARTESIAN_POINT ( 'NONE',  ( 0.000000000000000000, -170.0000000000000000, 0.000000000000000000 ) ) ;
#26400 = EDGE_LOOP ( 'NONE', ( #47113, #16408, #26429, #17605 ) ) ;
#26401 = CARTESIAN_POINT ( 'NONE',  ( 2.229367062500001939, -105.9791666653010651, 3.861377020970579999 ) ) ;
#26402 = CARTESIAN_POINT ( 'NONE',  ( 4.458734124999999437, -3.062499998634407472, -5.460374474430324690E-16 ) ) ;
#26403 = VECTOR ( 'NONE', #11904, 1000.000000000000000 ) ;
#26404 = CARTESIAN_POINT ( 'NONE',  ( -2.480964764533239819E-13, -73.62499999726883004, 5.000000000000000000 ) ) ;
#26405 = CARTESIAN_POINT ( 'NONE',  ( -5.000000000000000000, -8.083333333333330373, -2.886751345948128211 ) ) ;
#26406 = CARTESIAN_POINT ( 'NONE',  ( -4.458734124999997661, -70.22916666530107932, 2.574251347313722516 ) ) ;
#26407 = AXIS2_PLACEMENT_3D ( 'NONE', #48040, #28730, #21800 ) ;
#26408 = CARTESIAN_POINT ( 'NONE',  ( -1.230605004983934782E-13, -25.75000000000000355, 5.000000000000000000 ) ) ;
#26409 = CARTESIAN_POINT ( 'NONE',  ( 5.000000000000000000, -7.291666663935481907, -2.886751345948129988 ) ) ;
#26411 = ORIENTED_EDGE ( 'NONE', *, *, #60517, .F. ) ;
#26410 = CARTESIAN_POINT ( 'NONE',  ( 4.458734124999999437, -39.81249999863440081, -5.460374474430324690E-16 ) ) ;
#26412 = AXIS2_PLACEMENT_3D ( 'NONE', #23466, #28902, #8661 ) ;
#26413 = CARTESIAN_POINT ( 'NONE',  ( 1.339745962155612702, -6.294658198738520838, -5.000000000000000000 ) ) ;
#26415 = EDGE_LOOP ( 'NONE', ( #62992, #56814, #51773, #42105 ) ) ;
#26414 = CARTESIAN_POINT ( 'NONE',  ( -3.152548672688508926E-16, 14.18750000136559386, -5.148502694627439702 ) ) ;
#26416 = CARTESIAN_POINT ( 'NONE',  ( 2.499999999999998668, -101.2083333306021444, -4.330127018922193649 ) ) ;
#26417 = CARTESIAN_POINT ( 'NONE',  ( 5.000000000000000000, -55.41666666666667140, -2.886751345948129988 ) ) ;
#26418 = CARTESIAN_POINT ( 'NONE',  ( -4.458734124999999437, -30.64583333196774007, -2.574251347313719407 ) ) ;
#26419 = CARTESIAN_POINT ( 'NONE',  ( -6.972266317189433020E-16, -10.24999999999999822, -5.000000000000000000 ) ) ;
#26420 = CARTESIAN_POINT ( 'NONE',  ( -4.458734124999998549, -75.22916666530106511, 2.574251347313722516 ) ) ;
#26421 = CARTESIAN_POINT ( 'NONE',  ( 3.061616997868383141E-16, -168.7500000000000000, -5.000000000000000000 ) ) ;
#26422 = CARTESIAN_POINT ( 'NONE',  ( -4.458734124999998549, -86.22916666530106511, 2.574251347313722516 ) ) ;
#26423 = CARTESIAN_POINT ( 'NONE',  ( -51.60603307380591787, -137.1875000013656063, -2.891590998281053704 ) ) ;
#26424 = CARTESIAN_POINT ( 'NONE',  ( 4.458734125000001214, -35.14583333196772941, 2.574251347313718519 ) ) ;
#26425 = CARTESIAN_POINT ( 'NONE',  ( -9.184850993605147944E-16, -150.3750000027312126, 5.000000000000000000 ) ) ;
#26426 = ORIENTED_EDGE ( 'NONE', *, *, #8291, .F. ) ;
#26427 = CARTESIAN_POINT ( 'NONE',  ( 4.458734125000001214, -81.14583333196773651, 2.574251347313718519 ) ) ;
#26428 = CARTESIAN_POINT ( 'NONE',  ( -5.000000000000000000, 13.12500000273118417, 0.000000000000000000 ) ) ;
#26429 = ORIENTED_EDGE ( 'NONE', *, *, #31510, .T. ) ;
#26430 = DIRECTION ( 'NONE',  ( -0.000000000000000000, 1.000000000000000000, -0.000000000000000000 ) ) ;
#26431 = CARTESIAN_POINT ( 'NONE',  ( -6.972266317189433020E-16, -19.12499999726880873, -5.000000000000000000 ) ) ;
#26432 = CARTESIAN_POINT ( 'NONE',  ( -3.152548672688508926E-16, -64.81249999863440792, -5.148502694627439702 ) ) ;
#26433 = CARTESIAN_POINT ( 'NONE',  ( 4.458734125000001214, -11.14583333196774007, 2.574251347313718519 ) ) ;
#26434 = ORIENTED_EDGE ( 'NONE', *, *, #60219, .T. ) ;
#26435 = CARTESIAN_POINT ( 'NONE',  ( -2.071067811865351604, -156.4375000027311842, 5.000000000000126121 ) ) ;
#26436 = ADVANCED_FACE ( 'NONE', ( #19631 ), #58868, .T. ) ;
#26437 = CARTESIAN_POINT ( 'NONE',  ( 0.000000000000000000, -120.0000000000000000, 5.000000000000000000 ) ) ;
#26438 = VERTEX_POINT ( 'NONE', #30550 ) ;
#26439 = CARTESIAN_POINT ( 'NONE',  ( -4.458734124999999437, -7.562499998634404363, 0.000000000000000000 ) ) ;
#26440 = CARTESIAN_POINT ( 'NONE',  ( 4.458734124999999437, 10.18750000136559386, -5.460374474430324690E-16 ) ) ;
#26441 = CARTESIAN_POINT ( 'NONE',  ( 2.071067811865264563, -153.8125000000000000, -5.000000000000211386 ) ) ;
#26442 = CARTESIAN_POINT ( 'NONE',  ( -4.458734125000000326, -157.8750000013655779, 1.846868145590734089 ) ) ;
#26443 = EDGE_CURVE ( 'NONE', #727, #22221, #20033, .T. ) ;
#26444 = VECTOR ( 'NONE', #48649, 1000.000000000000000 ) ;
#26445 = DIRECTION ( 'NONE',  ( -0.6485228581062915110, 0.000000000000000000, -0.7611951803011149931 ) ) ;
#26446 = VERTEX_POINT ( 'NONE', #6450 ) ;
#26447 = CARTESIAN_POINT ( 'NONE',  ( 2.229367062500001939, -86.97916666530107932, 3.861377020970579999 ) ) ;
#26448 = CARTESIAN_POINT ( 'NONE',  ( 0.000000000000000000, -170.0000000000000000, 0.000000000000000000 ) ) ;
#26449 = CARTESIAN_POINT ( 'NONE',  ( -3.152548672688508926E-16, -5.562499998634402587, -5.148502694627439702 ) ) ;
#26450 = AXIS2_PLACEMENT_3D ( 'NONE', #51412, #41423, #16993 ) ;
#26451 = EDGE_CURVE ( 'NONE', #50637, #6014, #47138, .T. ) ;
#26452 = DIRECTION ( 'NONE',  ( -0.000000000000000000, 1.000000000000000000, -0.000000000000000000 ) ) ;
#26453 =( BOUNDED_CURVE ( )  B_SPLINE_CURVE ( 2, ( #36252, #50412, #60068, #61341, #17263, #31409, #56517, #55244, #12438 ),
 .UNSPECIFIED., .F., .F. ) 
 B_SPLINE_CURVE_WITH_KNOTS ( ( 3, 2, 2, 2, 3 ),
 ( 0.04375000000000000416, 0.04444444444444444614, 0.04583333333333333010, 0.04722222222222222099, 0.04791666666666666990 ),
 .UNSPECIFIED. ) 
 CURVE ( )  GEOMETRIC_REPRESENTATION_ITEM ( )  RATIONAL_B_SPLINE_CURVE ( ( 0.9330127018922192983, 0.9330127018922196314, 1.000000000000000000, 0.8660254037844387076, 1.000000000000000000, 0.8660254037844387076, 1.000000000000000000, 0.9330127018922189652, 0.9330127018922192983 ) ) 
 REPRESENTATION_ITEM ( '' )  );
#26454 = VECTOR ( 'NONE', #43579, 1000.000000000000000 ) ;
#26455 = CARTESIAN_POINT ( 'NONE',  ( 5.000000000000000888, -28.45833333060214443, 2.886751345948126879 ) ) ;
#26456 = CARTESIAN_POINT ( 'NONE',  ( -6.972266317189433020E-16, -77.12499999726881583, -5.000000000000000000 ) ) ;
#26457 = CARTESIAN_POINT ( 'NONE',  ( -4.458734124999999437, 24.68750000136559208, 0.000000000000000000 ) ) ;
#26458 = CARTESIAN_POINT ( 'NONE',  ( -6.972266317189433020E-16, -110.1249999972688158, -5.000000000000000000 ) ) ;
#26459 = CARTESIAN_POINT ( 'NONE',  ( 1.339745962155615144, -58.70534180126147561, 4.999999999999999112 ) ) ;
#26460 = EDGE_CURVE ( 'NONE', #19049, #58767, #22533, .T. ) ;
#26461 = CARTESIAN_POINT ( 'NONE',  ( -4.458734124999998549, -50.22916666530107221, 2.574251347313722516 ) ) ;
#26462 = CARTESIAN_POINT ( 'NONE',  ( -4.458734124999999437, -37.64583333196774362, -2.574251347313719407 ) ) ;
#26463 = CARTESIAN_POINT ( 'NONE',  ( 4.458734124999999437, 1.937500001365593416, -5.460374474430324690E-16 ) ) ;
#26464 = CARTESIAN_POINT ( 'NONE',  ( -9.184850993605147944E-16, -160.3750000027311842, 5.000000000000000000 ) ) ;
#26465 = CARTESIAN_POINT ( 'NONE',  ( 5.000000000000000000, 15.58333333333333215, -2.886751345948129988 ) ) ;
#26466 = EDGE_CURVE ( 'NONE', #23647, #43124, #38117, .T. ) ;
#26467 = CARTESIAN_POINT ( 'NONE',  ( 5.000000000000000888, -147.0625000027311842, -2.071067811865475505 ) ) ;
#26468 = LINE ( 'NONE', #2043, #28459 ) ;
#26469 = CARTESIAN_POINT ( 'NONE',  ( 4.458734125000001214, -44.89583333196774362, 2.574251347313718519 ) ) ;
#26470 = CARTESIAN_POINT ( 'NONE',  ( 1.060575238724906964E-15, -78.62499999726880162, 5.773502691896257311 ) ) ;
#26471 = CARTESIAN_POINT ( 'NONE',  ( -57.19623071787017210, -141.6250000013656063, 4.297418129356382899 ) ) ;
#26472 = CARTESIAN_POINT ( 'NONE',  ( -6.972266317189433020E-16, -87.25000000000001421, -5.000000000000000000 ) ) ;
#26473 = EDGE_CURVE ( 'NONE', #23523, #57684, #1002, .T. ) ;
#26474 = CARTESIAN_POINT ( 'NONE',  ( -1.339745962155610925, -87.79465819873851729, 5.000000000000000000 ) ) ;
#26475 = CARTESIAN_POINT ( 'NONE',  ( 4.458734125000000326, -85.14583333196773651, 2.574251347313718519 ) ) ;
#26476 = CARTESIAN_POINT ( 'NONE',  ( -4.458734124999999437, -161.1875000013655779, -5.460374474430324690E-16 ) ) ;
#26477 = CARTESIAN_POINT ( 'NONE',  ( -6.484173630544109557, -4.916614646775610886, -7.642786413610934915 ) ) ;
#26478 = CARTESIAN_POINT ( 'NONE',  ( 2.500000000000002220, -27.66666666666666430, 4.330127018922192761 ) ) ;
#26479 = CARTESIAN_POINT ( 'NONE',  ( -3.152801135295367985, -140.8125000013655779, 3.152801135295367096 ) ) ;
#26480 = ORIENTED_EDGE ( 'NONE', *, *, #17333, .F. ) ;
#26481 = CARTESIAN_POINT ( 'NONE',  ( 4.458734125000001214, 22.85416666803225993, 2.574251347313718519 ) ) ;
#26482 = ORIENTED_EDGE ( 'NONE', *, *, #3249, .T. ) ;
#26483 = CARTESIAN_POINT ( 'NONE',  ( -2.229367062500000163, -89.47916666530106511, -3.861377020970580443 ) ) ;
#26484 = CARTESIAN_POINT ( 'NONE',  ( -4.458734124999999437, 12.43750000136559564, 0.000000000000000000 ) ) ;
#26485 = CARTESIAN_POINT ( 'NONE',  ( -2.500000000000000444, 14.95833333606451809, -4.330127018922193649 ) ) ;
#26486 = LINE ( 'NONE', #1107, #19588 ) ;
#26487 = CARTESIAN_POINT ( 'NONE',  ( -3.535250795749689387E-16, 9.749999999999998224, -5.773502691896257311 ) ) ;
#26488 = CARTESIAN_POINT ( 'NONE',  ( 2.229367062500001939, -55.97916666530107221, 3.861377020970579999 ) ) ;
#26489 = CARTESIAN_POINT ( 'NONE',  ( -2.229367062499996610, -14.14583333196774184, 3.861377020970582219 ) ) ;
#26490 = DIRECTION ( 'NONE',  ( -0.000000000000000000, 1.000000000000000000, -0.000000000000000000 ) ) ;
#26491 = CARTESIAN_POINT ( 'NONE',  ( -52.10840900171896806, -135.4375000013656063, 3.393966926194110556 ) ) ;
#26492 = DIRECTION ( 'NONE',  ( -0.000000000000000000, 1.000000000000000000, -0.000000000000000000 ) ) ;
#26493 = DIRECTION ( 'NONE',  ( -0.000000000000000000, 1.000000000000000000, -0.000000000000000000 ) ) ;
#26494 = CARTESIAN_POINT ( 'NONE',  ( -3.535250795749689387E-16, -37.25000000000001421, -5.773502691896257311 ) ) ;
#26495 = CARTESIAN_POINT ( 'NONE',  ( 6.123233995736766282E-16, -170.0000000000000000, -5.000000000000000000 ) ) ;
#26497 = CARTESIAN_POINT ( 'NONE',  ( 4.458734124999999437, -15.06249999863440436, -5.460374474430324690E-16 ) ) ;
#26496 = CARTESIAN_POINT ( 'NONE',  ( -53.33387254593703375, -138.8125000000000000, 5.149110718188541824 ) ) ;
#26498 = VECTOR ( 'NONE', #60644, 1000.000000000000227 ) ;
#26499 = CARTESIAN_POINT ( 'NONE',  ( 1.339745962155600711, 17.41965820146970145, 5.000000000000007994 ) ) ;
#26500 = CARTESIAN_POINT ( 'NONE',  ( 2.229367062500001939, -58.97916666530106511, 3.861377020970579999 ) ) ;
#26501 = CARTESIAN_POINT ( 'NONE',  ( 4.458734124999999437, -153.7500000013656063, 1.846868145590737864 ) ) ;
#26502 = CARTESIAN_POINT ( 'NONE',  ( -2.229367062499996610, -70.14583333196773651, 3.861377020970582219 ) ) ;
#26503 = AXIS2_PLACEMENT_3D ( 'NONE', #7552, #32616, #42580 ) ;
#26504 = CARTESIAN_POINT ( 'NONE',  ( -52.80376928212989185, -148.1250000013656063, -4.297418129356379346 ) ) ;
#26505 = CARTESIAN_POINT ( 'NONE',  ( -2.229367062500000163, -18.72916666530106866, -3.861377020970580443 ) ) ;
#26506 = CARTESIAN_POINT ( 'NONE',  ( -4.999999999999999112, -60.79166666393547303, 2.886751345948131764 ) ) ;
#26507 = ORIENTED_EDGE ( 'NONE', *, *, #17395, .T. ) ;
#26508 = ORIENTED_EDGE ( 'NONE', *, *, #9075, .T. ) ;
#26509 = CARTESIAN_POINT ( 'NONE',  ( -4.458734124999998549, -64.47916666530106511, 2.574251347313722516 ) ) ;
#26510 = DIRECTION ( 'NONE',  ( 0.000000000000000000, 0.000000000000000000, 1.000000000000000000 ) ) ;
#26511 = CARTESIAN_POINT ( 'NONE',  ( -4.458734125000001214, -150.8750000013655779, 1.846868145590734089 ) ) ;
#26512 = ORIENTED_EDGE ( 'NONE', *, *, #26466, .F. ) ;
#26513 = CARTESIAN_POINT ( 'NONE',  ( 1.975475456537005874E-15, -7.624999997268812280, 5.000000000000000000 ) ) ;
#26514 = CARTESIAN_POINT ( 'NONE',  ( 2.621086668468698644, 7.606368536631364030, -7.634085501268425666 ) ) ;
#26515 = CARTESIAN_POINT ( 'NONE',  ( 1.975475456537005874E-15, -64.62499999726880162, 5.000000000000000000 ) ) ;
#26516 = CARTESIAN_POINT ( 'NONE',  ( -2.229367062500000163, -48.72916666530106511, -3.861377020970580443 ) ) ;
#26517 = ORIENTED_EDGE ( 'NONE', *, *, #31885, .F. ) ;
#26518 = CARTESIAN_POINT ( 'NONE',  ( -1.339745962155610925, -109.6696581960073047, 5.000000000000000000 ) ) ;
#26519 = CARTESIAN_POINT ( 'NONE',  ( -2.229367062499996610, 9.854166668032261711, 3.861377020970582219 ) ) ;
#26520 = CARTESIAN_POINT ( 'NONE',  ( 4.458734125000001214, 26.10416666803225993, 2.574251347313718519 ) ) ;
#26521 = CARTESIAN_POINT ( 'NONE',  ( -56.48576386720575471, -148.7500000013655779, -4.591703134518078322 ) ) ;
#26522 = CARTESIAN_POINT ( 'NONE',  ( -55.39835681537999790, -150.0000000027312126, 4.984105922594378235 ) ) ;
#26523 = CARTESIAN_POINT ( 'NONE',  ( 6.123233995736766282E-16, -120.0000000000000000, -5.000000000000000000 ) ) ;
#26524 =( BOUNDED_CURVE ( )  B_SPLINE_CURVE ( 2, ( #62213, #18129, #61581, #12364, #31978, #36487, #61900, #2719, #57074, #27781, #56756, #12679, #28096, #31663, #37756, #22342, #7860, #51613, #32932, #47405, #41612, #42573, #47714, #51299, #41940, #42884, #57388, #7546, #26849, #17516, #52555, #3669, #37136, #56114, #23282, #12038, #46462, #2405, #43196, #9730, #19386, #49296, #62530, #53486, #39002, #8797, #9110, #28717, #58004, #54112, #9415, #48341, #58634, #5236, #48963, #24535, #108, #23599, #62838, #3979, #29025, #48650, #18449, #43821, #24856, #14244, #38072, #63467, #19704, #57700, #58319, #52864, #13626, #34173, #33867, #4592, #33244, #29333, #39313, #43506, #28409, #4915, #18753, #38377, #24215, #44138, #4287, #14554, #48029, #10052, #53796, #58941, #23905, #14871, #13930, #34480, #29665, #33555, #53176, #63151, #19062, #38680, #21305, #30627, #20349, #35462, #740, #36097, #55724, #55406, #50893, #1071, #59267, #15199, #39948, #60555, #45105, #35784, #44460, #419, #26128, #25484, #44778, #59596, #20023, #6197, #10693, #45425, #1390, #20677, #40283, #11638, #34824, #45748, #30303, #59921, #15529, #40910, #15843, #49613, #25164, #31259, #54447, #54765, #6835, #11322, #35149, #10375, #49923, #50249, #1702, #5876, #39629, #55083, #11005, #20990, #16477, #25812, #30947, #40594, #60239, #29983, #16157, #50573, #5552, #6516, #36734, #21939, #18050, #17438, #56366, #22585, #13231, #12909, #52160, #27707, #51219, #26766, #31585, #37055, #22900, #46064, #7784, #52482, #41861, #26442, #27387, #47334, #2024, #22262, #16794, #32854, #61822, #61508, #56683, #21629, #37364, #3284, #7470, #41221, #27079, #7156, #46386, #12599, #8103, #12288, #42183, #36412, #37672, #17747, #41537, #31904, #56994, #60868, #56042, #2332, #62132, #47019, #11958, #61189, #32212, #17111, #32531, #51533, #46695, #51841, #42495, #2643, #2969, #57313, #8416, #13854, #19308, #38922, #29263, #23198, #48260, #47638, #18989, #28019, #53408, #38604, #9654, #9340, #33477, #53099, #14795, #58557, #34407, #39237, #4836, #47948, #26, #34098, #53723, #42811, #58863, #58237, #14477, #13554, #52788, #3902, #63390, #3593, #4517, #63079, #14164, #48891, #4218, #62451, #28645, #48577, #24143, #33792, #9033, #43746, #8720, #24455, #44061, #18373, #23831, #28954, #19627, #37994, #57626, #33173, #23521, #28334, #43122, #62762, #18682, #38308, #57935, #43434, #5157, #24777, #29906, #6446, #54687, #45352, #54036, #59194, #19941, #44698, #5794, #10298, #40835, #21229, #34743, #60480, #16083, #59842, #35707, #55334, #50170, #20272, #50503, #998, #29585, #59518, #26055, #15123, #54371, #15767, #6124, #25738, #9974, #20602, #44380, #49217, #30223, #11251, #20914, #16405, #45669, #341, #55003, #49534, #39553, #1628, #5475, #15453, #1319, #40518, #30875, #25090, #49848, #663, #40206, #39871, #35383, #35070, #25411, #10610, #10931, #45030, #30546, #60162, #26367, #22827, #7715, #11880, #27634, #61748, #17675, #50818, #3207, #2570, #22507, #41149, #16722, #31829, #37290, #21869, #32136, #45986, #47262, #27319, #51144, #46309, #46948, #12524, #51771, #46624, #61116, #2895, #36338, #12837, #32457, #1952, #51460, #31189, #42102, #42417, #22186, #36023, #55969, #8027, #56919, #31499, #7078, #52089, #62060, #56285, #6755, #21553, #26692, #55655, #36656, #11569, #60796, #2266, #41465, #17040, #12211, #7398, #27005, #41787, #61431, #17355, #36979, #56607, #13783, #9587, #32778, #63311, #47870, #33405, #57554, #14409, #53020, #23127, #62376, #23764, #33718, #53337, #37597, #28571, #8343, #17973, #57861, #4145, #38849, #8645, #57241, #48192, #8961, #18918, #58483, #18299, #28886, #38532, #58160, #42731, #48507, #43363, #37922, #9270, #13157, #27942, #63009, #14092, #3830, #4445, #24074, #23449, #34031, #43670, #52412, #43053, #53652, #3516, #24385, #19233, #29193, #47565, #28258, #43986, #48819, #52711, #13480 ),
 .UNSPECIFIED., .F., .F. ) 
 B_SPLINE_CURVE_WITH_KNOTS ( ( 3, 2, 2, 2, 2, 2, 2, 2, 2, 2, 2, 2, 2, 2, 2, 2, 2, 2, 2, 2, 2, 2, 2, 2, 2, 2, 2, 2, 2, 2, 2, 2, 2, 2, 2, 2, 2, 2, 2, 2, 2, 2, 2, 2, 2, 2, 2, 2, 2, 2, 2, 2, 2, 2, 2, 2, 2, 2, 2, 2, 2, 2, 2, 2, 2, 2, 2, 2, 2, 2, 2, 2, 2, 2, 2, 2, 2, 2, 2, 2, 2, 2, 2, 2, 2, 2, 2, 2, 2, 2, 2, 2, 2, 2, 2, 2, 2, 2, 2, 2, 2, 2, 2, 2, 2, 2, 2, 2, 2, 2, 2, 2, 2, 2, 2, 2, 2, 2, 2, 2, 2, 2, 2, 2, 2, 2, 2, 2, 2, 2, 2, 2, 2, 2, 2, 2, 2, 2, 2, 2, 2, 2, 2, 2, 2, 2, 2, 2, 2, 2, 2, 2, 2, 2, 2, 2, 2, 2, 2, 2, 2, 2, 2, 2, 2, 2, 2, 2, 2, 2, 2, 2, 2, 2, 2, 2, 2, 2, 2, 2, 2, 2, 2, 2, 2, 2, 2, 2, 2, 2, 2, 2, 2, 2, 2, 2, 2, 2, 2, 2, 2, 2, 2, 2, 2, 2, 2, 2, 2, 2, 2, 2, 2, 2, 2, 2, 2, 2, 2, 2, 2, 2, 2, 2, 2, 2, 2, 2, 2, 2, 2, 2, 2, 2, 2, 2, 2, 2, 2, 2, 3 ),
 ( 0.000000000000000000, 0.004166666666666666609, 0.008333333333333333218, 0.01250000000000000069, 0.01666666666666666644, 0.02083333333333333218, 0.02500000000000000139, 0.02916666666666666713, 0.03333333333333333287, 0.03749999999999999861, 0.04166666666666666435, 0.04583333333333333010, 0.05000000000000000278, 0.05416666666666666852, 0.05833333333333333426, 0.06250000000000000000, 0.06666666666666666574, 0.07083333333333333148, 0.07499999999999999722, 0.07916666666666666297, 0.08333333333333332871, 0.08749999999999999445, 0.09166666666666666019, 0.09583333333333333981, 0.1000000000000000056, 0.1041666666666666713, 0.1083333333333333370, 0.1125000000000000028, 0.1166666666666666685, 0.1208333333333333343, 0.1250000000000000000, 0.1291666666666666796, 0.1333333333333333315, 0.1375000000000000111, 0.1416666666666666630, 0.1458333333333333426, 0.1499999999999999944, 0.1541666666666666741, 0.1583333333333333259, 0.1625000000000000056, 0.1666666666666666574, 0.1708333333333333370, 0.1749999999999999889, 0.1791666666666666685, 0.1833333333333333204, 0.1875000000000000000, 0.1916666666666666796, 0.1958333333333333315, 0.2000000000000000111, 0.2041666666666666630, 0.2083333333333333426, 0.2124999999999999944, 0.2166666666666666741, 0.2208333333333333259, 0.2250000000000000056, 0.2291666666666666574, 0.2333333333333333370, 0.2374999999999999889, 0.2416666666666666685, 0.2458333333333333204, 0.2500000000000000000, 0.2541666666666666519, 0.2583333333333333592, 0.2625000000000000111, 0.2666666666666666630, 0.2708333333333333148, 0.2750000000000000222, 0.2791666666666666741, 0.2833333333333333259, 0.2874999999999999778, 0.2916666666666666852, 0.2958333333333333370, 0.2999999999999999889, 0.3041666666666666408, 0.3083333333333333481, 0.3125000000000000000, 0.3166666666666666519, 0.3208333333333333592, 0.3250000000000000111, 0.3291666666666666630, 0.3333333333333333148, 0.3375000000000000222, 0.3416666666666666741, 0.3458333333333333259, 0.3499999999999999778, 0.3541666666666666852, 0.3583333333333333370, 0.3624999999999999889, 0.3666666666666666408, 0.3708333333333333481, 0.3750000000000000000, 0.3791666666666666519, 0.3833333333333333592, 0.3875000000000000111, 0.3916666666666666630, 0.3958333333333333148, 0.4000000000000000222, 0.4041666666666666741, 0.4083333333333333259, 0.4124999999999999778, 0.4166666666666666852, 0.4208333333333333370, 0.4249999999999999889, 0.4291666666666666408, 0.4333333333333333481, 0.4375000000000000000, 0.4416666666666666519, 0.4458333333333333592, 0.4500000000000000111, 0.4541666666666666630, 0.4583333333333333148, 0.4625000000000000222, 0.4666666666666666741, 0.4708333333333333259, 0.4749999999999999778, 0.4791666666666666852, 0.4833333333333333370, 0.4874999999999999889, 0.4916666666666666408, 0.4958333333333333481, 0.5000000000000000000, 0.5041666666666666519, 0.5083333333333333037, 0.5124999999999999556, 0.5166666666666667185, 0.5208333333333333703, 0.5250000000000000222, 0.5291666666666666741, 0.5333333333333333259, 0.5374999999999999778, 0.5416666666666666297, 0.5458333333333332815, 0.5500000000000000444, 0.5541666666666666963, 0.5583333333333333481, 0.5625000000000000000, 0.5666666666666666519, 0.5708333333333333037, 0.5749999999999999556, 0.5791666666666667185, 0.5833333333333333703, 0.5875000000000000222, 0.5916666666666666741, 0.5958333333333333259, 0.5999999999999999778, 0.6041666666666666297, 0.6083333333333332815, 0.6125000000000000444, 0.6166666666666666963, 0.6208333333333333481, 0.6250000000000000000, 0.6291666666666666519, 0.6333333333333333037, 0.6374999999999999556, 0.6416666666666667185, 0.6458333333333333703, 0.6500000000000000222, 0.6541666666666666741, 0.6583333333333333259, 0.6624999999999999778, 0.6666666666666666297, 0.6708333333333332815, 0.6750000000000000444, 0.6791666666666666963, 0.6833333333333333481, 0.6875000000000000000, 0.6916666666666666519, 0.6958333333333333037, 0.6999999999999999556, 0.7041666666666667185, 0.7083333333333333703, 0.7125000000000000222, 0.7166666666666666741, 0.7208333333333333259, 0.7249999999999999778, 0.7291666666666666297, 0.7333333333333332815, 0.7375000000000000444, 0.7416666666666666963, 0.7458333333333333481, 0.7500000000000000000, 0.7541666666666666519, 0.7583333333333333037, 0.7624999999999999556, 0.7666666666666667185, 0.7708333333333333703, 0.7750000000000000222, 0.7791666666666666741, 0.7833333333333333259, 0.7874999999999999778, 0.7916666666666666297, 0.7958333333333332815, 0.8000000000000000444, 0.8041666666666666963, 0.8083333333333333481, 0.8125000000000000000, 0.8166666666666666519, 0.8208333333333333037, 0.8249999999999999556, 0.8291666666666667185, 0.8333333333333333703, 0.8375000000000000222, 0.8416666666666666741, 0.8458333333333333259, 0.8499999999999999778, 0.8541666666666666297, 0.8583333333333332815, 0.8625000000000000444, 0.8666666666666666963, 0.8708333333333333481, 0.8750000000000000000, 0.8791666666666666519, 0.8833333333333333037, 0.8874999999999999556, 0.8916666666666667185, 0.8958333333333333703, 0.9000000000000000222, 0.9041666666666666741, 0.9083333333333333259, 0.9124999999999999778, 0.9166666666666666297, 0.9208333333333332815, 0.9250000000000000444, 0.9291666666666666963, 0.9333333333333333481, 0.9375000000000000000, 0.9416666666666666519, 0.9458333333333333037, 0.9499999999999999556, 0.9541666666666667185, 0.9583333333333333703, 0.9625000000000000222, 0.9666666666666666741, 0.9708333333333333259, 0.9749999999999999778, 0.9791666666666666297, 0.9833333333333332815, 0.9875000000000000444, 0.9916666666666666963, 0.9958333333333333481, 1.000000000000000000 ),
 .UNSPECIFIED. ) 
 CURVE ( )  GEOMETRIC_REPRESENTATION_ITEM ( )  RATIONAL_B_SPLINE_CURVE ( ( 1.000000000000000000, 0.9238795325112867385, 1.000000000000000000, 0.9238795325112867385, 1.000000000000000000, 0.9238795325112867385, 1.000000000000000000, 0.9238795325112867385, 1.000000000000000000, 0.9238795325112867385, 1.000000000000000000, 0.9238795325112867385, 1.000000000000000000, 0.9238795325112867385, 1.000000000000000000, 0.9238795325112867385, 1.000000000000000000, 0.9238795325112867385, 1.000000000000000000, 0.9238795325112867385, 1.000000000000000000, 0.9238795325112867385, 1.000000000000000000, 0.9238795325112867385, 1.000000000000000000, 0.9238795325112867385, 1.000000000000000000, 0.9238795325112867385, 1.000000000000000000, 0.9238795325112867385, 1.000000000000000000, 0.9238795325112867385, 1.000000000000000000, 0.9238795325112867385, 1.000000000000000000, 0.9238795325112867385, 1.000000000000000000, 0.9238795325112867385, 1.000000000000000000, 0.9238795325112867385, 1.000000000000000000, 0.9238795325112867385, 1.000000000000000000, 0.9238795325112867385, 1.000000000000000000, 0.9238795325112867385, 1.000000000000000000, 0.9238795325112867385, 1.000000000000000000, 0.9238795325112867385, 1.000000000000000000, 0.9238795325112867385, 1.000000000000000000, 0.9238795325112867385, 1.000000000000000000, 0.9238795325112867385, 1.000000000000000000, 0.9238795325112867385, 1.000000000000000000, 0.9238795325112867385, 1.000000000000000000, 0.9238795325112867385, 1.000000000000000000, 0.9238795325112867385, 1.000000000000000000, 0.9238795325112867385, 1.000000000000000000, 0.9238795325112867385, 1.000000000000000000, 0.9238795325112867385, 1.000000000000000000, 0.9238795325112867385, 1.000000000000000000, 0.9238795325112867385, 1.000000000000000000, 0.9238795325112867385, 1.000000000000000000, 0.9238795325112867385, 1.000000000000000000, 0.9238795325112867385, 1.000000000000000000, 0.9238795325112867385, 1.000000000000000000, 0.9238795325112867385, 1.000000000000000000, 0.9238795325112867385, 1.000000000000000000, 0.9238795325112867385, 1.000000000000000000, 0.9238795325112867385, 1.000000000000000000, 0.9238795325112867385, 1.000000000000000000, 0.9238795325112867385, 1.000000000000000000, 0.9238795325112867385, 1.000000000000000000, 0.9238795325112867385, 1.000000000000000000, 0.9238795325112867385, 1.000000000000000000, 0.9238795325112867385, 1.000000000000000000, 0.9238795325112867385, 1.000000000000000000, 0.9238795325112867385, 1.000000000000000000, 0.9238795325112867385, 1.000000000000000000, 0.9238795325112867385, 1.000000000000000000, 0.9238795325112867385, 1.000000000000000000, 0.9238795325112867385, 1.000000000000000000, 0.9238795325112867385, 1.000000000000000000, 0.9238795325112867385, 1.000000000000000000, 0.9238795325112867385, 1.000000000000000000, 0.9238795325112867385, 1.000000000000000000, 0.9238795325112867385, 1.000000000000000000, 0.9238795325112867385, 1.000000000000000000, 0.9238795325112867385, 1.000000000000000000, 0.9238795325112867385, 1.000000000000000000, 0.9238795325112867385, 1.000000000000000000, 0.9238795325112867385, 1.000000000000000000, 0.9238795325112867385, 1.000000000000000000, 0.9238795325112867385, 1.000000000000000000, 0.9238795325112867385, 1.000000000000000000, 0.9238795325112867385, 1.000000000000000000, 0.9238795325112867385, 1.000000000000000000, 0.9238795325112867385, 1.000000000000000000, 0.9238795325112867385, 1.000000000000000000, 0.9238795325112867385, 1.000000000000000000, 0.9238795325112867385, 1.000000000000000000, 0.9238795325112867385, 1.000000000000000000, 0.9238795325112867385, 1.000000000000000000, 0.9238795325112867385, 1.000000000000000000, 0.9238795325112867385, 1.000000000000000000, 0.9238795325112867385, 1.000000000000000000, 0.9238795325112867385, 1.000000000000000000, 0.9238795325112867385, 1.000000000000000000, 0.9238795325112867385, 1.000000000000000000, 0.9238795325112867385, 1.000000000000000000, 0.9238795325112867385, 1.000000000000000000, 0.9238795325112867385, 1.000000000000000000, 0.9238795325112867385, 1.000000000000000000, 0.9238795325112867385, 1.000000000000000000, 0.9238795325112867385, 1.000000000000000000, 0.9238795325112867385, 1.000000000000000000, 0.9238795325112867385, 1.000000000000000000, 0.9238795325112867385, 1.000000000000000000, 0.9238795325112867385, 1.000000000000000000, 0.9238795325112867385, 1.000000000000000000, 0.9238795325112867385, 1.000000000000000000, 0.9238795325112867385, 1.000000000000000000, 0.9238795325112867385, 1.000000000000000000, 0.9238795325112867385, 1.000000000000000000, 0.9238795325112867385, 1.000000000000000000, 0.9238795325112867385, 1.000000000000000000, 0.9238795325112867385, 1.000000000000000000, 0.9238795325112867385, 1.000000000000000000, 0.9238795325112867385, 1.000000000000000000, 0.9238795325112867385, 1.000000000000000000, 0.9238795325112867385, 1.000000000000000000, 0.9238795325112867385, 1.000000000000000000, 0.9238795325112867385, 1.000000000000000000, 0.9238795325112867385, 1.000000000000000000, 0.9238795325112867385, 1.000000000000000000, 0.9238795325112867385, 1.000000000000000000, 0.9238795325112867385, 1.000000000000000000, 0.9238795325112867385, 1.000000000000000000, 0.9238795325112867385, 1.000000000000000000, 0.9238795325112867385, 1.000000000000000000, 0.9238795325112867385, 1.000000000000000000, 0.9238795325112867385, 1.000000000000000000, 0.9238795325112867385, 1.000000000000000000, 0.9238795325112867385, 1.000000000000000000, 0.9238795325112867385, 1.000000000000000000, 0.9238795325112867385, 1.000000000000000000, 0.9238795325112867385, 1.000000000000000000, 0.9238795325112867385, 1.000000000000000000, 0.9238795325112867385, 1.000000000000000000, 0.9238795325112867385, 1.000000000000000000, 0.9238795325112867385, 1.000000000000000000, 0.9238795325112867385, 1.000000000000000000, 0.9238795325112867385, 1.000000000000000000, 0.9238795325112867385, 1.000000000000000000, 0.9238795325112867385, 1.000000000000000000, 0.9238795325112867385, 1.000000000000000000, 0.9238795325112867385, 1.000000000000000000, 0.9238795325112867385, 1.000000000000000000, 0.9238795325112867385, 1.000000000000000000, 0.9238795325112867385, 1.000000000000000000, 0.9238795325112867385, 1.000000000000000000, 0.9238795325112867385, 1.000000000000000000, 0.9238795325112867385, 1.000000000000000000, 0.9238795325112867385, 1.000000000000000000, 0.9238795325112867385, 1.000000000000000000, 0.9238795325112867385, 1.000000000000000000, 0.9238795325112867385, 1.000000000000000000, 0.9238795325112867385, 1.000000000000000000, 0.9238795325112867385, 1.000000000000000000, 0.9238795325112867385, 1.000000000000000000, 0.9238795325112867385, 1.000000000000000000, 0.9238795325112867385, 1.000000000000000000, 0.9238795325112867385, 1.000000000000000000, 0.9238795325112867385, 1.000000000000000000, 0.9238795325112867385, 1.000000000000000000, 0.9238795325112867385, 1.000000000000000000, 0.9238795325112867385, 1.000000000000000000, 0.9238795325112867385, 1.000000000000000000, 0.9238795325112867385, 1.000000000000000000, 0.9238795325112867385, 1.000000000000000000, 0.9238795325112867385, 1.000000000000000000, 0.9238795325112867385, 1.000000000000000000, 0.9238795325112867385, 1.000000000000000000, 0.9238795325112867385, 1.000000000000000000, 0.9238795325112867385, 1.000000000000000000, 0.9238795325112867385, 1.000000000000000000, 0.9238795325112867385, 1.000000000000000000, 0.9238795325112867385, 1.000000000000000000, 0.9238795325112867385, 1.000000000000000000, 0.9238795325112867385, 1.000000000000000000, 0.9238795325112867385, 1.000000000000000000, 0.9238795325112867385, 1.000000000000000000, 0.9238795325112867385, 1.000000000000000000, 0.9238795325112867385, 1.000000000000000000, 0.9238795325112867385, 1.000000000000000000, 0.9238795325112867385, 1.000000000000000000, 0.9238795325112867385, 1.000000000000000000, 0.9238795325112867385, 1.000000000000000000, 0.9238795325112867385, 1.000000000000000000, 0.9238795325112867385, 1.000000000000000000, 0.9238795325112867385, 1.000000000000000000, 0.9238795325112867385, 1.000000000000000000, 0.9238795325112867385, 1.000000000000000000, 0.9238795325112867385, 1.000000000000000000, 0.9238795325112867385, 1.000000000000000000, 0.9238795325112867385, 1.000000000000000000, 0.9238795325112867385, 1.000000000000000000, 0.9238795325112867385, 1.000000000000000000, 0.9238795325112867385, 1.000000000000000000, 0.9238795325112867385, 1.000000000000000000, 0.9238795325112867385, 1.000000000000000000, 0.9238795325112867385, 1.000000000000000000, 0.9238795325112867385, 1.000000000000000000, 0.9238795325112867385, 1.000000000000000000, 0.9238795325112867385, 1.000000000000000000, 0.9238795325112867385, 1.000000000000000000, 0.9238795325112867385, 1.000000000000000000, 0.9238795325112867385, 1.000000000000000000, 0.9238795325112867385, 1.000000000000000000, 0.9238795325112867385, 1.000000000000000000, 0.9238795325112867385, 1.000000000000000000, 0.9238795325112867385, 1.000000000000000000, 0.9238795325112867385, 1.000000000000000000, 0.9238795325112867385, 1.000000000000000000, 0.9238795325112867385, 1.000000000000000000, 0.9238795325112867385, 1.000000000000000000, 0.9238795325112867385, 1.000000000000000000, 0.9238795325112867385, 1.000000000000000000, 0.9238795325112867385, 1.000000000000000000, 0.9238795325112867385, 1.000000000000000000, 0.9238795325112867385, 1.000000000000000000, 0.9238795325112867385, 1.000000000000000000, 0.9238795325112867385, 1.000000000000000000, 0.9238795325112867385, 1.000000000000000000, 0.9238795325112867385, 1.000000000000000000, 0.9238795325112867385, 1.000000000000000000, 0.9238795325112867385, 1.000000000000000000, 0.9238795325112867385, 1.000000000000000000, 0.9238795325112867385, 1.000000000000000000, 0.9238795325112867385, 1.000000000000000000, 0.9238795325112867385, 1.000000000000000000, 0.9238795325112867385, 1.000000000000000000, 0.9238795325112867385, 1.000000000000000000, 0.9238795325112867385, 1.000000000000000000, 0.9238795325112867385, 1.000000000000000000, 0.9238795325112867385, 1.000000000000000000, 0.9238795325112867385, 1.000000000000000000, 0.9238795325112867385, 1.000000000000000000, 0.9238795325112867385, 1.000000000000000000, 0.9238795325112867385, 1.000000000000000000, 0.9238795325112867385, 1.000000000000000000, 0.9238795325112867385, 1.000000000000000000, 0.9238795325112867385, 1.000000000000000000, 0.9238795325112867385, 1.000000000000000000, 0.9238795325112867385, 1.000000000000000000, 0.9238795325112867385, 1.000000000000000000, 0.9238795325112867385, 1.000000000000000000, 0.9238795325112867385, 1.000000000000000000, 0.9238795325112867385, 1.000000000000000000, 0.9238795325112867385, 1.000000000000000000, 0.9238795325112867385, 1.000000000000000000, 0.9238795325112867385, 1.000000000000000000, 0.9238795325112867385, 1.000000000000000000, 0.9238795325112867385, 1.000000000000000000, 0.9238795325112867385, 1.000000000000000000 ) ) 
 REPRESENTATION_ITEM ( '' )  );
#26525 = ORIENTED_EDGE ( 'NONE', *, *, #48349, .F. ) ;
#26526 = CARTESIAN_POINT ( 'NONE',  ( -4.458734124999997661, -71.22916666530107932, 2.574251347313722516 ) ) ;
#26527 = CARTESIAN_POINT ( 'NONE',  ( 0.000000000000000000, -120.0000000000000000, 5.000000000000000000 ) ) ;
#26528 = CARTESIAN_POINT ( 'NONE',  ( 2.229367062499998831, 10.35416666803225993, -3.861377020970580887 ) ) ;
#26529 = CARTESIAN_POINT ( 'NONE',  ( -2.500000000000000444, -63.16666666666666430, -4.330127018922193649 ) ) ;
#26530 = CARTESIAN_POINT ( 'NONE',  ( 5.000000000000000000, -169.1250000027312126, 0.000000000000000000 ) ) ;
#26531 = CARTESIAN_POINT ( 'NONE',  ( -4.458734124999999437, -56.64583333196773651, -2.574251347313719407 ) ) ;
#26532 = CARTESIAN_POINT ( 'NONE',  ( 2.499999999999998668, -15.20833333060214443, -4.330127018922193649 ) ) ;
#26533 = DIRECTION ( 'NONE',  ( -0.000000000000000000, 1.000000000000000000, -0.000000000000000000 ) ) ;
#26534 = CARTESIAN_POINT ( 'NONE',  ( -2.229367062500000163, -22.72916666530107221, -3.861377020970580443 ) ) ;
#26535 = ORIENTED_EDGE ( 'NONE', *, *, #40185, .T. ) ;
#26536 = VECTOR ( 'NONE', #2964, 1000.000000000000000 ) ;
#26537 = CARTESIAN_POINT ( 'NONE',  ( -2.499999999999996447, -4.708333330602147981, 4.330127018922195425 ) ) ;
#26538 = CARTESIAN_POINT ( 'NONE',  ( 5.000000000000000000, 29.50000000000000000, -6.123233995736766282E-16 ) ) ;
#26540 = CARTESIAN_POINT ( 'NONE',  ( -3.535533905932738641, -157.5000000027312126, 3.535533905932737309 ) ) ;
#26539 =( REPRESENTATION_RELATIONSHIP ('NONE','NONE', #27855, #21293 ) REPRESENTATION_RELATIONSHIP_WITH_TRANSFORMATION ( #34319 )SHAPE_REPRESENTATION_RELATIONSHIP( ) );
#26541 = VERTEX_POINT ( 'NONE', #36027 ) ;
#26542 = CARTESIAN_POINT ( 'NONE',  ( -3.152548672688508926E-16, -103.8124999986344221, -5.148502694627439702 ) ) ;
#26543 = AXIS2_PLACEMENT_3D ( 'NONE', #24269, #34885, #49987 ) ;
#26544 = CARTESIAN_POINT ( 'NONE',  ( -4.458734124999999437, -27.31249999863440081, 0.000000000000000000 ) ) ;
#26545 = CARTESIAN_POINT ( 'NONE',  ( -2.499999999999996447, -63.70833333060215153, 4.330127018922195425 ) ) ;
#26546 = CARTESIAN_POINT ( 'NONE',  ( -50.55543936806279248, -152.3125000013656063, 0.3552334253322060320 ) ) ;
#26547 = CARTESIAN_POINT ( 'NONE',  ( -52.80376928212989185, -142.8750000013656063, -4.297418129356378458 ) ) ;
#26548 = CARTESIAN_POINT ( 'NONE',  ( -3.152548672688508926E-16, -23.56249999863440436, -5.148502694627439702 ) ) ;
#26549 = CARTESIAN_POINT ( 'NONE',  ( -2.229367062500000163, -71.72916666530107932, -3.861377020970580443 ) ) ;
#26550 = CARTESIAN_POINT ( 'NONE',  ( 0.000000000000000000, -120.0000000000000000, 5.000000000000000000 ) ) ;
#26551 = CARTESIAN_POINT ( 'NONE',  ( -4.458734124999999437, -27.31249999863440081, 0.000000000000000000 ) ) ;
#26552 = CARTESIAN_POINT ( 'NONE',  ( -9.184850993605147944E-16, -147.2500000000000284, 5.000000000000000000 ) ) ;
#26553 = CARTESIAN_POINT ( 'NONE',  ( -5.000000000000000888, -151.4375000000000000, 2.071067811865474617 ) ) ;
#26554 = CARTESIAN_POINT ( 'NONE',  ( 2.499999999999998668, -10.33333333333333393, -4.330127018922193649 ) ) ;
#26555 = CARTESIAN_POINT ( 'NONE',  ( 3.152801135295366208, -152.5625000013655779, 3.152801135295367985 ) ) ;
#26556 = VERTEX_POINT ( 'NONE', #21233 ) ;
#26557 = CARTESIAN_POINT ( 'NONE',  ( 2.229367062499998831, -52.89583333196773651, -3.861377020970580887 ) ) ;
#26558 =( BOUNDED_CURVE ( )  B_SPLINE_CURVE ( 2, ( #14882, #29994, #40606, #16170, #50584, #25176, #35795, #44148, #39640 ),
 .UNSPECIFIED., .F., .F. ) 
 B_SPLINE_CURVE_WITH_KNOTS ( ( 3, 2, 2, 2, 3 ),
 ( 0.2124999999999999944, 0.2130952380952380876, 0.2142857142857142738, 0.2154761904761904878, 0.2160714285714285809 ),
 .UNSPECIFIED. ) 
 CURVE ( )  GEOMETRIC_REPRESENTATION_ITEM ( )  RATIONAL_B_SPLINE_CURVE ( ( 0.9330127018922194093, 0.9330127018922194093, 1.000000000000000000, 0.8660254037844387076, 1.000000000000000000, 0.8660254037844387076, 1.000000000000000000, 0.9330127018922194093, 0.9330127018922194093 ) ) 
 REPRESENTATION_ITEM ( '' )  );
#26559 = CARTESIAN_POINT ( 'NONE',  ( -5.000000000000000000, -2.874999997268815832, 0.000000000000000000 ) ) ;
#26560 = CARTESIAN_POINT ( 'NONE',  ( 2.500000000000002220, -90.66666666666665719, 4.330127018922192761 ) ) ;
#26561 = CARTESIAN_POINT ( 'NONE',  ( -5.000000000000000000, 21.91666666666666785, -2.886751345948128211 ) ) ;
#26562 = AXIS2_PLACEMENT_3D ( 'NONE', #24618, #38454, #58403 ) ;
#26563 = CARTESIAN_POINT ( 'NONE',  ( 5.000000000000000000, 25.58333333333333215, -2.886751345948130876 ) ) ;
#26564 = CARTESIAN_POINT ( 'NONE',  ( 4.458734124999998549, 6.270833334698928674, -2.574251347313721627 ) ) ;
#26565 = DIRECTION ( 'NONE',  ( -1.000000000000000000, 0.000000000000000000, 0.000000000000000000 ) ) ;
#26566 = CARTESIAN_POINT ( 'NONE',  ( -5.000000000000000000, 29.56250000136559208, 0.000000000000000000 ) ) ;
#26567 = CARTESIAN_POINT ( 'NONE',  ( 5.000000000000000888, -7.583333333333330373, 2.886751345948126879 ) ) ;
#26568 = CARTESIAN_POINT ( 'NONE',  ( 4.458734125000001214, 16.85416666803225638, 2.574251347313718519 ) ) ;
#26569 = AXIS2_PLACEMENT_3D ( 'NONE', #60155, #35702, #658 ) ;
#26570 = CARTESIAN_POINT ( 'NONE',  ( 5.000000000000000000, 3.708333336064517205, -2.886751345948129988 ) ) ;
#26571 = ORIENTED_EDGE ( 'NONE', *, *, #51583, .F. ) ;
#26572 = CARTESIAN_POINT ( 'NONE',  ( -6.972266317189433020E-16, -42.24999999999998579, -5.000000000000000000 ) ) ;
#26573 = ORIENTED_EDGE ( 'NONE', *, *, #12582, .T. ) ;
#26574 = CARTESIAN_POINT ( 'NONE',  ( -1.339745962155613812, -54.08034179853029144, -5.000000000000000000 ) ) ;
#26575 = CARTESIAN_POINT ( 'NONE',  ( -2.229367062500000163, -43.47916666530106511, -3.861377020970580443 ) ) ;
#26576 = CARTESIAN_POINT ( 'NONE',  ( -4.458734125000000326, -165.2500000013655779, -1.846868145590735644 ) ) ;
#26577 = CARTESIAN_POINT ( 'NONE',  ( -2.499999999999996447, -42.70833333060214443, 4.330127018922195425 ) ) ;
#26578 = ORIENTED_EDGE ( 'NONE', *, *, #38048, .F. ) ;
#26579 = CARTESIAN_POINT ( 'NONE',  ( 4.458734124999998549, -18.72916666530106866, -2.574251347313721627 ) ) ;
#26580 = ORIENTED_EDGE ( 'NONE', *, *, #50061, .T. ) ;
#26581 = CARTESIAN_POINT ( 'NONE',  ( 5.000000000000000000, -89.50000000000000000, -6.123233995736766282E-16 ) ) ;
#26582 = CARTESIAN_POINT ( 'NONE',  ( 3.152801135295366208, -163.5625000013656063, 3.152801135295367985 ) ) ;
#26583 = VECTOR ( 'NONE', #30029, 1000.000000000000000 ) ;
#26585 = ORIENTED_EDGE ( 'NONE', *, *, #39305, .F. ) ;
#26584 = CARTESIAN_POINT ( 'NONE',  ( 1.975475456537005874E-15, -55.74999999999999289, 5.000000000000000000 ) ) ;
#26586 = CARTESIAN_POINT ( 'NONE',  ( -60.14911071818854538, -140.0625000000000000, 1.666127454062681368 ) ) ;
#26587 = VECTOR ( 'NONE', #39215, 1000.000000000000000 ) ;
#26588 = CARTESIAN_POINT ( 'NONE',  ( 4.458734125000001214, -30.14583333196773296, 2.574251347313718519 ) ) ;
#26589 = CARTESIAN_POINT ( 'NONE',  ( -2.499999999999996447, -38.83333333333332860, 4.330127018922195425 ) ) ;
#26590 = ORIENTED_EDGE ( 'NONE', *, *, #15430, .T. ) ;
#26591 = CARTESIAN_POINT ( 'NONE',  ( -2.229367062500000163, -76.47916666530106511, -3.861377020970580443 ) ) ;
#26592 = CARTESIAN_POINT ( 'NONE',  ( -4.458734124999998549, 28.77083333469892779, 2.574251347313722516 ) ) ;
#26593 = CARTESIAN_POINT ( 'NONE',  ( -57.46284108482265651, -137.0625000027312126, 4.819101127000238627 ) ) ;
#26594 = EDGE_LOOP ( 'NONE', ( #40194, #1073, #17499 ) ) ;
#26595 = CARTESIAN_POINT ( 'NONE',  ( -5.000000000000000000, 5.041666669397853795, -2.886751345948128211 ) ) ;
#26596 = CARTESIAN_POINT ( 'NONE',  ( -59.44456063193725015, -143.8125000013656063, -0.3552334253322034230 ) ) ;
#26597 = EDGE_CURVE ( 'NONE', #14391, #55487, #20606, .T. ) ;
#26598 = CARTESIAN_POINT ( 'NONE',  ( 9.457646018065525792E-16, -79.31249999863439371, 5.148502694627439702 ) ) ;
#26599 = CARTESIAN_POINT ( 'NONE',  ( -53.33387254593733928, -131.9375000027312126, 5.149110718188519620 ) ) ;
#26600 = DIRECTION ( 'NONE',  ( -0.000000000000000000, 1.000000000000000000, -0.000000000000000000 ) ) ;
#26601 = CARTESIAN_POINT ( 'NONE',  ( 4.458734124999999437, -140.6875000013656063, 0.000000000000000000 ) ) ;
#26602 = CARTESIAN_POINT ( 'NONE',  ( 1.975475456537005874E-15, -48.62499999726880162, 5.000000000000000000 ) ) ;
#26603 = CARTESIAN_POINT ( 'NONE',  ( -2.229367062500000163, -54.47916666530107221, -3.861377020970580443 ) ) ;
#26604 = CARTESIAN_POINT ( 'NONE',  ( -2.229367062499996610, -46.14583333196774362, 3.861377020970582219 ) ) ;
#26605 = CARTESIAN_POINT ( 'NONE',  ( -2.229367062499996610, 27.85416666803225993, 3.861377020970582219 ) ) ;
#26606 = CARTESIAN_POINT ( 'NONE',  ( -4.999999999999999112, -107.9166666666666572, 2.886751345948131764 ) ) ;
#26607 = CARTESIAN_POINT ( 'NONE',  ( 9.457646018065525792E-16, -36.31249999863440792, 5.148502694627439702 ) ) ;
#26608 = CARTESIAN_POINT ( 'NONE',  ( 5.000000000000000888, 3.541666669397852019, 2.886751345948126879 ) ) ;
#26609 = CARTESIAN_POINT ( 'NONE',  ( 1.975475456537005874E-15, -28.74999999999999645, 5.000000000000000000 ) ) ;
#26610 = CARTESIAN_POINT ( 'NONE',  ( -59.29741812935640155, -128.6250000013656063, -2.196230717870135685 ) ) ;
#26611 = CARTESIAN_POINT ( 'NONE',  ( -4.458734124999999437, -77.56249999863440792, 0.000000000000000000 ) ) ;
#26612 = CARTESIAN_POINT ( 'NONE',  ( -6.972266317189433020E-16, -76.12499999726880162, -5.000000000000000000 ) ) ;
#26613 = CARTESIAN_POINT ( 'NONE',  ( -2.229367062499996610, -98.14583333196773651, 3.861377020970582219 ) ) ;
#26614 = CARTESIAN_POINT ( 'NONE',  ( -4.458734124999999437, -7.562499998634404363, 0.000000000000000000 ) ) ;
#26615 = VERTEX_POINT ( 'NONE', #35388 ) ;
#26616 = DIRECTION ( 'NONE',  ( -0.000000000000000000, 1.000000000000000000, -0.000000000000000000 ) ) ;
#26617 = DIRECTION ( 'NONE',  ( -0.000000000000000000, 1.000000000000000000, -0.000000000000000000 ) ) ;
#26618 = CARTESIAN_POINT ( 'NONE',  ( 2.229367062500001939, -86.97916666530107932, 3.861377020970579999 ) ) ;
#26619 = CARTESIAN_POINT ( 'NONE',  ( -4.458734124999999437, -87.56249999863439371, 0.000000000000000000 ) ) ;
#26620 = CARTESIAN_POINT ( 'NONE',  ( 4.458734124999998549, 12.02083333469892601, -2.574251347313721627 ) ) ;
#26621 = CARTESIAN_POINT ( 'NONE',  ( 2.500000000000002220, -2.541666663935477466, 4.330127018922192761 ) ) ;
#26622 = CARTESIAN_POINT ( 'NONE',  ( -59.59170313451811296, -134.5000000013656063, 1.485763867205729394 ) ) ;
#26623 = CARTESIAN_POINT ( 'NONE',  ( 2.229367062499998831, -8.645833331967736513, -3.861377020970580887 ) ) ;
#26624 = CARTESIAN_POINT ( 'NONE',  ( -4.458734124999999437, 17.43750000136559208, 0.000000000000000000 ) ) ;
#26625 = CARTESIAN_POINT ( 'NONE',  ( 4.458734124999999437, -50.06249999863440792, -5.460374474430324690E-16 ) ) ;
#26626 = CARTESIAN_POINT ( 'NONE',  ( -2.500000000000000444, -16.04166666393548368, -4.330127018922193649 ) ) ;
#26627 = CARTESIAN_POINT ( 'NONE',  ( -4.458734124999999437, -86.39583333196772230, -2.574251347313719407 ) ) ;
#26628 = CARTESIAN_POINT ( 'NONE',  ( 2.229367062499998831, -8.645833331967736513, -3.861377020970580887 ) ) ;
#26629 = CARTESIAN_POINT ( 'NONE',  ( 1.975475456537005874E-15, -84.74999999999998579, 5.000000000000000000 ) ) ;
#26630 = ORIENTED_EDGE ( 'NONE', *, *, #26912, .T. ) ;
#26631 = CARTESIAN_POINT ( 'NONE',  ( 4.458734124999998549, -37.97916666530107221, -2.574251347313721627 ) ) ;
#26632 = VECTOR ( 'NONE', #61568, 1000.000000000000000 ) ;
#26633 = CARTESIAN_POINT ( 'NONE',  ( -58.39396692619412477, -129.6875000013656063, 2.891590998281057701 ) ) ;
#26634 = CARTESIAN_POINT ( 'NONE',  ( 4.458734124999999437, -77.81249999863440792, -5.460374474430324690E-16 ) ) ;
#26635 = CARTESIAN_POINT ( 'NONE',  ( -3.152548672688508926E-16, 28.18750000136559564, -5.148502694627439702 ) ) ;
#26636 = VECTOR ( 'NONE', #8247, 1000.000000000000000 ) ;
#26637 =( BOUNDED_CURVE ( )  B_SPLINE_CURVE ( 2, ( #50973, #12041, #15918, #45183, #55802, #30383, #50006, #17189, #26204 ),
 .UNSPECIFIED., .F., .F. ) 
 B_SPLINE_CURVE_WITH_KNOTS ( ( 3, 2, 2, 2, 3 ),
 ( 0.5625000000000000000, 0.5630952380952380931, 0.5642857142857142794, 0.5654761904761904656, 0.5660714285714285587 ),
 .UNSPECIFIED. ) 
 CURVE ( )  GEOMETRIC_REPRESENTATION_ITEM ( )  RATIONAL_B_SPLINE_CURVE ( ( 0.9330127018922194093, 0.9330127018922194093, 1.000000000000000000, 0.8660254037844387076, 1.000000000000000000, 0.8660254037844387076, 1.000000000000000000, 0.9330127018922194093, 0.9330127018922194093 ) ) 
 REPRESENTATION_ITEM ( '' )  );
#26638 = CARTESIAN_POINT ( 'NONE',  ( 4.458734125000001214, 18.10416666803225638, 2.574251347313718519 ) ) ;
#26639 = CARTESIAN_POINT ( 'NONE',  ( -2.500000000000000444, -44.04166666393546592, -4.330127018922193649 ) ) ;
#26640 = CARTESIAN_POINT ( 'NONE',  ( -2.071067811865562991, -145.4375000027312126, 4.999999999999913847 ) ) ;
#26641 = CARTESIAN_POINT ( 'NONE',  ( 4.458734125000000326, -79.14583333196773651, 2.574251347313718519 ) ) ;
#26642 = CARTESIAN_POINT ( 'NONE',  ( -2.500000000000000444, -65.16666666666667140, -4.330127018922193649 ) ) ;
#26643 = CARTESIAN_POINT ( 'NONE',  ( 1.975475456537005874E-15, -72.62499999726878741, 5.000000000000000000 ) ) ;
#26644 = CARTESIAN_POINT ( 'NONE',  ( -3.535250795749689387E-16, 17.87500000273118417, -5.773502691896257311 ) ) ;
#26645 = VERTEX_POINT ( 'NONE', #40839 ) ;
#26646 = DIRECTION ( 'NONE',  ( -0.000000000000000000, 1.000000000000000000, -0.000000000000000000 ) ) ;
#26647 = CARTESIAN_POINT ( 'NONE',  ( -4.999999999999998224, 9.083333333333333925, 2.886751345948131764 ) ) ;
#26649 = CARTESIAN_POINT ( 'NONE',  ( -5.000000000000000000, -22.08333333333333215, -2.886751345948128211 ) ) ;
#26648 = CARTESIAN_POINT ( 'NONE',  ( 0.000000000000000000, -170.0000000000000000, 5.000000000000000000 ) ) ;
#26650 = CARTESIAN_POINT ( 'NONE',  ( 4.458734125000001214, -27.89583333196774007, 2.574251347313718519 ) ) ;
#26651 = EDGE_CURVE ( 'NONE', #63596, #34574, #48796, .T. ) ;
#26652 = CARTESIAN_POINT ( 'NONE',  ( -3.152548672688508926E-16, -85.56249999863439371, -5.148502694627439702 ) ) ;
#26653 =( BOUNDED_CURVE ( )  B_SPLINE_CURVE ( 2, ( #52329, #8264, #16960, #3439, #36572, #62921, #48732, #190, #48114 ),
 .UNSPECIFIED., .F., .F. ) 
 B_SPLINE_CURVE_WITH_KNOTS ( ( 3, 2, 2, 2, 3 ),
 ( 0.6229166666666666741, 0.6236111111111111160, 0.6250000000000000000, 0.6263888888888888840, 0.6270833333333333259 ),
 .UNSPECIFIED. ) 
 CURVE ( )  GEOMETRIC_REPRESENTATION_ITEM ( )  RATIONAL_B_SPLINE_CURVE ( ( 0.9330127018922194093, 0.9330127018922194093, 1.000000000000000000, 0.8660254037844387076, 1.000000000000000000, 0.8660254037844387076, 1.000000000000000000, 0.9330127018922194093, 0.9330127018922194093 ) ) 
 REPRESENTATION_ITEM ( '' )  );
#26654 = CARTESIAN_POINT ( 'NONE',  ( -2.500000000000000444, -28.04166666393548013, -4.330127018922193649 ) ) ;
#26656 = ORIENTED_EDGE ( 'NONE', *, *, #41340, .T. ) ;
#26655 = CARTESIAN_POINT ( 'NONE',  ( -4.458734124999998549, -55.22916666530107932, 2.574251347313722516 ) ) ;
#26657 = CARTESIAN_POINT ( 'NONE',  ( -51.75738570946856498, -150.8750000027312126, 3.805975901505576964 ) ) ;
#26658 = CARTESIAN_POINT ( 'NONE',  ( -62.00000000000001421, -135.0000000000000284, -4.041451884327373456 ) ) ;
#26660 = ORIENTED_EDGE ( 'NONE', *, *, #40155, .T. ) ;
#26659 = CARTESIAN_POINT ( 'NONE',  ( -4.458734124999999437, -5.562499998634402587, 0.000000000000000000 ) ) ;
#26661 = CARTESIAN_POINT ( 'NONE',  ( -5.000000000000000000, -69.99999999999998579, 0.000000000000000000 ) ) ;
#26662 = CARTESIAN_POINT ( 'NONE',  ( -52.80376928212989185, -136.8750000013656063, -4.297418129356378458 ) ) ;
#26663 = CARTESIAN_POINT ( 'NONE',  ( 4.458734124999998549, -52.97916666530107932, -2.574251347313721627 ) ) ;
#26664 = DIRECTION ( 'NONE',  ( -0.000000000000000000, 1.000000000000000000, -0.000000000000000000 ) ) ;
#26665 = CARTESIAN_POINT ( 'NONE',  ( -5.000000000000000000, -68.95833333060214443, -2.886751345948128211 ) ) ;
#26666 = CARTESIAN_POINT ( 'NONE',  ( 1.975475456537005874E-15, -10.62499999726881228, 5.000000000000000000 ) ) ;
#26667 = CARTESIAN_POINT ( 'NONE',  ( -50.01589407740564042, -152.6250000000000284, 0.3983568153799778022 ) ) ;
#26668 = CARTESIAN_POINT ( 'NONE',  ( 4.458734124999998549, -13.97916666530107221, -2.574251347313721627 ) ) ;
#26669 = CARTESIAN_POINT ( 'NONE',  ( 2.229367062500001939, -54.22916666530107221, 3.861377020970579999 ) ) ;
#26670 = ADVANCED_FACE ( 'NONE', ( #42107 ), #31833, .F. ) ;
#26671 = FACE_OUTER_BOUND ( 'NONE', #41989, .T. ) ;
#26672 = CARTESIAN_POINT ( 'NONE',  ( 3.152801135295366208, -140.5625000013655779, 3.152801135295367985 ) ) ;
#26673 = ADVANCED_FACE ( 'NONE', ( #7719 ), #27637, .T. ) ;
#26674 = CARTESIAN_POINT ( 'NONE',  ( 4.458734125000001214, -96.14583333196772230, 2.574251347313718519 ) ) ;
#26675 = DIRECTION ( 'NONE',  ( -0.000000000000000000, 1.000000000000000000, -0.000000000000000000 ) ) ;
#26676 = VERTEX_POINT ( 'NONE', #27009 ) ;
#26677 = CARTESIAN_POINT ( 'NONE',  ( -5.000000000000000888, -155.4375000000000000, 2.071067811865474617 ) ) ;
#26678 = CARTESIAN_POINT ( 'NONE',  ( 2.229367062500001939, 23.77083333469892779, 3.861377020970579999 ) ) ;
#26679 = CARTESIAN_POINT ( 'NONE',  ( -50.01589407740564042, -144.7500000027312126, 0.3983568153799778022 ) ) ;
#26680 = PRODUCT_DEFINITION_FORMATION_WITH_SPECIFIED_SOURCE ( 'ANY', '', #18875, .NOT_KNOWN. ) ;
#26681 = DIRECTION ( 'NONE',  ( -0.000000000000000000, 1.000000000000000000, -0.000000000000000000 ) ) ;
#26682 = VECTOR ( 'NONE', #33429, 1000.000000000000000 ) ;
#26683 = ADVANCED_FACE ( 'NONE', ( #61752 ), #51148, .T. ) ;
#26684 = CARTESIAN_POINT ( 'NONE',  ( -4.458734124999999437, -2.312499998634407028, 0.000000000000000000 ) ) ;
#26685 = CARTESIAN_POINT ( 'NONE',  ( -2.229367062499996610, -93.39583333196773651, 3.861377020970582219 ) ) ;
#26686 = CARTESIAN_POINT ( 'NONE',  ( 1.846868145590736310, -149.8750000013655779, 4.458734124999999437 ) ) ;
#26687 = CARTESIAN_POINT ( 'NONE',  ( 2.229367062500001939, -21.22916666530107221, 3.861377020970579999 ) ) ;
#26688 = LINE ( 'NONE', #8338, #39610 ) ;
#26689 = CARTESIAN_POINT ( 'NONE',  ( 4.458734124999999437, -65.06249999863440792, -5.460374474430324690E-16 ) ) ;
#26690 = CARTESIAN_POINT ( 'NONE',  ( 7.500000000000000000, 4.330127018922190096, -7.422398894150032511 ) ) ;
#26691 = CARTESIAN_POINT ( 'NONE',  ( 5.088535779737119569, -5.722386535631984295, -7.491772860715834703 ) ) ;
#26692 = CARTESIAN_POINT ( 'NONE',  ( -3.152801135295367096, -144.0625000013655779, -3.152801135295367541 ) ) ;
#26693 = CARTESIAN_POINT ( 'NONE',  ( -4.458734124999999437, 17.35416666803225993, -2.574251347313719407 ) ) ;
#26694 = ORIENTED_EDGE ( 'NONE', *, *, #9347, .T. ) ;
#26695 = CARTESIAN_POINT ( 'NONE',  ( 1.975475456537005874E-15, -52.62499999726880873, 5.000000000000000000 ) ) ;
#26696 = DIRECTION ( 'NONE',  ( -0.000000000000000000, 1.000000000000000000, 0.000000000000000000 ) ) ;
#26698 = CARTESIAN_POINT ( 'NONE',  ( -4.458734124999998549, -20.22916666530107221, 2.574251347313722516 ) ) ;
#26697 = CARTESIAN_POINT ( 'NONE',  ( 1.060575238724906964E-15, -84.74999999999998579, 5.773502691896257311 ) ) ;
#26699 = CARTESIAN_POINT ( 'NONE',  ( 4.458734124999999437, 28.93750000136559208, -5.460374474430324690E-16 ) ) ;
#26700 = CARTESIAN_POINT ( 'NONE',  ( 2.500000000000002220, -88.54166666393548724, 4.330127018922192761 ) ) ;
#26701 = CARTESIAN_POINT ( 'NONE',  ( -52.80376928212989185, -144.8750000013655779, -4.297418129356379346 ) ) ;
#26702 = EDGE_CURVE ( 'NONE', #62889, #45023, #42240, .T. ) ;
#26703 = CARTESIAN_POINT ( 'NONE',  ( 2.499999999999998668, -48.20833333060215153, -4.330127018922193649 ) ) ;
#26704 = DIRECTION ( 'NONE',  ( 0.000000000000000000, 0.000000000000000000, 1.000000000000000000 ) ) ;
#26705 = CARTESIAN_POINT ( 'NONE',  ( 4.458734124999999437, 7.187500001365594748, -5.460374474430324690E-16 ) ) ;
#26706 = LINE ( 'NONE', #8042, #34502 ) ;
#26707 = FACE_OUTER_BOUND ( 'NONE', #44046, .T. ) ;
#26708 = CARTESIAN_POINT ( 'NONE',  ( -4.458734124999999437, 14.68750000136559386, 0.000000000000000000 ) ) ;
#26709 = CARTESIAN_POINT ( 'NONE',  ( 4.458734125000001214, -67.89583333196773651, 2.574251347313718519 ) ) ;
#26710 = CARTESIAN_POINT ( 'NONE',  ( -2.229367062499996610, -18.39583333196774007, 3.861377020970582219 ) ) ;
#26711 =( BOUNDED_CURVE ( )  B_SPLINE_CURVE ( 2, ( #9684, #34130, #4870, #54400, #59, #39905, #39268, #373, #29292 ),
 .UNSPECIFIED., .F., .F. ) 
 B_SPLINE_CURVE_WITH_KNOTS ( ( 3, 2, 2, 2, 3 ),
 ( 0.6354166666666666297, 0.6361111111111110716, 0.6374999999999999556, 0.6388888888888888395, 0.6395833333333332815 ),
 .UNSPECIFIED. ) 
 CURVE ( )  GEOMETRIC_REPRESENTATION_ITEM ( )  RATIONAL_B_SPLINE_CURVE ( ( 0.9330127018922194093, 0.9330127018922194093, 1.000000000000000000, 0.8660254037844387076, 1.000000000000000000, 0.8660254037844387076, 1.000000000000000000, 0.9330127018922194093, 0.9330127018922194093 ) ) 
 REPRESENTATION_ITEM ( '' )  );
#26712 = CARTESIAN_POINT ( 'NONE',  ( 2.500000000000002220, -1.666666666666663410, 4.330127018922192761 ) ) ;
#26713 = CARTESIAN_POINT ( 'NONE',  ( 2.730187237215162345E-16, -161.1875000013655779, -4.458734124999999437 ) ) ;
#26714 = CARTESIAN_POINT ( 'NONE',  ( -6.972266317189433020E-16, -99.12499999726880162, -5.000000000000000000 ) ) ;
#26715 = CARTESIAN_POINT ( 'NONE',  ( 9.457646018065525792E-16, -58.06249999863440081, 5.148502694627439702 ) ) ;
#26716 = CARTESIAN_POINT ( 'NONE',  ( 5.000000000000000000, -92.29166666393547303, -2.886751345948129988 ) ) ;
#26717 = CARTESIAN_POINT ( 'NONE',  ( 3.061616997868383141E-16, -161.8750000027311842, -5.000000000000000000 ) ) ;
#26718 = CARTESIAN_POINT ( 'NONE',  ( 5.000000000000000000, -56.41666666666667140, -2.886751345948130876 ) ) ;
#26719 = CARTESIAN_POINT ( 'NONE',  ( 2.229367062499998831, -36.64583333196773651, -3.861377020970580887 ) ) ;
#26720 = CARTESIAN_POINT ( 'NONE',  ( -2.499999999999996447, -90.70833333060214443, 4.330127018922195425 ) ) ;
#26721 = CARTESIAN_POINT ( 'NONE',  ( 1.060575238724906964E-15, -47.75000000000000000, 5.773502691896257311 ) ) ;
#26722 = CARTESIAN_POINT ( 'NONE',  ( 3.044556291839386294E-14, 18.75000000000000355, -5.000000000000000000 ) ) ;
#26723 = CARTESIAN_POINT ( 'NONE',  ( 1.339745962155612702, -36.16965819600732601, -5.000000000000000000 ) ) ;
#26724 = VERTEX_POINT ( 'NONE', #57245 ) ;
#26725 = CARTESIAN_POINT ( 'NONE',  ( 4.458734124999999437, -107.8124999986343937, -5.460374474430324690E-16 ) ) ;
#26726 = CARTESIAN_POINT ( 'NONE',  ( -4.458734124999999437, -0.5624999986344053626, 0.000000000000000000 ) ) ;
#26727 = CARTESIAN_POINT ( 'NONE',  ( 1.975475456537005874E-15, -67.62499999726881583, 5.000000000000000000 ) ) ;
#26728 = CARTESIAN_POINT ( 'NONE',  ( 1.060575238724906964E-15, -8.750000000000000000, 5.773502691896257311 ) ) ;
#26729 = AXIS2_PLACEMENT_3D ( 'NONE', #35828, #30988, #11051 ) ;
#26730 = EDGE_CURVE ( 'NONE', #61537, #14751, #49181, .T. ) ;
#26731 = CARTESIAN_POINT ( 'NONE',  ( 2.229367062499998831, -74.64583333196773651, -3.861377020970580887 ) ) ;
#26732 = CARTESIAN_POINT ( 'NONE',  ( 5.000000000000000000, -22.37499999726881228, -6.123233995736766282E-16 ) ) ;
#26733 = CARTESIAN_POINT ( 'NONE',  ( 5.000000000000000888, -6.458333330602148870, 2.886751345948126879 ) ) ;
#26735 = EDGE_LOOP ( 'NONE', ( #11148, #34541, #41281, #32747 ) ) ;
#26734 = CARTESIAN_POINT ( 'NONE',  ( 4.458734125000001214, -37.89583333196772941, 2.574251347313718519 ) ) ;
#26736 = CARTESIAN_POINT ( 'NONE',  ( -55.00000000000001421, -135.0000000000000284, 8.082903768654762899 ) ) ;
#26738 = ORIENTED_EDGE ( 'NONE', *, *, #37339, .F. ) ;
#26737 = CARTESIAN_POINT ( 'NONE',  ( 9.457646018065525792E-16, 12.68750000136559208, 5.148502694627439702 ) ) ;
#26739 = DIRECTION ( 'NONE',  ( -0.000000000000000000, 1.000000000000000000, -0.000000000000000000 ) ) ;
#26740 = CARTESIAN_POINT ( 'NONE',  ( -5.000000000000000000, -56.08333333333332860, -2.886751345948128211 ) ) ;
#26741 = CARTESIAN_POINT ( 'NONE',  ( 4.458734124999999437, -159.7500000013656063, 1.846868145590737864 ) ) ;
#26742 = CARTESIAN_POINT ( 'NONE',  ( 4.458734124999999437, -32.06249999863440792, -5.460374474430324690E-16 ) ) ;
#26743 = CARTESIAN_POINT ( 'NONE',  ( -2.500000000000000444, -35.16666666666666430, -4.330127018922193649 ) ) ;
#26744 = CARTESIAN_POINT ( 'NONE',  ( 4.458734124999998549, -82.72916666530106511, -2.574251347313721627 ) ) ;
#26745 = CARTESIAN_POINT ( 'NONE',  ( 2.071067811865475505, -169.8125000000000000, -5.000000000000000888 ) ) ;
#26746 = CARTESIAN_POINT ( 'NONE',  ( 2.229367062499998831, -85.64583333196773651, -3.861377020970580887 ) ) ;
#26747 = CARTESIAN_POINT ( 'NONE',  ( -51.60603307380591787, -135.1875000013656063, -2.891590998281053704 ) ) ;
#26748 = CARTESIAN_POINT ( 'NONE',  ( -2.229367062499996610, -33.39583333196772941, 3.861377020970582219 ) ) ;
#26749 = CARTESIAN_POINT ( 'NONE',  ( 1.339745962155612702, -70.16965819600731891, -5.000000000000000000 ) ) ;
#26751 = EDGE_CURVE ( 'NONE', #1132, #55402, #51653, .T. ) ;
#26750 = VERTEX_POINT ( 'NONE', #31503 ) ;
#26752 = CARTESIAN_POINT ( 'NONE',  ( 4.458734124999999437, -76.06249999863440792, -5.460374474430324690E-16 ) ) ;
#26753 = CARTESIAN_POINT ( 'NONE',  ( -3.750000000000001776, 6.495190528383289141, -6.991905250253753756 ) ) ;
#26754 = ORIENTED_EDGE ( 'NONE', *, *, #45704, .T. ) ;
#26755 = CARTESIAN_POINT ( 'NONE',  ( 0.000000000000000000, -120.0000000000000000, 0.000000000000000000 ) ) ;
#26756 =( BOUNDED_CURVE ( )  B_SPLINE_CURVE ( 2, ( #46699, #21943, #32858, #42499, #56370, #8725, #18055, #37676, #33177 ),
 .UNSPECIFIED., .F., .F. ) 
 B_SPLINE_CURVE_WITH_KNOTS ( ( 3, 2, 2, 2, 3 ),
 ( 0.6982142857142856762, 0.6988095238095237693, 0.6999999999999999556, 0.7011904761904761418, 0.7017857142857142350 ),
 .UNSPECIFIED. ) 
 CURVE ( )  GEOMETRIC_REPRESENTATION_ITEM ( )  RATIONAL_B_SPLINE_CURVE ( ( 0.9330127018922194093, 0.9330127018922194093, 1.000000000000000000, 0.8660254037844387076, 1.000000000000000000, 0.8660254037844387076, 1.000000000000000000, 0.9330127018922194093, 0.9330127018922194093 ) ) 
 REPRESENTATION_ITEM ( '' )  );
#26757 = DIRECTION ( 'NONE',  ( -0.000000000000000000, 1.000000000000000000, -0.000000000000000000 ) ) ;
#26758 = CARTESIAN_POINT ( 'NONE',  ( 2.229367062500001939, -63.22916666530106511, 3.861377020970579999 ) ) ;
#26759 = CARTESIAN_POINT ( 'NONE',  ( 4.458734124999999437, -7.062499998634404363, -5.460374474430324690E-16 ) ) ;
#26760 = ORIENTED_EDGE ( 'NONE', *, *, #40084, .T. ) ;
#26761 = CARTESIAN_POINT ( 'NONE',  ( 1.975475456537005874E-15, 19.37500000273118772, 5.000000000000000000 ) ) ;
#26762 = CARTESIAN_POINT ( 'NONE',  ( -2.229367062500000163, -6.729166665301073103, -3.861377020970580443 ) ) ;
#26763 = FACE_OUTER_BOUND ( 'NONE', #13542, .T. ) ;
#26764 = CARTESIAN_POINT ( 'NONE',  ( 2.229367062499998831, 9.354166668032261711, -3.861377020970580887 ) ) ;
#26765 = CARTESIAN_POINT ( 'NONE',  ( 5.000000000000000000, -64.50000000000000000, -6.123233995736766282E-16 ) ) ;
#26766 = CARTESIAN_POINT ( 'NONE',  ( 4.458734124999999437, -158.3750000013655779, -1.846868145590734978 ) ) ;
#26767 = CARTESIAN_POINT ( 'NONE',  ( -1.339745962155613812, 18.91965820146970501, -5.000000000000000000 ) ) ;
#26768 = ORIENTED_EDGE ( 'NONE', *, *, #26730, .F. ) ;
#26769 = CARTESIAN_POINT ( 'NONE',  ( -2.229367062500000163, -85.47916666530107932, -3.861377020970580443 ) ) ;
#26770 = CARTESIAN_POINT ( 'NONE',  ( -4.458734124999999437, -3.312499998634407916, 0.000000000000000000 ) ) ;
#26771 = AXIS2_PLACEMENT_3D ( 'NONE', #30746, #50681, #26236 ) ;
#26772 = ADVANCED_FACE ( 'NONE', ( #36983 ), #8348, .T. ) ;
#26773 = CARTESIAN_POINT ( 'NONE',  ( 2.500000000000002220, -51.66666666666666430, 4.330127018922192761 ) ) ;
#26774 = CARTESIAN_POINT ( 'NONE',  ( 5.000000000000000000, -30.37499999726881228, -6.123233995736766282E-16 ) ) ;
#26775 = CARTESIAN_POINT ( 'NONE',  ( 5.000000000000000000, -78.50000000000000000, -6.123233995736766282E-16 ) ) ;
#26776 = CARTESIAN_POINT ( 'NONE',  ( -3.152548672688508926E-16, 23.43750000136559564, -5.148502694627439702 ) ) ;
#26777 = CARTESIAN_POINT ( 'NONE',  ( -1.339745962155613812, -21.08034179853029144, -5.000000000000000000 ) ) ;
#26778 = CARTESIAN_POINT ( 'NONE',  ( -4.458734124999997661, 28.77083333469892779, 2.574251347313722516 ) ) ;
#26779 = CARTESIAN_POINT ( 'NONE',  ( -4.458734124999999437, -50.31249999863440792, 0.000000000000000000 ) ) ;
#26780 = CARTESIAN_POINT ( 'NONE',  ( 9.457646018065525792E-16, -35.31249999863440792, 5.148502694627439702 ) ) ;
#26781 = CARTESIAN_POINT ( 'NONE',  ( -4.458734124999999437, -0.6458333319677399542, -2.574251347313719407 ) ) ;
#26782 = CARTESIAN_POINT ( 'NONE',  ( 2.500000000000002220, 15.33333333333333215, 4.330127018922192761 ) ) ;
#26783 = CARTESIAN_POINT ( 'NONE',  ( -3.535533905932737309, -144.7500000027311842, -3.535533905932738197 ) ) ;
#26784 = VECTOR ( 'NONE', #27771, 1000.000000000000000 ) ;
#26785 = DIRECTION ( 'NONE',  ( -0.000000000000000000, 1.000000000000000000, -0.000000000000000000 ) ) ;
#26786 = CARTESIAN_POINT ( 'NONE',  ( -4.458734124999999437, -40.31249999863440081, 0.000000000000000000 ) ) ;
#26787 = CARTESIAN_POINT ( 'NONE',  ( 5.000000000000000888, -80.45833333060213022, 2.886751345948126879 ) ) ;
#26788 = CARTESIAN_POINT ( 'NONE',  ( -59.59170313451811296, -141.7500000013656063, 1.485763867205729394 ) ) ;
#26789 = CARTESIAN_POINT ( 'NONE',  ( 2.499999999999998668, -65.20833333060213022, -4.330127018922193649 ) ) ;
#26790 = CARTESIAN_POINT ( 'NONE',  ( 7.894787914004607998, 1.243647571710251278E-13, -7.591390474663425536 ) ) ;
#26791 = CARTESIAN_POINT ( 'NONE',  ( 2.229367062500001939, -83.22916666530106511, 3.861377020970579999 ) ) ;
#26792 = CARTESIAN_POINT ( 'NONE',  ( -8.190561711645485556E-16, -161.9375000013655779, 4.458734124999999437 ) ) ;
#26793 = CARTESIAN_POINT ( 'NONE',  ( -3.295171437451516638, -7.213553046160524396, -7.590212325761481971 ) ) ;
#26794 = CARTESIAN_POINT ( 'NONE',  ( -5.000000000000000000, -34.00000000000000000, 0.000000000000000000 ) ) ;
#26795 = CARTESIAN_POINT ( 'NONE',  ( -5.000000000000000000, -90.87499999726880162, 0.000000000000000000 ) ) ;
#26796 = ORIENTED_EDGE ( 'NONE', *, *, #37716, .F. ) ;
#26797 = CARTESIAN_POINT ( 'NONE',  ( -4.458734124999999437, 21.35416666803225993, -2.574251347313719407 ) ) ;
#26798 = ORIENTED_EDGE ( 'NONE', *, *, #8658, .F. ) ;
#26799 = CARTESIAN_POINT ( 'NONE',  ( -4.458734124999998549, -90.22916666530106511, 2.574251347313722516 ) ) ;
#26800 = CARTESIAN_POINT ( 'NONE',  ( -4.458734124999999437, 11.35416666803225993, -2.574251347313719407 ) ) ;
#26801 = CARTESIAN_POINT ( 'NONE',  ( 1.060575238724906964E-15, 14.37500000273118594, 5.773502691896257311 ) ) ;
#26802 = CARTESIAN_POINT ( 'NONE',  ( 5.000000000000000000, 9.499999999999998224, -6.123233995736766282E-16 ) ) ;
#26803 = CARTESIAN_POINT ( 'NONE',  ( 9.457646018065525792E-16, -54.06249999863440081, 5.148502694627439702 ) ) ;
#26804 = CARTESIAN_POINT ( 'NONE',  ( 7.500000000000000000, -1.645076096015019695, -7.030022527230891605 ) ) ;
#26805 = EDGE_CURVE ( 'NONE', #62283, #33389, #61977, .T. ) ;
#26806 = EDGE_CURVE ( 'NONE', #5681, #42641, #22831, .T. ) ;
#26807 = CARTESIAN_POINT ( 'NONE',  ( -2.499999999999996447, 20.16666666666666430, 4.330127018922195425 ) ) ;
#26808 = CARTESIAN_POINT ( 'NONE',  ( -6.972266317189433020E-16, -107.2499999999999858, -5.000000000000000000 ) ) ;
#26809 = CARTESIAN_POINT ( 'NONE',  ( 5.000000000000000888, -33.45833333060215153, 2.886751345948126879 ) ) ;
#26810 = EDGE_CURVE ( 'NONE', #25630, #7254, #22910, .T. ) ;
#26811 = CARTESIAN_POINT ( 'NONE',  ( 2.500000000000002220, -11.54166666393547835, 4.330127018922192761 ) ) ;
#26812 = CARTESIAN_POINT ( 'NONE',  ( -3.535250795749689387E-16, -42.24999999999999289, -5.773502691896257311 ) ) ;
#26813 = CARTESIAN_POINT ( 'NONE',  ( -5.000000000000000000, 13.04166666939785379, -2.886751345948128211 ) ) ;
#26815 = CARTESIAN_POINT ( 'NONE',  ( -4.458734124999999437, -14.56249999863440436, 0.000000000000000000 ) ) ;
#26814 = CARTESIAN_POINT ( 'NONE',  ( -59.98410592259440222, -139.1250000000000284, -0.3983568153799752487 ) ) ;
#26816 = ADVANCED_FACE ( 'NONE', ( #13484, #57865 ), #29511, .F. ) ;
#26817 = CARTESIAN_POINT ( 'NONE',  ( -2.071067811865562991, -143.3124999999999716, 4.999999999999913847 ) ) ;
#26818 = CARTESIAN_POINT ( 'NONE',  ( -4.458734124999999437, -61.39583333196774362, -2.574251347313719407 ) ) ;
#26819 = CARTESIAN_POINT ( 'NONE',  ( -4.458734125000000326, -150.2500000013656063, -1.846868145590735644 ) ) ;
#26820 = AXIS2_PLACEMENT_3D ( 'NONE', #2446, #13662, #56796 ) ;
#26821 = CARTESIAN_POINT ( 'NONE',  ( 2.229367062500001939, -72.97916666530107932, 3.861377020970579999 ) ) ;
#26822 = CARTESIAN_POINT ( 'NONE',  ( -50.70258187064364108, -145.3750000013656347, 2.196230717870141014 ) ) ;
#26823 = EDGE_CURVE ( 'NONE', #45741, #39400, #29067, .T. ) ;
#26824 = EDGE_CURVE ( 'NONE', #29833, #57689, #53656, .T. ) ;
#26825 = CARTESIAN_POINT ( 'NONE',  ( -3.152548672688508926E-16, -18.81249999863440792, -5.148502694627439702 ) ) ;
#26826 = CARTESIAN_POINT ( 'NONE',  ( 5.000000000000000000, -59.29166666393547303, -2.886751345948129988 ) ) ;
#26827 = ORIENTED_EDGE ( 'NONE', *, *, #25920, .F. ) ;
#26828 = CARTESIAN_POINT ( 'NONE',  ( 1.339745962155615144, -31.58034179853029499, 4.999999999999999112 ) ) ;
#26829 = VERTEX_POINT ( 'NONE', #29198 ) ;
#26830 = CARTESIAN_POINT ( 'NONE',  ( -4.458734124999998549, -63.47916666530106511, 2.574251347313722516 ) ) ;
#26832 = CARTESIAN_POINT ( 'NONE',  ( -4.999999999999998224, -85.91666666666667140, 2.886751345948131764 ) ) ;
#26831 = DIRECTION ( 'NONE',  ( -1.000000000000000000, 0.000000000000000000, -0.000000000000000000 ) ) ;
#26833 = CARTESIAN_POINT ( 'NONE',  ( 4.458734125000000326, -152.3750000013655779, -1.846868145590734978 ) ) ;
#26834 = EDGE_CURVE ( 'NONE', #44276, #1660, #59916, .T. ) ;
#26835 = VERTEX_POINT ( 'NONE', #33722 ) ;
#26836 = ADVANCED_FACE ( 'NONE', ( #3835 ), #23453, .T. ) ;
#26837 = EDGE_CURVE ( 'NONE', #35151, #29442, #58200, .T. ) ;
#26838 = CARTESIAN_POINT ( 'NONE',  ( 5.000000000000000000, -54.41666666666667140, -2.886751345948130876 ) ) ;
#26839 = CARTESIAN_POINT ( 'NONE',  ( -60.14911071818854538, -126.0625000000000284, 1.666127454062681368 ) ) ;
#26840 = CARTESIAN_POINT ( 'NONE',  ( -5.000000000000000000, -55.87499999726880162, 0.000000000000000000 ) ) ;
#26841 = CARTESIAN_POINT ( 'NONE',  ( 4.458734125000001214, -50.14583333196773651, 2.574251347313718519 ) ) ;
#26842 = ORIENTED_EDGE ( 'NONE', *, *, #10250, .T. ) ;
#26843 =( BOUNDED_CURVE ( )  B_SPLINE_CURVE ( 2, ( #43426, #62443, #38594, #9647, #57927, #37985, #62122, #13544, #28322 ),
 .UNSPECIFIED., .F., .F. ) 
 B_SPLINE_CURVE_WITH_KNOTS ( ( 3, 2, 2, 2, 3 ),
 ( 0.2604166666666666852, 0.2611111111111111271, 0.2625000000000000111, 0.2638888888888888951, 0.2645833333333333370 ),
 .UNSPECIFIED. ) 
 CURVE ( )  GEOMETRIC_REPRESENTATION_ITEM ( )  RATIONAL_B_SPLINE_CURVE ( ( 0.9330127018922194093, 0.9330127018922194093, 1.000000000000000000, 0.8660254037844387076, 1.000000000000000000, 0.8660254037844387076, 1.000000000000000000, 0.9330127018922194093, 0.9330127018922194093 ) ) 
 REPRESENTATION_ITEM ( '' )  );
#26844 = CARTESIAN_POINT ( 'NONE',  ( -6.972266317189433020E-16, -76.24999999999998579, -5.000000000000000000 ) ) ;
#26845 = CARTESIAN_POINT ( 'NONE',  ( 4.458734125000001214, 6.104166668032262599, 2.574251347313718519 ) ) ;
#26846 = CARTESIAN_POINT ( 'NONE',  ( 2.229367062500001939, 22.02083333469892779, 3.861377020970579999 ) ) ;
#26847 = CARTESIAN_POINT ( 'NONE',  ( -52.80376928212989185, -148.8750000013655779, -4.297418129356379346 ) ) ;
#26848 = CARTESIAN_POINT ( 'NONE',  ( 1.339745962155615144, -78.58034179853028434, 4.999999999999999112 ) ) ;
#26849 = CARTESIAN_POINT ( 'NONE',  ( -8.190561711645485556E-16, -167.6875000013655779, 4.458734124999999437 ) ) ;
#26850 = ORIENTED_EDGE ( 'NONE', *, *, #15034, .F. ) ;
#26851 = CARTESIAN_POINT ( 'NONE',  ( 4.458734124999998549, -69.72916666530107932, -2.574251347313721627 ) ) ;
#26852 = CARTESIAN_POINT ( 'NONE',  ( -0.04725809328185606034, 9.175759667312519241, -8.057670357645360326 ) ) ;
#26853 = CARTESIAN_POINT ( 'NONE',  ( 4.458734124999998549, 14.27083333469892779, -2.574251347313721627 ) ) ;
#26854 = CARTESIAN_POINT ( 'NONE',  ( -51.75738570946856498, -137.7500000000000000, 3.805975901505576964 ) ) ;
#26855 = CARTESIAN_POINT ( 'NONE',  ( 2.493747252781420335E-13, -42.25000000000000711, -5.000000000000000000 ) ) ;
#26856 = CARTESIAN_POINT ( 'NONE',  ( 4.458734125000001214, -54.14583333196773651, 2.574251347313718519 ) ) ;
#26857 = CARTESIAN_POINT ( 'NONE',  ( -2.500000000000000444, -13.04166666393548013, -4.330127018922193649 ) ) ;
#26858 = CARTESIAN_POINT ( 'NONE',  ( -5.147856630858197489E-14, 4.249999999999996447, 5.000000000000000000 ) ) ;
#26859 = CARTESIAN_POINT ( 'NONE',  ( -6.972266317189433020E-16, -45.24999999999999289, -5.000000000000000000 ) ) ;
#26860 = CARTESIAN_POINT ( 'NONE',  ( -75.00000000000001421, 15.00000000000000000, -9.000000000000001776 ) ) ;
#26861 = CARTESIAN_POINT ( 'NONE',  ( 2.229367062500001939, -21.22916666530107221, 3.861377020970579999 ) ) ;
#26862 = ORIENTED_EDGE ( 'NONE', *, *, #50427, .F. ) ;
#26863 = CARTESIAN_POINT ( 'NONE',  ( -4.999999999999998224, -4.791666663935479242, 2.886751345948131764 ) ) ;
#26864 = CARTESIAN_POINT ( 'NONE',  ( 4.458734125000001214, -108.8958333319677365, 2.574251347313718519 ) ) ;
#26865 = CARTESIAN_POINT ( 'NONE',  ( -5.000000000000000888, -158.5625000027312126, 2.071067811865474617 ) ) ;
#26866 = ORIENTED_EDGE ( 'NONE', *, *, #21949, .F. ) ;
#26867 = CARTESIAN_POINT ( 'NONE',  ( 2.229367062499998831, -100.8958333319677365, -3.861377020970580887 ) ) ;
#26868 = VECTOR ( 'NONE', #26171, 1000.000000000000000 ) ;
#26869 = CARTESIAN_POINT ( 'NONE',  ( 4.458734124999998549, -24.72916666530106866, -2.574251347313721627 ) ) ;
#26870 = CARTESIAN_POINT ( 'NONE',  ( -3.535250795749689387E-16, -65.12499999726881583, -5.773502691896257311 ) ) ;
#26871 = CARTESIAN_POINT ( 'NONE',  ( -50.55543936806279248, -151.3125000013656063, 0.3552334253322060320 ) ) ;
#26872 = CARTESIAN_POINT ( 'NONE',  ( -5.000000000000000888, -147.5625000000000284, -2.071067811865475949 ) ) ;
#26873 = CARTESIAN_POINT ( 'NONE',  ( 2.229367062499998831, -25.64583333196773651, -3.861377020970580887 ) ) ;
#26874 = CARTESIAN_POINT ( 'NONE',  ( 4.458734125000000326, -72.14583333196773651, 2.574251347313718519 ) ) ;
#26875 = CARTESIAN_POINT ( 'NONE',  ( -2.500000000000000444, -40.04166666393548013, -4.330127018922193649 ) ) ;
#26876 = CARTESIAN_POINT ( 'NONE',  ( 4.458734124999998549, -23.72916666530107577, -2.574251347313721627 ) ) ;
#26877 = CARTESIAN_POINT ( 'NONE',  ( 2.071067811865476394, -150.1874999999999716, 5.000000000000000000 ) ) ;
#26878 = CARTESIAN_POINT ( 'NONE',  ( -2.499999999999996447, -15.83333333333333037, 4.330127018922195425 ) ) ;
#26879 = CARTESIAN_POINT ( 'NONE',  ( 2.730187237215162345E-16, -152.1875000013656063, -4.458734124999999437 ) ) ;
#26880 = ORIENTED_EDGE ( 'NONE', *, *, #27013, .T. ) ;
#26881 = CYLINDRICAL_SURFACE ( 'NONE', #4042, 5.000000000000000000 ) ;
#26882 = CARTESIAN_POINT ( 'NONE',  ( 4.458734124999998549, -49.97916666530106511, -2.574251347313721627 ) ) ;
#26883 = CARTESIAN_POINT ( 'NONE',  ( 2.499999999999998668, -58.20833333060214443, -4.330127018922193649 ) ) ;
#26884 = CARTESIAN_POINT ( 'NONE',  ( 7.500000000000000000, 4.330127018922199866, -1.000000000000000888 ) ) ;
#26885 = CARTESIAN_POINT ( 'NONE',  ( -2.499999999999996447, 24.16666666666666785, 4.330127018922195425 ) ) ;
#26886 = CARTESIAN_POINT ( 'NONE',  ( 1.339745962155615144, -76.58034179853029855, 4.999999999999999112 ) ) ;
#26887 = CARTESIAN_POINT ( 'NONE',  ( 2.229367062499998831, 6.354166668032262599, -3.861377020970580887 ) ) ;
#26888 = CARTESIAN_POINT ( 'NONE',  ( 1.339745962155615144, 1.419658201469705672, 4.999999999999999112 ) ) ;
#26889 = CARTESIAN_POINT ( 'NONE',  ( 5.000000000000000000, -11.37499999726881583, -6.123233995736766282E-16 ) ) ;
#26890 = DIRECTION ( 'NONE',  ( -0.000000000000000000, 1.000000000000000000, -0.000000000000000000 ) ) ;
#26891 = CARTESIAN_POINT ( 'NONE',  ( -2.229367062499996610, 16.60416666803225638, 3.861377020970582219 ) ) ;
#26892 = CARTESIAN_POINT ( 'NONE',  ( -5.000000000000000000, 2.041666669397854239, -2.886751345948128211 ) ) ;
#26893 = ORIENTED_EDGE ( 'NONE', *, *, #9368, .F. ) ;
#26894 = CARTESIAN_POINT ( 'NONE',  ( 2.499999999999998668, 26.66666666666666430, -4.330127018922193649 ) ) ;
#26895 = VERTEX_POINT ( 'NONE', #58165 ) ;
#26896 = CARTESIAN_POINT ( 'NONE',  ( -1.339745962155610925, -23.66965819600732956, 5.000000000000000000 ) ) ;
#26897 = CARTESIAN_POINT ( 'NONE',  ( -2.229367062500000163, -44.47916666530106511, -3.861377020970580443 ) ) ;
#26898 = CARTESIAN_POINT ( 'NONE',  ( -1.846868145590737420, -164.0000000013656063, 4.458734124999999437 ) ) ;
#26899 = CARTESIAN_POINT ( 'NONE',  ( 2.500000000000002220, -42.54166666393548013, 4.330127018922192761 ) ) ;
#26900 = ORIENTED_EDGE ( 'NONE', *, *, #1416, .T. ) ;
#26901 = CARTESIAN_POINT ( 'NONE',  ( 2.229367062499998831, -19.64583333196774007, -3.861377020970580887 ) ) ;
#26902 = ORIENTED_EDGE ( 'NONE', *, *, #31803, .F. ) ;
#26903 = CARTESIAN_POINT ( 'NONE',  ( 5.000000000000000000, -87.41666666666667140, -2.886751345948129988 ) ) ;
#26904 = CARTESIAN_POINT ( 'NONE',  ( -4.458734124999999437, -165.9375000013655779, -5.460374474430324690E-16 ) ) ;
#26905 = EDGE_CURVE ( 'NONE', #14930, #53159, #14096, .T. ) ;
#26907 = ORIENTED_EDGE ( 'NONE', *, *, #63066, .T. ) ;
#26906 = CARTESIAN_POINT ( 'NONE',  ( -4.999999999999998224, -60.79166666393547303, 2.886751345948131764 ) ) ;
#26908 = CARTESIAN_POINT ( 'NONE',  ( -53.33387254593733928, -135.8125000000000000, 5.149110718188519620 ) ) ;
#26909 = CARTESIAN_POINT ( 'NONE',  ( 4.458734125000001214, -31.14583333196773651, 2.574251347313718519 ) ) ;
#26910 = CARTESIAN_POINT ( 'NONE',  ( -14.99999999999998934, -1.734723475976807094E-15, -10.00000000000000000 ) ) ;
#26911 = ORIENTED_EDGE ( 'NONE', *, *, #60368, .T. ) ;
#26912 = EDGE_CURVE ( 'NONE', #9066, #13678, #55779, .T. ) ;
#26913 = CONTEXT_DEPENDENT_SHAPE_REPRESENTATION ( #55298, #25080 ) ;
#26914 = CARTESIAN_POINT ( 'NONE',  ( 2.229367062500001939, -77.97916666530106511, 3.861377020970579999 ) ) ;
#26915 = CARTESIAN_POINT ( 'NONE',  ( -2.229367062499996610, 25.85416666803225993, 3.861377020970582219 ) ) ;
#26916 = CARTESIAN_POINT ( 'NONE',  ( 2.499999999999998668, 24.79166666939785202, -4.330127018922193649 ) ) ;
#26917 = EDGE_LOOP ( 'NONE', ( #31961, #13931, #55545, #62440 ) ) ;
#26918 = CARTESIAN_POINT ( 'NONE',  ( -4.999999999999998224, 5.208333336064518981, 2.886751345948131764 ) ) ;
#26919 = CARTESIAN_POINT ( 'NONE',  ( -52.10840900171896806, -141.4375000013656063, 3.393966926194110556 ) ) ;
#26920 = VECTOR ( 'NONE', #20332, 1000.000000000000000 ) ;
#26921 = CARTESIAN_POINT ( 'NONE',  ( -4.458734124999999437, -82.56249999863440792, 0.000000000000000000 ) ) ;
#26922 = CARTESIAN_POINT ( 'NONE',  ( -49.85088928181150436, -131.6875000027312126, -1.666127454062680702 ) ) ;
#26923 = CARTESIAN_POINT ( 'NONE',  ( -6.972266317189433020E-16, 15.87500000273118417, -5.000000000000000000 ) ) ;
#26924 = CARTESIAN_POINT ( 'NONE',  ( -1.339745962155613812, 5.919658201469705894, -5.000000000000000000 ) ) ;
#26925 = CARTESIAN_POINT ( 'NONE',  ( -3.152548672688508926E-16, -52.56249999863440792, -5.148502694627439702 ) ) ;
#26926 = CARTESIAN_POINT ( 'NONE',  ( 2.229367062500001939, -44.97916666530106511, 3.861377020970579999 ) ) ;
#26927 = CARTESIAN_POINT ( 'NONE',  ( 4.458734125000001214, 26.10416666803225993, 2.574251347313718519 ) ) ;
#26928 = CARTESIAN_POINT ( 'NONE',  ( 5.000000000000000000, -106.4166666666666572, -2.886751345948129988 ) ) ;
#26929 = CYLINDRICAL_SURFACE ( 'NONE', #22738, 5.000000000000000000 ) ;
#26930 = CARTESIAN_POINT ( 'NONE',  ( -2.229367062500000163, -40.72916666530107221, -3.861377020970580443 ) ) ;
#26931 = CARTESIAN_POINT ( 'NONE',  ( -3.535250795749689387E-16, -0.1249999972688133065, -5.773502691896257311 ) ) ;
#26932 = CARTESIAN_POINT ( 'NONE',  ( -58.80597590150559739, -154.0000000000000284, 3.242614290531460330 ) ) ;
#26933 = CARTESIAN_POINT ( 'NONE',  ( 0.000000000000000000, -170.0000000000000000, 0.000000000000000000 ) ) ;
#26934 = CARTESIAN_POINT ( 'NONE',  ( 9.457646018065525792E-16, -79.31249999863439371, 5.148502694627439702 ) ) ;
#26935 = CARTESIAN_POINT ( 'NONE',  ( 5.000000000000000888, 24.41666666666666785, 2.886751345948126879 ) ) ;
#26936 = CARTESIAN_POINT ( 'NONE',  ( -2.229367062500000163, -101.4791666653010651, -3.861377020970580443 ) ) ;
#26937 =( BOUNDED_CURVE ( )  B_SPLINE_CURVE ( 2, ( #49922, #739, #45104, #20676, #15842, #19703, #54446, #59595, #5875 ),
 .UNSPECIFIED., .F., .F. ) 
 B_SPLINE_CURVE_WITH_KNOTS ( ( 3, 2, 2, 2, 3 ),
 ( 0.5446428571428570953, 0.5452380952380951884, 0.5464285714285713746, 0.5476190476190476719, 0.5482142857142857650 ),
 .UNSPECIFIED. ) 
 CURVE ( )  GEOMETRIC_REPRESENTATION_ITEM ( )  RATIONAL_B_SPLINE_CURVE ( ( 0.9330127018922194093, 0.9330127018922194093, 1.000000000000000000, 0.8660254037844387076, 1.000000000000000000, 0.8660254037844387076, 1.000000000000000000, 0.9330127018922194093, 0.9330127018922194093 ) ) 
 REPRESENTATION_ITEM ( '' )  );
#26938 = CARTESIAN_POINT ( 'NONE',  ( -3.152548672688508926E-16, -5.812499998634404363, -5.148502694627439702 ) ) ;
#26939 = VERTEX_POINT ( 'NONE', #926 ) ;
#26940 = DIRECTION ( 'NONE',  ( -0.000000000000000000, 1.000000000000000000, -0.000000000000000000 ) ) ;
#26941 = CARTESIAN_POINT ( 'NONE',  ( -2.499999999999996447, -35.70833333060213732, 4.330127018922195425 ) ) ;
#26942 = CARTESIAN_POINT ( 'NONE',  ( 2.229367062499998831, -93.64583333196772230, -3.861377020970580887 ) ) ;
#26943 = CARTESIAN_POINT ( 'NONE',  ( -5.000000000000000888, -167.5625000027312126, 2.071067811865474617 ) ) ;
#26944 = CARTESIAN_POINT ( 'NONE',  ( 2.229367062500001939, -89.22916666530106511, 3.861377020970579999 ) ) ;
#26945 = CARTESIAN_POINT ( 'NONE',  ( -4.458734124999997661, 13.52083333469892779, 2.574251347313722516 ) ) ;
#26946 = DIRECTION ( 'NONE',  ( 0.000000000000000000, 0.000000000000000000, 1.000000000000000000 ) ) ;
#26947 = CARTESIAN_POINT ( 'NONE',  ( -56.48576386720575471, -132.7500000013656063, -4.591703134518078322 ) ) ;
#26948 = CARTESIAN_POINT ( 'NONE',  ( 2.229367062499998831, -9.645833331967738289, -3.861377020970580887 ) ) ;
#26949 = CARTESIAN_POINT ( 'NONE',  ( -2.229367062500000163, 14.27083333469892601, -3.861377020970580443 ) ) ;
#26950 = CARTESIAN_POINT ( 'NONE',  ( 2.229367062499998831, -53.89583333196773651, -3.861377020970580887 ) ) ;
#26951 = CARTESIAN_POINT ( 'NONE',  ( 2.500000000000002220, -38.54166666393548013, 4.330127018922192761 ) ) ;
#26952 = CARTESIAN_POINT ( 'NONE',  ( -4.458734124999999437, -85.39583333196773651, -2.574251347313719407 ) ) ;
#26953 = CARTESIAN_POINT ( 'NONE',  ( -3.152548672688508926E-16, -7.562499998634404363, -5.148502694627439702 ) ) ;
#26954 = ORIENTED_EDGE ( 'NONE', *, *, #8682, .T. ) ;
#26955 = CARTESIAN_POINT ( 'NONE',  ( -3.152548672688508926E-16, -33.81249999863440792, -5.148502694627439702 ) ) ;
#26956 = CARTESIAN_POINT ( 'NONE',  ( -52.10840900171896806, -126.4375000013656063, 3.393966926194110556 ) ) ;
#26957 = CARTESIAN_POINT ( 'NONE',  ( -4.458734124999998549, -82.22916666530107932, 2.574251347313722516 ) ) ;
#26958 = CARTESIAN_POINT ( 'NONE',  ( 2.229367062500001939, 26.77083333469892423, 3.861377020970579999 ) ) ;
#26959 = CARTESIAN_POINT ( 'NONE',  ( 1.846868145590735200, -150.5000000013656347, -4.458734124999999437 ) ) ;
#26960 = CARTESIAN_POINT ( 'NONE',  ( -2.229367062499996610, 22.85416666803225993, 3.861377020970582219 ) ) ;
#26961 = CARTESIAN_POINT ( 'NONE',  ( -5.000000000000000000, -94.08333333333332860, -2.886751345948128211 ) ) ;
#26962 = CARTESIAN_POINT ( 'NONE',  ( -58.24261429053147765, -135.2500000000000284, -3.805975901505573855 ) ) ;
#26963 = CARTESIAN_POINT ( 'NONE',  ( -4.458734124999997661, -83.47916666530106511, 2.574251347313722516 ) ) ;
#26964 = CARTESIAN_POINT ( 'NONE',  ( 5.000000000000000000, -63.50000000000000000, -6.123233995736766282E-16 ) ) ;
#26965 = CYLINDRICAL_SURFACE ( 'NONE', #20296, 5.000000000000000000 ) ;
#26966 = CARTESIAN_POINT ( 'NONE',  ( 5.000000000000000888, 17.54166666939785557, 2.886751345948126879 ) ) ;
#26967 = ORIENTED_EDGE ( 'NONE', *, *, #22095, .F. ) ;
#26968 = CARTESIAN_POINT ( 'NONE',  ( -5.000000000000000000, 27.99999999999999645, 0.000000000000000000 ) ) ;
#26970 = CARTESIAN_POINT ( 'NONE',  ( 5.000000000000000888, -22.58333333333333215, 2.886751345948126879 ) ) ;
#26969 = CARTESIAN_POINT ( 'NONE',  ( -1.339745962155613812, -107.0803417985302843, -5.000000000000000000 ) ) ;
#26971 = CARTESIAN_POINT ( 'NONE',  ( 4.458734124999999437, -27.81249999863440081, -5.460374474430324690E-16 ) ) ;
#26972 = CARTESIAN_POINT ( 'NONE',  ( -4.458734124999999437, -88.31249999863439371, 0.000000000000000000 ) ) ;
#26973 = CARTESIAN_POINT ( 'NONE',  ( -5.000000000000000000, -27.95833333060214798, -2.886751345948128211 ) ) ;
#26975 = ORIENTED_EDGE ( 'NONE', *, *, #55500, .T. ) ;
#26974 = CARTESIAN_POINT ( 'NONE',  ( 9.457646018065525792E-16, -56.06249999863440792, 5.148502694627439702 ) ) ;
#26976 = CARTESIAN_POINT ( 'NONE',  ( 5.000000000000000000, -28.49999999999999645, -6.123233995736766282E-16 ) ) ;
#26978 = ORIENTED_EDGE ( 'NONE', *, *, #8824, .T. ) ;
#26977 = CARTESIAN_POINT ( 'NONE',  ( -4.458734124999999437, -9.645833331967738289, -2.574251347313719407 ) ) ;
#26979 = CARTESIAN_POINT ( 'NONE',  ( 2.499999999999998668, -71.33333333333332860, -4.330127018922193649 ) ) ;
#26980 = CARTESIAN_POINT ( 'NONE',  ( -59.59170313451810586, -140.5000000013655779, 1.485763867205729394 ) ) ;
#26981 = CARTESIAN_POINT ( 'NONE',  ( -2.229367062499996610, -53.39583333196773651, 3.861377020970582219 ) ) ;
#26982 = CARTESIAN_POINT ( 'NONE',  ( -6.972266317189433020E-16, -96.25000000000000000, -5.000000000000000000 ) ) ;
#26983 = CARTESIAN_POINT ( 'NONE',  ( -3.535250795749689387E-16, -78.12499999726880162, -5.773502691896257311 ) ) ;
#26984 = CARTESIAN_POINT ( 'NONE',  ( -2.500000000000000444, -86.16666666666667140, -4.330127018922193649 ) ) ;
#26985 = CARTESIAN_POINT ( 'NONE',  ( -58.80597590150559739, -150.0000000000000284, 3.242614290531460330 ) ) ;
#26986 = CARTESIAN_POINT ( 'NONE',  ( 4.458734124999998549, -16.97916666530107221, -2.574251347313721627 ) ) ;
#26987 = CARTESIAN_POINT ( 'NONE',  ( -3.152548672688508926E-16, -50.81249999863440792, -5.148502694627439702 ) ) ;
#26988 = CARTESIAN_POINT ( 'NONE',  ( -1.339745962155610925, -29.66965819600733312, 5.000000000000000000 ) ) ;
#26989 = CARTESIAN_POINT ( 'NONE',  ( 4.458734124999999437, -140.4375000013656063, 0.000000000000000000 ) ) ;
#26990 = CARTESIAN_POINT ( 'NONE',  ( -3.152548672688508926E-16, -100.8124999986343937, -5.148502694627439702 ) ) ;
#26991 = CARTESIAN_POINT ( 'NONE',  ( 1.339745962155641346, -2.294658198738521726, -4.999999999999983125 ) ) ;
#26992 = ORIENTED_EDGE ( 'NONE', *, *, #44872, .T. ) ;
#26993 = FACE_OUTER_BOUND ( 'NONE', #25800, .T. ) ;
#26994 = CARTESIAN_POINT ( 'NONE',  ( -58.24261429053147765, -144.3750000027312126, -3.805975901505573855 ) ) ;
#26995 = CARTESIAN_POINT ( 'NONE',  ( 1.339745962155612702, 18.70534180126147916, -5.000000000000000000 ) ) ;
#26996 = CARTESIAN_POINT ( 'NONE',  ( 4.458734125000001214, 0.1041666680322607674, 2.574251347313718519 ) ) ;
#26997 = CARTESIAN_POINT ( 'NONE',  ( 4.458734125000000326, -93.14583333196773651, 2.574251347313718519 ) ) ;
#26998 = CARTESIAN_POINT ( 'NONE',  ( -3.152801135295367096, -149.3125000013655779, -3.152801135295367541 ) ) ;
#26999 = CARTESIAN_POINT ( 'NONE',  ( -4.458734124999998549, -25.47916666530106866, 2.574251347313722516 ) ) ;
#27000 = CARTESIAN_POINT ( 'NONE',  ( 1.975475456537005874E-15, -46.74999999999999289, 5.000000000000000000 ) ) ;
#27001 = CARTESIAN_POINT ( 'NONE',  ( -51.60603307380591787, -138.9375000013656063, -2.891590998281053704 ) ) ;
#27002 = CARTESIAN_POINT ( 'NONE',  ( 9.457646018065525792E-16, -62.31249999863440792, 5.148502694627439702 ) ) ;
#27003 = CYLINDRICAL_SURFACE ( 'NONE', #43511, 5.000000000000000000 ) ;
#27004 = CARTESIAN_POINT ( 'NONE',  ( 75.00000000000000000, 0.000000000000000000, 8.999999999999998224 ) ) ;
#27005 = CARTESIAN_POINT ( 'NONE',  ( 4.458734124999999437, -143.4375000013656063, 0.000000000000000000 ) ) ;
#27006 = CARTESIAN_POINT ( 'NONE',  ( 4.458734124999998549, 12.02083333469892601, -2.574251347313721627 ) ) ;
#27007 = ORIENTED_EDGE ( 'NONE', *, *, #11313, .F. ) ;
#27008 = CARTESIAN_POINT ( 'NONE',  ( 1.975475456537005874E-15, -4.749999999999999112, 5.000000000000000000 ) ) ;
#27009 = CARTESIAN_POINT ( 'NONE',  ( -75.00000000000002842, 0.000000000000000000, -5.000000000000000000 ) ) ;
#27011 = CARTESIAN_POINT ( 'NONE',  ( 2.229367062500001939, -25.97916666530106866, 3.861377020970579999 ) ) ;
#27010 = CARTESIAN_POINT ( 'NONE',  ( -3.535250795749689387E-16, -88.25000000000000000, -5.773502691896257311 ) ) ;
#27012 = CARTESIAN_POINT ( 'NONE',  ( 4.458734124999998549, -72.97916666530107932, -2.574251347313721627 ) ) ;
#27013 = EDGE_CURVE ( 'NONE', #5864, #7305, #55400, .T. ) ;
#27014 = DIRECTION ( 'NONE',  ( -0.000000000000000000, 1.000000000000000000, -0.000000000000000000 ) ) ;
#27015 = CARTESIAN_POINT ( 'NONE',  ( -6.972266317189433020E-16, 14.74999999999999822, -5.000000000000000000 ) ) ;
#27016 =( BOUNDED_CURVE ( )  B_SPLINE_CURVE ( 2, ( #40393, #11445, #30099, #60034, #45543, #867, #41030, #1503, #29779 ),
 .UNSPECIFIED., .F., .F. ) 
 B_SPLINE_CURVE_WITH_KNOTS ( ( 3, 2, 2, 2, 3 ),
 ( 0.02678571428571428770, 0.02738095238095238082, 0.02857142857142857054, 0.02976190476190476025, 0.03035714285714285685 ),
 .UNSPECIFIED. ) 
 CURVE ( )  GEOMETRIC_REPRESENTATION_ITEM ( )  RATIONAL_B_SPLINE_CURVE ( ( 0.9330127018922194093, 0.9330127018922195203, 1.000000000000000000, 0.8660254037844387076, 1.000000000000000000, 0.8660254037844387076, 1.000000000000000000, 0.9330127018922194093, 0.9330127018922194093 ) ) 
 REPRESENTATION_ITEM ( '' )  );
#27017 = CARTESIAN_POINT ( 'NONE',  ( -52.10840900171896806, -147.1875000013656063, 3.393966926194110556 ) ) ;
#27018 = CARTESIAN_POINT ( 'NONE',  ( -5.000000000000000000, -51.87499999726881583, 0.000000000000000000 ) ) ;
#27019 = CARTESIAN_POINT ( 'NONE',  ( 2.499999999999998668, -24.33333333333333215, -4.330127018922193649 ) ) ;
#27020 = CARTESIAN_POINT ( 'NONE',  ( -3.152548672688508926E-16, 8.437500001365595637, -5.148502694627439702 ) ) ;
#27021 = LINE ( 'NONE', #7411, #45825 ) ;
#27022 = DIRECTION ( 'NONE',  ( -0.000000000000000000, 1.000000000000000000, -0.000000000000000000 ) ) ;
#27023 = CARTESIAN_POINT ( 'NONE',  ( -2.229367062500000163, 5.520833334698927786, -3.861377020970580443 ) ) ;
#27024 = CARTESIAN_POINT ( 'NONE',  ( 2.229367062500001939, -72.97916666530107932, 3.861377020970579999 ) ) ;
#27025 = CARTESIAN_POINT ( 'NONE',  ( 2.229367062499998831, -18.89583333196774007, -3.861377020970580887 ) ) ;
#27026 = CARTESIAN_POINT ( 'NONE',  ( 5.000000000000000000, -0.4166666666666659080, -2.886751345948129988 ) ) ;
#27027 = CARTESIAN_POINT ( 'NONE',  ( 4.458734125000000326, -159.3750000013656347, -1.846868145590734978 ) ) ;
#27028 = CARTESIAN_POINT ( 'NONE',  ( -2.071067811865580754, -158.6875000000000000, -4.999999999999894307 ) ) ;
#27029 = CARTESIAN_POINT ( 'NONE',  ( 4.458734125000001214, -64.89583333196773651, 2.574251347313718519 ) ) ;
#27030 = CARTESIAN_POINT ( 'NONE',  ( -4.999999999999999112, -94.79166666393547303, 2.886751345948131764 ) ) ;
#27031 =( BOUNDED_CURVE ( )  B_SPLINE_CURVE ( 2, ( #52003, #36568, #31746, #42023, #42339, #41384, #12443, #51377, #32055 ),
 .UNSPECIFIED., .F., .F. ) 
 B_SPLINE_CURVE_WITH_KNOTS ( ( 3, 2, 2, 2, 3 ),
 ( 0.4916666666666670849, 0.4958333333333337922, 0.5000000000000004441, 0.5041666666666670960, 0.5083333333333337478 ),
 .UNSPECIFIED. ) 
 CURVE ( )  GEOMETRIC_REPRESENTATION_ITEM ( )  RATIONAL_B_SPLINE_CURVE ( ( 0.9999999999999918954, 0.9238795325112948431, 1.000000000000000000, 0.9238795325112867385, 1.000000000000000000, 0.9238795325112867385, 1.000000000000000000, 0.9238795325112786339, 1.000000000000008216 ) ) 
 REPRESENTATION_ITEM ( '' )  );
#27032 = CARTESIAN_POINT ( 'NONE',  ( -59.81910112700025905, -152.3125000027312126, -2.462841084822604110 ) ) ;
#27033 = CARTESIAN_POINT ( 'NONE',  ( -4.458734124999999437, -40.39583333196773651, -2.574251347313719407 ) ) ;
#27034 = CARTESIAN_POINT ( 'NONE',  ( 5.000000000000000000, 19.62500000273118772, -6.123233995736766282E-16 ) ) ;
#27035 = CARTESIAN_POINT ( 'NONE',  ( 4.458734124999998549, -65.97916666530106511, -2.574251347313721627 ) ) ;
#27036 = CARTESIAN_POINT ( 'NONE',  ( -2.500000000000000444, -47.16666666666666430, -4.330127018922193649 ) ) ;
#27037 = CARTESIAN_POINT ( 'NONE',  ( 0.000000000000000000, -170.0000000000000000, 5.000000000000000000 ) ) ;
#27038 = CARTESIAN_POINT ( 'NONE',  ( -6.972266317189433020E-16, -36.12499999726880162, -5.000000000000000000 ) ) ;
#27039 = ORIENTED_EDGE ( 'NONE', *, *, #28102, .F. ) ;
#27040 = CARTESIAN_POINT ( 'NONE',  ( 0.000000000000000000, -120.0000000000000000, 5.000000000000000000 ) ) ;
#27041 = CARTESIAN_POINT ( 'NONE',  ( -3.152548672688508926E-16, -2.812499998634407028, -5.148502694627439702 ) ) ;
#27042 = CARTESIAN_POINT ( 'NONE',  ( -2.499999999999996447, -67.70833333060214443, 4.330127018922195425 ) ) ;
#27043 = CARTESIAN_POINT ( 'NONE',  ( 2.499999999999998668, -10.33333333333333393, -4.330127018922193649 ) ) ;
#27044 = CARTESIAN_POINT ( 'NONE',  ( 4.458734124999998549, -70.72916666530107932, -2.574251347313721627 ) ) ;
#27045 = CARTESIAN_POINT ( 'NONE',  ( -1.339745962155610925, -4.669658196007337558, 5.000000000000000000 ) ) ;
#27046 = CARTESIAN_POINT ( 'NONE',  ( -5.000000000000000000, -13.87499999726881228, 0.000000000000000000 ) ) ;
#27048 = ORIENTED_EDGE ( 'NONE', *, *, #1576, .F. ) ;
#27047 = CARTESIAN_POINT ( 'NONE',  ( -3.152548672688508926E-16, -40.56249999863440081, -5.148502694627439702 ) ) ;
#27049 = CARTESIAN_POINT ( 'NONE',  ( 2.500000000000002220, -81.66666666666667140, 4.330127018922192761 ) ) ;
#27051 = EDGE_LOOP ( 'NONE', ( #49091, #57147, #51667, #50376 ) ) ;
#27050 = CARTESIAN_POINT ( 'NONE',  ( 2.229367062499998831, 10.10416666803225993, -3.861377020970580887 ) ) ;
#27052 = CARTESIAN_POINT ( 'NONE',  ( 1.975475456537005874E-15, -81.74999999999998579, 5.000000000000000000 ) ) ;
#27053 = CARTESIAN_POINT ( 'NONE',  ( 5.000000000000000000, -54.49999999999999289, -6.123233995736766282E-16 ) ) ;
#27054 = CARTESIAN_POINT ( 'NONE',  ( 3.152801135295367541, -160.5625000013656063, -3.152801135295367541 ) ) ;
#27055 = CARTESIAN_POINT ( 'NONE',  ( 2.229367062500001939, -33.22916666530106511, 3.861377020970579999 ) ) ;
#27056 = CARTESIAN_POINT ( 'NONE',  ( -2.499999999999996447, -86.83333333333332860, 4.330127018922195425 ) ) ;
#27057 = CARTESIAN_POINT ( 'NONE',  ( -4.458734124999998549, -79.22916666530107932, 2.574251347313722516 ) ) ;
#27058 = CARTESIAN_POINT ( 'NONE',  ( 5.000000000000000888, -164.9375000000000284, -2.071067811865475505 ) ) ;
#27059 = CARTESIAN_POINT ( 'NONE',  ( 4.458734124999998549, -87.72916666530107932, -2.574251347313721627 ) ) ;
#27060 = CARTESIAN_POINT ( 'NONE',  ( -59.44456063193725015, -136.8125000013656063, -0.3552334253322034230 ) ) ;
#27061 = CARTESIAN_POINT ( 'NONE',  ( -3.152548672688508926E-16, -0.8124999986344055847, -5.148502694627439702 ) ) ;
#27062 = CARTESIAN_POINT ( 'NONE',  ( 2.229367062499998831, -36.89583333196773651, -3.861377020970580887 ) ) ;
#27063 = VECTOR ( 'NONE', #21219, 1000.000000000000000 ) ;
#27064 = CARTESIAN_POINT ( 'NONE',  ( 5.000000000000000000, -72.41666666666665719, -2.886751345948130876 ) ) ;
#27065 = CARTESIAN_POINT ( 'NONE',  ( -2.229367062499996610, -78.39583333196773651, 3.861377020970582219 ) ) ;
#27066 = FACE_OUTER_BOUND ( 'NONE', #43217, .T. ) ;
#27067 = ORIENTED_EDGE ( 'NONE', *, *, #52004, .F. ) ;
#27068 = CARTESIAN_POINT ( 'NONE',  ( -3.535533905932737309, -141.6250000000000000, -3.535533905932738197 ) ) ;
#27069 = CARTESIAN_POINT ( 'NONE',  ( -2.500000000000000444, -19.04166666393547658, -4.330127018922193649 ) ) ;
#27070 = CARTESIAN_POINT ( 'NONE',  ( 2.229367062499998831, -71.89583333196773651, -3.861377020970580887 ) ) ;
#27071 = CARTESIAN_POINT ( 'NONE',  ( 2.229367062499998831, -7.895833331967735624, -3.861377020970580887 ) ) ;
#27072 = VERTEX_POINT ( 'NONE', #50741 ) ;
#27073 = CARTESIAN_POINT ( 'NONE',  ( -3.535533905932737309, -150.7500000027312126, -3.535533905932738197 ) ) ;
#27074 = CARTESIAN_POINT ( 'NONE',  ( -3.535533905932737309, -146.7500000027311842, -3.535533905932738197 ) ) ;
#27075 = CARTESIAN_POINT ( 'NONE',  ( -4.458734124999998549, -8.479166665301073991, 2.574251347313722516 ) ) ;
#27076 = CARTESIAN_POINT ( 'NONE',  ( -50.01589407740564042, -148.7500000027312126, 0.3983568153799778022 ) ) ;
#27077 = CARTESIAN_POINT ( 'NONE',  ( 9.457646018065525792E-16, 6.937500001365594748, 5.148502694627439702 ) ) ;
#27078 = LINE ( 'NONE', #40593, #61405 ) ;
#27079 = CARTESIAN_POINT ( 'NONE',  ( -4.458734124999999437, -156.9375000013655779, -5.460374474430324690E-16 ) ) ;
#27080 =( BOUNDED_CURVE ( )  B_SPLINE_CURVE ( 2, ( #30480, #929, #35960, #21160, #51704, #32067, #45599, #16970, #36581 ),
 .UNSPECIFIED., .F., .F. ) 
 B_SPLINE_CURVE_WITH_KNOTS ( ( 3, 2, 2, 2, 3 ),
 ( 0.2895833333333333592, 0.2902777777777778012, 0.2916666666666666852, 0.2930555555555555691, 0.2937500000000000111 ),
 .UNSPECIFIED. ) 
 CURVE ( )  GEOMETRIC_REPRESENTATION_ITEM ( )  RATIONAL_B_SPLINE_CURVE ( ( 0.9330127018922194093, 0.9330127018922220739, 1.000000000000000000, 0.8660254037844387076, 1.000000000000000000, 0.8660254037844387076, 1.000000000000000000, 0.9330127018922194093, 0.9330127018922194093 ) ) 
 REPRESENTATION_ITEM ( '' )  );
#27081 = CARTESIAN_POINT ( 'NONE',  ( 2.229367062500001939, 28.77083333469892779, 3.861377020970579999 ) ) ;
#27082 = VERTEX_POINT ( 'NONE', #60088 ) ;
#27083 = CARTESIAN_POINT ( 'NONE',  ( 2.229367062500001939, -87.97916666530107932, 3.861377020970579999 ) ) ;
#27084 = LINE ( 'NONE', #47953, #42835 ) ;
#27085 = CARTESIAN_POINT ( 'NONE',  ( 2.229367062499998831, -8.645833331967736513, -3.861377020970580887 ) ) ;
#27086 = EDGE_CURVE ( 'NONE', #55783, #28080, #40128, .T. ) ;
#27087 = CARTESIAN_POINT ( 'NONE',  ( 4.403473400622098133, 6.117907484625861869, 2.043043468777371629E-15 ) ) ;
#27088 = CYLINDRICAL_SURFACE ( 'NONE', #11973, 5.000000000000000000 ) ;
#27089 = CARTESIAN_POINT ( 'NONE',  ( -5.000000000000000000, -32.95833333060215153, -2.886751345948128211 ) ) ;
#27090 = CARTESIAN_POINT ( 'NONE',  ( 0.000000000000000000, -120.0000000000000000, 5.000000000000000000 ) ) ;
#27091 = CARTESIAN_POINT ( 'NONE',  ( -2.229367062499996610, 25.85416666803225993, 3.861377020970582219 ) ) ;
#27092 = CARTESIAN_POINT ( 'NONE',  ( 1.975475456537005874E-15, -7.750000000000000000, 5.000000000000000000 ) ) ;
#27093 = CARTESIAN_POINT ( 'NONE',  ( -4.458734124999999437, 24.68750000136559208, 0.000000000000000000 ) ) ;
#27094 = CARTESIAN_POINT ( 'NONE',  ( -2.229367062500000163, -51.47916666530107221, -3.861377020970580443 ) ) ;
#27095 = CARTESIAN_POINT ( 'NONE',  ( 2.229367062500001939, -37.22916666530107221, 3.861377020970579999 ) ) ;
#27096 = CARTESIAN_POINT ( 'NONE',  ( 4.458734125000000326, -5.145833331967740065, 2.574251347313718519 ) ) ;
#27097 = CARTESIAN_POINT ( 'NONE',  ( -5.000000000000000000, -149.6250000027312126, -6.123233995736766282E-16 ) ) ;
#27098 = CARTESIAN_POINT ( 'NONE',  ( -5.000000000000000000, 13.00000000000000178, 0.000000000000000000 ) ) ;
#27099 = CARTESIAN_POINT ( 'NONE',  ( -2.071067811865475061, -140.8125000027312126, -5.000000000000000888 ) ) ;
#27101 = EDGE_CURVE ( 'NONE', #26096, #62985, #35673, .T. ) ;
#27100 = CARTESIAN_POINT ( 'NONE',  ( 2.500000000000002220, -33.54166666393547303, 4.330127018922192761 ) ) ;
#27102 = CARTESIAN_POINT ( 'NONE',  ( -2.229367062499996610, -48.14583333196772941, 3.861377020970582219 ) ) ;
#27103 = CARTESIAN_POINT ( 'NONE',  ( -3.535250795749689387E-16, -79.12499999726881583, -5.773502691896257311 ) ) ;
#27104 = CARTESIAN_POINT ( 'NONE',  ( -54.64476657466781973, -140.0625000013656063, -4.444560631937228834 ) ) ;
#27105 = AXIS2_PLACEMENT_3D ( 'NONE', #12906, #32529, #27704 ) ;
#27106 = DIRECTION ( 'NONE',  ( -0.000000000000000000, 1.000000000000000000, -0.000000000000000000 ) ) ;
#27107 = CARTESIAN_POINT ( 'NONE',  ( -5.000000000000000000, -63.87499999726880873, 0.000000000000000000 ) ) ;
#27108 = EDGE_CURVE ( 'NONE', #1919, #7754, #35001, .T. ) ;
#27109 = CARTESIAN_POINT ( 'NONE',  ( -2.229367062500000163, -85.72916666530107932, -3.861377020970580443 ) ) ;
#27110 = CARTESIAN_POINT ( 'NONE',  ( 3.152801135295367541, -162.5625000013656063, -3.152801135295367541 ) ) ;
#27111 = CARTESIAN_POINT ( 'NONE',  ( 1.060575238724906964E-15, -30.75000000000000000, 5.773502691896257311 ) ) ;
#27112 = FACE_OUTER_BOUND ( 'NONE', #61637, .T. ) ;
#27113 = ORIENTED_EDGE ( 'NONE', *, *, #29470, .T. ) ;
#27114 = CARTESIAN_POINT ( 'NONE',  ( -4.458734124999998549, 18.52083333469892779, 2.574251347313722516 ) ) ;
#27115 = VERTEX_POINT ( 'NONE', #15695 ) ;
#27116 = CARTESIAN_POINT ( 'NONE',  ( 2.229367062500001939, -91.97916666530106511, 3.861377020970579999 ) ) ;
#27117 = CARTESIAN_POINT ( 'NONE',  ( 2.229367062500001939, 15.77083333469892601, 3.861377020970579999 ) ) ;
#27118 = CARTESIAN_POINT ( 'NONE',  ( -5.000000000000000000, 17.04166666939785202, -2.886751345948128211 ) ) ;
#27119 = CARTESIAN_POINT ( 'NONE',  ( 1.975475456537005874E-15, -34.62499999726880873, 5.000000000000000000 ) ) ;
#27120 = CARTESIAN_POINT ( 'NONE',  ( -2.500000000000000444, 10.83333333333333393, -4.330127018922193649 ) ) ;
#27121 = CARTESIAN_POINT ( 'NONE',  ( -3.152548672688508926E-16, -57.56249999863440792, -5.148502694627439702 ) ) ;
#27122 = DIRECTION ( 'NONE',  ( 0.8660254037844505870, 0.4999999999999792388, -0.000000000000000000 ) ) ;
#27123 = CARTESIAN_POINT ( 'NONE',  ( 5.000000000000000000, -78.50000000000000000, -6.123233995736766282E-16 ) ) ;
#27124 = CARTESIAN_POINT ( 'NONE',  ( -6.972266317189433020E-16, -13.12499999726881050, -5.000000000000000000 ) ) ;
#27125 = CARTESIAN_POINT ( 'NONE',  ( -2.500000000000000444, -13.04166666393548013, -4.330127018922193649 ) ) ;
#27126 = CARTESIAN_POINT ( 'NONE',  ( 10.39117206796836257, 0.000000000000000000, -8.499999999999998224 ) ) ;
#27127 = CARTESIAN_POINT ( 'NONE',  ( 1.060575238724906964E-15, -40.74999999999999289, 5.773502691896257311 ) ) ;
#27128 = CARTESIAN_POINT ( 'NONE',  ( 1.975475456537005874E-15, -88.62499999726880162, 5.000000000000000000 ) ) ;
#27130 = CARTESIAN_POINT ( 'NONE',  ( -2.229367062500000163, -17.72916666530106866, -3.861377020970580443 ) ) ;
#27129 = CARTESIAN_POINT ( 'NONE',  ( -59.81910112700027327, -139.1874999999999716, -2.462841084822392279 ) ) ;
#27131 = CARTESIAN_POINT ( 'NONE',  ( -2.071067811865432873, -143.6875000000000000, -5.000000000000041744 ) ) ;
#27132 = CARTESIAN_POINT ( 'NONE',  ( -4.458734124999999437, -63.39583333196772941, -2.574251347313719407 ) ) ;
#27133 =( BOUNDED_CURVE ( )  B_SPLINE_CURVE ( 2, ( #10464, #5652, #25265, #3118, #27858, #12753, #17593, #53252, #3432 ),
 .UNSPECIFIED., .F., .F. ) 
 B_SPLINE_CURVE_WITH_KNOTS ( ( 3, 2, 2, 2, 3 ),
 ( 0.8395833333333333481, 0.8402777777777777901, 0.8416666666666666741, 0.8430555555555555580, 0.8437500000000000000 ),
 .UNSPECIFIED. ) 
 CURVE ( )  GEOMETRIC_REPRESENTATION_ITEM ( )  RATIONAL_B_SPLINE_CURVE ( ( 0.9330127018922194093, 0.9330127018922194093, 1.000000000000000000, 0.8660254037844387076, 1.000000000000000000, 0.8660254037844387076, 1.000000000000000000, 0.9330127018922194093, 0.9330127018922194093 ) ) 
 REPRESENTATION_ITEM ( '' )  );
#27134 = CARTESIAN_POINT ( 'NONE',  ( -1.846868145590737420, -153.0000000013656063, 4.458734124999999437 ) ) ;
#27135 = CARTESIAN_POINT ( 'NONE',  ( 4.458734124999999437, -69.81249999863439371, -5.460374474430324690E-16 ) ) ;
#27136 = CARTESIAN_POINT ( 'NONE',  ( -50.40829686548195099, -148.2500000013656063, -1.485763867205728284 ) ) ;
#27137 = CARTESIAN_POINT ( 'NONE',  ( -2.229367062500000163, -19.72916666530107221, -3.861377020970580443 ) ) ;
#27138 = CARTESIAN_POINT ( 'NONE',  ( 5.000000000000000000, -62.29166666393547303, -2.886751345948129988 ) ) ;
#27139 = ORIENTED_EDGE ( 'NONE', *, *, #41984, .T. ) ;
#27140 = EDGE_CURVE ( 'NONE', #16274, #56674, #53688, .T. ) ;
#27141 = CARTESIAN_POINT ( 'NONE',  ( -6.972266317189433020E-16, -49.24999999999999289, -5.000000000000000000 ) ) ;
#27142 = VERTEX_POINT ( 'NONE', #30152 ) ;
#27143 = CARTESIAN_POINT ( 'NONE',  ( -4.458734124999999437, -64.64583333196772230, -2.574251347313719407 ) ) ;
#27144 = CARTESIAN_POINT ( 'NONE',  ( 5.000000000000000888, -149.0625000027311842, -2.071067811865475505 ) ) ;
#27145 = CARTESIAN_POINT ( 'NONE',  ( -3.152801135295367985, -152.8125000013656063, 3.152801135295367096 ) ) ;
#27146 = ORIENTED_EDGE ( 'NONE', *, *, #30734, .T. ) ;
#27147 = CARTESIAN_POINT ( 'NONE',  ( -1.339745962155613812, 2.919658201469706782, -5.000000000000000000 ) ) ;
#27148 = FACE_OUTER_BOUND ( 'NONE', #16472, .T. ) ;
#27149 = CARTESIAN_POINT ( 'NONE',  ( 1.975475456537005874E-15, -55.62499999726880873, 5.000000000000000000 ) ) ;
#27150 = CARTESIAN_POINT ( 'NONE',  ( 4.458734125000001214, -56.14583333196774362, 2.574251347313718519 ) ) ;
#27151 = ORIENTED_EDGE ( 'NONE', *, *, #31884, .F. ) ;
#27152 = AXIS2_PLACEMENT_3D ( 'NONE', #63124, #5204, #49267 ) ;
#27153 = FACE_OUTER_BOUND ( 'NONE', #49204, .T. ) ;
#27154 = CARTESIAN_POINT ( 'NONE',  ( -4.458734124999999437, 6.687500001365593860, 0.000000000000000000 ) ) ;
#27155 = CARTESIAN_POINT ( 'NONE',  ( 4.458734124999998549, 25.27083333469892779, -2.574251347313721627 ) ) ;
#27156 = CARTESIAN_POINT ( 'NONE',  ( -52.10840900171896806, -148.1875000013656063, 3.393966926194110556 ) ) ;
#27157 = CARTESIAN_POINT ( 'NONE',  ( 1.062108568985190270E-13, -13.12499999726881583, -4.999999999999999112 ) ) ;
#27158 = CARTESIAN_POINT ( 'NONE',  ( 1.975475456537005874E-15, -23.75000000000000000, 5.000000000000000000 ) ) ;
#27159 = ORIENTED_EDGE ( 'NONE', *, *, #49870, .F. ) ;
#27160 = CARTESIAN_POINT ( 'NONE',  ( 4.458734125000000326, -71.89583333196773651, 2.574251347313718519 ) ) ;
#27161 = CARTESIAN_POINT ( 'NONE',  ( -6.972266317189433020E-16, -86.12499999726880162, -5.000000000000000000 ) ) ;
#27162 = CARTESIAN_POINT ( 'NONE',  ( -3.152548672688508926E-16, 11.43750000136559386, -5.148502694627439702 ) ) ;
#27163 = EDGE_CURVE ( 'NONE', #42248, #59111, #2804, .T. ) ;
#27164 = CARTESIAN_POINT ( 'NONE',  ( 0.000000000000000000, -170.0000000000000000, 0.000000000000000000 ) ) ;
#27165 = EDGE_CURVE ( 'NONE', #53696, #48010, #60291, .T. ) ;
#27166 = CARTESIAN_POINT ( 'NONE',  ( 9.457646018065525792E-16, -55.31249999863439371, 5.148502694627439702 ) ) ;
#27167 = CARTESIAN_POINT ( 'NONE',  ( 5.000000000000000000, -16.37499999726881228, -6.123233995736766282E-16 ) ) ;
#27168 = CARTESIAN_POINT ( 'NONE',  ( -2.500000000000000444, -19.16666666666666430, -4.330127018922193649 ) ) ;
#27169 = CARTESIAN_POINT ( 'NONE',  ( 6.123233995736766282E-16, -120.0000000000000000, -5.000000000000000000 ) ) ;
#27170 = CARTESIAN_POINT ( 'NONE',  ( -4.458734124999998549, -34.22916666530107221, 2.574251347313722516 ) ) ;
#27171 = CARTESIAN_POINT ( 'NONE',  ( -4.458734124999999437, -23.64583333196773651, -2.574251347313719407 ) ) ;
#27172 = ORIENTED_EDGE ( 'NONE', *, *, #39359, .T. ) ;
#27173 = CARTESIAN_POINT ( 'NONE',  ( 1.975475456537005874E-15, -27.62499999726880873, 5.000000000000000000 ) ) ;
#27174 = CARTESIAN_POINT ( 'NONE',  ( -5.000000000000000000, 28.99999999999999645, 0.000000000000000000 ) ) ;
#27175 = CARTESIAN_POINT ( 'NONE',  ( 3.535533905932738197, -154.0000000027312126, -3.535533905932738197 ) ) ;
#27176 = ORIENTED_EDGE ( 'NONE', *, *, #22478, .T. ) ;
#27177 = CARTESIAN_POINT ( 'NONE',  ( -4.458734124999999437, -103.5624999986344079, 0.000000000000000000 ) ) ;
#27178 = CARTESIAN_POINT ( 'NONE',  ( 4.458734124999998549, -28.72916666530107221, -2.574251347313721627 ) ) ;
#27179 = CARTESIAN_POINT ( 'NONE',  ( 5.000000000000000888, -63.45833333060215153, 2.886751345948126879 ) ) ;
#27180 = EDGE_CURVE ( 'NONE', #21022, #37557, #27246, .T. ) ;
#27181 = CARTESIAN_POINT ( 'NONE',  ( -55.35523342533222291, -152.5625000013656063, 4.444560631937231499 ) ) ;
#27182 = CARTESIAN_POINT ( 'NONE',  ( -3.535533905932738641, -147.3750000000000000, 3.535533905932737309 ) ) ;
#27183 = CARTESIAN_POINT ( 'NONE',  ( -3.152548672688508926E-16, -30.56249999863440436, -5.148502694627439702 ) ) ;
#27184 = EDGE_CURVE ( 'NONE', #34622, #35553, #9723, .T. ) ;
#27185 = CARTESIAN_POINT ( 'NONE',  ( 4.458734124999998549, -71.97916666530107932, -2.574251347313721627 ) ) ;
#27186 = CARTESIAN_POINT ( 'NONE',  ( -2.229367062499996610, -25.14583333196773651, 3.861377020970582219 ) ) ;
#27187 = CARTESIAN_POINT ( 'NONE',  ( 1.339745962155615144, -32.58034179853029144, 4.999999999999999112 ) ) ;
#27188 = CARTESIAN_POINT ( 'NONE',  ( -2.500000000000000444, 8.958333336064518093, -4.330127018922193649 ) ) ;
#27189 = CARTESIAN_POINT ( 'NONE',  ( 1.060575238724906964E-15, -15.75000000000000178, 5.773502691896257311 ) ) ;
#27190 = CARTESIAN_POINT ( 'NONE',  ( -1.846868145590737420, -151.7500000013655779, 4.458734124999999437 ) ) ;
#27191 = EDGE_LOOP ( 'NONE', ( #10978, #23086, #57197, #1476 ) ) ;
#27192 = CARTESIAN_POINT ( 'NONE',  ( -51.75738570946856498, -152.7500000000000284, 3.805975901505576964 ) ) ;
#27193 = CARTESIAN_POINT ( 'NONE',  ( -4.458734124999999437, -53.64583333196773651, -2.574251347313719407 ) ) ;
#27194 = CARTESIAN_POINT ( 'NONE',  ( 1.339745962155612702, -58.16965819600732601, -5.000000000000000000 ) ) ;
#27195 = CARTESIAN_POINT ( 'NONE',  ( 5.000000000000000000, -81.37499999726881583, -6.123233995736766282E-16 ) ) ;
#27196 = CARTESIAN_POINT ( 'NONE',  ( 1.060575238724906964E-15, 26.25000000000000000, 5.773502691896257311 ) ) ;
#27197 = CARTESIAN_POINT ( 'NONE',  ( -56.66612745406274598, -152.3125000000000284, -5.149110718188520508 ) ) ;
#27198 = CARTESIAN_POINT ( 'NONE',  ( -4.458734124999999437, 0.6041666680322611560, -2.574251347313719407 ) ) ;
#27199 = CARTESIAN_POINT ( 'NONE',  ( -2.071067811865394237, -160.4375000027312410, 5.000000000000084377 ) ) ;
#27200 = CARTESIAN_POINT ( 'NONE',  ( -9.184850993605147944E-16, -164.2500000000000000, 5.000000000000000000 ) ) ;
#27201 = CARTESIAN_POINT ( 'NONE',  ( 1.975475456537005874E-15, -62.62499999726880873, 5.000000000000000000 ) ) ;
#27202 = CARTESIAN_POINT ( 'NONE',  ( 2.229367062499998831, 16.10416666803225993, -3.861377020970580887 ) ) ;
#27203 = CARTESIAN_POINT ( 'NONE',  ( -2.500000000000000444, 2.958333336064520314, -4.330127018922193649 ) ) ;
#27204 = ORIENTED_EDGE ( 'NONE', *, *, #22999, .T. ) ;
#27205 = CARTESIAN_POINT ( 'NONE',  ( -7.500000000000000888, -3.640541674360520119, -0.7158139487964623182 ) ) ;
#27206 = VERTEX_POINT ( 'NONE', #32065 ) ;
#27207 = CARTESIAN_POINT ( 'NONE',  ( 5.000000000000000000, -7.291666663935481907, -2.886751345948130876 ) ) ;
#27208 = CARTESIAN_POINT ( 'NONE',  ( -4.458734124999998549, -47.22916666530106511, 2.574251347313722516 ) ) ;
#27209 = CARTESIAN_POINT ( 'NONE',  ( -4.458734125000001214, -164.1250000013656063, 1.846868145590734089 ) ) ;
#27210 =( BOUNDED_CURVE ( )  B_SPLINE_CURVE ( 2, ( #15035, #40428, #2181, #51047, #16950, #51372, #6667, #26924, #36888 ),
 .UNSPECIFIED., .F., .F. ) 
 B_SPLINE_CURVE_WITH_KNOTS ( ( 3, 2, 2, 2, 3 ),
 ( 0.1895833333333333259, 0.1902777777777777679, 0.1916666666666666796, 0.1930555555555555636, 0.1937500000000000056 ),
 .UNSPECIFIED. ) 
 CURVE ( )  GEOMETRIC_REPRESENTATION_ITEM ( )  RATIONAL_B_SPLINE_CURVE ( ( 0.9330127018922194093, 0.9330127018922194093, 1.000000000000000000, 0.8660254037844387076, 1.000000000000000000, 0.8660254037844387076, 1.000000000000000000, 0.9330127018922194093, 0.9330127018922194093 ) ) 
 REPRESENTATION_ITEM ( '' )  );
#27211 = CARTESIAN_POINT ( 'NONE',  ( 5.000000000000000000, -44.29166666393546592, -2.886751345948129988 ) ) ;
#27212 = ORIENTED_EDGE ( 'NONE', *, *, #18886, .F. ) ;
#27213 = CARTESIAN_POINT ( 'NONE',  ( 4.458734125000001214, -24.89583333196773651, 2.574251347313718519 ) ) ;
#27214 = ORIENTED_EDGE ( 'NONE', *, *, #7927, .T. ) ;
#27215 = CARTESIAN_POINT ( 'NONE',  ( 2.499999999999998668, -87.33333333333332860, -4.330127018922193649 ) ) ;
#27216 = CARTESIAN_POINT ( 'NONE',  ( -4.458734125000000326, -163.0000000013655779, -1.846868145590735644 ) ) ;
#27217 = CARTESIAN_POINT ( 'NONE',  ( 5.000000000000000000, -39.37499999726880162, -6.123233995736766282E-16 ) ) ;
#27218 = CARTESIAN_POINT ( 'NONE',  ( -52.53715891517739323, -136.4375000000000000, -4.819101127000233298 ) ) ;
#27219 = CARTESIAN_POINT ( 'NONE',  ( -2.229367062499996610, -30.39583333196773651, 3.861377020970582219 ) ) ;
#27220 = CARTESIAN_POINT ( 'NONE',  ( -4.999999999999998224, 23.20833333606451632, 2.886751345948131764 ) ) ;
#27221 = EDGE_LOOP ( 'NONE', ( #59982, #13140, #33516, #32280, #62733 ) ) ;
#27222 = CARTESIAN_POINT ( 'NONE',  ( -2.229367062499996610, -78.14583333196773651, 3.861377020970582219 ) ) ;
#27223 = CARTESIAN_POINT ( 'NONE',  ( 4.458734125000001214, 22.10416666803225993, 2.574251347313718519 ) ) ;
#27224 = ORIENTED_EDGE ( 'NONE', *, *, #56265, .F. ) ;
#27225 = CARTESIAN_POINT ( 'NONE',  ( -55.00000000000002132, -155.0000000000000284, 1.734723475976807094E-15 ) ) ;
#27226 = CARTESIAN_POINT ( 'NONE',  ( -57.19623071787016499, -143.6250000013655779, 4.297418129356382899 ) ) ;
#27227 = CARTESIAN_POINT ( 'NONE',  ( 4.458734124999998549, -79.97916666530107932, -2.574251347313721627 ) ) ;
#27228 = CARTESIAN_POINT ( 'NONE',  ( -57.46284108482265651, -130.0625000027311842, 4.819101127000239515 ) ) ;
#27229 = CARTESIAN_POINT ( 'NONE',  ( 2.499999999999998668, -74.20833333060214443, -4.330127018922193649 ) ) ;
#27230 = CARTESIAN_POINT ( 'NONE',  ( -1.846868145590737420, -140.0000000013655779, 4.458734124999997661 ) ) ;
#27231 = CARTESIAN_POINT ( 'NONE',  ( 5.000000000000000000, -84.29166666393547303, -2.886751345948130876 ) ) ;
#27232 = CARTESIAN_POINT ( 'NONE',  ( -3.152548672688508926E-16, -55.56249999863440081, -5.148502694627439702 ) ) ;
#27233 = CARTESIAN_POINT ( 'NONE',  ( 2.229367062499998831, -47.64583333196774362, -3.861377020970580887 ) ) ;
#27234 = CARTESIAN_POINT ( 'NONE',  ( -6.972266317189433020E-16, 27.74999999999999645, -5.000000000000000000 ) ) ;
#27235 = CARTESIAN_POINT ( 'NONE',  ( -5.000000000000000000, -109.0833333333333286, -2.886751345948128211 ) ) ;
#27236 = CIRCLE ( 'NONE', #63192, 7.500000000000001776 ) ;
#27237 = DIRECTION ( 'NONE',  ( -0.000000000000000000, 1.000000000000000000, -0.000000000000000000 ) ) ;
#27238 = EDGE_CURVE ( 'NONE', #15898, #51084, #31151, .T. ) ;
#27239 = CARTESIAN_POINT ( 'NONE',  ( -4.458734124999999437, -36.56249999863440792, 0.000000000000000000 ) ) ;
#27240 = CARTESIAN_POINT ( 'NONE',  ( -4.999999999999999112, 2.208333336064519870, 2.886751345948131764 ) ) ;
#27241 = CARTESIAN_POINT ( 'NONE',  ( -56.48576386720575471, -125.7500000013656347, -4.591703134518078322 ) ) ;
#27242 = CARTESIAN_POINT ( 'NONE',  ( 4.458734124999999437, -80.06249999863440792, -5.460374474430324690E-16 ) ) ;
#27243 = CARTESIAN_POINT ( 'NONE',  ( -4.458734124999999437, -101.3958333319677365, -2.574251347313719407 ) ) ;
#27244 = CARTESIAN_POINT ( 'NONE',  ( -4.458734124999997661, -3.479166665301069994, 2.574251347313722516 ) ) ;
#27245 = ORIENTED_EDGE ( 'NONE', *, *, #57454, .F. ) ;
#27246 = LINE ( 'NONE', #2815, #50364 ) ;
#27247 = CARTESIAN_POINT ( 'NONE',  ( -3.152548672688508926E-16, -93.56249999863439371, -5.148502694627439702 ) ) ;
#27248 = CARTESIAN_POINT ( 'NONE',  ( 2.071067811865475505, -167.9375000027312126, -5.000000000000000888 ) ) ;
#27249 = CARTESIAN_POINT ( 'NONE',  ( 2.229367062500001939, -85.22916666530107932, 3.861377020970579999 ) ) ;
#27250 = CARTESIAN_POINT ( 'NONE',  ( -4.458734124999999437, 13.35416666803225993, -2.574251347313719407 ) ) ;
#27251 = CYLINDRICAL_SURFACE ( 'NONE', #32557, 5.000000000000000000 ) ;
#27252 = CARTESIAN_POINT ( 'NONE',  ( -52.80376928212989185, -133.8750000013656063, -4.297418129356379346 ) ) ;
#27253 = CARTESIAN_POINT ( 'NONE',  ( 2.229367062499998831, -10.64583333196773829, -3.861377020970580887 ) ) ;
#27254 = CARTESIAN_POINT ( 'NONE',  ( 9.457646018065525792E-16, 14.68750000136559208, 5.148502694627439702 ) ) ;
#27255 = CARTESIAN_POINT ( 'NONE',  ( 2.229367062499998831, -51.89583333196773651, -3.861377020970580887 ) ) ;
#27256 =( BOUNDED_CURVE ( )  B_SPLINE_CURVE ( 2, ( #31578, #53868, #44210, #54186, #31252, #41215, #60548, #19456, #51212 ),
 .UNSPECIFIED., .F., .F. ) 
 B_SPLINE_CURVE_WITH_KNOTS ( ( 3, 2, 2, 2, 3 ),
 ( 0.1750000000000001554, 0.1791666666666668351, 0.1833333333333334869, 0.1875000000000001665, 0.1916666666666668462 ),
 .UNSPECIFIED. ) 
 CURVE ( )  GEOMETRIC_REPRESENTATION_ITEM ( )  RATIONAL_B_SPLINE_CURVE ( ( 0.9999999999999970024, 0.9238795325112897361, 1.000000000000000000, 0.9238795325112867385, 1.000000000000000000, 0.9238795325112867385, 1.000000000000000000, 0.9238795325112837409, 1.000000000000003109 ) ) 
 REPRESENTATION_ITEM ( '' )  );
#27257 = CARTESIAN_POINT ( 'NONE',  ( -4.999999999999998224, -13.79166666393548191, 2.886751345948131764 ) ) ;
#27258 = CARTESIAN_POINT ( 'NONE',  ( 2.499999999999998668, 17.66666666666666430, -4.330127018922193649 ) ) ;
#27259 = CARTESIAN_POINT ( 'NONE',  ( -4.458734124999999437, -6.395833331967741842, -2.574251347313719407 ) ) ;
#27260 = CARTESIAN_POINT ( 'NONE',  ( 1.339745962155612702, -106.1696581960073331, -5.000000000000000000 ) ) ;
#27261 = ADVANCED_FACE ( 'NONE', ( #57169 ), #36903, .T. ) ;
#27262 = ORIENTED_EDGE ( 'NONE', *, *, #46048, .F. ) ;
#27263 = CARTESIAN_POINT ( 'NONE',  ( 2.229367062500001939, -34.22916666530107221, 3.861377020970579999 ) ) ;
#27264 = CARTESIAN_POINT ( 'NONE',  ( -57.89159099828107458, -126.9375000013656063, -3.393966926194107447 ) ) ;
#27265 = EDGE_CURVE ( 'NONE', #100, #16461, #46872, .T. ) ;
#27266 = FACE_OUTER_BOUND ( 'NONE', #40866, .T. ) ;
#27267 = CARTESIAN_POINT ( 'NONE',  ( 4.458734125000001214, -78.89583333196772230, 2.574251347313718519 ) ) ;
#27268 = CARTESIAN_POINT ( 'NONE',  ( -4.458734124999998549, 22.52083333469892423, 2.574251347313722516 ) ) ;
#27269 = CARTESIAN_POINT ( 'NONE',  ( -4.458734124999999437, -151.2500000013656063, -1.846868145590735644 ) ) ;
#27270 = CARTESIAN_POINT ( 'NONE',  ( -2.229367062500000163, 14.52083333469892779, -3.861377020970580443 ) ) ;
#27271 = EDGE_CURVE ( 'NONE', #26215, #11760, #52013, .T. ) ;
#27272 = CARTESIAN_POINT ( 'NONE',  ( -1.339745962155613812, -58.08034179853029144, -5.000000000000000000 ) ) ;
#27273 = CARTESIAN_POINT ( 'NONE',  ( 5.000000000000000888, -55.58333333333332860, 2.886751345948126879 ) ) ;
#27274 = CARTESIAN_POINT ( 'NONE',  ( 4.458734124999999437, -83.06249999863440792, -5.460374474430324690E-16 ) ) ;
#27275 = CARTESIAN_POINT ( 'NONE',  ( 1.060575238724906964E-15, -63.75000000000000000, 5.773502691896257311 ) ) ;
#27276 = FACE_OUTER_BOUND ( 'NONE', #26400, .T. ) ;
#27277 = CARTESIAN_POINT ( 'NONE',  ( -5.000000000000000000, 17.12500000273118417, 0.000000000000000000 ) ) ;
#27278 = ORIENTED_EDGE ( 'NONE', *, *, #13645, .F. ) ;
#27279 = CARTESIAN_POINT ( 'NONE',  ( 5.000000000000000000, -25.41666666666666430, -2.886751345948130876 ) ) ;
#27280 = CARTESIAN_POINT ( 'NONE',  ( -9.184850993605147944E-16, -168.3750000027312126, 5.000000000000000000 ) ) ;
#27282 = CARTESIAN_POINT ( 'NONE',  ( 5.000000000000000000, -25.50000000000000355, -6.123233995736766282E-16 ) ) ;
#27281 = CARTESIAN_POINT ( 'NONE',  ( 0.000000000000000000, -120.0000000000000000, 0.000000000000000000 ) ) ;
#27283 = CARTESIAN_POINT ( 'NONE',  ( -4.458734124999999437, -25.39583333196773651, -2.574251347313719407 ) ) ;
#27284 = CARTESIAN_POINT ( 'NONE',  ( 5.000000000000000888, 18.41666666666666430, 2.886751345948126879 ) ) ;
#27285 = VECTOR ( 'NONE', #33618, 1000.000000000000000 ) ;
#27286 = CARTESIAN_POINT ( 'NONE',  ( 2.500000000000002220, -27.54166666393548013, 4.330127018922192761 ) ) ;
#27288 = VERTEX_POINT ( 'NONE', #12454 ) ;
#27287 = CARTESIAN_POINT ( 'NONE',  ( -4.458734124999999437, -58.31249999863440081, 0.000000000000000000 ) ) ;
#27289 = DIRECTION ( 'NONE',  ( -0.8660254037844387076, 0.000000000000000000, 0.4999999999999998890 ) ) ;
#27291 = ORIENTED_EDGE ( 'NONE', *, *, #16503, .T. ) ;
#27290 = CARTESIAN_POINT ( 'NONE',  ( -4.458734124999999437, -10.56249999863440792, 0.000000000000000000 ) ) ;
#27292 = CARTESIAN_POINT ( 'NONE',  ( -3.535250795749689387E-16, -74.25000000000000000, -5.773502691896257311 ) ) ;
#27293 = CARTESIAN_POINT ( 'NONE',  ( -50.70258187064364108, -139.1250000013656063, 2.196230717870141014 ) ) ;
#27294 = CARTESIAN_POINT ( 'NONE',  ( -3.152548672688508926E-16, -52.81249999863440792, -5.148502694627439702 ) ) ;
#27295 = CARTESIAN_POINT ( 'NONE',  ( 5.000000000000000000, -74.37499999726880162, -6.123233995736766282E-16 ) ) ;
#27297 = ORIENTED_EDGE ( 'NONE', *, *, #45520, .T. ) ;
#27296 = CARTESIAN_POINT ( 'NONE',  ( -5.000000000000000000, -86.08333333333332860, -2.886751345948128211 ) ) ;
#27298 = CARTESIAN_POINT ( 'NONE',  ( -54.60164318462004474, -149.3750000000000284, -4.984105922594373794 ) ) ;
#27299 = CARTESIAN_POINT ( 'NONE',  ( -2.229367062500000163, -16.72916666530107577, -3.861377020970580443 ) ) ;
#27300 = CARTESIAN_POINT ( 'NONE',  ( -2.229367062500000163, -54.72916666530107221, -3.861377020970580443 ) ) ;
#27301 =( NAMED_UNIT ( * ) PLANE_ANGLE_UNIT ( ) SI_UNIT ( $, .RADIAN. ) );
#27302 = CARTESIAN_POINT ( 'NONE',  ( -4.458734124999999437, -169.1875000013656063, -5.460374474430324690E-16 ) ) ;
#27303 = CARTESIAN_POINT ( 'NONE',  ( -2.229367062499996610, -101.3958333319677365, 3.861377020970582219 ) ) ;
#27304 = CARTESIAN_POINT ( 'NONE',  ( 1.339745962155615144, -2.705341801261480050, 4.999999999999999112 ) ) ;
#27305 = ORIENTED_EDGE ( 'NONE', *, *, #58230, .F. ) ;
#27306 = CARTESIAN_POINT ( 'NONE',  ( -50.40829686548195099, -153.2500000013656063, -1.485763867205728284 ) ) ;
#27307 = CARTESIAN_POINT ( 'NONE',  ( -58.80597590150559739, -142.1250000027312126, 3.242614290531460330 ) ) ;
#27308 =( BOUNDED_CURVE ( )  B_SPLINE_CURVE ( 2, ( #10692, #30302, #50248, #24534, #1389 ),
 .UNSPECIFIED., .F., .F. ) 
 B_SPLINE_CURVE_WITH_KNOTS ( ( 3, 2, 3 ),
 ( 0.000000000000000000, 0.004166666666666670078, 0.008333333333333340157 ),
 .UNSPECIFIED. ) 
 CURVE ( )  GEOMETRIC_REPRESENTATION_ITEM ( )  RATIONAL_B_SPLINE_CURVE ( ( 1.000000000000000000, 0.9238795325112867385, 1.000000000000000000, 0.9238795325112866275, 1.000000000000000222 ) ) 
 REPRESENTATION_ITEM ( '' )  );
#27309 = CARTESIAN_POINT ( 'NONE',  ( -5.000000000000000000, -12.95833333060214798, -2.886751345948128211 ) ) ;
#27310 = CARTESIAN_POINT ( 'NONE',  ( 4.458734125000001214, -6.895833331967734736, 2.574251347313718519 ) ) ;
#27311 = CARTESIAN_POINT ( 'NONE',  ( 2.229367062500001939, -94.22916666530106511, 3.861377020970579999 ) ) ;
#27312 = CARTESIAN_POINT ( 'NONE',  ( 4.458734124999999437, -146.6875000013656063, 0.000000000000000000 ) ) ;
#27313 = CARTESIAN_POINT ( 'NONE',  ( 4.458734124999998549, -21.97916666530107221, -2.574251347313721627 ) ) ;
#27314 = CARTESIAN_POINT ( 'NONE',  ( 0.000000000000000000, -120.0000000000000000, 0.000000000000000000 ) ) ;
#27315 = CARTESIAN_POINT ( 'NONE',  ( -52.10840900171896806, -136.1875000013656063, 3.393966926194110556 ) ) ;
#27316 = CARTESIAN_POINT ( 'NONE',  ( -4.458734124999998549, -63.47916666530106511, 2.574251347313722516 ) ) ;
#27317 = CARTESIAN_POINT ( 'NONE',  ( 7.703928834700296768, 4.447865386531931975, -7.917997657324726823 ) ) ;
#27318 = CARTESIAN_POINT ( 'NONE',  ( 0.000000000000000000, -120.0000000000000000, 5.000000000000000000 ) ) ;
#27319 = CARTESIAN_POINT ( 'NONE',  ( -4.458734125000000326, -145.8750000013656063, 1.846868145590734089 ) ) ;
#27320 = CARTESIAN_POINT ( 'NONE',  ( 9.457646018065525792E-16, 11.68750000136559564, 5.148502694627439702 ) ) ;
#27321 = ORIENTED_EDGE ( 'NONE', *, *, #5165, .T. ) ;
#27322 = DIRECTION ( 'NONE',  ( 0.000000000000000000, 0.000000000000000000, 1.000000000000000000 ) ) ;
#27324 = CARTESIAN_POINT ( 'NONE',  ( 9.457646018065525792E-16, -23.06249999863440792, 5.148502694627439702 ) ) ;
#27323 = CARTESIAN_POINT ( 'NONE',  ( -4.999999999999999112, -90.91666666666665719, 2.886751345948131764 ) ) ;
#27325 = CARTESIAN_POINT ( 'NONE',  ( 5.000000000000000000, 4.625000002731187720, -6.123233995736766282E-16 ) ) ;
#27326 = CARTESIAN_POINT ( 'NONE',  ( 4.458734125000001214, -72.14583333196773651, 2.574251347313718519 ) ) ;
#27327 = CARTESIAN_POINT ( 'NONE',  ( -3.152548672688508926E-16, 28.18750000136558853, -5.148502694627439702 ) ) ;
#27328 = CARTESIAN_POINT ( 'NONE',  ( 1.975475456537005874E-15, -38.62499999726880873, 5.000000000000000000 ) ) ;
#27329 = CARTESIAN_POINT ( 'NONE',  ( -51.60603307380591787, -145.9375000013656063, -2.891590998281053704 ) ) ;
#27330 = FACE_OUTER_BOUND ( 'NONE', #6438, .T. ) ;
#27331 = CARTESIAN_POINT ( 'NONE',  ( -4.458734124999997661, 6.770833334698928674, 2.574251347313722516 ) ) ;
#27332 = CARTESIAN_POINT ( 'NONE',  ( 0.000000000000000000, -120.0000000000000000, 0.000000000000000000 ) ) ;
#27333 = CARTESIAN_POINT ( 'NONE',  ( -56.66612745406288099, -141.4375000027311842, -5.149110718188529390 ) ) ;
#27334 = CARTESIAN_POINT ( 'NONE',  ( 2.229367062499998831, 8.354166668032261711, -3.861377020970580887 ) ) ;
#27335 = CARTESIAN_POINT ( 'NONE',  ( -4.458734124999999437, -72.39583333196775072, -2.574251347313719407 ) ) ;
#27336 = CARTESIAN_POINT ( 'NONE',  ( 2.229367062500001939, -20.22916666530107221, 3.861377020970579999 ) ) ;
#27337 = CARTESIAN_POINT ( 'NONE',  ( 2.499999999999998668, -2.333333333333333037, -4.330127018922193649 ) ) ;
#27338 = CARTESIAN_POINT ( 'NONE',  ( -4.458734125000000326, -161.0000000013656063, -1.846868145590735644 ) ) ;
#27339 = CARTESIAN_POINT ( 'NONE',  ( -3.152548672688508926E-16, -66.56249999863440792, -5.148502694627439702 ) ) ;
#27340 = CARTESIAN_POINT ( 'NONE',  ( -5.000000000000000000, -101.8749999972688158, 0.000000000000000000 ) ) ;
#27341 = CARTESIAN_POINT ( 'NONE',  ( 1.339745962155615144, 5.419658201469705894, 4.999999999999999112 ) ) ;
#27342 = CARTESIAN_POINT ( 'NONE',  ( 4.458734125000000326, -38.89583333196773651, 2.574251347313718519 ) ) ;
#27343 = CARTESIAN_POINT ( 'NONE',  ( -5.000000000000000000, -90.87499999726880162, 0.000000000000000000 ) ) ;
#27344 = CARTESIAN_POINT ( 'NONE',  ( -2.229367062500000163, -67.72916666530106511, -3.861377020970580443 ) ) ;
#27345 = CARTESIAN_POINT ( 'NONE',  ( -5.000000000000000000, -50.08333333333332149, -2.886751345948128211 ) ) ;
#27346 = CARTESIAN_POINT ( 'NONE',  ( -1.339745962155613812, -23.20534180126147916, -5.000000000000000000 ) ) ;
#27347 = ORIENTED_EDGE ( 'NONE', *, *, #3493, .T. ) ;
#27348 = CYLINDRICAL_SURFACE ( 'NONE', #7315, 5.000000000000000000 ) ;
#27349 = CARTESIAN_POINT ( 'NONE',  ( -5.000000000000000000, -7.083333333333330373, -2.886751345948128211 ) ) ;
#27350 = CARTESIAN_POINT ( 'NONE',  ( -4.458734124999997661, -71.22916666530107932, 2.574251347313722516 ) ) ;
#27351 = DIRECTION ( 'NONE',  ( -0.000000000000000000, 1.000000000000000000, -0.000000000000000000 ) ) ;
#27352 = CARTESIAN_POINT ( 'NONE',  ( 2.500000000000002220, -14.54166666393548191, 4.330127018922192761 ) ) ;
#27354 = ORIENTED_EDGE ( 'NONE', *, *, #38202, .T. ) ;
#27353 = CARTESIAN_POINT ( 'NONE',  ( -4.458734124999999437, -38.39583333196773651, -2.574251347313719407 ) ) ;
#27355 = DIRECTION ( 'NONE',  ( 0.000000000000000000, 0.000000000000000000, 1.000000000000000000 ) ) ;
#27357 = ORIENTED_EDGE ( 'NONE', *, *, #19324, .F. ) ;
#27356 = CARTESIAN_POINT ( 'NONE',  ( -4.458734124999999437, 6.437500001365593860, 0.000000000000000000 ) ) ;
#27358 = CARTESIAN_POINT ( 'NONE',  ( 5.000000000000000000, -34.37499999726881583, -6.123233995736766282E-16 ) ) ;
#27359 = CARTESIAN_POINT ( 'NONE',  ( 1.060575238724906964E-15, -56.74999999999999289, 5.773502691896257311 ) ) ;
#27360 = CARTESIAN_POINT ( 'NONE',  ( 4.458734125000000326, -159.6250000013656063, -1.846868145590734978 ) ) ;
#27361 = CARTESIAN_POINT ( 'NONE',  ( 2.229367062500001939, -35.22916666530107221, 3.861377020970579999 ) ) ;
#27362 = CARTESIAN_POINT ( 'NONE',  ( 5.000000000000000000, -145.0000000000000284, 0.000000000000000000 ) ) ;
#27363 = CARTESIAN_POINT ( 'NONE',  ( 2.229367062500001939, -78.97916666530106511, 3.861377020970579999 ) ) ;
#27364 = CARTESIAN_POINT ( 'NONE',  ( -3.535533905932737309, -167.6250000000000284, -3.535533905932738197 ) ) ;
#27365 = CARTESIAN_POINT ( 'NONE',  ( -2.229367062500000163, -89.47916666530106511, -3.861377020970580443 ) ) ;
#27366 = CARTESIAN_POINT ( 'NONE',  ( -53.51423613279429503, -129.5000000013656347, 4.591703134518082763 ) ) ;
#27367 = CARTESIAN_POINT ( 'NONE',  ( 2.229367062499998831, 2.104166668032262599, -3.861377020970580887 ) ) ;
#27368 = VECTOR ( 'NONE', #48269, 1000.000000000000000 ) ;
#27369 = CARTESIAN_POINT ( 'NONE',  ( -4.458734124999999437, -39.64583333196774362, -2.574251347313719407 ) ) ;
#27370 = CARTESIAN_POINT ( 'NONE',  ( 2.500000000000002220, -70.54166666393547303, 4.330127018922192761 ) ) ;
#27371 = CARTESIAN_POINT ( 'NONE',  ( 4.458734125000001214, -85.14583333196773651, 2.574251347313718519 ) ) ;
#27372 = CARTESIAN_POINT ( 'NONE',  ( -0.6250000000000001110, 8.299410119600874935, -7.298562697733108173 ) ) ;
#27373 = VERTEX_POINT ( 'NONE', #7642 ) ;
#27374 = CARTESIAN_POINT ( 'NONE',  ( -6.972266317189433020E-16, -64.12499999726880162, -5.000000000000000000 ) ) ;
#27375 = CARTESIAN_POINT ( 'NONE',  ( 5.000000000000000000, -152.0000000000000284, 0.000000000000000000 ) ) ;
#27376 = CARTESIAN_POINT ( 'NONE',  ( -3.152548672688508926E-16, -71.81249999863439371, -5.148502694627439702 ) ) ;
#27377 = CARTESIAN_POINT ( 'NONE',  ( -4.458734124999999437, -37.31249999863440792, 0.000000000000000000 ) ) ;
#27378 = CARTESIAN_POINT ( 'NONE',  ( 4.458734124999999437, -9.062499998634406140, -5.460374474430324690E-16 ) ) ;
#27379 = VERTEX_POINT ( 'NONE', #22751 ) ;
#27380 =( BOUNDED_CURVE ( )  B_SPLINE_CURVE ( 2, ( #17785, #55450, #26807, #46739, #2684, #38001, #17444, #22592, #42189 ),
 .UNSPECIFIED., .F., .F. ) 
 B_SPLINE_CURVE_WITH_KNOTS ( ( 3, 2, 2, 2, 3 ),
 ( 0.06964285714285714524, 0.07023809523809523836, 0.07142857142857142461, 0.07261904761904762473, 0.07321428571428571785 ),
 .UNSPECIFIED. ) 
 CURVE ( )  GEOMETRIC_REPRESENTATION_ITEM ( )  RATIONAL_B_SPLINE_CURVE ( ( 0.9330127018922194093, 0.9330127018922194093, 1.000000000000000000, 0.8660254037844387076, 1.000000000000000000, 0.8660254037844387076, 1.000000000000000000, 0.9330127018922194093, 0.9330127018922194093 ) ) 
 REPRESENTATION_ITEM ( '' )  );
#27381 = CARTESIAN_POINT ( 'NONE',  ( 5.000000000000000888, -163.9375000000000000, -2.071067811865475505 ) ) ;
#27382 = CARTESIAN_POINT ( 'NONE',  ( 5.000000000000000888, 17.41666666666666430, 2.886751345948126879 ) ) ;
#27383 = CARTESIAN_POINT ( 'NONE',  ( -4.458734124999999437, -8.645833331967736513, -2.574251347313719407 ) ) ;
#27384 = CARTESIAN_POINT ( 'NONE',  ( -5.000000000000000000, 2.916666666666668739, -2.886751345948128211 ) ) ;
#27385 = CARTESIAN_POINT ( 'NONE',  ( 4.458734124999998549, 1.270833334698927342, -2.574251347313721627 ) ) ;
#27386 = CARTESIAN_POINT ( 'NONE',  ( 5.000000000000000000, -154.0625000000000284, 2.071067811865478614 ) ) ;
#27387 = CARTESIAN_POINT ( 'NONE',  ( -3.152801135295367985, -157.8125000013656063, 3.152801135295367096 ) ) ;
#27388 = CARTESIAN_POINT ( 'NONE',  ( 2.229367062499998831, 28.10416666803225993, -3.861377020970580887 ) ) ;
#27389 = VERTEX_POINT ( 'NONE', #22436 ) ;
#27390 = CARTESIAN_POINT ( 'NONE',  ( -2.229367062499996610, -88.14583333196773651, 3.861377020970582219 ) ) ;
#27391 = CARTESIAN_POINT ( 'NONE',  ( 1.975475456537005874E-15, -46.74999999999999289, 5.000000000000000000 ) ) ;
#27392 = CARTESIAN_POINT ( 'NONE',  ( 4.458734125000001214, -7.895833331967735624, 2.574251347313718519 ) ) ;
#27393 = CARTESIAN_POINT ( 'NONE',  ( -6.972266317189433020E-16, -51.25000000000000000, -5.000000000000000000 ) ) ;
#27394 = CYLINDRICAL_SURFACE ( 'NONE', #9852, 5.000000000000000000 ) ;
#27395 =( BOUNDED_CURVE ( )  B_SPLINE_CURVE ( 2, ( #39401, #15617, #49056, #44552, #45195, #10457, #35234, #5329, #1162 ),
 .UNSPECIFIED., .F., .F. ) 
 B_SPLINE_CURVE_WITH_KNOTS ( ( 3, 2, 2, 2, 3 ),
 ( 0.5410714285714285365, 0.5416666666666666297, 0.5428571428571428159, 0.5440476190476190022, 0.5446428571428570953 ),
 .UNSPECIFIED. ) 
 CURVE ( )  GEOMETRIC_REPRESENTATION_ITEM ( )  RATIONAL_B_SPLINE_CURVE ( ( 0.9330127018922194093, 0.9330127018922194093, 1.000000000000000000, 0.8660254037844387076, 1.000000000000000000, 0.8660254037844387076, 1.000000000000000000, 0.9330127018922194093, 0.9330127018922194093 ) ) 
 REPRESENTATION_ITEM ( '' )  );
#27396 = CARTESIAN_POINT ( 'NONE',  ( -54.60164318462004474, -138.3750000000000284, -4.984105922594373794 ) ) ;
#27397 = CARTESIAN_POINT ( 'NONE',  ( 5.000000000000000000, -38.29166666393548013, -2.886751345948129988 ) ) ;
#27398 = DIRECTION ( 'NONE',  ( 0.000000000000000000, 0.000000000000000000, 1.000000000000000000 ) ) ;
#27399 = CARTESIAN_POINT ( 'NONE',  ( -2.229367062499996610, 26.85416666803225993, 3.861377020970582219 ) ) ;
#27400 = CARTESIAN_POINT ( 'NONE',  ( -2.500000000000000444, -98.04166666393545881, -4.330127018922193649 ) ) ;
#27401 = CARTESIAN_POINT ( 'NONE',  ( -4.458734124999999437, 23.68750000136559564, 0.000000000000000000 ) ) ;
#27402 = CARTESIAN_POINT ( 'NONE',  ( 4.458734125000001214, -54.89583333196773651, 2.574251347313718519 ) ) ;
#27403 = CARTESIAN_POINT ( 'NONE',  ( 4.458734124999998549, -3.979166665301070438, -2.574251347313721627 ) ) ;
#27404 = CARTESIAN_POINT ( 'NONE',  ( 2.071067811865370256, -159.9375000027312410, -5.000000000000105693 ) ) ;
#27405 = CARTESIAN_POINT ( 'NONE',  ( 5.000000000000000000, 13.49999999999999822, -6.123233995736766282E-16 ) ) ;
#27406 = CARTESIAN_POINT ( 'NONE',  ( -9.184850993605147944E-16, -140.3750000027312126, 5.000000000000000000 ) ) ;
#27407 = LINE ( 'NONE', #52503, #5877 ) ;
#27408 = CARTESIAN_POINT ( 'NONE',  ( 9.457646018065525792E-16, -48.06249999863440081, 5.148502694627439702 ) ) ;
#27409 = CARTESIAN_POINT ( 'NONE',  ( -3.535250795749689387E-16, -84.12499999726880162, -5.773502691896257311 ) ) ;
#27410 = VECTOR ( 'NONE', #40770, 1000.000000000000000 ) ;
#27411 = CARTESIAN_POINT ( 'NONE',  ( -58.39396692619412477, -137.6875000013656063, 2.891590998281057701 ) ) ;
#27412 = CARTESIAN_POINT ( 'NONE',  ( 2.499999999999998668, -37.20833333060213732, -4.330127018922193649 ) ) ;
#27413 = CARTESIAN_POINT ( 'NONE',  ( -6.972266317189433020E-16, -22.24999999999999645, -5.000000000000000000 ) ) ;
#27414 = CARTESIAN_POINT ( 'NONE',  ( -4.458734124999997661, -85.47916666530107932, 2.574251347313722516 ) ) ;
#27415 = CARTESIAN_POINT ( 'NONE',  ( -3.152801135295367096, -158.3125000013656063, -3.152801135295367541 ) ) ;
#27416 = CARTESIAN_POINT ( 'NONE',  ( -3.535250795749689387E-16, -34.25000000000000711, -5.773502691896257311 ) ) ;
#27417 = CARTESIAN_POINT ( 'NONE',  ( 2.499999999999998668, 8.791666669397853795, -4.330127018922193649 ) ) ;
#27418 = EDGE_LOOP ( 'NONE', ( #16663, #60086, #15392, #3731 ) ) ;
#27419 = CARTESIAN_POINT ( 'NONE',  ( -4.458734124999999437, 19.43750000136559208, 0.000000000000000000 ) ) ;
#27420 = EDGE_LOOP ( 'NONE', ( #17099, #4121, #48566, #21082 ) ) ;
#27421 = CARTESIAN_POINT ( 'NONE',  ( -4.458734124999998549, -94.22916666530106511, 2.574251347313722516 ) ) ;
#27422 = CARTESIAN_POINT ( 'NONE',  ( 9.457646018065525792E-16, 13.68750000136559208, 5.148502694627439702 ) ) ;
#27423 = CARTESIAN_POINT ( 'NONE',  ( -2.499999999999996447, 18.29166666939785202, 4.330127018922195425 ) ) ;
#27424 = CARTESIAN_POINT ( 'NONE',  ( -5.000000000000000000, -34.95833333060213732, -2.886751345948128211 ) ) ;
#27425 = CARTESIAN_POINT ( 'NONE',  ( -4.999999999999999112, 9.083333333333333925, 2.886751345948131764 ) ) ;
#27426 = CARTESIAN_POINT ( 'NONE',  ( 2.229367062500001939, -53.97916666530107221, 3.861377020970579999 ) ) ;
#27427 = CARTESIAN_POINT ( 'NONE',  ( -4.999999999999998224, -52.79166666393548013, 2.886751345948131764 ) ) ;
#27428 = CARTESIAN_POINT ( 'NONE',  ( 5.000000000000000000, -81.50000000000000000, -6.123233995736766282E-16 ) ) ;
#27429 = CARTESIAN_POINT ( 'NONE',  ( -55.52884467124510337, -135.0324864422690894, -4.515220955086300059 ) ) ;
#27430 = CARTESIAN_POINT ( 'NONE',  ( 1.975475456537005874E-15, -12.62499999726881050, 5.000000000000000000 ) ) ;
#27431 = CARTESIAN_POINT ( 'NONE',  ( 1.975475456537005874E-15, -109.7499999999999858, 5.000000000000000000 ) ) ;
#27432 = CARTESIAN_POINT ( 'NONE',  ( 5.000000000000000888, -38.58333333333332860, 2.886751345948126879 ) ) ;
#27433 = CARTESIAN_POINT ( 'NONE',  ( 2.071067811865349828, -149.1875000000000284, 5.000000000000126121 ) ) ;
#27435 = CARTESIAN_POINT ( 'NONE',  ( 4.458734124999999437, -20.06249999863440081, -5.460374474430324690E-16 ) ) ;
#27434 = CARTESIAN_POINT ( 'NONE',  ( -1.339745962155613812, 13.79465819873852084, -5.000000000000000000 ) ) ;
#27436 = CARTESIAN_POINT ( 'NONE',  ( 2.499999999999998668, -107.2083333306021444, -4.330127018922193649 ) ) ;
#27437 = CARTESIAN_POINT ( 'NONE',  ( -3.152548672688508926E-16, -66.56249999863440792, -5.148502694627439702 ) ) ;
#27438 = CARTESIAN_POINT ( 'NONE',  ( 1.846868145590735200, -147.5000000013656063, -4.458734125000000326 ) ) ;
#27440 = EDGE_CURVE ( 'NONE', #52254, #44414, #31912, .T. ) ;
#27439 = CARTESIAN_POINT ( 'NONE',  ( 9.457646018065525792E-16, -69.06249999863439371, 5.148502694627439702 ) ) ;
#27441 = CARTESIAN_POINT ( 'NONE',  ( -53.51423613279429503, -142.5000000013656347, 4.591703134518082763 ) ) ;
#27442 = CARTESIAN_POINT ( 'NONE',  ( -4.458734124999999437, -18.56249999863440792, 0.000000000000000000 ) ) ;
#27443 = CARTESIAN_POINT ( 'NONE',  ( 2.499999999999998668, -61.20833333060214443, -4.330127018922193649 ) ) ;
#27444 = VERTEX_POINT ( 'NONE', #61987 ) ;
#27445 = CARTESIAN_POINT ( 'NONE',  ( -3.535533905932737309, -150.6250000000000000, -3.535533905932738197 ) ) ;
#27446 = EDGE_LOOP ( 'NONE', ( #20504, #34162, #45393, #4212 ) ) ;
#27447 = CARTESIAN_POINT ( 'NONE',  ( -2.229367062499996610, -66.39583333196773651, 3.861377020970582219 ) ) ;
#27448 = FACE_OUTER_BOUND ( 'NONE', #15333, .T. ) ;
#27449 = CARTESIAN_POINT ( 'NONE',  ( -5.000000000000000000, -5.958333330602149758, -2.886751345948128211 ) ) ;
#27450 = VERTEX_POINT ( 'NONE', #42349 ) ;
#27451 =( BOUNDED_CURVE ( )  B_SPLINE_CURVE ( 2, ( #55292, #11530, #16679, #45630, #60117, #36300, #15723, #11838, #26013 ),
 .UNSPECIFIED., .F., .F. ) 
 B_SPLINE_CURVE_WITH_KNOTS ( ( 3, 2, 2, 2, 3 ),
 ( 0.6196428571428571619, 0.6202380952380952550, 0.6214285714285714413, 0.6226190476190476275, 0.6232142857142857206 ),
 .UNSPECIFIED. ) 
 CURVE ( )  GEOMETRIC_REPRESENTATION_ITEM ( )  RATIONAL_B_SPLINE_CURVE ( ( 0.9330127018922194093, 0.9330127018922194093, 1.000000000000000000, 0.8660254037844387076, 1.000000000000000000, 0.8660254037844387076, 1.000000000000000000, 0.9330127018922194093, 0.9330127018922194093 ) ) 
 REPRESENTATION_ITEM ( '' )  );
#27452 = CARTESIAN_POINT ( 'NONE',  ( -5.000000000000000000, 3.125000002731185944, 0.000000000000000000 ) ) ;
#27453 = CARTESIAN_POINT ( 'NONE',  ( -56.66612745406270335, -126.3125000000000284, -5.149110718188516067 ) ) ;
#27454 = CARTESIAN_POINT ( 'NONE',  ( -4.999999999999998224, -55.79166666393548013, 2.886751345948131764 ) ) ;
#27455 = CARTESIAN_POINT ( 'NONE',  ( -2.229367062499996610, -56.39583333196773651, 3.861377020970582219 ) ) ;
#27456 = AXIS2_PLACEMENT_3D ( 'NONE', #43061, #33725, #9277 ) ;
#27457 = ORIENTED_EDGE ( 'NONE', *, *, #28268, .F. ) ;
#27458 = VECTOR ( 'NONE', #44385, 1000.000000000000000 ) ;
#27459 = ADVANCED_FACE ( 'NONE', ( #17907 ), #21801, .T. ) ;
#27460 = CARTESIAN_POINT ( 'NONE',  ( 4.336808689942017736E-16, 8.660254037844390851, -1.000000000000000888 ) ) ;
#27461 = EDGE_CURVE ( 'NONE', #31328, #30756, #38468, .T. ) ;
#27462 = CARTESIAN_POINT ( 'NONE',  ( -3.152548672688508926E-16, 9.437500001365593860, -5.148502694627439702 ) ) ;
#27463 = CARTESIAN_POINT ( 'NONE',  ( 2.229367062500001939, 20.02083333469892779, 3.861377020970579999 ) ) ;
#27464 = CARTESIAN_POINT ( 'NONE',  ( -50.55543936806279248, -147.0625000013656063, 0.3552334253322060320 ) ) ;
#27465 = CARTESIAN_POINT ( 'NONE',  ( -58.24261429053147765, -150.3750000027312126, -3.805975901505573855 ) ) ;
#27466 = FACE_OUTER_BOUND ( 'NONE', #16127, .T. ) ;
#27467 = ORIENTED_EDGE ( 'NONE', *, *, #53033, .F. ) ;
#27468 = CARTESIAN_POINT ( 'NONE',  ( -4.458734124999999437, -69.31249999863439371, 0.000000000000000000 ) ) ;
#27469 = DIRECTION ( 'NONE',  ( -0.000000000000000000, 1.000000000000000000, -0.000000000000000000 ) ) ;
#27470 = CARTESIAN_POINT ( 'NONE',  ( 2.229367062500001939, 6.020833334698927786, 3.861377020970579999 ) ) ;
#27471 = EDGE_CURVE ( 'NONE', #53941, #27799, #1125, .T. ) ;
#27472 = DIRECTION ( 'NONE',  ( 0.000000000000000000, 0.000000000000000000, 1.000000000000000000 ) ) ;
#27473 = CARTESIAN_POINT ( 'NONE',  ( -4.458734124999999437, -61.56249999863440081, 0.000000000000000000 ) ) ;
#27474 = CARTESIAN_POINT ( 'NONE',  ( 5.000000000000000000, -21.37499999726881228, -6.123233995736766282E-16 ) ) ;
#27475 = CARTESIAN_POINT ( 'NONE',  ( -2.500000000000000444, -33.04166666393547303, -4.330127018922193649 ) ) ;
#27476 = CARTESIAN_POINT ( 'NONE',  ( -58.24261429053147765, -140.3750000027312126, -3.805975901505573855 ) ) ;
#27477 = CARTESIAN_POINT ( 'NONE',  ( 1.975475456537005874E-15, 19.25000000000000000, 5.000000000000000000 ) ) ;
#27478 = CARTESIAN_POINT ( 'NONE',  ( -4.458734124999998549, -42.22916666530107932, 2.574251347313722516 ) ) ;
#27479 = CARTESIAN_POINT ( 'NONE',  ( 4.458734125000000326, -22.14583333196773296, 2.574251347313718519 ) ) ;
#27480 = ORIENTED_EDGE ( 'NONE', *, *, #31853, .T. ) ;
#27481 = CARTESIAN_POINT ( 'NONE',  ( 1.975475456537005874E-15, -101.7499999999999858, 5.000000000000000000 ) ) ;
#27482 = CARTESIAN_POINT ( 'NONE',  ( 2.499999999999998668, 28.66666666666666785, -4.330127018922193649 ) ) ;
#27483 = CARTESIAN_POINT ( 'NONE',  ( -3.535533905932738641, -153.5000000027312126, 3.535533905932737309 ) ) ;
#27484 = EDGE_LOOP ( 'NONE', ( #16903, #59683, #27673, #21371 ) ) ;
#27485 = CARTESIAN_POINT ( 'NONE',  ( 4.458734124999999437, -108.0624999986343937, -5.460374474430324690E-16 ) ) ;
#27486 = CARTESIAN_POINT ( 'NONE',  ( 9.457646018065525792E-16, -34.06249999863440792, 5.148502694627439702 ) ) ;
#27487 = CARTESIAN_POINT ( 'NONE',  ( 1.060575238724906964E-15, -61.62499999726880873, 5.773502691896257311 ) ) ;
#27488 = CARTESIAN_POINT ( 'NONE',  ( -50.70258187064364108, -150.3750000013656063, 2.196230717870141014 ) ) ;
#27489 = CARTESIAN_POINT ( 'NONE',  ( -5.000000000000000000, -145.5000000000000284, -6.123233995736766282E-16 ) ) ;
#27490 = EDGE_CURVE ( 'NONE', #8617, #4579, #4845, .T. ) ;
#27491 = CARTESIAN_POINT ( 'NONE',  ( -2.229367062500000163, -26.47916666530106866, -3.861377020970580443 ) ) ;
#27492 = CARTESIAN_POINT ( 'NONE',  ( -2.229367062500000163, -69.72916666530107932, -3.861377020970580443 ) ) ;
#27493 = CARTESIAN_POINT ( 'NONE',  ( 5.000000000000000000, 22.62500000273118772, -6.123233995736766282E-16 ) ) ;
#27494 = CARTESIAN_POINT ( 'NONE',  ( 2.229367062500001939, -24.97916666530106866, 3.861377020970579999 ) ) ;
#27495 = CARTESIAN_POINT ( 'NONE',  ( 5.000000000000000000, 14.49999999999999822, -6.123233995736766282E-16 ) ) ;
#27496 = DIRECTION ( 'NONE',  ( 0.000000000000000000, 0.000000000000000000, 1.000000000000000000 ) ) ;
#27497 = CARTESIAN_POINT ( 'NONE',  ( -2.499999999999996447, -14.83333333333333037, 4.330127018922195425 ) ) ;
#27498 = CARTESIAN_POINT ( 'NONE',  ( -1.846868145590737420, -147.7500000013655779, 4.458734124999999437 ) ) ;
#27499 = EDGE_LOOP ( 'NONE', ( #36961, #58750, #60695, #19927 ) ) ;
#27500 = CARTESIAN_POINT ( 'NONE',  ( -60.14911071818854538, -153.0625000000000284, 1.666127454062681146 ) ) ;
#27501 = CARTESIAN_POINT ( 'NONE',  ( 4.458734124999999437, -50.06249999863440792, -5.460374474430324690E-16 ) ) ;
#27502 = VECTOR ( 'NONE', #5231, 1000.000000000000000 ) ;
#27503 = CARTESIAN_POINT ( 'NONE',  ( 0.000000000000000000, -120.0000000000000000, 5.000000000000000000 ) ) ;
#27504 = CARTESIAN_POINT ( 'NONE',  ( 2.499999999999998668, 24.66666666666666785, -4.330127018922193649 ) ) ;
#27505 = VECTOR ( 'NONE', #62939, 1000.000000000000000 ) ;
#27506 = CARTESIAN_POINT ( 'NONE',  ( 5.000000000000000888, 25.41666666666666430, 2.886751345948126879 ) ) ;
#27507 = CARTESIAN_POINT ( 'NONE',  ( -2.229367062499996610, -3.145833331967738733, 3.861377020970582219 ) ) ;
#27508 = CARTESIAN_POINT ( 'NONE',  ( -5.000000000000000888, -154.5625000000000000, -2.071067811865475949 ) ) ;
#27509 = CARTESIAN_POINT ( 'NONE',  ( 0.000000000000000000, -120.0000000000000000, 0.000000000000000000 ) ) ;
#27510 = FACE_OUTER_BOUND ( 'NONE', #47699, .T. ) ;
#27511 = CARTESIAN_POINT ( 'NONE',  ( -4.458734124999999437, 10.43750000136559386, 0.000000000000000000 ) ) ;
#27512 = VERTEX_POINT ( 'NONE', #4071 ) ;
#27513 = CARTESIAN_POINT ( 'NONE',  ( 1.975475456537005874E-15, -29.62499999726881228, 5.000000000000000000 ) ) ;
#27514 = ORIENTED_EDGE ( 'NONE', *, *, #61394, .F. ) ;
#27515 = DIRECTION ( 'NONE',  ( -0.000000000000000000, 1.000000000000000000, -0.000000000000000000 ) ) ;
#27516 = CARTESIAN_POINT ( 'NONE',  ( -4.458734124999999437, -46.39583333196774362, -2.574251347313719407 ) ) ;
#27517 = CARTESIAN_POINT ( 'NONE',  ( 4.458734125000000326, -161.6250000013656063, -1.846868145590734978 ) ) ;
#27518 = EDGE_CURVE ( 'NONE', #33686, #49037, #7318, .T. ) ;
#27519 = EDGE_CURVE ( 'NONE', #21524, #53932, #29432, .T. ) ;
#27520 = CARTESIAN_POINT ( 'NONE',  ( -2.500000000000000444, -43.04166666393548013, -4.330127018922193649 ) ) ;
#27521 = EDGE_CURVE ( 'NONE', #39916, #62968, #3757, .T. ) ;
#27522 = ORIENTED_EDGE ( 'NONE', *, *, #33933, .T. ) ;
#27523 = CARTESIAN_POINT ( 'NONE',  ( 4.458734124999999437, -22.81249999863440436, -5.460374474430324690E-16 ) ) ;
#27524 = EDGE_LOOP ( 'NONE', ( #54177, #17852, #34100, #4130 ) ) ;
#27525 = DIRECTION ( 'NONE',  ( 0.000000000000000000, 1.000000000000000000, 0.000000000000000000 ) ) ;
#27526 = CARTESIAN_POINT ( 'NONE',  ( -4.458734125000001214, -164.8750000013655779, 1.846868145590734089 ) ) ;
#27527 = CYLINDRICAL_SURFACE ( 'NONE', #44708, 5.000000000000000000 ) ;
#27528 = CARTESIAN_POINT ( 'NONE',  ( -51.19402409849444524, -137.5000000000000284, -3.242614290531456334 ) ) ;
#27529 = CARTESIAN_POINT ( 'NONE',  ( 4.458734124999998549, -37.97916666530107932, -2.574251347313721627 ) ) ;
#27530 = ORIENTED_EDGE ( 'NONE', *, *, #62972, .F. ) ;
#27531 = CARTESIAN_POINT ( 'NONE',  ( 4.458734124999999437, -84.81249999863439371, -5.460374474430324690E-16 ) ) ;
#27532 = EDGE_CURVE ( 'NONE', #942, #11069, #11427, .T. ) ;
#27533 = CARTESIAN_POINT ( 'NONE',  ( 2.229367062500001939, 25.02083333469892779, 3.861377020970579999 ) ) ;
#27534 = CARTESIAN_POINT ( 'NONE',  ( -5.000000000000000000, -54.08333333333332860, -2.886751345948128211 ) ) ;
#27535 = ORIENTED_EDGE ( 'NONE', *, *, #18493, .F. ) ;
#27536 = CARTESIAN_POINT ( 'NONE',  ( 0.000000000000000000, -170.0000000000000000, 0.000000000000000000 ) ) ;
#27537 = CARTESIAN_POINT ( 'NONE',  ( -55.35523342533222291, -137.5625000013656063, 4.444560631937231499 ) ) ;
#27538 = CARTESIAN_POINT ( 'NONE',  ( 2.229367062500001939, -86.22916666530107932, 3.861377020970579999 ) ) ;
#27539 = CARTESIAN_POINT ( 'NONE',  ( -55.39835681537999790, -131.0000000027312126, 4.984105922594378235 ) ) ;
#27540 = CARTESIAN_POINT ( 'NONE',  ( 1.975475456537005874E-15, 0.3750000027311862216, 5.000000000000000000 ) ) ;
#27541 = VECTOR ( 'NONE', #2419, 1000.000000000000000 ) ;
#27542 = CARTESIAN_POINT ( 'NONE',  ( 2.499999999999998668, -57.33333333333333570, -4.330127018922193649 ) ) ;
#27543 = CARTESIAN_POINT ( 'NONE',  ( 4.458734125000000326, -55.89583333196773651, 2.574251347313718519 ) ) ;
#27544 = CARTESIAN_POINT ( 'NONE',  ( 1.975475456537005874E-15, 10.24999999999999822, 5.000000000000000000 ) ) ;
#27545 = CARTESIAN_POINT ( 'NONE',  ( 2.229367062499998831, 25.35416666803225993, -3.861377020970580887 ) ) ;
#27546 = CARTESIAN_POINT ( 'NONE',  ( 5.000000000000000000, -104.5000000000000142, -6.123233995736766282E-16 ) ) ;
#27547 = CARTESIAN_POINT ( 'NONE',  ( -4.999999999999998224, 4.083333333333334814, 2.886751345948131764 ) ) ;
#27548 = CARTESIAN_POINT ( 'NONE',  ( 2.229367062500001939, -46.22916666530106511, 3.861377020970579999 ) ) ;
#27549 = CARTESIAN_POINT ( 'NONE',  ( -5.000000000000000000, 0.04166666939785235169, -2.886751345948128211 ) ) ;
#27550 = CARTESIAN_POINT ( 'NONE',  ( 6.123233995736766282E-16, -120.0000000000000000, -5.000000000000000000 ) ) ;
#27551 = CARTESIAN_POINT ( 'NONE',  ( 1.975475456537005874E-15, -82.62499999726878741, 5.000000000000000000 ) ) ;
#27552 = CARTESIAN_POINT ( 'NONE',  ( -2.229367062499996610, -81.39583333196773651, 3.861377020970582219 ) ) ;
#27553 = CARTESIAN_POINT ( 'NONE',  ( -2.229367062500000163, -100.4791666653010651, -3.861377020970580443 ) ) ;
#27554 = CARTESIAN_POINT ( 'NONE',  ( -4.458734124999999437, -4.562499998634401699, 0.000000000000000000 ) ) ;
#27555 = ORIENTED_EDGE ( 'NONE', *, *, #26805, .F. ) ;
#27556 = DIRECTION ( 'NONE',  ( 0.000000000000000000, 0.000000000000000000, 1.000000000000000000 ) ) ;
#27557 = CARTESIAN_POINT ( 'NONE',  ( -4.458734124999999437, -92.39583333196773651, -2.574251347313719407 ) ) ;
#27558 = CARTESIAN_POINT ( 'NONE',  ( -3.535533905932738641, -165.5000000027312126, 3.535533905932737309 ) ) ;
#27559 = CARTESIAN_POINT ( 'NONE',  ( 4.458734125000001214, -86.14583333196775072, 2.574251347313718519 ) ) ;
#27560 = CARTESIAN_POINT ( 'NONE',  ( 4.458734124999999437, 10.93750000136559386, -5.460374474430324690E-16 ) ) ;
#27561 = CYLINDRICAL_SURFACE ( 'NONE', #58218, 5.000000000000000000 ) ;
#27562 = CARTESIAN_POINT ( 'NONE',  ( -59.29741812935640155, -134.6250000013656347, -2.196230717870135685 ) ) ;
#27563 = CARTESIAN_POINT ( 'NONE',  ( 4.458734125000000326, -11.89583333196774184, 2.574251347313718519 ) ) ;
#27564 = CARTESIAN_POINT ( 'NONE',  ( 4.458734125000001214, 16.85416666803225638, 2.574251347313718519 ) ) ;
#27565 = CARTESIAN_POINT ( 'NONE',  ( -2.229367062499996610, -55.39583333196773651, 3.861377020970582219 ) ) ;
#27566 = CARTESIAN_POINT ( 'NONE',  ( -6.972266317189433020E-16, -16.12499999726881228, -5.000000000000000000 ) ) ;
#27567 = CYLINDRICAL_SURFACE ( 'NONE', #33650, 5.000000000000000000 ) ;
#27568 = CARTESIAN_POINT ( 'NONE',  ( 4.458734124999998549, -6.729166665301073103, -2.574251347313721627 ) ) ;
#27569 = CARTESIAN_POINT ( 'NONE',  ( 5.000000000000000888, -84.58333333333332860, 2.886751345948126879 ) ) ;
#27570 = EDGE_LOOP ( 'NONE', ( #5444, #34344, #13380, #28097 ) ) ;
#27571 = CARTESIAN_POINT ( 'NONE',  ( 2.229367062500001939, -37.22916666530107221, 3.861377020970579999 ) ) ;
#27572 = CARTESIAN_POINT ( 'NONE',  ( -50.40829686548195099, -128.2500000013656063, -1.485763867205728284 ) ) ;
#27573 = CARTESIAN_POINT ( 'NONE',  ( 1.975475456537005874E-15, -11.74999999999999645, 5.000000000000000000 ) ) ;
#27574 = CARTESIAN_POINT ( 'NONE',  ( -3.152548672688508926E-16, -79.56249999863440792, -5.148502694627439702 ) ) ;
#27575 = CARTESIAN_POINT ( 'NONE',  ( 4.458734125000001214, 23.85416666803225993, 2.574251347313718519 ) ) ;
#27576 =( BOUNDED_CURVE ( )  B_SPLINE_CURVE ( 2, ( #29649, #10989, #40577, #25797, #403, #19687, #20976, #29317, #39934 ),
 .UNSPECIFIED., .F., .F. ) 
 B_SPLINE_CURVE_WITH_KNOTS ( ( 3, 2, 2, 2, 3 ),
 ( 0.7982142857142857650, 0.7988095238095238582, 0.8000000000000000444, 0.8011904761904762307, 0.8017857142857143238 ),
 .UNSPECIFIED. ) 
 CURVE ( )  GEOMETRIC_REPRESENTATION_ITEM ( )  RATIONAL_B_SPLINE_CURVE ( ( 0.9330127018922194093, 0.9330127018922194093, 1.000000000000000000, 0.8660254037844387076, 1.000000000000000000, 0.8660254037844387076, 1.000000000000000000, 0.9330127018922194093, 0.9330127018922194093 ) ) 
 REPRESENTATION_ITEM ( '' )  );
#27577 = CARTESIAN_POINT ( 'NONE',  ( 4.458734124999998549, 14.27083333469892779, -2.574251347313721627 ) ) ;
#27578 = CARTESIAN_POINT ( 'NONE',  ( 0.000000000000000000, -120.0000000000000000, 0.000000000000000000 ) ) ;
#27579 = CARTESIAN_POINT ( 'NONE',  ( 1.975475456537005874E-15, -6.749999999999999112, 5.000000000000000000 ) ) ;
#27580 = CARTESIAN_POINT ( 'NONE',  ( 4.458734125000000326, -86.14583333196775072, 2.574251347313718519 ) ) ;
#27581 = CARTESIAN_POINT ( 'NONE',  ( -4.999999999999999112, -65.91666666666665719, 2.886751345948131764 ) ) ;
#27582 = CARTESIAN_POINT ( 'NONE',  ( 1.339745962155612702, -63.16965819600734022, -5.000000000000000000 ) ) ;
#27583 = CARTESIAN_POINT ( 'NONE',  ( -3.535250795749689387E-16, 20.87500000273118417, -5.773502691896257311 ) ) ;
#27584 = ORIENTED_EDGE ( 'NONE', *, *, #43803, .T. ) ;
#27585 = CARTESIAN_POINT ( 'NONE',  ( 5.000000000000000888, -35.58333333333332860, 2.886751345948126879 ) ) ;
#27586 = VECTOR ( 'NONE', #8412, 1000.000000000000000 ) ;
#27587 = CARTESIAN_POINT ( 'NONE',  ( 1.339745962155612702, 7.705341801261479162, -5.000000000000000000 ) ) ;
#27588 = CARTESIAN_POINT ( 'NONE',  ( -5.000000000000000000, -31.08333333333332860, -2.886751345948128211 ) ) ;
#27589 = CARTESIAN_POINT ( 'NONE',  ( 2.229367062499998831, -31.64583333196773651, -3.861377020970580887 ) ) ;
#27590 = VECTOR ( 'NONE', #60772, 1000.000000000000000 ) ;
#27591 = CARTESIAN_POINT ( 'NONE',  ( 1.975475456537005874E-15, 0.2500000000000001665, 5.000000000000000000 ) ) ;
#27592 = EDGE_CURVE ( 'NONE', #35368, #45099, #44665, .T. ) ;
#27593 = CARTESIAN_POINT ( 'NONE',  ( 5.000000000000000000, -28.37499999726881228, -6.123233995736766282E-16 ) ) ;
#27594 = EDGE_CURVE ( 'NONE', #48474, #42868, #14238, .T. ) ;
#27596 = ORIENTED_EDGE ( 'NONE', *, *, #57044, .F. ) ;
#27595 = CARTESIAN_POINT ( 'NONE',  ( -4.458734124999998549, -61.22916666530106511, 2.574251347313722516 ) ) ;
#27597 = DIRECTION ( 'NONE',  ( 0.000000000000000000, 0.000000000000000000, 1.000000000000000000 ) ) ;
#27599 = ORIENTED_EDGE ( 'NONE', *, *, #18015, .T. ) ;
#27598 = CARTESIAN_POINT ( 'NONE',  ( -4.458734124999998549, -6.479166665301073103, 2.574251347313722516 ) ) ;
#27600 = EDGE_CURVE ( 'NONE', #25203, #7464, #51279, .T. ) ;
#27601 = CARTESIAN_POINT ( 'NONE',  ( 1.060575238724906964E-15, -77.75000000000000000, 5.773502691896257311 ) ) ;
#27602 = CARTESIAN_POINT ( 'NONE',  ( -55.35523342533222291, -138.3125000013656063, 4.444560631937231499 ) ) ;
#27603 = CARTESIAN_POINT ( 'NONE',  ( -4.458734124999999437, -53.64583333196772941, -2.574251347313719407 ) ) ;
#27604 = ADVANCED_FACE ( 'NONE', ( #34914 ), #25258, .T. ) ;
#27605 = CARTESIAN_POINT ( 'NONE',  ( -2.500000000000000444, -78.04166666393547303, -4.330127018922193649 ) ) ;
#27607 = ORIENTED_EDGE ( 'NONE', *, *, #29741, .T. ) ;
#27606 = FACE_OUTER_BOUND ( 'NONE', #40683, .T. ) ;
#27608 = CARTESIAN_POINT ( 'NONE',  ( -59.98410592259440222, -148.1250000000000284, -0.3983568153799752487 ) ) ;
#27609 = EDGE_CURVE ( 'NONE', #48046, #14245, #20833, .T. ) ;
#27610 = CARTESIAN_POINT ( 'NONE',  ( -2.229367062499996610, -20.39583333196774007, 3.861377020970582219 ) ) ;
#27611 = EDGE_CURVE ( 'NONE', #58224, #38122, #27395, .T. ) ;
#27612 = CARTESIAN_POINT ( 'NONE',  ( 4.458734124999999437, -59.06249999863440081, -5.460374474430324690E-16 ) ) ;
#27613 = FILL_AREA_STYLE_COLOUR ( '', #11242 ) ;
#27614 = CARTESIAN_POINT ( 'NONE',  ( 4.458734124999999437, -141.4375000013656063, 0.000000000000000000 ) ) ;
#27615 = CARTESIAN_POINT ( 'NONE',  ( -4.458734124999999437, -101.6458333319677365, -2.574251347313719407 ) ) ;
#27616 = DIRECTION ( 'NONE',  ( -0.000000000000000000, 1.000000000000000000, -0.000000000000000000 ) ) ;
#27617 = VERTEX_POINT ( 'NONE', #10786 ) ;
#27618 = EDGE_CURVE ( 'NONE', #2786, #26202, #62356, .T. ) ;
#27619 = CARTESIAN_POINT ( 'NONE',  ( -50.55543936806279248, -151.3125000013656063, 0.3552334253322060320 ) ) ;
#27620 = CARTESIAN_POINT ( 'NONE',  ( -57.46284108482265651, -144.0625000027312126, 4.819101127000239515 ) ) ;
#27621 = EDGE_CURVE ( 'NONE', #18331, #27768, #36049, .T. ) ;
#27622 = DIRECTION ( 'NONE',  ( -0.5000000000000005551, 0.8660254037844383745, 0.000000000000000000 ) ) ;
#27623 = CARTESIAN_POINT ( 'NONE',  ( -2.229367062499996610, -9.145833331967736513, 3.861377020970582219 ) ) ;
#27624 = CARTESIAN_POINT ( 'NONE',  ( -4.458734124999999437, -96.64583333196773651, -2.574251347313719407 ) ) ;
#27625 = ADVANCED_FACE ( 'NONE', ( #37458 ), #21401, .F. ) ;
#27626 = CARTESIAN_POINT ( 'NONE',  ( -1.846868145590734756, -149.3750000013656347, -4.458734125000000326 ) ) ;
#27627 = CARTESIAN_POINT ( 'NONE',  ( -4.458734124999999437, -25.64583333196773651, -2.574251347313719407 ) ) ;
#27628 = CARTESIAN_POINT ( 'NONE',  ( 5.000000000000000000, -46.50000000000000000, -6.123233995736766282E-16 ) ) ;
#27629 = CARTESIAN_POINT ( 'NONE',  ( -59.29741812935640155, -138.6250000013655779, -2.196230717870135685 ) ) ;
#27630 =( BOUNDED_CURVE ( )  B_SPLINE_CURVE ( 2, ( #47166, #56186, #3110, #12106, #31733, #51363, #7619, #22410, #45888 ),
 .UNSPECIFIED., .F., .F. ) 
 B_SPLINE_CURVE_WITH_KNOTS ( ( 3, 2, 2, 2, 3 ),
 ( 0.4812500000000000111, 0.4819444444444444531, 0.4833333333333333370, 0.4847222222222222210, 0.4854166666666666630 ),
 .UNSPECIFIED. ) 
 CURVE ( )  GEOMETRIC_REPRESENTATION_ITEM ( )  RATIONAL_B_SPLINE_CURVE ( ( 0.9330127018922194093, 0.9330127018922194093, 1.000000000000000000, 0.8660254037844387076, 1.000000000000000000, 0.8660254037844387076, 1.000000000000000000, 0.9330127018922194093, 0.9330127018922194093 ) ) 
 REPRESENTATION_ITEM ( '' )  );
#27631 = CARTESIAN_POINT ( 'NONE',  ( 4.458734124999998549, -64.97916666530106511, -2.574251347313721627 ) ) ;
#27632 = CARTESIAN_POINT ( 'NONE',  ( 1.339745962155612702, -70.29465819873850307, -5.000000000000000000 ) ) ;
#27633 = CARTESIAN_POINT ( 'NONE',  ( 5.000000000000000000, -88.29166666393548724, -2.886751345948130876 ) ) ;
#27634 = CARTESIAN_POINT ( 'NONE',  ( -3.152801135295367985, -146.8125000013655779, 3.152801135295367096 ) ) ;
#27635 = CARTESIAN_POINT ( 'NONE',  ( -4.458734124999999437, 10.35416666803225993, -2.574251347313719407 ) ) ;
#27636 = VERTEX_POINT ( 'NONE', #60965 ) ;
#27637 = CYLINDRICAL_SURFACE ( 'NONE', #9393, 5.000000000000000000 ) ;
#27639 = CARTESIAN_POINT ( 'NONE',  ( 2.229367062500001939, -22.97916666530107221, 3.861377020970579999 ) ) ;
#27638 = CARTESIAN_POINT ( 'NONE',  ( -5.000000000000000000, -92.08333333333334281, -2.886751345948128211 ) ) ;
#27640 = CARTESIAN_POINT ( 'NONE',  ( -2.500000000000000444, -77.04166666393547303, -4.330127018922193649 ) ) ;
#27641 = CARTESIAN_POINT ( 'NONE',  ( -4.458734124999999437, -70.56249999863439371, 0.000000000000000000 ) ) ;
#27642 = AXIS2_PLACEMENT_3D ( 'NONE', #9795, #6510, #2018 ) ;
#27643 = CARTESIAN_POINT ( 'NONE',  ( -4.769696007084728073, -114.9999999999999858, -1.500000000000000000 ) ) ;
#27644 = CYLINDRICAL_SURFACE ( 'NONE', #56120, 5.000000000000000000 ) ;
#27645 = CARTESIAN_POINT ( 'NONE',  ( -53.51423613279429503, -146.2500000013656063, 4.591703134518082763 ) ) ;
#27646 = CARTESIAN_POINT ( 'NONE',  ( -4.458734124999997661, 5.770833334698928674, 2.574251347313722516 ) ) ;
#27647 = CYLINDRICAL_SURFACE ( 'NONE', #12993, 5.000000000000000000 ) ;
#27648 = CARTESIAN_POINT ( 'NONE',  ( -49.85088928181150436, -141.6875000027311842, -1.666127454062680480 ) ) ;
#27649 = CARTESIAN_POINT ( 'NONE',  ( -3.152548672688508926E-16, 5.437500001365592084, -5.148502694627439702 ) ) ;
#27650 = CARTESIAN_POINT ( 'NONE',  ( -4.458734124999998549, -74.22916666530106511, 2.574251347313722516 ) ) ;
#27651 = CARTESIAN_POINT ( 'NONE',  ( -4.458734124999997661, -21.47916666530107221, 2.574251347313722516 ) ) ;
#27652 = CARTESIAN_POINT ( 'NONE',  ( -3.535250795749689387E-16, -7.249999999999999112, -5.773502691896257311 ) ) ;
#27653 = CARTESIAN_POINT ( 'NONE',  ( 4.458734124999999437, -160.5000000013656347, 1.846868145590737864 ) ) ;
#27654 = CARTESIAN_POINT ( 'NONE',  ( -5.000000000000000000, -158.5000000000000000, -6.123233995736766282E-16 ) ) ;
#27655 = CARTESIAN_POINT ( 'NONE',  ( 4.458734124999998549, -61.72916666530106511, -2.574251347313721627 ) ) ;
#27656 = CARTESIAN_POINT ( 'NONE',  ( 5.000000000000000000, -98.29166666393545881, -2.886751345948129988 ) ) ;
#27657 = CARTESIAN_POINT ( 'NONE',  ( 3.044556291839386294E-14, 16.87500000273118417, -5.000000000000000000 ) ) ;
#27658 = CARTESIAN_POINT ( 'NONE',  ( 9.457646018065525792E-16, -40.06249999863440081, 5.148502694627439702 ) ) ;
#27659 = CARTESIAN_POINT ( 'NONE',  ( 9.457646018065525792E-16, -106.3124999986343937, 5.148502694627439702 ) ) ;
#27660 = CARTESIAN_POINT ( 'NONE',  ( 4.458734124999998549, -64.97916666530106511, -2.574251347313721627 ) ) ;
#27661 = CARTESIAN_POINT ( 'NONE',  ( 5.000000000000000000, -46.50000000000000000, -6.123233995736766282E-16 ) ) ;
#27662 = CARTESIAN_POINT ( 'NONE',  ( 1.339745962155615144, -72.58034179853027013, 4.999999999999999112 ) ) ;
#27663 = DIRECTION ( 'NONE',  ( -3.614007241618347908E-17, 0.000000000000000000, 1.000000000000000000 ) ) ;
#27664 = ORIENTED_EDGE ( 'NONE', *, *, #49692, .T. ) ;
#27665 = DIRECTION ( 'NONE',  ( 0.000000000000000000, 1.000000000000000000, 0.000000000000000000 ) ) ;
#27666 = CYLINDRICAL_SURFACE ( 'NONE', #32971, 5.000000000000000000 ) ;
#27667 = CARTESIAN_POINT ( 'NONE',  ( 2.500000000000002220, -15.66666666666666963, 4.330127018922192761 ) ) ;
#27668 = CARTESIAN_POINT ( 'NONE',  ( 4.458734124999998549, -17.72916666530106866, -2.574251347313721627 ) ) ;
#27669 = CARTESIAN_POINT ( 'NONE',  ( -4.458734124999999437, -77.31249999863440792, 0.000000000000000000 ) ) ;
#27670 = DIRECTION ( 'NONE',  ( -0.000000000000000000, 1.000000000000000000, -0.000000000000000000 ) ) ;
#27671 = CARTESIAN_POINT ( 'NONE',  ( 5.000000000000000000, -11.29166666393547835, -2.886751345948129988 ) ) ;
#27673 = ORIENTED_EDGE ( 'NONE', *, *, #51539, .T. ) ;
#27672 = CARTESIAN_POINT ( 'NONE',  ( -4.458734124999999437, -44.31249999863440081, 0.000000000000000000 ) ) ;
#27674 = CARTESIAN_POINT ( 'NONE',  ( 5.000000000000000888, -81.58333333333332860, 2.886751345948126879 ) ) ;
#27676 = VERTEX_POINT ( 'NONE', #17532 ) ;
#27675 = CARTESIAN_POINT ( 'NONE',  ( -4.458734124999999437, 9.354166668032261711, -2.574251347313719407 ) ) ;
#27677 = CARTESIAN_POINT ( 'NONE',  ( 0.000000000000000000, -120.0000000000000000, 0.000000000000000000 ) ) ;
#27678 = CARTESIAN_POINT ( 'NONE',  ( -5.000000000000000000, -57.08333333333333570, -2.886751345948128211 ) ) ;
#27679 = CARTESIAN_POINT ( 'NONE',  ( 2.730187237215162345E-16, -158.4375000013655779, -4.458734124999999437 ) ) ;
#27680 = CARTESIAN_POINT ( 'NONE',  ( 9.457646018065525792E-16, -34.31249999863440792, 5.148502694627439702 ) ) ;
#27681 = PRESENTATION_LAYER_ASSIGNMENT (  '', '', ( #55424 ) ) ;
#27682 = CARTESIAN_POINT ( 'NONE',  ( -1.339745962155610925, -86.79465819873851729, 5.000000000000000000 ) ) ;
#27683 = CARTESIAN_POINT ( 'NONE',  ( 2.229367062499998831, -79.64583333196773651, -3.861377020970580887 ) ) ;
#27684 =( BOUNDED_CURVE ( )  B_SPLINE_CURVE ( 2, ( #16435, #1348, #21583, #36056, #25443, #10961, #55684, #11598, #36368 ),
 .UNSPECIFIED., .F., .F. ) 
 B_SPLINE_CURVE_WITH_KNOTS ( ( 3, 2, 2, 2, 3 ),
 ( 0.3303571428571428492, 0.3309523809523809423, 0.3321428571428571286, 0.3333333333333333148, 0.3339285714285714080 ),
 .UNSPECIFIED. ) 
 CURVE ( )  GEOMETRIC_REPRESENTATION_ITEM ( )  RATIONAL_B_SPLINE_CURVE ( ( 0.9330127018922194093, 0.9330127018922194093, 1.000000000000000000, 0.8660254037844387076, 1.000000000000000000, 0.8660254037844387076, 1.000000000000000000, 0.9330127018922194093, 0.9330127018922194093 ) ) 
 REPRESENTATION_ITEM ( '' )  );
#27685 = CARTESIAN_POINT ( 'NONE',  ( 2.071067811865475505, -165.8125000000000000, -5.000000000000000888 ) ) ;
#27686 = FACE_OUTER_BOUND ( 'NONE', #19225, .T. ) ;
#27687 = VECTOR ( 'NONE', #63180, 1000.000000000000000 ) ;
#27688 = CARTESIAN_POINT ( 'NONE',  ( -50.40829686548195099, -131.2500000013656347, -1.485763867205728284 ) ) ;
#27689 = CARTESIAN_POINT ( 'NONE',  ( -3.152548672688508926E-16, -2.812499998634407028, -5.148502694627439702 ) ) ;
#27690 = CARTESIAN_POINT ( 'NONE',  ( 4.458734124999998549, -38.97916666530107221, -2.574251347313721627 ) ) ;
#27691 = CARTESIAN_POINT ( 'NONE',  ( 1.975475456537005874E-15, -54.74999999999999289, 5.000000000000000000 ) ) ;
#27692 = CARTESIAN_POINT ( 'NONE',  ( -4.458734124999999437, -83.56249999863439371, 0.000000000000000000 ) ) ;
#27693 = DIRECTION ( 'NONE',  ( 0.000000000000000000, 0.000000000000000000, 1.000000000000000000 ) ) ;
#27694 = VERTEX_POINT ( 'NONE', #12694 ) ;
#27695 = CARTESIAN_POINT ( 'NONE',  ( 0.000000000000000000, -170.0000000000000000, 5.000000000000000000 ) ) ;
#27696 = CARTESIAN_POINT ( 'NONE',  ( -1.339745962155610925, -11.66965819600733667, 5.000000000000000000 ) ) ;
#27697 = CARTESIAN_POINT ( 'NONE',  ( -4.458734124999998549, -68.47916666530106511, 2.574251347313722516 ) ) ;
#27698 = CARTESIAN_POINT ( 'NONE',  ( 2.229367062500001939, -9.229166665301075767, 3.861377020970579999 ) ) ;
#27699 = VERTEX_POINT ( 'NONE', #7561 ) ;
#27700 = CARTESIAN_POINT ( 'NONE',  ( 1.339745962155615144, -5.705341801261479162, 4.999999999999999112 ) ) ;
#27701 = ADVANCED_FACE ( 'NONE', ( #31345 ), #51936, .T. ) ;
#27702 = CARTESIAN_POINT ( 'NONE',  ( 6.123233995736766282E-16, -120.0000000000000000, -5.000000000000000000 ) ) ;
#27703 = CARTESIAN_POINT ( 'NONE',  ( -4.458734124999998549, -6.479166665301073103, 2.574251347313722516 ) ) ;
#27704 = DIRECTION ( 'NONE',  ( 0.000000000000000000, 0.000000000000000000, 1.000000000000000000 ) ) ;
#27705 = CARTESIAN_POINT ( 'NONE',  ( 4.458734125000001214, 0.1041666680322607674, 2.574251347313718519 ) ) ;
#27706 = CARTESIAN_POINT ( 'NONE',  ( 0.000000000000000000, -120.0000000000000000, 0.000000000000000000 ) ) ;
#27707 = CARTESIAN_POINT ( 'NONE',  ( 4.458734124999997661, -158.5000000013656347, 1.846868145590737864 ) ) ;
#27708 = CARTESIAN_POINT ( 'NONE',  ( -4.458734124999997661, 25.52083333469892423, 2.574251347313722516 ) ) ;
#27709 = ORIENTED_EDGE ( 'NONE', *, *, #13018, .T. ) ;
#27710 = CARTESIAN_POINT ( 'NONE',  ( -4.458734124999999437, -92.31249999863440792, 0.000000000000000000 ) ) ;
#27711 = CARTESIAN_POINT ( 'NONE',  ( -4.999999999999998224, -46.91666666666666430, 2.886751345948131764 ) ) ;
#27712 = CARTESIAN_POINT ( 'NONE',  ( -3.152548672688508926E-16, -8.562499998634404363, -5.148502694627439702 ) ) ;
#27713 = CARTESIAN_POINT ( 'NONE',  ( 3.535533905932736864, -140.1250000000000000, 3.535533905932738641 ) ) ;
#27714 = LINE ( 'NONE', #38316, #3732 ) ;
#27715 = CARTESIAN_POINT ( 'NONE',  ( 1.975475456537005874E-15, 15.25000000000000000, 5.000000000000000000 ) ) ;
#27716 = CARTESIAN_POINT ( 'NONE',  ( 2.500000000000002220, -38.54166666393548013, 4.330127018922192761 ) ) ;
#27717 = CARTESIAN_POINT ( 'NONE',  ( 2.499999999999998668, -78.33333333333332860, -4.330127018922193649 ) ) ;
#27718 = CARTESIAN_POINT ( 'NONE',  ( -4.458734124999999437, 19.60416666803225993, -2.574251347313719407 ) ) ;
#27719 = CARTESIAN_POINT ( 'NONE',  ( 2.499999999999998668, -10.33333333333333393, -4.330127018922193649 ) ) ;
#27720 = CARTESIAN_POINT ( 'NONE',  ( -2.229367062500000163, 23.52083333469892779, -3.861377020970580443 ) ) ;
#27721 = CARTESIAN_POINT ( 'NONE',  ( 4.458734124999998549, -54.72916666530107932, -2.574251347313721627 ) ) ;
#27722 = CARTESIAN_POINT ( 'NONE',  ( 2.229367062500001939, -2.229166665301068662, 3.861377020970579999 ) ) ;
#27723 = FACE_OUTER_BOUND ( 'NONE', #3771, .T. ) ;
#27724 = CARTESIAN_POINT ( 'NONE',  ( 1.060575238724906964E-15, 13.24999999999999822, 5.773502691896257311 ) ) ;
#27725 = CARTESIAN_POINT ( 'NONE',  ( -2.071067811865478170, -143.4375000027312410, 5.000000000000000000 ) ) ;
#27726 = CIRCLE ( 'NONE', #59602, 5.000000000000000888 ) ;
#27727 = CARTESIAN_POINT ( 'NONE',  ( -4.458734124999999437, -50.31249999863440792, 0.000000000000000000 ) ) ;
#27728 = CARTESIAN_POINT ( 'NONE',  ( 2.500000000000002220, -84.54166666393547303, 4.330127018922192761 ) ) ;
#27729 = CARTESIAN_POINT ( 'NONE',  ( -59.44456063193725015, -135.8125000013656063, -0.3552334253322034230 ) ) ;
#27730 = LINE ( 'NONE', #7810, #6203 ) ;
#27731 = CARTESIAN_POINT ( 'NONE',  ( -2.500000000000000444, -105.0416666639354730, -4.330127018922193649 ) ) ;
#27732 = CARTESIAN_POINT ( 'NONE',  ( 2.229367062500001939, -85.22916666530107932, 3.861377020970579999 ) ) ;
#27733 = CARTESIAN_POINT ( 'NONE',  ( 3.152801135295367541, -159.5625000013656063, -3.152801135295367541 ) ) ;
#27734 = CARTESIAN_POINT ( 'NONE',  ( -2.499999999999996447, -34.83333333333332860, 4.330127018922195425 ) ) ;
#27735 = CARTESIAN_POINT ( 'NONE',  ( -1.339745962155613812, 23.79465819873851729, -5.000000000000000000 ) ) ;
#27736 = ORIENTED_EDGE ( 'NONE', *, *, #22246, .T. ) ;
#27737 = CARTESIAN_POINT ( 'NONE',  ( 2.229367062500001939, 15.77083333469892601, 3.861377020970579999 ) ) ;
#27738 = ORIENTED_EDGE ( 'NONE', *, *, #5996, .F. ) ;
#27739 = CARTESIAN_POINT ( 'NONE',  ( 4.458734124999998549, -97.72916666530106511, -2.574251347313721627 ) ) ;
#27740 = CARTESIAN_POINT ( 'NONE',  ( -3.152548672688508926E-16, 7.187500001365594748, -5.148502694627439702 ) ) ;
#27741 = CARTESIAN_POINT ( 'NONE',  ( 2.500000000000002220, 11.45833333606451809, 4.330127018922192761 ) ) ;
#27742 = CARTESIAN_POINT ( 'NONE',  ( 1.975475456537005874E-15, -43.62499999726880873, 5.000000000000000000 ) ) ;
#27743 = CARTESIAN_POINT ( 'NONE',  ( 5.000000000000000000, 8.500000000000000000, -6.123233995736766282E-16 ) ) ;
#27744 = CARTESIAN_POINT ( 'NONE',  ( 4.458734125000000326, -60.89583333196774362, 2.574251347313718519 ) ) ;
#27745 = CARTESIAN_POINT ( 'NONE',  ( 1.975475456537005874E-15, -39.75000000000000000, 5.000000000000000000 ) ) ;
#27746 = CARTESIAN_POINT ( 'NONE',  ( 5.000000000000000888, -80.58333333333332860, 2.886751345948126879 ) ) ;
#27747 = CARTESIAN_POINT ( 'NONE',  ( 9.457646018065525792E-16, -31.06249999863440436, 5.148502694627439702 ) ) ;
#27748 = DIRECTION ( 'NONE',  ( -0.000000000000000000, 1.000000000000000000, -0.000000000000000000 ) ) ;
#27749 = CARTESIAN_POINT ( 'NONE',  ( 6.123233995736766282E-16, -170.0000000000000000, -5.000000000000000000 ) ) ;
#27750 = FACE_OUTER_BOUND ( 'NONE', #45875, .T. ) ;
#27751 = CARTESIAN_POINT ( 'NONE',  ( -5.000000000000000000, -42.08333333333333570, -2.886751345948128211 ) ) ;
#27752 = CARTESIAN_POINT ( 'NONE',  ( -2.480964764533239819E-13, -107.7500000000000000, 5.000000000000000000 ) ) ;
#27754 = CARTESIAN_POINT ( 'NONE',  ( -4.458734124999998549, -22.47916666530107577, 2.574251347313722516 ) ) ;
#27753 = CARTESIAN_POINT ( 'NONE',  ( -2.500000000000000444, -48.16666666666666430, -4.330127018922193649 ) ) ;
#27755 = CARTESIAN_POINT ( 'NONE',  ( 1.243387493232115550E-13, -8.250000000000003553, -5.000000000000000000 ) ) ;
#27756 = CARTESIAN_POINT ( 'NONE',  ( -3.152548672688508926E-16, -67.56249999863440792, -5.148502694627439702 ) ) ;
#27757 = CARTESIAN_POINT ( 'NONE',  ( 1.846868145590736310, -147.8750000013656063, 4.458734124999999437 ) ) ;
#27758 = CARTESIAN_POINT ( 'NONE',  ( 4.458734125000001214, -73.89583333196773651, 2.574251347313718519 ) ) ;
#27759 = CARTESIAN_POINT ( 'NONE',  ( -57.19623071787017210, -142.6250000013655779, 4.297418129356382899 ) ) ;
#27760 =( BOUNDED_CURVE ( )  B_SPLINE_CURVE ( 2, ( #8545, #42950, #17879, #17574, #27217, #52920, #32035, #47157, #8858 ),
 .UNSPECIFIED., .F., .F. ) 
 B_SPLINE_CURVE_WITH_KNOTS ( ( 3, 2, 2, 2, 3 ),
 ( 0.5687499999999999778, 0.5694444444444444198, 0.5708333333333333037, 0.5722222222222221877, 0.5729166666666666297 ),
 .UNSPECIFIED. ) 
 CURVE ( )  GEOMETRIC_REPRESENTATION_ITEM ( )  RATIONAL_B_SPLINE_CURVE ( ( 0.9330127018922194093, 0.9330127018922194093, 1.000000000000000000, 0.8660254037844387076, 1.000000000000000000, 0.8660254037844387076, 1.000000000000000000, 0.9330127018922194093, 0.9330127018922194093 ) ) 
 REPRESENTATION_ITEM ( '' )  );
#27761 = CARTESIAN_POINT ( 'NONE',  ( 4.458734124999998549, -23.97916666530107221, -2.574251347313721627 ) ) ;
#27762 = CARTESIAN_POINT ( 'NONE',  ( 1.060575238724906964E-15, -65.62499999726881583, 5.773502691896257311 ) ) ;
#27763 = ORIENTED_EDGE ( 'NONE', *, *, #21284, .F. ) ;
#27764 = CARTESIAN_POINT ( 'NONE',  ( -6.972266317189433020E-16, -93.12499999726881583, -5.000000000000000000 ) ) ;
#27765 = VERTEX_POINT ( 'NONE', #27173 ) ;
#27766 = CARTESIAN_POINT ( 'NONE',  ( 9.457646018065525792E-16, -67.31249999863440792, 5.148502694627439702 ) ) ;
#27767 = CARTESIAN_POINT ( 'NONE',  ( 55.00000000000002132, -0.000000000000000000, -5.000000000000000000 ) ) ;
#27768 = VERTEX_POINT ( 'NONE', #46790 ) ;
#27769 = VECTOR ( 'NONE', #59769, 1000.000000000000000 ) ;
#27770 = CYLINDRICAL_SURFACE ( 'NONE', #26182, 5.000000000000000000 ) ;
#27772 = CIRCLE ( 'NONE', #59650, 5.000000000000001776 ) ;
#27771 = DIRECTION ( 'NONE',  ( -0.000000000000000000, 1.000000000000000000, -0.000000000000000000 ) ) ;
#27773 = CARTESIAN_POINT ( 'NONE',  ( 9.457646018065525792E-16, -52.31249999863440792, 5.148502694627439702 ) ) ;
#27774 = VERTEX_POINT ( 'NONE', #51627 ) ;
#27775 =( BOUNDED_CURVE ( )  B_SPLINE_CURVE ( 2, ( #44748, #49894, #26416, #45398, #15500, #26100, #16132, #46033, #36070 ),
 .UNSPECIFIED., .F., .F. ) 
 B_SPLINE_CURVE_WITH_KNOTS ( ( 3, 2, 2, 2, 3 ),
 ( 0.9303571428571428825, 0.9309523809523809756, 0.9321428571428571619, 0.9333333333333333481, 0.9339285714285714413 ),
 .UNSPECIFIED. ) 
 CURVE ( )  GEOMETRIC_REPRESENTATION_ITEM ( )  RATIONAL_B_SPLINE_CURVE ( ( 0.9330127018922194093, 0.9330127018922194093, 1.000000000000000000, 0.8660254037844387076, 1.000000000000000000, 0.8660254037844387076, 1.000000000000000000, 0.9330127018922194093, 0.9330127018922194093 ) ) 
 REPRESENTATION_ITEM ( '' )  );
#27776 = CARTESIAN_POINT ( 'NONE',  ( 0.5984201754795568373, 8.314755988442765755, -0.7022220667781353676 ) ) ;
#27777 = CARTESIAN_POINT ( 'NONE',  ( -2.229367062499996610, 6.854166668032259935, 3.861377020970582219 ) ) ;
#27778 = CARTESIAN_POINT ( 'NONE',  ( -3.152548672688508926E-16, 20.43750000136559208, -5.148502694627439702 ) ) ;
#27779 = CARTESIAN_POINT ( 'NONE',  ( -53.51423613279429503, -148.2500000013656063, 4.591703134518082763 ) ) ;
#27780 = CARTESIAN_POINT ( 'NONE',  ( 5.000000000000000888, 16.41666666666666785, 2.886751345948126879 ) ) ;
#27781 = CARTESIAN_POINT ( 'NONE',  ( -4.458734125000000326, -168.8750000013656063, 1.846868145590734089 ) ) ;
#27782 = ORIENTED_EDGE ( 'NONE', *, *, #45086, .F. ) ;
#27783 = CARTESIAN_POINT ( 'NONE',  ( -3.152548672688508926E-16, -71.56249999863439371, -5.148502694627439702 ) ) ;
#27784 = CYLINDRICAL_SURFACE ( 'NONE', #23289, 5.000000000000000000 ) ;
#27785 = CARTESIAN_POINT ( 'NONE',  ( 2.229367062499998831, 5.354166668032261711, -3.861377020970580887 ) ) ;
#27786 = CARTESIAN_POINT ( 'NONE',  ( -9.184850993605147944E-16, -140.3750000027312126, 5.000000000000000000 ) ) ;
#27787 = CARTESIAN_POINT ( 'NONE',  ( -4.458734124999998549, -58.47916666530106511, 2.574251347313722516 ) ) ;
#27788 = CARTESIAN_POINT ( 'NONE',  ( -5.000000000000000000, -21.87499999726881228, 0.000000000000000000 ) ) ;
#27789 = CARTESIAN_POINT ( 'NONE',  ( 75.00000000000002842, 15.00000000000000000, -5.000000000000000000 ) ) ;
#27790 = CARTESIAN_POINT ( 'NONE',  ( 3.535533905932738197, -160.8750000000000284, -3.535533905932738197 ) ) ;
#27791 = CARTESIAN_POINT ( 'NONE',  ( 1.339745962155615144, -76.70534180126148271, 4.999999999999999112 ) ) ;
#27792 = FACE_OUTER_BOUND ( 'NONE', #9104, .T. ) ;
#27793 = CARTESIAN_POINT ( 'NONE',  ( -2.229367062499996610, -43.14583333196773651, 3.861377020970582219 ) ) ;
#27794 = CARTESIAN_POINT ( 'NONE',  ( -4.458734124999999437, -22.64583333196773651, -2.574251347313719407 ) ) ;
#27795 = EDGE_LOOP ( 'NONE', ( #28225, #2396, #54264, #40821 ) ) ;
#27796 = LINE ( 'NONE', #13007, #53425 ) ;
#27797 = CARTESIAN_POINT ( 'NONE',  ( 4.458734125000001214, -109.8958333319677365, 2.574251347313718519 ) ) ;
#27798 = CARTESIAN_POINT ( 'NONE',  ( 5.000000000000000000, -155.1875000027312126, 2.071067811865478614 ) ) ;
#27799 = VERTEX_POINT ( 'NONE', #12380 ) ;
#27800 = CARTESIAN_POINT ( 'NONE',  ( -4.458734124999999437, -109.6458333319677365, -2.574251347313719407 ) ) ;
#27801 = EDGE_CURVE ( 'NONE', #13440, #44449, #42617, .T. ) ;
#27802 = CARTESIAN_POINT ( 'NONE',  ( -2.229367062499996610, -30.14583333196773651, 3.861377020970582219 ) ) ;
#27803 = CARTESIAN_POINT ( 'NONE',  ( 2.500000000000002220, -68.54166666393547303, 4.330127018922192761 ) ) ;
#27804 = CARTESIAN_POINT ( 'NONE',  ( -55.35523342533222291, -148.5625000013656063, 4.444560631937231499 ) ) ;
#27805 = CARTESIAN_POINT ( 'NONE',  ( 3.535533905932736864, -145.1250000000000000, 3.535533905932738641 ) ) ;
#27806 = CARTESIAN_POINT ( 'NONE',  ( 4.458734125000000326, -30.89583333196773651, 2.574251347313718519 ) ) ;
#27807 = CARTESIAN_POINT ( 'NONE',  ( 4.458734125000000326, -68.14583333196773651, 2.574251347313718519 ) ) ;
#27808 = CARTESIAN_POINT ( 'NONE',  ( 4.458734124999999437, -168.6250000013656063, -1.846868145590734978 ) ) ;
#27809 = CARTESIAN_POINT ( 'NONE',  ( -2.229367062499996610, -26.14583333196773651, 3.861377020970582219 ) ) ;
#27810 = CARTESIAN_POINT ( 'NONE',  ( 1.339745962155612702, -32.16965819600733312, -5.000000000000000000 ) ) ;
#27811 = CARTESIAN_POINT ( 'NONE',  ( -6.972266317189433020E-16, 8.875000002731184168, -5.000000000000000000 ) ) ;
#27812 = CARTESIAN_POINT ( 'NONE',  ( 5.000000000000000888, -17.58333333333333215, 2.886751345948126879 ) ) ;
#27813 = CARTESIAN_POINT ( 'NONE',  ( 1.846868145590736310, -146.6250000013655779, 4.458734124999999437 ) ) ;
#27814 = ORIENTED_EDGE ( 'NONE', *, *, #53861, .T. ) ;
#27815 = CARTESIAN_POINT ( 'NONE',  ( 6.123233995736766282E-16, -170.0000000000000000, -5.000000000000000000 ) ) ;
#27816 = CARTESIAN_POINT ( 'NONE',  ( 2.229367062500001939, -56.22916666530107221, 3.861377020970579999 ) ) ;
#27817 = CARTESIAN_POINT ( 'NONE',  ( -1.339745962155585168, -3.080341798530293662, -5.000000000000015987 ) ) ;
#27818 = CARTESIAN_POINT ( 'NONE',  ( -6.972266317189433020E-16, -81.12499999726881583, -5.000000000000000000 ) ) ;
#27819 = CARTESIAN_POINT ( 'NONE',  ( -2.500000000000000444, 26.83333333333333570, -4.330127018922193649 ) ) ;
#27820 = AXIS2_PLACEMENT_3D ( 'NONE', #5196, #38641, #58901 ) ;
#27821 = CARTESIAN_POINT ( 'NONE',  ( 1.975475456537005874E-15, -17.62499999726881938, 5.000000000000000000 ) ) ;
#27822 = CARTESIAN_POINT ( 'NONE',  ( 2.229367062499998831, -2.645833331967738289, -3.861377020970580887 ) ) ;
#27823 = EDGE_CURVE ( 'NONE', #47490, #10933, #16570, .T. ) ;
#27824 = CARTESIAN_POINT ( 'NONE',  ( -2.500000000000000444, -52.04166666393547303, -4.330127018922193649 ) ) ;
#27825 = CARTESIAN_POINT ( 'NONE',  ( 2.071067811865517694, -140.8124999999999716, -4.999999999999958256 ) ) ;
#27826 = CARTESIAN_POINT ( 'NONE',  ( -2.229367062499996610, 12.60416666803226171, 3.861377020970582219 ) ) ;
#27827 = ORIENTED_EDGE ( 'NONE', *, *, #40459, .F. ) ;
#27828 = DIRECTION ( 'NONE',  ( -0.000000000000000000, 1.000000000000000000, -0.000000000000000000 ) ) ;
#27829 = ORIENTED_EDGE ( 'NONE', *, *, #50727, .F. ) ;
#27830 =( BOUNDED_CURVE ( )  B_SPLINE_CURVE ( 2, ( #32735, #62016, #46905, #56244, #7358, #12483, #17934, #52362, #57198 ),
 .UNSPECIFIED., .F., .F. ) 
 B_SPLINE_CURVE_WITH_KNOTS ( ( 3, 2, 2, 2, 3 ),
 ( 0.7249999999999996447, 0.7291666666666662966, 0.7333333333333329485, 0.7374999999999998224, 0.7416666666666664742 ),
 .UNSPECIFIED. ) 
 CURVE ( )  GEOMETRIC_REPRESENTATION_ITEM ( )  RATIONAL_B_SPLINE_CURVE ( ( 1.000000000000005995, 0.9238795325112806323, 1.000000000000000000, 0.9238795325112867385, 1.000000000000000000, 0.9238795325112867385, 1.000000000000000000, 0.9238795325112908463, 0.9999999999999958922 ) ) 
 REPRESENTATION_ITEM ( '' )  );
#27831 = LINE ( 'NONE', #61948, #31682 ) ;
#27832 = CARTESIAN_POINT ( 'NONE',  ( 4.458734124999999437, -49.81249999863440792, -5.460374474430324690E-16 ) ) ;
#27833 = CARTESIAN_POINT ( 'NONE',  ( -4.458734125000001214, -160.1250000013655779, 1.846868145590734089 ) ) ;
#27834 = CARTESIAN_POINT ( 'NONE',  ( -2.499999999999996447, -44.70833333060214443, 4.330127018922195425 ) ) ;
#27835 = VERTEX_POINT ( 'NONE', #61915 ) ;
#27836 = CARTESIAN_POINT ( 'NONE',  ( 9.457646018065525792E-16, -23.06249999863440792, 5.148502694627439702 ) ) ;
#27837 = ORIENTED_EDGE ( 'NONE', *, *, #43993, .T. ) ;
#27838 = CARTESIAN_POINT ( 'NONE',  ( 5.000000000000000888, -53.58333333333333570, 2.886751345948126879 ) ) ;
#27839 = CARTESIAN_POINT ( 'NONE',  ( -1.846868145590734756, -160.1250000013655779, -4.458734125000000326 ) ) ;
#27840 = CARTESIAN_POINT ( 'NONE',  ( 0.000000000000000000, -170.0000000000000000, 0.000000000000000000 ) ) ;
#27841 = CARTESIAN_POINT ( 'NONE',  ( -53.33387254593733928, -136.8125000000000284, 5.149110718188519620 ) ) ;
#27842 = CARTESIAN_POINT ( 'NONE',  ( 9.457646018065525792E-16, -40.31249999863440081, 5.148502694627439702 ) ) ;
#27843 = CARTESIAN_POINT ( 'NONE',  ( -6.972266317189433020E-16, 19.87500000273118417, -5.000000000000000000 ) ) ;
#27844 = VERTEX_POINT ( 'NONE', #22356 ) ;
#27845 = CARTESIAN_POINT ( 'NONE',  ( -2.229367062499996610, -85.14583333196773651, 3.861377020970582219 ) ) ;
#27846 = CARTESIAN_POINT ( 'NONE',  ( -4.458734124999999437, 23.68750000136559564, 0.000000000000000000 ) ) ;
#27847 = FACE_OUTER_BOUND ( 'NONE', #42945, .T. ) ;
#27848 = ORIENTED_EDGE ( 'NONE', *, *, #58331, .T. ) ;
#27849 = CARTESIAN_POINT ( 'NONE',  ( 5.000000000000000888, 14.41666666666666430, 2.886751345948126879 ) ) ;
#27850 = CARTESIAN_POINT ( 'NONE',  ( -57.89159099828107458, -138.9375000013656063, -3.393966926194107447 ) ) ;
#27851 = CARTESIAN_POINT ( 'NONE',  ( -2.229367062499996610, -83.39583333196773651, 3.861377020970582219 ) ) ;
#27852 = CARTESIAN_POINT ( 'NONE',  ( -57.46284108482265651, -129.0625000027312126, 4.819101127000239515 ) ) ;
#27853 = FACE_OUTER_BOUND ( 'NONE', #59392, .T. ) ;
#27854 = CARTESIAN_POINT ( 'NONE',  ( -9.184850993605147944E-16, -158.3750000027311842, 5.000000000000000000 ) ) ;
#27855 = SHAPE_REPRESENTATION ( 'MAS-184', ( #43100, #50315, #25663, #47251, #1033, #35953, #53385, #4088, #22602, #8225, #49255 ), #29721 ) ;
#27856 = CARTESIAN_POINT ( 'NONE',  ( -1.339745962155610925, -46.66965819600733312, 5.000000000000000000 ) ) ;
#27857 = CARTESIAN_POINT ( 'NONE',  ( -2.229367062499996610, -52.14583333196773651, 3.861377020970582219 ) ) ;
#27858 = CARTESIAN_POINT ( 'NONE',  ( -5.000000000000000000, -71.87499999726880162, 0.000000000000000000 ) ) ;
#27859 = VECTOR ( 'NONE', #25137, 1000.000000000000000 ) ;
#27860 = CARTESIAN_POINT ( 'NONE',  ( 2.229367062500001939, 25.02083333469892779, 3.861377020970579999 ) ) ;
#27861 = CARTESIAN_POINT ( 'NONE',  ( -3.535250795749689387E-16, -108.2499999999999858, -5.773502691896257311 ) ) ;
#27862 = LINE ( 'NONE', #43586, #61769 ) ;
#27863 = CARTESIAN_POINT ( 'NONE',  ( 9.457646018065525792E-16, -45.31249999863440081, 5.148502694627439702 ) ) ;
#27864 = CARTESIAN_POINT ( 'NONE',  ( -2.500000000000000444, -6.041666663935481019, -4.330127018922193649 ) ) ;
#27865 = DIRECTION ( 'NONE',  ( -0.000000000000000000, 1.000000000000000000, -0.000000000000000000 ) ) ;
#27866 = CARTESIAN_POINT ( 'NONE',  ( -59.44456063193725015, -126.5625000013655921, -0.3552334253322034230 ) ) ;
#27867 = CARTESIAN_POINT ( 'NONE',  ( -2.229367062500000163, -85.72916666530107932, -3.861377020970580443 ) ) ;
#27868 = CARTESIAN_POINT ( 'NONE',  ( -4.458734124999999437, -104.3124999986344079, 0.000000000000000000 ) ) ;
#27869 = CARTESIAN_POINT ( 'NONE',  ( 4.458734124999999437, -5.062499998634402587, -5.460374474430324690E-16 ) ) ;
#27870 = VERTEX_POINT ( 'NONE', #11729 ) ;
#27871 = CARTESIAN_POINT ( 'NONE',  ( -2.500000000000000444, -15.04166666393548191, -4.330127018922193649 ) ) ;
#27872 = CARTESIAN_POINT ( 'NONE',  ( -3.152548672688508926E-16, -90.56249999863440792, -5.148502694627439702 ) ) ;
#27873 = CARTESIAN_POINT ( 'NONE',  ( 2.071067811865475505, -163.9375000027311842, -5.000000000000000888 ) ) ;
#27874 = CARTESIAN_POINT ( 'NONE',  ( -2.229367062500000163, -93.72916666530106511, -3.861377020970580443 ) ) ;
#27875 = ADVANCED_FACE ( 'NONE', ( #31037 ), #26216, .T. ) ;
#27876 = CARTESIAN_POINT ( 'NONE',  ( 2.229367062500001939, 6.770833334698928674, 3.861377020970579999 ) ) ;
#27877 = CYLINDRICAL_SURFACE ( 'NONE', #57189, 5.000000000000000000 ) ;
#27878 = CARTESIAN_POINT ( 'NONE',  ( -52.80376928212989185, -129.8750000013656063, -4.297418129356379346 ) ) ;
#27879 = CARTESIAN_POINT ( 'NONE',  ( 4.458734124999999437, -10.81249999863440792, -5.460374474430324690E-16 ) ) ;
#27880 = CARTESIAN_POINT ( 'NONE',  ( 4.458734124999999437, 12.93750000136559208, -5.460374474430324690E-16 ) ) ;
#27881 = CARTESIAN_POINT ( 'NONE',  ( 2.229367062500001939, -56.22916666530107221, 3.861377020970579999 ) ) ;
#27882 = CARTESIAN_POINT ( 'NONE',  ( -1.339745962155660663, -19.79465819873851729, 4.999999999999972466 ) ) ;
#27883 = CARTESIAN_POINT ( 'NONE',  ( -1.230605004983934782E-13, -36.75000000000000711, 5.000000000000000000 ) ) ;
#27884 = CARTESIAN_POINT ( 'NONE',  ( 4.458734124999999437, -9.812499998634406140, -5.460374474430324690E-16 ) ) ;
#27885 = CARTESIAN_POINT ( 'NONE',  ( 0.000000000000000000, -120.0000000000000000, 5.000000000000000000 ) ) ;
#27886 = EDGE_LOOP ( 'NONE', ( #46775, #54671, #22114, #61945 ) ) ;
#27887 = CARTESIAN_POINT ( 'NONE',  ( -2.229367062499996610, -35.39583333196772941, 3.861377020970582219 ) ) ;
#27888 = CARTESIAN_POINT ( 'NONE',  ( -52.10840900171896806, -128.4375000013656063, 3.393966926194110556 ) ) ;
#27889 = CARTESIAN_POINT ( 'NONE',  ( 1.975475456537005874E-15, -76.75000000000000000, 5.000000000000000000 ) ) ;
#27890 = EDGE_CURVE ( 'NONE', #44569, #62283, #5229, .T. ) ;
#27891 = CARTESIAN_POINT ( 'NONE',  ( -1.339745962155613812, 9.794658198738519062, -5.000000000000000000 ) ) ;
#27892 = CARTESIAN_POINT ( 'NONE',  ( 2.229367062499998831, -79.64583333196773651, -3.861377020970580887 ) ) ;
#27893 = CARTESIAN_POINT ( 'NONE',  ( -2.229367062500000163, 25.27083333469892779, -3.861377020970580443 ) ) ;
#27894 = CARTESIAN_POINT ( 'NONE',  ( 4.458734125000001214, 16.10416666803225993, 2.574251347313718519 ) ) ;
#27895 = FACE_OUTER_BOUND ( 'NONE', #49982, .T. ) ;
#27896 = EDGE_CURVE ( 'NONE', #13678, #39270, #17200, .T. ) ;
#27897 = CYLINDRICAL_SURFACE ( 'NONE', #35861, 5.000000000000000000 ) ;
#27898 = CARTESIAN_POINT ( 'NONE',  ( 4.458734124999998549, -82.97916666530106511, -2.574251347313721627 ) ) ;
#27899 = CARTESIAN_POINT ( 'NONE',  ( -4.999999999999999112, -69.91666666666667140, 2.886751345948131764 ) ) ;
#27900 = CARTESIAN_POINT ( 'NONE',  ( 2.499999999999998668, 20.79166666939784847, -4.330127018922193649 ) ) ;
#27901 = EDGE_LOOP ( 'NONE', ( #23171, #24198, #6231, #36704, #13203 ) ) ;
#27902 = CYLINDRICAL_SURFACE ( 'NONE', #18092, 5.000000000000000000 ) ;
#27903 = CARTESIAN_POINT ( 'NONE',  ( 2.071067811865508812, -167.1875000000000284, 4.999999999999968026 ) ) ;
#27905 = CARTESIAN_POINT ( 'NONE',  ( -4.999999999999999112, -30.91666666666666785, 2.886751345948131764 ) ) ;
#27904 = CARTESIAN_POINT ( 'NONE',  ( -6.972266317189433020E-16, -52.25000000000000711, -5.000000000000000000 ) ) ;
#27906 = CARTESIAN_POINT ( 'NONE',  ( -4.458734124999999437, -35.39583333196773651, -2.574251347313719407 ) ) ;
#27907 = CARTESIAN_POINT ( 'NONE',  ( 5.000000000000000000, 0.5833333333333314830, -2.886751345948130876 ) ) ;
#27908 = CARTESIAN_POINT ( 'NONE',  ( -2.499999999999996447, -28.70833333060214798, 4.330127018922195425 ) ) ;
#27910 = ORIENTED_EDGE ( 'NONE', *, *, #37339, .T. ) ;
#27909 = CARTESIAN_POINT ( 'NONE',  ( 2.229367062500001939, -58.97916666530106511, 3.861377020970579999 ) ) ;
#27911 = CARTESIAN_POINT ( 'NONE',  ( 5.000000000000000888, -28.58333333333333570, 2.886751345948126879 ) ) ;
#27913 = VERTEX_POINT ( 'NONE', #46159 ) ;
#27912 = CARTESIAN_POINT ( 'NONE',  ( 2.229367062500001939, -7.229166665301073103, 3.861377020970579999 ) ) ;
#27914 = CARTESIAN_POINT ( 'NONE',  ( 5.000000000000000888, -77.58333333333334281, 2.886751345948126879 ) ) ;
#27915 = CARTESIAN_POINT ( 'NONE',  ( -1.339745962155610925, 1.330341803992665106, 5.000000000000000000 ) ) ;
#27916 = CARTESIAN_POINT ( 'NONE',  ( 2.229367062500001939, -53.22916666530107221, 3.861377020970579999 ) ) ;
#27917 = CARTESIAN_POINT ( 'NONE',  ( 1.060575238724906964E-15, -78.62499999726880162, 5.773502691896257311 ) ) ;
#27919 = ORIENTED_EDGE ( 'NONE', *, *, #25475, .T. ) ;
#27918 = CARTESIAN_POINT ( 'NONE',  ( 5.000000000000000000, -65.29166666393547303, -2.886751345948130876 ) ) ;
#27920 = CARTESIAN_POINT ( 'NONE',  ( -53.33387254593733928, -149.8124999999999716, 5.149110718188519620 ) ) ;
#27921 = EDGE_CURVE ( 'NONE', #21128, #27373, #33598, .T. ) ;
#27922 = CARTESIAN_POINT ( 'NONE',  ( -3.152548672688508926E-16, -22.81249999863440436, -5.148502694627439702 ) ) ;
#27924 = ORIENTED_EDGE ( 'NONE', *, *, #35458, .T. ) ;
#27923 = CARTESIAN_POINT ( 'NONE',  ( 2.229367062500001939, -59.22916666530106511, 3.861377020970579999 ) ) ;
#27925 =( LENGTH_UNIT ( ) NAMED_UNIT ( * ) SI_UNIT ( .MILLI., .METRE. ) );
#27926 = CARTESIAN_POINT ( 'NONE',  ( -8.190561711645485556E-16, -141.6875000013656063, 4.458734124999999437 ) ) ;
#27927 = CARTESIAN_POINT ( 'NONE',  ( -3.152548672688508926E-16, -98.81249999863440792, -5.148502694627439702 ) ) ;
#27928 = CARTESIAN_POINT ( 'NONE',  ( 5.000000000000000000, -50.29166666393548013, -2.886751345948130876 ) ) ;
#27929 = ORIENTED_EDGE ( 'NONE', *, *, #53609, .T. ) ;
#27930 = CARTESIAN_POINT ( 'NONE',  ( -57.89159099828107458, -151.9375000013656063, -3.393966926194107447 ) ) ;
#27931 = CARTESIAN_POINT ( 'NONE',  ( -49.85088928181150436, -140.6875000027312410, -1.666127454062680702 ) ) ;
#27932 = LINE ( 'NONE', #3503, #60999 ) ;
#27933 = CARTESIAN_POINT ( 'NONE',  ( 9.457646018065525792E-16, -7.062499998634404363, 5.148502694627439702 ) ) ;
#27934 = CARTESIAN_POINT ( 'NONE',  ( 4.458734124999999437, -97.06249999863440792, -5.460374474430324690E-16 ) ) ;
#27935 = CARTESIAN_POINT ( 'NONE',  ( -4.458734125000000326, -146.2500000013656063, -1.846868145590735644 ) ) ;
#27936 = CARTESIAN_POINT ( 'NONE',  ( 2.229367062499998831, -25.89583333196773651, -3.861377020970580887 ) ) ;
#27937 = CARTESIAN_POINT ( 'NONE',  ( -1.339745962155613812, -67.20534180126149693, -5.000000000000000000 ) ) ;
#27938 = CARTESIAN_POINT ( 'NONE',  ( -58.39396692619412477, -135.4375000013656063, 2.891590998281057701 ) ) ;
#27939 = CARTESIAN_POINT ( 'NONE',  ( 4.458734125000001214, -70.14583333196773651, 2.574251347313718519 ) ) ;
#27940 = FACE_OUTER_BOUND ( 'NONE', #47671, .T. ) ;
#27941 = CARTESIAN_POINT ( 'NONE',  ( 0.000000000000000000, -120.0000000000000000, 0.000000000000000000 ) ) ;
#27942 = CARTESIAN_POINT ( 'NONE',  ( -1.846868145590737420, -140.7500000013655779, 4.458734124999997661 ) ) ;
#27943 = CARTESIAN_POINT ( 'NONE',  ( -2.229367062500000163, 11.27083333469892601, -3.861377020970580443 ) ) ;
#27944 = ORIENTED_EDGE ( 'NONE', *, *, #5070, .F. ) ;
#27945 = CARTESIAN_POINT ( 'NONE',  ( 7.204675194429079505E-15, 26.87500000273118417, -5.000000000000000000 ) ) ;
#27946 = CARTESIAN_POINT ( 'NONE',  ( -2.071067811865391128, -144.6875000000000568, -5.000000000000086153 ) ) ;
#27948 = CARTESIAN_POINT ( 'NONE',  ( -4.458734124999999437, -24.39583333196773651, -2.574251347313719407 ) ) ;
#27947 = CARTESIAN_POINT ( 'NONE',  ( -5.000000000000000000, -91.08333333333334281, -2.886751345948128211 ) ) ;
#27949 = DIRECTION ( 'NONE',  ( -0.000000000000000000, 1.000000000000000000, -0.000000000000000000 ) ) ;
#27950 = CARTESIAN_POINT ( 'NONE',  ( -4.458734124999999437, -78.56249999863440792, 0.000000000000000000 ) ) ;
#27951 = CARTESIAN_POINT ( 'NONE',  ( -4.458734124999999437, 27.35416666803225993, -2.574251347313719407 ) ) ;
#27952 = CARTESIAN_POINT ( 'NONE',  ( 2.499999999999998668, -76.20833333060214443, -4.330127018922193649 ) ) ;
#27953 =( BOUNDED_CURVE ( )  B_SPLINE_CURVE ( 2, ( #729, #34471, #30294, #50239, #59912, #45415, #10680, #11311, #55074 ),
 .UNSPECIFIED., .F., .F. ) 
 B_SPLINE_CURVE_WITH_KNOTS ( ( 3, 2, 2, 2, 3 ),
 ( 0.1553571428571428603, 0.1559523809523809534, 0.1571428571428571397, 0.1583333333333333259, 0.1589285714285714191 ),
 .UNSPECIFIED. ) 
 CURVE ( )  GEOMETRIC_REPRESENTATION_ITEM ( )  RATIONAL_B_SPLINE_CURVE ( ( 0.9330127018922194093, 0.9330127018922194093, 1.000000000000000000, 0.8660254037844387076, 1.000000000000000000, 0.8660254037844387076, 1.000000000000000000, 0.9330127018922194093, 0.9330127018922194093 ) ) 
 REPRESENTATION_ITEM ( '' )  );
#27954 = CARTESIAN_POINT ( 'NONE',  ( -59.44456063193725015, -144.5625000013656063, -0.3552334253322034230 ) ) ;
#27955 = EDGE_CURVE ( 'NONE', #62968, #10267, #63482, .T. ) ;
#27956 = EDGE_CURVE ( 'NONE', #11458, #44963, #53503, .T. ) ;
#27957 = CARTESIAN_POINT ( 'NONE',  ( -2.229367062499996610, 1.854166668032262377, 3.861377020970582219 ) ) ;
#27958 = EDGE_CURVE ( 'NONE', #46124, #38768, #27796, .T. ) ;
#27959 = CARTESIAN_POINT ( 'NONE',  ( 4.458734125000000326, 8.104166668032261711, 2.574251347313718519 ) ) ;
#27960 = CARTESIAN_POINT ( 'NONE',  ( 9.457646018065525792E-16, -71.06249999863440792, 5.148502694627439702 ) ) ;
#27961 = CARTESIAN_POINT ( 'NONE',  ( -2.229367062499996610, -20.39583333196774007, 3.861377020970582219 ) ) ;
#27962 = CARTESIAN_POINT ( 'NONE',  ( -4.999999999999999112, -4.916666666666666075, 2.886751345948131764 ) ) ;
#27963 = CARTESIAN_POINT ( 'NONE',  ( -3.152801135295367985, -158.8125000013656063, 3.152801135295367096 ) ) ;
#27964 = CARTESIAN_POINT ( 'NONE',  ( 3.061616997868383141E-16, -158.7500000000000000, -5.000000000000000000 ) ) ;
#27965 = CARTESIAN_POINT ( 'NONE',  ( -4.458734124999999437, -64.31249999863440792, 0.000000000000000000 ) ) ;
#27966 = CARTESIAN_POINT ( 'NONE',  ( 2.499999999999998668, -98.20833333060214443, -4.330127018922193649 ) ) ;
#27967 = EDGE_CURVE ( 'NONE', #2367, #27870, #32627, .T. ) ;
#27968 = CARTESIAN_POINT ( 'NONE',  ( 0.000000000000000000, -170.0000000000000000, 0.000000000000000000 ) ) ;
#27969 = CARTESIAN_POINT ( 'NONE',  ( -4.458734124999997661, -39.22916666530107221, 2.574251347313722516 ) ) ;
#27970 = CARTESIAN_POINT ( 'NONE',  ( -1.339745962155610925, -63.79465819873851729, 5.000000000000000000 ) ) ;
#27971 = EDGE_CURVE ( 'NONE', #3560, #11132, #11798, .T. ) ;
#27972 = CARTESIAN_POINT ( 'NONE',  ( -3.152548672688508926E-16, -105.8124999986344221, -5.148502694627439702 ) ) ;
#27973 = CARTESIAN_POINT ( 'NONE',  ( -2.229367062500000163, -65.72916666530106511, -3.861377020970580443 ) ) ;
#27974 = CARTESIAN_POINT ( 'NONE',  ( -4.999999999999999112, -52.91666666666666430, 2.886751345948131764 ) ) ;
#27975 = CARTESIAN_POINT ( 'NONE',  ( 1.339745962155612702, -57.16965819600733312, -5.000000000000000000 ) ) ;
#27976 = CARTESIAN_POINT ( 'NONE',  ( 3.535533905932738197, -152.0000000027312126, -3.535533905932738197 ) ) ;
#27977 = ORIENTED_EDGE ( 'NONE', *, *, #51779, .F. ) ;
#27978 = CARTESIAN_POINT ( 'NONE',  ( 0.000000000000000000, 15.00000000000000000, 4.999999999999999112 ) ) ;
#27979 = CARTESIAN_POINT ( 'NONE',  ( 1.975475456537005874E-15, -89.62499999726880162, 5.000000000000000000 ) ) ;
#27980 = CARTESIAN_POINT ( 'NONE',  ( 1.060575238724906964E-15, -12.74999999999999822, 5.773502691896257311 ) ) ;
#27981 = CARTESIAN_POINT ( 'NONE',  ( -4.458734124999998549, -18.22916666530107221, 2.574251347313722516 ) ) ;
#27982 = ADVANCED_FACE ( 'NONE', ( #48043 ), #18767, .T. ) ;
#27983 = CARTESIAN_POINT ( 'NONE',  ( 4.458734124999999437, -75.81249999863440792, -5.460374474430324690E-16 ) ) ;
#27984 = CARTESIAN_POINT ( 'NONE',  ( 1.975475456537005874E-15, -4.624999997268815832, 5.000000000000000000 ) ) ;
#27985 = CARTESIAN_POINT ( 'NONE',  ( -2.499999999999996447, -12.70833333060214798, 4.330127018922195425 ) ) ;
#27987 = ORIENTED_EDGE ( 'NONE', *, *, #21742, .F. ) ;
#27986 = CARTESIAN_POINT ( 'NONE',  ( 4.458734124999998549, -45.72916666530106511, -2.574251347313721627 ) ) ;
#27988 = CYLINDRICAL_SURFACE ( 'NONE', #53849, 5.000000000000000000 ) ;
#27990 = ORIENTED_EDGE ( 'NONE', *, *, #16484, .F. ) ;
#27989 = CARTESIAN_POINT ( 'NONE',  ( -3.152548672688508926E-16, 8.187500001365595637, -5.148502694627439702 ) ) ;
#27991 = CARTESIAN_POINT ( 'NONE',  ( 1.339745962155612702, -81.16965819600734733, -5.000000000000000000 ) ) ;
#27992 = CARTESIAN_POINT ( 'NONE',  ( -5.000000000000000000, -60.08333333333333570, -2.886751345948128211 ) ) ;
#27993 = CARTESIAN_POINT ( 'NONE',  ( 1.846868145590735200, -159.5000000013655779, -4.458734125000000326 ) ) ;
#27994 = CARTESIAN_POINT ( 'NONE',  ( 9.457646018065525792E-16, -37.31249999863440792, 5.148502694627439702 ) ) ;
#27995 = CARTESIAN_POINT ( 'NONE',  ( 1.339745962155615144, -14.70534180126147916, 4.999999999999999112 ) ) ;
#27996 = CARTESIAN_POINT ( 'NONE',  ( -4.458734124999999437, -81.31249999863440792, 0.000000000000000000 ) ) ;
#27997 = CARTESIAN_POINT ( 'NONE',  ( 5.000000000000000000, -168.0000000000000000, 0.000000000000000000 ) ) ;
#27998 = CARTESIAN_POINT ( 'NONE',  ( 9.457646018065525792E-16, -90.06249999863440792, 5.148502694627439702 ) ) ;
#27999 = CARTESIAN_POINT ( 'NONE',  ( -52.10840900171896806, -129.4375000013656063, 3.393966926194110556 ) ) ;
#28000 = CARTESIAN_POINT ( 'NONE',  ( 4.458734124999999437, -4.062499998634408804, -5.460374474430324690E-16 ) ) ;
#28001 = CARTESIAN_POINT ( 'NONE',  ( -2.229367062499996610, -43.39583333196773651, 3.861377020970582219 ) ) ;
#28002 = CARTESIAN_POINT ( 'NONE',  ( 1.339745962155612702, -67.16965819600733312, -5.000000000000000000 ) ) ;
#28003 = CARTESIAN_POINT ( 'NONE',  ( 2.229367062499998831, -83.89583333196773651, -3.861377020970580887 ) ) ;
#28004 = CARTESIAN_POINT ( 'NONE',  ( 1.975475456537005874E-15, -3.624999997268814056, 5.000000000000000000 ) ) ;
#28005 =( BOUNDED_CURVE ( )  B_SPLINE_CURVE ( 2, ( #63206, #20082, #39057, #13984, #24268, #15260, #33614, #49026, #33921 ),
 .UNSPECIFIED., .F., .F. ) 
 B_SPLINE_CURVE_WITH_KNOTS ( ( 3, 2, 2, 2, 3 ),
 ( 0.2446428571428571341, 0.2452380952380952273, 0.2464285714285714413, 0.2476190476190476275, 0.2482142857142857206 ),
 .UNSPECIFIED. ) 
 CURVE ( )  GEOMETRIC_REPRESENTATION_ITEM ( )  RATIONAL_B_SPLINE_CURVE ( ( 0.9330127018922194093, 0.9330127018922194093, 1.000000000000000000, 0.8660254037844387076, 1.000000000000000000, 0.8660254037844387076, 1.000000000000000000, 0.9330127018922194093, 0.9330127018922194093 ) ) 
 REPRESENTATION_ITEM ( '' )  );
#28006 = ORIENTED_EDGE ( 'NONE', *, *, #33138, .F. ) ;
#28007 = CARTESIAN_POINT ( 'NONE',  ( -55.39835681537999790, -153.0000000027312410, 4.984105922594378235 ) ) ;
#28008 =( BOUNDED_CURVE ( )  B_SPLINE_CURVE ( 2, ( #10818, #30430, #60365, #16918, #41037, #45231, #25931, #35589, #2152 ),
 .UNSPECIFIED., .F., .F. ) 
 B_SPLINE_CURVE_WITH_KNOTS ( ( 3, 2, 2, 2, 3 ),
 ( 0.8232142857142856762, 0.8238095238095237693, 0.8249999999999999556, 0.8261904761904761418, 0.8267857142857142350 ),
 .UNSPECIFIED. ) 
 CURVE ( )  GEOMETRIC_REPRESENTATION_ITEM ( )  RATIONAL_B_SPLINE_CURVE ( ( 0.9330127018922194093, 0.9330127018922194093, 1.000000000000000000, 0.8660254037844387076, 1.000000000000000000, 0.8660254037844387076, 1.000000000000000000, 0.9330127018922194093, 0.9330127018922194093 ) ) 
 REPRESENTATION_ITEM ( '' )  );
#28009 = CARTESIAN_POINT ( 'NONE',  ( 2.499999999999998668, -82.20833333060214443, -4.330127018922193649 ) ) ;
#28010 = CARTESIAN_POINT ( 'NONE',  ( -2.229367062500000163, -68.72916666530107932, -3.861377020970580443 ) ) ;
#28011 = CARTESIAN_POINT ( 'NONE',  ( -8.190561711645485556E-16, -147.9375000013656063, 4.458734124999999437 ) ) ;
#28012 = ORIENTED_EDGE ( 'NONE', *, *, #13304, .F. ) ;
#28013 = CARTESIAN_POINT ( 'NONE',  ( 3.535533905932738197, -163.8750000000000284, -3.535533905932738197 ) ) ;
#28014 = LINE ( 'NONE', #12594, #22467 ) ;
#28015 = CARTESIAN_POINT ( 'NONE',  ( -4.458734124999999437, -9.562499998634406140, 0.000000000000000000 ) ) ;
#28016 = CARTESIAN_POINT ( 'NONE',  ( -5.000000000000000000, -35.00000000000000000, 0.000000000000000000 ) ) ;
#28017 = CARTESIAN_POINT ( 'NONE',  ( 4.458734124999998549, 4.270833334698926897, -2.574251347313721627 ) ) ;
#28018 = FACE_OUTER_BOUND ( 'NONE', #61161, .T. ) ;
#28019 = CARTESIAN_POINT ( 'NONE',  ( 4.458734124999997661, -154.5000000013656347, 1.846868145590737864 ) ) ;
#28020 = CARTESIAN_POINT ( 'NONE',  ( -2.229367062500000163, 25.27083333469892779, -3.861377020970580443 ) ) ;
#28021 = ORIENTED_EDGE ( 'NONE', *, *, #3544, .F. ) ;
#28022 = CARTESIAN_POINT ( 'NONE',  ( -3.152548672688508926E-16, -94.56249999863440792, -5.148502694627439702 ) ) ;
#28023 = CARTESIAN_POINT ( 'NONE',  ( -2.500000000000000444, -97.16666666666665719, -4.330127018922193649 ) ) ;
#28024 = DIRECTION ( 'NONE',  ( -0.000000000000000000, 1.000000000000000000, -0.000000000000000000 ) ) ;
#28025 = CARTESIAN_POINT ( 'NONE',  ( 9.457646018065525792E-16, -9.062499998634406140, 5.148502694627439702 ) ) ;
#28026 = LINE ( 'NONE', #42502, #22150 ) ;
#28027 = CARTESIAN_POINT ( 'NONE',  ( 1.975475456537005874E-15, -27.62499999726880873, 5.000000000000000000 ) ) ;
#28028 = LINE ( 'NONE', #60325, #8903 ) ;
#28029 = ADVANCED_FACE ( 'NONE', ( #38698 ), #4607, .T. ) ;
#28030 = CARTESIAN_POINT ( 'NONE',  ( 5.000000000000000000, -35.29166666393547303, -2.886751345948129988 ) ) ;
#28031 = CYLINDRICAL_SURFACE ( 'NONE', #12359, 5.000000000000000000 ) ;
#28032 = CARTESIAN_POINT ( 'NONE',  ( -2.229367062499996610, 20.85416666803226349, 3.861377020970582219 ) ) ;
#28033 = CARTESIAN_POINT ( 'NONE',  ( 1.975475456537005874E-15, -20.62499999726881228, 5.000000000000000000 ) ) ;
#28034 =( BOUNDED_CURVE ( )  B_SPLINE_CURVE ( 2, ( #31298, #40640, #17152, #46426, #6875, #46106, #50935, #36776, #6241 ),
 .UNSPECIFIED., .F., .F. ) 
 B_SPLINE_CURVE_WITH_KNOTS ( ( 3, 2, 2, 2, 3 ),
 ( 0.3020833333333333148, 0.3027777777777777568, 0.3041666666666666408, 0.3055555555555555802, 0.3062500000000000222 ),
 .UNSPECIFIED. ) 
 CURVE ( )  GEOMETRIC_REPRESENTATION_ITEM ( )  RATIONAL_B_SPLINE_CURVE ( ( 0.9330127018922194093, 0.9330127018922194093, 1.000000000000000000, 0.8660254037844387076, 1.000000000000000000, 0.8660254037844387076, 1.000000000000000000, 0.9330127018922194093, 0.9330127018922194093 ) ) 
 REPRESENTATION_ITEM ( '' )  );
#28035 = CARTESIAN_POINT ( 'NONE',  ( 4.458734125000000326, 25.10416666803225993, 2.574251347313718519 ) ) ;
#28036 = CARTESIAN_POINT ( 'NONE',  ( -2.229367062500000163, -56.47916666530107221, -3.861377020970580443 ) ) ;
#28037 = CARTESIAN_POINT ( 'NONE',  ( -4.458734124999997661, -2.479166665301069106, 2.574251347313722516 ) ) ;
#28038 = DIRECTION ( 'NONE',  ( -0.000000000000000000, -0.000000000000000000, 1.000000000000000000 ) ) ;
#28039 = CARTESIAN_POINT ( 'NONE',  ( 5.000000000000000000, 8.500000000000000000, -6.123233995736766282E-16 ) ) ;
#28040 = CARTESIAN_POINT ( 'NONE',  ( 3.535533905932738197, -142.0000000027311842, -3.535533905932738197 ) ) ;
#28041 = FACE_OUTER_BOUND ( 'NONE', #17961, .T. ) ;
#28042 = CARTESIAN_POINT ( 'NONE',  ( -4.458734124999999437, -48.31249999863440792, 0.000000000000000000 ) ) ;
#28043 = CARTESIAN_POINT ( 'NONE',  ( -2.499999999999996447, -82.70833333060214443, 4.330127018922195425 ) ) ;
#28044 = CARTESIAN_POINT ( 'NONE',  ( -53.51423613279429503, -134.5000000013656063, 4.591703134518082763 ) ) ;
#28045 = DIRECTION ( 'NONE',  ( 0.000000000000000000, 1.000000000000000000, 0.000000000000000000 ) ) ;
#28046 = FACE_OUTER_BOUND ( 'NONE', #56436, .T. ) ;
#28047 = CARTESIAN_POINT ( 'NONE',  ( 4.458734124999999437, -92.06249999863440792, -5.460374474430324690E-16 ) ) ;
#28048 = CARTESIAN_POINT ( 'NONE',  ( -1.846868145590734756, -156.3750000013655779, -4.458734124999999437 ) ) ;
#28049 = CARTESIAN_POINT ( 'NONE',  ( 5.000000000000000888, -39.58333333333333570, 2.886751345948126879 ) ) ;
#28050 = ORIENTED_EDGE ( 'NONE', *, *, #45176, .T. ) ;
#28051 = EDGE_CURVE ( 'NONE', #34010, #27913, #57844, .T. ) ;
#28052 = CARTESIAN_POINT ( 'NONE',  ( -2.229367062499996610, 18.60416666803225993, 3.861377020970582219 ) ) ;
#28053 = EDGE_CURVE ( 'NONE', #60982, #42868, #33261, .T. ) ;
#28054 = ORIENTED_EDGE ( 'NONE', *, *, #3151, .T. ) ;
#28055 = CARTESIAN_POINT ( 'NONE',  ( -4.458734124999999437, -96.39583333196772230, -2.574251347313719407 ) ) ;
#28056 = CARTESIAN_POINT ( 'NONE',  ( 2.229367062500001939, 6.770833334698928674, 3.861377020970579999 ) ) ;
#28057 = CARTESIAN_POINT ( 'NONE',  ( -4.999999999999999112, 11.20833333606451632, 2.886751345948131764 ) ) ;
#28058 =( BOUNDED_CURVE ( )  B_SPLINE_CURVE ( 2, ( #9747, #10071, #29045, #764, #63485, #48670, #5900, #1090, #44160 ),
 .UNSPECIFIED., .F., .F. ) 
 B_SPLINE_CURVE_WITH_KNOTS ( ( 3, 2, 2, 2, 3 ),
 ( 0.008333333333333340157, 0.01250000000000001110, 0.01666666666666668031, 0.02083333333333334952, 0.02500000000000002220 ),
 .UNSPECIFIED. ) 
 CURVE ( )  GEOMETRIC_REPRESENTATION_ITEM ( )  RATIONAL_B_SPLINE_CURVE ( ( 0.9999999999999998890, 0.9238795325112868495, 1.000000000000000000, 0.9238795325112867385, 1.000000000000000000, 0.9238795325112867385, 1.000000000000000000, 0.9238795325112864054, 1.000000000000000444 ) ) 
 REPRESENTATION_ITEM ( '' )  );
#28059 = CARTESIAN_POINT ( 'NONE',  ( -1.339745962155613812, -35.08034179853028434, -5.000000000000000000 ) ) ;
#28060 = ADVANCED_FACE ( 'NONE', ( #28733 ), #4303, .T. ) ;
#28061 = CARTESIAN_POINT ( 'NONE',  ( 2.499999999999998668, 1.666666666666666963, -4.330127018922193649 ) ) ;
#28062 = CARTESIAN_POINT ( 'NONE',  ( -4.458734124999999437, -63.31249999863440792, 0.000000000000000000 ) ) ;
#28063 = CARTESIAN_POINT ( 'NONE',  ( 1.975475456537005874E-15, 6.375000002731185944, 5.000000000000000000 ) ) ;
#28064 = EDGE_CURVE ( 'NONE', #62355, #50926, #28113, .T. ) ;
#28065 = CARTESIAN_POINT ( 'NONE',  ( -3.152548672688508926E-16, -29.56249999863440436, -5.148502694627439702 ) ) ;
#28066 = CARTESIAN_POINT ( 'NONE',  ( -2.500000000000000444, -38.04166666393548013, -4.330127018922193649 ) ) ;
#28067 = DIRECTION ( 'NONE',  ( -0.000000000000000000, 1.000000000000000000, -0.000000000000000000 ) ) ;
#28068 = DIRECTION ( 'NONE',  ( 0.000000000000000000, 1.000000000000000000, 0.000000000000000000 ) ) ;
#28069 = CARTESIAN_POINT ( 'NONE',  ( 5.000000000000000000, -46.41666666666666430, -2.886751345948129988 ) ) ;
#28070 = CARTESIAN_POINT ( 'NONE',  ( -6.972266317189433020E-16, -21.24999999999999289, -5.000000000000000000 ) ) ;
#28072 = CARTESIAN_POINT ( 'NONE',  ( 9.457646018065525792E-16, -19.31249999863440792, 5.148502694627439702 ) ) ;
#28071 = CARTESIAN_POINT ( 'NONE',  ( 2.499999999999998668, -26.20833333060214798, -4.330127018922193649 ) ) ;
#28073 = CARTESIAN_POINT ( 'NONE',  ( -5.007715329123872641E-16, -8.660254037844399733, -7.422398894150038728 ) ) ;
#28074 = CARTESIAN_POINT ( 'NONE',  ( -4.458734124999999437, -64.31249999863440792, 0.000000000000000000 ) ) ;
#28075 = CARTESIAN_POINT ( 'NONE',  ( 4.458734125000000326, -148.6250000013655779, -1.846868145590734978 ) ) ;
#28076 = CARTESIAN_POINT ( 'NONE',  ( -4.458734124999999437, -77.31249999863440792, 0.000000000000000000 ) ) ;
#28077 = CARTESIAN_POINT ( 'NONE',  ( -59.59170313451811296, -144.7500000013656063, 1.485763867205729394 ) ) ;
#28078 = CARTESIAN_POINT ( 'NONE',  ( 4.458734124999998549, -26.97916666530107221, -2.574251347313721627 ) ) ;
#28079 = CARTESIAN_POINT ( 'NONE',  ( 5.000000000000000000, -68.37499999726881583, -6.123233995736766282E-16 ) ) ;
#28080 = VERTEX_POINT ( 'NONE', #8814 ) ;
#28081 = CARTESIAN_POINT ( 'NONE',  ( 6.123233995736766282E-16, -170.0000000000000000, -5.000000000000000000 ) ) ;
#28082 = ORIENTED_EDGE ( 'NONE', *, *, #2095, .F. ) ;
#28083 = CARTESIAN_POINT ( 'NONE',  ( -2.229367062500000163, -65.72916666530106511, -3.861377020970580443 ) ) ;
#28084 = DIRECTION ( 'NONE',  ( -0.000000000000000000, 1.000000000000000000, -0.000000000000000000 ) ) ;
#28085 = DIRECTION ( 'NONE',  ( 0.000000000000000000, 0.000000000000000000, 1.000000000000000000 ) ) ;
#28086 = ORIENTED_EDGE ( 'NONE', *, *, #24496, .F. ) ;
#28087 = DIRECTION ( 'NONE',  ( -0.000000000000000000, 1.000000000000000000, -0.000000000000000000 ) ) ;
#28088 = CARTESIAN_POINT ( 'NONE',  ( -4.458734124999998549, -53.47916666530106511, 2.574251347313722516 ) ) ;
#28089 = CARTESIAN_POINT ( 'NONE',  ( -2.229367062500000163, 0.2708333346989263979, -3.861377020970580443 ) ) ;
#28090 = ORIENTED_EDGE ( 'NONE', *, *, #54696, .F. ) ;
#28091 = CYLINDRICAL_SURFACE ( 'NONE', #11099, 5.000000000000000000 ) ;
#28092 = CARTESIAN_POINT ( 'NONE',  ( 4.458734124999998549, 4.270833334698926897, -2.574251347313721627 ) ) ;
#28093 = CARTESIAN_POINT ( 'NONE',  ( -2.229367062499996610, 20.85416666803226349, 3.861377020970582219 ) ) ;
#28094 = CARTESIAN_POINT ( 'NONE',  ( -51.60603307380591787, -144.9375000013656063, -2.891590998281053704 ) ) ;
#28095 = CARTESIAN_POINT ( 'NONE',  ( -1.339745962155613812, 5.919658201469705894, -5.000000000000000000 ) ) ;
#28096 = CARTESIAN_POINT ( 'NONE',  ( -8.190561711645485556E-16, -168.6875000013656063, 4.458734124999999437 ) ) ;
#28097 = ORIENTED_EDGE ( 'NONE', *, *, #52242, .F. ) ;
#28098 = CARTESIAN_POINT ( 'NONE',  ( -2.229367062500000163, -76.47916666530106511, -3.861377020970580443 ) ) ;
#28099 = FACE_OUTER_BOUND ( 'NONE', #46207, .T. ) ;
#28100 = CARTESIAN_POINT ( 'NONE',  ( -3.152548672688508926E-16, 5.437500001365592084, -5.148502694627439702 ) ) ;
#28101 = VECTOR ( 'NONE', #26757, 1000.000000000000000 ) ;
#28102 = EDGE_CURVE ( 'NONE', #20861, #53594, #23922, .T. ) ;
#28103 = CYLINDRICAL_SURFACE ( 'NONE', #58312, 5.000000000000000000 ) ;
#28104 = CARTESIAN_POINT ( 'NONE',  ( -3.152548672688508926E-16, -62.81249999863440792, -5.148502694627439702 ) ) ;
#28105 = CARTESIAN_POINT ( 'NONE',  ( -2.499999999999996447, -22.70833333060214443, 4.330127018922195425 ) ) ;
#28106 = CARTESIAN_POINT ( 'NONE',  ( 5.000000000000000000, -20.49999999999999645, -6.123233995736766282E-16 ) ) ;
#28107 = CARTESIAN_POINT ( 'NONE',  ( -6.972266317189433020E-16, -28.12499999726880873, -5.000000000000000000 ) ) ;
#28108 = DIRECTION ( 'NONE',  ( -0.000000000000000000, 1.000000000000000000, -0.000000000000000000 ) ) ;
#28109 = CARTESIAN_POINT ( 'NONE',  ( 2.500000000000002220, -18.54166666393547658, 4.330127018922192761 ) ) ;
#28110 = CARTESIAN_POINT ( 'NONE',  ( 1.975475456537005874E-15, -54.74999999999999289, 5.000000000000000000 ) ) ;
#28111 = CARTESIAN_POINT ( 'NONE',  ( -2.229367062499996610, -40.14583333196773651, 3.861377020970582219 ) ) ;
#28112 = CARTESIAN_POINT ( 'NONE',  ( -2.229367062499996610, -28.39583333196774007, 3.861377020970582219 ) ) ;
#28113 = LINE ( 'NONE', #47730, #42141 ) ;
#28114 = CARTESIAN_POINT ( 'NONE',  ( 1.060575238724906964E-15, 24.24999999999999645, 5.773502691896257311 ) ) ;
#28115 = CARTESIAN_POINT ( 'NONE',  ( -9.184850993605147944E-16, -154.3750000027311842, 5.000000000000000000 ) ) ;
#28116 = ORIENTED_EDGE ( 'NONE', *, *, #22896, .F. ) ;
#28117 = CARTESIAN_POINT ( 'NONE',  ( -2.229367062499996610, -110.3958333319677507, 3.861377020970582219 ) ) ;
#28118 = CARTESIAN_POINT ( 'NONE',  ( -4.458734124999999437, -32.31249999863440792, 0.000000000000000000 ) ) ;
#28119 = CARTESIAN_POINT ( 'NONE',  ( 5.000000000000000000, -70.29166666393547303, -2.886751345948129988 ) ) ;
#28120 = CARTESIAN_POINT ( 'NONE',  ( -59.59170313451811296, -148.7500000013655779, 1.485763867205729394 ) ) ;
#28121 = CARTESIAN_POINT ( 'NONE',  ( 2.071067811865476394, -148.1875000000000000, 5.000000000000000000 ) ) ;
#28122 = CARTESIAN_POINT ( 'NONE',  ( -2.229367062500000163, -28.47916666530107221, -3.861377020970580443 ) ) ;
#28123 = CARTESIAN_POINT ( 'NONE',  ( 2.229367062499998831, -76.89583333196773651, -3.861377020970580887 ) ) ;
#28124 = CARTESIAN_POINT ( 'NONE',  ( -8.190561711645485556E-16, -167.9375000013655779, 4.458734124999999437 ) ) ;
#28125 = CARTESIAN_POINT ( 'NONE',  ( 4.458734125000000326, -28.89583333196774007, 2.574251347313718519 ) ) ;
#28126 = CARTESIAN_POINT ( 'NONE',  ( -55.39835681537999790, -136.0000000027312126, 4.984105922594378235 ) ) ;
#28127 = DIRECTION ( 'NONE',  ( -0.000000000000000000, -1.000000000000000000, -0.000000000000000000 ) ) ;
#28128 = CARTESIAN_POINT ( 'NONE',  ( -4.999999999999999112, -18.91666666666666430, 2.886751345948131764 ) ) ;
#28129 = CARTESIAN_POINT ( 'NONE',  ( -4.458734125000001214, -147.8750000013656063, 1.846868145590734089 ) ) ;
#28130 = ORIENTED_EDGE ( 'NONE', *, *, #18075, .F. ) ;
#28131 = LINE ( 'NONE', #57110, #60529 ) ;
#28132 = CARTESIAN_POINT ( 'NONE',  ( -2.229367062500000163, -55.72916666530107221, -3.861377020970580443 ) ) ;
#28133 = CARTESIAN_POINT ( 'NONE',  ( 2.500000000000002220, 28.45833333606451987, 4.330127018922192761 ) ) ;
#28134 = CARTESIAN_POINT ( 'NONE',  ( 5.000000000000000888, -81.45833333060213022, 2.886751345948126879 ) ) ;
#28135 = CARTESIAN_POINT ( 'NONE',  ( 5.000000000000000888, 19.41666666666666075, 2.886751345948126879 ) ) ;
#28136 =( BOUNDED_CURVE ( )  B_SPLINE_CURVE ( 2, ( #27764, #53158, #38363, #43492, #38665, #13611, #14225, #24199, #33542 ),
 .UNSPECIFIED., .F., .F. ) 
 B_SPLINE_CURVE_WITH_KNOTS ( ( 3, 2, 2, 2, 3 ),
 ( 0.8732142857142857206, 0.8738095238095238138, 0.8750000000000000000, 0.8761904761904761862, 0.8767857142857142794 ),
 .UNSPECIFIED. ) 
 CURVE ( )  GEOMETRIC_REPRESENTATION_ITEM ( )  RATIONAL_B_SPLINE_CURVE ( ( 0.9330127018922194093, 0.9330127018922194093, 1.000000000000000000, 0.8660254037844387076, 1.000000000000000000, 0.8660254037844387076, 1.000000000000000000, 0.9330127018922194093, 0.9330127018922194093 ) ) 
 REPRESENTATION_ITEM ( '' )  );
#28137 = CARTESIAN_POINT ( 'NONE',  ( 6.123233995736766282E-16, -170.0000000000000000, -5.000000000000000000 ) ) ;
#28138 = CARTESIAN_POINT ( 'NONE',  ( 4.458734125000001214, 1.104166668032261711, 2.574251347313718519 ) ) ;
#28139 = CARTESIAN_POINT ( 'NONE',  ( 1.339745962155615144, -48.70534180126148271, 4.999999999999999112 ) ) ;
#28140 = CARTESIAN_POINT ( 'NONE',  ( 0.000000000000000000, -170.0000000000000000, 0.000000000000000000 ) ) ;
#28141 = CARTESIAN_POINT ( 'NONE',  ( 2.229367062499998831, 10.10416666803225993, -3.861377020970580887 ) ) ;
#28142 = VERTEX_POINT ( 'NONE', #1087 ) ;
#28143 = CARTESIAN_POINT ( 'NONE',  ( -6.972266317189433020E-16, -39.25000000000000000, -5.000000000000000000 ) ) ;
#28144 = VERTEX_POINT ( 'NONE', #4932 ) ;
#28145 = CARTESIAN_POINT ( 'NONE',  ( 0.000000000000000000, -120.0000000000000000, 0.000000000000000000 ) ) ;
#28146 = CARTESIAN_POINT ( 'NONE',  ( -2.229367062500000163, -49.47916666530107221, -3.861377020970580443 ) ) ;
#28147 = CARTESIAN_POINT ( 'NONE',  ( -3.152801135295367096, -159.3125000013656063, -3.152801135295367541 ) ) ;
#28148 = VECTOR ( 'NONE', #29409, 1000.000000000000000 ) ;
#28149 =( BOUNDED_CURVE ( )  B_SPLINE_CURVE ( 2, ( #47599, #28605, #38270, #23482, #57894, #43703, #33437, #43085, #13818 ),
 .UNSPECIFIED., .F., .F. ) 
 B_SPLINE_CURVE_WITH_KNOTS ( ( 3, 2, 2, 2, 3 ),
 ( 0.1395833333333333370, 0.1402777777777777790, 0.1416666666666666630, 0.1430555555555555469, 0.1437499999999999889 ),
 .UNSPECIFIED. ) 
 CURVE ( )  GEOMETRIC_REPRESENTATION_ITEM ( )  RATIONAL_B_SPLINE_CURVE ( ( 0.9330127018922194093, 0.9330127018922194093, 1.000000000000000000, 0.8660254037844387076, 1.000000000000000000, 0.8660254037844387076, 1.000000000000000000, 0.9330127018922194093, 0.9330127018922194093 ) ) 
 REPRESENTATION_ITEM ( '' )  );
#28150 = CARTESIAN_POINT ( 'NONE',  ( -5.000000000000000000, -47.87499999726880873, 0.000000000000000000 ) ) ;
#28151 = EDGE_LOOP ( 'NONE', ( #21231, #57660, #30225, #63141 ) ) ;
#28152 = CARTESIAN_POINT ( 'NONE',  ( -2.229367062500000163, -22.47916666530107221, -3.861377020970580443 ) ) ;
#28153 = ORIENTED_EDGE ( 'NONE', *, *, #24234, .T. ) ;
#28155 = CARTESIAN_POINT ( 'NONE',  ( -2.071067811865562991, -142.4375000027312126, 4.999999999999913847 ) ) ;
#28154 = CARTESIAN_POINT ( 'NONE',  ( 1.975475456537005874E-15, 21.24999999999999289, 5.000000000000000000 ) ) ;
#28156 = CARTESIAN_POINT ( 'NONE',  ( -4.458734124999999437, -160.9375000013655779, -5.460374474430324690E-16 ) ) ;
#28157 = DIRECTION ( 'NONE',  ( -0.000000000000000000, 1.000000000000000000, -0.000000000000000000 ) ) ;
#28158 = CARTESIAN_POINT ( 'NONE',  ( -52.53715891517739323, -138.4375000000000000, -4.819101127000233298 ) ) ;
#28159 = EDGE_CURVE ( 'NONE', #859, #57124, #18383, .T. ) ;
#28160 = CARTESIAN_POINT ( 'NONE',  ( 9.457646018065525792E-16, -38.31249999863441502, 5.148502694627439702 ) ) ;
#28161 = EDGE_LOOP ( 'NONE', ( #52852, #39183, #25549, #22675 ) ) ;
#28162 = CARTESIAN_POINT ( 'NONE',  ( -4.458734124999999437, -83.39583333196772230, -2.574251347313719407 ) ) ;
#28163 = CARTESIAN_POINT ( 'NONE',  ( 9.457646018065525792E-16, 23.93750000136559564, 5.148502694627439702 ) ) ;
#28164 = CARTESIAN_POINT ( 'NONE',  ( 0.000000000000000000, -120.0000000000000000, 5.000000000000000000 ) ) ;
#28165 = ORIENTED_EDGE ( 'NONE', *, *, #58181, .F. ) ;
#28166 = CARTESIAN_POINT ( 'NONE',  ( -53.51423613279429503, -138.5000000013656063, 4.591703134518083651 ) ) ;
#28167 = CARTESIAN_POINT ( 'NONE',  ( -2.229367062499996610, -86.39583333196773651, 3.861377020970582219 ) ) ;
#28168 = CARTESIAN_POINT ( 'NONE',  ( -60.14911071818854538, -128.1875000027312410, 1.666127454062681368 ) ) ;
#28169 = DIRECTION ( 'NONE',  ( 0.000000000000000000, 0.000000000000000000, 1.000000000000000000 ) ) ;
#28170 = CARTESIAN_POINT ( 'NONE',  ( 5.000000000000000000, -57.41666666666667140, -2.886751345948130876 ) ) ;
#28171 = CARTESIAN_POINT ( 'NONE',  ( -4.458734124999999437, -60.31249999863440081, 0.000000000000000000 ) ) ;
#28172 = CARTESIAN_POINT ( 'NONE',  ( -53.33387254593728954, -150.9375000027311842, 5.149110718188522284 ) ) ;
#28173 = CARTESIAN_POINT ( 'NONE',  ( -3.152548672688508926E-16, 23.43750000136559564, -5.148502694627439702 ) ) ;
#28174 = CARTESIAN_POINT ( 'NONE',  ( 0.000000000000000000, -170.0000000000000000, 0.000000000000000000 ) ) ;
#28175 = CARTESIAN_POINT ( 'NONE',  ( -7.922281120364393914, -4.573931137438277617, -8.047472243342932430 ) ) ;
#28176 = CARTESIAN_POINT ( 'NONE',  ( -2.229367062500000163, -41.72916666530107932, -3.861377020970580443 ) ) ;
#28177 = CARTESIAN_POINT ( 'NONE',  ( 1.060575238724906964E-15, -6.624999997268813168, 5.773502691896257311 ) ) ;
#28178 = CARTESIAN_POINT ( 'NONE',  ( 5.000000000000000888, -31.58333333333333215, 2.886751345948126879 ) ) ;
#28179 = CARTESIAN_POINT ( 'NONE',  ( -50.70258187064364108, -125.1250000013656205, 2.196230717870141014 ) ) ;
#28180 = CARTESIAN_POINT ( 'NONE',  ( 4.458734125000001214, -87.14583333196772230, 2.574251347313718519 ) ) ;
#28181 = CARTESIAN_POINT ( 'NONE',  ( 2.229367062499998831, -104.6458333319677365, -3.861377020970580887 ) ) ;
#28182 = CARTESIAN_POINT ( 'NONE',  ( 4.458734124999999437, -10.06249999863440614, -5.460374474430324690E-16 ) ) ;
#28183 = EDGE_LOOP ( 'NONE', ( #2008, #63517, #13344, #51970 ) ) ;
#28184 = CARTESIAN_POINT ( 'NONE',  ( -3.535533905932738641, -155.5000000027312126, 3.535533905932737309 ) ) ;
#28185 = CARTESIAN_POINT ( 'NONE',  ( -3.152548672688508926E-16, -95.56249999863442213, -5.148502694627439702 ) ) ;
#28186 = CARTESIAN_POINT ( 'NONE',  ( 5.000000000000000888, -166.0625000027312410, -2.071067811865475505 ) ) ;
#28187 = CARTESIAN_POINT ( 'NONE',  ( 2.229367062499998831, -93.89583333196772230, -3.861377020970580887 ) ) ;
#28188 = CARTESIAN_POINT ( 'NONE',  ( -2.499999999999996447, -51.70833333060213732, 4.330127018922195425 ) ) ;
#28189 = CARTESIAN_POINT ( 'NONE',  ( 1.975475456537005874E-15, 10.37500000273118417, 5.000000000000000000 ) ) ;
#28190 = AXIS2_PLACEMENT_3D ( 'NONE', #31960, #36471, #57059 ) ;
#28191 = CARTESIAN_POINT ( 'NONE',  ( -51.60603307380591787, -129.9375000013656063, -2.891590998281053704 ) ) ;
#28192 = CARTESIAN_POINT ( 'NONE',  ( -4.458734124999997661, -11.22916666530107044, 2.574251347313722516 ) ) ;
#28193 = CARTESIAN_POINT ( 'NONE',  ( 4.458734124999999437, 11.93750000136559564, -5.460374474430324690E-16 ) ) ;
#28194 = CARTESIAN_POINT ( 'NONE',  ( -2.229367062500000163, -55.72916666530107221, -3.861377020970580443 ) ) ;
#28195 = CARTESIAN_POINT ( 'NONE',  ( 0.000000000000000000, 0.000000000000000000, 0.000000000000000000 ) ) ;
#28196 = CARTESIAN_POINT ( 'NONE',  ( 0.000000000000000000, -170.0000000000000000, 5.000000000000000000 ) ) ;
#28197 = CARTESIAN_POINT ( 'NONE',  ( -3.152548672688508926E-16, -14.56249999863440259, -5.148502694627439702 ) ) ;
#28198 = CARTESIAN_POINT ( 'NONE',  ( -55.39835672516371545, -134.9999999999999716, 4.984105929804953483 ) ) ;
#28199 = ORIENTED_EDGE ( 'NONE', *, *, #57550, .F. ) ;
#28200 = CARTESIAN_POINT ( 'NONE',  ( -2.229367062500000163, -39.72916666530107221, -3.861377020970580443 ) ) ;
#28201 =( BOUNDED_CURVE ( )  B_SPLINE_CURVE ( 2, ( #6404, #40476, #46265, #1585, #21185, #2224, #13118, #37558, #42377 ),
 .UNSPECIFIED., .F., .F. ) 
 B_SPLINE_CURVE_WITH_KNOTS ( ( 3, 2, 2, 2, 3 ),
 ( 0.7979166666666667185, 0.7986111111111111605, 0.8000000000000000444, 0.8013888888888889284, 0.8020833333333333703 ),
 .UNSPECIFIED. ) 
 CURVE ( )  GEOMETRIC_REPRESENTATION_ITEM ( )  RATIONAL_B_SPLINE_CURVE ( ( 0.9330127018922194093, 0.9330127018922194093, 1.000000000000000000, 0.8660254037844387076, 1.000000000000000000, 0.8660254037844387076, 1.000000000000000000, 0.9330127018922194093, 0.9330127018922194093 ) ) 
 REPRESENTATION_ITEM ( '' )  );
#28202 = CYLINDRICAL_SURFACE ( 'NONE', #30475, 5.000000000000000000 ) ;
#28203 = CARTESIAN_POINT ( 'NONE',  ( 1.975475456537005874E-15, -8.750000000000000000, 5.000000000000000000 ) ) ;
#28204 = DIRECTION ( 'NONE',  ( -0.000000000000000000, 1.000000000000000000, -0.000000000000000000 ) ) ;
#28205 = CARTESIAN_POINT ( 'NONE',  ( -4.458734124999999437, -86.39583333196772230, -2.574251347313719407 ) ) ;
#28206 = CARTESIAN_POINT ( 'NONE',  ( -4.458734124999999437, 24.43750000136559208, 0.000000000000000000 ) ) ;
#28207 = CARTESIAN_POINT ( 'NONE',  ( 9.457646018065525792E-16, 15.93750000136559564, 5.148502694627439702 ) ) ;
#28208 = DIRECTION ( 'NONE',  ( 0.000000000000000000, 1.000000000000000000, 0.000000000000000000 ) ) ;
#28209 = CARTESIAN_POINT ( 'NONE',  ( -5.000000000000000000, -64.87499999726881583, 0.000000000000000000 ) ) ;
#28210 = CARTESIAN_POINT ( 'NONE',  ( 4.458734124999998549, -84.97916666530107932, -2.574251347313721627 ) ) ;
#28211 = CARTESIAN_POINT ( 'NONE',  ( -3.535250795749689387E-16, -69.24999999999998579, -5.773502691896257311 ) ) ;
#28212 = CARTESIAN_POINT ( 'NONE',  ( 2.500000000000002220, 12.45833333606451809, 4.330127018922192761 ) ) ;
#28213 = ORIENTED_EDGE ( 'NONE', *, *, #1370, .T. ) ;
#28214 = CARTESIAN_POINT ( 'NONE',  ( -6.972266317189433020E-16, -18.12499999726881228, -5.000000000000000000 ) ) ;
#28215 = CARTESIAN_POINT ( 'NONE',  ( -5.000000000000000000, 16.00000000000000000, 0.000000000000000000 ) ) ;
#28217 = CARTESIAN_POINT ( 'NONE',  ( 1.060575238724906964E-15, -27.74999999999999645, 5.773502691896257311 ) ) ;
#28216 = CARTESIAN_POINT ( 'NONE',  ( 5.000000000000000888, -40.58333333333334281, 2.886751345948126879 ) ) ;
#28218 = CARTESIAN_POINT ( 'NONE',  ( -2.229367062499996610, -32.14583333196773651, 3.861377020970582219 ) ) ;
#28219 = CARTESIAN_POINT ( 'NONE',  ( 5.000000000000000000, 18.50000000000000000, -6.123233995736766282E-16 ) ) ;
#28220 = CARTESIAN_POINT ( 'NONE',  ( 5.000000000000000000, -35.29166666393547303, -2.886751345948129988 ) ) ;
#28222 = ORIENTED_EDGE ( 'NONE', *, *, #814, .F. ) ;
#28221 = CARTESIAN_POINT ( 'NONE',  ( -2.229367062500000163, -61.47916666530106511, -3.861377020970580443 ) ) ;
#28223 = CARTESIAN_POINT ( 'NONE',  ( -54.64476657466781973, -150.0625000013656063, -4.444560631937228834 ) ) ;
#28225 = ORIENTED_EDGE ( 'NONE', *, *, #12141, .F. ) ;
#28224 = CARTESIAN_POINT ( 'NONE',  ( -2.229367062500000163, -7.729166665301073991, -3.861377020970580443 ) ) ;
#28226 = CARTESIAN_POINT ( 'NONE',  ( -3.535250795749689387E-16, -77.25000000000000000, -5.773502691896257311 ) ) ;
#28227 = CARTESIAN_POINT ( 'NONE',  ( -57.89159099828107458, -136.6875000013656063, -3.393966926194107447 ) ) ;
#28228 = CARTESIAN_POINT ( 'NONE',  ( 2.229367062500001939, -55.22916666530107221, 3.861377020970579999 ) ) ;
#28229 =( BOUNDED_CURVE ( )  B_SPLINE_CURVE ( 2, ( #40471, #61383, #45624, #61069, #16990, #1267, #1579, #35661, #22138 ),
 .UNSPECIFIED., .F., .F. ) 
 B_SPLINE_CURVE_WITH_KNOTS ( ( 3, 2, 2, 2, 3 ),
 ( 0.8020833333333333703, 0.8027777777777778123, 0.8041666666666666963, 0.8055555555555555802, 0.8062500000000000222 ),
 .UNSPECIFIED. ) 
 CURVE ( )  GEOMETRIC_REPRESENTATION_ITEM ( )  RATIONAL_B_SPLINE_CURVE ( ( 0.9330127018922194093, 0.9330127018922194093, 1.000000000000000000, 0.8660254037844387076, 1.000000000000000000, 0.8660254037844387076, 1.000000000000000000, 0.9330127018922194093, 0.9330127018922194093 ) ) 
 REPRESENTATION_ITEM ( '' )  );
#28230 = CARTESIAN_POINT ( 'NONE',  ( 5.000000000000000888, -75.45833333060214443, 2.886751345948126879 ) ) ;
#28232 = VERTEX_POINT ( 'NONE', #24552 ) ;
#28231 = CARTESIAN_POINT ( 'NONE',  ( 1.339745962155612702, -13.29465819873852084, -5.000000000000000000 ) ) ;
#28233 = CARTESIAN_POINT ( 'NONE',  ( -50.18089887299979068, -149.6875000000000284, 2.462841084822635640 ) ) ;
#28234 = ADVANCED_FACE ( 'NONE', ( #20695 ), #30646, .T. ) ;
#28235 = CARTESIAN_POINT ( 'NONE',  ( 4.458734125000001214, -23.14583333196773651, 2.574251347313718519 ) ) ;
#28237 = ORIENTED_EDGE ( 'NONE', *, *, #31900, .T. ) ;
#28236 = CARTESIAN_POINT ( 'NONE',  ( -2.229367062499996610, -54.39583333196773651, 3.861377020970582219 ) ) ;
#28238 = AXIS2_PLACEMENT_3D ( 'NONE', #13297, #58547, #39861 ) ;
#28239 = CARTESIAN_POINT ( 'NONE',  ( 0.000000000000000000, 0.000000000000000000, 0.000000000000000000 ) ) ;
#28240 = CARTESIAN_POINT ( 'NONE',  ( -8.190561711645485556E-16, -166.9375000013655779, 4.458734124999999437 ) ) ;
#28241 = CARTESIAN_POINT ( 'NONE',  ( -3.152548672688508926E-16, -99.81249999863442213, -5.148502694627439702 ) ) ;
#28242 = CARTESIAN_POINT ( 'NONE',  ( -1.339745962155669101, -26.66965819600733667, 4.999999999999966249 ) ) ;
#28243 = ORIENTED_EDGE ( 'NONE', *, *, #13736, .F. ) ;
#28244 = CARTESIAN_POINT ( 'NONE',  ( -54.64476657466781973, -150.0625000013656063, -4.444560631937228834 ) ) ;
#28245 = CARTESIAN_POINT ( 'NONE',  ( -57.46284108482265651, -143.0625000027312126, 4.819101127000239515 ) ) ;
#28246 = CARTESIAN_POINT ( 'NONE',  ( -2.499999999999996447, 1.291666669397853351, 4.330127018922195425 ) ) ;
#28247 = CARTESIAN_POINT ( 'NONE',  ( 4.458734124999999437, -9.812499998634406140, -5.460374474430324690E-16 ) ) ;
#28248 = CARTESIAN_POINT ( 'NONE',  ( -2.229367062500000163, -101.7291666653010651, -3.861377020970580443 ) ) ;
#28249 = ADVANCED_FACE ( 'NONE', ( #45122 ), #44156, .T. ) ;
#28250 = CARTESIAN_POINT ( 'NONE',  ( 4.458734124999999437, -144.7500000013656063, 1.846868145590737864 ) ) ;
#28251 = CARTESIAN_POINT ( 'NONE',  ( 9.457646018065525792E-16, -28.31249999863440081, 5.148502694627439702 ) ) ;
#28252 = EDGE_CURVE ( 'NONE', #24591, #53169, #734, .T. ) ;
#28253 = CARTESIAN_POINT ( 'NONE',  ( -58.24261429053147765, -139.3750000027312126, -3.805975901505573855 ) ) ;
#28254 = CARTESIAN_POINT ( 'NONE',  ( -54.64476657466781973, -135.8125000013656063, -4.444560631937228834 ) ) ;
#28255 = CARTESIAN_POINT ( 'NONE',  ( -3.152548672688508926E-16, -70.81249999863440792, -5.148502694627439702 ) ) ;
#28256 = CARTESIAN_POINT ( 'NONE',  ( 0.000000000000000000, -120.0000000000000000, 0.000000000000000000 ) ) ;
#28257 = DIRECTION ( 'NONE',  ( 0.000000000000000000, 0.000000000000000000, 1.000000000000000000 ) ) ;
#28258 = CARTESIAN_POINT ( 'NONE',  ( -8.190561711645485556E-16, -139.6875000013656063, 4.458734124999999437 ) ) ;
#28259 = CARTESIAN_POINT ( 'NONE',  ( 9.457646018065525792E-16, 7.687500001365596525, 5.148502694627439702 ) ) ;
#28260 = EDGE_LOOP ( 'NONE', ( #56490, #5778, #11098, #14617 ) ) ;
#28261 = CARTESIAN_POINT ( 'NONE',  ( 0.000000000000000000, 0.000000000000000000, -9.999999999999998224 ) ) ;
#28262 = CARTESIAN_POINT ( 'NONE',  ( 5.000000000000000000, 9.583333333333332149, -2.886751345948130876 ) ) ;
#28264 = CARTESIAN_POINT ( 'NONE',  ( 4.458734124999999437, -26.81249999863440081, -5.460374474430324690E-16 ) ) ;
#28263 = CARTESIAN_POINT ( 'NONE',  ( -5.000000000000000000, -90.08333333333332860, -2.886751345948128211 ) ) ;
#28265 = DIRECTION ( 'NONE',  ( -0.000000000000000000, 1.000000000000000000, -0.000000000000000000 ) ) ;
#28266 = CARTESIAN_POINT ( 'NONE',  ( -3.152548672688508926E-16, -76.81249999863440792, -5.148502694627439702 ) ) ;
#28267 = CARTESIAN_POINT ( 'NONE',  ( 4.458734125000000326, 22.85416666803225993, 2.574251347313718519 ) ) ;
#28268 = EDGE_CURVE ( 'NONE', #62891, #3107, #45443, .T. ) ;
#28269 = CARTESIAN_POINT ( 'NONE',  ( -57.89159099828107458, -141.6875000013656063, -3.393966926194107447 ) ) ;
#28270 = CARTESIAN_POINT ( 'NONE',  ( -4.458734124999997661, 2.770833334698928674, 2.574251347313722516 ) ) ;
#28271 = CARTESIAN_POINT ( 'NONE',  ( 2.229367062500001939, 28.77083333469892779, 3.861377020970579999 ) ) ;
#28272 = CARTESIAN_POINT ( 'NONE',  ( -4.458734124999999437, -37.56249999863440792, 0.000000000000000000 ) ) ;
#28273 = CARTESIAN_POINT ( 'NONE',  ( -54.60164318462004474, -144.3750000000000284, -4.984105922594373794 ) ) ;
#28274 = CARTESIAN_POINT ( 'NONE',  ( -3.152548672688508926E-16, 4.437500001365595637, -5.148502694627439702 ) ) ;
#28275 = AXIS2_PLACEMENT_3D ( 'NONE', #31326, #2098, #21700 ) ;
#28276 = CARTESIAN_POINT ( 'NONE',  ( -4.458734124999999437, -70.39583333196773651, -2.574251347313719407 ) ) ;
#28277 = CARTESIAN_POINT ( 'NONE',  ( 9.457646018065525792E-16, -22.31249999863440792, 5.148502694627439702 ) ) ;
#28278 = CARTESIAN_POINT ( 'NONE',  ( 2.730187237215162345E-16, -156.1875000013655779, -4.458734124999999437 ) ) ;
#28279 = CARTESIAN_POINT ( 'NONE',  ( 4.458734124999998549, -63.72916666530107221, -2.574251347313721627 ) ) ;
#28280 = CARTESIAN_POINT ( 'NONE',  ( -2.500000000000000444, -99.04166666393545881, -4.330127018922193649 ) ) ;
#28281 = AXIS2_PLACEMENT_3D ( 'NONE', #33928, #24597, #10117 ) ;
#28282 = CARTESIAN_POINT ( 'NONE',  ( -4.458734124999999437, 28.68750000136559208, 0.000000000000000000 ) ) ;
#28283 = CARTESIAN_POINT ( 'NONE',  ( -2.229367062500000163, -41.47916666530107932, -3.861377020970580443 ) ) ;
#28284 = CARTESIAN_POINT ( 'NONE',  ( -4.999999999999998224, -83.91666666666667140, 2.886751345948131764 ) ) ;
#28285 = ADVANCED_FACE ( 'NONE', ( #126 ), #1407, .F. ) ;
#28286 = CARTESIAN_POINT ( 'NONE',  ( 4.458734124999998549, -103.9791666653010509, -2.574251347313721627 ) ) ;
#28287 = CARTESIAN_POINT ( 'NONE',  ( -4.458734124999997661, -69.47916666530107932, 2.574251347313722516 ) ) ;
#28288 = CARTESIAN_POINT ( 'NONE',  ( -5.000000000000000000, -52.99999999999999289, 0.000000000000000000 ) ) ;
#28289 = CARTESIAN_POINT ( 'NONE',  ( 1.975475456537005874E-15, -72.62499999726878741, 5.000000000000000000 ) ) ;
#28290 = DIRECTION ( 'NONE',  ( -0.000000000000000000, 1.000000000000000000, -0.000000000000000000 ) ) ;
#28291 = ORIENTED_EDGE ( 'NONE', *, *, #40167, .F. ) ;
#28292 = CARTESIAN_POINT ( 'NONE',  ( -2.500000000000000444, 14.95833333606451809, -4.330127018922193649 ) ) ;
#28293 = CARTESIAN_POINT ( 'NONE',  ( 5.000000000000000000, 2.625000002731185500, -6.123233995736766282E-16 ) ) ;
#28294 = CARTESIAN_POINT ( 'NONE',  ( 1.060575238724906964E-15, -10.75000000000000178, 5.773502691896257311 ) ) ;
#28295 = CARTESIAN_POINT ( 'NONE',  ( 9.457646018065525792E-16, -19.06249999863440792, 5.148502694627439702 ) ) ;
#28296 = CARTESIAN_POINT ( 'NONE',  ( 9.457646018065525792E-16, -79.06249999863440792, 5.148502694627439702 ) ) ;
#28297 = CARTESIAN_POINT ( 'NONE',  ( 5.000000000000000000, -59.29166666393547303, -2.886751345948130876 ) ) ;
#28298 = CARTESIAN_POINT ( 'NONE',  ( 2.499999999999998668, -15.20833333060214443, -4.330127018922193649 ) ) ;
#28300 = ORIENTED_EDGE ( 'NONE', *, *, #31974, .F. ) ;
#28299 = CARTESIAN_POINT ( 'NONE',  ( -4.458734124999999437, -42.31249999863440081, 0.000000000000000000 ) ) ;
#28301 = DIRECTION ( 'NONE',  ( -0.000000000000000000, 1.000000000000000000, -0.000000000000000000 ) ) ;
#28303 = VERTEX_POINT ( 'NONE', #10068 ) ;
#28302 = CARTESIAN_POINT ( 'NONE',  ( -2.229367062500000163, 6.270833334698928674, -3.861377020970580443 ) ) ;
#28304 = CARTESIAN_POINT ( 'NONE',  ( -2.499999999999996447, -59.83333333333333570, 4.330127018922195425 ) ) ;
#28305 = CARTESIAN_POINT ( 'NONE',  ( -4.458734125000000326, -158.2500000013656063, -1.846868145590735644 ) ) ;
#28306 = CARTESIAN_POINT ( 'NONE',  ( 4.458734124999998549, -36.97916666530107221, -2.574251347313721627 ) ) ;
#28307 = CARTESIAN_POINT ( 'NONE',  ( -56.66612745406278151, -149.4375000027312410, -5.149110718188523173 ) ) ;
#28308 = CARTESIAN_POINT ( 'NONE',  ( 5.000000000000000888, -166.9375000000000284, -2.071067811865475505 ) ) ;
#28309 = CARTESIAN_POINT ( 'NONE',  ( 3.061616997868383141E-16, -167.7500000000000000, -5.000000000000000000 ) ) ;
#28310 = CARTESIAN_POINT ( 'NONE',  ( -50.70258187064364108, -130.3750000013656631, 2.196230717870141014 ) ) ;
#28311 = EDGE_CURVE ( 'NONE', #42248, #43569, #48983, .T. ) ;
#28312 = CARTESIAN_POINT ( 'NONE',  ( -2.229367062500000163, -3.729166665301070438, -3.861377020970580443 ) ) ;
#28313 = CARTESIAN_POINT ( 'NONE',  ( -4.458734124999999437, -38.56249999863440081, 0.000000000000000000 ) ) ;
#28314 = EDGE_CURVE ( 'NONE', #30756, #52679, #24954, .T. ) ;
#28315 = EDGE_CURVE ( 'NONE', #11358, #8866, #40168, .T. ) ;
#28316 = CARTESIAN_POINT ( 'NONE',  ( 1.975475456537005874E-15, -54.74999999999999289, 5.000000000000000000 ) ) ;
#28317 = CARTESIAN_POINT ( 'NONE',  ( -8.190561711645485556E-16, -153.6875000013656063, 4.458734124999999437 ) ) ;
#28318 = CARTESIAN_POINT ( 'NONE',  ( -2.229367062499996610, -83.39583333196773651, 3.861377020970582219 ) ) ;
#28319 = CARTESIAN_POINT ( 'NONE',  ( 5.000000000000000000, -167.1250000027312126, 0.000000000000000000 ) ) ;
#28320 = ORIENTED_EDGE ( 'NONE', *, *, #36538, .T. ) ;
#28321 = CARTESIAN_POINT ( 'NONE',  ( -2.071067811865604735, -148.4375000027312410, 4.999999999999872990 ) ) ;
#28322 = CARTESIAN_POINT ( 'NONE',  ( 1.975475456537005874E-15, -2.624999997268813168, 5.000000000000000000 ) ) ;
#28323 = CARTESIAN_POINT ( 'NONE',  ( 2.229367062500001939, -69.22916666530107932, 3.861377020970579999 ) ) ;
#28324 = CARTESIAN_POINT ( 'NONE',  ( -8.190561711645485556E-16, -144.9375000013656063, 4.458734124999999437 ) ) ;
#28325 = ORIENTED_EDGE ( 'NONE', *, *, #60075, .T. ) ;
#28326 = ADVANCED_FACE ( 'NONE', ( #2658 ), #7173, .F. ) ;
#28327 =( BOUNDED_CURVE ( )  B_SPLINE_CURVE ( 2, ( #47721, #62847, #34184, #18761, #48037, #38386, #24223, #19070, #62541 ),
 .UNSPECIFIED., .F., .F. ) 
 B_SPLINE_CURVE_WITH_KNOTS ( ( 3, 2, 2, 2, 3 ),
 ( 0.4250000000000003220, 0.4291666666666669738, 0.4333333333333336812, 0.4375000000000003886, 0.4416666666666670404 ),
 .UNSPECIFIED. ) 
 CURVE ( )  GEOMETRIC_REPRESENTATION_ITEM ( )  RATIONAL_B_SPLINE_CURVE ( ( 0.9999999999999938938, 0.9238795325112928447, 1.000000000000000000, 0.9238795325112867385, 1.000000000000000000, 0.9238795325112867385, 1.000000000000000000, 0.9238795325112796331, 1.000000000000007105 ) ) 
 REPRESENTATION_ITEM ( '' )  );
#28328 = CARTESIAN_POINT ( 'NONE',  ( 5.000000000000000000, -78.41666666666667140, -2.886751345948130876 ) ) ;
#28329 = CARTESIAN_POINT ( 'NONE',  ( 9.457646018065525792E-16, -11.31249999863440792, 5.148502694627439702 ) ) ;
#28330 = EDGE_CURVE ( 'NONE', #49599, #60646, #12616, .T. ) ;
#28331 = CARTESIAN_POINT ( 'NONE',  ( -55.00000000000002132, -155.0000000000000284, 1.734723475976807094E-15 ) ) ;
#28332 = CARTESIAN_POINT ( 'NONE',  ( 9.457646018065525792E-16, 4.937500001365596525, 5.148502694627439702 ) ) ;
#28333 = CARTESIAN_POINT ( 'NONE',  ( -1.339745962155610925, -79.79465819873850307, 5.000000000000000000 ) ) ;
#28334 = CARTESIAN_POINT ( 'NONE',  ( 4.458734124999997661, -151.5000000013655779, 1.846868145590737864 ) ) ;
#28335 = CARTESIAN_POINT ( 'NONE',  ( -3.152548672688508926E-16, 24.18750000136559564, -5.148502694627439702 ) ) ;
#28336 = ORIENTED_EDGE ( 'NONE', *, *, #41666, .F. ) ;
#28337 = CARTESIAN_POINT ( 'NONE',  ( -2.229367062499996610, -91.14583333196773651, 3.861377020970582219 ) ) ;
#28338 = CARTESIAN_POINT ( 'NONE',  ( -1.339745962155564296, -25.20534180126148271, -5.000000000000028422 ) ) ;
#28339 = CARTESIAN_POINT ( 'NONE',  ( -4.458734124999999437, -7.312499998634404363, 0.000000000000000000 ) ) ;
#28340 = CYLINDRICAL_SURFACE ( 'NONE', #24194, 5.000000000000000000 ) ;
#28341 = CARTESIAN_POINT ( 'NONE',  ( -57.19623071787017210, -152.3750000013656063, 4.297418129356382899 ) ) ;
#28342 = CARTESIAN_POINT ( 'NONE',  ( 5.000000000000000000, -38.37499999726881583, -6.123233995736766282E-16 ) ) ;
#28343 = DIRECTION ( 'NONE',  ( -0.000000000000000000, 1.000000000000000000, -0.000000000000000000 ) ) ;
#28344 = CARTESIAN_POINT ( 'NONE',  ( 2.229367062499998831, 18.35416666803225993, -3.861377020970580887 ) ) ;
#28345 = CARTESIAN_POINT ( 'NONE',  ( -4.999999999999998224, -71.91666666666667140, 2.886751345948131764 ) ) ;
#28346 = CARTESIAN_POINT ( 'NONE',  ( -4.458734124999997661, 22.77083333469892068, 2.574251347313722516 ) ) ;
#28347 = CARTESIAN_POINT ( 'NONE',  ( 4.458734124999998549, -55.72916666530107221, -2.574251347313721627 ) ) ;
#28348 = CARTESIAN_POINT ( 'NONE',  ( -2.229367062499996610, -4.395833331967740065, 3.861377020970582219 ) ) ;
#28349 = CARTESIAN_POINT ( 'NONE',  ( -2.499999999999996447, -62.83333333333333570, 4.330127018922195425 ) ) ;
#28350 = CARTESIAN_POINT ( 'NONE',  ( 2.500000000000002220, 12.33333333333333215, 4.330127018922192761 ) ) ;
#28351 = CARTESIAN_POINT ( 'NONE',  ( -5.000000000000000888, -140.6875000027311842, -2.071067811865475949 ) ) ;
#28352 = CARTESIAN_POINT ( 'NONE',  ( -2.229367062500000163, -46.47916666530106511, -3.861377020970580443 ) ) ;
#28353 = CARTESIAN_POINT ( 'NONE',  ( 1.060575238724906964E-15, -84.62499999726880162, 5.773502691896257311 ) ) ;
#28354 = CARTESIAN_POINT ( 'NONE',  ( -59.44456063193725015, -137.8125000013656063, -0.3552334253322034230 ) ) ;
#28355 = CARTESIAN_POINT ( 'NONE',  ( 2.500000000000002220, -37.54166666393548013, 4.330127018922192761 ) ) ;
#28356 = DIRECTION ( 'NONE',  ( -0.000000000000000000, 1.000000000000000000, -0.000000000000000000 ) ) ;
#28357 = CARTESIAN_POINT ( 'NONE',  ( -2.229367062500000163, -90.72916666530106511, -3.861377020970580443 ) ) ;
#28358 = CARTESIAN_POINT ( 'NONE',  ( 3.152801135295367541, -157.5625000013656063, -3.152801135295367541 ) ) ;
#28359 = CARTESIAN_POINT ( 'NONE',  ( 2.499999999999998668, -36.33333333333332860, -4.330127018922193649 ) ) ;
#28360 = CARTESIAN_POINT ( 'NONE',  ( 3.061616997868383141E-16, -147.7500000000000284, -5.000000000000000000 ) ) ;
#28361 = VERTEX_POINT ( 'NONE', #36115 ) ;
#28362 = CARTESIAN_POINT ( 'NONE',  ( -2.229367062500000163, 18.27083333469892779, -3.861377020970580443 ) ) ;
#28363 = ORIENTED_EDGE ( 'NONE', *, *, #12667, .F. ) ;
#28364 = CARTESIAN_POINT ( 'NONE',  ( -4.458734124999998549, -95.22916666530106511, 2.574251347313722516 ) ) ;
#28365 = CARTESIAN_POINT ( 'NONE',  ( 4.458734124999999437, 5.937500001365593860, -5.460374474430324690E-16 ) ) ;
#28366 = CARTESIAN_POINT ( 'NONE',  ( -3.535250795749689387E-16, 9.875000002731184168, -5.773502691896257311 ) ) ;
#28367 = CARTESIAN_POINT ( 'NONE',  ( 1.339745962155612702, 12.70534180126147916, -5.000000000000000000 ) ) ;
#28368 = CARTESIAN_POINT ( 'NONE',  ( -2.500000000000000444, 3.833333333333334370, -4.330127018922193649 ) ) ;
#28369 = AXIS2_PLACEMENT_3D ( 'NONE', #24340, #28843, #19509 ) ;
#28370 = CARTESIAN_POINT ( 'NONE',  ( -2.229367062500000163, -60.47916666530106511, -3.861377020970580443 ) ) ;
#28371 = AXIS2_PLACEMENT_3D ( 'NONE', #44546, #16249, #24617 ) ;
#28372 = CARTESIAN_POINT ( 'NONE',  ( -4.999999999999998224, 15.20833333606451987, 2.886751345948131764 ) ) ;
#28373 = CARTESIAN_POINT ( 'NONE',  ( -3.535250795749689387E-16, 1.875000002731185056, -5.773502691896257311 ) ) ;
#28374 = CARTESIAN_POINT ( 'NONE',  ( 2.229367062499998831, -27.64583333196774007, -3.861377020970580887 ) ) ;
#28375 = CARTESIAN_POINT ( 'NONE',  ( -59.81910112700026616, -144.3125000027311842, -2.462841084822481541 ) ) ;
#28376 = DIRECTION ( 'NONE',  ( -0.000000000000000000, 1.000000000000000000, -0.000000000000000000 ) ) ;
#28377 =( BOUNDED_CURVE ( )  B_SPLINE_CURVE ( 2, ( #33453, #53070, #28622, #4195, #23808, #43410, #38581, #33766, #59819 ),
 .UNSPECIFIED., .F., .F. ) 
 B_SPLINE_CURVE_WITH_KNOTS ( ( 3, 2, 2, 2, 3 ),
 ( 0.9062500000000000000, 0.9069444444444444420, 0.9083333333333333259, 0.9097222222222222099, 0.9104166666666666519 ),
 .UNSPECIFIED. ) 
 CURVE ( )  GEOMETRIC_REPRESENTATION_ITEM ( )  RATIONAL_B_SPLINE_CURVE ( ( 0.9330127018922194093, 0.9330127018922194093, 1.000000000000000000, 0.8660254037844387076, 1.000000000000000000, 0.8660254037844387076, 1.000000000000000000, 0.9330127018922194093, 0.9330127018922194093 ) ) 
 REPRESENTATION_ITEM ( '' )  );
#28378 = CARTESIAN_POINT ( 'NONE',  ( 1.243387493232115550E-13, -19.25000000000000000, -5.000000000000000000 ) ) ;
#28379 = CARTESIAN_POINT ( 'NONE',  ( -5.000000000000000000, -44.00000000000000000, 0.000000000000000000 ) ) ;
#28382 = CARTESIAN_POINT ( 'NONE',  ( 2.229367062499998831, -18.89583333196774007, -3.861377020970580887 ) ) ;
#28381 =( BOUNDED_CURVE ( )  B_SPLINE_CURVE ( 2, ( #38494, #4405, #39752, #24342, #5362, #9233, #28846, #63271, #63590 ),
 .UNSPECIFIED., .F., .F. ) 
 B_SPLINE_CURVE_WITH_KNOTS ( ( 3, 2, 2, 2, 3 ),
 ( 0.9604166666666666963, 0.9611111111111111382, 0.9625000000000000222, 0.9638888888888889062, 0.9645833333333333481 ),
 .UNSPECIFIED. ) 
 CURVE ( )  GEOMETRIC_REPRESENTATION_ITEM ( )  RATIONAL_B_SPLINE_CURVE ( ( 0.9330127018922194093, 0.9330127018922194093, 1.000000000000000000, 0.8660254037844387076, 1.000000000000000000, 0.8660254037844387076, 1.000000000000000000, 0.9330127018922194093, 0.9330127018922194093 ) ) 
 REPRESENTATION_ITEM ( '' )  );
#28380 = DIRECTION ( 'NONE',  ( -0.000000000000000000, 1.000000000000000000, -0.000000000000000000 ) ) ;
#28383 = CARTESIAN_POINT ( 'NONE',  ( 1.975475456537005874E-15, -4.624999997268815832, 5.000000000000000000 ) ) ;
#28384 = CARTESIAN_POINT ( 'NONE',  ( 4.458734124999999437, -66.81249999863440792, -5.460374474430324690E-16 ) ) ;
#28385 = CARTESIAN_POINT ( 'NONE',  ( -4.458734125000001214, -146.1250000013655779, 1.846868145590734089 ) ) ;
#28386 = CARTESIAN_POINT ( 'NONE',  ( -4.458734124999998549, -77.22916666530106511, 2.574251347313722516 ) ) ;
#28387 = CARTESIAN_POINT ( 'NONE',  ( -57.19623071787017210, -144.6250000013656063, 4.297418129356382899 ) ) ;
#28388 = CARTESIAN_POINT ( 'NONE',  ( -4.458734124999999437, -26.56249999863440792, 0.000000000000000000 ) ) ;
#28389 = CARTESIAN_POINT ( 'NONE',  ( -2.499999999999996447, -65.70833333060213022, 4.330127018922195425 ) ) ;
#28391 = EDGE_LOOP ( 'NONE', ( #50363, #47761, #53997, #9656 ) ) ;
#28390 = EDGE_CURVE ( 'NONE', #60295, #37393, #46753, .T. ) ;
#28392 = CARTESIAN_POINT ( 'NONE',  ( 1.339745962155615144, -1.705341801261478274, 4.999999999999999112 ) ) ;
#28393 = ORIENTED_EDGE ( 'NONE', *, *, #9167, .T. ) ;
#28394 = CARTESIAN_POINT ( 'NONE',  ( -2.229367062500000163, -66.72916666530106511, -3.861377020970580443 ) ) ;
#28395 = CARTESIAN_POINT ( 'NONE',  ( -4.999999999999998224, 8.208333336064518093, 2.886751345948131764 ) ) ;
#28396 =( NAMED_UNIT ( * ) PLANE_ANGLE_UNIT ( ) SI_UNIT ( $, .RADIAN. ) );
#28397 = ORIENTED_EDGE ( 'NONE', *, *, #19163, .T. ) ;
#28398 = EDGE_CURVE ( 'NONE', #56025, #17652, #31529, .T. ) ;
#28399 = CARTESIAN_POINT ( 'NONE',  ( 0.000000000000000000, -170.0000000000000000, 5.000000000000000000 ) ) ;
#28400 = CARTESIAN_POINT ( 'NONE',  ( -4.458734124999998549, -54.47916666530107932, 2.574251347313722516 ) ) ;
#28401 = EDGE_CURVE ( 'NONE', #10944, #37366, #35285, .T. ) ;
#28402 = CARTESIAN_POINT ( 'NONE',  ( 2.229367062500001939, 0.7708333346989268975, 3.861377020970579999 ) ) ;
#28403 = VERTEX_POINT ( 'NONE', #11974 ) ;
#28404 = CARTESIAN_POINT ( 'NONE',  ( 4.458734125000001214, 1.104166668032261711, 2.574251347313718519 ) ) ;
#28405 = EDGE_CURVE ( 'NONE', #3107, #56488, #33226, .T. ) ;
#28406 = CARTESIAN_POINT ( 'NONE',  ( 4.458734124999999437, 16.18750000136559564, -5.460374474430324690E-16 ) ) ;
#28407 = CARTESIAN_POINT ( 'NONE',  ( -59.44456063193725015, -143.5625000013656063, -0.3552334253322034230 ) ) ;
#28408 = LINE ( 'NONE', #58003, #19217 ) ;
#28409 = CARTESIAN_POINT ( 'NONE',  ( 4.458734124999999437, -164.4375000013655779, 0.000000000000000000 ) ) ;
#28411 = EDGE_CURVE ( 'NONE', #18181, #50566, #60571, .T. ) ;
#28410 = ORIENTED_EDGE ( 'NONE', *, *, #4006, .T. ) ;
#28412 = CARTESIAN_POINT ( 'NONE',  ( -4.458734124999999437, -78.31249999863440792, 0.000000000000000000 ) ) ;
#28413 = FACE_OUTER_BOUND ( 'NONE', #25602, .T. ) ;
#28414 = CARTESIAN_POINT ( 'NONE',  ( 4.458734125000001214, 9.104166668032261711, 2.574251347313718519 ) ) ;
#28415 = AXIS2_PLACEMENT_3D ( 'NONE', #57125, #13040, #51969 ) ;
#28416 = AXIS2_PLACEMENT_3D ( 'NONE', #49391, #20125, #60015 ) ;
#28417 = EDGE_CURVE ( 'NONE', #57628, #23954, #6935, .T. ) ;
#28418 = LINE ( 'NONE', #58950, #41823 ) ;
#28419 = CARTESIAN_POINT ( 'NONE',  ( 2.229367062500001939, -59.22916666530106511, 3.861377020970579999 ) ) ;
#28420 = AXIS2_PLACEMENT_3D ( 'NONE', #18313, #37938, #43380 ) ;
#28421 = CARTESIAN_POINT ( 'NONE',  ( 5.000000000000000000, -20.37499999726880873, -6.123233995736766282E-16 ) ) ;
#28422 = CARTESIAN_POINT ( 'NONE',  ( -4.999999999999998224, 6.083333333333333037, 2.886751345948131764 ) ) ;
#28423 = CYLINDRICAL_SURFACE ( 'NONE', #10041, 5.000000000000000000 ) ;
#28424 = DIRECTION ( 'NONE',  ( -0.6485228581062915110, 0.000000000000000000, -0.7611951803011149931 ) ) ;
#28425 = CARTESIAN_POINT ( 'NONE',  ( -1.339745962155610925, -105.6696581960073473, 5.000000000000000000 ) ) ;
#28426 = CARTESIAN_POINT ( 'NONE',  ( 1.975475456537005874E-15, -38.75000000000000000, 5.000000000000000000 ) ) ;
#28427 = CARTESIAN_POINT ( 'NONE',  ( 9.457646018065525792E-16, -42.06249999863440081, 5.148502694627439702 ) ) ;
#28428 = CARTESIAN_POINT ( 'NONE',  ( 9.457646018065525792E-16, -26.31249999863440792, 5.148502694627439702 ) ) ;
#28429 =( BOUNDED_CURVE ( )  B_SPLINE_CURVE ( 2, ( #10025, #19995, #24826, #39603, #54419, #29957, #25139, #22702, #27821 ),
 .UNSPECIFIED., .F., .F. ) 
 B_SPLINE_CURVE_WITH_KNOTS ( ( 3, 2, 2, 2, 3 ),
 ( 0.3854166666666666852, 0.3861111111111111271, 0.3875000000000000111, 0.3888888888888888951, 0.3895833333333333370 ),
 .UNSPECIFIED. ) 
 CURVE ( )  GEOMETRIC_REPRESENTATION_ITEM ( )  RATIONAL_B_SPLINE_CURVE ( ( 0.9330127018922194093, 0.9330127018922194093, 1.000000000000000000, 0.8660254037844387076, 1.000000000000000000, 0.8660254037844387076, 1.000000000000000000, 0.9330127018922194093, 0.9330127018922194093 ) ) 
 REPRESENTATION_ITEM ( '' )  );
#28430 = CARTESIAN_POINT ( 'NONE',  ( 6.123233995736766282E-16, -120.0000000000000000, -5.000000000000000000 ) ) ;
#28431 = CARTESIAN_POINT ( 'NONE',  ( -2.499999999999996447, 27.16666666666666430, 4.330127018922195425 ) ) ;
#28432 = CARTESIAN_POINT ( 'NONE',  ( -3.535533905932737309, -151.7500000027312126, -3.535533905932738197 ) ) ;
#28433 = ORIENTED_EDGE ( 'NONE', *, *, #48778, .F. ) ;
#28434 = CARTESIAN_POINT ( 'NONE',  ( 9.457646018065525792E-16, -106.3124999986343795, 5.148502694627439702 ) ) ;
#28435 = CARTESIAN_POINT ( 'NONE',  ( 2.229367062500001939, -32.97916666530106511, 3.861377020970579999 ) ) ;
#28436 = CARTESIAN_POINT ( 'NONE',  ( -4.999999999999999112, -68.79166666393547303, 2.886751345948131764 ) ) ;
#28437 = CARTESIAN_POINT ( 'NONE',  ( -59.29741812935640155, -149.8750000013655779, -2.196230717870135685 ) ) ;
#28438 = CARTESIAN_POINT ( 'NONE',  ( -2.071067811865475061, -144.6875000000000853, -5.000000000000000888 ) ) ;
#28439 = CARTESIAN_POINT ( 'NONE',  ( -2.229367062500000163, -29.47916666530107221, -3.861377020970580443 ) ) ;
#28440 = CARTESIAN_POINT ( 'NONE',  ( -2.229367062499996610, -72.39583333196773651, 3.861377020970582219 ) ) ;
#28441 = CARTESIAN_POINT ( 'NONE',  ( -4.458734124999999437, -28.31249999863440081, 0.000000000000000000 ) ) ;
#28442 = CARTESIAN_POINT ( 'NONE',  ( 0.000000000000000000, -120.0000000000000000, 0.000000000000000000 ) ) ;
#28443 = CARTESIAN_POINT ( 'NONE',  ( -6.972266317189433020E-16, 18.87500000273119127, -5.000000000000000000 ) ) ;
#28444 = CARTESIAN_POINT ( 'NONE',  ( -5.000000000000000000, -22.00000000000000000, 0.000000000000000000 ) ) ;
#28445 = CARTESIAN_POINT ( 'NONE',  ( -4.458734125000000326, -146.0000000013655779, -1.846868145590735644 ) ) ;
#28446 = ORIENTED_EDGE ( 'NONE', *, *, #15284, .T. ) ;
#28447 = DIRECTION ( 'NONE',  ( 0.000000000000000000, 0.000000000000000000, 1.000000000000000000 ) ) ;
#28448 = CARTESIAN_POINT ( 'NONE',  ( -2.229367062499996610, -59.39583333196773651, 3.861377020970582219 ) ) ;
#28449 = CARTESIAN_POINT ( 'NONE',  ( 5.000000000000000000, 25.62500000273118417, -6.123233995736766282E-16 ) ) ;
#28450 = CARTESIAN_POINT ( 'NONE',  ( 0.000000000000000000, -170.0000000000000000, 5.000000000000000000 ) ) ;
#28451 = CARTESIAN_POINT ( 'NONE',  ( 2.499999999999998668, 18.66666666666666430, -4.330127018922193649 ) ) ;
#28452 = CARTESIAN_POINT ( 'NONE',  ( -5.000000000000000000, -36.87499999726881583, 0.000000000000000000 ) ) ;
#28453 = CARTESIAN_POINT ( 'NONE',  ( 4.458734124999999437, 1.187500001365596081, -5.460374474430324690E-16 ) ) ;
#28454 = CARTESIAN_POINT ( 'NONE',  ( -5.000000000000000000, -51.95833333060214443, -2.886751345948128211 ) ) ;
#28455 = CYLINDRICAL_SURFACE ( 'NONE', #12212, 5.000000000000000000 ) ;
#28456 = CARTESIAN_POINT ( 'NONE',  ( 9.457646018065525792E-16, 11.68750000136559564, 5.148502694627439702 ) ) ;
#28457 = DIRECTION ( 'NONE',  ( -0.000000000000000000, 1.000000000000000000, -0.000000000000000000 ) ) ;
#28458 = VERTEX_POINT ( 'NONE', #33190 ) ;
#28459 = VECTOR ( 'NONE', #35485, 1000.000000000000000 ) ;
#28460 = CARTESIAN_POINT ( 'NONE',  ( -6.972266317189433020E-16, 10.87500000273118417, -5.000000000000000000 ) ) ;
#28461 = CARTESIAN_POINT ( 'NONE',  ( -3.152548672688508926E-16, -51.56249999863441502, -5.148502694627439702 ) ) ;
#28462 = CARTESIAN_POINT ( 'NONE',  ( -1.846868145590734756, -161.3750000013656063, -4.458734125000000326 ) ) ;
#28463 = PRESENTATION_LAYER_ASSIGNMENT (  '', '', ( #2819 ) ) ;
#28464 = VECTOR ( 'NONE', #25340, 1000.000000000000000 ) ;
#28465 = CARTESIAN_POINT ( 'NONE',  ( 2.500000000000002220, -50.54166666393547303, 4.330127018922192761 ) ) ;
#28466 = ORIENTED_EDGE ( 'NONE', *, *, #10634, .T. ) ;
#28467 = AXIS2_PLACEMENT_3D ( 'NONE', #19870, #921, #59120 ) ;
#28468 = CARTESIAN_POINT ( 'NONE',  ( -2.229367062500000163, -23.47916666530107221, -3.861377020970580443 ) ) ;
#28469 = ORIENTED_EDGE ( 'NONE', *, *, #15253, .F. ) ;
#28471 = CARTESIAN_POINT ( 'NONE',  ( -3.535533905932737309, -142.7500000027311842, -3.535533905932738197 ) ) ;
#28470 = PLANE ( 'NONE',  #61499 ) ;
#28472 = CARTESIAN_POINT ( 'NONE',  ( 4.458734124999999437, -159.4375000013655779, 0.000000000000000000 ) ) ;
#28473 = ORIENTED_EDGE ( 'NONE', *, *, #20483, .F. ) ;
#28474 = CARTESIAN_POINT ( 'NONE',  ( 1.975475456537005874E-15, -38.62499999726880873, 5.000000000000000000 ) ) ;
#28475 = CARTESIAN_POINT ( 'NONE',  ( -55.39835681537999790, -132.8750000000000284, 4.984105922594378235 ) ) ;
#28476 = CARTESIAN_POINT ( 'NONE',  ( -2.229367062499996610, -35.39583333196772941, 3.861377020970582219 ) ) ;
#28477 = ORIENTED_EDGE ( 'NONE', *, *, #52830, .F. ) ;
#28478 = CARTESIAN_POINT ( 'NONE',  ( -4.458734124999998549, -83.22916666530106511, 2.574251347313722516 ) ) ;
#28479 = CARTESIAN_POINT ( 'NONE',  ( 9.457646018065525792E-16, 20.93750000136558853, 5.148502694627439702 ) ) ;
#28480 = CARTESIAN_POINT ( 'NONE',  ( -1.339745962155610925, -17.66965819600733312, 5.000000000000000000 ) ) ;
#28481 = VERTEX_POINT ( 'NONE', #38622 ) ;
#28482 = CARTESIAN_POINT ( 'NONE',  ( -58.39396692619412477, -138.6875000013656347, 2.891590998281057701 ) ) ;
#28483 = CARTESIAN_POINT ( 'NONE',  ( -3.152548672688508926E-16, -83.81249999863439371, -5.148502694627439702 ) ) ;
#28484 = CARTESIAN_POINT ( 'NONE',  ( -58.24261429053147765, -127.3750000027312268, -3.805975901505573855 ) ) ;
#28485 = CARTESIAN_POINT ( 'NONE',  ( -6.972266317189433020E-16, -4.124999997268814056, -5.000000000000000000 ) ) ;
#28486 = CARTESIAN_POINT ( 'NONE',  ( 1.339745962155615144, -39.70534180126147561, 4.999999999999999112 ) ) ;
#28487 = CARTESIAN_POINT ( 'NONE',  ( 5.000000000000000888, 4.416666666666666075, 2.886751345948126879 ) ) ;
#28488 = CARTESIAN_POINT ( 'NONE',  ( -3.152548672688508926E-16, -59.56249999863440081, -5.148502694627439702 ) ) ;
#28489 = CARTESIAN_POINT ( 'NONE',  ( -2.229367062499996610, 25.85416666803225993, 3.861377020970582219 ) ) ;
#28490 = CARTESIAN_POINT ( 'NONE',  ( 1.975475456537005874E-15, -97.74999999999998579, 5.000000000000000000 ) ) ;
#28491 = CARTESIAN_POINT ( 'NONE',  ( -6.972266317189433020E-16, -44.25000000000000000, -5.000000000000000000 ) ) ;
#28492 = CARTESIAN_POINT ( 'NONE',  ( -4.458734124999998549, -44.47916666530106511, 2.574251347313722516 ) ) ;
#28493 = CARTESIAN_POINT ( 'NONE',  ( 5.000000000000000888, -6.458333330602148870, 2.886751345948126879 ) ) ;
#28494 = CARTESIAN_POINT ( 'NONE',  ( -2.500000000000000444, -93.16666666666665719, -4.330127018922193649 ) ) ;
#28495 = DIRECTION ( 'NONE',  ( -0.000000000000000000, 1.000000000000000000, -0.000000000000000000 ) ) ;
#28496 = CARTESIAN_POINT ( 'NONE',  ( 4.458734124999999437, -82.06249999863440792, -5.460374474430324690E-16 ) ) ;
#28497 = CARTESIAN_POINT ( 'NONE',  ( 4.458734125000000326, -109.8958333319677365, 2.574251347313718519 ) ) ;
#28498 = CARTESIAN_POINT ( 'NONE',  ( -2.229367062500000163, -11.72916666530107044, -3.861377020970580443 ) ) ;
#28499 = ORIENTED_EDGE ( 'NONE', *, *, #16940, .F. ) ;
#28500 = CARTESIAN_POINT ( 'NONE',  ( 2.500000000000002220, -9.541666663935483683, 4.330127018922192761 ) ) ;
#28501 = CARTESIAN_POINT ( 'NONE',  ( -3.152548672688508926E-16, -100.5624999986344079, -5.148502694627439702 ) ) ;
#28502 = CARTESIAN_POINT ( 'NONE',  ( -9.184850993605147944E-16, -164.3750000027311842, 5.000000000000000000 ) ) ;
#28503 = CARTESIAN_POINT ( 'NONE',  ( -2.229367062500000163, -94.72916666530106511, -3.861377020970580443 ) ) ;
#28504 = CARTESIAN_POINT ( 'NONE',  ( 1.060575238724906964E-15, -52.62499999726881583, 5.773502691896257311 ) ) ;
#28505 = CARTESIAN_POINT ( 'NONE',  ( -5.000000000000000000, -36.95833333060213022, -2.886751345948128211 ) ) ;
#28506 = AXIS2_PLACEMENT_3D ( 'NONE', #17858, #7275, #60672 ) ;
#28507 =( BOUNDED_CURVE ( )  B_SPLINE_CURVE ( 2, ( #11229, #32112, #16700, #7690, #50483, #50798, #6734, #6422, #26666 ),
 .UNSPECIFIED., .F., .F. ) 
 B_SPLINE_CURVE_WITH_KNOTS ( ( 3, 2, 2, 2, 3 ),
 ( 0.3270833333333333370, 0.3277777777777777790, 0.3291666666666666630, 0.3305555555555555469, 0.3312499999999999889 ),
 .UNSPECIFIED. ) 
 CURVE ( )  GEOMETRIC_REPRESENTATION_ITEM ( )  RATIONAL_B_SPLINE_CURVE ( ( 0.9330127018922194093, 0.9330127018922194093, 1.000000000000000000, 0.8660254037844387076, 1.000000000000000000, 0.8660254037844387076, 1.000000000000000000, 0.9330127018922194093, 0.9330127018922194093 ) ) 
 REPRESENTATION_ITEM ( '' )  );
#28508 = CARTESIAN_POINT ( 'NONE',  ( -53.51423613279429503, -130.2500000013656063, 4.591703134518082763 ) ) ;
#28509 = CARTESIAN_POINT ( 'NONE',  ( -50.70258187064364108, -147.1250000013656063, 2.196230717870141014 ) ) ;
#28510 = CARTESIAN_POINT ( 'NONE',  ( 4.458734125000000326, -10.89583333196773651, 2.574251347313718519 ) ) ;
#28511 = CARTESIAN_POINT ( 'NONE',  ( 4.458734124999998549, 9.020833334698927786, -2.574251347313721627 ) ) ;
#28512 = CARTESIAN_POINT ( 'NONE',  ( -2.229367062499996610, -57.39583333196773651, 3.861377020970582219 ) ) ;
#28513 = CARTESIAN_POINT ( 'NONE',  ( -6.972266317189433020E-16, -52.25000000000000711, -5.000000000000000000 ) ) ;
#28514 = CARTESIAN_POINT ( 'NONE',  ( 5.000000000000000888, -15.45833333060214443, 2.886751345948126879 ) ) ;
#28515 = CARTESIAN_POINT ( 'NONE',  ( 2.229367062500001939, -16.97916666530106866, 3.861377020970579999 ) ) ;
#28516 = CARTESIAN_POINT ( 'NONE',  ( 2.500000000000002220, -71.66666666666667140, 4.330127018922192761 ) ) ;
#28517 = ORIENTED_EDGE ( 'NONE', *, *, #21575, .F. ) ;
#28518 = CARTESIAN_POINT ( 'NONE',  ( 4.458734125000000326, -43.14583333196773651, 2.574251347313718519 ) ) ;
#28519 = UNCERTAINTY_MEASURE_WITH_UNIT (LENGTH_MEASURE( 1.000000000000000082E-05 ), #41093, 'distance_accuracy_value', 'NONE');
#28520 = CARTESIAN_POINT ( 'NONE',  ( 5.000000000000000888, -83.45833333060213022, 2.886751345948126879 ) ) ;
#28521 = DIRECTION ( 'NONE',  ( -0.000000000000000000, 1.000000000000000000, -0.000000000000000000 ) ) ;
#28522 = CARTESIAN_POINT ( 'NONE',  ( -4.613983237546153582, 6.452243898629808960, -7.591546097228401457 ) ) ;
#28523 = CARTESIAN_POINT ( 'NONE',  ( 9.457646018065525792E-16, -85.06249999863440792, 5.148502694627439702 ) ) ;
#28524 = CARTESIAN_POINT ( 'NONE',  ( -4.458734124999999437, 21.43750000136559208, 0.000000000000000000 ) ) ;
#28525 = CARTESIAN_POINT ( 'NONE',  ( 2.229367062499998831, 13.35416666803226171, -3.861377020970580887 ) ) ;
#28526 =( BOUNDED_CURVE ( )  B_SPLINE_CURVE ( 2, ( #8684, #18014, #13197, #28297, #32819, #47910, #11136, #18652, #55217 ),
 .UNSPECIFIED., .F., .F. ) 
 B_SPLINE_CURVE_WITH_KNOTS ( ( 3, 2, 2, 2, 3 ),
 ( 0.7354166666666667185, 0.7361111111111111605, 0.7375000000000000444, 0.7388888888888889284, 0.7395833333333333703 ),
 .UNSPECIFIED. ) 
 CURVE ( )  GEOMETRIC_REPRESENTATION_ITEM ( )  RATIONAL_B_SPLINE_CURVE ( ( 0.9330127018922194093, 0.9330127018922194093, 1.000000000000000000, 0.8660254037844387076, 1.000000000000000000, 0.8660254037844387076, 1.000000000000000000, 0.9330127018922194093, 0.9330127018922194093 ) ) 
 REPRESENTATION_ITEM ( '' )  );
#28527 = CARTESIAN_POINT ( 'NONE',  ( -4.330127018922101279, 45.00000000000000000, 7.500000000000002665 ) ) ;
#28528 = CARTESIAN_POINT ( 'NONE',  ( 4.458734124999998549, -88.97916666530106511, -2.574251347313721627 ) ) ;
#28529 = CARTESIAN_POINT ( 'NONE',  ( 1.060575238724906964E-15, -67.75000000000000000, 5.773502691896257311 ) ) ;
#28530 = CARTESIAN_POINT ( 'NONE',  ( -2.499999999999996447, 16.29166666939785202, 4.330127018922195425 ) ) ;
#28531 = ORIENTED_EDGE ( 'NONE', *, *, #3320, .T. ) ;
#28532 = CARTESIAN_POINT ( 'NONE',  ( -6.972266317189433020E-16, -79.24999999999998579, -5.000000000000000000 ) ) ;
#28533 = CARTESIAN_POINT ( 'NONE',  ( -9.184850993605147944E-16, -167.2500000000000000, 5.000000000000000000 ) ) ;
#28535 = CARTESIAN_POINT ( 'NONE',  ( -2.499999999999996447, -29.83333333333332860, 4.330127018922195425 ) ) ;
#28534 = DIRECTION ( 'NONE',  ( -0.000000000000000000, 1.000000000000000000, -0.000000000000000000 ) ) ;
#28536 = CARTESIAN_POINT ( 'NONE',  ( 9.457646018065525792E-16, -33.06249999863440792, 5.148502694627439702 ) ) ;
#28537 = CARTESIAN_POINT ( 'NONE',  ( -5.000000000000000000, -35.95833333060213732, -2.886751345948128211 ) ) ;
#28539 = VERTEX_POINT ( 'NONE', #17762 ) ;
#28538 = CARTESIAN_POINT ( 'NONE',  ( 4.458734124999999437, -60.81249999863440081, -5.460374474430324690E-16 ) ) ;
#28540 = CARTESIAN_POINT ( 'NONE',  ( -50.70258187064364108, -149.3750000013656347, 2.196230717870141014 ) ) ;
#28542 = ORIENTED_EDGE ( 'NONE', *, *, #15425, .F. ) ;
#28541 = CARTESIAN_POINT ( 'NONE',  ( 2.229367062499998831, -12.89583333196774007, -3.861377020970580887 ) ) ;
#28543 = CARTESIAN_POINT ( 'NONE',  ( -5.000000000000000000, -75.08333333333332860, -2.886751345948128211 ) ) ;
#28544 = CARTESIAN_POINT ( 'NONE',  ( -57.19623071787016499, -135.3750000013656063, 4.297418129356382899 ) ) ;
#28545 = CARTESIAN_POINT ( 'NONE',  ( 4.458734125000001214, -56.14583333196774362, 2.574251347313718519 ) ) ;
#28546 = VECTOR ( 'NONE', #9197, 1000.000000000000000 ) ;
#28547 = CARTESIAN_POINT ( 'NONE',  ( -5.000000000000000000, -82.87499999726881583, 0.000000000000000000 ) ) ;
#28549 = ORIENTED_EDGE ( 'NONE', *, *, #42487, .F. ) ;
#28548 = CARTESIAN_POINT ( 'NONE',  ( 0.000000000000000000, -170.0000000000000000, 0.000000000000000000 ) ) ;
#28550 = CARTESIAN_POINT ( 'NONE',  ( -57.46284108482265651, -144.9375000000000000, 4.819101127000239515 ) ) ;
#28551 = CARTESIAN_POINT ( 'NONE',  ( -2.229367062499996610, -21.39583333196774007, 3.861377020970582219 ) ) ;
#28553 = VERTEX_POINT ( 'NONE', #47656 ) ;
#28552 = CARTESIAN_POINT ( 'NONE',  ( -4.458734124999998549, -57.47916666530108643, 2.574251347313722516 ) ) ;
#28554 = CARTESIAN_POINT ( 'NONE',  ( -1.846868145590734756, -168.3750000013655779, -4.458734125000000326 ) ) ;
#28555 = CARTESIAN_POINT ( 'NONE',  ( -3.152548672688508926E-16, -106.8124999986343795, -5.148502694627439702 ) ) ;
#28556 = CARTESIAN_POINT ( 'NONE',  ( -4.999999999999998224, -68.79166666393547303, 2.886751345948131764 ) ) ;
#28557 = ORIENTED_EDGE ( 'NONE', *, *, #23713, .T. ) ;
#28558 = CARTESIAN_POINT ( 'NONE',  ( -50.55543936806279248, -150.3125000013656063, 0.3552334253322060320 ) ) ;
#28559 = CARTESIAN_POINT ( 'NONE',  ( -58.80597590150559739, -137.1250000027312410, 3.242614290531460330 ) ) ;
#28560 = CARTESIAN_POINT ( 'NONE',  ( -4.458734124999999437, -38.31249999863439371, 0.000000000000000000 ) ) ;
#28561 = DIRECTION ( 'NONE',  ( 0.000000000000000000, 0.000000000000000000, -1.000000000000000000 ) ) ;
#28562 = CARTESIAN_POINT ( 'NONE',  ( -3.152548672688508926E-16, -8.562499998634404363, -5.148502694627439702 ) ) ;
#28563 = CARTESIAN_POINT ( 'NONE',  ( 2.229367062499998831, -101.8958333319677365, -3.861377020970580887 ) ) ;
#28564 = CARTESIAN_POINT ( 'NONE',  ( 1.846868145590736310, -142.8750000013656063, 4.458734124999999437 ) ) ;
#28565 = CARTESIAN_POINT ( 'NONE',  ( -4.458734124999999437, -30.56249999863440436, 0.000000000000000000 ) ) ;
#28566 = CARTESIAN_POINT ( 'NONE',  ( -51.75738570946856498, -139.8750000027312126, 3.805975901505576964 ) ) ;
#28567 = CARTESIAN_POINT ( 'NONE',  ( -58.39396692619412477, -131.4375000013656063, 2.891590998281057701 ) ) ;
#28568 = CARTESIAN_POINT ( 'NONE',  ( -3.152548672688508926E-16, -67.81249999863440792, -5.148502694627439702 ) ) ;
#28569 = CARTESIAN_POINT ( 'NONE',  ( -2.500000000000000444, -16.16666666666666785, -4.330127018922193649 ) ) ;
#28570 = CARTESIAN_POINT ( 'NONE',  ( -1.339745962155613812, 16.79465819873852084, -5.000000000000000000 ) ) ;
#28571 = CARTESIAN_POINT ( 'NONE',  ( -1.846868145590734756, -142.1250000013656063, -4.458734124999999437 ) ) ;
#28572 = CARTESIAN_POINT ( 'NONE',  ( 4.458734124999999437, 4.937500001365595637, -5.460374474430324690E-16 ) ) ;
#28573 =( BOUNDED_CURVE ( )  B_SPLINE_CURVE ( 2, ( #24225, #63477, #36110, #40921, #45117, #6210, #35477, #1401, #31269 ),
 .UNSPECIFIED., .F., .F. ) 
 B_SPLINE_CURVE_WITH_KNOTS ( ( 3, 2, 2, 2, 3 ),
 ( 0.9312500000000000222, 0.9319444444444444642, 0.9333333333333333481, 0.9347222222222222321, 0.9354166666666666741 ),
 .UNSPECIFIED. ) 
 CURVE ( )  GEOMETRIC_REPRESENTATION_ITEM ( )  RATIONAL_B_SPLINE_CURVE ( ( 0.9330127018922194093, 0.9330127018922194093, 1.000000000000000000, 0.8660254037844387076, 1.000000000000000000, 0.8660254037844387076, 1.000000000000000000, 0.9330127018922194093, 0.9330127018922194093 ) ) 
 REPRESENTATION_ITEM ( '' )  );
#28574 = EDGE_LOOP ( 'NONE', ( #27977, #53888, #29977, #48324 ) ) ;
#28575 = CARTESIAN_POINT ( 'NONE',  ( 1.975475456537005874E-15, -70.62499999726880162, 5.000000000000000000 ) ) ;
#28576 = CARTESIAN_POINT ( 'NONE',  ( 5.000000000000000000, 9.499999999999998224, -6.123233995736766282E-16 ) ) ;
#28578 = CARTESIAN_POINT ( 'NONE',  ( 4.458734124999999437, -31.81249999863440436, -5.460374474430324690E-16 ) ) ;
#28577 = CARTESIAN_POINT ( 'NONE',  ( 5.000000000000000000, -93.41666666666667140, -2.886751345948129988 ) ) ;
#28579 = FACE_OUTER_BOUND ( 'NONE', #8386, .T. ) ;
#28580 = CARTESIAN_POINT ( 'NONE',  ( -4.458734124999999437, -73.64583333196773651, -2.574251347313719407 ) ) ;
#28581 = CARTESIAN_POINT ( 'NONE',  ( -4.458734124999999437, 23.35416666803226349, -2.574251347313719407 ) ) ;
#28582 = CARTESIAN_POINT ( 'NONE',  ( 5.000000000000000000, -18.50000000000000355, -6.123233995736766282E-16 ) ) ;
#28583 = CARTESIAN_POINT ( 'NONE',  ( -50.40829686548195099, -141.0000000013656063, -1.485763867205728284 ) ) ;
#28584 = CARTESIAN_POINT ( 'NONE',  ( -2.229367062499996610, 3.854166668032260823, 3.861377020970582219 ) ) ;
#28585 = CARTESIAN_POINT ( 'NONE',  ( -4.458734124999999437, 27.43750000136559208, 0.000000000000000000 ) ) ;
#28586 = CARTESIAN_POINT ( 'NONE',  ( 4.458734124999999437, -43.06249999863440081, -5.460374474430324690E-16 ) ) ;
#28587 = DIRECTION ( 'NONE',  ( 0.6592143633790508161, -0.4999999999999791833, -0.5616372700549471242 ) ) ;
#28588 = CARTESIAN_POINT ( 'NONE',  ( 2.229367062500001939, 1.020833334698927120, 3.861377020970579999 ) ) ;
#28589 = CARTESIAN_POINT ( 'NONE',  ( -4.458734124999997661, -23.47916666530107221, 2.574251347313722516 ) ) ;
#28590 = AXIS2_PLACEMENT_3D ( 'NONE', #53171, #10047, #25159 ) ;
#28591 = CARTESIAN_POINT ( 'NONE',  ( 4.458734124999999437, -155.5000000013655779, 1.846868145590737864 ) ) ;
#28592 = CARTESIAN_POINT ( 'NONE',  ( 9.457646018065525792E-16, -70.06249999863439371, 5.148502694627439702 ) ) ;
#28593 = CARTESIAN_POINT ( 'NONE',  ( 2.499999999999998668, -102.2083333306021444, -4.330127018922193649 ) ) ;
#28594 = EDGE_CURVE ( 'NONE', #60902, #25319, #23849, .T. ) ;
#28595 = VECTOR ( 'NONE', #14605, 1000.000000000000000 ) ;
#28596 = CARTESIAN_POINT ( 'NONE',  ( -2.229367062500000163, 28.52083333469892779, -3.861377020970580443 ) ) ;
#28597 = CYLINDRICAL_SURFACE ( 'NONE', #63642, 5.000000000000000000 ) ;
#28598 = CARTESIAN_POINT ( 'NONE',  ( -3.152548672688508926E-16, -104.8124999986344079, -5.148502694627439702 ) ) ;
#28599 = CARTESIAN_POINT ( 'NONE',  ( 9.457646018065525792E-16, -73.31249999863439371, 5.148502694627439702 ) ) ;
#28600 = CARTESIAN_POINT ( 'NONE',  ( -2.499999999999996447, -51.83333333333332860, 4.330127018922195425 ) ) ;
#28601 = CARTESIAN_POINT ( 'NONE',  ( -6.972266317189433020E-16, -22.24999999999999645, -5.000000000000000000 ) ) ;
#28602 = CARTESIAN_POINT ( 'NONE',  ( 0.000000000000000000, -170.0000000000000000, 5.000000000000000000 ) ) ;
#28603 = ORIENTED_EDGE ( 'NONE', *, *, #20789, .F. ) ;
#28604 =( BOUNDED_CURVE ( )  B_SPLINE_CURVE ( 2, ( #24530, #44455, #735, #415, #58629, #20018, #19381, #4587, #59262 ),
 .UNSPECIFIED., .F., .F. ) 
 B_SPLINE_CURVE_WITH_KNOTS ( ( 3, 2, 2, 2, 3 ),
 ( 0.7749999999999998002, 0.7791666666666664520, 0.7833333333333331039, 0.7874999999999997558, 0.7916666666666664076 ),
 .UNSPECIFIED. ) 
 CURVE ( )  GEOMETRIC_REPRESENTATION_ITEM ( )  RATIONAL_B_SPLINE_CURVE ( ( 1.000000000000003997, 0.9238795325112826307, 1.000000000000000000, 0.9238795325112867385, 1.000000000000000000, 0.9238795325112867385, 1.000000000000000000, 0.9238795325112908463, 0.9999999999999958922 ) ) 
 REPRESENTATION_ITEM ( '' )  );
#28605 = CARTESIAN_POINT ( 'NONE',  ( -1.339745962155610925, 12.33034180399266333, 5.000000000000000000 ) ) ;
#28606 = CARTESIAN_POINT ( 'NONE',  ( 2.500000000000002220, -11.66666666666666607, 4.330127018922192761 ) ) ;
#28607 = CARTESIAN_POINT ( 'NONE',  ( 4.458734124999999437, -14.81249999863440436, -5.460374474430324690E-16 ) ) ;
#28608 = CARTESIAN_POINT ( 'NONE',  ( 4.458734125000000326, -75.89583333196775072, 2.574251347313718519 ) ) ;
#28609 = CARTESIAN_POINT ( 'NONE',  ( -3.152801135295367096, -168.3125000013656063, -3.152801135295367541 ) ) ;
#28610 = ADVANCED_FACE ( 'NONE', ( #13248 ), #57012, .T. ) ;
#28611 = CARTESIAN_POINT ( 'NONE',  ( -2.499999999999996447, -17.70833333060214443, 4.330127018922195425 ) ) ;
#28613 = ORIENTED_EDGE ( 'NONE', *, *, #9964, .T. ) ;
#28612 = CARTESIAN_POINT ( 'NONE',  ( 9.457646018065525792E-16, -47.06249999863440792, 5.148502694627439702 ) ) ;
#28614 = CARTESIAN_POINT ( 'NONE',  ( 2.499999999999998668, -45.20833333060214443, -4.330127018922193649 ) ) ;
#28615 = ADVANCED_FACE ( 'NONE', ( #33500 ), #52805, .T. ) ;
#28617 = VERTEX_POINT ( 'NONE', #23217 ) ;
#28616 = CARTESIAN_POINT ( 'NONE',  ( -2.229367062499996610, 5.604166668032261711, 3.861377020970582219 ) ) ;
#28618 = CARTESIAN_POINT ( 'NONE',  ( -5.000000000000000000, -86.87499999726880162, 0.000000000000000000 ) ) ;
#28619 = CARTESIAN_POINT ( 'NONE',  ( -5.000000000000000000, -63.00000000000000000, 0.000000000000000000 ) ) ;
#28620 = CARTESIAN_POINT ( 'NONE',  ( -3.152801135295367985, -158.0625000013656063, 3.152801135295367096 ) ) ;
#28621 = CARTESIAN_POINT ( 'NONE',  ( 9.457646018065525792E-16, -42.31249999863440081, 5.148502694627439702 ) ) ;
#28622 = CARTESIAN_POINT ( 'NONE',  ( -2.499999999999996447, -78.83333333333332860, 4.330127018922195425 ) ) ;
#28623 = CARTESIAN_POINT ( 'NONE',  ( -3.535533905932738641, -163.3750000000000284, 3.535533905932737309 ) ) ;
#28624 = DIRECTION ( 'NONE',  ( -0.000000000000000000, 1.000000000000000000, -0.000000000000000000 ) ) ;
#28625 = CARTESIAN_POINT ( 'NONE',  ( -57.19623071787017210, -128.6250000013656347, 4.297418129356382899 ) ) ;
#28626 = CARTESIAN_POINT ( 'NONE',  ( -4.458734124999999437, -7.562499998634404363, 0.000000000000000000 ) ) ;
#28627 = CARTESIAN_POINT ( 'NONE',  ( 2.229367062499998831, -40.89583333196773651, -3.861377020970580887 ) ) ;
#28628 = LINE ( 'NONE', #28937, #18287 ) ;
#28629 = CARTESIAN_POINT ( 'NONE',  ( 4.458734125000000326, -148.3750000013655779, -1.846868145590734978 ) ) ;
#28630 = CARTESIAN_POINT ( 'NONE',  ( 4.458734124999998549, -86.97916666530106511, -2.574251347313721627 ) ) ;
#28631 = CARTESIAN_POINT ( 'NONE',  ( 1.975475456537005874E-15, -108.7499999999999858, 5.000000000000000000 ) ) ;
#28632 = ORIENTED_EDGE ( 'NONE', *, *, #18079, .T. ) ;
#28633 = CARTESIAN_POINT ( 'NONE',  ( -55.39835681537999790, -151.8750000000000284, 4.984105922594378235 ) ) ;
#28634 = CARTESIAN_POINT ( 'NONE',  ( -51.19402409849444524, -152.6250000027312126, -3.242614290531456334 ) ) ;
#28635 = AXIS2_PLACEMENT_3D ( 'NONE', #20963, #44745, #5520 ) ;
#28636 = CARTESIAN_POINT ( 'NONE',  ( -4.458734124999999437, -77.56249999863440792, 0.000000000000000000 ) ) ;
#28637 = VECTOR ( 'NONE', #56429, 1000.000000000000000 ) ;
#28638 = ORIENTED_EDGE ( 'NONE', *, *, #17400, .T. ) ;
#28639 = DIRECTION ( 'NONE',  ( -0.000000000000000000, 1.000000000000000000, -0.000000000000000000 ) ) ;
#28640 = EDGE_CURVE ( 'NONE', #43748, #18601, #349, .T. ) ;
#28641 = CARTESIAN_POINT ( 'NONE',  ( 4.458734124999998549, -11.97916666530107044, -2.574251347313721627 ) ) ;
#28642 = CARTESIAN_POINT ( 'NONE',  ( 2.500000000000002220, -105.5416666639354730, 4.330127018922192761 ) ) ;
#28643 = CARTESIAN_POINT ( 'NONE',  ( -2.229367062499996610, -1.145833331967736957, 3.861377020970582219 ) ) ;
#28644 = CARTESIAN_POINT ( 'NONE',  ( -2.480964764533239819E-13, -95.62499999726883004, 5.000000000000000000 ) ) ;
#28645 = CARTESIAN_POINT ( 'NONE',  ( 3.152801135295366208, -152.5625000013655779, 3.152801135295367985 ) ) ;
#28646 = CARTESIAN_POINT ( 'NONE',  ( 4.458734124999999437, 19.93750000136559208, -5.460374474430324690E-16 ) ) ;
#28647 = ORIENTED_EDGE ( 'NONE', *, *, #57893, .T. ) ;
#28648 = CARTESIAN_POINT ( 'NONE',  ( -3.152548672688508926E-16, -90.56249999863440792, -5.148502694627439702 ) ) ;
#28649 = CARTESIAN_POINT ( 'NONE',  ( -1.994931997373328159E-14, -8.660254037844390851, -1.000000000000000888 ) ) ;
#28650 = CARTESIAN_POINT ( 'NONE',  ( 5.000000000000000000, -12.37499999726881050, -6.123233995736766282E-16 ) ) ;
#28651 = CARTESIAN_POINT ( 'NONE',  ( -4.458734124999999437, -12.39583333196774184, -2.574251347313719407 ) ) ;
#28652 = CARTESIAN_POINT ( 'NONE',  ( -58.80597590150559739, -154.1250000027312126, 3.242614290531460330 ) ) ;
#28653 = CARTESIAN_POINT ( 'NONE',  ( -5.000000000000000000, -73.08333333333332860, -2.886751345948128211 ) ) ;
#28654 = CARTESIAN_POINT ( 'NONE',  ( -57.19623071787017210, -154.3750000013656063, 4.297418129356382899 ) ) ;
#28655 = CARTESIAN_POINT ( 'NONE',  ( -2.500000000000000444, -38.04166666393548013, -4.330127018922193649 ) ) ;
#28656 = CYLINDRICAL_SURFACE ( 'NONE', #3139, 5.000000000000000000 ) ;
#28657 = CARTESIAN_POINT ( 'NONE',  ( -4.458734124999999437, 20.68750000136559208, 0.000000000000000000 ) ) ;
#28658 = CARTESIAN_POINT ( 'NONE',  ( -6.972266317189433020E-16, -46.12499999726880873, -5.000000000000000000 ) ) ;
#28659 = CARTESIAN_POINT ( 'NONE',  ( -3.152548672688508926E-16, 19.43750000136559208, -5.148502694627439702 ) ) ;
#28660 = CARTESIAN_POINT ( 'NONE',  ( -4.458734124999998549, -55.22916666530107932, 2.574251347313722516 ) ) ;
#28661 = CARTESIAN_POINT ( 'NONE',  ( 9.457646018065525792E-16, -10.31249999863440969, 5.148502694627439702 ) ) ;
#28662 = CARTESIAN_POINT ( 'NONE',  ( -2.500000000000000444, -63.16666666666666430, -4.330127018922193649 ) ) ;
#28663 = CARTESIAN_POINT ( 'NONE',  ( -2.499999999999996447, 9.166666666666666075, 4.330127018922195425 ) ) ;
#28664 = CARTESIAN_POINT ( 'NONE',  ( -4.458734125000001214, -167.8750000013656063, 1.846868145590734089 ) ) ;
#28665 = CARTESIAN_POINT ( 'NONE',  ( 9.457646018065525792E-16, -53.06249999863441502, 5.148502694627439702 ) ) ;
#28666 = CARTESIAN_POINT ( 'NONE',  ( -2.500000000000000444, -82.04166666393547303, -4.330127018922193649 ) ) ;
#28667 = EDGE_CURVE ( 'NONE', #176, #21872, #39392, .T. ) ;
#28668 = CARTESIAN_POINT ( 'NONE',  ( -50.40829686548195099, -134.2500000013656063, -1.485763867205728284 ) ) ;
#28669 = CARTESIAN_POINT ( 'NONE',  ( -6.972266317189433020E-16, -14.12499999726881228, -5.000000000000000000 ) ) ;
#28670 = DIRECTION ( 'NONE',  ( -0.000000000000000000, 1.000000000000000000, -0.000000000000000000 ) ) ;
#28671 = CARTESIAN_POINT ( 'NONE',  ( -3.152548672688508926E-16, -91.81249999863442213, -5.148502694627439702 ) ) ;
#28672 = CARTESIAN_POINT ( 'NONE',  ( 4.458734124999997661, -158.7500000013656063, 1.846868145590737864 ) ) ;
#28673 = CARTESIAN_POINT ( 'NONE',  ( -2.500000000000000444, -38.16666666666667140, -4.330127018922193649 ) ) ;
#28674 = CARTESIAN_POINT ( 'NONE',  ( -58.24261429053147765, -140.2500000000000000, -3.805975901505573855 ) ) ;
#28675 = CARTESIAN_POINT ( 'NONE',  ( -57.61805966450963012, -135.0000000000000000, -3.717333593771256606 ) ) ;
#28676 = ORIENTED_EDGE ( 'NONE', *, *, #54891, .T. ) ;
#28677 = CARTESIAN_POINT ( 'NONE',  ( 4.458734125000001214, -97.89583333196773651, 2.574251347313718519 ) ) ;
#28678 = CARTESIAN_POINT ( 'NONE',  ( -4.458734124999999437, 6.354166668032259047, -2.574251347313719407 ) ) ;
#28679 = CARTESIAN_POINT ( 'NONE',  ( 5.000000000000000000, 11.62500000273118594, -6.123233995736766282E-16 ) ) ;
#28680 = LINE ( 'NONE', #38032, #49388 ) ;
#28681 = CARTESIAN_POINT ( 'NONE',  ( -2.499999999999996447, 1.166666666666666519, 4.330127018922195425 ) ) ;
#28682 = AXIS2_PLACEMENT_3D ( 'NONE', #61382, #6707, #56556 ) ;
#28683 = CARTESIAN_POINT ( 'NONE',  ( 4.458734124999998549, -59.72916666530106511, -2.574251347313721627 ) ) ;
#28684 = CARTESIAN_POINT ( 'NONE',  ( -55.00000000000001421, -155.0000000000000284, 8.082903768654762899 ) ) ;
#28685 = CARTESIAN_POINT ( 'NONE',  ( -2.499999999999996447, -1.708333330602145761, 4.330127018922195425 ) ) ;
#28686 = CARTESIAN_POINT ( 'NONE',  ( 4.458734125000001214, -30.89583333196773296, 2.574251347313718519 ) ) ;
#28687 = CARTESIAN_POINT ( 'NONE',  ( 5.000000000000000000, 17.70833333606451632, -2.886751345948130876 ) ) ;
#28688 = CARTESIAN_POINT ( 'NONE',  ( -58.24261429053147765, -147.3750000027312126, -3.805975901505573855 ) ) ;
#28689 = EDGE_CURVE ( 'NONE', #41293, #21365, #52175, .T. ) ;
#28690 = CARTESIAN_POINT ( 'NONE',  ( -4.999999999999999112, -46.91666666666665719, 2.886751345948131764 ) ) ;
#28691 = ADVANCED_FACE ( 'NONE', ( #62472 ), #3610, .T. ) ;
#28693 = CARTESIAN_POINT ( 'NONE',  ( 9.457646018065525792E-16, -27.31249999863440436, 5.148502694627439702 ) ) ;
#28692 = CARTESIAN_POINT ( 'NONE',  ( -5.000000000000000000, -89.95833333060214443, -2.886751345948128211 ) ) ;
#28694 = CARTESIAN_POINT ( 'NONE',  ( 5.000000000000000888, -64.58333333333332860, 2.886751345948126879 ) ) ;
#28695 = CARTESIAN_POINT ( 'NONE',  ( 4.458734124999998549, -69.72916666530107932, -2.574251347313721627 ) ) ;
#28696 = CARTESIAN_POINT ( 'NONE',  ( 2.730187237215162345E-16, -147.4375000013656063, -4.458734124999999437 ) ) ;
#28697 = CARTESIAN_POINT ( 'NONE',  ( -2.229367062500000163, -78.47916666530106511, -3.861377020970580443 ) ) ;
#28698 = CARTESIAN_POINT ( 'NONE',  ( -54.64476657466781973, -142.0625000013656063, -4.444560631937228834 ) ) ;
#28699 = CARTESIAN_POINT ( 'NONE',  ( 2.229367062500001939, -24.22916666530107577, 3.861377020970579999 ) ) ;
#28700 =( BOUNDED_CURVE ( )  B_SPLINE_CURVE ( 2, ( #49305, #55417, #49626, #59608, #25822, #754, #25175, #26137, #10061 ),
 .UNSPECIFIED., .F., .F. ) 
 B_SPLINE_CURVE_WITH_KNOTS ( ( 3, 2, 2, 2, 3 ),
 ( 0.4229166666666666630, 0.4236111111111111049, 0.4249999999999999889, 0.4263888888888888729, 0.4270833333333333148 ),
 .UNSPECIFIED. ) 
 CURVE ( )  GEOMETRIC_REPRESENTATION_ITEM ( )  RATIONAL_B_SPLINE_CURVE ( ( 0.9330127018922194093, 0.9330127018922194093, 1.000000000000000000, 0.8660254037844387076, 1.000000000000000000, 0.8660254037844387076, 1.000000000000000000, 0.9330127018922194093, 0.9330127018922194093 ) ) 
 REPRESENTATION_ITEM ( '' )  );
#28701 = CARTESIAN_POINT ( 'NONE',  ( -2.500000000000000444, -64.04166666393547303, -4.330127018922193649 ) ) ;
#28702 = ORIENTED_EDGE ( 'NONE', *, *, #4006, .F. ) ;
#28703 = DIRECTION ( 'NONE',  ( 0.000000000000000000, -1.000000000000000000, 0.000000000000000000 ) ) ;
#28704 = ORIENTED_EDGE ( 'NONE', *, *, #25404, .T. ) ;
#28705 = CARTESIAN_POINT ( 'NONE',  ( 2.229367062499998831, -65.89583333196773651, -3.861377020970580887 ) ) ;
#28706 = CARTESIAN_POINT ( 'NONE',  ( -2.500000000000000444, 7.958333336064518093, -4.330127018922193649 ) ) ;
#28707 = ORIENTED_EDGE ( 'NONE', *, *, #48087, .F. ) ;
#28708 = CARTESIAN_POINT ( 'NONE',  ( -2.500000000000000444, -78.04166666393547303, -4.330127018922193649 ) ) ;
#28709 = EDGE_CURVE ( 'NONE', #61790, #29720, #13874, .T. ) ;
#28710 = CARTESIAN_POINT ( 'NONE',  ( -2.229367062499996610, -60.39583333196774362, 3.861377020970582219 ) ) ;
#28711 = CARTESIAN_POINT ( 'NONE',  ( 2.229367062499998831, 0.1041666680322607397, -3.861377020970580887 ) ) ;
#28712 = VERTEX_POINT ( 'NONE', #28973 ) ;
#28713 = CARTESIAN_POINT ( 'NONE',  ( -9.184850993605147944E-16, -142.2500000000000284, 5.000000000000000000 ) ) ;
#28714 = CARTESIAN_POINT ( 'NONE',  ( 9.457646018065525792E-16, 16.93750000136559564, 5.148502694627439702 ) ) ;
#28715 = CARTESIAN_POINT ( 'NONE',  ( -56.48576386720575471, -145.7500000013655779, -4.591703134518078322 ) ) ;
#28716 = CARTESIAN_POINT ( 'NONE',  ( 5.000000000000000000, -92.29166666393547303, -2.886751345948130876 ) ) ;
#28717 = CARTESIAN_POINT ( 'NONE',  ( 4.458734124999997661, -166.5000000013655779, 1.846868145590737864 ) ) ;
#28718 = STYLED_ITEM ( 'NONE', ( #1933 ), #60912 ) ;
#28719 = ORIENTED_EDGE ( 'NONE', *, *, #12995, .F. ) ;
#28720 = CARTESIAN_POINT ( 'NONE',  ( -4.458734124999999437, -77.39583333196772230, -2.574251347313719407 ) ) ;
#28721 = LINE ( 'NONE', #20354, #22333 ) ;
#28722 = CARTESIAN_POINT ( 'NONE',  ( 2.229367062499998831, 6.354166668032262599, -3.861377020970580887 ) ) ;
#28723 = CARTESIAN_POINT ( 'NONE',  ( 5.000000000000000000, -40.37499999726880162, -6.123233995736766282E-16 ) ) ;
#28724 = CARTESIAN_POINT ( 'NONE',  ( -2.229367062499996610, -66.39583333196773651, 3.861377020970582219 ) ) ;
#28725 = CARTESIAN_POINT ( 'NONE',  ( -4.999999999999999112, -18.79166666393547658, 2.886751345948131764 ) ) ;
#28726 = CARTESIAN_POINT ( 'NONE',  ( 5.000000000000000888, -20.58333333333333215, 2.886751345948126879 ) ) ;
#28727 = CARTESIAN_POINT ( 'NONE',  ( 0.000000000000000000, -120.0000000000000000, 0.000000000000000000 ) ) ;
#28728 = CARTESIAN_POINT ( 'NONE',  ( 2.499999999999998668, -49.33333333333332860, -4.330127018922193649 ) ) ;
#28729 = CARTESIAN_POINT ( 'NONE',  ( -3.535533905932738641, -156.3750000000000000, 3.535533905932737309 ) ) ;
#28730 = DIRECTION ( 'NONE',  ( -0.000000000000000000, 1.000000000000000000, -0.000000000000000000 ) ) ;
#28731 = CARTESIAN_POINT ( 'NONE',  ( 4.458734124999999437, -39.81249999863440081, -5.460374474430324690E-16 ) ) ;
#28732 = CARTESIAN_POINT ( 'NONE',  ( 9.457646018065525792E-16, -25.31249999863440792, 5.148502694627439702 ) ) ;
#28733 = FACE_OUTER_BOUND ( 'NONE', #18194, .T. ) ;
#28734 = CARTESIAN_POINT ( 'NONE',  ( -5.000000000000000000, 23.91666666666666785, -2.886751345948128211 ) ) ;
#28735 = CARTESIAN_POINT ( 'NONE',  ( -2.071067811865475061, -147.8125000027311842, -5.000000000000000888 ) ) ;
#28736 = CARTESIAN_POINT ( 'NONE',  ( -4.458734124999998549, -106.4791666653010651, 2.574251347313722516 ) ) ;
#28737 = CARTESIAN_POINT ( 'NONE',  ( 2.229367062499998831, -29.64583333196773296, -3.861377020970580887 ) ) ;
#28738 = CARTESIAN_POINT ( 'NONE',  ( 2.500000000000002220, -65.54166666393547303, 4.330127018922192761 ) ) ;
#28739 = CARTESIAN_POINT ( 'NONE',  ( -52.10840900171896806, -148.4375000013656063, 3.393966926194110556 ) ) ;
#28740 = CARTESIAN_POINT ( 'NONE',  ( -9.184850993605147944E-16, -142.2500000000000284, 5.000000000000000000 ) ) ;
#28741 = ADVANCED_FACE ( 'NONE', ( #22920 ), #4234, .F. ) ;
#28742 = EDGE_CURVE ( 'NONE', #47984, #39890, #8120, .T. ) ;
#28743 = CARTESIAN_POINT ( 'NONE',  ( 2.229367062499998831, -74.89583333196773651, -3.861377020970580887 ) ) ;
#28744 = CARTESIAN_POINT ( 'NONE',  ( -1.846868145590737420, -168.0000000013656347, 4.458734124999997661 ) ) ;
#28745 = CARTESIAN_POINT ( 'NONE',  ( 2.229367062500001939, -29.97916666530107221, 3.861377020970579999 ) ) ;
#28746 = ADVANCED_FACE ( 'NONE', ( #27723 ), #47350, .T. ) ;
#28747 = FACE_OUTER_BOUND ( 'NONE', #24779, .T. ) ;
#28748 = CARTESIAN_POINT ( 'NONE',  ( 5.000000000000000000, -45.37499999726880873, -6.123233995736766282E-16 ) ) ;
#28749 = CARTESIAN_POINT ( 'NONE',  ( -2.500000000000000444, -20.16666666666666430, -4.330127018922193649 ) ) ;
#28750 = CARTESIAN_POINT ( 'NONE',  ( -1.846868145590734756, -148.1250000013655779, -4.458734125000000326 ) ) ;
#28751 = VERTEX_POINT ( 'NONE', #21495 ) ;
#28752 = CARTESIAN_POINT ( 'NONE',  ( 5.000000000000000888, -89.45833333060215864, 2.886751345948126879 ) ) ;
#28753 = CARTESIAN_POINT ( 'NONE',  ( 1.975475456537005874E-15, 1.250000000000000000, 5.000000000000000000 ) ) ;
#28754 = CARTESIAN_POINT ( 'NONE',  ( -4.458734124999999437, -58.64583333196773651, -2.574251347313719407 ) ) ;
#28755 =( BOUNDED_CURVE ( )  B_SPLINE_CURVE ( 2, ( #2994, #2358, #7495, #46088, #27107, #22611, #56390, #50917, #21968 ),
 .UNSPECIFIED., .F., .F. ) 
 B_SPLINE_CURVE_WITH_KNOTS ( ( 3, 2, 2, 2, 3 ),
 ( 0.6624999999999999778, 0.6630952380952380709, 0.6642857142857142572, 0.6654761904761904434, 0.6660714285714285365 ),
 .UNSPECIFIED. ) 
 CURVE ( )  GEOMETRIC_REPRESENTATION_ITEM ( )  RATIONAL_B_SPLINE_CURVE ( ( 0.9330127018922194093, 0.9330127018922194093, 1.000000000000000000, 0.8660254037844387076, 1.000000000000000000, 0.8660254037844387076, 1.000000000000000000, 0.9330127018922194093, 0.9330127018922194093 ) ) 
 REPRESENTATION_ITEM ( '' )  );
#28756 = EDGE_CURVE ( 'NONE', #4948, #2786, #57473, .T. ) ;
#28757 = CARTESIAN_POINT ( 'NONE',  ( -2.500000000000000444, 25.95833333606451632, -4.330127018922193649 ) ) ;
#28758 = CARTESIAN_POINT ( 'NONE',  ( 1.339745962155615144, 4.419658201469705894, 4.999999999999999112 ) ) ;
#28759 = CARTESIAN_POINT ( 'NONE',  ( -2.499999999999996447, 18.16666666666666430, 4.330127018922195425 ) ) ;
#28760 = ADVANCED_FACE ( 'NONE', ( #19645 ), #14813, .T. ) ;
#28761 = EDGE_CURVE ( 'NONE', #10189, #42151, #11821, .T. ) ;
#28762 = CARTESIAN_POINT ( 'NONE',  ( 9.457646018065525792E-16, -5.062499998634401699, 5.148502694627439702 ) ) ;
#28763 = CARTESIAN_POINT ( 'NONE',  ( -9.184850993605147944E-16, -154.2500000000000000, 5.000000000000000000 ) ) ;
#28764 = CARTESIAN_POINT ( 'NONE',  ( -1.339745962155613812, -41.08034179853029144, -5.000000000000000000 ) ) ;
#28765 = CARTESIAN_POINT ( 'NONE',  ( -2.229367062500000163, 8.270833334698926009, -3.861377020970580443 ) ) ;
#28766 = ADVANCED_FACE ( 'NONE', ( #29280 ), #26306, .F. ) ;
#28767 = EDGE_CURVE ( 'NONE', #26541, #871, #34427, .T. ) ;
#28768 = FACE_OUTER_BOUND ( 'NONE', #27524, .T. ) ;
#28769 = DIRECTION ( 'NONE',  ( 0.000000000000000000, -0.000000000000000000, 1.000000000000000000 ) ) ;
#28770 = CARTESIAN_POINT ( 'NONE',  ( 4.458734125000001214, -56.89583333196774362, 2.574251347313718519 ) ) ;
#28771 = EDGE_CURVE ( 'NONE', #8963, #26541, #15179, .T. ) ;
#28772 = CARTESIAN_POINT ( 'NONE',  ( -3.152801135295367985, -160.0625000013656063, 3.152801135295367096 ) ) ;
#28773 = EDGE_CURVE ( 'NONE', #33543, #29634, #6390, .T. ) ;
#28774 = AXIS2_PLACEMENT_3D ( 'NONE', #47665, #18399, #63104 ) ;
#28775 = B_SPLINE_CURVE_WITH_KNOTS ( 'NONE', 3,
 ( #5263, #44484, #30328, #20704, #15555, #49319, #35810, #25192, #10077 ),
 .UNSPECIFIED., .F., .F.,
 ( 4, 2, 1, 2, 4 ),
 ( 0.000000000000000000, 0.002165063509461097064, 0.004330127018922194128, 0.006495190528383290758, 0.008660254037844389990 ),
 .UNSPECIFIED. ) ;
#28776 = CARTESIAN_POINT ( 'NONE',  ( 5.000000000000000888, -50.45833333060213732, 2.886751345948126879 ) ) ;
#28777 = VERTEX_POINT ( 'NONE', #4856 ) ;
#28778 = CARTESIAN_POINT ( 'NONE',  ( -4.458734124999999437, 3.354166668032260823, -2.574251347313719407 ) ) ;
#28779 = EDGE_LOOP ( 'NONE', ( #11762, #14236, #62039, #10087 ) ) ;
#28781 = CARTESIAN_POINT ( 'NONE',  ( -6.972266317189433020E-16, -12.24999999999999645, -5.000000000000000000 ) ) ;
#28780 = CARTESIAN_POINT ( 'NONE',  ( 0.000000000000000000, -170.0000000000000000, 0.000000000000000000 ) ) ;
#28782 = CARTESIAN_POINT ( 'NONE',  ( -8.190561711645485556E-16, -158.6875000013655779, 4.458734124999999437 ) ) ;
#28783 = ORIENTED_EDGE ( 'NONE', *, *, #28159, .T. ) ;
#28784 = PRODUCT_DEFINITION_CONTEXT ( 'detailed design', #5591, 'design' ) ;
#28785 = CARTESIAN_POINT ( 'NONE',  ( 2.499999999999998668, -23.20833333060214443, -4.330127018922193649 ) ) ;
#28786 = CARTESIAN_POINT ( 'NONE',  ( -57.46284108482265651, -131.9375000000000000, 4.819101127000239515 ) ) ;
#28787 = CARTESIAN_POINT ( 'NONE',  ( 2.499999999999998668, -47.20833333060214443, -4.330127018922193649 ) ) ;
#28788 = CARTESIAN_POINT ( 'NONE',  ( -2.229367062500000163, -36.72916666530107221, -3.861377020970580443 ) ) ;
#28789 = ORIENTED_EDGE ( 'NONE', *, *, #44151, .T. ) ;
#28790 = CARTESIAN_POINT ( 'NONE',  ( -2.229367062500000163, -82.47916666530106511, -3.861377020970580443 ) ) ;
#28791 = CARTESIAN_POINT ( 'NONE',  ( -4.458734124999999437, 21.60416666803225993, -2.574251347313719407 ) ) ;
#28792 = CARTESIAN_POINT ( 'NONE',  ( -3.535533905932737309, -156.7500000027312126, -3.535533905932738197 ) ) ;
#28793 = VERTEX_POINT ( 'NONE', #60103 ) ;
#28794 = CARTESIAN_POINT ( 'NONE',  ( 4.458734124999998549, -86.97916666530106511, -2.574251347313721627 ) ) ;
#28795 = CARTESIAN_POINT ( 'NONE',  ( -50.18089887299979068, -125.8125000027312268, 2.462841084822635640 ) ) ;
#28796 = CARTESIAN_POINT ( 'NONE',  ( -5.000000000000000000, 25.12500000273118417, 0.000000000000000000 ) ) ;
#28797 = CARTESIAN_POINT ( 'NONE',  ( -6.972266317189433020E-16, -7.249999999999998224, -5.000000000000000000 ) ) ;
#28798 =( BOUNDED_CURVE ( )  B_SPLINE_CURVE ( 2, ( #62225, #18143, #37771, #16647, #47726, #51063, #46233, #16967, #60725 ),
 .UNSPECIFIED., .F., .F. ) 
 B_SPLINE_CURVE_WITH_KNOTS ( ( 3, 2, 2, 2, 3 ),
 ( 0.5083333333333337478, 0.5125000000000003997, 0.5166666666666671626, 0.5208333333333338144, 0.5250000000000004663 ),
 .UNSPECIFIED. ) 
 CURVE ( )  GEOMETRIC_REPRESENTATION_ITEM ( )  RATIONAL_B_SPLINE_CURVE ( ( 0.9999999999999918954, 0.9238795325112948431, 1.000000000000000000, 0.9238795325112867385, 1.000000000000000000, 0.9238795325112867385, 1.000000000000000000, 0.9238795325112786339, 1.000000000000008216 ) ) 
 REPRESENTATION_ITEM ( '' )  );
#28799 = CARTESIAN_POINT ( 'NONE',  ( -2.499999999999996447, -44.70833333060214443, 4.330127018922195425 ) ) ;
#28800 = CARTESIAN_POINT ( 'NONE',  ( -2.229367062500000163, -61.47916666530106511, -3.861377020970580443 ) ) ;
#28801 = CARTESIAN_POINT ( 'NONE',  ( -6.972266317189433020E-16, -85.12499999726880162, -5.000000000000000000 ) ) ;
#28802 = CARTESIAN_POINT ( 'NONE',  ( -4.458734124999998549, 22.77083333469892423, 2.574251347313722516 ) ) ;
#28803 = CARTESIAN_POINT ( 'NONE',  ( 5.000000000000000000, -97.50000000000000000, -6.123233995736766282E-16 ) ) ;
#28804 = CARTESIAN_POINT ( 'NONE',  ( -7.703920929261744988, -4.447860822324864571, -7.917989418073275942 ) ) ;
#28805 = CARTESIAN_POINT ( 'NONE',  ( -4.458734124999998549, -46.47916666530107221, 2.574251347313722516 ) ) ;
#28806 = CARTESIAN_POINT ( 'NONE',  ( 5.000000000000000000, -3.374999997268816276, -6.123233995736766282E-16 ) ) ;
#28807 = CARTESIAN_POINT ( 'NONE',  ( -2.499999999999996447, -92.83333333333334281, 4.330127018922195425 ) ) ;
#28808 = CARTESIAN_POINT ( 'NONE',  ( -2.229367062500000163, -84.72916666530107932, -3.861377020970580443 ) ) ;
#28809 = CARTESIAN_POINT ( 'NONE',  ( -4.458734124999997661, -110.2291666653010651, 2.574251347313722516 ) ) ;
#28810 = CARTESIAN_POINT ( 'NONE',  ( 2.229367062499998831, -9.895833331967738289, -3.861377020970580887 ) ) ;
#28811 = ORIENTED_EDGE ( 'NONE', *, *, #14877, .T. ) ;
#28812 = CARTESIAN_POINT ( 'NONE',  ( 1.975475456537005874E-15, -52.75000000000000000, 5.000000000000000000 ) ) ;
#28813 = CARTESIAN_POINT ( 'NONE',  ( 4.458734124999998549, -100.7291666653010651, -2.574251347313721627 ) ) ;
#28814 = CARTESIAN_POINT ( 'NONE',  ( -5.000000000000000000, -160.6250000027311842, -6.123233995736766282E-16 ) ) ;
#28815 = CARTESIAN_POINT ( 'NONE',  ( 4.458734124999999437, -93.06249999863440792, -5.460374474430324690E-16 ) ) ;
#28816 = MANIFOLD_SOLID_BREP ( 'Cavity1', #5842 ) ;
#28817 = CARTESIAN_POINT ( 'NONE',  ( 5.000000000000000888, -49.45833333060213732, 2.886751345948126879 ) ) ;
#28818 = CARTESIAN_POINT ( 'NONE',  ( 0.000000000000000000, -170.0000000000000000, 0.000000000000000000 ) ) ;
#28819 = CARTESIAN_POINT ( 'NONE',  ( -58.39396692619412477, -130.4375000013656063, 2.891590998281057701 ) ) ;
#28820 = CARTESIAN_POINT ( 'NONE',  ( -56.48576386720575471, -147.7500000013656063, -4.591703134518078322 ) ) ;
#28821 = CARTESIAN_POINT ( 'NONE',  ( 4.458734125000000326, -19.89583333196774007, 2.574251347313718519 ) ) ;
#28822 = CARTESIAN_POINT ( 'NONE',  ( -2.229367062500000163, 10.27083333469892779, -3.861377020970580443 ) ) ;
#28823 = CARTESIAN_POINT ( 'NONE',  ( -4.458734124999999437, -61.56249999863440081, 0.000000000000000000 ) ) ;
#28824 = FACE_OUTER_BOUND ( 'NONE', #59830, .T. ) ;
#28825 = CARTESIAN_POINT ( 'NONE',  ( -2.229367062500000163, -12.47916666530107044, -3.861377020970580443 ) ) ;
#28826 = CARTESIAN_POINT ( 'NONE',  ( 1.975475456537005874E-15, -36.62499999726880873, 5.000000000000000000 ) ) ;
#28827 = CARTESIAN_POINT ( 'NONE',  ( 3.535533905932738197, -154.8750000000000000, -3.535533905932738197 ) ) ;
#28828 = VERTEX_POINT ( 'NONE', #14496 ) ;
#28829 = CARTESIAN_POINT ( 'NONE',  ( -4.458734124999997661, -39.47916666530106511, 2.574251347313722516 ) ) ;
#28830 = CARTESIAN_POINT ( 'NONE',  ( 6.123233995736766282E-16, -120.0000000000000000, -5.000000000000000000 ) ) ;
#28831 = CARTESIAN_POINT ( 'NONE',  ( -2.499999999999996447, -11.83333333333333393, 4.330127018922195425 ) ) ;
#28832 = CYLINDRICAL_SURFACE ( 'NONE', #62461, 5.000000000000000000 ) ;
#28833 = CARTESIAN_POINT ( 'NONE',  ( -2.229367062500000163, -84.47916666530107932, -3.861377020970580443 ) ) ;
#28834 = CARTESIAN_POINT ( 'NONE',  ( 4.458734124999999437, 16.93750000136559564, -5.460374474430324690E-16 ) ) ;
#28835 = CARTESIAN_POINT ( 'NONE',  ( -4.458734124999999437, 8.604166668032261711, -2.574251347313719407 ) ) ;
#28836 = CARTESIAN_POINT ( 'NONE',  ( -5.000000000000000000, 6.999999999999999112, 0.000000000000000000 ) ) ;
#28837 = CARTESIAN_POINT ( 'NONE',  ( -1.339745962155610925, -68.79465819873850307, 5.000000000000000000 ) ) ;
#28838 = CYLINDRICAL_SURFACE ( 'NONE', #5744, 5.000000000000000000 ) ;
#28839 = CARTESIAN_POINT ( 'NONE',  ( 5.000000000000000000, -70.41666666666667140, -2.886751345948129988 ) ) ;
#28840 = CARTESIAN_POINT ( 'NONE',  ( 5.000000000000000000, 12.70833333606451809, -2.886751345948129988 ) ) ;
#28842 = EDGE_LOOP ( 'NONE', ( #30150, #17143 ) ) ;
#28841 = EDGE_CURVE ( 'NONE', #10579, #57689, #56719, .T. ) ;
#28843 = DIRECTION ( 'NONE',  ( -0.000000000000000000, 1.000000000000000000, -0.000000000000000000 ) ) ;
#28844 = ORIENTED_EDGE ( 'NONE', *, *, #52476, .T. ) ;
#28845 = LINE ( 'NONE', #25216, #31998 ) ;
#28847 = CARTESIAN_POINT ( 'NONE',  ( 1.060575238724906964E-15, -29.74999999999999645, 5.773502691896257311 ) ) ;
#28846 = CARTESIAN_POINT ( 'NONE',  ( 2.500000000000002220, -85.66666666666667140, 4.330127018922192761 ) ) ;
#28848 = CARTESIAN_POINT ( 'NONE',  ( -2.229367062500000163, -34.47916666530107221, -3.861377020970580443 ) ) ;
#28849 = EDGE_CURVE ( 'NONE', #50783, #34309, #3457, .T. ) ;
#28850 = CARTESIAN_POINT ( 'NONE',  ( -5.000000000000000000, -31.95833333060214443, -2.886751345948128211 ) ) ;
#28852 = EDGE_LOOP ( 'NONE', ( #30021, #31055, #30696, #22390 ) ) ;
#28851 = CARTESIAN_POINT ( 'NONE',  ( 2.229367062499998831, -64.64583333196773651, -3.861377020970580887 ) ) ;
#28853 = CARTESIAN_POINT ( 'NONE',  ( -54.64476657466781973, -153.0625000013656063, -4.444560631937228834 ) ) ;
#28855 = ORIENTED_EDGE ( 'NONE', *, *, #37404, .T. ) ;
#28854 = CARTESIAN_POINT ( 'NONE',  ( 4.458734125000001214, -13.14583333196774184, 2.574251347313718519 ) ) ;
#28856 = CARTESIAN_POINT ( 'NONE',  ( -3.535250795749689387E-16, -79.25000000000000000, -5.773502691896257311 ) ) ;
#28857 = CARTESIAN_POINT ( 'NONE',  ( 5.000000000000000888, 28.54166666939784847, 2.886751345948126879 ) ) ;
#28858 = CARTESIAN_POINT ( 'NONE',  ( 4.458734124999998549, -58.97916666530105800, -2.574251347313721627 ) ) ;
#28859 = CARTESIAN_POINT ( 'NONE',  ( 1.060575238724906964E-15, -80.62499999726881583, 5.773502691896257311 ) ) ;
#28861 = ORIENTED_EDGE ( 'NONE', *, *, #42941, .T. ) ;
#28860 = CARTESIAN_POINT ( 'NONE',  ( -2.499999999999996447, -31.83333333333333215, 4.330127018922195425 ) ) ;
#28862 = AXIS2_PLACEMENT_3D ( 'NONE', #3475, #23088, #42692 ) ;
#28863 = CARTESIAN_POINT ( 'NONE',  ( -53.33387254593733928, -146.8125000000000284, 5.149110718188519620 ) ) ;
#28864 = CARTESIAN_POINT ( 'NONE',  ( 2.229367062499998831, -23.89583333196773651, -3.861377020970580887 ) ) ;
#28866 = ORIENTED_EDGE ( 'NONE', *, *, #45252, .F. ) ;
#28865 = CARTESIAN_POINT ( 'NONE',  ( 2.229367062500001939, -60.22916666530106511, 3.861377020970579999 ) ) ;
#28867 = DIRECTION ( 'NONE',  ( 1.000000000000000000, 0.000000000000000000, 0.000000000000000000 ) ) ;
#28868 = CARTESIAN_POINT ( 'NONE',  ( 1.846868145590736310, -166.8750000013655779, 4.458734124999999437 ) ) ;
#28869 = CARTESIAN_POINT ( 'NONE',  ( 2.229367062499998831, -102.8958333319677365, -3.861377020970580887 ) ) ;
#28870 = CARTESIAN_POINT ( 'NONE',  ( -59.98410592259440222, -135.2500000027312126, -0.3983568153799752487 ) ) ;
#28871 = VERTEX_POINT ( 'NONE', #36917 ) ;
#28872 = CARTESIAN_POINT ( 'NONE',  ( -59.44456063193725015, -150.8125000013656063, -0.3552334253322034230 ) ) ;
#28873 = CARTESIAN_POINT ( 'NONE',  ( -52.53715891517739323, -140.5625000027311842, -4.819101127000233298 ) ) ;
#28874 = CARTESIAN_POINT ( 'NONE',  ( 4.458734125000000326, -38.89583333196773651, 2.574251347313718519 ) ) ;
#28875 = CARTESIAN_POINT ( 'NONE',  ( 1.975475456537005874E-15, -58.62499999726880162, 5.000000000000000000 ) ) ;
#28876 = CARTESIAN_POINT ( 'NONE',  ( -2.229367062499996610, -13.14583333196774007, 3.861377020970582219 ) ) ;
#28877 =( BOUNDED_CURVE ( )  B_SPLINE_CURVE ( 2, ( #34340, #25018, #53965, #30146, #9896, #29505, #24702, #5402, #44628 ),
 .UNSPECIFIED., .F., .F. ) 
 B_SPLINE_CURVE_WITH_KNOTS ( ( 3, 2, 2, 2, 3 ),
 ( 0.8083333333333331261, 0.8124999999999997780, 0.8166666666666664298, 0.8208333333333330817, 0.8249999999999997335 ),
 .UNSPECIFIED. ) 
 CURVE ( )  GEOMETRIC_REPRESENTATION_ITEM ( )  RATIONAL_B_SPLINE_CURVE ( ( 1.000000000000003997, 0.9238795325112826307, 1.000000000000000000, 0.9238795325112867385, 1.000000000000000000, 0.9238795325112867385, 1.000000000000000000, 0.9238795325112908463, 0.9999999999999958922 ) ) 
 REPRESENTATION_ITEM ( '' )  );
#28878 = CARTESIAN_POINT ( 'NONE',  ( -2.229367062500000163, -99.72916666530106511, -3.861377020970580443 ) ) ;
#28879 = CARTESIAN_POINT ( 'NONE',  ( 3.152801135295367541, -142.5625000013655779, -3.152801135295367541 ) ) ;
#28880 = CARTESIAN_POINT ( 'NONE',  ( 2.229367062499998831, -27.89583333196774007, -3.861377020970580887 ) ) ;
#28881 = CARTESIAN_POINT ( 'NONE',  ( 5.000000000000000000, -70.50000000000000000, -6.123233995736766282E-16 ) ) ;
#28882 = CARTESIAN_POINT ( 'NONE',  ( -52.10840900171896806, -131.1875000013656063, 3.393966926194110556 ) ) ;
#28883 = CARTESIAN_POINT ( 'NONE',  ( -3.152548672688508926E-16, -68.81249999863439371, -5.148502694627439702 ) ) ;
#28884 = CARTESIAN_POINT ( 'NONE',  ( -6.972266317189433020E-16, -17.25000000000000000, -5.000000000000000000 ) ) ;
#28885 = CARTESIAN_POINT ( 'NONE',  ( -1.339745962155613812, -70.20534180126148271, -5.000000000000000000 ) ) ;
#28886 = CARTESIAN_POINT ( 'NONE',  ( 3.152801135295367541, -141.3125000013655779, -3.152801135295367541 ) ) ;
#28887 = CARTESIAN_POINT ( 'NONE',  ( 2.229367062499998831, 3.104166668032259935, -3.861377020970580887 ) ) ;
#28888 = ORIENTED_EDGE ( 'NONE', *, *, #7948, .F. ) ;
#28889 = CARTESIAN_POINT ( 'NONE',  ( -1.339745962155610925, -70.66965819600731891, 5.000000000000000000 ) ) ;
#28890 = CARTESIAN_POINT ( 'NONE',  ( 5.000000000000000000, 2.499999999999998668, -6.123233995736766282E-16 ) ) ;
#28892 = CARTESIAN_POINT ( 'NONE',  ( 2.229367062500001939, -28.97916666530107221, 3.861377020970579999 ) ) ;
#28891 = CARTESIAN_POINT ( 'NONE',  ( 1.060575238724906964E-15, -97.75000000000000000, 5.773502691896257311 ) ) ;
#28893 = CARTESIAN_POINT ( 'NONE',  ( -1.339745962155613812, -77.08034179853029855, -5.000000000000000000 ) ) ;
#28894 = CARTESIAN_POINT ( 'NONE',  ( -3.152548672688508926E-16, -73.81249999863440792, -5.148502694627439702 ) ) ;
#28895 = CARTESIAN_POINT ( 'NONE',  ( -4.458734124999999437, 24.35416666803225993, -2.574251347313719407 ) ) ;
#28896 = CARTESIAN_POINT ( 'NONE',  ( -6.972266317189433020E-16, -18.25000000000000000, -5.000000000000000000 ) ) ;
#28898 = EDGE_CURVE ( 'NONE', #29821, #1507, #61371, .T. ) ;
#28897 = CARTESIAN_POINT ( 'NONE',  ( -59.29741812935640155, -141.6250000013656063, -2.196230717870135685 ) ) ;
#28899 = CARTESIAN_POINT ( 'NONE',  ( -2.229367062499996610, 2.854166668032259935, 3.861377020970582219 ) ) ;
#28900 = CARTESIAN_POINT ( 'NONE',  ( -4.458734124999998549, 25.52083333469893134, 2.574251347313722516 ) ) ;
#28901 = CARTESIAN_POINT ( 'NONE',  ( 9.457646018065525792E-16, -44.31249999863440081, 5.148502694627439702 ) ) ;
#28902 = DIRECTION ( 'NONE',  ( -0.000000000000000000, 1.000000000000000000, -0.000000000000000000 ) ) ;
#28903 = CARTESIAN_POINT ( 'NONE',  ( 4.458734124999999437, -0.8124999986344055847, -5.460374474430324690E-16 ) ) ;
#28904 = ORIENTED_EDGE ( 'NONE', *, *, #54153, .F. ) ;
#28905 = CARTESIAN_POINT ( 'NONE',  ( 4.458734125000000326, -27.14583333196774717, 2.574251347313718519 ) ) ;
#28906 = CARTESIAN_POINT ( 'NONE',  ( 4.458734124999999437, -157.5000000013656063, 1.846868145590737864 ) ) ;
#28907 = VECTOR ( 'NONE', #20967, 1000.000000000000000 ) ;
#28908 = CARTESIAN_POINT ( 'NONE',  ( 4.458734124999999437, -70.81249999863439371, -5.460374474430324690E-16 ) ) ;
#28909 = CARTESIAN_POINT ( 'NONE',  ( -3.535250795749689387E-16, -104.1249999972688158, -5.773502691896257311 ) ) ;
#28910 = CARTESIAN_POINT ( 'NONE',  ( -4.458734124999997661, -105.4791666653010509, 2.574251347313722516 ) ) ;
#28911 = CARTESIAN_POINT ( 'NONE',  ( 4.458734125000000326, -71.14583333196773651, 2.574251347313718519 ) ) ;
#28912 = CARTESIAN_POINT ( 'NONE',  ( 5.000000000000000888, -53.58333333333333570, 2.886751345948126879 ) ) ;
#28913 = CARTESIAN_POINT ( 'NONE',  ( -1.339745962155610925, -21.79465819873851729, 5.000000000000000000 ) ) ;
#28914 = FACE_OUTER_BOUND ( 'NONE', #34382, .T. ) ;
#28915 = EDGE_LOOP ( 'NONE', ( #5546, #45487, #45514, #57316 ) ) ;
#28916 = CARTESIAN_POINT ( 'NONE',  ( 3.061616997868383141E-16, -140.7500000000000000, -5.000000000000000000 ) ) ;
#28917 = CARTESIAN_POINT ( 'NONE',  ( -51.75738570946856498, -155.0000000000000284, 3.805975901505577408 ) ) ;
#28918 = CARTESIAN_POINT ( 'NONE',  ( -5.000000000000000000, -15.08333333333333215, -2.886751345948128211 ) ) ;
#28919 = CARTESIAN_POINT ( 'NONE',  ( 2.229367062499998831, -16.64583333196773651, -3.861377020970580887 ) ) ;
#28920 = CARTESIAN_POINT ( 'NONE',  ( -3.152548672688508926E-16, -78.56249999863440792, -5.148502694627439702 ) ) ;
#28921 = CARTESIAN_POINT ( 'NONE',  ( 3.152801135295366208, -167.8125000013656063, 3.152801135295367985 ) ) ;
#28922 = CARTESIAN_POINT ( 'NONE',  ( -3.535250795749689387E-16, -16.12499999726881228, -5.773502691896257311 ) ) ;
#28924 = ORIENTED_EDGE ( 'NONE', *, *, #55435, .T. ) ;
#28923 = CARTESIAN_POINT ( 'NONE',  ( -2.229367062500000163, -48.47916666530106511, -3.861377020970580443 ) ) ;
#28925 = CARTESIAN_POINT ( 'NONE',  ( -6.972266317189433020E-16, -15.12499999726881050, -5.000000000000000000 ) ) ;
#28927 = ORIENTED_EDGE ( 'NONE', *, *, #33847, .F. ) ;
#28926 = CARTESIAN_POINT ( 'NONE',  ( 9.457646018065525792E-16, -0.3124999986344051961, 5.148502694627439702 ) ) ;
#28928 = CARTESIAN_POINT ( 'NONE',  ( -50.70258187064364108, -152.1250000013656063, 2.196230717870141014 ) ) ;
#28929 = CARTESIAN_POINT ( 'NONE',  ( 1.060575238724906964E-15, -60.75000000000000000, 5.773502691896257311 ) ) ;
#28930 = CARTESIAN_POINT ( 'NONE',  ( 3.152801135295366208, -157.8125000013656063, 3.152801135295367985 ) ) ;
#28931 = CARTESIAN_POINT ( 'NONE',  ( 9.457646018065525792E-16, -39.31249999863439371, 5.148502694627439702 ) ) ;
#28932 = LINE ( 'NONE', #48238, #34802 ) ;
#28933 = CARTESIAN_POINT ( 'NONE',  ( -5.000000000000000000, -161.5000000000000000, -6.123233995736766282E-16 ) ) ;
#28934 = CARTESIAN_POINT ( 'NONE',  ( -51.60603307380591787, -129.1875000013656063, -2.891590998281053704 ) ) ;
#28935 = CARTESIAN_POINT ( 'NONE',  ( -2.229367062500000163, -5.729166665301072214, -3.861377020970580443 ) ) ;
#28936 = CARTESIAN_POINT ( 'NONE',  ( 2.229367062499998831, -47.89583333196774362, -3.861377020970580887 ) ) ;
#28937 = CARTESIAN_POINT ( 'NONE',  ( -51.75738570946856498, -155.0000000000000284, 3.805975901505577408 ) ) ;
#28938 = CARTESIAN_POINT ( 'NONE',  ( 2.730187237215162345E-16, -150.1875000013656063, -4.458734124999999437 ) ) ;
#28939 = CARTESIAN_POINT ( 'NONE',  ( -4.458734124999999437, -86.64583333196773651, -2.574251347313719407 ) ) ;
#28940 = CARTESIAN_POINT ( 'NONE',  ( -58.24261429053147765, -155.0000000000000284, -3.805975901505573411 ) ) ;
#28941 = VERTEX_POINT ( 'NONE', #17619 ) ;
#28942 = CARTESIAN_POINT ( 'NONE',  ( 5.000000000000000000, -155.1875000027312126, 2.071067811865478614 ) ) ;
#28943 = CARTESIAN_POINT ( 'NONE',  ( -4.999999999999998224, -68.79166666393547303, 2.886751345948131764 ) ) ;
#28944 = CARTESIAN_POINT ( 'NONE',  ( -51.19402409849444524, -150.6250000027312126, -3.242614290531456334 ) ) ;
#28945 =( BOUNDED_CURVE ( )  B_SPLINE_CURVE ( 2, ( #1240, #25020, #55258, #30800, #3367, #55580, #56768, #12689, #41076 ),
 .UNSPECIFIED., .F., .F. ) 
 B_SPLINE_CURVE_WITH_KNOTS ( ( 3, 2, 2, 2, 3 ),
 ( 0.4232142857142857095, 0.4238095238095238027, 0.4249999999999999889, 0.4261904761904761751, 0.4267857142857142683 ),
 .UNSPECIFIED. ) 
 CURVE ( )  GEOMETRIC_REPRESENTATION_ITEM ( )  RATIONAL_B_SPLINE_CURVE ( ( 0.9330127018922194093, 0.9330127018922194093, 1.000000000000000000, 0.8660254037844387076, 1.000000000000000000, 0.8660254037844387076, 1.000000000000000000, 0.9330127018922194093, 0.9330127018922194093 ) ) 
 REPRESENTATION_ITEM ( '' )  );
#28946 = CARTESIAN_POINT ( 'NONE',  ( 1.339745962155612702, -43.29465819873851729, -5.000000000000000000 ) ) ;
#28947 = ADVANCED_FACE ( 'NONE', ( #2210 ), #61688, .T. ) ;
#28948 = ORIENTED_EDGE ( 'NONE', *, *, #48776, .F. ) ;
#28949 = CYLINDRICAL_SURFACE ( 'NONE', #44163, 5.000000000000000000 ) ;
#28950 = CARTESIAN_POINT ( 'NONE',  ( -2.229367062499996610, -10.39583333196773829, 3.861377020970582219 ) ) ;
#28951 = CARTESIAN_POINT ( 'NONE',  ( -52.53715891517739323, -150.5625000027311842, -4.819101127000233298 ) ) ;
#28952 = CARTESIAN_POINT ( 'NONE',  ( -3.152548672688508926E-16, -1.562499998634406140, -5.148502694627439702 ) ) ;
#28953 = CARTESIAN_POINT ( 'NONE',  ( -6.972266317189433020E-16, -12.12499999726881406, -5.000000000000000000 ) ) ;
#28954 = CARTESIAN_POINT ( 'NONE',  ( -4.458734125000000326, -151.8750000013655779, 1.846868145590734089 ) ) ;
#28955 = CARTESIAN_POINT ( 'NONE',  ( 4.458734124999998549, 20.02083333469892779, -2.574251347313721627 ) ) ;
#28956 = VERTEX_POINT ( 'NONE', #62001 ) ;
#28957 = CARTESIAN_POINT ( 'NONE',  ( 2.229367062500001939, -89.97916666530106511, 3.861377020970579999 ) ) ;
#28958 = CARTESIAN_POINT ( 'NONE',  ( 3.061616997868383141E-16, -148.7500000000000284, -5.000000000000000000 ) ) ;
#28959 = CARTESIAN_POINT ( 'NONE',  ( 2.499999999999998668, -40.33333333333332860, -4.330127018922193649 ) ) ;
#28960 = CARTESIAN_POINT ( 'NONE',  ( 4.458734124999998549, -12.72916666530107044, -2.574251347313721627 ) ) ;
#28961 = CARTESIAN_POINT ( 'NONE',  ( -6.972266317189433020E-16, -85.12499999726880162, -5.000000000000000000 ) ) ;
#28962 = CARTESIAN_POINT ( 'NONE',  ( -1.339745962155727277, -72.79465819873851729, 4.999999999999933387 ) ) ;
#28963 = CARTESIAN_POINT ( 'NONE',  ( -50.55543936806279248, -152.0625000013656063, 0.3552334253322060320 ) ) ;
#28964 = CARTESIAN_POINT ( 'NONE',  ( -2.499999999999996447, -41.70833333060214443, 4.330127018922195425 ) ) ;
#28965 = CARTESIAN_POINT ( 'NONE',  ( 5.000000000000000000, -29.41666666666666785, -2.886751345948130876 ) ) ;
#28966 = CARTESIAN_POINT ( 'NONE',  ( 2.229367062500001939, 21.02083333469892779, 3.861377020970579999 ) ) ;
#28967 = CARTESIAN_POINT ( 'NONE',  ( -2.499999999999996447, 12.29166666939785202, 4.330127018922195425 ) ) ;
#28968 = ORIENTED_EDGE ( 'NONE', *, *, #45520, .F. ) ;
#28969 = CARTESIAN_POINT ( 'NONE',  ( 4.458734125000000326, 15.10416666803225993, 2.574251347313718519 ) ) ;
#28970 = CARTESIAN_POINT ( 'NONE',  ( 2.229367062500001939, -62.97916666530106511, 3.861377020970579999 ) ) ;
#28971 = CARTESIAN_POINT ( 'NONE',  ( 4.458734124999999437, -9.062499998634406140, -5.460374474430324690E-16 ) ) ;
#28972 =( BOUNDED_CURVE ( )  B_SPLINE_CURVE ( 2, ( #44459, #11004, #49612, #34479, #5551, #25163, #44777, #6196, #25811 ),
 .UNSPECIFIED., .F., .F. ) 
 B_SPLINE_CURVE_WITH_KNOTS ( ( 3, 2, 2, 2, 3 ),
 ( 0.2562499999999999778, 0.2569444444444444198, 0.2583333333333333592, 0.2597222222222222432, 0.2604166666666666852 ),
 .UNSPECIFIED. ) 
 CURVE ( )  GEOMETRIC_REPRESENTATION_ITEM ( )  RATIONAL_B_SPLINE_CURVE ( ( 0.9330127018922194093, 0.9330127018922194093, 1.000000000000000000, 0.8660254037844387076, 1.000000000000000000, 0.8660254037844387076, 1.000000000000000000, 0.9330127018922194093, 0.9330127018922194093 ) ) 
 REPRESENTATION_ITEM ( '' )  );
#28973 = CARTESIAN_POINT ( 'NONE',  ( -51.75738570946856498, -152.7500000000000284, 3.805975901505576964 ) ) ;
#28974 = CARTESIAN_POINT ( 'NONE',  ( 5.000000000000000000, 10.58333333333333393, -2.886751345948129988 ) ) ;
#28975 = CARTESIAN_POINT ( 'NONE',  ( 4.458734124999999437, -167.4375000013655779, 0.000000000000000000 ) ) ;
#28976 = CARTESIAN_POINT ( 'NONE',  ( 2.500000000000002220, -88.66666666666665719, 4.330127018922192761 ) ) ;
#28977 = CARTESIAN_POINT ( 'NONE',  ( -4.458734124999999437, -53.31249999863439371, 0.000000000000000000 ) ) ;
#28978 = CARTESIAN_POINT ( 'NONE',  ( 5.000000000000000000, -88.29166666393547303, -2.886751345948129988 ) ) ;
#28979 = CARTESIAN_POINT ( 'NONE',  ( -52.80376928212989185, -133.1250000013656063, -4.297418129356379346 ) ) ;
#28980 = CARTESIAN_POINT ( 'NONE',  ( -6.972266317189433020E-16, -67.25000000000000000, -5.000000000000000000 ) ) ;
#28981 = CARTESIAN_POINT ( 'NONE',  ( -2.499999999999996447, -91.83333333333334281, 4.330127018922195425 ) ) ;
#28982 = CARTESIAN_POINT ( 'NONE',  ( 2.229367062500001939, -89.22916666530106511, 3.861377020970579999 ) ) ;
#28983 = CARTESIAN_POINT ( 'NONE',  ( 2.730187237215162345E-16, -154.4375000013655779, -4.458734124999999437 ) ) ;
#28984 = CARTESIAN_POINT ( 'NONE',  ( -5.000000000000000000, -39.08333333333332860, -2.886751345948128211 ) ) ;
#28985 = CARTESIAN_POINT ( 'NONE',  ( -9.184850993605147944E-16, -163.2500000000000000, 5.000000000000000000 ) ) ;
#28986 = VERTEX_POINT ( 'NONE', #37235 ) ;
#28987 = CARTESIAN_POINT ( 'NONE',  ( -4.458734124999999437, -102.3124999986344079, 0.000000000000000000 ) ) ;
#28988 = CARTESIAN_POINT ( 'NONE',  ( -3.152548672688508926E-16, 8.187500001365595637, -5.148502694627439702 ) ) ;
#28989 = CARTESIAN_POINT ( 'NONE',  ( 3.061616997868383141E-16, -161.7500000000000000, -5.000000000000000000 ) ) ;
#28990 = CARTESIAN_POINT ( 'NONE',  ( 5.000000000000000000, 4.583333333333331261, -2.886751345948129988 ) ) ;
#28991 = CARTESIAN_POINT ( 'NONE',  ( -4.458734124999999437, -62.39583333196774362, -2.574251347313719407 ) ) ;
#28992 = CARTESIAN_POINT ( 'NONE',  ( 1.975475456537005874E-15, 20.24999999999999289, 5.000000000000000000 ) ) ;
#28993 = CARTESIAN_POINT ( 'NONE',  ( 1.060575238724906964E-15, -1.624999997268814500, 5.773502691896257311 ) ) ;
#28994 = CARTESIAN_POINT ( 'NONE',  ( 9.457646018065525792E-16, -30.06249999863440081, 5.148502694627439702 ) ) ;
#28995 = CARTESIAN_POINT ( 'NONE',  ( -1.339745962155613812, -11.20534180126147916, -5.000000000000000000 ) ) ;
#28996 = DIRECTION ( 'NONE',  ( 0.000000000000000000, 0.000000000000000000, 1.000000000000000000 ) ) ;
#28997 = CARTESIAN_POINT ( 'NONE',  ( 1.975475456537005874E-15, -19.75000000000000000, 5.000000000000000000 ) ) ;
#28998 = CARTESIAN_POINT ( 'NONE',  ( -5.000000000000000000, -47.08333333333333570, -2.886751345948128211 ) ) ;
#29000 = CARTESIAN_POINT ( 'NONE',  ( -4.458734124999999437, -25.56249999863440792, 0.000000000000000000 ) ) ;
#28999 = CARTESIAN_POINT ( 'NONE',  ( 5.000000000000000000, 6.708333336064521646, -2.886751345948130876 ) ) ;
#29001 = CARTESIAN_POINT ( 'NONE',  ( 1.975475456537005874E-15, -64.74999999999998579, 5.000000000000000000 ) ) ;
#29002 = CARTESIAN_POINT ( 'NONE',  ( -2.229367062500000163, -69.47916666530107932, -3.861377020970580443 ) ) ;
#29003 = CARTESIAN_POINT ( 'NONE',  ( 4.458734125000000326, -143.6250000013656347, -1.846868145590734978 ) ) ;
#29004 = CARTESIAN_POINT ( 'NONE',  ( 4.458734124999999437, -78.81249999863440792, -5.460374474430324690E-16 ) ) ;
#29005 = CARTESIAN_POINT ( 'NONE',  ( -51.60603307380591787, -138.1875000013656347, -2.891590998281053704 ) ) ;
#29006 = CARTESIAN_POINT ( 'NONE',  ( -2.229367062500000163, -23.72916666530107577, -3.861377020970580443 ) ) ;
#29007 = CARTESIAN_POINT ( 'NONE',  ( 2.500000000000002220, -67.54166666393547303, 4.330127018922192761 ) ) ;
#29008 = ORIENTED_EDGE ( 'NONE', *, *, #17227, .F. ) ;
#29009 = CARTESIAN_POINT ( 'NONE',  ( -59.81910112700027327, -148.3125000027311557, -2.462841084822540605 ) ) ;
#29010 = ORIENTED_EDGE ( 'NONE', *, *, #10698, .T. ) ;
#29011 = CARTESIAN_POINT ( 'NONE',  ( 4.458734124999999437, -73.06249999863439371, -5.460374474430324690E-16 ) ) ;
#29012 = CARTESIAN_POINT ( 'NONE',  ( 3.061616997868383141E-16, -165.7500000000000000, -5.000000000000000000 ) ) ;
#29013 = ORIENTED_EDGE ( 'NONE', *, *, #61587, .T. ) ;
#29014 = CARTESIAN_POINT ( 'NONE',  ( 1.339745962155612702, 27.70534180126147561, -5.000000000000000000 ) ) ;
#29015 = MANIFOLD_SOLID_BREP ( 'AdvancedHole2', #25352 ) ;
#29016 = CARTESIAN_POINT ( 'NONE',  ( -6.972266317189433020E-16, -78.12499999726881583, -5.000000000000000000 ) ) ;
#29018 = EDGE_CURVE ( 'NONE', #3585, #16917, #39771, .T. ) ;
#29017 = CARTESIAN_POINT ( 'NONE',  ( -2.229367062499996610, -61.39583333196774362, 3.861377020970582219 ) ) ;
#29019 = CARTESIAN_POINT ( 'NONE',  ( 4.458734124999998549, 2.020833334698927786, -2.574251347313721627 ) ) ;
#29020 = EDGE_LOOP ( 'NONE', ( #44310, #54822, #18344, #46572 ) ) ;
#29021 = CYLINDRICAL_SURFACE ( 'NONE', #30668, 5.000000000000000000 ) ;
#29022 = CARTESIAN_POINT ( 'NONE',  ( -6.972266317189433020E-16, -61.12499999726880162, -5.000000000000000000 ) ) ;
#29023 = CARTESIAN_POINT ( 'NONE',  ( 9.457646018065525792E-16, 11.93750000136559386, 5.148502694627439702 ) ) ;
#29024 = CARTESIAN_POINT ( 'NONE',  ( -52.80376928212989185, -145.8750000013655779, -4.297418129356379346 ) ) ;
#29025 = CARTESIAN_POINT ( 'NONE',  ( -8.190561711645485556E-16, -165.6875000013655779, 4.458734124999999437 ) ) ;
#29026 = ORIENTED_EDGE ( 'NONE', *, *, #29090, .F. ) ;
#29027 = CARTESIAN_POINT ( 'NONE',  ( 9.457646018065525792E-16, -76.06249999863440792, 5.148502694627439702 ) ) ;
#29028 = EDGE_CURVE ( 'NONE', #50534, #5440, #50512, .T. ) ;
#29029 = CARTESIAN_POINT ( 'NONE',  ( 5.000000000000000000, -0.3749999972688135008, -6.123233995736766282E-16 ) ) ;
#29030 = CARTESIAN_POINT ( 'NONE',  ( 2.229367062499998831, 0.3541666680322609340, -3.861377020970580887 ) ) ;
#29031 = DIRECTION ( 'NONE',  ( 0.000000000000000000, 0.000000000000000000, 1.000000000000000000 ) ) ;
#29032 = CARTESIAN_POINT ( 'NONE',  ( 2.229367062499998831, -63.89583333196772941, -3.861377020970580887 ) ) ;
#29033 = CARTESIAN_POINT ( 'NONE',  ( -2.500000000000000444, -26.04166666393547658, -4.330127018922193649 ) ) ;
#29034 = EDGE_CURVE ( 'NONE', #41864, #33407, #13506, .T. ) ;
#29035 = CARTESIAN_POINT ( 'NONE',  ( -1.339745962155610925, 6.205341801261478274, 5.000000000000000000 ) ) ;
#29036 = CARTESIAN_POINT ( 'NONE',  ( 5.000000000000000888, -45.58333333333333570, 2.886751345948126879 ) ) ;
#29037 = CARTESIAN_POINT ( 'NONE',  ( 5.000000000000000888, -61.58333333333333570, 2.886751345948126879 ) ) ;
#29038 = DIRECTION ( 'NONE',  ( -0.000000000000000000, 1.000000000000000000, -0.000000000000000000 ) ) ;
#29039 = CARTESIAN_POINT ( 'NONE',  ( 2.499999999999998668, -43.20833333060214443, -4.330127018922193649 ) ) ;
#29040 = CARTESIAN_POINT ( 'NONE',  ( -4.458734124999999437, -44.39583333196773651, -2.574251347313719407 ) ) ;
#29041 = CARTESIAN_POINT ( 'NONE',  ( -4.458734124999997661, -27.47916666530107221, 2.574251347313722516 ) ) ;
#29042 = CARTESIAN_POINT ( 'NONE',  ( 4.458734124999999437, 6.937500001365594748, -5.460374474430324690E-16 ) ) ;
#29043 = CARTESIAN_POINT ( 'NONE',  ( -5.000000000000000000, 27.00000000000000000, 0.000000000000000000 ) ) ;
#29044 = CARTESIAN_POINT ( 'NONE',  ( 5.000000000000000000, -150.1875000027311842, 2.071067811865478614 ) ) ;
#29045 = CARTESIAN_POINT ( 'NONE',  ( -50.01589407740564042, -154.6250000000000284, 0.3983568153799778022 ) ) ;
#29046 = CARTESIAN_POINT ( 'NONE',  ( -4.458734124999999437, -35.31249999863440792, 0.000000000000000000 ) ) ;
#29047 = CARTESIAN_POINT ( 'NONE',  ( 5.000000000000000888, -65.45833333060214443, 2.886751345948126879 ) ) ;
#29048 =( BOUNDED_CURVE ( )  B_SPLINE_CURVE ( 2, ( #59365, #15298, #45202, #34921, #55185, #40374, #59693, #40049, #15938 ),
 .UNSPECIFIED., .F., .F. ) 
 B_SPLINE_CURVE_WITH_KNOTS ( ( 3, 2, 2, 2, 3 ),
 ( 0.6517857142857143016, 0.6523809523809523947, 0.6535714285714285809, 0.6547619047619047672, 0.6553571428571428603 ),
 .UNSPECIFIED. ) 
 CURVE ( )  GEOMETRIC_REPRESENTATION_ITEM ( )  RATIONAL_B_SPLINE_CURVE ( ( 0.9330127018922194093, 0.9330127018922194093, 1.000000000000000000, 0.8660254037844387076, 1.000000000000000000, 0.8660254037844387076, 1.000000000000000000, 0.9330127018922194093, 0.9330127018922194093 ) ) 
 REPRESENTATION_ITEM ( '' )  );
#29049 = CARTESIAN_POINT ( 'NONE',  ( -59.29741812935640155, -148.8750000013655779, -2.196230717870135685 ) ) ;
#29050 = CARTESIAN_POINT ( 'NONE',  ( 2.071067811865475505, -144.8125000000000000, -5.000000000000000888 ) ) ;
#29051 = CARTESIAN_POINT ( 'NONE',  ( -4.458734124999997661, -76.47916666530105090, 2.574251347313722516 ) ) ;
#29052 = CARTESIAN_POINT ( 'NONE',  ( 1.846868145590735200, -165.5000000013655779, -4.458734124999999437 ) ) ;
#29053 = CARTESIAN_POINT ( 'NONE',  ( -4.458734124999997661, -28.22916666530107221, 2.574251347313722516 ) ) ;
#29054 = CARTESIAN_POINT ( 'NONE',  ( -2.500000000000000444, -28.04166666393548013, -4.330127018922193649 ) ) ;
#29055 = CARTESIAN_POINT ( 'NONE',  ( 0.000000000000000000, -170.0000000000000000, 0.000000000000000000 ) ) ;
#29056 = CARTESIAN_POINT ( 'NONE',  ( 2.500000000000002220, -22.66666666666666785, 4.330127018922192761 ) ) ;
#29057 = CARTESIAN_POINT ( 'NONE',  ( -1.846868145590737420, -144.7500000013656063, 4.458734124999999437 ) ) ;
#29058 = VERTEX_POINT ( 'NONE', #9828 ) ;
#29059 = CARTESIAN_POINT ( 'NONE',  ( -3.152548672688508926E-16, 26.18750000136559564, -5.148502694627439702 ) ) ;
#29060 = CARTESIAN_POINT ( 'NONE',  ( -5.000000000000000000, -78.87499999726881583, 0.000000000000000000 ) ) ;
#29061 = CARTESIAN_POINT ( 'NONE',  ( 4.458734125000000326, -55.14583333196773651, 2.574251347313718519 ) ) ;
#29062 = CARTESIAN_POINT ( 'NONE',  ( -5.000000000000000000, 28.12500000273118417, 0.000000000000000000 ) ) ;
#29063 = CARTESIAN_POINT ( 'NONE',  ( 5.000000000000000000, -48.29166666393548724, -2.886751345948130876 ) ) ;
#29064 = CARTESIAN_POINT ( 'NONE',  ( -2.500000000000000444, 19.83333333333333570, -4.330127018922193649 ) ) ;
#29065 = CARTESIAN_POINT ( 'NONE',  ( -1.339745962155610925, 8.330341803992665106, 5.000000000000000000 ) ) ;
#29066 = CARTESIAN_POINT ( 'NONE',  ( -2.229367062499996610, -5.145833331967740065, 3.861377020970582219 ) ) ;
#29067 =( BOUNDED_CURVE ( )  B_SPLINE_CURVE ( 2, ( #62696, #53973, #52715, #8649, #28890, #24708, #19874, #63637, #34035 ),
 .UNSPECIFIED., .F., .F. ) 
 B_SPLINE_CURVE_WITH_KNOTS ( ( 3, 2, 2, 2, 3 ),
 ( 0.1946428571428571452, 0.1952380952380952384, 0.1964285714285714246, 0.1976190476190476109, 0.1982142857142857040 ),
 .UNSPECIFIED. ) 
 CURVE ( )  GEOMETRIC_REPRESENTATION_ITEM ( )  RATIONAL_B_SPLINE_CURVE ( ( 0.9330127018922194093, 0.9330127018922194093, 1.000000000000000000, 0.8660254037844387076, 1.000000000000000000, 0.8660254037844387076, 1.000000000000000000, 0.9330127018922194093, 0.9330127018922194093 ) ) 
 REPRESENTATION_ITEM ( '' )  );
#29068 = FACE_OUTER_BOUND ( 'NONE', #37644, .T. ) ;
#29069 = EDGE_CURVE ( 'NONE', #25740, #61101, #33348, .T. ) ;
#29070 = CARTESIAN_POINT ( 'NONE',  ( -5.000000000000000000, -9.083333333333333925, -2.886751345948128211 ) ) ;
#29071 = CARTESIAN_POINT ( 'NONE',  ( -6.972266317189433020E-16, -74.12499999726878741, -5.000000000000000000 ) ) ;
#29072 = CARTESIAN_POINT ( 'NONE',  ( -1.339745962155613812, -88.08034179853028434, -5.000000000000000000 ) ) ;
#29073 = CARTESIAN_POINT ( 'NONE',  ( -3.152548672688508926E-16, -22.56249999863440081, -5.148502694627439702 ) ) ;
#29074 = CARTESIAN_POINT ( 'NONE',  ( 2.229367062500001939, -54.97916666530107221, 3.861377020970579999 ) ) ;
#29075 = CARTESIAN_POINT ( 'NONE',  ( 4.458734124999999437, -155.7500000013655779, 1.846868145590737864 ) ) ;
#29076 = CARTESIAN_POINT ( 'NONE',  ( 5.000000000000000000, -48.37499999726880873, -6.123233995736766282E-16 ) ) ;
#29077 = VERTEX_POINT ( 'NONE', #42994 ) ;
#29078 = CARTESIAN_POINT ( 'NONE',  ( -3.152548672688508926E-16, 5.187500001365592972, -5.148502694627439702 ) ) ;
#29079 = ORIENTED_EDGE ( 'NONE', *, *, #40089, .T. ) ;
#29081 = CARTESIAN_POINT ( 'NONE',  ( 5.000000000000000888, -9.458333330602146205, 2.886751345948126879 ) ) ;
#29080 = CARTESIAN_POINT ( 'NONE',  ( -6.972266317189433020E-16, -53.24999999999999289, -5.000000000000000000 ) ) ;
#29082 = CARTESIAN_POINT ( 'NONE',  ( -4.458734125000001214, -159.8750000013655779, 1.846868145590734089 ) ) ;
#29083 = ORIENTED_EDGE ( 'NONE', *, *, #50427, .T. ) ;
#29084 = CARTESIAN_POINT ( 'NONE',  ( -59.98410592259440222, -135.1250000000000284, -0.3983568153799752487 ) ) ;
#29085 = CARTESIAN_POINT ( 'NONE',  ( -6.972266317189433020E-16, -59.25000000000000000, -5.000000000000000000 ) ) ;
#29086 = CARTESIAN_POINT ( 'NONE',  ( -4.458734124999999437, -41.56249999863440081, 0.000000000000000000 ) ) ;
#29087 = ORIENTED_EDGE ( 'NONE', *, *, #58256, .F. ) ;
#29088 = AXIS2_PLACEMENT_3D ( 'NONE', #31892, #16783, #7142 ) ;
#29089 = EDGE_CURVE ( 'NONE', #22037, #28828, #20067, .T. ) ;
#29090 = EDGE_CURVE ( 'NONE', #50637, #49359, #33037, .T. ) ;
#29091 = DIRECTION ( 'NONE',  ( -0.000000000000000000, 1.000000000000000000, -0.000000000000000000 ) ) ;
#29092 = CARTESIAN_POINT ( 'NONE',  ( 2.229367062499998831, 18.35416666803225993, -3.861377020970580887 ) ) ;
#29093 = FACE_OUTER_BOUND ( 'NONE', #40801, .T. ) ;
#29094 = ORIENTED_EDGE ( 'NONE', *, *, #32351, .F. ) ;
#29095 = CARTESIAN_POINT ( 'NONE',  ( -2.229367062499996610, 26.85416666803225993, 3.861377020970582219 ) ) ;
#29096 = CARTESIAN_POINT ( 'NONE',  ( -51.19402409849444524, -128.6250000027312126, -3.242614290531456334 ) ) ;
#29097 = CARTESIAN_POINT ( 'NONE',  ( 1.975475456537005874E-15, -35.62499999726880162, 5.000000000000000000 ) ) ;
#29098 = CARTESIAN_POINT ( 'NONE',  ( -50.78616202067674834, -135.0000000000000568, 2.038383678880063332 ) ) ;
#29099 = CARTESIAN_POINT ( 'NONE',  ( -1.339745962155617365, 24.20534180126148271, 4.999999999999998224 ) ) ;
#29100 = CARTESIAN_POINT ( 'NONE',  ( -4.458734124999999437, -62.39583333196774362, -2.574251347313719407 ) ) ;
#29101 = CARTESIAN_POINT ( 'NONE',  ( 0.000000000000000000, -120.0000000000000000, 5.000000000000000000 ) ) ;
#29102 = CARTESIAN_POINT ( 'NONE',  ( 4.458734125000001214, 16.10416666803225993, 2.574251347313718519 ) ) ;
#29103 = EDGE_CURVE ( 'NONE', #11394, #2464, #53902, .T. ) ;
#29104 = CARTESIAN_POINT ( 'NONE',  ( 4.330127018922154569, 30.00000000000000000, -7.499999999999971578 ) ) ;
#29105 = CARTESIAN_POINT ( 'NONE',  ( -4.458734124999999437, -49.64583333196772941, -2.574251347313719407 ) ) ;
#29106 = CARTESIAN_POINT ( 'NONE',  ( -2.500000000000000444, -2.041666663935480575, -4.330127018922193649 ) ) ;
#29107 = CYLINDRICAL_SURFACE ( 'NONE', #58173, 5.000000000000000000 ) ;
#29108 = EDGE_CURVE ( 'NONE', #63378, #44876, #19299, .T. ) ;
#29109 = CYLINDRICAL_SURFACE ( 'NONE', #26562, 5.000000000000000000 ) ;
#29110 = CARTESIAN_POINT ( 'NONE',  ( -2.229367062499996610, -86.39583333196773651, 3.861377020970582219 ) ) ;
#29111 = CARTESIAN_POINT ( 'NONE',  ( -2.229367062500000163, -108.4791666653010651, -3.861377020970580443 ) ) ;
#29112 = CARTESIAN_POINT ( 'NONE',  ( -4.458734124999997661, -13.47916666530107221, 2.574251347313722516 ) ) ;
#29113 =( BOUNDED_CURVE ( )  B_SPLINE_CURVE ( 2, ( #63157, #48656, #59928, #25493, #27325, #11331, #42110, #54455, #45433 ),
 .UNSPECIFIED., .F., .F. ) 
 B_SPLINE_CURVE_WITH_KNOTS ( ( 3, 2, 2, 2, 3 ),
 ( 0.2020833333333333370, 0.2027777777777777790, 0.2041666666666666630, 0.2055555555555555469, 0.2062499999999999889 ),
 .UNSPECIFIED. ) 
 CURVE ( )  GEOMETRIC_REPRESENTATION_ITEM ( )  RATIONAL_B_SPLINE_CURVE ( ( 0.9330127018922194093, 0.9330127018922194093, 1.000000000000000000, 0.8660254037844387076, 1.000000000000000000, 0.8660254037844387076, 1.000000000000000000, 0.9330127018922194093, 0.9330127018922194093 ) ) 
 REPRESENTATION_ITEM ( '' )  );
#29114 = ORIENTED_EDGE ( 'NONE', *, *, #16671, .T. ) ;
#29115 = CARTESIAN_POINT ( 'NONE',  ( -5.000000000000000000, -81.08333333333332860, -2.886751345948128211 ) ) ;
#29116 = CARTESIAN_POINT ( 'NONE',  ( -2.229367062499996610, -100.1458333319677365, 3.861377020970582219 ) ) ;
#29117 = CARTESIAN_POINT ( 'NONE',  ( 3.535533905932738197, -162.0000000027312126, -3.535533905932738197 ) ) ;
#29118 = CARTESIAN_POINT ( 'NONE',  ( 4.458734125000001214, -90.14583333196773651, 2.574251347313718519 ) ) ;
#29119 = DIRECTION ( 'NONE',  ( -0.000000000000000000, 1.000000000000000000, -0.000000000000000000 ) ) ;
#29120 = CARTESIAN_POINT ( 'NONE',  ( 1.060575238724906964E-15, -50.62499999726881583, 5.773502691896257311 ) ) ;
#29121 = CARTESIAN_POINT ( 'NONE',  ( -7.894787914004607998, -1.230850257101226302E-13, -7.591390474663425536 ) ) ;
#29122 = CARTESIAN_POINT ( 'NONE',  ( -57.19623071787017210, -129.3750000013656347, 4.297418129356382899 ) ) ;
#29123 = CARTESIAN_POINT ( 'NONE',  ( -55.35523342533222291, -147.3125000013656063, 4.444560631937231499 ) ) ;
#29124 = CARTESIAN_POINT ( 'NONE',  ( 2.229367062499998831, -15.64583333196773651, -3.861377020970580887 ) ) ;
#29125 = CARTESIAN_POINT ( 'NONE',  ( 4.458734124999999437, 9.937500001365593860, -5.460374474430324690E-16 ) ) ;
#29126 = CARTESIAN_POINT ( 'NONE',  ( -3.152548672688508926E-16, -60.81249999863440081, -5.148502694627439702 ) ) ;
#29127 = CARTESIAN_POINT ( 'NONE',  ( -4.999999999999998224, -68.91666666666667140, 2.886751345948131764 ) ) ;
#29128 = CARTESIAN_POINT ( 'NONE',  ( 4.458734125000000326, -13.89583333196774007, 2.574251347313718519 ) ) ;
#29129 = CARTESIAN_POINT ( 'NONE',  ( 0.000000000000000000, -170.0000000000000000, 0.000000000000000000 ) ) ;
#29130 = CARTESIAN_POINT ( 'NONE',  ( -5.000000000000000000, -153.5000000000000284, -6.123233995736766282E-16 ) ) ;
#29131 = CARTESIAN_POINT ( 'NONE',  ( 2.499999999999998668, -7.333333333333330373, -4.330127018922193649 ) ) ;
#29132 = ORIENTED_EDGE ( 'NONE', *, *, #4279, .F. ) ;
#29133 = CARTESIAN_POINT ( 'NONE',  ( 2.229367062499998831, -39.89583333196773651, -3.861377020970580887 ) ) ;
#29134 = FACE_OUTER_BOUND ( 'NONE', #14521, .T. ) ;
#29135 = CARTESIAN_POINT ( 'NONE',  ( -1.339745962155610925, -11.79465819873851906, 5.000000000000000000 ) ) ;
#29136 = LINE ( 'NONE', #13432, #44996 ) ;
#29137 = CARTESIAN_POINT ( 'NONE',  ( -3.152548672688508926E-16, -87.56249999863440792, -5.148502694627439702 ) ) ;
#29138 = CARTESIAN_POINT ( 'NONE',  ( -4.458734124999999437, 17.43750000136559208, 0.000000000000000000 ) ) ;
#29139 = VECTOR ( 'NONE', #49669, 1000.000000000000000 ) ;
#29140 = CARTESIAN_POINT ( 'NONE',  ( -4.458734124999999437, 9.687500001365593860, 0.000000000000000000 ) ) ;
#29141 = CARTESIAN_POINT ( 'NONE',  ( -1.339745962155610925, -43.79465819873851729, 5.000000000000000000 ) ) ;
#29142 = CARTESIAN_POINT ( 'NONE',  ( -2.500000000000000444, -69.16666666666667140, -4.330127018922193649 ) ) ;
#29143 = CARTESIAN_POINT ( 'NONE',  ( 2.229367062500001939, -88.22916666530107932, 3.861377020970579999 ) ) ;
#29144 = CARTESIAN_POINT ( 'NONE',  ( 4.458734125000001214, 20.85416666803226349, 2.574251347313718519 ) ) ;
#29145 = CARTESIAN_POINT ( 'NONE',  ( 2.499999999999998668, -74.33333333333332860, -4.330127018922193649 ) ) ;
#29146 = CARTESIAN_POINT ( 'NONE',  ( -2.499999999999996447, 15.29166666939785202, 4.330127018922195425 ) ) ;
#29147 = EDGE_LOOP ( 'NONE', ( #58145, #59740, #59299, #40970 ) ) ;
#29148 = CYLINDRICAL_SURFACE ( 'NONE', #10969, 5.000000000000000000 ) ;
#29149 = PRODUCT_DEFINITION_SHAPE ( 'NONE', 'NONE',  #34693 ) ;
#29150 = ORIENTED_EDGE ( 'NONE', *, *, #43262, .F. ) ;
#29152 = CARTESIAN_POINT ( 'NONE',  ( 5.000000000000000888, -34.58333333333332860, 2.886751345948126879 ) ) ;
#29151 = DIRECTION ( 'NONE',  ( -0.000000000000000000, 1.000000000000000000, -0.000000000000000000 ) ) ;
#29153 = CARTESIAN_POINT ( 'NONE',  ( -4.458734124999999437, -36.31249999863440792, 0.000000000000000000 ) ) ;
#29154 = CARTESIAN_POINT ( 'NONE',  ( -2.499999999999996447, -32.70833333060215153, 4.330127018922195425 ) ) ;
#29156 = ORIENTED_EDGE ( 'NONE', *, *, #44069, .F. ) ;
#29155 = CARTESIAN_POINT ( 'NONE',  ( 4.458734124999998549, -66.72916666530106511, -2.574251347313721627 ) ) ;
#29157 = CARTESIAN_POINT ( 'NONE',  ( -55.35523342533222291, -151.5625000013656063, 4.444560631937231499 ) ) ;
#29158 = CARTESIAN_POINT ( 'NONE',  ( -2.229367062500000163, -11.47916666530107044, -3.861377020970580443 ) ) ;
#29160 = ORIENTED_EDGE ( 'NONE', *, *, #18546, .T. ) ;
#29159 = CARTESIAN_POINT ( 'NONE',  ( 4.458734124999998549, -11.97916666530107044, -2.574251347313721627 ) ) ;
#29161 = CARTESIAN_POINT ( 'NONE',  ( 5.000000000000000000, -83.41666666666667140, -2.886751345948129988 ) ) ;
#29162 = CARTESIAN_POINT ( 'NONE',  ( -52.10840900171896806, -136.1875000013656063, 3.393966926194110556 ) ) ;
#29163 = CARTESIAN_POINT ( 'NONE',  ( -4.458734124999999437, -56.56249999863440081, 0.000000000000000000 ) ) ;
#29164 =( BOUNDED_CURVE ( )  B_SPLINE_CURVE ( 2, ( #11009, #30631, #50253, #25816, #1394, #57318, #28023, #52792, #2647 ),
 .UNSPECIFIED., .F., .F. ) 
 B_SPLINE_CURVE_WITH_KNOTS ( ( 3, 2, 2, 2, 3 ),
 ( 0.9053571428571428603, 0.9059523809523809534, 0.9071428571428571397, 0.9083333333333333259, 0.9089285714285714191 ),
 .UNSPECIFIED. ) 
 CURVE ( )  GEOMETRIC_REPRESENTATION_ITEM ( )  RATIONAL_B_SPLINE_CURVE ( ( 0.9330127018922194093, 0.9330127018922194093, 1.000000000000000000, 0.8660254037844387076, 1.000000000000000000, 0.8660254037844387076, 1.000000000000000000, 0.9330127018922194093, 0.9330127018922194093 ) ) 
 REPRESENTATION_ITEM ( '' )  );
#29165 = CARTESIAN_POINT ( 'NONE',  ( 5.000000000000000000, -83.37499999726881583, -6.123233995736766282E-16 ) ) ;
#29167 = ORIENTED_EDGE ( 'NONE', *, *, #56136, .F. ) ;
#29166 = CARTESIAN_POINT ( 'NONE',  ( 1.975475456537005874E-15, -18.74999999999999645, 5.000000000000000000 ) ) ;
#29168 = CARTESIAN_POINT ( 'NONE',  ( -59.98410592259440222, -147.1250000000000284, -0.3983568153799752487 ) ) ;
#29169 = CARTESIAN_POINT ( 'NONE',  ( -4.458734124999998549, -28.47916666530107221, 2.574251347313722516 ) ) ;
#29170 = ORIENTED_EDGE ( 'NONE', *, *, #20488, .F. ) ;
#29171 = ADVANCED_FACE ( 'NONE', ( #52653 ), #57802, .T. ) ;
#29172 =( LENGTH_UNIT ( ) NAMED_UNIT ( * ) SI_UNIT ( .MILLI., .METRE. ) );
#29173 = CARTESIAN_POINT ( 'NONE',  ( -4.458734125000001214, -166.1250000013655779, 1.846868145590734089 ) ) ;
#29174 = CARTESIAN_POINT ( 'NONE',  ( -3.152548672688508926E-16, -102.8124999986344221, -5.148502694627439702 ) ) ;
#29175 = CARTESIAN_POINT ( 'NONE',  ( 5.000000000000000888, -8.458333330602144429, 2.886751345948126879 ) ) ;
#29176 = ORIENTED_EDGE ( 'NONE', *, *, #31046, .F. ) ;
#29177 = CARTESIAN_POINT ( 'NONE',  ( -50.70258187064364108, -145.3750000013656063, 2.196230717870141014 ) ) ;
#29178 = CARTESIAN_POINT ( 'NONE',  ( -59.98410592259440222, -139.2500000027312126, -0.3983568153799752487 ) ) ;
#29179 = CARTESIAN_POINT ( 'NONE',  ( 2.229367062499998831, -38.64583333196773651, -3.861377020970580887 ) ) ;
#29180 = LINE ( 'NONE', #48807, #23967 ) ;
#29181 = CARTESIAN_POINT ( 'NONE',  ( -1.339745962155585168, -2.205341801261480938, -5.000000000000015987 ) ) ;
#29182 = CARTESIAN_POINT ( 'NONE',  ( 4.458734124999998549, -11.72916666530107044, -2.574251347313721627 ) ) ;
#29183 = CARTESIAN_POINT ( 'NONE',  ( 9.457646018065525792E-16, -100.3124999986343937, 5.148502694627439702 ) ) ;
#29184 = EDGE_LOOP ( 'NONE', ( #45717, #54656, #48636, #12410 ) ) ;
#29185 = CARTESIAN_POINT ( 'NONE',  ( -4.458734125000000326, -144.2500000013656063, -1.846868145590735644 ) ) ;
#29186 = CARTESIAN_POINT ( 'NONE',  ( 4.458734125000001214, -31.14583333196773651, 2.574251347313718519 ) ) ;
#29187 = CARTESIAN_POINT ( 'NONE',  ( -50.18089887299979068, -153.6875000000000284, 2.462841084822613436 ) ) ;
#29188 = CARTESIAN_POINT ( 'NONE',  ( -50.70258187064364108, -132.1250000013656347, 2.196230717870141014 ) ) ;
#29189 = CARTESIAN_POINT ( 'NONE',  ( 4.458734124999999437, -69.06249999863439371, -5.460374474430324690E-16 ) ) ;
#29190 = EDGE_CURVE ( 'NONE', #57375, #20078, #62636, .T. ) ;
#29191 = CARTESIAN_POINT ( 'NONE',  ( 2.500000000000002220, -17.66666666666666430, 4.330127018922192761 ) ) ;
#29192 = CARTESIAN_POINT ( 'NONE',  ( -6.972266317189433020E-16, -1.124999997268814278, -5.000000000000000000 ) ) ;
#29193 = CARTESIAN_POINT ( 'NONE',  ( -3.152801135295367985, -139.8125000013655779, 3.152801135295367096 ) ) ;
#29194 = CARTESIAN_POINT ( 'NONE',  ( -4.458734124999997661, 4.520833334698926897, 2.574251347313722516 ) ) ;
#29195 = ORIENTED_EDGE ( 'NONE', *, *, #1286, .T. ) ;
#29196 = DIRECTION ( 'NONE',  ( -0.000000000000000000, 1.000000000000000000, -0.000000000000000000 ) ) ;
#29197 = ADVANCED_FACE ( 'NONE', ( #53278 ), #8588, .T. ) ;
#29198 = CARTESIAN_POINT ( 'NONE',  ( 1.975475456537005874E-15, -42.62499999726880873, 5.000000000000000000 ) ) ;
#29200 = CARTESIAN_POINT ( 'NONE',  ( -2.229367062500000163, -32.47916666530106511, -3.861377020970580443 ) ) ;
#29199 = CARTESIAN_POINT ( 'NONE',  ( -5.000000000000000000, -96.00000000000000000, 0.000000000000000000 ) ) ;
#29201 = CARTESIAN_POINT ( 'NONE',  ( -6.972266317189433020E-16, -36.25000000000000000, -5.000000000000000000 ) ) ;
#29202 = CARTESIAN_POINT ( 'NONE',  ( 4.458734124999998549, -77.97916666530106511, -2.574251347313721627 ) ) ;
#29203 = CARTESIAN_POINT ( 'NONE',  ( 4.458734124999998549, 25.02083333469892779, -2.574251347313721627 ) ) ;
#29204 = CARTESIAN_POINT ( 'NONE',  ( -59.59170313451811296, -141.5000000013656063, 1.485763867205729394 ) ) ;
#29205 = ADVANCED_FACE ( 'NONE', ( #13724 ), #8900, .T. ) ;
#29206 = CARTESIAN_POINT ( 'NONE',  ( 2.229367062499998831, -4.645833331967740065, -3.861377020970580887 ) ) ;
#29207 = CARTESIAN_POINT ( 'NONE',  ( 4.458734125000001214, 25.85416666803225638, 2.574251347313718519 ) ) ;
#29208 = CARTESIAN_POINT ( 'NONE',  ( 2.229367062499998831, -40.89583333196773651, -3.861377020970580887 ) ) ;
#29209 = CARTESIAN_POINT ( 'NONE',  ( 5.000000000000000000, -60.37499999726880873, -6.123233995736766282E-16 ) ) ;
#29210 = CARTESIAN_POINT ( 'NONE',  ( 4.458734124999999437, 2.187500001365593416, -5.460374474430324690E-16 ) ) ;
#29211 = ORIENTED_EDGE ( 'NONE', *, *, #59560, .F. ) ;
#29212 = CARTESIAN_POINT ( 'NONE',  ( 2.229367062499998831, -25.89583333196773651, -3.861377020970580887 ) ) ;
#29213 = CARTESIAN_POINT ( 'NONE',  ( 4.458734125000001214, -66.89583333196773651, 2.574251347313718519 ) ) ;
#29214 = CARTESIAN_POINT ( 'NONE',  ( -5.000000000000000000, -107.9583333306021444, -2.886751345948128211 ) ) ;
#29215 = CARTESIAN_POINT ( 'NONE',  ( 4.458734125000001214, 27.10416666803225993, 2.574251347313718519 ) ) ;
#29216 = CARTESIAN_POINT ( 'NONE',  ( 6.123233995736766282E-16, -170.0000000000000000, -5.000000000000000000 ) ) ;
#29217 = LINE ( 'NONE', #39191, #59410 ) ;
#29218 = CARTESIAN_POINT ( 'NONE',  ( 2.229367062499998831, -71.89583333196773651, -3.861377020970580887 ) ) ;
#29219 = CARTESIAN_POINT ( 'NONE',  ( -5.000000000000000000, -53.08333333333332860, -2.886751345948128211 ) ) ;
#29220 = CYLINDRICAL_SURFACE ( 'NONE', #55248, 5.000000000000000000 ) ;
#29221 = CARTESIAN_POINT ( 'NONE',  ( -9.184850993605147944E-16, -156.3750000027311842, 5.000000000000000000 ) ) ;
#29222 = VERTEX_POINT ( 'NONE', #28198 ) ;
#29223 = FACE_OUTER_BOUND ( 'NONE', #56744, .T. ) ;
#29224 = DIRECTION ( 'NONE',  ( -0.000000000000000000, 1.000000000000000000, -0.000000000000000000 ) ) ;
#29225 = CARTESIAN_POINT ( 'NONE',  ( 2.500000000000002220, -19.66666666666666430, 4.330127018922192761 ) ) ;
#29226 = CARTESIAN_POINT ( 'NONE',  ( 9.457646018065525792E-16, -20.06249999863440081, 5.148502694627439702 ) ) ;
#29227 = CARTESIAN_POINT ( 'NONE',  ( 4.458734124999998549, -81.72916666530106511, -2.574251347313721627 ) ) ;
#29228 = AXIS2_PLACEMENT_3D ( 'NONE', #19918, #39532, #29883 ) ;
#29229 = CARTESIAN_POINT ( 'NONE',  ( 4.458734124999999437, -168.6875000013656063, 0.000000000000000000 ) ) ;
#29230 = CARTESIAN_POINT ( 'NONE',  ( -2.499999999999996447, -15.70833333060214443, 4.330127018922195425 ) ) ;
#29232 = VERTEX_POINT ( 'NONE', #39104 ) ;
#29231 = CARTESIAN_POINT ( 'NONE',  ( -2.229367062500000163, -47.47916666530106511, -3.861377020970580443 ) ) ;
#29233 = CARTESIAN_POINT ( 'NONE',  ( -2.499999999999996447, -23.83333333333333215, 4.330127018922195425 ) ) ;
#29234 = LINE ( 'NONE', #19909, #19970 ) ;
#29236 = ORIENTED_EDGE ( 'NONE', *, *, #9875, .T. ) ;
#29235 = CARTESIAN_POINT ( 'NONE',  ( -4.458734124999999437, 1.437500001365592972, 0.000000000000000000 ) ) ;
#29237 = CARTESIAN_POINT ( 'NONE',  ( -6.972266317189433020E-16, -87.12499999726880162, -5.000000000000000000 ) ) ;
#29238 = CARTESIAN_POINT ( 'NONE',  ( 1.060575238724906964E-15, -59.74999999999999289, 5.773502691896257311 ) ) ;
#29239 = CARTESIAN_POINT ( 'NONE',  ( 3.152801135295366208, -155.8125000013656063, 3.152801135295367985 ) ) ;
#29240 = CARTESIAN_POINT ( 'NONE',  ( 4.458734124999998549, -42.97916666530107221, -2.574251347313721627 ) ) ;
#29241 = CARTESIAN_POINT ( 'NONE',  ( 1.975475456537005874E-15, -6.749999999999999112, 5.000000000000000000 ) ) ;
#29242 = CARTESIAN_POINT ( 'NONE',  ( -2.071067811865475061, -162.6875000000000568, -5.000000000000000888 ) ) ;
#29243 = CYLINDRICAL_SURFACE ( 'NONE', #55992, 5.000000000000000000 ) ;
#29244 = CARTESIAN_POINT ( 'NONE',  ( -57.89159099828107458, -128.9375000013656063, -3.393966926194107447 ) ) ;
#29245 = CARTESIAN_POINT ( 'NONE',  ( 4.458734125000001214, -5.145833331967740065, 2.574251347313718519 ) ) ;
#29246 = CARTESIAN_POINT ( 'NONE',  ( -4.458734124999999437, -48.56249999863440792, 0.000000000000000000 ) ) ;
#29247 =( BOUNDED_CURVE ( )  B_SPLINE_CURVE ( 2, ( #36965, #41455, #51449, #30866, #12514, #27309, #61735, #37280, #41774 ),
 .UNSPECIFIED., .F., .F. ) 
 B_SPLINE_CURVE_WITH_KNOTS ( ( 3, 2, 2, 2, 3 ),
 ( 0.3479166666666666519, 0.3486111111111110938, 0.3499999999999999778, 0.3513888888888888618, 0.3520833333333333592 ),
 .UNSPECIFIED. ) 
 CURVE ( )  GEOMETRIC_REPRESENTATION_ITEM ( )  RATIONAL_B_SPLINE_CURVE ( ( 0.9330127018922194093, 0.9330127018922194093, 1.000000000000000000, 0.8660254037844387076, 1.000000000000000000, 0.8660254037844387076, 1.000000000000000000, 0.9330127018922167448, 0.9330127018922194093 ) ) 
 REPRESENTATION_ITEM ( '' )  );
#29248 = CARTESIAN_POINT ( 'NONE',  ( 1.975475456537005874E-15, -7.624999997268812280, 5.000000000000000000 ) ) ;
#29249 = CARTESIAN_POINT ( 'NONE',  ( 3.152801135295366208, -148.5625000013655779, 3.152801135295367985 ) ) ;
#29250 = CARTESIAN_POINT ( 'NONE',  ( 9.457646018065525792E-16, -90.31249999863439371, 5.148502694627439702 ) ) ;
#29251 = DIRECTION ( 'NONE',  ( -0.000000000000000000, 1.000000000000000000, -0.000000000000000000 ) ) ;
#29252 = VERTEX_POINT ( 'NONE', #28826 ) ;
#29253 = CARTESIAN_POINT ( 'NONE',  ( 0.000000000000000000, -120.0000000000000000, 5.000000000000000000 ) ) ;
#29254 = CARTESIAN_POINT ( 'NONE',  ( -1.339745962155660663, -5.669658196007336670, 4.999999999999972466 ) ) ;
#29255 = CARTESIAN_POINT ( 'NONE',  ( -55.39835681537999790, -149.0000000027312126, 4.984105922594378235 ) ) ;
#29256 = CARTESIAN_POINT ( 'NONE',  ( 1.339745962155615144, -30.70534180126147916, 4.999999999999999112 ) ) ;
#29257 = ORIENTED_EDGE ( 'NONE', *, *, #43199, .F. ) ;
#29258 = CARTESIAN_POINT ( 'NONE',  ( -4.999999999999998224, -13.91666666666666785, 2.886751345948131764 ) ) ;
#29259 = CARTESIAN_POINT ( 'NONE',  ( 4.458734125000001214, -14.14583333196774184, 2.574251347313718519 ) ) ;
#29260 = CARTESIAN_POINT ( 'NONE',  ( -1.339745962155613812, -35.20534180126148271, -5.000000000000000000 ) ) ;
#29261 = CARTESIAN_POINT ( 'NONE',  ( 9.457646018065525792E-16, -2.062499998634407028, 5.148502694627439702 ) ) ;
#29262 = CARTESIAN_POINT ( 'NONE',  ( 55.00000000000002132, 0.000000000000000000, 5.000000000000000000 ) ) ;
#29263 = CARTESIAN_POINT ( 'NONE',  ( -3.152801135295367985, -154.8125000013656063, 3.152801135295367096 ) ) ;
#29264 = CARTESIAN_POINT ( 'NONE',  ( 9.457646018065525792E-16, 18.68750000136559208, 5.148502694627439702 ) ) ;
#29265 = ORIENTED_EDGE ( 'NONE', *, *, #53095, .T. ) ;
#29266 = CARTESIAN_POINT ( 'NONE',  ( 2.229367062500001939, -98.97916666530105090, 3.861377020970579999 ) ) ;
#29267 = CARTESIAN_POINT ( 'NONE',  ( 5.276765049035074817, -6.073111908730307817, -7.634085501268428331 ) ) ;
#29268 = CARTESIAN_POINT ( 'NONE',  ( -4.458734124999999437, -14.31249999863440436, 0.000000000000000000 ) ) ;
#29269 = CARTESIAN_POINT ( 'NONE',  ( 0.000000000000000000, -120.0000000000000000, 0.000000000000000000 ) ) ;
#29270 = CARTESIAN_POINT ( 'NONE',  ( 5.000000000000000000, 8.708333336064518093, -2.886751345948130876 ) ) ;
#29271 = CARTESIAN_POINT ( 'NONE',  ( -1.339745962155610925, -87.79465819873851729, 5.000000000000000000 ) ) ;
#29272 = CARTESIAN_POINT ( 'NONE',  ( -2.499999999999996447, -43.70833333060214443, 4.330127018922195425 ) ) ;
#29273 = DIRECTION ( 'NONE',  ( 0.000000000000000000, 0.000000000000000000, 1.000000000000000000 ) ) ;
#29274 = CARTESIAN_POINT ( 'NONE',  ( 2.229367062500001939, 16.02083333469892779, 3.861377020970579999 ) ) ;
#29275 = CARTESIAN_POINT ( 'NONE',  ( -6.972266317189433020E-16, -72.25000000000000000, -5.000000000000000000 ) ) ;
#29276 = ORIENTED_EDGE ( 'NONE', *, *, #38635, .T. ) ;
#29277 = CARTESIAN_POINT ( 'NONE',  ( 2.229367062500001939, 20.02083333469892779, 3.861377020970579999 ) ) ;
#29278 = CARTESIAN_POINT ( 'NONE',  ( 4.458734125000001214, -62.89583333196775072, 2.574251347313718519 ) ) ;
#29279 = CARTESIAN_POINT ( 'NONE',  ( -2.229367062500000163, -7.729166665301073991, -3.861377020970580443 ) ) ;
#29280 = FACE_OUTER_BOUND ( 'NONE', #51562, .T. ) ;
#29281 = CARTESIAN_POINT ( 'NONE',  ( -3.535250795749689387E-16, 11.74999999999999822, -5.773502691896257311 ) ) ;
#29282 = CARTESIAN_POINT ( 'NONE',  ( 4.458734124999999437, -166.4375000013655779, 0.000000000000000000 ) ) ;
#29283 = CARTESIAN_POINT ( 'NONE',  ( -6.972266317189433020E-16, -24.24999999999999645, -5.000000000000000000 ) ) ;
#29284 = CARTESIAN_POINT ( 'NONE',  ( 4.458734124999999437, -55.81249999863440081, -5.460374474430324690E-16 ) ) ;
#29285 = CARTESIAN_POINT ( 'NONE',  ( 1.060575238724906964E-15, -87.62499999726880162, 5.773502691896257311 ) ) ;
#29286 = CARTESIAN_POINT ( 'NONE',  ( 3.061616997868383141E-16, -151.7500000000000284, -5.000000000000000000 ) ) ;
#29287 = CARTESIAN_POINT ( 'NONE',  ( 1.975475456537005874E-15, -49.62499999726880873, 5.000000000000000000 ) ) ;
#29288 = LINE ( 'NONE', #34436, #46012 ) ;
#29289 = CARTESIAN_POINT ( 'NONE',  ( 1.846868145590736310, -153.8750000013655779, 4.458734124999997661 ) ) ;
#29290 =( BOUNDED_CURVE ( )  B_SPLINE_CURVE ( 2, ( #6317, #60355, #50686, #35579, #55206, #36527, #32019, #26888, #40391 ),
 .UNSPECIFIED., .F., .F. ) 
 B_SPLINE_CURVE_WITH_KNOTS ( ( 3, 2, 2, 2, 3 ),
 ( 0.1946428571428571452, 0.1952380952380952384, 0.1964285714285714246, 0.1976190476190476109, 0.1982142857142857040 ),
 .UNSPECIFIED. ) 
 CURVE ( )  GEOMETRIC_REPRESENTATION_ITEM ( )  RATIONAL_B_SPLINE_CURVE ( ( 0.9330127018922194093, 0.9330127018922194093, 1.000000000000000000, 0.8660254037844387076, 1.000000000000000000, 0.8660254037844387076, 1.000000000000000000, 0.9330127018922194093, 0.9330127018922194093 ) ) 
 REPRESENTATION_ITEM ( '' )  );
#29291 = CARTESIAN_POINT ( 'NONE',  ( -5.000000000000000000, -36.00000000000000711, 0.000000000000000000 ) ) ;
#29292 = CARTESIAN_POINT ( 'NONE',  ( 1.975475456537005874E-15, -46.74999999999999289, 5.000000000000000000 ) ) ;
#29293 = CARTESIAN_POINT ( 'NONE',  ( 2.071067811865401787, -162.8124999999999716, -5.000000000000074607 ) ) ;
#29294 = VERTEX_POINT ( 'NONE', #4694 ) ;
#29295 = CARTESIAN_POINT ( 'NONE',  ( 4.458734124999998549, -99.72916666530105090, -2.574251347313721627 ) ) ;
#29296 = CARTESIAN_POINT ( 'NONE',  ( -2.229367062500000163, 2.270833334698928230, -3.861377020970580443 ) ) ;
#29297 = CARTESIAN_POINT ( 'NONE',  ( 2.499999999999998668, -80.33333333333332860, -4.330127018922193649 ) ) ;
#29298 = CARTESIAN_POINT ( 'NONE',  ( 2.500000000000002220, 3.333333333333333925, 4.330127018922192761 ) ) ;
#29299 = CARTESIAN_POINT ( 'NONE',  ( -4.458734124999999437, -68.39583333196773651, -2.574251347313719407 ) ) ;
#29300 = CARTESIAN_POINT ( 'NONE',  ( -2.499999999999996447, -30.70833333060214443, 4.330127018922195425 ) ) ;
#29301 = CARTESIAN_POINT ( 'NONE',  ( 5.000000000000000888, -1.458333330602149092, 2.886751345948126879 ) ) ;
#29303 = ORIENTED_EDGE ( 'NONE', *, *, #21379, .T. ) ;
#29302 = CARTESIAN_POINT ( 'NONE',  ( -2.229367062499996610, -36.14583333196773651, 3.861377020970582219 ) ) ;
#29304 = LINE ( 'NONE', #63123, #49160 ) ;
#29305 = DIRECTION ( 'NONE',  ( -0.000000000000000000, 1.000000000000000000, -0.000000000000000000 ) ) ;
#29306 = CARTESIAN_POINT ( 'NONE',  ( -51.75738570946856498, -136.7500000000000284, 3.805975901505576964 ) ) ;
#29307 = CARTESIAN_POINT ( 'NONE',  ( -2.499999999999996447, -43.83333333333333570, 4.330127018922195425 ) ) ;
#29308 = CARTESIAN_POINT ( 'NONE',  ( 4.458734124999999437, -24.06249999863440436, -5.460374474430324690E-16 ) ) ;
#29309 = CARTESIAN_POINT ( 'NONE',  ( 4.458734124999999437, -69.81249999863439371, -5.460374474430324690E-16 ) ) ;
#29310 = CARTESIAN_POINT ( 'NONE',  ( -3.152801135295367096, -145.3125000013655779, -3.152801135295367541 ) ) ;
#29311 = CARTESIAN_POINT ( 'NONE',  ( -2.229367062499996610, -77.14583333196773651, 3.861377020970582219 ) ) ;
#29312 = CARTESIAN_POINT ( 'NONE',  ( -50.40829686548195099, -140.2500000013656063, -1.485763867205728284 ) ) ;
#29313 = AXIS2_PLACEMENT_3D ( 'NONE', #49541, #6452, #29915 ) ;
#29314 = CARTESIAN_POINT ( 'NONE',  ( 9.457646018065525792E-16, -32.31249999863440792, 5.148502694627439702 ) ) ;
#29315 = CARTESIAN_POINT ( 'NONE',  ( -5.000000000000000000, -71.95833333060214443, -2.886751345948128211 ) ) ;
#29316 = EDGE_LOOP ( 'NONE', ( #10993, #10112, #14300, #11626 ) ) ;
#29317 = CARTESIAN_POINT ( 'NONE',  ( -1.339745962155613812, -83.08034179853028434, -5.000000000000000000 ) ) ;
#29318 = VERTEX_POINT ( 'NONE', #3770 ) ;
#29319 = CARTESIAN_POINT ( 'NONE',  ( 2.229367062499998831, -74.89583333196773651, -3.861377020970580887 ) ) ;
#29320 = CARTESIAN_POINT ( 'NONE',  ( 3.535533905932736864, -166.1250000000000284, 3.535533905932738641 ) ) ;
#29321 = VERTEX_POINT ( 'NONE', #18558 ) ;
#29322 = EDGE_CURVE ( 'NONE', #41425, #6544, #9213, .T. ) ;
#29323 = CARTESIAN_POINT ( 'NONE',  ( 1.339745962155670655, -20.16965819600734022, -4.999999999999966249 ) ) ;
#29324 = CARTESIAN_POINT ( 'NONE',  ( -2.499999999999996447, -2.833333333333333481, 4.330127018922195425 ) ) ;
#29325 = CARTESIAN_POINT ( 'NONE',  ( 2.229367062500001939, -59.22916666530106511, 3.861377020970579999 ) ) ;
#29326 = CARTESIAN_POINT ( 'NONE',  ( 4.458734125000001214, 1.854166668032262155, 2.574251347313718519 ) ) ;
#29327 = ORIENTED_EDGE ( 'NONE', *, *, #55522, .F. ) ;
#29328 = CARTESIAN_POINT ( 'NONE',  ( -2.499999999999996447, -19.83333333333333570, 4.330127018922195425 ) ) ;
#29329 = CARTESIAN_POINT ( 'NONE',  ( 0.000000000000000000, 30.00000000000000000, 0.000000000000000000 ) ) ;
#29330 = CARTESIAN_POINT ( 'NONE',  ( -4.458734124999999437, 14.60416666803226171, -2.574251347313719407 ) ) ;
#29331 = CARTESIAN_POINT ( 'NONE',  ( -57.89159099828107458, -145.6875000013656063, -3.393966926194107447 ) ) ;
#29332 = CARTESIAN_POINT ( 'NONE',  ( 1.975475456537005874E-15, -32.74999999999999289, 5.000000000000000000 ) ) ;
#29333 = CARTESIAN_POINT ( 'NONE',  ( 1.846868145590736310, -164.6250000013656063, 4.458734124999997661 ) ) ;
#29334 =( BOUNDED_CURVE ( )  B_SPLINE_CURVE ( 2, ( #34243, #43578, #42961, #62604, #4356, #63221, #38147, #4055, #43271 ),
 .UNSPECIFIED., .F., .F. ) 
 B_SPLINE_CURVE_WITH_KNOTS ( ( 3, 2, 2, 2, 3 ),
 ( 0.2374999999999999889, 0.2380952380952380820, 0.2392857142857142960, 0.2404761904761904823, 0.2410714285714285754 ),
 .UNSPECIFIED. ) 
 CURVE ( )  GEOMETRIC_REPRESENTATION_ITEM ( )  RATIONAL_B_SPLINE_CURVE ( ( 0.9330127018922194093, 0.9330127018922194093, 1.000000000000000000, 0.8660254037844387076, 1.000000000000000000, 0.8660254037844387076, 1.000000000000000000, 0.9330127018922194093, 0.9330127018922194093 ) ) 
 REPRESENTATION_ITEM ( '' )  );
#29335 = VERTEX_POINT ( 'NONE', #48447 ) ;
#29336 = CARTESIAN_POINT ( 'NONE',  ( -2.229367062500000163, -75.47916666530106511, -3.861377020970580443 ) ) ;
#29337 = CARTESIAN_POINT ( 'NONE',  ( -5.000000000000000000, -51.87499999726881583, 0.000000000000000000 ) ) ;
#29338 = CARTESIAN_POINT ( 'NONE',  ( 2.229367062500001939, 3.020833334698928674, 3.861377020970579999 ) ) ;
#29339 = DIRECTION ( 'NONE',  ( -0.000000000000000000, 1.000000000000000000, -0.000000000000000000 ) ) ;
#29340 = CARTESIAN_POINT ( 'NONE',  ( -2.229367062499996610, -65.39583333196773651, 3.861377020970582219 ) ) ;
#29341 = CARTESIAN_POINT ( 'NONE',  ( 2.499999999999998668, -25.20833333060214443, -4.330127018922193649 ) ) ;
#29342 = DIRECTION ( 'NONE',  ( -0.000000000000000000, 1.000000000000000000, -0.000000000000000000 ) ) ;
#29343 = CARTESIAN_POINT ( 'NONE',  ( 5.000000000000000888, -28.45833333060214443, 2.886751345948126879 ) ) ;
#29344 = CARTESIAN_POINT ( 'NONE',  ( 1.339745962155612702, -61.29465819873851729, -5.000000000000000000 ) ) ;
#29345 = CARTESIAN_POINT ( 'NONE',  ( 1.975475456537005874E-15, -3.624999997268814056, 5.000000000000000000 ) ) ;
#29346 = CARTESIAN_POINT ( 'NONE',  ( 2.229367062499998831, -47.64583333196774362, -3.861377020970580887 ) ) ;
#29347 = CARTESIAN_POINT ( 'NONE',  ( 4.458734125000000326, -26.14583333196773651, 2.574251347313718519 ) ) ;
#29348 = CARTESIAN_POINT ( 'NONE',  ( -3.152548672688508926E-16, 7.187500001365594748, -5.148502694627439702 ) ) ;
#29349 = CARTESIAN_POINT ( 'NONE',  ( 5.000000000000000000, -146.1250000027312126, 0.000000000000000000 ) ) ;
#29350 = CARTESIAN_POINT ( 'NONE',  ( -5.000000000000000000, 27.99999999999999645, 0.000000000000000000 ) ) ;
#29351 = CARTESIAN_POINT ( 'NONE',  ( -3.535533905932737309, -150.7500000027312126, -3.535533905932738197 ) ) ;
#29352 = CARTESIAN_POINT ( 'NONE',  ( -2.499999999999996447, 29.16666666666666785, 4.330127018922195425 ) ) ;
#29353 = CARTESIAN_POINT ( 'NONE',  ( 2.229367062500001939, -39.97916666530107221, 3.861377020970579999 ) ) ;
#29354 = CARTESIAN_POINT ( 'NONE',  ( 2.500000000000002220, -74.54166666393547303, 4.330127018922192761 ) ) ;
#29355 = AXIS2_PLACEMENT_3D ( 'NONE', #38269, #7744, #7430 ) ;
#29356 = VECTOR ( 'NONE', #45037, 1000.000000000000000 ) ;
#29357 = CARTESIAN_POINT ( 'NONE',  ( -50.40829686548195099, -142.2500000013656063, -1.485763867205728284 ) ) ;
#29358 = CARTESIAN_POINT ( 'NONE',  ( -2.071067811865478170, -142.3125000000000000, 5.000000000000000000 ) ) ;
#29359 = CARTESIAN_POINT ( 'NONE',  ( 4.458734124999998549, -76.97916666530106511, -2.574251347313721627 ) ) ;
#29360 = CARTESIAN_POINT ( 'NONE',  ( -8.190561711645485556E-16, -166.9375000013655779, 4.458734124999999437 ) ) ;
#29361 = CARTESIAN_POINT ( 'NONE',  ( 4.458734124999998549, -32.72916666530106511, -2.574251347313721627 ) ) ;
#29362 = DIRECTION ( 'NONE',  ( -0.000000000000000000, 1.000000000000000000, -0.000000000000000000 ) ) ;
#29363 = CARTESIAN_POINT ( 'NONE',  ( 0.000000000000000000, -170.0000000000000000, 0.000000000000000000 ) ) ;
#29364 = CARTESIAN_POINT ( 'NONE',  ( -3.535250795749689387E-16, -23.25000000000000000, -5.773502691896257311 ) ) ;
#29365 = CARTESIAN_POINT ( 'NONE',  ( 2.730187237215162345E-16, -145.1875000013656063, -4.458734124999999437 ) ) ;
#29366 = VERTEX_POINT ( 'NONE', #38180 ) ;
#29367 = CARTESIAN_POINT ( 'NONE',  ( -4.458734124999999437, 28.35416666803226349, -2.574251347313719407 ) ) ;
#29368 = EDGE_LOOP ( 'NONE', ( #31251, #2390, #34092, #35524 ) ) ;
#29369 = CARTESIAN_POINT ( 'NONE',  ( 4.458734124999998549, -62.97916666530106511, -2.574251347313721627 ) ) ;
#29370 = CARTESIAN_POINT ( 'NONE',  ( -3.535250795749689387E-16, 21.87500000273118062, -5.773502691896257311 ) ) ;
#29371 = CARTESIAN_POINT ( 'NONE',  ( -6.972266317189433020E-16, 4.875000002731184168, -5.000000000000000000 ) ) ;
#29372 = CARTESIAN_POINT ( 'NONE',  ( -5.000000000000000000, 19.00000000000000000, 0.000000000000000000 ) ) ;
#29373 = EDGE_CURVE ( 'NONE', #29058, #32825, #42344, .T. ) ;
#29374 = CARTESIAN_POINT ( 'NONE',  ( -5.000000000000000000, -89.00000000000000000, 0.000000000000000000 ) ) ;
#29375 = CARTESIAN_POINT ( 'NONE',  ( 9.457646018065525792E-16, -7.062499998634404363, 5.148502694627439702 ) ) ;
#29376 = CARTESIAN_POINT ( 'NONE',  ( 3.061616997868383141E-16, -168.7500000000000000, -5.000000000000000000 ) ) ;
#29377 = CARTESIAN_POINT ( 'NONE',  ( 0.000000000000000000, -170.0000000000000000, 5.000000000000000000 ) ) ;
#29378 = CARTESIAN_POINT ( 'NONE',  ( 1.975475456537005874E-15, -12.74999999999999822, 5.000000000000000000 ) ) ;
#29380 = CARTESIAN_POINT ( 'NONE',  ( -3.152548672688508926E-16, -23.56249999863440436, -5.148502694627439702 ) ) ;
#29379 = CARTESIAN_POINT ( 'NONE',  ( -2.916731409357579869E-14, 18.24999999999999645, 5.000000000000000888 ) ) ;
#29381 = CARTESIAN_POINT ( 'NONE',  ( 2.499999999999998668, 10.79166666939785202, -4.330127018922193649 ) ) ;
#29382 = CARTESIAN_POINT ( 'NONE',  ( 4.458734125000001214, -52.89583333196772941, 2.574251347313718519 ) ) ;
#29383 = CARTESIAN_POINT ( 'NONE',  ( 4.458734124999999437, -157.7500000013656063, 1.846868145590737864 ) ) ;
#29384 = EDGE_CURVE ( 'NONE', #26085, #43575, #43530, .T. ) ;
#29385 = CARTESIAN_POINT ( 'NONE',  ( 1.060575238724906964E-15, -47.62499999726881583, 5.773502691896257311 ) ) ;
#29386 = ORIENTED_EDGE ( 'NONE', *, *, #59398, .T. ) ;
#29388 = ADVANCED_FACE ( 'NONE', ( #59373 ), #54550, .T. ) ;
#29387 = CARTESIAN_POINT ( 'NONE',  ( 4.458734124999998549, 4.020833334698926009, -2.574251347313721627 ) ) ;
#29389 = VERTEX_POINT ( 'NONE', #45211 ) ;
#29391 = CARTESIAN_POINT ( 'NONE',  ( 0.000000000000000000, -114.9999999999999858, 0.000000000000000000 ) ) ;
#29390 = FACE_OUTER_BOUND ( 'NONE', #44700, .T. ) ;
#29392 = CARTESIAN_POINT ( 'NONE',  ( -1.846868145590737420, -155.7500000013655779, 4.458734124999999437 ) ) ;
#29393 = ORIENTED_EDGE ( 'NONE', *, *, #19048, .T. ) ;
#29394 = AXIS2_PLACEMENT_3D ( 'NONE', #52117, #27663, #42766 ) ;
#29395 = DIRECTION ( 'NONE',  ( -0.000000000000000000, 1.000000000000000000, -0.000000000000000000 ) ) ;
#29396 = CARTESIAN_POINT ( 'NONE',  ( -58.24261429053147765, -133.2500000000000284, -3.805975901505573855 ) ) ;
#29397 = CARTESIAN_POINT ( 'NONE',  ( -6.972266317189433020E-16, -13.25000000000000000, -5.000000000000000000 ) ) ;
#29398 = CARTESIAN_POINT ( 'NONE',  ( -4.458734124999998549, -41.47916666530107221, 2.574251347313722516 ) ) ;
#29399 = ORIENTED_EDGE ( 'NONE', *, *, #38067, .F. ) ;
#29400 = EDGE_CURVE ( 'NONE', #7429, #32043, #25274, .T. ) ;
#29401 = CARTESIAN_POINT ( 'NONE',  ( 5.000000000000000000, 9.625000002731184168, -6.123233995736766282E-16 ) ) ;
#29402 = CARTESIAN_POINT ( 'NONE',  ( 9.457646018065525792E-16, 17.93750000136559208, 5.148502694627439702 ) ) ;
#29403 = CARTESIAN_POINT ( 'NONE',  ( 6.123233995736766282E-16, -170.0000000000000000, -5.000000000000000000 ) ) ;
#29404 = VERTEX_POINT ( 'NONE', #11433 ) ;
#29405 = CARTESIAN_POINT ( 'NONE',  ( -4.458734124999999437, -88.56249999863439371, 0.000000000000000000 ) ) ;
#29406 = CARTESIAN_POINT ( 'NONE',  ( -52.53715891517739323, -126.5625000027312268, -4.819101127000233298 ) ) ;
#29407 = DIRECTION ( 'NONE',  ( 0.000000000000000000, 0.000000000000000000, -1.000000000000000000 ) ) ;
#29408 = CARTESIAN_POINT ( 'NONE',  ( 5.000000000000000000, -100.5000000000000000, -6.123233995736766282E-16 ) ) ;
#29409 = DIRECTION ( 'NONE',  ( 0.000000000000000000, -1.000000000000000000, 0.000000000000000000 ) ) ;
#29410 = CARTESIAN_POINT ( 'NONE',  ( -4.458734124999997661, -58.22916666530106511, 2.574251347313722516 ) ) ;
#29411 = CARTESIAN_POINT ( 'NONE',  ( 0.000000000000000000, -120.0000000000000000, 5.000000000000000000 ) ) ;
#29412 = CARTESIAN_POINT ( 'NONE',  ( -3.152548672688508926E-16, 15.43750000136559564, -5.148502694627439702 ) ) ;
#29413 =( BOUNDED_CURVE ( )  B_SPLINE_CURVE ( 2, ( #17350, #7393, #51140, #41461, #27628, #12206, #62055, #56602, #27000 ),
 .UNSPECIFIED., .F., .F. ) 
 B_SPLINE_CURVE_WITH_KNOTS ( ( 3, 2, 2, 2, 3 ),
 ( 0.5446428571428570953, 0.5452380952380951884, 0.5464285714285713746, 0.5476190476190476719, 0.5482142857142857650 ),
 .UNSPECIFIED. ) 
 CURVE ( )  GEOMETRIC_REPRESENTATION_ITEM ( )  RATIONAL_B_SPLINE_CURVE ( ( 0.9330127018922194093, 0.9330127018922194093, 1.000000000000000000, 0.8660254037844387076, 1.000000000000000000, 0.8660254037844387076, 1.000000000000000000, 0.9330127018922194093, 0.9330127018922194093 ) ) 
 REPRESENTATION_ITEM ( '' )  );
#29414 = CARTESIAN_POINT ( 'NONE',  ( -4.999999999999998224, -78.79166666393547303, 2.886751345948131764 ) ) ;
#29415 = CARTESIAN_POINT ( 'NONE',  ( 4.458734124999998549, -47.97916666530107221, -2.574251347313721627 ) ) ;
#29416 = ADVANCED_FACE ( 'NONE', ( #20777 ), #49399, .T. ) ;
#29417 = CARTESIAN_POINT ( 'NONE',  ( 2.500000000000002220, -7.541666663935481907, 4.330127018922192761 ) ) ;
#29418 = CYLINDRICAL_SURFACE ( 'NONE', #31447, 5.000000000000000000 ) ;
#29419 = LINE ( 'NONE', #14331, #46072 ) ;
#29420 = CARTESIAN_POINT ( 'NONE',  ( -1.339745962155610925, -73.79465819873853150, 5.000000000000000000 ) ) ;
#29421 = CARTESIAN_POINT ( 'NONE',  ( -3.152548672688508926E-16, -107.5624999986343937, -5.148502694627439702 ) ) ;
#29422 = CARTESIAN_POINT ( 'NONE',  ( 4.458734124999998549, -10.97916666530107044, -2.574251347313721627 ) ) ;
#29423 = ORIENTED_EDGE ( 'NONE', *, *, #40113, .F. ) ;
#29424 = CARTESIAN_POINT ( 'NONE',  ( -5.000000000000000888, -155.6875000027312126, -2.071067811865475949 ) ) ;
#29425 = CARTESIAN_POINT ( 'NONE',  ( -2.229367062500000163, -99.47916666530106511, -3.861377020970580443 ) ) ;
#29426 = CARTESIAN_POINT ( 'NONE',  ( 3.535533905932738197, -163.0000000027312126, -3.535533905932738197 ) ) ;
#29427 = CARTESIAN_POINT ( 'NONE',  ( -4.458734124999998549, -99.47916666530105090, 2.574251347313722516 ) ) ;
#29428 = CARTESIAN_POINT ( 'NONE',  ( -1.339745962155610925, -7.794658198738519950, 5.000000000000000000 ) ) ;
#29429 = CARTESIAN_POINT ( 'NONE',  ( -4.999999999999999112, -56.79166666393548013, 2.886751345948131764 ) ) ;
#29430 = CARTESIAN_POINT ( 'NONE',  ( -5.000000000000000000, -36.87499999726881583, 0.000000000000000000 ) ) ;
#29431 = CARTESIAN_POINT ( 'NONE',  ( -55.35523342533222291, -125.3125000013655921, 4.444560631937231499 ) ) ;
#29432 =( BOUNDED_CURVE ( )  B_SPLINE_CURVE ( 2, ( #58408, #37852, #14336, #29424, #23059, #33957, #28184, #53578, #33331 ),
 .UNSPECIFIED., .F., .F. ) 
 B_SPLINE_CURVE_WITH_KNOTS ( ( 3, 2, 2, 2, 3 ),
 ( 0.4416666666666670404, 0.4458333333333337478, 0.4500000000000003997, 0.4541666666666671071, 0.4583333333333337589 ),
 .UNSPECIFIED. ) 
 CURVE ( )  GEOMETRIC_REPRESENTATION_ITEM ( )  RATIONAL_B_SPLINE_CURVE ( ( 0.9999999999999928946, 0.9238795325112938439, 1.000000000000000000, 0.9238795325112867385, 1.000000000000000000, 0.9238795325112867385, 1.000000000000000000, 0.9238795325112786339, 1.000000000000008216 ) ) 
 REPRESENTATION_ITEM ( '' )  );
#29433 = CARTESIAN_POINT ( 'NONE',  ( -55.35523342533222291, -146.3125000013656063, 4.444560631937231499 ) ) ;
#29434 = CARTESIAN_POINT ( 'NONE',  ( 4.458734125000000326, -15.89583333196773651, 2.574251347313718519 ) ) ;
#29435 = CARTESIAN_POINT ( 'NONE',  ( -4.458734124999999437, 8.437500001365595637, 0.000000000000000000 ) ) ;
#29436 = CARTESIAN_POINT ( 'NONE',  ( -4.458734124999999437, -58.64583333196773651, -2.574251347313719407 ) ) ;
#29437 = CARTESIAN_POINT ( 'NONE',  ( 0.000000000000000000, -120.0000000000000000, 0.000000000000000000 ) ) ;
#29438 = CARTESIAN_POINT ( 'NONE',  ( 4.458734124999998549, -12.72916666530106866, -2.574251347313721627 ) ) ;
#29439 = CARTESIAN_POINT ( 'NONE',  ( 0.000000000000000000, -170.0000000000000000, 5.000000000000000000 ) ) ;
#29440 = CARTESIAN_POINT ( 'NONE',  ( -5.000000000000000000, -156.5000000000000000, -6.123233995736766282E-16 ) ) ;
#29441 = CARTESIAN_POINT ( 'NONE',  ( -3.535250795749689387E-16, -8.250000000000000000, -5.773502691896257311 ) ) ;
#29442 = VERTEX_POINT ( 'NONE', #1177 ) ;
#29443 = CARTESIAN_POINT ( 'NONE',  ( 4.458734125000000326, -42.14583333196773651, 2.574251347313718519 ) ) ;
#29444 = AXIS2_PLACEMENT_3D ( 'NONE', #25160, #55079, #30623 ) ;
#29445 = CARTESIAN_POINT ( 'NONE',  ( -50.70258187064364108, -125.3750000013656205, 2.196230717870141014 ) ) ;
#29446 = CARTESIAN_POINT ( 'NONE',  ( -2.229367062500000163, -85.47916666530107932, -3.861377020970580443 ) ) ;
#29447 = CARTESIAN_POINT ( 'NONE',  ( -4.458734124999999437, 18.43750000136559564, 0.000000000000000000 ) ) ;
#29448 = ADVANCED_FACE ( 'NONE', ( #40697 ), #16270, .F. ) ;
#29449 = VECTOR ( 'NONE', #21521, 1000.000000000000000 ) ;
#29450 = CARTESIAN_POINT ( 'NONE',  ( -4.458734124999999437, 7.687500001365594748, 0.000000000000000000 ) ) ;
#29451 = ADVANCED_FACE ( 'NONE', ( #40382 ), #44895, .T. ) ;
#29452 = ADVANCED_FACE ( 'NONE', ( #49716 ), #855, .T. ) ;
#29453 = CARTESIAN_POINT ( 'NONE',  ( 1.975475456537005874E-15, -93.74999999999998579, 5.000000000000000000 ) ) ;
#29454 = AXIS2_PLACEMENT_3D ( 'NONE', #31516, #17375, #41480 ) ;
#29455 = CARTESIAN_POINT ( 'NONE',  ( -2.499999999999996447, -68.83333333333332860, 4.330127018922195425 ) ) ;
#29456 = CARTESIAN_POINT ( 'NONE',  ( 9.457646018065525792E-16, -86.31249999863439371, 5.148502694627439702 ) ) ;
#29457 = CARTESIAN_POINT ( 'NONE',  ( -2.229367062499996610, 20.60416666803225993, 3.861377020970582219 ) ) ;
#29458 = CARTESIAN_POINT ( 'NONE',  ( -5.000000000000000000, -73.08333333333334281, -2.886751345948128211 ) ) ;
#29459 = CARTESIAN_POINT ( 'NONE',  ( -5.000000000000000000, 12.04166666939785379, -2.886751345948128211 ) ) ;
#29460 = ORIENTED_EDGE ( 'NONE', *, *, #62903, .T. ) ;
#29461 = CARTESIAN_POINT ( 'NONE',  ( 5.000000000000000000, -102.5000000000000142, -6.123233995736766282E-16 ) ) ;
#29462 = ORIENTED_EDGE ( 'NONE', *, *, #27609, .F. ) ;
#29463 = CARTESIAN_POINT ( 'NONE',  ( 2.500000000000002220, -35.66666666666666430, 4.330127018922192761 ) ) ;
#29464 = CARTESIAN_POINT ( 'NONE',  ( -4.458734124999998549, -40.22916666530107932, 2.574251347313722516 ) ) ;
#29465 = CARTESIAN_POINT ( 'NONE',  ( 2.499999999999998668, -33.20833333060215153, -4.330127018922193649 ) ) ;
#29467 = VERTEX_POINT ( 'NONE', #35568 ) ;
#29466 = CARTESIAN_POINT ( 'NONE',  ( 2.229367062500001939, -64.97916666530106511, 3.861377020970579999 ) ) ;
#29468 = CARTESIAN_POINT ( 'NONE',  ( -54.64476657466781973, -151.0625000013656063, -4.444560631937228834 ) ) ;
#29470 = EDGE_CURVE ( 'NONE', #43179, #17081, #50196, .T. ) ;
#29469 = CARTESIAN_POINT ( 'NONE',  ( 9.457646018065525792E-16, -11.06249999863440969, 5.148502694627439702 ) ) ;
#29472 = ORIENTED_EDGE ( 'NONE', *, *, #55804, .F. ) ;
#29471 = CARTESIAN_POINT ( 'NONE',  ( -2.229367062500000163, -15.72916666530107399, -3.861377020970580443 ) ) ;
#29473 = CARTESIAN_POINT ( 'NONE',  ( -5.000000000000000000, -81.00000000000000000, 0.000000000000000000 ) ) ;
#29474 = CARTESIAN_POINT ( 'NONE',  ( 4.458734125000000326, -167.3750000013656347, -1.846868145590734978 ) ) ;
#29475 = CARTESIAN_POINT ( 'NONE',  ( -2.229367062500000163, -59.72916666530106511, -3.861377020970580443 ) ) ;
#29476 = CARTESIAN_POINT ( 'NONE',  ( 1.060575238724906964E-15, -81.62499999726881583, 5.773502691896257311 ) ) ;
#29478 = VERTEX_POINT ( 'NONE', #5343 ) ;
#29477 = CARTESIAN_POINT ( 'NONE',  ( -1.339745962155610925, -48.66965819600732601, 5.000000000000000000 ) ) ;
#29479 = CARTESIAN_POINT ( 'NONE',  ( -58.24261429053147765, -144.2500000000000284, -3.805975901505573855 ) ) ;
#29480 = CARTESIAN_POINT ( 'NONE',  ( 2.229367062499998831, -27.89583333196774007, -3.861377020970580887 ) ) ;
#29481 = ORIENTED_EDGE ( 'NONE', *, *, #53011, .T. ) ;
#29482 = CARTESIAN_POINT ( 'NONE',  ( -4.458734125000000326, -168.2500000013656063, -1.846868145590735644 ) ) ;
#29483 = CARTESIAN_POINT ( 'NONE',  ( -4.458734124999999437, -103.6458333319677223, -2.574251347313719407 ) ) ;
#29484 = CARTESIAN_POINT ( 'NONE',  ( 2.500000000000002220, -55.54166666393548013, 4.330127018922192761 ) ) ;
#29485 = ORIENTED_EDGE ( 'NONE', *, *, #40609, .T. ) ;
#29486 = CARTESIAN_POINT ( 'NONE',  ( -59.44456063193725015, -145.8125000013656063, -0.3552334253322034230 ) ) ;
#29487 = CARTESIAN_POINT ( 'NONE',  ( -49.85088928181150436, -138.6875000027312126, -1.666127454062680702 ) ) ;
#29488 = CARTESIAN_POINT ( 'NONE',  ( 4.458734124999998549, -37.72916666530107221, -2.574251347313721627 ) ) ;
#29489 = CARTESIAN_POINT ( 'NONE',  ( 4.458734124999999437, -144.6250000013655779, -1.846868145590734978 ) ) ;
#29490 =( BOUNDED_CURVE ( )  B_SPLINE_CURVE ( 2, ( #13098, #2828, #13722, #52025, #61369, #47811, #56859, #52345, #57495 ),
 .UNSPECIFIED., .F., .F. ) 
 B_SPLINE_CURVE_WITH_KNOTS ( ( 3, 2, 2, 2, 3 ),
 ( 0.9696428571428571397, 0.9702380952380952328, 0.9714285714285714191, 0.9726190476190476053, 0.9732142857142856984 ),
 .UNSPECIFIED. ) 
 CURVE ( )  GEOMETRIC_REPRESENTATION_ITEM ( )  RATIONAL_B_SPLINE_CURVE ( ( 0.9330127018922194093, 0.9330127018922194093, 1.000000000000000000, 0.8660254037844387076, 1.000000000000000000, 0.8660254037844387076, 1.000000000000000000, 0.9330127018922194093, 0.9330127018922194093 ) ) 
 REPRESENTATION_ITEM ( '' )  );
#29491 = CIRCLE ( 'NONE', #3861, 11.00000000000000000 ) ;
#29492 = CARTESIAN_POINT ( 'NONE',  ( -7.500000000000000000, -1.572902445675612659, -7.069816568113127531 ) ) ;
#29493 = B_SPLINE_CURVE_WITH_KNOTS ( 'NONE', 3,
 ( #12977, #47396, #18120, #26514, #56105, #12026, #31655, #22008, #51290, #41602 ),
 .UNSPECIFIED., .F., .F.,
 ( 4, 2, 2, 2, 4 ),
 ( 1.572453990175171705E-19, 0.002305503304226491201, 0.004611006608452982401, 0.006916509912679473168, 0.009222013216905964803 ),
 .UNSPECIFIED. ) ;
#29494 = CARTESIAN_POINT ( 'NONE',  ( -2.500000000000000444, -0.1666666666666656582, -4.330127018922193649 ) ) ;
#29495 = CARTESIAN_POINT ( 'NONE',  ( -4.458734124999999437, -13.31249999863440259, 0.000000000000000000 ) ) ;
#29496 = VECTOR ( 'NONE', #35510, 1000.000000000000000 ) ;
#29497 = CARTESIAN_POINT ( 'NONE',  ( 4.458734124999998549, -101.9791666653010651, -2.574251347313721627 ) ) ;
#29498 = ORIENTED_EDGE ( 'NONE', *, *, #22562, .T. ) ;
#29499 = CARTESIAN_POINT ( 'NONE',  ( -8.190561711645485556E-16, -140.9375000013656063, 4.458734124999999437 ) ) ;
#29500 = CARTESIAN_POINT ( 'NONE',  ( -4.458734124999999437, -32.64583333196774362, -2.574251347313719407 ) ) ;
#29501 = VECTOR ( 'NONE', #62912, 1000.000000000000000 ) ;
#29502 = CARTESIAN_POINT ( 'NONE',  ( -5.000000000000000000, 5.125000002731184168, 0.000000000000000000 ) ) ;
#29503 = CARTESIAN_POINT ( 'NONE',  ( -52.10840900171896806, -134.1875000013656063, 3.393966926194110556 ) ) ;
#29504 = CARTESIAN_POINT ( 'NONE',  ( -2.229367062499996610, -71.39583333196773651, 3.861377020970582219 ) ) ;
#29505 = CARTESIAN_POINT ( 'NONE',  ( -5.000000000000000888, -144.5625000027311842, 2.071067811865474617 ) ) ;
#29506 = CARTESIAN_POINT ( 'NONE',  ( 0.000000000000000000, -170.0000000000000000, 0.000000000000000000 ) ) ;
#29507 = CARTESIAN_POINT ( 'NONE',  ( -7.922281120364393914, -4.573931137438277617, -8.047472243342932430 ) ) ;
#29508 = CARTESIAN_POINT ( 'NONE',  ( -3.152548672688508926E-16, 6.187500001365593860, -5.148502694627439702 ) ) ;
#29509 = EDGE_LOOP ( 'NONE', ( #38410, #47913, #2223, #1321 ) ) ;
#29510 = CARTESIAN_POINT ( 'NONE',  ( -1.339745962155613812, 1.794658198738520616, -5.000000000000000000 ) ) ;
#29511 = PLANE ( 'NONE',  #55525 ) ;
#29513 = CARTESIAN_POINT ( 'NONE',  ( 4.458734125000001214, -28.89583333196774007, 2.574251347313718519 ) ) ;
#29512 = CARTESIAN_POINT ( 'NONE',  ( -5.000000000000000000, -95.00000000000000000, 0.000000000000000000 ) ) ;
#29514 = CARTESIAN_POINT ( 'NONE',  ( 5.000000000000000000, -9.416666666666662522, -2.886751345948130876 ) ) ;
#29515 = CARTESIAN_POINT ( 'NONE',  ( -4.458734124999999437, -81.64583333196773651, -2.574251347313719407 ) ) ;
#29516 = CARTESIAN_POINT ( 'NONE',  ( 4.458734125000000326, 21.85416666803225993, 2.574251347313718519 ) ) ;
#29517 = CARTESIAN_POINT ( 'NONE',  ( 1.255007937094098239E-14, 22.87500000273118772, -4.999999999999999112 ) ) ;
#29518 = CARTESIAN_POINT ( 'NONE',  ( -59.29741812935640155, -142.6250000013655779, -2.196230717870135685 ) ) ;
#29519 = CARTESIAN_POINT ( 'NONE',  ( 4.458734124999998549, -2.729166665301069550, -2.574251347313721627 ) ) ;
#29520 = CARTESIAN_POINT ( 'NONE',  ( -4.458734124999998549, 23.52083333469892779, 2.574251347313722516 ) ) ;
#29521 = CARTESIAN_POINT ( 'NONE',  ( -4.458734124999997661, -41.47916666530107932, 2.574251347313722516 ) ) ;
#29522 = CARTESIAN_POINT ( 'NONE',  ( 1.975475456537005874E-15, -9.750000000000000000, 5.000000000000000000 ) ) ;
#29523 = CARTESIAN_POINT ( 'NONE',  ( -4.458734124999997661, 0.7708333346989268975, 2.574251347313722516 ) ) ;
#29524 = CARTESIAN_POINT ( 'NONE',  ( -3.152548672688508926E-16, -25.81249999863440792, -5.148502694627439702 ) ) ;
#29525 =( BOUNDED_CURVE ( )  B_SPLINE_CURVE ( 2, ( #19105, #14918, #34525, #58043, #38722, #53220, #59309, #44185, #58989 ),
 .UNSPECIFIED., .F., .F. ) 
 B_SPLINE_CURVE_WITH_KNOTS ( ( 3, 2, 2, 2, 3 ),
 ( 0.7624999999999999556, 0.7630952380952380487, 0.7642857142857142350, 0.7654761904761904212, 0.7660714285714286254 ),
 .UNSPECIFIED. ) 
 CURVE ( )  GEOMETRIC_REPRESENTATION_ITEM ( )  RATIONAL_B_SPLINE_CURVE ( ( 0.9330127018922194093, 0.9330127018922194093, 1.000000000000000000, 0.8660254037844387076, 1.000000000000000000, 0.8660254037844387076, 1.000000000000000000, 0.9330127018922130810, 0.9330127018922194093 ) ) 
 REPRESENTATION_ITEM ( '' )  );
#29526 = CARTESIAN_POINT ( 'NONE',  ( 4.458734124999998549, -70.72916666530107932, -2.574251347313721627 ) ) ;
#29527 = CARTESIAN_POINT ( 'NONE',  ( 2.499999999999998668, -103.2083333306021444, -4.330127018922193649 ) ) ;
#29528 = CARTESIAN_POINT ( 'NONE',  ( 2.229367062500001939, 28.02083333469892779, 3.861377020970579999 ) ) ;
#29529 = EDGE_CURVE ( 'NONE', #3800, #34229, #20458, .T. ) ;
#29530 = EDGE_CURVE ( 'NONE', #43260, #60995, #15572, .T. ) ;
#29531 = LINE ( 'NONE', #44984, #4045 ) ;
#29532 = CARTESIAN_POINT ( 'NONE',  ( 4.458734124999999437, -110.0624999986343937, -5.460374474430324690E-16 ) ) ;
#29533 = CARTESIAN_POINT ( 'NONE',  ( 4.458734124999998549, -72.97916666530107932, -2.574251347313721627 ) ) ;
#29534 = CARTESIAN_POINT ( 'NONE',  ( -2.499999999999996447, -59.83333333333333570, 4.330127018922195425 ) ) ;
#29535 = EDGE_CURVE ( 'NONE', #12722, #12555, #17639, .T. ) ;
#29536 = CARTESIAN_POINT ( 'NONE',  ( -2.500000000000000444, -11.04166666393547835, -4.330127018922193649 ) ) ;
#29537 = ORIENTED_EDGE ( 'NONE', *, *, #12938, .F. ) ;
#29538 = CARTESIAN_POINT ( 'NONE',  ( -3.535533905932738641, -140.3750000000000000, 3.535533905932737309 ) ) ;
#29539 = EDGE_CURVE ( 'NONE', #25625, #29321, #41640, .T. ) ;
#29540 = VECTOR ( 'NONE', #41312, 1000.000000000000000 ) ;
#29541 = FACE_OUTER_BOUND ( 'NONE', #53401, .T. ) ;
#29542 =( BOUNDED_CURVE ( )  B_SPLINE_CURVE ( 2, ( #21561, #60169, #30554, #16730, #41158, #36346, #30230, #20609, #30882 ),
 .UNSPECIFIED., .F., .F. ) 
 B_SPLINE_CURVE_WITH_KNOTS ( ( 3, 2, 2, 2, 3 ),
 ( 0.5583333333333337922, 0.5625000000000004441, 0.5666666666666670960, 0.5708333333333338588, 0.5750000000000005107 ),
 .UNSPECIFIED. ) 
 CURVE ( )  GEOMETRIC_REPRESENTATION_ITEM ( )  RATIONAL_B_SPLINE_CURVE ( ( 0.9999999999999918954, 0.9238795325112948431, 1.000000000000000000, 0.9238795325112867385, 1.000000000000000000, 0.9238795325112867385, 1.000000000000000000, 0.9238795325112766355, 1.000000000000010214 ) ) 
 REPRESENTATION_ITEM ( '' )  );
#29543 = CARTESIAN_POINT ( 'NONE',  ( 2.500000000000002220, -16.66666666666666430, 4.330127018922192761 ) ) ;
#29544 = CARTESIAN_POINT ( 'NONE',  ( -2.229367062500000163, -23.47916666530107221, -3.861377020970580443 ) ) ;
#29545 = EDGE_CURVE ( 'NONE', #40158, #20174, #46379, .T. ) ;
#29546 = CARTESIAN_POINT ( 'NONE',  ( -4.458734124999999437, -85.31249999863439371, 0.000000000000000000 ) ) ;
#29547 = EDGE_CURVE ( 'NONE', #20024, #12722, #4108, .T. ) ;
#29548 = CARTESIAN_POINT ( 'NONE',  ( -3.152801135295367985, -166.0625000013656063, 3.152801135295367096 ) ) ;
#29549 = CARTESIAN_POINT ( 'NONE',  ( 2.499999999999998668, -19.20833333060214798, -4.330127018922193649 ) ) ;
#29551 = ORIENTED_EDGE ( 'NONE', *, *, #46424, .F. ) ;
#29550 = CARTESIAN_POINT ( 'NONE',  ( 4.458734124999999437, -50.81249999863440792, -5.460374474430324690E-16 ) ) ;
#29552 = CARTESIAN_POINT ( 'NONE',  ( -1.339745962155610925, -75.66965819600731891, 5.000000000000000000 ) ) ;
#29553 = DIRECTION ( 'NONE',  ( 1.000000000000000000, 0.000000000000000000, 0.000000000000000000 ) ) ;
#29555 = VERTEX_POINT ( 'NONE', #46490 ) ;
#29554 = CARTESIAN_POINT ( 'NONE',  ( 2.229367062499998831, -0.8958333319677401763, -3.861377020970580887 ) ) ;
#29556 = CARTESIAN_POINT ( 'NONE',  ( -54.64476657466781973, -153.8125000013656347, -4.444560631937228834 ) ) ;
#29557 = CARTESIAN_POINT ( 'NONE',  ( 5.000000000000000000, -66.41666666666667140, -2.886751345948129988 ) ) ;
#29558 = EDGE_CURVE ( 'NONE', #63269, #51535, #51326, .T. ) ;
#29559 = CARTESIAN_POINT ( 'NONE',  ( 4.458734125000000326, -157.6250000013655779, -1.846868145590734978 ) ) ;
#29560 = CARTESIAN_POINT ( 'NONE',  ( 2.229367062500001939, -43.22916666530107932, 3.861377020970579999 ) ) ;
#29561 = CARTESIAN_POINT ( 'NONE',  ( -4.999999999999998224, -80.79166666393547303, 2.886751345948131764 ) ) ;
#29562 = CARTESIAN_POINT ( 'NONE',  ( 5.000000000000000000, -164.0625000000000000, 2.071067811865478614 ) ) ;
#29563 = EDGE_CURVE ( 'NONE', #4102, #454, #6941, .T. ) ;
#29564 = EDGE_CURVE ( 'NONE', #24132, #56134, #48420, .T. ) ;
#29565 = CARTESIAN_POINT ( 'NONE',  ( -6.972266317189433020E-16, -26.12499999726881583, -5.000000000000000000 ) ) ;
#29566 = CARTESIAN_POINT ( 'NONE',  ( -59.44456063193725015, -128.8125000013656063, -0.3552334253322034230 ) ) ;
#29567 = CARTESIAN_POINT ( 'NONE',  ( 4.458734125000001214, -12.14583333196774007, 2.574251347313718519 ) ) ;
#29568 = CARTESIAN_POINT ( 'NONE',  ( 4.458734124999999437, -45.06249999863440081, -5.460374474430324690E-16 ) ) ;
#29569 = FACE_OUTER_BOUND ( 'NONE', #44229, .T. ) ;
#29570 = CARTESIAN_POINT ( 'NONE',  ( 1.846868145590735200, -150.2500000013656063, -4.458734125000000326 ) ) ;
#29571 = CARTESIAN_POINT ( 'NONE',  ( 4.458734124999999437, -89.06249999863439371, -5.460374474430324690E-16 ) ) ;
#29572 = CARTESIAN_POINT ( 'NONE',  ( 5.000000000000000000, -108.4999999999999858, -6.123233995736766282E-16 ) ) ;
#29573 = ORIENTED_EDGE ( 'NONE', *, *, #27101, .T. ) ;
#29574 = CARTESIAN_POINT ( 'NONE',  ( 6.123233995736766282E-16, -170.0000000000000000, -5.000000000000000000 ) ) ;
#29575 = CARTESIAN_POINT ( 'NONE',  ( -6.972266317189433020E-16, -45.12499999726880162, -5.000000000000000000 ) ) ;
#29576 = CARTESIAN_POINT ( 'NONE',  ( -58.80597590150559739, -149.1250000027312126, 3.242614290531460330 ) ) ;
#29577 = CARTESIAN_POINT ( 'NONE',  ( -4.999999999999998224, -61.91666666666666430, 2.886751345948131764 ) ) ;
#29578 = ORIENTED_EDGE ( 'NONE', *, *, #20929, .T. ) ;
#29579 = CARTESIAN_POINT ( 'NONE',  ( -4.458734124999999437, 1.604166668032262155, -2.574251347313719407 ) ) ;
#29580 = CARTESIAN_POINT ( 'NONE',  ( -2.500000000000000444, -71.04166666393547303, -4.330127018922193649 ) ) ;
#29581 = CARTESIAN_POINT ( 'NONE',  ( -2.229367062499996610, -18.39583333196774007, 3.861377020970582219 ) ) ;
#29582 = CARTESIAN_POINT ( 'NONE',  ( -1.339745962155613812, -51.20534180126148271, -5.000000000000000000 ) ) ;
#29583 = CARTESIAN_POINT ( 'NONE',  ( -2.229367062500000163, -3.479166665301069994, -3.861377020970580443 ) ) ;
#29584 = CARTESIAN_POINT ( 'NONE',  ( -2.480964764533239819E-13, -73.62499999726883004, 5.000000000000000000 ) ) ;
#29585 = CARTESIAN_POINT ( 'NONE',  ( 3.152801135295366208, -149.5625000013655779, 3.152801135295367985 ) ) ;
#29586 = VECTOR ( 'NONE', #16478, 1000.000000000000000 ) ;
#29587 = CARTESIAN_POINT ( 'NONE',  ( 4.458734125000000326, 22.85416666803225993, 2.574251347313718519 ) ) ;
#29588 = VERTEX_POINT ( 'NONE', #47124 ) ;
#29589 = CARTESIAN_POINT ( 'NONE',  ( -4.458734124999999437, -98.31249999863440792, 0.000000000000000000 ) ) ;
#29590 = DIRECTION ( 'NONE',  ( 0.000000000000000000, 0.000000000000000000, 1.000000000000000000 ) ) ;
#29591 = CARTESIAN_POINT ( 'NONE',  ( 1.305263714129178743, -8.377797850839291627, -7.792447862505339273 ) ) ;
#29592 = CARTESIAN_POINT ( 'NONE',  ( 4.458734125000001214, -11.89583333196774007, 2.574251347313718519 ) ) ;
#29593 = CARTESIAN_POINT ( 'NONE',  ( 1.975475456537005874E-15, -81.62499999726881583, 5.000000000000000000 ) ) ;
#29594 = DIRECTION ( 'NONE',  ( -0.000000000000000000, 1.000000000000000000, -0.000000000000000000 ) ) ;
#29595 = CARTESIAN_POINT ( 'NONE',  ( -50.55543936806279248, -153.0625000013656063, 0.3552334253322060320 ) ) ;
#29596 = CARTESIAN_POINT ( 'NONE',  ( 1.060575238724906964E-15, -39.62499999726880873, 5.773502691896257311 ) ) ;
#29597 = CARTESIAN_POINT ( 'NONE',  ( 1.339745962155612702, -67.16965819600733312, -5.000000000000000000 ) ) ;
#29598 = CARTESIAN_POINT ( 'NONE',  ( 2.229367062500001939, 12.02083333469892601, 3.861377020970579999 ) ) ;
#29599 = CARTESIAN_POINT ( 'NONE',  ( 1.339745962155615144, -51.58034179853028434, 4.999999999999999112 ) ) ;
#29600 = PRODUCT_RELATED_PRODUCT_CATEGORY ( 'part', '', ( #24548 ) ) ;
#29601 = DIRECTION ( 'NONE',  ( 0.000000000000000000, 0.000000000000000000, 1.000000000000000000 ) ) ;
#29602 = CARTESIAN_POINT ( 'NONE',  ( 4.458734125000000326, 19.10416666803225638, 2.574251347313718519 ) ) ;
#29603 = CARTESIAN_POINT ( 'NONE',  ( 4.458734124999998549, -61.72916666530106511, -2.574251347313721627 ) ) ;
#29604 = ORIENTED_EDGE ( 'NONE', *, *, #5971, .F. ) ;
#29605 = CARTESIAN_POINT ( 'NONE',  ( 9.457646018065525792E-16, -6.312499998634403475, 5.148502694627439702 ) ) ;
#29606 = CARTESIAN_POINT ( 'NONE',  ( 5.000000000000000000, -109.3749999972688016, -6.123233995736766282E-16 ) ) ;
#29607 = CARTESIAN_POINT ( 'NONE',  ( -4.999999999999999112, 5.083333333333332149, 2.886751345948131764 ) ) ;
#29608 = CARTESIAN_POINT ( 'NONE',  ( -4.458734125000001214, -168.8750000013655779, 1.846868145590734089 ) ) ;
#29609 = CARTESIAN_POINT ( 'NONE',  ( 2.500000000000002220, -63.54166666393547303, 4.330127018922192761 ) ) ;
#29610 = CARTESIAN_POINT ( 'NONE',  ( 2.229367062499998831, -51.64583333196773651, -3.861377020970580887 ) ) ;
#29611 = CARTESIAN_POINT ( 'NONE',  ( -5.000000000000000000, -86.95833333060214443, -2.886751345948128211 ) ) ;
#29612 = CARTESIAN_POINT ( 'NONE',  ( 4.458734125000000326, -33.89583333196772941, 2.574251347313718519 ) ) ;
#29613 = AXIS2_PLACEMENT_3D ( 'NONE', #45832, #40037, #45190 ) ;
#29614 = CARTESIAN_POINT ( 'NONE',  ( -6.972266317189433020E-16, -77.25000000000000000, -5.000000000000000000 ) ) ;
#29615 = DIRECTION ( 'NONE',  ( -0.000000000000000000, 1.000000000000000000, -0.000000000000000000 ) ) ;
#29616 = LINE ( 'NONE', #24805, #49061 ) ;
#29617 = CARTESIAN_POINT ( 'NONE',  ( 4.458734124999999437, -151.6875000013656063, 0.000000000000000000 ) ) ;
#29618 = CARTESIAN_POINT ( 'NONE',  ( 2.500000000000002220, -42.66666666666667140, 4.330127018922192761 ) ) ;
#29619 = CYLINDRICAL_SURFACE ( 'NONE', #34602, 5.000000000000000000 ) ;
#29620 = CARTESIAN_POINT ( 'NONE',  ( -59.70202243701069023, -135.0000000000000853, 1.323094887694161281 ) ) ;
#29621 = VERTEX_POINT ( 'NONE', #42289 ) ;
#29622 = CARTESIAN_POINT ( 'NONE',  ( 2.229367062499998831, -101.6458333319677365, -3.861377020970580887 ) ) ;
#29623 = CARTESIAN_POINT ( 'NONE',  ( 2.229367062499998831, 4.104166668032260823, -3.861377020970580887 ) ) ;
#29624 = CARTESIAN_POINT ( 'NONE',  ( -51.75738570946856498, -155.0000000000000284, 3.805975901505577408 ) ) ;
#29625 = CARTESIAN_POINT ( 'NONE',  ( -2.499999999999996447, -0.8333333333333317050, 4.330127018922195425 ) ) ;
#29626 = CARTESIAN_POINT ( 'NONE',  ( -4.458734124999999437, -64.39583333196773651, -2.574251347313719407 ) ) ;
#29627 =( BOUNDED_CURVE ( )  B_SPLINE_CURVE ( 2, ( #53859, #53239, #28787, #9477, #58381, #4976, #48403, #4345, #33930 ),
 .UNSPECIFIED., .F., .F. ) 
 B_SPLINE_CURVE_WITH_KNOTS ( ( 3, 2, 2, 2, 3 ),
 ( 0.6354166666666666297, 0.6361111111111110716, 0.6374999999999999556, 0.6388888888888888395, 0.6395833333333332815 ),
 .UNSPECIFIED. ) 
 CURVE ( )  GEOMETRIC_REPRESENTATION_ITEM ( )  RATIONAL_B_SPLINE_CURVE ( ( 0.9330127018922194093, 0.9330127018922194093, 1.000000000000000000, 0.8660254037844387076, 1.000000000000000000, 0.8660254037844387076, 1.000000000000000000, 0.9330127018922194093, 0.9330127018922194093 ) ) 
 REPRESENTATION_ITEM ( '' )  );
#29628 = DIRECTION ( 'NONE',  ( 0.8660254037844410391, -0.4999999999999958367, -0.000000000000000000 ) ) ;
#29629 = CARTESIAN_POINT ( 'NONE',  ( 1.060575238724906964E-15, -2.624999997268815388, 5.773502691896257311 ) ) ;
#29631 = VERTEX_POINT ( 'NONE', #2438 ) ;
#29630 = CARTESIAN_POINT ( 'NONE',  ( 4.458734124999999437, -33.81249999863440792, -5.460374474430324690E-16 ) ) ;
#29632 = CARTESIAN_POINT ( 'NONE',  ( 5.000000000000000000, -153.1875000027312126, 2.071067811865478614 ) ) ;
#29633 = CARTESIAN_POINT ( 'NONE',  ( -1.339745962155610925, -47.66965819600734022, 5.000000000000000000 ) ) ;
#29634 = VERTEX_POINT ( 'NONE', #36841 ) ;
#29635 = CARTESIAN_POINT ( 'NONE',  ( -6.972266317189433020E-16, -100.1249999972688016, -5.000000000000000000 ) ) ;
#29636 = CARTESIAN_POINT ( 'NONE',  ( -2.499999999999996447, -49.83333333333332860, 4.330127018922195425 ) ) ;
#29638 = CARTESIAN_POINT ( 'NONE',  ( 9.457646018065525792E-16, -24.31249999863440792, 5.148502694627439702 ) ) ;
#29637 = CYLINDRICAL_SURFACE ( 'NONE', #54166, 5.000000000000000000 ) ;
#29639 = CARTESIAN_POINT ( 'NONE',  ( 1.339745962155615144, -32.58034179853029144, 4.999999999999999112 ) ) ;
#29640 = CARTESIAN_POINT ( 'NONE',  ( 4.458734125000001214, -69.89583333196773651, 2.574251347313718519 ) ) ;
#29641 = CARTESIAN_POINT ( 'NONE',  ( 3.152801135295366208, -142.8125000013655779, 3.152801135295367985 ) ) ;
#29642 = CARTESIAN_POINT ( 'NONE',  ( -2.229367062500000163, -82.47916666530106511, -3.861377020970580443 ) ) ;
#29643 = AXIS2_PLACEMENT_3D ( 'NONE', #47383, #12009, #7521 ) ;
#29644 = CARTESIAN_POINT ( 'NONE',  ( -53.51423613279429503, -140.5000000013656347, 4.591703134518082763 ) ) ;
#29645 = CARTESIAN_POINT ( 'NONE',  ( 2.229367062499998831, -28.89583333196774007, -3.861377020970580887 ) ) ;
#29646 = CARTESIAN_POINT ( 'NONE',  ( 1.060575238724906964E-15, -72.62499999726880162, 5.773502691896257311 ) ) ;
#29647 = EDGE_CURVE ( 'NONE', #1425, #37461, #23824, .T. ) ;
#29648 = ORIENTED_EDGE ( 'NONE', *, *, #2745, .F. ) ;
#29649 = CARTESIAN_POINT ( 'NONE',  ( 1.975475456537005874E-15, -82.62499999726878741, 5.000000000000000000 ) ) ;
#29650 = ORIENTED_EDGE ( 'NONE', *, *, #47515, .F. ) ;
#29651 = CARTESIAN_POINT ( 'NONE',  ( 2.229367062500001939, -71.22916666530107932, 3.861377020970579999 ) ) ;
#29652 = CARTESIAN_POINT ( 'NONE',  ( -5.000000000000000000, 28.91666666666666430, -2.886751345948128211 ) ) ;
#29653 = SURFACE_STYLE_USAGE ( .BOTH. , #726 ) ;
#29654 = EDGE_LOOP ( 'NONE', ( #34968, #9857, #49736, #61282 ) ) ;
#29655 = DIRECTION ( 'NONE',  ( -3.614007241618347908E-17, 0.000000000000000000, -1.000000000000000000 ) ) ;
#29656 = CARTESIAN_POINT ( 'NONE',  ( 5.000000000000000000, -12.41666666666666607, -2.886751345948130876 ) ) ;
#29657 = CARTESIAN_POINT ( 'NONE',  ( 2.229367062500001939, -57.22916666530107932, 3.861377020970579999 ) ) ;
#29658 = CARTESIAN_POINT ( 'NONE',  ( 2.229367062499998831, -1.895833331967737623, -3.861377020970580887 ) ) ;
#29659 = ORIENTED_EDGE ( 'NONE', *, *, #22758, .T. ) ;
#29660 = CARTESIAN_POINT ( 'NONE',  ( -51.75738570946856498, -136.8750000027312126, 3.805975901505576964 ) ) ;
#29661 = CARTESIAN_POINT ( 'NONE',  ( -5.000000000000000000, -45.08333333333333570, -2.886751345948128211 ) ) ;
#29662 = CARTESIAN_POINT ( 'NONE',  ( -4.458734124999998549, 13.77083333469892779, 2.574251347313722516 ) ) ;
#29663 = CARTESIAN_POINT ( 'NONE',  ( -50.70258187064364108, -140.1250000013655779, 2.196230717870141014 ) ) ;
#29664 = FACE_OUTER_BOUND ( 'NONE', #56272, .T. ) ;
#29665 = CARTESIAN_POINT ( 'NONE',  ( 4.458734124999999437, -163.4375000013655779, 0.000000000000000000 ) ) ;
#29666 = ORIENTED_EDGE ( 'NONE', *, *, #52400, .F. ) ;
#29667 = CARTESIAN_POINT ( 'NONE',  ( -4.458734124999999437, -83.39583333196773651, -2.574251347313719407 ) ) ;
#29668 = CARTESIAN_POINT ( 'NONE',  ( -4.458734124999999437, -0.3958333319677397322, -2.574251347313719407 ) ) ;
#29669 = CARTESIAN_POINT ( 'NONE',  ( 5.000000000000000000, -83.49999999999998579, -6.123233995736766282E-16 ) ) ;
#29670 = CARTESIAN_POINT ( 'NONE',  ( 1.339745962155612702, -40.16965819600733312, -5.000000000000000000 ) ) ;
#29671 = CARTESIAN_POINT ( 'NONE',  ( -4.458734124999998549, -66.47916666530106511, 2.574251347313722516 ) ) ;
#29672 = CARTESIAN_POINT ( 'NONE',  ( -2.500000000000000444, -27.04166666393548013, -4.330127018922193649 ) ) ;
#29673 = FACE_OUTER_BOUND ( 'NONE', #12697, .T. ) ;
#29674 = CARTESIAN_POINT ( 'NONE',  ( -2.229367062500000163, 27.52083333469892779, -3.861377020970580443 ) ) ;
#29675 = CARTESIAN_POINT ( 'NONE',  ( -2.500000000000000444, -65.04166666393547303, -4.330127018922193649 ) ) ;
#29676 =( BOUNDED_CURVE ( )  B_SPLINE_CURVE ( 2, ( #8517, #51953, #37166, #7891, #61612, #13341, #27188, #46804, #27811 ),
 .UNSPECIFIED., .F., .F. ) 
 B_SPLINE_CURVE_WITH_KNOTS ( ( 3, 2, 2, 2, 3 ),
 ( 0.1645833333333333315, 0.1652777777777777735, 0.1666666666666666574, 0.1680555555555555691, 0.1687500000000000111 ),
 .UNSPECIFIED. ) 
 CURVE ( )  GEOMETRIC_REPRESENTATION_ITEM ( )  RATIONAL_B_SPLINE_CURVE ( ( 0.9330127018922194093, 0.9330127018922194093, 1.000000000000000000, 0.8660254037844387076, 1.000000000000000000, 0.8660254037844387076, 1.000000000000000000, 0.9330127018922194093, 0.9330127018922194093 ) ) 
 REPRESENTATION_ITEM ( '' )  );
#29677 = DIRECTION ( 'NONE',  ( -0.000000000000000000, 1.000000000000000000, -0.000000000000000000 ) ) ;
#29678 = CARTESIAN_POINT ( 'NONE',  ( 2.229367062499998831, -43.64583333196773651, -3.861377020970580887 ) ) ;
#29679 = CARTESIAN_POINT ( 'NONE',  ( -4.458734124999999437, -32.64583333196773651, -2.574251347313719407 ) ) ;
#29680 = CARTESIAN_POINT ( 'NONE',  ( 4.458734125000000326, 7.854166668032260823, 2.574251347313718519 ) ) ;
#29681 =( GEOMETRIC_REPRESENTATION_CONTEXT ( 3 ) GLOBAL_UNCERTAINTY_ASSIGNED_CONTEXT ( ( #33040 ) ) GLOBAL_UNIT_ASSIGNED_CONTEXT ( ( #13615, #28396, #12664 ) ) REPRESENTATION_CONTEXT ( 'NONE', 'WORKASPACE' ) );
#29682 = CARTESIAN_POINT ( 'NONE',  ( -5.000000000000000000, -9.874999997268815832, 0.000000000000000000 ) ) ;
#29683 = CARTESIAN_POINT ( 'NONE',  ( 5.000000000000000888, 20.41666666666666430, 2.886751345948126879 ) ) ;
#29684 = CARTESIAN_POINT ( 'NONE',  ( 3.535533905932736864, -148.2500000027311842, 3.535533905932738641 ) ) ;
#29685 = CARTESIAN_POINT ( 'NONE',  ( -2.229367062499996610, -36.14583333196773651, 3.861377020970582219 ) ) ;
#29686 = CARTESIAN_POINT ( 'NONE',  ( -4.999999999999999112, -75.79166666393545881, 2.886751345948131764 ) ) ;
#29687 = CARTESIAN_POINT ( 'NONE',  ( -58.39396692619412477, -143.6875000013656063, 2.891590998281057701 ) ) ;
#29688 = CARTESIAN_POINT ( 'NONE',  ( 2.071067811865476394, -142.1875000000000284, 5.000000000000000000 ) ) ;
#29689 = CARTESIAN_POINT ( 'NONE',  ( -4.458734124999997661, -81.47916666530106511, 2.574251347313722516 ) ) ;
#29690 = CARTESIAN_POINT ( 'NONE',  ( 4.458734124999999437, -163.6875000013655779, 0.000000000000000000 ) ) ;
#29691 = CARTESIAN_POINT ( 'NONE',  ( -4.458734124999997661, -38.22916666530107932, 2.574251347313722516 ) ) ;
#29692 = CARTESIAN_POINT ( 'NONE',  ( -5.000000000000000000, -33.00000000000000000, 0.000000000000000000 ) ) ;
#29693 = LINE ( 'NONE', #53827, #49259 ) ;
#29694 = CARTESIAN_POINT ( 'NONE',  ( -5.000000000000000000, -23.00000000000000000, 0.000000000000000000 ) ) ;
#29695 = CARTESIAN_POINT ( 'NONE',  ( 1.846868145590736310, -142.6250000013655779, 4.458734124999999437 ) ) ;
#29696 = ORIENTED_EDGE ( 'NONE', *, *, #13810, .F. ) ;
#29697 = CARTESIAN_POINT ( 'NONE',  ( -3.152548672688508926E-16, 28.18750000136559564, -5.148502694627439702 ) ) ;
#29698 = ORIENTED_EDGE ( 'NONE', *, *, #60875, .T. ) ;
#29699 = CARTESIAN_POINT ( 'NONE',  ( -3.152548672688508926E-16, -61.81249999863440081, -5.148502694627439702 ) ) ;
#29700 = CARTESIAN_POINT ( 'NONE',  ( -5.000000000000000000, 20.12500000273118772, 0.000000000000000000 ) ) ;
#29701 = CARTESIAN_POINT ( 'NONE',  ( 1.975475456537005874E-15, 13.37500000273118417, 5.000000000000000000 ) ) ;
#29702 = CARTESIAN_POINT ( 'NONE',  ( -4.999999999999999112, 11.08333333333333393, 2.886751345948131764 ) ) ;
#29703 = CARTESIAN_POINT ( 'NONE',  ( 9.457646018065525792E-16, -53.06249999863440792, 5.148502694627439702 ) ) ;
#29704 = CARTESIAN_POINT ( 'NONE',  ( -4.458734124999999437, -5.395833331967740953, -2.574251347313719407 ) ) ;
#29705 = CARTESIAN_POINT ( 'NONE',  ( 2.071067811865508812, -166.3125000027312126, 4.999999999999968026 ) ) ;
#29706 = CARTESIAN_POINT ( 'NONE',  ( -2.500000000000000444, -41.04166666393548013, -4.330127018922193649 ) ) ;
#29707 = CARTESIAN_POINT ( 'NONE',  ( 5.000000000000000000, -158.1875000027312126, 2.071067811865478614 ) ) ;
#29708 = CARTESIAN_POINT ( 'NONE',  ( 1.062108568985190270E-13, -10.25000000000000355, -4.999999999999999112 ) ) ;
#29710 = CARTESIAN_POINT ( 'NONE',  ( 4.458734124999999437, -20.81249999863440081, -5.460374474430324690E-16 ) ) ;
#29709 = CARTESIAN_POINT ( 'NONE',  ( -6.972266317189433020E-16, -36.12499999726880162, -5.000000000000000000 ) ) ;
#29711 = CARTESIAN_POINT ( 'NONE',  ( 1.339745962155612702, -97.16965819600731891, -5.000000000000000000 ) ) ;
#29712 = CARTESIAN_POINT ( 'NONE',  ( -2.229367062500000163, -54.47916666530107221, -3.861377020970580443 ) ) ;
#29713 = CARTESIAN_POINT ( 'NONE',  ( 2.730187237215162345E-16, -155.4375000013655779, -4.458734124999999437 ) ) ;
#29714 = CARTESIAN_POINT ( 'NONE',  ( -3.535250795749689387E-16, -58.12499999726880162, -5.773502691896257311 ) ) ;
#29715 = EDGE_LOOP ( 'NONE', ( #24843, #45383, #58856, #39933 ) ) ;
#29716 = CARTESIAN_POINT ( 'NONE',  ( 2.229367062499998831, 5.104166668032261711, -3.861377020970580887 ) ) ;
#29717 = VERTEX_POINT ( 'NONE', #61611 ) ;
#29718 = CYLINDRICAL_SURFACE ( 'NONE', #59465, 5.000000000000000000 ) ;
#29719 = CARTESIAN_POINT ( 'NONE',  ( 4.458734124999999437, -158.4375000013655779, 0.000000000000000000 ) ) ;
#29720 = VERTEX_POINT ( 'NONE', #32322 ) ;
#29721 =( GEOMETRIC_REPRESENTATION_CONTEXT ( 3 ) GLOBAL_UNCERTAINTY_ASSIGNED_CONTEXT ( ( #60809 ) ) GLOBAL_UNIT_ASSIGNED_CONTEXT ( ( #29172, #43964, #29806 ) ) REPRESENTATION_CONTEXT ( 'NONE', 'WORKASPACE' ) );
#29722 =( BOUNDED_CURVE ( )  B_SPLINE_CURVE ( 2, ( #7099, #17060, #55026, #6466, #36677, #6144, #20936, #45692, #25759 ),
 .UNSPECIFIED., .F., .F. ) 
 B_SPLINE_CURVE_WITH_KNOTS ( ( 3, 2, 2, 2, 3 ),
 ( 0.05535714285714286170, 0.05595238095238095483, 0.05714285714285714107, 0.05833333333333333426, 0.05892857142857142738 ),
 .UNSPECIFIED. ) 
 CURVE ( )  GEOMETRIC_REPRESENTATION_ITEM ( )  RATIONAL_B_SPLINE_CURVE ( ( 0.9330127018922194093, 0.9330127018922197424, 1.000000000000000000, 0.8660254037844387076, 1.000000000000000000, 0.8660254037844387076, 1.000000000000000000, 0.9330127018922194093, 0.9330127018922194093 ) ) 
 REPRESENTATION_ITEM ( '' )  );
#29723 = LINE ( 'NONE', #48713, #27285 ) ;
#29724 = CARTESIAN_POINT ( 'NONE',  ( -60.14911071818854538, -131.0625000000000284, 1.666127454062681368 ) ) ;
#29726 = VECTOR ( 'NONE', #41110, 1000.000000000000000 ) ;
#29725 = CARTESIAN_POINT ( 'NONE',  ( 5.000000000000000000, -153.0000000000000284, 0.000000000000000000 ) ) ;
#29727 = CARTESIAN_POINT ( 'NONE',  ( 4.458734125000001214, -45.14583333196774362, 2.574251347313718519 ) ) ;
#29728 = VERTEX_POINT ( 'NONE', #51952 ) ;
#29729 = CARTESIAN_POINT ( 'NONE',  ( 0.000000000000000000, -170.0000000000000000, 0.000000000000000000 ) ) ;
#29730 = CARTESIAN_POINT ( 'NONE',  ( 9.457646018065525792E-16, 13.93750000136559564, 5.148502694627439702 ) ) ;
#29731 = CARTESIAN_POINT ( 'NONE',  ( -6.972266317189433020E-16, 3.875000002731185500, -5.000000000000000000 ) ) ;
#29732 = ORIENTED_EDGE ( 'NONE', *, *, #57478, .T. ) ;
#29733 = CARTESIAN_POINT ( 'NONE',  ( -3.152548672688508926E-16, -88.81249999863439371, -5.148502694627439702 ) ) ;
#29734 = CARTESIAN_POINT ( 'NONE',  ( -59.44456063193725015, -153.5625000013656063, -0.3552334253322034230 ) ) ;
#29735 = CARTESIAN_POINT ( 'NONE',  ( -2.916731409357579869E-14, 12.37500000273118594, 5.000000000000000888 ) ) ;
#29736 = CARTESIAN_POINT ( 'NONE',  ( -6.972266317189433020E-16, -6.249999999999999112, -5.000000000000000000 ) ) ;
#29737 = CARTESIAN_POINT ( 'NONE',  ( -6.972266317189433020E-16, -29.12499999726881228, -5.000000000000000000 ) ) ;
#29738 = CARTESIAN_POINT ( 'NONE',  ( 4.458734125000000326, -63.89583333196772941, 2.574251347313718519 ) ) ;
#29739 = CARTESIAN_POINT ( 'NONE',  ( -51.75738570946856498, -155.0000000000000284, 3.805975901505577408 ) ) ;
#29740 = CARTESIAN_POINT ( 'NONE',  ( 9.457646018065525792E-16, 15.93750000136559564, 5.148502694627439702 ) ) ;
#29741 = EDGE_CURVE ( 'NONE', #46354, #4805, #13123, .T. ) ;
#29742 = CARTESIAN_POINT ( 'NONE',  ( -1.339745962155599601, 17.79465819873852439, -5.000000000000007994 ) ) ;
#29743 = CARTESIAN_POINT ( 'NONE',  ( 9.457646018065525792E-16, -47.31249999863440792, 5.148502694627439702 ) ) ;
#29744 = CARTESIAN_POINT ( 'NONE',  ( -5.000000000000000000, -7.874999997268813168, 0.000000000000000000 ) ) ;
#29745 = CARTESIAN_POINT ( 'NONE',  ( -6.972266317189433020E-16, -42.12499999726880873, -5.000000000000000000 ) ) ;
#29746 = CARTESIAN_POINT ( 'NONE',  ( -1.339745962155613812, -67.08034179853029855, -5.000000000000000000 ) ) ;
#29747 = CARTESIAN_POINT ( 'NONE',  ( 9.457646018065525792E-16, -90.31249999863439371, 5.148502694627439702 ) ) ;
#29748 = CARTESIAN_POINT ( 'NONE',  ( -4.458734124999999437, -106.3124999986343937, 0.000000000000000000 ) ) ;
#29749 = CARTESIAN_POINT ( 'NONE',  ( -2.229367062499996610, -17.39583333196773651, 3.861377020970582219 ) ) ;
#29750 = ORIENTED_EDGE ( 'NONE', *, *, #60151, .T. ) ;
#29751 = CARTESIAN_POINT ( 'NONE',  ( -5.000000000000000888, -143.5625000027311842, 2.071067811865474617 ) ) ;
#29752 = CARTESIAN_POINT ( 'NONE',  ( 4.458734124999998549, -98.72916666530105090, -2.574251347313721627 ) ) ;
#29753 = CARTESIAN_POINT ( 'NONE',  ( 3.061616997868383141E-16, -161.8750000027311842, -5.000000000000000000 ) ) ;
#29754 = CARTESIAN_POINT ( 'NONE',  ( 2.229367062500001939, -95.22916666530106511, 3.861377020970579999 ) ) ;
#29755 = CARTESIAN_POINT ( 'NONE',  ( -6.972266317189433020E-16, -7.124999997268814056, -5.000000000000000000 ) ) ;
#29756 = CARTESIAN_POINT ( 'NONE',  ( 1.060575238724906964E-15, -56.62499999726880162, 5.773502691896257311 ) ) ;
#29757 = DIRECTION ( 'NONE',  ( 0.000000000000000000, 0.000000000000000000, 1.000000000000000000 ) ) ;
#29758 = CARTESIAN_POINT ( 'NONE',  ( -54.64476657466781973, -125.8125000013655921, -4.444560631937228834 ) ) ;
#29759 = CARTESIAN_POINT ( 'NONE',  ( -50.55543936806279248, -148.0625000013656063, 0.3552334253322060320 ) ) ;
#29760 = CARTESIAN_POINT ( 'NONE',  ( -4.458734124999997661, -19.22916666530106866, 2.574251347313722516 ) ) ;
#29761 = CARTESIAN_POINT ( 'NONE',  ( 4.458734124999999437, 5.937500001365593860, -5.460374474430324690E-16 ) ) ;
#29762 = CARTESIAN_POINT ( 'NONE',  ( -4.458734124999997661, -61.47916666530106511, 2.574251347313722516 ) ) ;
#29763 = DIRECTION ( 'NONE',  ( 0.000000000000000000, 0.000000000000000000, 1.000000000000000000 ) ) ;
#29764 = CARTESIAN_POINT ( 'NONE',  ( 4.458734124999999437, -19.81249999863440081, -5.460374474430324690E-16 ) ) ;
#29765 = CARTESIAN_POINT ( 'NONE',  ( 75.00000000000000000, 15.00000000000000000, 8.999999999999998224 ) ) ;
#29766 = CARTESIAN_POINT ( 'NONE',  ( -9.184850993605147944E-16, -156.2500000000000000, 5.000000000000000000 ) ) ;
#29767 = CARTESIAN_POINT ( 'NONE',  ( 2.500000000000002220, -6.666666666666667851, 4.330127018922192761 ) ) ;
#29768 = VERTEX_POINT ( 'NONE', #18162 ) ;
#29769 = CARTESIAN_POINT ( 'NONE',  ( -4.458734124999999437, -44.64583333196773651, -2.574251347313719407 ) ) ;
#29770 = CARTESIAN_POINT ( 'NONE',  ( -1.339745962155614034, 26.20534180126147561, 4.999999999999999112 ) ) ;
#29771 = CARTESIAN_POINT ( 'NONE',  ( 1.339745962155612702, -66.29465819873851729, -5.000000000000000000 ) ) ;
#29772 = CARTESIAN_POINT ( 'NONE',  ( -2.499999999999996447, 27.29166666939785202, 4.330127018922195425 ) ) ;
#29773 = CARTESIAN_POINT ( 'NONE',  ( -4.458734124999999437, -88.31249999863439371, 0.000000000000000000 ) ) ;
#29774 = CARTESIAN_POINT ( 'NONE',  ( -4.458734124999999437, 19.43750000136559208, 0.000000000000000000 ) ) ;
#29775 = VECTOR ( 'NONE', #32975, 1000.000000000000000 ) ;
#29776 = CARTESIAN_POINT ( 'NONE',  ( -4.458734124999998549, 11.77083333469892601, 2.574251347313722516 ) ) ;
#29777 = CARTESIAN_POINT ( 'NONE',  ( -5.000000000000000000, -44.00000000000000000, 0.000000000000000000 ) ) ;
#29778 = CARTESIAN_POINT ( 'NONE',  ( 5.275681513340003914E-14, 11.74999999999999645, -5.000000000000000000 ) ) ;
#29779 = CARTESIAN_POINT ( 'NONE',  ( -6.972266317189433020E-16, 25.74999999999999645, -5.000000000000000000 ) ) ;
#29780 = CARTESIAN_POINT ( 'NONE',  ( -2.229367062500000163, 19.27083333469892779, -3.861377020970580443 ) ) ;
#29781 = CARTESIAN_POINT ( 'NONE',  ( 1.060575238724906964E-15, -73.75000000000000000, 5.773502691896257311 ) ) ;
#29782 = CARTESIAN_POINT ( 'NONE',  ( -5.000000000000000000, 7.041666669397851130, -2.886751345948128211 ) ) ;
#29783 = ORIENTED_EDGE ( 'NONE', *, *, #30346, .T. ) ;
#29784 = DIRECTION ( 'NONE',  ( -0.000000000000000000, 1.000000000000000000, -0.000000000000000000 ) ) ;
#29785 = EDGE_LOOP ( 'NONE', ( #55540, #48394, #35044, #5114 ) ) ;
#29786 = DIRECTION ( 'NONE',  ( -0.000000000000000000, 1.000000000000000000, -0.000000000000000000 ) ) ;
#29787 = CARTESIAN_POINT ( 'NONE',  ( -4.458734124999999437, -39.31249999863440081, 0.000000000000000000 ) ) ;
#29788 = CARTESIAN_POINT ( 'NONE',  ( 5.000000000000000888, -39.45833333060214443, 2.886751345948126879 ) ) ;
#29789 = ORIENTED_EDGE ( 'NONE', *, *, #50875, .F. ) ;
#29790 = CARTESIAN_POINT ( 'NONE',  ( -58.39396692619412477, -147.6875000013656063, 2.891590998281057701 ) ) ;
#29791 = CARTESIAN_POINT ( 'NONE',  ( -4.458734124999998549, -14.22916666530107221, 2.574251347313722516 ) ) ;
#29793 = ORIENTED_EDGE ( 'NONE', *, *, #42834, .T. ) ;
#29792 = CARTESIAN_POINT ( 'NONE',  ( -3.152548672688508926E-16, -11.81249999863440969, -5.148502694627439702 ) ) ;
#29794 = CARTESIAN_POINT ( 'NONE',  ( 1.060575238724906964E-15, -84.74999999999998579, 5.773502691896257311 ) ) ;
#29795 = CARTESIAN_POINT ( 'NONE',  ( -4.999999999999998224, 1.208333336064518981, 2.886751345948131764 ) ) ;
#29796 = CARTESIAN_POINT ( 'NONE',  ( 2.229367062499998831, -63.89583333196772941, -3.861377020970580887 ) ) ;
#29798 = CARTESIAN_POINT ( 'NONE',  ( 5.000000000000000888, -80.45833333060213022, 2.886751345948126879 ) ) ;
#29797 = APPLICATION_CONTEXT ( 'automotive_design' ) ;
#29800 = EDGE_LOOP ( 'NONE', ( #39308, #61511, #22171, #167 ) ) ;
#29799 = CARTESIAN_POINT ( 'NONE',  ( -5.000000000000000000, -32.08333333333332860, -2.886751345948128211 ) ) ;
#29801 = CARTESIAN_POINT ( 'NONE',  ( -55.39835681537999790, -144.8750000000000284, 4.984105922594378235 ) ) ;
#29802 = CARTESIAN_POINT ( 'NONE',  ( 4.458734125000001214, -28.14583333196774007, 2.574251347313718519 ) ) ;
#29803 = CARTESIAN_POINT ( 'NONE',  ( 1.975475456537005874E-15, -52.75000000000000000, 5.000000000000000000 ) ) ;
#29804 = ORIENTED_EDGE ( 'NONE', *, *, #35657, .T. ) ;
#29805 =( BOUNDED_CURVE ( )  B_SPLINE_CURVE ( 2, ( #38432, #51671, #46834, #7612, #42001, #61642, #37193, #37499, #38741 ),
 .UNSPECIFIED., .F., .F. ) 
 B_SPLINE_CURVE_WITH_KNOTS ( ( 3, 2, 2, 2, 3 ),
 ( 0.5696428571428571175, 0.5702380952380952106, 0.5714285714285713969, 0.5726190476190475831, 0.5732142857142856762 ),
 .UNSPECIFIED. ) 
 CURVE ( )  GEOMETRIC_REPRESENTATION_ITEM ( )  RATIONAL_B_SPLINE_CURVE ( ( 0.9330127018922194093, 0.9330127018922194093, 1.000000000000000000, 0.8660254037844387076, 1.000000000000000000, 0.8660254037844387076, 1.000000000000000000, 0.9330127018922194093, 0.9330127018922194093 ) ) 
 REPRESENTATION_ITEM ( '' )  );
#29806 =( NAMED_UNIT ( * ) SI_UNIT ( $, .STERADIAN. ) SOLID_ANGLE_UNIT ( ) );
#29807 = CARTESIAN_POINT ( 'NONE',  ( 3.152801135295367541, -162.5625000013656063, -3.152801135295367541 ) ) ;
#29808 = CARTESIAN_POINT ( 'NONE',  ( 4.458734125000001214, -104.1458333319677365, 2.574251347313718519 ) ) ;
#29809 = CARTESIAN_POINT ( 'NONE',  ( 3.535533905932738197, -147.8750000000000000, -3.535533905932738197 ) ) ;
#29810 = ORIENTED_EDGE ( 'NONE', *, *, #11348, .T. ) ;
#29811 = CARTESIAN_POINT ( 'NONE',  ( -57.19623071787016499, -147.6250000013655779, 4.297418129356382899 ) ) ;
#29812 = VECTOR ( 'NONE', #15771, 1000.000000000000000 ) ;
#29813 = CARTESIAN_POINT ( 'NONE',  ( -2.229367062500000163, -72.72916666530107932, -3.861377020970580443 ) ) ;
#29814 = CARTESIAN_POINT ( 'NONE',  ( -60.14911071818854538, -137.1875000027312126, 1.666127454062681368 ) ) ;
#29815 = CARTESIAN_POINT ( 'NONE',  ( 9.457646018065525792E-16, -46.06249999863440081, 5.148502694627439702 ) ) ;
#29816 = CARTESIAN_POINT ( 'NONE',  ( -1.846868145590737420, -146.0000000013655779, 4.458734124999997661 ) ) ;
#29817 = CARTESIAN_POINT ( 'NONE',  ( -1.510657702057710340E-15, 28.25000000000000000, 5.000000000000000000 ) ) ;
#29818 = ADVANCED_FACE ( 'NONE', ( #28747 ), #4942, .T. ) ;
#29819 = CARTESIAN_POINT ( 'NONE',  ( -2.229367062500000163, -13.47916666530107221, -3.861377020970580443 ) ) ;
#29820 = CARTESIAN_POINT ( 'NONE',  ( 5.000000000000000000, -101.4166666666666572, -2.886751345948129988 ) ) ;
#29821 = VERTEX_POINT ( 'NONE', #58659 ) ;
#29822 =( BOUNDED_CURVE ( )  B_SPLINE_CURVE ( 2, ( #55055, #10979, #60208, #6170, #25787, #1364, #16451, #37332, #8389 ),
 .UNSPECIFIED., .F., .F. ) 
 B_SPLINE_CURVE_WITH_KNOTS ( ( 3, 2, 2, 2, 3 ),
 ( 0.4250000000000003220, 0.4291666666666669738, 0.4333333333333336812, 0.4375000000000003886, 0.4416666666666670404 ),
 .UNSPECIFIED. ) 
 CURVE ( )  GEOMETRIC_REPRESENTATION_ITEM ( )  RATIONAL_B_SPLINE_CURVE ( ( 0.9999999999999938938, 0.9238795325112928447, 1.000000000000000000, 0.9238795325112867385, 1.000000000000000000, 0.9238795325112867385, 1.000000000000000000, 0.9238795325112796331, 1.000000000000007105 ) ) 
 REPRESENTATION_ITEM ( '' )  );
#29823 = CARTESIAN_POINT ( 'NONE',  ( 1.975475456537005874E-15, -10.62499999726881228, 5.000000000000000000 ) ) ;
#29824 = CARTESIAN_POINT ( 'NONE',  ( 2.229367062499998831, -34.89583333196772941, -3.861377020970580887 ) ) ;
#29825 = CARTESIAN_POINT ( 'NONE',  ( -4.999999999999999112, 6.208333336064520758, 2.886751345948131764 ) ) ;
#29826 = CYLINDRICAL_SURFACE ( 'NONE', #14956, 5.000000000000000000 ) ;
#29827 = CARTESIAN_POINT ( 'NONE',  ( -54.64476657466781973, -131.8125000013656063, -4.444560631937228834 ) ) ;
#29828 = CARTESIAN_POINT ( 'NONE',  ( -4.458734124999999437, -74.64583333196773651, -2.574251347313719407 ) ) ;
#29829 = LINE ( 'NONE', #45273, #14775 ) ;
#29830 = CARTESIAN_POINT ( 'NONE',  ( -49.85088928181150436, -146.6875000027312126, -1.666127454062680480 ) ) ;
#29831 = LINE ( 'NONE', #25337, #60356 ) ;
#29832 = CARTESIAN_POINT ( 'NONE',  ( 4.458734124999999437, 3.937500001365595192, -5.460374474430324690E-16 ) ) ;
#29833 = VERTEX_POINT ( 'NONE', #63179 ) ;
#29834 = LINE ( 'NONE', #54290, #14081 ) ;
#29835 = CARTESIAN_POINT ( 'NONE',  ( 2.500000000000002220, -15.66666666666666963, 4.330127018922192761 ) ) ;
#29837 = CARTESIAN_POINT ( 'NONE',  ( -4.458734124999999437, -31.39583333196773296, -2.574251347313719407 ) ) ;
#29836 = CARTESIAN_POINT ( 'NONE',  ( 5.000000000000000000, -98.50000000000000000, -6.123233995736766282E-16 ) ) ;
#29838 = ADVANCED_FACE ( 'NONE', ( #33585 ), #13340, .T. ) ;
#29839 = CARTESIAN_POINT ( 'NONE',  ( -5.000000000000000000, -36.08333333333332860, -2.886751345948128211 ) ) ;
#29840 = CARTESIAN_POINT ( 'NONE',  ( -2.229367062499996610, -83.39583333196773651, 3.861377020970582219 ) ) ;
#29841 = CARTESIAN_POINT ( 'NONE',  ( 4.458734124999998549, 20.02083333469892779, -2.574251347313721627 ) ) ;
#29842 = CARTESIAN_POINT ( 'NONE',  ( -1.339745962155611370, 26.79465819873851729, -5.000000000000000888 ) ) ;
#29843 = CARTESIAN_POINT ( 'NONE',  ( -59.29741812935640155, -138.6250000013655779, -2.196230717870135685 ) ) ;
#29844 = CARTESIAN_POINT ( 'NONE',  ( 4.458734124999999437, -0.8124999986344055847, -5.460374474430324690E-16 ) ) ;
#29845 = CARTESIAN_POINT ( 'NONE',  ( 4.458734125000001214, 23.85416666803225993, 2.574251347313718519 ) ) ;
#29846 = ADVANCED_FACE ( 'NONE', ( #57419 ), #53204, .T. ) ;
#29847 = CARTESIAN_POINT ( 'NONE',  ( -3.152548672688508926E-16, -40.81249999863440081, -5.148502694627439702 ) ) ;
#29848 = CARTESIAN_POINT ( 'NONE',  ( -6.972266317189433020E-16, -105.2500000000000000, -5.000000000000000000 ) ) ;
#29849 = CARTESIAN_POINT ( 'NONE',  ( -2.229367062499996610, 0.8541666680322613781, 3.861377020970582219 ) ) ;
#29850 = CARTESIAN_POINT ( 'NONE',  ( -2.229367062499996610, -32.39583333196773651, 3.861377020970582219 ) ) ;
#29851 = CARTESIAN_POINT ( 'NONE',  ( -3.152548672688508926E-16, -68.56249999863439371, -5.148502694627439702 ) ) ;
#29852 = CARTESIAN_POINT ( 'NONE',  ( -5.000000000000000000, -106.8749999972687874, 0.000000000000000000 ) ) ;
#29853 = CARTESIAN_POINT ( 'NONE',  ( 9.457646018065525792E-16, 23.93750000136559564, 5.148502694627439702 ) ) ;
#29854 = CARTESIAN_POINT ( 'NONE',  ( -2.499999999999996447, -64.83333333333332860, 4.330127018922195425 ) ) ;
#29855 = CARTESIAN_POINT ( 'NONE',  ( -55.39835681537999790, -153.0000000027312410, 4.984105922594378235 ) ) ;
#29856 = CARTESIAN_POINT ( 'NONE',  ( -2.229367062499996610, -70.39583333196773651, 3.861377020970582219 ) ) ;
#29857 = CARTESIAN_POINT ( 'NONE',  ( -5.000000000000000000, -60.08333333333333570, -2.886751345948128211 ) ) ;
#29858 = CARTESIAN_POINT ( 'NONE',  ( -1.339745962155613812, -66.08034179853028434, -5.000000000000000000 ) ) ;
#29859 = CARTESIAN_POINT ( 'NONE',  ( -5.000000000000000000, 24.04166666939785202, -2.886751345948128211 ) ) ;
#29860 = VERTEX_POINT ( 'NONE', #57728 ) ;
#29861 = CARTESIAN_POINT ( 'NONE',  ( 1.975475456537005874E-15, 6.249999999999998224, 5.000000000000000000 ) ) ;
#29862 = VECTOR ( 'NONE', #1891, 1000.000000000000000 ) ;
#29863 = CARTESIAN_POINT ( 'NONE',  ( 0.000000000000000000, -170.0000000000000000, 5.000000000000000000 ) ) ;
#29864 = CARTESIAN_POINT ( 'NONE',  ( -3.535250795749689387E-16, -20.24999999999999645, -5.773502691896257311 ) ) ;
#29865 = CARTESIAN_POINT ( 'NONE',  ( 2.229367062500001939, -20.97916666530107221, 3.861377020970579999 ) ) ;
#29866 = AXIS2_PLACEMENT_3D ( 'NONE', #3246, #51803, #62093 ) ;
#29867 = EDGE_CURVE ( 'NONE', #54415, #31328, #62243, .T. ) ;
#29868 = CARTESIAN_POINT ( 'NONE',  ( 4.458734125000000326, -80.89583333196773651, 2.574251347313718519 ) ) ;
#29869 = CARTESIAN_POINT ( 'NONE',  ( 5.000000000000000000, -20.37499999726880873, -6.123233995736766282E-16 ) ) ;
#29871 = ORIENTED_EDGE ( 'NONE', *, *, #15680, .T. ) ;
#29870 = CARTESIAN_POINT ( 'NONE',  ( 9.457646018065525792E-16, -50.06249999863440792, 5.148502694627439702 ) ) ;
#29872 = CARTESIAN_POINT ( 'NONE',  ( 5.000000000000000888, -35.45833333060213732, 2.886751345948126879 ) ) ;
#29873 = CARTESIAN_POINT ( 'NONE',  ( -5.000000000000000000, -27.95833333060214798, -2.886751345948128211 ) ) ;
#29875 = ORIENTED_EDGE ( 'NONE', *, *, #29539, .T. ) ;
#29874 = CARTESIAN_POINT ( 'NONE',  ( 2.229367062500001939, 3.770833334698926009, 3.861377020970579999 ) ) ;
#29876 = CARTESIAN_POINT ( 'NONE',  ( -50.70258187064364108, -149.1250000013656063, 2.196230717870141014 ) ) ;
#29877 = CARTESIAN_POINT ( 'NONE',  ( -4.999999999999999112, -67.91666666666667140, 2.886751345948131764 ) ) ;
#29878 = CARTESIAN_POINT ( 'NONE',  ( -1.846868145590737420, -151.0000000013656063, 4.458734124999999437 ) ) ;
#29879 = CARTESIAN_POINT ( 'NONE',  ( 2.229367062499998831, -41.89583333196773651, -3.861377020970580887 ) ) ;
#29880 = CARTESIAN_POINT ( 'NONE',  ( -2.500000000000000444, -77.04166666393547303, -4.330127018922193649 ) ) ;
#29881 =( BOUNDED_CURVE ( )  B_SPLINE_CURVE ( 2, ( #42450, #8377, #17398, #47293, #46656, #37632, #2602, #52442, #37013 ),
 .UNSPECIFIED., .F., .F. ) 
 B_SPLINE_CURVE_WITH_KNOTS ( ( 3, 2, 2, 2, 3 ),
 ( 0.9562500000000000444, 0.9569444444444444864, 0.9583333333333333703, 0.9597222222222222543, 0.9604166666666666963 ),
 .UNSPECIFIED. ) 
 CURVE ( )  GEOMETRIC_REPRESENTATION_ITEM ( )  RATIONAL_B_SPLINE_CURVE ( ( 0.9330127018922194093, 0.9330127018922194093, 1.000000000000000000, 0.8660254037844387076, 1.000000000000000000, 0.8660254037844387076, 1.000000000000000000, 0.9330127018922194093, 0.9330127018922194093 ) ) 
 REPRESENTATION_ITEM ( '' )  );
#29882 = CARTESIAN_POINT ( 'NONE',  ( 3.061616997868383141E-16, -161.7500000000000000, -5.000000000000000000 ) ) ;
#29883 = DIRECTION ( 'NONE',  ( 0.000000000000000000, 0.000000000000000000, 1.000000000000000000 ) ) ;
#29884 = CARTESIAN_POINT ( 'NONE',  ( -57.19623071787017210, -125.6250000013656205, 4.297418129356382899 ) ) ;
#29885 = CARTESIAN_POINT ( 'NONE',  ( -4.458734124999999437, -11.64583333196773829, -2.574251347313719407 ) ) ;
#29886 = CARTESIAN_POINT ( 'NONE',  ( 9.457646018065525792E-16, -44.31249999863440081, 5.148502694627439702 ) ) ;
#29887 = DIRECTION ( 'NONE',  ( -0.000000000000000000, 1.000000000000000000, -0.000000000000000000 ) ) ;
#29888 = CARTESIAN_POINT ( 'NONE',  ( -1.846868145590737420, -144.7500000013656063, 4.458734124999999437 ) ) ;
#29889 = CARTESIAN_POINT ( 'NONE',  ( 4.458734124999998549, -88.97916666530107932, -2.574251347313721627 ) ) ;
#29890 = DIRECTION ( 'NONE',  ( -0.000000000000000000, 1.000000000000000000, -0.000000000000000000 ) ) ;
#29891 = ORIENTED_EDGE ( 'NONE', *, *, #55046, .F. ) ;
#29892 = DIRECTION ( 'NONE',  ( 0.000000000000000000, 0.000000000000000000, 1.000000000000000000 ) ) ;
#29893 = CARTESIAN_POINT ( 'NONE',  ( 9.457646018065525792E-16, 28.68750000136559208, 5.148502694627439702 ) ) ;
#29894 = CARTESIAN_POINT ( 'NONE',  ( -56.66612745406270335, -152.4375000027311842, -5.149110718188516067 ) ) ;
#29895 = CARTESIAN_POINT ( 'NONE',  ( 1.975475456537005874E-15, -29.62499999726881228, 5.000000000000000000 ) ) ;
#29896 = VERTEX_POINT ( 'NONE', #52893 ) ;
#29897 = CARTESIAN_POINT ( 'NONE',  ( -4.458734124999998549, 2.770833334698928674, 2.574251347313722516 ) ) ;
#29898 = EDGE_CURVE ( 'NONE', #45305, #41928, #34203, .T. ) ;
#29899 = EDGE_CURVE ( 'NONE', #16288, #3805, #8610, .T. ) ;
#29900 = CARTESIAN_POINT ( 'NONE',  ( 5.000000000000000000, -106.4999999999999858, -6.123233995736766282E-16 ) ) ;
#29901 = CARTESIAN_POINT ( 'NONE',  ( -4.458734124999999437, -15.64583333196773474, -2.574251347313719407 ) ) ;
#29902 = ADVANCED_FACE ( 'NONE', ( #39032 ), #33894, .T. ) ;
#29903 = FACE_OUTER_BOUND ( 'NONE', #15095, .T. ) ;
#29904 = CARTESIAN_POINT ( 'NONE',  ( 2.229367062500001939, -4.979166665301071326, 3.861377020970579999 ) ) ;
#29905 = CARTESIAN_POINT ( 'NONE',  ( -1.339745962155727277, -73.66965819600733312, 4.999999999999933387 ) ) ;
#29906 = CARTESIAN_POINT ( 'NONE',  ( -4.458734124999999437, -150.9375000013656063, -5.460374474430324690E-16 ) ) ;
#29907 =( BOUNDED_CURVE ( )  B_SPLINE_CURVE ( 2, ( #3327, #61232, #61870, #8459, #36778, #7199, #17786, #22945, #22305 ),
 .UNSPECIFIED., .F., .F. ) 
 B_SPLINE_CURVE_WITH_KNOTS ( ( 3, 2, 2, 2, 3 ),
 ( 0.1770833333333333426, 0.1777777777777777846, 0.1791666666666666685, 0.1805555555555555525, 0.1812499999999999944 ),
 .UNSPECIFIED. ) 
 CURVE ( )  GEOMETRIC_REPRESENTATION_ITEM ( )  RATIONAL_B_SPLINE_CURVE ( ( 0.9330127018922194093, 0.9330127018922194093, 1.000000000000000000, 0.8660254037844387076, 1.000000000000000000, 0.8660254037844387076, 1.000000000000000000, 0.9330127018922194093, 0.9330127018922194093 ) ) 
 REPRESENTATION_ITEM ( '' )  );
#29908 = CARTESIAN_POINT ( 'NONE',  ( 2.229367062499998831, 23.10416666803225993, -3.861377020970580887 ) ) ;
#29909 = ORIENTED_EDGE ( 'NONE', *, *, #8580, .T. ) ;
#29910 = CARTESIAN_POINT ( 'NONE',  ( 4.458734125000000326, -94.89583333196775072, 2.574251347313718519 ) ) ;
#29911 = CARTESIAN_POINT ( 'NONE',  ( -2.500000000000000444, -34.04166666393547303, -4.330127018922193649 ) ) ;
#29912 = CARTESIAN_POINT ( 'NONE',  ( 5.000000000000000888, -57.45833333060214443, 2.886751345948126879 ) ) ;
#29913 = CARTESIAN_POINT ( 'NONE',  ( 4.458734124999998549, -14.72916666530107399, -2.574251347313721627 ) ) ;
#29914 = VECTOR ( 'NONE', #4364, 1000.000000000000000 ) ;
#29916 = EDGE_CURVE ( 'NONE', #35585, #1423, #34904, .T. ) ;
#29915 = DIRECTION ( 'NONE',  ( 0.000000000000000000, 0.000000000000000000, 1.000000000000000000 ) ) ;
#29917 = CARTESIAN_POINT ( 'NONE',  ( 1.339745962155615144, 8.419658201469706782, 4.999999999999999112 ) ) ;
#29918 = CARTESIAN_POINT ( 'NONE',  ( -58.39396692619412477, -148.4375000013656063, 2.891590998281057701 ) ) ;
#29919 = CARTESIAN_POINT ( 'NONE',  ( 5.000000000000000888, -39.45833333060214443, 2.886751345948126879 ) ) ;
#29920 = CARTESIAN_POINT ( 'NONE',  ( -1.339745962155618253, 21.33034180399265978, 4.999999999999996447 ) ) ;
#29921 = CARTESIAN_POINT ( 'NONE',  ( 4.458734124999999437, 13.18750000136559208, -5.460374474430324690E-16 ) ) ;
#29922 = CYLINDRICAL_SURFACE ( 'NONE', #5785, 5.000000000000000000 ) ;
#29923 = ADVANCED_FACE ( 'NONE', ( #42916 ), #18482, .T. ) ;
#29924 = CARTESIAN_POINT ( 'NONE',  ( 4.458734124999999437, 20.18750000136559208, -5.460374474430324690E-16 ) ) ;
#29925 = CARTESIAN_POINT ( 'NONE',  ( 2.229367062499998831, -59.64583333196774362, -3.861377020970580887 ) ) ;
#29926 = EDGE_LOOP ( 'NONE', ( #23956, #37508, #31132, #52761 ) ) ;
#29927 = CARTESIAN_POINT ( 'NONE',  ( -3.152548672688508926E-16, -6.812499998634404363, -5.148502694627439702 ) ) ;
#29928 = CARTESIAN_POINT ( 'NONE',  ( 2.499999999999998668, 5.666666666666666963, -4.330127018922193649 ) ) ;
#29929 = CARTESIAN_POINT ( 'NONE',  ( 1.846868145590735200, -163.2500000013655495, -4.458734125000000326 ) ) ;
#29931 = EDGE_CURVE ( 'NONE', #5270, #51028, #30385, .T. ) ;
#29930 = CARTESIAN_POINT ( 'NONE',  ( 1.975475456537005874E-15, -88.74999999999998579, 5.000000000000000000 ) ) ;
#29932 = CARTESIAN_POINT ( 'NONE',  ( 4.458734124999999437, -54.81249999863440081, -5.460374474430324690E-16 ) ) ;
#29933 = CARTESIAN_POINT ( 'NONE',  ( -5.000000000000000000, -87.95833333060213022, -2.886751345948128211 ) ) ;
#29934 = CARTESIAN_POINT ( 'NONE',  ( -4.458734124999997661, -32.22916666530106511, 2.574251347313722516 ) ) ;
#29935 = DIRECTION ( 'NONE',  ( -0.000000000000000000, 1.000000000000000000, -0.000000000000000000 ) ) ;
#29936 = LINE ( 'NONE', #55, #35774 ) ;
#29937 = DIRECTION ( 'NONE',  ( -0.000000000000000000, 1.000000000000000000, -0.000000000000000000 ) ) ;
#29938 = CARTESIAN_POINT ( 'NONE',  ( -8.190561711645485556E-16, -153.9375000013655779, 4.458734124999999437 ) ) ;
#29939 = CARTESIAN_POINT ( 'NONE',  ( -4.999999999999999112, -41.91666666666667140, 2.886751345948131764 ) ) ;
#29940 = CARTESIAN_POINT ( 'NONE',  ( 1.339745962155612702, -98.16965819600733312, -5.000000000000000000 ) ) ;
#29941 = CARTESIAN_POINT ( 'NONE',  ( -58.09382797660032338, -135.0000000000000284, -3.377790754402798967 ) ) ;
#29942 = ORIENTED_EDGE ( 'NONE', *, *, #50397, .T. ) ;
#29943 = CARTESIAN_POINT ( 'NONE',  ( -4.458734124999999437, -101.3958333319677365, -2.574251347313719407 ) ) ;
#29944 = CARTESIAN_POINT ( 'NONE',  ( 4.458734124999999437, 3.937500001365595192, -5.460374474430324690E-16 ) ) ;
#29945 = CARTESIAN_POINT ( 'NONE',  ( 0.000000000000000000, -120.0000000000000000, 5.000000000000000000 ) ) ;
#29946 = CARTESIAN_POINT ( 'NONE',  ( 5.000000000000000888, -1.583333333333332593, 2.886751345948126879 ) ) ;
#29947 = CARTESIAN_POINT ( 'NONE',  ( 2.229367062500001939, -66.97916666530106511, 3.861377020970579999 ) ) ;
#29948 = CYLINDRICAL_SURFACE ( 'NONE', #2099, 5.000000000000000000 ) ;
#29949 = CARTESIAN_POINT ( 'NONE',  ( -5.000000000000000000, -3.874999997268816720, 0.000000000000000000 ) ) ;
#29951 = ORIENTED_EDGE ( 'NONE', *, *, #26033, .F. ) ;
#29950 = CARTESIAN_POINT ( 'NONE',  ( 4.458734125000001214, -32.89583333196774362, 2.574251347313718519 ) ) ;
#29952 = CYLINDRICAL_SURFACE ( 'NONE', #45081, 5.000000000000000000 ) ;
#29953 = CARTESIAN_POINT ( 'NONE',  ( -4.999999999999998224, -47.79166666393547303, 2.886751345948131764 ) ) ;
#29954 = ORIENTED_EDGE ( 'NONE', *, *, #17376, .T. ) ;
#29955 = CARTESIAN_POINT ( 'NONE',  ( -2.499999999999996447, -55.70833333060214443, 4.330127018922195425 ) ) ;
#29956 = CARTESIAN_POINT ( 'NONE',  ( 5.000000000000000000, -49.41666666666667140, -2.886751345948129988 ) ) ;
#29958 = CARTESIAN_POINT ( 'NONE',  ( -3.152548672688508926E-16, -24.81249999863440436, -5.148502694627439702 ) ) ;
#29957 = CARTESIAN_POINT ( 'NONE',  ( 5.000000000000000888, -17.45833333060214443, 2.886751345948126879 ) ) ;
#29959 = CARTESIAN_POINT ( 'NONE',  ( -6.972266317189433020E-16, 13.87500000273118594, -5.000000000000000000 ) ) ;
#29960 = CARTESIAN_POINT ( 'NONE',  ( -4.458734124999998549, -68.22916666530107932, 2.574251347313722516 ) ) ;
#29961 = CARTESIAN_POINT ( 'NONE',  ( 2.730187237215162345E-16, -144.4375000013656063, -4.458734124999999437 ) ) ;
#29962 = CARTESIAN_POINT ( 'NONE',  ( 4.458734125000001214, -83.89583333196773651, 2.574251347313718519 ) ) ;
#29963 = CARTESIAN_POINT ( 'NONE',  ( -52.80376928212989185, -138.1250000013656063, -4.297418129356379346 ) ) ;
#29964 = CARTESIAN_POINT ( 'NONE',  ( -3.152548672688508926E-16, -31.81249999863440792, -5.148502694627439702 ) ) ;
#29965 = CARTESIAN_POINT ( 'NONE',  ( -3.535250795749689387E-16, -72.12499999726881583, -5.773502691896257311 ) ) ;
#29966 = ORIENTED_EDGE ( 'NONE', *, *, #62981, .T. ) ;
#29967 = CARTESIAN_POINT ( 'NONE',  ( 5.000000000000000000, -20.37499999726880873, -6.123233995736766282E-16 ) ) ;
#29968 = ORIENTED_EDGE ( 'NONE', *, *, #59618, .F. ) ;
#29969 = CARTESIAN_POINT ( 'NONE',  ( -4.458734124999999437, -72.56249999863439371, 0.000000000000000000 ) ) ;
#29970 = CARTESIAN_POINT ( 'NONE',  ( 0.000000000000000000, -120.0000000000000000, 0.000000000000000000 ) ) ;
#29971 = ORIENTED_EDGE ( 'NONE', *, *, #9514, .F. ) ;
#29972 = VECTOR ( 'NONE', #5218, 1000.000000000000000 ) ;
#29973 = CARTESIAN_POINT ( 'NONE',  ( -58.24261429053147765, -140.2500000000000000, -3.805975901505573855 ) ) ;
#29974 = CARTESIAN_POINT ( 'NONE',  ( -2.499999999999996447, -75.70833333060214443, 4.330127018922195425 ) ) ;
#29975 = CARTESIAN_POINT ( 'NONE',  ( 2.229367062499998831, -58.89583333196773651, -3.861377020970580887 ) ) ;
#29976 = CARTESIAN_POINT ( 'NONE',  ( 2.229367062499998831, -5.895833331967740953, -3.861377020970580887 ) ) ;
#29977 = ORIENTED_EDGE ( 'NONE', *, *, #34178, .T. ) ;
#29978 = EDGE_CURVE ( 'NONE', #31397, #14365, #10668, .T. ) ;
#29979 = CARTESIAN_POINT ( 'NONE',  ( -5.000000000000000000, -20.08333333333333925, -2.886751345948128211 ) ) ;
#29980 = CARTESIAN_POINT ( 'NONE',  ( 0.000000000000000000, 0.000000000000000000, -10.00000000000000000 ) ) ;
#29981 = CARTESIAN_POINT ( 'NONE',  ( -2.229367062499996610, 14.85416666803226171, 3.861377020970582219 ) ) ;
#29982 = CARTESIAN_POINT ( 'NONE',  ( -59.29741812935640155, -141.6250000013656063, -2.196230717870135685 ) ) ;
#29983 = CARTESIAN_POINT ( 'NONE',  ( 4.458734124999999437, -159.3750000013656063, -1.846868145590734978 ) ) ;
#29984 = CYLINDRICAL_SURFACE ( 'NONE', #38867, 5.000000000000000000 ) ;
#29985 = VERTEX_POINT ( 'NONE', #14902 ) ;
#29986 = CARTESIAN_POINT ( 'NONE',  ( -3.152548672688508926E-16, -83.56249999863440792, -5.148502694627439702 ) ) ;
#29987 = DIRECTION ( 'NONE',  ( -0.000000000000000000, 1.000000000000000000, -0.000000000000000000 ) ) ;
#29988 = CARTESIAN_POINT ( 'NONE',  ( -4.458734124999999437, 1.604166668032262155, -2.574251347313719407 ) ) ;
#29989 = CARTESIAN_POINT ( 'NONE',  ( 5.000000000000000000, -85.41666666666665719, -2.886751345948129988 ) ) ;
#29990 = CARTESIAN_POINT ( 'NONE',  ( 5.000000000000000000, -36.50000000000000711, -6.123233995736766282E-16 ) ) ;
#29991 = CARTESIAN_POINT ( 'NONE',  ( -2.229367062500000163, -63.72916666530106511, -3.861377020970580443 ) ) ;
#29992 = CARTESIAN_POINT ( 'NONE',  ( -2.500000000000000444, -23.04166666393548013, -4.330127018922193649 ) ) ;
#29993 = CARTESIAN_POINT ( 'NONE',  ( 5.000000000000000888, 12.54166666939785557, 2.886751345948126879 ) ) ;
#29994 = CARTESIAN_POINT ( 'NONE',  ( -1.339745962155610925, -0.6696581960073348938, 5.000000000000000000 ) ) ;
#29995 = CARTESIAN_POINT ( 'NONE',  ( -5.000000000000000000, -37.87499999726881583, 0.000000000000000000 ) ) ;
#29996 = CARTESIAN_POINT ( 'NONE',  ( 1.975475456537005874E-15, -8.750000000000000000, 5.000000000000000000 ) ) ;
#29997 = EDGE_CURVE ( 'NONE', #1043, #25291, #25197, .T. ) ;
#29998 = CARTESIAN_POINT ( 'NONE',  ( -4.458734124999998549, -46.22916666530106511, 2.574251347313722516 ) ) ;
#29999 = CARTESIAN_POINT ( 'NONE',  ( -4.458734124999997661, -30.47916666530107221, 2.574251347313722516 ) ) ;
#30000 = CARTESIAN_POINT ( 'NONE',  ( -4.458734124999997661, 5.520833334698926009, 2.574251347313722516 ) ) ;
#30001 = CARTESIAN_POINT ( 'NONE',  ( 5.000000000000000888, -146.0625000027312126, -2.071067811865475505 ) ) ;
#30002 = CARTESIAN_POINT ( 'NONE',  ( -2.499999999999996447, 22.16666666666666785, 4.330127018922195425 ) ) ;
#30003 = EDGE_CURVE ( 'NONE', #14537, #14586, #25516, .T. ) ;
#30004 = CARTESIAN_POINT ( 'NONE',  ( -9.184850993605147944E-16, -150.3750000027312126, 5.000000000000000000 ) ) ;
#30005 = CARTESIAN_POINT ( 'NONE',  ( -5.000000000000000000, 28.91666666666666430, -2.886751345948128211 ) ) ;
#30006 = CARTESIAN_POINT ( 'NONE',  ( 9.457646018065525792E-16, -38.06249999863441502, 5.148502694627439702 ) ) ;
#30007 = CARTESIAN_POINT ( 'NONE',  ( 2.499999999999998668, -72.20833333060214443, -4.330127018922193649 ) ) ;
#30008 = CARTESIAN_POINT ( 'NONE',  ( -52.10840900171896806, -145.4375000013656063, 3.393966926194110556 ) ) ;
#30009 =( BOUNDED_CURVE ( )  B_SPLINE_CURVE ( 2, ( #3269, #42478, #62116, #18035, #48872, #25073, #38907, #5140, #19289 ),
 .UNSPECIFIED., .F., .F. ) 
 B_SPLINE_CURVE_WITH_KNOTS ( ( 3, 2, 2, 2, 3 ),
 ( 0.5916666666666671182, 0.5958333333333335480, 0.6000000000000000888, 0.6041666666666665186, 0.6083333333333329485 ),
 .UNSPECIFIED. ) 
 CURVE ( )  GEOMETRIC_REPRESENTATION_ITEM ( )  RATIONAL_B_SPLINE_CURVE ( ( 0.9999999999999918954, 0.9238795325112948431, 1.000000000000000000, 0.9238795325112867385, 1.000000000000000000, 0.9238795325112867385, 1.000000000000000000, 0.9238795325112928447, 0.9999999999999938938 ) ) 
 REPRESENTATION_ITEM ( '' )  );
#30010 = CARTESIAN_POINT ( 'NONE',  ( -6.972266317189433020E-16, -61.12499999726880162, -5.000000000000000000 ) ) ;
#30011 = ADVANCED_FACE ( 'NONE', ( #34511 ), #137, .T. ) ;
#30012 = CARTESIAN_POINT ( 'NONE',  ( 1.339745962155615144, -15.58034179853029499, 4.999999999999999112 ) ) ;
#30013 = CARTESIAN_POINT ( 'NONE',  ( 4.458734124999999437, -79.06249999863440792, -5.460374474430324690E-16 ) ) ;
#30014 = CARTESIAN_POINT ( 'NONE',  ( -1.846868145590737420, -165.0000000013655779, 4.458734124999997661 ) ) ;
#30015 = DIRECTION ( 'NONE',  ( -0.000000000000000000, 1.000000000000000000, -0.000000000000000000 ) ) ;
#30016 = FACE_OUTER_BOUND ( 'NONE', #52919, .T. ) ;
#30017 = CARTESIAN_POINT ( 'NONE',  ( -4.999999999999999112, -26.91666666666666075, 2.886751345948131764 ) ) ;
#30018 = CARTESIAN_POINT ( 'NONE',  ( -4.458734125000001214, -143.8750000013656063, 1.846868145590734089 ) ) ;
#30019 = VERTEX_POINT ( 'NONE', #6227 ) ;
#30020 = CARTESIAN_POINT ( 'NONE',  ( 5.000000000000000888, -90.45833333060214443, 2.886751345948126879 ) ) ;
#30021 = ORIENTED_EDGE ( 'NONE', *, *, #56237, .T. ) ;
#30022 = CARTESIAN_POINT ( 'NONE',  ( 4.458734125000000326, -61.14583333196773651, 2.574251347313718519 ) ) ;
#30023 = CARTESIAN_POINT ( 'NONE',  ( -3.535250795749689387E-16, 23.87500000273118417, -5.773502691896257311 ) ) ;
#30024 = CARTESIAN_POINT ( 'NONE',  ( -51.75738570946856498, -138.8750000027312126, 3.805975901505576964 ) ) ;
#30025 = CARTESIAN_POINT ( 'NONE',  ( -2.499999999999996447, 13.16666666666666607, 4.330127018922195425 ) ) ;
#30026 = CARTESIAN_POINT ( 'NONE',  ( 4.458734125000000326, -49.89583333196772941, 2.574251347313718519 ) ) ;
#30027 = CARTESIAN_POINT ( 'NONE',  ( 4.458734125000001214, -7.895833331967735624, 2.574251347313718519 ) ) ;
#30028 = CARTESIAN_POINT ( 'NONE',  ( 5.000000000000000000, -166.1250000027312126, 0.000000000000000000 ) ) ;
#30029 = DIRECTION ( 'NONE',  ( -0.000000000000000000, 1.000000000000000000, -0.000000000000000000 ) ) ;
#30030 = CARTESIAN_POINT ( 'NONE',  ( -75.00000000000000000, 15.00000000000000000, 8.999999999999998224 ) ) ;
#30031 = CARTESIAN_POINT ( 'NONE',  ( -1.339745962155613812, -80.08034179853028434, -5.000000000000000000 ) ) ;
#30032 = CARTESIAN_POINT ( 'NONE',  ( 0.000000000000000000, -120.0000000000000000, 0.000000000000000000 ) ) ;
#30034 = CARTESIAN_POINT ( 'NONE',  ( 2.229367062500001939, -22.97916666530107221, 3.861377020970579999 ) ) ;
#30033 = CARTESIAN_POINT ( 'NONE',  ( 1.975475456537005874E-15, -58.75000000000000000, 5.000000000000000000 ) ) ;
#30035 = CARTESIAN_POINT ( 'NONE',  ( -6.972266317189433020E-16, -32.12499999726880873, -5.000000000000000000 ) ) ;
#30036 = CARTESIAN_POINT ( 'NONE',  ( -4.458734124999999437, -52.31249999863440792, 0.000000000000000000 ) ) ;
#30037 = CARTESIAN_POINT ( 'NONE',  ( 1.846868145590735200, -154.5000000013656347, -4.458734125000000326 ) ) ;
#30038 = CARTESIAN_POINT ( 'NONE',  ( 1.060575238724906964E-15, -55.62499999726880873, 5.773502691896257311 ) ) ;
#30039 = VERTEX_POINT ( 'NONE', #54142 ) ;
#30040 = DIRECTION ( 'NONE',  ( -0.000000000000000000, 1.000000000000000000, -0.000000000000000000 ) ) ;
#30041 = CARTESIAN_POINT ( 'NONE',  ( 2.229367062500001939, 2.770833334698928674, 3.861377020970579999 ) ) ;
#30042 = EDGE_LOOP ( 'NONE', ( #54996, #60951, #30051 ) ) ;
#30044 = CARTESIAN_POINT ( 'NONE',  ( -2.499999999999996447, -2.833333333333333481, 4.330127018922195425 ) ) ;
#30043 = DIRECTION ( 'NONE',  ( 0.000000000000000000, 0.000000000000000000, 1.000000000000000000 ) ) ;
#30045 = CARTESIAN_POINT ( 'NONE',  ( 2.730187237215162345E-16, -158.1875000013655779, -4.458734124999999437 ) ) ;
#30046 = ORIENTED_EDGE ( 'NONE', *, *, #38208, .F. ) ;
#30047 = CARTESIAN_POINT ( 'NONE',  ( -6.972266317189433020E-16, -83.24999999999998579, -5.000000000000000000 ) ) ;
#30048 = CARTESIAN_POINT ( 'NONE',  ( -53.33387254593733928, -127.8125000000000142, 5.149110718188519620 ) ) ;
#30049 = CARTESIAN_POINT ( 'NONE',  ( 2.071067811865264563, -152.8125000000000000, -5.000000000000211386 ) ) ;
#30050 = CARTESIAN_POINT ( 'NONE',  ( -4.458734124999998549, -44.47916666530106511, 2.574251347313722516 ) ) ;
#30051 = ORIENTED_EDGE ( 'NONE', *, *, #44444, .F. ) ;
#30052 = CARTESIAN_POINT ( 'NONE',  ( 2.499999999999998668, 9.791666669397850242, -4.330127018922193649 ) ) ;
#30053 = CARTESIAN_POINT ( 'NONE',  ( 9.457646018065525792E-16, 15.93750000136559564, 5.148502694627439702 ) ) ;
#30054 =( BOUNDED_CURVE ( )  B_SPLINE_CURVE ( 2, ( #54990, #10594, #11237, #11556, #36010, #55641, #16067, #30861, #5460 ),
 .UNSPECIFIED., .F., .F. ) 
 B_SPLINE_CURVE_WITH_KNOTS ( ( 3, 2, 2, 2, 3 ),
 ( 0.9767857142857142572, 0.9773809523809523503, 0.9785714285714285365, 0.9797619047619047228, 0.9803571428571428159 ),
 .UNSPECIFIED. ) 
 CURVE ( )  GEOMETRIC_REPRESENTATION_ITEM ( )  RATIONAL_B_SPLINE_CURVE ( ( 0.9330127018922194093, 0.9330127018922194093, 1.000000000000000000, 0.8660254037844387076, 1.000000000000000000, 0.8660254037844387076, 1.000000000000000000, 0.9330127018922194093, 0.9330127018922194093 ) ) 
 REPRESENTATION_ITEM ( '' )  );
#30055 = CARTESIAN_POINT ( 'NONE',  ( 4.458734125000001214, -89.14583333196775072, 2.574251347313718519 ) ) ;
#30056 = CARTESIAN_POINT ( 'NONE',  ( -51.60603307380591787, -151.9375000013656063, -2.891590998281053704 ) ) ;
#30057 = CARTESIAN_POINT ( 'NONE',  ( 75.00000000000002842, 0.000000000000000000, -5.000000000000000000 ) ) ;
#30058 = CARTESIAN_POINT ( 'NONE',  ( 1.975475456537005874E-15, -35.62499999726880162, 5.000000000000000000 ) ) ;
#30059 =( BOUNDED_CURVE ( )  B_SPLINE_CURVE ( 2, ( #794, #55772, #35837, #20401, #50623, #44831, #45155, #30684, #31308 ),
 .UNSPECIFIED., .F., .F. ) 
 B_SPLINE_CURVE_WITH_KNOTS ( ( 3, 2, 2, 2, 3 ),
 ( 0.9416666666666665408, 0.9458333333333331927, 0.9499999999999997335, 0.9541666666666664964, 0.9583333333333331483 ),
 .UNSPECIFIED. ) 
 CURVE ( )  GEOMETRIC_REPRESENTATION_ITEM ( )  RATIONAL_B_SPLINE_CURVE ( ( 1.000000000000001998, 0.9238795325112847401, 1.000000000000000000, 0.9238795325112867385, 1.000000000000000000, 0.9238795325112867385, 1.000000000000000000, 0.9238795325112908463, 0.9999999999999958922 ) ) 
 REPRESENTATION_ITEM ( '' )  );
#30060 = CARTESIAN_POINT ( 'NONE',  ( -1.339745962155608039, 23.79465819873852084, -5.000000000000004441 ) ) ;
#30061 = CARTESIAN_POINT ( 'NONE',  ( -4.458734124999997661, -64.22916666530106511, 2.574251347313722516 ) ) ;
#30062 = CARTESIAN_POINT ( 'NONE',  ( 2.229367062500001939, 20.02083333469892779, 3.861377020970579999 ) ) ;
#30063 = CYLINDRICAL_SURFACE ( 'NONE', #24684, 5.000000000000000000 ) ;
#30064 = CARTESIAN_POINT ( 'NONE',  ( 2.229367062500001939, -47.22916666530106511, 3.861377020970579999 ) ) ;
#30065 = CARTESIAN_POINT ( 'NONE',  ( 5.000000000000000000, -10.37499999726881583, -6.123233995736766282E-16 ) ) ;
#30066 = CYLINDRICAL_SURFACE ( 'NONE', #59187, 5.000000000000000000 ) ;
#30067 = CARTESIAN_POINT ( 'NONE',  ( -2.500000000000000444, -66.04166666393547303, -4.330127018922193649 ) ) ;
#30068 = CARTESIAN_POINT ( 'NONE',  ( -1.339745962155613812, -74.20534180126145429, -5.000000000000000000 ) ) ;
#30069 = CARTESIAN_POINT ( 'NONE',  ( -1.339745962155589165, 10.91965820146970323, -5.000000000000014211 ) ) ;
#30070 = CARTESIAN_POINT ( 'NONE',  ( 4.458734125000000326, -18.14583333196773651, 2.574251347313718519 ) ) ;
#30071 = ORIENTED_EDGE ( 'NONE', *, *, #16667, .F. ) ;
#30072 = CARTESIAN_POINT ( 'NONE',  ( -4.458734124999999437, -106.3124999986343937, 0.000000000000000000 ) ) ;
#30073 = CARTESIAN_POINT ( 'NONE',  ( 3.061616997868383141E-16, -159.8750000027311842, -5.000000000000000000 ) ) ;
#30074 = ORIENTED_EDGE ( 'NONE', *, *, #62117, .T. ) ;
#30075 = CARTESIAN_POINT ( 'NONE',  ( 4.458734125000001214, -96.14583333196772230, 2.574251347313718519 ) ) ;
#30076 = CARTESIAN_POINT ( 'NONE',  ( 1.060575238724906964E-15, -58.62499999726880873, 5.773502691896257311 ) ) ;
#30077 = FACE_OUTER_BOUND ( 'NONE', #3721, .T. ) ;
#30078 = CARTESIAN_POINT ( 'NONE',  ( -51.60603307380591787, -125.9375000013656063, -2.891590998281053704 ) ) ;
#30079 = CARTESIAN_POINT ( 'NONE',  ( -54.64476657466781973, -143.8125000013656063, -4.444560631937228834 ) ) ;
#30080 = CARTESIAN_POINT ( 'NONE',  ( 2.229367062499998831, -18.64583333196774007, -3.861377020970580887 ) ) ;
#30081 = CARTESIAN_POINT ( 'NONE',  ( -2.229367062499996610, 7.604166668032260823, 3.861377020970582219 ) ) ;
#30082 =( BOUNDED_CURVE ( )  B_SPLINE_CURVE ( 2, ( #1497, #60985, #6949, #36211, #44903, #50043, #45219, #51334, #1185 ),
 .UNSPECIFIED., .F., .F. ) 
 B_SPLINE_CURVE_WITH_KNOTS ( ( 3, 2, 2, 2, 3 ),
 ( 0.8732142857142857206, 0.8738095238095238138, 0.8750000000000000000, 0.8761904761904761862, 0.8767857142857142794 ),
 .UNSPECIFIED. ) 
 CURVE ( )  GEOMETRIC_REPRESENTATION_ITEM ( )  RATIONAL_B_SPLINE_CURVE ( ( 0.9330127018922194093, 0.9330127018922194093, 1.000000000000000000, 0.8660254037844387076, 1.000000000000000000, 0.8660254037844387076, 1.000000000000000000, 0.9330127018922194093, 0.9330127018922194093 ) ) 
 REPRESENTATION_ITEM ( '' )  );
#30083 = CARTESIAN_POINT ( 'NONE',  ( 9.457646018065525792E-16, -63.31249999863440792, 5.148502694627439702 ) ) ;
#30084 = CARTESIAN_POINT ( 'NONE',  ( -5.000000000000000888, -141.5625000027312126, 2.071067811865474617 ) ) ;
#30085 = CARTESIAN_POINT ( 'NONE',  ( 2.229367062499998831, -21.64583333196774007, -3.861377020970580887 ) ) ;
#30086 = DIRECTION ( 'NONE',  ( -7.709882115452477180E-16, 0.000000000000000000, 1.000000000000000000 ) ) ;
#30087 = CARTESIAN_POINT ( 'NONE',  ( 2.071067811865476394, -154.1874999999999716, 5.000000000000000000 ) ) ;
#30088 = CARTESIAN_POINT ( 'NONE',  ( -5.000000000000000000, -11.08333333333333393, -2.886751345948128211 ) ) ;
#30089 = CARTESIAN_POINT ( 'NONE',  ( 3.152801135295367541, -156.3125000013656063, -3.152801135295367541 ) ) ;
#30090 = ORIENTED_EDGE ( 'NONE', *, *, #17029, .T. ) ;
#30091 = CARTESIAN_POINT ( 'NONE',  ( 4.458734125000000326, -46.14583333196773651, 2.574251347313718519 ) ) ;
#30092 = CARTESIAN_POINT ( 'NONE',  ( 2.500000000000002220, -44.54166666393547303, 4.330127018922192761 ) ) ;
#30093 = FACE_OUTER_BOUND ( 'NONE', #30103, .T. ) ;
#30094 = CARTESIAN_POINT ( 'NONE',  ( 4.458734124999998549, -88.72916666530106511, -2.574251347313721627 ) ) ;
#30095 = CARTESIAN_POINT ( 'NONE',  ( -4.458734124999998549, -92.22916666530106511, 2.574251347313722516 ) ) ;
#30096 = CARTESIAN_POINT ( 'NONE',  ( 2.229367062499998831, 10.35416666803225993, -3.861377020970580887 ) ) ;
#30097 = CARTESIAN_POINT ( 'NONE',  ( 1.339745962155612702, -93.29465819873853150, -5.000000000000000000 ) ) ;
#30098 = DIRECTION ( 'NONE',  ( 0.000000000000000000, 0.000000000000000000, 1.000000000000000000 ) ) ;
#30099 = CARTESIAN_POINT ( 'NONE',  ( -2.499999999999996447, 26.16666666666666430, 4.330127018922195425 ) ) ;
#30100 = CARTESIAN_POINT ( 'NONE',  ( -4.458734124999999437, 21.35416666803225993, -2.574251347313719407 ) ) ;
#30101 = CARTESIAN_POINT ( 'NONE',  ( 5.000000000000000000, -76.41666666666665719, -2.886751345948129988 ) ) ;
#30102 = CARTESIAN_POINT ( 'NONE',  ( 1.060575238724906964E-15, 6.375000002731185056, 5.773502691896257311 ) ) ;
#30103 = EDGE_LOOP ( 'NONE', ( #18894, #48249, #39525, #31657 ) ) ;
#30104 = CARTESIAN_POINT ( 'NONE',  ( 1.975475456537005874E-15, -33.75000000000000000, 5.000000000000000000 ) ) ;
#30105 = ORIENTED_EDGE ( 'NONE', *, *, #36244, .F. ) ;
#30106 =( BOUNDED_CURVE ( )  B_SPLINE_CURVE ( 2, ( #16251, #3601, #23208, #18384, #38003, #57636, #35871, #13564, #1473 ),
 .UNSPECIFIED., .F., .F. ) 
 B_SPLINE_CURVE_WITH_KNOTS ( ( 3, 2, 2, 2, 3 ),
 ( 0.9770833333333333037, 0.9777777777777777457, 0.9791666666666666297, 0.9805555555555555136, 0.9812499999999999556 ),
 .UNSPECIFIED. ) 
 CURVE ( )  GEOMETRIC_REPRESENTATION_ITEM ( )  RATIONAL_B_SPLINE_CURVE ( ( 0.9330127018922194093, 0.9330127018922194093, 1.000000000000000000, 0.8660254037844387076, 1.000000000000000000, 0.8660254037844387076, 1.000000000000000000, 0.9330127018922194093, 0.9330127018922194093 ) ) 
 REPRESENTATION_ITEM ( '' )  );
#30107 = CARTESIAN_POINT ( 'NONE',  ( -5.000000000000000000, -51.00000000000000711, 0.000000000000000000 ) ) ;
#30108 = CARTESIAN_POINT ( 'NONE',  ( 9.457646018065525792E-16, -39.06249999863440081, 5.148502694627439702 ) ) ;
#30109 = EDGE_CURVE ( 'NONE', #53004, #35151, #26263, .T. ) ;
#30110 = CARTESIAN_POINT ( 'NONE',  ( -4.999999999999999112, -38.79166666393548013, 2.886751345948131764 ) ) ;
#30111 = ORIENTED_EDGE ( 'NONE', *, *, #31183, .F. ) ;
#30112 = CARTESIAN_POINT ( 'NONE',  ( -4.458734124999999437, -10.39583333196773829, -2.574251347313719407 ) ) ;
#30114 = ORIENTED_EDGE ( 'NONE', *, *, #63423, .F. ) ;
#30113 = CARTESIAN_POINT ( 'NONE',  ( 2.229367062500001939, -18.22916666530106866, 3.861377020970579999 ) ) ;
#30115 = CARTESIAN_POINT ( 'NONE',  ( 2.500000000000002220, -84.66666666666667140, 4.330127018922192761 ) ) ;
#30116 = CARTESIAN_POINT ( 'NONE',  ( -8.190561711645485556E-16, -168.6875000013656063, 4.458734124999999437 ) ) ;
#30117 = CARTESIAN_POINT ( 'NONE',  ( 4.458734124999999437, -61.06249999863440081, -5.460374474430324690E-16 ) ) ;
#30118 = CARTESIAN_POINT ( 'NONE',  ( 5.000000000000000888, -88.45833333060214443, 2.886751345948126879 ) ) ;
#30120 = ORIENTED_EDGE ( 'NONE', *, *, #33369, .F. ) ;
#30119 = CARTESIAN_POINT ( 'NONE',  ( -4.999999999999998224, -48.79166666393547303, 2.886751345948131764 ) ) ;
#30121 = CARTESIAN_POINT ( 'NONE',  ( -49.85088928181150436, -140.5625000000000284, -1.666127454062680702 ) ) ;
#30122 = CARTESIAN_POINT ( 'NONE',  ( -4.458734124999999437, -27.56249999863440081, 0.000000000000000000 ) ) ;
#30123 = CARTESIAN_POINT ( 'NONE',  ( 1.339745962155565406, -5.580341798530294106, 5.000000000000028422 ) ) ;
#30124 = ORIENTED_EDGE ( 'NONE', *, *, #13315, .T. ) ;
#30125 = APPLICATION_PROTOCOL_DEFINITION ( 'draft international standard', 'automotive_design', 1998, #44181 ) ;
#30126 = CARTESIAN_POINT ( 'NONE',  ( -4.458734125000000326, -164.2500000013656063, -1.846868145590735644 ) ) ;
#30127 = CARTESIAN_POINT ( 'NONE',  ( -2.229367062500000163, 29.52083333469892779, -3.861377020970580443 ) ) ;
#30128 = CARTESIAN_POINT ( 'NONE',  ( -9.184850993605147944E-16, -156.2500000000000000, 5.000000000000000000 ) ) ;
#30129 = VERTEX_POINT ( 'NONE', #44811 ) ;
#30130 = CARTESIAN_POINT ( 'NONE',  ( -58.39396692619412477, -145.6875000013656063, 2.891590998281057701 ) ) ;
#30131 = CARTESIAN_POINT ( 'NONE',  ( 4.458734125000001214, -75.14583333196775072, 2.574251347313718519 ) ) ;
#30132 = CARTESIAN_POINT ( 'NONE',  ( -50.18089887299979068, -135.8125000027312126, 2.462841084822635640 ) ) ;
#30133 = CARTESIAN_POINT ( 'NONE',  ( -4.458734124999997661, -46.22916666530106511, 2.574251347313722516 ) ) ;
#30134 = CARTESIAN_POINT ( 'NONE',  ( -3.152801135295367096, -146.3125000013655779, -3.152801135295367541 ) ) ;
#30135 = FACE_OUTER_BOUND ( 'NONE', #41057, .T. ) ;
#30136 = CARTESIAN_POINT ( 'NONE',  ( 9.457646018065525792E-16, -47.06249999863440792, 5.148502694627439702 ) ) ;
#30137 = CARTESIAN_POINT ( 'NONE',  ( 0.000000000000000000, -120.0000000000000000, 0.000000000000000000 ) ) ;
#30138 = CARTESIAN_POINT ( 'NONE',  ( -2.229367062500000163, -14.47916666530107221, -3.861377020970580443 ) ) ;
#30139 = CARTESIAN_POINT ( 'NONE',  ( 2.500000000000002220, -101.6666666666666572, 4.330127018922192761 ) ) ;
#30140 = CARTESIAN_POINT ( 'NONE',  ( -4.458734125000000326, -142.2500000013656063, -1.846868145590735644 ) ) ;
#30141 = CARTESIAN_POINT ( 'NONE',  ( 4.458734125000001214, -35.14583333196772941, 2.574251347313718519 ) ) ;
#30142 = CARTESIAN_POINT ( 'NONE',  ( -2.500000000000000444, 8.958333336064518093, -4.330127018922193649 ) ) ;
#30143 = DIRECTION ( 'NONE',  ( 0.000000000000000000, 0.000000000000000000, 1.000000000000000000 ) ) ;
#30144 = CARTESIAN_POINT ( 'NONE',  ( -51.60603307380591787, -127.9375000013656063, -2.891590998281053704 ) ) ;
#30145 = CARTESIAN_POINT ( 'NONE',  ( -2.229367062499996610, -73.39583333196773651, 3.861377020970582219 ) ) ;
#30146 = CARTESIAN_POINT ( 'NONE',  ( -5.000000000000000888, -144.6875000027312126, -2.071067811865475949 ) ) ;
#30147 = CARTESIAN_POINT ( 'NONE',  ( -6.972266317189433020E-16, 20.87500000273118062, -5.000000000000000000 ) ) ;
#30148 = CARTESIAN_POINT ( 'NONE',  ( -51.75738570946856498, -136.7500000000000284, 3.805975901505576964 ) ) ;
#30149 = CARTESIAN_POINT ( 'NONE',  ( 4.458734124999999437, -2.062499998634406584, -5.460374474430324690E-16 ) ) ;
#30150 = ORIENTED_EDGE ( 'NONE', *, *, #39788, .F. ) ;
#30151 = LINE ( 'NONE', #49780, #28464 ) ;
#30152 = CARTESIAN_POINT ( 'NONE',  ( 1.975475456537005874E-15, -34.75000000000000000, 5.000000000000000000 ) ) ;
#30154 = CARTESIAN_POINT ( 'NONE',  ( 4.458734125000001214, -37.89583333196772941, 2.574251347313718519 ) ) ;
#30153 = CARTESIAN_POINT ( 'NONE',  ( -4.458734124999998549, -89.22916666530106511, 2.574251347313722516 ) ) ;
#30155 = CARTESIAN_POINT ( 'NONE',  ( 1.975475456537005874E-15, -35.75000000000000711, 5.000000000000000000 ) ) ;
#30156 = CARTESIAN_POINT ( 'NONE',  ( 4.458734125000001214, -81.14583333196773651, 2.574251347313718519 ) ) ;
#30157 = CARTESIAN_POINT ( 'NONE',  ( -4.458734124999999437, 20.35416666803225993, -2.574251347313719407 ) ) ;
#30158 = DIRECTION ( 'NONE',  ( -0.000000000000000000, 1.000000000000000000, -0.000000000000000000 ) ) ;
#30159 = CARTESIAN_POINT ( 'NONE',  ( -54.64476657466781973, -135.8125000013656063, -4.444560631937228834 ) ) ;
#30160 = CARTESIAN_POINT ( 'NONE',  ( -2.229367062499996610, -2.145833331967737845, 3.861377020970582219 ) ) ;
#30161 = CARTESIAN_POINT ( 'NONE',  ( -3.152548672688508926E-16, 20.18750000136559208, -5.148502694627439702 ) ) ;
#30162 = CARTESIAN_POINT ( 'NONE',  ( 4.458734124999999437, -46.06249999863440081, -5.460374474430324690E-16 ) ) ;
#30163 = CARTESIAN_POINT ( 'NONE',  ( 2.499999999999998668, -15.33333333333333037, -4.330127018922193649 ) ) ;
#30164 = CARTESIAN_POINT ( 'NONE',  ( -2.229367062499996610, -6.145833331967740953, 3.861377020970582219 ) ) ;
#30165 = ORIENTED_EDGE ( 'NONE', *, *, #61394, .T. ) ;
#30166 = CARTESIAN_POINT ( 'NONE',  ( 2.229367062499998831, -29.89583333196773296, -3.861377020970580887 ) ) ;
#30167 = CARTESIAN_POINT ( 'NONE',  ( -50.70258187064364108, -130.3750000013656631, 2.196230717870141014 ) ) ;
#30168 = CARTESIAN_POINT ( 'NONE',  ( -2.229367062500000163, -75.47916666530106511, -3.861377020970580443 ) ) ;
#30169 = CARTESIAN_POINT ( 'NONE',  ( 2.499999999999998668, -105.2083333306021444, -4.330127018922193649 ) ) ;
#30170 = CARTESIAN_POINT ( 'NONE',  ( -2.229367062500000163, 23.52083333469892779, -3.861377020970580443 ) ) ;
#30171 = CARTESIAN_POINT ( 'NONE',  ( 5.000000000000000888, 26.54166666939784847, 2.886751345948126879 ) ) ;
#30172 = DIRECTION ( 'NONE',  ( -0.000000000000000000, 1.000000000000000000, -0.000000000000000000 ) ) ;
#30173 = CARTESIAN_POINT ( 'NONE',  ( -4.458734124999999437, -80.56249999863440792, 0.000000000000000000 ) ) ;
#30174 = CARTESIAN_POINT ( 'NONE',  ( -2.500000000000000444, -59.16666666666665719, -4.330127018922193649 ) ) ;
#30175 = CARTESIAN_POINT ( 'NONE',  ( -6.972266317189433020E-16, -35.25000000000000000, -5.000000000000000000 ) ) ;
#30176 = CARTESIAN_POINT ( 'NONE',  ( -5.000000000000000000, 22.04166666939785202, -2.886751345948128211 ) ) ;
#30177 = ORIENTED_EDGE ( 'NONE', *, *, #19513, .T. ) ;
#30178 = CARTESIAN_POINT ( 'NONE',  ( -5.000000000000000000, -72.87499999726880162, 0.000000000000000000 ) ) ;
#30179 = CARTESIAN_POINT ( 'NONE',  ( 5.000000000000000000, -67.50000000000000000, -6.123233995736766282E-16 ) ) ;
#30180 = CARTESIAN_POINT ( 'NONE',  ( -2.499999999999996447, -15.83333333333333037, 4.330127018922195425 ) ) ;
#30181 = CARTESIAN_POINT ( 'NONE',  ( 2.229367062500001939, -23.97916666530107577, 3.861377020970579999 ) ) ;
#30182 = EDGE_CURVE ( 'NONE', #21511, #18022, #773, .T. ) ;
#30183 = CARTESIAN_POINT ( 'NONE',  ( 9.457646018065525792E-16, -83.06249999863439371, 5.148502694627439702 ) ) ;
#30184 =( BOUNDED_CURVE ( )  B_SPLINE_CURVE ( 2, ( #57370, #8781, #47698, #52847, #37738, #47391, #62822, #28392, #13291 ),
 .UNSPECIFIED., .F., .F. ) 
 B_SPLINE_CURVE_WITH_KNOTS ( ( 3, 2, 2, 2, 3 ),
 ( 0.2604166666666666852, 0.2611111111111111271, 0.2625000000000000111, 0.2638888888888888951, 0.2645833333333333370 ),
 .UNSPECIFIED. ) 
 CURVE ( )  GEOMETRIC_REPRESENTATION_ITEM ( )  RATIONAL_B_SPLINE_CURVE ( ( 0.9330127018922194093, 0.9330127018922194093, 1.000000000000000000, 0.8660254037844387076, 1.000000000000000000, 0.8660254037844387076, 1.000000000000000000, 0.9330127018922194093, 0.9330127018922194093 ) ) 
 REPRESENTATION_ITEM ( '' )  );
#30185 = CARTESIAN_POINT ( 'NONE',  ( -4.999999999999999112, -23.79166666393548013, 2.886751345948131764 ) ) ;
#30187 = ORIENTED_EDGE ( 'NONE', *, *, #11365, .F. ) ;
#30186 = CARTESIAN_POINT ( 'NONE',  ( 4.458734124999998549, -49.72916666530106511, -2.574251347313721627 ) ) ;
#30188 = CARTESIAN_POINT ( 'NONE',  ( -2.500000000000000444, -76.04166666393547303, -4.330127018922193649 ) ) ;
#30189 = CYLINDRICAL_SURFACE ( 'NONE', #35409, 5.000000000000000000 ) ;
#30191 = ORIENTED_EDGE ( 'NONE', *, *, #43018, .T. ) ;
#30190 = CARTESIAN_POINT ( 'NONE',  ( 4.458734125000001214, 2.854166668032259491, 2.574251347313718519 ) ) ;
#30192 = CARTESIAN_POINT ( 'NONE',  ( -58.39396692619412477, -150.4375000013656063, 2.891590998281057701 ) ) ;
#30193 = CARTESIAN_POINT ( 'NONE',  ( -3.535250795749689387E-16, -64.25000000000000000, -5.773502691896257311 ) ) ;
#30194 = CARTESIAN_POINT ( 'NONE',  ( -4.458734125000001214, -153.1250000013656063, 1.846868145590734089 ) ) ;
#30195 = CARTESIAN_POINT ( 'NONE',  ( -4.458734124999999437, -48.64583333196773651, -2.574251347313719407 ) ) ;
#30196 = CARTESIAN_POINT ( 'NONE',  ( -1.339745962155610925, -80.66965819600734733, 5.000000000000000000 ) ) ;
#30197 = CARTESIAN_POINT ( 'NONE',  ( 5.000000000000000888, -157.9375000000000000, -2.071067811865475505 ) ) ;
#30198 = DIRECTION ( 'NONE',  ( -0.000000000000000000, -1.000000000000000000, 0.000000000000000000 ) ) ;
#30199 = CARTESIAN_POINT ( 'NONE',  ( -58.80597590150559739, -155.0000000000000284, 3.242614290531460330 ) ) ;
#30200 = CARTESIAN_POINT ( 'NONE',  ( -2.229367062499996610, -11.39583333196773829, 3.861377020970582219 ) ) ;
#30201 = CARTESIAN_POINT ( 'NONE',  ( -4.458734124999998549, -47.47916666530106511, 2.574251347313722516 ) ) ;
#30202 = VECTOR ( 'NONE', #26274, 1000.000000000000000 ) ;
#30203 =( BOUNDED_CURVE ( )  B_SPLINE_CURVE ( 2, ( #3636, #42541, #2378, #3014, #56725, #41906, #12645, #18100, #27431 ),
 .UNSPECIFIED., .F., .F. ) 
 B_SPLINE_CURVE_WITH_KNOTS ( ( 3, 2, 2, 2, 3 ),
 ( 0.9946428571428571619, 0.9952380952380952550, 0.9964285714285714413, 0.9976190476190476275, 0.9982142857142857206 ),
 .UNSPECIFIED. ) 
 CURVE ( )  GEOMETRIC_REPRESENTATION_ITEM ( )  RATIONAL_B_SPLINE_CURVE ( ( 0.9330127018922194093, 0.9330127018922194093, 1.000000000000000000, 0.8660254037844387076, 1.000000000000000000, 0.8660254037844387076, 1.000000000000000000, 0.9330127018922194093, 0.9330127018922194093 ) ) 
 REPRESENTATION_ITEM ( '' )  );
#30204 = EDGE_CURVE ( 'NONE', #1698, #2721, #18428, .T. ) ;
#30205 = CARTESIAN_POINT ( 'NONE',  ( -4.999999999999998224, -7.791666663935482795, 2.886751345948131764 ) ) ;
#30206 = CARTESIAN_POINT ( 'NONE',  ( 3.152801135295367541, -143.3125000013655779, -3.152801135295367541 ) ) ;
#30207 = EDGE_CURVE ( 'NONE', #54038, #23647, #17253, .T. ) ;
#30208 = CARTESIAN_POINT ( 'NONE',  ( 2.229367062499998831, -91.89583333196773651, -3.861377020970580887 ) ) ;
#30209 = CARTESIAN_POINT ( 'NONE',  ( -1.994931997373328159E-14, -8.660254037844390851, -1.000000000000000888 ) ) ;
#30210 = EDGE_LOOP ( 'NONE', ( #60768, #39004, #13843, #38492 ) ) ;
#30211 = CARTESIAN_POINT ( 'NONE',  ( -6.972266317189433020E-16, -98.12499999726880162, -5.000000000000000000 ) ) ;
#30212 = CARTESIAN_POINT ( 'NONE',  ( -1.339745962155613812, -6.080341798530292330, -5.000000000000000000 ) ) ;
#30213 = CARTESIAN_POINT ( 'NONE',  ( -52.53715891517739323, -146.5625000027311842, -4.819101127000233298 ) ) ;
#30214 = CARTESIAN_POINT ( 'NONE',  ( 1.339745962155615144, -38.70534180126146850, 4.999999999999999112 ) ) ;
#30215 = ORIENTED_EDGE ( 'NONE', *, *, #14895, .T. ) ;
#30216 = EDGE_CURVE ( 'NONE', #18086, #11538, #24138, .T. ) ;
#30217 = CARTESIAN_POINT ( 'NONE',  ( 2.229367062500001939, 2.020833334698927786, 3.861377020970579999 ) ) ;
#30218 = LINE ( 'NONE', #6749, #12369 ) ;
#30219 = CARTESIAN_POINT ( 'NONE',  ( 4.458734124999999437, -15.06249999863440436, -5.460374474430324690E-16 ) ) ;
#30220 = CARTESIAN_POINT ( 'NONE',  ( -2.071067811865644259, -154.8125000027311842, -4.999999999999831246 ) ) ;
#30221 = CARTESIAN_POINT ( 'NONE',  ( -4.458734124999998549, -6.229166665301072214, 2.574251347313722516 ) ) ;
#30222 = DIRECTION ( 'NONE',  ( -0.000000000000000000, 1.000000000000000000, -0.000000000000000000 ) ) ;
#30223 = CARTESIAN_POINT ( 'NONE',  ( -3.152801135295367985, -148.8125000013655779, 3.152801135295367096 ) ) ;
#30224 = CARTESIAN_POINT ( 'NONE',  ( -2.229367062499996610, 14.60416666803226171, 3.861377020970582219 ) ) ;
#30225 = ORIENTED_EDGE ( 'NONE', *, *, #63327, .T. ) ;
#30226 = CARTESIAN_POINT ( 'NONE',  ( -1.339745962155613812, -63.08034179853028434, -5.000000000000000000 ) ) ;
#30227 = CARTESIAN_POINT ( 'NONE',  ( -2.500000000000000444, -21.16666666666666785, -4.330127018922193649 ) ) ;
#30228 = CARTESIAN_POINT ( 'NONE',  ( -4.458734124999999437, -17.39583333196773651, -2.574251347313719407 ) ) ;
#30229 = CYLINDRICAL_SURFACE ( 'NONE', #29313, 5.000000000000000000 ) ;
#30230 = CARTESIAN_POINT ( 'NONE',  ( -55.39835681537999790, -137.8750000000000284, 4.984105922594378235 ) ) ;
#30231 = CARTESIAN_POINT ( 'NONE',  ( -52.10840900171896806, -148.1875000013656063, 3.393966926194110556 ) ) ;
#30232 = ADVANCED_FACE ( 'NONE', ( #58231 ), #34093, .T. ) ;
#30233 = CARTESIAN_POINT ( 'NONE',  ( 5.000000000000000888, -43.45833333060214443, 2.886751345948126879 ) ) ;
#30234 = CARTESIAN_POINT ( 'NONE',  ( -7.500000000000000000, 4.330127018922191873, -7.422398894150032511 ) ) ;
#30235 = CARTESIAN_POINT ( 'NONE',  ( 4.458734124999998549, 15.27083333469893134, -2.574251347313721627 ) ) ;
#30236 = DIRECTION ( 'NONE',  ( -0.000000000000000000, 1.000000000000000000, -0.000000000000000000 ) ) ;
#30237 = DIRECTION ( 'NONE',  ( -0.4999999999999998335, 0.000000000000000000, 0.8660254037844388186 ) ) ;
#30238 = CARTESIAN_POINT ( 'NONE',  ( -3.152548672688508926E-16, 11.43750000136559564, -5.148502694627439702 ) ) ;
#30239 = CARTESIAN_POINT ( 'NONE',  ( -4.458734124999998549, -63.22916666530106511, 2.574251347313722516 ) ) ;
#30240 = VERTEX_POINT ( 'NONE', #38303 ) ;
#30241 = CARTESIAN_POINT ( 'NONE',  ( 4.458734124999998549, -12.97916666530107399, -2.574251347313721627 ) ) ;
#30242 = CARTESIAN_POINT ( 'NONE',  ( 5.000000000000000000, 5.583333333333332149, -2.886751345948129988 ) ) ;
#30243 = CARTESIAN_POINT ( 'NONE',  ( 3.152801135295367541, -164.3125000013656063, -3.152801135295367541 ) ) ;
#30244 = CARTESIAN_POINT ( 'NONE',  ( 5.000000000000000000, -88.41666666666665719, -2.886751345948130876 ) ) ;
#30245 = CARTESIAN_POINT ( 'NONE',  ( -2.229367062500000163, -57.47916666530107932, -3.861377020970580443 ) ) ;
#30246 = CARTESIAN_POINT ( 'NONE',  ( -4.999999999999999112, -86.79166666393548724, 2.886751345948131764 ) ) ;
#30247 = CARTESIAN_POINT ( 'NONE',  ( 4.458734125000000326, -32.89583333196774362, 2.574251347313718519 ) ) ;
#30248 = AXIS2_PLACEMENT_3D ( 'NONE', #23585, #62195, #63451 ) ;
#30249 = DIRECTION ( 'NONE',  ( 0.000000000000000000, 0.000000000000000000, 1.000000000000000000 ) ) ;
#30250 = DIRECTION ( 'NONE',  ( -0.6485228581062915110, 0.000000000000000000, -0.7611951803011149931 ) ) ;
#30251 = CARTESIAN_POINT ( 'NONE',  ( 1.975475456537005874E-15, -16.62499999726881583, 5.000000000000000000 ) ) ;
#30252 = CARTESIAN_POINT ( 'NONE',  ( 1.975475456537005874E-15, -16.62499999726881583, 5.000000000000000000 ) ) ;
#30253 = CARTESIAN_POINT ( 'NONE',  ( 1.846868145590736310, -154.8750000013655779, 4.458734124999997661 ) ) ;
#30254 = CARTESIAN_POINT ( 'NONE',  ( -3.535250795749689387E-16, -44.25000000000000000, -5.773502691896257311 ) ) ;
#30255 = CARTESIAN_POINT ( 'NONE',  ( 0.000000000000000000, 15.00000000000000000, 0.000000000000000000 ) ) ;
#30256 = CARTESIAN_POINT ( 'NONE',  ( -1.339745962155613812, -108.2053418012614543, -5.000000000000000000 ) ) ;
#30257 = ORIENTED_EDGE ( 'NONE', *, *, #46409, .T. ) ;
#30258 = CARTESIAN_POINT ( 'NONE',  ( 4.458734124999999437, -103.8124999986344079, -5.460374474430324690E-16 ) ) ;
#30259 = CARTESIAN_POINT ( 'NONE',  ( 4.458734124999999437, 4.937500001365595637, -5.460374474430324690E-16 ) ) ;
#30260 =( BOUNDED_SURFACE ( )  B_SPLINE_SURFACE ( 1, 2, ( 
 ( #23776, #9912, #4159, #24088, #43683, #58176, #8975, #63329, #28271, #24399, #44000, #37936, #43378, #62390, #19246, #47578, #33731, #3530, #47886, #19567, #38862, #3844, #14422, #23464, #28585, #53349, #39179, #9599, #48206, #63023, #13798, #18311, #43067, #57569, #52726, #13494, #38253, #18930, #62705, #23139, #33110, #18631, #57874, #29207, #9284, #38546, #33418, #28900, #53037, #48520, #4461, #58498, #34044, #53666, #48832, #4772, #63648, #58804, #25990, #1564, #16344, #45609, #55592, #30488, #49478, #5098, #40773, #29845, #21166, #50110, #35966, #29520, #20540, #6065, #39497, #39815, #59456, #25033, #60419, #40137, #25679, #603, #45287, #49154, #10871, #5416, #59781, #44643, #34681, #15705, #24717, #1253, #15388, #285, #35323, #30813, #20856, #35013, #10551, #44321, #60098, #19884, #59133, #15069, #20213, #54300, #55272, #11191, #16019, #54626, #25354, #30161, #54944, #50445, #40458, #10242, #49790, #35646, #5736, #44972, #6385, #937, #21809, #22444, #50750, #1887, #7016, #56543, #46881, #32073, #41716, #17614, #21490, #2825, #12143, #61367, #42041, #26300, #52022, #17288, #51077, #2506, #31435, #3141, #26624, #37230, #36912, #41088, #45924, #60735, #46244, #27564, #31763, #61682, #11511, #31127, #56856, #12774, #56223, #11816, #2205, #6695, #12462, #41404, #51710, #7651, #51396, #7338, #22760, #16656, #32396, #61056, #16976, #7966, #36281, #55905, #36587, #27254, #47197, #42357, #61996, #17916, #26949, #37538, #46566, #22124, #24002, #8276, #33968, #43300, #33032, #48129, #13411, #48748, #52648, #19162, #18850, #23066, #27880, #47501, #8582, #9518, #57797, #48443, #57177, #13095, #38780, #58419, #38175, #57492, #28193, #32714, #38471, #23389, #58097, #14027, #33342, #52958, #4690, #3452, #14346, #42989, #3765, #13718, #42671, #8896, #62310, #37859, #62936, #9209, #28822, #52342, #4080, #18234, #29125, #33656, #53588, #24312, #43919, #63566, #19486, #53274, #47808, #62631, #18553, #28511, #23703, #4383, #43604, #63248, #59369, #5657, #29435, #34586, #54218, #39412, #45207, #15303, #25270, #14978, #44890, #1173, #30081, #19803, #34925, #59050, #5015, #54546, #5988, #49712, #10156, #53899, #10469, #10795, #851, #49395, #5339, #40378, #40053, #60019, #20773, #50031, #29761, #25593, #35245, #54864, #59697, #24957, #520, #44562, #20455, #30407, #15628, #39099, #20130, #58728, #49068, #14654, #34273, #39730, #9824, #24634, #44241, #205, #63460, #57692, #57997, #43500, #4908, #58627, #13924, #33549, #62830, #47706, #33237, #3661, #38063, #62523, #23593, #48334, #52856, #19697, #99, #13619, #39307, #14547, #38674, #34166, #53789, #29019, #18746, #29326, #18442, #33860, #52548, #19378, #8789, #58934, #38993, #24528, #23274, #43190, #32925, #43814, #28402, #48643, #48022, #8480, #9721, #38371, #28089, #63144, #28711, #53480, #48956, #3973, #44131, #9409, #4584, #53168, #42878, #4280, #9103, #24208, #23897, #19056, #58313, #14235, #35451, #40276, #25477, #54105, #49914, #35775, #30296, #15835, #29658, #54757, #10045, #45098, #34473, #59914, #40902, #5868, #14862, #55076, #55397, #49289, #10683, #5227, #1693, #50242, #1063, #20670, #21296, #25805, #6191, #10997, #34816, #45740, #20342, #24847, #16149, #15192, #45417, #44453, #30620, #1384, #20984, #40585, #60229, #413, #35142, #11314, #30939, #50565, #39942, #6508, #59260, #26120, #20015, #39622, #54439, #10367, #29976, #49604, #5545, #25157, #44771, #732, #59589, #15523, #47326, #60546, #51526, #17430, #6827, #7144, #26759, #56032, #52152, #7463, #56673, #31576, #12591, #8095, #41851, #36402, #27071, #11949, #2016, #46688, #56985, #37045, #46376, #31250, #2634, #61811, #61500, #2324, #41530, #3277, #27378, #22888, #27698, #12900, #51210, #16468, #22577, #42174, #47011, #21931, #56359, #61180, #22254, #17737, #32204, #36089, #17103, #51833, #50884, #55717, #7775, #36727, #12279, #2960, #11630, #26433, #31894, #37355, #32524, #46054, #21619, #41213, #60859, #16785, #16208, #60921, #12340, #55771, #25537, #6248, #61237, #41271, #25858, #56088, #50300, #50622, #36150, #17160, #51272, #6561, #26176, #55458, #40328, #45474, #59971, #30683, #55131, #35836, #40961, #1438, #31950, #56416, #21040, #51582, #7205, #31307, #26815, #46436, #21682, #11374, #21992, #11058, #26497, #45154, #12008, #40647, #1120, #31635, #36782, #15892, #30996, #20724, #36461, #60286, #16840, #45795, #35511, #2382, #1755, #21356, #11688, #60609, #46113, #41585, #16526, #50943, #6884, #2075, #33220, #3641, #37415, #3954, #37110, #8464, #27130, #57675, #56729, #13905, #13601, #62811, #41911, #17791, #33533, #18422, #12649, #23252, #32264, #46746, #28382, #61875, #2691, #18104, #3333, #28072, #48001, #51893, #38043, #47689, #42860, #7834, #52838, #22949, #27435, #62504, #22311, #61556, #57360, #8772, #23576, #32907, #37727, #17489, #42545, #43171, #62184, #18729, #47068, #47382, #3018, #13281, #22633, #52530, #7520, #38354, #42232, #57980, #57049, #12960, #32585, #52207, #8155, #27754, #48939, #4887, #59571, #394, #44433, #19676, #9390, #20322, #58608, #4262, #54420, #53460, #19996, #39923, #49273, #44112, #75, #39604, #29308, #15504, #9702, #29638, #5208, #39288, #14528, #24827, #33841, #29958, #58915, #43795, #63128, #63442, #59240, #53148, #14844, #9083, #29000, #25140, #15173, #48625, #34797, #14213, #34148, #34456, #44751, #10349, #53770, #24509, #19359, #23880, #4564, #43483, #58295, #19039, #38971, #54087, #24188, #28693, #48312, #10026, #49583, #5525, #712, #38656, #11615, #59897, #46035, #50548, #15817, #6809, #10661, #25459, #21277, #31235, #55701, #60528, #45723, #30277, #6492, #56017, #26103, #36072, #49897, #11296, #5851, #1675, #54740, #16453, #61165, #40884, #35125, #50867, #11930, #45080, #30921, #1047, #21915, #26418, #1998, #21603, #41512, #41197, #60842, #16768, #55057, #2312, #40569, #20653, #36386, #35432, #31561, #40257, #51194, #7126, #26742, #46358, #10981, #30601, #55380, #50222, #6172, #25789, #60210, #45400, #1367, #20969, #16134, #35756, #27055, #7758, #52458, #3878, #47308, #17088, #61481, #52765, #32829, #17414, #47614, #41836, #42158, #27680, #8694, #42785, #61794, #17721, #46995, #31876, #37029, #51510, #22236, #46673, #27361, #32505, #56655, #23497, #47920, #12572, #43099, #62430, #22873, #18348, #37971, #13207, #2943, #13531, #2618, #18026, #36709, #3567, #32185, #56342, #23174, #28306, #7447, #22557, #12262, #27994, #51816, #8393, #37335, #56968, #57604, #12887, #52137, #3261, #8079, #37648, #42466, #33151, #62107, #57291, #62740, #18662, #44354, #317, #43721, #63054, #38580, #38284, #24433, #28931, #2039, #19602, #38896, #58531, #54343, #13833, #19915, #48554, #9317, #63366, #48236, #19281, #4194, #43409, #4810, #14768, #34386, #57910, #9632, #53069, #15099, #44035, #59167, #34716, #49509, #10275, #25066, #39214, #18965, #33452, #29879, #58211, #5448, #58839, #9009, #28621, #53700, #54014, #23807, #4493, #24121, #14138, #33765, #29240, #9944, #53384, #29560, #14455, #49193, #34077, #48865, #5131, #24749, #39529, #41123, #1603, #54978, #15427, #55311, #45957, #45645, #50145, #25714, #51113, #11545, #7050, #11854, #60771, #20575, #36315, #6730, #26340, #31162, #15740, #40493, #6100, #35683, #1922, #11226, #44676, #30522, #40807, #35048, #55939, #16380, #59818, #10907, #55630, #20246, #54660, #40182, #26030, #36000, #21201, #30850, #50792, #35357, #21527, #10583, #45325, #16696, #59491, #31472, #50480, #1293, #6420, #973, #636, #20890, #39848, #60455, #30195, #49824, #5768, #25386, #45007, #60134, #16055, #61404, #22483, #51746, #17649, #47538, #37264, #52685, #12498, #22798, #17011, #37897, #62031, #41754, #36950, #37573, #2240, #36627, #22160, #8000, #17949, #47236, #56892, #32751, #17328, #3488, #56259, #2544, #57213, #41440, #23102, #12812, #56577, #32433, #46600, #18270, #32110, #52379, #52062, #12184, #61089, #31798, #7688, #42705, #27294, #13132, #26663, #46282, #8317, #27916, #46919, #26981, #2861, #21844, #27603, #42078, #3179, #42391, #61720, #62349, #57526, #51431, #13448, #33072, #7373, #53310, #57836, #9244, #13755, #52991, #14380, #24355, #43955, #28228, #19202, #62667, #24671, #34004, #5053, #44279, #59089, #241, #34630, #9558, #28545, #47844, #19839, #8932, #39453, #29163, #15015, #8620, #63285, #48788, #18587, #18891, #38505, #4118, #3802, #38815, #4730, #43333, #63603, #23424, #53627, #48165, #58457, #23738, #33377, #19523, #43027, #39137, #58133, #38211, #58764, #9865, #14693, #14064, #28858, #62975, #34312, #33689, #48480, #4417, #24042, #43644, #53935, #29475, #49107, #54255, #46125, #12019, #558, #883, #20491, #49747, #46758, #2089, #51284, #25307, #7217, #2703, #36473, #30117, #21693, #5691, #59409, #41283, #51596, #31649, #40090, #24991, #60933, #56428, #56099, #59732, #35276, #61566, #22003, #17500, #22322, #7531, #44928, #41924, #17170, #36796, #41597, #15658, #50954, #54898, #16852, #12350, #26830, #10196, #11699, #46447, #44598, #29796, #2393, #31319, #6895, #61248, #49429, #20166, #26509, #31962, #27143, #5373, #39763, #15341, #34964, #54580, #10502, #12972, #3966, #51906, #13917, #23267, #32595, #28083, #57061, #28705, #52221, #62824, #62518, #3029, #7845, #27447, #8166, #53160, #37740, #28394, #37122, #56741, #18741, #38365, #18116, #37428, #27766, #12662, #18434, #3344, #38055, #57687, #13293, #32918, #48325, #47081, #57991, #22960, #47393, #57372, #22645, #52541, #42245, #17803, #42871, #52849, #8783, #32277, #47700, #61886, #9098, #13613, #33544, #4274, #23892, #43494, #63139, #33231, #42557, #62198, #8475, #48013, #23587, #43182, #3654, #58305, #54098, #39936, #34467, #20008, #33854, #58927, #14227, #29651, #38667, #405, #45092, #10037, #19052, #39616, #59582, #53471, #14855, #9402, #5862, #54432, #49282, #5220, #25469, #29969, #10360, #24840, #38983, #49908, #24522, #29011, #20334, #19371, #49596, #48637, #15184, #44446, #59253, #5538, #34809, #4576, #39299, #25151, #44763, #724, #44123, #15516, #63453, #35136, #54751, #9715, #24201, #29319, #10674, #43807, #30289, #58621, #14540, #34160, #53781, #48950, #4899, #89, #19690, #11624, #36721, #26752, #26115, #1687, #30932, #15828, #1378, #35443, #6185, #30612, #55391, #16462, #20978, #51520, #31887, #45410, #7457, #46369, #6821, #2319, #21924, #60852, #50558, #61174, #50235, #2010, #20663, #51203, #25799, #27065, #7137, #56352, #55069, #11307, #1057, #11943, #40579, #16778, #60222, #40268, #41522, #6502, #59908, #31244, #60540, #21613, #17097, #16144, #31570, #41206, #36395, #35767, #12273, #36081, #45734, #56026, #10991, #21288, #50878, #40894, #46045, #55711, #26427, #13216, #52775, #17730, #23506, #37038, #22570, #13540, #61493, #43109, #32839, #42167, #37659, #2952, #38294, #61803, #8703, #8404, #12583, #17424, #56666, #37347, #62750, #47320, #37982, #46681, #2628, #28318, #47935, #27692, #47004, #56978, #22248, #28003, #12894, #47622, #3578, #22882, #42479, #57922, #32197, #3888, #32515, #52146, #3270, #51826, #62118, #7767, #27371, #52467, #62438, #18356, #41845, #57300, #8088, #18671, #23185, #13841, #33461, #53084, #9020, #18036, #42798, #57613, #33161, #39857, #28939, #646, #49202, #15439, #28630, #19612, #5142, #38589, #38909, #58543, #24130, #20259, #39224, #24761, #63376, #44365, #59500, #9956, #4504, #58848, #43733, #33777, #14778, #25075, #326, #14464, #63063, #34395, #29889, #29571, #34086, #9642, #35057, #59176, #54669, #48247, #44685, #19291, #4203, #54354, #10284, #15110, #53709, #24441, #29250, #54022, #49519, #19925, #23816, #48874, #39538, #18975, #43420, #34726, #4822, #44044, #5459, #58222, #14151, #11, #53395, #9326, #48564, #30208, #60782, #59828, #17023, #16708, #2250, #45016, #20900, #36638, #21538, #40192, #6741, #15750, #49833, #31481, #1304, #5776, #21212, #6428, #11555, #51125, #54989, #41134, #31173, #50805, #35366, #36323, #26040, #10916, #45971, #25398, #982, #60465, #26349, #1936, #36009, #40819, #20585, #45655, #7061, #1612, #55950, #30533, #50489, #50155, #16390, #6109, #55640, #10593, #11865, #25724, #26674, #46293, #45334, #21854, #40503, #61099, #41449, #60144, #16066, #35694, #55321, #11236, #30860, #12509, #23436, #61730, #7383, #57537, #56589, #47548, #43037, #52392, #47246, #3192, #42716, #32442, #18599, #12821, #32762, #8327, #22808, #17659, #27927, #36959, #33081, #42401, #46928, #2555, #2877, #3498, #62677, #62043, #56270, #32120, #28241, #23112, #51756, #62359, #17339, #37275, #17959, #47855, #18282, #56903, #52071, #22492, #26990, #7700, #46609, #61416, #22169, #42088, #8012, #27303, #12194, #31809, #27615, #51444, #37907, #37582, #13462, #52694, #8629, #3812, #41766, #57223, #13143, #53946, #18901, #15026, #29174, #28869, #48176, #48491, #9876, #24999, #4739, #38225, #38516, #10206, #29483, #58143, #5061, #62989, #63293, #48799, #29808, #251, #19211, #38828, #4428, #53002, #14073, #8941, #43345, #4128, #24054, #53635, #33701, #44608, #5383, #53321, #568, #19849, #43966, #39463, #59099, #34321, #43652, #34642, #23751, #39146, #57847, #24681, #9254, #13765, #44289, #49441, #28555, #58465, #33387, #49119, #14389, #54266, #34012, #9567, #24364, #63612, #19532, #58773, #14702, #21131, #60701, #895, #31093, #40736, #60383, #44937, #50714, #35608, #20502, #55558, #59422, #10513, #6349, #16309, #35930, #45570, #30778, #15351, #55234, #41055, #11156, #11472, #34975, #60059, #54591, #50399, #39775, #1527, #46209, #25954, #20177, #6658 ),
 ( #20819, #26265, #30127, #49756, #1849, #21455, #1219, #40100, #6981, #51038, #59744, #26592, #45887, #16621, #36242, #55870, #11782, #50076, #31400, #5702, #25317, #15669, #35288, #54908, #10836, #30451, #6034, #25637, #45253, #40419, #15983, #31732, #61964, #51362, #41369, #23037, #56508, #21777, #12743, #61648, #3109, #42639, #46532, #13060, #22726, #42324, #26915, #32679, #17582, #2473, #37506, #61015, #56185, #51987, #17885, #57145, #27533, #32363, #16941, #37199, #62282, #56825, #52311, #36554, #42008, #12105, #7930, #7303, #47165, #28163, #8246, #2171, #27846, #18203, #22086, #47467, #41685, #52615, #3421, #37824, #57457, #8550, #13378, #32999, #61332, #17256, #36878, #7618, #12430, #32041, #51678, #27223, #46843, #2790, #22409, #13997, #58065, #28791, #49036, #4351, #24282, #43884, #58387, #9179, #63532, #28479, #24603, #38748, #13688, #23356, #4980, #38438, #3735, #14313, #43572, #48719, #44209, #48094, #58697, #4659, #19455, #8864, #14625, #63216, #4049, #39068, #42955, #38141, #33935, #34238, #53867, #9481, #53557, #62598, #19131, #174, #29092, #9794, #18520, #23970, #57766, #29402, #33307, #19774, #10123, #39382, #47778, #59013, #14944, #52927, #34553, #23667, #54185, #43264, #62904, #18818, #33625, #53243, #48407, #59989, #49682, #60630, #35215, #44532, #31016, #30053, #21059, #16549, #25879, #20743, #59666, #40022, #10764, #50644, #49999, #6273, #45495, #40347, #54835, #1459, #10440, #6582, #15912, #20422, #39699, #15597, #40665, #36174, #35532, #29730, #5628, #1779, #60308, #25239, #16237, #54517, #30376, #55160, #21378, #55482, #5950, #25559, #45177, #489, #44854, #20092, #1143, #40986, #5306, #817, #11080, #55795, #49362, #30702, #24924, #11398, #50327, #26197, #45817, #35856, #59339, #15271, #34895, #12675, #31330, #61896, #60945, #18125, #17813, #3352, #46135, #22014, #37752, #22657, #41296, #7856, #42568, #17182, #26519, #12982, #12033, #3038, #62208, #27462, #2716, #41608, #61258, #56438, #32607, #31973, #51915, #47091, #22338, #36808, #42255, #56110, #52233, #41936, #2402, #21704, #12360, #37439, #11712, #61577, #50965, #31659, #47401, #57070, #51295, #8175, #36484, #51609, #17512, #22969, #27777, #7541, #27154, #46770, #2103, #7230, #16866, #37132, #6908, #26845, #46458, #56751, #32289, #25406, #38068, #45024, #20266, #335, #39865, #59512, #54365, #24449, #54677, #23278, #59186, #13305, #44693, #42881, #992, #657, #49842, #28092, #4830, #20595, #5469, #62526, #10292, #18445, #32928, #15447, #48884, #52551, #5148, #54030, #15118, #35065, #57695, #25084, #34736, #29897, #13622, #10601, #9967, #33240, #49527, #8483, #47710, #44374, #30217, #5786, #19935, #24769, #3664, #29579, #57384, #49212, #52860, #8793, #34401, #28404, #39547, #44053, #19, #19621, #39232, #58857, #14788, #61106, #2561, #36017, #30541, #26996, #11872, #55649, #11563, #46615, #51134, #31489, #6748, #60154, #40200, #7389, #36644, #16076, #31819, #2257, #21861, #7069, #11245, #31182, #1620, #50811, #17030, #26358, #59836, #26048, #36331, #50163, #51451, #55959, #26684, #1945, #6439, #15758, #6118, #35701, #21546, #46300, #60789, #45979, #41456, #30868, #56276, #25732, #55328, #12200, #54998, #35375, #41141, #50497, #16714, #45663, #10924, #21222, #45345, #1312, #20908, #40511, #40829, #60473, #16399, #22816, #13471, #22175, #41776, #61737, #57230, #51762, #17964, #17666, #61422, #47556, #52080, #23118, #42722, #62049, #37588, #13773, #36968, #3821, #8017, #32448, #3198, #7706, #42406, #27310, #2885, #27933, #37912, #57543, #17346, #32768, #12515, #38233, #3504, #18605, #57853, #8950, #33395, #48183, #62366, #42094, #56597, #53009, #22498, #28562, #18290, #32126, #46935, #13148, #33087, #37281, #27623, #47253, #56909, #12828, #52402, #52701, #8334, #8636, #28247, #47861, #23442, #43044, #62684, #9262, #58781, #579, #24691, #14399, #38523, #14711, #5393, #5071, #9575, #48809, #10524, #34655, #25010, #24373, #44297, #261, #34329, #29182, #19858, #48498, #44619, #53955, #58473, #14080, #34021, #39472, #54602, #9887, #4136, #4435, #39789, #59109, #24064, #54276, #28876, #4747, #29495, #59435, #29819, #43976, #63621, #53642, #18908, #43660, #58151, #19543, #15363, #43352, #38836, #63301, #30138, #34987, #19222, #23757, #49451, #49128, #20188, #63000, #15038, #39156, #33708, #53328, #10215, #49767, #1540, #40114, #5713, #21144, #11488, #20515, #6044, #25327, #40749, #15681, #25967, #35299, #908, #35943, #25651, #44949, #6362, #11168, #60398, #59755, #1232, #31106, #16322, #55572, #20831, #54920, #45583, #40433, #10846, #50090, #45265, #30462, #60072, #15997, #35621, #55249, #50418, #30791, #792, #58993, #44507, #58366, #19751, #19108, #54160, #63198, #24905, #5928, #14922, #43552, #471, #20400, #38726, #39362, #33912, #30352, #15249, #34528, #10102, #49977, #54496, #34875, #29710, #63512, #10744, #49013, #14293, #44830, #43864, #10422, #53537, #39678, #49341, #9774, #53845, #24584, #5287, #19436, #35198, #39048, #5602, #20072, #9463, #29073, #48697, #58677, #59646, #44190, #30034, #4637, #24261, #14604, #59313, #34219, #49663, #29380, #4962, #25219, #155, #39999, #15579, #54813, #36833, #2126, #22039, #51318, #6298, #41322, #60013, #26869, #25903, #46795, #46481, #31999, #11104, #50667, #2741, #7256, #45521, #36506, #1481, #15936, #61284, #31042, #35559, #50993, #36197, #60970, #17206, #21084, #2427, #16890, #56137, #40689, #41630, #55818, #60334, #12058, #55183, #30728, #26544, #31683, #56463, #21727, #6932, #50351, #11734, #12385, #31351, #51632, #16262, #16576, #35880, #46164, #55509, #7566, #40372, #27178, #11424, #6608, #26221, #45841, #1803, #21407, #41010, #60652, #18151, #37779, #28737, #33266, #13646, #52576, #42281, #53197, #27802, #37156, #23622, #22681, #52885, #9131, #18474, #13331, #52261, #32632, #3378, #43219, #42596, #62553, #38094, #32952, #47427, #57720, #3064, #62859, #8508, #13012, #32312, #8199, #8819, #48363, #28118, #22361, #61920, #58022, #4001, #18772, #47735, #38399, #28435, #51941, #23305, #41961, #48048, #7883, #61602, #13950, #33576, #56780, #22995, #17537, #12699, #27486, #47115, #17840, #37463, #57093, #62233, #57411, #3691, #42905, #5258, #44802, #48671, #15219, #24879, #44480, #29046, #34848, #19724, #4611, #39650, #43527, #58339, #54134, #439, #20045, #29685, #14893, #63172, #39333, #25187, #58966, #59288, #19082, #44161, #38702, #34500, #23926, #49315, #30324, #10073, #4307, #54469, #765, #14268, #130, #33887, #54787, #10396, #30006, #49636, #10717, #5573, #20373, #39974, #24235, #35171, #9748, #53507, #59619, #43840, #15550, #9437, #63486, #19410, #34195, #14572, #48988, #39024, #24557, #58652, #53818, #29353, #4935, #2044, #30651, #26786, #40929, #40618, #59942, #60261, #21649, #36756, #16498, #49946, #50273, #21961, #41242, #6219, #16812, #11027, #11346, #60576, #41557, #11978, #30969, #50594, #16180, #1091, #25831, #20700, #45767, #61208, #25507, #21011, #45447, #56386, #17132, #1411, #12313, #31607, #55742, #40304, #15865, #35805, #2354, #6534, #60888, #5901, #45127, #55430, #21329, #35486, #1723, #26148, #55103, #11658, #36119, #50912, #6854, #31278, #26469, #46084, #36432, #56062, #51242, #7178, #46404, #17460, #32554, #37082, #12620, #37694, #47662, #3614, #51553, #42517, #22282, #47970, #57336, #28352, #3925, #18703, #23544, #57957, #32876, #51864, #7488, #43144, #32232, #62784, #52504, #38328, #31925, #22925, #8438, #41882, #42203, #61847, #27408, #27102, #62154, #28042, #2989, #23221, #46717, #13252, #7807, #18073, #47040, #56702, #42832, #2662, #62476, #17766, #61528, #18396, #33194, #38017, #37383, #12932, #22607, #57648, #57016, #52179, #8124, #27727, #47354, #13576, #52809, #8747, #3303, #9676, #38945, #4859, #34767, #24480, #39895, #63414, #9997, #4238, #25111, #29610, #49240, #39260, #43768, #53121, #23853, #9364, #58886, #5184, #34431, #44086, #19967, #48599, #54393, #43456, #53432, #44405, #28665, #10320, #51, #28977, #19649, #33813, #5498, #4539, #39577, #14817, #63101, #48283, #15146, #14187, #24800, #685, #364, #54059, #19332, #24165, #58582, #29932, #34121, #59215, #49556, #44723, #14500, #20294, #58266, #13878, #33506, #53744, #19013, #29284, #9055, #38626, #48914, #59541, #40230, #31525, #11591, #59865, #26391, #20624, #20937, #6467, #51167, #21573, #40541, #60182, #25761, #10632, #15789, #30245, #55357, #7100, #35092, #30569, #35405, #46330, #26715, #55027, #2288, #41172, #1650, #60818, #55990, #21249, #16743, #6780, #25434, #60499, #15476, #46009, #45052, #21891, #1974, #54713, #49868, #6145, #5816, #36360, #1019, #55676, #10950, #50193, #11905, #45373, #1338, #26075, #11271, #16427, #16104, #35728, #30897, #36047, #31211, #50525, #45693, #40856, #50840, #13181, #17061, #31850, #27655, #37621, #62082, #3231, #52109, #36678, #12861, #62399, #56940, #42439, #56309, #17697, #12236, #8051, #61139, #22849, #3849, #32480, #41487, #17995, #18320, #51483, #37311, #7420, #28279, #32803, #47282, #57262, #47893, #52432, #8365, #27965, #61455, #8667, #46970, #57578, #42127, #47588, #27029, #46647, #17385, #3539, #2592, #23148, #37004, #22212, #42756, #7735, #37945, #13504, #33120, #52736, #41809, #56631, #12545, #32157, #51793, #22531, #27339, #61770, #2918, #4167, #29213, #39186, #58812, #43074, #34051, #13805, #39504, #48838, #19889, #59139, #10248, #15073, #49484, #24405, #43384, #62711, #34686, #23782, #54308, #44008, #29851, #23470, #14427, #63654, #33425, #33738, #53355, #18936, #18637, #53672, #19573, #58184, #14742, #38259, #4778, #63029, #9605, #38552, #28592, #34358, #57880, #53988, #9290, #53044, #9916, #24723, #29526, #28908, #4468, #8981, #49161, #48212, #14112, #48528, #24095, #43690, #5105, #44327, #291, #63337, #19253, #38868, #58504, #26310, #60107, #31444, #54951, #1574, #59463, #16668, #21174, #40782, #30824, #35331, #44649, #15395, #946, #50454, #60428, #26000, #35655, #11520, #40145, #45932, #35020, #44980, #35975, #20220, #1895, #55282, #20548, #16028, #25361, #60744, #59790, #31135, #6394, #54633, #39821, #10557, #15713, #25038, #55603, #30168, #11825, #50760, #36290, #49798, #10880, #5422, #16354, #5742, #6704, #30497, #611, #21501, #50118, #6074, #11201, #1261, #45618, #41097, #25687, #55913, #45296, #20864, #40467, #62006, #2835, #12153, #22771, #26634, #41415, #37241, #47208, #7976, #12784, #61693, #46254, #22453, #8287, #42051, #52034, #2214, #27267, #21817, #17624, #7025, #32406, #13421, #56866, #51087, #27574, #27892, #61065, #46892, #16985, #37872, #42367, #3152, #17925, #57505, #37547, #57187, #13108, #7346, #18246, #56552, #36597, #52352, #51404, #32725, #56232, #47513, #3464, #17297, #61376, #32083, #23077, #7661, #42681, #62322, #31772, #12473, #26957, #46575, #2517, #22132, #41727, #36923, #51720, #4702, #19815, #63259, #33044, #13731, #5027, #48760, #33353, #63578, #57808, #58109, #43616, #24646, #58740, #14037, #33665, #62947, #47819, #52969, #3776, #28833, #44253, #8594, #4092, #8907, #39423, #217, #28523, #59065, #14667, #38791, #34287, #29446, #58429, #53910, #43930, #62645, #33979, #9836, #48456, #53600, #23400, #9220, #28205, #19176, #52660, #14357, #43000, #4394, #18564, #9532, #49080, #38187, #24013, #48140, #23715, #24326, #29137, #19497, #43312, #39112, #18861, #38481, #53284, #46729, #21342, #29773, #17146, #15316, #7191, #2674, #11994, #6868, #45780, #26161, #60592, #36770, #36133, #56074, #31621, #26483, #40942, #51256, #59382, #56400, #46097, #5671, #24969, #1739, #26799, #22296, #2057, #14990, #34938, #51565, #46419, #54559, #2368, #39741, #16512, #21665, #7504, #41570, #55755, #11672, #31291, #49407, #10482, #5351, #50927, #27116, #54230, #49725, #30095, #41895, #34600, #41256, #10169, #61222, #60903, #12326, #31937, #16826, #44575, #21977, #532, #36445, #20145, #47985, #47052, #4249, #3939, #53135, #32248, #8136, #23864, #8758, #27421, #57661, #3002, #37094, #18715, #52191, #17473, #8451, #57347, #62490, #38340, #42215, #28364, #18408, #38029, #22619, #23558, #13264, #61860, #33206, #56713, #51878, #47674, #13587, #52821, #23233, #28055, #12631, #32888, #52516, #43156, #32569, #62796, #9067, #42847, #37396, #3626, #57031, #17777, #57967, #13890, #33517, #27739, #7818, #28677, #48296, #61540, #3316, #42530, #12945, #47368, #22936, #62167, #18087, #37710, #35108, #5507, #25122, #10333, #14511, #39271, #4873, #34442, #695, #54071, #5830, #29295, #39589, #33825, #54725, #59226, #15158, #5194, #9687, #19024, #53444, #38955, #24812, #34779, #376, #10010, #49568, #34133, #20308, #9376, #19343, #29943, #58280, #39908, #29622, #58593, #49253, #63426, #10645, #53754, #44735, #44415, #28987, #14199, #48611, #48924, #59553, #44098, #54403, #43467, #63113, #24493, #14828, #4550, #58899, #62, #38638, #19980, #19659, #15488, #30258, #49881, #24175, #43779, #31220, #60828, #10963, #35741, #6478, #30585, #26086, #50207, #6157, #50851, #41183, #16753, #45065, #36058, #15801, #41497, #6793, #21900, #61150, #12247, #17072, #51493, #26401, #45384, #1031, #36691, #25773, #56324, #46021, #31860, #25445, #16437, #1983, #35418, #55367, #11282, #20952, #20636, #40242, #21585, #55686, #30908, #50535, #45707, #26725, #1661, #36370, #56001, #11600, #21260, #11916, #1350, #2298, #31539, #16113, #55038, #40867, #51178, #59880, #7110, #40554, #60195, #60511, #46341, #51802, #37956, #32169, #32490, #18009, #43084, #33132, #52119, #8063, #37321, #22222 ) ),
 .UNSPECIFIED., .F., .F., .F. ) 
 B_SPLINE_SURFACE_WITH_KNOTS ( ( 2, 2 ),
 ( 3, 2, 2, 2, 2, 2, 2, 2, 2, 2, 2, 2, 2, 2, 2, 2, 2, 2, 2, 2, 2, 2, 2, 2, 2, 2, 2, 2, 2, 2, 2, 2, 2, 2, 2, 2, 2, 2, 2, 2, 2, 2, 2, 2, 2, 2, 2, 2, 2, 2, 2, 2, 2, 2, 2, 2, 2, 2, 2, 2, 2, 2, 2, 2, 2, 2, 2, 2, 2, 2, 2, 2, 2, 2, 2, 2, 2, 2, 2, 2, 2, 2, 2, 2, 2, 2, 2, 2, 2, 2, 2, 2, 2, 2, 2, 2, 2, 2, 2, 2, 2, 2, 2, 2, 2, 2, 2, 2, 2, 2, 2, 2, 2, 2, 2, 2, 2, 2, 2, 2, 2, 2, 2, 2, 2, 2, 2, 2, 2, 2, 2, 2, 2, 2, 2, 2, 2, 2, 2, 2, 2, 2, 2, 2, 2, 2, 2, 2, 2, 2, 2, 2, 2, 2, 2, 2, 2, 2, 2, 2, 2, 2, 2, 2, 2, 2, 2, 2, 2, 2, 2, 2, 2, 2, 2, 2, 2, 2, 2, 2, 2, 2, 2, 2, 2, 2, 2, 2, 2, 2, 2, 2, 2, 2, 2, 2, 2, 2, 2, 2, 2, 2, 2, 2, 2, 2, 2, 2, 2, 2, 2, 2, 2, 2, 2, 2, 2, 2, 2, 2, 2, 2, 2, 2, 2, 2, 2, 2, 2, 2, 2, 2, 2, 2, 2, 2, 2, 2, 2, 2, 2, 2, 2, 2, 2, 2, 2, 2, 2, 2, 2, 2, 2, 2, 2, 2, 2, 2, 2, 2, 2, 2, 2, 2, 2, 2, 2, 2, 2, 2, 2, 2, 2, 2, 2, 2, 2, 2, 2, 2, 2, 2, 2, 2, 2, 2, 2, 2, 2, 2, 2, 2, 2, 2, 2, 2, 2, 2, 2, 2, 2, 2, 2, 2, 2, 2, 2, 2, 2, 2, 2, 2, 2, 2, 2, 2, 2, 2, 2, 2, 2, 2, 2, 2, 2, 2, 2, 2, 2, 2, 2, 2, 2, 2, 2, 2, 2, 2, 2, 2, 2, 2, 2, 2, 2, 2, 2, 2, 2, 2, 2, 2, 2, 2, 2, 2, 2, 2, 2, 2, 2, 2, 2, 2, 2, 2, 2, 2, 2, 2, 2, 2, 2, 2, 2, 2, 2, 2, 2, 2, 2, 2, 2, 2, 2, 2, 2, 2, 2, 2, 2, 2, 2, 2, 2, 2, 2, 2, 2, 2, 2, 2, 2, 2, 2, 2, 2, 2, 2, 2, 2, 2, 2, 2, 2, 2, 2, 2, 2, 2, 2, 2, 2, 2, 2, 2, 2, 2, 2, 2, 2, 2, 2, 2, 2, 2, 2, 2, 2, 2, 2, 2, 2, 2, 2, 2, 2, 2, 2, 2, 2, 2, 2, 2, 2, 2, 2, 2, 2, 2, 2, 2, 2, 2, 2, 2, 2, 2, 2, 2, 2, 2, 2, 2, 2, 2, 2, 2, 2, 2, 2, 2, 2, 2, 2, 2, 2, 2, 2, 2, 2, 2, 2, 2, 2, 2, 2, 2, 2, 2, 2, 2, 2, 2, 2, 2, 2, 2, 2, 2, 2, 2, 2, 2, 2, 2, 2, 2, 2, 2, 2, 2, 2, 2, 2, 2, 2, 2, 2, 2, 2, 2, 2, 2, 2, 2, 2, 2, 2, 2, 2, 2, 2, 2, 2, 2, 2, 2, 2, 2, 2, 2, 2, 2, 2, 2, 2, 2, 2, 2, 2, 2, 2, 2, 2, 2, 2, 2, 2, 2, 2, 2, 2, 2, 2, 2, 2, 2, 2, 2, 2, 2, 2, 2, 2, 2, 2, 2, 2, 2, 2, 2, 2, 2, 2, 2, 2, 2, 2, 2, 2, 2, 2, 2, 2, 2, 2, 2, 2, 2, 2, 2, 2, 2, 2, 2, 2, 2, 2, 2, 2, 2, 2, 2, 2, 2, 2, 2, 2, 2, 2, 2, 2, 2, 2, 2, 2, 2, 2, 2, 2, 2, 2, 2, 2, 2, 2, 2, 2, 2, 2, 2, 2, 2, 2, 2, 2, 2, 2, 2, 2, 2, 2, 2, 2, 2, 2, 2, 2, 2, 2, 2, 2, 2, 2, 2, 2, 2, 2, 2, 2, 2, 2, 2, 2, 2, 2, 2, 2, 2, 2, 2, 2, 2, 2, 2, 2, 2, 2, 2, 2, 2, 2, 2, 2, 2, 2, 2, 2, 2, 2, 2, 2, 2, 2, 2, 2, 2, 2, 2, 2, 2, 2, 2, 2, 2, 2, 2, 2, 2, 2, 2, 2, 2, 2, 2, 2, 2, 2, 2, 2, 2, 2, 2, 2, 2, 2, 2, 2, 2, 2, 2, 2, 2, 2, 2, 2, 2, 2, 2, 2, 2, 2, 2, 2, 2, 2, 2, 2, 2, 2, 2, 2, 2, 2, 2, 2, 2, 2, 2, 2, 2, 2, 2, 2, 2, 2, 2, 2, 2, 2, 2, 2, 2, 2, 2, 2, 2, 2, 2, 2, 2, 2, 2, 2, 2, 2, 2, 2, 2, 2, 2, 2, 2, 2, 2, 2, 2, 2, 2, 2, 2, 2, 2, 2, 2, 2, 2, 2, 2, 2, 2, 2, 2, 2, 2, 2, 2, 2, 2, 3 ),
 ( 0.000000000000000000, 1.000000000000000000 ),
 ( 0.000000000000000000, 0.001190476190476190584, 0.002380952380952381167, 0.003571428571428571317, 0.004761904761904762334, 0.005952380952380952051, 0.007142857142857142634, 0.008333333333333333218, 0.009523809523809524669, 0.01071428571428571438, 0.01190476190476190410, 0.01309523809523809555, 0.01428571428571428527, 0.01547619047619047672, 0.01666666666666666644, 0.01785714285714285615, 0.01904761904761904934, 0.02023809523809523905, 0.02142857142857142877, 0.02261904761904761849, 0.02380952380952380820, 0.02500000000000000139, 0.02619047619047619110, 0.02738095238095238082, 0.02857142857142857054, 0.02976190476190476025, 0.03095238095238095344, 0.03214285714285713969, 0.03333333333333333287, 0.03452380952380952606, 0.03571428571428571230, 0.03690476190476190549, 0.03809523809523809867, 0.03928571428571428492, 0.04047619047619047811, 0.04166666666666666435, 0.04285714285714285754, 0.04404761904761905073, 0.04523809523809523697, 0.04642857142857143016, 0.04761904761904761640, 0.04880952380952380959, 0.05000000000000000278, 0.05119047619047618902, 0.05238095238095238221, 0.05357142857142856845, 0.05476190476190476164, 0.05595238095238095483, 0.05714285714285714107, 0.05833333333333333426, 0.05952380952380952051, 0.06071428571428571369, 0.06190476190476190688, 0.06309523809523809312, 0.06428571428571427937, 0.06547619047619047949, 0.06666666666666666574, 0.06785714285714285199, 0.06904761904761905211, 0.07023809523809523836, 0.07142857142857142461, 0.07261904761904762473, 0.07380952380952381098, 0.07499999999999999722, 0.07619047619047619735, 0.07738095238095238360, 0.07857142857142856984, 0.07976190476190475609, 0.08095238095238095621, 0.08214285714285714246, 0.08333333333333332871, 0.08452380952380952883, 0.08571428571428571508, 0.08690476190476190133, 0.08809523809523810145, 0.08928571428571428770, 0.09047619047619047394, 0.09166666666666666019, 0.09285714285714286031, 0.09404761904761904656, 0.09523809523809523281, 0.09642857142857143293, 0.09761904761904761918, 0.09880952380952380543, 0.1000000000000000056, 0.1011904761904761918, 0.1023809523809523780, 0.1035714285714285782, 0.1047619047619047644, 0.1059523809523809507, 0.1071428571428571369, 0.1083333333333333370, 0.1095238095238095233, 0.1107142857142857095, 0.1119047619047619097, 0.1130952380952380959, 0.1142857142857142821, 0.1154761904761904823, 0.1166666666666666685, 0.1178571428571428548, 0.1190476190476190410, 0.1202380952380952411, 0.1214285714285714274, 0.1226190476190476136, 0.1238095238095238138, 0.1250000000000000000, 0.1261904761904761862, 0.1273809523809523725, 0.1285714285714285587, 0.1297619047619047727, 0.1309523809523809590, 0.1321428571428571452, 0.1333333333333333315, 0.1345238095238095177, 0.1357142857142857040, 0.1369047619047619180, 0.1380952380952381042, 0.1392857142857142905, 0.1404761904761904767, 0.1416666666666666630, 0.1428571428571428492, 0.1440476190476190355, 0.1452380952380952495, 0.1464285714285714357, 0.1476190476190476220, 0.1488095238095238082, 0.1499999999999999944, 0.1511904761904761807, 0.1523809523809523947, 0.1535714285714285809, 0.1547619047619047672, 0.1559523809523809534, 0.1571428571428571397, 0.1583333333333333259, 0.1595238095238095122, 0.1607142857142857262, 0.1619047619047619124, 0.1630952380952380987, 0.1642857142857142849, 0.1654761904761904712, 0.1666666666666666574, 0.1678571428571428437, 0.1690476190476190577, 0.1702380952380952439, 0.1714285714285714302, 0.1726190476190476164, 0.1738095238095238027, 0.1749999999999999889, 0.1761904761904762029, 0.1773809523809523891, 0.1785714285714285754, 0.1797619047619047616, 0.1809523809523809479, 0.1821428571428571341, 0.1833333333333333204, 0.1845238095238095344, 0.1857142857142857206, 0.1869047619047619069, 0.1880952380952380931, 0.1892857142857142794, 0.1904761904761904656, 0.1916666666666666796, 0.1928571428571428659, 0.1940476190476190521, 0.1952380952380952384, 0.1964285714285714246, 0.1976190476190476109, 0.1988095238095237971, 0.2000000000000000111, 0.2011904761904761973, 0.2023809523809523836, 0.2035714285714285698, 0.2047619047619047561, 0.2059523809523809423, 0.2071428571428571563, 0.2083333333333333426, 0.2095238095238095288, 0.2107142857142857151, 0.2119047619047619013, 0.2130952380952380876, 0.2142857142857142738, 0.2154761904761904878, 0.2166666666666666741, 0.2178571428571428603, 0.2190476190476190466, 0.2202380952380952328, 0.2214285714285714191, 0.2226190476190476053, 0.2238095238095238193, 0.2250000000000000056, 0.2261904761904761918, 0.2273809523809523780, 0.2285714285714285643, 0.2297619047619047505, 0.2309523809523809645, 0.2321428571428571508, 0.2333333333333333370, 0.2345238095238095233, 0.2357142857142857095, 0.2369047619047618958, 0.2380952380952380820, 0.2392857142857142960, 0.2404761904761904823, 0.2416666666666666685, 0.2428571428571428548, 0.2440476190476190410, 0.2452380952380952273, 0.2464285714285714413, 0.2476190476190476275, 0.2488095238095238138, 0.2500000000000000000, 0.2511904761904761862, 0.2523809523809523725, 0.2535714285714285587, 0.2547619047619047450, 0.2559523809523809312, 0.2571428571428571175, 0.2583333333333333592, 0.2595238095238095455, 0.2607142857142857317, 0.2619047619047619180, 0.2630952380952381042, 0.2642857142857142905, 0.2654761904761904767, 0.2666666666666666630, 0.2678571428571428492, 0.2690476190476190355, 0.2702380952380952217, 0.2714285714285714080, 0.2726190476190475942, 0.2738095238095238360, 0.2750000000000000222, 0.2761904761904762085, 0.2773809523809523947, 0.2785714285714285809, 0.2797619047619047672, 0.2809523809523809534, 0.2821428571428571397, 0.2833333333333333259, 0.2845238095238095122, 0.2857142857142856984, 0.2869047619047618847, 0.2880952380952380709, 0.2892857142857143127, 0.2904761904761904989, 0.2916666666666666852, 0.2928571428571428714, 0.2940476190476190577, 0.2952380952380952439, 0.2964285714285714302, 0.2976190476190476164, 0.2988095238095238027, 0.2999999999999999889, 0.3011904761904761751, 0.3023809523809523614, 0.3035714285714285476, 0.3047619047619047894, 0.3059523809523809756, 0.3071428571428571619, 0.3083333333333333481, 0.3095238095238095344, 0.3107142857142857206, 0.3119047619047619069, 0.3130952380952380931, 0.3142857142857142794, 0.3154761904761904656, 0.3166666666666666519, 0.3178571428571428381, 0.3190476190476190244, 0.3202380952380952106, 0.3214285714285714524, 0.3226190476190476386, 0.3238095238095238249, 0.3250000000000000111, 0.3261904761904761973, 0.3273809523809523836, 0.3285714285714285698, 0.3297619047619047561, 0.3309523809523809423, 0.3321428571428571286, 0.3333333333333333148, 0.3345238095238095011, 0.3357142857142856873, 0.3369047619047619291, 0.3380952380952381153, 0.3392857142857143016, 0.3404761904761904878, 0.3416666666666666741, 0.3428571428571428603, 0.3440476190476190466, 0.3452380952380952328, 0.3464285714285714191, 0.3476190476190476053, 0.3488095238095237915, 0.3499999999999999778, 0.3511904761904761640, 0.3523809523809524058, 0.3535714285714285920, 0.3547619047619047783, 0.3559523809523809645, 0.3571428571428571508, 0.3583333333333333370, 0.3595238095238095233, 0.3607142857142857095, 0.3619047619047618958, 0.3630952380952380820, 0.3642857142857142683, 0.3654761904761904545, 0.3666666666666666408, 0.3678571428571428825, 0.3690476190476190688, 0.3702380952380952550, 0.3714285714285714413, 0.3726190476190476275, 0.3738095238095238138, 0.3750000000000000000, 0.3761904761904761862, 0.3773809523809523725, 0.3785714285714285587, 0.3797619047619047450, 0.3809523809523809312, 0.3821428571428571175, 0.3833333333333333592, 0.3845238095238095455, 0.3857142857142857317, 0.3869047619047619180, 0.3880952380952381042, 0.3892857142857142905, 0.3904761904761904767, 0.3916666666666666630, 0.3928571428571428492, 0.3940476190476190355, 0.3952380952380952217, 0.3964285714285714080, 0.3976190476190475942, 0.3988095238095238360, 0.4000000000000000222, 0.4011904761904762085, 0.4023809523809523947, 0.4035714285714285809, 0.4047619047619047672, 0.4059523809523809534, 0.4071428571428571397, 0.4083333333333333259, 0.4095238095238095122, 0.4107142857142856984, 0.4119047619047618847, 0.4130952380952380709, 0.4142857142857143127, 0.4154761904761904989, 0.4166666666666666852, 0.4178571428571428714, 0.4190476190476190577, 0.4202380952380952439, 0.4214285714285714302, 0.4226190476190476164, 0.4238095238095238027, 0.4249999999999999889, 0.4261904761904761751, 0.4273809523809523614, 0.4285714285714285476, 0.4297619047619047894, 0.4309523809523809756, 0.4321428571428571619, 0.4333333333333333481, 0.4345238095238095344, 0.4357142857142857206, 0.4369047619047619069, 0.4380952380952380931, 0.4392857142857142794, 0.4404761904761904656, 0.4416666666666666519, 0.4428571428571428381, 0.4440476190476190244, 0.4452380952380952106, 0.4464285714285714524, 0.4476190476190476386, 0.4488095238095238249, 0.4500000000000000111, 0.4511904761904761973, 0.4523809523809523836, 0.4535714285714285698, 0.4547619047619047561, 0.4559523809523809423, 0.4571428571428571286, 0.4583333333333333148, 0.4595238095238095011, 0.4607142857142856873, 0.4619047619047619291, 0.4630952380952381153, 0.4642857142857143016, 0.4654761904761904878, 0.4666666666666666741, 0.4678571428571428603, 0.4690476190476190466, 0.4702380952380952328, 0.4714285714285714191, 0.4726190476190476053, 0.4738095238095237915, 0.4749999999999999778, 0.4761904761904761640, 0.4773809523809524058, 0.4785714285714285920, 0.4797619047619047783, 0.4809523809523809645, 0.4821428571428571508, 0.4833333333333333370, 0.4845238095238095233, 0.4857142857142857095, 0.4869047619047618958, 0.4880952380952380820, 0.4892857142857142683, 0.4904761904761904545, 0.4916666666666666408, 0.4928571428571428825, 0.4940476190476190688, 0.4952380952380952550, 0.4964285714285714413, 0.4976190476190476275, 0.4988095238095238138, 0.5000000000000000000, 0.5011904761904761862, 0.5023809523809523725, 0.5035714285714285587, 0.5047619047619047450, 0.5059523809523809312, 0.5071428571428571175, 0.5083333333333333037, 0.5095238095238094900, 0.5107142857142856762, 0.5119047619047618625, 0.5130952380952380487, 0.5142857142857142350, 0.5154761904761904212, 0.5166666666666667185, 0.5178571428571429047, 0.5190476190476190910, 0.5202380952380952772, 0.5214285714285714635, 0.5226190476190476497, 0.5238095238095238360, 0.5250000000000000222, 0.5261904761904762085, 0.5273809523809523947, 0.5285714285714285809, 0.5297619047619047672, 0.5309523809523809534, 0.5321428571428571397, 0.5333333333333333259, 0.5345238095238095122, 0.5357142857142856984, 0.5369047619047618847, 0.5380952380952380709, 0.5392857142857142572, 0.5404761904761904434, 0.5416666666666666297, 0.5428571428571428159, 0.5440476190476190022, 0.5452380952380951884, 0.5464285714285713746, 0.5476190476190476719, 0.5488095238095238582, 0.5500000000000000444, 0.5511904761904762307, 0.5523809523809524169, 0.5535714285714286031, 0.5547619047619047894, 0.5559523809523809756, 0.5571428571428571619, 0.5583333333333333481, 0.5595238095238095344, 0.5607142857142857206, 0.5619047619047619069, 0.5630952380952380931, 0.5642857142857142794, 0.5654761904761904656, 0.5666666666666666519, 0.5678571428571428381, 0.5690476190476190244, 0.5702380952380952106, 0.5714285714285713969, 0.5726190476190475831, 0.5738095238095237693, 0.5749999999999999556, 0.5761904761904761418, 0.5773809523809523281, 0.5785714285714286254, 0.5797619047619048116, 0.5809523809523809978, 0.5821428571428571841, 0.5833333333333333703, 0.5845238095238095566, 0.5857142857142857428, 0.5869047619047619291, 0.5880952380952381153, 0.5892857142857143016, 0.5904761904761904878, 0.5916666666666666741, 0.5928571428571428603, 0.5940476190476190466, 0.5952380952380952328, 0.5964285714285714191, 0.5976190476190476053, 0.5988095238095237915, 0.5999999999999999778, 0.6011904761904761640, 0.6023809523809523503, 0.6035714285714285365, 0.6047619047619047228, 0.6059523809523809090, 0.6071428571428570953, 0.6083333333333332815, 0.6095238095238095788, 0.6107142857142857650, 0.6119047619047619513, 0.6130952380952381375, 0.6142857142857143238, 0.6154761904761905100, 0.6166666666666666963, 0.6178571428571428825, 0.6190476190476190688, 0.6202380952380952550, 0.6214285714285714413, 0.6226190476190476275, 0.6238095238095238138, 0.6250000000000000000, 0.6261904761904761862, 0.6273809523809523725, 0.6285714285714285587, 0.6297619047619047450, 0.6309523809523809312, 0.6321428571428571175, 0.6333333333333333037, 0.6345238095238094900, 0.6357142857142856762, 0.6369047619047618625, 0.6380952380952380487, 0.6392857142857142350, 0.6404761904761904212, 0.6416666666666667185, 0.6428571428571429047, 0.6440476190476190910, 0.6452380952380952772, 0.6464285714285714635, 0.6476190476190476497, 0.6488095238095238360, 0.6500000000000000222, 0.6511904761904762085, 0.6523809523809523947, 0.6535714285714285809, 0.6547619047619047672, 0.6559523809523809534, 0.6571428571428571397, 0.6583333333333333259, 0.6595238095238095122, 0.6607142857142856984, 0.6619047619047618847, 0.6630952380952380709, 0.6642857142857142572, 0.6654761904761904434, 0.6666666666666666297, 0.6678571428571428159, 0.6690476190476190022, 0.6702380952380951884, 0.6714285714285713746, 0.6726190476190476719, 0.6738095238095238582, 0.6750000000000000444, 0.6761904761904762307, 0.6773809523809524169, 0.6785714285714286031, 0.6797619047619047894, 0.6809523809523809756, 0.6821428571428571619, 0.6833333333333333481, 0.6845238095238095344, 0.6857142857142857206, 0.6869047619047619069, 0.6880952380952380931, 0.6892857142857142794, 0.6904761904761904656, 0.6916666666666666519, 0.6928571428571428381, 0.6940476190476190244, 0.6952380952380952106, 0.6964285714285713969, 0.6976190476190475831, 0.6988095238095237693, 0.6999999999999999556, 0.7011904761904761418, 0.7023809523809523281, 0.7035714285714286254, 0.7047619047619048116, 0.7059523809523809978, 0.7071428571428571841, 0.7083333333333333703, 0.7095238095238095566, 0.7107142857142857428, 0.7119047619047619291, 0.7130952380952381153, 0.7142857142857143016, 0.7154761904761904878, 0.7166666666666666741, 0.7178571428571428603, 0.7190476190476190466, 0.7202380952380952328, 0.7214285714285714191, 0.7226190476190476053, 0.7238095238095237915, 0.7249999999999999778, 0.7261904761904761640, 0.7273809523809523503, 0.7285714285714285365, 0.7297619047619047228, 0.7309523809523809090, 0.7321428571428570953, 0.7333333333333332815, 0.7345238095238095788, 0.7357142857142857650, 0.7369047619047619513, 0.7380952380952381375, 0.7392857142857143238, 0.7404761904761905100, 0.7416666666666666963, 0.7428571428571428825, 0.7440476190476190688, 0.7452380952380952550, 0.7464285714285714413, 0.7476190476190476275, 0.7488095238095238138, 0.7500000000000000000, 0.7511904761904761862, 0.7523809523809523725, 0.7535714285714285587, 0.7547619047619047450, 0.7559523809523809312, 0.7571428571428571175, 0.7583333333333333037, 0.7595238095238094900, 0.7607142857142856762, 0.7619047619047618625, 0.7630952380952380487, 0.7642857142857142350, 0.7654761904761904212, 0.7666666666666667185, 0.7678571428571429047, 0.7690476190476190910, 0.7702380952380952772, 0.7714285714285714635, 0.7726190476190476497, 0.7738095238095238360, 0.7750000000000000222, 0.7761904761904762085, 0.7773809523809523947, 0.7785714285714285809, 0.7797619047619047672, 0.7809523809523809534, 0.7821428571428571397, 0.7833333333333333259, 0.7845238095238095122, 0.7857142857142856984, 0.7869047619047618847, 0.7880952380952380709, 0.7892857142857142572, 0.7904761904761904434, 0.7916666666666666297, 0.7928571428571428159, 0.7940476190476190022, 0.7952380952380951884, 0.7964285714285713746, 0.7976190476190476719, 0.7988095238095238582, 0.8000000000000000444, 0.8011904761904762307, 0.8023809523809524169, 0.8035714285714286031, 0.8047619047619047894, 0.8059523809523809756, 0.8071428571428571619, 0.8083333333333333481, 0.8095238095238095344, 0.8107142857142857206, 0.8119047619047619069, 0.8130952380952380931, 0.8142857142857142794, 0.8154761904761904656, 0.8166666666666666519, 0.8178571428571428381, 0.8190476190476190244, 0.8202380952380952106, 0.8214285714285713969, 0.8226190476190475831, 0.8238095238095237693, 0.8249999999999999556, 0.8261904761904761418, 0.8273809523809523281, 0.8285714285714286254, 0.8297619047619048116, 0.8309523809523809978, 0.8321428571428571841, 0.8333333333333333703, 0.8345238095238095566, 0.8357142857142857428, 0.8369047619047619291, 0.8380952380952381153, 0.8392857142857143016, 0.8404761904761904878, 0.8416666666666666741, 0.8428571428571428603, 0.8440476190476190466, 0.8452380952380952328, 0.8464285714285714191, 0.8476190476190476053, 0.8488095238095237915, 0.8499999999999999778, 0.8511904761904761640, 0.8523809523809523503, 0.8535714285714285365, 0.8547619047619047228, 0.8559523809523809090, 0.8571428571428570953, 0.8583333333333332815, 0.8595238095238095788, 0.8607142857142857650, 0.8619047619047619513, 0.8630952380952381375, 0.8642857142857143238, 0.8654761904761905100, 0.8666666666666666963, 0.8678571428571428825, 0.8690476190476190688, 0.8702380952380952550, 0.8714285714285714413, 0.8726190476190476275, 0.8738095238095238138, 0.8750000000000000000, 0.8761904761904761862, 0.8773809523809523725, 0.8785714285714285587, 0.8797619047619047450, 0.8809523809523809312, 0.8821428571428571175, 0.8833333333333333037, 0.8845238095238094900, 0.8857142857142856762, 0.8869047619047618625, 0.8880952380952380487, 0.8892857142857142350, 0.8904761904761904212, 0.8916666666666667185, 0.8928571428571429047, 0.8940476190476190910, 0.8952380952380952772, 0.8964285714285714635, 0.8976190476190476497, 0.8988095238095238360, 0.9000000000000000222, 0.9011904761904762085, 0.9023809523809523947, 0.9035714285714285809, 0.9047619047619047672, 0.9059523809523809534, 0.9071428571428571397, 0.9083333333333333259, 0.9095238095238095122, 0.9107142857142856984, 0.9119047619047618847, 0.9130952380952380709, 0.9142857142857142572, 0.9154761904761904434, 0.9166666666666666297, 0.9178571428571428159, 0.9190476190476190022, 0.9202380952380951884, 0.9214285714285713746, 0.9226190476190476719, 0.9238095238095238582, 0.9250000000000000444, 0.9261904761904762307, 0.9273809523809524169, 0.9285714285714286031, 0.9297619047619047894, 0.9309523809523809756, 0.9321428571428571619, 0.9333333333333333481, 0.9345238095238095344, 0.9357142857142857206, 0.9369047619047619069, 0.9380952380952380931, 0.9392857142857142794, 0.9404761904761904656, 0.9416666666666666519, 0.9428571428571428381, 0.9440476190476190244, 0.9452380952380952106, 0.9464285714285713969, 0.9476190476190475831, 0.9488095238095237693, 0.9499999999999999556, 0.9511904761904761418, 0.9523809523809523281, 0.9535714285714286254, 0.9547619047619048116, 0.9559523809523809978, 0.9571428571428571841, 0.9583333333333333703, 0.9595238095238095566, 0.9607142857142857428, 0.9619047619047619291, 0.9630952380952381153, 0.9642857142857143016, 0.9654761904761904878, 0.9666666666666666741, 0.9678571428571428603, 0.9690476190476190466, 0.9702380952380952328, 0.9714285714285714191, 0.9726190476190476053, 0.9738095238095237915, 0.9749999999999999778, 0.9761904761904761640, 0.9773809523809523503, 0.9785714285714285365, 0.9797619047619047228, 0.9809523809523809090, 0.9821428571428570953, 0.9833333333333332815, 0.9845238095238095788, 0.9857142857142857650, 0.9869047619047619513, 0.9880952380952381375, 0.9892857142857143238, 0.9904761904761905100, 0.9916666666666666963, 0.9928571428571428825, 0.9940476190476190688, 0.9952380952380952550, 0.9964285714285714413, 0.9976190476190476275, 0.9988095238095238138, 1.000000000000000000 ),
 .UNSPECIFIED. ) 
 GEOMETRIC_REPRESENTATION_ITEM ( )  RATIONAL_B_SPLINE_SURFACE ( (
 ( 1.000000000000000000, 0.8660254037844387076, 1.000000000000000000, 0.8660254037844387076, 1.000000000000000000, 0.8660254037844387076, 1.000000000000000000, 0.8660254037844387076, 1.000000000000000000, 0.8660254037844387076, 1.000000000000000000, 0.8660254037844387076, 1.000000000000000000, 0.8660254037844387076, 1.000000000000000000, 0.8660254037844387076, 1.000000000000000000, 0.8660254037844387076, 1.000000000000000000, 0.8660254037844387076, 1.000000000000000000, 0.8660254037844387076, 1.000000000000000000, 0.8660254037844387076, 1.000000000000000000, 0.8660254037844387076, 1.000000000000000000, 0.8660254037844387076, 1.000000000000000000, 0.8660254037844387076, 1.000000000000000000, 0.8660254037844387076, 1.000000000000000000, 0.8660254037844387076, 1.000000000000000000, 0.8660254037844387076, 1.000000000000000000, 0.8660254037844387076, 1.000000000000000000, 0.8660254037844387076, 1.000000000000000000, 0.8660254037844387076, 1.000000000000000000, 0.8660254037844387076, 1.000000000000000000, 0.8660254037844387076, 1.000000000000000000, 0.8660254037844387076, 1.000000000000000000, 0.8660254037844387076, 1.000000000000000000, 0.8660254037844387076, 1.000000000000000000, 0.8660254037844387076, 1.000000000000000000, 0.8660254037844387076, 1.000000000000000000, 0.8660254037844387076, 1.000000000000000000, 0.8660254037844387076, 1.000000000000000000, 0.8660254037844387076, 1.000000000000000000, 0.8660254037844387076, 1.000000000000000000, 0.8660254037844387076, 1.000000000000000000, 0.8660254037844387076, 1.000000000000000000, 0.8660254037844387076, 1.000000000000000000, 0.8660254037844387076, 1.000000000000000000, 0.8660254037844387076, 1.000000000000000000, 0.8660254037844387076, 1.000000000000000000, 0.8660254037844387076, 1.000000000000000000, 0.8660254037844387076, 1.000000000000000000, 0.8660254037844387076, 1.000000000000000000, 0.8660254037844387076, 1.000000000000000000, 0.8660254037844387076, 1.000000000000000000, 0.8660254037844387076, 1.000000000000000000, 0.8660254037844387076, 1.000000000000000000, 0.8660254037844387076, 1.000000000000000000, 0.8660254037844387076, 1.000000000000000000, 0.8660254037844387076, 1.000000000000000000, 0.8660254037844387076, 1.000000000000000000, 0.8660254037844387076, 1.000000000000000000, 0.8660254037844387076, 1.000000000000000000, 0.8660254037844387076, 1.000000000000000000, 0.8660254037844387076, 1.000000000000000000, 0.8660254037844387076, 1.000000000000000000, 0.8660254037844387076, 1.000000000000000000, 0.8660254037844387076, 1.000000000000000000, 0.8660254037844387076, 1.000000000000000000, 0.8660254037844387076, 1.000000000000000000, 0.8660254037844387076, 1.000000000000000000, 0.8660254037844387076, 1.000000000000000000, 0.8660254037844387076, 1.000000000000000000, 0.8660254037844387076, 1.000000000000000000, 0.8660254037844387076, 1.000000000000000000, 0.8660254037844387076, 1.000000000000000000, 0.8660254037844387076, 1.000000000000000000, 0.8660254037844387076, 1.000000000000000000, 0.8660254037844387076, 1.000000000000000000, 0.8660254037844387076, 1.000000000000000000, 0.8660254037844387076, 1.000000000000000000, 0.8660254037844387076, 1.000000000000000000, 0.8660254037844387076, 1.000000000000000000, 0.8660254037844387076, 1.000000000000000000, 0.8660254037844387076, 1.000000000000000000, 0.8660254037844387076, 1.000000000000000000, 0.8660254037844387076, 1.000000000000000000, 0.8660254037844387076, 1.000000000000000000, 0.8660254037844387076, 1.000000000000000000, 0.8660254037844387076, 1.000000000000000000, 0.8660254037844387076, 1.000000000000000000, 0.8660254037844387076, 1.000000000000000000, 0.8660254037844387076, 1.000000000000000000, 0.8660254037844387076, 1.000000000000000000, 0.8660254037844387076, 1.000000000000000000, 0.8660254037844387076, 1.000000000000000000, 0.8660254037844387076, 1.000000000000000000, 0.8660254037844387076, 1.000000000000000000, 0.8660254037844387076, 1.000000000000000000, 0.8660254037844387076, 1.000000000000000000, 0.8660254037844387076, 1.000000000000000000, 0.8660254037844387076, 1.000000000000000000, 0.8660254037844387076, 1.000000000000000000, 0.8660254037844387076, 1.000000000000000000, 0.8660254037844387076, 1.000000000000000000, 0.8660254037844387076, 1.000000000000000000, 0.8660254037844387076, 1.000000000000000000, 0.8660254037844387076, 1.000000000000000000, 0.8660254037844387076, 1.000000000000000000, 0.8660254037844387076, 1.000000000000000000, 0.8660254037844387076, 1.000000000000000000, 0.8660254037844387076, 1.000000000000000000, 0.8660254037844387076, 1.000000000000000000, 0.8660254037844387076, 1.000000000000000000, 0.8660254037844387076, 1.000000000000000000, 0.8660254037844387076, 1.000000000000000000, 0.8660254037844387076, 1.000000000000000000, 0.8660254037844387076, 1.000000000000000000, 0.8660254037844387076, 1.000000000000000000, 0.8660254037844387076, 1.000000000000000000, 0.8660254037844387076, 1.000000000000000000, 0.8660254037844387076, 1.000000000000000000, 0.8660254037844387076, 1.000000000000000000, 0.8660254037844387076, 1.000000000000000000, 0.8660254037844387076, 1.000000000000000000, 0.8660254037844387076, 1.000000000000000000, 0.8660254037844387076, 1.000000000000000000, 0.8660254037844387076, 1.000000000000000000, 0.8660254037844387076, 1.000000000000000000, 0.8660254037844387076, 1.000000000000000000, 0.8660254037844387076, 1.000000000000000000, 0.8660254037844387076, 1.000000000000000000, 0.8660254037844387076, 1.000000000000000000, 0.8660254037844387076, 1.000000000000000000, 0.8660254037844387076, 1.000000000000000000, 0.8660254037844387076, 1.000000000000000000, 0.8660254037844387076, 1.000000000000000000, 0.8660254037844387076, 1.000000000000000000, 0.8660254037844387076, 1.000000000000000000, 0.8660254037844387076, 1.000000000000000000, 0.8660254037844387076, 1.000000000000000000, 0.8660254037844387076, 1.000000000000000000, 0.8660254037844387076, 1.000000000000000000, 0.8660254037844387076, 1.000000000000000000, 0.8660254037844387076, 1.000000000000000000, 0.8660254037844387076, 1.000000000000000000, 0.8660254037844387076, 1.000000000000000000, 0.8660254037844387076, 1.000000000000000000, 0.8660254037844387076, 1.000000000000000000, 0.8660254037844387076, 1.000000000000000000, 0.8660254037844387076, 1.000000000000000000, 0.8660254037844387076, 1.000000000000000000, 0.8660254037844387076, 1.000000000000000000, 0.8660254037844387076, 1.000000000000000000, 0.8660254037844387076, 1.000000000000000000, 0.8660254037844387076, 1.000000000000000000, 0.8660254037844387076, 1.000000000000000000, 0.8660254037844387076, 1.000000000000000000, 0.8660254037844387076, 1.000000000000000000, 0.8660254037844387076, 1.000000000000000000, 0.8660254037844387076, 1.000000000000000000, 0.8660254037844387076, 1.000000000000000000, 0.8660254037844387076, 1.000000000000000000, 0.8660254037844387076, 1.000000000000000000, 0.8660254037844387076, 1.000000000000000000, 0.8660254037844387076, 1.000000000000000000, 0.8660254037844387076, 1.000000000000000000, 0.8660254037844387076, 1.000000000000000000, 0.8660254037844387076, 1.000000000000000000, 0.8660254037844387076, 1.000000000000000000, 0.8660254037844387076, 1.000000000000000000, 0.8660254037844387076, 1.000000000000000000, 0.8660254037844387076, 1.000000000000000000, 0.8660254037844387076, 1.000000000000000000, 0.8660254037844387076, 1.000000000000000000, 0.8660254037844387076, 1.000000000000000000, 0.8660254037844387076, 1.000000000000000000, 0.8660254037844387076, 1.000000000000000000, 0.8660254037844387076, 1.000000000000000000, 0.8660254037844387076, 1.000000000000000000, 0.8660254037844387076, 1.000000000000000000, 0.8660254037844387076, 1.000000000000000000, 0.8660254037844387076, 1.000000000000000000, 0.8660254037844387076, 1.000000000000000000, 0.8660254037844387076, 1.000000000000000000, 0.8660254037844387076, 1.000000000000000000, 0.8660254037844387076, 1.000000000000000000, 0.8660254037844387076, 1.000000000000000000, 0.8660254037844387076, 1.000000000000000000, 0.8660254037844387076, 1.000000000000000000, 0.8660254037844387076, 1.000000000000000000, 0.8660254037844387076, 1.000000000000000000, 0.8660254037844387076, 1.000000000000000000, 0.8660254037844387076, 1.000000000000000000, 0.8660254037844387076, 1.000000000000000000, 0.8660254037844387076, 1.000000000000000000, 0.8660254037844387076, 1.000000000000000000, 0.8660254037844387076, 1.000000000000000000, 0.8660254037844387076, 1.000000000000000000, 0.8660254037844387076, 1.000000000000000000, 0.8660254037844387076, 1.000000000000000000, 0.8660254037844387076, 1.000000000000000000, 0.8660254037844387076, 1.000000000000000000, 0.8660254037844387076, 1.000000000000000000, 0.8660254037844387076, 1.000000000000000000, 0.8660254037844387076, 1.000000000000000000, 0.8660254037844387076, 1.000000000000000000, 0.8660254037844387076, 1.000000000000000000, 0.8660254037844387076, 1.000000000000000000, 0.8660254037844387076, 1.000000000000000000, 0.8660254037844387076, 1.000000000000000000, 0.8660254037844387076, 1.000000000000000000, 0.8660254037844387076, 1.000000000000000000, 0.8660254037844387076, 1.000000000000000000, 0.8660254037844387076, 1.000000000000000000, 0.8660254037844387076, 1.000000000000000000, 0.8660254037844387076, 1.000000000000000000, 0.8660254037844387076, 1.000000000000000000, 0.8660254037844387076, 1.000000000000000000, 0.8660254037844387076, 1.000000000000000000, 0.8660254037844387076, 1.000000000000000000, 0.8660254037844387076, 1.000000000000000000, 0.8660254037844387076, 1.000000000000000000, 0.8660254037844387076, 1.000000000000000000, 0.8660254037844387076, 1.000000000000000000, 0.8660254037844387076, 1.000000000000000000, 0.8660254037844387076, 1.000000000000000000, 0.8660254037844387076, 1.000000000000000000, 0.8660254037844387076, 1.000000000000000000, 0.8660254037844387076, 1.000000000000000000, 0.8660254037844387076, 1.000000000000000000, 0.8660254037844387076, 1.000000000000000000, 0.8660254037844387076, 1.000000000000000000, 0.8660254037844387076, 1.000000000000000000, 0.8660254037844387076, 1.000000000000000000, 0.8660254037844387076, 1.000000000000000000, 0.8660254037844387076, 1.000000000000000000, 0.8660254037844387076, 1.000000000000000000, 0.8660254037844387076, 1.000000000000000000, 0.8660254037844387076, 1.000000000000000000, 0.8660254037844387076, 1.000000000000000000, 0.8660254037844387076, 1.000000000000000000, 0.8660254037844387076, 1.000000000000000000, 0.8660254037844387076, 1.000000000000000000, 0.8660254037844387076, 1.000000000000000000, 0.8660254037844387076, 1.000000000000000000, 0.8660254037844387076, 1.000000000000000000, 0.8660254037844387076, 1.000000000000000000, 0.8660254037844387076, 1.000000000000000000, 0.8660254037844387076, 1.000000000000000000, 0.8660254037844387076, 1.000000000000000000, 0.8660254037844387076, 1.000000000000000000, 0.8660254037844387076, 1.000000000000000000, 0.8660254037844387076, 1.000000000000000000, 0.8660254037844387076, 1.000000000000000000, 0.8660254037844387076, 1.000000000000000000, 0.8660254037844387076, 1.000000000000000000, 0.8660254037844387076, 1.000000000000000000, 0.8660254037844387076, 1.000000000000000000, 0.8660254037844387076, 1.000000000000000000, 0.8660254037844387076, 1.000000000000000000, 0.8660254037844387076, 1.000000000000000000, 0.8660254037844387076, 1.000000000000000000, 0.8660254037844387076, 1.000000000000000000, 0.8660254037844387076, 1.000000000000000000, 0.8660254037844387076, 1.000000000000000000, 0.8660254037844387076, 1.000000000000000000, 0.8660254037844387076, 1.000000000000000000, 0.8660254037844387076, 1.000000000000000000, 0.8660254037844387076, 1.000000000000000000, 0.8660254037844387076, 1.000000000000000000, 0.8660254037844387076, 1.000000000000000000, 0.8660254037844387076, 1.000000000000000000, 0.8660254037844387076, 1.000000000000000000, 0.8660254037844387076, 1.000000000000000000, 0.8660254037844387076, 1.000000000000000000, 0.8660254037844387076, 1.000000000000000000, 0.8660254037844387076, 1.000000000000000000, 0.8660254037844387076, 1.000000000000000000, 0.8660254037844387076, 1.000000000000000000, 0.8660254037844387076, 1.000000000000000000, 0.8660254037844387076, 1.000000000000000000, 0.8660254037844387076, 1.000000000000000000, 0.8660254037844387076, 1.000000000000000000, 0.8660254037844387076, 1.000000000000000000, 0.8660254037844387076, 1.000000000000000000, 0.8660254037844387076, 1.000000000000000000, 0.8660254037844387076, 1.000000000000000000, 0.8660254037844387076, 1.000000000000000000, 0.8660254037844387076, 1.000000000000000000, 0.8660254037844387076, 1.000000000000000000, 0.8660254037844387076, 1.000000000000000000, 0.8660254037844387076, 1.000000000000000000, 0.8660254037844387076, 1.000000000000000000, 0.8660254037844387076, 1.000000000000000000, 0.8660254037844387076, 1.000000000000000000, 0.8660254037844387076, 1.000000000000000000, 0.8660254037844387076, 1.000000000000000000, 0.8660254037844387076, 1.000000000000000000, 0.8660254037844387076, 1.000000000000000000, 0.8660254037844387076, 1.000000000000000000, 0.8660254037844387076, 1.000000000000000000, 0.8660254037844387076, 1.000000000000000000, 0.8660254037844387076, 1.000000000000000000, 0.8660254037844387076, 1.000000000000000000, 0.8660254037844387076, 1.000000000000000000, 0.8660254037844387076, 1.000000000000000000, 0.8660254037844387076, 1.000000000000000000, 0.8660254037844387076, 1.000000000000000000, 0.8660254037844387076, 1.000000000000000000, 0.8660254037844387076, 1.000000000000000000, 0.8660254037844387076, 1.000000000000000000, 0.8660254037844387076, 1.000000000000000000, 0.8660254037844387076, 1.000000000000000000, 0.8660254037844387076, 1.000000000000000000, 0.8660254037844387076, 1.000000000000000000, 0.8660254037844387076, 1.000000000000000000, 0.8660254037844387076, 1.000000000000000000, 0.8660254037844387076, 1.000000000000000000, 0.8660254037844387076, 1.000000000000000000, 0.8660254037844387076, 1.000000000000000000, 0.8660254037844387076, 1.000000000000000000, 0.8660254037844387076, 1.000000000000000000, 0.8660254037844387076, 1.000000000000000000, 0.8660254037844387076, 1.000000000000000000, 0.8660254037844387076, 1.000000000000000000, 0.8660254037844387076, 1.000000000000000000, 0.8660254037844387076, 1.000000000000000000, 0.8660254037844387076, 1.000000000000000000, 0.8660254037844387076, 1.000000000000000000, 0.8660254037844387076, 1.000000000000000000, 0.8660254037844387076, 1.000000000000000000, 0.8660254037844387076, 1.000000000000000000, 0.8660254037844387076, 1.000000000000000000, 0.8660254037844387076, 1.000000000000000000, 0.8660254037844387076, 1.000000000000000000, 0.8660254037844387076, 1.000000000000000000, 0.8660254037844387076, 1.000000000000000000, 0.8660254037844387076, 1.000000000000000000, 0.8660254037844387076, 1.000000000000000000, 0.8660254037844387076, 1.000000000000000000, 0.8660254037844387076, 1.000000000000000000, 0.8660254037844387076, 1.000000000000000000, 0.8660254037844387076, 1.000000000000000000, 0.8660254037844387076, 1.000000000000000000, 0.8660254037844387076, 1.000000000000000000, 0.8660254037844387076, 1.000000000000000000, 0.8660254037844387076, 1.000000000000000000, 0.8660254037844387076, 1.000000000000000000, 0.8660254037844387076, 1.000000000000000000, 0.8660254037844387076, 1.000000000000000000, 0.8660254037844387076, 1.000000000000000000, 0.8660254037844387076, 1.000000000000000000, 0.8660254037844387076, 1.000000000000000000, 0.8660254037844387076, 1.000000000000000000, 0.8660254037844387076, 1.000000000000000000, 0.8660254037844387076, 1.000000000000000000, 0.8660254037844387076, 1.000000000000000000, 0.8660254037844387076, 1.000000000000000000, 0.8660254037844387076, 1.000000000000000000, 0.8660254037844387076, 1.000000000000000000, 0.8660254037844387076, 1.000000000000000000, 0.8660254037844387076, 1.000000000000000000, 0.8660254037844387076, 1.000000000000000000, 0.8660254037844387076, 1.000000000000000000, 0.8660254037844387076, 1.000000000000000000, 0.8660254037844387076, 1.000000000000000000, 0.8660254037844387076, 1.000000000000000000, 0.8660254037844387076, 1.000000000000000000, 0.8660254037844387076, 1.000000000000000000, 0.8660254037844387076, 1.000000000000000000, 0.8660254037844387076, 1.000000000000000000, 0.8660254037844387076, 1.000000000000000000, 0.8660254037844387076, 1.000000000000000000, 0.8660254037844387076, 1.000000000000000000, 0.8660254037844387076, 1.000000000000000000, 0.8660254037844387076, 1.000000000000000000, 0.8660254037844387076, 1.000000000000000000, 0.8660254037844387076, 1.000000000000000000, 0.8660254037844387076, 1.000000000000000000, 0.8660254037844387076, 1.000000000000000000, 0.8660254037844387076, 1.000000000000000000, 0.8660254037844387076, 1.000000000000000000, 0.8660254037844387076, 1.000000000000000000, 0.8660254037844387076, 1.000000000000000000, 0.8660254037844387076, 1.000000000000000000, 0.8660254037844387076, 1.000000000000000000, 0.8660254037844387076, 1.000000000000000000, 0.8660254037844387076, 1.000000000000000000, 0.8660254037844387076, 1.000000000000000000, 0.8660254037844387076, 1.000000000000000000, 0.8660254037844387076, 1.000000000000000000, 0.8660254037844387076, 1.000000000000000000, 0.8660254037844387076, 1.000000000000000000, 0.8660254037844387076, 1.000000000000000000, 0.8660254037844387076, 1.000000000000000000, 0.8660254037844387076, 1.000000000000000000, 0.8660254037844387076, 1.000000000000000000, 0.8660254037844387076, 1.000000000000000000, 0.8660254037844387076, 1.000000000000000000, 0.8660254037844387076, 1.000000000000000000, 0.8660254037844387076, 1.000000000000000000, 0.8660254037844387076, 1.000000000000000000, 0.8660254037844387076, 1.000000000000000000, 0.8660254037844387076, 1.000000000000000000, 0.8660254037844387076, 1.000000000000000000, 0.8660254037844387076, 1.000000000000000000, 0.8660254037844387076, 1.000000000000000000, 0.8660254037844387076, 1.000000000000000000, 0.8660254037844387076, 1.000000000000000000, 0.8660254037844387076, 1.000000000000000000, 0.8660254037844387076, 1.000000000000000000, 0.8660254037844387076, 1.000000000000000000, 0.8660254037844387076, 1.000000000000000000, 0.8660254037844387076, 1.000000000000000000, 0.8660254037844387076, 1.000000000000000000, 0.8660254037844387076, 1.000000000000000000, 0.8660254037844387076, 1.000000000000000000, 0.8660254037844387076, 1.000000000000000000, 0.8660254037844387076, 1.000000000000000000, 0.8660254037844387076, 1.000000000000000000, 0.8660254037844387076, 1.000000000000000000, 0.8660254037844387076, 1.000000000000000000, 0.8660254037844387076, 1.000000000000000000, 0.8660254037844387076, 1.000000000000000000, 0.8660254037844387076, 1.000000000000000000, 0.8660254037844387076, 1.000000000000000000, 0.8660254037844387076, 1.000000000000000000, 0.8660254037844387076, 1.000000000000000000, 0.8660254037844387076, 1.000000000000000000, 0.8660254037844387076, 1.000000000000000000, 0.8660254037844387076, 1.000000000000000000, 0.8660254037844387076, 1.000000000000000000, 0.8660254037844387076, 1.000000000000000000, 0.8660254037844387076, 1.000000000000000000, 0.8660254037844387076, 1.000000000000000000, 0.8660254037844387076, 1.000000000000000000, 0.8660254037844387076, 1.000000000000000000, 0.8660254037844387076, 1.000000000000000000, 0.8660254037844387076, 1.000000000000000000, 0.8660254037844387076, 1.000000000000000000, 0.8660254037844387076, 1.000000000000000000, 0.8660254037844387076, 1.000000000000000000, 0.8660254037844387076, 1.000000000000000000, 0.8660254037844387076, 1.000000000000000000, 0.8660254037844387076, 1.000000000000000000, 0.8660254037844387076, 1.000000000000000000, 0.8660254037844387076, 1.000000000000000000, 0.8660254037844387076, 1.000000000000000000, 0.8660254037844387076, 1.000000000000000000, 0.8660254037844387076, 1.000000000000000000, 0.8660254037844387076, 1.000000000000000000, 0.8660254037844387076, 1.000000000000000000, 0.8660254037844387076, 1.000000000000000000, 0.8660254037844387076, 1.000000000000000000, 0.8660254037844387076, 1.000000000000000000, 0.8660254037844387076, 1.000000000000000000, 0.8660254037844387076, 1.000000000000000000, 0.8660254037844387076, 1.000000000000000000, 0.8660254037844387076, 1.000000000000000000, 0.8660254037844387076, 1.000000000000000000, 0.8660254037844387076, 1.000000000000000000, 0.8660254037844387076, 1.000000000000000000, 0.8660254037844387076, 1.000000000000000000, 0.8660254037844387076, 1.000000000000000000, 0.8660254037844387076, 1.000000000000000000, 0.8660254037844387076, 1.000000000000000000, 0.8660254037844387076, 1.000000000000000000, 0.8660254037844387076, 1.000000000000000000, 0.8660254037844387076, 1.000000000000000000, 0.8660254037844387076, 1.000000000000000000, 0.8660254037844387076, 1.000000000000000000, 0.8660254037844387076, 1.000000000000000000, 0.8660254037844387076, 1.000000000000000000, 0.8660254037844387076, 1.000000000000000000, 0.8660254037844387076, 1.000000000000000000, 0.8660254037844387076, 1.000000000000000000, 0.8660254037844387076, 1.000000000000000000, 0.8660254037844387076, 1.000000000000000000, 0.8660254037844387076, 1.000000000000000000, 0.8660254037844387076, 1.000000000000000000, 0.8660254037844387076, 1.000000000000000000, 0.8660254037844387076, 1.000000000000000000, 0.8660254037844387076, 1.000000000000000000, 0.8660254037844387076, 1.000000000000000000, 0.8660254037844387076, 1.000000000000000000, 0.8660254037844387076, 1.000000000000000000, 0.8660254037844387076, 1.000000000000000000, 0.8660254037844387076, 1.000000000000000000, 0.8660254037844387076, 1.000000000000000000, 0.8660254037844387076, 1.000000000000000000, 0.8660254037844387076, 1.000000000000000000, 0.8660254037844387076, 1.000000000000000000, 0.8660254037844387076, 1.000000000000000000, 0.8660254037844387076, 1.000000000000000000, 0.8660254037844387076, 1.000000000000000000, 0.8660254037844387076, 1.000000000000000000, 0.8660254037844387076, 1.000000000000000000, 0.8660254037844387076, 1.000000000000000000, 0.8660254037844387076, 1.000000000000000000, 0.8660254037844387076, 1.000000000000000000, 0.8660254037844387076, 1.000000000000000000, 0.8660254037844387076, 1.000000000000000000, 0.8660254037844387076, 1.000000000000000000, 0.8660254037844387076, 1.000000000000000000, 0.8660254037844387076, 1.000000000000000000, 0.8660254037844387076, 1.000000000000000000, 0.8660254037844387076, 1.000000000000000000, 0.8660254037844387076, 1.000000000000000000, 0.8660254037844387076, 1.000000000000000000, 0.8660254037844387076, 1.000000000000000000, 0.8660254037844387076, 1.000000000000000000, 0.8660254037844387076, 1.000000000000000000, 0.8660254037844387076, 1.000000000000000000, 0.8660254037844387076, 1.000000000000000000, 0.8660254037844387076, 1.000000000000000000, 0.8660254037844387076, 1.000000000000000000, 0.8660254037844387076, 1.000000000000000000, 0.8660254037844387076, 1.000000000000000000, 0.8660254037844387076, 1.000000000000000000, 0.8660254037844387076, 1.000000000000000000, 0.8660254037844387076, 1.000000000000000000, 0.8660254037844387076, 1.000000000000000000, 0.8660254037844387076, 1.000000000000000000, 0.8660254037844387076, 1.000000000000000000, 0.8660254037844387076, 1.000000000000000000, 0.8660254037844387076, 1.000000000000000000, 0.8660254037844387076, 1.000000000000000000, 0.8660254037844387076, 1.000000000000000000, 0.8660254037844387076, 1.000000000000000000, 0.8660254037844387076, 1.000000000000000000, 0.8660254037844387076, 1.000000000000000000, 0.8660254037844387076, 1.000000000000000000, 0.8660254037844387076, 1.000000000000000000, 0.8660254037844387076, 1.000000000000000000, 0.8660254037844387076, 1.000000000000000000, 0.8660254037844387076, 1.000000000000000000, 0.8660254037844387076, 1.000000000000000000, 0.8660254037844387076, 1.000000000000000000, 0.8660254037844387076, 1.000000000000000000, 0.8660254037844387076, 1.000000000000000000, 0.8660254037844387076, 1.000000000000000000, 0.8660254037844387076, 1.000000000000000000, 0.8660254037844387076, 1.000000000000000000, 0.8660254037844387076, 1.000000000000000000, 0.8660254037844387076, 1.000000000000000000, 0.8660254037844387076, 1.000000000000000000, 0.8660254037844387076, 1.000000000000000000, 0.8660254037844387076, 1.000000000000000000, 0.8660254037844387076, 1.000000000000000000, 0.8660254037844387076, 1.000000000000000000, 0.8660254037844387076, 1.000000000000000000, 0.8660254037844387076, 1.000000000000000000, 0.8660254037844387076, 1.000000000000000000, 0.8660254037844387076, 1.000000000000000000, 0.8660254037844387076, 1.000000000000000000, 0.8660254037844387076, 1.000000000000000000, 0.8660254037844387076, 1.000000000000000000, 0.8660254037844387076, 1.000000000000000000, 0.8660254037844387076, 1.000000000000000000, 0.8660254037844387076, 1.000000000000000000, 0.8660254037844387076, 1.000000000000000000, 0.8660254037844387076, 1.000000000000000000, 0.8660254037844387076, 1.000000000000000000, 0.8660254037844387076, 1.000000000000000000, 0.8660254037844387076, 1.000000000000000000, 0.8660254037844387076, 1.000000000000000000, 0.8660254037844387076, 1.000000000000000000, 0.8660254037844387076, 1.000000000000000000, 0.8660254037844387076, 1.000000000000000000, 0.8660254037844387076, 1.000000000000000000, 0.8660254037844387076, 1.000000000000000000, 0.8660254037844387076, 1.000000000000000000, 0.8660254037844387076, 1.000000000000000000, 0.8660254037844387076, 1.000000000000000000, 0.8660254037844387076, 1.000000000000000000, 0.8660254037844387076, 1.000000000000000000, 0.8660254037844387076, 1.000000000000000000, 0.8660254037844387076, 1.000000000000000000, 0.8660254037844387076, 1.000000000000000000, 0.8660254037844387076, 1.000000000000000000, 0.8660254037844387076, 1.000000000000000000, 0.8660254037844387076, 1.000000000000000000, 0.8660254037844387076, 1.000000000000000000, 0.8660254037844387076, 1.000000000000000000, 0.8660254037844387076, 1.000000000000000000, 0.8660254037844387076, 1.000000000000000000, 0.8660254037844387076, 1.000000000000000000, 0.8660254037844387076, 1.000000000000000000, 0.8660254037844387076, 1.000000000000000000, 0.8660254037844387076, 1.000000000000000000, 0.8660254037844387076, 1.000000000000000000, 0.8660254037844387076, 1.000000000000000000, 0.8660254037844387076, 1.000000000000000000, 0.8660254037844387076, 1.000000000000000000, 0.8660254037844387076, 1.000000000000000000, 0.8660254037844387076, 1.000000000000000000, 0.8660254037844387076, 1.000000000000000000, 0.8660254037844387076, 1.000000000000000000, 0.8660254037844387076, 1.000000000000000000, 0.8660254037844387076, 1.000000000000000000, 0.8660254037844387076, 1.000000000000000000, 0.8660254037844387076, 1.000000000000000000, 0.8660254037844387076, 1.000000000000000000, 0.8660254037844387076, 1.000000000000000000, 0.8660254037844387076, 1.000000000000000000, 0.8660254037844387076, 1.000000000000000000, 0.8660254037844387076, 1.000000000000000000, 0.8660254037844387076, 1.000000000000000000, 0.8660254037844387076, 1.000000000000000000, 0.8660254037844387076, 1.000000000000000000, 0.8660254037844387076, 1.000000000000000000, 0.8660254037844387076, 1.000000000000000000, 0.8660254037844387076, 1.000000000000000000, 0.8660254037844387076, 1.000000000000000000, 0.8660254037844387076, 1.000000000000000000, 0.8660254037844387076, 1.000000000000000000, 0.8660254037844387076, 1.000000000000000000, 0.8660254037844387076, 1.000000000000000000, 0.8660254037844387076, 1.000000000000000000, 0.8660254037844387076, 1.000000000000000000, 0.8660254037844387076, 1.000000000000000000, 0.8660254037844387076, 1.000000000000000000, 0.8660254037844387076, 1.000000000000000000, 0.8660254037844387076, 1.000000000000000000, 0.8660254037844387076, 1.000000000000000000, 0.8660254037844387076, 1.000000000000000000, 0.8660254037844387076, 1.000000000000000000, 0.8660254037844387076, 1.000000000000000000, 0.8660254037844387076, 1.000000000000000000, 0.8660254037844387076, 1.000000000000000000, 0.8660254037844387076, 1.000000000000000000, 0.8660254037844387076, 1.000000000000000000, 0.8660254037844387076, 1.000000000000000000, 0.8660254037844387076, 1.000000000000000000, 0.8660254037844387076, 1.000000000000000000, 0.8660254037844387076, 1.000000000000000000, 0.8660254037844387076, 1.000000000000000000, 0.8660254037844387076, 1.000000000000000000, 0.8660254037844387076, 1.000000000000000000, 0.8660254037844387076, 1.000000000000000000, 0.8660254037844387076, 1.000000000000000000, 0.8660254037844387076, 1.000000000000000000, 0.8660254037844387076, 1.000000000000000000, 0.8660254037844387076, 1.000000000000000000, 0.8660254037844387076, 1.000000000000000000, 0.8660254037844387076, 1.000000000000000000, 0.8660254037844387076, 1.000000000000000000, 0.8660254037844387076, 1.000000000000000000, 0.8660254037844387076, 1.000000000000000000, 0.8660254037844387076, 1.000000000000000000, 0.8660254037844387076, 1.000000000000000000, 0.8660254037844387076, 1.000000000000000000, 0.8660254037844387076, 1.000000000000000000, 0.8660254037844387076, 1.000000000000000000, 0.8660254037844387076, 1.000000000000000000, 0.8660254037844387076, 1.000000000000000000, 0.8660254037844387076, 1.000000000000000000, 0.8660254037844387076, 1.000000000000000000, 0.8660254037844387076, 1.000000000000000000, 0.8660254037844387076, 1.000000000000000000, 0.8660254037844387076, 1.000000000000000000, 0.8660254037844387076, 1.000000000000000000, 0.8660254037844387076, 1.000000000000000000, 0.8660254037844387076, 1.000000000000000000, 0.8660254037844387076, 1.000000000000000000, 0.8660254037844387076, 1.000000000000000000, 0.8660254037844387076, 1.000000000000000000, 0.8660254037844387076, 1.000000000000000000, 0.8660254037844387076, 1.000000000000000000, 0.8660254037844387076, 1.000000000000000000, 0.8660254037844387076, 1.000000000000000000, 0.8660254037844387076, 1.000000000000000000, 0.8660254037844387076, 1.000000000000000000, 0.8660254037844387076, 1.000000000000000000, 0.8660254037844387076, 1.000000000000000000, 0.8660254037844387076, 1.000000000000000000, 0.8660254037844387076, 1.000000000000000000, 0.8660254037844387076, 1.000000000000000000, 0.8660254037844387076, 1.000000000000000000, 0.8660254037844387076, 1.000000000000000000, 0.8660254037844387076, 1.000000000000000000, 0.8660254037844387076, 1.000000000000000000, 0.8660254037844387076, 1.000000000000000000, 0.8660254037844387076, 1.000000000000000000, 0.8660254037844387076, 1.000000000000000000, 0.8660254037844387076, 1.000000000000000000, 0.8660254037844387076, 1.000000000000000000, 0.8660254037844387076, 1.000000000000000000, 0.8660254037844387076, 1.000000000000000000, 0.8660254037844387076, 1.000000000000000000, 0.8660254037844387076, 1.000000000000000000, 0.8660254037844387076, 1.000000000000000000, 0.8660254037844387076, 1.000000000000000000, 0.8660254037844387076, 1.000000000000000000, 0.8660254037844387076, 1.000000000000000000, 0.8660254037844387076, 1.000000000000000000, 0.8660254037844387076, 1.000000000000000000, 0.8660254037844387076, 1.000000000000000000, 0.8660254037844387076, 1.000000000000000000, 0.8660254037844387076, 1.000000000000000000, 0.8660254037844387076, 1.000000000000000000, 0.8660254037844387076, 1.000000000000000000, 0.8660254037844387076, 1.000000000000000000, 0.8660254037844387076, 1.000000000000000000, 0.8660254037844387076, 1.000000000000000000, 0.8660254037844387076, 1.000000000000000000, 0.8660254037844387076, 1.000000000000000000, 0.8660254037844387076, 1.000000000000000000, 0.8660254037844387076, 1.000000000000000000, 0.8660254037844387076, 1.000000000000000000, 0.8660254037844387076, 1.000000000000000000, 0.8660254037844387076, 1.000000000000000000, 0.8660254037844387076, 1.000000000000000000, 0.8660254037844387076, 1.000000000000000000, 0.8660254037844387076, 1.000000000000000000, 0.8660254037844387076, 1.000000000000000000, 0.8660254037844387076, 1.000000000000000000, 0.8660254037844387076, 1.000000000000000000, 0.8660254037844387076, 1.000000000000000000, 0.8660254037844387076, 1.000000000000000000, 0.8660254037844387076, 1.000000000000000000, 0.8660254037844387076, 1.000000000000000000, 0.8660254037844387076, 1.000000000000000000, 0.8660254037844387076, 1.000000000000000000, 0.8660254037844387076, 1.000000000000000000, 0.8660254037844387076, 1.000000000000000000, 0.8660254037844387076, 1.000000000000000000, 0.8660254037844387076, 1.000000000000000000, 0.8660254037844387076, 1.000000000000000000, 0.8660254037844387076, 1.000000000000000000, 0.8660254037844387076, 1.000000000000000000, 0.8660254037844387076, 1.000000000000000000, 0.8660254037844387076, 1.000000000000000000, 0.8660254037844387076, 1.000000000000000000, 0.8660254037844387076, 1.000000000000000000, 0.8660254037844387076, 1.000000000000000000, 0.8660254037844387076, 1.000000000000000000, 0.8660254037844387076, 1.000000000000000000, 0.8660254037844387076, 1.000000000000000000, 0.8660254037844387076, 1.000000000000000000, 0.8660254037844387076, 1.000000000000000000, 0.8660254037844387076, 1.000000000000000000, 0.8660254037844387076, 1.000000000000000000, 0.8660254037844387076, 1.000000000000000000, 0.8660254037844387076, 1.000000000000000000, 0.8660254037844387076, 1.000000000000000000, 0.8660254037844387076, 1.000000000000000000, 0.8660254037844387076, 1.000000000000000000, 0.8660254037844387076, 1.000000000000000000, 0.8660254037844387076, 1.000000000000000000, 0.8660254037844387076, 1.000000000000000000, 0.8660254037844387076, 1.000000000000000000, 0.8660254037844387076, 1.000000000000000000, 0.8660254037844387076, 1.000000000000000000, 0.8660254037844387076, 1.000000000000000000, 0.8660254037844387076, 1.000000000000000000, 0.8660254037844387076, 1.000000000000000000, 0.8660254037844387076, 1.000000000000000000, 0.8660254037844387076, 1.000000000000000000, 0.8660254037844387076, 1.000000000000000000, 0.8660254037844387076, 1.000000000000000000, 0.8660254037844387076, 1.000000000000000000, 0.8660254037844387076, 1.000000000000000000, 0.8660254037844387076, 1.000000000000000000, 0.8660254037844387076, 1.000000000000000000, 0.8660254037844387076, 1.000000000000000000, 0.8660254037844387076, 1.000000000000000000, 0.8660254037844387076, 1.000000000000000000, 0.8660254037844387076, 1.000000000000000000, 0.8660254037844387076, 1.000000000000000000, 0.8660254037844387076, 1.000000000000000000, 0.8660254037844387076, 1.000000000000000000, 0.8660254037844387076, 1.000000000000000000, 0.8660254037844387076, 1.000000000000000000, 0.8660254037844387076, 1.000000000000000000, 0.8660254037844387076, 1.000000000000000000, 0.8660254037844387076, 1.000000000000000000, 0.8660254037844387076, 1.000000000000000000, 0.8660254037844387076, 1.000000000000000000, 0.8660254037844387076, 1.000000000000000000, 0.8660254037844387076, 1.000000000000000000, 0.8660254037844387076, 1.000000000000000000, 0.8660254037844387076, 1.000000000000000000, 0.8660254037844387076, 1.000000000000000000, 0.8660254037844387076, 1.000000000000000000, 0.8660254037844387076, 1.000000000000000000, 0.8660254037844387076, 1.000000000000000000, 0.8660254037844387076, 1.000000000000000000, 0.8660254037844387076, 1.000000000000000000, 0.8660254037844387076, 1.000000000000000000, 0.8660254037844387076, 1.000000000000000000, 0.8660254037844387076, 1.000000000000000000, 0.8660254037844387076, 1.000000000000000000, 0.8660254037844387076, 1.000000000000000000, 0.8660254037844387076, 1.000000000000000000, 0.8660254037844387076, 1.000000000000000000, 0.8660254037844387076, 1.000000000000000000, 0.8660254037844387076, 1.000000000000000000, 0.8660254037844387076, 1.000000000000000000, 0.8660254037844387076, 1.000000000000000000, 0.8660254037844387076, 1.000000000000000000, 0.8660254037844387076, 1.000000000000000000, 0.8660254037844387076, 1.000000000000000000, 0.8660254037844387076, 1.000000000000000000, 0.8660254037844387076, 1.000000000000000000, 0.8660254037844387076, 1.000000000000000000, 0.8660254037844387076, 1.000000000000000000, 0.8660254037844387076, 1.000000000000000000, 0.8660254037844387076, 1.000000000000000000, 0.8660254037844387076, 1.000000000000000000, 0.8660254037844387076, 1.000000000000000000, 0.8660254037844387076, 1.000000000000000000, 0.8660254037844387076, 1.000000000000000000, 0.8660254037844387076, 1.000000000000000000, 0.8660254037844387076, 1.000000000000000000, 0.8660254037844387076, 1.000000000000000000, 0.8660254037844387076, 1.000000000000000000, 0.8660254037844387076, 1.000000000000000000, 0.8660254037844387076, 1.000000000000000000, 0.8660254037844387076, 1.000000000000000000, 0.8660254037844387076, 1.000000000000000000, 0.8660254037844387076, 1.000000000000000000, 0.8660254037844387076, 1.000000000000000000, 0.8660254037844387076, 1.000000000000000000, 0.8660254037844387076, 1.000000000000000000, 0.8660254037844387076, 1.000000000000000000, 0.8660254037844387076, 1.000000000000000000, 0.8660254037844387076, 1.000000000000000000, 0.8660254037844387076, 1.000000000000000000, 0.8660254037844387076, 1.000000000000000000, 0.8660254037844387076, 1.000000000000000000, 0.8660254037844387076, 1.000000000000000000, 0.8660254037844387076, 1.000000000000000000, 0.8660254037844387076, 1.000000000000000000, 0.8660254037844387076, 1.000000000000000000, 0.8660254037844387076, 1.000000000000000000, 0.8660254037844387076, 1.000000000000000000, 0.8660254037844387076, 1.000000000000000000, 0.8660254037844387076, 1.000000000000000000, 0.8660254037844387076, 1.000000000000000000, 0.8660254037844387076, 1.000000000000000000, 0.8660254037844387076, 1.000000000000000000, 0.8660254037844387076, 1.000000000000000000, 0.8660254037844387076, 1.000000000000000000, 0.8660254037844387076, 1.000000000000000000, 0.8660254037844387076, 1.000000000000000000, 0.8660254037844387076, 1.000000000000000000, 0.8660254037844387076, 1.000000000000000000, 0.8660254037844387076, 1.000000000000000000, 0.8660254037844387076, 1.000000000000000000, 0.8660254037844387076, 1.000000000000000000),
 ( 1.000000000000000000, 0.8660254037844387076, 1.000000000000000000, 0.8660254037844387076, 1.000000000000000000, 0.8660254037844387076, 1.000000000000000000, 0.8660254037844387076, 1.000000000000000000, 0.8660254037844387076, 1.000000000000000000, 0.8660254037844387076, 1.000000000000000000, 0.8660254037844387076, 1.000000000000000000, 0.8660254037844387076, 1.000000000000000000, 0.8660254037844387076, 1.000000000000000000, 0.8660254037844387076, 1.000000000000000000, 0.8660254037844387076, 1.000000000000000000, 0.8660254037844387076, 1.000000000000000000, 0.8660254037844387076, 1.000000000000000000, 0.8660254037844387076, 1.000000000000000000, 0.8660254037844387076, 1.000000000000000000, 0.8660254037844387076, 1.000000000000000000, 0.8660254037844387076, 1.000000000000000000, 0.8660254037844387076, 1.000000000000000000, 0.8660254037844387076, 1.000000000000000000, 0.8660254037844387076, 1.000000000000000000, 0.8660254037844387076, 1.000000000000000000, 0.8660254037844387076, 1.000000000000000000, 0.8660254037844387076, 1.000000000000000000, 0.8660254037844387076, 1.000000000000000000, 0.8660254037844387076, 1.000000000000000000, 0.8660254037844387076, 1.000000000000000000, 0.8660254037844387076, 1.000000000000000000, 0.8660254037844387076, 1.000000000000000000, 0.8660254037844387076, 1.000000000000000000, 0.8660254037844387076, 1.000000000000000000, 0.8660254037844387076, 1.000000000000000000, 0.8660254037844387076, 1.000000000000000000, 0.8660254037844387076, 1.000000000000000000, 0.8660254037844387076, 1.000000000000000000, 0.8660254037844387076, 1.000000000000000000, 0.8660254037844387076, 1.000000000000000000, 0.8660254037844387076, 1.000000000000000000, 0.8660254037844387076, 1.000000000000000000, 0.8660254037844387076, 1.000000000000000000, 0.8660254037844387076, 1.000000000000000000, 0.8660254037844387076, 1.000000000000000000, 0.8660254037844387076, 1.000000000000000000, 0.8660254037844387076, 1.000000000000000000, 0.8660254037844387076, 1.000000000000000000, 0.8660254037844387076, 1.000000000000000000, 0.8660254037844387076, 1.000000000000000000, 0.8660254037844387076, 1.000000000000000000, 0.8660254037844387076, 1.000000000000000000, 0.8660254037844387076, 1.000000000000000000, 0.8660254037844387076, 1.000000000000000000, 0.8660254037844387076, 1.000000000000000000, 0.8660254037844387076, 1.000000000000000000, 0.8660254037844387076, 1.000000000000000000, 0.8660254037844387076, 1.000000000000000000, 0.8660254037844387076, 1.000000000000000000, 0.8660254037844387076, 1.000000000000000000, 0.8660254037844387076, 1.000000000000000000, 0.8660254037844387076, 1.000000000000000000, 0.8660254037844387076, 1.000000000000000000, 0.8660254037844387076, 1.000000000000000000, 0.8660254037844387076, 1.000000000000000000, 0.8660254037844387076, 1.000000000000000000, 0.8660254037844387076, 1.000000000000000000, 0.8660254037844387076, 1.000000000000000000, 0.8660254037844387076, 1.000000000000000000, 0.8660254037844387076, 1.000000000000000000, 0.8660254037844387076, 1.000000000000000000, 0.8660254037844387076, 1.000000000000000000, 0.8660254037844387076, 1.000000000000000000, 0.8660254037844387076, 1.000000000000000000, 0.8660254037844387076, 1.000000000000000000, 0.8660254037844387076, 1.000000000000000000, 0.8660254037844387076, 1.000000000000000000, 0.8660254037844387076, 1.000000000000000000, 0.8660254037844387076, 1.000000000000000000, 0.8660254037844387076, 1.000000000000000000, 0.8660254037844387076, 1.000000000000000000, 0.8660254037844387076, 1.000000000000000000, 0.8660254037844387076, 1.000000000000000000, 0.8660254037844387076, 1.000000000000000000, 0.8660254037844387076, 1.000000000000000000, 0.8660254037844387076, 1.000000000000000000, 0.8660254037844387076, 1.000000000000000000, 0.8660254037844387076, 1.000000000000000000, 0.8660254037844387076, 1.000000000000000000, 0.8660254037844387076, 1.000000000000000000, 0.8660254037844387076, 1.000000000000000000, 0.8660254037844387076, 1.000000000000000000, 0.8660254037844387076, 1.000000000000000000, 0.8660254037844387076, 1.000000000000000000, 0.8660254037844387076, 1.000000000000000000, 0.8660254037844387076, 1.000000000000000000, 0.8660254037844387076, 1.000000000000000000, 0.8660254037844387076, 1.000000000000000000, 0.8660254037844387076, 1.000000000000000000, 0.8660254037844387076, 1.000000000000000000, 0.8660254037844387076, 1.000000000000000000, 0.8660254037844387076, 1.000000000000000000, 0.8660254037844387076, 1.000000000000000000, 0.8660254037844387076, 1.000000000000000000, 0.8660254037844387076, 1.000000000000000000, 0.8660254037844387076, 1.000000000000000000, 0.8660254037844387076, 1.000000000000000000, 0.8660254037844387076, 1.000000000000000000, 0.8660254037844387076, 1.000000000000000000, 0.8660254037844387076, 1.000000000000000000, 0.8660254037844387076, 1.000000000000000000, 0.8660254037844387076, 1.000000000000000000, 0.8660254037844387076, 1.000000000000000000, 0.8660254037844387076, 1.000000000000000000, 0.8660254037844387076, 1.000000000000000000, 0.8660254037844387076, 1.000000000000000000, 0.8660254037844387076, 1.000000000000000000, 0.8660254037844387076, 1.000000000000000000, 0.8660254037844387076, 1.000000000000000000, 0.8660254037844387076, 1.000000000000000000, 0.8660254037844387076, 1.000000000000000000, 0.8660254037844387076, 1.000000000000000000, 0.8660254037844387076, 1.000000000000000000, 0.8660254037844387076, 1.000000000000000000, 0.8660254037844387076, 1.000000000000000000, 0.8660254037844387076, 1.000000000000000000, 0.8660254037844387076, 1.000000000000000000, 0.8660254037844387076, 1.000000000000000000, 0.8660254037844387076, 1.000000000000000000, 0.8660254037844387076, 1.000000000000000000, 0.8660254037844387076, 1.000000000000000000, 0.8660254037844387076, 1.000000000000000000, 0.8660254037844387076, 1.000000000000000000, 0.8660254037844387076, 1.000000000000000000, 0.8660254037844387076, 1.000000000000000000, 0.8660254037844387076, 1.000000000000000000, 0.8660254037844387076, 1.000000000000000000, 0.8660254037844387076, 1.000000000000000000, 0.8660254037844387076, 1.000000000000000000, 0.8660254037844387076, 1.000000000000000000, 0.8660254037844387076, 1.000000000000000000, 0.8660254037844387076, 1.000000000000000000, 0.8660254037844387076, 1.000000000000000000, 0.8660254037844387076, 1.000000000000000000, 0.8660254037844387076, 1.000000000000000000, 0.8660254037844387076, 1.000000000000000000, 0.8660254037844387076, 1.000000000000000000, 0.8660254037844387076, 1.000000000000000000, 0.8660254037844387076, 1.000000000000000000, 0.8660254037844387076, 1.000000000000000000, 0.8660254037844387076, 1.000000000000000000, 0.8660254037844387076, 1.000000000000000000, 0.8660254037844387076, 1.000000000000000000, 0.8660254037844387076, 1.000000000000000000, 0.8660254037844387076, 1.000000000000000000, 0.8660254037844387076, 1.000000000000000000, 0.8660254037844387076, 1.000000000000000000, 0.8660254037844387076, 1.000000000000000000, 0.8660254037844387076, 1.000000000000000000, 0.8660254037844387076, 1.000000000000000000, 0.8660254037844387076, 1.000000000000000000, 0.8660254037844387076, 1.000000000000000000, 0.8660254037844387076, 1.000000000000000000, 0.8660254037844387076, 1.000000000000000000, 0.8660254037844387076, 1.000000000000000000, 0.8660254037844387076, 1.000000000000000000, 0.8660254037844387076, 1.000000000000000000, 0.8660254037844387076, 1.000000000000000000, 0.8660254037844387076, 1.000000000000000000, 0.8660254037844387076, 1.000000000000000000, 0.8660254037844387076, 1.000000000000000000, 0.8660254037844387076, 1.000000000000000000, 0.8660254037844387076, 1.000000000000000000, 0.8660254037844387076, 1.000000000000000000, 0.8660254037844387076, 1.000000000000000000, 0.8660254037844387076, 1.000000000000000000, 0.8660254037844387076, 1.000000000000000000, 0.8660254037844387076, 1.000000000000000000, 0.8660254037844387076, 1.000000000000000000, 0.8660254037844387076, 1.000000000000000000, 0.8660254037844387076, 1.000000000000000000, 0.8660254037844387076, 1.000000000000000000, 0.8660254037844387076, 1.000000000000000000, 0.8660254037844387076, 1.000000000000000000, 0.8660254037844387076, 1.000000000000000000, 0.8660254037844387076, 1.000000000000000000, 0.8660254037844387076, 1.000000000000000000, 0.8660254037844387076, 1.000000000000000000, 0.8660254037844387076, 1.000000000000000000, 0.8660254037844387076, 1.000000000000000000, 0.8660254037844387076, 1.000000000000000000, 0.8660254037844387076, 1.000000000000000000, 0.8660254037844387076, 1.000000000000000000, 0.8660254037844387076, 1.000000000000000000, 0.8660254037844387076, 1.000000000000000000, 0.8660254037844387076, 1.000000000000000000, 0.8660254037844387076, 1.000000000000000000, 0.8660254037844387076, 1.000000000000000000, 0.8660254037844387076, 1.000000000000000000, 0.8660254037844387076, 1.000000000000000000, 0.8660254037844387076, 1.000000000000000000, 0.8660254037844387076, 1.000000000000000000, 0.8660254037844387076, 1.000000000000000000, 0.8660254037844387076, 1.000000000000000000, 0.8660254037844387076, 1.000000000000000000, 0.8660254037844387076, 1.000000000000000000, 0.8660254037844387076, 1.000000000000000000, 0.8660254037844387076, 1.000000000000000000, 0.8660254037844387076, 1.000000000000000000, 0.8660254037844387076, 1.000000000000000000, 0.8660254037844387076, 1.000000000000000000, 0.8660254037844387076, 1.000000000000000000, 0.8660254037844387076, 1.000000000000000000, 0.8660254037844387076, 1.000000000000000000, 0.8660254037844387076, 1.000000000000000000, 0.8660254037844387076, 1.000000000000000000, 0.8660254037844387076, 1.000000000000000000, 0.8660254037844387076, 1.000000000000000000, 0.8660254037844387076, 1.000000000000000000, 0.8660254037844387076, 1.000000000000000000, 0.8660254037844387076, 1.000000000000000000, 0.8660254037844387076, 1.000000000000000000, 0.8660254037844387076, 1.000000000000000000, 0.8660254037844387076, 1.000000000000000000, 0.8660254037844387076, 1.000000000000000000, 0.8660254037844387076, 1.000000000000000000, 0.8660254037844387076, 1.000000000000000000, 0.8660254037844387076, 1.000000000000000000, 0.8660254037844387076, 1.000000000000000000, 0.8660254037844387076, 1.000000000000000000, 0.8660254037844387076, 1.000000000000000000, 0.8660254037844387076, 1.000000000000000000, 0.8660254037844387076, 1.000000000000000000, 0.8660254037844387076, 1.000000000000000000, 0.8660254037844387076, 1.000000000000000000, 0.8660254037844387076, 1.000000000000000000, 0.8660254037844387076, 1.000000000000000000, 0.8660254037844387076, 1.000000000000000000, 0.8660254037844387076, 1.000000000000000000, 0.8660254037844387076, 1.000000000000000000, 0.8660254037844387076, 1.000000000000000000, 0.8660254037844387076, 1.000000000000000000, 0.8660254037844387076, 1.000000000000000000, 0.8660254037844387076, 1.000000000000000000, 0.8660254037844387076, 1.000000000000000000, 0.8660254037844387076, 1.000000000000000000, 0.8660254037844387076, 1.000000000000000000, 0.8660254037844387076, 1.000000000000000000, 0.8660254037844387076, 1.000000000000000000, 0.8660254037844387076, 1.000000000000000000, 0.8660254037844387076, 1.000000000000000000, 0.8660254037844387076, 1.000000000000000000, 0.8660254037844387076, 1.000000000000000000, 0.8660254037844387076, 1.000000000000000000, 0.8660254037844387076, 1.000000000000000000, 0.8660254037844387076, 1.000000000000000000, 0.8660254037844387076, 1.000000000000000000, 0.8660254037844387076, 1.000000000000000000, 0.8660254037844387076, 1.000000000000000000, 0.8660254037844387076, 1.000000000000000000, 0.8660254037844387076, 1.000000000000000000, 0.8660254037844387076, 1.000000000000000000, 0.8660254037844387076, 1.000000000000000000, 0.8660254037844387076, 1.000000000000000000, 0.8660254037844387076, 1.000000000000000000, 0.8660254037844387076, 1.000000000000000000, 0.8660254037844387076, 1.000000000000000000, 0.8660254037844387076, 1.000000000000000000, 0.8660254037844387076, 1.000000000000000000, 0.8660254037844387076, 1.000000000000000000, 0.8660254037844387076, 1.000000000000000000, 0.8660254037844387076, 1.000000000000000000, 0.8660254037844387076, 1.000000000000000000, 0.8660254037844387076, 1.000000000000000000, 0.8660254037844387076, 1.000000000000000000, 0.8660254037844387076, 1.000000000000000000, 0.8660254037844387076, 1.000000000000000000, 0.8660254037844387076, 1.000000000000000000, 0.8660254037844387076, 1.000000000000000000, 0.8660254037844387076, 1.000000000000000000, 0.8660254037844387076, 1.000000000000000000, 0.8660254037844387076, 1.000000000000000000, 0.8660254037844387076, 1.000000000000000000, 0.8660254037844387076, 1.000000000000000000, 0.8660254037844387076, 1.000000000000000000, 0.8660254037844387076, 1.000000000000000000, 0.8660254037844387076, 1.000000000000000000, 0.8660254037844387076, 1.000000000000000000, 0.8660254037844387076, 1.000000000000000000, 0.8660254037844387076, 1.000000000000000000, 0.8660254037844387076, 1.000000000000000000, 0.8660254037844387076, 1.000000000000000000, 0.8660254037844387076, 1.000000000000000000, 0.8660254037844387076, 1.000000000000000000, 0.8660254037844387076, 1.000000000000000000, 0.8660254037844387076, 1.000000000000000000, 0.8660254037844387076, 1.000000000000000000, 0.8660254037844387076, 1.000000000000000000, 0.8660254037844387076, 1.000000000000000000, 0.8660254037844387076, 1.000000000000000000, 0.8660254037844387076, 1.000000000000000000, 0.8660254037844387076, 1.000000000000000000, 0.8660254037844387076, 1.000000000000000000, 0.8660254037844387076, 1.000000000000000000, 0.8660254037844387076, 1.000000000000000000, 0.8660254037844387076, 1.000000000000000000, 0.8660254037844387076, 1.000000000000000000, 0.8660254037844387076, 1.000000000000000000, 0.8660254037844387076, 1.000000000000000000, 0.8660254037844387076, 1.000000000000000000, 0.8660254037844387076, 1.000000000000000000, 0.8660254037844387076, 1.000000000000000000, 0.8660254037844387076, 1.000000000000000000, 0.8660254037844387076, 1.000000000000000000, 0.8660254037844387076, 1.000000000000000000, 0.8660254037844387076, 1.000000000000000000, 0.8660254037844387076, 1.000000000000000000, 0.8660254037844387076, 1.000000000000000000, 0.8660254037844387076, 1.000000000000000000, 0.8660254037844387076, 1.000000000000000000, 0.8660254037844387076, 1.000000000000000000, 0.8660254037844387076, 1.000000000000000000, 0.8660254037844387076, 1.000000000000000000, 0.8660254037844387076, 1.000000000000000000, 0.8660254037844387076, 1.000000000000000000, 0.8660254037844387076, 1.000000000000000000, 0.8660254037844387076, 1.000000000000000000, 0.8660254037844387076, 1.000000000000000000, 0.8660254037844387076, 1.000000000000000000, 0.8660254037844387076, 1.000000000000000000, 0.8660254037844387076, 1.000000000000000000, 0.8660254037844387076, 1.000000000000000000, 0.8660254037844387076, 1.000000000000000000, 0.8660254037844387076, 1.000000000000000000, 0.8660254037844387076, 1.000000000000000000, 0.8660254037844387076, 1.000000000000000000, 0.8660254037844387076, 1.000000000000000000, 0.8660254037844387076, 1.000000000000000000, 0.8660254037844387076, 1.000000000000000000, 0.8660254037844387076, 1.000000000000000000, 0.8660254037844387076, 1.000000000000000000, 0.8660254037844387076, 1.000000000000000000, 0.8660254037844387076, 1.000000000000000000, 0.8660254037844387076, 1.000000000000000000, 0.8660254037844387076, 1.000000000000000000, 0.8660254037844387076, 1.000000000000000000, 0.8660254037844387076, 1.000000000000000000, 0.8660254037844387076, 1.000000000000000000, 0.8660254037844387076, 1.000000000000000000, 0.8660254037844387076, 1.000000000000000000, 0.8660254037844387076, 1.000000000000000000, 0.8660254037844387076, 1.000000000000000000, 0.8660254037844387076, 1.000000000000000000, 0.8660254037844387076, 1.000000000000000000, 0.8660254037844387076, 1.000000000000000000, 0.8660254037844387076, 1.000000000000000000, 0.8660254037844387076, 1.000000000000000000, 0.8660254037844387076, 1.000000000000000000, 0.8660254037844387076, 1.000000000000000000, 0.8660254037844387076, 1.000000000000000000, 0.8660254037844387076, 1.000000000000000000, 0.8660254037844387076, 1.000000000000000000, 0.8660254037844387076, 1.000000000000000000, 0.8660254037844387076, 1.000000000000000000, 0.8660254037844387076, 1.000000000000000000, 0.8660254037844387076, 1.000000000000000000, 0.8660254037844387076, 1.000000000000000000, 0.8660254037844387076, 1.000000000000000000, 0.8660254037844387076, 1.000000000000000000, 0.8660254037844387076, 1.000000000000000000, 0.8660254037844387076, 1.000000000000000000, 0.8660254037844387076, 1.000000000000000000, 0.8660254037844387076, 1.000000000000000000, 0.8660254037844387076, 1.000000000000000000, 0.8660254037844387076, 1.000000000000000000, 0.8660254037844387076, 1.000000000000000000, 0.8660254037844387076, 1.000000000000000000, 0.8660254037844387076, 1.000000000000000000, 0.8660254037844387076, 1.000000000000000000, 0.8660254037844387076, 1.000000000000000000, 0.8660254037844387076, 1.000000000000000000, 0.8660254037844387076, 1.000000000000000000, 0.8660254037844387076, 1.000000000000000000, 0.8660254037844387076, 1.000000000000000000, 0.8660254037844387076, 1.000000000000000000, 0.8660254037844387076, 1.000000000000000000, 0.8660254037844387076, 1.000000000000000000, 0.8660254037844387076, 1.000000000000000000, 0.8660254037844387076, 1.000000000000000000, 0.8660254037844387076, 1.000000000000000000, 0.8660254037844387076, 1.000000000000000000, 0.8660254037844387076, 1.000000000000000000, 0.8660254037844387076, 1.000000000000000000, 0.8660254037844387076, 1.000000000000000000, 0.8660254037844387076, 1.000000000000000000, 0.8660254037844387076, 1.000000000000000000, 0.8660254037844387076, 1.000000000000000000, 0.8660254037844387076, 1.000000000000000000, 0.8660254037844387076, 1.000000000000000000, 0.8660254037844387076, 1.000000000000000000, 0.8660254037844387076, 1.000000000000000000, 0.8660254037844387076, 1.000000000000000000, 0.8660254037844387076, 1.000000000000000000, 0.8660254037844387076, 1.000000000000000000, 0.8660254037844387076, 1.000000000000000000, 0.8660254037844387076, 1.000000000000000000, 0.8660254037844387076, 1.000000000000000000, 0.8660254037844387076, 1.000000000000000000, 0.8660254037844387076, 1.000000000000000000, 0.8660254037844387076, 1.000000000000000000, 0.8660254037844387076, 1.000000000000000000, 0.8660254037844387076, 1.000000000000000000, 0.8660254037844387076, 1.000000000000000000, 0.8660254037844387076, 1.000000000000000000, 0.8660254037844387076, 1.000000000000000000, 0.8660254037844387076, 1.000000000000000000, 0.8660254037844387076, 1.000000000000000000, 0.8660254037844387076, 1.000000000000000000, 0.8660254037844387076, 1.000000000000000000, 0.8660254037844387076, 1.000000000000000000, 0.8660254037844387076, 1.000000000000000000, 0.8660254037844387076, 1.000000000000000000, 0.8660254037844387076, 1.000000000000000000, 0.8660254037844387076, 1.000000000000000000, 0.8660254037844387076, 1.000000000000000000, 0.8660254037844387076, 1.000000000000000000, 0.8660254037844387076, 1.000000000000000000, 0.8660254037844387076, 1.000000000000000000, 0.8660254037844387076, 1.000000000000000000, 0.8660254037844387076, 1.000000000000000000, 0.8660254037844387076, 1.000000000000000000, 0.8660254037844387076, 1.000000000000000000, 0.8660254037844387076, 1.000000000000000000, 0.8660254037844387076, 1.000000000000000000, 0.8660254037844387076, 1.000000000000000000, 0.8660254037844387076, 1.000000000000000000, 0.8660254037844387076, 1.000000000000000000, 0.8660254037844387076, 1.000000000000000000, 0.8660254037844387076, 1.000000000000000000, 0.8660254037844387076, 1.000000000000000000, 0.8660254037844387076, 1.000000000000000000, 0.8660254037844387076, 1.000000000000000000, 0.8660254037844387076, 1.000000000000000000, 0.8660254037844387076, 1.000000000000000000, 0.8660254037844387076, 1.000000000000000000, 0.8660254037844387076, 1.000000000000000000, 0.8660254037844387076, 1.000000000000000000, 0.8660254037844387076, 1.000000000000000000, 0.8660254037844387076, 1.000000000000000000, 0.8660254037844387076, 1.000000000000000000, 0.8660254037844387076, 1.000000000000000000, 0.8660254037844387076, 1.000000000000000000, 0.8660254037844387076, 1.000000000000000000, 0.8660254037844387076, 1.000000000000000000, 0.8660254037844387076, 1.000000000000000000, 0.8660254037844387076, 1.000000000000000000, 0.8660254037844387076, 1.000000000000000000, 0.8660254037844387076, 1.000000000000000000, 0.8660254037844387076, 1.000000000000000000, 0.8660254037844387076, 1.000000000000000000, 0.8660254037844387076, 1.000000000000000000, 0.8660254037844387076, 1.000000000000000000, 0.8660254037844387076, 1.000000000000000000, 0.8660254037844387076, 1.000000000000000000, 0.8660254037844387076, 1.000000000000000000, 0.8660254037844387076, 1.000000000000000000, 0.8660254037844387076, 1.000000000000000000, 0.8660254037844387076, 1.000000000000000000, 0.8660254037844387076, 1.000000000000000000, 0.8660254037844387076, 1.000000000000000000, 0.8660254037844387076, 1.000000000000000000, 0.8660254037844387076, 1.000000000000000000, 0.8660254037844387076, 1.000000000000000000, 0.8660254037844387076, 1.000000000000000000, 0.8660254037844387076, 1.000000000000000000, 0.8660254037844387076, 1.000000000000000000, 0.8660254037844387076, 1.000000000000000000, 0.8660254037844387076, 1.000000000000000000, 0.8660254037844387076, 1.000000000000000000, 0.8660254037844387076, 1.000000000000000000, 0.8660254037844387076, 1.000000000000000000, 0.8660254037844387076, 1.000000000000000000, 0.8660254037844387076, 1.000000000000000000, 0.8660254037844387076, 1.000000000000000000, 0.8660254037844387076, 1.000000000000000000, 0.8660254037844387076, 1.000000000000000000, 0.8660254037844387076, 1.000000000000000000, 0.8660254037844387076, 1.000000000000000000, 0.8660254037844387076, 1.000000000000000000, 0.8660254037844387076, 1.000000000000000000, 0.8660254037844387076, 1.000000000000000000, 0.8660254037844387076, 1.000000000000000000, 0.8660254037844387076, 1.000000000000000000, 0.8660254037844387076, 1.000000000000000000, 0.8660254037844387076, 1.000000000000000000, 0.8660254037844387076, 1.000000000000000000, 0.8660254037844387076, 1.000000000000000000, 0.8660254037844387076, 1.000000000000000000, 0.8660254037844387076, 1.000000000000000000, 0.8660254037844387076, 1.000000000000000000, 0.8660254037844387076, 1.000000000000000000, 0.8660254037844387076, 1.000000000000000000, 0.8660254037844387076, 1.000000000000000000, 0.8660254037844387076, 1.000000000000000000, 0.8660254037844387076, 1.000000000000000000, 0.8660254037844387076, 1.000000000000000000, 0.8660254037844387076, 1.000000000000000000, 0.8660254037844387076, 1.000000000000000000, 0.8660254037844387076, 1.000000000000000000, 0.8660254037844387076, 1.000000000000000000, 0.8660254037844387076, 1.000000000000000000, 0.8660254037844387076, 1.000000000000000000, 0.8660254037844387076, 1.000000000000000000, 0.8660254037844387076, 1.000000000000000000, 0.8660254037844387076, 1.000000000000000000, 0.8660254037844387076, 1.000000000000000000, 0.8660254037844387076, 1.000000000000000000, 0.8660254037844387076, 1.000000000000000000, 0.8660254037844387076, 1.000000000000000000, 0.8660254037844387076, 1.000000000000000000, 0.8660254037844387076, 1.000000000000000000, 0.8660254037844387076, 1.000000000000000000, 0.8660254037844387076, 1.000000000000000000, 0.8660254037844387076, 1.000000000000000000, 0.8660254037844387076, 1.000000000000000000, 0.8660254037844387076, 1.000000000000000000, 0.8660254037844387076, 1.000000000000000000, 0.8660254037844387076, 1.000000000000000000, 0.8660254037844387076, 1.000000000000000000, 0.8660254037844387076, 1.000000000000000000, 0.8660254037844387076, 1.000000000000000000, 0.8660254037844387076, 1.000000000000000000, 0.8660254037844387076, 1.000000000000000000, 0.8660254037844387076, 1.000000000000000000, 0.8660254037844387076, 1.000000000000000000, 0.8660254037844387076, 1.000000000000000000, 0.8660254037844387076, 1.000000000000000000, 0.8660254037844387076, 1.000000000000000000, 0.8660254037844387076, 1.000000000000000000, 0.8660254037844387076, 1.000000000000000000, 0.8660254037844387076, 1.000000000000000000, 0.8660254037844387076, 1.000000000000000000, 0.8660254037844387076, 1.000000000000000000, 0.8660254037844387076, 1.000000000000000000, 0.8660254037844387076, 1.000000000000000000, 0.8660254037844387076, 1.000000000000000000, 0.8660254037844387076, 1.000000000000000000, 0.8660254037844387076, 1.000000000000000000, 0.8660254037844387076, 1.000000000000000000, 0.8660254037844387076, 1.000000000000000000, 0.8660254037844387076, 1.000000000000000000, 0.8660254037844387076, 1.000000000000000000, 0.8660254037844387076, 1.000000000000000000, 0.8660254037844387076, 1.000000000000000000, 0.8660254037844387076, 1.000000000000000000, 0.8660254037844387076, 1.000000000000000000, 0.8660254037844387076, 1.000000000000000000, 0.8660254037844387076, 1.000000000000000000, 0.8660254037844387076, 1.000000000000000000, 0.8660254037844387076, 1.000000000000000000, 0.8660254037844387076, 1.000000000000000000, 0.8660254037844387076, 1.000000000000000000, 0.8660254037844387076, 1.000000000000000000, 0.8660254037844387076, 1.000000000000000000, 0.8660254037844387076, 1.000000000000000000, 0.8660254037844387076, 1.000000000000000000, 0.8660254037844387076, 1.000000000000000000, 0.8660254037844387076, 1.000000000000000000, 0.8660254037844387076, 1.000000000000000000, 0.8660254037844387076, 1.000000000000000000, 0.8660254037844387076, 1.000000000000000000, 0.8660254037844387076, 1.000000000000000000, 0.8660254037844387076, 1.000000000000000000, 0.8660254037844387076, 1.000000000000000000, 0.8660254037844387076, 1.000000000000000000, 0.8660254037844387076, 1.000000000000000000, 0.8660254037844387076, 1.000000000000000000, 0.8660254037844387076, 1.000000000000000000, 0.8660254037844387076, 1.000000000000000000, 0.8660254037844387076, 1.000000000000000000, 0.8660254037844387076, 1.000000000000000000, 0.8660254037844387076, 1.000000000000000000, 0.8660254037844387076, 1.000000000000000000, 0.8660254037844387076, 1.000000000000000000, 0.8660254037844387076, 1.000000000000000000, 0.8660254037844387076, 1.000000000000000000, 0.8660254037844387076, 1.000000000000000000, 0.8660254037844387076, 1.000000000000000000, 0.8660254037844387076, 1.000000000000000000, 0.8660254037844387076, 1.000000000000000000, 0.8660254037844387076, 1.000000000000000000, 0.8660254037844387076, 1.000000000000000000, 0.8660254037844387076, 1.000000000000000000, 0.8660254037844387076, 1.000000000000000000, 0.8660254037844387076, 1.000000000000000000, 0.8660254037844387076, 1.000000000000000000, 0.8660254037844387076, 1.000000000000000000, 0.8660254037844387076, 1.000000000000000000, 0.8660254037844387076, 1.000000000000000000, 0.8660254037844387076, 1.000000000000000000, 0.8660254037844387076, 1.000000000000000000, 0.8660254037844387076, 1.000000000000000000, 0.8660254037844387076, 1.000000000000000000, 0.8660254037844387076, 1.000000000000000000, 0.8660254037844387076, 1.000000000000000000, 0.8660254037844387076, 1.000000000000000000, 0.8660254037844387076, 1.000000000000000000, 0.8660254037844387076, 1.000000000000000000, 0.8660254037844387076, 1.000000000000000000, 0.8660254037844387076, 1.000000000000000000, 0.8660254037844387076, 1.000000000000000000, 0.8660254037844387076, 1.000000000000000000, 0.8660254037844387076, 1.000000000000000000, 0.8660254037844387076, 1.000000000000000000, 0.8660254037844387076, 1.000000000000000000, 0.8660254037844387076, 1.000000000000000000, 0.8660254037844387076, 1.000000000000000000, 0.8660254037844387076, 1.000000000000000000, 0.8660254037844387076, 1.000000000000000000, 0.8660254037844387076, 1.000000000000000000, 0.8660254037844387076, 1.000000000000000000, 0.8660254037844387076, 1.000000000000000000, 0.8660254037844387076, 1.000000000000000000, 0.8660254037844387076, 1.000000000000000000, 0.8660254037844387076, 1.000000000000000000, 0.8660254037844387076, 1.000000000000000000, 0.8660254037844387076, 1.000000000000000000, 0.8660254037844387076, 1.000000000000000000, 0.8660254037844387076, 1.000000000000000000, 0.8660254037844387076, 1.000000000000000000, 0.8660254037844387076, 1.000000000000000000, 0.8660254037844387076, 1.000000000000000000, 0.8660254037844387076, 1.000000000000000000, 0.8660254037844387076, 1.000000000000000000, 0.8660254037844387076, 1.000000000000000000, 0.8660254037844387076, 1.000000000000000000, 0.8660254037844387076, 1.000000000000000000, 0.8660254037844387076, 1.000000000000000000, 0.8660254037844387076, 1.000000000000000000, 0.8660254037844387076, 1.000000000000000000, 0.8660254037844387076, 1.000000000000000000, 0.8660254037844387076, 1.000000000000000000, 0.8660254037844387076, 1.000000000000000000, 0.8660254037844387076, 1.000000000000000000, 0.8660254037844387076, 1.000000000000000000, 0.8660254037844387076, 1.000000000000000000, 0.8660254037844387076, 1.000000000000000000, 0.8660254037844387076, 1.000000000000000000, 0.8660254037844387076, 1.000000000000000000, 0.8660254037844387076, 1.000000000000000000, 0.8660254037844387076, 1.000000000000000000, 0.8660254037844387076, 1.000000000000000000, 0.8660254037844387076, 1.000000000000000000, 0.8660254037844387076, 1.000000000000000000, 0.8660254037844387076, 1.000000000000000000, 0.8660254037844387076, 1.000000000000000000, 0.8660254037844387076, 1.000000000000000000, 0.8660254037844387076, 1.000000000000000000, 0.8660254037844387076, 1.000000000000000000, 0.8660254037844387076, 1.000000000000000000, 0.8660254037844387076, 1.000000000000000000, 0.8660254037844387076, 1.000000000000000000, 0.8660254037844387076, 1.000000000000000000, 0.8660254037844387076, 1.000000000000000000, 0.8660254037844387076, 1.000000000000000000, 0.8660254037844387076, 1.000000000000000000, 0.8660254037844387076, 1.000000000000000000, 0.8660254037844387076, 1.000000000000000000, 0.8660254037844387076, 1.000000000000000000, 0.8660254037844387076, 1.000000000000000000, 0.8660254037844387076, 1.000000000000000000, 0.8660254037844387076, 1.000000000000000000, 0.8660254037844387076, 1.000000000000000000, 0.8660254037844387076, 1.000000000000000000, 0.8660254037844387076, 1.000000000000000000, 0.8660254037844387076, 1.000000000000000000, 0.8660254037844387076, 1.000000000000000000, 0.8660254037844387076, 1.000000000000000000, 0.8660254037844387076, 1.000000000000000000, 0.8660254037844387076, 1.000000000000000000, 0.8660254037844387076, 1.000000000000000000, 0.8660254037844387076, 1.000000000000000000, 0.8660254037844387076, 1.000000000000000000, 0.8660254037844387076, 1.000000000000000000, 0.8660254037844387076, 1.000000000000000000, 0.8660254037844387076, 1.000000000000000000, 0.8660254037844387076, 1.000000000000000000, 0.8660254037844387076, 1.000000000000000000, 0.8660254037844387076, 1.000000000000000000, 0.8660254037844387076, 1.000000000000000000, 0.8660254037844387076, 1.000000000000000000, 0.8660254037844387076, 1.000000000000000000, 0.8660254037844387076, 1.000000000000000000, 0.8660254037844387076, 1.000000000000000000, 0.8660254037844387076, 1.000000000000000000, 0.8660254037844387076, 1.000000000000000000, 0.8660254037844387076, 1.000000000000000000, 0.8660254037844387076, 1.000000000000000000, 0.8660254037844387076, 1.000000000000000000, 0.8660254037844387076, 1.000000000000000000, 0.8660254037844387076, 1.000000000000000000, 0.8660254037844387076, 1.000000000000000000, 0.8660254037844387076, 1.000000000000000000, 0.8660254037844387076, 1.000000000000000000, 0.8660254037844387076, 1.000000000000000000, 0.8660254037844387076, 1.000000000000000000, 0.8660254037844387076, 1.000000000000000000, 0.8660254037844387076, 1.000000000000000000, 0.8660254037844387076, 1.000000000000000000, 0.8660254037844387076, 1.000000000000000000, 0.8660254037844387076, 1.000000000000000000, 0.8660254037844387076, 1.000000000000000000, 0.8660254037844387076, 1.000000000000000000, 0.8660254037844387076, 1.000000000000000000, 0.8660254037844387076, 1.000000000000000000, 0.8660254037844387076, 1.000000000000000000, 0.8660254037844387076, 1.000000000000000000, 0.8660254037844387076, 1.000000000000000000, 0.8660254037844387076, 1.000000000000000000, 0.8660254037844387076, 1.000000000000000000, 0.8660254037844387076, 1.000000000000000000, 0.8660254037844387076, 1.000000000000000000, 0.8660254037844387076, 1.000000000000000000, 0.8660254037844387076, 1.000000000000000000, 0.8660254037844387076, 1.000000000000000000, 0.8660254037844387076, 1.000000000000000000, 0.8660254037844387076, 1.000000000000000000, 0.8660254037844387076, 1.000000000000000000, 0.8660254037844387076, 1.000000000000000000, 0.8660254037844387076, 1.000000000000000000, 0.8660254037844387076, 1.000000000000000000, 0.8660254037844387076, 1.000000000000000000, 0.8660254037844387076, 1.000000000000000000, 0.8660254037844387076, 1.000000000000000000, 0.8660254037844387076, 1.000000000000000000, 0.8660254037844387076, 1.000000000000000000, 0.8660254037844387076, 1.000000000000000000, 0.8660254037844387076, 1.000000000000000000, 0.8660254037844387076, 1.000000000000000000, 0.8660254037844387076, 1.000000000000000000, 0.8660254037844387076, 1.000000000000000000, 0.8660254037844387076, 1.000000000000000000, 0.8660254037844387076, 1.000000000000000000, 0.8660254037844387076, 1.000000000000000000, 0.8660254037844387076, 1.000000000000000000, 0.8660254037844387076, 1.000000000000000000, 0.8660254037844387076, 1.000000000000000000, 0.8660254037844387076, 1.000000000000000000, 0.8660254037844387076, 1.000000000000000000, 0.8660254037844387076, 1.000000000000000000, 0.8660254037844387076, 1.000000000000000000, 0.8660254037844387076, 1.000000000000000000, 0.8660254037844387076, 1.000000000000000000, 0.8660254037844387076, 1.000000000000000000, 0.8660254037844387076, 1.000000000000000000, 0.8660254037844387076, 1.000000000000000000, 0.8660254037844387076, 1.000000000000000000, 0.8660254037844387076, 1.000000000000000000, 0.8660254037844387076, 1.000000000000000000, 0.8660254037844387076, 1.000000000000000000, 0.8660254037844387076, 1.000000000000000000, 0.8660254037844387076, 1.000000000000000000, 0.8660254037844387076, 1.000000000000000000, 0.8660254037844387076, 1.000000000000000000, 0.8660254037844387076, 1.000000000000000000, 0.8660254037844387076, 1.000000000000000000, 0.8660254037844387076, 1.000000000000000000, 0.8660254037844387076, 1.000000000000000000, 0.8660254037844387076, 1.000000000000000000, 0.8660254037844387076, 1.000000000000000000, 0.8660254037844387076, 1.000000000000000000, 0.8660254037844387076, 1.000000000000000000, 0.8660254037844387076, 1.000000000000000000, 0.8660254037844387076, 1.000000000000000000, 0.8660254037844387076, 1.000000000000000000, 0.8660254037844387076, 1.000000000000000000, 0.8660254037844387076, 1.000000000000000000, 0.8660254037844387076, 1.000000000000000000, 0.8660254037844387076, 1.000000000000000000, 0.8660254037844387076, 1.000000000000000000, 0.8660254037844387076, 1.000000000000000000, 0.8660254037844387076, 1.000000000000000000, 0.8660254037844387076, 1.000000000000000000, 0.8660254037844387076, 1.000000000000000000, 0.8660254037844387076, 1.000000000000000000, 0.8660254037844387076, 1.000000000000000000, 0.8660254037844387076, 1.000000000000000000, 0.8660254037844387076, 1.000000000000000000, 0.8660254037844387076, 1.000000000000000000, 0.8660254037844387076, 1.000000000000000000, 0.8660254037844387076, 1.000000000000000000, 0.8660254037844387076, 1.000000000000000000, 0.8660254037844387076, 1.000000000000000000, 0.8660254037844387076, 1.000000000000000000, 0.8660254037844387076, 1.000000000000000000, 0.8660254037844387076, 1.000000000000000000, 0.8660254037844387076, 1.000000000000000000, 0.8660254037844387076, 1.000000000000000000, 0.8660254037844387076, 1.000000000000000000, 0.8660254037844387076, 1.000000000000000000, 0.8660254037844387076, 1.000000000000000000, 0.8660254037844387076, 1.000000000000000000, 0.8660254037844387076, 1.000000000000000000, 0.8660254037844387076, 1.000000000000000000, 0.8660254037844387076, 1.000000000000000000, 0.8660254037844387076, 1.000000000000000000, 0.8660254037844387076, 1.000000000000000000, 0.8660254037844387076, 1.000000000000000000, 0.8660254037844387076, 1.000000000000000000, 0.8660254037844387076, 1.000000000000000000, 0.8660254037844387076, 1.000000000000000000, 0.8660254037844387076, 1.000000000000000000, 0.8660254037844387076, 1.000000000000000000, 0.8660254037844387076, 1.000000000000000000, 0.8660254037844387076, 1.000000000000000000, 0.8660254037844387076, 1.000000000000000000, 0.8660254037844387076, 1.000000000000000000, 0.8660254037844387076, 1.000000000000000000, 0.8660254037844387076, 1.000000000000000000, 0.8660254037844387076, 1.000000000000000000, 0.8660254037844387076, 1.000000000000000000, 0.8660254037844387076, 1.000000000000000000, 0.8660254037844387076, 1.000000000000000000, 0.8660254037844387076, 1.000000000000000000, 0.8660254037844387076, 1.000000000000000000, 0.8660254037844387076, 1.000000000000000000, 0.8660254037844387076, 1.000000000000000000, 0.8660254037844387076, 1.000000000000000000, 0.8660254037844387076, 1.000000000000000000, 0.8660254037844387076, 1.000000000000000000, 0.8660254037844387076, 1.000000000000000000, 0.8660254037844387076, 1.000000000000000000, 0.8660254037844387076, 1.000000000000000000, 0.8660254037844387076, 1.000000000000000000, 0.8660254037844387076, 1.000000000000000000, 0.8660254037844387076, 1.000000000000000000, 0.8660254037844387076, 1.000000000000000000, 0.8660254037844387076, 1.000000000000000000, 0.8660254037844387076, 1.000000000000000000, 0.8660254037844387076, 1.000000000000000000, 0.8660254037844387076, 1.000000000000000000, 0.8660254037844387076, 1.000000000000000000, 0.8660254037844387076, 1.000000000000000000, 0.8660254037844387076, 1.000000000000000000) ) ) 
 REPRESENTATION_ITEM ( '' )  SURFACE ( )  );
#30261 = CARTESIAN_POINT ( 'NONE',  ( 0.000000000000000000, -170.0000000000000000, 0.000000000000000000 ) ) ;
#30262 = CARTESIAN_POINT ( 'NONE',  ( -2.500000000000000444, -4.166666666666666075, -4.330127018922193649 ) ) ;
#30263 = ADVANCED_FACE ( 'NONE', ( #9028 ), #28949, .T. ) ;
#30264 = CARTESIAN_POINT ( 'NONE',  ( 4.458734124999998549, -64.72916666530106511, -2.574251347313721627 ) ) ;
#30265 = DIRECTION ( 'NONE',  ( 0.000000000000000000, 0.000000000000000000, 1.000000000000000000 ) ) ;
#30266 = ADVANCED_FACE ( 'NONE', ( #43429 ), #52783, .T. ) ;
#30267 = ADVANCED_FACE ( 'NONE', ( #33787 ), #8714, .T. ) ;
#30268 = CARTESIAN_POINT ( 'NONE',  ( -3.535250795749689387E-16, -5.124999997268809615, -5.773502691896257311 ) ) ;
#30270 = ORIENTED_EDGE ( 'NONE', *, *, #45964, .T. ) ;
#30269 = CARTESIAN_POINT ( 'NONE',  ( -4.458734124999999437, -33.39583333196772941, -2.574251347313719407 ) ) ;
#30271 = DIRECTION ( 'NONE',  ( 0.000000000000000000, 1.000000000000000000, 0.000000000000000000 ) ) ;
#30272 = CARTESIAN_POINT ( 'NONE',  ( -1.339745962155613146, 28.33034180399266333, 5.000000000000000000 ) ) ;
#30273 = ORIENTED_EDGE ( 'NONE', *, *, #25652, .F. ) ;
#30274 = CARTESIAN_POINT ( 'NONE',  ( -5.000000000000000000, -48.95833333060213732, -2.886751345948128211 ) ) ;
#30275 = CARTESIAN_POINT ( 'NONE',  ( -2.499999999999996447, -50.83333333333332860, 4.330127018922195425 ) ) ;
#30277 = CARTESIAN_POINT ( 'NONE',  ( 4.458734124999998549, -28.97916666530107577, -2.574251347313721627 ) ) ;
#30276 = FACE_OUTER_BOUND ( 'NONE', #4220, .T. ) ;
#30278 = CARTESIAN_POINT ( 'NONE',  ( 1.975475456537005874E-15, -41.62499999726880162, 5.000000000000000000 ) ) ;
#30279 = CARTESIAN_POINT ( 'NONE',  ( 2.229367062499998831, -77.64583333196773651, -3.861377020970580887 ) ) ;
#30280 = CARTESIAN_POINT ( 'NONE',  ( -1.846868145590734756, -143.3750000013656063, -4.458734125000000326 ) ) ;
#30281 = CARTESIAN_POINT ( 'NONE',  ( -2.229367062500000163, -80.47916666530106511, -3.861377020970580443 ) ) ;
#30282 = CARTESIAN_POINT ( 'NONE',  ( -53.51423613279429503, -137.5000000013656063, 4.591703134518082763 ) ) ;
#30283 = EDGE_CURVE ( 'NONE', #61600, #22073, #63275, .T. ) ;
#30284 = CARTESIAN_POINT ( 'NONE',  ( 9.457646018065525792E-16, -28.31249999863440081, 5.148502694627439702 ) ) ;
#30285 = EDGE_LOOP ( 'NONE', ( #35610, #19235, #50545 ) ) ;
#30286 = LINE ( 'NONE', #15182, #26920 ) ;
#30288 = EDGE_CURVE ( 'NONE', #25936, #18086, #18985, .T. ) ;
#30287 = ORIENTED_EDGE ( 'NONE', *, *, #38479, .F. ) ;
#30289 = CARTESIAN_POINT ( 'NONE',  ( 4.458734125000001214, -75.14583333196775072, 2.574251347313718519 ) ) ;
#30290 = CARTESIAN_POINT ( 'NONE',  ( -52.46430154831001857, -135.0000000000000284, -3.678960875299264188 ) ) ;
#30291 = EDGE_LOOP ( 'NONE', ( #26967, #14797, #12365, #24471 ) ) ;
#30292 = CARTESIAN_POINT ( 'NONE',  ( 6.123233995736766282E-16, -170.0000000000000000, -5.000000000000000000 ) ) ;
#30293 =( BOUNDED_CURVE ( )  B_SPLINE_CURVE ( 2, ( #3469, #23082, #42371, #17928, #18250, #27273, #32729, #13425, #47823 ),
 .UNSPECIFIED., .F., .F. ) 
 B_SPLINE_CURVE_WITH_KNOTS ( ( 3, 2, 2, 2, 3 ),
 ( 0.7104166666666666963, 0.7111111111111111382, 0.7125000000000000222, 0.7138888888888889062, 0.7145833333333333481 ),
 .UNSPECIFIED. ) 
 CURVE ( )  GEOMETRIC_REPRESENTATION_ITEM ( )  RATIONAL_B_SPLINE_CURVE ( ( 0.9330127018922194093, 0.9330127018922194093, 1.000000000000000000, 0.8660254037844387076, 1.000000000000000000, 0.8660254037844387076, 1.000000000000000000, 0.9330127018922194093, 0.9330127018922194093 ) ) 
 REPRESENTATION_ITEM ( '' )  );
#30294 = CARTESIAN_POINT ( 'NONE',  ( -2.499999999999996447, 8.166666666666666075, 4.330127018922195425 ) ) ;
#30295 = CARTESIAN_POINT ( 'NONE',  ( 9.457646018065525792E-16, -63.31249999863440081, 5.148502694627439702 ) ) ;
#30296 = CARTESIAN_POINT ( 'NONE',  ( -2.229367062500000163, -1.729166665301071992, -3.861377020970580443 ) ) ;
#30297 = ORIENTED_EDGE ( 'NONE', *, *, #37065, .T. ) ;
#30298 = CARTESIAN_POINT ( 'NONE',  ( -1.339745962155613812, -93.08034179853027013, -5.000000000000000000 ) ) ;
#30299 = CARTESIAN_POINT ( 'NONE',  ( 5.000000000000000000, -27.41666666666666430, -2.886751345948130876 ) ) ;
#30300 = CARTESIAN_POINT ( 'NONE',  ( -4.458734124999999437, 15.60416666803225993, -2.574251347313719407 ) ) ;
#30301 = CARTESIAN_POINT ( 'NONE',  ( -52.10840900171896806, -141.1875000013656063, 3.393966926194110556 ) ) ;
#30302 = CARTESIAN_POINT ( 'NONE',  ( -57.46284108482265651, -154.9375000000000000, 4.819101127000238627 ) ) ;
#30303 = CARTESIAN_POINT ( 'NONE',  ( -3.152801135295367096, -161.0625000013656063, -3.152801135295367541 ) ) ;
#30304 = FACE_OUTER_BOUND ( 'NONE', #2211, .T. ) ;
#30305 = VERTEX_POINT ( 'NONE', #53402 ) ;
#30306 = CARTESIAN_POINT ( 'NONE',  ( 4.458734124999998549, -78.72916666530106511, -2.574251347313721627 ) ) ;
#30307 = CARTESIAN_POINT ( 'NONE',  ( 5.000000000000000888, -75.58333333333334281, 2.886751345948126879 ) ) ;
#30308 = CARTESIAN_POINT ( 'NONE',  ( -3.152548672688508926E-16, 4.437500001365595637, -5.148502694627439702 ) ) ;
#30309 = LINE ( 'NONE', #59927, #17049 ) ;
#30310 = CYLINDRICAL_SURFACE ( 'NONE', #9999, 5.000000000000000000 ) ;
#30311 = CARTESIAN_POINT ( 'NONE',  ( 2.229367062500001939, -69.22916666530107932, 3.861377020970579999 ) ) ;
#30312 = CARTESIAN_POINT ( 'NONE',  ( 2.500000000000002220, -27.54166666393548013, 4.330127018922192761 ) ) ;
#30313 = CARTESIAN_POINT ( 'NONE',  ( 2.500000000000002220, 12.45833333606451809, 4.330127018922192761 ) ) ;
#30314 = CARTESIAN_POINT ( 'NONE',  ( -2.499999999999996447, -40.83333333333333570, 4.330127018922195425 ) ) ;
#30315 = CARTESIAN_POINT ( 'NONE',  ( -2.500000000000000444, -56.16666666666667140, -4.330127018922193649 ) ) ;
#30316 = CARTESIAN_POINT ( 'NONE',  ( 6.123233995736766282E-16, -170.0000000000000000, -5.000000000000000000 ) ) ;
#30317 = CARTESIAN_POINT ( 'NONE',  ( -3.152548672688508926E-16, -47.56249999863440792, -5.148502694627439702 ) ) ;
#30318 = CARTESIAN_POINT ( 'NONE',  ( 2.229367062500001939, -31.22916666530107221, 3.861377020970579999 ) ) ;
#30319 = CARTESIAN_POINT ( 'NONE',  ( 4.458734124999998549, 2.020833334698927786, -2.574251347313721627 ) ) ;
#30320 = CARTESIAN_POINT ( 'NONE',  ( -5.000000000000000888, -161.5625000027312126, 2.071067811865474617 ) ) ;
#30321 = CARTESIAN_POINT ( 'NONE',  ( -4.999999999999999112, 21.08333333333333215, 2.886751345948131764 ) ) ;
#30322 = CARTESIAN_POINT ( 'NONE',  ( 3.061616997868383141E-16, -144.8750000027312126, -5.000000000000000000 ) ) ;
#30323 = CARTESIAN_POINT ( 'NONE',  ( 1.975475456537005874E-15, 17.37500000273118417, 5.000000000000000000 ) ) ;
#30324 = CARTESIAN_POINT ( 'NONE',  ( -4.458734124999998549, -37.22916666530107221, 2.574251347313722516 ) ) ;
#30325 = CARTESIAN_POINT ( 'NONE',  ( 1.060575238724906964E-15, -75.62499999726880162, 5.773502691896257311 ) ) ;
#30326 = CARTESIAN_POINT ( 'NONE',  ( -59.29741812935640155, -144.8750000013655779, -2.196230717870135685 ) ) ;
#30327 = CARTESIAN_POINT ( 'NONE',  ( 1.339745962155615144, -24.58034179853029499, 4.999999999999999112 ) ) ;
#30328 = CARTESIAN_POINT ( 'NONE',  ( -6.250000000000000000, -5.051814855409233473, -7.198902722707430257 ) ) ;
#30329 = CARTESIAN_POINT ( 'NONE',  ( 4.458734124999999437, -82.06249999863440792, -5.460374474430324690E-16 ) ) ;
#30330 = CARTESIAN_POINT ( 'NONE',  ( -8.190561711645485556E-16, -163.9375000013655779, 4.458734124999999437 ) ) ;
#30331 = CARTESIAN_POINT ( 'NONE',  ( 1.339745962155615144, 18.41965820146970856, 4.999999999999999112 ) ) ;
#30332 = CARTESIAN_POINT ( 'NONE',  ( -9.184850993605147944E-16, -159.3750000027311842, 5.000000000000000000 ) ) ;
#30333 = CARTESIAN_POINT ( 'NONE',  ( 5.000000000000000888, -26.58333333333333570, 2.886751345948126879 ) ) ;
#30334 = CARTESIAN_POINT ( 'NONE',  ( -1.846868145590734756, -143.1250000013656063, -4.458734125000000326 ) ) ;
#30335 = ORIENTED_EDGE ( 'NONE', *, *, #33623, .F. ) ;
#30336 = CARTESIAN_POINT ( 'NONE',  ( 4.458734124999999437, 20.93750000136559208, -5.460374474430324690E-16 ) ) ;
#30337 = ORIENTED_EDGE ( 'NONE', *, *, #53182, .T. ) ;
#30338 = CARTESIAN_POINT ( 'NONE',  ( 4.458734124999999437, -62.06249999863440792, -5.460374474430324690E-16 ) ) ;
#30339 = CARTESIAN_POINT ( 'NONE',  ( 5.000000000000000000, 21.62500000273118417, -6.123233995736766282E-16 ) ) ;
#30340 = DIRECTION ( 'NONE',  ( -0.000000000000000000, 1.000000000000000000, -0.000000000000000000 ) ) ;
#30341 = CARTESIAN_POINT ( 'NONE',  ( -3.535250795749689387E-16, 13.75000000000000000, -5.773502691896257311 ) ) ;
#30342 = CARTESIAN_POINT ( 'NONE',  ( -3.152548672688508926E-16, -51.56249999863440792, -5.148502694627439702 ) ) ;
#30343 = AXIS2_PLACEMENT_3D ( 'NONE', #20589, #54357, #40195 ) ;
#30344 = CARTESIAN_POINT ( 'NONE',  ( -4.458734124999999437, -10.31249999863440792, 0.000000000000000000 ) ) ;
#30345 = CARTESIAN_POINT ( 'NONE',  ( -2.500000000000000444, 3.958333336064518093, -4.330127018922193649 ) ) ;
#30346 = EDGE_CURVE ( 'NONE', #52846, #21770, #41854, .T. ) ;
#30347 = CARTESIAN_POINT ( 'NONE',  ( -1.339745962155613812, 13.79465819873852084, -5.000000000000000000 ) ) ;
#30348 = CARTESIAN_POINT ( 'NONE',  ( -5.000000000000000000, -0.08333333333333454995, -2.886751345948128211 ) ) ;
#30349 = CARTESIAN_POINT ( 'NONE',  ( 1.339745962155613146, 28.41965820146970501, 5.000000000000000888 ) ) ;
#30350 = DIRECTION ( 'NONE',  ( 0.000000000000000000, 0.000000000000000000, 1.000000000000000000 ) ) ;
#30352 = CARTESIAN_POINT ( 'NONE',  ( -4.458734124999998549, -20.22916666530107221, 2.574251347313722516 ) ) ;
#30351 = CARTESIAN_POINT ( 'NONE',  ( 1.339745962155612702, 21.83034180399266333, -5.000000000000000000 ) ) ;
#30353 = EDGE_CURVE ( 'NONE', #19989, #42565, #3896, .T. ) ;
#30354 = CARTESIAN_POINT ( 'NONE',  ( -5.000000000000000000, -77.87499999726881583, 0.000000000000000000 ) ) ;
#30355 = CARTESIAN_POINT ( 'NONE',  ( -4.458734124999999437, -57.39583333196773651, -2.574251347313719407 ) ) ;
#30356 = CARTESIAN_POINT ( 'NONE',  ( -4.458734125000000326, -155.2500000013656063, -1.846868145590735644 ) ) ;
#30357 = ADVANCED_FACE ( 'NONE', ( #18368 ), #23825, .T. ) ;
#30358 = EDGE_CURVE ( 'NONE', #56173, #44977, #21775, .T. ) ;
#30359 = CARTESIAN_POINT ( 'NONE',  ( 5.000000000000000000, -53.29166666393547303, -2.886751345948129988 ) ) ;
#30360 = ORIENTED_EDGE ( 'NONE', *, *, #48877, .F. ) ;
#30361 = CARTESIAN_POINT ( 'NONE',  ( 6.123233995736766282E-16, -120.0000000000000000, -5.000000000000000000 ) ) ;
#30362 = CARTESIAN_POINT ( 'NONE',  ( 4.458734124999999437, 1.937500001365593416, -5.460374474430324690E-16 ) ) ;
#30363 = VERTEX_POINT ( 'NONE', #30870 ) ;
#30365 = CARTESIAN_POINT ( 'NONE',  ( 1.243387493232115550E-13, -9.124999997268817609, -5.000000000000000000 ) ) ;
#30364 = CARTESIAN_POINT ( 'NONE',  ( -5.000000000000000888, -157.5625000027312410, 2.071067811865474617 ) ) ;
#30366 = CARTESIAN_POINT ( 'NONE',  ( -1.846868145590737420, -154.7500000013656063, 4.458734124999999437 ) ) ;
#30367 = EDGE_CURVE ( 'NONE', #13643, #29768, #55012, .T. ) ;
#30368 = ORIENTED_EDGE ( 'NONE', *, *, #52376, .F. ) ;
#30369 = EDGE_CURVE ( 'NONE', #14857, #25665, #30218, .T. ) ;
#30370 = CARTESIAN_POINT ( 'NONE',  ( -6.972266317189433020E-16, -99.24999999999998579, -5.000000000000000000 ) ) ;
#30371 = CARTESIAN_POINT ( 'NONE',  ( -51.75738570946856498, -130.7500000000000284, 3.805975901505576964 ) ) ;
#30372 = CARTESIAN_POINT ( 'NONE',  ( 2.229367062499998831, -44.89583333196774362, -3.861377020970580887 ) ) ;
#30373 = EDGE_LOOP ( 'NONE', ( #54643, #38925, #43402, #545 ) ) ;
#30374 = EDGE_CURVE ( 'NONE', #34229, #24623, #19684, .T. ) ;
#30375 = DIRECTION ( 'NONE',  ( -1.000000000000000000, -0.000000000000000000, -0.000000000000000000 ) ) ;
#30376 = CARTESIAN_POINT ( 'NONE',  ( 2.229367062499998831, 13.35416666803226171, -3.861377020970580887 ) ) ;
#30377 = CARTESIAN_POINT ( 'NONE',  ( 2.229367062499998831, 27.35416666803225993, -3.861377020970580887 ) ) ;
#30378 = CARTESIAN_POINT ( 'NONE',  ( -59.59170313451811296, -153.5000000013656063, 1.485763867205729394 ) ) ;
#30379 = CARTESIAN_POINT ( 'NONE',  ( 0.000000000000000000, -120.0000000000000000, 0.000000000000000000 ) ) ;
#30380 = CARTESIAN_POINT ( 'NONE',  ( 2.499999999999998668, -61.20833333060214443, -4.330127018922193649 ) ) ;
#30381 = CARTESIAN_POINT ( 'NONE',  ( -55.39835681537999790, -147.0000000027312126, 4.984105922594378235 ) ) ;
#30382 = CARTESIAN_POINT ( 'NONE',  ( 2.229367062499998831, -66.64583333196773651, -3.861377020970580887 ) ) ;
#30383 = CARTESIAN_POINT ( 'NONE',  ( -5.000000000000000000, -49.95833333060213022, -2.886751345948128211 ) ) ;
#30384 = CARTESIAN_POINT ( 'NONE',  ( -2.229367062499996610, 19.85416666803225993, 3.861377020970582219 ) ) ;
#30385 =( BOUNDED_CURVE ( )  B_SPLINE_CURVE ( 2, ( #54796, #24565, #45454, #54476, #29692, #44488, #15558, #59626, #5909 ),
 .UNSPECIFIED., .F., .F. ) 
 B_SPLINE_CURVE_WITH_KNOTS ( ( 3, 2, 2, 2, 3 ),
 ( 0.5229166666666666963, 0.5236111111111111382, 0.5250000000000000222, 0.5263888888888889062, 0.5270833333333333481 ),
 .UNSPECIFIED. ) 
 CURVE ( )  GEOMETRIC_REPRESENTATION_ITEM ( )  RATIONAL_B_SPLINE_CURVE ( ( 0.9330127018922194093, 0.9330127018922194093, 1.000000000000000000, 0.8660254037844387076, 1.000000000000000000, 0.8660254037844387076, 1.000000000000000000, 0.9330127018922194093, 0.9330127018922194093 ) ) 
 REPRESENTATION_ITEM ( '' )  );
#30386 = DIRECTION ( 'NONE',  ( 0.000000000000000000, 0.000000000000000000, 1.000000000000000000 ) ) ;
#30387 = CARTESIAN_POINT ( 'NONE',  ( -9.184850993605147944E-16, -157.2500000000000000, 5.000000000000000000 ) ) ;
#30388 = CARTESIAN_POINT ( 'NONE',  ( 4.458734124999999437, -47.06249999863440792, -5.460374474430324690E-16 ) ) ;
#30389 = CARTESIAN_POINT ( 'NONE',  ( 1.060575238724906964E-15, -7.624999997268813168, 5.773502691896257311 ) ) ;
#30390 = CARTESIAN_POINT ( 'NONE',  ( -2.500000000000000444, 24.83333333333333215, -4.330127018922193649 ) ) ;
#30391 = CARTESIAN_POINT ( 'NONE',  ( -1.339745962155613812, -66.08034179853028434, -5.000000000000000000 ) ) ;
#30392 = CARTESIAN_POINT ( 'NONE',  ( 4.458734125000001214, -90.14583333196773651, 2.574251347313718519 ) ) ;
#30393 = CARTESIAN_POINT ( 'NONE',  ( 0.000000000000000000, -170.0000000000000000, 0.000000000000000000 ) ) ;
#30394 = CARTESIAN_POINT ( 'NONE',  ( -3.152548672688508926E-16, -14.81249999863440436, -5.148502694627439702 ) ) ;
#30395 = VERTEX_POINT ( 'NONE', #45026 ) ;
#30396 = CARTESIAN_POINT ( 'NONE',  ( -6.972266317189433020E-16, -31.24999999999999645, -5.000000000000000000 ) ) ;
#30397 = CARTESIAN_POINT ( 'NONE',  ( -4.458734124999998549, -104.2291666653010651, 2.574251347313722516 ) ) ;
#30398 = CARTESIAN_POINT ( 'NONE',  ( -5.000000000000000000, -156.6250000027311842, -6.123233995736766282E-16 ) ) ;
#30399 = VERTEX_POINT ( 'NONE', #20597 ) ;
#30400 = CARTESIAN_POINT ( 'NONE',  ( 2.229367062500001939, -99.22916666530105090, 3.861377020970579999 ) ) ;
#30401 = CARTESIAN_POINT ( 'NONE',  ( 2.499999999999998668, -49.20833333060213732, -4.330127018922193649 ) ) ;
#30402 = CARTESIAN_POINT ( 'NONE',  ( -5.000000000000000000, -57.87499999726880873, 0.000000000000000000 ) ) ;
#30403 = CARTESIAN_POINT ( 'NONE',  ( -1.339745962155610925, -66.79465819873851729, 5.000000000000000000 ) ) ;
#30404 = CARTESIAN_POINT ( 'NONE',  ( -57.89159099828107458, -126.6875000013656063, -3.393966926194107447 ) ) ;
#30405 = CARTESIAN_POINT ( 'NONE',  ( -59.44456063193725015, -141.5625000013656063, -0.3552334253322034230 ) ) ;
#30406 = CARTESIAN_POINT ( 'NONE',  ( 9.457646018065525792E-16, -24.06249999863440436, 5.148502694627439702 ) ) ;
#30407 = CARTESIAN_POINT ( 'NONE',  ( -3.152548672688508926E-16, 5.187500001365592972, -5.148502694627439702 ) ) ;
#30408 = CARTESIAN_POINT ( 'NONE',  ( -2.229367062500000163, -62.72916666530106511, -3.861377020970580443 ) ) ;
#30409 = CARTESIAN_POINT ( 'NONE',  ( 2.500000000000002220, -48.54166666393547303, 4.330127018922192761 ) ) ;
#30410 = CARTESIAN_POINT ( 'NONE',  ( 4.458734124999998549, -21.72916666530107221, -2.574251347313721627 ) ) ;
#30411 = CARTESIAN_POINT ( 'NONE',  ( -1.339745962155610925, -32.79465819873851729, 5.000000000000000000 ) ) ;
#30412 = CARTESIAN_POINT ( 'NONE',  ( -3.535533905932737309, -149.6250000000000000, -3.535533905932738197 ) ) ;
#30413 = CARTESIAN_POINT ( 'NONE',  ( 5.000000000000000888, -12.58333333333333570, 2.886751345948126879 ) ) ;
#30414 = CARTESIAN_POINT ( 'NONE',  ( -1.846868145590734756, -154.1250000013656063, -4.458734125000000326 ) ) ;
#30415 = ORIENTED_EDGE ( 'NONE', *, *, #54183, .T. ) ;
#30416 = CARTESIAN_POINT ( 'NONE',  ( 9.457646018065525792E-16, -48.31249999863440792, 5.148502694627439702 ) ) ;
#30417 = CARTESIAN_POINT ( 'NONE',  ( -2.500000000000000444, 25.83333333333333215, -4.330127018922193649 ) ) ;
#30418 = CARTESIAN_POINT ( 'NONE',  ( 2.499999999999998668, -90.33333333333332860, -4.330127018922193649 ) ) ;
#30419 = CARTESIAN_POINT ( 'NONE',  ( -4.458734124999999437, -88.39583333196773651, -2.574251347313719407 ) ) ;
#30420 = CARTESIAN_POINT ( 'NONE',  ( -4.458734124999998549, 2.770833334698928674, 2.574251347313722516 ) ) ;
#30421 = CARTESIAN_POINT ( 'NONE',  ( 1.339745962155615144, -82.70534180126146850, 4.999999999999999112 ) ) ;
#30422 = CARTESIAN_POINT ( 'NONE',  ( 2.500000000000002220, 13.33333333333333215, 4.330127018922192761 ) ) ;
#30423 = CARTESIAN_POINT ( 'NONE',  ( -51.75738570946856498, -155.0000000000000284, 3.805975901505577408 ) ) ;
#30424 = CARTESIAN_POINT ( 'NONE',  ( 4.458734124999999437, 18.93750000136559564, -5.460374474430324690E-16 ) ) ;
#30425 = CARTESIAN_POINT ( 'NONE',  ( 2.500000000000002220, -77.66666666666665719, 4.330127018922192761 ) ) ;
#30426 = CARTESIAN_POINT ( 'NONE',  ( -3.535250795749689387E-16, 5.875000002731185056, -5.773502691896257311 ) ) ;
#30427 = ORIENTED_EDGE ( 'NONE', *, *, #44530, .T. ) ;
#30428 = CARTESIAN_POINT ( 'NONE',  ( 2.500000000000002220, -80.54166666393547303, 4.330127018922192761 ) ) ;
#30429 = ORIENTED_EDGE ( 'NONE', *, *, #20933, .F. ) ;
#30430 = CARTESIAN_POINT ( 'NONE',  ( 1.339745962155612702, -85.29465819873851729, -5.000000000000000000 ) ) ;
#30431 = CARTESIAN_POINT ( 'NONE',  ( -2.229367062499996610, -38.14583333196773651, 3.861377020970582219 ) ) ;
#30432 = CIRCLE ( 'NONE', #58170, 5.000000000000000000 ) ;
#30433 = CARTESIAN_POINT ( 'NONE',  ( 5.000000000000000888, -37.45833333060213732, 2.886751345948126879 ) ) ;
#30434 = ORIENTED_EDGE ( 'NONE', *, *, #13335, .F. ) ;
#30435 = CARTESIAN_POINT ( 'NONE',  ( -4.458734124999999437, -13.31249999863440259, 0.000000000000000000 ) ) ;
#30436 = ORIENTED_EDGE ( 'NONE', *, *, #34637, .F. ) ;
#30437 =( BOUNDED_CURVE ( )  B_SPLINE_CURVE ( 2, ( #14856, #19691, #53161, #4900, #13918, #54099, #53782, #33232, #5221 ),
 .UNSPECIFIED., .F., .F. ) 
 B_SPLINE_CURVE_WITH_KNOTS ( ( 3, 2, 2, 2, 3 ),
 ( 0.1416666666666667740, 0.1458333333333334814, 0.1500000000000001332, 0.1541666666666668406, 0.1583333333333334925 ),
 .UNSPECIFIED. ) 
 CURVE ( )  GEOMETRIC_REPRESENTATION_ITEM ( )  RATIONAL_B_SPLINE_CURVE ( ( 0.9999999999999980016, 0.9238795325112887369, 1.000000000000000000, 0.9238795325112867385, 1.000000000000000000, 0.9238795325112867385, 1.000000000000000000, 0.9238795325112837409, 1.000000000000003109 ) ) 
 REPRESENTATION_ITEM ( '' )  );
#30438 = CARTESIAN_POINT ( 'NONE',  ( -2.499999999999996447, -80.83333333333332860, 4.330127018922195425 ) ) ;
#30439 = CARTESIAN_POINT ( 'NONE',  ( 1.846868145590736310, -168.6250000013655779, 4.458734124999999437 ) ) ;
#30440 =( BOUNDED_CURVE ( )  B_SPLINE_CURVE ( 2, ( #30900, #50528, #36680, #1653, #56314, #6470, #7103, #40859, #16430 ),
 .UNSPECIFIED., .F., .F. ) 
 B_SPLINE_CURVE_WITH_KNOTS ( ( 3, 2, 2, 2, 3 ),
 ( 0.7839285714285714191, 0.7845238095238095122, 0.7857142857142856984, 0.7869047619047618847, 0.7874999999999999778 ),
 .UNSPECIFIED. ) 
 CURVE ( )  GEOMETRIC_REPRESENTATION_ITEM ( )  RATIONAL_B_SPLINE_CURVE ( ( 0.9330127018922194093, 0.9330127018922194093, 1.000000000000000000, 0.8660254037844387076, 1.000000000000000000, 0.8660254037844387076, 1.000000000000000000, 0.9330127018922194093, 0.9330127018922194093 ) ) 
 REPRESENTATION_ITEM ( '' )  );
#30441 = CARTESIAN_POINT ( 'NONE',  ( -3.535250795749689387E-16, -85.12499999726881583, -5.773502691896257311 ) ) ;
#30443 = ORIENTED_EDGE ( 'NONE', *, *, #29563, .T. ) ;
#30442 = CARTESIAN_POINT ( 'NONE',  ( 3.061616997868383141E-16, -144.8750000027312126, -5.000000000000000000 ) ) ;
#30444 = CARTESIAN_POINT ( 'NONE',  ( -53.33387254593733928, -142.8125000000000568, 5.149110718188519620 ) ) ;
#30445 = CARTESIAN_POINT ( 'NONE',  ( 2.229367062500001939, -27.22916666530106866, 3.861377020970579999 ) ) ;
#30446 = CARTESIAN_POINT ( 'NONE',  ( -2.499999999999996447, -83.83333333333332860, 4.330127018922195425 ) ) ;
#30447 = VERTEX_POINT ( 'NONE', #16400 ) ;
#30448 = EDGE_CURVE ( 'NONE', #29631, #27636, #50120, .T. ) ;
#30449 = APPLICATION_PROTOCOL_DEFINITION ( 'draft international standard', 'automotive_design', 1998, #29797 ) ;
#30450 = CARTESIAN_POINT ( 'NONE',  ( 4.458734125000000326, -162.6250000013655779, -1.846868145590734978 ) ) ;
#30451 = CARTESIAN_POINT ( 'NONE',  ( -4.458734124999999437, 27.60416666803226349, -2.574251347313719407 ) ) ;
#30452 = CARTESIAN_POINT ( 'NONE',  ( -1.339745962155613812, -39.08034179853028434, -5.000000000000000000 ) ) ;
#30453 = ORIENTED_EDGE ( 'NONE', *, *, #12655, .T. ) ;
#30454 = CARTESIAN_POINT ( 'NONE',  ( -51.60603307380591787, -147.1875000013656063, -2.891590998281053704 ) ) ;
#30455 = CARTESIAN_POINT ( 'NONE',  ( -4.458734124999999437, -75.64583333196775072, -2.574251347313719407 ) ) ;
#30456 = CARTESIAN_POINT ( 'NONE',  ( -58.80597590150559739, -133.1250000027312126, 3.242614290531460330 ) ) ;
#30457 = CARTESIAN_POINT ( 'NONE',  ( -4.458734124999999437, -41.39583333196773651, -2.574251347313719407 ) ) ;
#30458 = CARTESIAN_POINT ( 'NONE',  ( -4.458734124999999437, -143.1875000013656063, -5.460374474430324690E-16 ) ) ;
#30459 = CARTESIAN_POINT ( 'NONE',  ( -2.499999999999996447, 23.16666666666666430, 4.330127018922195425 ) ) ;
#30460 = CARTESIAN_POINT ( 'NONE',  ( -4.458734124999999437, -51.31249999863440792, 0.000000000000000000 ) ) ;
#30461 = CARTESIAN_POINT ( 'NONE',  ( 5.000000000000000888, 2.541666669397851130, 2.886751345948126879 ) ) ;
#30462 = CARTESIAN_POINT ( 'NONE',  ( -4.458734124999998549, -18.22916666530107221, 2.574251347313722516 ) ) ;
#30463 = CARTESIAN_POINT ( 'NONE',  ( 2.499999999999998668, -103.3333333333333286, -4.330127018922193649 ) ) ;
#30464 = CARTESIAN_POINT ( 'NONE',  ( -9.184850993605147944E-16, -167.2500000000000000, 5.000000000000000000 ) ) ;
#30465 = CARTESIAN_POINT ( 'NONE',  ( -2.229367062500000163, -33.72916666530107221, -3.861377020970580443 ) ) ;
#30466 = CARTESIAN_POINT ( 'NONE',  ( 5.000000000000000000, 8.708333336064518093, -2.886751345948129988 ) ) ;
#30467 = CARTESIAN_POINT ( 'NONE',  ( -2.500000000000000444, -53.16666666666666430, -4.330127018922193649 ) ) ;
#30468 = CARTESIAN_POINT ( 'NONE',  ( -53.51423613279429503, -128.2500000013656063, 4.591703134518082763 ) ) ;
#30469 =( BOUNDED_CURVE ( )  B_SPLINE_CURVE ( 2, ( #17783, #23568, #43163, #37402, #62802, #57038, #22942, #22302, #8145 ),
 .UNSPECIFIED., .F., .F. ) 
 B_SPLINE_CURVE_WITH_KNOTS ( ( 3, 2, 2, 2, 3 ),
 ( 0.3145833333333333259, 0.3152777777777777679, 0.3166666666666666519, 0.3180555555555555358, 0.3187499999999999778 ),
 .UNSPECIFIED. ) 
 CURVE ( )  GEOMETRIC_REPRESENTATION_ITEM ( )  RATIONAL_B_SPLINE_CURVE ( ( 0.9330127018922194093, 0.9330127018922194093, 1.000000000000000000, 0.8660254037844387076, 1.000000000000000000, 0.8660254037844387076, 1.000000000000000000, 0.9330127018922194093, 0.9330127018922194093 ) ) 
 REPRESENTATION_ITEM ( '' )  );
#30470 = CARTESIAN_POINT ( 'NONE',  ( -2.229367062500000163, -72.72916666530107932, -3.861377020970580443 ) ) ;
#30471 = CARTESIAN_POINT ( 'NONE',  ( -2.071067811865520358, -139.4375000027311842, 4.999999999999957367 ) ) ;
#30472 = CYLINDRICAL_SURFACE ( 'NONE', #57141, 5.000000000000000000 ) ;
#30473 = CARTESIAN_POINT ( 'NONE',  ( 2.229367062500001939, -0.2291666653010705768, 3.861377020970579999 ) ) ;
#30474 = ORIENTED_EDGE ( 'NONE', *, *, #16235, .F. ) ;
#30475 = AXIS2_PLACEMENT_3D ( 'NONE', #37868, #48452, #42997 ) ;
#30476 = CARTESIAN_POINT ( 'NONE',  ( 2.500000000000002220, -30.66666666666666785, 4.330127018922192761 ) ) ;
#30477 = CARTESIAN_POINT ( 'NONE',  ( 1.975475456537005874E-15, -15.75000000000000000, 5.000000000000000000 ) ) ;
#30479 = CARTESIAN_POINT ( 'NONE',  ( 4.458734124999999437, -37.81249999863440792, -5.460374474430324690E-16 ) ) ;
#30478 = CARTESIAN_POINT ( 'NONE',  ( 4.458734124999998549, -88.72916666530106511, -2.574251347313721627 ) ) ;
#30480 = CARTESIAN_POINT ( 'NONE',  ( -1.049326080737009628E-13, -4.750000000000003553, 5.000000000000000000 ) ) ;
#30481 = CARTESIAN_POINT ( 'NONE',  ( 4.458734124999998549, -83.97916666530107932, -2.574251347313721627 ) ) ;
#30482 = CARTESIAN_POINT ( 'NONE',  ( 9.457646018065525792E-16, 15.68750000136559564, 5.148502694627439702 ) ) ;
#30483 = DIRECTION ( 'NONE',  ( 0.000000000000000000, 0.000000000000000000, 1.000000000000000000 ) ) ;
#30484 = VECTOR ( 'NONE', #44640, 1000.000000000000000 ) ;
#30485 = CARTESIAN_POINT ( 'NONE',  ( -55.35523342533222291, -139.3125000013656063, 4.444560631937231499 ) ) ;
#30486 = VECTOR ( 'NONE', #28587, 1000.000000000000114 ) ;
#30487 = CARTESIAN_POINT ( 'NONE',  ( -4.458734124999999437, -3.395833331967739177, -2.574251347313719407 ) ) ;
#30488 = CARTESIAN_POINT ( 'NONE',  ( -3.152548672688508926E-16, 24.18750000136559564, -5.148502694627439702 ) ) ;
#30489 = CARTESIAN_POINT ( 'NONE',  ( 4.458734124999998549, -46.97916666530106511, -2.574251347313721627 ) ) ;
#30490 = CARTESIAN_POINT ( 'NONE',  ( -4.999999999999998224, -50.79166666393547303, 2.886751345948131764 ) ) ;
#30491 = CARTESIAN_POINT ( 'NONE',  ( 4.458734124999998549, -87.72916666530107932, -2.574251347313721627 ) ) ;
#30492 = CARTESIAN_POINT ( 'NONE',  ( 2.229367062499998831, -3.645833331967739177, -3.861377020970580887 ) ) ;
#30493 = ORIENTED_EDGE ( 'NONE', *, *, #61761, .F. ) ;
#30494 = CARTESIAN_POINT ( 'NONE',  ( -4.458734124999997661, -29.47916666530106866, 2.574251347313722516 ) ) ;
#30495 =( BOUNDED_CURVE ( )  B_SPLINE_CURVE ( 2, ( #60029, #59379, #15313, #34935, #54556, #10479, #30092, #5668, #25280 ),
 .UNSPECIFIED., .F., .F. ) 
 B_SPLINE_CURVE_WITH_KNOTS ( ( 3, 2, 2, 2, 3 ),
 ( 0.6104166666666667185, 0.6111111111111111605, 0.6125000000000000444, 0.6138888888888889284, 0.6145833333333333703 ),
 .UNSPECIFIED. ) 
 CURVE ( )  GEOMETRIC_REPRESENTATION_ITEM ( )  RATIONAL_B_SPLINE_CURVE ( ( 0.9330127018922194093, 0.9330127018922194093, 1.000000000000000000, 0.8660254037844387076, 1.000000000000000000, 0.8660254037844387076, 1.000000000000000000, 0.9330127018922194093, 0.9330127018922194093 ) ) 
 REPRESENTATION_ITEM ( '' )  );
#30496 = CARTESIAN_POINT ( 'NONE',  ( -50.40829686548195099, -133.2500000013656347, -1.485763867205728284 ) ) ;
#30497 = CARTESIAN_POINT ( 'NONE',  ( -4.458734124999999437, -76.31249999863440792, 0.000000000000000000 ) ) ;
#30498 = CARTESIAN_POINT ( 'NONE',  ( 2.229367062499998831, 29.10416666803225993, -3.861377020970580887 ) ) ;
#30499 = CARTESIAN_POINT ( 'NONE',  ( -4.458734124999998549, 21.77083333469892779, 2.574251347313722516 ) ) ;
#30500 = CARTESIAN_POINT ( 'NONE',  ( 6.123233995736766282E-16, -170.0000000000000000, -5.000000000000000000 ) ) ;
#30501 = CARTESIAN_POINT ( 'NONE',  ( 2.229367062499998831, -109.8958333319677365, -3.861377020970580887 ) ) ;
#30502 = CARTESIAN_POINT ( 'NONE',  ( -3.152548672688508926E-16, -76.81249999863440792, -5.148502694627439702 ) ) ;
#30503 = CARTESIAN_POINT ( 'NONE',  ( -5.000000000000000000, -57.99999999999999289, 0.000000000000000000 ) ) ;
#30504 = CARTESIAN_POINT ( 'NONE',  ( -51.19402409849444524, -151.5000000000000284, -3.242614290531456334 ) ) ;
#30505 = CARTESIAN_POINT ( 'NONE',  ( 2.499999999999998668, 21.79166666939785202, -4.330127018922193649 ) ) ;
#30506 = ORIENTED_EDGE ( 'NONE', *, *, #30353, .T. ) ;
#30507 = CARTESIAN_POINT ( 'NONE',  ( -2.500000000000000444, -73.04166666393548724, -4.330127018922193649 ) ) ;
#30509 = CARTESIAN_POINT ( 'NONE',  ( -3.535250795749689387E-16, -16.25000000000000000, -5.773502691896257311 ) ) ;
#30508 = FACE_OUTER_BOUND ( 'NONE', #26735, .T. ) ;
#30510 = CARTESIAN_POINT ( 'NONE',  ( -4.458734124999999437, -23.31249999863440436, 0.000000000000000000 ) ) ;
#30511 = CARTESIAN_POINT ( 'NONE',  ( 4.458734125000000326, -84.89583333196773651, 2.574251347313718519 ) ) ;
#30512 = CARTESIAN_POINT ( 'NONE',  ( 5.000000000000000000, -24.29166666393548368, -2.886751345948129988 ) ) ;
#30514 = ORIENTED_EDGE ( 'NONE', *, *, #8142, .F. ) ;
#30513 = CARTESIAN_POINT ( 'NONE',  ( 4.458734125000001214, -56.89583333196774362, 2.574251347313718519 ) ) ;
#30515 = DIRECTION ( 'NONE',  ( -0.000000000000000000, 1.000000000000000000, -0.000000000000000000 ) ) ;
#30516 = CARTESIAN_POINT ( 'NONE',  ( -1.339745962155613812, 10.91965820146970678, -5.000000000000000000 ) ) ;
#30518 = ORIENTED_EDGE ( 'NONE', *, *, #16216, .T. ) ;
#30517 = CARTESIAN_POINT ( 'NONE',  ( 2.229367062499998831, -5.895833331967740953, -3.861377020970580887 ) ) ;
#30519 = CARTESIAN_POINT ( 'NONE',  ( -59.44456063193725015, -150.5625000013656063, -0.3552334253322034230 ) ) ;
#30520 = CARTESIAN_POINT ( 'NONE',  ( 5.000000000000000000, -64.41666666666667140, -2.886751345948129988 ) ) ;
#30521 = CARTESIAN_POINT ( 'NONE',  ( 1.846868145590735200, -150.5000000013656347, -4.458734125000000326 ) ) ;
#30522 = CARTESIAN_POINT ( 'NONE',  ( 4.458734124999999437, -46.06249999863440081, -5.460374474430324690E-16 ) ) ;
#30523 = CARTESIAN_POINT ( 'NONE',  ( 6.123233995736766282E-16, -120.0000000000000000, -5.000000000000000000 ) ) ;
#30524 = CARTESIAN_POINT ( 'NONE',  ( 3.535533905932736864, -159.1250000000000284, 3.535533905932738641 ) ) ;
#30525 = FACE_OUTER_BOUND ( 'NONE', #48923, .T. ) ;
#30526 = CARTESIAN_POINT ( 'NONE',  ( -51.75738570946856498, -151.7500000000000284, 3.805975901505576964 ) ) ;
#30527 = CARTESIAN_POINT ( 'NONE',  ( 4.458734124999999437, -11.06249999863440792, -5.460374474430324690E-16 ) ) ;
#30528 = VECTOR ( 'NONE', #60165, 1000.000000000000000 ) ;
#30529 = CARTESIAN_POINT ( 'NONE',  ( -4.458734124999999437, -51.64583333196773651, -2.574251347313719407 ) ) ;
#30530 = CARTESIAN_POINT ( 'NONE',  ( -56.66612745406293783, -136.4375000027312126, -5.149110718188535607 ) ) ;
#30531 = CARTESIAN_POINT ( 'NONE',  ( 3.152801135295367541, -145.3125000013655779, -3.152801135295367541 ) ) ;
#30532 = AXIS2_PLACEMENT_3D ( 'NONE', #3043, #12986, #61262 ) ;
#30533 = CARTESIAN_POINT ( 'NONE',  ( -2.229367062499996610, -95.39583333196773651, 3.861377020970582219 ) ) ;
#30534 = CARTESIAN_POINT ( 'NONE',  ( 0.000000000000000000, -120.0000000000000000, 5.000000000000000000 ) ) ;
#30535 = ORIENTED_EDGE ( 'NONE', *, *, #27896, .T. ) ;
#30536 = CARTESIAN_POINT ( 'NONE',  ( 1.975475456537005874E-15, -71.62499999726878741, 5.000000000000000000 ) ) ;
#30537 = CARTESIAN_POINT ( 'NONE',  ( 9.457646018065525792E-16, 27.68750000136559208, 5.148502694627439702 ) ) ;
#30538 = CARTESIAN_POINT ( 'NONE',  ( -51.75738570946856498, -147.8750000027312126, 3.805975901505576964 ) ) ;
#30539 = CARTESIAN_POINT ( 'NONE',  ( 7.922281120364393914, 4.573931137438269623, -8.047472243342930653 ) ) ;
#30540 = VERTEX_POINT ( 'NONE', #10926 ) ;
#30541 = CARTESIAN_POINT ( 'NONE',  ( 4.458734124999999437, 0.1875000013655953035, -5.460374474430324690E-16 ) ) ;
#30542 = CARTESIAN_POINT ( 'NONE',  ( 2.229367062499998831, -17.89583333196773651, -3.861377020970580887 ) ) ;
#30543 = CARTESIAN_POINT ( 'NONE',  ( 5.000000000000000888, 11.54166666939785202, 2.886751345948126879 ) ) ;
#30544 = CARTESIAN_POINT ( 'NONE',  ( -3.152548672688508926E-16, -5.562499998634402587, -5.148502694627439702 ) ) ;
#30545 = CARTESIAN_POINT ( 'NONE',  ( 1.975475456537005874E-15, -77.62499999726881583, 5.000000000000000000 ) ) ;
#30546 = CARTESIAN_POINT ( 'NONE',  ( 2.730187237215162345E-16, -147.1875000013656063, -4.458734124999999437 ) ) ;
#30547 = CARTESIAN_POINT ( 'NONE',  ( 4.458734125000000326, 16.85416666803225993, 2.574251347313718519 ) ) ;
#30548 = ORIENTED_EDGE ( 'NONE', *, *, #39010, .F. ) ;
#30549 = CARTESIAN_POINT ( 'NONE',  ( 3.061616997868383141E-16, -164.8750000027311842, -5.000000000000000000 ) ) ;
#30550 = CARTESIAN_POINT ( 'NONE',  ( -9.184850993605147944E-16, -147.3750000027312126, 5.000000000000000000 ) ) ;
#30551 = CARTESIAN_POINT ( 'NONE',  ( 4.458734124999999437, -20.81249999863440081, -5.460374474430324690E-16 ) ) ;
#30552 = ADVANCED_FACE ( 'NONE', ( #31184 ), #39548, .T. ) ;
#30553 = CARTESIAN_POINT ( 'NONE',  ( -2.480964764533239819E-13, -73.62499999726883004, 5.000000000000000000 ) ) ;
#30554 = CARTESIAN_POINT ( 'NONE',  ( -59.98410592259440222, -138.1250000000000284, -0.3983568153799752487 ) ) ;
#30555 = CARTESIAN_POINT ( 'NONE',  ( -59.59170313451811296, -149.5000000013655779, 1.485763867205729394 ) ) ;
#30556 = CARTESIAN_POINT ( 'NONE',  ( -5.000000000000000000, -48.87499999726880873, 0.000000000000000000 ) ) ;
#30557 = CARTESIAN_POINT ( 'NONE',  ( -2.499999999999996447, 21.29166666939785202, 4.330127018922195425 ) ) ;
#30558 = CARTESIAN_POINT ( 'NONE',  ( 4.458734125000000326, 14.10416666803226349, 2.574251347313718519 ) ) ;
#30559 = CARTESIAN_POINT ( 'NONE',  ( 1.339745962155612702, -35.29465819873851729, -5.000000000000000000 ) ) ;
#30560 = CARTESIAN_POINT ( 'NONE',  ( -55.00000000000002132, -155.0000000000000284, 1.734723475976807094E-15 ) ) ;
#30561 = CARTESIAN_POINT ( 'NONE',  ( 4.458734124999999437, 10.18750000136559386, -5.460374474430324690E-16 ) ) ;
#30562 = CARTESIAN_POINT ( 'NONE',  ( -4.458734124999999437, -69.31249999863439371, 0.000000000000000000 ) ) ;
#30563 = VERTEX_POINT ( 'NONE', #34738 ) ;
#30564 = CARTESIAN_POINT ( 'NONE',  ( 2.229367062499998831, -15.89583333196773651, -3.861377020970580887 ) ) ;
#30565 = VECTOR ( 'NONE', #340, 1000.000000000000000 ) ;
#30566 = CARTESIAN_POINT ( 'NONE',  ( 5.000000000000000888, 4.416666666666666075, 2.886751345948126879 ) ) ;
#30567 = CARTESIAN_POINT ( 'NONE',  ( 2.730187237215162345E-16, -164.1875000013655779, -4.458734124999999437 ) ) ;
#30568 = DIRECTION ( 'NONE',  ( 0.000000000000000000, 0.000000000000000000, -1.000000000000000000 ) ) ;
#30569 = CARTESIAN_POINT ( 'NONE',  ( 4.458734124999999437, -57.81249999863440081, -5.460374474430324690E-16 ) ) ;
#30570 = CARTESIAN_POINT ( 'NONE',  ( 5.000000000000000000, -95.29166666393547303, -2.886751345948129988 ) ) ;
#30571 = CIRCLE ( 'NONE', #57321, 10.12668159690567649 ) ;
#30572 = CARTESIAN_POINT ( 'NONE',  ( 2.229367062500001939, -35.97916666530107221, 3.861377020970579999 ) ) ;
#30573 =( BOUNDED_CURVE ( )  B_SPLINE_CURVE ( 2, ( #15168, #44108, #39599, #43791, #4560, #53454, #25134, #34792, #14523 ),
 .UNSPECIFIED., .F., .F. ) 
 B_SPLINE_CURVE_WITH_KNOTS ( ( 3, 2, 2, 2, 3 ),
 ( 0.4250000000000003220, 0.4291666666666669738, 0.4333333333333336812, 0.4375000000000003886, 0.4416666666666670404 ),
 .UNSPECIFIED. ) 
 CURVE ( )  GEOMETRIC_REPRESENTATION_ITEM ( )  RATIONAL_B_SPLINE_CURVE ( ( 0.9999999999999938938, 0.9238795325112928447, 1.000000000000000000, 0.9238795325112867385, 1.000000000000000000, 0.9238795325112867385, 1.000000000000000000, 0.9238795325112796331, 1.000000000000007105 ) ) 
 REPRESENTATION_ITEM ( '' )  );
#30574 = CARTESIAN_POINT ( 'NONE',  ( 0.000000000000000000, -170.0000000000000000, 5.000000000000000000 ) ) ;
#30575 = EDGE_CURVE ( 'NONE', #24664, #6571, #24196, .T. ) ;
#30576 = DIRECTION ( 'NONE',  ( 0.000000000000000000, 0.000000000000000000, 1.000000000000000000 ) ) ;
#30577 = CARTESIAN_POINT ( 'NONE',  ( -6.972266317189433020E-16, -69.24999999999998579, -5.000000000000000000 ) ) ;
#30578 = EDGE_CURVE ( 'NONE', #7254, #60295, #16465, .T. ) ;
#30579 = CARTESIAN_POINT ( 'NONE',  ( 5.000000000000000000, -16.37499999726881228, -6.123233995736766282E-16 ) ) ;
#30580 = CARTESIAN_POINT ( 'NONE',  ( 3.152801135295366208, -148.8125000013655779, 3.152801135295367985 ) ) ;
#30581 = CARTESIAN_POINT ( 'NONE',  ( 2.499999999999998668, -45.33333333333333570, -4.330127018922193649 ) ) ;
#30582 = CARTESIAN_POINT ( 'NONE',  ( 0.000000000000000000, -120.0000000000000000, 5.000000000000000000 ) ) ;
#30583 = CARTESIAN_POINT ( 'NONE',  ( -56.75196168792112417, -135.0000000000000853, -4.145498605701915196 ) ) ;
#30584 = ORIENTED_EDGE ( 'NONE', *, *, #34941, .T. ) ;
#30585 = CARTESIAN_POINT ( 'NONE',  ( -3.152548672688508926E-16, -104.5624999986343937, -5.148502694627439702 ) ) ;
#30586 = CARTESIAN_POINT ( 'NONE',  ( 4.458734125000001214, 2.854166668032259491, 2.574251347313718519 ) ) ;
#30587 = FACE_OUTER_BOUND ( 'NONE', #22616, .T. ) ;
#30588 = CARTESIAN_POINT ( 'NONE',  ( -4.999999999999999112, -2.916666666666664742, 2.886751345948131764 ) ) ;
#30589 = CARTESIAN_POINT ( 'NONE',  ( -3.152548672688508926E-16, -67.56249999863440792, -5.148502694627439702 ) ) ;
#30591 =( BOUNDED_CURVE ( )  B_SPLINE_CURVE ( 2, ( #53759, #4255, #9073, #23870, #48930, #10338, #38647, #25129, #9693 ),
 .UNSPECIFIED., .F., .F. ) 
 B_SPLINE_CURVE_WITH_KNOTS ( ( 3, 2, 2, 2, 3 ),
 ( 0.1910714285714285865, 0.1916666666666666796, 0.1928571428571428659, 0.1940476190476190521, 0.1946428571428571452 ),
 .UNSPECIFIED. ) 
 CURVE ( )  GEOMETRIC_REPRESENTATION_ITEM ( )  RATIONAL_B_SPLINE_CURVE ( ( 0.9330127018922194093, 0.9330127018922209636, 1.000000000000000000, 0.8660254037844387076, 1.000000000000000000, 0.8660254037844387076, 1.000000000000000000, 0.9330127018922194093, 0.9330127018922194093 ) ) 
 REPRESENTATION_ITEM ( '' )  );
#30590 = CYLINDRICAL_SURFACE ( 'NONE', #44143, 5.000000000000000000 ) ;
#30592 = CARTESIAN_POINT ( 'NONE',  ( 5.000000000000000000, -9.291666663935483683, -2.886751345948129988 ) ) ;
#30594 = ORIENTED_EDGE ( 'NONE', *, *, #55852, .T. ) ;
#30593 = CARTESIAN_POINT ( 'NONE',  ( 4.458734124999998549, -35.72916666530107221, -2.574251347313721627 ) ) ;
#30595 = FACE_OUTER_BOUND ( 'NONE', #55725, .T. ) ;
#30596 = CARTESIAN_POINT ( 'NONE',  ( 0.000000000000000000, -170.0000000000000000, 0.000000000000000000 ) ) ;
#30598 = ORIENTED_EDGE ( 'NONE', *, *, #50916, .F. ) ;
#30597 = CARTESIAN_POINT ( 'NONE',  ( -2.229367062500000163, 14.27083333469892601, -3.861377020970580443 ) ) ;
#30599 = CARTESIAN_POINT ( 'NONE',  ( -6.972266317189433020E-16, -36.12499999726880162, -5.000000000000000000 ) ) ;
#30600 = CARTESIAN_POINT ( 'NONE',  ( 5.000000000000000000, -52.50000000000000711, -6.123233995736766282E-16 ) ) ;
#30601 = CARTESIAN_POINT ( 'NONE',  ( 9.457646018065525792E-16, -32.31249999863440792, 5.148502694627439702 ) ) ;
#30602 = CARTESIAN_POINT ( 'NONE',  ( -2.500000000000000444, -42.04166666393548013, -4.330127018922193649 ) ) ;
#30603 = CARTESIAN_POINT ( 'NONE',  ( -2.229367062499996610, -75.14583333196773651, 3.861377020970582219 ) ) ;
#30604 = CARTESIAN_POINT ( 'NONE',  ( -1.846868145590734756, -140.3750000013656063, -4.458734125000000326 ) ) ;
#30605 = CARTESIAN_POINT ( 'NONE',  ( 4.458734124999999437, -81.81249999863440792, -5.460374474430324690E-16 ) ) ;
#30606 = CARTESIAN_POINT ( 'NONE',  ( -50.70258187064364108, -135.3750000013656063, 2.196230717870141014 ) ) ;
#30607 = CARTESIAN_POINT ( 'NONE',  ( -4.458734124999999437, -31.64583333196773651, -2.574251347313719407 ) ) ;
#30608 = ORIENTED_EDGE ( 'NONE', *, *, #53434, .F. ) ;
#30609 = ADVANCED_FACE ( 'NONE', ( #55072 ), #51206, .T. ) ;
#30610 = CARTESIAN_POINT ( 'NONE',  ( 5.000000000000000888, -20.45833333060214798, 2.886751345948126879 ) ) ;
#30611 = VERTEX_POINT ( 'NONE', #30935 ) ;
#30612 = CARTESIAN_POINT ( 'NONE',  ( -2.229367062500000163, -76.72916666530106511, -3.861377020970580443 ) ) ;
#30613 = CARTESIAN_POINT ( 'NONE',  ( -4.999999999999998224, 13.20833333606451987, 2.886751345948131764 ) ) ;
#30614 = ORIENTED_EDGE ( 'NONE', *, *, #2880, .F. ) ;
#30615 = CARTESIAN_POINT ( 'NONE',  ( 4.729367062499999719, -169.8437500006828031, 0.000000000000000000 ) ) ;
#30616 = VECTOR ( 'NONE', #29038, 1000.000000000000000 ) ;
#30617 = CARTESIAN_POINT ( 'NONE',  ( 1.975475456537005874E-15, -31.62499999726880873, 5.000000000000000000 ) ) ;
#30618 = CARTESIAN_POINT ( 'NONE',  ( 2.229367062499998831, -62.89583333196774362, -3.861377020970580887 ) ) ;
#30619 = AXIS2_PLACEMENT_3D ( 'NONE', #34616, #14053, #59396 ) ;
#30620 = CARTESIAN_POINT ( 'NONE',  ( -2.229367062499996610, -4.395833331967740065, 3.861377020970582219 ) ) ;
#30621 = ORIENTED_EDGE ( 'NONE', *, *, #9223, .T. ) ;
#30622 = LINE ( 'NONE', #1386, #27586 ) ;
#30623 = DIRECTION ( 'NONE',  ( 0.000000000000000000, 0.000000000000000000, 1.000000000000000000 ) ) ;
#30624 = CARTESIAN_POINT ( 'NONE',  ( -4.458734124999999437, 6.604166668032259047, -2.574251347313719407 ) ) ;
#30625 = CARTESIAN_POINT ( 'NONE',  ( -57.89159099828107458, -141.6875000013656063, -3.393966926194107447 ) ) ;
#30626 = CARTESIAN_POINT ( 'NONE',  ( 1.975475456537005874E-15, -27.62499999726881228, 5.000000000000000000 ) ) ;
#30627 = CARTESIAN_POINT ( 'NONE',  ( -4.458734124999999437, -163.0000000013655779, -1.846868145590735644 ) ) ;
#30628 = CARTESIAN_POINT ( 'NONE',  ( -2.499999999999996447, 19.29166666939785202, 4.330127018922195425 ) ) ;
#30629 = ORIENTED_EDGE ( 'NONE', *, *, #20817, .F. ) ;
#30630 = CARTESIAN_POINT ( 'NONE',  ( 4.458734125000000326, -79.89583333196773651, 2.574251347313718519 ) ) ;
#30631 = CARTESIAN_POINT ( 'NONE',  ( -1.339745962155610925, -96.79465819873851729, 5.000000000000000000 ) ) ;
#30632 = CARTESIAN_POINT ( 'NONE',  ( -2.229367062499996610, -5.145833331967740065, 3.861377020970582219 ) ) ;
#30633 = ADVANCED_FACE ( 'NONE', ( #1060 ), #50881, .T. ) ;
#30634 = DIRECTION ( 'NONE',  ( -0.000000000000000000, 1.000000000000000000, -0.000000000000000000 ) ) ;
#30635 = CARTESIAN_POINT ( 'NONE',  ( 1.975475456537005874E-15, -67.74999999999998579, 5.000000000000000000 ) ) ;
#30636 = CARTESIAN_POINT ( 'NONE',  ( 4.458734125000001214, -69.14583333196773651, 2.574251347313718519 ) ) ;
#30637 = CARTESIAN_POINT ( 'NONE',  ( 2.499999999999998668, -33.20833333060215153, -4.330127018922193649 ) ) ;
#30638 = CARTESIAN_POINT ( 'NONE',  ( 1.975475456537005874E-15, -28.74999999999999645, 5.000000000000000000 ) ) ;
#30639 = CARTESIAN_POINT ( 'NONE',  ( -5.000000000000000000, -40.99999999999999289, 0.000000000000000000 ) ) ;
#30640 = CARTESIAN_POINT ( 'NONE',  ( 1.339745962155615144, -104.7053418012614827, 4.999999999999999112 ) ) ;
#30641 = CARTESIAN_POINT ( 'NONE',  ( 4.458734125000000326, 27.10416666803225993, 2.574251347313718519 ) ) ;
#30642 = CARTESIAN_POINT ( 'NONE',  ( 4.458734124999998549, -53.72916666530106511, -2.574251347313721627 ) ) ;
#30643 = CARTESIAN_POINT ( 'NONE',  ( -4.458734124999997661, -32.47916666530106511, 2.574251347313722516 ) ) ;
#30644 = CARTESIAN_POINT ( 'NONE',  ( 2.229367062500001939, 1.770833334698927786, 3.861377020970579999 ) ) ;
#30645 =( BOUNDED_CURVE ( )  B_SPLINE_CURVE ( 2, ( #59783, #58807, #54629, #53985, #15708, #50447, #5101, #10553, #24719 ),
 .UNSPECIFIED., .F., .F. ) 
 B_SPLINE_CURVE_WITH_KNOTS ( ( 3, 2, 2, 2, 3 ),
 ( 0.5339285714285714191, 0.5345238095238095122, 0.5357142857142856984, 0.5369047619047618847, 0.5374999999999999778 ),
 .UNSPECIFIED. ) 
 CURVE ( )  GEOMETRIC_REPRESENTATION_ITEM ( )  RATIONAL_B_SPLINE_CURVE ( ( 0.9330127018922194093, 0.9330127018922194093, 1.000000000000000000, 0.8660254037844387076, 1.000000000000000000, 0.8660254037844387076, 1.000000000000000000, 0.9330127018922194093, 0.9330127018922194093 ) ) 
 REPRESENTATION_ITEM ( '' )  );
#30646 = CYLINDRICAL_SURFACE ( 'NONE', #43186, 5.000000000000000000 ) ;
#30647 = CARTESIAN_POINT ( 'NONE',  ( -4.999999999999999112, 23.08333333333332860, 2.886751345948131764 ) ) ;
#30648 = CARTESIAN_POINT ( 'NONE',  ( 2.071067811865476394, -145.3125000027312126, 5.000000000000000000 ) ) ;
#30650 = EDGE_CURVE ( 'NONE', #21128, #10962, #41526, .T. ) ;
#30649 = CARTESIAN_POINT ( 'NONE',  ( 1.339745962155615144, -33.58034179853029144, 4.999999999999999112 ) ) ;
#30651 = CARTESIAN_POINT ( 'NONE',  ( -4.458734124999998549, -40.22916666530107932, 2.574251347313722516 ) ) ;
#30652 = CARTESIAN_POINT ( 'NONE',  ( -5.000000000000000000, -73.95833333060214443, -2.886751345948128211 ) ) ;
#30653 = CARTESIAN_POINT ( 'NONE',  ( -52.10840900171896806, -142.4375000013656063, 3.393966926194110556 ) ) ;
#30654 = CARTESIAN_POINT ( 'NONE',  ( -6.972266317189433020E-16, -76.12499999726880162, -5.000000000000000000 ) ) ;
#30655 = CARTESIAN_POINT ( 'NONE',  ( -6.972266317189433020E-16, 3.749999999999999556, -5.000000000000000000 ) ) ;
#30656 = ADVANCED_FACE ( 'NONE', ( #17100 ), #11627, .F. ) ;
#30657 = CARTESIAN_POINT ( 'NONE',  ( -4.458734124999997661, -78.47916666530106511, 2.574251347313722516 ) ) ;
#30658 = CARTESIAN_POINT ( 'NONE',  ( 4.458734124999999437, -162.6250000013656063, -1.846868145590734978 ) ) ;
#30659 = CARTESIAN_POINT ( 'NONE',  ( 6.123233995736766282E-16, -170.0000000000000000, -5.000000000000000000 ) ) ;
#30660 = DIRECTION ( 'NONE',  ( -0.000000000000000000, 1.000000000000000000, -0.000000000000000000 ) ) ;
#30661 = CARTESIAN_POINT ( 'NONE',  ( -2.500000000000000444, -28.16666666666666785, -4.330127018922193649 ) ) ;
#30662 = CARTESIAN_POINT ( 'NONE',  ( 3.152801135295366208, -140.5625000013655779, 3.152801135295367985 ) ) ;
#30663 = ORIENTED_EDGE ( 'NONE', *, *, #20453, .T. ) ;
#30664 = CARTESIAN_POINT ( 'NONE',  ( -4.458734124999998549, 20.52083333469892423, 2.574251347313722516 ) ) ;
#30666 = EDGE_CURVE ( 'NONE', #15028, #2754, #2064, .T. ) ;
#30665 = ORIENTED_EDGE ( 'NONE', *, *, #25677, .F. ) ;
#30667 = CARTESIAN_POINT ( 'NONE',  ( -4.458734124999999437, -59.64583333196775072, -2.574251347313719407 ) ) ;
#30668 = AXIS2_PLACEMENT_3D ( 'NONE', #49607, #44133, #48336 ) ;
#30669 = CARTESIAN_POINT ( 'NONE',  ( 5.000000000000000000, 23.62500000273118417, -6.123233995736766282E-16 ) ) ;
#30670 = CARTESIAN_POINT ( 'NONE',  ( -5.000000000000000000, -2.874999997268815832, 0.000000000000000000 ) ) ;
#30671 = CARTESIAN_POINT ( 'NONE',  ( -4.999999999999999112, 15.08333333333333215, 2.886751345948131764 ) ) ;
#30672 = AXIS2_PLACEMENT_3D ( 'NONE', #7910, #27515, #47145 ) ;
#30673 = CARTESIAN_POINT ( 'NONE',  ( -2.229367062499996610, -52.14583333196773651, 3.861377020970582219 ) ) ;
#30674 = CARTESIAN_POINT ( 'NONE',  ( -4.458734124999998549, -9.229166665301068662, 2.574251347313722516 ) ) ;
#30675 = CARTESIAN_POINT ( 'NONE',  ( 7.499999999998625100, 3.882635837268474166, -7.781684861371460649 ) ) ;
#30676 = DIRECTION ( 'NONE',  ( -0.000000000000000000, 1.000000000000000000, -0.000000000000000000 ) ) ;
#30677 = CARTESIAN_POINT ( 'NONE',  ( 1.339745962155615144, -1.705341801261478274, 4.999999999999999112 ) ) ;
#30678 = CARTESIAN_POINT ( 'NONE',  ( -1.975475456537005874E-15, 28.37500000273118772, 5.000000000000000000 ) ) ;
#30679 = CARTESIAN_POINT ( 'NONE',  ( 2.500000000000002220, -32.66666666666666430, 4.330127018922192761 ) ) ;
#30680 = CARTESIAN_POINT ( 'NONE',  ( 5.000000000000000888, -66.45833333060213022, 2.886751345948126879 ) ) ;
#30681 =( BOUNDED_CURVE ( )  B_SPLINE_CURVE ( 2, ( #44618, #43974, #34986, #11167, #19857 ),
 .UNSPECIFIED., .F., .F. ) 
 B_SPLINE_CURVE_WITH_KNOTS ( ( 3, 2, 3 ),
 ( 0.6583333333333329929, 0.6624999999999996447, 0.6666666666666662966 ),
 .UNSPECIFIED. ) 
 CURVE ( )  GEOMETRIC_REPRESENTATION_ITEM ( )  RATIONAL_B_SPLINE_CURVE ( ( 1.000000000000005995, 0.9238795325112806323, 1.000000000000000000, 0.9238795325112928447, 0.9999999999999938938 ) ) 
 REPRESENTATION_ITEM ( '' )  );
#30683 = CARTESIAN_POINT ( 'NONE',  ( -4.458734124999999437, -13.64583333196774007, -2.574251347313719407 ) ) ;
#30682 = CARTESIAN_POINT ( 'NONE',  ( -5.000000000000000000, -79.08333333333332860, -2.886751345948128211 ) ) ;
#30684 = CARTESIAN_POINT ( 'NONE',  ( -2.071067811865562991, -140.4375000027311842, 4.999999999999913847 ) ) ;
#30685 = CARTESIAN_POINT ( 'NONE',  ( 4.458734124999998549, -58.72916666530106511, -2.574251347313721627 ) ) ;
#30686 = CARTESIAN_POINT ( 'NONE',  ( 3.152801135295366208, -153.8125000013656063, 3.152801135295367985 ) ) ;
#30687 = ADVANCED_FACE ( 'NONE', ( #16146 ), #6188, .T. ) ;
#30688 = CARTESIAN_POINT ( 'NONE',  ( -2.229367062499996610, -66.14583333196773651, 3.861377020970582219 ) ) ;
#30689 = CARTESIAN_POINT ( 'NONE',  ( -5.000000000000000000, -53.95833333060214443, -2.886751345948128211 ) ) ;
#30690 = VERTEX_POINT ( 'NONE', #45737 ) ;
#30691 = CARTESIAN_POINT ( 'NONE',  ( 1.975475456537005874E-15, 13.37500000273118417, 5.000000000000000000 ) ) ;
#30692 = CARTESIAN_POINT ( 'NONE',  ( -2.229367062500000163, -0.7291666653010709931, -3.861377020970580443 ) ) ;
#30693 = ORIENTED_EDGE ( 'NONE', *, *, #16593, .F. ) ;
#30694 = CARTESIAN_POINT ( 'NONE',  ( -2.499999999999996447, -85.83333333333332860, 4.330127018922195425 ) ) ;
#30695 = CARTESIAN_POINT ( 'NONE',  ( -4.458734125000000326, -158.0000000013655779, -1.846868145590735644 ) ) ;
#30696 = ORIENTED_EDGE ( 'NONE', *, *, #43189, .F. ) ;
#30697 = DIRECTION ( 'NONE',  ( 0.000000000000000000, 0.000000000000000000, 1.000000000000000000 ) ) ;
#30698 = CARTESIAN_POINT ( 'NONE',  ( -52.53715891517739323, -128.4375000000000284, -4.819101127000233298 ) ) ;
#30699 = CARTESIAN_POINT ( 'NONE',  ( -4.458734124999998549, -50.47916666530107221, 2.574251347313722516 ) ) ;
#30700 = ORIENTED_EDGE ( 'NONE', *, *, #62327, .T. ) ;
#30701 = CARTESIAN_POINT ( 'NONE',  ( 5.275681513340003914E-14, 10.87500000273118239, -5.000000000000000000 ) ) ;
#30702 = CARTESIAN_POINT ( 'NONE',  ( 9.457646018065525792E-16, 11.93750000136559386, 5.148502694627439702 ) ) ;
#30703 = CARTESIAN_POINT ( 'NONE',  ( 2.229367062499998831, 22.35416666803225993, -3.861377020970580887 ) ) ;
#30704 = CARTESIAN_POINT ( 'NONE',  ( -55.35523342533222291, -151.3125000013656063, 4.444560631937231499 ) ) ;
#30705 = LINE ( 'NONE', #11402, #41830 ) ;
#30706 = AXIS2_PLACEMENT_3D ( 'NONE', #52665, #47214, #62650 ) ;
#30707 = CARTESIAN_POINT ( 'NONE',  ( 2.229367062500001939, -62.97916666530106511, 3.861377020970579999 ) ) ;
#30708 = CARTESIAN_POINT ( 'NONE',  ( -1.339745962155613812, 0.7946581987385198387, -5.000000000000000000 ) ) ;
#30709 = CARTESIAN_POINT ( 'NONE',  ( -4.458734124999999437, 14.60416666803226171, -2.574251347313719407 ) ) ;
#30710 = AXIS2_PLACEMENT_3D ( 'NONE', #29970, #60541, #16463 ) ;
#30711 = DIRECTION ( 'NONE',  ( -0.000000000000000000, -1.000000000000000000, -0.000000000000000000 ) ) ;
#30712 = EDGE_CURVE ( 'NONE', #51645, #30540, #11310, .T. ) ;
#30713 = CARTESIAN_POINT ( 'NONE',  ( 1.975475456537005874E-15, -26.74999999999999645, 5.000000000000000000 ) ) ;
#30714 = EDGE_CURVE ( 'NONE', #14857, #32214, #32848, .T. ) ;
#30715 = CARTESIAN_POINT ( 'NONE',  ( -3.152548672688508926E-16, -55.81249999863440081, -5.148502694627439702 ) ) ;
#30716 = CARTESIAN_POINT ( 'NONE',  ( -5.000000000000000000, -13.87499999726881228, 0.000000000000000000 ) ) ;
#30717 = CARTESIAN_POINT ( 'NONE',  ( 5.000000000000000000, -42.37499999726880873, -6.123233995736766282E-16 ) ) ;
#30718 = CARTESIAN_POINT ( 'NONE',  ( -4.458734124999998549, -87.47916666530107932, 2.574251347313722516 ) ) ;
#30719 = EDGE_CURVE ( 'NONE', #9561, #46354, #40582, .T. ) ;
#30720 = CARTESIAN_POINT ( 'NONE',  ( 5.000000000000000888, -104.4583333306021586, 2.886751345948126879 ) ) ;
#30721 = CARTESIAN_POINT ( 'NONE',  ( -2.229367062500000163, -16.72916666530107577, -3.861377020970580443 ) ) ;
#30722 = EDGE_LOOP ( 'NONE', ( #38092, #61473, #53550, #59329 ) ) ;
#30723 = CARTESIAN_POINT ( 'NONE',  ( 5.000000000000000000, 23.58333333333333215, -2.886751345948130876 ) ) ;
#30724 = CARTESIAN_POINT ( 'NONE',  ( -4.458734124999999437, -106.3958333319677507, -2.574251347313719407 ) ) ;
#30725 = CARTESIAN_POINT ( 'NONE',  ( -2.071067811865478170, -158.4375000027312126, 5.000000000000000000 ) ) ;
#30726 = ORIENTED_EDGE ( 'NONE', *, *, #10507, .T. ) ;
#30727 = CARTESIAN_POINT ( 'NONE',  ( -2.229367062499996610, -100.3958333319677365, 3.861377020970582219 ) ) ;
#30728 = CARTESIAN_POINT ( 'NONE',  ( -4.458734124999998549, -27.22916666530107221, 2.574251347313722516 ) ) ;
#30729 = CARTESIAN_POINT ( 'NONE',  ( 5.000000000000000888, -59.45833333060214443, 2.886751345948126879 ) ) ;
#30730 = EDGE_CURVE ( 'NONE', #12628, #55786, #59527, .T. ) ;
#30731 = CARTESIAN_POINT ( 'NONE',  ( -57.89159099828107458, -125.6875000013656063, -3.393966926194107447 ) ) ;
#30732 = CARTESIAN_POINT ( 'NONE',  ( -59.44456063193725015, -143.5625000013656063, -0.3552334253322034230 ) ) ;
#30733 = CARTESIAN_POINT ( 'NONE',  ( 4.458734124999999437, -23.81249999863440436, -5.460374474430324690E-16 ) ) ;
#30734 = EDGE_CURVE ( 'NONE', #48784, #52220, #61605, .T. ) ;
#30735 = CARTESIAN_POINT ( 'NONE',  ( 4.458734124999998549, -61.97916666530106511, -2.574251347313721627 ) ) ;
#30736 = CARTESIAN_POINT ( 'NONE',  ( 0.000000000000000000, -120.0000000000000000, 0.000000000000000000 ) ) ;
#30737 = CARTESIAN_POINT ( 'NONE',  ( -4.458734124999999437, -19.39583333196774007, -2.574251347313719407 ) ) ;
#30738 = CARTESIAN_POINT ( 'NONE',  ( 1.339745962155615144, -75.70534180126148271, 4.999999999999999112 ) ) ;
#30739 = CARTESIAN_POINT ( 'NONE',  ( -5.000000000000000000, -152.5000000000000284, -6.123233995736766282E-16 ) ) ;
#30740 = CARTESIAN_POINT ( 'NONE',  ( 5.000000000000000000, -11.41666666666666607, -2.886751345948129988 ) ) ;
#30741 = EDGE_CURVE ( 'NONE', #10944, #35151, #2631, .T. ) ;
#30742 = CARTESIAN_POINT ( 'NONE',  ( 1.846868145590736310, -150.6250000013655779, 4.458734124999999437 ) ) ;
#30743 = ORIENTED_EDGE ( 'NONE', *, *, #29899, .T. ) ;
#30744 = CARTESIAN_POINT ( 'NONE',  ( 2.229367062499998831, -47.89583333196774362, -3.861377020970580887 ) ) ;
#30745 = CARTESIAN_POINT ( 'NONE',  ( -5.000000000000000000, -37.99999999999999289, 0.000000000000000000 ) ) ;
#30746 = CARTESIAN_POINT ( 'NONE',  ( 75.00000000000000000, 15.00000000000000000, 8.999999999999998224 ) ) ;
#30747 = EDGE_CURVE ( 'NONE', #54588, #22588, #47938, .T. ) ;
#30748 = CARTESIAN_POINT ( 'NONE',  ( 5.000000000000000888, 29.41666666666666785, 2.886751345948126879 ) ) ;
#30749 = CARTESIAN_POINT ( 'NONE',  ( -2.229367062499996610, 3.854166668032260823, 3.861377020970582219 ) ) ;
#30750 = CARTESIAN_POINT ( 'NONE',  ( -6.972266317189433020E-16, -57.12499999726880162, -5.000000000000000000 ) ) ;
#30751 = CARTESIAN_POINT ( 'NONE',  ( 1.975475456537005874E-15, -41.62499999726880162, 5.000000000000000000 ) ) ;
#30752 = CARTESIAN_POINT ( 'NONE',  ( -6.972266317189433020E-16, -17.25000000000000000, -5.000000000000000000 ) ) ;
#30753 = CARTESIAN_POINT ( 'NONE',  ( 9.457646018065525792E-16, 13.68750000136559208, 5.148502694627439702 ) ) ;
#30754 = CARTESIAN_POINT ( 'NONE',  ( -3.535250795749689387E-16, -78.25000000000001421, -5.773502691896257311 ) ) ;
#30755 = CARTESIAN_POINT ( 'NONE',  ( -5.000000000000000000, 9.041666669397852019, -2.886751345948128211 ) ) ;
#30756 = VERTEX_POINT ( 'NONE', #62441 ) ;
#30757 = CARTESIAN_POINT ( 'NONE',  ( -6.972266317189433020E-16, 7.750000000000000000, -5.000000000000000000 ) ) ;
#30758 = ORIENTED_EDGE ( 'NONE', *, *, #62201, .F. ) ;
#30759 = LINE ( 'NONE', #50380, #17318 ) ;
#30760 = CARTESIAN_POINT ( 'NONE',  ( -3.152548672688508926E-16, -42.56249999863440792, -5.148502694627439702 ) ) ;
#30761 = CARTESIAN_POINT ( 'NONE',  ( -1.846868145590737420, -169.0000000013655779, 4.458734124999999437 ) ) ;
#30762 = CARTESIAN_POINT ( 'NONE',  ( -3.535250795749689387E-16, -39.12499999726880162, -5.773502691896257311 ) ) ;
#30763 = ORIENTED_EDGE ( 'NONE', *, *, #19972, .T. ) ;
#30764 = CARTESIAN_POINT ( 'NONE',  ( 2.229367062499998831, -20.64583333196774007, -3.861377020970580887 ) ) ;
#30765 = EDGE_LOOP ( 'NONE', ( #9712, #62661, #21384, #6823 ) ) ;
#30766 = CARTESIAN_POINT ( 'NONE',  ( 5.000000000000000000, -85.41666666666665719, -2.886751345948129988 ) ) ;
#30767 = CARTESIAN_POINT ( 'NONE',  ( -5.000000000000000000, 1.125000002731184390, 0.000000000000000000 ) ) ;
#30768 = CARTESIAN_POINT ( 'NONE',  ( -2.499999999999996447, -86.70833333060214443, 4.330127018922195425 ) ) ;
#30770 = VERTEX_POINT ( 'NONE', #27374 ) ;
#30769 = CARTESIAN_POINT ( 'NONE',  ( 2.493747252781420335E-13, -55.24999999999999289, -5.000000000000000000 ) ) ;
#30771 = CARTESIAN_POINT ( 'NONE',  ( -56.66612745406270335, -143.3125000000000284, -5.149110718188516067 ) ) ;
#30772 = CARTESIAN_POINT ( 'NONE',  ( -4.458734124999999437, -32.64583333196774362, -2.574251347313719407 ) ) ;
#30773 = LINE ( 'NONE', #24996, #57036 ) ;
#30774 = ORIENTED_EDGE ( 'NONE', *, *, #23952, .F. ) ;
#30775 =( BOUNDED_CURVE ( )  B_SPLINE_CURVE ( 2, ( #55174, #21074, #55498, #10781, #31032, #60643, #11093, #50982, #15287 ),
 .UNSPECIFIED., .F., .F. ) 
 B_SPLINE_CURVE_WITH_KNOTS ( ( 3, 2, 2, 2, 3 ),
 ( 0.2583333333333335813, 0.2625000000000002331, 0.2666666666666668850, 0.2708333333333335369, 0.2750000000000002442 ),
 .UNSPECIFIED. ) 
 CURVE ( )  GEOMETRIC_REPRESENTATION_ITEM ( )  RATIONAL_B_SPLINE_CURVE ( ( 0.9999999999999958922, 0.9238795325112908463, 1.000000000000000000, 0.9238795325112867385, 1.000000000000000000, 0.9238795325112867385, 1.000000000000000000, 0.9238795325112826307, 1.000000000000003997 ) ) 
 REPRESENTATION_ITEM ( '' )  );
#30776 = ITEM_DEFINED_TRANSFORMATION ( 'NONE', 'NONE', #4088,  #43054 ) ;
#30777 = CARTESIAN_POINT ( 'NONE',  ( 4.458734125000001214, -74.89583333196773651, 2.574251347313718519 ) ) ;
#30778 = CARTESIAN_POINT ( 'NONE',  ( 9.457646018065525792E-16, -109.3124999986343937, 5.148502694627439702 ) ) ;
#30779 = CARTESIAN_POINT ( 'NONE',  ( 1.339745962155615144, -23.70534180126148271, 4.999999999999999112 ) ) ;
#30780 = ORIENTED_EDGE ( 'NONE', *, *, #48712, .F. ) ;
#30781 = CARTESIAN_POINT ( 'NONE',  ( -9.184850993605147944E-16, -161.2500000000000000, 5.000000000000000000 ) ) ;
#30782 = CARTESIAN_POINT ( 'NONE',  ( -56.48576386720575471, -143.0000000013655779, -4.591703134518078322 ) ) ;
#30783 = CARTESIAN_POINT ( 'NONE',  ( 2.229367062500001939, -77.22916666530106511, 3.861377020970579999 ) ) ;
#30784 = CARTESIAN_POINT ( 'NONE',  ( -54.60164318462004474, -134.5000000027312126, -4.984105922594373794 ) ) ;
#30785 = CARTESIAN_POINT ( 'NONE',  ( 2.229367062499998831, -42.64583333196773651, -3.861377020970580887 ) ) ;
#30786 = CARTESIAN_POINT ( 'NONE',  ( -4.458734124999999437, -141.1875000013656063, -5.460374474430324690E-16 ) ) ;
#30787 = LINE ( 'NONE', #2483, #49726 ) ;
#30788 = CARTESIAN_POINT ( 'NONE',  ( -4.458734124999999437, -48.31249999863440792, 0.000000000000000000 ) ) ;
#30789 = CARTESIAN_POINT ( 'NONE',  ( -4.458734124999999437, -45.31249999863440081, 0.000000000000000000 ) ) ;
#30790 = FACE_OUTER_BOUND ( 'NONE', #22373, .T. ) ;
#30791 = CARTESIAN_POINT ( 'NONE',  ( 4.458734124999998549, -18.72916666530106866, -2.574251347313721627 ) ) ;
#30792 = CARTESIAN_POINT ( 'NONE',  ( 5.000000000000000000, -103.5000000000000142, -6.123233995736766282E-16 ) ) ;
#30793 = CARTESIAN_POINT ( 'NONE',  ( -4.458734125000000326, -140.2500000013656063, -1.846868145590735644 ) ) ;
#30794 = CARTESIAN_POINT ( 'NONE',  ( -4.458734124999998549, -37.47916666530107221, 2.574251347313722516 ) ) ;
#30795 = CARTESIAN_POINT ( 'NONE',  ( -2.500000000000000444, 6.958333336064520758, -4.330127018922193649 ) ) ;
#30796 = CARTESIAN_POINT ( 'NONE',  ( -5.000000000000000000, -39.87499999726880162, 0.000000000000000000 ) ) ;
#30797 = CARTESIAN_POINT ( 'NONE',  ( -54.64476657466781973, -127.8125000013655921, -4.444560631937228834 ) ) ;
#30798 = CARTESIAN_POINT ( 'NONE',  ( 9.457646018065525792E-16, -72.31249999863440792, 5.148502694627439702 ) ) ;
#30799 = DIRECTION ( 'NONE',  ( 0.000000000000000000, 0.000000000000000000, 1.000000000000000000 ) ) ;
#30800 = CARTESIAN_POINT ( 'NONE',  ( 5.000000000000000000, -30.29166666393547658, -2.886751345948130876 ) ) ;
#30801 = CARTESIAN_POINT ( 'NONE',  ( 2.229367062499998831, 1.104166668032261711, -3.861377020970580887 ) ) ;
#30802 = ORIENTED_EDGE ( 'NONE', *, *, #4992, .F. ) ;
#30803 = CARTESIAN_POINT ( 'NONE',  ( 5.000000000000000000, -30.41666666666666785, -2.886751345948130876 ) ) ;
#30805 = CARTESIAN_POINT ( 'NONE',  ( 4.458734124999999437, -32.81249999863440792, -5.460374474430324690E-16 ) ) ;
#30804 = CARTESIAN_POINT ( 'NONE',  ( 4.458734125000001214, -89.89583333196775072, 2.574251347313718519 ) ) ;
#30806 = CYLINDRICAL_SURFACE ( 'NONE', #57277, 5.000000000000000000 ) ;
#30807 = CARTESIAN_POINT ( 'NONE',  ( -4.458734124999999437, -80.64583333196773651, -2.574251347313719407 ) ) ;
#30808 = AXIS2_PLACEMENT_3D ( 'NONE', #13897, #58598, #14518 ) ;
#30809 = CARTESIAN_POINT ( 'NONE',  ( -4.458734124999997661, 15.52083333469892779, 2.574251347313722516 ) ) ;
#30810 = FACE_OUTER_BOUND ( 'NONE', #42461, .T. ) ;
#30811 = CARTESIAN_POINT ( 'NONE',  ( -57.19623071787017210, -136.3750000013656063, 4.297418129356382899 ) ) ;
#30812 = CARTESIAN_POINT ( 'NONE',  ( -2.229367062500000163, -8.479166665301073991, -3.861377020970580443 ) ) ;
#30813 = CARTESIAN_POINT ( 'NONE',  ( -4.458734124999998549, 21.52083333469893134, 2.574251347313722516 ) ) ;
#30814 = CARTESIAN_POINT ( 'NONE',  ( -4.458734124999997661, -49.47916666530107221, 2.574251347313722516 ) ) ;
#30815 = CARTESIAN_POINT ( 'NONE',  ( -2.499999999999996447, -50.70833333060213732, 4.330127018922195425 ) ) ;
#30816 = CARTESIAN_POINT ( 'NONE',  ( -4.458734124999998549, -87.22916666530107932, 2.574251347313722516 ) ) ;
#30817 = CARTESIAN_POINT ( 'NONE',  ( 9.457646018065525792E-16, -1.062499998634405696, 5.148502694627439702 ) ) ;
#30818 = CARTESIAN_POINT ( 'NONE',  ( 3.061616997868383141E-16, -168.8750000027312126, -5.000000000000000000 ) ) ;
#30819 = EDGE_CURVE ( 'NONE', #55230, #37557, #45995, .T. ) ;
#30820 = ORIENTED_EDGE ( 'NONE', *, *, #23259, .F. ) ;
#30821 = CARTESIAN_POINT ( 'NONE',  ( -4.458734124999999437, -28.56249999863440081, 0.000000000000000000 ) ) ;
#30822 = CARTESIAN_POINT ( 'NONE',  ( -59.44456063193725015, -133.8125000013656063, -0.3552334253322034230 ) ) ;
#30823 = EDGE_CURVE ( 'NONE', #6601, #45642, #4470, .T. ) ;
#30824 = CARTESIAN_POINT ( 'NONE',  ( 4.458734125000001214, -72.89583333196775072, 2.574251347313718519 ) ) ;
#30825 = CARTESIAN_POINT ( 'NONE',  ( -3.152548672688508926E-16, 29.18750000136559208, -5.148502694627439702 ) ) ;
#30826 = CARTESIAN_POINT ( 'NONE',  ( 2.229367062500001939, 19.02083333469892779, 3.861377020970579999 ) ) ;
#30827 = ADVANCED_FACE ( 'NONE', ( #2955 ), #2431, .F. ) ;
#30828 = FACE_OUTER_BOUND ( 'NONE', #22618, .T. ) ;
#30829 = CARTESIAN_POINT ( 'NONE',  ( -6.972266317189433020E-16, 1.750000000000000444, -5.000000000000000000 ) ) ;
#30830 = CARTESIAN_POINT ( 'NONE',  ( 4.458734125000000326, -77.14583333196775072, 2.574251347313718519 ) ) ;
#30831 = CARTESIAN_POINT ( 'NONE',  ( 1.060575238724906964E-15, -60.75000000000000000, 5.773502691896257311 ) ) ;
#30832 = CARTESIAN_POINT ( 'NONE',  ( -5.000000000000000000, 23.04166666939785557, -2.886751345948128211 ) ) ;
#30833 = EDGE_LOOP ( 'NONE', ( #17531, #21078, #24366, #10750 ) ) ;
#30834 = CARTESIAN_POINT ( 'NONE',  ( 2.500000000000002220, -1.541666663935480130, 4.330127018922192761 ) ) ;
#30835 =( BOUNDED_CURVE ( )  B_SPLINE_CURVE ( 2, ( #31531, #22214, #41811, #61457, #50843, #35734, #51485, #27341, #51795 ),
 .UNSPECIFIED., .F., .F. ) 
 B_SPLINE_CURVE_WITH_KNOTS ( ( 3, 2, 2, 2, 3 ),
 ( 0.1660714285714285643, 0.1666666666666666574, 0.1678571428571428437, 0.1690476190476190577, 0.1696428571428571508 ),
 .UNSPECIFIED. ) 
 CURVE ( )  GEOMETRIC_REPRESENTATION_ITEM ( )  RATIONAL_B_SPLINE_CURVE ( ( 0.9330127018922194093, 0.9330127018922194093, 1.000000000000000000, 0.8660254037844387076, 1.000000000000000000, 0.8660254037844387076, 1.000000000000000000, 0.9330127018922194093, 0.9330127018922194093 ) ) 
 REPRESENTATION_ITEM ( '' )  );
#30836 = CARTESIAN_POINT ( 'NONE',  ( 1.339745962155612702, -67.29465819873851729, -5.000000000000000000 ) ) ;
#30838 = CARTESIAN_POINT ( 'NONE',  ( 5.000000000000000888, -25.58333333333333215, 2.886751345948126879 ) ) ;
#30837 = CARTESIAN_POINT ( 'NONE',  ( -2.500000000000000444, -107.0416666639354730, -4.330127018922193649 ) ) ;
#30839 = CARTESIAN_POINT ( 'NONE',  ( -4.458734124999999437, -26.31249999863440792, 0.000000000000000000 ) ) ;
#30840 = CARTESIAN_POINT ( 'NONE',  ( -4.458734124999997661, -88.22916666530107932, 2.574251347313722516 ) ) ;
#30841 = CARTESIAN_POINT ( 'NONE',  ( -5.000000000000000000, -21.87499999726881228, 0.000000000000000000 ) ) ;
#30843 = ORIENTED_EDGE ( 'NONE', *, *, #61479, .F. ) ;
#30842 = CARTESIAN_POINT ( 'NONE',  ( 2.229367062500001939, -55.97916666530107221, 3.861377020970579999 ) ) ;
#30844 = CARTESIAN_POINT ( 'NONE',  ( 1.975475456537005874E-15, -49.74999999999999289, 5.000000000000000000 ) ) ;
#30846 = ORIENTED_EDGE ( 'NONE', *, *, #33485, .T. ) ;
#30845 = CARTESIAN_POINT ( 'NONE',  ( -3.152548672688508926E-16, -2.812499998634407028, -5.148502694627439702 ) ) ;
#30847 = CARTESIAN_POINT ( 'NONE',  ( 2.499999999999998668, -64.33333333333332860, -4.330127018922193649 ) ) ;
#30848 = CARTESIAN_POINT ( 'NONE',  ( -8.190561711645485556E-16, -153.9375000013655779, 4.458734124999999437 ) ) ;
#30849 = VECTOR ( 'NONE', #12765, 1000.000000000000000 ) ;
#30850 = CARTESIAN_POINT ( 'NONE',  ( 2.229367062500001939, -47.22916666530106511, 3.861377020970579999 ) ) ;
#30851 = CARTESIAN_POINT ( 'NONE',  ( -5.000000000000000000, -15.95833333060214443, -2.886751345948128211 ) ) ;
#30852 = CARTESIAN_POINT ( 'NONE',  ( 3.535533905932736864, -160.1250000000000284, 3.535533905932738641 ) ) ;
#30853 = CARTESIAN_POINT ( 'NONE',  ( -6.972266317189433020E-16, -38.12499999726880873, -5.000000000000000000 ) ) ;
#30854 = VECTOR ( 'NONE', #28045, 1000.000000000000000 ) ;
#30855 = CARTESIAN_POINT ( 'NONE',  ( -50.18089887299979068, -151.6875000000000284, 2.462841084822635640 ) ) ;
#30856 = CARTESIAN_POINT ( 'NONE',  ( -3.152548672688508926E-16, -13.81249999863440436, -5.148502694627439702 ) ) ;
#30857 = CARTESIAN_POINT ( 'NONE',  ( 4.458734124999998549, -50.97916666530107221, -2.574251347313721627 ) ) ;
#30858 = CARTESIAN_POINT ( 'NONE',  ( -1.336351044127974539E-14, 22.24999999999999645, 5.000000000000000000 ) ) ;
#30859 = CARTESIAN_POINT ( 'NONE',  ( -3.152801135295367096, -143.0625000013655779, -3.152801135295367541 ) ) ;
#30860 = CARTESIAN_POINT ( 'NONE',  ( 4.458734125000001214, -97.14583333196773651, 2.574251347313718519 ) ) ;
#30861 = CARTESIAN_POINT ( 'NONE',  ( -1.339745962155613812, -107.2053418012614543, -5.000000000000000000 ) ) ;
#30862 = VERTEX_POINT ( 'NONE', #22430 ) ;
#30863 = CARTESIAN_POINT ( 'NONE',  ( -5.000000000000000000, 14.12500000273118594, 0.000000000000000000 ) ) ;
#30864 = CARTESIAN_POINT ( 'NONE',  ( -2.229367062499996610, 25.60416666803225993, 3.861377020970582219 ) ) ;
#30865 = CARTESIAN_POINT ( 'NONE',  ( -55.39835681537999790, -148.0000000027312126, 4.984105922594378235 ) ) ;
#30866 = CARTESIAN_POINT ( 'NONE',  ( -4.999999999999998224, -12.79166666393547835, 2.886751345948131764 ) ) ;
#30867 = ORIENTED_EDGE ( 'NONE', *, *, #16065, .T. ) ;
#30868 = CARTESIAN_POINT ( 'NONE',  ( -4.458734124999998549, -3.229166665301069994, 2.574251347313722516 ) ) ;
#30869 = ADVANCED_FACE ( 'NONE', ( #42027 ), #17601, .T. ) ;
#30870 = CARTESIAN_POINT ( 'NONE',  ( -6.972266317189433020E-16, 22.87500000273118417, -5.000000000000000000 ) ) ;
#30871 = CARTESIAN_POINT ( 'NONE',  ( 2.229367062500001939, -16.22916666530107577, 3.861377020970579999 ) ) ;
#30872 = CARTESIAN_POINT ( 'NONE',  ( -1.339745962155613812, -101.0803417985302843, -5.000000000000000000 ) ) ;
#30873 = CARTESIAN_POINT ( 'NONE',  ( 4.458734124999998549, -5.729166665301072214, -2.574251347313721627 ) ) ;
#30874 = CARTESIAN_POINT ( 'NONE',  ( 5.000000000000000000, 6.708333336064521646, -2.886751345948130876 ) ) ;
#30875 = CARTESIAN_POINT ( 'NONE',  ( -4.458734124999999437, -147.9375000013656063, -5.460374474430324690E-16 ) ) ;
#30876 =( BOUNDED_CURVE ( )  B_SPLINE_CURVE ( 2, ( #1591, #16685, #36305, #31462, #62339, #47225, #56883, #47528, #24583 ),
 .UNSPECIFIED., .F., .F. ) 
 B_SPLINE_CURVE_WITH_KNOTS ( ( 3, 2, 2, 2, 3 ),
 ( 0.6589285714285714191, 0.6595238095238095122, 0.6607142857142856984, 0.6619047619047618847, 0.6624999999999999778 ),
 .UNSPECIFIED. ) 
 CURVE ( )  GEOMETRIC_REPRESENTATION_ITEM ( )  RATIONAL_B_SPLINE_CURVE ( ( 0.9330127018922194093, 0.9330127018922194093, 1.000000000000000000, 0.8660254037844387076, 1.000000000000000000, 0.8660254037844387076, 1.000000000000000000, 0.9330127018922194093, 0.9330127018922194093 ) ) 
 REPRESENTATION_ITEM ( '' )  );
#30877 = CARTESIAN_POINT ( 'NONE',  ( -3.152548672688508926E-16, 16.18750000136559564, -5.148502694627439702 ) ) ;
#30878 = EDGE_LOOP ( 'NONE', ( #37091, #10600, #26219, #17084 ) ) ;
#30879 = CARTESIAN_POINT ( 'NONE',  ( 0.000000000000000000, -120.0000000000000000, 0.000000000000000000 ) ) ;
#30880 = CARTESIAN_POINT ( 'NONE',  ( -6.972266317189433020E-16, -13.25000000000000000, -5.000000000000000000 ) ) ;
#30881 = CARTESIAN_POINT ( 'NONE',  ( 4.458734124999998549, -19.72916666530107221, -2.574251347313721627 ) ) ;
#30882 = CARTESIAN_POINT ( 'NONE',  ( -51.75738570946856498, -137.7500000000000000, 3.805975901505576964 ) ) ;
#30883 = CARTESIAN_POINT ( 'NONE',  ( -50.40829686548195099, -150.0000000013655779, -1.485763867205728284 ) ) ;
#30884 = CARTESIAN_POINT ( 'NONE',  ( 5.000000000000000000, -45.37499999726880873, -6.123233995736766282E-16 ) ) ;
#30885 = CARTESIAN_POINT ( 'NONE',  ( -7.549004593702452581, 4.358419834287830419, -7.700121441565820568 ) ) ;
#30886 = CARTESIAN_POINT ( 'NONE',  ( -3.152548672688508926E-16, 7.437500001365594748, -5.148502694627439702 ) ) ;
#30887 = CARTESIAN_POINT ( 'NONE',  ( 2.500000000000002220, -35.66666666666666430, 4.330127018922192761 ) ) ;
#30888 = CARTESIAN_POINT ( 'NONE',  ( 1.975475456537005874E-15, -10.75000000000000000, 5.000000000000000000 ) ) ;
#30889 = CARTESIAN_POINT ( 'NONE',  ( -4.458734124999997661, 9.770833334698927786, 2.574251347313722516 ) ) ;
#30890 = CARTESIAN_POINT ( 'NONE',  ( 4.458734125000001214, -65.89583333196772230, 2.574251347313718519 ) ) ;
#30891 = AXIS2_PLACEMENT_3D ( 'NONE', #59938, #5569, #15860 ) ;
#30892 = CARTESIAN_POINT ( 'NONE',  ( -3.152548672688508926E-16, -15.81249999863440436, -5.148502694627439702 ) ) ;
#30893 = CARTESIAN_POINT ( 'NONE',  ( -2.499999999999996447, 2.166666666666667407, 4.330127018922195425 ) ) ;
#30894 = CARTESIAN_POINT ( 'NONE',  ( -3.152801135295367985, -164.8125000013656063, 3.152801135295367096 ) ) ;
#30895 = LINE ( 'NONE', #59864, #26403 ) ;
#30896 = CIRCLE ( 'NONE', #29866, 5.000000000000000000 ) ;
#30897 = CARTESIAN_POINT ( 'NONE',  ( 4.458734125000001214, -60.89583333196774362, 2.574251347313718519 ) ) ;
#30898 = CARTESIAN_POINT ( 'NONE',  ( 5.000000000000000000, -96.29166666393547303, -2.886751345948129988 ) ) ;
#30899 = LINE ( 'NONE', #30574, #54500 ) ;
#30900 = CARTESIAN_POINT ( 'NONE',  ( 1.975475456537005874E-15, -79.74999999999998579, 5.000000000000000000 ) ) ;
#30901 = CARTESIAN_POINT ( 'NONE',  ( -1.339745962155613812, -36.20534180126147561, -5.000000000000000000 ) ) ;
#30902 = CARTESIAN_POINT ( 'NONE',  ( 9.457646018065525792E-16, -36.06249999863440792, 5.148502694627439702 ) ) ;
#30903 = CARTESIAN_POINT ( 'NONE',  ( 1.975475456537005874E-15, 19.37500000273118772, 5.000000000000000000 ) ) ;
#30904 = CARTESIAN_POINT ( 'NONE',  ( 5.000000000000000000, -41.49999999999999289, -6.123233995736766282E-16 ) ) ;
#30905 = CARTESIAN_POINT ( 'NONE',  ( 1.339745962155612702, -13.29465819873852084, -5.000000000000000000 ) ) ;
#30906 = CARTESIAN_POINT ( 'NONE',  ( 2.500000000000002220, -6.541666663935481019, 4.330127018922192761 ) ) ;
#30907 = ORIENTED_EDGE ( 'NONE', *, *, #28252, .F. ) ;
#30908 = CARTESIAN_POINT ( 'NONE',  ( -3.152548672688508926E-16, -107.5624999986343795, -5.148502694627439702 ) ) ;
#30909 = CARTESIAN_POINT ( 'NONE',  ( -2.229367062499996610, -0.3958333319677397322, 3.861377020970582219 ) ) ;
#30910 = CARTESIAN_POINT ( 'NONE',  ( -6.972266317189433020E-16, -73.12499999726878741, -5.000000000000000000 ) ) ;
#30911 = CARTESIAN_POINT ( 'NONE',  ( 2.500000000000002220, -0.6666666666666660745, 4.330127018922192761 ) ) ;
#30912 = CARTESIAN_POINT ( 'NONE',  ( -4.458734124999999437, -72.31249999863439371, 0.000000000000000000 ) ) ;
#30913 = LINE ( 'NONE', #45070, #8229 ) ;
#30914 = CARTESIAN_POINT ( 'NONE',  ( -5.000000000000000000, -7.958333330602145317, -2.886751345948128211 ) ) ;
#30916 = ORIENTED_EDGE ( 'NONE', *, *, #38902, .T. ) ;
#30915 = CARTESIAN_POINT ( 'NONE',  ( -4.458734124999999437, -40.31249999863440081, 0.000000000000000000 ) ) ;
#30917 = DIRECTION ( 'NONE',  ( 0.000000000000000000, 0.000000000000000000, 1.000000000000000000 ) ) ;
#30919 = ORIENTED_EDGE ( 'NONE', *, *, #43708, .T. ) ;
#30918 = CARTESIAN_POINT ( 'NONE',  ( -4.458734124999998549, 10.52083333469892779, 2.574251347313722516 ) ) ;
#30920 = CARTESIAN_POINT ( 'NONE',  ( -2.499999999999996447, -47.83333333333332149, 4.330127018922195425 ) ) ;
#30921 = CARTESIAN_POINT ( 'NONE',  ( -2.229367062499996610, -30.39583333196773651, 3.861377020970582219 ) ) ;
#30922 = CARTESIAN_POINT ( 'NONE',  ( -1.339745962155610925, -34.79465819873851729, 5.000000000000000000 ) ) ;
#30923 = CARTESIAN_POINT ( 'NONE',  ( 4.458734125000001214, -76.89583333196775072, 2.574251347313718519 ) ) ;
#30924 = CARTESIAN_POINT ( 'NONE',  ( -5.000000000000000000, -169.5000000000000000, -6.123233995736766282E-16 ) ) ;
#30926 = ADVANCED_FACE ( 'NONE', ( #57479 ), #61982, .T. ) ;
#30925 = CARTESIAN_POINT ( 'NONE',  ( -4.458734124999998549, -87.22916666530107932, 2.574251347313722516 ) ) ;
#30927 = CARTESIAN_POINT ( 'NONE',  ( -50.55543936806279248, -136.3125000013656063, 0.3552334253322060320 ) ) ;
#30928 = CARTESIAN_POINT ( 'NONE',  ( 4.458734124999998549, -37.97916666530107932, -2.574251347313721627 ) ) ;
#30929 = ORIENTED_EDGE ( 'NONE', *, *, #37056, .F. ) ;
#30930 = CARTESIAN_POINT ( 'NONE',  ( -4.999999999999998224, 24.20833333606451987, 2.886751345948131764 ) ) ;
#30931 = ORIENTED_EDGE ( 'NONE', *, *, #40797, .T. ) ;
#30932 = CARTESIAN_POINT ( 'NONE',  ( 9.457646018065525792E-16, -76.31249999863439371, 5.148502694627439702 ) ) ;
#30933 = CARTESIAN_POINT ( 'NONE',  ( -56.09268833151246980, -135.0000000000000853, -4.332774804594910378 ) ) ;
#30934 = EDGE_LOOP ( 'NONE', ( #4402, #23742, #2671, #63278 ) ) ;
#30935 = CARTESIAN_POINT ( 'NONE',  ( 1.975475456537005874E-15, -22.62499999726880873, 5.000000000000000000 ) ) ;
#30937 = CIRCLE ( 'NONE', #40212, 11.00000000000000000 ) ;
#30936 = FACE_OUTER_BOUND ( 'NONE', #11475, .T. ) ;
#30938 = CARTESIAN_POINT ( 'NONE',  ( 4.458734124999998549, -62.97916666530107221, -2.574251347313721627 ) ) ;
#30939 = CARTESIAN_POINT ( 'NONE',  ( 4.458734124999999437, -5.062499998634402587, -5.460374474430324690E-16 ) ) ;
#30940 = EDGE_LOOP ( 'NONE', ( #1694, #59520, #23635, #45409 ) ) ;
#30941 = CARTESIAN_POINT ( 'NONE',  ( -1.339745962155610925, -9.669658196007334894, 5.000000000000000000 ) ) ;
#30942 = CARTESIAN_POINT ( 'NONE',  ( 1.975475456537005874E-15, -19.62499999726881228, 5.000000000000000000 ) ) ;
#30943 = ORIENTED_EDGE ( 'NONE', *, *, #15730, .F. ) ;
#30944 = CARTESIAN_POINT ( 'NONE',  ( 0.000000000000000000, -120.0000000000000000, 5.000000000000000000 ) ) ;
#30945 = CARTESIAN_POINT ( 'NONE',  ( 2.229367062500001939, 6.020833334698927786, 3.861377020970579999 ) ) ;
#30946 = CARTESIAN_POINT ( 'NONE',  ( 2.500000000000002220, -64.66666666666665719, 4.330127018922192761 ) ) ;
#30947 = CARTESIAN_POINT ( 'NONE',  ( 3.152801135295366208, -159.5625000013656063, 3.152801135295367985 ) ) ;
#30948 = LINE ( 'NONE', #60556, #29586 ) ;
#30949 = VERTEX_POINT ( 'NONE', #17901 ) ;
#30950 = CARTESIAN_POINT ( 'NONE',  ( -4.458734124999999437, -81.39583333196773651, -2.574251347313719407 ) ) ;
#30951 = CARTESIAN_POINT ( 'NONE',  ( 1.339745962155612702, -75.29465819873853150, -5.000000000000000000 ) ) ;
#30952 = CARTESIAN_POINT ( 'NONE',  ( 2.229367062500001939, -3.979166665301070438, 3.861377020970579999 ) ) ;
#30953 = CARTESIAN_POINT ( 'NONE',  ( 5.000000000000000000, 25.70833333606452342, -2.886751345948130876 ) ) ;
#30954 =( BOUNDED_SURFACE ( )  B_SPLINE_SURFACE ( 3, 2, ( 
 ( #49126, #15677, #34019 ),
 ( #35296, #49449, #14396 ),
 ( #5391, #34652, #4746 ),
 ( #25007, #44616, #576 ),
 ( #29492, #24370, #53640 ),
 ( #1228, #14709, #39784 ),
 ( #10843, #20185, #9573 ),
 ( #20512, #54917, #5068 ) ),
 .UNSPECIFIED., .F., .F., .F. ) 
 B_SPLINE_SURFACE_WITH_KNOTS ( ( 4, 2, 2, 4 ),
 ( 3, 3 ),
 ( 0.03851319102641418551, 0.04314724750133520914, 0.04546427573879571749, 0.04778130397625623277 ),
 ( 0.000000000000000000, 1.000000000000000000 ),
 .UNSPECIFIED. ) 
 GEOMETRIC_REPRESENTATION_ITEM ( )  RATIONAL_B_SPLINE_SURFACE ( (
 ( 1.000000000000000000, 0.8047781573724569482, 1.000000000000000000),
 ( 1.000000000000000000, 0.8123768202405010630, 1.000000000000000000),
 ( 1.000000000000000000, 0.8190667609311549358, 1.000000000000000000),
 ( 1.000000000000000000, 0.8191933927154739781, 1.000000000000000000),
 ( 1.000000000000000000, 0.8176088169850088683, 1.000000000000000000),
 ( 1.000000000000000000, 0.8122958474542694152, 1.000000000000000000),
 ( 1.000000000000000000, 0.8086309703845098174, 1.000000000000000000),
 ( 1.000000000000000000, 0.8047712409910821041, 1.000000000000000000) ) ) 
 REPRESENTATION_ITEM ( '' )  SURFACE ( )  );
#30955 = CARTESIAN_POINT ( 'NONE',  ( -6.972266317189433020E-16, -68.24999999999998579, -5.000000000000000000 ) ) ;
#30956 = CARTESIAN_POINT ( 'NONE',  ( -2.229367062500000163, -68.72916666530107932, -3.861377020970580443 ) ) ;
#30957 = CARTESIAN_POINT ( 'NONE',  ( 5.000000000000000000, -29.29166666393547658, -2.886751345948129988 ) ) ;
#30958 = CARTESIAN_POINT ( 'NONE',  ( -2.499999999999996447, -28.83333333333333570, 4.330127018922195425 ) ) ;
#30959 = CARTESIAN_POINT ( 'NONE',  ( -4.458734124999997661, 28.77083333469892779, 2.574251347313722516 ) ) ;
#30960 = CARTESIAN_POINT ( 'NONE',  ( -1.339745962155669101, -37.66965819600733312, 4.999999999999966249 ) ) ;
#30961 = CARTESIAN_POINT ( 'NONE',  ( 4.458734124999998549, 26.27083333469892423, -2.574251347313721627 ) ) ;
#30962 = CARTESIAN_POINT ( 'NONE',  ( -4.458734124999999437, -52.39583333196773651, -2.574251347313719407 ) ) ;
#30963 = CARTESIAN_POINT ( 'NONE',  ( 2.229367062499998831, -29.89583333196773296, -3.861377020970580887 ) ) ;
#30964 = CARTESIAN_POINT ( 'NONE',  ( -3.152548672688508926E-16, 1.187500001365596081, -5.148502694627439702 ) ) ;
#30965 = CARTESIAN_POINT ( 'NONE',  ( -3.535533905932738641, -149.5000000027311842, 3.535533905932737309 ) ) ;
#30966 = CARTESIAN_POINT ( 'NONE',  ( -2.500000000000000444, 22.83333333333333215, -4.330127018922193649 ) ) ;
#30967 = CARTESIAN_POINT ( 'NONE',  ( -5.000000000000000888, -145.6875000027312126, -2.071067811865475949 ) ) ;
#30968 = CARTESIAN_POINT ( 'NONE',  ( -9.184850993605147944E-16, -155.3750000027311842, 5.000000000000000000 ) ) ;
#30969 = CARTESIAN_POINT ( 'NONE',  ( 4.458734125000001214, -41.89583333196773651, 2.574251347313718519 ) ) ;
#30970 = CARTESIAN_POINT ( 'NONE',  ( 5.000000000000000000, -77.37499999726881583, -6.123233995736766282E-16 ) ) ;
#30971 = CARTESIAN_POINT ( 'NONE',  ( -50.55543936806279248, -141.3125000013656063, 0.3552334253322060320 ) ) ;
#30972 = CARTESIAN_POINT ( 'NONE',  ( -2.071067811865475061, -140.6875000000000568, -5.000000000000000888 ) ) ;
#30973 = CARTESIAN_POINT ( 'NONE',  ( 1.975475456537005874E-15, -87.75000000000001421, 5.000000000000000000 ) ) ;
#30974 = CARTESIAN_POINT ( 'NONE',  ( -4.458734124999997661, -80.47916666530105090, 2.574251347313722516 ) ) ;
#30975 = CARTESIAN_POINT ( 'NONE',  ( -3.152801135295367985, -161.0625000013656063, 3.152801135295367096 ) ) ;
#30976 = CARTESIAN_POINT ( 'NONE',  ( 2.500000000000002220, 13.45833333606451987, 4.330127018922192761 ) ) ;
#30977 = CARTESIAN_POINT ( 'NONE',  ( -2.500000000000000444, -25.16666666666666430, -4.330127018922193649 ) ) ;
#30978 = CARTESIAN_POINT ( 'NONE',  ( -4.458734125000000326, -141.0000000013656063, -1.846868145590735644 ) ) ;
#30979 = EDGE_LOOP ( 'NONE', ( #45076, #5059, #17104, #22480 ) ) ;
#30980 = CARTESIAN_POINT ( 'NONE',  ( 4.458734124999999437, 23.93750000136559564, -5.460374474430324690E-16 ) ) ;
#30981 = VERTEX_POINT ( 'NONE', #27551 ) ;
#30982 = CARTESIAN_POINT ( 'NONE',  ( -3.152548672688508926E-16, 13.18750000136559208, -5.148502694627439702 ) ) ;
#30983 = CARTESIAN_POINT ( 'NONE',  ( 5.000000000000000000, 16.70833333606451987, -2.886751345948129988 ) ) ;
#30984 = CARTESIAN_POINT ( 'NONE',  ( -4.999999999999998224, -60.79166666393547303, 2.886751345948131764 ) ) ;
#30985 = CARTESIAN_POINT ( 'NONE',  ( 1.060575238724906964E-15, 16.25000000000000000, 5.773502691896257311 ) ) ;
#30986 = CARTESIAN_POINT ( 'NONE',  ( -2.229367062500000163, -52.47916666530107221, -3.861377020970580443 ) ) ;
#30987 = CARTESIAN_POINT ( 'NONE',  ( 4.458734125000001214, -13.89583333196774007, 2.574251347313718519 ) ) ;
#30988 = DIRECTION ( 'NONE',  ( 0.000000000000000000, 1.000000000000000000, 0.000000000000000000 ) ) ;
#30989 = CARTESIAN_POINT ( 'NONE',  ( -50.55543936806279248, -136.3125000013656063, 0.3552334253322060320 ) ) ;
#30990 = FACE_OUTER_BOUND ( 'NONE', #3815, .T. ) ;
#30991 = CARTESIAN_POINT ( 'NONE',  ( 1.339745962155615144, -89.58034179853028434, 4.999999999999999112 ) ) ;
#30992 = CARTESIAN_POINT ( 'NONE',  ( 1.975475456537005874E-15, -61.74999999999999289, 5.000000000000000000 ) ) ;
#30993 = CARTESIAN_POINT ( 'NONE',  ( -5.000000000000000000, -33.08333333333332149, -2.886751345948128211 ) ) ;
#30994 = CARTESIAN_POINT ( 'NONE',  ( 4.458734124999999437, -139.6875000013656063, 0.000000000000000000 ) ) ;
#30996 = CARTESIAN_POINT ( 'NONE',  ( -2.229367062500000163, -15.72916666530107399, -3.861377020970580443 ) ) ;
#30995 = CARTESIAN_POINT ( 'NONE',  ( -6.972266317189433020E-16, -59.25000000000000000, -5.000000000000000000 ) ) ;
#30997 = CARTESIAN_POINT ( 'NONE',  ( -2.229367062499996610, -57.14583333196773651, 3.861377020970582219 ) ) ;
#30998 = CARTESIAN_POINT ( 'NONE',  ( 3.152801135295366208, -152.8125000013656063, 3.152801135295367985 ) ) ;
#31000 = EDGE_CURVE ( 'NONE', #62942, #27799, #56202, .T. ) ;
#30999 = CARTESIAN_POINT ( 'NONE',  ( -4.458734124999998549, -66.22916666530107932, 2.574251347313722516 ) ) ;
#31001 = CARTESIAN_POINT ( 'NONE',  ( -57.89159099828107458, -146.9375000013656063, -3.393966926194107447 ) ) ;
#31002 = CARTESIAN_POINT ( 'NONE',  ( 1.060575238724906964E-15, -57.62499999726880873, 5.773502691896257311 ) ) ;
#31003 = ORIENTED_EDGE ( 'NONE', *, *, #47630, .T. ) ;
#31004 = ORIENTED_EDGE ( 'NONE', *, *, #35811, .T. ) ;
#31006 = CARTESIAN_POINT ( 'NONE',  ( 1.243387493232115550E-13, -8.250000000000003553, -5.000000000000000000 ) ) ;
#31005 = CARTESIAN_POINT ( 'NONE',  ( 5.000000000000000000, -21.41666666666666430, -2.886751345948130876 ) ) ;
#31007 = CARTESIAN_POINT ( 'NONE',  ( -8.190561711645485556E-16, -151.6875000013656063, 4.458734124999999437 ) ) ;
#31008 = EDGE_LOOP ( 'NONE', ( #3243, #24839, #43191, #50039 ) ) ;
#31009 = CARTESIAN_POINT ( 'NONE',  ( 1.339745962155612702, -54.29465819873851729, -5.000000000000000000 ) ) ;
#31010 = CARTESIAN_POINT ( 'NONE',  ( -59.81910112700025905, -128.1875000000000568, -2.462841084822630311 ) ) ;
#31011 = CARTESIAN_POINT ( 'NONE',  ( 2.500000000000002220, 15.33333333333333215, 4.330127018922192761 ) ) ;
#31012 = CARTESIAN_POINT ( 'NONE',  ( -4.458734124999999437, -47.56249999863440792, 0.000000000000000000 ) ) ;
#31013 = ORIENTED_EDGE ( 'NONE', *, *, #28709, .T. ) ;
#31014 = LINE ( 'NONE', #50964, #58355 ) ;
#31015 = EDGE_CURVE ( 'NONE', #21097, #25291, #26653, .T. ) ;
#31016 = CARTESIAN_POINT ( 'NONE',  ( 2.229367062500001939, 16.02083333469892779, 3.861377020970579999 ) ) ;
#31017 = CARTESIAN_POINT ( 'NONE',  ( 9.457646018065525792E-16, 25.93750000136559564, 5.148502694627439702 ) ) ;
#31018 = CARTESIAN_POINT ( 'NONE',  ( -59.98410592259440222, -124.2500000027311984, -0.3983568153799752487 ) ) ;
#31019 = CARTESIAN_POINT ( 'NONE',  ( 2.500000000000002220, -78.54166666393547303, 4.330127018922192761 ) ) ;
#31020 = CARTESIAN_POINT ( 'NONE',  ( 1.975475456537005874E-15, -61.62499999726880873, 5.000000000000000000 ) ) ;
#31021 =( BOUNDED_CURVE ( )  B_SPLINE_CURVE ( 2, ( #32075, #51080, #51712, #55907, #31129, #56858, #32398, #52024, #6697 ),
 .UNSPECIFIED., .F., .F. ) 
 B_SPLINE_CURVE_WITH_KNOTS ( ( 3, 2, 2, 2, 3 ),
 ( 0.2083333333333335091, 0.2125000000000001610, 0.2166666666666668406, 0.2208333333333335202, 0.2250000000000001998 ),
 .UNSPECIFIED. ) 
 CURVE ( )  GEOMETRIC_REPRESENTATION_ITEM ( )  RATIONAL_B_SPLINE_CURVE ( ( 0.9999999999999970024, 0.9238795325112897361, 1.000000000000000000, 0.9238795325112867385, 1.000000000000000000, 0.9238795325112867385, 1.000000000000000000, 0.9238795325112831858, 1.000000000000003553 ) ) 
 REPRESENTATION_ITEM ( '' )  );
#31022 = ORIENTED_EDGE ( 'NONE', *, *, #18867, .F. ) ;
#31023 = CARTESIAN_POINT ( 'NONE',  ( -3.152548672688508926E-16, -66.56249999863440792, -5.148502694627439702 ) ) ;
#31024 = CARTESIAN_POINT ( 'NONE',  ( 6.123233995736766282E-16, -120.0000000000000000, -5.000000000000000000 ) ) ;
#31025 = CARTESIAN_POINT ( 'NONE',  ( -4.458734124999999437, 10.68750000136559386, 0.000000000000000000 ) ) ;
#31026 = ADVANCED_FACE ( 'NONE', ( #59030 ), #19469, .T. ) ;
#31027 = CARTESIAN_POINT ( 'NONE',  ( -5.000000000000000000, -69.95833333060214443, -2.886751345948128211 ) ) ;
#31028 = CARTESIAN_POINT ( 'NONE',  ( -3.535533905932738641, -157.3750000000000284, 3.535533905932737309 ) ) ;
#31029 = CARTESIAN_POINT ( 'NONE',  ( -4.458734124999999437, -52.64583333196773651, -2.574251347313719407 ) ) ;
#31030 = CARTESIAN_POINT ( 'NONE',  ( -4.999999999999999112, -14.79166666393548368, 2.886751345948131764 ) ) ;
#31031 = CARTESIAN_POINT ( 'NONE',  ( 1.975475456537005874E-15, -42.62499999726880873, 5.000000000000000000 ) ) ;
#31032 = CARTESIAN_POINT ( 'NONE',  ( -58.80597590150559739, -147.0000000000000284, 3.242614290531460330 ) ) ;
#31033 = DIRECTION ( 'NONE',  ( -0.5000000000000009992, 0.000000000000000000, -0.8660254037844380415 ) ) ;
#31034 = CYLINDRICAL_SURFACE ( 'NONE', #25472, 5.000000000000000000 ) ;
#31035 = CARTESIAN_POINT ( 'NONE',  ( 2.229367062499998831, -15.89583333196773651, -3.861377020970580887 ) ) ;
#31036 = ORIENTED_EDGE ( 'NONE', *, *, #14231, .T. ) ;
#31037 = FACE_OUTER_BOUND ( 'NONE', #62487, .T. ) ;
#31038 = CARTESIAN_POINT ( 'NONE',  ( -3.152548672688508926E-16, -105.5624999986344079, -5.148502694627439702 ) ) ;
#31039 = CARTESIAN_POINT ( 'NONE',  ( -5.000000000000000000, -155.6250000027311842, -6.123233995736766282E-16 ) ) ;
#31040 = ORIENTED_EDGE ( 'NONE', *, *, #48347, .T. ) ;
#31041 = CARTESIAN_POINT ( 'NONE',  ( 9.457646018065525792E-16, -103.3124999986344079, 5.148502694627439702 ) ) ;
#31042 = CARTESIAN_POINT ( 'NONE',  ( 4.458734125000001214, -25.89583333196774007, 2.574251347313718519 ) ) ;
#31043 = CARTESIAN_POINT ( 'NONE',  ( 2.500000000000002220, -61.54166666393547303, 4.330127018922192761 ) ) ;
#31044 = CARTESIAN_POINT ( 'NONE',  ( -59.59170313451811296, -151.7500000013655779, 1.485763867205729394 ) ) ;
#31045 = CARTESIAN_POINT ( 'NONE',  ( -52.80376928212989185, -141.8750000013655779, -4.297418129356378458 ) ) ;
#31046 = EDGE_CURVE ( 'NONE', #38768, #10267, #13196, .T. ) ;
#31047 = CARTESIAN_POINT ( 'NONE',  ( 2.229367062499998831, -21.64583333196774007, -3.861377020970580887 ) ) ;
#31048 = CARTESIAN_POINT ( 'NONE',  ( 2.229367062499998831, -63.89583333196772941, -3.861377020970580887 ) ) ;
#31049 = CARTESIAN_POINT ( 'NONE',  ( -5.926426369611017623E-15, 25.37500000273118062, 5.000000000000000000 ) ) ;
#31050 = CARTESIAN_POINT ( 'NONE',  ( -4.458734124999999437, -21.31249999863440436, 0.000000000000000000 ) ) ;
#31051 = CARTESIAN_POINT ( 'NONE',  ( 0.000000000000000000, -170.0000000000000000, 0.000000000000000000 ) ) ;
#31052 = CARTESIAN_POINT ( 'NONE',  ( 3.535533905932736864, -152.1250000000000000, 3.535533905932738641 ) ) ;
#31053 = CARTESIAN_POINT ( 'NONE',  ( -5.000000000000000000, -14.08333333333333037, -2.886751345948128211 ) ) ;
#31054 = CARTESIAN_POINT ( 'NONE',  ( -4.458734125000000326, -150.0000000013655779, -1.846868145590735644 ) ) ;
#31055 = ORIENTED_EDGE ( 'NONE', *, *, #18963, .T. ) ;
#31056 = CARTESIAN_POINT ( 'NONE',  ( -4.458734124999997661, -45.47916666530106511, 2.574251347313722516 ) ) ;
#31057 =( BOUNDED_CURVE ( )  B_SPLINE_CURVE ( 2, ( #47789, #14008, #13699, #8876, #28803, #3434, #42969, #33321, #28490 ),
 .UNSPECIFIED., .F., .F. ) 
 B_SPLINE_CURVE_WITH_KNOTS ( ( 3, 2, 2, 2, 3 ),
 ( 0.9089285714285714191, 0.9095238095238095122, 0.9107142857142856984, 0.9119047619047618847, 0.9124999999999999778 ),
 .UNSPECIFIED. ) 
 CURVE ( )  GEOMETRIC_REPRESENTATION_ITEM ( )  RATIONAL_B_SPLINE_CURVE ( ( 0.9330127018922194093, 0.9330127018922194093, 1.000000000000000000, 0.8660254037844387076, 1.000000000000000000, 0.8660254037844387076, 1.000000000000000000, 0.9330127018922194093, 0.9330127018922194093 ) ) 
 REPRESENTATION_ITEM ( '' )  );
#31058 = CARTESIAN_POINT ( 'NONE',  ( 2.499999999999998668, 21.79166666939785202, -4.330127018922193649 ) ) ;
#31059 = CARTESIAN_POINT ( 'NONE',  ( 5.000000000000000000, -90.50000000000000000, -6.123233995736766282E-16 ) ) ;
#31060 = CARTESIAN_POINT ( 'NONE',  ( 2.229367062500001939, -89.97916666530106511, 3.861377020970579999 ) ) ;
#31061 = CARTESIAN_POINT ( 'NONE',  ( -3.152548672688508926E-16, 2.437500001365594304, -5.148502694627439702 ) ) ;
#31062 = CARTESIAN_POINT ( 'NONE',  ( 3.061616997868383141E-16, -160.8750000027311842, -5.000000000000000000 ) ) ;
#31063 = CARTESIAN_POINT ( 'NONE',  ( 1.339745962155615144, -11.58034179853029499, 4.999999999999999112 ) ) ;
#31064 = PLANE ( 'NONE',  #13952 ) ;
#31065 = CARTESIAN_POINT ( 'NONE',  ( -4.458734124999998549, 17.52083333469892779, 2.574251347313722516 ) ) ;
#31066 = CARTESIAN_POINT ( 'NONE',  ( 2.499999999999998668, -81.33333333333332860, -4.330127018922193649 ) ) ;
#31067 = CARTESIAN_POINT ( 'NONE',  ( -2.500000000000000444, 9.958333336064519870, -4.330127018922193649 ) ) ;
#31068 = ORIENTED_EDGE ( 'NONE', *, *, #48349, .T. ) ;
#31069 = CARTESIAN_POINT ( 'NONE',  ( -9.184850993605147944E-16, -162.3750000027311842, 5.000000000000000000 ) ) ;
#31070 = ORIENTED_EDGE ( 'NONE', *, *, #12302, .F. ) ;
#31071 = CARTESIAN_POINT ( 'NONE',  ( 1.975475456537005874E-15, -34.62499999726880873, 5.000000000000000000 ) ) ;
#31072 = CARTESIAN_POINT ( 'NONE',  ( 2.229367062500001939, -40.97916666530107221, 3.861377020970579999 ) ) ;
#31073 = CARTESIAN_POINT ( 'NONE',  ( 1.846868145590735200, -162.5000000013655779, -4.458734125000000326 ) ) ;
#31074 = ADVANCED_FACE ( 'NONE', ( #18836 ), #18540, .T. ) ;
#31075 = ADVANCED_FACE ( 'NONE', ( #34570 ), #29109, .T. ) ;
#31076 = CARTESIAN_POINT ( 'NONE',  ( 5.000000000000000000, -37.29166666393548013, -2.886751345948129988 ) ) ;
#31077 = ADVANCED_FACE ( 'NONE', ( #10140 ), #33952, .T. ) ;
#31078 = ORIENTED_EDGE ( 'NONE', *, *, #16562, .T. ) ;
#31079 = CARTESIAN_POINT ( 'NONE',  ( -2.229367062499996610, -18.14583333196773651, 3.861377020970582219 ) ) ;
#31080 = ORIENTED_EDGE ( 'NONE', *, *, #34729, .T. ) ;
#31081 = CARTESIAN_POINT ( 'NONE',  ( -2.499999999999996447, -85.83333333333332860, 4.330127018922195425 ) ) ;
#31082 = CARTESIAN_POINT ( 'NONE',  ( 4.458734125000000326, -166.3750000013655779, -1.846868145590734978 ) ) ;
#31083 = CARTESIAN_POINT ( 'NONE',  ( -2.500000000000000444, -85.04166666393547303, -4.330127018922193649 ) ) ;
#31085 = ORIENTED_EDGE ( 'NONE', *, *, #46502, .T. ) ;
#31084 = CARTESIAN_POINT ( 'NONE',  ( -5.000000000000000000, -34.87499999726881583, 0.000000000000000000 ) ) ;
#31086 = CARTESIAN_POINT ( 'NONE',  ( -53.33387254593733928, -139.8125000000000000, 5.149110718188519620 ) ) ;
#31087 = CARTESIAN_POINT ( 'NONE',  ( -3.152548672688508926E-16, -31.81249999863440792, -5.148502694627439702 ) ) ;
#31088 = CARTESIAN_POINT ( 'NONE',  ( -1.339745962155613812, -50.20534180126148271, -5.000000000000000000 ) ) ;
#31089 = EDGE_CURVE ( 'NONE', #25310, #19310, #52579, .T. ) ;
#31090 = VERTEX_POINT ( 'NONE', #33640 ) ;
#31091 = CARTESIAN_POINT ( 'NONE',  ( 4.458734124999998549, -74.72916666530106511, -2.574251347313721627 ) ) ;
#31092 = EDGE_CURVE ( 'NONE', #16051, #45174, #36990, .T. ) ;
#31093 = CARTESIAN_POINT ( 'NONE',  ( 4.458734125000001214, -108.1458333319677365, 2.574251347313718519 ) ) ;
#31094 = CARTESIAN_POINT ( 'NONE',  ( -6.972266317189433020E-16, -108.1249999972688016, -5.000000000000000000 ) ) ;
#31095 = EDGE_LOOP ( 'NONE', ( #29666, #54182, #62670, #38054 ) ) ;
#31096 = DIRECTION ( 'NONE',  ( 0.000000000000000000, 0.000000000000000000, 1.000000000000000000 ) ) ;
#31097 = CARTESIAN_POINT ( 'NONE',  ( -50.55543936806279248, -144.3125000013656063, 0.3552334253322060320 ) ) ;
#31098 = CARTESIAN_POINT ( 'NONE',  ( 9.457646018065525792E-16, -82.31249999863440792, 5.148502694627439702 ) ) ;
#31099 = CARTESIAN_POINT ( 'NONE',  ( -51.19402409849444524, -134.6250000027312126, -3.242614290531456334 ) ) ;
#31100 = CARTESIAN_POINT ( 'NONE',  ( -2.229367062500000163, -45.47916666530106511, -3.861377020970580443 ) ) ;
#31101 = CARTESIAN_POINT ( 'NONE',  ( -3.152801135295367985, -141.0625000013655779, 3.152801135295367096 ) ) ;
#31102 = CARTESIAN_POINT ( 'NONE',  ( -2.500000000000000444, -58.16666666666665719, -4.330127018922193649 ) ) ;
#31103 = CARTESIAN_POINT ( 'NONE',  ( 2.229367062499998831, -50.64583333196772941, -3.861377020970580887 ) ) ;
#31104 = CARTESIAN_POINT ( 'NONE',  ( 9.457646018065525792E-16, -43.06249999863440081, 5.148502694627439702 ) ) ;
#31105 = CARTESIAN_POINT ( 'NONE',  ( -4.458734124999999437, 26.68750000136559564, 0.000000000000000000 ) ) ;
#31106 = CARTESIAN_POINT ( 'NONE',  ( -4.458734124999999437, -17.39583333196773651, -2.574251347313719407 ) ) ;
#31107 = CARTESIAN_POINT ( 'NONE',  ( 2.500000000000002220, -103.6666666666666572, 4.330127018922192761 ) ) ;
#31108 = CARTESIAN_POINT ( 'NONE',  ( 4.458734124999998549, -39.97916666530107221, -2.574251347313721627 ) ) ;
#31109 = CARTESIAN_POINT ( 'NONE',  ( -5.000000000000000000, 3.041666669397851130, -2.886751345948128211 ) ) ;
#31110 = CARTESIAN_POINT ( 'NONE',  ( 1.975475456537005874E-15, -39.62499999726880162, 5.000000000000000000 ) ) ;
#31111 = CARTESIAN_POINT ( 'NONE',  ( -55.35523342533222291, -127.3125000013655921, 4.444560631937231499 ) ) ;
#31112 = CARTESIAN_POINT ( 'NONE',  ( -4.458734124999998549, -80.47916666530106511, 2.574251347313722516 ) ) ;
#31113 = CARTESIAN_POINT ( 'NONE',  ( -58.24261429053147765, -142.3750000027312126, -3.805975901505573855 ) ) ;
#31114 = CARTESIAN_POINT ( 'NONE',  ( 4.458734125000000326, -97.89583333196773651, 2.574251347313718519 ) ) ;
#31115 = LINE ( 'NONE', #22671, #4867 ) ;
#31116 = CARTESIAN_POINT ( 'NONE',  ( -4.458734124999999437, -2.645833331967738289, -2.574251347313719407 ) ) ;
#31117 = VERTEX_POINT ( 'NONE', #14013 ) ;
#31118 = CARTESIAN_POINT ( 'NONE',  ( 2.071067811865392461, -146.1875000000000284, 5.000000000000084377 ) ) ;
#31119 = CARTESIAN_POINT ( 'NONE',  ( 1.975475456537005874E-15, -75.74999999999998579, 5.000000000000000000 ) ) ;
#31120 = CARTESIAN_POINT ( 'NONE',  ( 4.458734124999999437, -85.81249999863439371, -5.460374474430324690E-16 ) ) ;
#31121 = CARTESIAN_POINT ( 'NONE',  ( -5.000000000000000000, -168.6250000027312126, -6.123233995736766282E-16 ) ) ;
#31122 = CARTESIAN_POINT ( 'NONE',  ( 4.458734124999999437, -86.06249999863439371, -5.460374474430324690E-16 ) ) ;
#31123 = CARTESIAN_POINT ( 'NONE',  ( -4.458734124999999437, 17.35416666803225993, -2.574251347313719407 ) ) ;
#31124 = DIRECTION ( 'NONE',  ( -0.000000000000000000, 1.000000000000000000, -0.000000000000000000 ) ) ;
#31125 = CARTESIAN_POINT ( 'NONE',  ( -54.64476657466781973, -137.8125000013656063, -4.444560631937228834 ) ) ;
#31126 = CARTESIAN_POINT ( 'NONE',  ( -4.458734124999999437, -5.312499998634402587, 0.000000000000000000 ) ) ;
#31127 = CARTESIAN_POINT ( 'NONE',  ( -4.458734124999998549, 16.52083333469892779, 2.574251347313722516 ) ) ;
#31128 = CARTESIAN_POINT ( 'NONE',  ( -3.152548672688508926E-16, -49.81249999863440081, -5.148502694627439702 ) ) ;
#31129 = CARTESIAN_POINT ( 'NONE',  ( -5.000000000000000000, -163.5000000000000000, -6.123233995736766282E-16 ) ) ;
#31130 = CARTESIAN_POINT ( 'NONE',  ( 9.457646018065525792E-16, -83.06249999863439371, 5.148502694627439702 ) ) ;
#31131 = CARTESIAN_POINT ( 'NONE',  ( -4.458734124999997661, -1.229166665301071548, 2.574251347313722516 ) ) ;
#31132 = ORIENTED_EDGE ( 'NONE', *, *, #654, .T. ) ;
#31133 = CARTESIAN_POINT ( 'NONE',  ( -4.458734124999997661, -32.47916666530106511, 2.574251347313722516 ) ) ;
#31134 = CARTESIAN_POINT ( 'NONE',  ( -56.48576386720575471, -131.0000000013656063, -4.591703134518078322 ) ) ;
#31135 = CARTESIAN_POINT ( 'NONE',  ( 4.458734124999999437, -74.81249999863440792, -5.460374474430324690E-16 ) ) ;
#31136 = CARTESIAN_POINT ( 'NONE',  ( -4.458734124999998549, 27.52083333469892779, 2.574251347313722516 ) ) ;
#31137 =( BOUNDED_CURVE ( )  B_SPLINE_CURVE ( 2, ( #53662, #18627, #53032, #63323, #44318, #38250, #24085, #9596, #23773 ),
 .UNSPECIFIED., .F., .F. ) 
 B_SPLINE_CURVE_WITH_KNOTS ( ( 3, 2, 2, 2, 3 ),
 ( 0.9339285714285714413, 0.9345238095238095344, 0.9357142857142857206, 0.9369047619047619069, 0.9375000000000000000 ),
 .UNSPECIFIED. ) 
 CURVE ( )  GEOMETRIC_REPRESENTATION_ITEM ( )  RATIONAL_B_SPLINE_CURVE ( ( 0.9330127018922194093, 0.9330127018922194093, 1.000000000000000000, 0.8660254037844387076, 1.000000000000000000, 0.8660254037844387076, 1.000000000000000000, 0.9330127018922194093, 0.9330127018922194093 ) ) 
 REPRESENTATION_ITEM ( '' )  );
#31138 = CARTESIAN_POINT ( 'NONE',  ( -4.458734124999999437, 21.60416666803225993, -2.574251347313719407 ) ) ;
#31139 = CARTESIAN_POINT ( 'NONE',  ( -55.00000000000002132, -155.0000000000000284, 1.734723475976807094E-15 ) ) ;
#31140 = CARTESIAN_POINT ( 'NONE',  ( 1.339745962155612702, 1.705341801261480272, -5.000000000000000000 ) ) ;
#31141 = CARTESIAN_POINT ( 'NONE',  ( -4.458734124999999437, -78.56249999863440792, 0.000000000000000000 ) ) ;
#31142 = CARTESIAN_POINT ( 'NONE',  ( -2.499999999999996447, -63.83333333333332860, 4.330127018922195425 ) ) ;
#31143 = CARTESIAN_POINT ( 'NONE',  ( -56.66612745406273888, -151.3125000000000000, -5.149110718188520508 ) ) ;
#31144 = CARTESIAN_POINT ( 'NONE',  ( -2.500000000000000444, 26.95833333606451632, -4.330127018922193649 ) ) ;
#31145 = ORIENTED_EDGE ( 'NONE', *, *, #22740, .T. ) ;
#31146 = CARTESIAN_POINT ( 'NONE',  ( 5.000000000000000000, 7.500000000000000000, -6.123233995736766282E-16 ) ) ;
#31148 = CARTESIAN_POINT ( 'NONE',  ( -2.499999999999996447, -23.83333333333333215, 4.330127018922195425 ) ) ;
#31147 = CARTESIAN_POINT ( 'NONE',  ( -2.071067811865306307, -149.6874999999999716, -5.000000000000171418 ) ) ;
#31149 = CARTESIAN_POINT ( 'NONE',  ( 2.229367062499998831, -27.64583333196774007, -3.861377020970580887 ) ) ;
#31150 = CARTESIAN_POINT ( 'NONE',  ( 4.458734124999999437, -88.81249999863439371, -5.460374474430324690E-16 ) ) ;
#31151 =( BOUNDED_CURVE ( )  B_SPLINE_CURVE ( 2, ( #7330, #3131, #26941, #16968, #46557, #56848, #41708, #56211, #61357 ),
 .UNSPECIFIED., .F., .F. ) 
 B_SPLINE_CURVE_WITH_KNOTS ( ( 3, 2, 2, 2, 3 ),
 ( 0.4625000000000000222, 0.4630952380952381153, 0.4642857142857143016, 0.4654761904761904878, 0.4660714285714285809 ),
 .UNSPECIFIED. ) 
 CURVE ( )  GEOMETRIC_REPRESENTATION_ITEM ( )  RATIONAL_B_SPLINE_CURVE ( ( 0.9330127018922194093, 0.9330127018922194093, 1.000000000000000000, 0.8660254037844387076, 1.000000000000000000, 0.8660254037844387076, 1.000000000000000000, 0.9330127018922194093, 0.9330127018922194093 ) ) 
 REPRESENTATION_ITEM ( '' )  );
#31152 = EDGE_CURVE ( 'NONE', #52220, #2151, #53260, .T. ) ;
#31153 = CARTESIAN_POINT ( 'NONE',  ( -2.500000000000000444, -22.04166666393548013, -4.330127018922193649 ) ) ;
#31155 = ORIENTED_EDGE ( 'NONE', *, *, #33485, .F. ) ;
#31154 = CARTESIAN_POINT ( 'NONE',  ( 4.458734125000001214, -52.89583333196772941, 2.574251347313718519 ) ) ;
#31156 = CARTESIAN_POINT ( 'NONE',  ( -6.972266317189433020E-16, -105.1249999972688016, -5.000000000000000000 ) ) ;
#31157 = CARTESIAN_POINT ( 'NONE',  ( 0.000000000000000000, -170.0000000000000000, 0.000000000000000000 ) ) ;
#31159 = ORIENTED_EDGE ( 'NONE', *, *, #51152, .F. ) ;
#31158 = CARTESIAN_POINT ( 'NONE',  ( -2.229367062499996610, -5.395833331967740953, 3.861377020970582219 ) ) ;
#31160 = CARTESIAN_POINT ( 'NONE',  ( -5.000000000000000000, -70.08333333333332860, -2.886751345948128211 ) ) ;
#31161 = CARTESIAN_POINT ( 'NONE',  ( 1.846868145590735200, -152.5000000013656347, -4.458734125000000326 ) ) ;
#31162 = CARTESIAN_POINT ( 'NONE',  ( -2.229367062499996610, -45.39583333196774362, 3.861377020970582219 ) ) ;
#31163 = LINE ( 'NONE', #7374, #52260 ) ;
#31164 = CARTESIAN_POINT ( 'NONE',  ( -9.184850993605147944E-16, -160.2500000000000000, 5.000000000000000000 ) ) ;
#31165 = CARTESIAN_POINT ( 'NONE',  ( 5.000000000000000000, -71.29166666393547303, -2.886751345948129988 ) ) ;
#31166 = CARTESIAN_POINT ( 'NONE',  ( 0.000000000000000000, -120.0000000000000000, 0.000000000000000000 ) ) ;
#31167 = CARTESIAN_POINT ( 'NONE',  ( -52.53715891517739323, -154.4375000000000284, -4.819101127000233298 ) ) ;
#31168 = EDGE_CURVE ( 'NONE', #37025, #19133, #29419, .T. ) ;
#31169 = CARTESIAN_POINT ( 'NONE',  ( -2.229367062500000163, -17.72916666530106866, -3.861377020970580443 ) ) ;
#31170 = CARTESIAN_POINT ( 'NONE',  ( 2.229367062499998831, -51.89583333196773651, -3.861377020970580887 ) ) ;
#31171 = CARTESIAN_POINT ( 'NONE',  ( -5.000000000000000000, -58.95833333060213732, -2.886751345948128211 ) ) ;
#31172 = CARTESIAN_POINT ( 'NONE',  ( 4.458734124999999437, -146.5000000013656347, 1.846868145590737864 ) ) ;
#31173 = CARTESIAN_POINT ( 'NONE',  ( -3.152548672688508926E-16, -93.81249999863440792, -5.148502694627439702 ) ) ;
#31174 = LINE ( 'NONE', #327, #60534 ) ;
#31175 = ORIENTED_EDGE ( 'NONE', *, *, #10172, .F. ) ;
#31176 = EDGE_CURVE ( 'NONE', #12980, #22037, #43591, .T. ) ;
#31177 = DIRECTION ( 'NONE',  ( 0.000000000000000000, 0.000000000000000000, 1.000000000000000000 ) ) ;
#31178 = CARTESIAN_POINT ( 'NONE',  ( -4.458734124999998549, 25.52083333469893134, 2.574251347313722516 ) ) ;
#31179 = CARTESIAN_POINT ( 'NONE',  ( -57.46284108482265651, -145.0625000027312126, 4.819101127000239515 ) ) ;
#31180 = EDGE_CURVE ( 'NONE', #59835, #42312, #41474, .T. ) ;
#31181 = CARTESIAN_POINT ( 'NONE',  ( 5.000000000000000000, -50.41666666666666430, -2.886751345948130876 ) ) ;
#31182 = CARTESIAN_POINT ( 'NONE',  ( -4.458734124999999437, -1.395833331967737179, -2.574251347313719407 ) ) ;
#31183 = EDGE_CURVE ( 'NONE', #59424, #7528, #30775, .T. ) ;
#31184 = FACE_OUTER_BOUND ( 'NONE', #32926, .T. ) ;
#31185 = CARTESIAN_POINT ( 'NONE',  ( 2.229367062499998831, -23.89583333196773651, -3.861377020970580887 ) ) ;
#31186 = CARTESIAN_POINT ( 'NONE',  ( 1.339745962155499015, -72.70534180126148271, 5.000000000000065725 ) ) ;
#31187 = CARTESIAN_POINT ( 'NONE',  ( -4.458734124999999437, -8.312499998634406140, 0.000000000000000000 ) ) ;
#31188 = CARTESIAN_POINT ( 'NONE',  ( 1.464175926609780648E-14, 23.87500000273118417, -5.000000000000000000 ) ) ;
#31189 = CARTESIAN_POINT ( 'NONE',  ( -4.458734124999999437, -145.0000000013656063, -1.846868145590735644 ) ) ;
#31190 = CARTESIAN_POINT ( 'NONE',  ( 4.458734124999999437, 14.93750000136559386, -5.460374474430324690E-16 ) ) ;
#31191 = ORIENTED_EDGE ( 'NONE', *, *, #44158, .T. ) ;
#31192 = CARTESIAN_POINT ( 'NONE',  ( 6.123233995736766282E-16, -170.0000000000000000, -5.000000000000000000 ) ) ;
#31193 = CARTESIAN_POINT ( 'NONE',  ( 1.339745962155612702, -57.16965819600733312, -5.000000000000000000 ) ) ;
#31195 = CARTESIAN_POINT ( 'NONE',  ( -2.229367062500000163, -21.47916666530107221, -3.861377020970580443 ) ) ;
#31194 = CARTESIAN_POINT ( 'NONE',  ( -4.999999999999999112, -87.91666666666667140, 2.886751345948131764 ) ) ;
#31196 = LINE ( 'NONE', #21560, #41681 ) ;
#31197 = CARTESIAN_POINT ( 'NONE',  ( 1.339745962155615144, -88.58034179853028434, 4.999999999999999112 ) ) ;
#31198 = CARTESIAN_POINT ( 'NONE',  ( -50.70258187064364108, -149.1250000013656063, 2.196230717870141014 ) ) ;
#31199 = CARTESIAN_POINT ( 'NONE',  ( 2.499999999999998668, -45.20833333060214443, -4.330127018922193649 ) ) ;
#31200 = CARTESIAN_POINT ( 'NONE',  ( -4.999999999999998224, -1.791666663935480353, 2.886751345948131764 ) ) ;
#31201 = CARTESIAN_POINT ( 'NONE',  ( -2.229367062499996610, 5.854166668032262599, 3.861377020970582219 ) ) ;
#31202 = DIRECTION ( 'NONE',  ( -0.000000000000000000, 1.000000000000000000, -0.000000000000000000 ) ) ;
#31203 = CARTESIAN_POINT ( 'NONE',  ( 0.000000000000000000, -120.0000000000000000, 0.000000000000000000 ) ) ;
#31204 = CARTESIAN_POINT ( 'NONE',  ( -4.458734124999999437, 14.60416666803226171, -2.574251347313719407 ) ) ;
#31205 = CARTESIAN_POINT ( 'NONE',  ( 4.458734125000001214, -69.89583333196773651, 2.574251347313718519 ) ) ;
#31206 = CARTESIAN_POINT ( 'NONE',  ( 9.457646018065525792E-16, -12.31249999863440259, 5.148502694627439702 ) ) ;
#31207 =( BOUNDED_CURVE ( )  B_SPLINE_CURVE ( 2, ( #6230, #50602, #11990, #31616, #26795 ),
 .UNSPECIFIED., .F., .F. ) 
 B_SPLINE_CURVE_WITH_KNOTS ( ( 3, 2, 3 ),
 ( 0.9979166666666666741, 0.9986111111111111160, 1.000000000000000000 ),
 .UNSPECIFIED. ) 
 CURVE ( )  GEOMETRIC_REPRESENTATION_ITEM ( )  RATIONAL_B_SPLINE_CURVE ( ( 0.9330127018922194093, 0.9330127018922194093, 1.000000000000000000, 0.8660254037844387076, 1.000000000000000000 ) ) 
 REPRESENTATION_ITEM ( '' )  );
#31208 = CARTESIAN_POINT ( 'NONE',  ( 5.000000000000000888, -2.583333333333333481, 2.886751345948126879 ) ) ;
#31209 = CARTESIAN_POINT ( 'NONE',  ( 4.458734125000000326, -164.3750000013656063, -1.846868145590734978 ) ) ;
#31210 = CARTESIAN_POINT ( 'NONE',  ( 6.123233995736766282E-16, -120.0000000000000000, -5.000000000000000000 ) ) ;
#31211 = CARTESIAN_POINT ( 'NONE',  ( 9.457646018065525792E-16, -61.06249999863440081, 5.148502694627439702 ) ) ;
#31212 = CARTESIAN_POINT ( 'NONE',  ( -4.999999999999999112, -96.79166666393545881, 2.886751345948131764 ) ) ;
#31213 = CARTESIAN_POINT ( 'NONE',  ( -6.972266317189433020E-16, -70.25000000000000000, -5.000000000000000000 ) ) ;
#31214 = CARTESIAN_POINT ( 'NONE',  ( -6.972266317189433020E-16, -89.12499999726880162, -5.000000000000000000 ) ) ;
#31215 = CARTESIAN_POINT ( 'NONE',  ( 9.457646018065525792E-16, -37.06249999863440792, 5.148502694627439702 ) ) ;
#31216 = CARTESIAN_POINT ( 'NONE',  ( -2.500000000000000444, -91.04166666393547303, -4.330127018922193649 ) ) ;
#31217 = CARTESIAN_POINT ( 'NONE',  ( -2.499999999999996447, -46.83333333333333570, 4.330127018922195425 ) ) ;
#31218 = CARTESIAN_POINT ( 'NONE',  ( -5.000000000000000000, -13.99999999999999822, 0.000000000000000000 ) ) ;
#31219 = ORIENTED_EDGE ( 'NONE', *, *, #37856, .F. ) ;
#31220 = CARTESIAN_POINT ( 'NONE',  ( -2.229367062499996610, -104.1458333319677365, 3.861377020970582219 ) ) ;
#31221 = CARTESIAN_POINT ( 'NONE',  ( -2.229367062500000163, -1.729166665301071992, -3.861377020970580443 ) ) ;
#31222 = CARTESIAN_POINT ( 'NONE',  ( 1.975475456537005874E-15, 12.24999999999999822, 5.000000000000000000 ) ) ;
#31223 = CARTESIAN_POINT ( 'NONE',  ( -5.000000000000000000, -6.999999999999999112, 0.000000000000000000 ) ) ;
#31224 = CARTESIAN_POINT ( 'NONE',  ( -4.458734124999999437, -73.31249999863439371, 0.000000000000000000 ) ) ;
#31225 = EDGE_CURVE ( 'NONE', #35143, #62889, #6181, .T. ) ;
#31226 = FACE_OUTER_BOUND ( 'NONE', #47303, .T. ) ;
#31227 = CARTESIAN_POINT ( 'NONE',  ( 5.000000000000000888, -8.458333330602146205, 2.886751345948126879 ) ) ;
#31229 = ORIENTED_EDGE ( 'NONE', *, *, #62998, .F. ) ;
#31228 = CARTESIAN_POINT ( 'NONE',  ( 9.457646018065525792E-16, -39.06249999863440081, 5.148502694627439702 ) ) ;
#31230 = CARTESIAN_POINT ( 'NONE',  ( -2.499999999999996447, -16.70833333060214443, 4.330127018922195425 ) ) ;
#31232 = ORIENTED_EDGE ( 'NONE', *, *, #59043, .T. ) ;
#31231 = CARTESIAN_POINT ( 'NONE',  ( 9.457646018065525792E-16, 13.68750000136559208, 5.148502694627439702 ) ) ;
#31233 = CARTESIAN_POINT ( 'NONE',  ( -1.339745962155613812, -49.08034179853029144, -5.000000000000000000 ) ) ;
#31234 = CARTESIAN_POINT ( 'NONE',  ( -2.500000000000000444, -53.16666666666666430, -4.330127018922193649 ) ) ;
#31235 = CARTESIAN_POINT ( 'NONE',  ( -4.458734124999999437, -28.64583333196774007, -2.574251347313719407 ) ) ;
#31236 = CARTESIAN_POINT ( 'NONE',  ( -6.972266317189433020E-16, -10.12499999726881406, -5.000000000000000000 ) ) ;
#31237 = CARTESIAN_POINT ( 'NONE',  ( -4.458734124999999437, -74.39583333196775072, -2.574251347313719407 ) ) ;
#31238 = CARTESIAN_POINT ( 'NONE',  ( 1.846868145590736310, -139.8750000013656063, 4.458734124999999437 ) ) ;
#31239 = CARTESIAN_POINT ( 'NONE',  ( 4.458734124999999437, -84.81249999863439371, -5.460374474430324690E-16 ) ) ;
#31240 = CARTESIAN_POINT ( 'NONE',  ( -50.70258187064364108, -136.3750000013656063, 2.196230717870141014 ) ) ;
#31241 = CARTESIAN_POINT ( 'NONE',  ( 9.457646018065525792E-16, -38.31249999863441502, 5.148502694627439702 ) ) ;
#31242 = CARTESIAN_POINT ( 'NONE',  ( 5.000000000000000000, -72.50000000000000000, -6.123233995736766282E-16 ) ) ;
#31243 = ORIENTED_EDGE ( 'NONE', *, *, #3156, .F. ) ;
#31244 = CARTESIAN_POINT ( 'NONE',  ( -4.458734124999999437, -79.56249999863440792, 0.000000000000000000 ) ) ;
#31245 = CARTESIAN_POINT ( 'NONE',  ( -53.23292615868056288, -134.9999999999999432, -4.104181387521468771 ) ) ;
#31246 = ORIENTED_EDGE ( 'NONE', *, *, #21146, .T. ) ;
#31247 =( BOUNDED_CURVE ( )  B_SPLINE_CURVE ( 2, ( #39998, #15578, #36149, #56415, #32584, #50941, #12959, #56087, #56728 ),
 .UNSPECIFIED., .F., .F. ) 
 B_SPLINE_CURVE_WITH_KNOTS ( ( 3, 2, 2, 2, 3 ),
 ( 0.1229166666666666741, 0.1236111111111111160, 0.1250000000000000000, 0.1263888888888888840, 0.1270833333333333259 ),
 .UNSPECIFIED. ) 
 CURVE ( )  GEOMETRIC_REPRESENTATION_ITEM ( )  RATIONAL_B_SPLINE_CURVE ( ( 0.9330127018922194093, 0.9330127018922200755, 1.000000000000000000, 0.8660254037844387076, 1.000000000000000000, 0.8660254037844387076, 1.000000000000000000, 0.9330127018922194093, 0.9330127018922194093 ) ) 
 REPRESENTATION_ITEM ( '' )  );
#31248 = CARTESIAN_POINT ( 'NONE',  ( 2.071067811865602959, -151.8125000000000284, -4.999999999999874767 ) ) ;
#31249 = CARTESIAN_POINT ( 'NONE',  ( -2.229367062500000163, -65.72916666530106511, -3.861377020970580443 ) ) ;
#31250 = CARTESIAN_POINT ( 'NONE',  ( -4.458734124999998549, -8.479166665301073991, 2.574251347313722516 ) ) ;
#31251 = ORIENTED_EDGE ( 'NONE', *, *, #43417, .F. ) ;
#31252 = CARTESIAN_POINT ( 'NONE',  ( -51.19402409849444524, -149.5000000000000284, -3.242614290531456334 ) ) ;
#31253 = CARTESIAN_POINT ( 'NONE',  ( 5.000000000000000888, -62.58333333333333570, 2.886751345948126879 ) ) ;
#31254 = ORIENTED_EDGE ( 'NONE', *, *, #49262, .T. ) ;
#31255 = CARTESIAN_POINT ( 'NONE',  ( 2.229367062500001939, -7.229166665301073103, 3.861377020970579999 ) ) ;
#31256 = AXIS2_PLACEMENT_3D ( 'NONE', #170, #24276, #43880 ) ;
#31257 = CARTESIAN_POINT ( 'NONE',  ( 4.458734124999998549, 6.270833334698928674, -2.574251347313721627 ) ) ;
#31258 = CARTESIAN_POINT ( 'NONE',  ( -2.499999999999996447, -11.70833333060214798, 4.330127018922195425 ) ) ;
#31259 = CARTESIAN_POINT ( 'NONE',  ( 1.846868145590736310, -160.6250000013656063, 4.458734124999997661 ) ) ;
#31260 = CARTESIAN_POINT ( 'NONE',  ( -4.458734124999999437, 29.35416666803225993, -2.574251347313719407 ) ) ;
#31261 = ORIENTED_EDGE ( 'NONE', *, *, #60913, .T. ) ;
#31262 = CARTESIAN_POINT ( 'NONE',  ( -4.458734124999999437, -84.31249999863439371, 0.000000000000000000 ) ) ;
#31263 = CARTESIAN_POINT ( 'NONE',  ( -4.458734124999999437, -2.312499998634407028, 0.000000000000000000 ) ) ;
#31264 = CARTESIAN_POINT ( 'NONE',  ( 1.339745962155615144, -71.58034179853027013, 4.999999999999999112 ) ) ;
#31265 = VECTOR ( 'NONE', #28703, 1000.000000000000000 ) ;
#31266 = CARTESIAN_POINT ( 'NONE',  ( 2.500000000000002220, -29.54166666393548013, 4.330127018922192761 ) ) ;
#31267 = CYLINDRICAL_SURFACE ( 'NONE', #18072, 5.000000000000000000 ) ;
#31268 = CARTESIAN_POINT ( 'NONE',  ( -2.229367062500000163, 24.52083333469892779, -3.861377020970580443 ) ) ;
#31269 = CARTESIAN_POINT ( 'NONE',  ( -6.972266317189433020E-16, -83.12499999726878741, -5.000000000000000000 ) ) ;
#31270 = CARTESIAN_POINT ( 'NONE',  ( 2.500000000000002220, -58.66666666666665719, 4.330127018922192761 ) ) ;
#31271 = CARTESIAN_POINT ( 'NONE',  ( 4.458734124999998549, -49.72916666530106511, -2.574251347313721627 ) ) ;
#31272 = CARTESIAN_POINT ( 'NONE',  ( -2.229367062499996610, -37.39583333196773651, 3.861377020970582219 ) ) ;
#31273 = CARTESIAN_POINT ( 'NONE',  ( -4.458734124999999437, 2.437500001365593860, 0.000000000000000000 ) ) ;
#31274 = CARTESIAN_POINT ( 'NONE',  ( -2.071067811865604735, -149.4375000027312410, 4.999999999999872990 ) ) ;
#31275 = CARTESIAN_POINT ( 'NONE',  ( 2.500000000000002220, 17.33333333333333215, 4.330127018922192761 ) ) ;
#31276 = CARTESIAN_POINT ( 'NONE',  ( 5.000000000000000888, -144.0625000027311842, -2.071067811865475505 ) ) ;
#31277 = LINE ( 'NONE', #16811, #18182 ) ;
#31278 = CARTESIAN_POINT ( 'NONE',  ( 4.458734124999999437, -44.81249999863440081, -5.460374474430324690E-16 ) ) ;
#31279 = CARTESIAN_POINT ( 'NONE',  ( -2.500000000000000444, -79.04166666393547303, -4.330127018922193649 ) ) ;
#31280 = CARTESIAN_POINT ( 'NONE',  ( -51.60603307380591787, -138.1875000013656347, -2.891590998281053704 ) ) ;
#31281 = CYLINDRICAL_SURFACE ( 'NONE', #23695, 5.000000000000000000 ) ;
#31282 = CARTESIAN_POINT ( 'NONE',  ( -5.000000000000000000, -88.08333333333332860, -2.886751345948128211 ) ) ;
#31283 = CARTESIAN_POINT ( 'NONE',  ( -2.229367062499996610, -86.39583333196773651, 3.861377020970582219 ) ) ;
#31284 = CARTESIAN_POINT ( 'NONE',  ( -3.152801135295367096, -160.3125000013656063, -3.152801135295367541 ) ) ;
#31285 = CARTESIAN_POINT ( 'NONE',  ( -0.3306966981848578069, -8.469326210127253063, -7.349897473154448413 ) ) ;
#31286 = CARTESIAN_POINT ( 'NONE',  ( 5.000000000000000888, -25.58333333333333215, 2.886751345948126879 ) ) ;
#31287 = DIRECTION ( 'NONE',  ( 0.000000000000000000, -1.000000000000000000, 0.000000000000000000 ) ) ;
#31288 = ORIENTED_EDGE ( 'NONE', *, *, #23528, .T. ) ;
#31289 = CARTESIAN_POINT ( 'NONE',  ( -4.458734124999998549, 23.52083333469892779, 2.574251347313722516 ) ) ;
#31290 = ORIENTED_EDGE ( 'NONE', *, *, #46703, .F. ) ;
#31291 = CARTESIAN_POINT ( 'NONE',  ( -3.152548672688508926E-16, -91.56249999863440792, -5.148502694627439702 ) ) ;
#31292 = CARTESIAN_POINT ( 'NONE',  ( 4.458734124999998549, 15.02083333469892601, -2.574251347313721627 ) ) ;
#31293 = CARTESIAN_POINT ( 'NONE',  ( -3.535250795749689387E-16, 18.87500000273118772, -5.773502691896257311 ) ) ;
#31294 = CARTESIAN_POINT ( 'NONE',  ( -4.999999999999998224, -2.791666663935478354, 2.886751345948131764 ) ) ;
#31295 = CARTESIAN_POINT ( 'NONE',  ( -3.535250795749689387E-16, 8.750000000000000000, -5.773502691896257311 ) ) ;
#31296 = CARTESIAN_POINT ( 'NONE',  ( 2.229367062500001939, -57.97916666530107932, 3.861377020970579999 ) ) ;
#31297 = CARTESIAN_POINT ( 'NONE',  ( 2.229367062500001939, -13.97916666530107221, 3.861377020970579999 ) ) ;
#31298 = CARTESIAN_POINT ( 'NONE',  ( -6.972266317189433020E-16, -6.249999999999999112, -5.000000000000000000 ) ) ;
#31299 = CARTESIAN_POINT ( 'NONE',  ( -57.89159099828107458, -136.9375000013655779, -3.393966926194107447 ) ) ;
#31300 = CARTESIAN_POINT ( 'NONE',  ( -2.500000000000000444, 13.83333333333333215, -4.330127018922193649 ) ) ;
#31301 = CARTESIAN_POINT ( 'NONE',  ( 2.499999999999998668, -33.20833333060215153, -4.330127018922193649 ) ) ;
#31302 = CARTESIAN_POINT ( 'NONE',  ( 2.499999999999998668, -11.20833333060214798, -4.330127018922193649 ) ) ;
#31303 = CARTESIAN_POINT ( 'NONE',  ( 1.060575238724906964E-15, -35.75000000000000711, 5.773502691896257311 ) ) ;
#31304 = LINE ( 'NONE', #52205, #63371 ) ;
#31305 = EDGE_CURVE ( 'NONE', #16219, #35844, #36188, .T. ) ;
#31307 = CARTESIAN_POINT ( 'NONE',  ( -4.458734124999998549, -14.47916666530107221, 2.574251347313722516 ) ) ;
#31306 = CARTESIAN_POINT ( 'NONE',  ( -1.339745962155610925, -42.79465819873851729, 5.000000000000000000 ) ) ;
#31308 = CARTESIAN_POINT ( 'NONE',  ( -9.184850993605147944E-16, -140.3750000027312126, 5.000000000000000000 ) ) ;
#31309 = CARTESIAN_POINT ( 'NONE',  ( 4.458734124999999437, -59.81249999863440081, -5.460374474430324690E-16 ) ) ;
#31310 = CARTESIAN_POINT ( 'NONE',  ( 4.458734125000000326, -150.6250000013655779, -1.846868145590734978 ) ) ;
#31311 = CARTESIAN_POINT ( 'NONE',  ( -2.229367062500000163, -72.47916666530107932, -3.861377020970580443 ) ) ;
#31312 = CARTESIAN_POINT ( 'NONE',  ( -57.89159099828107458, -148.9375000013656063, -3.393966926194107447 ) ) ;
#31313 = VECTOR ( 'NONE', #13534, 1000.000000000000000 ) ;
#31314 = CARTESIAN_POINT ( 'NONE',  ( 2.229367062499998831, -21.89583333196774007, -3.861377020970580887 ) ) ;
#31315 = CARTESIAN_POINT ( 'NONE',  ( 2.499999999999998668, -62.20833333060214443, -4.330127018922193649 ) ) ;
#31316 = ORIENTED_EDGE ( 'NONE', *, *, #63608, .F. ) ;
#31317 = CARTESIAN_POINT ( 'NONE',  ( 2.500000000000002220, -31.54166666393548724, 4.330127018922192761 ) ) ;
#31318 = VERTEX_POINT ( 'NONE', #59352 ) ;
#31319 = CARTESIAN_POINT ( 'NONE',  ( 4.458734124999999437, -64.06249999863440792, -5.460374474430324690E-16 ) ) ;
#31321 = CARTESIAN_POINT ( 'NONE',  ( 2.500000000000002220, 11.45833333606451809, 4.330127018922192761 ) ) ;
#31320 = CARTESIAN_POINT ( 'NONE',  ( -58.24261429053147765, -149.3750000027312126, -3.805975901505573855 ) ) ;
#31322 = CARTESIAN_POINT ( 'NONE',  ( -1.846868145590734756, -151.1250000013655779, -4.458734125000000326 ) ) ;
#31323 = ORIENTED_EDGE ( 'NONE', *, *, #33581, .F. ) ;
#31324 = CYLINDRICAL_SURFACE ( 'NONE', #53942, 5.000000000000000000 ) ;
#31325 = CARTESIAN_POINT ( 'NONE',  ( -50.01589407740564042, -125.6250000000000142, 0.3983568153799778022 ) ) ;
#31326 = CARTESIAN_POINT ( 'NONE',  ( 0.000000000000000000, -170.0000000000000000, 0.000000000000000000 ) ) ;
#31327 = CARTESIAN_POINT ( 'NONE',  ( -2.229367062499996610, -48.39583333196772941, 3.861377020970582219 ) ) ;
#31328 = VERTEX_POINT ( 'NONE', #6288 ) ;
#31329 =( BOUNDED_CURVE ( )  B_SPLINE_CURVE ( 2, ( #54362, #5466, #20593, #50160, #54675, #49840, #54028, #29256, #6115 ),
 .UNSPECIFIED., .F., .F. ) 
 B_SPLINE_CURVE_WITH_KNOTS ( ( 3, 2, 2, 2, 3 ),
 ( 0.5020833333333333259, 0.5027777777777777679, 0.5041666666666666519, 0.5055555555555555358, 0.5062499999999999778 ),
 .UNSPECIFIED. ) 
 CURVE ( )  GEOMETRIC_REPRESENTATION_ITEM ( )  RATIONAL_B_SPLINE_CURVE ( ( 0.9330127018922194093, 0.9330127018922194093, 1.000000000000000000, 0.8660254037844387076, 1.000000000000000000, 0.8660254037844387076, 1.000000000000000000, 0.9330127018922194093, 0.9330127018922194093 ) ) 
 REPRESENTATION_ITEM ( '' )  );
#31330 = CARTESIAN_POINT ( 'NONE',  ( 2.229367062500001939, 11.02083333469892956, 3.861377020970579999 ) ) ;
#31331 = CARTESIAN_POINT ( 'NONE',  ( 4.458734124999999437, 25.18750000136559208, -5.460374474430324690E-16 ) ) ;
#31332 = CARTESIAN_POINT ( 'NONE',  ( -57.19623071787017210, -148.3750000013656063, 4.297418129356382899 ) ) ;
#31333 = CARTESIAN_POINT ( 'NONE',  ( 1.339745962155615144, -61.58034179853027723, 4.999999999999999112 ) ) ;
#31334 = ORIENTED_EDGE ( 'NONE', *, *, #28640, .F. ) ;
#31335 = CARTESIAN_POINT ( 'NONE',  ( -4.458734124999999437, -71.39583333196773651, -2.574251347313719407 ) ) ;
#31336 = CARTESIAN_POINT ( 'NONE',  ( 1.060314165522845187, 8.048081368953960535, -7.659344964963204383 ) ) ;
#31337 = CARTESIAN_POINT ( 'NONE',  ( -4.458734124999999437, 12.68750000136559564, 0.000000000000000000 ) ) ;
#31338 = CARTESIAN_POINT ( 'NONE',  ( 2.500000000000002220, 7.458333336064517205, 4.330127018922192761 ) ) ;
#31339 = CARTESIAN_POINT ( 'NONE',  ( -54.60164318462004474, -152.5000000027312410, -4.984105922594373794 ) ) ;
#31340 = CARTESIAN_POINT ( 'NONE',  ( -4.458734124999999437, -52.56249999863440792, 0.000000000000000000 ) ) ;
#31341 = CARTESIAN_POINT ( 'NONE',  ( -5.000000000000000000, -12.87499999726881050, 0.000000000000000000 ) ) ;
#31342 = FACE_OUTER_BOUND ( 'NONE', #7877, .T. ) ;
#31343 = CARTESIAN_POINT ( 'NONE',  ( 4.458734125000000326, -20.14583333196774007, 2.574251347313718519 ) ) ;
#31344 = ORIENTED_EDGE ( 'NONE', *, *, #787, .T. ) ;
#31345 = FACE_OUTER_BOUND ( 'NONE', #5679, .T. ) ;
#31346 = CARTESIAN_POINT ( 'NONE',  ( 4.458734125000001214, -102.8958333319677365, 2.574251347313718519 ) ) ;
#31347 = CARTESIAN_POINT ( 'NONE',  ( 2.071067811865476394, -159.3125000027311842, 5.000000000000000000 ) ) ;
#31348 = EDGE_LOOP ( 'NONE', ( #404, #38128, #30763, #28320, #50633, #1815 ) ) ;
#31349 = CARTESIAN_POINT ( 'NONE',  ( -3.152548672688508926E-16, -104.8124999986344079, -5.148502694627439702 ) ) ;
#31350 = ADVANCED_FACE ( 'NONE', ( #5966 ), #11413, .T. ) ;
#31351 = CARTESIAN_POINT ( 'NONE',  ( 2.229367062500001939, -27.97916666530107221, 3.861377020970579999 ) ) ;
#31352 = CARTESIAN_POINT ( 'NONE',  ( -5.000000000000000000, -64.87499999726881583, 0.000000000000000000 ) ) ;
#31353 = VECTOR ( 'NONE', #44368, 1000.000000000000000 ) ;
#31354 = CARTESIAN_POINT ( 'NONE',  ( -50.40829686548195099, -152.2500000013656347, -1.485763867205728284 ) ) ;
#31355 = CARTESIAN_POINT ( 'NONE',  ( -53.51423613279429503, -143.2500000013656063, 4.591703134518083651 ) ) ;
#31356 = CARTESIAN_POINT ( 'NONE',  ( 2.229367062500001939, -24.97916666530106866, 3.861377020970579999 ) ) ;
#31357 = CARTESIAN_POINT ( 'NONE',  ( -4.458734124999999437, -64.64583333196773651, -2.574251347313719407 ) ) ;
#31358 = CARTESIAN_POINT ( 'NONE',  ( -60.14911071818854538, -137.0625000000000284, 1.666127454062681146 ) ) ;
#31359 = CARTESIAN_POINT ( 'NONE',  ( -3.152548672688508926E-16, -26.56249999863440436, -5.148502694627439702 ) ) ;
#31360 = CARTESIAN_POINT ( 'NONE',  ( 4.330127018922258486, 45.00000000000000000, 7.499999999999910294 ) ) ;
#31361 = CARTESIAN_POINT ( 'NONE',  ( 3.535533905932738197, -150.8750000000000000, -3.535533905932738197 ) ) ;
#31362 = CARTESIAN_POINT ( 'NONE',  ( 5.000000000000000000, -10.41666666666666430, -2.886751345948129988 ) ) ;
#31363 = CARTESIAN_POINT ( 'NONE',  ( -4.458734125000001214, -152.8750000013655779, 1.846868145590734089 ) ) ;
#31364 = ORIENTED_EDGE ( 'NONE', *, *, #20854, .T. ) ;
#31365 = CARTESIAN_POINT ( 'NONE',  ( 2.229367062499998831, -50.89583333196772941, -3.861377020970580887 ) ) ;
#31366 = CARTESIAN_POINT ( 'NONE',  ( 1.975475456537005874E-15, -86.62499999726880162, 5.000000000000000000 ) ) ;
#31367 = CARTESIAN_POINT ( 'NONE',  ( -57.46284108482265651, -135.9375000000000284, 4.819101127000238627 ) ) ;
#31368 = CARTESIAN_POINT ( 'NONE',  ( 2.500000000000002220, 22.33333333333333215, 4.330127018922192761 ) ) ;
#31369 = CARTESIAN_POINT ( 'NONE',  ( 0.000000000000000000, -170.0000000000000000, 5.000000000000000000 ) ) ;
#31370 = CARTESIAN_POINT ( 'NONE',  ( 4.458734125000001214, 4.104166668032260823, 2.574251347313718519 ) ) ;
#31371 = ADVANCED_FACE ( 'NONE', ( #35549 ), #54531, .T. ) ;
#31372 = LINE ( 'NONE', #26239, #15433 ) ;
#31373 = ADVANCED_FACE ( 'NONE', ( #40679 ), #55809, .T. ) ;
#31374 = CARTESIAN_POINT ( 'NONE',  ( 5.000000000000000000, -95.37499999726881583, -6.123233995736766282E-16 ) ) ;
#31375 = CYLINDRICAL_SURFACE ( 'NONE', #2681, 5.000000000000000000 ) ;
#31376 = CARTESIAN_POINT ( 'NONE',  ( 4.458734124999998549, 13.02083333469892779, -2.574251347313721627 ) ) ;
#31377 =( BOUNDED_CURVE ( )  B_SPLINE_CURVE ( 2, ( #36215, #45540, #60990, #11123, #25922, #11755, #46817, #16280, #35898 ),
 .UNSPECIFIED., .F., .F. ) 
 B_SPLINE_CURVE_WITH_KNOTS ( ( 3, 2, 2, 2, 3 ),
 ( 0.8562499999999999556, 0.8569444444444443976, 0.8583333333333332815, 0.8597222222222222765, 0.8604166666666667185 ),
 .UNSPECIFIED. ) 
 CURVE ( )  GEOMETRIC_REPRESENTATION_ITEM ( )  RATIONAL_B_SPLINE_CURVE ( ( 0.9330127018922194093, 0.9330127018922194093, 1.000000000000000000, 0.8660254037844387076, 1.000000000000000000, 0.8660254037844387076, 1.000000000000000000, 0.9330127018922194093, 0.9330127018922194093 ) ) 
 REPRESENTATION_ITEM ( '' )  );
#31378 = CARTESIAN_POINT ( 'NONE',  ( -3.535250795749689387E-16, 0.8750000027311874984, -5.773502691896257311 ) ) ;
#31379 = ORIENTED_EDGE ( 'NONE', *, *, #54341, .T. ) ;
#31380 = CARTESIAN_POINT ( 'NONE',  ( -6.972266317189433020E-16, -23.12499999726880873, -5.000000000000000000 ) ) ;
#31381 = ORIENTED_EDGE ( 'NONE', *, *, #61823, .F. ) ;
#31382 = CARTESIAN_POINT ( 'NONE',  ( 2.499999999999998668, 27.79166666939785202, -4.330127018922193649 ) ) ;
#31383 = CARTESIAN_POINT ( 'NONE',  ( -2.229367062499996610, -41.14583333196773651, 3.861377020970582219 ) ) ;
#31384 = CARTESIAN_POINT ( 'NONE',  ( 4.458734124999999437, -164.7500000013656063, 1.846868145590737864 ) ) ;
#31385 = EDGE_CURVE ( 'NONE', #1507, #40464, #12179, .T. ) ;
#31386 = CARTESIAN_POINT ( 'NONE',  ( 5.000000000000000000, -43.29166666393548724, -2.886751345948129988 ) ) ;
#31387 = ORIENTED_EDGE ( 'NONE', *, *, #62040, .T. ) ;
#31388 = CARTESIAN_POINT ( 'NONE',  ( -4.458734124999998549, -19.22916666530106866, 2.574251347313722516 ) ) ;
#31389 = ORIENTED_EDGE ( 'NONE', *, *, #2353, .F. ) ;
#31390 = CARTESIAN_POINT ( 'NONE',  ( 5.000000000000000888, -88.58333333333332860, 2.886751345948126879 ) ) ;
#31391 = CARTESIAN_POINT ( 'NONE',  ( -1.846868145590734756, -164.1250000013656063, -4.458734125000000326 ) ) ;
#31393 = ORIENTED_EDGE ( 'NONE', *, *, #52689, .F. ) ;
#31392 = CARTESIAN_POINT ( 'NONE',  ( 1.062108568985190270E-13, -28.12499999726880873, -4.999999999999999112 ) ) ;
#31394 = CARTESIAN_POINT ( 'NONE',  ( -50.18089887299979068, -140.6875000000000284, 2.462841084822635640 ) ) ;
#31395 = CARTESIAN_POINT ( 'NONE',  ( 4.458734124999998549, -30.97916666530107577, -2.574251347313721627 ) ) ;
#31396 = CARTESIAN_POINT ( 'NONE',  ( -6.972266317189433020E-16, 20.74999999999999645, -5.000000000000000000 ) ) ;
#31397 = VERTEX_POINT ( 'NONE', #44547 ) ;
#31398 = EDGE_CURVE ( 'NONE', #18523, #1698, #20756, .T. ) ;
#31399 = CARTESIAN_POINT ( 'NONE',  ( -4.458734124999999437, -76.31249999863440792, 0.000000000000000000 ) ) ;
#31400 = CARTESIAN_POINT ( 'NONE',  ( 4.458734124999999437, 28.18750000136559208, -5.460374474430324690E-16 ) ) ;
#31401 = CARTESIAN_POINT ( 'NONE',  ( -6.972266317189433020E-16, -54.24999999999999289, -5.000000000000000000 ) ) ;
#31402 = VERTEX_POINT ( 'NONE', #503 ) ;
#31403 = CARTESIAN_POINT ( 'NONE',  ( 1.975475456537005874E-15, 5.375000002731185944, 5.000000000000000000 ) ) ;
#31404 = CARTESIAN_POINT ( 'NONE',  ( -57.89159099828107458, -142.9375000013656063, -3.393966926194107447 ) ) ;
#31405 = CARTESIAN_POINT ( 'NONE',  ( -2.229367062500000163, -82.72916666530106511, -3.861377020970580443 ) ) ;
#31406 = CARTESIAN_POINT ( 'NONE',  ( -50.18089887299979068, -128.8125000027312126, 2.462841084822635640 ) ) ;
#31407 = CARTESIAN_POINT ( 'NONE',  ( 5.000000000000000000, -143.0000000000000284, 0.000000000000000000 ) ) ;
#31408 = CARTESIAN_POINT ( 'NONE',  ( -4.458734124999999437, -142.1875000013656063, -5.460374474430324690E-16 ) ) ;
#31409 = CARTESIAN_POINT ( 'NONE',  ( 5.000000000000000888, 24.41666666666666785, 2.886751345948126879 ) ) ;
#31410 = CARTESIAN_POINT ( 'NONE',  ( 2.229367062499998831, -48.64583333196772941, -3.861377020970580887 ) ) ;
#31411 = CARTESIAN_POINT ( 'NONE',  ( 4.458734124999999437, -45.81249999863440081, -5.460374474430324690E-16 ) ) ;
#31412 = CARTESIAN_POINT ( 'NONE',  ( 9.457646018065525792E-16, 26.93750000136559564, 5.148502694627439702 ) ) ;
#31413 = CARTESIAN_POINT ( 'NONE',  ( -2.500000000000000444, -108.1666666666666572, -4.330127018922193649 ) ) ;
#31414 = LINE ( 'NONE', #61664, #5277 ) ;
#31415 = CARTESIAN_POINT ( 'NONE',  ( -4.458734124999999437, -38.64583333196772941, -2.574251347313719407 ) ) ;
#31416 = CARTESIAN_POINT ( 'NONE',  ( -4.999999999999999112, 3.208333336064520758, 2.886751345948131764 ) ) ;
#31417 = LINE ( 'NONE', #7635, #41729 ) ;
#31418 = CARTESIAN_POINT ( 'NONE',  ( -59.59170313451811296, -129.5000000013656347, 1.485763867205729394 ) ) ;
#31419 = CARTESIAN_POINT ( 'NONE',  ( 4.458734124999998549, -77.97916666530106511, -2.574251347313721627 ) ) ;
#31420 = CARTESIAN_POINT ( 'NONE',  ( 5.000000000000000888, -71.58333333333332860, 2.886751345948126879 ) ) ;
#31421 = CARTESIAN_POINT ( 'NONE',  ( -4.458734124999997661, -98.22916666530103669, 2.574251347313722516 ) ) ;
#31422 =( BOUNDED_CURVE ( )  B_SPLINE_CURVE ( 2, ( #33629, #52933, #53248, #9184, #28796, #39074, #58392, #18210, #48412 ),
 .UNSPECIFIED., .F., .F. ) 
 B_SPLINE_CURVE_WITH_KNOTS ( ( 3, 2, 2, 2, 3 ),
 ( 0.03125000000000000000, 0.03194444444444444198, 0.03333333333333333287, 0.03472222222222222376, 0.03541666666666666574 ),
 .UNSPECIFIED. ) 
 CURVE ( )  GEOMETRIC_REPRESENTATION_ITEM ( )  RATIONAL_B_SPLINE_CURVE ( ( 0.9330127018922194093, 0.9330127018922195203, 1.000000000000000000, 0.8660254037844387076, 1.000000000000000000, 0.8660254037844387076, 1.000000000000000000, 0.9330127018922194093, 0.9330127018922194093 ) ) 
 REPRESENTATION_ITEM ( '' )  );
#31423 = CARTESIAN_POINT ( 'NONE',  ( 9.457646018065525792E-16, -5.312499998634401699, 5.148502694627439702 ) ) ;
#31424 = EDGE_LOOP ( 'NONE', ( #27987, #60364, #14436, #4520 ) ) ;
#31425 = CARTESIAN_POINT ( 'NONE',  ( -6.972266317189433020E-16, -68.12499999726881583, -5.000000000000000000 ) ) ;
#31426 = CARTESIAN_POINT ( 'NONE',  ( -1.339745962155610925, -85.66965819600731891, 5.000000000000000000 ) ) ;
#31427 = CARTESIAN_POINT ( 'NONE',  ( 9.457646018065525792E-16, -88.06249999863439371, 5.148502694627439702 ) ) ;
#31428 = FACE_OUTER_BOUND ( 'NONE', #51255, .T. ) ;
#31429 = CARTESIAN_POINT ( 'NONE',  ( 2.229367062499998831, -87.89583333196773651, -3.861377020970580887 ) ) ;
#31430 = ADVANCED_FACE ( 'NONE', ( #10452 ), #49696, .T. ) ;
#31431 = CARTESIAN_POINT ( 'NONE',  ( -3.152548672688508926E-16, 13.18750000136559208, -5.148502694627439702 ) ) ;
#31432 = LINE ( 'NONE', #40454, #27410 ) ;
#31433 = CARTESIAN_POINT ( 'NONE',  ( -57.89159099828107458, -133.6875000013656063, -3.393966926194107447 ) ) ;
#31434 = CARTESIAN_POINT ( 'NONE',  ( 2.229367062499998831, -6.645833331967741842, -3.861377020970580887 ) ) ;
#31435 = CARTESIAN_POINT ( 'NONE',  ( -2.229367062499996610, 17.60416666803225993, 3.861377020970582219 ) ) ;
#31436 = CARTESIAN_POINT ( 'NONE',  ( -4.458734124999999437, -50.56249999863440792, 0.000000000000000000 ) ) ;
#31437 = CARTESIAN_POINT ( 'NONE',  ( -1.339745962155610925, -15.66965819600733134, 5.000000000000000000 ) ) ;
#31438 = CARTESIAN_POINT ( 'NONE',  ( -2.229367062500000163, -84.47916666530107932, -3.861377020970580443 ) ) ;
#31439 = CARTESIAN_POINT ( 'NONE',  ( 2.229367062499998831, -5.645833331967740953, -3.861377020970580887 ) ) ;
#31440 = EDGE_LOOP ( 'NONE', ( #8319, #27262, #2954, #16464 ) ) ;
#31441 = CARTESIAN_POINT ( 'NONE',  ( 4.458734124999998549, -36.97916666530107221, -2.574251347313721627 ) ) ;
#31442 = AXIS2_PLACEMENT_3D ( 'NONE', #38042, #58294, #3953 ) ;
#31443 = CARTESIAN_POINT ( 'NONE',  ( -51.60603307380591787, -127.1875000013656063, -2.891590998281053704 ) ) ;
#31444 = CARTESIAN_POINT ( 'NONE',  ( -4.458734124999999437, -72.31249999863439371, 0.000000000000000000 ) ) ;
#31445 = CARTESIAN_POINT ( 'NONE',  ( -2.500000000000000444, -109.0416666639354730, -4.330127018922193649 ) ) ;
#31446 = AXIS2_PLACEMENT_3D ( 'NONE', #50184, #45043, #35719 ) ;
#31447 = AXIS2_PLACEMENT_3D ( 'NONE', #48425, #13394, #33017 ) ;
#31448 = CARTESIAN_POINT ( 'NONE',  ( -3.152548672688508926E-16, 22.43750000136559208, -5.148502694627439702 ) ) ;
#31449 = CARTESIAN_POINT ( 'NONE',  ( -4.999999999999998224, -93.91666666666665719, 2.886751345948131764 ) ) ;
#31450 = EDGE_CURVE ( 'NONE', #49754, #18888, #44870, .T. ) ;
#31451 = CARTESIAN_POINT ( 'NONE',  ( -1.339745962155610925, -25.66965819600733312, 5.000000000000000000 ) ) ;
#31452 = CARTESIAN_POINT ( 'NONE',  ( 4.458734124999998549, -75.97916666530106511, -2.574251347313721627 ) ) ;
#31453 = CARTESIAN_POINT ( 'NONE',  ( -2.499999999999996447, -66.83333333333332860, 4.330127018922195425 ) ) ;
#31454 = CARTESIAN_POINT ( 'NONE',  ( 0.000000000000000000, -170.0000000000000000, 0.000000000000000000 ) ) ;
#31455 = CARTESIAN_POINT ( 'NONE',  ( -2.500000000000000444, 18.95833333606451632, -4.330127018922193649 ) ) ;
#31456 = ORIENTED_EDGE ( 'NONE', *, *, #30003, .T. ) ;
#31457 = CYLINDRICAL_SURFACE ( 'NONE', #52036, 5.000000000000000000 ) ;
#31458 = CARTESIAN_POINT ( 'NONE',  ( -1.339745962155610925, 9.205341801261479162, 5.000000000000000000 ) ) ;
#31460 = CARTESIAN_POINT ( 'NONE',  ( -3.535250795749689387E-16, -23.25000000000000000, -5.773502691896257311 ) ) ;
#31459 = CARTESIAN_POINT ( 'NONE',  ( -5.000000000000000888, -149.4375000000000000, 2.071067811865474617 ) ) ;
#31461 = CARTESIAN_POINT ( 'NONE',  ( 4.458734124999999437, -26.81249999863440081, -5.460374474430324690E-16 ) ) ;
#31462 = CARTESIAN_POINT ( 'NONE',  ( 5.000000000000000000, -62.41666666666666430, -2.886751345948130876 ) ) ;
#31463 = CARTESIAN_POINT ( 'NONE',  ( -2.500000000000000444, -26.04166666393547658, -4.330127018922193649 ) ) ;
#31465 = VERTEX_POINT ( 'NONE', #12374 ) ;
#31464 = CARTESIAN_POINT ( 'NONE',  ( 4.458734125000001214, -54.89583333196773651, 2.574251347313718519 ) ) ;
#31466 = CARTESIAN_POINT ( 'NONE',  ( 0.000000000000000000, 0.000000000000000000, 0.000000000000000000 ) ) ;
#31467 = CARTESIAN_POINT ( 'NONE',  ( 5.000000000000000000, -59.37499999726880873, -6.123233995736766282E-16 ) ) ;
#31469 = ORIENTED_EDGE ( 'NONE', *, *, #15773, .T. ) ;
#31468 = CARTESIAN_POINT ( 'NONE',  ( -3.152548672688508926E-16, -3.812499998634408360, -5.148502694627439702 ) ) ;
#31470 = CARTESIAN_POINT ( 'NONE',  ( 5.000000000000000888, -71.58333333333332860, 2.886751345948126879 ) ) ;
#31471 = CARTESIAN_POINT ( 'NONE',  ( -50.40829686548195099, -138.0000000013656063, -1.485763867205728284 ) ) ;
#31472 = CARTESIAN_POINT ( 'NONE',  ( 2.229367062499998831, -47.89583333196774362, -3.861377020970580887 ) ) ;
#31473 = DIRECTION ( 'NONE',  ( -0.000000000000000000, 1.000000000000000000, -0.000000000000000000 ) ) ;
#31474 = CARTESIAN_POINT ( 'NONE',  ( -2.499999999999996447, -70.70833333060214443, 4.330127018922195425 ) ) ;
#31475 = CARTESIAN_POINT ( 'NONE',  ( -1.339745962155613812, -82.08034179853031276, -5.000000000000000000 ) ) ;
#31476 = CARTESIAN_POINT ( 'NONE',  ( -58.80597590150559739, -153.0000000000000284, 3.242614290531460330 ) ) ;
#31477 = CARTESIAN_POINT ( 'NONE',  ( -4.458734124999998549, -18.47916666530106866, 2.574251347313722516 ) ) ;
#31478 = CARTESIAN_POINT ( 'NONE',  ( -4.458734124999999437, -53.56249999863439371, 0.000000000000000000 ) ) ;
#31479 = CARTESIAN_POINT ( 'NONE',  ( 1.339745962155608039, 22.29465819873851729, 5.000000000000003553 ) ) ;
#31480 = CARTESIAN_POINT ( 'NONE',  ( 4.458734124999999437, -139.4375000013656063, 0.000000000000000000 ) ) ;
#31481 = CARTESIAN_POINT ( 'NONE',  ( 4.458734124999999437, -93.06249999863440792, -5.460374474430324690E-16 ) ) ;
#31482 = CARTESIAN_POINT ( 'NONE',  ( 5.000000000000000888, -2.583333333333333481, 2.886751345948126879 ) ) ;
#31483 = ORIENTED_EDGE ( 'NONE', *, *, #40513, .T. ) ;
#31484 = CARTESIAN_POINT ( 'NONE',  ( -6.972266317189433020E-16, -29.25000000000000000, -5.000000000000000000 ) ) ;
#31485 = CARTESIAN_POINT ( 'NONE',  ( 4.458734124999998549, 24.02083333469892423, -2.574251347313721627 ) ) ;
#31486 = CARTESIAN_POINT ( 'NONE',  ( -57.46284108482265651, -147.0625000027312126, 4.819101127000239515 ) ) ;
#31487 = CARTESIAN_POINT ( 'NONE',  ( 5.000000000000000888, -50.58333333333332860, 2.886751345948126879 ) ) ;
#31488 = AXIS2_PLACEMENT_3D ( 'NONE', #12723, #47143, #3090 ) ;
#31489 = CARTESIAN_POINT ( 'NONE',  ( -4.458734124999999437, -0.3958333319677397322, -2.574251347313719407 ) ) ;
#31490 = AXIS2_PLACEMENT_3D ( 'NONE', #35642, #21163, #59776 ) ;
#31491 = CARTESIAN_POINT ( 'NONE',  ( 4.458734124999998549, -93.97916666530106511, -2.574251347313721627 ) ) ;
#31492 = CARTESIAN_POINT ( 'NONE',  ( 4.458734124999999437, -147.6875000013656063, 0.000000000000000000 ) ) ;
#31493 = CARTESIAN_POINT ( 'NONE',  ( -2.229367062500000163, -24.72916666530106866, -3.861377020970580443 ) ) ;
#31494 = CARTESIAN_POINT ( 'NONE',  ( -7.500000000000001776, 2.932633423934442263, -0.4709827563909292358 ) ) ;
#31495 = CARTESIAN_POINT ( 'NONE',  ( -4.458734124999999437, -64.64583333196772230, -2.574251347313719407 ) ) ;
#31496 = FACE_OUTER_BOUND ( 'NONE', #565, .T. ) ;
#31497 = CARTESIAN_POINT ( 'NONE',  ( -3.152548672688508926E-16, -9.562499998634406140, -5.148502694627439702 ) ) ;
#31498 = CARTESIAN_POINT ( 'NONE',  ( -6.972266317189433020E-16, -98.24999999999998579, -5.000000000000000000 ) ) ;
#31499 = CARTESIAN_POINT ( 'NONE',  ( 4.458734124999997661, -144.5000000013656063, 1.846868145590737864 ) ) ;
#31500 = CARTESIAN_POINT ( 'NONE',  ( 4.458734124999999437, 13.93750000136559386, -5.460374474430324690E-16 ) ) ;
#31501 = EDGE_LOOP ( 'NONE', ( #59101, #47390, #25884, #12353, #11253, #52513 ) ) ;
#31502 = CARTESIAN_POINT ( 'NONE',  ( -5.000000000000000888, -164.5625000027312126, 2.071067811865474617 ) ) ;
#31503 = CARTESIAN_POINT ( 'NONE',  ( -6.972266317189433020E-16, -8.249999999999998224, -5.000000000000000000 ) ) ;
#31505 = CARTESIAN_POINT ( 'NONE',  ( -3.152548672688508926E-16, -18.56249999863440792, -5.148502694627439702 ) ) ;
#31504 = CARTESIAN_POINT ( 'NONE',  ( -5.000000000000000000, -83.99999999999998579, 0.000000000000000000 ) ) ;
#31506 = CARTESIAN_POINT ( 'NONE',  ( 9.457646018065525792E-16, 28.68750000136559208, 5.148502694627439702 ) ) ;
#31507 = CARTESIAN_POINT ( 'NONE',  ( -1.339745962155610925, -5.794658198738521726, 5.000000000000000000 ) ) ;
#31508 =( BOUNDED_CURVE ( )  B_SPLINE_CURVE ( 2, ( #31654, #50638, #45810, #1771, #1452, #15906, #21053, #40660, #21372 ),
 .UNSPECIFIED., .F., .F. ) 
 B_SPLINE_CURVE_WITH_KNOTS ( ( 3, 2, 2, 2, 3 ),
 ( 0.2839285714285714191, 0.2845238095238095122, 0.2857142857142856984, 0.2869047619047618847, 0.2874999999999999778 ),
 .UNSPECIFIED. ) 
 CURVE ( )  GEOMETRIC_REPRESENTATION_ITEM ( )  RATIONAL_B_SPLINE_CURVE ( ( 0.9330127018922194093, 0.9330127018922194093, 1.000000000000000000, 0.8660254037844387076, 1.000000000000000000, 0.8660254037844387076, 1.000000000000000000, 0.9330127018922194093, 0.9330127018922194093 ) ) 
 REPRESENTATION_ITEM ( '' )  );
#31509 = CARTESIAN_POINT ( 'NONE',  ( -59.44456063193725015, -145.5625000013656063, -0.3552334253322034230 ) ) ;
#31510 = EDGE_CURVE ( 'NONE', #12052, #34023, #37144, .T. ) ;
#31511 = EDGE_CURVE ( 'NONE', #8991, #45549, #51929, .T. ) ;
#31512 = CARTESIAN_POINT ( 'NONE',  ( 5.000000000000000000, -47.29166666393547303, -2.886751345948129988 ) ) ;
#31513 = CARTESIAN_POINT ( 'NONE',  ( 5.000000000000000000, -41.29166666393548013, -2.886751345948130876 ) ) ;
#31514 = CARTESIAN_POINT ( 'NONE',  ( 4.458734124999998549, 7.270833334698930450, -2.574251347313721627 ) ) ;
#31515 = CARTESIAN_POINT ( 'NONE',  ( 2.499999999999998668, -56.20833333060214443, -4.330127018922193649 ) ) ;
#31517 = EDGE_CURVE ( 'NONE', #4102, #14760, #59141, .T. ) ;
#31516 = CARTESIAN_POINT ( 'NONE',  ( 0.000000000000000000, -170.0000000000000000, 0.000000000000000000 ) ) ;
#31518 = CARTESIAN_POINT ( 'NONE',  ( 4.458734124999999437, 14.18750000136559386, -5.460374474430324690E-16 ) ) ;
#31519 = CARTESIAN_POINT ( 'NONE',  ( -3.152548672688508926E-16, -65.56249999863440792, -5.148502694627439702 ) ) ;
#31520 = CARTESIAN_POINT ( 'NONE',  ( 2.229367062499998831, -11.89583333196774007, -3.861377020970580887 ) ) ;
#31521 = EDGE_CURVE ( 'NONE', #37461, #42937, #12740, .T. ) ;
#31522 = CARTESIAN_POINT ( 'NONE',  ( 2.499999999999998668, -0.3333333333333348136, -4.330127018922193649 ) ) ;
#31523 = CARTESIAN_POINT ( 'NONE',  ( -4.458734125000001214, -159.8750000013655779, 1.846868145590734089 ) ) ;
#31524 = CARTESIAN_POINT ( 'NONE',  ( -1.339745962155610925, -37.79465819873851729, 5.000000000000000000 ) ) ;
#31525 = CARTESIAN_POINT ( 'NONE',  ( -4.458734124999999437, -56.31249999863440081, 0.000000000000000000 ) ) ;
#31526 = CARTESIAN_POINT ( 'NONE',  ( 2.499999999999998668, -92.20833333060214443, -4.330127018922193649 ) ) ;
#31527 = EDGE_CURVE ( 'NONE', #30039, #34132, #52941, .T. ) ;
#31528 = EDGE_CURVE ( 'NONE', #2792, #61933, #11050, .T. ) ;
#31529 =( BOUNDED_CURVE ( )  B_SPLINE_CURVE ( 2, ( #41237, #7802, #60884, #6530, #2349, #35801, #50908, #47036, #56058 ),
 .UNSPECIFIED., .F., .F. ) 
 B_SPLINE_CURVE_WITH_KNOTS ( ( 3, 2, 2, 2, 3 ),
 ( 0.3410714285714285809, 0.3416666666666666741, 0.3428571428571428603, 0.3440476190476190466, 0.3446428571428571397 ),
 .UNSPECIFIED. ) 
 CURVE ( )  GEOMETRIC_REPRESENTATION_ITEM ( )  RATIONAL_B_SPLINE_CURVE ( ( 0.9330127018922194093, 0.9330127018922194093, 1.000000000000000000, 0.8660254037844387076, 1.000000000000000000, 0.8660254037844387076, 1.000000000000000000, 0.9330127018922194093, 0.9330127018922194093 ) ) 
 REPRESENTATION_ITEM ( '' )  );
#31530 = CARTESIAN_POINT ( 'NONE',  ( -4.999999999999998224, -27.91666666666666430, 2.886751345948131764 ) ) ;
#31531 = CARTESIAN_POINT ( 'NONE',  ( -6.972266317189433020E-16, 5.875000002731184168, -5.000000000000000000 ) ) ;
#31532 = CARTESIAN_POINT ( 'NONE',  ( 2.229367062500001939, -33.97916666530107221, 3.861377020970579999 ) ) ;
#31533 = DIRECTION ( 'NONE',  ( -0.000000000000000000, -1.000000000000000000, 0.000000000000000000 ) ) ;
#31534 = CARTESIAN_POINT ( 'NONE',  ( 2.500000000000002220, -50.66666666666666430, 4.330127018922192761 ) ) ;
#31535 = CARTESIAN_POINT ( 'NONE',  ( 7.500000000000006217, -4.330127018922195425, -7.564338275809326717 ) ) ;
#31536 = EDGE_CURVE ( 'NONE', #51626, #14365, #17194, .T. ) ;
#31537 = CARTESIAN_POINT ( 'NONE',  ( 5.000000000000000000, -36.37499999726881583, -6.123233995736766282E-16 ) ) ;
#31538 = ORIENTED_EDGE ( 'NONE', *, *, #22841, .F. ) ;
#31539 = CARTESIAN_POINT ( 'NONE',  ( -3.152548672688508926E-16, -108.5624999986343937, -5.148502694627439702 ) ) ;
#31540 = CARTESIAN_POINT ( 'NONE',  ( 2.229367062500001939, -1.229166665301071548, 3.861377020970579999 ) ) ;
#31541 = AXIS2_PLACEMENT_3D ( 'NONE', #40855, #30568, #11590 ) ;
#31542 = DIRECTION ( 'NONE',  ( 0.000000000000000000, 0.000000000000000000, 1.000000000000000000 ) ) ;
#31543 = EDGE_CURVE ( 'NONE', #60982, #43179, #34770, .T. ) ;
#31544 = CARTESIAN_POINT ( 'NONE',  ( 2.499999999999998668, -8.333333333333332149, -4.330127018922193649 ) ) ;
#31545 = ADVANCED_FACE ( 'NONE', ( #56452 ), #56125, .T. ) ;
#31546 =( GEOMETRIC_REPRESENTATION_CONTEXT ( 3 ) GLOBAL_UNCERTAINTY_ASSIGNED_CONTEXT ( ( #38183 ) ) GLOBAL_UNIT_ASSIGNED_CONTEXT ( ( #22932, #61856, #57027 ) ) REPRESENTATION_CONTEXT ( 'NONE', 'WORKASPACE' ) );
#31547 = CARTESIAN_POINT ( 'NONE',  ( -2.229367062500000163, -74.47916666530106511, -3.861377020970580443 ) ) ;
#31548 = VECTOR ( 'NONE', #4595, 1000.000000000000000 ) ;
#31549 = CARTESIAN_POINT ( 'NONE',  ( -2.500000000000000444, -17.16666666666666430, -4.330127018922193649 ) ) ;
#31550 = CARTESIAN_POINT ( 'NONE',  ( 1.060575238724906964E-15, -7.624999997268813168, 5.773502691896257311 ) ) ;
#31552 = ORIENTED_EDGE ( 'NONE', *, *, #44054, .F. ) ;
#31551 = CARTESIAN_POINT ( 'NONE',  ( 4.458734124999999437, -38.81249999863440081, -5.460374474430324690E-16 ) ) ;
#31553 = CLOSED_SHELL ( 'NONE', ( #35762, #39545, #12175, #17728, #14684, #30011, #47212, #34532, #63119, #42319, #51670, #3665, #36257, #40034, #41635, #37865, #16217, #35465, #43693, #1621, #44523, #48290, #54832, #5607, #59711, #20849, #36707, #47231, #23265, #29197, #61013, #15398, #14516, #40893, #11834, #10526, #41959, #28691, #57764, #34137, #43556, #30263, #45982, #51573, #40818, #19316, #41286, #53516, #24397, #35095, #47634, #53878, #40008, #40588, #53373, #23624, #23205, #27701, #43367, #53541, #43724, #52997, #47479, #47558, #39276, #32693, #42793, #44834, #5981, #9933, #26028, #46787, #3675, #4442, #31350, #28029, #17032, #40180, #59508, #3575, #31077, #43730, #4, #30267, #41760, #33154, #24053, #7102, #12997, #21930, #47057, #40256, #42006, #22084, #17026, #12969, #43560, #47908, #23627, #33505, #7792, #15399, #5531, #63326, #2872, #9012, #47163, #3510, #31373, #6798, #19688, #53163, #59877, #62280, #50401, #29818, #8381, #46121, #31430, #15837, #24030, #44902, #52723, #9019, #36187, #18720, #60685, #5859, #20642, #9279, #45313, #45539, #22473, #55462, #4021, #22555, #57471, #61126, #36088, #38642, #32174, #12221, #9045, #23899, #30552, #35096, #52742, #55231, #43278, #12043, #51588, #53964, #55850, #49973, #39991, #28234, #38554, #14527, #55341, #25576, #14601, #62843, #57104, #61851, #61316, #24333, #17997, #46841, #60581, #62256, #24490, #41241, #34179, #6656, #19766, #2852, #40844, #6796, #7596, #57429, #49619, #20116, #12155, #48701, #30869, #20800, #33134, #23184, #31371, #8, #20588, #549, #5960, #7602, #59032, #29388, #907, #19453, #32234, #45788, #62175, #42779, #52230, #28947, #22908, #42443, #20592, #20511, #25557, #45679, #29846, #52696, #61380, #61680, #23247, #51522, #55126, #1187, #58614, #2067, #2623, #34974, #62627, #7441, #52032, #26836, #17729, #29205, #2773, #39797, #50845, #52380, #38906, #58690, #17670, #22906, #46864, #44268, #45696, #62863, #62190, #58265, #25290, #36107, #46430, #24852, #61711, #60604, #60687, #7067, #45710, #2489, #44864, #39638, #63645, #4290, #20112, #9793, #45882, #35010, #366, #41982, #4781, #5150, #54327, #17002, #10776, #32349, #26019, #8562, #26683, #50442, #62988, #38297, #45158, #44866, #48645, #6783, #27261, #56663, #46068, #32259, #11579, #3586, #474, #57666, #58385, #30232, #55602, #49060, #26772, #14148, #26331, #58445, #11928, #49257, #16637, #28060, #19772, #56957, #36105, #51948, #2083, #37430, #19142, #10561, #41275, #52738, #12640, #30656, #38065, #20501, #25299, #7494 ) ) ;
#31554 = LINE ( 'NONE', #26736, #40500 ) ;
#31555 = B_SPLINE_CURVE_WITH_KNOTS ( 'NONE', 3,
 ( #28175, #24293, #28804, #47482, #13700, #43897 ),
 .UNSPECIFIED., .F., .F.,
 ( 4, 2, 4 ),
 ( -5.145455527293010977E-06, 0.0004153350442917510058, 0.0008358155441107968436 ),
 .UNSPECIFIED. ) ;
#31557 = ORIENTED_EDGE ( 'NONE', *, *, #25652, .T. ) ;
#31556 = CARTESIAN_POINT ( 'NONE',  ( -4.458734124999998549, 13.52083333469892779, 2.574251347313722516 ) ) ;
#31558 = DIRECTION ( 'NONE',  ( 0.000000000000000000, 0.000000000000000000, 1.000000000000000000 ) ) ;
#31559 = CARTESIAN_POINT ( 'NONE',  ( -3.535250795749689387E-16, -54.24999999999999289, -5.773502691896257311 ) ) ;
#31560 = CARTESIAN_POINT ( 'NONE',  ( -4.458734125000001214, -160.1250000013655779, 1.846868145590734089 ) ) ;
#31561 = CARTESIAN_POINT ( 'NONE',  ( -2.229367062500000163, -31.72916666530107577, -3.861377020970580443 ) ) ;
#31562 = CARTESIAN_POINT ( 'NONE',  ( -6.972266317189433020E-16, -106.2500000000000000, -5.000000000000000000 ) ) ;
#31563 = CARTESIAN_POINT ( 'NONE',  ( 4.458734125000001214, -73.89583333196773651, 2.574251347313718519 ) ) ;
#31564 = CARTESIAN_POINT ( 'NONE',  ( -1.846868145590737420, -141.0000000013656063, 4.458734124999999437 ) ) ;
#31565 = CARTESIAN_POINT ( 'NONE',  ( -4.458734124999999437, -85.31249999863439371, 0.000000000000000000 ) ) ;
#31566 = CARTESIAN_POINT ( 'NONE',  ( -52.80376928212989185, -136.1250000013656063, -4.297418129356379346 ) ) ;
#31567 = CARTESIAN_POINT ( 'NONE',  ( 9.457646018065525792E-16, -34.31249999863440792, 5.148502694627439702 ) ) ;
#31568 = CARTESIAN_POINT ( 'NONE',  ( 2.499999999999998668, -83.20833333060214443, -4.330127018922193649 ) ) ;
#31569 = ORIENTED_EDGE ( 'NONE', *, *, #4672, .F. ) ;
#31570 = CARTESIAN_POINT ( 'NONE',  ( 4.458734124999998549, -79.97916666530107932, -2.574251347313721627 ) ) ;
#31571 = CARTESIAN_POINT ( 'NONE',  ( 1.339745962155612702, -84.29465819873850307, -5.000000000000000000 ) ) ;
#31572 = VERTEX_POINT ( 'NONE', #56766 ) ;
#31573 = DIRECTION ( 'NONE',  ( 0.000000000000000000, 0.000000000000000000, 1.000000000000000000 ) ) ;
#31574 = DIRECTION ( 'NONE',  ( -0.000000000000000000, 1.000000000000000000, -0.000000000000000000 ) ) ;
#31575 = CARTESIAN_POINT ( 'NONE',  ( -4.458734124999999437, -62.56249999863440792, 0.000000000000000000 ) ) ;
#31576 = CARTESIAN_POINT ( 'NONE',  ( -4.458734124999998549, -7.479166665301073991, 2.574251347313722516 ) ) ;
#31577 = ORIENTED_EDGE ( 'NONE', *, *, #4033, .T. ) ;
#31578 = CARTESIAN_POINT ( 'NONE',  ( -51.75738570946856498, -149.7500000000000284, 3.805975901505576964 ) ) ;
#31579 = CARTESIAN_POINT ( 'NONE',  ( -5.000000000000000000, 3.041666669397851130, -2.886751345948128211 ) ) ;
#31580 = EDGE_LOOP ( 'NONE', ( #36640, #43905, #50174, #10499 ) ) ;
#31581 = CARTESIAN_POINT ( 'NONE',  ( -2.229367062499996610, -7.395833331967735624, 3.861377020970582219 ) ) ;
#31582 = CARTESIAN_POINT ( 'NONE',  ( 0.000000000000000000, -120.0000000000000000, 0.000000000000000000 ) ) ;
#31583 = CARTESIAN_POINT ( 'NONE',  ( -4.458734124999999437, 9.687500001365593860, 0.000000000000000000 ) ) ;
#31584 = DIRECTION ( 'NONE',  ( -0.000000000000000000, 1.000000000000000000, -0.000000000000000000 ) ) ;
#31585 = CARTESIAN_POINT ( 'NONE',  ( 3.152801135295367541, -158.3125000013656063, -3.152801135295367541 ) ) ;
#31586 =( BOUNDED_CURVE ( )  B_SPLINE_CURVE ( 2, ( #28360, #47364, #52512, #41891, #8132, #7500, #62163, #51561, #13260 ),
 .UNSPECIFIED., .F., .F. ) 
 B_SPLINE_CURVE_WITH_KNOTS ( ( 3, 2, 2, 2, 3 ),
 ( 0.7416666666666664742, 0.7458333333333331261, 0.7499999999999997780, 0.7541666666666664298, 0.7583333333333330817 ),
 .UNSPECIFIED. ) 
 CURVE ( )  GEOMETRIC_REPRESENTATION_ITEM ( )  RATIONAL_B_SPLINE_CURVE ( ( 1.000000000000003997, 0.9238795325112826307, 1.000000000000000000, 0.9238795325112867385, 1.000000000000000000, 0.9238795325112867385, 1.000000000000000000, 0.9238795325112908463, 0.9999999999999958922 ) ) 
 REPRESENTATION_ITEM ( '' )  );
#31587 = VECTOR ( 'NONE', #33554, 1000.000000000000000 ) ;
#31588 = ORIENTED_EDGE ( 'NONE', *, *, #9380, .T. ) ;
#31589 = CARTESIAN_POINT ( 'NONE',  ( 4.458734124999999437, -84.81249999863439371, -5.460374474430324690E-16 ) ) ;
#31590 = FACE_OUTER_BOUND ( 'NONE', #46726, .T. ) ;
#31591 = CARTESIAN_POINT ( 'NONE',  ( -3.152548672688508926E-16, -2.562499998634407028, -5.148502694627439702 ) ) ;
#31592 = AXIS2_PLACEMENT_3D ( 'NONE', #2843, #22463, #62013 ) ;
#31593 = CARTESIAN_POINT ( 'NONE',  ( 2.499999999999998668, -71.20833333060214443, -4.330127018922193649 ) ) ;
#31594 = AXIS2_PLACEMENT_3D ( 'NONE', #757, #23917, #48979 ) ;
#31595 = CARTESIAN_POINT ( 'NONE',  ( -5.000000000000000000, -28.95833333060215153, -2.886751345948128211 ) ) ;
#31596 = CARTESIAN_POINT ( 'NONE',  ( -6.972266317189433020E-16, -73.12499999726878741, -5.000000000000000000 ) ) ;
#31597 = CARTESIAN_POINT ( 'NONE',  ( 2.229367062499998831, 22.35416666803225993, -3.861377020970580887 ) ) ;
#31598 = DIRECTION ( 'NONE',  ( -0.000000000000000000, 1.000000000000000000, -0.000000000000000000 ) ) ;
#31599 = CARTESIAN_POINT ( 'NONE',  ( 9.457646018065525792E-16, 27.93750000136559208, 5.148502694627439702 ) ) ;
#31600 = CARTESIAN_POINT ( 'NONE',  ( 2.229367062499998831, -49.64583333196772941, -3.861377020970580887 ) ) ;
#31601 = CARTESIAN_POINT ( 'NONE',  ( 9.457646018065525792E-16, -39.31249999863439371, 5.148502694627439702 ) ) ;
#31602 = CARTESIAN_POINT ( 'NONE',  ( 4.458734125000000326, -0.1458333319677394824, 2.574251347313718519 ) ) ;
#31603 = CARTESIAN_POINT ( 'NONE',  ( 5.000000000000000000, -0.3749999972688135008, -6.123233995736766282E-16 ) ) ;
#31604 = CARTESIAN_POINT ( 'NONE',  ( 5.000000000000000888, 16.41666666666666785, 2.886751345948126879 ) ) ;
#31605 = CARTESIAN_POINT ( 'NONE',  ( 3.061616997868383141E-16, -145.8750000027312126, -5.000000000000000000 ) ) ;
#31606 = CARTESIAN_POINT ( 'NONE',  ( 1.339745962155612702, -75.16965819600731891, -5.000000000000000000 ) ) ;
#31607 = CARTESIAN_POINT ( 'NONE',  ( -2.229367062499996610, -43.14583333196773651, 3.861377020970582219 ) ) ;
#31608 = CARTESIAN_POINT ( 'NONE',  ( -2.499999999999996447, -79.70833333060213022, 4.330127018922195425 ) ) ;
#31609 = CARTESIAN_POINT ( 'NONE',  ( -56.48576386720575471, -142.0000000013656063, -4.591703134518078322 ) ) ;
#31610 = DIRECTION ( 'NONE',  ( -0.000000000000000000, 1.000000000000000000, -0.000000000000000000 ) ) ;
#31611 = CARTESIAN_POINT ( 'NONE',  ( 1.339745962155612702, -36.29465819873852439, -5.000000000000000000 ) ) ;
#31612 = CARTESIAN_POINT ( 'NONE',  ( -3.152548672688508926E-16, -87.81249999863437949, -5.148502694627439702 ) ) ;
#31613 = CARTESIAN_POINT ( 'NONE',  ( 4.458734124999999437, -162.6875000013655779, 0.000000000000000000 ) ) ;
#31614 = CARTESIAN_POINT ( 'NONE',  ( 1.975475456537005874E-15, 13.37500000273118417, 5.000000000000000000 ) ) ;
#31615 = CARTESIAN_POINT ( 'NONE',  ( 2.500000000000002220, -31.66666666666666075, 4.330127018922192761 ) ) ;
#31616 = CARTESIAN_POINT ( 'NONE',  ( -4.999999999999998224, -90.79166666393547303, 2.886751345948131764 ) ) ;
#31617 = ORIENTED_EDGE ( 'NONE', *, *, #13286, .F. ) ;
#31618 = ADVANCED_FACE ( 'NONE', ( #46154 ), #31672, .T. ) ;
#31619 = CARTESIAN_POINT ( 'NONE',  ( 2.229367062500001939, 21.77083333469892779, 3.861377020970579999 ) ) ;
#31620 = ORIENTED_EDGE ( 'NONE', *, *, #26473, .T. ) ;
#31621 = CARTESIAN_POINT ( 'NONE',  ( -4.458734124999999437, -89.39583333196773651, -2.574251347313719407 ) ) ;
#31622 = CARTESIAN_POINT ( 'NONE',  ( -2.229367062499996610, 11.60416666803225993, 3.861377020970582219 ) ) ;
#31623 = CARTESIAN_POINT ( 'NONE',  ( 5.000000000000000888, 18.54166666939785202, 2.886751345948126879 ) ) ;
#31624 = DIRECTION ( 'NONE',  ( 0.000000000000000000, 1.000000000000000000, 0.000000000000000000 ) ) ;
#31625 = CARTESIAN_POINT ( 'NONE',  ( 2.499999999999998668, 7.666666666666665186, -4.330127018922193649 ) ) ;
#31626 = CARTESIAN_POINT ( 'NONE',  ( 4.458734124999999437, -58.81249999863440081, -5.460374474430324690E-16 ) ) ;
#31627 = FACE_OUTER_BOUND ( 'NONE', #58438, .T. ) ;
#31628 = EDGE_CURVE ( 'NONE', #51345, #52848, #28327, .T. ) ;
#31629 = CARTESIAN_POINT ( 'NONE',  ( -54.64476657466781973, -135.0625000013656063, -4.444560631937228834 ) ) ;
#31630 = DIRECTION ( 'NONE',  ( 0.000000000000000000, 0.000000000000000000, 1.000000000000000000 ) ) ;
#31631 = CARTESIAN_POINT ( 'NONE',  ( 1.339745962155612702, -33.16965819600733312, -5.000000000000000000 ) ) ;
#31632 = CARTESIAN_POINT ( 'NONE',  ( -5.000000000000000000, 18.12500000273118417, 0.000000000000000000 ) ) ;
#31633 = CARTESIAN_POINT ( 'NONE',  ( -2.499999999999996447, -37.83333333333332860, 4.330127018922195425 ) ) ;
#31635 = CARTESIAN_POINT ( 'NONE',  ( -4.458734124999998549, -15.47916666530107399, 2.574251347313722516 ) ) ;
#31634 = CARTESIAN_POINT ( 'NONE',  ( -2.499999999999996447, -44.83333333333333570, 4.330127018922195425 ) ) ;
#31636 = VECTOR ( 'NONE', #59988, 1000.000000000000000 ) ;
#31637 = CARTESIAN_POINT ( 'NONE',  ( 0.000000000000000000, -170.0000000000000000, 5.000000000000000000 ) ) ;
#31638 = CARTESIAN_POINT ( 'NONE',  ( 2.229367062499998831, -58.64583333196773651, -3.861377020970580887 ) ) ;
#31639 =( BOUNDED_CURVE ( )  B_SPLINE_CURVE ( 2, ( #58872, #9662, #35, #19634, #39245, #14802, #34415, #1005, #40526 ),
 .UNSPECIFIED., .F., .F. ) 
 B_SPLINE_CURVE_WITH_KNOTS ( ( 3, 2, 2, 2, 3 ),
 ( 0.002083333333333333738, 0.002777777777777777884, 0.004166666666666666609, 0.005555555555555555768, 0.006250000000000000347 ),
 .UNSPECIFIED. ) 
 CURVE ( )  GEOMETRIC_REPRESENTATION_ITEM ( )  RATIONAL_B_SPLINE_CURVE ( ( 0.9330127018922194093, 0.9330127018922194093, 1.000000000000000000, 0.8660254037844387076, 1.000000000000000000, 0.8660254037844387076, 1.000000000000000000, 0.9330127018922192983, 0.9330127018922194093 ) ) 
 REPRESENTATION_ITEM ( '' )  );
#31640 = CARTESIAN_POINT ( 'NONE',  ( -3.152801135295367096, -153.3125000013656063, -3.152801135295367541 ) ) ;
#31641 = CARTESIAN_POINT ( 'NONE',  ( -4.458734124999999437, -70.39583333196773651, -2.574251347313719407 ) ) ;
#31642 = AXIS2_PLACEMENT_3D ( 'NONE', #48917, #39900, #30576 ) ;
#31643 = CARTESIAN_POINT ( 'NONE',  ( -50.55543936806279248, -148.3125000013656063, 0.3552334253322060320 ) ) ;
#31644 = CARTESIAN_POINT ( 'NONE',  ( 2.229367062500001939, -19.22916666530106866, 3.861377020970579999 ) ) ;
#31645 = CARTESIAN_POINT ( 'NONE',  ( 5.000000000000000888, -63.45833333060215153, 2.886751345948126879 ) ) ;
#31646 = ORIENTED_EDGE ( 'NONE', *, *, #8635, .F. ) ;
#31647 = CARTESIAN_POINT ( 'NONE',  ( 1.975475456537005874E-15, -68.74999999999998579, 5.000000000000000000 ) ) ;
#31648 = EDGE_LOOP ( 'NONE', ( #14066, #49111, #51716, #49551 ) ) ;
#31649 = CARTESIAN_POINT ( 'NONE',  ( -4.458734124999999437, -61.56249999863440081, 0.000000000000000000 ) ) ;
#31651 = CARTESIAN_POINT ( 'NONE',  ( 5.000000000000000000, -8.500000000000000000, -6.123233995736766282E-16 ) ) ;
#31650 = DIRECTION ( 'NONE',  ( 0.000000000000000000, 0.000000000000000000, 1.000000000000000000 ) ) ;
#31652 = CARTESIAN_POINT ( 'NONE',  ( 3.152801135295366208, -151.5625000013655779, 3.152801135295367985 ) ) ;
#31653 = EDGE_LOOP ( 'NONE', ( #39351, #47150, #4790, #6945 ) ) ;
#31654 = CARTESIAN_POINT ( 'NONE',  ( 1.975475456537005874E-15, -9.750000000000000000, 5.000000000000000000 ) ) ;
#31655 = CARTESIAN_POINT ( 'NONE',  ( 5.274401269815139237, 6.074457022762083547, -7.633824513837111247 ) ) ;
#31656 = CARTESIAN_POINT ( 'NONE',  ( -2.229367062499996610, -49.39583333196772941, 3.861377020970582219 ) ) ;
#31657 = ORIENTED_EDGE ( 'NONE', *, *, #11751, .F. ) ;
#31658 = CARTESIAN_POINT ( 'NONE',  ( 2.499999999999998668, 10.79166666939785202, -4.330127018922193649 ) ) ;
#31659 = CARTESIAN_POINT ( 'NONE',  ( -4.458734124999999437, 7.604166668032259935, -2.574251347313719407 ) ) ;
#31660 = CARTESIAN_POINT ( 'NONE',  ( 9.457646018065525792E-16, 23.93750000136559564, 5.148502694627439702 ) ) ;
#31661 = CARTESIAN_POINT ( 'NONE',  ( -50.55543936806279248, -150.0625000013656063, 0.3552334253322060320 ) ) ;
#31662 = CARTESIAN_POINT ( 'NONE',  ( -6.972266317189433020E-16, -24.12499999726881228, -5.000000000000000000 ) ) ;
#31663 = CARTESIAN_POINT ( 'NONE',  ( 1.846868145590736310, -168.6250000013656063, 4.458734124999997661 ) ) ;
#31664 = VERTEX_POINT ( 'NONE', #119 ) ;
#31665 = CARTESIAN_POINT ( 'NONE',  ( -2.229367062500000163, -68.47916666530107932, -3.861377020970580443 ) ) ;
#31666 = CARTESIAN_POINT ( 'NONE',  ( 1.013163106016871096, 8.075304045852551127, -7.231838333420561149 ) ) ;
#31667 = CARTESIAN_POINT ( 'NONE',  ( 9.457646018065525792E-16, 11.93750000136559386, 5.148502694627439702 ) ) ;
#31668 = CARTESIAN_POINT ( 'NONE',  ( 0.000000000000000000, -120.0000000000000000, 0.000000000000000000 ) ) ;
#31669 = CARTESIAN_POINT ( 'NONE',  ( 2.071067811865348940, -156.9375000027312410, -5.000000000000127898 ) ) ;
#31670 = CARTESIAN_POINT ( 'NONE',  ( -2.229367062499996610, -53.39583333196773651, 3.861377020970582219 ) ) ;
#31671 = CARTESIAN_POINT ( 'NONE',  ( -3.535250795749689387E-16, -15.12499999726881406, -5.773502691896257311 ) ) ;
#31672 = CYLINDRICAL_SURFACE ( 'NONE', #23486, 5.000000000000000000 ) ;
#31673 = LINE ( 'NONE', #27169, #29540 ) ;
#31674 = CARTESIAN_POINT ( 'NONE',  ( -2.499999999999996447, 19.16666666666666430, 4.330127018922195425 ) ) ;
#31675 = CARTESIAN_POINT ( 'NONE',  ( -4.458734124999997661, -23.47916666530107221, 2.574251347313722516 ) ) ;
#31676 = ORIENTED_EDGE ( 'NONE', *, *, #47226, .F. ) ;
#31677 = VECTOR ( 'NONE', #30172, 1000.000000000000000 ) ;
#31678 = CARTESIAN_POINT ( 'NONE',  ( -3.152548672688508926E-16, -107.5624999986343795, -5.148502694627439702 ) ) ;
#31679 = CARTESIAN_POINT ( 'NONE',  ( 3.535533905932738197, -159.0000000027312126, -3.535533905932738197 ) ) ;
#31680 = VERTEX_POINT ( 'NONE', #8806 ) ;
#31681 = CARTESIAN_POINT ( 'NONE',  ( 2.229367062500001939, -105.2291666653010651, 3.861377020970579999 ) ) ;
#31682 = VECTOR ( 'NONE', #8226, 1000.000000000000000 ) ;
#31683 = CARTESIAN_POINT ( 'NONE',  ( -4.458734124999999437, -27.39583333196773651, -2.574251347313719407 ) ) ;
#31684 = CARTESIAN_POINT ( 'NONE',  ( -2.500000000000000444, -65.04166666393547303, -4.330127018922193649 ) ) ;
#31685 = CARTESIAN_POINT ( 'NONE',  ( -50.70258187064364108, -152.3750000013656063, 2.196230717870141014 ) ) ;
#31686 = CARTESIAN_POINT ( 'NONE',  ( 5.000000000000000000, -149.0000000000000284, 0.000000000000000000 ) ) ;
#31687 = CARTESIAN_POINT ( 'NONE',  ( -2.229367062500000163, -21.47916666530107221, -3.861377020970580443 ) ) ;
#31688 = CARTESIAN_POINT ( 'NONE',  ( 4.458734124999999437, -71.06249999863439371, -5.460374474430324690E-16 ) ) ;
#31689 = CARTESIAN_POINT ( 'NONE',  ( -51.19402409849444524, -153.6250000027312126, -3.242614290531456334 ) ) ;
#31690 = CARTESIAN_POINT ( 'NONE',  ( 2.229367062499998831, -27.64583333196774007, -3.861377020970580887 ) ) ;
#31691 = CARTESIAN_POINT ( 'NONE',  ( 5.000000000000000888, 14.41666666666666430, 2.886751345948126879 ) ) ;
#31692 = CARTESIAN_POINT ( 'NONE',  ( 3.061616997868383141E-16, -152.7500000000000000, -5.000000000000000000 ) ) ;
#31693 = CARTESIAN_POINT ( 'NONE',  ( 2.500000000000002220, -17.66666666666666430, 4.330127018922192761 ) ) ;
#31694 = CARTESIAN_POINT ( 'NONE',  ( 3.152801135295366208, -150.5625000013655779, 3.152801135295367985 ) ) ;
#31695 = VERTEX_POINT ( 'NONE', #43514 ) ;
#31696 = DIRECTION ( 'NONE',  ( -0.000000000000000000, 1.000000000000000000, -0.000000000000000000 ) ) ;
#31697 = CARTESIAN_POINT ( 'NONE',  ( 9.457646018065525792E-16, -50.31249999863440792, 5.148502694627439702 ) ) ;
#31698 = CARTESIAN_POINT ( 'NONE',  ( 5.000000000000000000, -84.37499999726880162, -6.123233995736766282E-16 ) ) ;
#31699 = CARTESIAN_POINT ( 'NONE',  ( -6.972266317189433020E-16, -14.24999999999999822, -5.000000000000000000 ) ) ;
#31700 = CARTESIAN_POINT ( 'NONE',  ( -3.535250795749689387E-16, 26.75000000000000000, -5.773502691896257311 ) ) ;
#31701 = AXIS2_PLACEMENT_3D ( 'NONE', #5640, #59679, #25253 ) ;
#31702 = FACE_OUTER_BOUND ( 'NONE', #33163, .T. ) ;
#31703 = CARTESIAN_POINT ( 'NONE',  ( 9.457646018065525792E-16, 5.937500001365592972, 5.148502694627439702 ) ) ;
#31704 = CARTESIAN_POINT ( 'NONE',  ( 2.499999999999998668, 19.66666666666666430, -4.330127018922193649 ) ) ;
#31705 = CARTESIAN_POINT ( 'NONE',  ( 2.499999999999998668, -95.20833333060213022, -4.330127018922193649 ) ) ;
#31706 = DIRECTION ( 'NONE',  ( 0.000000000000000000, 0.000000000000000000, 1.000000000000000000 ) ) ;
#31707 = CARTESIAN_POINT ( 'NONE',  ( -3.152548672688508926E-16, 16.18750000136559564, -5.148502694627439702 ) ) ;
#31708 = CARTESIAN_POINT ( 'NONE',  ( 1.060575238724906964E-15, 3.375000002731186388, 5.773502691896257311 ) ) ;
#31709 = EDGE_LOOP ( 'NONE', ( #37661, #16860, #48194, #44399 ) ) ;
#31710 = CARTESIAN_POINT ( 'NONE',  ( -7.499999999999999112, -2.930060224340425901, -0.4701183149080249146 ) ) ;
#31711 = ORIENTED_EDGE ( 'NONE', *, *, #35445, .F. ) ;
#31712 = FACE_OUTER_BOUND ( 'NONE', #1524, .T. ) ;
#31713 = CARTESIAN_POINT ( 'NONE',  ( -4.458734124999999437, -43.39583333196774362, -2.574251347313719407 ) ) ;
#31714 = CARTESIAN_POINT ( 'NONE',  ( 1.846868145590736310, -163.8750000013655779, 4.458734124999999437 ) ) ;
#31715 =( BOUNDED_CURVE ( )  B_SPLINE_CURVE ( 2, ( #48953, #34812, #44450, #19694, #38671, #4903, #59257, #38988, #15519 ),
 .UNSPECIFIED., .F., .F. ) 
 B_SPLINE_CURVE_WITH_KNOTS ( ( 3, 2, 2, 2, 3 ),
 ( 0.1232142857142857206, 0.1238095238095238138, 0.1250000000000000000, 0.1261904761904761862, 0.1267857142857142794 ),
 .UNSPECIFIED. ) 
 CURVE ( )  GEOMETRIC_REPRESENTATION_ITEM ( )  RATIONAL_B_SPLINE_CURVE ( ( 0.9330127018922192983, 0.9330127018922200755, 1.000000000000000000, 0.8660254037844387076, 1.000000000000000000, 0.8660254037844387076, 1.000000000000000000, 0.9330127018922194093, 0.9330127018922194093 ) ) 
 REPRESENTATION_ITEM ( '' )  );
#31716 = CARTESIAN_POINT ( 'NONE',  ( 2.499999999999998668, -47.20833333060214443, -4.330127018922193649 ) ) ;
#31717 = ORIENTED_EDGE ( 'NONE', *, *, #27621, .T. ) ;
#31718 = CARTESIAN_POINT ( 'NONE',  ( -3.152548672688508926E-16, -16.56249999863440792, -5.148502694627439702 ) ) ;
#31719 = VERTEX_POINT ( 'NONE', #14562 ) ;
#31720 = CARTESIAN_POINT ( 'NONE',  ( 1.060575238724906964E-15, -86.75000000000000000, 5.773502691896257311 ) ) ;
#31721 = CARTESIAN_POINT ( 'NONE',  ( -3.152801135295367096, -166.0625000013656063, -3.152801135295367541 ) ) ;
#31722 = AXIS2_PLACEMENT_3D ( 'NONE', #46506, #50049, #40708 ) ;
#31724 = ORIENTED_EDGE ( 'NONE', *, *, #23697, .T. ) ;
#31723 = CARTESIAN_POINT ( 'NONE',  ( 2.499999999999998668, -20.20833333060214798, -4.330127018922193649 ) ) ;
#31725 = CARTESIAN_POINT ( 'NONE',  ( -49.85088928181150436, -137.5625000000000284, -1.666127454062680702 ) ) ;
#31726 = EDGE_CURVE ( 'NONE', #16689, #23906, #58643, .T. ) ;
#31727 = VECTOR ( 'NONE', #1613, 1000.000000000000000 ) ;
#31728 = CARTESIAN_POINT ( 'NONE',  ( -4.458734124999998549, -33.47916666530107221, 2.574251347313722516 ) ) ;
#31729 = LINE ( 'NONE', #57140, #5284 ) ;
#31730 = ORIENTED_EDGE ( 'NONE', *, *, #62817, .F. ) ;
#31731 = CARTESIAN_POINT ( 'NONE',  ( 4.458734125000001214, -76.89583333196775072, 2.574251347313718519 ) ) ;
#31732 = CARTESIAN_POINT ( 'NONE',  ( 4.458734125000001214, 27.10416666803225993, 2.574251347313718519 ) ) ;
#31733 = CARTESIAN_POINT ( 'NONE',  ( -5.000000000000000000, -28.87499999726881228, 0.000000000000000000 ) ) ;
#31734 = ORIENTED_EDGE ( 'NONE', *, *, #48070, .T. ) ;
#31735 = CYLINDRICAL_SURFACE ( 'NONE', #6899, 5.000000000000000000 ) ;
#31736 = CARTESIAN_POINT ( 'NONE',  ( -55.35523342533222291, -143.5625000013656063, 4.444560631937231499 ) ) ;
#31737 = CARTESIAN_POINT ( 'NONE',  ( -2.229367062499996610, -80.39583333196773651, 3.861377020970582219 ) ) ;
#31738 = CARTESIAN_POINT ( 'NONE',  ( -54.60164318462004474, -132.5000000027312126, -4.984105922594373794 ) ) ;
#31739 = CARTESIAN_POINT ( 'NONE',  ( 3.152801135295367541, -143.5625000013655779, -3.152801135295367541 ) ) ;
#31740 = CARTESIAN_POINT ( 'NONE',  ( 1.339745962155615144, -84.58034179853028434, 4.999999999999999112 ) ) ;
#31741 = CARTESIAN_POINT ( 'NONE',  ( -3.152548672688508926E-16, -56.56249999863439371, -5.148502694627439702 ) ) ;
#31742 = CARTESIAN_POINT ( 'NONE',  ( -4.458734124999999437, -44.39583333196774362, -2.574251347313719407 ) ) ;
#31743 = CARTESIAN_POINT ( 'NONE',  ( 2.229367062499998831, 29.35416666803225993, -3.861377020970580887 ) ) ;
#31744 = VECTOR ( 'NONE', #22047, 1000.000000000000000 ) ;
#31745 = CARTESIAN_POINT ( 'NONE',  ( 2.500000000000002220, -104.6666666666666572, 4.330127018922192761 ) ) ;
#31746 = CARTESIAN_POINT ( 'NONE',  ( 3.535533905932736864, -154.2500000027312126, 3.535533905932738641 ) ) ;
#31747 = CARTESIAN_POINT ( 'NONE',  ( 4.458734125000001214, -39.14583333196773651, 2.574251347313718519 ) ) ;
#31748 = CARTESIAN_POINT ( 'NONE',  ( 2.500000000000002220, 1.458333336064519203, 4.330127018922192761 ) ) ;
#31749 = CARTESIAN_POINT ( 'NONE',  ( -58.39396692619412477, -126.4375000013656063, 2.891590998281057701 ) ) ;
#31750 = CARTESIAN_POINT ( 'NONE',  ( 4.458734124999999437, -79.06249999863440792, -5.460374474430324690E-16 ) ) ;
#31751 = CARTESIAN_POINT ( 'NONE',  ( -2.229367062499996610, -102.1458333319677365, 3.861377020970582219 ) ) ;
#31752 = CARTESIAN_POINT ( 'NONE',  ( 2.229367062499998831, -4.895833331967740065, -3.861377020970580887 ) ) ;
#31753 = ORIENTED_EDGE ( 'NONE', *, *, #49918, .T. ) ;
#31754 = CYLINDRICAL_SURFACE ( 'NONE', #51120, 5.000000000000000000 ) ;
#31755 = CARTESIAN_POINT ( 'NONE',  ( -5.000000000000000000, -14.95833333060214621, -2.886751345948128211 ) ) ;
#31756 = CARTESIAN_POINT ( 'NONE',  ( 4.458734124999999437, -91.81249999863440792, -5.460374474430324690E-16 ) ) ;
#31757 = CARTESIAN_POINT ( 'NONE',  ( 3.535533905932736864, -168.2500000027312126, 3.535533905932738641 ) ) ;
#31758 = CARTESIAN_POINT ( 'NONE',  ( -2.229367062500000163, -88.72916666530106511, -3.861377020970580443 ) ) ;
#31759 = CARTESIAN_POINT ( 'NONE',  ( -2.229367062499996610, 13.60416666803226171, 3.861377020970582219 ) ) ;
#31760 = CARTESIAN_POINT ( 'NONE',  ( 5.000000000000000000, -2.291666663935477466, -2.886751345948130876 ) ) ;
#31761 = CARTESIAN_POINT ( 'NONE',  ( -55.35523342533222291, -133.3125000013656063, 4.444560631937231499 ) ) ;
#31762 = CARTESIAN_POINT ( 'NONE',  ( -4.458734124999999437, -8.395833331967736513, -2.574251347313719407 ) ) ;
#31763 = CARTESIAN_POINT ( 'NONE',  ( 2.229367062500001939, 16.77083333469892779, 3.861377020970579999 ) ) ;
#31764 = CARTESIAN_POINT ( 'NONE',  ( 4.458734124999998549, -53.97916666530107221, -2.574251347313721627 ) ) ;
#31765 =( BOUNDED_CURVE ( )  B_SPLINE_CURVE ( 2, ( #2522, #55916, #11830, #31449, #7028, #26961, #46258, #61068, #16989 ),
 .UNSPECIFIED., .F., .F. ) 
 B_SPLINE_CURVE_WITH_KNOTS ( ( 3, 2, 2, 2, 3 ),
 ( 0.8839285714285713969, 0.8845238095238094900, 0.8857142857142856762, 0.8869047619047618625, 0.8874999999999999556 ),
 .UNSPECIFIED. ) 
 CURVE ( )  GEOMETRIC_REPRESENTATION_ITEM ( )  RATIONAL_B_SPLINE_CURVE ( ( 0.9330127018922194093, 0.9330127018922194093, 1.000000000000000000, 0.8660254037844387076, 1.000000000000000000, 0.8660254037844387076, 1.000000000000000000, 0.9330127018922194093, 0.9330127018922194093 ) ) 
 REPRESENTATION_ITEM ( '' )  );
#31766 = CARTESIAN_POINT ( 'NONE',  ( 2.500000000000002220, -11.66666666666666607, 4.330127018922192761 ) ) ;
#31767 = CARTESIAN_POINT ( 'NONE',  ( -4.458734124999998549, -83.22916666530106511, 2.574251347313722516 ) ) ;
#31768 = CARTESIAN_POINT ( 'NONE',  ( 9.457646018065525792E-16, -9.062499998634407916, 5.148502694627439702 ) ) ;
#31769 = ORIENTED_EDGE ( 'NONE', *, *, #34251, .T. ) ;
#31770 = CARTESIAN_POINT ( 'NONE',  ( 2.229367062500001939, -36.22916666530107221, 3.861377020970579999 ) ) ;
#31771 = CARTESIAN_POINT ( 'NONE',  ( -57.19623071787017210, -126.6250000013656489, 4.297418129356382899 ) ) ;
#31772 = CARTESIAN_POINT ( 'NONE',  ( 9.457646018065525792E-16, -82.06249999863442213, 5.148502694627439702 ) ) ;
#31773 = CARTESIAN_POINT ( 'NONE',  ( -5.000000000000000000, -109.9583333306021444, -2.886751345948128211 ) ) ;
#31774 = AXIS2_PLACEMENT_3D ( 'NONE', #35334, #6079, #9919 ) ;
#31775 = CARTESIAN_POINT ( 'NONE',  ( 1.846868145590735200, -149.5000000013656063, -4.458734124999999437 ) ) ;
#31776 = CARTESIAN_POINT ( 'NONE',  ( -4.458734124999999437, 19.68750000136559208, 0.000000000000000000 ) ) ;
#31777 = DIRECTION ( 'NONE',  ( -0.000000000000000000, 1.000000000000000000, -0.000000000000000000 ) ) ;
#31778 = CYLINDRICAL_SURFACE ( 'NONE', #48104, 5.000000000000000000 ) ;
#31779 = CARTESIAN_POINT ( 'NONE',  ( -2.229367062499996610, -81.39583333196773651, 3.861377020970582219 ) ) ;
#31780 = CARTESIAN_POINT ( 'NONE',  ( 2.499999999999998668, -67.33333333333332860, -4.330127018922193649 ) ) ;
#31781 = CARTESIAN_POINT ( 'NONE',  ( -6.972266317189433020E-16, -72.12499999726878741, -5.000000000000000000 ) ) ;
#31782 = CARTESIAN_POINT ( 'NONE',  ( 1.060575238724906964E-15, 19.37500000273118772, 5.773502691896257311 ) ) ;
#31783 = VERTEX_POINT ( 'NONE', #19713 ) ;
#31784 = CARTESIAN_POINT ( 'NONE',  ( -2.500000000000000444, -62.04166666393547303, -4.330127018922193649 ) ) ;
#31785 = DIRECTION ( 'NONE',  ( 0.000000000000000000, 0.000000000000000000, 1.000000000000000000 ) ) ;
#31787 = CARTESIAN_POINT ( 'NONE',  ( -4.999999999999999112, -21.91666666666666785, 2.886751345948131764 ) ) ;
#31786 = DIRECTION ( 'NONE',  ( -0.000000000000000000, -1.000000000000000000, -0.000000000000000000 ) ) ;
#31788 = CARTESIAN_POINT ( 'NONE',  ( 2.229367062500001939, -25.97916666530106866, 3.861377020970579999 ) ) ;
#31789 = CARTESIAN_POINT ( 'NONE',  ( 2.229367062499998831, -89.64583333196773651, -3.861377020970580887 ) ) ;
#31790 = CARTESIAN_POINT ( 'NONE',  ( -3.535250795749689387E-16, -28.12499999726880873, -5.773502691896257311 ) ) ;
#31792 = ORIENTED_EDGE ( 'NONE', *, *, #45714, .F. ) ;
#31791 = CARTESIAN_POINT ( 'NONE',  ( -3.152548672688508926E-16, -55.56249999863440081, -5.148502694627439702 ) ) ;
#31793 = CARTESIAN_POINT ( 'NONE',  ( -52.10840900171896806, -153.4375000013656063, 3.393966926194110556 ) ) ;
#31795 = ORIENTED_EDGE ( 'NONE', *, *, #37856, .T. ) ;
#31794 = CARTESIAN_POINT ( 'NONE',  ( 4.458734125000001214, -1.145833331967740509, 2.574251347313718519 ) ) ;
#31796 = CARTESIAN_POINT ( 'NONE',  ( -3.535250795749689387E-16, -70.25000000000000000, -5.773502691896257311 ) ) ;
#31797 = CARTESIAN_POINT ( 'NONE',  ( -59.29741812935640155, -138.6250000013656063, -2.196230717870135685 ) ) ;
#31798 = CARTESIAN_POINT ( 'NONE',  ( -4.458734124999999437, -52.56249999863440792, 0.000000000000000000 ) ) ;
#31799 = CARTESIAN_POINT ( 'NONE',  ( -4.999999999999998224, 0.2083333360645180099, 2.886751345948131764 ) ) ;
#31800 = CARTESIAN_POINT ( 'NONE',  ( -4.999999999999999112, -74.79166666393547303, 2.886751345948131764 ) ) ;
#31801 = CARTESIAN_POINT ( 'NONE',  ( -2.500000000000000444, -54.04166666393548013, -4.330127018922193649 ) ) ;
#31802 = CARTESIAN_POINT ( 'NONE',  ( -58.80597590150559739, -149.0000000000000284, 3.242614290531460330 ) ) ;
#31803 = EDGE_CURVE ( 'NONE', #25841, #1596, #52563, .T. ) ;
#31804 = CARTESIAN_POINT ( 'NONE',  ( -4.458734124999999437, -18.56249999863440792, 0.000000000000000000 ) ) ;
#31805 = CARTESIAN_POINT ( 'NONE',  ( 2.229367062499998831, -49.89583333196772941, -3.861377020970580887 ) ) ;
#31806 = CARTESIAN_POINT ( 'NONE',  ( 2.499999999999998668, 10.66666666666666430, -4.330127018922193649 ) ) ;
#31807 = SURFACE_STYLE_USAGE ( .BOTH. , #47244 ) ;
#31808 = CARTESIAN_POINT ( 'NONE',  ( -3.152801135295367096, -141.0625000013655779, -3.152801135295367541 ) ) ;
#31809 = CARTESIAN_POINT ( 'NONE',  ( -4.458734124999999437, -101.5624999986344079, 0.000000000000000000 ) ) ;
#31810 = CARTESIAN_POINT ( 'NONE',  ( 2.071067811865644703, -147.9375000027312126, -4.999999999999831246 ) ) ;
#31811 = ORIENTED_EDGE ( 'NONE', *, *, #18079, .F. ) ;
#31812 = CARTESIAN_POINT ( 'NONE',  ( -51.60603307380591787, -154.1875000013656063, -2.891590998281053704 ) ) ;
#31813 = CARTESIAN_POINT ( 'NONE',  ( -51.19402409849444524, -143.6250000027312126, -3.242614290531456334 ) ) ;
#31814 = STYLED_ITEM ( 'NONE', ( #13763 ), #57040 ) ;
#31815 =( BOUNDED_CURVE ( )  B_SPLINE_CURVE ( 2, ( #40909, #46385, #2642, #37054, #32211, #6834, #51840, #60554, #36096 ),
 .UNSPECIFIED., .F., .F. ) 
 B_SPLINE_CURVE_WITH_KNOTS ( ( 3, 2, 2, 2, 3 ),
 ( 0.5145833333333332815, 0.5152777777777777235, 0.5166666666666667185, 0.5180555555555556024, 0.5187500000000000444 ),
 .UNSPECIFIED. ) 
 CURVE ( )  GEOMETRIC_REPRESENTATION_ITEM ( )  RATIONAL_B_SPLINE_CURVE ( ( 0.9330127018922194093, 0.9330127018922194093, 1.000000000000000000, 0.8660254037844387076, 1.000000000000000000, 0.8660254037844387076, 1.000000000000000000, 0.9330127018922194093, 0.9330127018922194093 ) ) 
 REPRESENTATION_ITEM ( '' )  );
#31816 = EDGE_CURVE ( 'NONE', #44367, #31572, #37358, .T. ) ;
#31817 = CARTESIAN_POINT ( 'NONE',  ( 2.499999999999998668, -50.33333333333332860, -4.330127018922193649 ) ) ;
#31818 = VECTOR ( 'NONE', #4397, 1000.000000000000000 ) ;
#31819 = CARTESIAN_POINT ( 'NONE',  ( 2.229367062500001939, -0.9791666653010712151, 3.861377020970579999 ) ) ;
#31820 = CARTESIAN_POINT ( 'NONE',  ( -2.229367062500000163, -97.72916666530105090, -3.861377020970580443 ) ) ;
#31821 = CARTESIAN_POINT ( 'NONE',  ( -1.846868145590737420, -147.0000000013655779, 4.458734124999999437 ) ) ;
#31822 = CARTESIAN_POINT ( 'NONE',  ( 9.457646018065525792E-16, -25.31249999863440792, 5.148502694627439702 ) ) ;
#31823 = ADVANCED_FACE ( 'NONE', ( #8496 ), #3988, .T. ) ;
#31824 = CARTESIAN_POINT ( 'NONE',  ( -7.500000000000001776, 0.000000000000000000, 0.000000000000000000 ) ) ;
#31825 = CARTESIAN_POINT ( 'NONE',  ( -54.64476657466781973, -139.8125000013656063, -4.444560631937228834 ) ) ;
#31826 = CARTESIAN_POINT ( 'NONE',  ( -4.458734124999998549, -62.47916666530106511, 2.574251347313722516 ) ) ;
#31827 = CARTESIAN_POINT ( 'NONE',  ( 5.000000000000000000, -70.41666666666667140, -2.886751345948130876 ) ) ;
#31828 = CARTESIAN_POINT ( 'NONE',  ( -0.3470952277635217520, -8.860649561028104415, -7.493596212620245112 ) ) ;
#31829 = CARTESIAN_POINT ( 'NONE',  ( 1.846868145590735200, -146.2500000013656347, -4.458734124999999437 ) ) ;
#31830 = CARTESIAN_POINT ( 'NONE',  ( 2.229367062500001939, 8.770833334698927786, 3.861377020970579999 ) ) ;
#31831 = ORIENTED_EDGE ( 'NONE', *, *, #38230, .F. ) ;
#31832 = CARTESIAN_POINT ( 'NONE',  ( -1.339745962155610925, -80.79465819873850307, 5.000000000000000000 ) ) ;
#31833 = PLANE ( 'NONE',  #11321 ) ;
#31835 = CARTESIAN_POINT ( 'NONE',  ( 9.457646018065525792E-16, -24.06249999863440436, 5.148502694627439702 ) ) ;
#31834 = CARTESIAN_POINT ( 'NONE',  ( -3.535250795749689387E-16, -87.24999999999998579, -5.773502691896257311 ) ) ;
#31836 = DIRECTION ( 'NONE',  ( -0.000000000000000000, 1.000000000000000000, -0.000000000000000000 ) ) ;
#31837 = DIRECTION ( 'NONE',  ( 0.000000000000000000, -1.000000000000000000, 0.000000000000000000 ) ) ;
#31838 = CARTESIAN_POINT ( 'NONE',  ( -57.19623071787017210, -147.3750000013656063, 4.297418129356382899 ) ) ;
#31839 = CARTESIAN_POINT ( 'NONE',  ( 5.000000000000000888, -50.45833333060213732, 2.886751345948126879 ) ) ;
#31840 = CARTESIAN_POINT ( 'NONE',  ( 1.339745962155612702, -24.29465819873852084, -5.000000000000000000 ) ) ;
#31841 = CARTESIAN_POINT ( 'NONE',  ( 4.458734124999999437, 10.18750000136559386, -5.460374474430324690E-16 ) ) ;
#31842 = DIRECTION ( 'NONE',  ( -0.000000000000000000, 1.000000000000000000, -0.000000000000000000 ) ) ;
#31843 = CARTESIAN_POINT ( 'NONE',  ( -54.60164318462004474, -141.5000000027312126, -4.984105922594373794 ) ) ;
#31844 = CARTESIAN_POINT ( 'NONE',  ( -2.229367062500000163, 7.520833334698929562, -3.861377020970580443 ) ) ;
#31845 = CARTESIAN_POINT ( 'NONE',  ( 9.457646018065525792E-16, -68.06249999863440792, 5.148502694627439702 ) ) ;
#31846 = CARTESIAN_POINT ( 'NONE',  ( 4.458734125000000326, -22.14583333196773296, 2.574251347313718519 ) ) ;
#31847 = CARTESIAN_POINT ( 'NONE',  ( -3.535250795749689387E-16, 1.750000000000001554, -5.773502691896257311 ) ) ;
#31848 = CARTESIAN_POINT ( 'NONE',  ( 4.458734124999999437, -161.5000000013656063, 1.846868145590737864 ) ) ;
#31849 = CARTESIAN_POINT ( 'NONE',  ( 0.000000000000000000, -170.0000000000000000, 5.000000000000000000 ) ) ;
#31850 = CARTESIAN_POINT ( 'NONE',  ( 2.229367062499998831, -61.64583333196774362, -3.861377020970580887 ) ) ;
#31851 = CARTESIAN_POINT ( 'NONE',  ( -4.999999999999999112, -93.79166666393545881, 2.886751345948131764 ) ) ;
#31852 = CARTESIAN_POINT ( 'NONE',  ( -3.152548672688508926E-16, -37.56249999863440792, -5.148502694627439702 ) ) ;
#31853 = EDGE_CURVE ( 'NONE', #34317, #25633, #8983, .T. ) ;
#31854 = CARTESIAN_POINT ( 'NONE',  ( 2.500000000000002220, -51.54166666393547303, 4.330127018922192761 ) ) ;
#31855 = CARTESIAN_POINT ( 'NONE',  ( 4.458734124999998549, -67.97916666530106511, -2.574251347313721627 ) ) ;
#31856 = CARTESIAN_POINT ( 'NONE',  ( -5.000000000000000000, -48.08333333333332860, -2.886751345948128211 ) ) ;
#31857 = CARTESIAN_POINT ( 'NONE',  ( -6.972266317189433020E-16, -23.24999999999999645, -5.000000000000000000 ) ) ;
#31858 = CARTESIAN_POINT ( 'NONE',  ( 5.000000000000000000, -68.37499999726881583, -6.123233995736766282E-16 ) ) ;
#31859 = ORIENTED_EDGE ( 'NONE', *, *, #22115, .T. ) ;
#31860 = CARTESIAN_POINT ( 'NONE',  ( -3.152548672688508926E-16, -106.5624999986343937, -5.148502694627439702 ) ) ;
#31861 = CARTESIAN_POINT ( 'NONE',  ( -4.458734124999999437, -3.562499998634407916, 0.000000000000000000 ) ) ;
#31862 = CARTESIAN_POINT ( 'NONE',  ( 5.000000000000000888, -144.0625000027311273, -2.071067811865475505 ) ) ;
#31863 = CARTESIAN_POINT ( 'NONE',  ( -2.500000000000000444, -10.16666666666666430, -4.330127018922193649 ) ) ;
#31864 = AXIS2_PLACEMENT_3D ( 'NONE', #15642, #35258, #40707 ) ;
#31865 = CARTESIAN_POINT ( 'NONE',  ( 2.229367062500001939, -69.97916666530107932, 3.861377020970579999 ) ) ;
#31866 = CARTESIAN_POINT ( 'NONE',  ( -1.339745962155613812, -31.08034179853029144, -5.000000000000000000 ) ) ;
#31867 = CARTESIAN_POINT ( 'NONE',  ( 2.499999999999998668, -11.20833333060214798, -4.330127018922193649 ) ) ;
#31869 = ORIENTED_EDGE ( 'NONE', *, *, #6302, .F. ) ;
#31868 = CARTESIAN_POINT ( 'NONE',  ( 9.457646018065525792E-16, -41.06249999863440792, 5.148502694627439702 ) ) ;
#31870 = LINE ( 'NONE', #42459, #56956 ) ;
#31872 = ORIENTED_EDGE ( 'NONE', *, *, #43360, .T. ) ;
#31871 = CARTESIAN_POINT ( 'NONE',  ( 2.229367062500001939, 10.77083333469892956, 3.861377020970579999 ) ) ;
#31873 = CARTESIAN_POINT ( 'NONE',  ( 0.000000000000000000, 0.000000000000000000, 0.000000000000000000 ) ) ;
#31874 = CARTESIAN_POINT ( 'NONE',  ( -2.500000000000000444, -55.16666666666667140, -4.330127018922193649 ) ) ;
#31875 = CARTESIAN_POINT ( 'NONE',  ( -1.846868145590737420, -161.0000000013656063, 4.458734124999999437 ) ) ;
#31876 = CARTESIAN_POINT ( 'NONE',  ( -3.152548672688508926E-16, -34.81249999863440792, -5.148502694627439702 ) ) ;
#31877 = CARTESIAN_POINT ( 'NONE',  ( 2.499999999999998668, -10.33333333333333393, -4.330127018922193649 ) ) ;
#31878 = CARTESIAN_POINT ( 'NONE',  ( 2.229367062499998831, -80.64583333196773651, -3.861377020970580887 ) ) ;
#31879 = CARTESIAN_POINT ( 'NONE',  ( 2.071067811865476394, -169.1875000000000000, 5.000000000000000000 ) ) ;
#31880 = CARTESIAN_POINT ( 'NONE',  ( 4.458734124999999437, -86.81249999863439371, -5.460374474430324690E-16 ) ) ;
#31881 = CARTESIAN_POINT ( 'NONE',  ( -55.35523342533222291, -133.5625000013656063, 4.444560631937231499 ) ) ;
#31882 = CARTESIAN_POINT ( 'NONE',  ( -2.229367062500000163, 0.2708333346989263979, -3.861377020970580443 ) ) ;
#31883 = CARTESIAN_POINT ( 'NONE',  ( -2.229367062500000163, -36.72916666530107221, -3.861377020970580443 ) ) ;
#31884 = EDGE_CURVE ( 'NONE', #52286, #4881, #22151, .T. ) ;
#31885 = EDGE_CURVE ( 'NONE', #9668, #20741, #50887, .T. ) ;
#31886 = CARTESIAN_POINT ( 'NONE',  ( -2.499999999999996447, 24.29166666939785202, 4.330127018922195425 ) ) ;
#31887 = CARTESIAN_POINT ( 'NONE',  ( 4.458734125000001214, -77.14583333196775072, 2.574251347313718519 ) ) ;
#31888 = CARTESIAN_POINT ( 'NONE',  ( -5.000000000000000888, 5.773502691896258199, -7.063244554130002406 ) ) ;
#31889 = EDGE_CURVE ( 'NONE', #32568, #30305, #48051, .T. ) ;
#31890 = ORIENTED_EDGE ( 'NONE', *, *, #38208, .T. ) ;
#31891 = CARTESIAN_POINT ( 'NONE',  ( -53.33387254593733928, -153.9375000027312126, 5.149110718188519620 ) ) ;
#31892 = CARTESIAN_POINT ( 'NONE',  ( 0.000000000000000000, -120.0000000000000000, 0.000000000000000000 ) ) ;
#31893 = CARTESIAN_POINT ( 'NONE',  ( -4.458734124999999437, -71.64583333196773651, -2.574251347313719407 ) ) ;
#31894 = CARTESIAN_POINT ( 'NONE',  ( 2.229367062500001939, -11.22916666530107044, 3.861377020970579999 ) ) ;
#31895 = ORIENTED_EDGE ( 'NONE', *, *, #48531, .T. ) ;
#31896 = EDGE_CURVE ( 'NONE', #35368, #33079, #24868, .T. ) ;
#31897 =( BOUNDED_CURVE ( )  B_SPLINE_CURVE ( 2, ( #30752, #21427, #60676, #10811, #16599, #36217, #15321, #54881, #16282 ),
 .UNSPECIFIED., .F., .F. ) 
 B_SPLINE_CURVE_WITH_KNOTS ( ( 3, 2, 2, 2, 3 ),
 ( 0.3937499999999999889, 0.3944444444444444309, 0.3958333333333333148, 0.3972222222222221988, 0.3979166666666666963 ),
 .UNSPECIFIED. ) 
 CURVE ( )  GEOMETRIC_REPRESENTATION_ITEM ( )  RATIONAL_B_SPLINE_CURVE ( ( 0.9330127018922194093, 0.9330127018922194093, 1.000000000000000000, 0.8660254037844387076, 1.000000000000000000, 0.8660254037844387076, 1.000000000000000000, 0.9330127018922167448, 0.9330127018922194093 ) ) 
 REPRESENTATION_ITEM ( '' )  );
#31898 = CARTESIAN_POINT ( 'NONE',  ( 5.000000000000000000, -164.0625000000000000, 2.071067811865478614 ) ) ;
#31899 = CARTESIAN_POINT ( 'NONE',  ( 9.457646018065525792E-16, -8.312499998634406140, 5.148502694627439702 ) ) ;
#31900 = EDGE_CURVE ( 'NONE', #25633, #5644, #28700, .T. ) ;
#31901 = CARTESIAN_POINT ( 'NONE',  ( -4.729367062499999719, 29.84375000068279604, 0.000000000000000000 ) ) ;
#31902 = CARTESIAN_POINT ( 'NONE',  ( -2.229367062499996610, 7.854166668032260823, 3.861377020970582219 ) ) ;
#31903 = AXIS2_PLACEMENT_3D ( 'NONE', #13415, #46571, #52027 ) ;
#31904 = CARTESIAN_POINT ( 'NONE',  ( 1.846868145590735200, -156.2500000013656063, -4.458734124999999437 ) ) ;
#31905 = CARTESIAN_POINT ( 'NONE',  ( 4.458734125000000326, 26.85416666803225993, 2.574251347313718519 ) ) ;
#31906 = EDGE_LOOP ( 'NONE', ( #49418, #8929, #7685, #11116 ) ) ;
#31907 = CARTESIAN_POINT ( 'NONE',  ( -2.229367062500000163, -86.47916666530107932, -3.861377020970580443 ) ) ;
#31908 = EDGE_CURVE ( 'NONE', #44350, #45572, #44790, .T. ) ;
#31909 = CARTESIAN_POINT ( 'NONE',  ( -5.000000000000000000, -31.00000000000000000, 0.000000000000000000 ) ) ;
#31910 = CARTESIAN_POINT ( 'NONE',  ( 2.229367062499998831, -3.645833331967739177, -3.861377020970580887 ) ) ;
#31911 = LINE ( 'NONE', #12916, #38555 ) ;
#31912 =( BOUNDED_CURVE ( )  B_SPLINE_CURVE ( 2, ( #17606, #31426, #37222, #2197, #13085, #7955, #32388, #51064, #47189 ),
 .UNSPECIFIED., .F., .F. ) 
 B_SPLINE_CURVE_WITH_KNOTS ( ( 3, 2, 2, 2, 3 ),
 ( 0.8196428571428571175, 0.8202380952380952106, 0.8214285714285713969, 0.8226190476190475831, 0.8232142857142856762 ),
 .UNSPECIFIED. ) 
 CURVE ( )  GEOMETRIC_REPRESENTATION_ITEM ( )  RATIONAL_B_SPLINE_CURVE ( ( 0.9330127018922194093, 0.9330127018922194093, 1.000000000000000000, 0.8660254037844387076, 1.000000000000000000, 0.8660254037844387076, 1.000000000000000000, 0.9330127018922194093, 0.9330127018922194093 ) ) 
 REPRESENTATION_ITEM ( '' )  );
#31913 = CARTESIAN_POINT ( 'NONE',  ( 1.060575238724906964E-15, -32.62499999726880873, 5.773502691896257311 ) ) ;
#31914 = LINE ( 'NONE', #61519, #9057 ) ;
#31915 = CARTESIAN_POINT ( 'NONE',  ( 2.229367062499998831, 25.35416666803225993, -3.861377020970580887 ) ) ;
#31916 = CARTESIAN_POINT ( 'NONE',  ( 2.500000000000002220, -7.666666666666668739, 4.330127018922192761 ) ) ;
#31917 = CARTESIAN_POINT ( 'NONE',  ( 2.229367062499998831, 28.35416666803225993, -3.861377020970580887 ) ) ;
#31918 = CARTESIAN_POINT ( 'NONE',  ( 4.458734125000001214, -50.89583333196772230, 2.574251347313718519 ) ) ;
#31919 = CARTESIAN_POINT ( 'NONE',  ( 4.458734124999998549, -36.97916666530107221, -2.574251347313721627 ) ) ;
#31920 = CARTESIAN_POINT ( 'NONE',  ( -4.458734124999999437, -3.562499998634407916, 0.000000000000000000 ) ) ;
#31921 = CARTESIAN_POINT ( 'NONE',  ( 1.339745962155615144, -0.5803417985302927740, 4.999999999999999112 ) ) ;
#31922 = CARTESIAN_POINT ( 'NONE',  ( 5.000000000000000000, 14.49999999999999822, -6.123233995736766282E-16 ) ) ;
#31923 = CARTESIAN_POINT ( 'NONE',  ( 3.061616997868383141E-16, -141.8750000027312126, -5.000000000000000000 ) ) ;
#31924 = CARTESIAN_POINT ( 'NONE',  ( 3.535533905932736864, -159.1250000000000284, 3.535533905932738641 ) ) ;
#31925 = CARTESIAN_POINT ( 'NONE',  ( -3.152548672688508926E-16, -47.56249999863440792, -5.148502694627439702 ) ) ;
#31926 = CARTESIAN_POINT ( 'NONE',  ( -2.500000000000000444, -77.04166666393547303, -4.330127018922193649 ) ) ;
#31927 = CARTESIAN_POINT ( 'NONE',  ( -59.29741812935640155, -138.8750000013655779, -2.196230717870135685 ) ) ;
#31928 = CARTESIAN_POINT ( 'NONE',  ( 0.000000000000000000, -170.0000000000000000, 0.000000000000000000 ) ) ;
#31929 = CARTESIAN_POINT ( 'NONE',  ( 2.500000000000002220, -22.66666666666666785, 4.330127018922192761 ) ) ;
#31930 = CARTESIAN_POINT ( 'NONE',  ( 4.458734124999999437, -83.06249999863440792, -5.460374474430324690E-16 ) ) ;
#31931 = CARTESIAN_POINT ( 'NONE',  ( 4.458734124999997661, -159.7500000013656063, 1.846868145590737864 ) ) ;
#31932 = CARTESIAN_POINT ( 'NONE',  ( -5.000000000000000000, -35.00000000000000000, 0.000000000000000000 ) ) ;
#31933 = CARTESIAN_POINT ( 'NONE',  ( -6.972266317189433020E-16, -57.25000000000000000, -5.000000000000000000 ) ) ;
#31934 = ORIENTED_EDGE ( 'NONE', *, *, #51847, .F. ) ;
#31935 = CARTESIAN_POINT ( 'NONE',  ( -4.458734124999999437, 18.43750000136559564, 0.000000000000000000 ) ) ;
#31936 = ORIENTED_EDGE ( 'NONE', *, *, #8583, .F. ) ;
#31937 = CARTESIAN_POINT ( 'NONE',  ( 4.458734125000001214, -92.89583333196775072, 2.574251347313718519 ) ) ;
#31938 = CARTESIAN_POINT ( 'NONE',  ( -4.458734124999999437, 15.35416666803225993, -2.574251347313719407 ) ) ;
#31939 = CARTESIAN_POINT ( 'NONE',  ( -5.000000000000000000, 18.12500000273118417, 0.000000000000000000 ) ) ;
#31940 = CARTESIAN_POINT ( 'NONE',  ( -6.972266317189433020E-16, -16.25000000000000000, -5.000000000000000000 ) ) ;
#31941 = CARTESIAN_POINT ( 'NONE',  ( 2.499999999999998668, 10.66666666666666430, -4.330127018922193649 ) ) ;
#31942 = CARTESIAN_POINT ( 'NONE',  ( -2.229367062500000163, -56.47916666530107221, -3.861377020970580443 ) ) ;
#31943 = LINE ( 'NONE', #42536, #40018 ) ;
#31944 = CARTESIAN_POINT ( 'NONE',  ( -50.55543936806279248, -135.3125000013656063, 0.3552334253322060320 ) ) ;
#31945 = CARTESIAN_POINT ( 'NONE',  ( 5.275681513340003914E-14, 9.875000002731184168, -5.000000000000000000 ) ) ;
#31946 = CARTESIAN_POINT ( 'NONE',  ( 1.339745962155615144, -33.58034179853029144, 4.999999999999999112 ) ) ;
#31947 = CARTESIAN_POINT ( 'NONE',  ( -3.535533905932738641, -151.5000000027312126, 3.535533905932737309 ) ) ;
#31948 = CARTESIAN_POINT ( 'NONE',  ( -3.535250795749689387E-16, -40.24999999999998579, -5.773502691896257311 ) ) ;
#31950 = CARTESIAN_POINT ( 'NONE',  ( 4.458734124999999437, -14.06249999863440436, -5.460374474430324690E-16 ) ) ;
#31949 = CARTESIAN_POINT ( 'NONE',  ( 0.000000000000000000, -120.0000000000000000, 0.000000000000000000 ) ) ;
#31951 = CARTESIAN_POINT ( 'NONE',  ( -6.972266317189433020E-16, -107.1249999972687874, -5.000000000000000000 ) ) ;
#31952 = CARTESIAN_POINT ( 'NONE',  ( 9.457646018065525792E-16, -64.06249999863440792, 5.148502694627439702 ) ) ;
#31953 = CARTESIAN_POINT ( 'NONE',  ( -4.458734124999999437, -152.1875000013656063, -5.460374474430324690E-16 ) ) ;
#31954 = CARTESIAN_POINT ( 'NONE',  ( -4.458734124999999437, -69.31249999863439371, 0.000000000000000000 ) ) ;
#31955 = CARTESIAN_POINT ( 'NONE',  ( -59.29741812935640155, -148.8750000013655779, -2.196230717870135685 ) ) ;
#31956 = CARTESIAN_POINT ( 'NONE',  ( -4.458734124999999437, -19.64583333196774362, -2.574251347313719407 ) ) ;
#31957 = CARTESIAN_POINT ( 'NONE',  ( -3.535250795749689387E-16, -60.12499999726880162, -5.773502691896257311 ) ) ;
#31959 = VERTEX_POINT ( 'NONE', #1399 ) ;
#31958 = EDGE_CURVE ( 'NONE', #60996, #37188, #43896, .T. ) ;
#31960 = CARTESIAN_POINT ( 'NONE',  ( 0.000000000000000000, -170.0000000000000000, 0.000000000000000000 ) ) ;
#31961 = ORIENTED_EDGE ( 'NONE', *, *, #5968, .F. ) ;
#31962 = CARTESIAN_POINT ( 'NONE',  ( -4.458734124999999437, -64.56249999863440792, 0.000000000000000000 ) ) ;
#31963 = CARTESIAN_POINT ( 'NONE',  ( -6.972266317189433020E-16, -21.12499999726881228, -5.000000000000000000 ) ) ;
#31964 = CARTESIAN_POINT ( 'NONE',  ( -4.458734124999999437, -150.9375000013656063, -5.460374474430324690E-16 ) ) ;
#31965 = ORIENTED_EDGE ( 'NONE', *, *, #42939, .T. ) ;
#31966 =( BOUNDED_CURVE ( )  B_SPLINE_CURVE ( 2, ( #59151, #15083, #9616, #4177, #14123, #4478, #34697, #10260, #29861 ),
 .UNSPECIFIED., .F., .F. ) 
 B_SPLINE_CURVE_WITH_KNOTS ( ( 3, 2, 2, 2, 3 ),
 ( 0.1937500000000000056, 0.1944444444444444475, 0.1958333333333333315, 0.1972222222222222154, 0.1979166666666666574 ),
 .UNSPECIFIED. ) 
 CURVE ( )  GEOMETRIC_REPRESENTATION_ITEM ( )  RATIONAL_B_SPLINE_CURVE ( ( 0.9330127018922194093, 0.9330127018922194093, 1.000000000000000000, 0.8660254037844387076, 1.000000000000000000, 0.8660254037844387076, 1.000000000000000000, 0.9330127018922194093, 0.9330127018922194093 ) ) 
 REPRESENTATION_ITEM ( '' )  );
#31967 = CARTESIAN_POINT ( 'NONE',  ( 5.000000000000000000, -155.1250000027311842, 0.000000000000000000 ) ) ;
#31968 = CARTESIAN_POINT ( 'NONE',  ( -51.19402409849444524, -125.5000000000000284, -3.242614290531456334 ) ) ;
#31969 = CARTESIAN_POINT ( 'NONE',  ( -75.00000000000000000, 15.00000000000000000, 8.999999999999998224 ) ) ;
#31970 = CARTESIAN_POINT ( 'NONE',  ( 4.458734125000001214, -47.14583333196774362, 2.574251347313718519 ) ) ;
#31971 = ORIENTED_EDGE ( 'NONE', *, *, #3527, .T. ) ;
#31972 = CARTESIAN_POINT ( 'NONE',  ( -6.031010364368858512E-14, 2.375000002731183280, 5.000000000000000000 ) ) ;
#31973 = CARTESIAN_POINT ( 'NONE',  ( 9.457646018065525792E-16, 8.937500001365597413, 5.148502694627439702 ) ) ;
#31974 = EDGE_CURVE ( 'NONE', #49174, #28941, #57096, .T. ) ;
#31975 = CARTESIAN_POINT ( 'NONE',  ( -4.458734124999999437, 21.60416666803225993, -2.574251347313719407 ) ) ;
#31976 = CARTESIAN_POINT ( 'NONE',  ( -54.64476657466781973, -148.8125000013656063, -4.444560631937228834 ) ) ;
#31977 = CARTESIAN_POINT ( 'NONE',  ( 1.339745962155729053, -77.29465819873853150, -4.999999999999933387 ) ) ;
#31978 = CARTESIAN_POINT ( 'NONE',  ( 2.730187237215162345E-16, -169.1875000013656063, -4.458734124999999437 ) ) ;
#31980 = ADVANCED_FACE ( 'NONE', ( #29673 ), #40919, .T. ) ;
#31979 = ORIENTED_EDGE ( 'NONE', *, *, #16484, .T. ) ;
#31981 = CARTESIAN_POINT ( 'NONE',  ( -4.458734124999999437, -73.31249999863439371, 0.000000000000000000 ) ) ;
#31982 = CARTESIAN_POINT ( 'NONE',  ( 5.000000000000000888, 14.54166666939785202, 2.886751345948126879 ) ) ;
#31983 = CARTESIAN_POINT ( 'NONE',  ( -2.229367062500000163, 11.52083333469892601, -3.861377020970580443 ) ) ;
#31984 = EDGE_CURVE ( 'NONE', #20487, #38204, #63656, .T. ) ;
#31985 = CYLINDRICAL_SURFACE ( 'NONE', #26503, 5.000000000000000000 ) ;
#31986 = CARTESIAN_POINT ( 'NONE',  ( -4.458734124999998549, -55.47916666530107221, 2.574251347313722516 ) ) ;
#31987 = CARTESIAN_POINT ( 'NONE',  ( -2.500000000000000444, -16.04166666393548368, -4.330127018922193649 ) ) ;
#31988 = CARTESIAN_POINT ( 'NONE',  ( -5.000000000000000000, -19.08333333333333570, -2.886751345948128211 ) ) ;
#31989 = CARTESIAN_POINT ( 'NONE',  ( -2.480964764533239819E-13, -60.62499999726880873, 5.000000000000000000 ) ) ;
#31990 = CARTESIAN_POINT ( 'NONE',  ( 2.229367062500001939, -32.97916666530106511, 3.861377020970579999 ) ) ;
#31991 = CARTESIAN_POINT ( 'NONE',  ( 4.458734124999999437, -22.06249999863440436, -5.460374474430324690E-16 ) ) ;
#31992 = VERTEX_POINT ( 'NONE', #2652 ) ;
#31993 = CARTESIAN_POINT ( 'NONE',  ( -5.000000000000000000, -61.08333333333333570, -2.886751345948128211 ) ) ;
#31994 = CARTESIAN_POINT ( 'NONE',  ( 4.458734124999998549, -107.7291666653010509, -2.574251347313721627 ) ) ;
#31995 = CARTESIAN_POINT ( 'NONE',  ( 2.071067811865475505, -154.9375000027311842, -5.000000000000000888 ) ) ;
#31996 = ORIENTED_EDGE ( 'NONE', *, *, #26751, .F. ) ;
#31997 = CARTESIAN_POINT ( 'NONE',  ( 4.458734125000001214, -103.1458333319677365, 2.574251347313718519 ) ) ;
#31998 = VECTOR ( 'NONE', #44827, 1000.000000000000000 ) ;
#31999 = CARTESIAN_POINT ( 'NONE',  ( 9.457646018065525792E-16, -25.06249999863440792, 5.148502694627439702 ) ) ;
#32000 = CARTESIAN_POINT ( 'NONE',  ( 5.000000000000000000, -63.29166666393547303, -2.886751345948129988 ) ) ;
#32001 = CARTESIAN_POINT ( 'NONE',  ( -54.64476657466781973, -153.0625000013656063, -4.444560631937228834 ) ) ;
#32002 = CARTESIAN_POINT ( 'NONE',  ( 5.000000000000000000, -148.0000000000000284, 0.000000000000000000 ) ) ;
#32003 = CARTESIAN_POINT ( 'NONE',  ( -3.152548672688508926E-16, -28.56249999863440081, -5.148502694627439702 ) ) ;
#32004 = CARTESIAN_POINT ( 'NONE',  ( -4.458734124999999437, -69.56249999863439371, 0.000000000000000000 ) ) ;
#32005 = CARTESIAN_POINT ( 'NONE',  ( -49.85088928181150436, -153.6875000027311842, -1.666127454062680480 ) ) ;
#32006 = CARTESIAN_POINT ( 'NONE',  ( -3.152548672688508926E-16, -22.56249999863440436, -5.148502694627439702 ) ) ;
#32007 = CARTESIAN_POINT ( 'NONE',  ( 5.000000000000000000, -32.50000000000000000, -6.123233995736766282E-16 ) ) ;
#32008 = CARTESIAN_POINT ( 'NONE',  ( 2.499999999999998668, -5.208333330602148870, -4.330127018922193649 ) ) ;
#32009 = CARTESIAN_POINT ( 'NONE',  ( -5.000000000000000000, -15.00000000000000000, 0.000000000000000000 ) ) ;
#32010 = CARTESIAN_POINT ( 'NONE',  ( 1.846868145590735200, -153.2500000013655779, -4.458734125000000326 ) ) ;
#32011 = ORIENTED_EDGE ( 'NONE', *, *, #55941, .F. ) ;
#32012 = CARTESIAN_POINT ( 'NONE',  ( -6.972266317189433020E-16, 17.75000000000000355, -5.000000000000000000 ) ) ;
#32013 = CARTESIAN_POINT ( 'NONE',  ( 9.457646018065525792E-16, -49.31249999863440792, 5.148502694627439702 ) ) ;
#32014 = CARTESIAN_POINT ( 'NONE',  ( 1.339745962155615144, -58.58034179853029855, 4.999999999999999112 ) ) ;
#32015 = DIRECTION ( 'NONE',  ( -0.000000000000000000, 1.000000000000000000, -0.000000000000000000 ) ) ;
#32016 = CARTESIAN_POINT ( 'NONE',  ( 5.000000000000000888, 22.41666666666666785, 2.886751345948126879 ) ) ;
#32017 = CARTESIAN_POINT ( 'NONE',  ( -51.19402409849444524, -152.5000000000000284, -3.242614290531456334 ) ) ;
#32018 = CARTESIAN_POINT ( 'NONE',  ( -4.458734124999998549, -2.229166665301068662, 2.574251347313722516 ) ) ;
#32019 = CARTESIAN_POINT ( 'NONE',  ( 2.500000000000002220, 1.458333336064519203, 4.330127018922192761 ) ) ;
#32020 = CARTESIAN_POINT ( 'NONE',  ( -4.458734124999998549, 15.52083333469892779, 2.574251347313722516 ) ) ;
#32021 = CARTESIAN_POINT ( 'NONE',  ( 2.499999999999998668, 4.791666669397852907, -4.330127018922193649 ) ) ;
#32022 = ORIENTED_EDGE ( 'NONE', *, *, #31511, .T. ) ;
#32023 = CARTESIAN_POINT ( 'NONE',  ( 1.975475456537005874E-15, -42.75000000000000000, 5.000000000000000000 ) ) ;
#32024 = VERTEX_POINT ( 'NONE', #22596 ) ;
#32025 = CARTESIAN_POINT ( 'NONE',  ( 2.500000000000002220, 27.45833333606451632, 4.330127018922192761 ) ) ;
#32026 = CARTESIAN_POINT ( 'NONE',  ( -4.458734124999998549, -42.22916666530107932, 2.574251347313722516 ) ) ;
#32027 = CARTESIAN_POINT ( 'NONE',  ( -1.846868145590734756, -164.3750000013656063, -4.458734125000000326 ) ) ;
#32028 = EDGE_CURVE ( 'NONE', #56895, #9036, #54635, .T. ) ;
#32029 = CARTESIAN_POINT ( 'NONE',  ( 5.000000000000000000, -46.29166666393547303, -2.886751345948129988 ) ) ;
#32030 = ORIENTED_EDGE ( 'NONE', *, *, #17388, .T. ) ;
#32031 = CARTESIAN_POINT ( 'NONE',  ( 9.457646018065525792E-16, -22.06249999863440436, 5.148502694627439702 ) ) ;
#32032 = ORIENTED_EDGE ( 'NONE', *, *, #40525, .T. ) ;
#32033 = CARTESIAN_POINT ( 'NONE',  ( 2.499999999999998668, -89.33333333333332860, -4.330127018922193649 ) ) ;
#32034 = CARTESIAN_POINT ( 'NONE',  ( 4.458734124999999437, -164.5000000013655779, 1.846868145590737864 ) ) ;
#32035 = CARTESIAN_POINT ( 'NONE',  ( 2.500000000000002220, -39.54166666393548013, 4.330127018922192761 ) ) ;
#32036 = CARTESIAN_POINT ( 'NONE',  ( -58.24261429053147765, -139.2500000000000000, -3.805975901505573855 ) ) ;
#32037 = CARTESIAN_POINT ( 'NONE',  ( 2.229367062500001939, -34.22916666530107221, 3.861377020970579999 ) ) ;
#32038 = CARTESIAN_POINT ( 'NONE',  ( -2.499999999999996447, 21.16666666666666785, 4.330127018922195425 ) ) ;
#32039 = ORIENTED_EDGE ( 'NONE', *, *, #16092, .T. ) ;
#32040 = CARTESIAN_POINT ( 'NONE',  ( -4.458734124999998549, -75.22916666530106511, 2.574251347313722516 ) ) ;
#32041 = CARTESIAN_POINT ( 'NONE',  ( 4.458734124999998549, 22.27083333469893134, -2.574251347313721627 ) ) ;
#32042 = CARTESIAN_POINT ( 'NONE',  ( 1.975475456537005874E-15, -87.62499999726880162, 5.000000000000000000 ) ) ;
#32043 = VERTEX_POINT ( 'NONE', #26456 ) ;
#32044 = CARTESIAN_POINT ( 'NONE',  ( -2.071067811865496378, -166.8125000027312410, -4.999999999999979572 ) ) ;
#32045 = CARTESIAN_POINT ( 'NONE',  ( -59.29741812935640155, -140.8750000013656063, -2.196230717870135685 ) ) ;
#32046 = CARTESIAN_POINT ( 'NONE',  ( -4.458734124999998549, -79.47916666530106511, 2.574251347313722516 ) ) ;
#32047 = CARTESIAN_POINT ( 'NONE',  ( -50.18089887299979068, -130.8125000027312410, 2.462841084822635640 ) ) ;
#32048 = CARTESIAN_POINT ( 'NONE',  ( 1.339745962155615144, -27.70534180126147561, 4.999999999999999112 ) ) ;
#32049 = CARTESIAN_POINT ( 'NONE',  ( -5.000000000000000888, -158.6875000027312126, -2.071067811865475949 ) ) ;
#32050 = CARTESIAN_POINT ( 'NONE',  ( 2.500000000000002220, 20.33333333333333215, 4.330127018922192761 ) ) ;
#32051 = CARTESIAN_POINT ( 'NONE',  ( 4.458734124999998549, -54.72916666530107221, -2.574251347313721627 ) ) ;
#32052 = CARTESIAN_POINT ( 'NONE',  ( 4.458734125000000326, -47.89583333196774362, 2.574251347313718519 ) ) ;
#32053 = CARTESIAN_POINT ( 'NONE',  ( 4.458734124999999437, 29.18750000136559208, -5.460374474430324690E-16 ) ) ;
#32054 = CARTESIAN_POINT ( 'NONE',  ( -2.499999999999996447, -105.8333333333333286, 4.330127018922195425 ) ) ;
#32055 = CARTESIAN_POINT ( 'NONE',  ( 3.061616997868383141E-16, -153.8750000027311842, -5.000000000000000000 ) ) ;
#32056 = CARTESIAN_POINT ( 'NONE',  ( 4.458734125000001214, -40.14583333196772941, 2.574251347313718519 ) ) ;
#32057 = CARTESIAN_POINT ( 'NONE',  ( 5.000000000000000000, 2.708333336064520314, -2.886751345948129988 ) ) ;
#32058 = CARTESIAN_POINT ( 'NONE',  ( 0.000000000000000000, -170.0000000000000000, 0.000000000000000000 ) ) ;
#32059 = CARTESIAN_POINT ( 'NONE',  ( -50.40829686548195099, -125.0000000013656205, -1.485763867205728284 ) ) ;
#32060 = CARTESIAN_POINT ( 'NONE',  ( 2.229367062499998831, -78.89583333196773651, -3.861377020970580887 ) ) ;
#32061 = CARTESIAN_POINT ( 'NONE',  ( -4.999999999999998224, 6.083333333333333037, 2.886751345948131764 ) ) ;
#32062 = CARTESIAN_POINT ( 'NONE',  ( 2.229367062499998831, -100.6458333319677365, -3.861377020970580887 ) ) ;
#32063 = CARTESIAN_POINT ( 'NONE',  ( -3.152548672688508926E-16, -3.812499998634408360, -5.148502694627439702 ) ) ;
#32064 = ORIENTED_EDGE ( 'NONE', *, *, #55598, .T. ) ;
#32065 = CARTESIAN_POINT ( 'NONE',  ( -1.510657702057710340E-15, 28.25000000000000000, 5.000000000000000000 ) ) ;
#32066 = CARTESIAN_POINT ( 'NONE',  ( 9.457646018065525792E-16, -95.06249999863440792, 5.148502694627439702 ) ) ;
#32067 = CARTESIAN_POINT ( 'NONE',  ( -5.000000000000000000, -5.083333333333334814, -2.886751345948128211 ) ) ;
#32068 = CARTESIAN_POINT ( 'NONE',  ( -2.229367062499996610, -88.39583333196773651, 3.861377020970582219 ) ) ;
#32069 = CARTESIAN_POINT ( 'NONE',  ( -4.458734124999999437, 10.43750000136559386, 0.000000000000000000 ) ) ;
#32070 = DIRECTION ( 'NONE',  ( 0.000000000000000000, 0.000000000000000000, 1.000000000000000000 ) ) ;
#32071 = CARTESIAN_POINT ( 'NONE',  ( -50.70258187064364108, -135.1250000013656063, 2.196230717870141014 ) ) ;
#32072 = CARTESIAN_POINT ( 'NONE',  ( 4.458734124999999437, -9.812499998634406140, -5.460374474430324690E-16 ) ) ;
#32073 = CARTESIAN_POINT ( 'NONE',  ( 9.457646018065525792E-16, 18.68750000136559208, 5.148502694627439702 ) ) ;
#32074 = CARTESIAN_POINT ( 'NONE',  ( 4.458734124999999437, -54.06249999863440081, -5.460374474430324690E-16 ) ) ;
#32075 = CARTESIAN_POINT ( 'NONE',  ( 3.061616997868383141E-16, -163.7500000000000000, -5.000000000000000000 ) ) ;
#32076 = CARTESIAN_POINT ( 'NONE',  ( -1.339745962155613812, -37.20534180126147561, -5.000000000000000000 ) ) ;
#32077 = CARTESIAN_POINT ( 'NONE',  ( 2.229367062500001939, -7.979166665301073991, 3.861377020970579999 ) ) ;
#32078 = CARTESIAN_POINT ( 'NONE',  ( 1.339745962155615144, -109.5803417985302843, 4.999999999999999112 ) ) ;
#32079 = VERTEX_POINT ( 'NONE', #2979 ) ;
#32080 = CARTESIAN_POINT ( 'NONE',  ( 4.458734125000000326, -37.14583333196773651, 2.574251347313718519 ) ) ;
#32081 = CARTESIAN_POINT ( 'NONE',  ( -52.80376928212989185, -129.1250000013655779, -4.297418129356379346 ) ) ;
#32082 = CARTESIAN_POINT ( 'NONE',  ( -6.972266317189433020E-16, -68.24999999999998579, -5.000000000000000000 ) ) ;
#32083 = CARTESIAN_POINT ( 'NONE',  ( 2.229367062499998831, -81.64583333196773651, -3.861377020970580887 ) ) ;
#32084 = CARTESIAN_POINT ( 'NONE',  ( 9.457646018065525792E-16, 22.68750000136559564, 5.148502694627439702 ) ) ;
#32085 = ADVANCED_FACE ( 'NONE', ( #61197, #21950 ), #46074, .T. ) ;
#32086 =( BOUNDED_CURVE ( )  B_SPLINE_CURVE ( 2, ( #11778, #36550, #32038, #46837, #22081, #51359, #56505, #61329, #31396 ),
 .UNSPECIFIED., .F., .F. ) 
 B_SPLINE_CURVE_WITH_KNOTS ( ( 3, 2, 2, 2, 3 ),
 ( 0.06250000000000000000, 0.06309523809523809312, 0.06428571428571427937, 0.06547619047619047949, 0.06607142857142857262 ),
 .UNSPECIFIED. ) 
 CURVE ( )  GEOMETRIC_REPRESENTATION_ITEM ( )  RATIONAL_B_SPLINE_CURVE ( ( 0.9330127018922194093, 0.9330127018922194093, 1.000000000000000000, 0.8660254037844387076, 1.000000000000000000, 0.8660254037844387076, 1.000000000000000000, 0.9330127018922194093, 0.9330127018922194093 ) ) 
 REPRESENTATION_ITEM ( '' )  );
#32087 = CARTESIAN_POINT ( 'NONE',  ( -3.152801135295367985, -151.0625000013655779, 3.152801135295367096 ) ) ;
#32088 = CARTESIAN_POINT ( 'NONE',  ( -4.458734124999999437, 12.60416666803225993, -2.574251347313719407 ) ) ;
#32089 = DIRECTION ( 'NONE',  ( -0.000000000000000000, 1.000000000000000000, -0.000000000000000000 ) ) ;
#32090 = FACE_OUTER_BOUND ( 'NONE', #40562, .T. ) ;
#32091 = CARTESIAN_POINT ( 'NONE',  ( -4.458734124999997661, -85.47916666530107932, 2.574251347313722516 ) ) ;
#32092 = CARTESIAN_POINT ( 'NONE',  ( 2.499999999999998668, -64.33333333333332860, -4.330127018922193649 ) ) ;
#32093 = CARTESIAN_POINT ( 'NONE',  ( 0.000000000000000000, -120.0000000000000000, 0.000000000000000000 ) ) ;
#32094 = CARTESIAN_POINT ( 'NONE',  ( 5.000000000000000000, 20.62500000273118772, -6.123233995736766282E-16 ) ) ;
#32095 = VERTEX_POINT ( 'NONE', #12609 ) ;
#32096 = CARTESIAN_POINT ( 'NONE',  ( 1.339745962155615144, -18.58034179853029499, 4.999999999999999112 ) ) ;
#32097 = CARTESIAN_POINT ( 'NONE',  ( 1.975475456537005874E-15, -55.74999999999999289, 5.000000000000000000 ) ) ;
#32099 = CARTESIAN_POINT ( 'NONE',  ( 2.499999999999998668, -22.33333333333332860, -4.330127018922193649 ) ) ;
#32098 = CARTESIAN_POINT ( 'NONE',  ( -1.339745962155613812, -72.20534180126148271, -5.000000000000000000 ) ) ;
#32100 = CARTESIAN_POINT ( 'NONE',  ( -4.458734124999999437, -28.39583333196774007, -2.574251347313719407 ) ) ;
#32101 = CARTESIAN_POINT ( 'NONE',  ( -2.229367062499996610, -90.14583333196773651, 3.861377020970582219 ) ) ;
#32102 = CARTESIAN_POINT ( 'NONE',  ( 5.000000000000000000, -27.37499999726880873, -6.123233995736766282E-16 ) ) ;
#32104 = ORIENTED_EDGE ( 'NONE', *, *, #6790, .T. ) ;
#32103 = CARTESIAN_POINT ( 'NONE',  ( -4.458734124999999437, -59.39583333196773651, -2.574251347313719407 ) ) ;
#32105 = CARTESIAN_POINT ( 'NONE',  ( 2.499999999999998668, -28.33333333333333570, -4.330127018922193649 ) ) ;
#32107 = VERTEX_POINT ( 'NONE', #57006 ) ;
#32106 = CARTESIAN_POINT ( 'NONE',  ( -4.458734124999998549, -10.47916666530107044, 2.574251347313722516 ) ) ;
#32108 = CARTESIAN_POINT ( 'NONE',  ( -2.500000000000000444, -74.16666666666665719, -4.330127018922193649 ) ) ;
#32109 = CARTESIAN_POINT ( 'NONE',  ( -57.19623071787016499, -138.3750000013656063, 4.297418129356382899 ) ) ;
#32110 = CARTESIAN_POINT ( 'NONE',  ( 4.458734125000001214, -52.14583333196772941, 2.574251347313718519 ) ) ;
#32111 = CARTESIAN_POINT ( 'NONE',  ( -2.500000000000000444, -75.04166666393547303, -4.330127018922193649 ) ) ;
#32113 = ORIENTED_EDGE ( 'NONE', *, *, #22458, .F. ) ;
#32112 = CARTESIAN_POINT ( 'NONE',  ( 1.339745962155612702, -10.16965819600733312, -5.000000000000000000 ) ) ;
#32114 = CARTESIAN_POINT ( 'NONE',  ( -51.19402409849444524, -150.5000000000000284, -3.242614290531456334 ) ) ;
#32115 = CARTESIAN_POINT ( 'NONE',  ( 4.458734124999999437, -16.06249999863440436, -5.460374474430324690E-16 ) ) ;
#32116 = CARTESIAN_POINT ( 'NONE',  ( -4.458734124999999437, -56.64583333196773651, -2.574251347313719407 ) ) ;
#32117 = CARTESIAN_POINT ( 'NONE',  ( -5.000000000000000000, -29.87499999726881228, 0.000000000000000000 ) ) ;
#32118 =( LENGTH_UNIT ( ) NAMED_UNIT ( * ) SI_UNIT ( .MILLI., .METRE. ) );
#32119 = CARTESIAN_POINT ( 'NONE',  ( 2.730187237215162345E-16, -140.1875000013656063, -4.458734124999999437 ) ) ;
#32120 = CARTESIAN_POINT ( 'NONE',  ( -2.229367062500000163, -99.72916666530106511, -3.861377020970580443 ) ) ;
#32121 = CARTESIAN_POINT ( 'NONE',  ( 3.535533905932736864, -158.1250000000000284, 3.535533905932738641 ) ) ;
#32122 = VERTEX_POINT ( 'NONE', #55731 ) ;
#32123 = CARTESIAN_POINT ( 'NONE',  ( -50.70258187064364108, -153.3750000013656063, 2.196230717870141014 ) ) ;
#32124 = CARTESIAN_POINT ( 'NONE',  ( -55.39835681537999790, -143.0000000027312126, 4.984105922594378235 ) ) ;
#32125 = CARTESIAN_POINT ( 'NONE',  ( 0.000000000000000000, -170.0000000000000000, 0.000000000000000000 ) ) ;
#32126 = CARTESIAN_POINT ( 'NONE',  ( 4.458734124999998549, -8.729166665301073991, -2.574251347313721627 ) ) ;
#32127 = CARTESIAN_POINT ( 'NONE',  ( -4.458734124999997661, -93.47916666530106511, 2.574251347313722516 ) ) ;
#32128 = CARTESIAN_POINT ( 'NONE',  ( -4.458734125000000326, -148.2500000013656063, -1.846868145590735644 ) ) ;
#32129 = CARTESIAN_POINT ( 'NONE',  ( 2.229367062499998831, -20.89583333196774007, -3.861377020970580887 ) ) ;
#32130 = CARTESIAN_POINT ( 'NONE',  ( -58.24261429053147765, -153.2500000000000284, -3.805975901505573855 ) ) ;
#32131 = CARTESIAN_POINT ( 'NONE',  ( -54.64476657466781973, -138.8125000013656063, -4.444560631937228834 ) ) ;
#32132 =( BOUNDED_CURVE ( )  B_SPLINE_CURVE ( 2, ( #52839, #33534, #53149, #16135, #21278, #45724, #35126, #10982, #29959 ),
 .UNSPECIFIED., .F., .F. ) 
 B_SPLINE_CURVE_WITH_KNOTS ( ( 3, 2, 2, 2, 3 ),
 ( 0.1229166666666666741, 0.1236111111111111160, 0.1250000000000000000, 0.1263888888888888840, 0.1270833333333333259 ),
 .UNSPECIFIED. ) 
 CURVE ( )  GEOMETRIC_REPRESENTATION_ITEM ( )  RATIONAL_B_SPLINE_CURVE ( ( 0.9330127018922194093, 0.9330127018922200755, 1.000000000000000000, 0.8660254037844387076, 1.000000000000000000, 0.8660254037844387076, 1.000000000000000000, 0.9330127018922194093, 0.9330127018922194093 ) ) 
 REPRESENTATION_ITEM ( '' )  );
#32133 = CARTESIAN_POINT ( 'NONE',  ( 4.458734124999999437, -62.06249999863440792, -5.460374474430324690E-16 ) ) ;
#32134 = CARTESIAN_POINT ( 'NONE',  ( 5.000000000000000888, -70.58333333333332860, 2.886751345948126879 ) ) ;
#32135 = CARTESIAN_POINT ( 'NONE',  ( -6.972266317189433020E-16, 16.74999999999999645, -5.000000000000000000 ) ) ;
#32136 = CARTESIAN_POINT ( 'NONE',  ( -3.152801135295367096, -146.0625000013655779, -3.152801135295367541 ) ) ;
#32137 = CARTESIAN_POINT ( 'NONE',  ( 9.457646018065525792E-16, 12.68750000136559208, 5.148502694627439702 ) ) ;
#32138 = EDGE_LOOP ( 'NONE', ( #34409, #8014, #60230, #12325, #53633 ) ) ;
#32139 = CARTESIAN_POINT ( 'NONE',  ( 1.975475456537005874E-15, -18.62499999726881228, 5.000000000000000000 ) ) ;
#32140 = CARTESIAN_POINT ( 'NONE',  ( -5.000000000000000000, -144.5000000000000284, -6.123233995736766282E-16 ) ) ;
#32142 = CARTESIAN_POINT ( 'NONE',  ( -4.458734124999999437, -22.39583333196773651, -2.574251347313719407 ) ) ;
#32141 = CARTESIAN_POINT ( 'NONE',  ( -2.500000000000000444, -90.16666666666665719, -4.330127018922193649 ) ) ;
#32143 = CARTESIAN_POINT ( 'NONE',  ( -5.000000000000000000, -67.99999999999998579, 0.000000000000000000 ) ) ;
#32144 = CARTESIAN_POINT ( 'NONE',  ( -4.458734124999999437, -69.56249999863439371, 0.000000000000000000 ) ) ;
#32145 = DIRECTION ( 'NONE',  ( -0.000000000000000000, 1.000000000000000000, -0.000000000000000000 ) ) ;
#32146 = CARTESIAN_POINT ( 'NONE',  ( -55.00000000000002132, -155.0000000000000284, 1.734723475976807094E-15 ) ) ;
#32147 = CARTESIAN_POINT ( 'NONE',  ( -55.35523342533222291, -147.3125000013656063, 4.444560631937231499 ) ) ;
#32148 = CARTESIAN_POINT ( 'NONE',  ( 4.458734124999999437, 8.187500001365595637, -5.460374474430324690E-16 ) ) ;
#32149 = CARTESIAN_POINT ( 'NONE',  ( -1.339745962155613812, -63.08034179853028434, -5.000000000000000000 ) ) ;
#32150 = CARTESIAN_POINT ( 'NONE',  ( 2.499999999999998668, 21.66666666666666785, -4.330127018922193649 ) ) ;
#32151 = CARTESIAN_POINT ( 'NONE',  ( 4.458734124999998549, 6.270833334698928674, -2.574251347313721627 ) ) ;
#32152 = CARTESIAN_POINT ( 'NONE',  ( -2.229367062500000163, -72.47916666530107932, -3.861377020970580443 ) ) ;
#32153 = CARTESIAN_POINT ( 'NONE',  ( 4.458734125000000326, -17.14583333196773651, 2.574251347313718519 ) ) ;
#32154 = CARTESIAN_POINT ( 'NONE',  ( 1.060575238724906964E-15, -1.750000000000001554, 5.773502691896257311 ) ) ;
#32155 = CARTESIAN_POINT ( 'NONE',  ( -4.458734125000001214, -158.8750000013655779, 1.846868145590734089 ) ) ;
#32156 = DIRECTION ( 'NONE',  ( 0.000000000000000000, 0.000000000000000000, 1.000000000000000000 ) ) ;
#32157 = CARTESIAN_POINT ( 'NONE',  ( -4.458734124999999437, -66.31249999863440792, 0.000000000000000000 ) ) ;
#32158 = CARTESIAN_POINT ( 'NONE',  ( 5.000000000000000000, -100.2916666639354730, -2.886751345948129988 ) ) ;
#32159 = EDGE_CURVE ( 'NONE', #46199, #7616, #17119, .T. ) ;
#32160 = CARTESIAN_POINT ( 'NONE',  ( -60.14911071818854538, -152.1875000027312126, 1.666127454062681146 ) ) ;
#32161 = CARTESIAN_POINT ( 'NONE',  ( 4.458734124999998549, -41.72916666530107932, -2.574251347313721627 ) ) ;
#32162 = CARTESIAN_POINT ( 'NONE',  ( 2.500000000000002220, 19.45833333606451632, 4.330127018922192761 ) ) ;
#32163 = CARTESIAN_POINT ( 'NONE',  ( 2.229367062500001939, -68.22916666530106511, 3.861377020970579999 ) ) ;
#32164 =( BOUNDED_CURVE ( )  B_SPLINE_CURVE ( 2, ( #12952, #38035, #32254, #27427, #3009, #37718, #52829, #37101, #51884 ),
 .UNSPECIFIED., .F., .F. ) 
 B_SPLINE_CURVE_WITH_KNOTS ( ( 3, 2, 2, 2, 3 ),
 ( 0.6812500000000000222, 0.6819444444444444642, 0.6833333333333333481, 0.6847222222222222321, 0.6854166666666666741 ),
 .UNSPECIFIED. ) 
 CURVE ( )  GEOMETRIC_REPRESENTATION_ITEM ( )  RATIONAL_B_SPLINE_CURVE ( ( 0.9330127018922194093, 0.9330127018922194093, 1.000000000000000000, 0.8660254037844387076, 1.000000000000000000, 0.8660254037844387076, 1.000000000000000000, 0.9330127018922194093, 0.9330127018922194093 ) ) 
 REPRESENTATION_ITEM ( '' )  );
#32165 = CARTESIAN_POINT ( 'NONE',  ( -2.499999999999996447, -50.83333333333332860, 4.330127018922195425 ) ) ;
#32166 = CARTESIAN_POINT ( 'NONE',  ( -55.00000000000002132, 0.000000000000000000, 5.000000000000000000 ) ) ;
#32167 = CARTESIAN_POINT ( 'NONE',  ( 5.000000000000000888, -89.58333333333332860, 2.886751345948126879 ) ) ;
#32168 = ORIENTED_EDGE ( 'NONE', *, *, #30712, .F. ) ;
#32169 = CARTESIAN_POINT ( 'NONE',  ( 2.229367062499998831, -109.6458333319677365, -3.861377020970580887 ) ) ;
#32170 = CARTESIAN_POINT ( 'NONE',  ( 5.000000000000000888, -73.45833333060214443, 2.886751345948126879 ) ) ;
#32171 = CARTESIAN_POINT ( 'NONE',  ( -4.999999999999999112, -8.916666666666664298, 2.886751345948131764 ) ) ;
#32172 = CARTESIAN_POINT ( 'NONE',  ( -4.458734124999997661, -72.22916666530107932, 2.574251347313722516 ) ) ;
#32173 = DIRECTION ( 'NONE',  ( -0.000000000000000000, 1.000000000000000000, -0.000000000000000000 ) ) ;
#32174 = ADVANCED_FACE ( 'NONE', ( #42193 ), #2032, .T. ) ;
#32175 = CARTESIAN_POINT ( 'NONE',  ( 5.000000000000000000, -14.29166666393548191, -2.886751345948129988 ) ) ;
#32177 = VERTEX_POINT ( 'NONE', #21637 ) ;
#32176 = CARTESIAN_POINT ( 'NONE',  ( 4.458734124999998549, -41.72916666530107932, -2.574251347313721627 ) ) ;
#32178 = DIRECTION ( 'NONE',  ( -0.000000000000000000, 1.000000000000000000, -0.000000000000000000 ) ) ;
#32179 = ADVANCED_FACE ( 'NONE', ( #32222 ), #41546, .F. ) ;
#32181 = VERTEX_POINT ( 'NONE', #12298 ) ;
#32180 = CARTESIAN_POINT ( 'NONE',  ( -2.229367062500000163, 8.270833334698926009, -3.861377020970580443 ) ) ;
#32182 = CARTESIAN_POINT ( 'NONE',  ( 1.339745962155612702, -34.16965819600732601, -5.000000000000000000 ) ) ;
#32183 = CARTESIAN_POINT ( 'NONE',  ( 1.060575238724906964E-15, -55.74999999999999289, 5.773502691896257311 ) ) ;
#32184 = CARTESIAN_POINT ( 'NONE',  ( -1.846868145590737420, -160.0000000013656063, 4.458734124999999437 ) ) ;
#32185 = CARTESIAN_POINT ( 'NONE',  ( -2.229367062500000163, -36.72916666530107221, -3.861377020970580443 ) ) ;
#32186 = CARTESIAN_POINT ( 'NONE',  ( -6.972266317189433020E-16, -87.25000000000001421, -5.000000000000000000 ) ) ;
#32187 = CARTESIAN_POINT ( 'NONE',  ( -4.458734124999998549, -80.22916666530106511, 2.574251347313722516 ) ) ;
#32188 =( BOUNDED_CURVE ( )  B_SPLINE_CURVE ( 2, ( #40617, #16179, #35804, #11345, #50593, #26147, #1722, #41240, #11657 ),
 .UNSPECIFIED., .F., .F. ) 
 B_SPLINE_CURVE_WITH_KNOTS ( ( 3, 2, 2, 2, 3 ),
 ( 0.3946428571428571286, 0.3952380952380952217, 0.3964285714285714080, 0.3976190476190475942, 0.3982142857142857428 ),
 .UNSPECIFIED. ) 
 CURVE ( )  GEOMETRIC_REPRESENTATION_ITEM ( )  RATIONAL_B_SPLINE_CURVE ( ( 0.9330127018922194093, 0.9330127018922194093, 1.000000000000000000, 0.8660254037844387076, 1.000000000000000000, 0.8660254037844387076, 1.000000000000000000, 0.9330127018922163007, 0.9330127018922194093 ) ) 
 REPRESENTATION_ITEM ( '' )  );
#32189 = CARTESIAN_POINT ( 'NONE',  ( -2.071067811865475061, -167.6875000000000000, -5.000000000000000888 ) ) ;
#32190 = CARTESIAN_POINT ( 'NONE',  ( -4.458734124999999437, -89.39583333196773651, -2.574251347313719407 ) ) ;
#32191 = CARTESIAN_POINT ( 'NONE',  ( -58.39396692619412477, -130.6875000013656063, 2.891590998281057701 ) ) ;
#32192 = CARTESIAN_POINT ( 'NONE',  ( 9.457646018065525792E-16, -1.312499998634405918, 5.148502694627439702 ) ) ;
#32193 = EDGE_CURVE ( 'NONE', #40991, #13039, #31914, .T. ) ;
#32194 = CARTESIAN_POINT ( 'NONE',  ( 4.458734125000001214, -33.14583333196774362, 2.574251347313718519 ) ) ;
#32195 = VECTOR ( 'NONE', #5710, 1000.000000000000000 ) ;
#32196 = CYLINDRICAL_SURFACE ( 'NONE', #16369, 5.000000000000000000 ) ;
#32197 = CARTESIAN_POINT ( 'NONE',  ( -4.458734124999998549, -84.47916666530107932, 2.574251347313722516 ) ) ;
#32198 = CARTESIAN_POINT ( 'NONE',  ( 1.975475456537005874E-15, -54.62499999726880873, 5.000000000000000000 ) ) ;
#32199 = VERTEX_POINT ( 'NONE', #37373 ) ;
#32200 = CARTESIAN_POINT ( 'NONE',  ( -51.75738570946856498, -153.8750000027312126, 3.805975901505576964 ) ) ;
#32201 = CARTESIAN_POINT ( 'NONE',  ( -1.339745962155613812, -19.08034179853029144, -5.000000000000000000 ) ) ;
#32202 = CARTESIAN_POINT ( 'NONE',  ( -3.152548672688508926E-16, -67.81249999863440792, -5.148502694627439702 ) ) ;
#32203 = CARTESIAN_POINT ( 'NONE',  ( -4.458734124999999437, -41.31249999863440081, 0.000000000000000000 ) ) ;
#32204 = CARTESIAN_POINT ( 'NONE',  ( 2.229367062500001939, -10.22916666530106866, 3.861377020970579999 ) ) ;
#32205 = EDGE_LOOP ( 'NONE', ( #63203, #53208, #39087, #12096 ) ) ;
#32206 = CARTESIAN_POINT ( 'NONE',  ( 0.000000000000000000, -120.0000000000000000, 5.000000000000000000 ) ) ;
#32207 = CARTESIAN_POINT ( 'NONE',  ( -5.000000000000000000, -146.6250000027312126, -6.123233995736766282E-16 ) ) ;
#32208 = EDGE_CURVE ( 'NONE', #24763, #12275, #41230, .T. ) ;
#32209 = CARTESIAN_POINT ( 'NONE',  ( -4.458734124999999437, -4.645833331967739177, -2.574251347313719407 ) ) ;
#32210 = CARTESIAN_POINT ( 'NONE',  ( 2.229367062499998831, 4.354166668032260823, -3.861377020970580887 ) ) ;
#32211 = CARTESIAN_POINT ( 'NONE',  ( -5.000000000000000000, -32.87499999726880873, 0.000000000000000000 ) ) ;
#32212 = CARTESIAN_POINT ( 'NONE',  ( -8.190561711645485556E-16, -155.6875000013655779, 4.458734124999999437 ) ) ;
#32213 = CARTESIAN_POINT ( 'NONE',  ( -2.229367062499996610, 28.60416666803226349, 3.861377020970582219 ) ) ;
#32214 = VERTEX_POINT ( 'NONE', #7796 ) ;
#32215 = CARTESIAN_POINT ( 'NONE',  ( 2.229367062499998831, -86.64583333196773651, -3.861377020970580887 ) ) ;
#32216 = CARTESIAN_POINT ( 'NONE',  ( 1.975475456537005874E-15, -24.74999999999999645, 5.000000000000000000 ) ) ;
#32217 = CARTESIAN_POINT ( 'NONE',  ( -3.152548672688508926E-16, -10.56249999863440792, -5.148502694627439702 ) ) ;
#32218 = DIRECTION ( 'NONE',  ( -0.000000000000000000, 1.000000000000000000, -0.000000000000000000 ) ) ;
#32219 = CARTESIAN_POINT ( 'NONE',  ( -6.972266317189433020E-16, -23.12499999726880873, -5.000000000000000000 ) ) ;
#32220 = CARTESIAN_POINT ( 'NONE',  ( -6.972266317189433020E-16, -67.25000000000000000, -5.000000000000000000 ) ) ;
#32221 = CARTESIAN_POINT ( 'NONE',  ( -4.999999999999999112, -33.79166666393547303, 2.886751345948131764 ) ) ;
#32222 = FACE_OUTER_BOUND ( 'NONE', #10822, .T. ) ;
#32223 = CARTESIAN_POINT ( 'NONE',  ( 4.458734124999999437, 26.18750000136559564, -5.460374474430324690E-16 ) ) ;
#32224 = CARTESIAN_POINT ( 'NONE',  ( -4.999999999999998224, -3.916666666666665630, 2.886751345948131764 ) ) ;
#32225 = CARTESIAN_POINT ( 'NONE',  ( 4.458734124999998549, 21.27083333469892779, -2.574251347313721627 ) ) ;
#32226 = CARTESIAN_POINT ( 'NONE',  ( 4.458734124999999437, -57.81249999863440081, -5.460374474430324690E-16 ) ) ;
#32227 = CARTESIAN_POINT ( 'NONE',  ( 4.458734125000000326, -2.145833331967737845, 2.574251347313718519 ) ) ;
#32228 = CARTESIAN_POINT ( 'NONE',  ( 1.975475456537005874E-15, 9.375000002731185944, 5.000000000000000000 ) ) ;
#32229 = CARTESIAN_POINT ( 'NONE',  ( -3.535250795749689387E-16, 15.75000000000000178, -5.773502691896257311 ) ) ;
#32230 = CARTESIAN_POINT ( 'NONE',  ( -9.184850993605147944E-16, -143.3750000027312126, 5.000000000000000000 ) ) ;
#32231 = DIRECTION ( 'NONE',  ( 0.000000000000000000, 0.000000000000000000, 1.000000000000000000 ) ) ;
#32232 = CARTESIAN_POINT ( 'NONE',  ( -4.458734124999998549, -47.22916666530106511, 2.574251347313722516 ) ) ;
#32233 = CARTESIAN_POINT ( 'NONE',  ( 5.000000000000000000, -79.29166666393548724, -2.886751345948129988 ) ) ;
#32234 = ADVANCED_FACE ( 'NONE', ( #46707 ), #31267, .T. ) ;
#32235 = CARTESIAN_POINT ( 'NONE',  ( -51.60603307380591787, -139.1875000013656347, -2.891590998281053704 ) ) ;
#32236 = VECTOR ( 'NONE', #54610, 1000.000000000000000 ) ;
#32237 = CARTESIAN_POINT ( 'NONE',  ( 1.339745962155612702, -37.16965819600733312, -5.000000000000000000 ) ) ;
#32238 = EDGE_CURVE ( 'NONE', #4573, #31397, #56693, .T. ) ;
#32239 = CARTESIAN_POINT ( 'NONE',  ( 5.000000000000000000, -36.50000000000000711, -6.123233995736766282E-16 ) ) ;
#32240 = ADVANCED_FACE ( 'NONE', ( #52169 ), #16802, .T. ) ;
#32241 = CARTESIAN_POINT ( 'NONE',  ( -2.229367062500000163, -83.72916666530106511, -3.861377020970580443 ) ) ;
#32242 = CARTESIAN_POINT ( 'NONE',  ( -1.846868145590737420, -157.0000000013655779, 4.458734124999997661 ) ) ;
#32243 = CARTESIAN_POINT ( 'NONE',  ( -5.000000000000000000, -31.00000000000000000, 0.000000000000000000 ) ) ;
#32244 = CARTESIAN_POINT ( 'NONE',  ( -5.000000000000000000, 23.91666666666666785, -2.886751345948128211 ) ) ;
#32245 = EDGE_LOOP ( 'NONE', ( #2813, #15487, #41669, #33869 ) ) ;
#32246 = CARTESIAN_POINT ( 'NONE',  ( 4.458734124999999437, 19.93750000136559208, -5.460374474430324690E-16 ) ) ;
#32247 = ORIENTED_EDGE ( 'NONE', *, *, #46960, .T. ) ;
#32248 = CARTESIAN_POINT ( 'NONE',  ( 4.458734125000001214, -93.89583333196772230, 2.574251347313718519 ) ) ;
#32249 = CARTESIAN_POINT ( 'NONE',  ( 4.458734124999999437, 13.93750000136559386, -5.460374474430324690E-16 ) ) ;
#32250 = CARTESIAN_POINT ( 'NONE',  ( 2.500000000000002220, 16.45833333606451987, 4.330127018922192761 ) ) ;
#32251 = CARTESIAN_POINT ( 'NONE',  ( -4.999999999999998224, -28.79166666393548013, 2.886751345948131764 ) ) ;
#32252 = CARTESIAN_POINT ( 'NONE',  ( 5.000000000000000000, 9.583333333333333925, -2.886751345948129988 ) ) ;
#32253 = CARTESIAN_POINT ( 'NONE',  ( -4.458734124999999437, -57.39583333196773651, -2.574251347313719407 ) ) ;
#32254 = CARTESIAN_POINT ( 'NONE',  ( -2.499999999999996447, -52.70833333060213732, 4.330127018922195425 ) ) ;
#32255 = CARTESIAN_POINT ( 'NONE',  ( 2.500000000000002220, -79.66666666666665719, 4.330127018922192761 ) ) ;
#32256 = DIRECTION ( 'NONE',  ( 0.000000000000000000, 0.000000000000000000, 1.000000000000000000 ) ) ;
#32257 = CARTESIAN_POINT ( 'NONE',  ( 2.500000000000002220, -40.54166666393548013, 4.330127018922192761 ) ) ;
#32258 = DIRECTION ( 'NONE',  ( 0.000000000000000000, 0.000000000000000000, 1.000000000000000000 ) ) ;
#32259 = ADVANCED_FACE ( 'NONE', ( #42506 ), #16487, .T. ) ;
#32260 = CARTESIAN_POINT ( 'NONE',  ( -2.071067811865686448, -151.8125000027311842, -4.999999999999789502 ) ) ;
#32261 = CARTESIAN_POINT ( 'NONE',  ( -2.500000000000000444, -41.16666666666667140, -4.330127018922193649 ) ) ;
#32262 = CARTESIAN_POINT ( 'NONE',  ( 1.339745962155615144, -96.70534180126146850, 4.999999999999999112 ) ) ;
#32264 = CARTESIAN_POINT ( 'NONE',  ( -2.229367062500000163, -18.72916666530106866, -3.861377020970580443 ) ) ;
#32263 = CARTESIAN_POINT ( 'NONE',  ( -4.999999999999998224, 14.08333333333333393, 2.886751345948131764 ) ) ;
#32265 = DIRECTION ( 'NONE',  ( 0.000000000000000000, 0.000000000000000000, 1.000000000000000000 ) ) ;
#32266 = CARTESIAN_POINT ( 'NONE',  ( -4.458734124999999437, -62.31249999863440792, 0.000000000000000000 ) ) ;
#32267 = CARTESIAN_POINT ( 'NONE',  ( -4.458734124999999437, -149.1875000013656063, -5.460374474430324690E-16 ) ) ;
#32268 =( REPRESENTATION_RELATIONSHIP ('NONE','NONE', #27855, #14320 ) REPRESENTATION_RELATIONSHIP_WITH_TRANSFORMATION ( #53944 )SHAPE_REPRESENTATION_RELATIONSHIP( ) );
#32269 = CARTESIAN_POINT ( 'NONE',  ( 4.458734124999999437, -73.81249999863440792, -5.460374474430324690E-16 ) ) ;
#32270 = CARTESIAN_POINT ( 'NONE',  ( -58.39396692619412477, -144.6875000013656063, 2.891590998281057701 ) ) ;
#32271 =( BOUNDED_SURFACE ( )  B_SPLINE_SURFACE ( 1, 2, ( 
 ( #63380, #59180, #43737, #49523, #19295, #34731, #59505, #34398, #54358, #29893, #5464, #54673, #20262, #10597, #38913, #45020, #987, #57377, #10919, #55325, #16070, #30537, #40823, #6433, #41138, #35698, #36013, #11240, #1308, #40196, #50158, #6745, #21858, #21542, #20904, #59832, #26044, #6113, #15754, #55645, #21215, #25728, #16394, #45339, #41453, #40507, #30864, #31178, #45659, #26353, #54993, #50493, #60469, #60149, #45975, #11559, #50808, #1940, #60786, #1616, #16711, #36327, #55955, #35370, #11869, #31485, #51130, #7065, #26678, #46297, #2254, #61102, #34294, #24653, #49088, #20150, #54882, #14673, #24336, #39118, #53916, #49731, #44259, #53606, #15645, #10812, #63584, #19821, #49412, #59716, #58745, #19505, #15322, #4711, #5356, #5034, #9540, #30100, #40073, #44582, #39747, #9842, #25611, #29144, #48766, #10177, #29457, #5676, #43937, #54236, #223, #39430, #59071, #54565, #868, #14996, #45225, #25287, #44912, #34609, #20471, #539, #29780, #24975, #59389, #35261, #30424, #50051, #40394, #34946, #10487, #6009, #1192, #20792, #60035, #33986, #21105, #46508, #56162, #41656, #6959, #2453, #6632, #31065, #16283, #51657, #61307, #41031, #16600, #51014, #16913, #26568, #40710, #15960, #26891, #36530, #50373, #46820, #12084, #31707, #27202, #7280, #11446, #36857, #22064, #11758, #17232, #32020, #56486, #7594, #12408, #60677, #45544, #2764, #22386, #21428, #46187, #51341, #41987, #35582, #55209, #50689, #55842, #2147, #21752, #41347, #60993, #11126, #35901, #30753, #6320, #26241, #25925, #1504, #55536, #60359, #45861, #31376, #1827, #36218, #4330, #8843, #27826, #18793, #8222, #38418, #56803, #38120, #58044, #13038, #13354, #52597, #47449, #28456, #3401, #47141, #23330, #37179, #23017, #17561, #61944, #43240, #13974, #52284, #32341, #62577, #57122, #57434, #27511, #48072, #23948, #42620, #28141, #57743, #33601, #4026, #62881, #32657, #37806, #32977, #47758, #3714, #8531, #53221, #17863, #42934, #13668, #62258, #9153, #23645, #37484, #61626, #12721, #18498, #28765, #33288, #51967, #48388, #18177, #7906, #52907, #3088, #22706, #42304, #38734, #19442, #59001, #33612, #9469, #9781, #43559, #39370, #4968, #24590, #14929, #34536, #4645, #63204, #9162, #162, #40007, #53544, #54172, #20080, #49670, #44197, #19759, #10111, #43872, #14299, #24266, #29078, #29716, #34882, #58372, #4337, #19115, #33919, #49349, #63518, #53230, #59324, #54504, #48705, #39055, #29387, #39685, #58683, #14612, #5294, #48395, #49023, #34225, #28778, #24912, #15257, #44516, #10428, #53852, #478, #30041, #802, #13982, #5613, #23955, #25227, #44838, #20408, #27367, #10752, #30362, #35519, #12892, #37035, #51516, #55142, #45162, #36717, #32511, #47001, #59977, #1447, #56661, #2949, #47315, #1130, #7453, #54821, #51822, #25544, #31882, #61800, #11068, #61489, #17421, #50309, #12270, #56348, #20731, #21921, #41842, #15586, #30692, #27061, #40335, #22243, #46679, #2625, #12579, #32192, #6258, #15900, #49984, #7764, #22879, #25867, #22566, #42164, #52143, #17726, #37342, #56975, #45482, #41519, #61171, #17094, #8085, #27689, #3267, #5938, #59654, #35204, #58217, #33156, #62114, #24126, #63372, #8400, #28312, #57916, #4498, #3573, #28000, #23812, #13213, #13837, #57609, #18032, #38585, #48559, #53076, #38903, #62746, #38289, #43105, #29245, #4817, #9322, #32835, #43727, #37978, #43415, #28935, #57297, #52464, #18353, #58538, #18970, #33457, #13536, #47619, #18667, #14460, #19287, #42792, #47928, #14145, #34082, #48870, #23181, #9015, #37655, #33771, #62435, #28626, #53705, #52770, #63058, #53391, #8699, #9637, #48243, #3883, #23502, #42473, #4199, #60140, #34392, #34721, #59172, #14773, #59496, #5453, #54983, #15105, #10589, #10280, #44359, #24437, #54018, #45012, #35689, #15745, #24755, #50485, #49515, #58844, #44040, #15435, #25071, #39219, #39853, #19607, #20252, #322, #25392, #30527, #16060, #35053, #54665, #30200, #54350, #19920, #29885, #39534, #49829, #45330, #5138, #9951, #29567, #44681, #40188, #642, #5, #6105, #1300, #49198, #5773, #978, #50150, #20581, #59824, #35361, #10912, #25720, #20896, #40498, #55317, #11231, #30856, #2871, #26668, #2245, #7056, #56897, #32438, #36955, #40813, #7693, #1928, #51437, #56584, #21207, #60460, #45966, #22488, #46605, #61094, #21533, #55636, #46288, #42084, #12503, #6736, #11861, #2550, #32115, #12817, #11551, #17018, #1608, #61411, #36005, #41445, #27299, #41130, #7378, #26986, #60777, #46924, #21849, #26345, #16386, #61726, #36633, #17655, #31169, #16702, #36320, #50800, #56266, #51119, #51751, #55947, #12189, #31477, #31804, #6424, #22165, #41761, #37270, #17334, #26036, #45650, #13456, #22803, #8007, #43032, #52690, #3186, #3807, #47241, #47849, #23431, #62672, #13138, #57532, #33382, #27610, #47543, #18593, #17954, #13760, #38219, #57841, #52998, #8937, #42711, #37578, #42397, #28551, #14385, #37902, #57218, #48170, #62037, #33077, #32757, #52385, #33697, #48486, #62353, #8322, #4123, #3494, #23745, #43338, #27922, #43649, #23107, #18277, #28235, #8625, #62982, #18896, #38510, #58138, #14069, #53315, #9249, #28864, #4422, #63289, #24048, #19207, #38823, #58462, #52067, #34635, #9870, #563, #20496, #15664, #44933, #40414, #59416, #9563, #54262, #5058, #40095, #48793, #890, #39143, #59738, #10508, #35282, #24995, #54903, #24678, #49114, #34316, #6029, #10831, #59094, #10201, #5378, #34970, #44603, #58769, #34009, #30445, #54586, #4735, #1214, #30122, #49752, #45246, #25312, #29480, #50072, #25632, #29802, #20811, #60054, #53632, #29169, #24360, #15020, #63609, #43962, #19528, #39459, #20172, #5697, #14699, #53940, #44285, #247, #49436, #39768, #15346, #19844, #6977, #61328, #16303, #26588, #12102, #50710, #27219, #2470, #35925, #42003, #55228, #55864, #56504, #31395, #22405, #26909, #45883, #36874, #26259, #21451, #15977, #36549, #55554, #31087, #51034, #46205, #1845, #46528, #35604, #11151, #11777, #11466, #51358, #30772, #36236, #6653, #41050, #60697, #56181, #22080, #16617, #7614, #7298, #31728, #2166, #41677, #21772, #41365, #61009, #16935, #17250, #12426, #32037, #50393, #51673, #6342, #46836, #2784, #25949, #45564, #1522, #21126, #40732, #60379, #23663, #52612, #28476, #52306, #13056, #61959, #33621, #43259, #23033, #62278, #32995, #62595, #8547, #22722, #61644, #8860, #18515, #32360, #28788, #38137, #57762, #9175, #52923, #57139, #18813, #4046, #57451, #62899, #13993, #48090, #53240, #38435, #42636, #27529, #58062, #4346, #3417, #28160, #13685, #48404, #23965, #17577, #32673, #37821, #47775, #3730, #23352, #42952, #37195, #17881, #33304, #56820, #8240, #12737, #51982, #37501, #7924, #47160, #13374, #3105, #42320, #27842, #47464, #18200, #811, #53860, #49033, #43568, #487, #43881, #58693, #59010, #34547, #9790, #10437, #29398, #29086, #5303, #19126, #4977, #63213, #63529, #25236, #40019, #34234, #14310, #44527, #39065, #39379, #49358, #19451, #35212, #14938, #20089, #54181, #4655, #38745, #54514, #39694, #33931, #10761, #59334, #15267, #54830, #34892, #14622, #20418, #49679, #10120, #5624, #59663, #30050, #15595, #44848, #24600, #9478, #30372, #49994, #44206, #29727, #5947, #58382, #53554, #48715, #171, #19770, #24921, #24277, #11708, #16546, #7227, #25876, #36169, #21701, #60303, #36803, #12028, #45492, #51606, #1140, #1773, #2400, #40983, #31970, #36482, #55478, #46455, #35852, #31012, #25553, #46132, #1455, #40663, #60627, #55790, #11392, #56107, #50641, #31327, #50320, #50962, #6903, #26516, #16232, #11077, #20740, #2100, #45173, #21056, #41292, #31656, #61255, #60941, #16859, #51292, #6579, #26194, #45813, #21375, #26841, #22010, #6269, #15909, #30699, #41603, #17178, #56435, #40343, #12357, #59986, #55153, #35529, #22966, #33236, #32284, #56748, #52547, #41932, #42563, #22654, #46766, #3659, #13618, #18122, #3972, #27773, #3349, #8172, #57996, #33548, #38062, #61574, #8788, #3035, #8479, #57691, #22331, #17509, #47087, #28088, #52855, #42252, #62829, #42876, #23273, #37435, #62522, #37747, #47398, #61893, #57379, #28400, #48021, #18440, #13923, #32924, #2711, #62206, #17809, #23592, #37128, #43188, #12672, #18745, #47705, #38370, #13299, #7538, #57067, #12979, #7852, #27150, #51912, #32602, #27455, #52227, #54104, #24527, #14233, #53166, #412, #10043, #23896, #20341, #29657, #49288, #730, #44452, #48642, #10366, #59259, #48955, #15190, #5544, #20014, #25156, #54438, #34165, #19055, #39620, #59588, #58626, #19696, #5226, #29975, #34815, #49602, #4583, #29325, #44130, #39306, #58933, #97, #44770, #53479, #14860, #24845, #24207, #39941, #15522, #9408, #9102, #28710, #4907, #48333, #34472, #4278, #43499, #19377, #63143, #63458, #14546, #38673, #58311, #29017, #43813, #33859, #38991, #53787, #9720, #50564, #16784, #6507, #10681, #40584, #54756, #35449, #36401, #31575, #25804, #5867, #36087, #30618, #30938, #40900, #10996, #26758, #30295, #49913, #11312, #55075, #6826, #25474, #55396, #50240, #6190, #45416, #26119, #60545, #1383, #46375, #45097, #1062, #45739, #20983, #26432, #20669, #1692, #60228, #16148, #35773, #55716, #2015, #21295, #2323, #46053, #31249, #16467, #50883, #11629, #21618, #41212, #60857, #56031, #11948, #51209, #41529, #7143, #40275, #21929, #61179, #35141, #59913, #15834, #22253, #47627, #57305, #42803, #8093, #3583, #7772, #32202, #17429, #52780, #62444, #42172, #17735, #52151, #18040, #27697, #41850, #17102, #28010, #37663, #51525, #47940, #13222, #32844, #28323, #8408, #12589, #37986, #23190, #12899, #18362, #33166, #57618, #8709, #13545, #61809, #46686, #3893, #23513, #22575, #47325, #52472, #43114, #36726, #56358, #51831, #56983, #3276, #22887, #42484, #62123, #12278, #37044, #31893, #7462, #27376, #27070, #2633, #56671, #61498, #47009, #32522, #2958, #37353, #6354, #10839, #29813, #20823, #10210, #5387, #62755, #20506, #63070, #15030, #15355, #54595, #49445, #34646, #34980, #45258, #10517, #38300, #25002, #18675, #18983, #1224, #60064, #54270, #33467, #899, #59103, #35292, #59748, #44612, #15673, #30131, #572, #38595, #49760, #50080, #40424, #30455, #25958, #25321, #57928, #20181, #39779, #6037, #13846, #25642, #4210, #15988, #40105, #35613, #5706, #55239, #59426, #44941, #54912, #11161, #30783, #50406, #53090, #9026, #28636, #48253, #23822, #43427, #56513, #2478, #16314, #12748, #22091, #41690, #56830, #36883, #41060, #2795, #51682, #41374, #7623, #61653, #12434, #17587, #46848, #26598, #11478, #32046, #51992, #51043, #12110, #61337, #22414, #27227, #42013, #60707, #21782, #16946, #31737, #51367, #36559, #37204, #45892, #56190, #17260, #16627, #32368, #7936, #1854, #45575, #21136, #61020, #1531, #7308, #40741, #60388, #11787, #35935, #55875, #6986, #55563, #31098, #21460, #36248, #26921, #46537, #31405, #46214, #50719, #6663, #26270, #2177, #33003, #47170, #27851, #9182, #23974, #18208, #61969, #28483, #23042, #23360, #33311, #3426, #19134, #3113, #22731, #3739, #47472, #62909, #42329, #47782, #42645, #62286, #37829, #48099, #58068, #57463, #38751, #42959, #4354, #62602, #33938, #38441, #13382, #48410, #52620, #8554, #27538, #4053, #28167, #18525, #38145, #57770, #13692, #52931, #8868, #28794, #23671, #17890, #43269, #37510, #18822, #43576, #63219, #14000, #57150, #33627, #53246, #58390, #14316, #53559, #13065, #32685, #52316, #8251, #29405, #44855, #48722, #29733, #24606, #49038, #44212, #30055, #40023, #177, #1144, #818, #5629, #39385, #25240, #20095, #10126, #4983, #39701, #59667, #54836, #20423, #15913, #34896, #4662 ),
 ( #10441, #19777, #10766, #49365, #59016, #43887, #45178, #5309, #20744, #19458, #14947, #34557, #63535, #44535, #54188, #15598, #24927, #59341, #492, #15272, #9484, #39072, #49684, #40348, #35216, #9797, #35534, #54518, #30377, #58700, #50000, #25561, #5951, #59990, #29095, #24284, #14628, #34241, #53870, #46138, #50328, #46459, #21061, #26520, #56439, #31017, #56111, #12035, #45818, #12361, #55796, #11399, #25880, #27155, #31331, #46771, #1460, #1780, #26198, #45496, #2104, #36175, #22015, #21380, #41297, #40987, #50645, #55162, #40666, #31660, #2717, #2403, #55483, #17513, #16551, #60310, #11081, #21705, #11713, #6274, #6909, #16238, #50966, #60946, #16867, #35857, #60631, #36485, #30703, #6583, #51296, #7232, #26846, #41609, #61259, #17183, #36809, #31975, #51610, #7543, #22339, #41937, #61578, #38069, #43193, #9107, #28093, #47711, #3666, #3353, #37440, #27778, #52234, #23279, #58001, #17815, #27463, #42256, #57071, #52861, #47402, #56753, #18750, #13927, #3040, #22970, #52552, #62835, #61897, #22658, #18446, #7857, #8484, #8176, #12676, #33241, #38374, #42882, #33552, #57385, #32929, #37753, #23903, #63148, #3976, #47092, #53173, #32608, #57697, #23596, #51916, #12983, #42570, #28714, #13623, #48337, #4284, #43503, #62210, #13306, #62527, #8794, #28406, #48026, #37133, #18126, #32290, #15196, #53793, #30300, #5549, #19383, #45102, #58316, #58939, #59593, #34477, #25481, #29981, #48960, #39945, #29330, #24532, #19059, #39626, #38999, #34170, #54109, #10049, #4912, #9727, #29662, #737, #49293, #14241, #44135, #38677, #58631, #20346, #15526, #105, #53484, #20020, #14551, #14868, #24853, #19701, #10690, #33864, #9412, #5233, #39311, #54444, #29023, #44457, #417, #59264, #34821, #10372, #49610, #25161, #49920, #44775, #35146, #54762, #5873, #48647, #4589, #24212, #43818, #63464, #46384, #11956, #7468, #26440, #40280, #21304, #35782, #51217, #15840, #31583, #6194, #7154, #41219, #26764, #55723, #2330, #55404, #16155, #1387, #36732, #21937, #26126, #1700, #36095, #2022, #11636, #25809, #1067, #41535, #21626, #35459, #31902, #60866, #16792, #12286, #56040, #60237, #61187, #17109, #60553, #56364, #51531, #27077, #20674, #59919, #45746, #30624, #55080, #11002, #6514, #31257, #36410, #50891, #30945, #20988, #11320, #50571, #6833, #50246, #45422, #40591, #40908, #16474, #46062, #37362, #2641, #28332, #3900, #12597, #32530, #62130, #8718, #7782, #32210, #28017, #17436, #18048, #61820, #22260, #42809, #52786, #57312, #43120, #3282, #42493, #47332, #33475, #9031, #13552, #37052, #47946, #42180, #47636, #33172, #61506, #56681, #22583, #62760, #23196, #37670, #17745, #51839, #22898, #18680, #23519, #47017, #52158, #62449, #38306, #53097, #27385, #13229, #41859, #37992, #2967, #32852, #57933, #56992, #3591, #18371, #12907, #13852, #52480, #8101, #27705, #46694, #8415, #57624, #38602, #38920, #63388, #18987, #24, #9652, #59192, #19306, #14793, #14475, #48575, #28643, #58235, #49215, #39869, #19939, #28952, #54685, #53721, #63077, #48258, #19625, #29261, #43432, #44060, #23829, #24453, #39235, #58861, #53406, #34096, #9972, #4216, #24141, #4515, #43744, #34405, #9338, #54034, #29583, #5155, #58555, #14162, #33790, #24775, #48889, #4834, #44378, #34741, #661, #339, #39551, #15122, #5473, #54369, #35068, #10296, #29904, #49532, #25088, #44697, #20270, #59516, #15451, #30544, #55332, #30873, #25736, #50168, #11249, #26365, #50501, #30221, #20912, #49846, #35380, #45985, #41147, #6123, #25409, #21227, #10929, #35705, #45667, #45350, #16720, #5792, #45029, #16081, #55001, #36021, #996, #60159, #1317, #40517, #6444, #40833, #31187, #26053, #60794, #55653, #60478, #1626, #16403, #11567, #50816, #6753, #1950, #21551, #36336, #55967, #11878, #31497, #20600, #10607, #40204, #59840, #15765, #34958, #9553, #54575, #44593, #30112, #59084, #10497, #58759, #19518, #4724, #40083, #49742, #29469, #5048, #39447, #5368, #15010, #29158, #4412, #15335, #24986, #38810, #35272, #553, #20162, #15654, #59403, #63598, #25302, #5686, #236, #44923, #20485, #878, #59727, #54894, #49102, #33999, #10823, #30435, #9859, #34624, #39758, #24036, #43638, #63280, #39132, #44274, #54249, #10191, #29791, #49424, #19197, #24350, #58452, #14375, #14689, #53622, #48782, #43950, #34307, #53930, #19834, #24666, #61002, #16294, #7291, #60371, #55546, #50064, #6969, #50385, #1514, #1837, #41043, #35917, #21117, #21439, #31718, #60690, #25624, #11457, #6019, #6333, #51352, #46521, #40724, #20803, #51027, #45556, #45874, #55856, #25937, #41670, #45238, #1203, #26251, #31079, #21765, #40406, #6644, #50701, #16610, #36229, #26579, #16926, #11769, #61319, #41358, #46198, #31388, #2158, #36541, #56174, #12095, #26901, #2463, #22074, #17243, #56497, #36867, #60045, #12418, #15969, #35596, #55220, #11140, #30764, #62585, #8540, #57753, #23026, #18508, #22716, #47151, #32354, #4036, #13677, #57134, #32667, #3410, #32987, #42629, #56813, #32031, #42944, #52606, #2778, #62890, #28152, #47767, #43249, #23343, #27523, #52914, #38129, #27836, #33296, #48081, #8851, #23655, #28468, #13050, #61638, #18803, #38426, #37493, #62268, #3722, #58052, #51666, #7608, #3099, #8233, #18193, #37815, #57443, #13366, #27213, #51976, #46830, #22397, #42313, #41997, #17570, #7917, #37189, #12730, #47458, #61953, #17874, #52297, #42538, #62176, #53453, #38650, #18416, #3326, #4257, #43788, #42854, #3947, #33527, #14207, #43477, #58288, #52523, #13595, #8766, #23570, #43165, #28374, #19033, #37720, #47995, #53142, #8458, #48618, #23872, #57355, #63435, #12954, #33214, #33836, #52832, #37406, #48306, #3633, #9384, #47682, #62498, #57041, #57974, #13274, #28065, #62804, #18724, #23244, #38037, #38348, #28994, #13900, #32578, #57669, #52200, #32898, #4557, #24182, #9077, #8147, #28686, #63122, #27747, #47376, #22944, #18096, #38964, #58602, #59232, #39280, #54732, #14520, #39596, #34449, #58908, #54081, #39915, #49889, #10019, #10972, #10653, #15495, #49264, #35118, #29950, #19988, #14835, #49575, #5840, #1039, #30269, #25781, #44743, #34142, #15165, #29630, #25452, #53761, #45072, #24502, #20645, #59563, #40249, #10341, #59889, #5201, #24819, #19669, #55049, #15809, #44425, #34789, #54411, #20314, #5518, #44105, #19350, #35425, #30593, #9695, #50214, #6164, #45392, #29302, #48932, #385, #4880, #25131, #69, #704, #60204, #60835, #16761, #36378, #26095, #6802, #46349, #20961, #60519, #21270, #16446, #11922, #45716, #56008, #26734, #2305, #55694, #50541, #16126, #51186, #27353, #40877, #21907, #7438, #37021, #31551, #7118, #41504, #31228, #1668, #11608, #36065, #61157, #22228, #50858, #55374, #6485, #26410, #17080, #46028, #40561, #46665, #41828, #30915, #1991, #36699, #27047, #21595, #41190, #56334, #35748, #12254, #31868, #11289, #51501, #2610, #61472, #17406, #56648, #12564, #32176, #51808, #1357, #7750, #17713, #48228, #42457, #28299, #13825, #61786, #37328, #22866, #63046, #23489, #37962, #62100, #32497, #23167, #18956, #33444, #47299, #52450, #43091, #53061, #33757, #52129, #57596, #42150, #38276, #38572, #47912, #27672, #12879, #3869, #62732, #37640, #4185, #47605, #3253, #56959, #58203, #42776, #14130, #8071, #57283, #18017, #13199, #18340, #27986, #9001, #32821, #33142, #8385, #3559, #46986, #62421, #18654, #53375, #57901, #13524, #9309, #52757, #8686, #2935, #28612, #23799, #43401, #22548, #15417, #29231, #54970, #4485, #5122, #5759, #44345, #35349, #39839, #58829, #49814, #39205, #34377, #28923, #49500, #48857, #44026, #308, #19906, #14759, #63673, #39521, #10575, #59158, #24114, #54005, #48546, #4800, #30186, #25377, #19593, #63356, #29870, #24424, #24742, #34707, #9935, #20566, #43712, #19272, #15091, #29550, #627, #38888, #49184, #54332, #10266, #5439, #25057, #59482, #44667, #40171, #20237, #35039, #54651, #44999, #964, #59809, #15731, #58522, #14447, #34068, #53691, #9623, #36307, #50136, #31154, #45637, #61082, #25704, #41433, #16046, #17004, #51105, #36619, #1914, #56252, #1595, #26021, #11218, #46593, #12176, #35991, #11537, #45949, #11846, #21519, #35675, #10898, #21836, #31464, #45315, #41747, #7043, #26655, #22153, #2232, #6411, #31791, #51423, #7366, #55622, #55302, #30842, #26974, #2537, #50782, #40484, #61396, #17321, #16372, #41115, #46273, #36944, #30513, #6091, #21193, #6722, #60763, #16688, #55931, #1282, #20881, #50472, #60125, #40800, #60447, #26332, #56885, #18883, #17941, #27287, #12491, #47531, #57206, #7681, #8308, #51739, #52371, #27909, #3481, #17641, #62024, #37890, #32103, #52055, #12805, #7993, #23095, #37257, #42698, #18263, #57520, #47228, #42071, #46912, #62342, #56569, #32426, #13439, #62660, #28538, #33064, #52678, #8613, #22791, #27595, #3171, #42384, #28221, #13748, #37566, #2854, #61712, #13125, #47837, #32743, #22476, #38203, #33370, #3796, #23417, #43020, #18580, #57828, #52984, #8925, #48158, #4111, #23731, #43326, #62967, #45478, #49099, #35840, #58756, #34304, #39129, #26180, #1759, #6253, #9237, #40651, #33996, #19831, #25862, #53303, #28851, #14372, #55463, #15895, #29466, #53619, #24033, #14686, #11379, #1442, #38807, #43947, #35515, #21044, #45799, #43635, #5045, #33682, #30688, #30999, #39444, #19194, #4409, #59081, #55136, #29155, #60290, #53927, #58449, #48473, #50627, #9856, #6565, #63277, #48779, #9550, #4721, #24663, #19515, #16214, #24347, #44271, #63595, #233, #38498, #11063, #50304, #58126, #14057, #7524, #47386, #60925, #22315, #27439, #57053, #12343, #31954, #51586, #51276, #21686, #12012, #36465, #27135, #42237, #2080, #11692, #26502, #41276, #37115, #31641, #40965, #3022, #61879, #50947, #7209, #36787, #47073, #46117, #6888, #2695, #55775, #56420, #56092, #60613, #17493, #22638, #46750, #17795, #41589, #17163, #21996, #8159, #21361, #51897, #31311, #37419, #16844, #41916, #7838, #36155, #26821, #46440, #12964, #61559, #56733, #2386, #61241, #12653, #32589, #52212, #32269, #27758, #16532, #33845, #53774, #8468, #57984, #62188, #58299, #38975, #4267, #47693, #32911, #23884, #43487, #57680, #4569, #3958, #23257, #37731, #58612, #43175, #14533, #13285, #13606, #38047, #57364, #38358, #48005, #53464, #33223, #53152, #52842, #42864, #3337, #52534, #63132, #34152, #14218, #3645, #29311, #28386, #28076, #22953, #13909, #23579, #18109, #18733, #62509, #62816, #33537, #9088, #18426, #8776, #48317, #42549, #28697, #19043, #38660, #9394, #29004, #48629, #24192, #43799, #63446, #19363, #9706, #45085, #55061, #59575, #45404, #5529, #44755, #49587, #35760, #11301, #15822, #19680, #50228, #44437, #30281, #35435, #80, #39292, #24831, #1371, #25463, #39928, #398, #34460, #25144, #20972, #10985, #49276, #54424, #1051, #30605, #55384, #54091, #15508, #44116, #40261, #40573, #49901, #29642, #14848, #5855, #20657, #39608, #6176, #716, #5212, #58919, #60214, #20326, #16138, #10030, #59245, #20000, #15176, #35129, #29962, #25793, #34801, #54745, #10353, #10665, #48943, #59901, #4891, #24514, #22240, #31239, #56973, #56021, #1679, #50552, #21919, #31565, #45728, #46362, #26108, #26746, #2316, #41516, #55705, #36390, #12267, #6496, #26422, #50871, #46039, #61169, #11619, #17092, #56346, #31880, #21607, #16457, #21281, #36715, #30925, #6815, #51514, #37033, #2947, #7451, #27059, #46677, #60846, #2003, #41202, #16772, #2622, #51820, #11936, #40888, #36076, #51198, #41840, #7130, #60533, #12577, #7762, #61487, #17418, #56659, #32190, #27365, #46999, #22563, #42162, #61798, #17724, #37340, #27998, #62744, #33769, #57295 ) ),
 .UNSPECIFIED., .F., .F., .F. ) 
 B_SPLINE_SURFACE_WITH_KNOTS ( ( 2, 2 ),
 ( 3, 2, 2, 2, 2, 2, 2, 2, 2, 2, 2, 2, 2, 2, 2, 2, 2, 2, 2, 2, 2, 2, 2, 2, 2, 2, 2, 2, 2, 2, 2, 2, 2, 2, 2, 2, 2, 2, 2, 2, 2, 2, 2, 2, 2, 2, 2, 2, 2, 2, 2, 2, 2, 2, 2, 2, 2, 2, 2, 2, 2, 2, 2, 2, 2, 2, 2, 2, 2, 2, 2, 2, 2, 2, 2, 2, 2, 2, 2, 2, 2, 2, 2, 2, 2, 2, 2, 2, 2, 2, 2, 2, 2, 2, 2, 2, 2, 2, 2, 2, 2, 2, 2, 2, 2, 2, 2, 2, 2, 2, 2, 2, 2, 2, 2, 2, 2, 2, 2, 2, 2, 2, 2, 2, 2, 2, 2, 2, 2, 2, 2, 2, 2, 2, 2, 2, 2, 2, 2, 2, 2, 2, 2, 2, 2, 2, 2, 2, 2, 2, 2, 2, 2, 2, 2, 2, 2, 2, 2, 2, 2, 2, 2, 2, 2, 2, 2, 2, 2, 2, 2, 2, 2, 2, 2, 2, 2, 2, 2, 2, 2, 2, 2, 2, 2, 2, 2, 2, 2, 2, 2, 2, 2, 2, 2, 2, 2, 2, 2, 2, 2, 2, 2, 2, 2, 2, 2, 2, 2, 2, 2, 2, 2, 2, 2, 2, 2, 2, 2, 2, 2, 2, 2, 2, 2, 2, 2, 2, 2, 2, 2, 2, 2, 2, 2, 2, 2, 2, 2, 2, 2, 2, 2, 2, 2, 2, 2, 2, 2, 2, 2, 2, 2, 2, 2, 2, 2, 2, 2, 2, 2, 2, 2, 2, 2, 2, 2, 2, 2, 2, 2, 2, 2, 2, 2, 2, 2, 2, 2, 2, 2, 2, 2, 2, 2, 2, 2, 2, 2, 2, 2, 2, 2, 2, 2, 2, 2, 2, 2, 2, 2, 2, 2, 2, 2, 2, 2, 2, 2, 2, 2, 2, 2, 2, 2, 2, 2, 2, 2, 2, 2, 2, 2, 2, 2, 2, 2, 2, 2, 2, 2, 2, 2, 2, 2, 2, 2, 2, 2, 2, 2, 2, 2, 2, 2, 2, 2, 2, 2, 2, 2, 2, 2, 2, 2, 2, 2, 2, 2, 2, 2, 2, 2, 2, 2, 2, 2, 2, 2, 2, 2, 2, 2, 2, 2, 2, 2, 2, 2, 2, 2, 2, 2, 2, 2, 2, 2, 2, 2, 2, 2, 2, 2, 2, 2, 2, 2, 2, 2, 2, 2, 2, 2, 2, 2, 2, 2, 2, 2, 2, 2, 2, 2, 2, 2, 2, 2, 2, 2, 2, 2, 2, 2, 2, 2, 2, 2, 2, 2, 2, 2, 2, 2, 2, 2, 2, 2, 2, 2, 2, 2, 2, 2, 2, 2, 2, 2, 2, 2, 2, 2, 2, 2, 2, 2, 2, 2, 2, 2, 2, 2, 2, 2, 2, 2, 2, 2, 2, 2, 2, 2, 2, 2, 2, 2, 2, 2, 2, 2, 2, 2, 2, 2, 2, 2, 2, 2, 2, 2, 2, 2, 2, 2, 2, 2, 2, 2, 2, 2, 2, 2, 2, 2, 2, 2, 2, 2, 2, 2, 2, 2, 2, 2, 2, 2, 2, 2, 2, 2, 2, 2, 2, 2, 2, 2, 2, 2, 2, 2, 2, 2, 2, 2, 2, 2, 2, 2, 2, 2, 2, 2, 2, 2, 2, 2, 2, 2, 2, 2, 2, 2, 2, 2, 2, 2, 2, 2, 2, 2, 2, 2, 2, 2, 2, 2, 2, 2, 2, 2, 2, 2, 2, 2, 2, 2, 2, 2, 2, 2, 2, 2, 2, 2, 2, 2, 2, 2, 2, 2, 2, 2, 2, 2, 2, 2, 2, 2, 2, 2, 2, 2, 2, 2, 2, 2, 2, 2, 2, 2, 2, 2, 2, 2, 2, 2, 2, 2, 2, 2, 2, 2, 2, 2, 2, 2, 2, 2, 2, 2, 2, 2, 2, 2, 2, 2, 2, 2, 2, 2, 2, 2, 2, 2, 2, 2, 2, 2, 2, 2, 2, 2, 2, 2, 2, 2, 2, 2, 2, 2, 2, 2, 2, 2, 2, 2, 2, 2, 2, 2, 2, 2, 2, 2, 2, 2, 2, 2, 2, 2, 2, 2, 2, 2, 2, 2, 2, 2, 2, 2, 2, 2, 2, 2, 2, 2, 2, 2, 2, 2, 2, 2, 2, 2, 2, 2, 2, 2, 2, 2, 2, 2, 2, 2, 2, 2, 2, 2, 2, 2, 2, 3 ),
 ( 0.000000000000000000, 1.000000000000000000 ),
 ( 0.000000000000000000, 0.001388888888888888942, 0.002777777777777777884, 0.004166666666666666609, 0.005555555555555555768, 0.006944444444444444059, 0.008333333333333333218, 0.009722222222222222376, 0.01111111111111111154, 0.01250000000000000069, 0.01388888888888888812, 0.01527777777777777728, 0.01666666666666666644, 0.01805555555555555386, 0.01944444444444444475, 0.02083333333333333218, 0.02222222222222222307, 0.02361111111111111049, 0.02500000000000000139, 0.02638888888888888881, 0.02777777777777777624, 0.02916666666666666713, 0.03055555555555555455, 0.03194444444444444198, 0.03333333333333333287, 0.03472222222222222376, 0.03611111111111110772, 0.03749999999999999861, 0.03888888888888888951, 0.04027777777777778040, 0.04166666666666666435, 0.04305555555555555525, 0.04444444444444444614, 0.04583333333333333010, 0.04722222222222222099, 0.04861111111111111188, 0.05000000000000000278, 0.05138888888888888673, 0.05277777777777777762, 0.05416666666666666852, 0.05555555555555555247, 0.05694444444444444337, 0.05833333333333333426, 0.05972222222222222515, 0.06111111111111110911, 0.06250000000000000000, 0.06388888888888888395, 0.06527777777777778179, 0.06666666666666666574, 0.06805555555555554970, 0.06944444444444444753, 0.07083333333333333148, 0.07222222222222221544, 0.07361111111111111327, 0.07499999999999999722, 0.07638888888888889506, 0.07777777777777777901, 0.07916666666666666297, 0.08055555555555556080, 0.08194444444444444475, 0.08333333333333332871, 0.08472222222222222654, 0.08611111111111111049, 0.08749999999999999445, 0.08888888888888889228, 0.09027777777777777624, 0.09166666666666666019, 0.09305555555555555802, 0.09444444444444444198, 0.09583333333333333981, 0.09722222222222222376, 0.09861111111111110772, 0.1000000000000000056, 0.1013888888888888895, 0.1027777777777777735, 0.1041666666666666713, 0.1055555555555555552, 0.1069444444444444392, 0.1083333333333333370, 0.1097222222222222210, 0.1111111111111111049, 0.1125000000000000028, 0.1138888888888888867, 0.1152777777777777846, 0.1166666666666666685, 0.1180555555555555525, 0.1194444444444444503, 0.1208333333333333343, 0.1222222222222222182, 0.1236111111111111160, 0.1250000000000000000, 0.1263888888888888840, 0.1277777777777777679, 0.1291666666666666796, 0.1305555555555555636, 0.1319444444444444475, 0.1333333333333333315, 0.1347222222222222154, 0.1361111111111110994, 0.1375000000000000111, 0.1388888888888888951, 0.1402777777777777790, 0.1416666666666666630, 0.1430555555555555469, 0.1444444444444444309, 0.1458333333333333426, 0.1472222222222222265, 0.1486111111111111105, 0.1499999999999999944, 0.1513888888888888784, 0.1527777777777777901, 0.1541666666666666741, 0.1555555555555555580, 0.1569444444444444420, 0.1583333333333333259, 0.1597222222222222099, 0.1611111111111111216, 0.1625000000000000056, 0.1638888888888888895, 0.1652777777777777735, 0.1666666666666666574, 0.1680555555555555691, 0.1694444444444444531, 0.1708333333333333370, 0.1722222222222222210, 0.1736111111111111049, 0.1749999999999999889, 0.1763888888888889006, 0.1777777777777777846, 0.1791666666666666685, 0.1805555555555555525, 0.1819444444444444364, 0.1833333333333333204, 0.1847222222222222321, 0.1861111111111111160, 0.1875000000000000000, 0.1888888888888888840, 0.1902777777777777679, 0.1916666666666666796, 0.1930555555555555636, 0.1944444444444444475, 0.1958333333333333315, 0.1972222222222222154, 0.1986111111111110994, 0.2000000000000000111, 0.2013888888888888951, 0.2027777777777777790, 0.2041666666666666630, 0.2055555555555555469, 0.2069444444444444309, 0.2083333333333333426, 0.2097222222222222265, 0.2111111111111111105, 0.2124999999999999944, 0.2138888888888888784, 0.2152777777777777901, 0.2166666666666666741, 0.2180555555555555580, 0.2194444444444444420, 0.2208333333333333259, 0.2222222222222222099, 0.2236111111111111216, 0.2250000000000000056, 0.2263888888888888895, 0.2277777777777777735, 0.2291666666666666574, 0.2305555555555555691, 0.2319444444444444531, 0.2333333333333333370, 0.2347222222222222210, 0.2361111111111111049, 0.2374999999999999889, 0.2388888888888889006, 0.2402777777777777846, 0.2416666666666666685, 0.2430555555555555525, 0.2444444444444444364, 0.2458333333333333204, 0.2472222222222222321, 0.2486111111111111160, 0.2500000000000000000, 0.2513888888888888840, 0.2527777777777777679, 0.2541666666666666519, 0.2555555555555555358, 0.2569444444444444198, 0.2583333333333333592, 0.2597222222222222432, 0.2611111111111111271, 0.2625000000000000111, 0.2638888888888888951, 0.2652777777777777790, 0.2666666666666666630, 0.2680555555555555469, 0.2694444444444444309, 0.2708333333333333148, 0.2722222222222221988, 0.2736111111111111382, 0.2750000000000000222, 0.2763888888888889062, 0.2777777777777777901, 0.2791666666666666741, 0.2805555555555555580, 0.2819444444444444420, 0.2833333333333333259, 0.2847222222222222099, 0.2861111111111110938, 0.2874999999999999778, 0.2888888888888888618, 0.2902777777777778012, 0.2916666666666666852, 0.2930555555555555691, 0.2944444444444444531, 0.2958333333333333370, 0.2972222222222222210, 0.2986111111111111049, 0.2999999999999999889, 0.3013888888888888729, 0.3027777777777777568, 0.3041666666666666408, 0.3055555555555555802, 0.3069444444444444642, 0.3083333333333333481, 0.3097222222222222321, 0.3111111111111111160, 0.3125000000000000000, 0.3138888888888888840, 0.3152777777777777679, 0.3166666666666666519, 0.3180555555555555358, 0.3194444444444444198, 0.3208333333333333592, 0.3222222222222222432, 0.3236111111111111271, 0.3250000000000000111, 0.3263888888888888951, 0.3277777777777777790, 0.3291666666666666630, 0.3305555555555555469, 0.3319444444444444309, 0.3333333333333333148, 0.3347222222222221988, 0.3361111111111111382, 0.3375000000000000222, 0.3388888888888889062, 0.3402777777777777901, 0.3416666666666666741, 0.3430555555555555580, 0.3444444444444444420, 0.3458333333333333259, 0.3472222222222222099, 0.3486111111111110938, 0.3499999999999999778, 0.3513888888888888618, 0.3527777777777778012, 0.3541666666666666852, 0.3555555555555555691, 0.3569444444444444531, 0.3583333333333333370, 0.3597222222222222210, 0.3611111111111111049, 0.3624999999999999889, 0.3638888888888888729, 0.3652777777777777568, 0.3666666666666666408, 0.3680555555555555802, 0.3694444444444444642, 0.3708333333333333481, 0.3722222222222222321, 0.3736111111111111160, 0.3750000000000000000, 0.3763888888888888840, 0.3777777777777777679, 0.3791666666666666519, 0.3805555555555555358, 0.3819444444444444198, 0.3833333333333333592, 0.3847222222222222432, 0.3861111111111111271, 0.3875000000000000111, 0.3888888888888888951, 0.3902777777777777790, 0.3916666666666666630, 0.3930555555555555469, 0.3944444444444444309, 0.3958333333333333148, 0.3972222222222221988, 0.3986111111111111382, 0.4000000000000000222, 0.4013888888888889062, 0.4027777777777777901, 0.4041666666666666741, 0.4055555555555555580, 0.4069444444444444420, 0.4083333333333333259, 0.4097222222222222099, 0.4111111111111110938, 0.4124999999999999778, 0.4138888888888888618, 0.4152777777777778012, 0.4166666666666666852, 0.4180555555555555691, 0.4194444444444444531, 0.4208333333333333370, 0.4222222222222222210, 0.4236111111111111049, 0.4249999999999999889, 0.4263888888888888729, 0.4277777777777777568, 0.4291666666666666408, 0.4305555555555555802, 0.4319444444444444642, 0.4333333333333333481, 0.4347222222222222321, 0.4361111111111111160, 0.4375000000000000000, 0.4388888888888888840, 0.4402777777777777679, 0.4416666666666666519, 0.4430555555555555358, 0.4444444444444444198, 0.4458333333333333592, 0.4472222222222222432, 0.4486111111111111271, 0.4500000000000000111, 0.4513888888888888951, 0.4527777777777777790, 0.4541666666666666630, 0.4555555555555555469, 0.4569444444444444309, 0.4583333333333333148, 0.4597222222222221988, 0.4611111111111111382, 0.4625000000000000222, 0.4638888888888889062, 0.4652777777777777901, 0.4666666666666666741, 0.4680555555555555580, 0.4694444444444444420, 0.4708333333333333259, 0.4722222222222222099, 0.4736111111111110938, 0.4749999999999999778, 0.4763888888888888618, 0.4777777777777778012, 0.4791666666666666852, 0.4805555555555555691, 0.4819444444444444531, 0.4833333333333333370, 0.4847222222222222210, 0.4861111111111111049, 0.4874999999999999889, 0.4888888888888888729, 0.4902777777777777568, 0.4916666666666666408, 0.4930555555555555802, 0.4944444444444444642, 0.4958333333333333481, 0.4972222222222222321, 0.4986111111111111160, 0.5000000000000000000, 0.5013888888888888840, 0.5027777777777777679, 0.5041666666666666519, 0.5055555555555555358, 0.5069444444444444198, 0.5083333333333333037, 0.5097222222222221877, 0.5111111111111110716, 0.5124999999999999556, 0.5138888888888888395, 0.5152777777777777235, 0.5166666666666667185, 0.5180555555555556024, 0.5194444444444444864, 0.5208333333333333703, 0.5222222222222222543, 0.5236111111111111382, 0.5250000000000000222, 0.5263888888888889062, 0.5277777777777777901, 0.5291666666666666741, 0.5305555555555555580, 0.5319444444444444420, 0.5333333333333333259, 0.5347222222222222099, 0.5361111111111110938, 0.5374999999999999778, 0.5388888888888888618, 0.5402777777777777457, 0.5416666666666666297, 0.5430555555555555136, 0.5444444444444443976, 0.5458333333333332815, 0.5472222222222222765, 0.5486111111111111605, 0.5500000000000000444, 0.5513888888888889284, 0.5527777777777778123, 0.5541666666666666963, 0.5555555555555555802, 0.5569444444444444642, 0.5583333333333333481, 0.5597222222222222321, 0.5611111111111111160, 0.5625000000000000000, 0.5638888888888888840, 0.5652777777777777679, 0.5666666666666666519, 0.5680555555555555358, 0.5694444444444444198, 0.5708333333333333037, 0.5722222222222221877, 0.5736111111111110716, 0.5749999999999999556, 0.5763888888888888395, 0.5777777777777777235, 0.5791666666666667185, 0.5805555555555556024, 0.5819444444444444864, 0.5833333333333333703, 0.5847222222222222543, 0.5861111111111111382, 0.5875000000000000222, 0.5888888888888889062, 0.5902777777777777901, 0.5916666666666666741, 0.5930555555555555580, 0.5944444444444444420, 0.5958333333333333259, 0.5972222222222222099, 0.5986111111111110938, 0.5999999999999999778, 0.6013888888888888618, 0.6027777777777777457, 0.6041666666666666297, 0.6055555555555555136, 0.6069444444444443976, 0.6083333333333332815, 0.6097222222222222765, 0.6111111111111111605, 0.6125000000000000444, 0.6138888888888889284, 0.6152777777777778123, 0.6166666666666666963, 0.6180555555555555802, 0.6194444444444444642, 0.6208333333333333481, 0.6222222222222222321, 0.6236111111111111160, 0.6250000000000000000, 0.6263888888888888840, 0.6277777777777777679, 0.6291666666666666519, 0.6305555555555555358, 0.6319444444444444198, 0.6333333333333333037, 0.6347222222222221877, 0.6361111111111110716, 0.6374999999999999556, 0.6388888888888888395, 0.6402777777777777235, 0.6416666666666667185, 0.6430555555555556024, 0.6444444444444444864, 0.6458333333333333703, 0.6472222222222222543, 0.6486111111111111382, 0.6500000000000000222, 0.6513888888888889062, 0.6527777777777777901, 0.6541666666666666741, 0.6555555555555555580, 0.6569444444444444420, 0.6583333333333333259, 0.6597222222222222099, 0.6611111111111110938, 0.6624999999999999778, 0.6638888888888888618, 0.6652777777777777457, 0.6666666666666666297, 0.6680555555555555136, 0.6694444444444443976, 0.6708333333333332815, 0.6722222222222222765, 0.6736111111111111605, 0.6750000000000000444, 0.6763888888888889284, 0.6777777777777778123, 0.6791666666666666963, 0.6805555555555555802, 0.6819444444444444642, 0.6833333333333333481, 0.6847222222222222321, 0.6861111111111111160, 0.6875000000000000000, 0.6888888888888888840, 0.6902777777777777679, 0.6916666666666666519, 0.6930555555555555358, 0.6944444444444444198, 0.6958333333333333037, 0.6972222222222221877, 0.6986111111111110716, 0.6999999999999999556, 0.7013888888888888395, 0.7027777777777777235, 0.7041666666666667185, 0.7055555555555556024, 0.7069444444444444864, 0.7083333333333333703, 0.7097222222222222543, 0.7111111111111111382, 0.7125000000000000222, 0.7138888888888889062, 0.7152777777777777901, 0.7166666666666666741, 0.7180555555555555580, 0.7194444444444444420, 0.7208333333333333259, 0.7222222222222222099, 0.7236111111111110938, 0.7249999999999999778, 0.7263888888888888618, 0.7277777777777777457, 0.7291666666666666297, 0.7305555555555555136, 0.7319444444444443976, 0.7333333333333332815, 0.7347222222222222765, 0.7361111111111111605, 0.7375000000000000444, 0.7388888888888889284, 0.7402777777777778123, 0.7416666666666666963, 0.7430555555555555802, 0.7444444444444444642, 0.7458333333333333481, 0.7472222222222222321, 0.7486111111111111160, 0.7500000000000000000, 0.7513888888888888840, 0.7527777777777777679, 0.7541666666666666519, 0.7555555555555555358, 0.7569444444444444198, 0.7583333333333333037, 0.7597222222222221877, 0.7611111111111110716, 0.7624999999999999556, 0.7638888888888888395, 0.7652777777777777235, 0.7666666666666667185, 0.7680555555555556024, 0.7694444444444444864, 0.7708333333333333703, 0.7722222222222222543, 0.7736111111111111382, 0.7750000000000000222, 0.7763888888888889062, 0.7777777777777777901, 0.7791666666666666741, 0.7805555555555555580, 0.7819444444444444420, 0.7833333333333333259, 0.7847222222222222099, 0.7861111111111110938, 0.7874999999999999778, 0.7888888888888888618, 0.7902777777777777457, 0.7916666666666666297, 0.7930555555555555136, 0.7944444444444443976, 0.7958333333333332815, 0.7972222222222222765, 0.7986111111111111605, 0.8000000000000000444, 0.8013888888888889284, 0.8027777777777778123, 0.8041666666666666963, 0.8055555555555555802, 0.8069444444444444642, 0.8083333333333333481, 0.8097222222222222321, 0.8111111111111111160, 0.8125000000000000000, 0.8138888888888888840, 0.8152777777777777679, 0.8166666666666666519, 0.8180555555555555358, 0.8194444444444444198, 0.8208333333333333037, 0.8222222222222221877, 0.8236111111111110716, 0.8249999999999999556, 0.8263888888888888395, 0.8277777777777777235, 0.8291666666666667185, 0.8305555555555556024, 0.8319444444444444864, 0.8333333333333333703, 0.8347222222222222543, 0.8361111111111111382, 0.8375000000000000222, 0.8388888888888889062, 0.8402777777777777901, 0.8416666666666666741, 0.8430555555555555580, 0.8444444444444444420, 0.8458333333333333259, 0.8472222222222222099, 0.8486111111111110938, 0.8499999999999999778, 0.8513888888888888618, 0.8527777777777777457, 0.8541666666666666297, 0.8555555555555555136, 0.8569444444444443976, 0.8583333333333332815, 0.8597222222222222765, 0.8611111111111111605, 0.8625000000000000444, 0.8638888888888889284, 0.8652777777777778123, 0.8666666666666666963, 0.8680555555555555802, 0.8694444444444444642, 0.8708333333333333481, 0.8722222222222222321, 0.8736111111111111160, 0.8750000000000000000, 0.8763888888888888840, 0.8777777777777777679, 0.8791666666666666519, 0.8805555555555555358, 0.8819444444444444198, 0.8833333333333333037, 0.8847222222222221877, 0.8861111111111110716, 0.8874999999999999556, 0.8888888888888888395, 0.8902777777777777235, 0.8916666666666667185, 0.8930555555555556024, 0.8944444444444444864, 0.8958333333333333703, 0.8972222222222222543, 0.8986111111111111382, 0.9000000000000000222, 0.9013888888888889062, 0.9027777777777777901, 0.9041666666666666741, 0.9055555555555555580, 0.9069444444444444420, 0.9083333333333333259, 0.9097222222222222099, 0.9111111111111110938, 0.9124999999999999778, 0.9138888888888888618, 0.9152777777777777457, 0.9166666666666666297, 0.9180555555555555136, 0.9194444444444443976, 0.9208333333333332815, 0.9222222222222222765, 0.9236111111111111605, 0.9250000000000000444, 0.9263888888888889284, 0.9277777777777778123, 0.9291666666666666963, 0.9305555555555555802, 0.9319444444444444642, 0.9333333333333333481, 0.9347222222222222321, 0.9361111111111111160, 0.9375000000000000000, 0.9388888888888888840, 0.9402777777777777679, 0.9416666666666666519, 0.9430555555555555358, 0.9444444444444444198, 0.9458333333333333037, 0.9472222222222221877, 0.9486111111111110716, 0.9499999999999999556, 0.9513888888888888395, 0.9527777777777777235, 0.9541666666666667185, 0.9555555555555556024, 0.9569444444444444864, 0.9583333333333333703, 0.9597222222222222543, 0.9611111111111111382, 0.9625000000000000222, 0.9638888888888889062, 0.9652777777777777901, 0.9666666666666666741, 0.9680555555555555580, 0.9694444444444444420, 0.9708333333333333259, 0.9722222222222222099, 0.9736111111111110938, 0.9749999999999999778, 0.9763888888888888618, 0.9777777777777777457, 0.9791666666666666297, 0.9805555555555555136, 0.9819444444444443976, 0.9833333333333332815, 0.9847222222222222765, 0.9861111111111111605, 0.9875000000000000444, 0.9888888888888889284, 0.9902777777777778123, 0.9916666666666666963, 0.9930555555555555802, 0.9944444444444444642, 0.9958333333333333481, 0.9972222222222222321, 0.9986111111111111160, 1.000000000000000000 ),
 .UNSPECIFIED. ) 
 GEOMETRIC_REPRESENTATION_ITEM ( )  RATIONAL_B_SPLINE_SURFACE ( (
 ( 1.000000000000000000, 0.8660254037844387076, 1.000000000000000000, 0.8660254037844387076, 1.000000000000000000, 0.8660254037844387076, 1.000000000000000000, 0.8660254037844387076, 1.000000000000000000, 0.8660254037844387076, 1.000000000000000000, 0.8660254037844387076, 1.000000000000000000, 0.8660254037844387076, 1.000000000000000000, 0.8660254037844387076, 1.000000000000000000, 0.8660254037844387076, 1.000000000000000000, 0.8660254037844387076, 1.000000000000000000, 0.8660254037844387076, 1.000000000000000000, 0.8660254037844387076, 1.000000000000000000, 0.8660254037844387076, 1.000000000000000000, 0.8660254037844387076, 1.000000000000000000, 0.8660254037844387076, 1.000000000000000000, 0.8660254037844387076, 1.000000000000000000, 0.8660254037844387076, 1.000000000000000000, 0.8660254037844387076, 1.000000000000000000, 0.8660254037844387076, 1.000000000000000000, 0.8660254037844387076, 1.000000000000000000, 0.8660254037844387076, 1.000000000000000000, 0.8660254037844387076, 1.000000000000000000, 0.8660254037844387076, 1.000000000000000000, 0.8660254037844387076, 1.000000000000000000, 0.8660254037844387076, 1.000000000000000000, 0.8660254037844387076, 1.000000000000000000, 0.8660254037844387076, 1.000000000000000000, 0.8660254037844387076, 1.000000000000000000, 0.8660254037844387076, 1.000000000000000000, 0.8660254037844387076, 1.000000000000000000, 0.8660254037844387076, 1.000000000000000000, 0.8660254037844387076, 1.000000000000000000, 0.8660254037844387076, 1.000000000000000000, 0.8660254037844387076, 1.000000000000000000, 0.8660254037844387076, 1.000000000000000000, 0.8660254037844387076, 1.000000000000000000, 0.8660254037844387076, 1.000000000000000000, 0.8660254037844387076, 1.000000000000000000, 0.8660254037844387076, 1.000000000000000000, 0.8660254037844387076, 1.000000000000000000, 0.8660254037844387076, 1.000000000000000000, 0.8660254037844387076, 1.000000000000000000, 0.8660254037844387076, 1.000000000000000000, 0.8660254037844387076, 1.000000000000000000, 0.8660254037844387076, 1.000000000000000000, 0.8660254037844387076, 1.000000000000000000, 0.8660254037844387076, 1.000000000000000000, 0.8660254037844387076, 1.000000000000000000, 0.8660254037844387076, 1.000000000000000000, 0.8660254037844387076, 1.000000000000000000, 0.8660254037844387076, 1.000000000000000000, 0.8660254037844387076, 1.000000000000000000, 0.8660254037844387076, 1.000000000000000000, 0.8660254037844387076, 1.000000000000000000, 0.8660254037844387076, 1.000000000000000000, 0.8660254037844387076, 1.000000000000000000, 0.8660254037844387076, 1.000000000000000000, 0.8660254037844387076, 1.000000000000000000, 0.8660254037844387076, 1.000000000000000000, 0.8660254037844387076, 1.000000000000000000, 0.8660254037844387076, 1.000000000000000000, 0.8660254037844387076, 1.000000000000000000, 0.8660254037844387076, 1.000000000000000000, 0.8660254037844387076, 1.000000000000000000, 0.8660254037844387076, 1.000000000000000000, 0.8660254037844387076, 1.000000000000000000, 0.8660254037844387076, 1.000000000000000000, 0.8660254037844387076, 1.000000000000000000, 0.8660254037844387076, 1.000000000000000000, 0.8660254037844387076, 1.000000000000000000, 0.8660254037844387076, 1.000000000000000000, 0.8660254037844387076, 1.000000000000000000, 0.8660254037844387076, 1.000000000000000000, 0.8660254037844387076, 1.000000000000000000, 0.8660254037844387076, 1.000000000000000000, 0.8660254037844387076, 1.000000000000000000, 0.8660254037844387076, 1.000000000000000000, 0.8660254037844387076, 1.000000000000000000, 0.8660254037844387076, 1.000000000000000000, 0.8660254037844387076, 1.000000000000000000, 0.8660254037844387076, 1.000000000000000000, 0.8660254037844387076, 1.000000000000000000, 0.8660254037844387076, 1.000000000000000000, 0.8660254037844387076, 1.000000000000000000, 0.8660254037844387076, 1.000000000000000000, 0.8660254037844387076, 1.000000000000000000, 0.8660254037844387076, 1.000000000000000000, 0.8660254037844387076, 1.000000000000000000, 0.8660254037844387076, 1.000000000000000000, 0.8660254037844387076, 1.000000000000000000, 0.8660254037844387076, 1.000000000000000000, 0.8660254037844387076, 1.000000000000000000, 0.8660254037844387076, 1.000000000000000000, 0.8660254037844387076, 1.000000000000000000, 0.8660254037844387076, 1.000000000000000000, 0.8660254037844387076, 1.000000000000000000, 0.8660254037844387076, 1.000000000000000000, 0.8660254037844387076, 1.000000000000000000, 0.8660254037844387076, 1.000000000000000000, 0.8660254037844387076, 1.000000000000000000, 0.8660254037844387076, 1.000000000000000000, 0.8660254037844387076, 1.000000000000000000, 0.8660254037844387076, 1.000000000000000000, 0.8660254037844387076, 1.000000000000000000, 0.8660254037844387076, 1.000000000000000000, 0.8660254037844387076, 1.000000000000000000, 0.8660254037844387076, 1.000000000000000000, 0.8660254037844387076, 1.000000000000000000, 0.8660254037844387076, 1.000000000000000000, 0.8660254037844387076, 1.000000000000000000, 0.8660254037844387076, 1.000000000000000000, 0.8660254037844387076, 1.000000000000000000, 0.8660254037844387076, 1.000000000000000000, 0.8660254037844387076, 1.000000000000000000, 0.8660254037844387076, 1.000000000000000000, 0.8660254037844387076, 1.000000000000000000, 0.8660254037844387076, 1.000000000000000000, 0.8660254037844387076, 1.000000000000000000, 0.8660254037844387076, 1.000000000000000000, 0.8660254037844387076, 1.000000000000000000, 0.8660254037844387076, 1.000000000000000000, 0.8660254037844387076, 1.000000000000000000, 0.8660254037844387076, 1.000000000000000000, 0.8660254037844387076, 1.000000000000000000, 0.8660254037844387076, 1.000000000000000000, 0.8660254037844387076, 1.000000000000000000, 0.8660254037844387076, 1.000000000000000000, 0.8660254037844387076, 1.000000000000000000, 0.8660254037844387076, 1.000000000000000000, 0.8660254037844387076, 1.000000000000000000, 0.8660254037844387076, 1.000000000000000000, 0.8660254037844387076, 1.000000000000000000, 0.8660254037844387076, 1.000000000000000000, 0.8660254037844387076, 1.000000000000000000, 0.8660254037844387076, 1.000000000000000000, 0.8660254037844387076, 1.000000000000000000, 0.8660254037844387076, 1.000000000000000000, 0.8660254037844387076, 1.000000000000000000, 0.8660254037844387076, 1.000000000000000000, 0.8660254037844387076, 1.000000000000000000, 0.8660254037844387076, 1.000000000000000000, 0.8660254037844387076, 1.000000000000000000, 0.8660254037844387076, 1.000000000000000000, 0.8660254037844387076, 1.000000000000000000, 0.8660254037844387076, 1.000000000000000000, 0.8660254037844387076, 1.000000000000000000, 0.8660254037844387076, 1.000000000000000000, 0.8660254037844387076, 1.000000000000000000, 0.8660254037844387076, 1.000000000000000000, 0.8660254037844387076, 1.000000000000000000, 0.8660254037844387076, 1.000000000000000000, 0.8660254037844387076, 1.000000000000000000, 0.8660254037844387076, 1.000000000000000000, 0.8660254037844387076, 1.000000000000000000, 0.8660254037844387076, 1.000000000000000000, 0.8660254037844387076, 1.000000000000000000, 0.8660254037844387076, 1.000000000000000000, 0.8660254037844387076, 1.000000000000000000, 0.8660254037844387076, 1.000000000000000000, 0.8660254037844387076, 1.000000000000000000, 0.8660254037844387076, 1.000000000000000000, 0.8660254037844387076, 1.000000000000000000, 0.8660254037844387076, 1.000000000000000000, 0.8660254037844387076, 1.000000000000000000, 0.8660254037844387076, 1.000000000000000000, 0.8660254037844387076, 1.000000000000000000, 0.8660254037844387076, 1.000000000000000000, 0.8660254037844387076, 1.000000000000000000, 0.8660254037844387076, 1.000000000000000000, 0.8660254037844387076, 1.000000000000000000, 0.8660254037844387076, 1.000000000000000000, 0.8660254037844387076, 1.000000000000000000, 0.8660254037844387076, 1.000000000000000000, 0.8660254037844387076, 1.000000000000000000, 0.8660254037844387076, 1.000000000000000000, 0.8660254037844387076, 1.000000000000000000, 0.8660254037844387076, 1.000000000000000000, 0.8660254037844387076, 1.000000000000000000, 0.8660254037844387076, 1.000000000000000000, 0.8660254037844387076, 1.000000000000000000, 0.8660254037844387076, 1.000000000000000000, 0.8660254037844387076, 1.000000000000000000, 0.8660254037844387076, 1.000000000000000000, 0.8660254037844387076, 1.000000000000000000, 0.8660254037844387076, 1.000000000000000000, 0.8660254037844387076, 1.000000000000000000, 0.8660254037844387076, 1.000000000000000000, 0.8660254037844387076, 1.000000000000000000, 0.8660254037844387076, 1.000000000000000000, 0.8660254037844387076, 1.000000000000000000, 0.8660254037844387076, 1.000000000000000000, 0.8660254037844387076, 1.000000000000000000, 0.8660254037844387076, 1.000000000000000000, 0.8660254037844387076, 1.000000000000000000, 0.8660254037844387076, 1.000000000000000000, 0.8660254037844387076, 1.000000000000000000, 0.8660254037844387076, 1.000000000000000000, 0.8660254037844387076, 1.000000000000000000, 0.8660254037844387076, 1.000000000000000000, 0.8660254037844387076, 1.000000000000000000, 0.8660254037844387076, 1.000000000000000000, 0.8660254037844387076, 1.000000000000000000, 0.8660254037844387076, 1.000000000000000000, 0.8660254037844387076, 1.000000000000000000, 0.8660254037844387076, 1.000000000000000000, 0.8660254037844387076, 1.000000000000000000, 0.8660254037844387076, 1.000000000000000000, 0.8660254037844387076, 1.000000000000000000, 0.8660254037844387076, 1.000000000000000000, 0.8660254037844387076, 1.000000000000000000, 0.8660254037844387076, 1.000000000000000000, 0.8660254037844387076, 1.000000000000000000, 0.8660254037844387076, 1.000000000000000000, 0.8660254037844387076, 1.000000000000000000, 0.8660254037844387076, 1.000000000000000000, 0.8660254037844387076, 1.000000000000000000, 0.8660254037844387076, 1.000000000000000000, 0.8660254037844387076, 1.000000000000000000, 0.8660254037844387076, 1.000000000000000000, 0.8660254037844387076, 1.000000000000000000, 0.8660254037844387076, 1.000000000000000000, 0.8660254037844387076, 1.000000000000000000, 0.8660254037844387076, 1.000000000000000000, 0.8660254037844387076, 1.000000000000000000, 0.8660254037844387076, 1.000000000000000000, 0.8660254037844387076, 1.000000000000000000, 0.8660254037844387076, 1.000000000000000000, 0.8660254037844387076, 1.000000000000000000, 0.8660254037844387076, 1.000000000000000000, 0.8660254037844387076, 1.000000000000000000, 0.8660254037844387076, 1.000000000000000000, 0.8660254037844387076, 1.000000000000000000, 0.8660254037844387076, 1.000000000000000000, 0.8660254037844387076, 1.000000000000000000, 0.8660254037844387076, 1.000000000000000000, 0.8660254037844387076, 1.000000000000000000, 0.8660254037844387076, 1.000000000000000000, 0.8660254037844387076, 1.000000000000000000, 0.8660254037844387076, 1.000000000000000000, 0.8660254037844387076, 1.000000000000000000, 0.8660254037844387076, 1.000000000000000000, 0.8660254037844387076, 1.000000000000000000, 0.8660254037844387076, 1.000000000000000000, 0.8660254037844387076, 1.000000000000000000, 0.8660254037844387076, 1.000000000000000000, 0.8660254037844387076, 1.000000000000000000, 0.8660254037844387076, 1.000000000000000000, 0.8660254037844387076, 1.000000000000000000, 0.8660254037844387076, 1.000000000000000000, 0.8660254037844387076, 1.000000000000000000, 0.8660254037844387076, 1.000000000000000000, 0.8660254037844387076, 1.000000000000000000, 0.8660254037844387076, 1.000000000000000000, 0.8660254037844387076, 1.000000000000000000, 0.8660254037844387076, 1.000000000000000000, 0.8660254037844387076, 1.000000000000000000, 0.8660254037844387076, 1.000000000000000000, 0.8660254037844387076, 1.000000000000000000, 0.8660254037844387076, 1.000000000000000000, 0.8660254037844387076, 1.000000000000000000, 0.8660254037844387076, 1.000000000000000000, 0.8660254037844387076, 1.000000000000000000, 0.8660254037844387076, 1.000000000000000000, 0.8660254037844387076, 1.000000000000000000, 0.8660254037844387076, 1.000000000000000000, 0.8660254037844387076, 1.000000000000000000, 0.8660254037844387076, 1.000000000000000000, 0.8660254037844387076, 1.000000000000000000, 0.8660254037844387076, 1.000000000000000000, 0.8660254037844387076, 1.000000000000000000, 0.8660254037844387076, 1.000000000000000000, 0.8660254037844387076, 1.000000000000000000, 0.8660254037844387076, 1.000000000000000000, 0.8660254037844387076, 1.000000000000000000, 0.8660254037844387076, 1.000000000000000000, 0.8660254037844387076, 1.000000000000000000, 0.8660254037844387076, 1.000000000000000000, 0.8660254037844387076, 1.000000000000000000, 0.8660254037844387076, 1.000000000000000000, 0.8660254037844387076, 1.000000000000000000, 0.8660254037844387076, 1.000000000000000000, 0.8660254037844387076, 1.000000000000000000, 0.8660254037844387076, 1.000000000000000000, 0.8660254037844387076, 1.000000000000000000, 0.8660254037844387076, 1.000000000000000000, 0.8660254037844387076, 1.000000000000000000, 0.8660254037844387076, 1.000000000000000000, 0.8660254037844387076, 1.000000000000000000, 0.8660254037844387076, 1.000000000000000000, 0.8660254037844387076, 1.000000000000000000, 0.8660254037844387076, 1.000000000000000000, 0.8660254037844387076, 1.000000000000000000, 0.8660254037844387076, 1.000000000000000000, 0.8660254037844387076, 1.000000000000000000, 0.8660254037844387076, 1.000000000000000000, 0.8660254037844387076, 1.000000000000000000, 0.8660254037844387076, 1.000000000000000000, 0.8660254037844387076, 1.000000000000000000, 0.8660254037844387076, 1.000000000000000000, 0.8660254037844387076, 1.000000000000000000, 0.8660254037844387076, 1.000000000000000000, 0.8660254037844387076, 1.000000000000000000, 0.8660254037844387076, 1.000000000000000000, 0.8660254037844387076, 1.000000000000000000, 0.8660254037844387076, 1.000000000000000000, 0.8660254037844387076, 1.000000000000000000, 0.8660254037844387076, 1.000000000000000000, 0.8660254037844387076, 1.000000000000000000, 0.8660254037844387076, 1.000000000000000000, 0.8660254037844387076, 1.000000000000000000, 0.8660254037844387076, 1.000000000000000000, 0.8660254037844387076, 1.000000000000000000, 0.8660254037844387076, 1.000000000000000000, 0.8660254037844387076, 1.000000000000000000, 0.8660254037844387076, 1.000000000000000000, 0.8660254037844387076, 1.000000000000000000, 0.8660254037844387076, 1.000000000000000000, 0.8660254037844387076, 1.000000000000000000, 0.8660254037844387076, 1.000000000000000000, 0.8660254037844387076, 1.000000000000000000, 0.8660254037844387076, 1.000000000000000000, 0.8660254037844387076, 1.000000000000000000, 0.8660254037844387076, 1.000000000000000000, 0.8660254037844387076, 1.000000000000000000, 0.8660254037844387076, 1.000000000000000000, 0.8660254037844387076, 1.000000000000000000, 0.8660254037844387076, 1.000000000000000000, 0.8660254037844387076, 1.000000000000000000, 0.8660254037844387076, 1.000000000000000000, 0.8660254037844387076, 1.000000000000000000, 0.8660254037844387076, 1.000000000000000000, 0.8660254037844387076, 1.000000000000000000, 0.8660254037844387076, 1.000000000000000000, 0.8660254037844387076, 1.000000000000000000, 0.8660254037844387076, 1.000000000000000000, 0.8660254037844387076, 1.000000000000000000, 0.8660254037844387076, 1.000000000000000000, 0.8660254037844387076, 1.000000000000000000, 0.8660254037844387076, 1.000000000000000000, 0.8660254037844387076, 1.000000000000000000, 0.8660254037844387076, 1.000000000000000000, 0.8660254037844387076, 1.000000000000000000, 0.8660254037844387076, 1.000000000000000000, 0.8660254037844387076, 1.000000000000000000, 0.8660254037844387076, 1.000000000000000000, 0.8660254037844387076, 1.000000000000000000, 0.8660254037844387076, 1.000000000000000000, 0.8660254037844387076, 1.000000000000000000, 0.8660254037844387076, 1.000000000000000000, 0.8660254037844387076, 1.000000000000000000, 0.8660254037844387076, 1.000000000000000000, 0.8660254037844387076, 1.000000000000000000, 0.8660254037844387076, 1.000000000000000000, 0.8660254037844387076, 1.000000000000000000, 0.8660254037844387076, 1.000000000000000000, 0.8660254037844387076, 1.000000000000000000, 0.8660254037844387076, 1.000000000000000000, 0.8660254037844387076, 1.000000000000000000, 0.8660254037844387076, 1.000000000000000000, 0.8660254037844387076, 1.000000000000000000, 0.8660254037844387076, 1.000000000000000000, 0.8660254037844387076, 1.000000000000000000, 0.8660254037844387076, 1.000000000000000000, 0.8660254037844387076, 1.000000000000000000, 0.8660254037844387076, 1.000000000000000000, 0.8660254037844387076, 1.000000000000000000, 0.8660254037844387076, 1.000000000000000000, 0.8660254037844387076, 1.000000000000000000, 0.8660254037844387076, 1.000000000000000000, 0.8660254037844387076, 1.000000000000000000, 0.8660254037844387076, 1.000000000000000000, 0.8660254037844387076, 1.000000000000000000, 0.8660254037844387076, 1.000000000000000000, 0.8660254037844387076, 1.000000000000000000, 0.8660254037844387076, 1.000000000000000000, 0.8660254037844387076, 1.000000000000000000, 0.8660254037844387076, 1.000000000000000000, 0.8660254037844387076, 1.000000000000000000, 0.8660254037844387076, 1.000000000000000000, 0.8660254037844387076, 1.000000000000000000, 0.8660254037844387076, 1.000000000000000000, 0.8660254037844387076, 1.000000000000000000, 0.8660254037844387076, 1.000000000000000000, 0.8660254037844387076, 1.000000000000000000, 0.8660254037844387076, 1.000000000000000000, 0.8660254037844387076, 1.000000000000000000, 0.8660254037844387076, 1.000000000000000000, 0.8660254037844387076, 1.000000000000000000, 0.8660254037844387076, 1.000000000000000000, 0.8660254037844387076, 1.000000000000000000, 0.8660254037844387076, 1.000000000000000000, 0.8660254037844387076, 1.000000000000000000, 0.8660254037844387076, 1.000000000000000000, 0.8660254037844387076, 1.000000000000000000, 0.8660254037844387076, 1.000000000000000000, 0.8660254037844387076, 1.000000000000000000, 0.8660254037844387076, 1.000000000000000000, 0.8660254037844387076, 1.000000000000000000, 0.8660254037844387076, 1.000000000000000000, 0.8660254037844387076, 1.000000000000000000, 0.8660254037844387076, 1.000000000000000000, 0.8660254037844387076, 1.000000000000000000, 0.8660254037844387076, 1.000000000000000000, 0.8660254037844387076, 1.000000000000000000, 0.8660254037844387076, 1.000000000000000000, 0.8660254037844387076, 1.000000000000000000, 0.8660254037844387076, 1.000000000000000000, 0.8660254037844387076, 1.000000000000000000, 0.8660254037844387076, 1.000000000000000000, 0.8660254037844387076, 1.000000000000000000, 0.8660254037844387076, 1.000000000000000000, 0.8660254037844387076, 1.000000000000000000, 0.8660254037844387076, 1.000000000000000000, 0.8660254037844387076, 1.000000000000000000, 0.8660254037844387076, 1.000000000000000000, 0.8660254037844387076, 1.000000000000000000, 0.8660254037844387076, 1.000000000000000000, 0.8660254037844387076, 1.000000000000000000, 0.8660254037844387076, 1.000000000000000000, 0.8660254037844387076, 1.000000000000000000, 0.8660254037844387076, 1.000000000000000000, 0.8660254037844387076, 1.000000000000000000, 0.8660254037844387076, 1.000000000000000000, 0.8660254037844387076, 1.000000000000000000, 0.8660254037844387076, 1.000000000000000000, 0.8660254037844387076, 1.000000000000000000, 0.8660254037844387076, 1.000000000000000000, 0.8660254037844387076, 1.000000000000000000, 0.8660254037844387076, 1.000000000000000000, 0.8660254037844387076, 1.000000000000000000, 0.8660254037844387076, 1.000000000000000000, 0.8660254037844387076, 1.000000000000000000, 0.8660254037844387076, 1.000000000000000000, 0.8660254037844387076, 1.000000000000000000, 0.8660254037844387076, 1.000000000000000000, 0.8660254037844387076, 1.000000000000000000, 0.8660254037844387076, 1.000000000000000000, 0.8660254037844387076, 1.000000000000000000, 0.8660254037844387076, 1.000000000000000000, 0.8660254037844387076, 1.000000000000000000, 0.8660254037844387076, 1.000000000000000000, 0.8660254037844387076, 1.000000000000000000, 0.8660254037844387076, 1.000000000000000000, 0.8660254037844387076, 1.000000000000000000, 0.8660254037844387076, 1.000000000000000000, 0.8660254037844387076, 1.000000000000000000, 0.8660254037844387076, 1.000000000000000000, 0.8660254037844387076, 1.000000000000000000, 0.8660254037844387076, 1.000000000000000000, 0.8660254037844387076, 1.000000000000000000, 0.8660254037844387076, 1.000000000000000000, 0.8660254037844387076, 1.000000000000000000, 0.8660254037844387076, 1.000000000000000000, 0.8660254037844387076, 1.000000000000000000, 0.8660254037844387076, 1.000000000000000000, 0.8660254037844387076, 1.000000000000000000, 0.8660254037844387076, 1.000000000000000000, 0.8660254037844387076, 1.000000000000000000, 0.8660254037844387076, 1.000000000000000000, 0.8660254037844387076, 1.000000000000000000, 0.8660254037844387076, 1.000000000000000000, 0.8660254037844387076, 1.000000000000000000, 0.8660254037844387076, 1.000000000000000000, 0.8660254037844387076, 1.000000000000000000, 0.8660254037844387076, 1.000000000000000000, 0.8660254037844387076, 1.000000000000000000, 0.8660254037844387076, 1.000000000000000000, 0.8660254037844387076, 1.000000000000000000, 0.8660254037844387076, 1.000000000000000000, 0.8660254037844387076, 1.000000000000000000, 0.8660254037844387076, 1.000000000000000000, 0.8660254037844387076, 1.000000000000000000, 0.8660254037844387076, 1.000000000000000000, 0.8660254037844387076, 1.000000000000000000, 0.8660254037844387076, 1.000000000000000000, 0.8660254037844387076, 1.000000000000000000, 0.8660254037844387076, 1.000000000000000000, 0.8660254037844387076, 1.000000000000000000, 0.8660254037844387076, 1.000000000000000000, 0.8660254037844387076, 1.000000000000000000, 0.8660254037844387076, 1.000000000000000000, 0.8660254037844387076, 1.000000000000000000, 0.8660254037844387076, 1.000000000000000000, 0.8660254037844387076, 1.000000000000000000, 0.8660254037844387076, 1.000000000000000000, 0.8660254037844387076, 1.000000000000000000, 0.8660254037844387076, 1.000000000000000000, 0.8660254037844387076, 1.000000000000000000, 0.8660254037844387076, 1.000000000000000000, 0.8660254037844387076, 1.000000000000000000, 0.8660254037844387076, 1.000000000000000000, 0.8660254037844387076, 1.000000000000000000, 0.8660254037844387076, 1.000000000000000000, 0.8660254037844387076, 1.000000000000000000, 0.8660254037844387076, 1.000000000000000000, 0.8660254037844387076, 1.000000000000000000, 0.8660254037844387076, 1.000000000000000000, 0.8660254037844387076, 1.000000000000000000, 0.8660254037844387076, 1.000000000000000000, 0.8660254037844387076, 1.000000000000000000, 0.8660254037844387076, 1.000000000000000000, 0.8660254037844387076, 1.000000000000000000, 0.8660254037844387076, 1.000000000000000000, 0.8660254037844387076, 1.000000000000000000, 0.8660254037844387076, 1.000000000000000000, 0.8660254037844387076, 1.000000000000000000, 0.8660254037844387076, 1.000000000000000000, 0.8660254037844387076, 1.000000000000000000, 0.8660254037844387076, 1.000000000000000000, 0.8660254037844387076, 1.000000000000000000, 0.8660254037844387076, 1.000000000000000000, 0.8660254037844387076, 1.000000000000000000, 0.8660254037844387076, 1.000000000000000000, 0.8660254037844387076, 1.000000000000000000, 0.8660254037844387076, 1.000000000000000000, 0.8660254037844387076, 1.000000000000000000, 0.8660254037844387076, 1.000000000000000000, 0.8660254037844387076, 1.000000000000000000, 0.8660254037844387076, 1.000000000000000000, 0.8660254037844387076, 1.000000000000000000, 0.8660254037844387076, 1.000000000000000000, 0.8660254037844387076, 1.000000000000000000, 0.8660254037844387076, 1.000000000000000000, 0.8660254037844387076, 1.000000000000000000, 0.8660254037844387076, 1.000000000000000000, 0.8660254037844387076, 1.000000000000000000, 0.8660254037844387076, 1.000000000000000000, 0.8660254037844387076, 1.000000000000000000, 0.8660254037844387076, 1.000000000000000000, 0.8660254037844387076, 1.000000000000000000, 0.8660254037844387076, 1.000000000000000000, 0.8660254037844387076, 1.000000000000000000, 0.8660254037844387076, 1.000000000000000000, 0.8660254037844387076, 1.000000000000000000, 0.8660254037844387076, 1.000000000000000000, 0.8660254037844387076, 1.000000000000000000, 0.8660254037844387076, 1.000000000000000000, 0.8660254037844387076, 1.000000000000000000, 0.8660254037844387076, 1.000000000000000000, 0.8660254037844387076, 1.000000000000000000, 0.8660254037844387076, 1.000000000000000000, 0.8660254037844387076, 1.000000000000000000, 0.8660254037844387076, 1.000000000000000000, 0.8660254037844387076, 1.000000000000000000, 0.8660254037844387076, 1.000000000000000000, 0.8660254037844387076, 1.000000000000000000, 0.8660254037844387076, 1.000000000000000000, 0.8660254037844387076, 1.000000000000000000, 0.8660254037844387076, 1.000000000000000000, 0.8660254037844387076, 1.000000000000000000, 0.8660254037844387076, 1.000000000000000000, 0.8660254037844387076, 1.000000000000000000, 0.8660254037844387076, 1.000000000000000000, 0.8660254037844387076, 1.000000000000000000, 0.8660254037844387076, 1.000000000000000000, 0.8660254037844387076, 1.000000000000000000, 0.8660254037844387076, 1.000000000000000000, 0.8660254037844387076, 1.000000000000000000, 0.8660254037844387076, 1.000000000000000000, 0.8660254037844387076, 1.000000000000000000, 0.8660254037844387076, 1.000000000000000000, 0.8660254037844387076, 1.000000000000000000, 0.8660254037844387076, 1.000000000000000000, 0.8660254037844387076, 1.000000000000000000, 0.8660254037844387076, 1.000000000000000000, 0.8660254037844387076, 1.000000000000000000, 0.8660254037844387076, 1.000000000000000000, 0.8660254037844387076, 1.000000000000000000, 0.8660254037844387076, 1.000000000000000000, 0.8660254037844387076, 1.000000000000000000, 0.8660254037844387076, 1.000000000000000000, 0.8660254037844387076, 1.000000000000000000, 0.8660254037844387076, 1.000000000000000000, 0.8660254037844387076, 1.000000000000000000, 0.8660254037844387076, 1.000000000000000000, 0.8660254037844387076, 1.000000000000000000, 0.8660254037844387076, 1.000000000000000000, 0.8660254037844387076, 1.000000000000000000, 0.8660254037844387076, 1.000000000000000000, 0.8660254037844387076, 1.000000000000000000, 0.8660254037844387076, 1.000000000000000000, 0.8660254037844387076, 1.000000000000000000, 0.8660254037844387076, 1.000000000000000000, 0.8660254037844387076, 1.000000000000000000, 0.8660254037844387076, 1.000000000000000000, 0.8660254037844387076, 1.000000000000000000, 0.8660254037844387076, 1.000000000000000000, 0.8660254037844387076, 1.000000000000000000, 0.8660254037844387076, 1.000000000000000000, 0.8660254037844387076, 1.000000000000000000, 0.8660254037844387076, 1.000000000000000000, 0.8660254037844387076, 1.000000000000000000, 0.8660254037844387076, 1.000000000000000000, 0.8660254037844387076, 1.000000000000000000, 0.8660254037844387076, 1.000000000000000000, 0.8660254037844387076, 1.000000000000000000, 0.8660254037844387076, 1.000000000000000000, 0.8660254037844387076, 1.000000000000000000, 0.8660254037844387076, 1.000000000000000000, 0.8660254037844387076, 1.000000000000000000, 0.8660254037844387076, 1.000000000000000000, 0.8660254037844387076, 1.000000000000000000, 0.8660254037844387076, 1.000000000000000000, 0.8660254037844387076, 1.000000000000000000, 0.8660254037844387076, 1.000000000000000000, 0.8660254037844387076, 1.000000000000000000, 0.8660254037844387076, 1.000000000000000000, 0.8660254037844387076, 1.000000000000000000, 0.8660254037844387076, 1.000000000000000000, 0.8660254037844387076, 1.000000000000000000, 0.8660254037844387076, 1.000000000000000000, 0.8660254037844387076, 1.000000000000000000, 0.8660254037844387076, 1.000000000000000000, 0.8660254037844387076, 1.000000000000000000, 0.8660254037844387076, 1.000000000000000000, 0.8660254037844387076, 1.000000000000000000, 0.8660254037844387076, 1.000000000000000000, 0.8660254037844387076, 1.000000000000000000, 0.8660254037844387076, 1.000000000000000000, 0.8660254037844387076, 1.000000000000000000, 0.8660254037844387076, 1.000000000000000000, 0.8660254037844387076, 1.000000000000000000, 0.8660254037844387076, 1.000000000000000000, 0.8660254037844387076, 1.000000000000000000, 0.8660254037844387076, 1.000000000000000000, 0.8660254037844387076, 1.000000000000000000, 0.8660254037844387076, 1.000000000000000000, 0.8660254037844387076, 1.000000000000000000, 0.8660254037844387076, 1.000000000000000000, 0.8660254037844387076, 1.000000000000000000, 0.8660254037844387076, 1.000000000000000000, 0.8660254037844387076, 1.000000000000000000, 0.8660254037844387076, 1.000000000000000000, 0.8660254037844387076, 1.000000000000000000, 0.8660254037844387076, 1.000000000000000000, 0.8660254037844387076, 1.000000000000000000, 0.8660254037844387076, 1.000000000000000000, 0.8660254037844387076, 1.000000000000000000, 0.8660254037844387076, 1.000000000000000000, 0.8660254037844387076, 1.000000000000000000, 0.8660254037844387076, 1.000000000000000000, 0.8660254037844387076, 1.000000000000000000, 0.8660254037844387076, 1.000000000000000000, 0.8660254037844387076, 1.000000000000000000, 0.8660254037844387076, 1.000000000000000000, 0.8660254037844387076, 1.000000000000000000, 0.8660254037844387076, 1.000000000000000000, 0.8660254037844387076, 1.000000000000000000, 0.8660254037844387076, 1.000000000000000000, 0.8660254037844387076, 1.000000000000000000, 0.8660254037844387076, 1.000000000000000000, 0.8660254037844387076, 1.000000000000000000, 0.8660254037844387076, 1.000000000000000000, 0.8660254037844387076, 1.000000000000000000, 0.8660254037844387076, 1.000000000000000000, 0.8660254037844387076, 1.000000000000000000, 0.8660254037844387076, 1.000000000000000000, 0.8660254037844387076, 1.000000000000000000, 0.8660254037844387076, 1.000000000000000000, 0.8660254037844387076, 1.000000000000000000, 0.8660254037844387076, 1.000000000000000000, 0.8660254037844387076, 1.000000000000000000, 0.8660254037844387076, 1.000000000000000000, 0.8660254037844387076, 1.000000000000000000, 0.8660254037844387076, 1.000000000000000000, 0.8660254037844387076, 1.000000000000000000, 0.8660254037844387076, 1.000000000000000000, 0.8660254037844387076, 1.000000000000000000, 0.8660254037844387076, 1.000000000000000000, 0.8660254037844387076, 1.000000000000000000, 0.8660254037844387076, 1.000000000000000000, 0.8660254037844387076, 1.000000000000000000, 0.8660254037844387076, 1.000000000000000000, 0.8660254037844387076, 1.000000000000000000, 0.8660254037844387076, 1.000000000000000000, 0.8660254037844387076, 1.000000000000000000, 0.8660254037844387076, 1.000000000000000000, 0.8660254037844387076, 1.000000000000000000, 0.8660254037844387076, 1.000000000000000000, 0.8660254037844387076, 1.000000000000000000, 0.8660254037844387076, 1.000000000000000000, 0.8660254037844387076, 1.000000000000000000, 0.8660254037844387076, 1.000000000000000000, 0.8660254037844387076, 1.000000000000000000, 0.8660254037844387076, 1.000000000000000000, 0.8660254037844387076, 1.000000000000000000, 0.8660254037844387076, 1.000000000000000000, 0.8660254037844387076, 1.000000000000000000, 0.8660254037844387076, 1.000000000000000000, 0.8660254037844387076, 1.000000000000000000, 0.8660254037844387076, 1.000000000000000000, 0.8660254037844387076, 1.000000000000000000, 0.8660254037844387076, 1.000000000000000000, 0.8660254037844387076, 1.000000000000000000, 0.8660254037844387076, 1.000000000000000000, 0.8660254037844387076, 1.000000000000000000, 0.8660254037844387076, 1.000000000000000000, 0.8660254037844387076, 1.000000000000000000, 0.8660254037844387076, 1.000000000000000000, 0.8660254037844387076, 1.000000000000000000, 0.8660254037844387076, 1.000000000000000000, 0.8660254037844387076, 1.000000000000000000, 0.8660254037844387076, 1.000000000000000000, 0.8660254037844387076, 1.000000000000000000, 0.8660254037844387076, 1.000000000000000000, 0.8660254037844387076, 1.000000000000000000, 0.8660254037844387076, 1.000000000000000000, 0.8660254037844387076, 1.000000000000000000, 0.8660254037844387076, 1.000000000000000000, 0.8660254037844387076, 1.000000000000000000, 0.8660254037844387076, 1.000000000000000000, 0.8660254037844387076, 1.000000000000000000, 0.8660254037844387076, 1.000000000000000000, 0.8660254037844387076, 1.000000000000000000, 0.8660254037844387076, 1.000000000000000000, 0.8660254037844387076, 1.000000000000000000, 0.8660254037844387076, 1.000000000000000000, 0.8660254037844387076, 1.000000000000000000, 0.8660254037844387076, 1.000000000000000000, 0.8660254037844387076, 1.000000000000000000),
 ( 1.000000000000000000, 0.8660254037844387076, 1.000000000000000000, 0.8660254037844387076, 1.000000000000000000, 0.8660254037844387076, 1.000000000000000000, 0.8660254037844387076, 1.000000000000000000, 0.8660254037844387076, 1.000000000000000000, 0.8660254037844387076, 1.000000000000000000, 0.8660254037844387076, 1.000000000000000000, 0.8660254037844387076, 1.000000000000000000, 0.8660254037844387076, 1.000000000000000000, 0.8660254037844387076, 1.000000000000000000, 0.8660254037844387076, 1.000000000000000000, 0.8660254037844387076, 1.000000000000000000, 0.8660254037844387076, 1.000000000000000000, 0.8660254037844387076, 1.000000000000000000, 0.8660254037844387076, 1.000000000000000000, 0.8660254037844387076, 1.000000000000000000, 0.8660254037844387076, 1.000000000000000000, 0.8660254037844387076, 1.000000000000000000, 0.8660254037844387076, 1.000000000000000000, 0.8660254037844387076, 1.000000000000000000, 0.8660254037844387076, 1.000000000000000000, 0.8660254037844387076, 1.000000000000000000, 0.8660254037844387076, 1.000000000000000000, 0.8660254037844387076, 1.000000000000000000, 0.8660254037844387076, 1.000000000000000000, 0.8660254037844387076, 1.000000000000000000, 0.8660254037844387076, 1.000000000000000000, 0.8660254037844387076, 1.000000000000000000, 0.8660254037844387076, 1.000000000000000000, 0.8660254037844387076, 1.000000000000000000, 0.8660254037844387076, 1.000000000000000000, 0.8660254037844387076, 1.000000000000000000, 0.8660254037844387076, 1.000000000000000000, 0.8660254037844387076, 1.000000000000000000, 0.8660254037844387076, 1.000000000000000000, 0.8660254037844387076, 1.000000000000000000, 0.8660254037844387076, 1.000000000000000000, 0.8660254037844387076, 1.000000000000000000, 0.8660254037844387076, 1.000000000000000000, 0.8660254037844387076, 1.000000000000000000, 0.8660254037844387076, 1.000000000000000000, 0.8660254037844387076, 1.000000000000000000, 0.8660254037844387076, 1.000000000000000000, 0.8660254037844387076, 1.000000000000000000, 0.8660254037844387076, 1.000000000000000000, 0.8660254037844387076, 1.000000000000000000, 0.8660254037844387076, 1.000000000000000000, 0.8660254037844387076, 1.000000000000000000, 0.8660254037844387076, 1.000000000000000000, 0.8660254037844387076, 1.000000000000000000, 0.8660254037844387076, 1.000000000000000000, 0.8660254037844387076, 1.000000000000000000, 0.8660254037844387076, 1.000000000000000000, 0.8660254037844387076, 1.000000000000000000, 0.8660254037844387076, 1.000000000000000000, 0.8660254037844387076, 1.000000000000000000, 0.8660254037844387076, 1.000000000000000000, 0.8660254037844387076, 1.000000000000000000, 0.8660254037844387076, 1.000000000000000000, 0.8660254037844387076, 1.000000000000000000, 0.8660254037844387076, 1.000000000000000000, 0.8660254037844387076, 1.000000000000000000, 0.8660254037844387076, 1.000000000000000000, 0.8660254037844387076, 1.000000000000000000, 0.8660254037844387076, 1.000000000000000000, 0.8660254037844387076, 1.000000000000000000, 0.8660254037844387076, 1.000000000000000000, 0.8660254037844387076, 1.000000000000000000, 0.8660254037844387076, 1.000000000000000000, 0.8660254037844387076, 1.000000000000000000, 0.8660254037844387076, 1.000000000000000000, 0.8660254037844387076, 1.000000000000000000, 0.8660254037844387076, 1.000000000000000000, 0.8660254037844387076, 1.000000000000000000, 0.8660254037844387076, 1.000000000000000000, 0.8660254037844387076, 1.000000000000000000, 0.8660254037844387076, 1.000000000000000000, 0.8660254037844387076, 1.000000000000000000, 0.8660254037844387076, 1.000000000000000000, 0.8660254037844387076, 1.000000000000000000, 0.8660254037844387076, 1.000000000000000000, 0.8660254037844387076, 1.000000000000000000, 0.8660254037844387076, 1.000000000000000000, 0.8660254037844387076, 1.000000000000000000, 0.8660254037844387076, 1.000000000000000000, 0.8660254037844387076, 1.000000000000000000, 0.8660254037844387076, 1.000000000000000000, 0.8660254037844387076, 1.000000000000000000, 0.8660254037844387076, 1.000000000000000000, 0.8660254037844387076, 1.000000000000000000, 0.8660254037844387076, 1.000000000000000000, 0.8660254037844387076, 1.000000000000000000, 0.8660254037844387076, 1.000000000000000000, 0.8660254037844387076, 1.000000000000000000, 0.8660254037844387076, 1.000000000000000000, 0.8660254037844387076, 1.000000000000000000, 0.8660254037844387076, 1.000000000000000000, 0.8660254037844387076, 1.000000000000000000, 0.8660254037844387076, 1.000000000000000000, 0.8660254037844387076, 1.000000000000000000, 0.8660254037844387076, 1.000000000000000000, 0.8660254037844387076, 1.000000000000000000, 0.8660254037844387076, 1.000000000000000000, 0.8660254037844387076, 1.000000000000000000, 0.8660254037844387076, 1.000000000000000000, 0.8660254037844387076, 1.000000000000000000, 0.8660254037844387076, 1.000000000000000000, 0.8660254037844387076, 1.000000000000000000, 0.8660254037844387076, 1.000000000000000000, 0.8660254037844387076, 1.000000000000000000, 0.8660254037844387076, 1.000000000000000000, 0.8660254037844387076, 1.000000000000000000, 0.8660254037844387076, 1.000000000000000000, 0.8660254037844387076, 1.000000000000000000, 0.8660254037844387076, 1.000000000000000000, 0.8660254037844387076, 1.000000000000000000, 0.8660254037844387076, 1.000000000000000000, 0.8660254037844387076, 1.000000000000000000, 0.8660254037844387076, 1.000000000000000000, 0.8660254037844387076, 1.000000000000000000, 0.8660254037844387076, 1.000000000000000000, 0.8660254037844387076, 1.000000000000000000, 0.8660254037844387076, 1.000000000000000000, 0.8660254037844387076, 1.000000000000000000, 0.8660254037844387076, 1.000000000000000000, 0.8660254037844387076, 1.000000000000000000, 0.8660254037844387076, 1.000000000000000000, 0.8660254037844387076, 1.000000000000000000, 0.8660254037844387076, 1.000000000000000000, 0.8660254037844387076, 1.000000000000000000, 0.8660254037844387076, 1.000000000000000000, 0.8660254037844387076, 1.000000000000000000, 0.8660254037844387076, 1.000000000000000000, 0.8660254037844387076, 1.000000000000000000, 0.8660254037844387076, 1.000000000000000000, 0.8660254037844387076, 1.000000000000000000, 0.8660254037844387076, 1.000000000000000000, 0.8660254037844387076, 1.000000000000000000, 0.8660254037844387076, 1.000000000000000000, 0.8660254037844387076, 1.000000000000000000, 0.8660254037844387076, 1.000000000000000000, 0.8660254037844387076, 1.000000000000000000, 0.8660254037844387076, 1.000000000000000000, 0.8660254037844387076, 1.000000000000000000, 0.8660254037844387076, 1.000000000000000000, 0.8660254037844387076, 1.000000000000000000, 0.8660254037844387076, 1.000000000000000000, 0.8660254037844387076, 1.000000000000000000, 0.8660254037844387076, 1.000000000000000000, 0.8660254037844387076, 1.000000000000000000, 0.8660254037844387076, 1.000000000000000000, 0.8660254037844387076, 1.000000000000000000, 0.8660254037844387076, 1.000000000000000000, 0.8660254037844387076, 1.000000000000000000, 0.8660254037844387076, 1.000000000000000000, 0.8660254037844387076, 1.000000000000000000, 0.8660254037844387076, 1.000000000000000000, 0.8660254037844387076, 1.000000000000000000, 0.8660254037844387076, 1.000000000000000000, 0.8660254037844387076, 1.000000000000000000, 0.8660254037844387076, 1.000000000000000000, 0.8660254037844387076, 1.000000000000000000, 0.8660254037844387076, 1.000000000000000000, 0.8660254037844387076, 1.000000000000000000, 0.8660254037844387076, 1.000000000000000000, 0.8660254037844387076, 1.000000000000000000, 0.8660254037844387076, 1.000000000000000000, 0.8660254037844387076, 1.000000000000000000, 0.8660254037844387076, 1.000000000000000000, 0.8660254037844387076, 1.000000000000000000, 0.8660254037844387076, 1.000000000000000000, 0.8660254037844387076, 1.000000000000000000, 0.8660254037844387076, 1.000000000000000000, 0.8660254037844387076, 1.000000000000000000, 0.8660254037844387076, 1.000000000000000000, 0.8660254037844387076, 1.000000000000000000, 0.8660254037844387076, 1.000000000000000000, 0.8660254037844387076, 1.000000000000000000, 0.8660254037844387076, 1.000000000000000000, 0.8660254037844387076, 1.000000000000000000, 0.8660254037844387076, 1.000000000000000000, 0.8660254037844387076, 1.000000000000000000, 0.8660254037844387076, 1.000000000000000000, 0.8660254037844387076, 1.000000000000000000, 0.8660254037844387076, 1.000000000000000000, 0.8660254037844387076, 1.000000000000000000, 0.8660254037844387076, 1.000000000000000000, 0.8660254037844387076, 1.000000000000000000, 0.8660254037844387076, 1.000000000000000000, 0.8660254037844387076, 1.000000000000000000, 0.8660254037844387076, 1.000000000000000000, 0.8660254037844387076, 1.000000000000000000, 0.8660254037844387076, 1.000000000000000000, 0.8660254037844387076, 1.000000000000000000, 0.8660254037844387076, 1.000000000000000000, 0.8660254037844387076, 1.000000000000000000, 0.8660254037844387076, 1.000000000000000000, 0.8660254037844387076, 1.000000000000000000, 0.8660254037844387076, 1.000000000000000000, 0.8660254037844387076, 1.000000000000000000, 0.8660254037844387076, 1.000000000000000000, 0.8660254037844387076, 1.000000000000000000, 0.8660254037844387076, 1.000000000000000000, 0.8660254037844387076, 1.000000000000000000, 0.8660254037844387076, 1.000000000000000000, 0.8660254037844387076, 1.000000000000000000, 0.8660254037844387076, 1.000000000000000000, 0.8660254037844387076, 1.000000000000000000, 0.8660254037844387076, 1.000000000000000000, 0.8660254037844387076, 1.000000000000000000, 0.8660254037844387076, 1.000000000000000000, 0.8660254037844387076, 1.000000000000000000, 0.8660254037844387076, 1.000000000000000000, 0.8660254037844387076, 1.000000000000000000, 0.8660254037844387076, 1.000000000000000000, 0.8660254037844387076, 1.000000000000000000, 0.8660254037844387076, 1.000000000000000000, 0.8660254037844387076, 1.000000000000000000, 0.8660254037844387076, 1.000000000000000000, 0.8660254037844387076, 1.000000000000000000, 0.8660254037844387076, 1.000000000000000000, 0.8660254037844387076, 1.000000000000000000, 0.8660254037844387076, 1.000000000000000000, 0.8660254037844387076, 1.000000000000000000, 0.8660254037844387076, 1.000000000000000000, 0.8660254037844387076, 1.000000000000000000, 0.8660254037844387076, 1.000000000000000000, 0.8660254037844387076, 1.000000000000000000, 0.8660254037844387076, 1.000000000000000000, 0.8660254037844387076, 1.000000000000000000, 0.8660254037844387076, 1.000000000000000000, 0.8660254037844387076, 1.000000000000000000, 0.8660254037844387076, 1.000000000000000000, 0.8660254037844387076, 1.000000000000000000, 0.8660254037844387076, 1.000000000000000000, 0.8660254037844387076, 1.000000000000000000, 0.8660254037844387076, 1.000000000000000000, 0.8660254037844387076, 1.000000000000000000, 0.8660254037844387076, 1.000000000000000000, 0.8660254037844387076, 1.000000000000000000, 0.8660254037844387076, 1.000000000000000000, 0.8660254037844387076, 1.000000000000000000, 0.8660254037844387076, 1.000000000000000000, 0.8660254037844387076, 1.000000000000000000, 0.8660254037844387076, 1.000000000000000000, 0.8660254037844387076, 1.000000000000000000, 0.8660254037844387076, 1.000000000000000000, 0.8660254037844387076, 1.000000000000000000, 0.8660254037844387076, 1.000000000000000000, 0.8660254037844387076, 1.000000000000000000, 0.8660254037844387076, 1.000000000000000000, 0.8660254037844387076, 1.000000000000000000, 0.8660254037844387076, 1.000000000000000000, 0.8660254037844387076, 1.000000000000000000, 0.8660254037844387076, 1.000000000000000000, 0.8660254037844387076, 1.000000000000000000, 0.8660254037844387076, 1.000000000000000000, 0.8660254037844387076, 1.000000000000000000, 0.8660254037844387076, 1.000000000000000000, 0.8660254037844387076, 1.000000000000000000, 0.8660254037844387076, 1.000000000000000000, 0.8660254037844387076, 1.000000000000000000, 0.8660254037844387076, 1.000000000000000000, 0.8660254037844387076, 1.000000000000000000, 0.8660254037844387076, 1.000000000000000000, 0.8660254037844387076, 1.000000000000000000, 0.8660254037844387076, 1.000000000000000000, 0.8660254037844387076, 1.000000000000000000, 0.8660254037844387076, 1.000000000000000000, 0.8660254037844387076, 1.000000000000000000, 0.8660254037844387076, 1.000000000000000000, 0.8660254037844387076, 1.000000000000000000, 0.8660254037844387076, 1.000000000000000000, 0.8660254037844387076, 1.000000000000000000, 0.8660254037844387076, 1.000000000000000000, 0.8660254037844387076, 1.000000000000000000, 0.8660254037844387076, 1.000000000000000000, 0.8660254037844387076, 1.000000000000000000, 0.8660254037844387076, 1.000000000000000000, 0.8660254037844387076, 1.000000000000000000, 0.8660254037844387076, 1.000000000000000000, 0.8660254037844387076, 1.000000000000000000, 0.8660254037844387076, 1.000000000000000000, 0.8660254037844387076, 1.000000000000000000, 0.8660254037844387076, 1.000000000000000000, 0.8660254037844387076, 1.000000000000000000, 0.8660254037844387076, 1.000000000000000000, 0.8660254037844387076, 1.000000000000000000, 0.8660254037844387076, 1.000000000000000000, 0.8660254037844387076, 1.000000000000000000, 0.8660254037844387076, 1.000000000000000000, 0.8660254037844387076, 1.000000000000000000, 0.8660254037844387076, 1.000000000000000000, 0.8660254037844387076, 1.000000000000000000, 0.8660254037844387076, 1.000000000000000000, 0.8660254037844387076, 1.000000000000000000, 0.8660254037844387076, 1.000000000000000000, 0.8660254037844387076, 1.000000000000000000, 0.8660254037844387076, 1.000000000000000000, 0.8660254037844387076, 1.000000000000000000, 0.8660254037844387076, 1.000000000000000000, 0.8660254037844387076, 1.000000000000000000, 0.8660254037844387076, 1.000000000000000000, 0.8660254037844387076, 1.000000000000000000, 0.8660254037844387076, 1.000000000000000000, 0.8660254037844387076, 1.000000000000000000, 0.8660254037844387076, 1.000000000000000000, 0.8660254037844387076, 1.000000000000000000, 0.8660254037844387076, 1.000000000000000000, 0.8660254037844387076, 1.000000000000000000, 0.8660254037844387076, 1.000000000000000000, 0.8660254037844387076, 1.000000000000000000, 0.8660254037844387076, 1.000000000000000000, 0.8660254037844387076, 1.000000000000000000, 0.8660254037844387076, 1.000000000000000000, 0.8660254037844387076, 1.000000000000000000, 0.8660254037844387076, 1.000000000000000000, 0.8660254037844387076, 1.000000000000000000, 0.8660254037844387076, 1.000000000000000000, 0.8660254037844387076, 1.000000000000000000, 0.8660254037844387076, 1.000000000000000000, 0.8660254037844387076, 1.000000000000000000, 0.8660254037844387076, 1.000000000000000000, 0.8660254037844387076, 1.000000000000000000, 0.8660254037844387076, 1.000000000000000000, 0.8660254037844387076, 1.000000000000000000, 0.8660254037844387076, 1.000000000000000000, 0.8660254037844387076, 1.000000000000000000, 0.8660254037844387076, 1.000000000000000000, 0.8660254037844387076, 1.000000000000000000, 0.8660254037844387076, 1.000000000000000000, 0.8660254037844387076, 1.000000000000000000, 0.8660254037844387076, 1.000000000000000000, 0.8660254037844387076, 1.000000000000000000, 0.8660254037844387076, 1.000000000000000000, 0.8660254037844387076, 1.000000000000000000, 0.8660254037844387076, 1.000000000000000000, 0.8660254037844387076, 1.000000000000000000, 0.8660254037844387076, 1.000000000000000000, 0.8660254037844387076, 1.000000000000000000, 0.8660254037844387076, 1.000000000000000000, 0.8660254037844387076, 1.000000000000000000, 0.8660254037844387076, 1.000000000000000000, 0.8660254037844387076, 1.000000000000000000, 0.8660254037844387076, 1.000000000000000000, 0.8660254037844387076, 1.000000000000000000, 0.8660254037844387076, 1.000000000000000000, 0.8660254037844387076, 1.000000000000000000, 0.8660254037844387076, 1.000000000000000000, 0.8660254037844387076, 1.000000000000000000, 0.8660254037844387076, 1.000000000000000000, 0.8660254037844387076, 1.000000000000000000, 0.8660254037844387076, 1.000000000000000000, 0.8660254037844387076, 1.000000000000000000, 0.8660254037844387076, 1.000000000000000000, 0.8660254037844387076, 1.000000000000000000, 0.8660254037844387076, 1.000000000000000000, 0.8660254037844387076, 1.000000000000000000, 0.8660254037844387076, 1.000000000000000000, 0.8660254037844387076, 1.000000000000000000, 0.8660254037844387076, 1.000000000000000000, 0.8660254037844387076, 1.000000000000000000, 0.8660254037844387076, 1.000000000000000000, 0.8660254037844387076, 1.000000000000000000, 0.8660254037844387076, 1.000000000000000000, 0.8660254037844387076, 1.000000000000000000, 0.8660254037844387076, 1.000000000000000000, 0.8660254037844387076, 1.000000000000000000, 0.8660254037844387076, 1.000000000000000000, 0.8660254037844387076, 1.000000000000000000, 0.8660254037844387076, 1.000000000000000000, 0.8660254037844387076, 1.000000000000000000, 0.8660254037844387076, 1.000000000000000000, 0.8660254037844387076, 1.000000000000000000, 0.8660254037844387076, 1.000000000000000000, 0.8660254037844387076, 1.000000000000000000, 0.8660254037844387076, 1.000000000000000000, 0.8660254037844387076, 1.000000000000000000, 0.8660254037844387076, 1.000000000000000000, 0.8660254037844387076, 1.000000000000000000, 0.8660254037844387076, 1.000000000000000000, 0.8660254037844387076, 1.000000000000000000, 0.8660254037844387076, 1.000000000000000000, 0.8660254037844387076, 1.000000000000000000, 0.8660254037844387076, 1.000000000000000000, 0.8660254037844387076, 1.000000000000000000, 0.8660254037844387076, 1.000000000000000000, 0.8660254037844387076, 1.000000000000000000, 0.8660254037844387076, 1.000000000000000000, 0.8660254037844387076, 1.000000000000000000, 0.8660254037844387076, 1.000000000000000000, 0.8660254037844387076, 1.000000000000000000, 0.8660254037844387076, 1.000000000000000000, 0.8660254037844387076, 1.000000000000000000, 0.8660254037844387076, 1.000000000000000000, 0.8660254037844387076, 1.000000000000000000, 0.8660254037844387076, 1.000000000000000000, 0.8660254037844387076, 1.000000000000000000, 0.8660254037844387076, 1.000000000000000000, 0.8660254037844387076, 1.000000000000000000, 0.8660254037844387076, 1.000000000000000000, 0.8660254037844387076, 1.000000000000000000, 0.8660254037844387076, 1.000000000000000000, 0.8660254037844387076, 1.000000000000000000, 0.8660254037844387076, 1.000000000000000000, 0.8660254037844387076, 1.000000000000000000, 0.8660254037844387076, 1.000000000000000000, 0.8660254037844387076, 1.000000000000000000, 0.8660254037844387076, 1.000000000000000000, 0.8660254037844387076, 1.000000000000000000, 0.8660254037844387076, 1.000000000000000000, 0.8660254037844387076, 1.000000000000000000, 0.8660254037844387076, 1.000000000000000000, 0.8660254037844387076, 1.000000000000000000, 0.8660254037844387076, 1.000000000000000000, 0.8660254037844387076, 1.000000000000000000, 0.8660254037844387076, 1.000000000000000000, 0.8660254037844387076, 1.000000000000000000, 0.8660254037844387076, 1.000000000000000000, 0.8660254037844387076, 1.000000000000000000, 0.8660254037844387076, 1.000000000000000000, 0.8660254037844387076, 1.000000000000000000, 0.8660254037844387076, 1.000000000000000000, 0.8660254037844387076, 1.000000000000000000, 0.8660254037844387076, 1.000000000000000000, 0.8660254037844387076, 1.000000000000000000, 0.8660254037844387076, 1.000000000000000000, 0.8660254037844387076, 1.000000000000000000, 0.8660254037844387076, 1.000000000000000000, 0.8660254037844387076, 1.000000000000000000, 0.8660254037844387076, 1.000000000000000000, 0.8660254037844387076, 1.000000000000000000, 0.8660254037844387076, 1.000000000000000000, 0.8660254037844387076, 1.000000000000000000, 0.8660254037844387076, 1.000000000000000000, 0.8660254037844387076, 1.000000000000000000, 0.8660254037844387076, 1.000000000000000000, 0.8660254037844387076, 1.000000000000000000, 0.8660254037844387076, 1.000000000000000000, 0.8660254037844387076, 1.000000000000000000, 0.8660254037844387076, 1.000000000000000000, 0.8660254037844387076, 1.000000000000000000, 0.8660254037844387076, 1.000000000000000000, 0.8660254037844387076, 1.000000000000000000, 0.8660254037844387076, 1.000000000000000000, 0.8660254037844387076, 1.000000000000000000, 0.8660254037844387076, 1.000000000000000000, 0.8660254037844387076, 1.000000000000000000, 0.8660254037844387076, 1.000000000000000000, 0.8660254037844387076, 1.000000000000000000, 0.8660254037844387076, 1.000000000000000000, 0.8660254037844387076, 1.000000000000000000, 0.8660254037844387076, 1.000000000000000000, 0.8660254037844387076, 1.000000000000000000, 0.8660254037844387076, 1.000000000000000000, 0.8660254037844387076, 1.000000000000000000, 0.8660254037844387076, 1.000000000000000000, 0.8660254037844387076, 1.000000000000000000, 0.8660254037844387076, 1.000000000000000000, 0.8660254037844387076, 1.000000000000000000, 0.8660254037844387076, 1.000000000000000000, 0.8660254037844387076, 1.000000000000000000, 0.8660254037844387076, 1.000000000000000000, 0.8660254037844387076, 1.000000000000000000, 0.8660254037844387076, 1.000000000000000000, 0.8660254037844387076, 1.000000000000000000, 0.8660254037844387076, 1.000000000000000000, 0.8660254037844387076, 1.000000000000000000, 0.8660254037844387076, 1.000000000000000000, 0.8660254037844387076, 1.000000000000000000, 0.8660254037844387076, 1.000000000000000000, 0.8660254037844387076, 1.000000000000000000, 0.8660254037844387076, 1.000000000000000000, 0.8660254037844387076, 1.000000000000000000, 0.8660254037844387076, 1.000000000000000000, 0.8660254037844387076, 1.000000000000000000, 0.8660254037844387076, 1.000000000000000000, 0.8660254037844387076, 1.000000000000000000, 0.8660254037844387076, 1.000000000000000000, 0.8660254037844387076, 1.000000000000000000, 0.8660254037844387076, 1.000000000000000000, 0.8660254037844387076, 1.000000000000000000, 0.8660254037844387076, 1.000000000000000000, 0.8660254037844387076, 1.000000000000000000, 0.8660254037844387076, 1.000000000000000000, 0.8660254037844387076, 1.000000000000000000, 0.8660254037844387076, 1.000000000000000000, 0.8660254037844387076, 1.000000000000000000, 0.8660254037844387076, 1.000000000000000000, 0.8660254037844387076, 1.000000000000000000, 0.8660254037844387076, 1.000000000000000000, 0.8660254037844387076, 1.000000000000000000, 0.8660254037844387076, 1.000000000000000000, 0.8660254037844387076, 1.000000000000000000, 0.8660254037844387076, 1.000000000000000000, 0.8660254037844387076, 1.000000000000000000, 0.8660254037844387076, 1.000000000000000000, 0.8660254037844387076, 1.000000000000000000, 0.8660254037844387076, 1.000000000000000000, 0.8660254037844387076, 1.000000000000000000, 0.8660254037844387076, 1.000000000000000000, 0.8660254037844387076, 1.000000000000000000, 0.8660254037844387076, 1.000000000000000000, 0.8660254037844387076, 1.000000000000000000, 0.8660254037844387076, 1.000000000000000000, 0.8660254037844387076, 1.000000000000000000, 0.8660254037844387076, 1.000000000000000000, 0.8660254037844387076, 1.000000000000000000, 0.8660254037844387076, 1.000000000000000000, 0.8660254037844387076, 1.000000000000000000, 0.8660254037844387076, 1.000000000000000000, 0.8660254037844387076, 1.000000000000000000, 0.8660254037844387076, 1.000000000000000000, 0.8660254037844387076, 1.000000000000000000, 0.8660254037844387076, 1.000000000000000000, 0.8660254037844387076, 1.000000000000000000, 0.8660254037844387076, 1.000000000000000000, 0.8660254037844387076, 1.000000000000000000, 0.8660254037844387076, 1.000000000000000000, 0.8660254037844387076, 1.000000000000000000, 0.8660254037844387076, 1.000000000000000000, 0.8660254037844387076, 1.000000000000000000, 0.8660254037844387076, 1.000000000000000000, 0.8660254037844387076, 1.000000000000000000, 0.8660254037844387076, 1.000000000000000000, 0.8660254037844387076, 1.000000000000000000, 0.8660254037844387076, 1.000000000000000000, 0.8660254037844387076, 1.000000000000000000, 0.8660254037844387076, 1.000000000000000000, 0.8660254037844387076, 1.000000000000000000, 0.8660254037844387076, 1.000000000000000000, 0.8660254037844387076, 1.000000000000000000, 0.8660254037844387076, 1.000000000000000000, 0.8660254037844387076, 1.000000000000000000, 0.8660254037844387076, 1.000000000000000000, 0.8660254037844387076, 1.000000000000000000, 0.8660254037844387076, 1.000000000000000000, 0.8660254037844387076, 1.000000000000000000, 0.8660254037844387076, 1.000000000000000000, 0.8660254037844387076, 1.000000000000000000, 0.8660254037844387076, 1.000000000000000000, 0.8660254037844387076, 1.000000000000000000, 0.8660254037844387076, 1.000000000000000000, 0.8660254037844387076, 1.000000000000000000, 0.8660254037844387076, 1.000000000000000000, 0.8660254037844387076, 1.000000000000000000, 0.8660254037844387076, 1.000000000000000000, 0.8660254037844387076, 1.000000000000000000, 0.8660254037844387076, 1.000000000000000000, 0.8660254037844387076, 1.000000000000000000, 0.8660254037844387076, 1.000000000000000000, 0.8660254037844387076, 1.000000000000000000, 0.8660254037844387076, 1.000000000000000000, 0.8660254037844387076, 1.000000000000000000, 0.8660254037844387076, 1.000000000000000000, 0.8660254037844387076, 1.000000000000000000, 0.8660254037844387076, 1.000000000000000000, 0.8660254037844387076, 1.000000000000000000, 0.8660254037844387076, 1.000000000000000000, 0.8660254037844387076, 1.000000000000000000, 0.8660254037844387076, 1.000000000000000000, 0.8660254037844387076, 1.000000000000000000, 0.8660254037844387076, 1.000000000000000000, 0.8660254037844387076, 1.000000000000000000, 0.8660254037844387076, 1.000000000000000000, 0.8660254037844387076, 1.000000000000000000, 0.8660254037844387076, 1.000000000000000000, 0.8660254037844387076, 1.000000000000000000, 0.8660254037844387076, 1.000000000000000000, 0.8660254037844387076, 1.000000000000000000, 0.8660254037844387076, 1.000000000000000000, 0.8660254037844387076, 1.000000000000000000, 0.8660254037844387076, 1.000000000000000000, 0.8660254037844387076, 1.000000000000000000, 0.8660254037844387076, 1.000000000000000000, 0.8660254037844387076, 1.000000000000000000, 0.8660254037844387076, 1.000000000000000000, 0.8660254037844387076, 1.000000000000000000, 0.8660254037844387076, 1.000000000000000000, 0.8660254037844387076, 1.000000000000000000, 0.8660254037844387076, 1.000000000000000000, 0.8660254037844387076, 1.000000000000000000, 0.8660254037844387076, 1.000000000000000000, 0.8660254037844387076, 1.000000000000000000, 0.8660254037844387076, 1.000000000000000000, 0.8660254037844387076, 1.000000000000000000, 0.8660254037844387076, 1.000000000000000000, 0.8660254037844387076, 1.000000000000000000, 0.8660254037844387076, 1.000000000000000000, 0.8660254037844387076, 1.000000000000000000, 0.8660254037844387076, 1.000000000000000000, 0.8660254037844387076, 1.000000000000000000, 0.8660254037844387076, 1.000000000000000000, 0.8660254037844387076, 1.000000000000000000, 0.8660254037844387076, 1.000000000000000000, 0.8660254037844387076, 1.000000000000000000, 0.8660254037844387076, 1.000000000000000000, 0.8660254037844387076, 1.000000000000000000, 0.8660254037844387076, 1.000000000000000000, 0.8660254037844387076, 1.000000000000000000, 0.8660254037844387076, 1.000000000000000000, 0.8660254037844387076, 1.000000000000000000, 0.8660254037844387076, 1.000000000000000000, 0.8660254037844387076, 1.000000000000000000, 0.8660254037844387076, 1.000000000000000000, 0.8660254037844387076, 1.000000000000000000, 0.8660254037844387076, 1.000000000000000000, 0.8660254037844387076, 1.000000000000000000, 0.8660254037844387076, 1.000000000000000000, 0.8660254037844387076, 1.000000000000000000, 0.8660254037844387076, 1.000000000000000000, 0.8660254037844387076, 1.000000000000000000, 0.8660254037844387076, 1.000000000000000000, 0.8660254037844387076, 1.000000000000000000, 0.8660254037844387076, 1.000000000000000000, 0.8660254037844387076, 1.000000000000000000, 0.8660254037844387076, 1.000000000000000000, 0.8660254037844387076, 1.000000000000000000, 0.8660254037844387076, 1.000000000000000000, 0.8660254037844387076, 1.000000000000000000, 0.8660254037844387076, 1.000000000000000000, 0.8660254037844387076, 1.000000000000000000, 0.8660254037844387076, 1.000000000000000000, 0.8660254037844387076, 1.000000000000000000, 0.8660254037844387076, 1.000000000000000000, 0.8660254037844387076, 1.000000000000000000, 0.8660254037844387076, 1.000000000000000000, 0.8660254037844387076, 1.000000000000000000, 0.8660254037844387076, 1.000000000000000000, 0.8660254037844387076, 1.000000000000000000, 0.8660254037844387076, 1.000000000000000000, 0.8660254037844387076, 1.000000000000000000, 0.8660254037844387076, 1.000000000000000000, 0.8660254037844387076, 1.000000000000000000, 0.8660254037844387076, 1.000000000000000000, 0.8660254037844387076, 1.000000000000000000, 0.8660254037844387076, 1.000000000000000000, 0.8660254037844387076, 1.000000000000000000, 0.8660254037844387076, 1.000000000000000000, 0.8660254037844387076, 1.000000000000000000, 0.8660254037844387076, 1.000000000000000000, 0.8660254037844387076, 1.000000000000000000, 0.8660254037844387076, 1.000000000000000000, 0.8660254037844387076, 1.000000000000000000, 0.8660254037844387076, 1.000000000000000000, 0.8660254037844387076, 1.000000000000000000, 0.8660254037844387076, 1.000000000000000000, 0.8660254037844387076, 1.000000000000000000, 0.8660254037844387076, 1.000000000000000000, 0.8660254037844387076, 1.000000000000000000, 0.8660254037844387076, 1.000000000000000000, 0.8660254037844387076, 1.000000000000000000, 0.8660254037844387076, 1.000000000000000000, 0.8660254037844387076, 1.000000000000000000, 0.8660254037844387076, 1.000000000000000000, 0.8660254037844387076, 1.000000000000000000, 0.8660254037844387076, 1.000000000000000000, 0.8660254037844387076, 1.000000000000000000, 0.8660254037844387076, 1.000000000000000000, 0.8660254037844387076, 1.000000000000000000, 0.8660254037844387076, 1.000000000000000000, 0.8660254037844387076, 1.000000000000000000, 0.8660254037844387076, 1.000000000000000000, 0.8660254037844387076, 1.000000000000000000, 0.8660254037844387076, 1.000000000000000000, 0.8660254037844387076, 1.000000000000000000, 0.8660254037844387076, 1.000000000000000000, 0.8660254037844387076, 1.000000000000000000, 0.8660254037844387076, 1.000000000000000000, 0.8660254037844387076, 1.000000000000000000, 0.8660254037844387076, 1.000000000000000000, 0.8660254037844387076, 1.000000000000000000, 0.8660254037844387076, 1.000000000000000000, 0.8660254037844387076, 1.000000000000000000, 0.8660254037844387076, 1.000000000000000000, 0.8660254037844387076, 1.000000000000000000, 0.8660254037844387076, 1.000000000000000000, 0.8660254037844387076, 1.000000000000000000, 0.8660254037844387076, 1.000000000000000000, 0.8660254037844387076, 1.000000000000000000, 0.8660254037844387076, 1.000000000000000000, 0.8660254037844387076, 1.000000000000000000, 0.8660254037844387076, 1.000000000000000000, 0.8660254037844387076, 1.000000000000000000, 0.8660254037844387076, 1.000000000000000000, 0.8660254037844387076, 1.000000000000000000, 0.8660254037844387076, 1.000000000000000000, 0.8660254037844387076, 1.000000000000000000, 0.8660254037844387076, 1.000000000000000000, 0.8660254037844387076, 1.000000000000000000, 0.8660254037844387076, 1.000000000000000000, 0.8660254037844387076, 1.000000000000000000, 0.8660254037844387076, 1.000000000000000000, 0.8660254037844387076, 1.000000000000000000, 0.8660254037844387076, 1.000000000000000000, 0.8660254037844387076, 1.000000000000000000, 0.8660254037844387076, 1.000000000000000000, 0.8660254037844387076, 1.000000000000000000, 0.8660254037844387076, 1.000000000000000000, 0.8660254037844387076, 1.000000000000000000, 0.8660254037844387076, 1.000000000000000000, 0.8660254037844387076, 1.000000000000000000, 0.8660254037844387076, 1.000000000000000000, 0.8660254037844387076, 1.000000000000000000, 0.8660254037844387076, 1.000000000000000000, 0.8660254037844387076, 1.000000000000000000, 0.8660254037844387076, 1.000000000000000000, 0.8660254037844387076, 1.000000000000000000, 0.8660254037844387076, 1.000000000000000000, 0.8660254037844387076, 1.000000000000000000, 0.8660254037844387076, 1.000000000000000000, 0.8660254037844387076, 1.000000000000000000, 0.8660254037844387076, 1.000000000000000000, 0.8660254037844387076, 1.000000000000000000, 0.8660254037844387076, 1.000000000000000000, 0.8660254037844387076, 1.000000000000000000, 0.8660254037844387076, 1.000000000000000000, 0.8660254037844387076, 1.000000000000000000, 0.8660254037844387076, 1.000000000000000000, 0.8660254037844387076, 1.000000000000000000) ) ) 
 REPRESENTATION_ITEM ( '' )  SURFACE ( )  );
#32272 = CARTESIAN_POINT ( 'NONE',  ( -3.152548672688508926E-16, -17.81249999863440792, -5.148502694627439702 ) ) ;
#32273 = CARTESIAN_POINT ( 'NONE',  ( 5.000000000000000888, -62.45833333060214443, 2.886751345948126879 ) ) ;
#32274 = ORIENTED_EDGE ( 'NONE', *, *, #16862, .T. ) ;
#32275 = CARTESIAN_POINT ( 'NONE',  ( 5.000000000000000888, -85.45833333060213022, 2.886751345948126879 ) ) ;
#32276 = EDGE_LOOP ( 'NONE', ( #11040, #17806, #37456, #10203 ) ) ;
#32277 = CARTESIAN_POINT ( 'NONE',  ( 4.458734124999999437, -69.06249999863439371, -5.460374474430324690E-16 ) ) ;
#32278 = CARTESIAN_POINT ( 'NONE',  ( -6.972266317189433020E-16, -6.124999997268813168, -5.000000000000000000 ) ) ;
#32279 = DIRECTION ( 'NONE',  ( 0.000000000000000000, 0.000000000000000000, -1.000000000000000000 ) ) ;
#32280 = ORIENTED_EDGE ( 'NONE', *, *, #47658, .T. ) ;
#32281 = CARTESIAN_POINT ( 'NONE',  ( -2.499999999999996447, 3.291666669397851575, 4.330127018922195425 ) ) ;
#32282 = CARTESIAN_POINT ( 'NONE',  ( -59.98410592259440222, -127.1250000000000142, -0.3983568153799752487 ) ) ;
#32283 = CARTESIAN_POINT ( 'NONE',  ( -9.184850993605147944E-16, -156.2500000000000000, 5.000000000000000000 ) ) ;
#32284 = CARTESIAN_POINT ( 'NONE',  ( -2.229367062499996610, -51.39583333196773651, 3.861377020970582219 ) ) ;
#32285 = ORIENTED_EDGE ( 'NONE', *, *, #5248, .F. ) ;
#32286 = VECTOR ( 'NONE', #5282, 1000.000000000000000 ) ;
#32287 =( BOUNDED_SURFACE ( )  B_SPLINE_SURFACE ( 1, 2, ( 
 ( #39762, #15014, #25627, #54897, #21120, #11143, #54579, #10501, #15972, #50388, #5372, #10826, #30116, #30439, #557, #40727, #6336, #50067, #6022, #45241, #60374, #24990, #25942, #1207, #16297, #59088, #44597, #59408, #5052, #24670, #20806, #35920, #9864, #29474, #49746, #49106, #882, #44278, #10195, #240, #15340, #19838, #5690, #34629, #25306, #20490, #40088, #16930, #2466, #31082, #12422, #36232, #47155, #22401, #31721, #26254, #26904, #55859, #7921, #61323, #56177, #46201, #51030, #61956, #2161, #60693, #21768, #46524, #41046, #17877, #41361, #37192, #3102, #27526, #45877, #17573, #22719, #41673, #50705, #32034, #42316, #32357, #51669, #16613, #7611, #31391, #21443, #56816, #22077, #12733, #11773, #17246, #51979, #6972, #26582, #61005, #36870, #36545, #56500, #12098, #46833, #51355, #55549, #27216, #11460, #6647, #1840, #7294, #2781, #42000, #61641, #14303, #38738, #13053, #52609, #52300, #8237, #13370, #53549, #8854, #47461, #57758, #48709, #37818, #9473, #4040, #8544, #23659, #62590, #32992, #57447, #58376, #33616, #57137, #13681, #47771, #28156, #3726, #9166, #18511, #23347, #42948, #18197, #32670, #19119, #38133, #23959, #53234, #23030, #27839, #33300, #52918, #3414, #29082, #33923, #42633, #62272, #63208, #63522, #37496, #28472, #4650, #48084, #43253, #62894, #18808, #24270, #38430, #4341, #58057, #13986, #43876, #28782, #48399, #43563, #14616, #29719, #25871, #15262, #58687, #30045, #25548, #45486, #30695, #10115, #35207, #14933, #10432, #59658, #4972, #59981, #34228, #53855, #54508, #15904, #19446, #45166, #40012, #39059, #6263, #24916, #44201, #34540, #25231, #44842, #54825, #54176, #49353, #10757, #44520, #5298, #482, #166, #9784, #1135, #20084, #5942, #15590, #24594, #29392, #39688, #59328, #49028, #11072, #20734, #19763, #39374, #40338, #59005, #34886, #49674, #55146, #5617, #806, #20412, #30366, #35523, #49988, #50313, #16541, #46128, #37981, #2092, #11387, #7220, #60298, #11702, #8702, #60936, #40658, #12022, #7533, #28317, #13539, #55785, #17172, #60621, #56102, #41599, #50636, #41927, #16224, #35847, #36476, #61569, #1450, #27145, #22005, #21051, #52774, #6897, #26189, #36164, #26833, #46450, #36798, #55471, #61250, #17503, #57612, #56430, #6574, #12352, #40975, #31007, #46761, #31652, #2706, #21370, #2395, #22325, #45808, #1768, #31322, #51287, #50957, #31964, #26511, #51598, #21696, #33160, #41287, #16854, #49201, #5141, #43732, #3887, #29570, #28938, #24760, #44363, #23505, #63062, #62749, #18670, #23815, #325, #19290, #57921, #4503, #59175, #48246, #19924, #14463, #18974, #34085, #9325, #43419, #4202, #39537, #44043, #43108, #24129, #58221, #29249, #38588, #39223, #28629, #15109, #24440, #38293, #34725, #54353, #63375, #13840, #10283, #48563, #47932, #33460, #53082, #14150, #9018, #33775, #53394, #38908, #58541, #53708, #9641, #48873, #4821, #10, #19610, #58847, #14777, #34394, #54021, #9955, #31172, #26039, #49518, #50154, #40191, #25396, #59827, #1611, #54987, #981, #15749, #10592, #25074, #11554, #10915, #16389, #45654, #15438, #645, #30531, #6108, #20257, #21537, #50804, #5457, #39856, #55639, #55949, #29888, #44684, #1934, #35365, #25723, #45015, #11235, #6740, #16064, #60464, #20584, #45333, #41133, #1303, #59499, #35693, #35056, #20899, #36322, #40502, #54668, #60143, #36008, #30206, #60781, #55320, #21211, #30859, #50488, #6427, #49832, #26348, #5775, #40817, #45970, #16707, #37906, #17958, #32441, #11864, #62358, #17338, #36637, #7382, #17658, #37274, #47245, #7060, #52070, #27926, #52391, #8011, #61098, #27614, #51442, #41448, #37581, #22491, #57222, #31808, #56902, #32761, #17022, #12193, #22168, #61729, #56269, #26672, #46292, #26989, #47547, #46927, #21853, #32119, #23111, #46608, #3497, #42087, #2554, #12820, #36958, #41765, #61415, #13142, #3191, #31480 ),
 ( #56588, #2249, #12507, #51755, #7699, #42715, #8326, #51124, #27302, #18281, #2876, #22807, #42400, #62042, #23749, #53320, #8940, #38827, #14701, #43651, #24362, #28554, #38514, #29482, #58142, #3811, #63291, #52693, #4127, #250, #9253, #33080, #4427, #63611, #19848, #5060, #48175, #9566, #53001, #48490, #34011, #43036, #34320, #8628, #28240, #28868, #53945, #57536, #19531, #14388, #13461, #44288, #62987, #18598, #43344, #19210, #58464, #29173, #47854, #53634, #9874, #49117, #48797, #62676, #4738, #33386, #23435, #39145, #24052, #58772, #13764, #43965, #24680, #38224, #57846, #18900, #14072, #33700, #894, #24998, #35287, #5382, #50075, #40099, #39462, #6033, #25636, #30126, #59098, #45251, #10512, #1218, #20816, #34640, #39774, #567, #49440, #40417, #44936, #60057, #44607, #20500, #15025, #20176, #59420, #34973, #59742, #15350, #15668, #54590, #54265, #49755, #10204, #30450, #29807, #5701, #25316, #54907, #10835, #18025, #17413, #13206, #37647, #11929, #51509, #51193, #7125, #12261, #52457, #7757, #46357, #56654, #47612, #36708, #8392, #2942, #7446, #22556, #61480, #31875, #56341, #57290, #32504, #56016, #12571, #46672, #27054, #2617, #8078, #37028, #22235, #41835, #17087, #31560, #32828, #32184, #22872, #52136, #21914, #26741, #51815, #27360, #2311, #27993, #3566, #41511, #61164, #62106, #62429, #36385, #46994, #23173, #42157, #61793, #17720, #37334, #42784, #56967, #3260, #12886, #27679, #47307, #42465, #28305, #24120, #13530, #28620, #24748, #14137, #57603, #28930, #24432, #44353, #29559, #9008, #34076, #13832, #9316, #58530, #3877, #58838, #33150, #52764, #53383, #14767, #18347, #44034, #38895, #37970, #5130, #23806, #43098, #33451, #43720, #63365, #53699, #8693, #14454, #34385, #54013, #9631, #23496, #29239, #9943, #47919, #38283, #48235, #62739, #18661, #48864, #49192, #4809, #57909, #18964, #53068, #48553, #9216, #4193, #19601, #43408, #63053, #38579, #58210, #39213, #33764, #4492, #19280, #10906, #39528, #20889, #44675, #55629, #30848, #40181, #34715, #35356, #635, #16379, #6099, #972, #54659, #59490, #6729, #10582, #5447, #30194, #54977, #49508, #26339, #49823, #45644, #11544, #35998, #54342, #26029, #31161, #50144, #15426, #21200, #10274, #35047, #45324, #50791, #316, #15739, #20245, #50479, #15098, #6419, #5767, #1292, #19914, #59166, #25712, #1602, #25385, #59817, #16054, #40806, #29878, #60454, #25065, #39847, #45006, #40492, #60133, #20574, #30521, #35682, #55310, #11225, #62052, #51138, #41779, #55963, #21863, #37283, #26686, #47255, #22500, #1946, #3200, #22820, #61425, #21547, #27626, #26998, #42409, #17966, #41142, #61108, #60790, #16716, #41459, #37590, #17348, #11874, #2563, #57233, #46302, #13150, #12517, #17033, #32128, #7391, #36647, #2260, #32770, #42096, #36333, #22177, #51764, #31492, #56278, #52405, #36972, #7071, #56599, #52082, #8336, #45980, #12204, #61741, #31821, #7708, #17668, #51454, #46618, #27312, #46939, #2888, #56912, #12830, #8020, #32450, #27935, #14714, #33398, #52704, #23444, #33711, #53330, #63304, #23120, #4437, #43979, #4750, #48500, #13473, #24067, #3823, #57545, #53645, #38525, #9579, #47864, #9264, #48812, #33089, #28250, #63625, #8638, #23759, #37915, #43046, #19226, #62686, #29185, #43663, #47559, #24378, #19546, #43355, #3508, #39159, #8953, #58784, #34334, #42724, #18607, #62368, #18292, #38235, #53958, #63002, #57855, #48185, #13776, #53012, #28564, #58153, #4138, #14084, #18911, #28879, #38841, #58476, #14402, #34024, #30140, #20190, #5396, #39791, #45267, #34989, #44622, #59437, #54279, #5074, #55251, #54604, #60076, #6046, #59112, #44300, #10527, #49769, #264, #1543, #11170, #29499, #19862, #35623, #35945, #9890, #49131, #45585, #15366, #5715, #25012, #54923, #30793, #59757, #40435, #581, #25330, #21147, #44952, #39476, #912, #15999 ) ),
 .UNSPECIFIED., .F., .F., .F. ) 
 B_SPLINE_SURFACE_WITH_KNOTS ( ( 2, 2 ),
 ( 3, 2, 2, 2, 2, 2, 2, 2, 2, 2, 2, 2, 2, 2, 2, 2, 2, 2, 2, 2, 2, 2, 2, 2, 2, 2, 2, 2, 2, 2, 2, 2, 2, 2, 2, 2, 2, 2, 2, 2, 2, 2, 2, 2, 2, 2, 2, 2, 2, 2, 2, 2, 2, 2, 2, 2, 2, 2, 2, 2, 2, 2, 2, 2, 2, 2, 2, 2, 2, 2, 2, 2, 2, 2, 2, 2, 2, 2, 2, 2, 2, 2, 2, 2, 2, 2, 2, 2, 2, 2, 2, 2, 2, 2, 2, 2, 2, 2, 2, 2, 2, 2, 2, 2, 2, 2, 2, 2, 2, 2, 2, 2, 2, 2, 2, 2, 2, 2, 2, 2, 2, 2, 2, 2, 2, 2, 2, 2, 2, 2, 2, 2, 2, 2, 2, 2, 2, 2, 2, 2, 2, 2, 2, 2, 2, 2, 2, 2, 2, 2, 2, 2, 2, 2, 2, 2, 2, 2, 2, 2, 2, 2, 2, 2, 2, 2, 2, 2, 2, 2, 2, 2, 2, 2, 2, 2, 2, 2, 2, 2, 2, 2, 2, 2, 2, 2, 2, 2, 2, 2, 2, 2, 2, 2, 2, 2, 2, 2, 2, 2, 2, 2, 2, 2, 2, 2, 2, 2, 2, 2, 2, 2, 2, 2, 2, 2, 2, 2, 2, 2, 2, 2, 2, 2, 2, 2, 2, 2, 2, 2, 2, 2, 2, 2, 2, 2, 2, 2, 2, 2, 3 ),
 ( 0.000000000000000000, 1.000000000000000000 ),
 ( 0.000000000000000000, 0.004166666666666666609, 0.008333333333333333218, 0.01250000000000000069, 0.01666666666666666644, 0.02083333333333333218, 0.02500000000000000139, 0.02916666666666666713, 0.03333333333333333287, 0.03749999999999999861, 0.04166666666666666435, 0.04583333333333333010, 0.05000000000000000278, 0.05416666666666666852, 0.05833333333333333426, 0.06250000000000000000, 0.06666666666666666574, 0.07083333333333333148, 0.07499999999999999722, 0.07916666666666666297, 0.08333333333333332871, 0.08749999999999999445, 0.09166666666666666019, 0.09583333333333333981, 0.1000000000000000056, 0.1041666666666666713, 0.1083333333333333370, 0.1125000000000000028, 0.1166666666666666685, 0.1208333333333333343, 0.1250000000000000000, 0.1291666666666666796, 0.1333333333333333315, 0.1375000000000000111, 0.1416666666666666630, 0.1458333333333333426, 0.1499999999999999944, 0.1541666666666666741, 0.1583333333333333259, 0.1625000000000000056, 0.1666666666666666574, 0.1708333333333333370, 0.1749999999999999889, 0.1791666666666666685, 0.1833333333333333204, 0.1875000000000000000, 0.1916666666666666796, 0.1958333333333333315, 0.2000000000000000111, 0.2041666666666666630, 0.2083333333333333426, 0.2124999999999999944, 0.2166666666666666741, 0.2208333333333333259, 0.2250000000000000056, 0.2291666666666666574, 0.2333333333333333370, 0.2374999999999999889, 0.2416666666666666685, 0.2458333333333333204, 0.2500000000000000000, 0.2541666666666666519, 0.2583333333333333592, 0.2625000000000000111, 0.2666666666666666630, 0.2708333333333333148, 0.2750000000000000222, 0.2791666666666666741, 0.2833333333333333259, 0.2874999999999999778, 0.2916666666666666852, 0.2958333333333333370, 0.2999999999999999889, 0.3041666666666666408, 0.3083333333333333481, 0.3125000000000000000, 0.3166666666666666519, 0.3208333333333333592, 0.3250000000000000111, 0.3291666666666666630, 0.3333333333333333148, 0.3375000000000000222, 0.3416666666666666741, 0.3458333333333333259, 0.3499999999999999778, 0.3541666666666666852, 0.3583333333333333370, 0.3624999999999999889, 0.3666666666666666408, 0.3708333333333333481, 0.3750000000000000000, 0.3791666666666666519, 0.3833333333333333592, 0.3875000000000000111, 0.3916666666666666630, 0.3958333333333333148, 0.4000000000000000222, 0.4041666666666666741, 0.4083333333333333259, 0.4124999999999999778, 0.4166666666666666852, 0.4208333333333333370, 0.4249999999999999889, 0.4291666666666666408, 0.4333333333333333481, 0.4375000000000000000, 0.4416666666666666519, 0.4458333333333333592, 0.4500000000000000111, 0.4541666666666666630, 0.4583333333333333148, 0.4625000000000000222, 0.4666666666666666741, 0.4708333333333333259, 0.4749999999999999778, 0.4791666666666666852, 0.4833333333333333370, 0.4874999999999999889, 0.4916666666666666408, 0.4958333333333333481, 0.5000000000000000000, 0.5041666666666666519, 0.5083333333333333037, 0.5124999999999999556, 0.5166666666666667185, 0.5208333333333333703, 0.5250000000000000222, 0.5291666666666666741, 0.5333333333333333259, 0.5374999999999999778, 0.5416666666666666297, 0.5458333333333332815, 0.5500000000000000444, 0.5541666666666666963, 0.5583333333333333481, 0.5625000000000000000, 0.5666666666666666519, 0.5708333333333333037, 0.5749999999999999556, 0.5791666666666667185, 0.5833333333333333703, 0.5875000000000000222, 0.5916666666666666741, 0.5958333333333333259, 0.5999999999999999778, 0.6041666666666666297, 0.6083333333333332815, 0.6125000000000000444, 0.6166666666666666963, 0.6208333333333333481, 0.6250000000000000000, 0.6291666666666666519, 0.6333333333333333037, 0.6374999999999999556, 0.6416666666666667185, 0.6458333333333333703, 0.6500000000000000222, 0.6541666666666666741, 0.6583333333333333259, 0.6624999999999999778, 0.6666666666666666297, 0.6708333333333332815, 0.6750000000000000444, 0.6791666666666666963, 0.6833333333333333481, 0.6875000000000000000, 0.6916666666666666519, 0.6958333333333333037, 0.6999999999999999556, 0.7041666666666667185, 0.7083333333333333703, 0.7125000000000000222, 0.7166666666666666741, 0.7208333333333333259, 0.7249999999999999778, 0.7291666666666666297, 0.7333333333333332815, 0.7375000000000000444, 0.7416666666666666963, 0.7458333333333333481, 0.7500000000000000000, 0.7541666666666666519, 0.7583333333333333037, 0.7624999999999999556, 0.7666666666666667185, 0.7708333333333333703, 0.7750000000000000222, 0.7791666666666666741, 0.7833333333333333259, 0.7874999999999999778, 0.7916666666666666297, 0.7958333333333332815, 0.8000000000000000444, 0.8041666666666666963, 0.8083333333333333481, 0.8125000000000000000, 0.8166666666666666519, 0.8208333333333333037, 0.8249999999999999556, 0.8291666666666667185, 0.8333333333333333703, 0.8375000000000000222, 0.8416666666666666741, 0.8458333333333333259, 0.8499999999999999778, 0.8541666666666666297, 0.8583333333333332815, 0.8625000000000000444, 0.8666666666666666963, 0.8708333333333333481, 0.8750000000000000000, 0.8791666666666666519, 0.8833333333333333037, 0.8874999999999999556, 0.8916666666666667185, 0.8958333333333333703, 0.9000000000000000222, 0.9041666666666666741, 0.9083333333333333259, 0.9124999999999999778, 0.9166666666666666297, 0.9208333333333332815, 0.9250000000000000444, 0.9291666666666666963, 0.9333333333333333481, 0.9375000000000000000, 0.9416666666666666519, 0.9458333333333333037, 0.9499999999999999556, 0.9541666666666667185, 0.9583333333333333703, 0.9625000000000000222, 0.9666666666666666741, 0.9708333333333333259, 0.9749999999999999778, 0.9791666666666666297, 0.9833333333333332815, 0.9875000000000000444, 0.9916666666666666963, 0.9958333333333333481, 1.000000000000000000 ),
 .UNSPECIFIED. ) 
 GEOMETRIC_REPRESENTATION_ITEM ( )  RATIONAL_B_SPLINE_SURFACE ( (
 ( 1.000000000000000000, 0.9238795325112867385, 1.000000000000000000, 0.9238795325112867385, 1.000000000000000000, 0.9238795325112867385, 1.000000000000000000, 0.9238795325112867385, 1.000000000000000000, 0.9238795325112867385, 1.000000000000000000, 0.9238795325112867385, 1.000000000000000000, 0.9238795325112867385, 1.000000000000000000, 0.9238795325112867385, 1.000000000000000000, 0.9238795325112867385, 1.000000000000000000, 0.9238795325112867385, 1.000000000000000000, 0.9238795325112867385, 1.000000000000000000, 0.9238795325112867385, 1.000000000000000000, 0.9238795325112867385, 1.000000000000000000, 0.9238795325112867385, 1.000000000000000000, 0.9238795325112867385, 1.000000000000000000, 0.9238795325112867385, 1.000000000000000000, 0.9238795325112867385, 1.000000000000000000, 0.9238795325112867385, 1.000000000000000000, 0.9238795325112867385, 1.000000000000000000, 0.9238795325112867385, 1.000000000000000000, 0.9238795325112867385, 1.000000000000000000, 0.9238795325112867385, 1.000000000000000000, 0.9238795325112867385, 1.000000000000000000, 0.9238795325112867385, 1.000000000000000000, 0.9238795325112867385, 1.000000000000000000, 0.9238795325112867385, 1.000000000000000000, 0.9238795325112867385, 1.000000000000000000, 0.9238795325112867385, 1.000000000000000000, 0.9238795325112867385, 1.000000000000000000, 0.9238795325112867385, 1.000000000000000000, 0.9238795325112867385, 1.000000000000000000, 0.9238795325112867385, 1.000000000000000000, 0.9238795325112867385, 1.000000000000000000, 0.9238795325112867385, 1.000000000000000000, 0.9238795325112867385, 1.000000000000000000, 0.9238795325112867385, 1.000000000000000000, 0.9238795325112867385, 1.000000000000000000, 0.9238795325112867385, 1.000000000000000000, 0.9238795325112867385, 1.000000000000000000, 0.9238795325112867385, 1.000000000000000000, 0.9238795325112867385, 1.000000000000000000, 0.9238795325112867385, 1.000000000000000000, 0.9238795325112867385, 1.000000000000000000, 0.9238795325112867385, 1.000000000000000000, 0.9238795325112867385, 1.000000000000000000, 0.9238795325112867385, 1.000000000000000000, 0.9238795325112867385, 1.000000000000000000, 0.9238795325112867385, 1.000000000000000000, 0.9238795325112867385, 1.000000000000000000, 0.9238795325112867385, 1.000000000000000000, 0.9238795325112867385, 1.000000000000000000, 0.9238795325112867385, 1.000000000000000000, 0.9238795325112867385, 1.000000000000000000, 0.9238795325112867385, 1.000000000000000000, 0.9238795325112867385, 1.000000000000000000, 0.9238795325112867385, 1.000000000000000000, 0.9238795325112867385, 1.000000000000000000, 0.9238795325112867385, 1.000000000000000000, 0.9238795325112867385, 1.000000000000000000, 0.9238795325112867385, 1.000000000000000000, 0.9238795325112867385, 1.000000000000000000, 0.9238795325112867385, 1.000000000000000000, 0.9238795325112867385, 1.000000000000000000, 0.9238795325112867385, 1.000000000000000000, 0.9238795325112867385, 1.000000000000000000, 0.9238795325112867385, 1.000000000000000000, 0.9238795325112867385, 1.000000000000000000, 0.9238795325112867385, 1.000000000000000000, 0.9238795325112867385, 1.000000000000000000, 0.9238795325112867385, 1.000000000000000000, 0.9238795325112867385, 1.000000000000000000, 0.9238795325112867385, 1.000000000000000000, 0.9238795325112867385, 1.000000000000000000, 0.9238795325112867385, 1.000000000000000000, 0.9238795325112867385, 1.000000000000000000, 0.9238795325112867385, 1.000000000000000000, 0.9238795325112867385, 1.000000000000000000, 0.9238795325112867385, 1.000000000000000000, 0.9238795325112867385, 1.000000000000000000, 0.9238795325112867385, 1.000000000000000000, 0.9238795325112867385, 1.000000000000000000, 0.9238795325112867385, 1.000000000000000000, 0.9238795325112867385, 1.000000000000000000, 0.9238795325112867385, 1.000000000000000000, 0.9238795325112867385, 1.000000000000000000, 0.9238795325112867385, 1.000000000000000000, 0.9238795325112867385, 1.000000000000000000, 0.9238795325112867385, 1.000000000000000000, 0.9238795325112867385, 1.000000000000000000, 0.9238795325112867385, 1.000000000000000000, 0.9238795325112867385, 1.000000000000000000, 0.9238795325112867385, 1.000000000000000000, 0.9238795325112867385, 1.000000000000000000, 0.9238795325112867385, 1.000000000000000000, 0.9238795325112867385, 1.000000000000000000, 0.9238795325112867385, 1.000000000000000000, 0.9238795325112867385, 1.000000000000000000, 0.9238795325112867385, 1.000000000000000000, 0.9238795325112867385, 1.000000000000000000, 0.9238795325112867385, 1.000000000000000000, 0.9238795325112867385, 1.000000000000000000, 0.9238795325112867385, 1.000000000000000000, 0.9238795325112867385, 1.000000000000000000, 0.9238795325112867385, 1.000000000000000000, 0.9238795325112867385, 1.000000000000000000, 0.9238795325112867385, 1.000000000000000000, 0.9238795325112867385, 1.000000000000000000, 0.9238795325112867385, 1.000000000000000000, 0.9238795325112867385, 1.000000000000000000, 0.9238795325112867385, 1.000000000000000000, 0.9238795325112867385, 1.000000000000000000, 0.9238795325112867385, 1.000000000000000000, 0.9238795325112867385, 1.000000000000000000, 0.9238795325112867385, 1.000000000000000000, 0.9238795325112867385, 1.000000000000000000, 0.9238795325112867385, 1.000000000000000000, 0.9238795325112867385, 1.000000000000000000, 0.9238795325112867385, 1.000000000000000000, 0.9238795325112867385, 1.000000000000000000, 0.9238795325112867385, 1.000000000000000000, 0.9238795325112867385, 1.000000000000000000, 0.9238795325112867385, 1.000000000000000000, 0.9238795325112867385, 1.000000000000000000, 0.9238795325112867385, 1.000000000000000000, 0.9238795325112867385, 1.000000000000000000, 0.9238795325112867385, 1.000000000000000000, 0.9238795325112867385, 1.000000000000000000, 0.9238795325112867385, 1.000000000000000000, 0.9238795325112867385, 1.000000000000000000, 0.9238795325112867385, 1.000000000000000000, 0.9238795325112867385, 1.000000000000000000, 0.9238795325112867385, 1.000000000000000000, 0.9238795325112867385, 1.000000000000000000, 0.9238795325112867385, 1.000000000000000000, 0.9238795325112867385, 1.000000000000000000, 0.9238795325112867385, 1.000000000000000000, 0.9238795325112867385, 1.000000000000000000, 0.9238795325112867385, 1.000000000000000000, 0.9238795325112867385, 1.000000000000000000, 0.9238795325112867385, 1.000000000000000000, 0.9238795325112867385, 1.000000000000000000, 0.9238795325112867385, 1.000000000000000000, 0.9238795325112867385, 1.000000000000000000, 0.9238795325112867385, 1.000000000000000000, 0.9238795325112867385, 1.000000000000000000, 0.9238795325112867385, 1.000000000000000000, 0.9238795325112867385, 1.000000000000000000, 0.9238795325112867385, 1.000000000000000000, 0.9238795325112867385, 1.000000000000000000, 0.9238795325112867385, 1.000000000000000000, 0.9238795325112867385, 1.000000000000000000, 0.9238795325112867385, 1.000000000000000000, 0.9238795325112867385, 1.000000000000000000, 0.9238795325112867385, 1.000000000000000000, 0.9238795325112867385, 1.000000000000000000, 0.9238795325112867385, 1.000000000000000000, 0.9238795325112867385, 1.000000000000000000, 0.9238795325112867385, 1.000000000000000000, 0.9238795325112867385, 1.000000000000000000, 0.9238795325112867385, 1.000000000000000000, 0.9238795325112867385, 1.000000000000000000, 0.9238795325112867385, 1.000000000000000000, 0.9238795325112867385, 1.000000000000000000, 0.9238795325112867385, 1.000000000000000000, 0.9238795325112867385, 1.000000000000000000, 0.9238795325112867385, 1.000000000000000000, 0.9238795325112867385, 1.000000000000000000, 0.9238795325112867385, 1.000000000000000000, 0.9238795325112867385, 1.000000000000000000, 0.9238795325112867385, 1.000000000000000000, 0.9238795325112867385, 1.000000000000000000, 0.9238795325112867385, 1.000000000000000000, 0.9238795325112867385, 1.000000000000000000, 0.9238795325112867385, 1.000000000000000000, 0.9238795325112867385, 1.000000000000000000, 0.9238795325112867385, 1.000000000000000000, 0.9238795325112867385, 1.000000000000000000, 0.9238795325112867385, 1.000000000000000000, 0.9238795325112867385, 1.000000000000000000, 0.9238795325112867385, 1.000000000000000000, 0.9238795325112867385, 1.000000000000000000, 0.9238795325112867385, 1.000000000000000000, 0.9238795325112867385, 1.000000000000000000, 0.9238795325112867385, 1.000000000000000000, 0.9238795325112867385, 1.000000000000000000, 0.9238795325112867385, 1.000000000000000000, 0.9238795325112867385, 1.000000000000000000, 0.9238795325112867385, 1.000000000000000000, 0.9238795325112867385, 1.000000000000000000, 0.9238795325112867385, 1.000000000000000000, 0.9238795325112867385, 1.000000000000000000, 0.9238795325112867385, 1.000000000000000000, 0.9238795325112867385, 1.000000000000000000, 0.9238795325112867385, 1.000000000000000000, 0.9238795325112867385, 1.000000000000000000, 0.9238795325112867385, 1.000000000000000000, 0.9238795325112867385, 1.000000000000000000, 0.9238795325112867385, 1.000000000000000000, 0.9238795325112867385, 1.000000000000000000, 0.9238795325112867385, 1.000000000000000000, 0.9238795325112867385, 1.000000000000000000, 0.9238795325112867385, 1.000000000000000000, 0.9238795325112867385, 1.000000000000000000, 0.9238795325112867385, 1.000000000000000000, 0.9238795325112867385, 1.000000000000000000, 0.9238795325112867385, 1.000000000000000000, 0.9238795325112867385, 1.000000000000000000, 0.9238795325112867385, 1.000000000000000000, 0.9238795325112867385, 1.000000000000000000, 0.9238795325112867385, 1.000000000000000000, 0.9238795325112867385, 1.000000000000000000, 0.9238795325112867385, 1.000000000000000000, 0.9238795325112867385, 1.000000000000000000, 0.9238795325112867385, 1.000000000000000000, 0.9238795325112867385, 1.000000000000000000, 0.9238795325112867385, 1.000000000000000000, 0.9238795325112867385, 1.000000000000000000, 0.9238795325112867385, 1.000000000000000000, 0.9238795325112867385, 1.000000000000000000, 0.9238795325112867385, 1.000000000000000000, 0.9238795325112867385, 1.000000000000000000, 0.9238795325112867385, 1.000000000000000000, 0.9238795325112867385, 1.000000000000000000, 0.9238795325112867385, 1.000000000000000000, 0.9238795325112867385, 1.000000000000000000, 0.9238795325112867385, 1.000000000000000000, 0.9238795325112867385, 1.000000000000000000, 0.9238795325112867385, 1.000000000000000000, 0.9238795325112867385, 1.000000000000000000, 0.9238795325112867385, 1.000000000000000000, 0.9238795325112867385, 1.000000000000000000, 0.9238795325112867385, 1.000000000000000000, 0.9238795325112867385, 1.000000000000000000, 0.9238795325112867385, 1.000000000000000000, 0.9238795325112867385, 1.000000000000000000, 0.9238795325112867385, 1.000000000000000000, 0.9238795325112867385, 1.000000000000000000, 0.9238795325112867385, 1.000000000000000000, 0.9238795325112867385, 1.000000000000000000, 0.9238795325112867385, 1.000000000000000000),
 ( 1.000000000000000000, 0.9238795325112867385, 1.000000000000000000, 0.9238795325112867385, 1.000000000000000000, 0.9238795325112867385, 1.000000000000000000, 0.9238795325112867385, 1.000000000000000000, 0.9238795325112867385, 1.000000000000000000, 0.9238795325112867385, 1.000000000000000000, 0.9238795325112867385, 1.000000000000000000, 0.9238795325112867385, 1.000000000000000000, 0.9238795325112867385, 1.000000000000000000, 0.9238795325112867385, 1.000000000000000000, 0.9238795325112867385, 1.000000000000000000, 0.9238795325112867385, 1.000000000000000000, 0.9238795325112867385, 1.000000000000000000, 0.9238795325112867385, 1.000000000000000000, 0.9238795325112867385, 1.000000000000000000, 0.9238795325112867385, 1.000000000000000000, 0.9238795325112867385, 1.000000000000000000, 0.9238795325112867385, 1.000000000000000000, 0.9238795325112867385, 1.000000000000000000, 0.9238795325112867385, 1.000000000000000000, 0.9238795325112867385, 1.000000000000000000, 0.9238795325112867385, 1.000000000000000000, 0.9238795325112867385, 1.000000000000000000, 0.9238795325112867385, 1.000000000000000000, 0.9238795325112867385, 1.000000000000000000, 0.9238795325112867385, 1.000000000000000000, 0.9238795325112867385, 1.000000000000000000, 0.9238795325112867385, 1.000000000000000000, 0.9238795325112867385, 1.000000000000000000, 0.9238795325112867385, 1.000000000000000000, 0.9238795325112867385, 1.000000000000000000, 0.9238795325112867385, 1.000000000000000000, 0.9238795325112867385, 1.000000000000000000, 0.9238795325112867385, 1.000000000000000000, 0.9238795325112867385, 1.000000000000000000, 0.9238795325112867385, 1.000000000000000000, 0.9238795325112867385, 1.000000000000000000, 0.9238795325112867385, 1.000000000000000000, 0.9238795325112867385, 1.000000000000000000, 0.9238795325112867385, 1.000000000000000000, 0.9238795325112867385, 1.000000000000000000, 0.9238795325112867385, 1.000000000000000000, 0.9238795325112867385, 1.000000000000000000, 0.9238795325112867385, 1.000000000000000000, 0.9238795325112867385, 1.000000000000000000, 0.9238795325112867385, 1.000000000000000000, 0.9238795325112867385, 1.000000000000000000, 0.9238795325112867385, 1.000000000000000000, 0.9238795325112867385, 1.000000000000000000, 0.9238795325112867385, 1.000000000000000000, 0.9238795325112867385, 1.000000000000000000, 0.9238795325112867385, 1.000000000000000000, 0.9238795325112867385, 1.000000000000000000, 0.9238795325112867385, 1.000000000000000000, 0.9238795325112867385, 1.000000000000000000, 0.9238795325112867385, 1.000000000000000000, 0.9238795325112867385, 1.000000000000000000, 0.9238795325112867385, 1.000000000000000000, 0.9238795325112867385, 1.000000000000000000, 0.9238795325112867385, 1.000000000000000000, 0.9238795325112867385, 1.000000000000000000, 0.9238795325112867385, 1.000000000000000000, 0.9238795325112867385, 1.000000000000000000, 0.9238795325112867385, 1.000000000000000000, 0.9238795325112867385, 1.000000000000000000, 0.9238795325112867385, 1.000000000000000000, 0.9238795325112867385, 1.000000000000000000, 0.9238795325112867385, 1.000000000000000000, 0.9238795325112867385, 1.000000000000000000, 0.9238795325112867385, 1.000000000000000000, 0.9238795325112867385, 1.000000000000000000, 0.9238795325112867385, 1.000000000000000000, 0.9238795325112867385, 1.000000000000000000, 0.9238795325112867385, 1.000000000000000000, 0.9238795325112867385, 1.000000000000000000, 0.9238795325112867385, 1.000000000000000000, 0.9238795325112867385, 1.000000000000000000, 0.9238795325112867385, 1.000000000000000000, 0.9238795325112867385, 1.000000000000000000, 0.9238795325112867385, 1.000000000000000000, 0.9238795325112867385, 1.000000000000000000, 0.9238795325112867385, 1.000000000000000000, 0.9238795325112867385, 1.000000000000000000, 0.9238795325112867385, 1.000000000000000000, 0.9238795325112867385, 1.000000000000000000, 0.9238795325112867385, 1.000000000000000000, 0.9238795325112867385, 1.000000000000000000, 0.9238795325112867385, 1.000000000000000000, 0.9238795325112867385, 1.000000000000000000, 0.9238795325112867385, 1.000000000000000000, 0.9238795325112867385, 1.000000000000000000, 0.9238795325112867385, 1.000000000000000000, 0.9238795325112867385, 1.000000000000000000, 0.9238795325112867385, 1.000000000000000000, 0.9238795325112867385, 1.000000000000000000, 0.9238795325112867385, 1.000000000000000000, 0.9238795325112867385, 1.000000000000000000, 0.9238795325112867385, 1.000000000000000000, 0.9238795325112867385, 1.000000000000000000, 0.9238795325112867385, 1.000000000000000000, 0.9238795325112867385, 1.000000000000000000, 0.9238795325112867385, 1.000000000000000000, 0.9238795325112867385, 1.000000000000000000, 0.9238795325112867385, 1.000000000000000000, 0.9238795325112867385, 1.000000000000000000, 0.9238795325112867385, 1.000000000000000000, 0.9238795325112867385, 1.000000000000000000, 0.9238795325112867385, 1.000000000000000000, 0.9238795325112867385, 1.000000000000000000, 0.9238795325112867385, 1.000000000000000000, 0.9238795325112867385, 1.000000000000000000, 0.9238795325112867385, 1.000000000000000000, 0.9238795325112867385, 1.000000000000000000, 0.9238795325112867385, 1.000000000000000000, 0.9238795325112867385, 1.000000000000000000, 0.9238795325112867385, 1.000000000000000000, 0.9238795325112867385, 1.000000000000000000, 0.9238795325112867385, 1.000000000000000000, 0.9238795325112867385, 1.000000000000000000, 0.9238795325112867385, 1.000000000000000000, 0.9238795325112867385, 1.000000000000000000, 0.9238795325112867385, 1.000000000000000000, 0.9238795325112867385, 1.000000000000000000, 0.9238795325112867385, 1.000000000000000000, 0.9238795325112867385, 1.000000000000000000, 0.9238795325112867385, 1.000000000000000000, 0.9238795325112867385, 1.000000000000000000, 0.9238795325112867385, 1.000000000000000000, 0.9238795325112867385, 1.000000000000000000, 0.9238795325112867385, 1.000000000000000000, 0.9238795325112867385, 1.000000000000000000, 0.9238795325112867385, 1.000000000000000000, 0.9238795325112867385, 1.000000000000000000, 0.9238795325112867385, 1.000000000000000000, 0.9238795325112867385, 1.000000000000000000, 0.9238795325112867385, 1.000000000000000000, 0.9238795325112867385, 1.000000000000000000, 0.9238795325112867385, 1.000000000000000000, 0.9238795325112867385, 1.000000000000000000, 0.9238795325112867385, 1.000000000000000000, 0.9238795325112867385, 1.000000000000000000, 0.9238795325112867385, 1.000000000000000000, 0.9238795325112867385, 1.000000000000000000, 0.9238795325112867385, 1.000000000000000000, 0.9238795325112867385, 1.000000000000000000, 0.9238795325112867385, 1.000000000000000000, 0.9238795325112867385, 1.000000000000000000, 0.9238795325112867385, 1.000000000000000000, 0.9238795325112867385, 1.000000000000000000, 0.9238795325112867385, 1.000000000000000000, 0.9238795325112867385, 1.000000000000000000, 0.9238795325112867385, 1.000000000000000000, 0.9238795325112867385, 1.000000000000000000, 0.9238795325112867385, 1.000000000000000000, 0.9238795325112867385, 1.000000000000000000, 0.9238795325112867385, 1.000000000000000000, 0.9238795325112867385, 1.000000000000000000, 0.9238795325112867385, 1.000000000000000000, 0.9238795325112867385, 1.000000000000000000, 0.9238795325112867385, 1.000000000000000000, 0.9238795325112867385, 1.000000000000000000, 0.9238795325112867385, 1.000000000000000000, 0.9238795325112867385, 1.000000000000000000, 0.9238795325112867385, 1.000000000000000000, 0.9238795325112867385, 1.000000000000000000, 0.9238795325112867385, 1.000000000000000000, 0.9238795325112867385, 1.000000000000000000, 0.9238795325112867385, 1.000000000000000000, 0.9238795325112867385, 1.000000000000000000, 0.9238795325112867385, 1.000000000000000000, 0.9238795325112867385, 1.000000000000000000, 0.9238795325112867385, 1.000000000000000000, 0.9238795325112867385, 1.000000000000000000, 0.9238795325112867385, 1.000000000000000000, 0.9238795325112867385, 1.000000000000000000, 0.9238795325112867385, 1.000000000000000000, 0.9238795325112867385, 1.000000000000000000, 0.9238795325112867385, 1.000000000000000000, 0.9238795325112867385, 1.000000000000000000, 0.9238795325112867385, 1.000000000000000000, 0.9238795325112867385, 1.000000000000000000, 0.9238795325112867385, 1.000000000000000000, 0.9238795325112867385, 1.000000000000000000, 0.9238795325112867385, 1.000000000000000000, 0.9238795325112867385, 1.000000000000000000, 0.9238795325112867385, 1.000000000000000000, 0.9238795325112867385, 1.000000000000000000, 0.9238795325112867385, 1.000000000000000000, 0.9238795325112867385, 1.000000000000000000, 0.9238795325112867385, 1.000000000000000000, 0.9238795325112867385, 1.000000000000000000, 0.9238795325112867385, 1.000000000000000000, 0.9238795325112867385, 1.000000000000000000, 0.9238795325112867385, 1.000000000000000000, 0.9238795325112867385, 1.000000000000000000, 0.9238795325112867385, 1.000000000000000000, 0.9238795325112867385, 1.000000000000000000, 0.9238795325112867385, 1.000000000000000000, 0.9238795325112867385, 1.000000000000000000, 0.9238795325112867385, 1.000000000000000000, 0.9238795325112867385, 1.000000000000000000, 0.9238795325112867385, 1.000000000000000000, 0.9238795325112867385, 1.000000000000000000, 0.9238795325112867385, 1.000000000000000000, 0.9238795325112867385, 1.000000000000000000, 0.9238795325112867385, 1.000000000000000000, 0.9238795325112867385, 1.000000000000000000, 0.9238795325112867385, 1.000000000000000000, 0.9238795325112867385, 1.000000000000000000, 0.9238795325112867385, 1.000000000000000000, 0.9238795325112867385, 1.000000000000000000, 0.9238795325112867385, 1.000000000000000000, 0.9238795325112867385, 1.000000000000000000, 0.9238795325112867385, 1.000000000000000000, 0.9238795325112867385, 1.000000000000000000, 0.9238795325112867385, 1.000000000000000000, 0.9238795325112867385, 1.000000000000000000, 0.9238795325112867385, 1.000000000000000000, 0.9238795325112867385, 1.000000000000000000, 0.9238795325112867385, 1.000000000000000000, 0.9238795325112867385, 1.000000000000000000, 0.9238795325112867385, 1.000000000000000000, 0.9238795325112867385, 1.000000000000000000, 0.9238795325112867385, 1.000000000000000000, 0.9238795325112867385, 1.000000000000000000, 0.9238795325112867385, 1.000000000000000000, 0.9238795325112867385, 1.000000000000000000, 0.9238795325112867385, 1.000000000000000000, 0.9238795325112867385, 1.000000000000000000, 0.9238795325112867385, 1.000000000000000000, 0.9238795325112867385, 1.000000000000000000, 0.9238795325112867385, 1.000000000000000000, 0.9238795325112867385, 1.000000000000000000, 0.9238795325112867385, 1.000000000000000000, 0.9238795325112867385, 1.000000000000000000, 0.9238795325112867385, 1.000000000000000000, 0.9238795325112867385, 1.000000000000000000, 0.9238795325112867385, 1.000000000000000000, 0.9238795325112867385, 1.000000000000000000, 0.9238795325112867385, 1.000000000000000000) ) ) 
 REPRESENTATION_ITEM ( '' )  SURFACE ( )  );
#32288 = CARTESIAN_POINT ( 'NONE',  ( -9.184850993605147944E-16, -157.2500000000000000, 5.000000000000000000 ) ) ;
#32289 = CARTESIAN_POINT ( 'NONE',  ( -2.229367062499996610, 5.854166668032262599, 3.861377020970582219 ) ) ;
#32290 = CARTESIAN_POINT ( 'NONE',  ( -2.229367062499996610, 15.85416666803226171, 3.861377020970582219 ) ) ;
#32291 = CARTESIAN_POINT ( 'NONE',  ( -52.10840900171896806, -147.1875000013656063, 3.393966926194110556 ) ) ;
#32292 = CARTESIAN_POINT ( 'NONE',  ( 5.000000000000000888, -77.58333333333334281, 2.886751345948126879 ) ) ;
#32293 = CARTESIAN_POINT ( 'NONE',  ( 2.071067811865540342, -165.1875000000000284, 4.999999999999936051 ) ) ;
#32294 = ORIENTED_EDGE ( 'NONE', *, *, #44808, .F. ) ;
#32295 = CARTESIAN_POINT ( 'NONE',  ( -2.229367062499996610, -69.14583333196773651, 3.861377020970582219 ) ) ;
#32296 = CARTESIAN_POINT ( 'NONE',  ( -1.339745962155610925, -85.66965819600731891, 5.000000000000000000 ) ) ;
#32297 = CARTESIAN_POINT ( 'NONE',  ( 9.457646018065525792E-16, 6.937500001365594748, 5.148502694627439702 ) ) ;
#32298 = CARTESIAN_POINT ( 'NONE',  ( 2.229367062500001939, -61.22916666530106511, 3.861377020970579999 ) ) ;
#32299 = CARTESIAN_POINT ( 'NONE',  ( 5.000000000000000888, -17.45833333060214443, 2.886751345948126879 ) ) ;
#32300 = CARTESIAN_POINT ( 'NONE',  ( -1.339745962155613812, -33.08034179853029144, -5.000000000000000000 ) ) ;
#32301 = CARTESIAN_POINT ( 'NONE',  ( -9.184850993605147944E-16, -139.3750000027312126, 5.000000000000000000 ) ) ;
#32302 = CARTESIAN_POINT ( 'NONE',  ( 6.042630808230842148E-15, 25.87500000273118062, -4.999999999999999112 ) ) ;
#32303 = DIRECTION ( 'NONE',  ( 0.000000000000000000, 0.000000000000000000, 1.000000000000000000 ) ) ;
#32304 = CARTESIAN_POINT ( 'NONE',  ( -2.229367062499996610, -34.14583333196772941, 3.861377020970582219 ) ) ;
#32305 = CARTESIAN_POINT ( 'NONE',  ( 9.457646018065525792E-16, -23.31249999863440436, 5.148502694627439702 ) ) ;
#32306 = ORIENTED_EDGE ( 'NONE', *, *, #55869, .F. ) ;
#32307 = CARTESIAN_POINT ( 'NONE',  ( -5.000000000000000000, -102.0000000000000142, 0.000000000000000000 ) ) ;
#32308 = CARTESIAN_POINT ( 'NONE',  ( 2.229367062499998831, -109.6458333319677365, -3.861377020970580887 ) ) ;
#32309 = CARTESIAN_POINT ( 'NONE',  ( 3.535533905932736864, -155.2500000027312126, 3.535533905932738641 ) ) ;
#32310 = ORIENTED_EDGE ( 'NONE', *, *, #63072, .F. ) ;
#32311 = CARTESIAN_POINT ( 'NONE',  ( -4.458734124999998549, -108.4791666653010793, 2.574251347313722516 ) ) ;
#32312 = CARTESIAN_POINT ( 'NONE',  ( 2.229367062500001939, -31.97916666530106866, 3.861377020970579999 ) ) ;
#32313 = CARTESIAN_POINT ( 'NONE',  ( 2.499999999999998668, -63.20833333060215153, -4.330127018922193649 ) ) ;
#32314 = CARTESIAN_POINT ( 'NONE',  ( -59.59170313451811296, -150.7500000013655495, 1.485763867205729394 ) ) ;
#32315 = CARTESIAN_POINT ( 'NONE',  ( 2.071067811865475505, -146.8125000000000000, -5.000000000000000888 ) ) ;
#32316 = EDGE_CURVE ( 'NONE', #43365, #22249, #61229, .T. ) ;
#32317 = CARTESIAN_POINT ( 'NONE',  ( 9.457646018065525792E-16, -30.06249999863440436, 5.148502694627439702 ) ) ;
#32318 = CARTESIAN_POINT ( 'NONE',  ( -4.458734124999997661, -71.47916666530107932, 2.574251347313722516 ) ) ;
#32319 = CARTESIAN_POINT ( 'NONE',  ( 1.975475456537005874E-15, -54.74999999999999289, 5.000000000000000000 ) ) ;
#32320 = CARTESIAN_POINT ( 'NONE',  ( -4.458734124999997661, -23.22916666530107221, 2.574251347313722516 ) ) ;
#32321 = EDGE_CURVE ( 'NONE', #13039, #34762, #6553, .T. ) ;
#32322 = CARTESIAN_POINT ( 'NONE',  ( -6.972266317189433020E-16, 6.875000002731185944, -5.000000000000000000 ) ) ;
#32323 = FACE_OUTER_BOUND ( 'NONE', #60027, .T. ) ;
#32324 = CARTESIAN_POINT ( 'NONE',  ( 5.000000000000000888, -16.58333333333333215, 2.886751345948126879 ) ) ;
#32325 = CARTESIAN_POINT ( 'NONE',  ( -1.846868145590734756, -147.1250000013656063, -4.458734125000000326 ) ) ;
#32326 = ORIENTED_EDGE ( 'NONE', *, *, #21676, .F. ) ;
#32327 = CARTESIAN_POINT ( 'NONE',  ( 3.535533905932736864, -150.1250000000000000, 3.535533905932738641 ) ) ;
#32328 = CARTESIAN_POINT ( 'NONE',  ( 4.458734124999998549, -51.97916666530107221, -2.574251347313721627 ) ) ;
#32329 = EDGE_CURVE ( 'NONE', #30019, #42348, #63402, .T. ) ;
#32330 = CARTESIAN_POINT ( 'NONE',  ( 5.000000000000000000, -2.500000000000002220, -6.123233995736766282E-16 ) ) ;
#32331 = CARTESIAN_POINT ( 'NONE',  ( -1.339745962155585168, -1.205341801261480716, -5.000000000000015987 ) ) ;
#32332 = CARTESIAN_POINT ( 'NONE',  ( -5.000000000000000000, 25.91666666666666430, -2.886751345948128211 ) ) ;
#32333 = ADVANCED_FACE ( 'NONE', ( #18062 ), #53732, .T. ) ;
#32334 = ADVANCED_FACE ( 'NONE', ( #48272 ), #28656, .T. ) ;
#32335 = CYLINDRICAL_SURFACE ( 'NONE', #42734, 5.000000000000000000 ) ;
#32336 = VECTOR ( 'NONE', #3881, 1000.000000000000000 ) ;
#32337 = CARTESIAN_POINT ( 'NONE',  ( -2.229367062499996610, 0.8541666680322613781, 3.861377020970582219 ) ) ;
#32338 = CARTESIAN_POINT ( 'NONE',  ( -6.972266317189433020E-16, -48.24999999999999289, -5.000000000000000000 ) ) ;
#32339 = CARTESIAN_POINT ( 'NONE',  ( -2.499999999999996447, -80.70833333060213022, 4.330127018922195425 ) ) ;
#32340 = CARTESIAN_POINT ( 'NONE',  ( -4.999999999999998224, -73.91666666666667140, 2.886751345948131764 ) ) ;
#32341 = CARTESIAN_POINT ( 'NONE',  ( 2.229367062500001939, 10.77083333469892956, 3.861377020970579999 ) ) ;
#32343 = ORIENTED_EDGE ( 'NONE', *, *, #23697, .F. ) ;
#32342 = EDGE_CURVE ( 'NONE', #29555, #57839, #45233, .T. ) ;
#32344 = CARTESIAN_POINT ( 'NONE',  ( -7.500000000000000000, -1.486698507076798847, -0.09861472150523968583 ) ) ;
#32345 = ORIENTED_EDGE ( 'NONE', *, *, #46840, .F. ) ;
#32346 =( BOUNDED_CURVE ( )  B_SPLINE_CURVE ( 2, ( #54007, #59160, #5441, #15093, #10268, #29872, #25059, #21195, #45317 ),
 .UNSPECIFIED., .F., .F. ) 
 B_SPLINE_CURVE_WITH_KNOTS ( ( 3, 2, 2, 2, 3 ),
 ( 0.4589285714285714080, 0.4595238095238095011, 0.4607142857142856873, 0.4619047619047619291, 0.4625000000000000222 ),
 .UNSPECIFIED. ) 
 CURVE ( )  GEOMETRIC_REPRESENTATION_ITEM ( )  RATIONAL_B_SPLINE_CURVE ( ( 0.9330127018922194093, 0.9330127018922194093, 1.000000000000000000, 0.8660254037844387076, 1.000000000000000000, 0.8660254037844387076, 1.000000000000000000, 0.9330127018922194093, 0.9330127018922194093 ) ) 
 REPRESENTATION_ITEM ( '' )  );
#32347 = CARTESIAN_POINT ( 'NONE',  ( 5.000000000000000000, -7.374999997268813168, -6.123233995736766282E-16 ) ) ;
#32348 = CARTESIAN_POINT ( 'NONE',  ( 4.458734124999999437, -47.81249999863440792, -5.460374474430324690E-16 ) ) ;
#32349 = ADVANCED_FACE ( 'NONE', ( #38615 ), #28031, .T. ) ;
#32350 = CARTESIAN_POINT ( 'NONE',  ( 4.458734124999999437, -165.6875000013655779, 0.000000000000000000 ) ) ;
#32351 = EDGE_CURVE ( 'NONE', #37665, #53636, #38005, .T. ) ;
#32352 = CARTESIAN_POINT ( 'NONE',  ( -5.000000000000000000, -43.87499999726880873, 0.000000000000000000 ) ) ;
#32353 = ORIENTED_EDGE ( 'NONE', *, *, #36239, .T. ) ;
#32354 = CARTESIAN_POINT ( 'NONE',  ( -4.458734124999999437, -21.31249999863440436, 0.000000000000000000 ) ) ;
#32355 = ORIENTED_EDGE ( 'NONE', *, *, #52292, .T. ) ;
#32356 = CARTESIAN_POINT ( 'NONE',  ( -5.000000000000000000, -11.99999999999999645, 0.000000000000000000 ) ) ;
#32357 = CARTESIAN_POINT ( 'NONE',  ( 4.458734125000000326, -164.3750000013656063, -1.846868145590734978 ) ) ;
#32358 = FACE_OUTER_BOUND ( 'NONE', #30042, .T. ) ;
#32359 = CARTESIAN_POINT ( 'NONE',  ( -54.60164318462004474, -138.3750000000000284, -4.984105922594373794 ) ) ;
#32360 = CARTESIAN_POINT ( 'NONE',  ( -4.458734124999999437, -36.64583333196773651, -2.574251347313719407 ) ) ;
#32361 = ORIENTED_EDGE ( 'NONE', *, *, #48718, .T. ) ;
#32362 = CARTESIAN_POINT ( 'NONE',  ( -2.229367062500000163, -83.47916666530106511, -3.861377020970580443 ) ) ;
#32363 = CARTESIAN_POINT ( 'NONE',  ( 9.457646018065525792E-16, 24.93750000136559564, 5.148502694627439702 ) ) ;
#32364 = CARTESIAN_POINT ( 'NONE',  ( -58.24261429053147765, -141.3750000027312126, -3.805975901505573855 ) ) ;
#32365 = ORIENTED_EDGE ( 'NONE', *, *, #54526, .T. ) ;
#32366 = CARTESIAN_POINT ( 'NONE',  ( -2.499999999999996447, -59.70833333060214443, 4.330127018922195425 ) ) ;
#32367 = CARTESIAN_POINT ( 'NONE',  ( -55.35523342533222291, -138.5625000013656063, 4.444560631937231499 ) ) ;
#32368 = CARTESIAN_POINT ( 'NONE',  ( 4.458734124999999437, -81.06249999863440792, -5.460374474430324690E-16 ) ) ;
#32369 = CARTESIAN_POINT ( 'NONE',  ( -51.19402409849444524, -129.6250000027312126, -3.242614290531456334 ) ) ;
#32370 = CARTESIAN_POINT ( 'NONE',  ( 3.535533905932738197, -142.8750000000000000, -3.535533905932738197 ) ) ;
#32371 = CARTESIAN_POINT ( 'NONE',  ( 1.846868145590736310, -139.8750000013656063, 4.458734124999997661 ) ) ;
#32372 =( BOUNDED_CURVE ( )  B_SPLINE_CURVE ( 2, ( #57433, #62576, #56801, #57120, #32655, #51965, #7904, #27825, #17230 ),
 .UNSPECIFIED., .F., .F. ) 
 B_SPLINE_CURVE_WITH_KNOTS ( ( 3, 2, 2, 2, 3 ),
 ( 0.9583333333333331483, 0.9624999999999998002, 0.9666666666666665630, 0.9708333333333332149, 0.9749999999999998668 ),
 .UNSPECIFIED. ) 
 CURVE ( )  GEOMETRIC_REPRESENTATION_ITEM ( )  RATIONAL_B_SPLINE_CURVE ( ( 1.000000000000003997, 0.9238795325112826307, 1.000000000000000000, 0.9238795325112867385, 1.000000000000000000, 0.9238795325112867385, 1.000000000000000000, 0.9238795325112887369, 0.9999999999999980016 ) ) 
 REPRESENTATION_ITEM ( '' )  );
#32373 = CARTESIAN_POINT ( 'NONE',  ( -4.999999999999998224, -46.79166666393547303, 2.886751345948131764 ) ) ;
#32374 = CARTESIAN_POINT ( 'NONE',  ( -2.229367062499996610, -54.14583333196773651, 3.861377020970582219 ) ) ;
#32375 = CARTESIAN_POINT ( 'NONE',  ( -58.80597590150559739, -151.1250000027312126, 3.242614290531460330 ) ) ;
#32376 = CARTESIAN_POINT ( 'NONE',  ( -4.458734124999999437, 25.68750000136559208, 0.000000000000000000 ) ) ;
#32377 = CARTESIAN_POINT ( 'NONE',  ( -2.500000000000000444, -104.1666666666666572, -4.330127018922193649 ) ) ;
#32378 = AXIS2_PLACEMENT_3D ( 'NONE', #41543, #2649, #22268 ) ;
#32379 = CARTESIAN_POINT ( 'NONE',  ( 5.000000000000000000, -159.1250000027311842, 0.000000000000000000 ) ) ;
#32380 = CARTESIAN_POINT ( 'NONE',  ( 2.229367062500001939, -42.22916666530107932, 3.861377020970579999 ) ) ;
#32381 = CARTESIAN_POINT ( 'NONE',  ( -5.000000000000000000, 1.041666669397853129, -2.886751345948128211 ) ) ;
#32382 = CARTESIAN_POINT ( 'NONE',  ( 1.975475456537005874E-15, 16.37500000273118417, 5.000000000000000000 ) ) ;
#32383 = CARTESIAN_POINT ( 'NONE',  ( -57.19623071787017210, -126.3750000013656489, 4.297418129356382899 ) ) ;
#32384 = CARTESIAN_POINT ( 'NONE',  ( -4.458734124999999437, -79.56249999863440792, 0.000000000000000000 ) ) ;
#32385 = CARTESIAN_POINT ( 'NONE',  ( -4.458734124999999437, -103.3958333319677223, -2.574251347313719407 ) ) ;
#32386 = CARTESIAN_POINT ( 'NONE',  ( -4.458734124999997661, -4.479166665301070438, 2.574251347313722516 ) ) ;
#32387 = VERTEX_POINT ( 'NONE', #38934 ) ;
#32388 = CARTESIAN_POINT ( 'NONE',  ( -2.500000000000000444, -86.04166666393547303, -4.330127018922193649 ) ) ;
#32389 = CARTESIAN_POINT ( 'NONE',  ( -4.458734124999998549, -95.22916666530106511, 2.574251347313722516 ) ) ;
#32390 = CARTESIAN_POINT ( 'NONE',  ( -5.000000000000000888, -165.6875000027312126, -2.071067811865475949 ) ) ;
#32391 = CARTESIAN_POINT ( 'NONE',  ( -4.458734124999998549, -85.47916666530106511, 2.574251347313722516 ) ) ;
#32392 = CARTESIAN_POINT ( 'NONE',  ( 9.457646018065525792E-16, 13.68750000136559386, 5.148502694627439702 ) ) ;
#32393 = FACE_OUTER_BOUND ( 'NONE', #51353, .T. ) ;
#32394 = CARTESIAN_POINT ( 'NONE',  ( -50.40829686548195099, -135.0000000013656347, -1.485763867205728284 ) ) ;
#32395 = CARTESIAN_POINT ( 'NONE',  ( 2.229367062499998831, -12.64583333196774007, -3.861377020970580887 ) ) ;
#32396 = CARTESIAN_POINT ( 'NONE',  ( -2.229367062500000163, 15.27083333469892779, -3.861377020970580443 ) ) ;
#32397 = CARTESIAN_POINT ( 'NONE',  ( -4.458734124999999437, -53.64583333196773651, -2.574251347313719407 ) ) ;
#32398 = CARTESIAN_POINT ( 'NONE',  ( -3.535533905932738641, -163.3750000000000284, 3.535533905932737309 ) ) ;
#32399 = CARTESIAN_POINT ( 'NONE',  ( -2.499999999999996447, -21.70833333060214798, 4.330127018922195425 ) ) ;
#32400 = CARTESIAN_POINT ( 'NONE',  ( 4.458734125000000326, -7.895833331967735624, 2.574251347313718519 ) ) ;
#32401 = CARTESIAN_POINT ( 'NONE',  ( -2.499999999999996447, -38.83333333333332860, 4.330127018922195425 ) ) ;
#32402 = ORIENTED_EDGE ( 'NONE', *, *, #16200, .T. ) ;
#32403 = CARTESIAN_POINT ( 'NONE',  ( -4.458734124999999437, -35.64583333196772941, -2.574251347313719407 ) ) ;
#32404 = CARTESIAN_POINT ( 'NONE',  ( -55.35523342533222291, -128.5625000013656063, 4.444560631937231499 ) ) ;
#32405 = CARTESIAN_POINT ( 'NONE',  ( 0.000000000000000000, -120.0000000000000000, 0.000000000000000000 ) ) ;
#32406 = CARTESIAN_POINT ( 'NONE',  ( -4.458734124999998549, -79.22916666530107932, 2.574251347313722516 ) ) ;
#32407 = CARTESIAN_POINT ( 'NONE',  ( 2.229367062499998831, 22.10416666803225993, -3.861377020970580887 ) ) ;
#32408 = CARTESIAN_POINT ( 'NONE',  ( 3.152801135295366208, -149.8125000013655779, 3.152801135295367985 ) ) ;
#32409 = CARTESIAN_POINT ( 'NONE',  ( -4.458734124999999437, 15.68750000136559564, 0.000000000000000000 ) ) ;
#32410 = CYLINDRICAL_SURFACE ( 'NONE', #48241, 5.000000000000000000 ) ;
#32411 = DIRECTION ( 'NONE',  ( -0.000000000000000000, 1.000000000000000000, -0.000000000000000000 ) ) ;
#32412 = CARTESIAN_POINT ( 'NONE',  ( 4.458734124999998549, -85.97916666530107932, -2.574251347313721627 ) ) ;
#32413 = CARTESIAN_POINT ( 'NONE',  ( 2.500000000000002220, -65.66666666666667140, 4.330127018922192761 ) ) ;
#32414 = CYLINDRICAL_SURFACE ( 'NONE', #31592, 5.000000000000000000 ) ;
#32415 = CARTESIAN_POINT ( 'NONE',  ( 2.500000000000002220, 20.45833333606451987, 4.330127018922192761 ) ) ;
#32416 = ORIENTED_EDGE ( 'NONE', *, *, #31536, .F. ) ;
#32417 = CARTESIAN_POINT ( 'NONE',  ( 2.499999999999998668, -79.33333333333332860, -4.330127018922193649 ) ) ;
#32418 = CARTESIAN_POINT ( 'NONE',  ( -48.00000000000002132, -155.0000000000000284, 4.041451884327384114 ) ) ;
#32420 = CARTESIAN_POINT ( 'NONE',  ( 2.500000000000002220, -27.66666666666666430, 4.330127018922192761 ) ) ;
#32419 = CARTESIAN_POINT ( 'NONE',  ( -2.499999999999996447, -71.83333333333332860, 4.330127018922195425 ) ) ;
#32421 = CARTESIAN_POINT ( 'NONE',  ( 4.458734124999999437, -34.81249999863440792, -5.460374474430324690E-16 ) ) ;
#32422 = LINE ( 'NONE', #14603, #44797 ) ;
#32423 = VECTOR ( 'NONE', #35390, 1000.000000000000000 ) ;
#32424 = EDGE_CURVE ( 'NONE', #37331, #45160, #58570, .T. ) ;
#32425 = CARTESIAN_POINT ( 'NONE',  ( -3.535250795749689387E-16, -27.12499999726881583, -5.773502691896257311 ) ) ;
#32427 = VERTEX_POINT ( 'NONE', #47960 ) ;
#32426 = CARTESIAN_POINT ( 'NONE',  ( -3.152548672688508926E-16, -60.56249999863440792, -5.148502694627439702 ) ) ;
#32428 = CARTESIAN_POINT ( 'NONE',  ( -55.35523342533222291, -153.5625000013656063, 4.444560631937231499 ) ) ;
#32430 = ORIENTED_EDGE ( 'NONE', *, *, #57897, .T. ) ;
#32429 = CARTESIAN_POINT ( 'NONE',  ( 4.458734125000001214, -8.145833331967736513, 2.574251347313718519 ) ) ;
#32431 = CARTESIAN_POINT ( 'NONE',  ( -2.500000000000000444, -69.16666666666667140, -4.330127018922193649 ) ) ;
#32432 = CARTESIAN_POINT ( 'NONE',  ( -54.64476657466781973, -138.8125000013656063, -4.444560631937228834 ) ) ;
#32433 = CARTESIAN_POINT ( 'NONE',  ( 2.229367062499998831, -51.89583333196773651, -3.861377020970580887 ) ) ;
#32434 = CARTESIAN_POINT ( 'NONE',  ( -5.000000000000000000, -75.95833333060215864, -2.886751345948128211 ) ) ;
#32436 = ORIENTED_EDGE ( 'NONE', *, *, #46061, .F. ) ;
#32435 = CARTESIAN_POINT ( 'NONE',  ( 1.339745962155615144, -13.70534180126148094, 4.999999999999999112 ) ) ;
#32437 = CARTESIAN_POINT ( 'NONE',  ( -54.60164318462004474, -148.3750000000000284, -4.984105922594373794 ) ) ;
#32438 = CARTESIAN_POINT ( 'NONE',  ( 9.457646018065525792E-16, -14.31249999863440259, 5.148502694627439702 ) ) ;
#32439 = CARTESIAN_POINT ( 'NONE',  ( 2.229367062499998831, -58.89583333196773651, -3.861377020970580887 ) ) ;
#32440 = CARTESIAN_POINT ( 'NONE',  ( 1.975475456537005874E-15, -10.62499999726881228, 5.000000000000000000 ) ) ;
#32441 = CARTESIAN_POINT ( 'NONE',  ( 4.458734125000000326, -142.3750000013656063, -1.846868145590734978 ) ) ;
#32442 = CARTESIAN_POINT ( 'NONE',  ( 2.229367062500001939, -98.22916666530105090, 3.861377020970579999 ) ) ;
#32443 = CARTESIAN_POINT ( 'NONE',  ( 3.535533905932738197, -148.0000000027311842, -3.535533905932738197 ) ) ;
#32444 = ORIENTED_EDGE ( 'NONE', *, *, #41778, .T. ) ;
#32445 = CARTESIAN_POINT ( 'NONE',  ( -59.44456063193725015, -152.8125000013656063, -0.3552334253322034230 ) ) ;
#32446 = CARTESIAN_POINT ( 'NONE',  ( -59.98410592259440222, -144.2500000027312126, -0.3983568153799752487 ) ) ;
#32447 = DIRECTION ( 'NONE',  ( -0.000000000000000000, 1.000000000000000000, -0.000000000000000000 ) ) ;
#32448 = CARTESIAN_POINT ( 'NONE',  ( -3.152548672688508926E-16, -6.562499998634404363, -5.148502694627439702 ) ) ;
#32449 = CARTESIAN_POINT ( 'NONE',  ( -4.458734124999997661, -96.47916666530105090, 2.574251347313722516 ) ) ;
#32450 = CARTESIAN_POINT ( 'NONE',  ( -3.152801135295367096, -146.3125000013655779, -3.152801135295367541 ) ) ;
#32451 = CARTESIAN_POINT ( 'NONE',  ( 4.458734124999999437, -22.06249999863440436, -5.460374474430324690E-16 ) ) ;
#32452 = CARTESIAN_POINT ( 'NONE',  ( -7.499999999999998224, 1.489914625143999416, -0.1187923833806747292 ) ) ;
#32453 = CARTESIAN_POINT ( 'NONE',  ( -59.29741812935640155, -135.6250000013655779, -2.196230717870135685 ) ) ;
#32454 = CARTESIAN_POINT ( 'NONE',  ( -4.458734124999999437, -64.56249999863440792, 0.000000000000000000 ) ) ;
#32455 = CARTESIAN_POINT ( 'NONE',  ( -2.480964764533239819E-13, -72.75000000000000000, 5.000000000000000000 ) ) ;
#32456 = CARTESIAN_POINT ( 'NONE',  ( -5.000000000000000000, 17.00000000000000000, 0.000000000000000000 ) ) ;
#32457 = CARTESIAN_POINT ( 'NONE',  ( 2.730187237215162345E-16, -145.1875000013656063, -4.458734124999999437 ) ) ;
#32458 = CARTESIAN_POINT ( 'NONE',  ( 4.458734125000000326, 8.854166668032261711, 2.574251347313718519 ) ) ;
#32459 = ORIENTED_EDGE ( 'NONE', *, *, #34267, .F. ) ;
#32460 = CARTESIAN_POINT ( 'NONE',  ( -5.000000000000000000, -81.00000000000000000, 0.000000000000000000 ) ) ;
#32461 = CARTESIAN_POINT ( 'NONE',  ( -6.972266317189433020E-16, -66.12499999726881583, -5.000000000000000000 ) ) ;
#32463 = CARTESIAN_POINT ( 'NONE',  ( 2.229367062499998831, -26.64583333196774007, -3.861377020970580887 ) ) ;
#32462 = CARTESIAN_POINT ( 'NONE',  ( 5.000000000000000000, -90.41666666666664298, -2.886751345948129988 ) ) ;
#32464 = CARTESIAN_POINT ( 'NONE',  ( -2.500000000000000444, 6.958333336064520758, -4.330127018922193649 ) ) ;
#32465 = CARTESIAN_POINT ( 'NONE',  ( 2.229367062499998831, -69.89583333196773651, -3.861377020970580887 ) ) ;
#32466 = CARTESIAN_POINT ( 'NONE',  ( 2.229367062500001939, 26.77083333469892423, 3.861377020970579999 ) ) ;
#32467 = DIRECTION ( 'NONE',  ( 0.000000000000000000, 0.000000000000000000, -1.000000000000000000 ) ) ;
#32468 = AXIS2_PLACEMENT_3D ( 'NONE', #23985, #8880, #14638 ) ;
#32469 =( BOUNDED_CURVE ( )  B_SPLINE_CURVE ( 2, ( #14621, #62898, #39378, #59009, #14937, #38744, #18812, #63212, #54180 ),
 .UNSPECIFIED., .F., .F. ) 
 B_SPLINE_CURVE_WITH_KNOTS ( ( 3, 2, 2, 2, 3 ),
 ( 0.7312499999999999556, 0.7319444444444443976, 0.7333333333333332815, 0.7347222222222222765, 0.7354166666666667185 ),
 .UNSPECIFIED. ) 
 CURVE ( )  GEOMETRIC_REPRESENTATION_ITEM ( )  RATIONAL_B_SPLINE_CURVE ( ( 0.9330127018922194093, 0.9330127018922194093, 1.000000000000000000, 0.8660254037844387076, 1.000000000000000000, 0.8660254037844387076, 1.000000000000000000, 0.9330127018922194093, 0.9330127018922194093 ) ) 
 REPRESENTATION_ITEM ( '' )  );
#32470 = CARTESIAN_POINT ( 'NONE',  ( -57.89159099828107458, -146.6875000013656063, -3.393966926194107447 ) ) ;
#32471 = CARTESIAN_POINT ( 'NONE',  ( 4.458734124999999437, 4.187500001365595637, -5.460374474430324690E-16 ) ) ;
#32472 = CARTESIAN_POINT ( 'NONE',  ( 5.000000000000000000, -56.37499999726880162, -6.123233995736766282E-16 ) ) ;
#32473 = CYLINDRICAL_SURFACE ( 'NONE', #29454, 5.000000000000000000 ) ;
#32474 = CARTESIAN_POINT ( 'NONE',  ( -4.458734124999999437, 5.687500001365592972, 0.000000000000000000 ) ) ;
#32475 = CARTESIAN_POINT ( 'NONE',  ( -3.152548672688508926E-16, -73.56249999863440792, -5.148502694627439702 ) ) ;
#32476 = CARTESIAN_POINT ( 'NONE',  ( 4.458734124999999437, -21.06249999863440436, -5.460374474430324690E-16 ) ) ;
#32477 = CARTESIAN_POINT ( 'NONE',  ( -4.999999999999999112, 1.083333333333331927, 2.886751345948131764 ) ) ;
#32478 = CARTESIAN_POINT ( 'NONE',  ( 4.458734124999999437, -158.4375000013655779, 0.000000000000000000 ) ) ;
#32479 = CARTESIAN_POINT ( 'NONE',  ( 1.339745962155602488, 15.41965820146970323, 5.000000000000007105 ) ) ;
#32480 = CARTESIAN_POINT ( 'NONE',  ( -2.229367062499996610, -63.14583333196774362, 3.861377020970582219 ) ) ;
#32481 = CARTESIAN_POINT ( 'NONE',  ( 5.000000000000000000, -101.3749999972688158, -6.123233995736766282E-16 ) ) ;
#32482 = LINE ( 'NONE', #32805, #52214 ) ;
#32483 = CARTESIAN_POINT ( 'NONE',  ( -4.458734124999997661, -40.22916666530107932, 2.574251347313722516 ) ) ;
#32484 = CARTESIAN_POINT ( 'NONE',  ( -4.458734124999997661, -108.4791666653010509, 2.574251347313722516 ) ) ;
#32485 = CARTESIAN_POINT ( 'NONE',  ( 4.458734125000000326, -68.14583333196773651, 2.574251347313718519 ) ) ;
#32486 = CARTESIAN_POINT ( 'NONE',  ( 1.060575238724906964E-15, -50.75000000000000000, 5.773502691896257311 ) ) ;
#32487 = CARTESIAN_POINT ( 'NONE',  ( -5.000000000000000000, -40.99999999999999289, 0.000000000000000000 ) ) ;
#32488 = CARTESIAN_POINT ( 'NONE',  ( 5.000000000000000888, -68.45833333060214443, 2.886751345948126879 ) ) ;
#32489 = EDGE_LOOP ( 'NONE', ( #58821, #49185, #27584, #56073 ) ) ;
#32490 = CARTESIAN_POINT ( 'NONE',  ( 4.458734124999998549, -109.7291666653010793, -2.574251347313721627 ) ) ;
#32491 = CARTESIAN_POINT ( 'NONE',  ( -1.339745962155610925, -67.66965819600733312, 5.000000000000000000 ) ) ;
#32492 = CARTESIAN_POINT ( 'NONE',  ( 1.060575238724906964E-15, -14.75000000000000000, 5.773502691896257311 ) ) ;
#32493 = CARTESIAN_POINT ( 'NONE',  ( 2.229367062499998831, -14.64583333196773474, -3.861377020970580887 ) ) ;
#32494 = CARTESIAN_POINT ( 'NONE',  ( -4.458734124999997661, -78.22916666530106511, 2.574251347313722516 ) ) ;
#32495 = CARTESIAN_POINT ( 'NONE',  ( -2.500000000000000444, -6.166666666666667851, -4.330127018922193649 ) ) ;
#32496 = CARTESIAN_POINT ( 'NONE',  ( -4.999999999999999112, -11.79166666393547835, 2.886751345948131764 ) ) ;
#32498 = ORIENTED_EDGE ( 'NONE', *, *, #7139, .F. ) ;
#32497 = CARTESIAN_POINT ( 'NONE',  ( 9.457646018065525792E-16, -43.06249999863440081, 5.148502694627439702 ) ) ;
#32499 = CARTESIAN_POINT ( 'NONE',  ( 1.339745962155615144, -100.5803417985302843, 4.999999999999999112 ) ) ;
#32501 = ORIENTED_EDGE ( 'NONE', *, *, #53079, .T. ) ;
#32500 = CARTESIAN_POINT ( 'NONE',  ( -4.458734124999999437, 8.354166668032261711, -2.574251347313719407 ) ) ;
#32502 = DIRECTION ( 'NONE',  ( 0.000000000000000000, 0.000000000000000000, 1.000000000000000000 ) ) ;
#32503 = CARTESIAN_POINT ( 'NONE',  ( 2.499999999999998668, -54.33333333333332860, -4.330127018922193649 ) ) ;
#32504 = CARTESIAN_POINT ( 'NONE',  ( 3.152801135295366208, -160.8125000013656063, 3.152801135295367985 ) ) ;
#32505 = CARTESIAN_POINT ( 'NONE',  ( 9.457646018065525792E-16, -35.31249999863440792, 5.148502694627439702 ) ) ;
#32506 = CARTESIAN_POINT ( 'NONE',  ( -2.500000000000000444, -11.04166666393547835, -4.330127018922193649 ) ) ;
#32507 = CARTESIAN_POINT ( 'NONE',  ( 4.458734124999999437, -81.81249999863440792, -5.460374474430324690E-16 ) ) ;
#32508 = CARTESIAN_POINT ( 'NONE',  ( 2.071067811865476394, -168.1875000000000284, 5.000000000000000000 ) ) ;
#32509 = CARTESIAN_POINT ( 'NONE',  ( -2.500000000000000444, -30.16666666666666785, -4.330127018922193649 ) ) ;
#32510 = CARTESIAN_POINT ( 'NONE',  ( -50.55543936806279248, -131.3125000013656063, 0.3552334253322060320 ) ) ;
#32511 = CARTESIAN_POINT ( 'NONE',  ( -2.229367062500000163, 1.270833334698927342, -3.861377020970580443 ) ) ;
#32512 = AXIS2_PLACEMENT_3D ( 'NONE', #61441, #31837, #32467 ) ;
#32513 = CARTESIAN_POINT ( 'NONE',  ( -4.458734124999998549, -42.47916666530107932, 2.574251347313722516 ) ) ;
#32514 = CARTESIAN_POINT ( 'NONE',  ( 1.339745962155615144, -83.58034179853031276, 4.999999999999999112 ) ) ;
#32515 = CARTESIAN_POINT ( 'NONE',  ( -4.458734124999999437, -84.64583333196773651, -2.574251347313719407 ) ) ;
#32516 = CARTESIAN_POINT ( 'NONE',  ( 0.000000000000000000, -170.0000000000000000, 0.000000000000000000 ) ) ;
#32517 =( BOUNDED_CURVE ( )  B_SPLINE_CURVE ( 2, ( #62751, #18672, #38295, #57923, #63064, #58223, #33778, #53396, #9327 ),
 .UNSPECIFIED., .F., .F. ) 
 B_SPLINE_CURVE_WITH_KNOTS ( ( 3, 2, 2, 2, 3 ),
 ( 0.4517857142857142905, 0.4523809523809523836, 0.4535714285714285698, 0.4547619047619047561, 0.4553571428571428492 ),
 .UNSPECIFIED. ) 
 CURVE ( )  GEOMETRIC_REPRESENTATION_ITEM ( )  RATIONAL_B_SPLINE_CURVE ( ( 0.9330127018922194093, 0.9330127018922194093, 1.000000000000000000, 0.8660254037844387076, 1.000000000000000000, 0.8660254037844387076, 1.000000000000000000, 0.9330127018922194093, 0.9330127018922194093 ) ) 
 REPRESENTATION_ITEM ( '' )  );
#32518 = EDGE_LOOP ( 'NONE', ( #18264, #60839, #53920, #58550 ) ) ;
#32519 = CARTESIAN_POINT ( 'NONE',  ( -59.81910112700025905, -153.3125000027312126, -2.462841084822630311 ) ) ;
#32520 =( BOUNDED_CURVE ( )  B_SPLINE_CURVE ( 2, ( #46014, #36363, #16746, #21254, #7737 ),
 .UNSPECIFIED., .F., .F. ) 
 B_SPLINE_CURVE_WITH_KNOTS ( ( 3, 2, 3 ),
 ( 0.9916666666666665853, 0.9958333333333333481, 1.000000000000000000 ),
 .UNSPECIFIED. ) 
 CURVE ( )  GEOMETRIC_REPRESENTATION_ITEM ( )  RATIONAL_B_SPLINE_CURVE ( ( 1.000000000000001998, 0.9238795325112847401, 1.000000000000000000, 0.9238795325112867385, 1.000000000000000000 ) ) 
 REPRESENTATION_ITEM ( '' )  );
#32521 = CARTESIAN_POINT ( 'NONE',  ( 6.123233995736766282E-16, -170.0000000000000000, -5.000000000000000000 ) ) ;
#32523 = ADVANCED_FACE ( 'NONE', ( #23533, #43133 ), #62773, .F. ) ;
#32522 = CARTESIAN_POINT ( 'NONE',  ( 9.457646018065525792E-16, -72.31249999863440792, 5.148502694627439702 ) ) ;
#32524 = CARTESIAN_POINT ( 'NONE',  ( -2.229367062499996610, -11.39583333196773829, 3.861377020970582219 ) ) ;
#32525 = VERTEX_POINT ( 'NONE', #48588 ) ;
#32526 = CARTESIAN_POINT ( 'NONE',  ( 3.061616997868383141E-16, -150.8750000027312126, -5.000000000000000000 ) ) ;
#32527 = CARTESIAN_POINT ( 'NONE',  ( -6.972266317189433020E-16, 2.875000002731185500, -5.000000000000000000 ) ) ;
#32528 = CARTESIAN_POINT ( 'NONE',  ( 9.457646018065525792E-16, -6.312499998634404363, 5.148502694627439702 ) ) ;
#32529 = DIRECTION ( 'NONE',  ( -0.000000000000000000, 1.000000000000000000, -0.000000000000000000 ) ) ;
#32530 = CARTESIAN_POINT ( 'NONE',  ( -4.458734124999999437, 4.687500001365595637, 0.000000000000000000 ) ) ;
#32531 = CARTESIAN_POINT ( 'NONE',  ( 3.152801135295366208, -155.5625000013656063, 3.152801135295367985 ) ) ;
#32532 = CARTESIAN_POINT ( 'NONE',  ( 4.458734124999998549, 27.02083333469892068, -2.574251347313721627 ) ) ;
#32533 = VERTEX_POINT ( 'NONE', #5487 ) ;
#32534 = CARTESIAN_POINT ( 'NONE',  ( 2.229367062499998831, -87.64583333196773651, -3.861377020970580887 ) ) ;
#32535 = CARTESIAN_POINT ( 'NONE',  ( -6.972266317189433020E-16, 15.75000000000000000, -5.000000000000000000 ) ) ;
#32536 = CARTESIAN_POINT ( 'NONE',  ( 4.458734124999999437, -6.812499998634404363, -5.460374474430324690E-16 ) ) ;
#32537 = FACE_OUTER_BOUND ( 'NONE', #53620, .T. ) ;
#32538 = CARTESIAN_POINT ( 'NONE',  ( -55.39835681537999790, -144.8750000000000284, 4.984105922594378235 ) ) ;
#32539 = EDGE_CURVE ( 'NONE', #60194, #30770, #16094, .T. ) ;
#32540 = CARTESIAN_POINT ( 'NONE',  ( -50.18089887299976937, -138.6875000000000000, 2.462841084822337656 ) ) ;
#32541 = CARTESIAN_POINT ( 'NONE',  ( -2.500000000000000444, -37.04166666393548013, -4.330127018922193649 ) ) ;
#32542 = DIRECTION ( 'NONE',  ( -0.000000000000000000, 1.000000000000000000, -0.000000000000000000 ) ) ;
#32543 = CARTESIAN_POINT ( 'NONE',  ( -3.152548672688508926E-16, 24.43750000136559564, -5.148502694627439702 ) ) ;
#32544 = CARTESIAN_POINT ( 'NONE',  ( -5.000000000000000000, -95.08333333333332860, -2.886751345948128211 ) ) ;
#32545 =( BOUNDED_CURVE ( )  B_SPLINE_CURVE ( 2, ( #40950, #16519, #36141, #7825, #23241, #12637, #33212, #8457, #51571 ),
 .UNSPECIFIED., .F., .F. ) 
 B_SPLINE_CURVE_WITH_KNOTS ( ( 3, 2, 2, 2, 3 ),
 ( 0.6446428571428571841, 0.6452380952380952772, 0.6464285714285714635, 0.6476190476190476497, 0.6482142857142857428 ),
 .UNSPECIFIED. ) 
 CURVE ( )  GEOMETRIC_REPRESENTATION_ITEM ( )  RATIONAL_B_SPLINE_CURVE ( ( 0.9330127018922194093, 0.9330127018922194093, 1.000000000000000000, 0.8660254037844387076, 1.000000000000000000, 0.8660254037844387076, 1.000000000000000000, 0.9330127018922194093, 0.9330127018922194093 ) ) 
 REPRESENTATION_ITEM ( '' )  );
#32546 = CARTESIAN_POINT ( 'NONE',  ( -2.229367062499996610, 20.85416666803226349, 3.861377020970582219 ) ) ;
#32547 = CARTESIAN_POINT ( 'NONE',  ( 2.229367062500001939, -56.97916666530107932, 3.861377020970579999 ) ) ;
#32548 = CARTESIAN_POINT ( 'NONE',  ( -4.458734124999997661, -1.479166665301071992, 2.574251347313722516 ) ) ;
#32549 = AXIS2_PLACEMENT_3D ( 'NONE', #40928, #26785, #17131 ) ;
#32550 = DIRECTION ( 'NONE',  ( 0.000000000000000000, 0.000000000000000000, 1.000000000000000000 ) ) ;
#32551 = CARTESIAN_POINT ( 'NONE',  ( -4.999999999999999112, 13.08333333333333037, 2.886751345948131764 ) ) ;
#32552 = CARTESIAN_POINT ( 'NONE',  ( 2.071067811865475505, -142.9375000027312126, -5.000000000000000888 ) ) ;
#32553 = CARTESIAN_POINT ( 'NONE',  ( 1.975475456537005874E-15, -45.74999999999999289, 5.000000000000000000 ) ) ;
#32554 = CARTESIAN_POINT ( 'NONE',  ( -3.152548672688508926E-16, -45.56249999863439371, -5.148502694627439702 ) ) ;
#32555 = CARTESIAN_POINT ( 'NONE',  ( 5.000000000000000888, -85.45833333060213022, 2.886751345948126879 ) ) ;
#32556 = VECTOR ( 'NONE', #22948, 1000.000000000000000 ) ;
#32557 = AXIS2_PLACEMENT_3D ( 'NONE', #41401, #36908, #7961 ) ;
#32558 = CARTESIAN_POINT ( 'NONE',  ( -52.80376928212989185, -135.1250000013656063, -4.297418129356379346 ) ) ;
#32559 = CYLINDRICAL_SURFACE ( 'NONE', #19541, 5.000000000000000000 ) ;
#32560 = CARTESIAN_POINT ( 'NONE',  ( -6.972266317189433020E-16, -92.24999999999998579, -5.000000000000000000 ) ) ;
#32561 = AXIS2_PLACEMENT_3D ( 'NONE', #38473, #19165, #48445 ) ;
#32562 = CARTESIAN_POINT ( 'NONE',  ( -4.458734124999999437, -84.64583333196773651, -2.574251347313719407 ) ) ;
#32563 = CARTESIAN_POINT ( 'NONE',  ( -3.152801135295367985, -158.0625000013656063, 3.152801135295367096 ) ) ;
#32564 = CARTESIAN_POINT ( 'NONE',  ( 5.000000000000000000, -31.41666666666667140, -2.886751345948129988 ) ) ;
#32565 = CARTESIAN_POINT ( 'NONE',  ( -1.339745962155610925, 24.20534180126147206, 5.000000000000000000 ) ) ;
#32566 = ORIENTED_EDGE ( 'NONE', *, *, #26111, .F. ) ;
#32567 = CARTESIAN_POINT ( 'NONE',  ( 2.229367062499998831, 18.10416666803225993, -3.861377020970580887 ) ) ;
#32568 = VERTEX_POINT ( 'NONE', #35081 ) ;
#32569 = CARTESIAN_POINT ( 'NONE',  ( 4.458734124999999437, -96.81249999863440792, -5.460374474430324690E-16 ) ) ;
#32570 = CARTESIAN_POINT ( 'NONE',  ( -2.229367062499996610, 8.604166668032261711, 3.861377020970582219 ) ) ;
#32571 = CARTESIAN_POINT ( 'NONE',  ( -2.499999999999996447, 12.29166666939785202, 4.330127018922195425 ) ) ;
#32572 =( BOUNDED_CURVE ( )  B_SPLINE_CURVE ( 2, ( #36, #29271, #23531, #19952, #48901, #4846, #350, #43755, #24465 ),
 .UNSPECIFIED., .F., .F. ) 
 B_SPLINE_CURVE_WITH_KNOTS ( ( 3, 2, 2, 2, 3 ),
 ( 0.8410714285714285809, 0.8416666666666666741, 0.8428571428571428603, 0.8440476190476190466, 0.8446428571428571397 ),
 .UNSPECIFIED. ) 
 CURVE ( )  GEOMETRIC_REPRESENTATION_ITEM ( )  RATIONAL_B_SPLINE_CURVE ( ( 0.9330127018922194093, 0.9330127018922194093, 1.000000000000000000, 0.8660254037844387076, 1.000000000000000000, 0.8660254037844387076, 1.000000000000000000, 0.9330127018922194093, 0.9330127018922194093 ) ) 
 REPRESENTATION_ITEM ( '' )  );
#32573 = CARTESIAN_POINT ( 'NONE',  ( -5.000000000000000000, -28.95833333060214443, -2.886751345948128211 ) ) ;
#32574 = CARTESIAN_POINT ( 'NONE',  ( 5.000000000000000000, 10.49999999999999822, -6.123233995736766282E-16 ) ) ;
#32575 = CARTESIAN_POINT ( 'NONE',  ( 2.229367062500001939, -54.97916666530107221, 3.861377020970579999 ) ) ;
#32576 = CARTESIAN_POINT ( 'NONE',  ( -1.339745962155610925, 15.33034180399266511, 5.000000000000000000 ) ) ;
#32577 = CARTESIAN_POINT ( 'NONE',  ( -4.999999999999999112, -79.91666666666667140, 2.886751345948131764 ) ) ;
#32578 = CARTESIAN_POINT ( 'NONE',  ( -4.458734124999998549, -30.22916666530106866, 2.574251347313722516 ) ) ;
#32579 = LINE ( 'NONE', #42226, #62548 ) ;
#32580 = CARTESIAN_POINT ( 'NONE',  ( -5.000000000000000000, -12.87499999726881050, 0.000000000000000000 ) ) ;
#32581 = CARTESIAN_POINT ( 'NONE',  ( 0.000000000000000000, -170.0000000000000000, 0.000000000000000000 ) ) ;
#32582 = CARTESIAN_POINT ( 'NONE',  ( -5.000000000000000000, -38.99999999999999289, 0.000000000000000000 ) ) ;
#32583 = LINE ( 'NONE', #11686, #32556 ) ;
#32585 = CARTESIAN_POINT ( 'NONE',  ( 2.229367062500001939, -22.22916666530107221, 3.861377020970579999 ) ) ;
#32584 = CARTESIAN_POINT ( 'NONE',  ( -5.000000000000000000, 15.00000000000000000, 0.000000000000000000 ) ) ;
#32586 = CARTESIAN_POINT ( 'NONE',  ( -4.229293425455167136E-15, -9.016621985895922009, -7.999704684617492845 ) ) ;
#32587 = CARTESIAN_POINT ( 'NONE',  ( -4.458734124999999437, -67.31249999863440792, 0.000000000000000000 ) ) ;
#32588 = CARTESIAN_POINT ( 'NONE',  ( 3.152801135295367541, -148.5625000013655779, -3.152801135295367541 ) ) ;
#32589 = CARTESIAN_POINT ( 'NONE',  ( 2.229367062499998831, -73.64583333196773651, -3.861377020970580887 ) ) ;
#32590 = CARTESIAN_POINT ( 'NONE',  ( -59.59170313451811296, -143.7500000013656063, 1.485763867205729394 ) ) ;
#32591 = CARTESIAN_POINT ( 'NONE',  ( -2.229367062499996610, -25.39583333196773651, 3.861377020970582219 ) ) ;
#32592 = CARTESIAN_POINT ( 'NONE',  ( -2.500000000000000444, -63.04166666393547303, -4.330127018922193649 ) ) ;
#32593 = VERTEX_POINT ( 'NONE', #5805 ) ;
#32594 = ORIENTED_EDGE ( 'NONE', *, *, #19414, .T. ) ;
#32595 = CARTESIAN_POINT ( 'NONE',  ( -4.458734124999999437, -65.64583333196773651, -2.574251347313719407 ) ) ;
#32596 = CARTESIAN_POINT ( 'NONE',  ( 5.000000000000000000, -7.291666663935481907, -2.886751345948130876 ) ) ;
#32597 = FACE_OUTER_BOUND ( 'NONE', #49493, .T. ) ;
#32598 = ORIENTED_EDGE ( 'NONE', *, *, #44055, .T. ) ;
#32599 = AXIS2_PLACEMENT_3D ( 'NONE', #56755, #56441, #16869 ) ;
#32600 = CARTESIAN_POINT ( 'NONE',  ( -50.01589407740564042, -126.6250000000000142, 0.3983568153799778022 ) ) ;
#32601 = FACE_OUTER_BOUND ( 'NONE', #37600, .T. ) ;
#32603 = ADVANCED_FACE ( 'NONE', ( #34756 ), #60172, .F. ) ;
#32602 = CARTESIAN_POINT ( 'NONE',  ( 9.457646018065525792E-16, -56.31249999863440081, 5.148502694627439702 ) ) ;
#32604 = AXIS2_PLACEMENT_3D ( 'NONE', #49249, #63110, #24172 ) ;
#32605 = ORIENTED_EDGE ( 'NONE', *, *, #52399, .T. ) ;
#32606 = AXIS2_PLACEMENT_3D ( 'NONE', #50737, #37452, #42895 ) ;
#32607 = CARTESIAN_POINT ( 'NONE',  ( 2.229367062500001939, 9.020833334698927786, 3.861377020970579999 ) ) ;
#32608 = CARTESIAN_POINT ( 'NONE',  ( -3.152548672688508926E-16, 17.43750000136559564, -5.148502694627439702 ) ) ;
#32609 = CARTESIAN_POINT ( 'NONE',  ( -56.48576386720575471, -149.7500000013656063, -4.591703134518078322 ) ) ;
#32610 = CARTESIAN_POINT ( 'NONE',  ( 2.500000000000002220, 20.45833333606451987, 4.330127018922192761 ) ) ;
#32611 = EDGE_LOOP ( 'NONE', ( #53235, #35119, #27814, #9230 ) ) ;
#32612 = CARTESIAN_POINT ( 'NONE',  ( 4.458734124999999437, -69.81249999863439371, -5.460374474430324690E-16 ) ) ;
#32613 = EDGE_CURVE ( 'NONE', #9714, #53941, #49857, .T. ) ;
#32614 = CARTESIAN_POINT ( 'NONE',  ( 2.499999999999998668, -10.20833333060214621, -4.330127018922193649 ) ) ;
#32615 = CARTESIAN_POINT ( 'NONE',  ( -3.152548672688508926E-16, 8.437500001365595637, -5.148502694627439702 ) ) ;
#32616 = DIRECTION ( 'NONE',  ( -0.000000000000000000, 1.000000000000000000, -0.000000000000000000 ) ) ;
#32617 = CARTESIAN_POINT ( 'NONE',  ( 4.458734124999999437, -62.06249999863440792, -5.460374474430324690E-16 ) ) ;
#32618 = CARTESIAN_POINT ( 'NONE',  ( 2.500000000000002220, -19.54166666393548013, 4.330127018922192761 ) ) ;
#32619 = EDGE_CURVE ( 'NONE', #35203, #4851, #41569, .T. ) ;
#32620 = CARTESIAN_POINT ( 'NONE',  ( -5.000000000000000000, -18.99999999999999645, 0.000000000000000000 ) ) ;
#32621 = CARTESIAN_POINT ( 'NONE',  ( 5.000000000000000000, -161.0625000000000000, 2.071067811865478614 ) ) ;
#32622 = CARTESIAN_POINT ( 'NONE',  ( 5.000000000000000888, 19.54166666939785202, 2.886751345948126879 ) ) ;
#32623 = CYLINDRICAL_SURFACE ( 'NONE', #838, 5.000000000000000000 ) ;
#32624 = CARTESIAN_POINT ( 'NONE',  ( -2.229367062500000163, -38.47916666530107221, -3.861377020970580443 ) ) ;
#32625 = CARTESIAN_POINT ( 'NONE',  ( 2.229367062499998831, -21.89583333196774007, -3.861377020970580887 ) ) ;
#32626 = ORIENTED_EDGE ( 'NONE', *, *, #18460, .F. ) ;
#32627 = LINE ( 'NONE', #37774, #50509 ) ;
#32628 = CARTESIAN_POINT ( 'NONE',  ( 4.458734124999999437, -106.8124999986343937, -5.460374474430324690E-16 ) ) ;
#32629 = CARTESIAN_POINT ( 'NONE',  ( -2.071067811865475061, -152.8125000027311842, -5.000000000000000888 ) ) ;
#32630 = ORIENTED_EDGE ( 'NONE', *, *, #39338, .F. ) ;
#32631 = CARTESIAN_POINT ( 'NONE',  ( -4.458734124999999437, -107.5624999986343937, 0.000000000000000000 ) ) ;
#32632 = CARTESIAN_POINT ( 'NONE',  ( 4.458734125000001214, -30.89583333196773296, 2.574251347313718519 ) ) ;
#32633 = CARTESIAN_POINT ( 'NONE',  ( -5.000000000000000000, -67.87499999726881583, 0.000000000000000000 ) ) ;
#32634 = CARTESIAN_POINT ( 'NONE',  ( -57.19623071787017210, -149.6250000013655779, 4.297418129356382899 ) ) ;
#32635 = CARTESIAN_POINT ( 'NONE',  ( -9.184850993605147944E-16, -145.2500000000000284, 5.000000000000000000 ) ) ;
#32636 = CARTESIAN_POINT ( 'NONE',  ( 4.458734125000000326, -29.89583333196773651, 2.574251347313718519 ) ) ;
#32637 = CARTESIAN_POINT ( 'NONE',  ( -3.152548672688508926E-16, -69.81249999863439371, -5.148502694627439702 ) ) ;
#32638 = CARTESIAN_POINT ( 'NONE',  ( 1.846868145590736310, -168.8750000013656063, 4.458734124999997661 ) ) ;
#32639 = CARTESIAN_POINT ( 'NONE',  ( 2.229367062499998831, -22.64583333196773651, -3.861377020970580887 ) ) ;
#32640 = CARTESIAN_POINT ( 'NONE',  ( 6.123233995736766282E-16, -170.0000000000000000, -5.000000000000000000 ) ) ;
#32641 = CARTESIAN_POINT ( 'NONE',  ( -5.000000000000000000, -17.08333333333333215, -2.886751345948128211 ) ) ;
#32642 = CARTESIAN_POINT ( 'NONE',  ( -8.190561711645485556E-16, -147.6875000013656063, 4.458734124999999437 ) ) ;
#32643 = ORIENTED_EDGE ( 'NONE', *, *, #41855, .T. ) ;
#32644 = CARTESIAN_POINT ( 'NONE',  ( 2.071067811865644703, -149.8125000000000568, -4.999999999999831246 ) ) ;
#32645 = CARTESIAN_POINT ( 'NONE',  ( -3.152548672688508926E-16, -51.81249999863440081, -5.148502694627439702 ) ) ;
#32646 = AXIS2_PLACEMENT_3D ( 'NONE', #54533, #36189, #40039 ) ;
#32647 = CARTESIAN_POINT ( 'NONE',  ( -6.972266317189433020E-16, -84.12499999726880162, -5.000000000000000000 ) ) ;
#32648 = CARTESIAN_POINT ( 'NONE',  ( 2.500000000000002220, -81.54166666393547303, 4.330127018922192761 ) ) ;
#32649 = CARTESIAN_POINT ( 'NONE',  ( 5.000000000000000000, 25.50000000000000000, -6.123233995736766282E-16 ) ) ;
#32650 = EDGE_CURVE ( 'NONE', #23818, #44517, #25511, .T. ) ;
#32651 =( BOUNDED_CURVE ( )  B_SPLINE_CURVE ( 2, ( #3561, #61788, #51503, #3255, #62424, #57285, #18342, #8073, #37964 ),
 .UNSPECIFIED., .F., .F. ) 
 B_SPLINE_CURVE_WITH_KNOTS ( ( 3, 2, 2, 2, 3 ),
 ( 0.8583333333333330595, 0.8624999999999998224, 0.8666666666666664742, 0.8708333333333332371, 0.8749999999999998890 ),
 .UNSPECIFIED. ) 
 CURVE ( )  GEOMETRIC_REPRESENTATION_ITEM ( )  RATIONAL_B_SPLINE_CURVE ( ( 1.000000000000003997, 0.9238795325112826307, 1.000000000000000000, 0.9238795325112867385, 1.000000000000000000, 0.9238795325112867385, 1.000000000000000000, 0.9238795325112887369, 0.9999999999999980016 ) ) 
 REPRESENTATION_ITEM ( '' )  );
#32652 = CARTESIAN_POINT ( 'NONE',  ( 2.500000000000002220, -76.54166666393547303, 4.330127018922192761 ) ) ;
#32653 = CARTESIAN_POINT ( 'NONE',  ( -4.458734124999999437, -3.395833331967739177, -2.574251347313719407 ) ) ;
#32654 = CARTESIAN_POINT ( 'NONE',  ( -6.972266317189433020E-16, -11.25000000000000178, -5.000000000000000000 ) ) ;
#32655 = CARTESIAN_POINT ( 'NONE',  ( 5.000000000000000000, -141.0000000000000000, 0.000000000000000000 ) ) ;
#32656 = CARTESIAN_POINT ( 'NONE',  ( -55.00000000000002132, -155.0000000000000284, 1.734723475976807094E-15 ) ) ;
#32657 = CARTESIAN_POINT ( 'NONE',  ( 9.457646018065525792E-16, 9.687500001365593860, 5.148502694627439702 ) ) ;
#32658 = ORIENTED_EDGE ( 'NONE', *, *, #22111, .F. ) ;
#32659 = CARTESIAN_POINT ( 'NONE',  ( 5.000000000000000888, -42.58333333333334281, 2.886751345948126879 ) ) ;
#32660 = ORIENTED_EDGE ( 'NONE', *, *, #48267, .T. ) ;
#32661 = CARTESIAN_POINT ( 'NONE',  ( 1.339745962155615144, -7.580341798530293218, 4.999999999999999112 ) ) ;
#32662 = CARTESIAN_POINT ( 'NONE',  ( -2.229367062500000163, -50.47916666530107221, -3.861377020970580443 ) ) ;
#32663 = CARTESIAN_POINT ( 'NONE',  ( 1.846868145590735200, -161.5000000013656063, -4.458734125000000326 ) ) ;
#32664 =( BOUNDED_CURVE ( )  B_SPLINE_CURVE ( 2, ( #28533, #27903, #48152, #49660, #18877, #34872, #58120, #14052, #9231 ),
 .UNSPECIFIED., .F., .F. ) 
 B_SPLINE_CURVE_WITH_KNOTS ( ( 3, 2, 2, 2, 3 ),
 ( 0.09166666666666674346, 0.09583333333333342308, 0.1000000000000000888, 0.1041666666666667546, 0.1083333333333334203 ),
 .UNSPECIFIED. ) 
 CURVE ( )  GEOMETRIC_REPRESENTATION_ITEM ( )  RATIONAL_B_SPLINE_CURVE ( ( 0.9999999999999984457, 0.9238795325112882928, 1.000000000000000000, 0.9238795325112867385, 1.000000000000000000, 0.9238795325112867385, 1.000000000000000000, 0.9238795325112851842, 1.000000000000001554 ) ) 
 REPRESENTATION_ITEM ( '' )  );
#32665 = CARTESIAN_POINT ( 'NONE',  ( -5.000000000000000000, -44.87499999726880873, 0.000000000000000000 ) ) ;
#32666 = EDGE_LOOP ( 'NONE', ( #33758, #20962, #33550, #25370 ) ) ;
#32667 = CARTESIAN_POINT ( 'NONE',  ( 2.229367062499998831, -21.64583333196774007, -3.861377020970580887 ) ) ;
#32668 = ORIENTED_EDGE ( 'NONE', *, *, #23178, .T. ) ;
#32669 = CARTESIAN_POINT ( 'NONE',  ( -3.535533905932738641, -142.5000000027311842, 3.535533905932737309 ) ) ;
#32670 = CARTESIAN_POINT ( 'NONE',  ( 4.458734124999999437, -160.5000000013656347, 1.846868145590737864 ) ) ;
#32671 = CARTESIAN_POINT ( 'NONE',  ( -4.999999999999998224, -38.79166666393548013, 2.886751345948131764 ) ) ;
#32672 = CARTESIAN_POINT ( 'NONE',  ( -58.80597590150559739, -138.0000000000000284, 3.242614290531460330 ) ) ;
#32673 = CARTESIAN_POINT ( 'NONE',  ( -2.229367062500000163, -38.72916666530107221, -3.861377020970580443 ) ) ;
#32674 = CARTESIAN_POINT ( 'NONE',  ( -3.535533905932738641, -147.5000000027311842, 3.535533905932737309 ) ) ;
#32675 = ORIENTED_EDGE ( 'NONE', *, *, #21760, .T. ) ;
#32676 = EDGE_CURVE ( 'NONE', #39148, #1448, #25128, .T. ) ;
#32677 = EDGE_CURVE ( 'NONE', #1040, #6259, #14805, .T. ) ;
#32678 = CARTESIAN_POINT ( 'NONE',  ( -4.458734124999999437, -81.39583333196773651, -2.574251347313719407 ) ) ;
#32679 = CARTESIAN_POINT ( 'NONE',  ( -4.458734124999998549, 25.77083333469892779, 2.574251347313722516 ) ) ;
#32680 = CARTESIAN_POINT ( 'NONE',  ( 1.975475456537005874E-15, -59.74999999999999289, 5.000000000000000000 ) ) ;
#32681 = EDGE_CURVE ( 'NONE', #30563, #57684, #47680, .T. ) ;
#32682 = ORIENTED_EDGE ( 'NONE', *, *, #30747, .T. ) ;
#32683 = CARTESIAN_POINT ( 'NONE',  ( -6.972266317189433020E-16, -60.12499999726880873, -5.000000000000000000 ) ) ;
#32684 = CARTESIAN_POINT ( 'NONE',  ( -52.10840900171896806, -138.4375000013656063, 3.393966926194110556 ) ) ;
#32685 = CARTESIAN_POINT ( 'NONE',  ( 9.457646018065525792E-16, -88.31249999863439371, 5.148502694627439702 ) ) ;
#32686 = CARTESIAN_POINT ( 'NONE',  ( -60.14911071818854538, -131.1875000027312126, 1.666127454062681368 ) ) ;
#32687 = CARTESIAN_POINT ( 'NONE',  ( 5.000000000000000000, 0.7083333360645185373, -2.886751345948130876 ) ) ;
#32688 = CARTESIAN_POINT ( 'NONE',  ( 2.071067811865392461, -145.3125000027312126, 5.000000000000084377 ) ) ;
#32689 = CARTESIAN_POINT ( 'NONE',  ( 4.458734124999998549, -55.72916666530107221, -2.574251347313721627 ) ) ;
#32690 = CARTESIAN_POINT ( 'NONE',  ( 1.339745962155615144, 21.29465819873852084, 4.999999999999999112 ) ) ;
#32691 = CARTESIAN_POINT ( 'NONE',  ( -4.458734124999999437, 23.68750000136559564, 0.000000000000000000 ) ) ;
#32692 = AXIS2_PLACEMENT_3D ( 'NONE', #41045, #4340, #52917 ) ;
#32693 = ADVANCED_FACE ( 'NONE', ( #19954 ), #25748, .T. ) ;
#32694 = CARTESIAN_POINT ( 'NONE',  ( 5.000000000000000000, -107.4166666666666572, -2.886751345948129988 ) ) ;
#32695 = CARTESIAN_POINT ( 'NONE',  ( -6.972266317189433020E-16, -63.12499999726880873, -5.000000000000000000 ) ) ;
#32696 = CARTESIAN_POINT ( 'NONE',  ( -4.458734124999999437, -41.56249999863440081, 0.000000000000000000 ) ) ;
#32697 = CARTESIAN_POINT ( 'NONE',  ( -3.535250795749689387E-16, -2.124999997268814944, -5.773502691896257311 ) ) ;
#32698 = CARTESIAN_POINT ( 'NONE',  ( -6.972266317189433020E-16, 16.87500000273118417, -5.000000000000000000 ) ) ;
#32699 = EDGE_CURVE ( 'NONE', #41738, #35585, #21014, .T. ) ;
#32700 = CARTESIAN_POINT ( 'NONE',  ( -4.458734124999999437, -83.56249999863439371, 0.000000000000000000 ) ) ;
#32701 = ADVANCED_FACE ( 'NONE', ( #51472 ), #36350, .T. ) ;
#32702 = CARTESIAN_POINT ( 'NONE',  ( -2.229367062500000163, -102.4791666653010651, -3.861377020970580443 ) ) ;
#32703 = CARTESIAN_POINT ( 'NONE',  ( -3.152548672688508926E-16, -6.812499998634404363, -5.148502694627439702 ) ) ;
#32704 = EDGE_LOOP ( 'NONE', ( #45839, #19832, #35520, #29026 ) ) ;
#32705 = CARTESIAN_POINT ( 'NONE',  ( 0.000000000000000000, -120.0000000000000000, 0.000000000000000000 ) ) ;
#32706 = CARTESIAN_POINT ( 'NONE',  ( -2.229367062500000163, -94.47916666530106511, -3.861377020970580443 ) ) ;
#32707 = EDGE_CURVE ( 'NONE', #44977, #35740, #7866, .T. ) ;
#32708 = CARTESIAN_POINT ( 'NONE',  ( 3.535533905932738197, -166.0000000027312126, -3.535533905932738197 ) ) ;
#32709 = CARTESIAN_POINT ( 'NONE',  ( -4.458734124999999437, -91.56249999863440792, 0.000000000000000000 ) ) ;
#32710 = CARTESIAN_POINT ( 'NONE',  ( 4.458734124999999437, 9.937500001365593860, -5.460374474430324690E-16 ) ) ;
#32711 = VECTOR ( 'NONE', #49934, 1000.000000000000000 ) ;
#32712 = CARTESIAN_POINT ( 'NONE',  ( -54.64476657466781973, -131.8125000013656063, -4.444560631937228834 ) ) ;
#32713 = CARTESIAN_POINT ( 'NONE',  ( 9.457646018065525792E-16, -12.06249999863440081, 5.148502694627439702 ) ) ;
#32714 = CARTESIAN_POINT ( 'NONE',  ( 4.458734125000001214, 11.85416666803225993, 2.574251347313718519 ) ) ;
#32715 = CARTESIAN_POINT ( 'NONE',  ( -4.458734124999999437, -55.56249999863440081, 0.000000000000000000 ) ) ;
#32716 = CARTESIAN_POINT ( 'NONE',  ( 4.458734124999999437, -169.6875000013656063, 0.000000000000000000 ) ) ;
#32717 = CARTESIAN_POINT ( 'NONE',  ( -4.458734124999999437, -10.31249999863440792, 0.000000000000000000 ) ) ;
#32718 = CARTESIAN_POINT ( 'NONE',  ( 2.500000000000002220, -109.5416666639354730, 4.330127018922192761 ) ) ;
#32719 = ORIENTED_EDGE ( 'NONE', *, *, #32424, .F. ) ;
#32720 = CARTESIAN_POINT ( 'NONE',  ( -2.229367062500000163, -33.72916666530107221, -3.861377020970580443 ) ) ;
#32721 =( BOUNDED_CURVE ( )  B_SPLINE_CURVE ( 2, ( #62543, #22983, #51931, #16332, #57083, #47723, #47416, #7872, #27476 ),
 .UNSPECIFIED., .F., .F. ) 
 B_SPLINE_CURVE_WITH_KNOTS ( ( 3, 2, 2, 2, 3 ),
 ( 0.4416666666666670404, 0.4458333333333337478, 0.4500000000000003997, 0.4541666666666671071, 0.4583333333333337589 ),
 .UNSPECIFIED. ) 
 CURVE ( )  GEOMETRIC_REPRESENTATION_ITEM ( )  RATIONAL_B_SPLINE_CURVE ( ( 0.9999999999999928946, 0.9238795325112938439, 1.000000000000000000, 0.9238795325112867385, 1.000000000000000000, 0.9238795325112867385, 1.000000000000000000, 0.9238795325112786339, 1.000000000000008216 ) ) 
 REPRESENTATION_ITEM ( '' )  );
#32722 = CARTESIAN_POINT ( 'NONE',  ( -51.60603307380591787, -128.1875000013656063, -2.891590998281053704 ) ) ;
#32723 = CARTESIAN_POINT ( 'NONE',  ( 0.000000000000000000, -120.0000000000000000, 0.000000000000000000 ) ) ;
#32724 = LINE ( 'NONE', #2290, #53216 ) ;
#32725 = CARTESIAN_POINT ( 'NONE',  ( -2.229367062499996610, -81.14583333196773651, 3.861377020970582219 ) ) ;
#32726 = CARTESIAN_POINT ( 'NONE',  ( 2.229367062499998831, 24.10416666803225993, -3.861377020970580887 ) ) ;
#32727 = CARTESIAN_POINT ( 'NONE',  ( 9.457646018065525792E-16, 12.93750000136559386, 5.148502694627439702 ) ) ;
#32728 = LINE ( 'NONE', #18868, #31818 ) ;
#32729 = CARTESIAN_POINT ( 'NONE',  ( 2.500000000000002220, -55.66666666666667140, 4.330127018922192761 ) ) ;
#32730 = CARTESIAN_POINT ( 'NONE',  ( -4.458734124999997661, -81.47916666530106511, 2.574251347313722516 ) ) ;
#32731 = CARTESIAN_POINT ( 'NONE',  ( -2.500000000000000444, -72.16666666666667140, -4.330127018922193649 ) ) ;
#32732 = CARTESIAN_POINT ( 'NONE',  ( 5.000000000000000000, -63.29166666393547303, -2.886751345948130876 ) ) ;
#32733 = CARTESIAN_POINT ( 'NONE',  ( -4.999999999999999112, 19.20833333606451632, 2.886751345948131764 ) ) ;
#32734 = ORIENTED_EDGE ( 'NONE', *, *, #50321, .T. ) ;
#32735 = CARTESIAN_POINT ( 'NONE',  ( -9.184850993605147944E-16, -147.3750000027312126, 5.000000000000000000 ) ) ;
#32736 = AXIS2_PLACEMENT_3D ( 'NONE', #18097, #37721, #2376 ) ;
#32738 = CARTESIAN_POINT ( 'NONE',  ( -5.000000000000000000, -30.08333333333333215, -2.886751345948128211 ) ) ;
#32737 = CARTESIAN_POINT ( 'NONE',  ( 1.162044386198238837E-16, 28.37500000273118417, 5.000000000000000000 ) ) ;
#32739 = CARTESIAN_POINT ( 'NONE',  ( 2.229367062500001939, -34.97916666530107221, 3.861377020970579999 ) ) ;
#32740 = AXIS2_PLACEMENT_3D ( 'NONE', #1048, #11297, #20654 ) ;
#32741 = DIRECTION ( 'NONE',  ( 0.000000000000000000, 0.000000000000000000, 1.000000000000000000 ) ) ;
#32742 = CARTESIAN_POINT ( 'NONE',  ( -5.000000000000000000, -29.95833333060214088, -2.886751345948128211 ) ) ;
#32744 = EDGE_LOOP ( 'NONE', ( #15353, #47838, #26590, #1216 ) ) ;
#32743 = CARTESIAN_POINT ( 'NONE',  ( 9.457646018065525792E-16, -62.06249999863440792, 5.148502694627439702 ) ) ;
#32745 = CARTESIAN_POINT ( 'NONE',  ( -7.500000000000000000, 4.330127018922191873, -10.00000000000000000 ) ) ;
#32747 = ORIENTED_EDGE ( 'NONE', *, *, #14147, .F. ) ;
#32746 = CARTESIAN_POINT ( 'NONE',  ( -4.458734124999999437, -11.64583333196773829, -2.574251347313719407 ) ) ;
#32748 = PRODUCT_DEFINITION ( 'UNKNOWN', '', #16439, #28784 ) ;
#32749 = CARTESIAN_POINT ( 'NONE',  ( 2.500000000000002220, -79.66666666666665719, 4.330127018922192761 ) ) ;
#32750 = CARTESIAN_POINT ( 'NONE',  ( -50.40829686548195099, -137.0000000013655779, -1.485763867205728284 ) ) ;
#32751 = CARTESIAN_POINT ( 'NONE',  ( 4.458734124999999437, -51.06249999863440792, -5.460374474430324690E-16 ) ) ;
#32752 =( BOUNDED_CURVE ( )  B_SPLINE_CURVE ( 2, ( #8809, #28425, #53498, #18763, #23916, #38085, #14256, #48039, #3682 ),
 .UNSPECIFIED., .F., .F. ) 
 B_SPLINE_CURVE_WITH_KNOTS ( ( 3, 2, 2, 2, 3 ),
 ( 0.9625000000000000222, 0.9630952380952381153, 0.9642857142857143016, 0.9654761904761904878, 0.9660714285714285809 ),
 .UNSPECIFIED. ) 
 CURVE ( )  GEOMETRIC_REPRESENTATION_ITEM ( )  RATIONAL_B_SPLINE_CURVE ( ( 0.9330127018922194093, 0.9330127018922194093, 1.000000000000000000, 0.8660254037844387076, 1.000000000000000000, 0.8660254037844387076, 1.000000000000000000, 0.9330127018922194093, 0.9330127018922194093 ) ) 
 REPRESENTATION_ITEM ( '' )  );
#32753 = CARTESIAN_POINT ( 'NONE',  ( 1.060575238724906964E-15, -77.62499999726881583, 5.773502691896257311 ) ) ;
#32755 = ORIENTED_EDGE ( 'NONE', *, *, #19406, .F. ) ;
#32754 = CARTESIAN_POINT ( 'NONE',  ( 1.975475456537005874E-15, -54.62499999726880873, 5.000000000000000000 ) ) ;
#32756 = CARTESIAN_POINT ( 'NONE',  ( -50.01589407740564042, -150.6250000000000284, 0.3983568153799778022 ) ) ;
#32757 = CARTESIAN_POINT ( 'NONE',  ( 4.458734124999998549, -21.97916666530107221, -2.574251347313721627 ) ) ;
#32759 = ORIENTED_EDGE ( 'NONE', *, *, #34361, .F. ) ;
#32758 = CARTESIAN_POINT ( 'NONE',  ( -4.458734124999999437, -58.56249999863440081, 0.000000000000000000 ) ) ;
#32760 = DIRECTION ( 'NONE',  ( 1.000000000000000000, 0.000000000000000000, 0.000000000000000000 ) ) ;
#32761 = CARTESIAN_POINT ( 'NONE',  ( -4.458734124999999437, -140.9375000013656063, -5.460374474430324690E-16 ) ) ;
#32762 = CARTESIAN_POINT ( 'NONE',  ( -4.458734124999998549, -98.47916666530105090, 2.574251347313722516 ) ) ;
#32763 = CARTESIAN_POINT ( 'NONE',  ( -5.000000000000000000, -26.87499999726881583, 0.000000000000000000 ) ) ;
#32764 = ORIENTED_EDGE ( 'NONE', *, *, #18629, .F. ) ;
#32765 = CARTESIAN_POINT ( 'NONE',  ( -57.19623071787016499, -151.6250000013655779, 4.297418129356382899 ) ) ;
#32766 = CARTESIAN_POINT ( 'NONE',  ( -51.75738570946856498, -140.8750000027312126, 3.805975901505576964 ) ) ;
#32767 = CARTESIAN_POINT ( 'NONE',  ( -1.339745962155610925, 1.330341803992665106, 5.000000000000000000 ) ) ;
#32768 = CARTESIAN_POINT ( 'NONE',  ( -4.458734124999999437, -7.395833331967734736, -2.574251347313719407 ) ) ;
#32769 = CARTESIAN_POINT ( 'NONE',  ( -4.458734124999999437, -95.56249999863440792, 0.000000000000000000 ) ) ;
#32770 = CARTESIAN_POINT ( 'NONE',  ( -1.846868145590737420, -148.0000000013655779, 4.458734124999999437 ) ) ;
#32771 = CARTESIAN_POINT ( 'NONE',  ( -2.229367062499996610, -29.39583333196774007, 3.861377020970582219 ) ) ;
#32772 = CARTESIAN_POINT ( 'NONE',  ( -2.500000000000000444, -67.16666666666667140, -4.330127018922193649 ) ) ;
#32773 = CARTESIAN_POINT ( 'NONE',  ( -52.80376928212989185, -136.8750000013656063, -4.297418129356379346 ) ) ;
#32774 = CARTESIAN_POINT ( 'NONE',  ( 2.229367062499998831, -67.89583333196773651, -3.861377020970580887 ) ) ;
#32775 = EDGE_CURVE ( 'NONE', #11538, #36394, #21239, .T. ) ;
#32776 = CARTESIAN_POINT ( 'NONE',  ( -6.972266317189433020E-16, -91.24999999999998579, -5.000000000000000000 ) ) ;
#32777 = CYLINDRICAL_SURFACE ( 'NONE', #58309, 5.000000000000000000 ) ;
#32778 = CARTESIAN_POINT ( 'NONE',  ( -4.458734124999999437, -142.9375000013656063, -5.460374474430324690E-16 ) ) ;
#32779 = VECTOR ( 'NONE', #13345, 1000.000000000000000 ) ;
#32780 = CARTESIAN_POINT ( 'NONE',  ( -3.152548672688508926E-16, 8.187500001365595637, -5.148502694627439702 ) ) ;
#32781 = ORIENTED_EDGE ( 'NONE', *, *, #50397, .F. ) ;
#32782 = CARTESIAN_POINT ( 'NONE',  ( -1.339745962155610925, -49.66965819600732601, 5.000000000000000000 ) ) ;
#32783 = EDGE_CURVE ( 'NONE', #33720, #57628, #49739, .T. ) ;
#32784 = CARTESIAN_POINT ( 'NONE',  ( 2.499999999999998668, 16.66666666666666785, -4.330127018922193649 ) ) ;
#32786 = CARTESIAN_POINT ( 'NONE',  ( 4.458734125000001214, -23.89583333196774007, 2.574251347313718519 ) ) ;
#32785 = CARTESIAN_POINT ( 'NONE',  ( -5.000000000000000000, -88.00000000000000000, 0.000000000000000000 ) ) ;
#32787 = CARTESIAN_POINT ( 'NONE',  ( -5.000000000000000000, 7.125000002731185944, 0.000000000000000000 ) ) ;
#32788 = CARTESIAN_POINT ( 'NONE',  ( -4.458734124999999437, -76.64583333196775072, -2.574251347313719407 ) ) ;
#32789 = AXIS2_PLACEMENT_3D ( 'NONE', #1133, #55784, #56100 ) ;
#32790 = CARTESIAN_POINT ( 'NONE',  ( -2.229367062499996610, 28.60416666803226349, 3.861377020970582219 ) ) ;
#32791 = CARTESIAN_POINT ( 'NONE',  ( 2.499999999999998668, -79.20833333060213022, -4.330127018922193649 ) ) ;
#32792 = CARTESIAN_POINT ( 'NONE',  ( -52.10840900171896806, -144.1875000013656063, 3.393966926194110556 ) ) ;
#32793 = EDGE_CURVE ( 'NONE', #14226, #33683, #58384, .T. ) ;
#32794 = CARTESIAN_POINT ( 'NONE',  ( 2.229367062500001939, 1.020833334698927120, 3.861377020970579999 ) ) ;
#32795 = DIRECTION ( 'NONE',  ( -0.000000000000000000, 1.000000000000000000, -0.000000000000000000 ) ) ;
#32796 = CARTESIAN_POINT ( 'NONE',  ( 1.975475456537005874E-15, -99.62499999726880162, 5.000000000000000000 ) ) ;
#32797 = CARTESIAN_POINT ( 'NONE',  ( -4.458734124999997661, 6.770833334698928674, 2.574251347313722516 ) ) ;
#32798 = CARTESIAN_POINT ( 'NONE',  ( 4.458734124999998549, -72.72916666530106511, -2.574251347313721627 ) ) ;
#32799 = CARTESIAN_POINT ( 'NONE',  ( -2.229367062500000163, -21.72916666530107221, -3.861377020970580443 ) ) ;
#32800 = CARTESIAN_POINT ( 'NONE',  ( -2.499999999999996447, -7.833333333333331261, 4.330127018922195425 ) ) ;
#32801 = CARTESIAN_POINT ( 'NONE',  ( 1.846868145590735200, -158.2500000013656063, -4.458734125000000326 ) ) ;
#32802 = CARTESIAN_POINT ( 'NONE',  ( -51.75738570946856498, -148.8750000027312126, 3.805975901505576964 ) ) ;
#32803 = CARTESIAN_POINT ( 'NONE',  ( 4.458734124999999437, -63.81249999863440792, -5.460374474430324690E-16 ) ) ;
#32804 = CARTESIAN_POINT ( 'NONE',  ( 5.000000000000000000, -101.2916666639354730, -2.886751345948129988 ) ) ;
#32805 = CARTESIAN_POINT ( 'NONE',  ( 0.000000000000000000, -120.0000000000000000, 5.000000000000000000 ) ) ;
#32806 = CARTESIAN_POINT ( 'NONE',  ( -2.229367062500000163, -39.47916666530107221, -3.861377020970580443 ) ) ;
#32807 = DIRECTION ( 'NONE',  ( -0.000000000000000000, 1.000000000000000000, -0.000000000000000000 ) ) ;
#32808 = CARTESIAN_POINT ( 'NONE',  ( -4.458734124999999437, -103.6458333319677365, -2.574251347313719407 ) ) ;
#32809 = CARTESIAN_POINT ( 'NONE',  ( 2.229367062500001939, -70.22916666530107932, 3.861377020970579999 ) ) ;
#32810 = CARTESIAN_POINT ( 'NONE',  ( -5.000000000000000000, -54.99999999999999289, 0.000000000000000000 ) ) ;
#32811 = CARTESIAN_POINT ( 'NONE',  ( 2.626220312808019583E-14, 14.87500000273118239, -5.000000000000000000 ) ) ;
#32812 = LINE ( 'NONE', #37319, #60257 ) ;
#32813 = ORIENTED_EDGE ( 'NONE', *, *, #58672, .F. ) ;
#32814 = CARTESIAN_POINT ( 'NONE',  ( 5.000000000000000888, -94.58333333333332860, 2.886751345948126879 ) ) ;
#32815 = CARTESIAN_POINT ( 'NONE',  ( 2.499999999999998668, -89.20833333060214443, -4.330127018922193649 ) ) ;
#32816 = CARTESIAN_POINT ( 'NONE',  ( -3.535250795749689387E-16, -11.25000000000000355, -5.773502691896257311 ) ) ;
#32817 = CARTESIAN_POINT ( 'NONE',  ( -4.458734124999999437, -15.31249999863440436, 0.000000000000000000 ) ) ;
#32818 = CARTESIAN_POINT ( 'NONE',  ( -4.458734124999997661, -77.22916666530106511, 2.574251347313722516 ) ) ;
#32819 = CARTESIAN_POINT ( 'NONE',  ( 5.000000000000000000, -59.37499999726880873, -6.123233995736766282E-16 ) ) ;
#32820 = CARTESIAN_POINT ( 'NONE',  ( 2.499999999999998668, -12.20833333060214798, -4.330127018922193649 ) ) ;
#32822 = EDGE_LOOP ( 'NONE', ( #48149, #3518, #8852, #41467 ) ) ;
#32821 = CARTESIAN_POINT ( 'NONE',  ( 4.458734125000001214, -45.89583333196774362, 2.574251347313718519 ) ) ;
#32823 = CARTESIAN_POINT ( 'NONE',  ( 1.339745962155615144, -81.70534180126146850, 4.999999999999999112 ) ) ;
#32825 = VERTEX_POINT ( 'NONE', #51783 ) ;
#32824 = CARTESIAN_POINT ( 'NONE',  ( -2.229367062500000163, 9.270833334698927786, -3.861377020970580443 ) ) ;
#32826 = CARTESIAN_POINT ( 'NONE',  ( 1.975475456537005874E-15, -71.62499999726878741, 5.000000000000000000 ) ) ;
#32827 = CARTESIAN_POINT ( 'NONE',  ( 1.060575238724906964E-15, -62.75000000000000000, 5.773502691896257311 ) ) ;
#32828 = CARTESIAN_POINT ( 'NONE',  ( -3.152801135295367985, -160.0625000013656063, 3.152801135295367096 ) ) ;
#32829 = CARTESIAN_POINT ( 'NONE',  ( 2.229367062499998831, -33.89583333196772941, -3.861377020970580887 ) ) ;
#32830 = CARTESIAN_POINT ( 'NONE',  ( 1.975475456537005874E-15, -55.74999999999999289, 5.000000000000000000 ) ) ;
#32831 = CARTESIAN_POINT ( 'NONE',  ( -4.458734124999999437, -78.31249999863440792, 0.000000000000000000 ) ) ;
#32832 = CARTESIAN_POINT ( 'NONE',  ( -5.000000000000000888, -164.5625000000000000, -2.071067811865475949 ) ) ;
#32833 = CARTESIAN_POINT ( 'NONE',  ( 1.975475456537005874E-15, -11.74999999999999645, 5.000000000000000000 ) ) ;
#32834 = CARTESIAN_POINT ( 'NONE',  ( -58.39396692619412477, -129.6875000013656063, 2.891590998281057701 ) ) ;
#32835 = CARTESIAN_POINT ( 'NONE',  ( -2.229367062499996610, -5.395833331967740953, 3.861377020970582219 ) ) ;
#32836 = CARTESIAN_POINT ( 'NONE',  ( -4.458734124999999437, -43.56249999863440081, 0.000000000000000000 ) ) ;
#32837 = ADVANCED_FACE ( 'NONE', ( #27330 ), #12225, .T. ) ;
#32838 = CARTESIAN_POINT ( 'NONE',  ( 2.500000000000002220, -26.66666666666666430, 4.330127018922192761 ) ) ;
#32839 = CARTESIAN_POINT ( 'NONE',  ( 4.458734124999998549, -81.97916666530106511, -2.574251347313721627 ) ) ;
#32840 = LINE ( 'NONE', #21925, #13270 ) ;
#32841 = ORIENTED_EDGE ( 'NONE', *, *, #31517, .F. ) ;
#32842 = CARTESIAN_POINT ( 'NONE',  ( -51.19402409849444524, -153.6250000027312126, -3.242614290531456334 ) ) ;
#32843 = DIRECTION ( 'NONE',  ( 0.000000000000000000, 0.000000000000000000, 1.000000000000000000 ) ) ;
#32844 = CARTESIAN_POINT ( 'NONE',  ( 4.458734125000001214, -69.14583333196773651, 2.574251347313718519 ) ) ;
#32845 = CARTESIAN_POINT ( 'NONE',  ( -3.152801135295367985, -145.0625000013655779, 3.152801135295367096 ) ) ;
#32846 = ORIENTED_EDGE ( 'NONE', *, *, #53511, .F. ) ;
#32847 = CARTESIAN_POINT ( 'NONE',  ( -5.000000000000000888, -150.5625000027311842, 2.071067811865474617 ) ) ;
#32848 =( BOUNDED_CURVE ( )  B_SPLINE_CURVE ( 2, ( #46050, #1690, #49911, #45413, #1381, #36398, #20981, #2013, #5865 ),
 .UNSPECIFIED., .F., .F. ) 
 B_SPLINE_CURVE_WITH_KNOTS ( ( 3, 2, 2, 2, 3 ),
 ( 0.3303571428571428492, 0.3309523809523809423, 0.3321428571428571286, 0.3333333333333333148, 0.3339285714285714080 ),
 .UNSPECIFIED. ) 
 CURVE ( )  GEOMETRIC_REPRESENTATION_ITEM ( )  RATIONAL_B_SPLINE_CURVE ( ( 0.9330127018922194093, 0.9330127018922194093, 1.000000000000000000, 0.8660254037844387076, 1.000000000000000000, 0.8660254037844387076, 1.000000000000000000, 0.9330127018922194093, 0.9330127018922194093 ) ) 
 REPRESENTATION_ITEM ( '' )  );
#32849 = CARTESIAN_POINT ( 'NONE',  ( 2.499999999999998668, 17.66666666666666430, -4.330127018922193649 ) ) ;
#32850 = CARTESIAN_POINT ( 'NONE',  ( 2.229367062500001939, -14.22916666530107221, 3.861377020970579999 ) ) ;
#32851 = CARTESIAN_POINT ( 'NONE',  ( 1.975475456537005874E-15, -34.75000000000000000, 5.000000000000000000 ) ) ;
#32852 = CARTESIAN_POINT ( 'NONE',  ( -2.229367062499996610, 0.8541666680322613781, 3.861377020970582219 ) ) ;
#32853 = CARTESIAN_POINT ( 'NONE',  ( 5.000000000000000000, -30.29166666393547658, -2.886751345948130876 ) ) ;
#32854 = CARTESIAN_POINT ( 'NONE',  ( 4.458734124999997661, -157.5000000013656063, 1.846868145590737864 ) ) ;
#32855 = CARTESIAN_POINT ( 'NONE',  ( -4.458734124999997661, 28.52083333469892423, 2.574251347313722516 ) ) ;
#32856 = ORIENTED_EDGE ( 'NONE', *, *, #27440, .T. ) ;
#32857 = CARTESIAN_POINT ( 'NONE',  ( 4.458734124999999437, -92.81249999863440792, -5.460374474430324690E-16 ) ) ;
#32858 = CARTESIAN_POINT ( 'NONE',  ( -2.499999999999996447, -67.83333333333332860, 4.330127018922195425 ) ) ;
#32859 = CARTESIAN_POINT ( 'NONE',  ( -5.000000000000000000, -63.08333333333331439, -2.886751345948128211 ) ) ;
#32860 = CARTESIAN_POINT ( 'NONE',  ( -2.229367062499996610, -6.145833331967740953, 3.861377020970582219 ) ) ;
#32861 = CARTESIAN_POINT ( 'NONE',  ( 1.339745962155615144, -51.70534180126148271, 4.999999999999999112 ) ) ;
#32862 = FACE_OUTER_BOUND ( 'NONE', #49501, .T. ) ;
#32863 = FACE_OUTER_BOUND ( 'NONE', #4447, .T. ) ;
#32864 = CARTESIAN_POINT ( 'NONE',  ( -3.535250795749689387E-16, -35.12499999726881583, -5.773502691896257311 ) ) ;
#32865 = CARTESIAN_POINT ( 'NONE',  ( 0.000000000000000000, -120.0000000000000000, 0.000000000000000000 ) ) ;
#32866 = CARTESIAN_POINT ( 'NONE',  ( -4.458734124999999437, 16.68750000136559564, 0.000000000000000000 ) ) ;
#32867 = DIRECTION ( 'NONE',  ( 0.000000000000000000, 0.000000000000000000, 1.000000000000000000 ) ) ;
#32868 = CARTESIAN_POINT ( 'NONE',  ( -3.152548672688508926E-16, 20.43750000136559208, -5.148502694627439702 ) ) ;
#32869 = CARTESIAN_POINT ( 'NONE',  ( 4.458734124999998549, -58.72916666530106511, -2.574251347313721627 ) ) ;
#32870 = CARTESIAN_POINT ( 'NONE',  ( 2.229367062500001939, -5.229166665301071326, 3.861377020970579999 ) ) ;
#32871 = CARTESIAN_POINT ( 'NONE',  ( 1.975475456537005874E-15, -33.62499999726880873, 5.000000000000000000 ) ) ;
#32872 = CARTESIAN_POINT ( 'NONE',  ( 5.000000000000000888, 10.41666666666666607, 2.886751345948126879 ) ) ;
#32873 = CARTESIAN_POINT ( 'NONE',  ( -5.000000000000000888, -142.5625000027312694, 2.071067811865474617 ) ) ;
#32874 = CARTESIAN_POINT ( 'NONE',  ( -53.33387254593719717, -144.9375000027312410, 5.149110718188530278 ) ) ;
#32875 = AXIS2_PLACEMENT_3D ( 'NONE', #2303, #20643, #30265 ) ;
#32876 = CARTESIAN_POINT ( 'NONE',  ( 4.458734125000001214, -46.89583333196773651, 2.574251347313718519 ) ) ;
#32877 = CARTESIAN_POINT ( 'NONE',  ( 5.000000000000000888, -82.45833333060214443, 2.886751345948126879 ) ) ;
#32878 = CARTESIAN_POINT ( 'NONE',  ( -50.40829686548195099, -135.2500000013656347, -1.485763867205728284 ) ) ;
#32879 = CARTESIAN_POINT ( 'NONE',  ( -1.339745962155613812, -17.20534180126147916, -5.000000000000000000 ) ) ;
#32880 = CARTESIAN_POINT ( 'NONE',  ( -54.60164318462004474, -145.3750000000000284, -4.984105922594373794 ) ) ;
#32881 = CARTESIAN_POINT ( 'NONE',  ( 2.229367062500001939, -90.22916666530106511, 3.861377020970579999 ) ) ;
#32882 = CARTESIAN_POINT ( 'NONE',  ( -8.190561711645485556E-16, -157.9375000013655779, 4.458734124999999437 ) ) ;
#32883 = CARTESIAN_POINT ( 'NONE',  ( -2.500000000000000444, -33.16666666666666430, -4.330127018922193649 ) ) ;
#32884 = SURFACE_STYLE_FILL_AREA ( #18083 ) ;
#32885 = ORIENTED_EDGE ( 'NONE', *, *, #31527, .T. ) ;
#32886 = CARTESIAN_POINT ( 'NONE',  ( -3.152548672688508926E-16, 17.18750000136559919, -5.148502694627439702 ) ) ;
#32887 = ORIENTED_EDGE ( 'NONE', *, *, #10339, .F. ) ;
#32888 = CARTESIAN_POINT ( 'NONE',  ( -3.152548672688508926E-16, -96.56249999863439371, -5.148502694627439702 ) ) ;
#32889 = CARTESIAN_POINT ( 'NONE',  ( -2.229367062499996610, 7.604166668032260823, 3.861377020970582219 ) ) ;
#32890 = CARTESIAN_POINT ( 'NONE',  ( 2.500000000000002220, 10.45833333606451987, 4.330127018922192761 ) ) ;
#32891 = DIRECTION ( 'NONE',  ( -0.000000000000000000, 1.000000000000000000, -0.000000000000000000 ) ) ;
#32892 = CARTESIAN_POINT ( 'NONE',  ( -3.535250795749689387E-16, 1.750000000000001554, -5.773502691896257311 ) ) ;
#32893 = EDGE_CURVE ( 'NONE', #55181, #32387, #44852, .T. ) ;
#32894 = AXIS2_PLACEMENT_3D ( 'NONE', #9969, #48886, #63073 ) ;
#32895 = CARTESIAN_POINT ( 'NONE',  ( -4.458734124999999437, -60.31249999863440081, 0.000000000000000000 ) ) ;
#32896 = CYLINDRICAL_SURFACE ( 'NONE', #61635, 5.000000000000000000 ) ;
#32897 = CARTESIAN_POINT ( 'NONE',  ( 5.000000000000000000, -81.41666666666667140, -2.886751345948129988 ) ) ;
#32898 = CARTESIAN_POINT ( 'NONE',  ( -2.229367062500000163, -30.47916666530107221, -3.861377020970580443 ) ) ;
#32899 = CARTESIAN_POINT ( 'NONE',  ( -1.339745962155610925, -37.66965819600733312, 5.000000000000000000 ) ) ;
#32900 = CARTESIAN_POINT ( 'NONE',  ( -2.500000000000000444, 25.95833333606451632, -4.330127018922193649 ) ) ;
#32901 =( BOUNDED_CURVE ( )  B_SPLINE_CURVE ( 2, ( #32830, #18349, #53386, #18966, #14456, #9010, #47921, #43722, #19283 ),
 .UNSPECIFIED., .F., .F. ) 
 B_SPLINE_CURVE_WITH_KNOTS ( ( 3, 2, 2, 2, 3 ),
 ( 0.7145833333333333481, 0.7152777777777777901, 0.7166666666666666741, 0.7180555555555555580, 0.7187500000000000000 ),
 .UNSPECIFIED. ) 
 CURVE ( )  GEOMETRIC_REPRESENTATION_ITEM ( )  RATIONAL_B_SPLINE_CURVE ( ( 0.9330127018922194093, 0.9330127018922194093, 1.000000000000000000, 0.8660254037844387076, 1.000000000000000000, 0.8660254037844387076, 1.000000000000000000, 0.9330127018922194093, 0.9330127018922194093 ) ) 
 REPRESENTATION_ITEM ( '' )  );
#32902 = CYLINDRICAL_SURFACE ( 'NONE', #8364, 5.000000000000000000 ) ;
#32903 = CARTESIAN_POINT ( 'NONE',  ( -4.999999999999999112, -39.91666666666667140, 2.886751345948131764 ) ) ;
#32904 = CARTESIAN_POINT ( 'NONE',  ( 0.000000000000000000, -170.0000000000000000, 5.000000000000000000 ) ) ;
#32907 = CARTESIAN_POINT ( 'NONE',  ( -4.458734124999999437, -20.64583333196774007, -2.574251347313719407 ) ) ;
#32906 =( BOUNDED_CURVE ( )  B_SPLINE_CURVE ( 2, ( #36475, #46127, #16223, #50635, #6573, #35846, #60935, #60620, #51286 ),
 .UNSPECIFIED., .F., .F. ) 
 B_SPLINE_CURVE_WITH_KNOTS ( ( 3, 2, 2, 2, 3 ),
 ( 0.9517857142857142350, 0.9523809523809523281, 0.9535714285714286254, 0.9547619047619048116, 0.9553571428571429047 ),
 .UNSPECIFIED. ) 
 CURVE ( )  GEOMETRIC_REPRESENTATION_ITEM ( )  RATIONAL_B_SPLINE_CURVE ( ( 0.9330127018922194093, 0.9330127018922194093, 1.000000000000000000, 0.8660254037844387076, 1.000000000000000000, 0.8660254037844387076, 1.000000000000000000, 0.9330127018922194093, 0.9330127018922194093 ) ) 
 REPRESENTATION_ITEM ( '' )  );
#32905 = CARTESIAN_POINT ( 'NONE',  ( 1.975475456537005874E-15, 6.375000002731185944, 5.000000000000000000 ) ) ;
#32908 = CARTESIAN_POINT ( 'NONE',  ( -3.823040241140506157E-16, -8.660254037844399733, -7.564338275809332046 ) ) ;
#32909 = CARTESIAN_POINT ( 'NONE',  ( 4.458734124999999437, -62.81249999863440792, -5.460374474430324690E-16 ) ) ;
#32910 = CARTESIAN_POINT ( 'NONE',  ( -1.846868145590737420, -149.0000000013656063, 4.458734124999999437 ) ) ;
#32911 = CARTESIAN_POINT ( 'NONE',  ( 4.458734124999999437, -74.81249999863440792, -5.460374474430324690E-16 ) ) ;
#32912 = CARTESIAN_POINT ( 'NONE',  ( -59.44456063193725015, -141.8125000013656063, -0.3552334253322034230 ) ) ;
#32913 = CARTESIAN_POINT ( 'NONE',  ( 2.229367062499998831, -26.89583333196774007, -3.861377020970580887 ) ) ;
#32914 = CARTESIAN_POINT ( 'NONE',  ( 2.500000000000002220, -64.54166666393547303, 4.330127018922192761 ) ) ;
#32915 = ORIENTED_EDGE ( 'NONE', *, *, #55941, .T. ) ;
#32916 = CARTESIAN_POINT ( 'NONE',  ( -57.46284108482265651, -148.0625000027312126, 4.819101127000238627 ) ) ;
#32917 = VERTEX_POINT ( 'NONE', #54587 ) ;
#32918 = CARTESIAN_POINT ( 'NONE',  ( 2.229367062499998831, -67.89583333196773651, -3.861377020970580887 ) ) ;
#32919 = FACE_OUTER_BOUND ( 'NONE', #60482, .T. ) ;
#32920 = ORIENTED_EDGE ( 'NONE', *, *, #34552, .T. ) ;
#32921 = LINE ( 'NONE', #14782, #5653 ) ;
#32923 = VECTOR ( 'NONE', #20465, 1000.000000000000000 ) ;
#32922 = CARTESIAN_POINT ( 'NONE',  ( -4.999999999999998224, -77.79166666393547303, 2.886751345948131764 ) ) ;
#32924 = CARTESIAN_POINT ( 'NONE',  ( -3.152548672688508926E-16, -54.81249999863440081, -5.148502694627439702 ) ) ;
#32925 = CARTESIAN_POINT ( 'NONE',  ( 4.458734124999999437, 0.9375000013655959696, -5.460374474430324690E-16 ) ) ;
#32926 = EDGE_LOOP ( 'NONE', ( #52451, #52600, #20164, #24733 ) ) ;
#32927 = CARTESIAN_POINT ( 'NONE',  ( -6.972266317189433020E-16, -45.24999999999999289, -5.000000000000000000 ) ) ;
#32928 = CARTESIAN_POINT ( 'NONE',  ( -4.458734124999999437, 3.687500001365594748, 0.000000000000000000 ) ) ;
#32929 = CARTESIAN_POINT ( 'NONE',  ( 2.229367062500001939, 18.02083333469892779, 3.861377020970579999 ) ) ;
#32930 = CARTESIAN_POINT ( 'NONE',  ( -52.10840900171896806, -145.1875000013656063, 3.393966926194110556 ) ) ;
#32931 = CARTESIAN_POINT ( 'NONE',  ( 1.339745962155612702, -92.16965819600733312, -5.000000000000000000 ) ) ;
#32932 = CARTESIAN_POINT ( 'NONE',  ( 3.152801135295367541, -168.3125000013656063, -3.152801135295367541 ) ) ;
#32933 = EDGE_LOOP ( 'NONE', ( #11623, #52347, #10199, #23395 ) ) ;
#32934 = CARTESIAN_POINT ( 'NONE',  ( -2.229367062499996610, -74.14583333196773651, 3.861377020970582219 ) ) ;
#32935 = CARTESIAN_POINT ( 'NONE',  ( 0.000000000000000000, -120.0000000000000000, 5.000000000000000000 ) ) ;
#32936 = CARTESIAN_POINT ( 'NONE',  ( 2.229367062500001939, 9.020833334698927786, 3.861377020970579999 ) ) ;
#32937 = FACE_OUTER_BOUND ( 'NONE', #37793, .T. ) ;
#32938 = CARTESIAN_POINT ( 'NONE',  ( -4.458734124999999437, -62.64583333196774362, -2.574251347313719407 ) ) ;
#32939 = CARTESIAN_POINT ( 'NONE',  ( 2.499999999999998668, -18.20833333060214798, -4.330127018922193649 ) ) ;
#32940 = DIRECTION ( 'NONE',  ( 0.000000000000000000, -1.000000000000000000, 0.000000000000000000 ) ) ;
#32941 = CARTESIAN_POINT ( 'NONE',  ( 1.975475456537005874E-15, -28.62499999726881583, 5.000000000000000000 ) ) ;
#32942 = CARTESIAN_POINT ( 'NONE',  ( 2.500000000000002220, -65.66666666666667140, 4.330127018922192761 ) ) ;
#32943 = CARTESIAN_POINT ( 'NONE',  ( 0.000000000000000000, -120.0000000000000000, 0.000000000000000000 ) ) ;
#32944 = CARTESIAN_POINT ( 'NONE',  ( 2.229367062499998831, -39.64583333196773651, -3.861377020970580887 ) ) ;
#32945 = CARTESIAN_POINT ( 'NONE',  ( 4.458734124999999437, -26.06249999863440792, -5.460374474430324690E-16 ) ) ;
#32946 =( BOUNDED_CURVE ( )  B_SPLINE_CURVE ( 2, ( #57979, #18421, #43794, #48938, #19038, #3640, #33840, #13904, #8771 ),
 .UNSPECIFIED., .F., .F. ) 
 B_SPLINE_CURVE_WITH_KNOTS ( ( 3, 2, 2, 2, 3 ),
 ( 0.03392857142857143293, 0.03452380952380952606, 0.03571428571428571230, 0.03690476190476190549, 0.03750000000000000555 ),
 .UNSPECIFIED. ) 
 CURVE ( )  GEOMETRIC_REPRESENTATION_ITEM ( )  RATIONAL_B_SPLINE_CURVE ( ( 0.9330127018922194093, 0.9330127018922197424, 1.000000000000000000, 0.8660254037844387076, 1.000000000000000000, 0.8660254037844387076, 1.000000000000000000, 0.9330127018922189652, 0.9330127018922194093 ) ) 
 REPRESENTATION_ITEM ( '' )  );
#32947 = CARTESIAN_POINT ( 'NONE',  ( 0.000000000000000000, -170.0000000000000000, 5.000000000000000000 ) ) ;
#32948 = CARTESIAN_POINT ( 'NONE',  ( 5.000000000000000000, 29.58333333333332860, -2.886751345948129988 ) ) ;
#32949 = CARTESIAN_POINT ( 'NONE',  ( -9.184850993605147944E-16, -152.3750000027311842, 5.000000000000000000 ) ) ;
#32950 = ORIENTED_EDGE ( 'NONE', *, *, #31015, .T. ) ;
#32951 = CARTESIAN_POINT ( 'NONE',  ( 2.229367062499998831, -107.8958333319677365, -3.861377020970580887 ) ) ;
#32952 = CARTESIAN_POINT ( 'NONE',  ( -4.458734124999999437, -31.39583333196773296, -2.574251347313719407 ) ) ;
#32953 = CARTESIAN_POINT ( 'NONE',  ( 2.499999999999998668, -66.20833333060213022, -4.330127018922193649 ) ) ;
#32954 = CARTESIAN_POINT ( 'NONE',  ( -50.40829686548195099, -149.2500000013655779, -1.485763867205728284 ) ) ;
#32955 = CARTESIAN_POINT ( 'NONE',  ( 5.000000000000000888, -148.9375000000000000, -2.071067811865475505 ) ) ;
#32956 = CARTESIAN_POINT ( 'NONE',  ( -2.229367062499996610, -30.14583333196773651, 3.861377020970582219 ) ) ;
#32957 = CARTESIAN_POINT ( 'NONE',  ( 2.229367062500001939, -70.22916666530107932, 3.861377020970579999 ) ) ;
#32958 = CARTESIAN_POINT ( 'NONE',  ( 2.730187237215162345E-16, -169.4375000013656063, -4.458734124999999437 ) ) ;
#32959 = CARTESIAN_POINT ( 'NONE',  ( -3.152548672688508926E-16, -30.56249999863440436, -5.148502694627439702 ) ) ;
#32960 = CARTESIAN_POINT ( 'NONE',  ( -58.24261429053147765, -136.3750000027312126, -3.805975901505573855 ) ) ;
#32961 = CARTESIAN_POINT ( 'NONE',  ( 0.000000000000000000, -120.0000000000000000, 0.000000000000000000 ) ) ;
#32962 = CARTESIAN_POINT ( 'NONE',  ( 5.000000000000000000, -16.41666666666667140, -2.886751345948129988 ) ) ;
#32963 = CARTESIAN_POINT ( 'NONE',  ( -3.152801135295367096, -147.0625000013655779, -3.152801135295367541 ) ) ;
#32964 = VERTEX_POINT ( 'NONE', #10202 ) ;
#32965 = MECHANICAL_DESIGN_GEOMETRIC_PRESENTATION_REPRESENTATION (  '', ( #34979 ), #20618 ) ;
#32966 = CARTESIAN_POINT ( 'NONE',  ( 5.000000000000000000, -150.0625000000000284, 2.071067811865478614 ) ) ;
#32967 = CARTESIAN_POINT ( 'NONE',  ( -4.458734124999997661, -54.47916666530107932, 2.574251347313722516 ) ) ;
#32968 = CARTESIAN_POINT ( 'NONE',  ( 5.000000000000000888, 27.54166666939785557, 2.886751345948126879 ) ) ;
#32969 = LINE ( 'NONE', #13031, #35036 ) ;
#32970 = CARTESIAN_POINT ( 'NONE',  ( 2.499999999999998668, 17.66666666666666430, -4.330127018922193649 ) ) ;
#32971 = AXIS2_PLACEMENT_3D ( 'NONE', #47294, #22223, #46023 ) ;
#32972 = ADVANCED_FACE ( 'NONE', ( #40096 ), #45884, .T. ) ;
#32973 = CARTESIAN_POINT ( 'NONE',  ( -4.999999999999998224, -88.91666666666667140, 2.886751345948131764 ) ) ;
#32974 = CARTESIAN_POINT ( 'NONE',  ( -4.458734124999999437, 1.687500001365593194, 0.000000000000000000 ) ) ;
#32975 = DIRECTION ( 'NONE',  ( -0.000000000000000000, 1.000000000000000000, -0.000000000000000000 ) ) ;
#32976 = CARTESIAN_POINT ( 'NONE',  ( -3.535533905932738641, -164.3750000000000284, 3.535533905932737309 ) ) ;
#32977 = CARTESIAN_POINT ( 'NONE',  ( -4.458734124999998549, 9.520833334698927786, 2.574251347313722516 ) ) ;
#32978 = ORIENTED_EDGE ( 'NONE', *, *, #14581, .T. ) ;
#32979 = DIRECTION ( 'NONE',  ( -0.000000000000000000, -1.000000000000000000, -0.000000000000000000 ) ) ;
#32980 = VERTEX_POINT ( 'NONE', #50073 ) ;
#32981 = CARTESIAN_POINT ( 'NONE',  ( 1.339745962155612702, -7.169658196007335782, -5.000000000000000000 ) ) ;
#32982 = CARTESIAN_POINT ( 'NONE',  ( 4.458734124999998549, -49.72916666530106511, -2.574251347313721627 ) ) ;
#32983 = CARTESIAN_POINT ( 'NONE',  ( -3.152801135295367985, -161.0625000013656063, 3.152801135295367096 ) ) ;
#32984 = EDGE_CURVE ( 'NONE', #44449, #41004, #51824, .T. ) ;
#32985 = CARTESIAN_POINT ( 'NONE',  ( 5.000000000000000000, -49.29166666393547303, -2.886751345948129988 ) ) ;
#32986 = ORIENTED_EDGE ( 'NONE', *, *, #13712, .F. ) ;
#32988 = EDGE_CURVE ( 'NONE', #49453, #46511, #30773, .T. ) ;
#32987 = CARTESIAN_POINT ( 'NONE',  ( 4.458734124999999437, -21.81249999863440436, -5.460374474430324690E-16 ) ) ;
#32989 = EDGE_LOOP ( 'NONE', ( #58761, #35956, #15650, #34474 ) ) ;
#32991 = CARTESIAN_POINT ( 'NONE',  ( -4.999999999999998224, -11.91666666666666607, 2.886751345948131764 ) ) ;
#32990 = CARTESIAN_POINT ( 'NONE',  ( -1.339745962155613812, -0.08034179853029406460, -5.000000000000000000 ) ) ;
#32992 = CARTESIAN_POINT ( 'NONE',  ( 4.458734125000000326, -161.3750000013656063, -1.846868145590734978 ) ) ;
#32993 = CYLINDRICAL_SURFACE ( 'NONE', #3647, 5.000000000000000000 ) ;
#32994 = CARTESIAN_POINT ( 'NONE',  ( -57.46284108482265651, -138.9375000000000000, 4.819101127000239515 ) ) ;
#32995 = CARTESIAN_POINT ( 'NONE',  ( 4.458734124999999437, -36.06249999863440792, -5.460374474430324690E-16 ) ) ;
#32996 = VERTEX_POINT ( 'NONE', #5698 ) ;
#32997 = EDGE_CURVE ( 'NONE', #60061, #3585, #49360, .T. ) ;
#32998 = CARTESIAN_POINT ( 'NONE',  ( 2.229367062500001939, -82.97916666530106511, 3.861377020970579999 ) ) ;
#32999 = CARTESIAN_POINT ( 'NONE',  ( -4.458734124999998549, 22.77083333469892423, 2.574251347313722516 ) ) ;
#33000 = CARTESIAN_POINT ( 'NONE',  ( 0.000000000000000000, -170.0000000000000000, 0.000000000000000000 ) ) ;
#33001 = ORIENTED_EDGE ( 'NONE', *, *, #14600, .T. ) ;
#33002 = CARTESIAN_POINT ( 'NONE',  ( -54.64476657466781973, -139.0625000013656063, -4.444560631937228834 ) ) ;
#33003 = CARTESIAN_POINT ( 'NONE',  ( 2.229367062500001939, -83.22916666530106511, 3.861377020970579999 ) ) ;
#33004 = CARTESIAN_POINT ( 'NONE',  ( -55.39835681537999790, -127.0000000027312126, 4.984105922594378235 ) ) ;
#33005 = CARTESIAN_POINT ( 'NONE',  ( 0.000000000000000000, -120.0000000000000000, 0.000000000000000000 ) ) ;
#33006 = CARTESIAN_POINT ( 'NONE',  ( -8.190561711645485556E-16, -139.9375000013656063, 4.458734124999999437 ) ) ;
#33007 = CARTESIAN_POINT ( 'NONE',  ( 1.339745962155586056, 4.294658198738518173, 5.000000000000015987 ) ) ;
#33008 = CARTESIAN_POINT ( 'NONE',  ( 2.229367062499998831, -56.64583333196773651, -3.861377020970580887 ) ) ;
#33009 = CARTESIAN_POINT ( 'NONE',  ( -6.972266317189433020E-16, 21.75000000000000000, -5.000000000000000000 ) ) ;
#33010 = VECTOR ( 'NONE', #41698, 1000.000000000000000 ) ;
#33011 = CARTESIAN_POINT ( 'NONE',  ( -2.229367062499996610, 21.85416666803226349, 3.861377020970582219 ) ) ;
#33012 = CARTESIAN_POINT ( 'NONE',  ( 1.339745962155612702, -102.1696581960073331, -5.000000000000000000 ) ) ;
#33013 = CARTESIAN_POINT ( 'NONE',  ( -5.000000000000000000, -82.08333333333332860, -2.886751345948128211 ) ) ;
#33014 = CARTESIAN_POINT ( 'NONE',  ( -4.458734124999999437, -45.56249999863440081, 0.000000000000000000 ) ) ;
#33015 = EDGE_CURVE ( 'NONE', #43823, #53443, #3361, .T. ) ;
#33016 = CARTESIAN_POINT ( 'NONE',  ( 5.000000000000000000, -6.291666663935480130, -2.886751345948129988 ) ) ;
#33017 = DIRECTION ( 'NONE',  ( 0.000000000000000000, 0.000000000000000000, 1.000000000000000000 ) ) ;
#33018 = CARTESIAN_POINT ( 'NONE',  ( -55.35523342533222291, -125.3125000013655921, 4.444560631937231499 ) ) ;
#33019 = CARTESIAN_POINT ( 'NONE',  ( -4.458734124999999437, -82.64583333196772230, -2.574251347313719407 ) ) ;
#33020 = CARTESIAN_POINT ( 'NONE',  ( -2.229367062500000163, -104.4791666653010651, -3.861377020970580443 ) ) ;
#33021 = CARTESIAN_POINT ( 'NONE',  ( -3.152548672688508926E-16, -11.81249999863440969, -5.148502694627439702 ) ) ;
#33022 = ORIENTED_EDGE ( 'NONE', *, *, #32783, .F. ) ;
#33023 = CARTESIAN_POINT ( 'NONE',  ( -5.000000000000000000, -16.95833333060214443, -2.886751345948128211 ) ) ;
#33024 = CARTESIAN_POINT ( 'NONE',  ( -4.458734124999998549, -92.22916666530106511, 2.574251347313722516 ) ) ;
#33025 = CARTESIAN_POINT ( 'NONE',  ( 2.071067811865476394, -167.3125000027312126, 5.000000000000000000 ) ) ;
#33026 = CARTESIAN_POINT ( 'NONE',  ( -4.458734124999998549, -94.47916666530106511, 2.574251347313722516 ) ) ;
#33027 = CARTESIAN_POINT ( 'NONE',  ( -5.000000000000000000, -52.87499999726881583, 0.000000000000000000 ) ) ;
#33028 = CARTESIAN_POINT ( 'NONE',  ( -1.339745962155610925, -29.79465819873851729, 5.000000000000000000 ) ) ;
#33029 =( BOUNDED_CURVE ( )  B_SPLINE_CURVE ( 2, ( #54192, #29099, #38755, #495, #10445, #49369, #20099, #30060, #49687 ),
 .UNSPECIFIED., .F., .F. ) 
 B_SPLINE_CURVE_WITH_KNOTS ( ( 3, 2, 2, 2, 3 ),
 ( 0.04791666666666666990, 0.04861111111111111188, 0.05000000000000000278, 0.05138888888888888673, 0.05208333333333333565 ),
 .UNSPECIFIED. ) 
 CURVE ( )  GEOMETRIC_REPRESENTATION_ITEM ( )  RATIONAL_B_SPLINE_CURVE ( ( 0.9330127018922192983, 0.9330127018922196314, 1.000000000000000000, 0.8660254037844387076, 1.000000000000000000, 0.8660254037844387076, 1.000000000000000000, 0.9330127018922189652, 0.9330127018922192983 ) ) 
 REPRESENTATION_ITEM ( '' )  );
#33030 = CARTESIAN_POINT ( 'NONE',  ( -54.64476657466781973, -129.8125000013656063, -4.444560631937228834 ) ) ;
#33031 = CARTESIAN_POINT ( 'NONE',  ( 4.458734125000000326, -14.89583333196773474, 2.574251347313718519 ) ) ;
#33032 = CARTESIAN_POINT ( 'NONE',  ( -2.229367062499996610, 13.60416666803226171, 3.861377020970582219 ) ) ;
#33033 = CARTESIAN_POINT ( 'NONE',  ( -3.152548672688508926E-16, -51.81249999863440081, -5.148502694627439702 ) ) ;
#33034 = CARTESIAN_POINT ( 'NONE',  ( 2.500000000000002220, -86.54166666393547303, 4.330127018922192761 ) ) ;
#33035 = CARTESIAN_POINT ( 'NONE',  ( -5.000000000000000000, -152.5000000000000284, -6.123233995736766282E-16 ) ) ;
#33036 = CARTESIAN_POINT ( 'NONE',  ( -4.458734124999999437, -11.39583333196774007, -2.574251347313719407 ) ) ;
#33037 = LINE ( 'NONE', #14658, #61719 ) ;
#33038 = VERTEX_POINT ( 'NONE', #29803 ) ;
#33039 = CARTESIAN_POINT ( 'NONE',  ( 4.458734124999999437, -39.06249999863440081, -5.460374474430324690E-16 ) ) ;
#33040 = UNCERTAINTY_MEASURE_WITH_UNIT (LENGTH_MEASURE( 1.000000000000000082E-05 ), #13615, 'distance_accuracy_value', 'NONE');
#33041 = CARTESIAN_POINT ( 'NONE',  ( -51.60603307380591787, -125.1875000013656063, -2.891590998281053704 ) ) ;
#33042 = CARTESIAN_POINT ( 'NONE',  ( 2.499999999999998668, 26.79166666939785202, -4.330127018922193649 ) ) ;
#33043 = DIRECTION ( 'NONE',  ( 0.000000000000000000, 0.000000000000000000, 1.000000000000000000 ) ) ;
#33044 = CARTESIAN_POINT ( 'NONE',  ( 9.457646018065525792E-16, -83.06249999863439371, 5.148502694627439702 ) ) ;
#33045 = CARTESIAN_POINT ( 'NONE',  ( 9.457646018065525792E-16, 23.68750000136559564, 5.148502694627439702 ) ) ;
#33046 = ADVANCED_FACE ( 'NONE', ( #10832 ), #59417, .T. ) ;
#33047 = CARTESIAN_POINT ( 'NONE',  ( 9.457646018065525792E-16, 16.93750000136559564, 5.148502694627439702 ) ) ;
#33048 = EDGE_CURVE ( 'NONE', #28941, #36379, #1313, .T. ) ;
#33049 = ADVANCED_FACE ( 'NONE', ( #39460, #59095 ), #46206, .F. ) ;
#33050 = FACE_OUTER_BOUND ( 'NONE', #10368, .T. ) ;
#33051 = DIRECTION ( 'NONE',  ( 0.000000000000000000, 0.000000000000000000, 1.000000000000000000 ) ) ;
#33052 = CARTESIAN_POINT ( 'NONE',  ( 2.229367062499998831, -83.89583333196773651, -3.861377020970580887 ) ) ;
#33053 = CARTESIAN_POINT ( 'NONE',  ( 5.000000000000000000, -67.50000000000000000, -6.123233995736766282E-16 ) ) ;
#33054 = CARTESIAN_POINT ( 'NONE',  ( -4.999999999999999112, 16.20833333606451987, 2.886751345948131764 ) ) ;
#33055 = ORIENTED_EDGE ( 'NONE', *, *, #42218, .F. ) ;
#33056 = CARTESIAN_POINT ( 'NONE',  ( 2.499999999999998668, -18.20833333060214798, -4.330127018922193649 ) ) ;
#33057 = CARTESIAN_POINT ( 'NONE',  ( -58.24261429053147765, -144.3750000027312126, -3.805975901505573855 ) ) ;
#33059 = CARTESIAN_POINT ( 'NONE',  ( 5.000000000000000888, -31.58333333333333215, 2.886751345948126879 ) ) ;
#33058 = CARTESIAN_POINT ( 'NONE',  ( 5.000000000000000000, -40.49999999999999289, -6.123233995736766282E-16 ) ) ;
#33060 = CARTESIAN_POINT ( 'NONE',  ( 9.457646018065525792E-16, -35.06249999863440792, 5.148502694627439702 ) ) ;
#33061 = DIRECTION ( 'NONE',  ( -0.000000000000000000, 1.000000000000000000, -0.000000000000000000 ) ) ;
#33062 = EDGE_CURVE ( 'NONE', #25630, #55067, #31729, .T. ) ;
#33063 = CARTESIAN_POINT ( 'NONE',  ( 5.000000000000000888, -30.45833333060214443, 2.886751345948126879 ) ) ;
#33065 = EDGE_LOOP ( 'NONE', ( #32594, #30867, #52573, #30802 ) ) ;
#33064 = CARTESIAN_POINT ( 'NONE',  ( 4.458734125000001214, -60.89583333196774362, 2.574251347313718519 ) ) ;
#33066 = CARTESIAN_POINT ( 'NONE',  ( -56.48576386720575471, -154.0000000013655779, -4.591703134518078322 ) ) ;
#33067 = EDGE_CURVE ( 'NONE', #23303, #30363, #5413, .T. ) ;
#33069 = ORIENTED_EDGE ( 'NONE', *, *, #61030, .F. ) ;
#33068 = CARTESIAN_POINT ( 'NONE',  ( -4.458734124999999437, -6.645833331967741842, -2.574251347313719407 ) ) ;
#33070 = CARTESIAN_POINT ( 'NONE',  ( 1.060575238724906964E-15, -76.74999999999998579, 5.773502691896257311 ) ) ;
#33071 = CARTESIAN_POINT ( 'NONE',  ( 1.162044386198238837E-16, 28.37500000273118417, 5.000000000000000000 ) ) ;
#33072 = CARTESIAN_POINT ( 'NONE',  ( -2.229367062499996610, -54.39583333196773651, 3.861377020970582219 ) ) ;
#33073 = CARTESIAN_POINT ( 'NONE',  ( -4.999999999999999112, -75.79166666393545881, 2.886751345948131764 ) ) ;
#33075 = ORIENTED_EDGE ( 'NONE', *, *, #17013, .F. ) ;
#33074 = DIRECTION ( 'NONE',  ( -0.000000000000000000, 1.000000000000000000, -0.000000000000000000 ) ) ;
#33076 = CARTESIAN_POINT ( 'NONE',  ( -53.33387254593733928, -147.8125000000000000, 5.149110718188519620 ) ) ;
#33077 = CARTESIAN_POINT ( 'NONE',  ( 2.229367062499998831, -21.89583333196774007, -3.861377020970580887 ) ) ;
#33079 = VERTEX_POINT ( 'NONE', #37196 ) ;
#33078 = CARTESIAN_POINT ( 'NONE',  ( -4.458734124999999437, -54.64583333196774362, -2.574251347313719407 ) ) ;
#33080 = CARTESIAN_POINT ( 'NONE',  ( 4.458734124999999437, -167.7500000013655779, 1.846868145590737864 ) ) ;
#33081 = CARTESIAN_POINT ( 'NONE',  ( 4.458734124999998549, -98.97916666530105090, -2.574251347313721627 ) ) ;
#33082 = CARTESIAN_POINT ( 'NONE',  ( 1.975475456537005874E-15, -8.624999997268812280, 5.000000000000000000 ) ) ;
#33083 = ORIENTED_EDGE ( 'NONE', *, *, #47502, .F. ) ;
#33084 = CARTESIAN_POINT ( 'NONE',  ( -50.55543936806279248, -152.3125000013656063, 0.3552334253322060320 ) ) ;
#33085 = CARTESIAN_POINT ( 'NONE',  ( -56.66612745406270335, -142.4375000027312126, -5.149110718188516067 ) ) ;
#33086 = CARTESIAN_POINT ( 'NONE',  ( 5.000000000000000888, -83.58333333333332860, 2.886751345948126879 ) ) ;
#33087 = CARTESIAN_POINT ( 'NONE',  ( 2.229367062500001939, -8.979166665301075767, 3.861377020970579999 ) ) ;
#33088 = CARTESIAN_POINT ( 'NONE',  ( 4.458734125000000326, -99.14583333196773651, 2.574251347313718519 ) ) ;
#33089 = CARTESIAN_POINT ( 'NONE',  ( 3.152801135295366208, -144.8125000013655779, 3.152801135295367985 ) ) ;
#33090 = CARTESIAN_POINT ( 'NONE',  ( 4.458734125000001214, -26.14583333196774007, 2.574251347313718519 ) ) ;
#33091 = DIRECTION ( 'NONE',  ( 0.000000000000000000, 0.000000000000000000, 1.000000000000000000 ) ) ;
#33092 = CARTESIAN_POINT ( 'NONE',  ( -59.44456063193725015, -137.5625000013656063, -0.3552334253322034230 ) ) ;
#33093 = CARTESIAN_POINT ( 'NONE',  ( 4.458734124999998549, -69.97916666530107932, -2.574251347313721627 ) ) ;
#33094 = CARTESIAN_POINT ( 'NONE',  ( 1.339745962155612702, -21.16965819600733312, -5.000000000000000000 ) ) ;
#33095 = CARTESIAN_POINT ( 'NONE',  ( 2.499999999999998668, -88.20833333060214443, -4.330127018922193649 ) ) ;
#33096 = CARTESIAN_POINT ( 'NONE',  ( -6.972266317189433020E-16, -68.24999999999998579, -5.000000000000000000 ) ) ;
#33097 = CARTESIAN_POINT ( 'NONE',  ( 4.458734125000000326, 7.854166668032260823, 2.574251347313718519 ) ) ;
#33098 =( BOUNDED_CURVE ( )  B_SPLINE_CURVE ( 2, ( #21383, #40026, #30380, #41300, #36178, #40669, #11716, #31333, #31020 ),
 .UNSPECIFIED., .F., .F. ) 
 B_SPLINE_CURVE_WITH_KNOTS ( ( 3, 2, 2, 2, 3 ),
 ( 0.7520833333333333259, 0.7527777777777777679, 0.7541666666666666519, 0.7555555555555555358, 0.7562499999999999778 ),
 .UNSPECIFIED. ) 
 CURVE ( )  GEOMETRIC_REPRESENTATION_ITEM ( )  RATIONAL_B_SPLINE_CURVE ( ( 0.9330127018922194093, 0.9330127018922194093, 1.000000000000000000, 0.8660254037844387076, 1.000000000000000000, 0.8660254037844387076, 1.000000000000000000, 0.9330127018922194093, 0.9330127018922194093 ) ) 
 REPRESENTATION_ITEM ( '' )  );
#33099 = ORIENTED_EDGE ( 'NONE', *, *, #36121, .F. ) ;
#33100 = LINE ( 'NONE', #19873, #47973 ) ;
#33101 = CARTESIAN_POINT ( 'NONE',  ( 5.000000000000000000, -160.0625000000000568, 2.071067811865478614 ) ) ;
#33103 = CARTESIAN_POINT ( 'NONE',  ( 4.458734125000001214, -25.89583333196774007, 2.574251347313718519 ) ) ;
#33102 = CARTESIAN_POINT ( 'NONE',  ( 2.500000000000002220, -90.66666666666665719, 4.330127018922192761 ) ) ;
#33104 = CARTESIAN_POINT ( 'NONE',  ( 0.000000000000000000, -120.0000000000000000, 5.000000000000000000 ) ) ;
#33105 = CARTESIAN_POINT ( 'NONE',  ( -3.152548672688508926E-16, -77.81249999863440792, -5.148502694627439702 ) ) ;
#33106 = CARTESIAN_POINT ( 'NONE',  ( 2.229367062499998831, 23.10416666803225993, -3.861377020970580887 ) ) ;
#33107 = CARTESIAN_POINT ( 'NONE',  ( 0.000000000000000000, -170.0000000000000000, 0.000000000000000000 ) ) ;
#33108 = CARTESIAN_POINT ( 'NONE',  ( -52.10840900171896806, -143.1875000013656063, 3.393966926194110556 ) ) ;
#33109 = CARTESIAN_POINT ( 'NONE',  ( -4.458734124999999437, 5.687500001365592972, 0.000000000000000000 ) ) ;
#33110 = CARTESIAN_POINT ( 'NONE',  ( 2.229367062499998831, 26.10416666803225993, -3.861377020970580887 ) ) ;
#33111 = CARTESIAN_POINT ( 'NONE',  ( 4.458734124999999437, -39.06249999863440081, -5.460374474430324690E-16 ) ) ;
#33112 = CARTESIAN_POINT ( 'NONE',  ( 1.339745962155612702, -43.16965819600731891, -5.000000000000000000 ) ) ;
#33113 = CARTESIAN_POINT ( 'NONE',  ( -4.458734124999999437, 4.604166668032261711, -2.574251347313719407 ) ) ;
#33114 = CARTESIAN_POINT ( 'NONE',  ( -2.229367062499996610, -72.14583333196773651, 3.861377020970582219 ) ) ;
#33115 = CARTESIAN_POINT ( 'NONE',  ( 4.458734124999999437, -17.06249999863440792, -5.460374474430324690E-16 ) ) ;
#33116 = CARTESIAN_POINT ( 'NONE',  ( 1.060575238724906964E-15, -3.750000000000003553, 5.773502691896257311 ) ) ;
#33117 = CARTESIAN_POINT ( 'NONE',  ( 3.152801135295366208, -157.5625000013656063, 3.152801135295367985 ) ) ;
#33118 = FACE_OUTER_BOUND ( 'NONE', #35878, .T. ) ;
#33119 =( REPRESENTATION_RELATIONSHIP ('NONE','NONE', #27855, #14320 ) REPRESENTATION_RELATIONSHIP_WITH_TRANSFORMATION ( #60056 )SHAPE_REPRESENTATION_RELATIONSHIP( ) );
#33120 = CARTESIAN_POINT ( 'NONE',  ( 4.458734125000001214, -65.89583333196772230, 2.574251347313718519 ) ) ;
#33121 = CARTESIAN_POINT ( 'NONE',  ( -2.500000000000000444, -98.04166666393545881, -4.330127018922193649 ) ) ;
#33122 = CARTESIAN_POINT ( 'NONE',  ( 9.457646018065525792E-16, 28.93750000136559564, 5.148502694627439702 ) ) ;
#33123 = CARTESIAN_POINT ( 'NONE',  ( 9.457646018065525792E-16, -41.06249999863440081, 5.148502694627439702 ) ) ;
#33124 = EDGE_CURVE ( 'NONE', #14229, #23523, #32086, .T. ) ;
#33125 = CARTESIAN_POINT ( 'NONE',  ( 0.2791032213812723040, -8.821394357840571132, -7.929128246061910801 ) ) ;
#33126 = CARTESIAN_POINT ( 'NONE',  ( -4.458734124999999437, -105.5624999986344221, 0.000000000000000000 ) ) ;
#33127 = CARTESIAN_POINT ( 'NONE',  ( -4.458734124999999437, -67.64583333196773651, -2.574251347313719407 ) ) ;
#33128 = CARTESIAN_POINT ( 'NONE',  ( -3.535250795749689387E-16, -53.24999999999999289, -5.773502691896257311 ) ) ;
#33129 = CARTESIAN_POINT ( 'NONE',  ( -4.999999999999998224, -22.91666666666666785, 2.886751345948131764 ) ) ;
#33130 = CARTESIAN_POINT ( 'NONE',  ( 2.500000000000002220, 28.45833333606451987, 4.330127018922192761 ) ) ;
#33131 = ORIENTED_EDGE ( 'NONE', *, *, #54313, .T. ) ;
#33132 = CARTESIAN_POINT ( 'NONE',  ( 2.229367062500001939, -109.9791666653010651, 3.861377020970579999 ) ) ;
#33133 =( BOUNDED_CURVE ( )  B_SPLINE_CURVE ( 2, ( #25690, #40786, #60433, #35979, #55608, #11524, #50766, #6709, #7666 ),
 .UNSPECIFIED., .F., .F. ) 
 B_SPLINE_CURVE_WITH_KNOTS ( ( 3, 2, 2, 2, 3 ),
 ( 0.4854166666666666630, 0.4861111111111111049, 0.4874999999999999889, 0.4888888888888888729, 0.4895833333333333148 ),
 .UNSPECIFIED. ) 
 CURVE ( )  GEOMETRIC_REPRESENTATION_ITEM ( )  RATIONAL_B_SPLINE_CURVE ( ( 0.9330127018922194093, 0.9330127018922194093, 1.000000000000000000, 0.8660254037844387076, 1.000000000000000000, 0.8660254037844387076, 1.000000000000000000, 0.9330127018922194093, 0.9330127018922194093 ) ) 
 REPRESENTATION_ITEM ( '' )  );
#33134 = ADVANCED_FACE ( 'NONE', ( #22406 ), #36237, .T. ) ;
#33135 = CARTESIAN_POINT ( 'NONE',  ( -6.972266317189433020E-16, -87.12499999726880162, -5.000000000000000000 ) ) ;
#33136 = CARTESIAN_POINT ( 'NONE',  ( 2.499999999999998668, -15.33333333333333037, -4.330127018922193649 ) ) ;
#33137 = CARTESIAN_POINT ( 'NONE',  ( 4.458734124999998549, -15.72916666530107399, -2.574251347313721627 ) ) ;
#33138 = EDGE_CURVE ( 'NONE', #14909, #26438, #34505, .T. ) ;
#33139 = CARTESIAN_POINT ( 'NONE',  ( -2.229367062499996610, -78.14583333196773651, 3.861377020970582219 ) ) ;
#33140 = CARTESIAN_POINT ( 'NONE',  ( -4.999999999999998224, -4.791666663935479242, 2.886751345948131764 ) ) ;
#33141 = CARTESIAN_POINT ( 'NONE',  ( -5.000000000000000000, -12.95833333060214976, -2.886751345948128211 ) ) ;
#33143 = ORIENTED_EDGE ( 'NONE', *, *, #36170, .T. ) ;
#33142 = CARTESIAN_POINT ( 'NONE',  ( 2.229367062500001939, -45.97916666530106511, 3.861377020970579999 ) ) ;
#33144 = CARTESIAN_POINT ( 'NONE',  ( 2.500000000000002220, -41.66666666666667140, 4.330127018922192761 ) ) ;
#33146 = EDGE_LOOP ( 'NONE', ( #21976, #19934, #23966, #6930 ) ) ;
#33145 = CARTESIAN_POINT ( 'NONE',  ( -4.458734124999999437, 7.437500001365594748, 0.000000000000000000 ) ) ;
#33147 = CARTESIAN_POINT ( 'NONE',  ( -56.48576386720575471, -153.7500000013656063, -4.591703134518078322 ) ) ;
#33148 = CARTESIAN_POINT ( 'NONE',  ( -2.500000000000000444, -59.16666666666665719, -4.330127018922193649 ) ) ;
#33149 = EDGE_CURVE ( 'NONE', #47469, #27835, #51452, .T. ) ;
#33150 = CARTESIAN_POINT ( 'NONE',  ( -4.458734125000001214, -157.1250000013656063, 1.846868145590734089 ) ) ;
#33151 = CARTESIAN_POINT ( 'NONE',  ( 9.457646018065525792E-16, -38.31249999863441502, 5.148502694627439702 ) ) ;
#33152 = CARTESIAN_POINT ( 'NONE',  ( -6.972266317189433020E-16, -14.24999999999999822, -5.000000000000000000 ) ) ;
#33153 = CARTESIAN_POINT ( 'NONE',  ( -5.000000000000000000, -167.5000000000000000, -6.123233995736766282E-16 ) ) ;
#33154 = ADVANCED_FACE ( 'NONE', ( #56821 ), #6978, .T. ) ;
#33155 = CARTESIAN_POINT ( 'NONE',  ( -59.29741812935640155, -132.8750000013656063, -2.196230717870135685 ) ) ;
#33156 = CARTESIAN_POINT ( 'NONE',  ( 9.457646018065525792E-16, -3.312499998634407472, 5.148502694627439702 ) ) ;
#33157 = CARTESIAN_POINT ( 'NONE',  ( 4.458734124999999437, -40.06249999863440081, -5.460374474430324690E-16 ) ) ;
#33158 = EDGE_CURVE ( 'NONE', #58699, #47465, #9909, .T. ) ;
#33159 = CARTESIAN_POINT ( 'NONE',  ( 1.975475456537005874E-15, -83.62499999726878741, 5.000000000000000000 ) ) ;
#33160 = CARTESIAN_POINT ( 'NONE',  ( -8.190561711645485556E-16, -150.6875000013656063, 4.458734124999999437 ) ) ;
#33161 = CARTESIAN_POINT ( 'NONE',  ( -4.458734124999998549, -86.47916666530107932, 2.574251347313722516 ) ) ;
#33162 = CARTESIAN_POINT ( 'NONE',  ( 5.000000000000000000, -108.4166666666666572, -2.886751345948130876 ) ) ;
#33163 = EDGE_LOOP ( 'NONE', ( #43877, #40977, #17956, #54852 ) ) ;
#33164 = CARTESIAN_POINT ( 'NONE',  ( -58.80597590150559739, -154.1250000027312126, 3.242614290531460330 ) ) ;
#33165 = DIRECTION ( 'NONE',  ( -0.000000000000000000, 1.000000000000000000, -0.000000000000000000 ) ) ;
#33166 = CARTESIAN_POINT ( 'NONE',  ( -3.152548672688508926E-16, -69.81249999863439371, -5.148502694627439702 ) ) ;
#33167 = CARTESIAN_POINT ( 'NONE',  ( 4.458734124999999437, -146.6250000013655779, -1.846868145590734978 ) ) ;
#33168 = ORIENTED_EDGE ( 'NONE', *, *, #8596, .T. ) ;
#33169 = CARTESIAN_POINT ( 'NONE',  ( -2.499999999999996447, -70.70833333060214443, 4.330127018922195425 ) ) ;
#33170 = CARTESIAN_POINT ( 'NONE',  ( -3.152548672688508926E-16, -11.81249999863440969, -5.148502694627439702 ) ) ;
#33171 = CARTESIAN_POINT ( 'NONE',  ( -9.184850993605147944E-16, -141.2500000000000284, 5.000000000000000000 ) ) ;
#33172 = CARTESIAN_POINT ( 'NONE',  ( -4.458734124999999437, 2.687500001365593860, 0.000000000000000000 ) ) ;
#33173 = CARTESIAN_POINT ( 'NONE',  ( 1.846868145590736310, -151.6250000013655779, 4.458734124999997661 ) ) ;
#33174 = CARTESIAN_POINT ( 'NONE',  ( -2.229367062500000163, 24.27083333469892779, -3.861377020970580443 ) ) ;
#33175 = ORIENTED_EDGE ( 'NONE', *, *, #42212, .F. ) ;
#33176 = CARTESIAN_POINT ( 'NONE',  ( 4.458734124999999437, -89.81249999863440792, -5.460374474430324690E-16 ) ) ;
#33177 = CARTESIAN_POINT ( 'NONE',  ( -6.972266317189433020E-16, -68.24999999999998579, -5.000000000000000000 ) ) ;
#33178 = CARTESIAN_POINT ( 'NONE',  ( 2.499999999999998668, -60.20833333060214443, -4.330127018922193649 ) ) ;
#33179 = CARTESIAN_POINT ( 'NONE',  ( 4.458734124999998549, -9.729166665301068662, -2.574251347313721627 ) ) ;
#33180 = CARTESIAN_POINT ( 'NONE',  ( 1.975475456537005874E-15, -84.62499999726880162, 5.000000000000000000 ) ) ;
#33181 = CARTESIAN_POINT ( 'NONE',  ( -53.33387254593719717, -144.8125000000000000, 5.149110718188530278 ) ) ;
#33182 = DIRECTION ( 'NONE',  ( -0.000000000000000000, 1.000000000000000000, -0.000000000000000000 ) ) ;
#33183 = CARTESIAN_POINT ( 'NONE',  ( -2.500000000000000444, -35.04166666393547303, -4.330127018922193649 ) ) ;
#33184 = CARTESIAN_POINT ( 'NONE',  ( 5.000000000000000888, -49.45833333060213732, 2.886751345948126879 ) ) ;
#33185 = CARTESIAN_POINT ( 'NONE',  ( -4.458734124999999437, 19.68750000136559208, 0.000000000000000000 ) ) ;
#33186 = CARTESIAN_POINT ( 'NONE',  ( -6.972266317189433020E-16, -44.25000000000000000, -5.000000000000000000 ) ) ;
#33187 = CARTESIAN_POINT ( 'NONE',  ( -3.152548672688508926E-16, 22.43750000136559564, -5.148502694627439702 ) ) ;
#33188 = CARTESIAN_POINT ( 'NONE',  ( 9.457646018065525792E-16, -54.06249999863440081, 5.148502694627439702 ) ) ;
#33189 = CARTESIAN_POINT ( 'NONE',  ( -4.458734124999999437, -5.562499998634402587, 0.000000000000000000 ) ) ;
#33190 = CARTESIAN_POINT ( 'NONE',  ( -6.972266317189433020E-16, -83.24999999999998579, -5.000000000000000000 ) ) ;
#33191 = CARTESIAN_POINT ( 'NONE',  ( -3.535250795749689387E-16, 7.749999999999999112, -5.773502691896257311 ) ) ;
#33192 = CARTESIAN_POINT ( 'NONE',  ( -3.535533905932737309, -142.7500000027311842, -3.535533905932738197 ) ) ;
#33193 = CARTESIAN_POINT ( 'NONE',  ( 5.000000000000000888, -75.45833333060214443, 2.886751345948126879 ) ) ;
#33194 = CARTESIAN_POINT ( 'NONE',  ( -3.152548672688508926E-16, -49.56249999863440792, -5.148502694627439702 ) ) ;
#33195 = CARTESIAN_POINT ( 'NONE',  ( -2.499999999999996447, -86.70833333060214443, 4.330127018922195425 ) ) ;
#33196 = CARTESIAN_POINT ( 'NONE',  ( -50.70258187064364108, -134.3750000013656347, 2.196230717870141014 ) ) ;
#33197 = CARTESIAN_POINT ( 'NONE',  ( 5.000000000000000888, -14.45833333060214976, 2.886751345948126879 ) ) ;
#33198 = CARTESIAN_POINT ( 'NONE',  ( 0.000000000000000000, -120.0000000000000000, 5.000000000000000000 ) ) ;
#33199 = CARTESIAN_POINT ( 'NONE',  ( 2.229367062499998831, -89.89583333196773651, -3.861377020970580887 ) ) ;
#33200 = CARTESIAN_POINT ( 'NONE',  ( 1.846868145590735200, -158.5000000013656347, -4.458734124999999437 ) ) ;
#33201 = CARTESIAN_POINT ( 'NONE',  ( 1.060575238724906964E-15, -37.75000000000000000, 5.773502691896257311 ) ) ;
#33202 = DIRECTION ( 'NONE',  ( 0.000000000000000000, 0.000000000000000000, 1.000000000000000000 ) ) ;
#33203 = ORIENTED_EDGE ( 'NONE', *, *, #53788, .F. ) ;
#33204 = CARTESIAN_POINT ( 'NONE',  ( -4.458734124999999437, 18.35416666803225993, -2.574251347313719407 ) ) ;
#33205 = ORIENTED_EDGE ( 'NONE', *, *, #29558, .T. ) ;
#33206 = CARTESIAN_POINT ( 'NONE',  ( 4.458734124999999437, -95.81249999863440792, -5.460374474430324690E-16 ) ) ;
#33207 = CARTESIAN_POINT ( 'NONE',  ( 2.229367062499998831, 6.104166668032262599, -3.861377020970580887 ) ) ;
#33208 = CARTESIAN_POINT ( 'NONE',  ( 5.000000000000000888, 10.54166666939785202, 2.886751345948126879 ) ) ;
#33209 = CARTESIAN_POINT ( 'NONE',  ( 5.000000000000000888, 5.416666666666666963, 2.886751345948126879 ) ) ;
#33210 =( BOUNDED_CURVE ( )  B_SPLINE_CURVE ( 2, ( #14960, #25252, #49376, #10451, #5321, #15610, #502, #20109, #35228 ),
 .UNSPECIFIED., .F., .F. ) 
 B_SPLINE_CURVE_WITH_KNOTS ( ( 3, 2, 2, 2, 3 ),
 ( 0.2062499999999999889, 0.2069444444444444309, 0.2083333333333333426, 0.2097222222222222265, 0.2104166666666666685 ),
 .UNSPECIFIED. ) 
 CURVE ( )  GEOMETRIC_REPRESENTATION_ITEM ( )  RATIONAL_B_SPLINE_CURVE ( ( 0.9330127018922194093, 0.9330127018922194093, 1.000000000000000000, 0.8660254037844387076, 1.000000000000000000, 0.8660254037844387076, 1.000000000000000000, 0.9330127018922194093, 0.9330127018922194093 ) ) 
 REPRESENTATION_ITEM ( '' )  );
#33211 = CARTESIAN_POINT ( 'NONE',  ( 2.229367062499998831, -60.64583333196774362, -3.861377020970580887 ) ) ;
#33212 = CARTESIAN_POINT ( 'NONE',  ( 2.500000000000002220, -61.54166666393547303, 4.330127018922192761 ) ) ;
#33213 = CARTESIAN_POINT ( 'NONE',  ( -3.535250795749689387E-16, 2.875000002731185944, -5.773502691896257311 ) ) ;
#33214 = CARTESIAN_POINT ( 'NONE',  ( -3.152548672688508926E-16, -28.56249999863440436, -5.148502694627439702 ) ) ;
#33215 = CARTESIAN_POINT ( 'NONE',  ( -5.000000000000000000, -41.99999999999999289, 0.000000000000000000 ) ) ;
#33216 = CYLINDRICAL_SURFACE ( 'NONE', #475, 5.000000000000000000 ) ;
#33217 = FACE_OUTER_BOUND ( 'NONE', #41371, .T. ) ;
#33218 = CARTESIAN_POINT ( 'NONE',  ( 5.000000000000000888, -42.58333333333334281, 2.886751345948126879 ) ) ;
#33220 = CARTESIAN_POINT ( 'NONE',  ( 2.229367062500001939, -17.22916666530106866, 3.861377020970579999 ) ) ;
#33219 = CARTESIAN_POINT ( 'NONE',  ( 5.000000000000000888, -26.45833333060214798, 2.886751345948126879 ) ) ;
#33221 = CARTESIAN_POINT ( 'NONE',  ( -4.458734124999999437, -66.31249999863440792, 0.000000000000000000 ) ) ;
#33222 = CARTESIAN_POINT ( 'NONE',  ( 3.152801135295366208, -147.8125000013655779, 3.152801135295367985 ) ) ;
#33223 = CARTESIAN_POINT ( 'NONE',  ( -4.458734124999999437, -76.31249999863440792, 0.000000000000000000 ) ) ;
#33224 = CARTESIAN_POINT ( 'NONE',  ( -56.48576386720575471, -145.0000000013656063, -4.591703134518078322 ) ) ;
#33225 = CARTESIAN_POINT ( 'NONE',  ( 9.457646018065525792E-16, -25.31249999863440792, 5.148502694627439702 ) ) ;
#33226 =( BOUNDED_CURVE ( )  B_SPLINE_CURVE ( 2, ( #21957, #36752, #56382, #7484, #31603, #46713, #2985, #31921, #60258 ),
 .UNSPECIFIED., .F., .F. ) 
 B_SPLINE_CURVE_WITH_KNOTS ( ( 3, 2, 2, 2, 3 ),
 ( 0.2437499999999999944, 0.2444444444444444364, 0.2458333333333333204, 0.2472222222222222321, 0.2479166666666666741 ),
 .UNSPECIFIED. ) 
 CURVE ( )  GEOMETRIC_REPRESENTATION_ITEM ( )  RATIONAL_B_SPLINE_CURVE ( ( 0.9330127018922194093, 0.9330127018922194093, 1.000000000000000000, 0.8660254037844387076, 1.000000000000000000, 0.8660254037844387076, 1.000000000000000000, 0.9330127018922194093, 0.9330127018922194093 ) ) 
 REPRESENTATION_ITEM ( '' )  );
#33227 = CARTESIAN_POINT ( 'NONE',  ( 2.499999999999998668, -66.20833333060213022, -4.330127018922193649 ) ) ;
#33228 = ORIENTED_EDGE ( 'NONE', *, *, #51213, .T. ) ;
#33229 = CARTESIAN_POINT ( 'NONE',  ( 1.975475456537005874E-15, -21.75000000000000000, 5.000000000000000000 ) ) ;
#33230 = VERTEX_POINT ( 'NONE', #14230 ) ;
#33231 = CARTESIAN_POINT ( 'NONE',  ( 2.229367062499998831, -69.89583333196773651, -3.861377020970580887 ) ) ;
#33232 = CARTESIAN_POINT ( 'NONE',  ( -56.66612745406278151, -150.3125000000000284, -5.149110718188523173 ) ) ;
#33233 = DIRECTION ( 'NONE',  ( -1.000000000000000000, 0.000000000000000000, 0.000000000000000000 ) ) ;
#33234 = EDGE_LOOP ( 'NONE', ( #54252, #23438, #48262, #31711 ) ) ;
#33235 = FACE_OUTER_BOUND ( 'NONE', #20315, .T. ) ;
#33236 = CARTESIAN_POINT ( 'NONE',  ( 9.457646018065525792E-16, -51.31249999863440792, 5.148502694627439702 ) ) ;
#33237 = CARTESIAN_POINT ( 'NONE',  ( -2.229367062500000163, 3.270833334698929118, -3.861377020970580443 ) ) ;
#33238 = ORIENTED_EDGE ( 'NONE', *, *, #45541, .T. ) ;
#33239 = CARTESIAN_POINT ( 'NONE',  ( 1.339745962155612702, -45.29465819873851729, -5.000000000000000000 ) ) ;
#33240 = CARTESIAN_POINT ( 'NONE',  ( -3.152548672688508926E-16, 2.437500001365594304, -5.148502694627439702 ) ) ;
#33241 = CARTESIAN_POINT ( 'NONE',  ( -3.152548672688508926E-16, 18.43750000136559564, -5.148502694627439702 ) ) ;
#33242 = CARTESIAN_POINT ( 'NONE',  ( -50.40829686548195099, -145.0000000013656063, -1.485763867205728284 ) ) ;
#33243 = CARTESIAN_POINT ( 'NONE',  ( 5.000000000000000000, 20.70833333606451987, -2.886751345948130876 ) ) ;
#33244 = CARTESIAN_POINT ( 'NONE',  ( -8.190561711645485556E-16, -164.6875000013655779, 4.458734124999999437 ) ) ;
#33245 = ORIENTED_EDGE ( 'NONE', *, *, #42487, .T. ) ;
#33246 = CARTESIAN_POINT ( 'NONE',  ( 4.458734125000000326, -77.89583333196773651, 2.574251347313718519 ) ) ;
#33247 = CARTESIAN_POINT ( 'NONE',  ( -2.499999999999996447, -39.83333333333332860, 4.330127018922195425 ) ) ;
#33248 = CARTESIAN_POINT ( 'NONE',  ( 9.457646018065525792E-16, 8.937500001365597413, 5.148502694627439702 ) ) ;
#33249 = VECTOR ( 'NONE', #38990, 1000.000000000000000 ) ;
#33250 = CARTESIAN_POINT ( 'NONE',  ( 0.000000000000000000, -170.0000000000000000, 0.000000000000000000 ) ) ;
#33251 = CARTESIAN_POINT ( 'NONE',  ( 4.458734125000001214, -58.14583333196773651, 2.574251347313718519 ) ) ;
#33252 = CARTESIAN_POINT ( 'NONE',  ( -4.999999999999999112, -17.79166666393547658, 2.886751345948131764 ) ) ;
#33253 = CARTESIAN_POINT ( 'NONE',  ( 2.500000000000002220, -96.54166666393545881, 4.330127018922192761 ) ) ;
#33254 = CARTESIAN_POINT ( 'NONE',  ( 1.339745962155615144, -42.58034179853029144, 4.999999999999999112 ) ) ;
#33255 = CARTESIAN_POINT ( 'NONE',  ( 0.000000000000000000, -170.0000000000000000, 0.000000000000000000 ) ) ;
#33256 = CARTESIAN_POINT ( 'NONE',  ( -51.75738570946856498, -139.7500000000000000, 3.805975901505576964 ) ) ;
#33257 = DIRECTION ( 'NONE',  ( -0.000000000000000000, -0.000000000000000000, 1.000000000000000000 ) ) ;
#33258 = CARTESIAN_POINT ( 'NONE',  ( 9.457646018065525792E-16, -40.06249999863439371, 5.148502694627439702 ) ) ;
#33259 = PRODUCT_DEFINITION_SHAPE ( 'NONE', 'NONE',  #63679 ) ;
#33260 = CARTESIAN_POINT ( 'NONE',  ( -4.458734124999999437, -26.64583333196774007, -2.574251347313719407 ) ) ;
#33261 = LINE ( 'NONE', #32947, #1069 ) ;
#33262 = CARTESIAN_POINT ( 'NONE',  ( -5.000000000000000000, 27.91666666666666430, -2.886751345948128211 ) ) ;
#33263 = CARTESIAN_POINT ( 'NONE',  ( -2.071067811865475061, -151.8125000027311842, -5.000000000000000888 ) ) ;
#33264 = ORIENTED_EDGE ( 'NONE', *, *, #18866, .T. ) ;
#33265 = CARTESIAN_POINT ( 'NONE',  ( 9.457646018065525792E-16, -108.3124999986343937, 5.148502694627439702 ) ) ;
#33266 = CARTESIAN_POINT ( 'NONE',  ( 4.458734124999998549, -29.72916666530107221, -2.574251347313721627 ) ) ;
#33267 = CARTESIAN_POINT ( 'NONE',  ( -5.000000000000000000, -67.95833333060214443, -2.886751345948128211 ) ) ;
#33268 = CARTESIAN_POINT ( 'NONE',  ( -54.64476657466781973, -146.0625000013656063, -4.444560631937228834 ) ) ;
#33269 = CARTESIAN_POINT ( 'NONE',  ( 3.535533905932736864, -141.1250000000000000, 3.535533905932738641 ) ) ;
#33270 = CARTESIAN_POINT ( 'NONE',  ( -4.458734124999997661, -27.22916666530107221, 2.574251347313722516 ) ) ;
#33271 = CARTESIAN_POINT ( 'NONE',  ( 4.458734124999999437, -76.06249999863440792, -5.460374474430324690E-16 ) ) ;
#33272 = CARTESIAN_POINT ( 'NONE',  ( -6.972266317189433020E-16, -55.24999999999999289, -5.000000000000000000 ) ) ;
#33273 = CARTESIAN_POINT ( 'NONE',  ( -2.229367062499996610, -29.14583333196774007, 3.861377020970582219 ) ) ;
#33274 = CARTESIAN_POINT ( 'NONE',  ( -58.80597590150559739, -148.0000000000000284, 3.242614290531460330 ) ) ;
#33275 = DIRECTION ( 'NONE',  ( 0.000000000000000000, 0.000000000000000000, 1.000000000000000000 ) ) ;
#33276 = CARTESIAN_POINT ( 'NONE',  ( -2.499999999999996447, -23.83333333333333215, 4.330127018922195425 ) ) ;
#33277 = CARTESIAN_POINT ( 'NONE',  ( 2.730187237215162345E-16, -147.1875000013656063, -4.458734124999999437 ) ) ;
#33278 = VERTEX_POINT ( 'NONE', #24205 ) ;
#33279 = CARTESIAN_POINT ( 'NONE',  ( -2.229367062500000163, -54.72916666530107221, -3.861377020970580443 ) ) ;
#33280 =( BOUNDED_CURVE ( )  B_SPLINE_CURVE ( 2, ( #33412, #13164, #63017, #8652, #32787, #18924, #32464, #3214, #23456 ),
 .UNSPECIFIED., .F., .F. ) 
 B_SPLINE_CURVE_WITH_KNOTS ( ( 3, 2, 2, 2, 3 ),
 ( 0.1553571428571428603, 0.1559523809523809534, 0.1571428571428571397, 0.1583333333333333259, 0.1589285714285714191 ),
 .UNSPECIFIED. ) 
 CURVE ( )  GEOMETRIC_REPRESENTATION_ITEM ( )  RATIONAL_B_SPLINE_CURVE ( ( 0.9330127018922194093, 0.9330127018922194093, 1.000000000000000000, 0.8660254037844387076, 1.000000000000000000, 0.8660254037844387076, 1.000000000000000000, 0.9330127018922194093, 0.9330127018922194093 ) ) 
 REPRESENTATION_ITEM ( '' )  );
#33281 = CARTESIAN_POINT ( 'NONE',  ( -5.000000000000000000, 26.12500000273118417, 0.000000000000000000 ) ) ;
#33282 = CARTESIAN_POINT ( 'NONE',  ( -5.000000000000000000, -1.000000000000000888, 0.000000000000000000 ) ) ;
#33283 = CARTESIAN_POINT ( 'NONE',  ( 5.000000000000000000, 19.50000000000000000, -6.123233995736766282E-16 ) ) ;
#33284 = CARTESIAN_POINT ( 'NONE',  ( -6.972266317189433020E-16, -89.24999999999998579, -5.000000000000000000 ) ) ;
#33285 = CARTESIAN_POINT ( 'NONE',  ( 4.458734124999999437, -1.812499998634406584, -5.460374474430324690E-16 ) ) ;
#33286 = CARTESIAN_POINT ( 'NONE',  ( -2.071067811865644259, -154.6875000000000000, -4.999999999999831246 ) ) ;
#33287 = DIRECTION ( 'NONE',  ( -0.000000000000000000, 1.000000000000000000, -0.000000000000000000 ) ) ;
#33288 = CARTESIAN_POINT ( 'NONE',  ( -3.152548672688508926E-16, 8.187500001365595637, -5.148502694627439702 ) ) ;
#33289 = ORIENTED_EDGE ( 'NONE', *, *, #31884, .T. ) ;
#33290 = CARTESIAN_POINT ( 'NONE',  ( 0.000000000000000000, 30.00000000000000000, 0.000000000000000000 ) ) ;
#33291 = CARTESIAN_POINT ( 'NONE',  ( 9.457646018065525792E-16, -49.06249999863440792, 5.148502694627439702 ) ) ;
#33292 = CARTESIAN_POINT ( 'NONE',  ( -4.458734125000000326, -160.2500000013656063, -1.846868145590735644 ) ) ;
#33293 = VECTOR ( 'NONE', #6752, 1000.000000000000000 ) ;
#33294 = CARTESIAN_POINT ( 'NONE',  ( 2.499999999999998668, -52.20833333060213732, -4.330127018922193649 ) ) ;
#33295 = ORIENTED_EDGE ( 'NONE', *, *, #37785, .F. ) ;
#33296 = CARTESIAN_POINT ( 'NONE',  ( -2.229367062499996610, -23.14583333196773651, 3.861377020970582219 ) ) ;
#33297 = VERTEX_POINT ( 'NONE', #10040 ) ;
#33299 = FACE_OUTER_BOUND ( 'NONE', #58063, .T. ) ;
#33298 = DIRECTION ( 'NONE',  ( -0.000000000000000000, 1.000000000000000000, -0.000000000000000000 ) ) ;
#33300 = CARTESIAN_POINT ( 'NONE',  ( -3.152801135295367096, -160.0625000013656063, -3.152801135295367541 ) ) ;
#33301 = ORIENTED_EDGE ( 'NONE', *, *, #35011, .T. ) ;
#33302 = CARTESIAN_POINT ( 'NONE',  ( -6.972266317189433020E-16, -39.12499999726880162, -5.000000000000000000 ) ) ;
#33303 = CARTESIAN_POINT ( 'NONE',  ( -59.81910112700025905, -135.1875000000000284, -2.462841084822630311 ) ) ;
#33304 = CARTESIAN_POINT ( 'NONE',  ( -2.229367062499996610, -39.39583333196773651, 3.861377020970582219 ) ) ;
#33305 = ORIENTED_EDGE ( 'NONE', *, *, #44784, .T. ) ;
#33306 = CARTESIAN_POINT ( 'NONE',  ( -3.152548672688508926E-16, -81.56249999863440792, -5.148502694627439702 ) ) ;
#33307 = CARTESIAN_POINT ( 'NONE',  ( -2.229367062499996610, 17.85416666803225993, 3.861377020970582219 ) ) ;
#33308 = DIRECTION ( 'NONE',  ( 0.000000000000000000, 0.000000000000000000, 1.000000000000000000 ) ) ;
#33309 = ORIENTED_EDGE ( 'NONE', *, *, #45607, .F. ) ;
#33310 = CARTESIAN_POINT ( 'NONE',  ( -51.60603307380591787, -140.1875000013656063, -2.891590998281053704 ) ) ;
#33311 = CARTESIAN_POINT ( 'NONE',  ( 4.458734124999999437, -84.06249999863439371, -5.460374474430324690E-16 ) ) ;
#33312 = CARTESIAN_POINT ( 'NONE',  ( -50.01589407740564042, -124.7500000027311984, 0.3983568153799778022 ) ) ;
#33313 = CARTESIAN_POINT ( 'NONE',  ( 2.500000000000002220, -88.66666666666665719, 4.330127018922192761 ) ) ;
#33314 = CARTESIAN_POINT ( 'NONE',  ( 2.500000000000002220, -9.666666666666664298, 4.330127018922192761 ) ) ;
#33315 =( BOUNDED_CURVE ( )  B_SPLINE_CURVE ( 2, ( #42930, #43547, #53529, #9457, #28452, #63191, #58360, #52593, #14286 ),
 .UNSPECIFIED., .F., .F. ) 
 B_SPLINE_CURVE_WITH_KNOTS ( ( 3, 2, 2, 2, 3 ),
 ( 0.5479166666666667185, 0.5486111111111111605, 0.5500000000000000444, 0.5513888888888889284, 0.5520833333333333703 ),
 .UNSPECIFIED. ) 
 CURVE ( )  GEOMETRIC_REPRESENTATION_ITEM ( )  RATIONAL_B_SPLINE_CURVE ( ( 0.9330127018922194093, 0.9330127018922194093, 1.000000000000000000, 0.8660254037844387076, 1.000000000000000000, 0.8660254037844387076, 1.000000000000000000, 0.9330127018922194093, 0.9330127018922194093 ) ) 
 REPRESENTATION_ITEM ( '' )  );
#33316 = CARTESIAN_POINT ( 'NONE',  ( 5.000000000000000000, -145.1250000027312126, 0.000000000000000000 ) ) ;
#33317 = CARTESIAN_POINT ( 'NONE',  ( -4.458734124999999437, -58.31249999863440081, 0.000000000000000000 ) ) ;
#33318 = CARTESIAN_POINT ( 'NONE',  ( 5.000000000000000000, 21.58333333333333215, -2.886751345948130876 ) ) ;
#33319 = CARTESIAN_POINT ( 'NONE',  ( 9.457646018065525792E-16, 22.93750000136559919, 5.148502694627439702 ) ) ;
#33320 = ADVANCED_FACE ( 'NONE', ( #53475 ), #43497, .T. ) ;
#33321 = CARTESIAN_POINT ( 'NONE',  ( 1.339745962155615144, -97.70534180126145429, 4.999999999999999112 ) ) ;
#33322 = CYLINDRICAL_SURFACE ( 'NONE', #3128, 5.000000000000000000 ) ;
#33323 = CARTESIAN_POINT ( 'NONE',  ( -4.458734124999999437, -42.56249999863440081, 0.000000000000000000 ) ) ;
#33324 = CARTESIAN_POINT ( 'NONE',  ( -2.499999999999996447, -5.708333330602148870, 4.330127018922195425 ) ) ;
#33325 = CARTESIAN_POINT ( 'NONE',  ( -4.999999999999998224, -92.91666666666665719, 2.886751345948131764 ) ) ;
#33326 = CARTESIAN_POINT ( 'NONE',  ( -5.000000000000000000, -61.00000000000000000, 0.000000000000000000 ) ) ;
#33327 = CARTESIAN_POINT ( 'NONE',  ( 9.457646018065525792E-16, -82.31249999863440792, 5.148502694627439702 ) ) ;
#33328 = CARTESIAN_POINT ( 'NONE',  ( -4.458734124999999437, -108.3958333319677365, -2.574251347313719407 ) ) ;
#33329 = CARTESIAN_POINT ( 'NONE',  ( -4.458734124999997661, -10.47916666530106866, 2.574251347313722516 ) ) ;
#33330 = EDGE_LOOP ( 'NONE', ( #17426, #9163, #13482, #48409 ) ) ;
#33331 = CARTESIAN_POINT ( 'NONE',  ( -9.184850993605147944E-16, -155.3750000027311842, 5.000000000000000000 ) ) ;
#33332 = CARTESIAN_POINT ( 'NONE',  ( 9.457646018065525792E-16, -97.06249999863439371, 5.148502694627439702 ) ) ;
#33333 = CARTESIAN_POINT ( 'NONE',  ( -2.071067811865478170, -165.4375000027312126, 5.000000000000000000 ) ) ;
#33334 = CARTESIAN_POINT ( 'NONE',  ( -4.458734124999999437, -94.64583333196773651, -2.574251347313719407 ) ) ;
#33335 = CARTESIAN_POINT ( 'NONE',  ( -5.000000000000000000, -49.87499999726881583, 0.000000000000000000 ) ) ;
#33336 = DIRECTION ( 'NONE',  ( -0.000000000000000000, 1.000000000000000000, -0.000000000000000000 ) ) ;
#33337 = VECTOR ( 'NONE', #16763, 1000.000000000000000 ) ;
#33338 = CARTESIAN_POINT ( 'NONE',  ( -59.44456063193725015, -131.5625000013656063, -0.3552334253322034230 ) ) ;
#33339 = EDGE_CURVE ( 'NONE', #37665, #1132, #58009, .T. ) ;
#33340 = CARTESIAN_POINT ( 'NONE',  ( -59.59170313451810586, -145.5000000013656063, 1.485763867205729394 ) ) ;
#33341 = CARTESIAN_POINT ( 'NONE',  ( -3.152548672688508926E-16, -12.56249999863440259, -5.148502694627439702 ) ) ;
#33342 = CARTESIAN_POINT ( 'NONE',  ( -4.458734124999999437, 11.43750000136559564, 0.000000000000000000 ) ) ;
#33343 = ADVANCED_FACE ( 'NONE', ( #44128 ), #408, .F. ) ;
#33344 = CARTESIAN_POINT ( 'NONE',  ( 2.229367062499998831, -56.89583333196773651, -3.861377020970580887 ) ) ;
#33345 = FACE_OUTER_BOUND ( 'NONE', #16295, .T. ) ;
#33346 = CARTESIAN_POINT ( 'NONE',  ( -2.500000000000000444, -37.16666666666666430, -4.330127018922193649 ) ) ;
#33347 = CARTESIAN_POINT ( 'NONE',  ( 4.458734124999998549, -16.72916666530107577, -2.574251347313721627 ) ) ;
#33348 = LINE ( 'NONE', #38784, #25755 ) ;
#33349 = ORIENTED_EDGE ( 'NONE', *, *, #41385, .F. ) ;
#33350 = CARTESIAN_POINT ( 'NONE',  ( 4.458734124999998549, -42.97916666530107932, -2.574251347313721627 ) ) ;
#33351 = CARTESIAN_POINT ( 'NONE',  ( -58.39396692619412477, -125.6875000013656063, 2.891590998281057701 ) ) ;
#33352 = CARTESIAN_POINT ( 'NONE',  ( 1.339745962155612702, -76.29465819873853150, -5.000000000000000000 ) ) ;
#33353 = CARTESIAN_POINT ( 'NONE',  ( -4.458734124999999437, -83.39583333196772230, -2.574251347313719407 ) ) ;
#33354 = CARTESIAN_POINT ( 'NONE',  ( -4.458734124999999437, 25.43750000136559208, 0.000000000000000000 ) ) ;
#33355 = EDGE_CURVE ( 'NONE', #24536, #20419, #31715, .T. ) ;
#33356 = CARTESIAN_POINT ( 'NONE',  ( -2.229367062499996610, 13.85416666803226171, 3.861377020970582219 ) ) ;
#33357 = CARTESIAN_POINT ( 'NONE',  ( -58.24261429053147765, -155.0000000000000284, -3.805975901505573411 ) ) ;
#33358 = CYLINDRICAL_SURFACE ( 'NONE', #21445, 5.000000000000000000 ) ;
#33359 = CARTESIAN_POINT ( 'NONE',  ( -4.458734124999997661, -90.47916666530106511, 2.574251347313722516 ) ) ;
#33360 = CARTESIAN_POINT ( 'NONE',  ( -2.499999999999996447, -71.83333333333332860, 4.330127018922195425 ) ) ;
#33361 = CARTESIAN_POINT ( 'NONE',  ( 1.060575238724906964E-15, 16.37500000273118417, 5.773502691896257311 ) ) ;
#33362 = ORIENTED_EDGE ( 'NONE', *, *, #50875, .T. ) ;
#33363 = CARTESIAN_POINT ( 'NONE',  ( -1.339745962155610925, -6.669658196007334894, 5.000000000000000000 ) ) ;
#33364 = CARTESIAN_POINT ( 'NONE',  ( -6.972266317189433020E-16, -80.12499999726881583, -5.000000000000000000 ) ) ;
#33366 = CARTESIAN_POINT ( 'NONE',  ( -5.000000000000000000, -29.08333333333332860, -2.886751345948128211 ) ) ;
#33365 = DIRECTION ( 'NONE',  ( 0.000000000000000000, 0.000000000000000000, 1.000000000000000000 ) ) ;
#33367 = CARTESIAN_POINT ( 'NONE',  ( 4.458734124999998549, -31.72916666530107577, -2.574251347313721627 ) ) ;
#33368 = CARTESIAN_POINT ( 'NONE',  ( -4.999999999999999112, -35.79166666393548013, 2.886751345948131764 ) ) ;
#33369 = EDGE_CURVE ( 'NONE', #2645, #10962, #38646, .T. ) ;
#33371 = VERTEX_POINT ( 'NONE', #9405 ) ;
#33370 = CARTESIAN_POINT ( 'NONE',  ( -4.458734124999999437, -62.31249999863440792, 0.000000000000000000 ) ) ;
#33372 = CARTESIAN_POINT ( 'NONE',  ( -59.59170313451811296, -151.7500000013655779, 1.485763867205729394 ) ) ;
#33374 = ORIENTED_EDGE ( 'NONE', *, *, #13465, .F. ) ;
#33373 = CARTESIAN_POINT ( 'NONE',  ( 2.229367062499998831, -13.89583333196774184, -3.861377020970580887 ) ) ;
#33375 = CARTESIAN_POINT ( 'NONE',  ( -5.000000000000000000, -79.00000000000000000, 0.000000000000000000 ) ) ;
#33376 = CARTESIAN_POINT ( 'NONE',  ( 1.339745962155614034, 28.41965820146970501, 5.000000000000000000 ) ) ;
#33377 = CARTESIAN_POINT ( 'NONE',  ( 4.458734125000001214, -58.14583333196773651, 2.574251347313718519 ) ) ;
#33378 = CARTESIAN_POINT ( 'NONE',  ( -3.535250795749689387E-16, -80.12499999726880162, -5.773502691896257311 ) ) ;
#33380 = ORIENTED_EDGE ( 'NONE', *, *, #16531, .T. ) ;
#33379 = DIRECTION ( 'NONE',  ( 0.000000000000000000, 0.000000000000000000, 1.000000000000000000 ) ) ;
#33381 = CARTESIAN_POINT ( 'NONE',  ( -49.85088928181150436, -147.5625000000000000, -1.666127454062680702 ) ) ;
#33382 = CARTESIAN_POINT ( 'NONE',  ( 9.457646018065525792E-16, -20.31249999863440081, 5.148502694627439702 ) ) ;
#33384 = ORIENTED_EDGE ( 'NONE', *, *, #44158, .F. ) ;
#33383 = CARTESIAN_POINT ( 'NONE',  ( 4.458734124999999437, -55.06249999863440081, -5.460374474430324690E-16 ) ) ;
#33385 = DIRECTION ( 'NONE',  ( 1.000000000000000000, 0.000000000000000000, 0.000000000000000000 ) ) ;
#33386 = CARTESIAN_POINT ( 'NONE',  ( 4.458734125000000326, -165.6250000013656063, -1.846868145590734978 ) ) ;
#33387 = CARTESIAN_POINT ( 'NONE',  ( 4.458734124999998549, -106.9791666653010509, -2.574251347313721627 ) ) ;
#33388 = CARTESIAN_POINT ( 'NONE',  ( 1.975475456537005874E-15, -50.62499999726881583, 5.000000000000000000 ) ) ;
#33389 = VERTEX_POINT ( 'NONE', #34470 ) ;
#33390 = CARTESIAN_POINT ( 'NONE',  ( -58.39396692619412477, -150.6875000013656063, 2.891590998281057701 ) ) ;
#33391 = CARTESIAN_POINT ( 'NONE',  ( -53.33387254593733928, -137.9375000027311842, 5.149110718188519620 ) ) ;
#33392 = CARTESIAN_POINT ( 'NONE',  ( -2.229367062500000163, -37.47916666530107221, -3.861377020970580443 ) ) ;
#33393 = CARTESIAN_POINT ( 'NONE',  ( -6.972266317189433020E-16, 0.8750000027311866102, -5.000000000000000000 ) ) ;
#33394 = EDGE_CURVE ( 'NONE', #15666, #18516, #14419, .T. ) ;
#33395 = CARTESIAN_POINT ( 'NONE',  ( 2.229367062500001939, -7.979166665301073991, 3.861377020970579999 ) ) ;
#33396 =( BOUNDED_CURVE ( )  B_SPLINE_CURVE ( 2, ( #32851, #24140, #13551, #52479, #28016, #47635, #52785, #29260, #33789 ),
 .UNSPECIFIED., .F., .F. ) 
 B_SPLINE_CURVE_WITH_KNOTS ( ( 3, 2, 2, 2, 3 ),
 ( 0.4625000000000000222, 0.4630952380952381153, 0.4642857142857143016, 0.4654761904761904878, 0.4660714285714285809 ),
 .UNSPECIFIED. ) 
 CURVE ( )  GEOMETRIC_REPRESENTATION_ITEM ( )  RATIONAL_B_SPLINE_CURVE ( ( 0.9330127018922194093, 0.9330127018922194093, 1.000000000000000000, 0.8660254037844387076, 1.000000000000000000, 0.8660254037844387076, 1.000000000000000000, 0.9330127018922194093, 0.9330127018922194093 ) ) 
 REPRESENTATION_ITEM ( '' )  );
#33397 = CARTESIAN_POINT ( 'NONE',  ( -2.229367062499996610, -101.3958333319677365, 3.861377020970582219 ) ) ;
#33398 = CARTESIAN_POINT ( 'NONE',  ( -4.458734125000001214, -146.1250000013655779, 1.846868145590734089 ) ) ;
#33399 = CARTESIAN_POINT ( 'NONE',  ( -3.152548672688508926E-16, -29.81249999863440436, -5.148502694627439702 ) ) ;
#33400 = CARTESIAN_POINT ( 'NONE',  ( -2.500000000000000444, 11.83333333333333037, -4.330127018922193649 ) ) ;
#33401 = CARTESIAN_POINT ( 'NONE',  ( -57.89159099828107458, -131.6875000013656063, -3.393966926194107447 ) ) ;
#33402 = CARTESIAN_POINT ( 'NONE',  ( -4.458734124999998549, -66.47916666530106511, 2.574251347313722516 ) ) ;
#33403 = CARTESIAN_POINT ( 'NONE',  ( -1.339745962155610925, -15.79465819873852261, 5.000000000000000000 ) ) ;
#33404 = DIRECTION ( 'NONE',  ( -0.000000000000000000, 1.000000000000000000, -0.000000000000000000 ) ) ;
#33405 = CARTESIAN_POINT ( 'NONE',  ( -1.846868145590737420, -142.7500000013655779, 4.458734124999997661 ) ) ;
#33406 = CARTESIAN_POINT ( 'NONE',  ( 4.458734124999999437, 5.937500001365593860, -5.460374474430324690E-16 ) ) ;
#33407 = VERTEX_POINT ( 'NONE', #58625 ) ;
#33408 = CARTESIAN_POINT ( 'NONE',  ( -6.972266317189433020E-16, -94.25000000000000000, -5.000000000000000000 ) ) ;
#33409 = CARTESIAN_POINT ( 'NONE',  ( 2.071067811865370256, -159.8125000000000000, -5.000000000000105693 ) ) ;
#33411 = CARTESIAN_POINT ( 'NONE',  ( 4.458734124999998549, -29.72916666530107221, -2.574251347313721627 ) ) ;
#33410 = CARTESIAN_POINT ( 'NONE',  ( 2.500000000000002220, -95.66666666666664298, 4.330127018922192761 ) ) ;
#33412 = CARTESIAN_POINT ( 'NONE',  ( 1.975475456537005874E-15, 7.375000002731186832, 5.000000000000000000 ) ) ;
#33413 = CARTESIAN_POINT ( 'NONE',  ( 9.457646018065525792E-16, -74.31249999863440792, 5.148502694627439702 ) ) ;
#33414 = CARTESIAN_POINT ( 'NONE',  ( -4.458734124999999437, 25.43750000136559208, 0.000000000000000000 ) ) ;
#33415 = CARTESIAN_POINT ( 'NONE',  ( -4.999999999999998224, 23.20833333606451632, 2.886751345948131764 ) ) ;
#33416 = CARTESIAN_POINT ( 'NONE',  ( -57.89159099828107458, -140.6875000013656063, -3.393966926194107447 ) ) ;
#33417 = CARTESIAN_POINT ( 'NONE',  ( 4.458734125000000326, 4.104166668032260823, 2.574251347313718519 ) ) ;
#33418 = CARTESIAN_POINT ( 'NONE',  ( -2.229367062499996610, 25.60416666803225993, 3.861377020970582219 ) ) ;
#33419 = EDGE_CURVE ( 'NONE', #19133, #49359, #62901, .T. ) ;
#33420 = CARTESIAN_POINT ( 'NONE',  ( -2.229367062500000163, -40.72916666530107221, -3.861377020970580443 ) ) ;
#33421 = CARTESIAN_POINT ( 'NONE',  ( 5.000000000000000000, -80.41666666666665719, -2.886751345948130876 ) ) ;
#33422 = CARTESIAN_POINT ( 'NONE',  ( 2.229367062500001939, 3.020833334698928674, 3.861377020970579999 ) ) ;
#33423 = CARTESIAN_POINT ( 'NONE',  ( -4.458734124999999437, -25.64583333196773651, -2.574251347313719407 ) ) ;
#33424 = CARTESIAN_POINT ( 'NONE',  ( -8.190561711645485556E-16, -156.6875000013655779, 4.458734124999999437 ) ) ;
#33425 = CARTESIAN_POINT ( 'NONE',  ( 4.458734125000001214, -68.89583333196773651, 2.574251347313718519 ) ) ;
#33426 = CARTESIAN_POINT ( 'NONE',  ( -2.500000000000000444, -102.0416666639354588, -4.330127018922193649 ) ) ;
#33427 = VECTOR ( 'NONE', #47341, 1000.000000000000000 ) ;
#33428 = CARTESIAN_POINT ( 'NONE',  ( 2.229367062500001939, 29.02083333469892779, 3.861377020970579999 ) ) ;
#33429 = DIRECTION ( 'NONE',  ( -0.000000000000000000, 1.000000000000000000, -0.000000000000000000 ) ) ;
#33430 = CARTESIAN_POINT ( 'NONE',  ( 4.458734124999998549, -104.9791666653010651, -2.574251347313721627 ) ) ;
#33431 = CARTESIAN_POINT ( 'NONE',  ( 2.229367062499998831, -72.89583333196773651, -3.861377020970580887 ) ) ;
#33432 = CARTESIAN_POINT ( 'NONE',  ( 2.499999999999998668, -54.33333333333332860, -4.330127018922193649 ) ) ;
#33433 = CARTESIAN_POINT ( 'NONE',  ( -5.000000000000000000, -66.08333333333332860, -2.886751345948128211 ) ) ;
#33434 = CARTESIAN_POINT ( 'NONE',  ( 2.071067811865327624, -155.9375000027312126, -5.000000000000148326 ) ) ;
#33435 = ORIENTED_EDGE ( 'NONE', *, *, #30374, .T. ) ;
#33436 = CYLINDRICAL_SURFACE ( 'NONE', #29355, 5.000000000000000000 ) ;
#33437 = CARTESIAN_POINT ( 'NONE',  ( -2.500000000000000444, 11.95833333606451809, -4.330127018922193649 ) ) ;
#33438 = CARTESIAN_POINT ( 'NONE',  ( 5.000000000000000000, -10.41666666666666430, -2.886751345948129988 ) ) ;
#33439 = CARTESIAN_POINT ( 'NONE',  ( 9.457646018065525792E-16, -17.06249999863440792, 5.148502694627439702 ) ) ;
#33440 = ADVANCED_FACE ( 'NONE', ( #10035 ), #59251, .T. ) ;
#33441 = CARTESIAN_POINT ( 'NONE',  ( -4.458734124999999437, -77.39583333196772230, -2.574251347313719407 ) ) ;
#33442 = CARTESIAN_POINT ( 'NONE',  ( 4.458734124999999437, -168.7500000013656063, 1.846868145590737864 ) ) ;
#33443 = CARTESIAN_POINT ( 'NONE',  ( -2.500000000000000444, -20.04166666393548013, -4.330127018922193649 ) ) ;
#33445 = ORIENTED_EDGE ( 'NONE', *, *, #29530, .T. ) ;
#33444 = CARTESIAN_POINT ( 'NONE',  ( -4.458734124999999437, -43.31249999863440081, 0.000000000000000000 ) ) ;
#33446 = CARTESIAN_POINT ( 'NONE',  ( 2.499999999999998668, -15.20833333060214443, -4.330127018922193649 ) ) ;
#33448 = ORIENTED_EDGE ( 'NONE', *, *, #57812, .F. ) ;
#33447 = CARTESIAN_POINT ( 'NONE',  ( 9.457646018065525792E-16, 5.687500001365592972, 5.148502694627439702 ) ) ;
#33449 = CARTESIAN_POINT ( 'NONE',  ( 1.339745962155615144, -34.58034179853028434, 4.999999999999999112 ) ) ;
#33450 = CARTESIAN_POINT ( 'NONE',  ( -3.535250795749689387E-16, -62.25000000000000000, -5.773502691896257311 ) ) ;
#33451 = CARTESIAN_POINT ( 'NONE',  ( 2.730187237215162345E-16, -156.4375000013655779, -4.458734124999999437 ) ) ;
#33452 = CARTESIAN_POINT ( 'NONE',  ( -3.152548672688508926E-16, -41.81249999863440081, -5.148502694627439702 ) ) ;
#33453 = CARTESIAN_POINT ( 'NONE',  ( 1.975475456537005874E-15, -78.74999999999998579, 5.000000000000000000 ) ) ;
#33454 = CARTESIAN_POINT ( 'NONE',  ( -3.535533905932738641, -165.3750000000000284, 3.535533905932737309 ) ) ;
#33455 = CARTESIAN_POINT ( 'NONE',  ( 2.499999999999998668, 5.791666669397853795, -4.330127018922193649 ) ) ;
#33456 = CARTESIAN_POINT ( 'NONE',  ( -59.44456063193725015, -132.8125000013656063, -0.3552334253322034230 ) ) ;
#33457 = CARTESIAN_POINT ( 'NONE',  ( 2.229367062500001939, -6.229166665301072214, 3.861377020970579999 ) ) ;
#33458 = CARTESIAN_POINT ( 'NONE',  ( 2.229367062499998831, -39.89583333196773651, -3.861377020970580887 ) ) ;
#33459 = CARTESIAN_POINT ( 'NONE',  ( -2.499999999999996447, -24.70833333060214443, 4.330127018922195425 ) ) ;
#33460 = CARTESIAN_POINT ( 'NONE',  ( -8.190561711645485556E-16, -147.6875000013656063, 4.458734124999999437 ) ) ;
#33461 = CARTESIAN_POINT ( 'NONE',  ( 4.458734124999998549, -85.97916666530107932, -2.574251347313721627 ) ) ;
#33462 = ORIENTED_EDGE ( 'NONE', *, *, #29997, .F. ) ;
#33463 = CARTESIAN_POINT ( 'NONE',  ( 2.500000000000002220, -99.66666666666665719, 4.330127018922192761 ) ) ;
#33464 = CARTESIAN_POINT ( 'NONE',  ( -49.85088928181150436, -150.6875000027312126, -1.666127454062680702 ) ) ;
#33465 =( BOUNDED_CURVE ( )  B_SPLINE_CURVE ( 2, ( #6772, #36997, #1966, #26384, #3223, #51786, #7728, #46001, #21567 ),
 .UNSPECIFIED., .F., .F. ) 
 B_SPLINE_CURVE_WITH_KNOTS ( ( 3, 2, 2, 2, 3 ),
 ( 0.3729166666666666741, 0.3736111111111111160, 0.3750000000000000000, 0.3763888888888888840, 0.3770833333333333259 ),
 .UNSPECIFIED. ) 
 CURVE ( )  GEOMETRIC_REPRESENTATION_ITEM ( )  RATIONAL_B_SPLINE_CURVE ( ( 0.9330127018922194093, 0.9330127018922194093, 1.000000000000000000, 0.8660254037844387076, 1.000000000000000000, 0.8660254037844387076, 1.000000000000000000, 0.9330127018922194093, 0.9330127018922194093 ) ) 
 REPRESENTATION_ITEM ( '' )  );
#33466 = CARTESIAN_POINT ( 'NONE',  ( -2.500000000000000444, -105.1666666666666572, -4.330127018922193649 ) ) ;
#33467 = CARTESIAN_POINT ( 'NONE',  ( -4.458734124999999437, -74.56249999863440792, 0.000000000000000000 ) ) ;
#33468 = EDGE_LOOP ( 'NONE', ( #41316, #61539, #29393, #29954 ) ) ;
#33469 = EDGE_CURVE ( 'NONE', #8855, #39123, #21389, .T. ) ;
#33470 = EDGE_CURVE ( 'NONE', #63012, #59890, #55066, .T. ) ;
#33471 = CARTESIAN_POINT ( 'NONE',  ( -55.00000000000001421, -155.0000000000000284, -8.082903768654752241 ) ) ;
#33472 = CARTESIAN_POINT ( 'NONE',  ( 2.229367062499998831, -11.89583333196774007, -3.861377020970580887 ) ) ;
#33473 = EDGE_CURVE ( 'NONE', #22889, #32917, #15826, .T. ) ;
#33474 = DIRECTION ( 'NONE',  ( -0.6485228581062915110, 0.000000000000000000, -0.7611951803011149931 ) ) ;
#33475 = CARTESIAN_POINT ( 'NONE',  ( 4.458734124999998549, 3.270833334698929118, -2.574251347313721627 ) ) ;
#33476 = CARTESIAN_POINT ( 'NONE',  ( -9.184850993605147944E-16, -164.2500000000000000, 5.000000000000000000 ) ) ;
#33477 = CARTESIAN_POINT ( 'NONE',  ( 2.730187237215162345E-16, -154.1875000013656063, -4.458734124999999437 ) ) ;
#33478 = EDGE_CURVE ( 'NONE', #17397, #51665, #40266, .T. ) ;
#33479 = CARTESIAN_POINT ( 'NONE',  ( -2.229367062499996610, 21.60416666803226349, 3.861377020970582219 ) ) ;
#33480 = VERTEX_POINT ( 'NONE', #44443 ) ;
#33481 = CARTESIAN_POINT ( 'NONE',  ( -4.458734124999997661, -90.22916666530106511, 2.574251347313722516 ) ) ;
#33482 = CARTESIAN_POINT ( 'NONE',  ( 2.500000000000002220, -47.66666666666666430, 4.330127018922192761 ) ) ;
#33483 = CARTESIAN_POINT ( 'NONE',  ( -2.500000000000000444, -104.0416666639354730, -4.330127018922193649 ) ) ;
#33484 = CARTESIAN_POINT ( 'NONE',  ( -2.229367062500000163, -11.47916666530107044, -3.861377020970580443 ) ) ;
#33485 = EDGE_CURVE ( 'NONE', #49915, #25201, #27576, .T. ) ;
#33487 = EDGE_CURVE ( 'NONE', #26202, #49021, #53779, .T. ) ;
#33486 = DIRECTION ( 'NONE',  ( 1.000000000000000000, 0.000000000000000000, 0.000000000000000000 ) ) ;
#33488 = CARTESIAN_POINT ( 'NONE',  ( -4.999999999999998224, -12.91666666666666607, 2.886751345948131764 ) ) ;
#33489 = CARTESIAN_POINT ( 'NONE',  ( -50.40829686548195099, -153.0000000013656063, -1.485763867205728284 ) ) ;
#33490 = CARTESIAN_POINT ( 'NONE',  ( 2.499999999999998668, -34.20833333060213732, -4.330127018922193649 ) ) ;
#33491 = DIRECTION ( 'NONE',  ( 0.000000000000000000, 0.000000000000000000, 1.000000000000000000 ) ) ;
#33492 = CARTESIAN_POINT ( 'NONE',  ( -4.458734124999999437, 17.60416666803225993, -2.574251347313719407 ) ) ;
#33493 = CARTESIAN_POINT ( 'NONE',  ( 2.500000000000002220, -44.66666666666665719, 4.330127018922192761 ) ) ;
#33494 = EDGE_CURVE ( 'NONE', #17397, #32122, #30286, .T. ) ;
#33495 = CARTESIAN_POINT ( 'NONE',  ( 4.458734124999998549, 18.27083333469893134, -2.574251347313721627 ) ) ;
#33496 = EDGE_CURVE ( 'NONE', #39254, #21932, #45090, .T. ) ;
#33497 = CARTESIAN_POINT ( 'NONE',  ( -2.229367062499996610, -57.14583333196773651, 3.861377020970582219 ) ) ;
#33498 = CARTESIAN_POINT ( 'NONE',  ( -2.229367062499996610, -8.395833331967736513, 3.861377020970582219 ) ) ;
#33499 =( BOUNDED_CURVE ( )  B_SPLINE_CURVE ( 2, ( #57625, #28333, #58236, #13853, #37363, #8719, #22899, #18049, #13553 ),
 .UNSPECIFIED., .F., .F. ) 
 B_SPLINE_CURVE_WITH_KNOTS ( ( 3, 2, 2, 2, 3 ),
 ( 0.9145833333333333037, 0.9152777777777777457, 0.9166666666666666297, 0.9180555555555555136, 0.9187499999999999556 ),
 .UNSPECIFIED. ) 
 CURVE ( )  GEOMETRIC_REPRESENTATION_ITEM ( )  RATIONAL_B_SPLINE_CURVE ( ( 0.9330127018922194093, 0.9330127018922194093, 1.000000000000000000, 0.8660254037844387076, 1.000000000000000000, 0.8660254037844387076, 1.000000000000000000, 0.9330127018922194093, 0.9330127018922194093 ) ) 
 REPRESENTATION_ITEM ( '' )  );
#33500 = FACE_OUTER_BOUND ( 'NONE', #24157, .T. ) ;
#33501 = CARTESIAN_POINT ( 'NONE',  ( 2.500000000000002220, 7.333333333333333925, 4.330127018922192761 ) ) ;
#33502 = EDGE_CURVE ( 'NONE', #10267, #2700, #24520, .T. ) ;
#33503 = CARTESIAN_POINT ( 'NONE',  ( 4.458734124999999437, -168.5000000013656063, 1.846868145590737864 ) ) ;
#33505 = ADVANCED_FACE ( 'NONE', ( #20661 ), #44121, .T. ) ;
#33504 = CARTESIAN_POINT ( 'NONE',  ( -59.98410592259440222, -145.2500000027312126, -0.3983568153799752487 ) ) ;
#33506 = CARTESIAN_POINT ( 'NONE',  ( -3.152548672688508926E-16, -55.56249999863440081, -5.148502694627439702 ) ) ;
#33507 = CARTESIAN_POINT ( 'NONE',  ( -2.500000000000000444, -84.04166666393547303, -4.330127018922193649 ) ) ;
#33508 = CARTESIAN_POINT ( 'NONE',  ( -56.48576386720575471, -137.0000000013655779, -4.591703134518078322 ) ) ;
#33509 = CARTESIAN_POINT ( 'NONE',  ( -2.499999999999996447, -16.83333333333333215, 4.330127018922195425 ) ) ;
#33510 = CARTESIAN_POINT ( 'NONE',  ( -2.500000000000000444, -92.16666666666665719, -4.330127018922193649 ) ) ;
#33511 = CARTESIAN_POINT ( 'NONE',  ( -4.458734124999999437, -92.64583333196773651, -2.574251347313719407 ) ) ;
#33512 = CARTESIAN_POINT ( 'NONE',  ( -1.846868145590737420, -156.0000000013656063, 4.458734124999997661 ) ) ;
#33513 = CARTESIAN_POINT ( 'NONE',  ( 1.060575238724906964E-15, -35.75000000000000711, 5.773502691896257311 ) ) ;
#33514 = CARTESIAN_POINT ( 'NONE',  ( -5.147856630858197489E-14, 2.375000002731183724, 5.000000000000000000 ) ) ;
#33515 = CARTESIAN_POINT ( 'NONE',  ( -58.64957059093959657, -135.0000000000000853, -2.842749532660685752 ) ) ;
#33516 = ORIENTED_EDGE ( 'NONE', *, *, #40875, .T. ) ;
#33517 = CARTESIAN_POINT ( 'NONE',  ( 2.229367062499998831, -97.64583333196773651, -3.861377020970580887 ) ) ;
#33518 = CARTESIAN_POINT ( 'NONE',  ( 4.458734125000001214, 9.854166668032263487, 2.574251347313718519 ) ) ;
#33519 = CARTESIAN_POINT ( 'NONE',  ( -2.499999999999996447, 13.29166666939785379, 4.330127018922195425 ) ) ;
#33520 = CARTESIAN_POINT ( 'NONE',  ( -51.75738570946856498, -155.0000000000000284, 3.805975901505577408 ) ) ;
#33521 = CARTESIAN_POINT ( 'NONE',  ( -5.000000000000000000, 4.000000000000000000, 0.000000000000000000 ) ) ;
#33522 = AXIS2_PLACEMENT_3D ( 'NONE', #44336, #18946, #53683 ) ;
#33523 = CARTESIAN_POINT ( 'NONE',  ( -2.229367062499996610, -64.14583333196773651, 3.861377020970582219 ) ) ;
#33524 = AXIS2_PLACEMENT_3D ( 'NONE', #25015, #59760, #35306 ) ;
#33525 = CARTESIAN_POINT ( 'NONE',  ( 0.000000000000000000, -114.9999999999999858, 0.000000000000000000 ) ) ;
#33526 = CARTESIAN_POINT ( 'NONE',  ( -5.000000000000000000, -1.958333330602145761, -2.886751345948128211 ) ) ;
#33527 = CARTESIAN_POINT ( 'NONE',  ( 4.458734125000001214, -26.89583333196774007, 2.574251347313718519 ) ) ;
#33528 = DIRECTION ( 'NONE',  ( 0.000000000000000000, 0.000000000000000000, 1.000000000000000000 ) ) ;
#33529 = CARTESIAN_POINT ( 'NONE',  ( 2.499999999999998668, 19.66666666666666430, -4.330127018922193649 ) ) ;
#33530 = CARTESIAN_POINT ( 'NONE',  ( 1.975475456537005874E-15, 7.249999999999998224, 5.000000000000000000 ) ) ;
#33531 = CARTESIAN_POINT ( 'NONE',  ( 2.500000000000002220, -46.66666666666666430, 4.330127018922192761 ) ) ;
#33533 = CARTESIAN_POINT ( 'NONE',  ( -2.229367062499996610, -18.39583333196774007, 3.861377020970582219 ) ) ;
#33532 = FACE_OUTER_BOUND ( 'NONE', #60854, .T. ) ;
#33534 = CARTESIAN_POINT ( 'NONE',  ( -1.339745962155623360, 14.33034180399266155, 4.999999999999991118 ) ) ;
#33535 = CARTESIAN_POINT ( 'NONE',  ( -2.229367062499996610, -68.14583333196773651, 3.861377020970582219 ) ) ;
#33536 = CARTESIAN_POINT ( 'NONE',  ( 4.458734124999999437, -148.6875000013656063, 0.000000000000000000 ) ) ;
#33537 = CARTESIAN_POINT ( 'NONE',  ( 2.229367062500001939, -77.97916666530106511, 3.861377020970579999 ) ) ;
#33538 = CARTESIAN_POINT ( 'NONE',  ( -50.70258187064364108, -141.3750000013656063, 2.196230717870141014 ) ) ;
#33539 = CARTESIAN_POINT ( 'NONE',  ( -4.458734124999999437, -23.56249999863440436, 0.000000000000000000 ) ) ;
#33540 = CARTESIAN_POINT ( 'NONE',  ( -5.000000000000000000, -63.95833333060213732, -2.886751345948128211 ) ) ;
#33541 = ORIENTED_EDGE ( 'NONE', *, *, #46011, .F. ) ;
#33542 = CARTESIAN_POINT ( 'NONE',  ( 1.975475456537005874E-15, -93.62499999726881583, 5.000000000000000000 ) ) ;
#33543 = VERTEX_POINT ( 'NONE', #39297 ) ;
#33544 = CARTESIAN_POINT ( 'NONE',  ( -4.458734124999998549, -69.47916666530107932, 2.574251347313722516 ) ) ;
#33545 = CARTESIAN_POINT ( 'NONE',  ( -1.339745962155613812, 7.919658201469706782, -5.000000000000000000 ) ) ;
#33546 = ORIENTED_EDGE ( 'NONE', *, *, #31225, .T. ) ;
#33547 = CARTESIAN_POINT ( 'NONE',  ( -60.14911071818854538, -143.1875000027312410, 1.666127454062681146 ) ) ;
#33548 = CARTESIAN_POINT ( 'NONE',  ( -4.458734124999999437, -52.64583333196773651, -2.574251347313719407 ) ) ;
#33549 = CARTESIAN_POINT ( 'NONE',  ( -4.458734124999998549, 3.520833334698929118, 2.574251347313722516 ) ) ;
#33550 = ORIENTED_EDGE ( 'NONE', *, *, #46056, .T. ) ;
#33551 = CARTESIAN_POINT ( 'NONE',  ( 1.975475456537005874E-15, 9.250000000000000000, 5.000000000000000000 ) ) ;
#33552 = CARTESIAN_POINT ( 'NONE',  ( 4.458734124999999437, 18.18750000136559564, -5.460374474430324690E-16 ) ) ;
#33553 = CARTESIAN_POINT ( 'NONE',  ( -55.35523342533222291, -145.3125000013656063, 4.444560631937231499 ) ) ;
#33554 = DIRECTION ( 'NONE',  ( 0.000000000000000000, 1.000000000000000000, 0.000000000000000000 ) ) ;
#33555 = CARTESIAN_POINT ( 'NONE',  ( 4.458734124999999437, -163.3750000013656347, -1.846868145590734978 ) ) ;
#33556 = ORIENTED_EDGE ( 'NONE', *, *, #24039, .T. ) ;
#33557 = CARTESIAN_POINT ( 'NONE',  ( -4.458734124999997661, -76.22916666530107932, 2.574251347313722516 ) ) ;
#33558 = CARTESIAN_POINT ( 'NONE',  ( 1.339745962155615144, -39.70534180126147561, 4.999999999999999112 ) ) ;
#33559 = CARTESIAN_POINT ( 'NONE',  ( 2.229367062499998831, 7.354166668032259935, -3.861377020970580887 ) ) ;
#33560 = AXIS2_PLACEMENT_3D ( 'NONE', #24657, #44263, #227 ) ;
#33561 = AXIS2_PLACEMENT_3D ( 'NONE', #28818, #48438, #63244 ) ;
#33562 = CARTESIAN_POINT ( 'NONE',  ( -2.499999999999996447, 2.166666666666667407, 4.330127018922195425 ) ) ;
#33563 = CARTESIAN_POINT ( 'NONE',  ( 9.457646018065525792E-16, -59.31249999863440081, 5.148502694627439702 ) ) ;
#33564 = CARTESIAN_POINT ( 'NONE',  ( -3.535250795749689387E-16, -18.12499999726881228, -5.773502691896257311 ) ) ;
#33565 = CARTESIAN_POINT ( 'NONE',  ( -54.60164318462004474, -142.5000000027312126, -4.984105922594373794 ) ) ;
#33566 = CARTESIAN_POINT ( 'NONE',  ( 2.499999999999998668, -45.33333333333333570, -4.330127018922193649 ) ) ;
#33567 = CARTESIAN_POINT ( 'NONE',  ( -2.499999999999996447, -58.83333333333333570, 4.330127018922195425 ) ) ;
#33568 = CARTESIAN_POINT ( 'NONE',  ( -3.535533905932737309, -156.6250000000000000, -3.535533905932738197 ) ) ;
#33569 = CARTESIAN_POINT ( 'NONE',  ( 0.000000000000000000, -170.0000000000000000, 0.000000000000000000 ) ) ;
#33570 = EDGE_CURVE ( 'NONE', #58699, #46845, #58925, .T. ) ;
#33571 = CARTESIAN_POINT ( 'NONE',  ( -4.458734124999999437, -42.31249999863440081, 0.000000000000000000 ) ) ;
#33572 = CARTESIAN_POINT ( 'NONE',  ( -2.229367062499996610, -29.39583333196774007, 3.861377020970582219 ) ) ;
#33573 = CARTESIAN_POINT ( 'NONE',  ( -5.000000000000000000, 26.00000000000000000, 0.000000000000000000 ) ) ;
#33574 = CARTESIAN_POINT ( 'NONE',  ( 5.000000000000000888, -148.0625000027312126, -2.071067811865475505 ) ) ;
#33575 = CARTESIAN_POINT ( 'NONE',  ( -4.458734124999999437, -105.5624999986344221, 0.000000000000000000 ) ) ;
#33576 = CARTESIAN_POINT ( 'NONE',  ( 2.229367062499998831, -33.64583333196772941, -3.861377020970580887 ) ) ;
#33577 = CARTESIAN_POINT ( 'NONE',  ( -5.000000000000000000, -68.95833333060214443, -2.886751345948128211 ) ) ;
#33578 =( BOUNDED_CURVE ( )  B_SPLINE_CURVE ( 2, ( #35900, #35260, #55208, #55841, #44581, #45224, #49411, #538, #6008 ),
 .UNSPECIFIED., .F., .F. ) 
 B_SPLINE_CURVE_WITH_KNOTS ( ( 3, 2, 2, 2, 3 ),
 ( 0.9354166666666666741, 0.9361111111111111160, 0.9375000000000000000, 0.9388888888888888840, 0.9395833333333333259 ),
 .UNSPECIFIED. ) 
 CURVE ( )  GEOMETRIC_REPRESENTATION_ITEM ( )  RATIONAL_B_SPLINE_CURVE ( ( 0.9330127018922194093, 0.9330127018922194093, 1.000000000000000000, 0.8660254037844387076, 1.000000000000000000, 0.8660254037844387076, 1.000000000000000000, 0.9330127018922194093, 0.9330127018922194093 ) ) 
 REPRESENTATION_ITEM ( '' )  );
#33579 = CARTESIAN_POINT ( 'NONE',  ( -54.64476657466781973, -147.0625000013656063, -4.444560631937228834 ) ) ;
#33580 = CARTESIAN_POINT ( 'NONE',  ( -3.535533905932738641, -143.3750000000000000, 3.535533905932737309 ) ) ;
#33581 = EDGE_CURVE ( 'NONE', #11760, #5864, #16501, .T. ) ;
#33582 = CARTESIAN_POINT ( 'NONE',  ( 2.229367062500001939, -76.22916666530106511, 3.861377020970579999 ) ) ;
#33583 = CARTESIAN_POINT ( 'NONE',  ( 1.975475456537005874E-15, -93.74999999999998579, 5.000000000000000000 ) ) ;
#33584 = CARTESIAN_POINT ( 'NONE',  ( -4.458734124999999437, -32.31249999863440792, 0.000000000000000000 ) ) ;
#33585 = FACE_OUTER_BOUND ( 'NONE', #28779, .T. ) ;
#33586 = CARTESIAN_POINT ( 'NONE',  ( 1.339745962155608039, 22.41965820146970501, 5.000000000000003553 ) ) ;
#33587 = CARTESIAN_POINT ( 'NONE',  ( 2.500000000000002220, -20.66666666666666785, 4.330127018922192761 ) ) ;
#33588 = CARTESIAN_POINT ( 'NONE',  ( -1.846868145590737420, -146.7500000013656063, 4.458734124999999437 ) ) ;
#33589 = ORIENTED_EDGE ( 'NONE', *, *, #27592, .F. ) ;
#33590 = CARTESIAN_POINT ( 'NONE',  ( 4.458734125000001214, 26.85416666803225993, 2.574251347313718519 ) ) ;
#33591 = CARTESIAN_POINT ( 'NONE',  ( -2.499999999999996447, -48.83333333333332860, 4.330127018922195425 ) ) ;
#33592 = CARTESIAN_POINT ( 'NONE',  ( 2.229367062500001939, -55.22916666530107221, 3.861377020970579999 ) ) ;
#33593 = CARTESIAN_POINT ( 'NONE',  ( -4.999999999999999112, 26.20833333606451632, 2.886751345948131764 ) ) ;
#33594 = CARTESIAN_POINT ( 'NONE',  ( 2.499999999999998668, 4.791666669397852907, -4.330127018922193649 ) ) ;
#33595 = CARTESIAN_POINT ( 'NONE',  ( -3.535250795749689387E-16, 16.75000000000000355, -5.773502691896257311 ) ) ;
#33596 = CARTESIAN_POINT ( 'NONE',  ( -1.339745962155613812, -89.20534180126146850, -5.000000000000000000 ) ) ;
#33597 = CARTESIAN_POINT ( 'NONE',  ( -4.458734124999999437, -7.312499998634404363, 0.000000000000000000 ) ) ;
#33598 =( BOUNDED_CURVE ( )  B_SPLINE_CURVE ( 2, ( #56130, #48359, #3995, #22990, #3686, #39020, #52255, #48667, #42900 ),
 .UNSPECIFIED., .F., .F. ) 
 B_SPLINE_CURVE_WITH_KNOTS ( ( 3, 2, 2, 2, 3 ),
 ( 0.4583333333333337589, 0.4625000000000004663, 0.4666666666666671182, 0.4708333333333337700, 0.4750000000000004219 ),
 .UNSPECIFIED. ) 
 CURVE ( )  GEOMETRIC_REPRESENTATION_ITEM ( )  RATIONAL_B_SPLINE_CURVE ( ( 0.9999999999999918954, 0.9238795325112948431, 1.000000000000000000, 0.9238795325112867385, 1.000000000000000000, 0.9238795325112867385, 1.000000000000000000, 0.9238795325112786339, 1.000000000000008216 ) ) 
 REPRESENTATION_ITEM ( '' )  );
#33599 = CARTESIAN_POINT ( 'NONE',  ( 2.499999999999998668, -48.33333333333332860, -4.330127018922193649 ) ) ;
#33600 = CARTESIAN_POINT ( 'NONE',  ( -5.000000000000000000, -40.87499999726880162, 0.000000000000000000 ) ) ;
#33601 = CARTESIAN_POINT ( 'NONE',  ( 4.458734124999999437, 9.937500001365593860, -5.460374474430324690E-16 ) ) ;
#33602 = CARTESIAN_POINT ( 'NONE',  ( 2.500000000000002220, -53.54166666393548013, 4.330127018922192761 ) ) ;
#33603 = ORIENTED_EDGE ( 'NONE', *, *, #26806, .T. ) ;
#33604 = VECTOR ( 'NONE', #39023, 1000.000000000000000 ) ;
#33605 = CARTESIAN_POINT ( 'NONE',  ( 5.000000000000000000, 10.70833333606451987, -2.886751345948130876 ) ) ;
#33606 = CARTESIAN_POINT ( 'NONE',  ( 4.458734125000001214, -54.89583333196773651, 2.574251347313718519 ) ) ;
#33607 = CARTESIAN_POINT ( 'NONE',  ( -4.458734124999999437, -159.1875000013655779, -5.460374474430324690E-16 ) ) ;
#33608 = MECHANICAL_DESIGN_GEOMETRIC_PRESENTATION_REPRESENTATION (  '', ( #2819 ), #31546 ) ;
#33609 = CARTESIAN_POINT ( 'NONE',  ( 2.499999999999998668, -49.20833333060213732, -4.330127018922193649 ) ) ;
#33610 = ORIENTED_EDGE ( 'NONE', *, *, #23901, .F. ) ;
#33611 = VECTOR ( 'NONE', #21064, 1000.000000000000000 ) ;
#33612 = CARTESIAN_POINT ( 'NONE',  ( -3.152548672688508926E-16, 7.187500001365594748, -5.148502694627439702 ) ) ;
#33613 = VERTEX_POINT ( 'NONE', #50556 ) ;
#33615 = DIRECTION ( 'NONE',  ( -0.6485228581062915110, 0.000000000000000000, -0.7611951803011149931 ) ) ;
#33614 = CARTESIAN_POINT ( 'NONE',  ( 2.500000000000002220, -4.666666666666666075, 4.330127018922192761 ) ) ;
#33616 = CARTESIAN_POINT ( 'NONE',  ( 2.730187237215162345E-16, -161.1875000013655779, -4.458734124999999437 ) ) ;
#33617 = ORIENTED_EDGE ( 'NONE', *, *, #14939, .F. ) ;
#33618 = DIRECTION ( 'NONE',  ( -0.000000000000000000, 1.000000000000000000, -0.000000000000000000 ) ) ;
#33619 = CARTESIAN_POINT ( 'NONE',  ( -52.53715891517739323, -135.4375000000000284, -4.819101127000233298 ) ) ;
#33620 = DIRECTION ( 'NONE',  ( 0.000000000000000000, 0.000000000000000000, 1.000000000000000000 ) ) ;
#33621 = CARTESIAN_POINT ( 'NONE',  ( -2.229367062500000163, -35.72916666530107221, -3.861377020970580443 ) ) ;
#33622 = ORIENTED_EDGE ( 'NONE', *, *, #53167, .F. ) ;
#33623 = EDGE_CURVE ( 'NONE', #44350, #51351, #34139, .T. ) ;
#33624 = CARTESIAN_POINT ( 'NONE',  ( -4.458734124999999437, -80.39583333196772230, -2.574251347313719407 ) ) ;
#33625 = CARTESIAN_POINT ( 'NONE',  ( -4.458734124999999437, 16.68750000136559564, 0.000000000000000000 ) ) ;
#33626 = ORIENTED_EDGE ( 'NONE', *, *, #39695, .T. ) ;
#33627 = CARTESIAN_POINT ( 'NONE',  ( -3.152548672688508926E-16, -87.81249999863439371, -5.148502694627439702 ) ) ;
#33628 = CARTESIAN_POINT ( 'NONE',  ( -58.24261429053147765, -125.3750000027312126, -3.805975901505573855 ) ) ;
#33629 = CARTESIAN_POINT ( 'NONE',  ( -4.764381983412779477E-15, 25.37500000273118062, 5.000000000000000000 ) ) ;
#33630 = CARTESIAN_POINT ( 'NONE',  ( -51.86629881543737497, -135.0000000000000000, 3.632629519372841287 ) ) ;
#33631 = CARTESIAN_POINT ( 'NONE',  ( -1.339745962155613812, -45.08034179853028434, -5.000000000000000000 ) ) ;
#33632 = CARTESIAN_POINT ( 'NONE',  ( -2.229367062499996610, -60.14583333196774362, 3.861377020970582219 ) ) ;
#33633 = CARTESIAN_POINT ( 'NONE',  ( 1.339745962155612702, 21.70534180126147916, -5.000000000000000000 ) ) ;
#33634 = CARTESIAN_POINT ( 'NONE',  ( -2.229367062500000163, 23.52083333469892779, -3.861377020970580443 ) ) ;
#33635 = CARTESIAN_POINT ( 'NONE',  ( 1.339745962155729053, -42.29465819873852439, -4.999999999999933387 ) ) ;
#33636 = DIRECTION ( 'NONE',  ( 1.000000000000000000, 0.000000000000000000, 0.000000000000000000 ) ) ;
#33637 = CARTESIAN_POINT ( 'NONE',  ( 2.229367062499998831, -45.89583333196774362, -3.861377020970580887 ) ) ;
#33638 = CARTESIAN_POINT ( 'NONE',  ( 1.060575238724906964E-15, -2.624999997268815388, 5.773502691896257311 ) ) ;
#33639 = DIRECTION ( 'NONE',  ( -0.000000000000000000, 1.000000000000000000, -0.000000000000000000 ) ) ;
#33640 = CARTESIAN_POINT ( 'NONE',  ( -6.972266317189433020E-16, -69.24999999999998579, -5.000000000000000000 ) ) ;
#33641 = CARTESIAN_POINT ( 'NONE',  ( -4.458734124999998549, -84.47916666530107932, 2.574251347313722516 ) ) ;
#33642 = CARTESIAN_POINT ( 'NONE',  ( -4.458734124999999437, -107.3958333319677649, -2.574251347313719407 ) ) ;
#33643 = CARTESIAN_POINT ( 'NONE',  ( 4.458734124999998549, -11.97916666530107044, -2.574251347313721627 ) ) ;
#33644 =( BOUNDED_SURFACE ( )  B_SPLINE_SURFACE ( 1, 2, ( 
 ( #16338, #56535, #46236, #61049, #55585, #56213, #12456, #21803, #31121, #41398, #50743, #1558, #12135, #17281, #31757, #6687, #45917, #51390, #36905, #27248, #1247, #1879, #21484, #7332, #20847, #26943, #46559, #47191, #3133, #33025, #33648, #13710, #17909, #42666, #8270, #37854, #4073, #57487, #9202, #52641, #57791, #62305, #48121, #62624, #18547, #8575, #13087, #22753, #37224, #28186, #32708, #38168, #3759, #13404, #52952, #32390, #14020, #53267, #27558, #33333, #61675, #23693, #47802, #42351, #23382, #61989, #38461, #37530, #8889, #42981, #12767, #17608, #56850, #57171, #62928, #47493, #28502, #46875, #2817, #52336, #18227, #52015, #43293, #27873, #22438, #18843, #3446, #7958, #42033, #23061, #58089, #48434, #34577, #510, #14338, #39090, #9815, #33959, #29426, #53580, #9508, #54209, #44554, #20120, #4376, #39403, #19154, #44879, #10146, #25260, #842, #197, #35236, #48738, #29117, #4682, #29753, #39722, #59359, #23993, #59039, #38772, #20445, #49386, #40044, #59686, #19795, #54855, #24304, #14969, #10459, #58410, #34263, #63558, #15619, #5331, #28814, #43597, #24948, #15294, #43909, #58720, #14646, #19476, #63240, #34916, #54538, #53891, #30073, #49058, #49703, #5006, #5647, #24626, #44232, #1800, #7253, #31347, #21081, #45197, #21403, #12055, #31679, #51315, #40686, #25584, #41319, #17202, #41627, #26865, #11101, #30725, #60649, #61281, #60967, #45517, #6604, #35877, #41007, #46478, #16572, #36830, #36194, #21724, #26218, #2424, #26540, #46161, #55815, #60331, #50348, #1164, #11731, #16258, #2123, #50990, #6929, #16887, #60010, #10788, #30398, #55180, #36503, #20763, #22036, #56133, #6295, #50021, #25900, #5975, #1478, #40369, #15933, #35556, #55506, #11420, #31039, #50664, #45838, #47732, #56460, #12382, #32309, #27798, #22358, #52257, #51938, #31995, #18148, #22678, #7563, #62856, #18769, #43216, #51629, #62230, #28115, #41956, #3060, #37460, #61599, #57090, #27175, #46792, #7880, #8816, #13009, #3688, #2738, #17534, #27483, #47423, #37152, #8196, #47112, #56777, #37776, #42277, #12696, #61917, #17837, #32629, #3375, #57408, #23302, #22992, #42593, #13328, #32949, #52572, #8505, #42902, #62551, #18471, #38091, #57717, #13642, #33263, #28432, #52881, #48045, #3997, #23619, #44800, #58337, #4934, #20043, #48361, #43838, #9435, #10394, #58964, #25185, #38396, #29351, #14891, #4305, #48669, #4609, #33885, #30004, #48985, #34498, #29044, #54132, #49634, #19722, #14265, #24554, #53505, #43525, #44159, #34844, #10070, #24232, #9128, #128, #39648, #59286, #15217, #63484, #53195, #5256, #763, #5571, #54467, #38700, #19407, #39331, #58020, #24877, #39022, #34193, #58650, #29684, #13948, #49313, #33574, #44478, #437, #53816, #28735, #23924, #63169, #19080, #14571, #9746, #10715, #26146, #50270, #55740, #40927, #50592, #26467, #5899, #51240, #7175, #1089, #50910, #35169, #60886, #6532, #59940, #11344, #40302, #11976, #15863, #46083, #45765, #49944, #55101, #16495, #31605, #1721, #35484, #30967, #11026, #25505, #21327, #16810, #60573, #30648, #54785, #36117, #21647, #41239, #36431, #6217, #30322, #6852, #26783, #46402, #56060, #20697, #25829, #11656, #20371, #2042, #45445, #16178, #1409, #31276, #39971, #59616, #15548, #45124, #21009, #35803, #40616, #60260, #55427, #27725, #32230, #2660, #56384, #8122, #51861, #37692, #22923, #32552, #8436, #51551, #33192, #52807, #46715, #32873, #17130, #42830, #52177, #41880, #57014, #22280, #57646, #61526, #28040, #47352, #31923, #36754, #12310, #17457, #18394, #2987, #57334, #2351, #21959, #37080, #37381, #7486, #61845, #56701, #41555, #3301, #7804, #27099, #8744, #28351, #61206, #12618, #42515, #13250, #27406, #47038, #22604, #42201, #17764, #12929, #62152, #18070, #52502, #47659, #3612, #23219, #62474, #38014, #13574, #44403, #19965, #19329, #54391, #4236, #14498 ),
 ( #39575, #38943, #44083, #48, #19647, #53119, #9362, #362, #9674, #29608, #58884, #13876, #48912, #3923, #34429, #33503, #10318, #54057, #59214, #18701, #58263, #47968, #14815, #9054, #39258, #28664, #23542, #24163, #43454, #48280, #15144, #49238, #28975, #23851, #48597, #9995, #4858, #24478, #63099, #5180, #63412, #19011, #24798, #43141, #38326, #34119, #34765, #62782, #29282, #58579, #57955, #53742, #38624, #14185, #33812, #53429, #43766, #4537, #40539, #49554, #11269, #55988, #45371, #1337, #5814, #55025, #20935, #25758, #20292, #16741, #1648, #25432, #5496, #45050, #30894, #21247, #60180, #49866, #60816, #35403, #44721, #31209, #30243, #1017, #30567, #25110, #40854, #59863, #40228, #10948, #50838, #16102, #50524, #60497, #39893, #50191, #45691, #10630, #6779, #29929, #36358, #26073, #54710, #16425, #683, #35726, #59539, #20621, #1972, #36044, #15787, #55674, #6143, #55355, #6465, #21572, #11589, #26389, #46007, #41169, #15474, #35091, #46327, #7733, #3537, #51165, #46645, #31848, #62397, #42754, #56308, #41808, #26713, #12234, #2286, #27338, #23146, #7098, #2590, #51480, #18318, #37943, #7418, #27653, #47280, #17059, #37002, #8362, #37309, #57260, #22847, #41485, #12859, #31523, #62080, #61137, #11903, #17993, #21889, #36676, #22210, #27027, #42437, #61453, #8049, #17383, #56629, #51791, #12542, #32155, #27963, #13179, #46969, #2916, #22529, #37619, #32478, #52107, #42125, #32801, #61767, #17695, #3229, #56938, #52430, #47586, #54553, #15310, #20137, #4467, #33117, #28906, #15635, #9289, #59376, #8666, #33737, #52734, #24094, #13501, #39736, #20780, #48527, #43689, #33424, #18935, #63336, #53354, #47892, #45214, #30089, #53043, #28278, #8980, #34932, #49719, #10476, #13804, #25601, #63028, #3848, #59703, #57879, #28591, #58183, #23469, #5664, #23781, #4166, #38551, #35251, #25277, #44899, #858, #43073, #14111, #20461, #38258, #54871, #57576, #1180, #40060, #18636, #10802, #62710, #30414, #48211, #43383, #50038, #5997, #21096, #7267, #1493, #1814, #51004, #12395, #2441, #21418, #41021, #32010, #21739, #16273, #6944, #35892, #45532, #31363, #36844, #60981, #50677, #11115, #26555, #41643, #61295, #17217, #6619, #55195, #26879, #46806, #7578, #56474, #40700, #60345, #46175, #27190, #46493, #11436, #36208, #60664, #2136, #51644, #41334, #2753, #16902, #51329, #55830, #40385, #56148, #12069, #36518, #26232, #55523, #30742, #31694, #45852, #22050, #60026, #15949, #35571, #25914, #50362, #6310, #31054, #16588, #11745, #62870, #8519, #61932, #13343, #42291, #13961, #17851, #48060, #47747, #51955, #37168, #56791, #37473, #38409, #23007, #13657, #22372, #41972, #57108, #57422, #7893, #18165, #13025, #61614, #3703, #52273, #12709, #28750, #48375, #9141, #17548, #28129, #57731, #27498, #32642, #3390, #47127, #42608, #3075, #22692, #23318, #38107, #33277, #32325, #32963, #8210, #58031, #42919, #18782, #33588, #52587, #27813, #47438, #62566, #4013, #62246, #37792, #18485, #53207, #52896, #8832, #28445, #23634, #43229, #14278, #14585, #34205, #63496, #59628, #58978, #453, #39035, #20057, #33897, #29365, #39661, #48681, #44814, #4317, #10727, #59298, #29057, #15230, #54799, #34514, #23937, #4621, #39983, #34858, #24246, #54479, #43850, #48998, #14905, #15561, #30018, #4945, #24568, #53829, #19093, #19421, #38711, #140, #35181, #43538, #58662, #9758, #30334, #63182, #44173, #10406, #49646, #9448, #19734, #776, #29695, #5583, #25200, #53520, #5269, #58350, #20383, #39348, #54145, #10084, #49326, #24890, #44491, #12322, #60899, #15876, #46093, #35496, #25519, #26157, #45457, #50283, #2364, #51252, #11355, #55114, #30978, #16822, #6864, #26479, #11039, #36441, #1735, #30662, #21661, #45137, #40315, #36129, #2053, #41252, #11668, #60588, #1101, #21338, #7187, #40938, #50922, #20710, #45776, #59953, #16508, #5912 ) ),
 .UNSPECIFIED., .F., .F., .F. ) 
 B_SPLINE_SURFACE_WITH_KNOTS ( ( 2, 2 ),
 ( 3, 2, 2, 2, 2, 2, 2, 2, 2, 2, 2, 2, 2, 2, 2, 2, 2, 2, 2, 2, 2, 2, 2, 2, 2, 2, 2, 2, 2, 2, 2, 2, 2, 2, 2, 2, 2, 2, 2, 2, 2, 2, 2, 2, 2, 2, 2, 2, 2, 2, 2, 2, 2, 2, 2, 2, 2, 2, 2, 2, 2, 2, 2, 2, 2, 2, 2, 2, 2, 2, 2, 2, 2, 2, 2, 2, 2, 2, 2, 2, 2, 2, 2, 2, 2, 2, 2, 2, 2, 2, 2, 2, 2, 2, 2, 2, 2, 2, 2, 2, 2, 2, 2, 2, 2, 2, 2, 2, 2, 2, 2, 2, 2, 2, 2, 2, 2, 2, 2, 2, 2, 2, 2, 2, 2, 2, 2, 2, 2, 2, 2, 2, 2, 2, 2, 2, 2, 2, 2, 2, 2, 2, 2, 2, 2, 2, 2, 2, 2, 2, 2, 2, 2, 2, 2, 2, 2, 2, 2, 2, 2, 2, 2, 2, 2, 2, 2, 2, 2, 2, 2, 2, 2, 2, 2, 2, 2, 2, 2, 2, 2, 2, 2, 2, 2, 2, 2, 2, 2, 2, 2, 2, 2, 2, 2, 2, 2, 2, 2, 2, 2, 2, 2, 2, 2, 2, 2, 2, 2, 2, 2, 2, 2, 2, 2, 2, 2, 2, 2, 2, 2, 2, 2, 2, 2, 2, 2, 2, 2, 2, 2, 2, 2, 2, 2, 2, 2, 2, 2, 2, 3 ),
 ( 0.000000000000000000, 1.000000000000000000 ),
 ( 0.000000000000000000, 0.004166666666666666609, 0.008333333333333333218, 0.01250000000000000069, 0.01666666666666666644, 0.02083333333333333218, 0.02500000000000000139, 0.02916666666666666713, 0.03333333333333333287, 0.03749999999999999861, 0.04166666666666666435, 0.04583333333333333010, 0.05000000000000000278, 0.05416666666666666852, 0.05833333333333333426, 0.06250000000000000000, 0.06666666666666666574, 0.07083333333333333148, 0.07499999999999999722, 0.07916666666666666297, 0.08333333333333332871, 0.08749999999999999445, 0.09166666666666666019, 0.09583333333333333981, 0.1000000000000000056, 0.1041666666666666713, 0.1083333333333333370, 0.1125000000000000028, 0.1166666666666666685, 0.1208333333333333343, 0.1250000000000000000, 0.1291666666666666796, 0.1333333333333333315, 0.1375000000000000111, 0.1416666666666666630, 0.1458333333333333426, 0.1499999999999999944, 0.1541666666666666741, 0.1583333333333333259, 0.1625000000000000056, 0.1666666666666666574, 0.1708333333333333370, 0.1749999999999999889, 0.1791666666666666685, 0.1833333333333333204, 0.1875000000000000000, 0.1916666666666666796, 0.1958333333333333315, 0.2000000000000000111, 0.2041666666666666630, 0.2083333333333333426, 0.2124999999999999944, 0.2166666666666666741, 0.2208333333333333259, 0.2250000000000000056, 0.2291666666666666574, 0.2333333333333333370, 0.2374999999999999889, 0.2416666666666666685, 0.2458333333333333204, 0.2500000000000000000, 0.2541666666666666519, 0.2583333333333333592, 0.2625000000000000111, 0.2666666666666666630, 0.2708333333333333148, 0.2750000000000000222, 0.2791666666666666741, 0.2833333333333333259, 0.2874999999999999778, 0.2916666666666666852, 0.2958333333333333370, 0.2999999999999999889, 0.3041666666666666408, 0.3083333333333333481, 0.3125000000000000000, 0.3166666666666666519, 0.3208333333333333592, 0.3250000000000000111, 0.3291666666666666630, 0.3333333333333333148, 0.3375000000000000222, 0.3416666666666666741, 0.3458333333333333259, 0.3499999999999999778, 0.3541666666666666852, 0.3583333333333333370, 0.3624999999999999889, 0.3666666666666666408, 0.3708333333333333481, 0.3750000000000000000, 0.3791666666666666519, 0.3833333333333333592, 0.3875000000000000111, 0.3916666666666666630, 0.3958333333333333148, 0.4000000000000000222, 0.4041666666666666741, 0.4083333333333333259, 0.4124999999999999778, 0.4166666666666666852, 0.4208333333333333370, 0.4249999999999999889, 0.4291666666666666408, 0.4333333333333333481, 0.4375000000000000000, 0.4416666666666666519, 0.4458333333333333592, 0.4500000000000000111, 0.4541666666666666630, 0.4583333333333333148, 0.4625000000000000222, 0.4666666666666666741, 0.4708333333333333259, 0.4749999999999999778, 0.4791666666666666852, 0.4833333333333333370, 0.4874999999999999889, 0.4916666666666666408, 0.4958333333333333481, 0.5000000000000000000, 0.5041666666666666519, 0.5083333333333333037, 0.5124999999999999556, 0.5166666666666667185, 0.5208333333333333703, 0.5250000000000000222, 0.5291666666666666741, 0.5333333333333333259, 0.5374999999999999778, 0.5416666666666666297, 0.5458333333333332815, 0.5500000000000000444, 0.5541666666666666963, 0.5583333333333333481, 0.5625000000000000000, 0.5666666666666666519, 0.5708333333333333037, 0.5749999999999999556, 0.5791666666666667185, 0.5833333333333333703, 0.5875000000000000222, 0.5916666666666666741, 0.5958333333333333259, 0.5999999999999999778, 0.6041666666666666297, 0.6083333333333332815, 0.6125000000000000444, 0.6166666666666666963, 0.6208333333333333481, 0.6250000000000000000, 0.6291666666666666519, 0.6333333333333333037, 0.6374999999999999556, 0.6416666666666667185, 0.6458333333333333703, 0.6500000000000000222, 0.6541666666666666741, 0.6583333333333333259, 0.6624999999999999778, 0.6666666666666666297, 0.6708333333333332815, 0.6750000000000000444, 0.6791666666666666963, 0.6833333333333333481, 0.6875000000000000000, 0.6916666666666666519, 0.6958333333333333037, 0.6999999999999999556, 0.7041666666666667185, 0.7083333333333333703, 0.7125000000000000222, 0.7166666666666666741, 0.7208333333333333259, 0.7249999999999999778, 0.7291666666666666297, 0.7333333333333332815, 0.7375000000000000444, 0.7416666666666666963, 0.7458333333333333481, 0.7500000000000000000, 0.7541666666666666519, 0.7583333333333333037, 0.7624999999999999556, 0.7666666666666667185, 0.7708333333333333703, 0.7750000000000000222, 0.7791666666666666741, 0.7833333333333333259, 0.7874999999999999778, 0.7916666666666666297, 0.7958333333333332815, 0.8000000000000000444, 0.8041666666666666963, 0.8083333333333333481, 0.8125000000000000000, 0.8166666666666666519, 0.8208333333333333037, 0.8249999999999999556, 0.8291666666666667185, 0.8333333333333333703, 0.8375000000000000222, 0.8416666666666666741, 0.8458333333333333259, 0.8499999999999999778, 0.8541666666666666297, 0.8583333333333332815, 0.8625000000000000444, 0.8666666666666666963, 0.8708333333333333481, 0.8750000000000000000, 0.8791666666666666519, 0.8833333333333333037, 0.8874999999999999556, 0.8916666666666667185, 0.8958333333333333703, 0.9000000000000000222, 0.9041666666666666741, 0.9083333333333333259, 0.9124999999999999778, 0.9166666666666666297, 0.9208333333333332815, 0.9250000000000000444, 0.9291666666666666963, 0.9333333333333333481, 0.9375000000000000000, 0.9416666666666666519, 0.9458333333333333037, 0.9499999999999999556, 0.9541666666666667185, 0.9583333333333333703, 0.9625000000000000222, 0.9666666666666666741, 0.9708333333333333259, 0.9749999999999999778, 0.9791666666666666297, 0.9833333333333332815, 0.9875000000000000444, 0.9916666666666666963, 0.9958333333333333481, 1.000000000000000000 ),
 .UNSPECIFIED. ) 
 GEOMETRIC_REPRESENTATION_ITEM ( )  RATIONAL_B_SPLINE_SURFACE ( (
 ( 1.000000000000000000, 0.9238795325112867385, 1.000000000000000000, 0.9238795325112867385, 1.000000000000000000, 0.9238795325112867385, 1.000000000000000000, 0.9238795325112867385, 1.000000000000000000, 0.9238795325112867385, 1.000000000000000000, 0.9238795325112867385, 1.000000000000000000, 0.9238795325112867385, 1.000000000000000000, 0.9238795325112867385, 1.000000000000000000, 0.9238795325112867385, 1.000000000000000000, 0.9238795325112867385, 1.000000000000000000, 0.9238795325112867385, 1.000000000000000000, 0.9238795325112867385, 1.000000000000000000, 0.9238795325112867385, 1.000000000000000000, 0.9238795325112867385, 1.000000000000000000, 0.9238795325112867385, 1.000000000000000000, 0.9238795325112867385, 1.000000000000000000, 0.9238795325112867385, 1.000000000000000000, 0.9238795325112867385, 1.000000000000000000, 0.9238795325112867385, 1.000000000000000000, 0.9238795325112867385, 1.000000000000000000, 0.9238795325112867385, 1.000000000000000000, 0.9238795325112867385, 1.000000000000000000, 0.9238795325112867385, 1.000000000000000000, 0.9238795325112867385, 1.000000000000000000, 0.9238795325112867385, 1.000000000000000000, 0.9238795325112867385, 1.000000000000000000, 0.9238795325112867385, 1.000000000000000000, 0.9238795325112867385, 1.000000000000000000, 0.9238795325112867385, 1.000000000000000000, 0.9238795325112867385, 1.000000000000000000, 0.9238795325112867385, 1.000000000000000000, 0.9238795325112867385, 1.000000000000000000, 0.9238795325112867385, 1.000000000000000000, 0.9238795325112867385, 1.000000000000000000, 0.9238795325112867385, 1.000000000000000000, 0.9238795325112867385, 1.000000000000000000, 0.9238795325112867385, 1.000000000000000000, 0.9238795325112867385, 1.000000000000000000, 0.9238795325112867385, 1.000000000000000000, 0.9238795325112867385, 1.000000000000000000, 0.9238795325112867385, 1.000000000000000000, 0.9238795325112867385, 1.000000000000000000, 0.9238795325112867385, 1.000000000000000000, 0.9238795325112867385, 1.000000000000000000, 0.9238795325112867385, 1.000000000000000000, 0.9238795325112867385, 1.000000000000000000, 0.9238795325112867385, 1.000000000000000000, 0.9238795325112867385, 1.000000000000000000, 0.9238795325112867385, 1.000000000000000000, 0.9238795325112867385, 1.000000000000000000, 0.9238795325112867385, 1.000000000000000000, 0.9238795325112867385, 1.000000000000000000, 0.9238795325112867385, 1.000000000000000000, 0.9238795325112867385, 1.000000000000000000, 0.9238795325112867385, 1.000000000000000000, 0.9238795325112867385, 1.000000000000000000, 0.9238795325112867385, 1.000000000000000000, 0.9238795325112867385, 1.000000000000000000, 0.9238795325112867385, 1.000000000000000000, 0.9238795325112867385, 1.000000000000000000, 0.9238795325112867385, 1.000000000000000000, 0.9238795325112867385, 1.000000000000000000, 0.9238795325112867385, 1.000000000000000000, 0.9238795325112867385, 1.000000000000000000, 0.9238795325112867385, 1.000000000000000000, 0.9238795325112867385, 1.000000000000000000, 0.9238795325112867385, 1.000000000000000000, 0.9238795325112867385, 1.000000000000000000, 0.9238795325112867385, 1.000000000000000000, 0.9238795325112867385, 1.000000000000000000, 0.9238795325112867385, 1.000000000000000000, 0.9238795325112867385, 1.000000000000000000, 0.9238795325112867385, 1.000000000000000000, 0.9238795325112867385, 1.000000000000000000, 0.9238795325112867385, 1.000000000000000000, 0.9238795325112867385, 1.000000000000000000, 0.9238795325112867385, 1.000000000000000000, 0.9238795325112867385, 1.000000000000000000, 0.9238795325112867385, 1.000000000000000000, 0.9238795325112867385, 1.000000000000000000, 0.9238795325112867385, 1.000000000000000000, 0.9238795325112867385, 1.000000000000000000, 0.9238795325112867385, 1.000000000000000000, 0.9238795325112867385, 1.000000000000000000, 0.9238795325112867385, 1.000000000000000000, 0.9238795325112867385, 1.000000000000000000, 0.9238795325112867385, 1.000000000000000000, 0.9238795325112867385, 1.000000000000000000, 0.9238795325112867385, 1.000000000000000000, 0.9238795325112867385, 1.000000000000000000, 0.9238795325112867385, 1.000000000000000000, 0.9238795325112867385, 1.000000000000000000, 0.9238795325112867385, 1.000000000000000000, 0.9238795325112867385, 1.000000000000000000, 0.9238795325112867385, 1.000000000000000000, 0.9238795325112867385, 1.000000000000000000, 0.9238795325112867385, 1.000000000000000000, 0.9238795325112867385, 1.000000000000000000, 0.9238795325112867385, 1.000000000000000000, 0.9238795325112867385, 1.000000000000000000, 0.9238795325112867385, 1.000000000000000000, 0.9238795325112867385, 1.000000000000000000, 0.9238795325112867385, 1.000000000000000000, 0.9238795325112867385, 1.000000000000000000, 0.9238795325112867385, 1.000000000000000000, 0.9238795325112867385, 1.000000000000000000, 0.9238795325112867385, 1.000000000000000000, 0.9238795325112867385, 1.000000000000000000, 0.9238795325112867385, 1.000000000000000000, 0.9238795325112867385, 1.000000000000000000, 0.9238795325112867385, 1.000000000000000000, 0.9238795325112867385, 1.000000000000000000, 0.9238795325112867385, 1.000000000000000000, 0.9238795325112867385, 1.000000000000000000, 0.9238795325112867385, 1.000000000000000000, 0.9238795325112867385, 1.000000000000000000, 0.9238795325112867385, 1.000000000000000000, 0.9238795325112867385, 1.000000000000000000, 0.9238795325112867385, 1.000000000000000000, 0.9238795325112867385, 1.000000000000000000, 0.9238795325112867385, 1.000000000000000000, 0.9238795325112867385, 1.000000000000000000, 0.9238795325112867385, 1.000000000000000000, 0.9238795325112867385, 1.000000000000000000, 0.9238795325112867385, 1.000000000000000000, 0.9238795325112867385, 1.000000000000000000, 0.9238795325112867385, 1.000000000000000000, 0.9238795325112867385, 1.000000000000000000, 0.9238795325112867385, 1.000000000000000000, 0.9238795325112867385, 1.000000000000000000, 0.9238795325112867385, 1.000000000000000000, 0.9238795325112867385, 1.000000000000000000, 0.9238795325112867385, 1.000000000000000000, 0.9238795325112867385, 1.000000000000000000, 0.9238795325112867385, 1.000000000000000000, 0.9238795325112867385, 1.000000000000000000, 0.9238795325112867385, 1.000000000000000000, 0.9238795325112867385, 1.000000000000000000, 0.9238795325112867385, 1.000000000000000000, 0.9238795325112867385, 1.000000000000000000, 0.9238795325112867385, 1.000000000000000000, 0.9238795325112867385, 1.000000000000000000, 0.9238795325112867385, 1.000000000000000000, 0.9238795325112867385, 1.000000000000000000, 0.9238795325112867385, 1.000000000000000000, 0.9238795325112867385, 1.000000000000000000, 0.9238795325112867385, 1.000000000000000000, 0.9238795325112867385, 1.000000000000000000, 0.9238795325112867385, 1.000000000000000000, 0.9238795325112867385, 1.000000000000000000, 0.9238795325112867385, 1.000000000000000000, 0.9238795325112867385, 1.000000000000000000, 0.9238795325112867385, 1.000000000000000000, 0.9238795325112867385, 1.000000000000000000, 0.9238795325112867385, 1.000000000000000000, 0.9238795325112867385, 1.000000000000000000, 0.9238795325112867385, 1.000000000000000000, 0.9238795325112867385, 1.000000000000000000, 0.9238795325112867385, 1.000000000000000000, 0.9238795325112867385, 1.000000000000000000, 0.9238795325112867385, 1.000000000000000000, 0.9238795325112867385, 1.000000000000000000, 0.9238795325112867385, 1.000000000000000000, 0.9238795325112867385, 1.000000000000000000, 0.9238795325112867385, 1.000000000000000000, 0.9238795325112867385, 1.000000000000000000, 0.9238795325112867385, 1.000000000000000000, 0.9238795325112867385, 1.000000000000000000, 0.9238795325112867385, 1.000000000000000000, 0.9238795325112867385, 1.000000000000000000, 0.9238795325112867385, 1.000000000000000000, 0.9238795325112867385, 1.000000000000000000, 0.9238795325112867385, 1.000000000000000000, 0.9238795325112867385, 1.000000000000000000, 0.9238795325112867385, 1.000000000000000000, 0.9238795325112867385, 1.000000000000000000, 0.9238795325112867385, 1.000000000000000000, 0.9238795325112867385, 1.000000000000000000, 0.9238795325112867385, 1.000000000000000000, 0.9238795325112867385, 1.000000000000000000, 0.9238795325112867385, 1.000000000000000000, 0.9238795325112867385, 1.000000000000000000, 0.9238795325112867385, 1.000000000000000000, 0.9238795325112867385, 1.000000000000000000, 0.9238795325112867385, 1.000000000000000000, 0.9238795325112867385, 1.000000000000000000, 0.9238795325112867385, 1.000000000000000000, 0.9238795325112867385, 1.000000000000000000, 0.9238795325112867385, 1.000000000000000000, 0.9238795325112867385, 1.000000000000000000, 0.9238795325112867385, 1.000000000000000000, 0.9238795325112867385, 1.000000000000000000, 0.9238795325112867385, 1.000000000000000000, 0.9238795325112867385, 1.000000000000000000, 0.9238795325112867385, 1.000000000000000000, 0.9238795325112867385, 1.000000000000000000, 0.9238795325112867385, 1.000000000000000000, 0.9238795325112867385, 1.000000000000000000, 0.9238795325112867385, 1.000000000000000000, 0.9238795325112867385, 1.000000000000000000, 0.9238795325112867385, 1.000000000000000000, 0.9238795325112867385, 1.000000000000000000, 0.9238795325112867385, 1.000000000000000000, 0.9238795325112867385, 1.000000000000000000, 0.9238795325112867385, 1.000000000000000000, 0.9238795325112867385, 1.000000000000000000, 0.9238795325112867385, 1.000000000000000000, 0.9238795325112867385, 1.000000000000000000, 0.9238795325112867385, 1.000000000000000000, 0.9238795325112867385, 1.000000000000000000, 0.9238795325112867385, 1.000000000000000000, 0.9238795325112867385, 1.000000000000000000, 0.9238795325112867385, 1.000000000000000000, 0.9238795325112867385, 1.000000000000000000, 0.9238795325112867385, 1.000000000000000000, 0.9238795325112867385, 1.000000000000000000, 0.9238795325112867385, 1.000000000000000000, 0.9238795325112867385, 1.000000000000000000, 0.9238795325112867385, 1.000000000000000000, 0.9238795325112867385, 1.000000000000000000, 0.9238795325112867385, 1.000000000000000000, 0.9238795325112867385, 1.000000000000000000, 0.9238795325112867385, 1.000000000000000000, 0.9238795325112867385, 1.000000000000000000, 0.9238795325112867385, 1.000000000000000000, 0.9238795325112867385, 1.000000000000000000, 0.9238795325112867385, 1.000000000000000000, 0.9238795325112867385, 1.000000000000000000, 0.9238795325112867385, 1.000000000000000000, 0.9238795325112867385, 1.000000000000000000, 0.9238795325112867385, 1.000000000000000000, 0.9238795325112867385, 1.000000000000000000, 0.9238795325112867385, 1.000000000000000000, 0.9238795325112867385, 1.000000000000000000, 0.9238795325112867385, 1.000000000000000000, 0.9238795325112867385, 1.000000000000000000, 0.9238795325112867385, 1.000000000000000000, 0.9238795325112867385, 1.000000000000000000, 0.9238795325112867385, 1.000000000000000000, 0.9238795325112867385, 1.000000000000000000),
 ( 1.000000000000000000, 0.9238795325112867385, 1.000000000000000000, 0.9238795325112867385, 1.000000000000000000, 0.9238795325112867385, 1.000000000000000000, 0.9238795325112867385, 1.000000000000000000, 0.9238795325112867385, 1.000000000000000000, 0.9238795325112867385, 1.000000000000000000, 0.9238795325112867385, 1.000000000000000000, 0.9238795325112867385, 1.000000000000000000, 0.9238795325112867385, 1.000000000000000000, 0.9238795325112867385, 1.000000000000000000, 0.9238795325112867385, 1.000000000000000000, 0.9238795325112867385, 1.000000000000000000, 0.9238795325112867385, 1.000000000000000000, 0.9238795325112867385, 1.000000000000000000, 0.9238795325112867385, 1.000000000000000000, 0.9238795325112867385, 1.000000000000000000, 0.9238795325112867385, 1.000000000000000000, 0.9238795325112867385, 1.000000000000000000, 0.9238795325112867385, 1.000000000000000000, 0.9238795325112867385, 1.000000000000000000, 0.9238795325112867385, 1.000000000000000000, 0.9238795325112867385, 1.000000000000000000, 0.9238795325112867385, 1.000000000000000000, 0.9238795325112867385, 1.000000000000000000, 0.9238795325112867385, 1.000000000000000000, 0.9238795325112867385, 1.000000000000000000, 0.9238795325112867385, 1.000000000000000000, 0.9238795325112867385, 1.000000000000000000, 0.9238795325112867385, 1.000000000000000000, 0.9238795325112867385, 1.000000000000000000, 0.9238795325112867385, 1.000000000000000000, 0.9238795325112867385, 1.000000000000000000, 0.9238795325112867385, 1.000000000000000000, 0.9238795325112867385, 1.000000000000000000, 0.9238795325112867385, 1.000000000000000000, 0.9238795325112867385, 1.000000000000000000, 0.9238795325112867385, 1.000000000000000000, 0.9238795325112867385, 1.000000000000000000, 0.9238795325112867385, 1.000000000000000000, 0.9238795325112867385, 1.000000000000000000, 0.9238795325112867385, 1.000000000000000000, 0.9238795325112867385, 1.000000000000000000, 0.9238795325112867385, 1.000000000000000000, 0.9238795325112867385, 1.000000000000000000, 0.9238795325112867385, 1.000000000000000000, 0.9238795325112867385, 1.000000000000000000, 0.9238795325112867385, 1.000000000000000000, 0.9238795325112867385, 1.000000000000000000, 0.9238795325112867385, 1.000000000000000000, 0.9238795325112867385, 1.000000000000000000, 0.9238795325112867385, 1.000000000000000000, 0.9238795325112867385, 1.000000000000000000, 0.9238795325112867385, 1.000000000000000000, 0.9238795325112867385, 1.000000000000000000, 0.9238795325112867385, 1.000000000000000000, 0.9238795325112867385, 1.000000000000000000, 0.9238795325112867385, 1.000000000000000000, 0.9238795325112867385, 1.000000000000000000, 0.9238795325112867385, 1.000000000000000000, 0.9238795325112867385, 1.000000000000000000, 0.9238795325112867385, 1.000000000000000000, 0.9238795325112867385, 1.000000000000000000, 0.9238795325112867385, 1.000000000000000000, 0.9238795325112867385, 1.000000000000000000, 0.9238795325112867385, 1.000000000000000000, 0.9238795325112867385, 1.000000000000000000, 0.9238795325112867385, 1.000000000000000000, 0.9238795325112867385, 1.000000000000000000, 0.9238795325112867385, 1.000000000000000000, 0.9238795325112867385, 1.000000000000000000, 0.9238795325112867385, 1.000000000000000000, 0.9238795325112867385, 1.000000000000000000, 0.9238795325112867385, 1.000000000000000000, 0.9238795325112867385, 1.000000000000000000, 0.9238795325112867385, 1.000000000000000000, 0.9238795325112867385, 1.000000000000000000, 0.9238795325112867385, 1.000000000000000000, 0.9238795325112867385, 1.000000000000000000, 0.9238795325112867385, 1.000000000000000000, 0.9238795325112867385, 1.000000000000000000, 0.9238795325112867385, 1.000000000000000000, 0.9238795325112867385, 1.000000000000000000, 0.9238795325112867385, 1.000000000000000000, 0.9238795325112867385, 1.000000000000000000, 0.9238795325112867385, 1.000000000000000000, 0.9238795325112867385, 1.000000000000000000, 0.9238795325112867385, 1.000000000000000000, 0.9238795325112867385, 1.000000000000000000, 0.9238795325112867385, 1.000000000000000000, 0.9238795325112867385, 1.000000000000000000, 0.9238795325112867385, 1.000000000000000000, 0.9238795325112867385, 1.000000000000000000, 0.9238795325112867385, 1.000000000000000000, 0.9238795325112867385, 1.000000000000000000, 0.9238795325112867385, 1.000000000000000000, 0.9238795325112867385, 1.000000000000000000, 0.9238795325112867385, 1.000000000000000000, 0.9238795325112867385, 1.000000000000000000, 0.9238795325112867385, 1.000000000000000000, 0.9238795325112867385, 1.000000000000000000, 0.9238795325112867385, 1.000000000000000000, 0.9238795325112867385, 1.000000000000000000, 0.9238795325112867385, 1.000000000000000000, 0.9238795325112867385, 1.000000000000000000, 0.9238795325112867385, 1.000000000000000000, 0.9238795325112867385, 1.000000000000000000, 0.9238795325112867385, 1.000000000000000000, 0.9238795325112867385, 1.000000000000000000, 0.9238795325112867385, 1.000000000000000000, 0.9238795325112867385, 1.000000000000000000, 0.9238795325112867385, 1.000000000000000000, 0.9238795325112867385, 1.000000000000000000, 0.9238795325112867385, 1.000000000000000000, 0.9238795325112867385, 1.000000000000000000, 0.9238795325112867385, 1.000000000000000000, 0.9238795325112867385, 1.000000000000000000, 0.9238795325112867385, 1.000000000000000000, 0.9238795325112867385, 1.000000000000000000, 0.9238795325112867385, 1.000000000000000000, 0.9238795325112867385, 1.000000000000000000, 0.9238795325112867385, 1.000000000000000000, 0.9238795325112867385, 1.000000000000000000, 0.9238795325112867385, 1.000000000000000000, 0.9238795325112867385, 1.000000000000000000, 0.9238795325112867385, 1.000000000000000000, 0.9238795325112867385, 1.000000000000000000, 0.9238795325112867385, 1.000000000000000000, 0.9238795325112867385, 1.000000000000000000, 0.9238795325112867385, 1.000000000000000000, 0.9238795325112867385, 1.000000000000000000, 0.9238795325112867385, 1.000000000000000000, 0.9238795325112867385, 1.000000000000000000, 0.9238795325112867385, 1.000000000000000000, 0.9238795325112867385, 1.000000000000000000, 0.9238795325112867385, 1.000000000000000000, 0.9238795325112867385, 1.000000000000000000, 0.9238795325112867385, 1.000000000000000000, 0.9238795325112867385, 1.000000000000000000, 0.9238795325112867385, 1.000000000000000000, 0.9238795325112867385, 1.000000000000000000, 0.9238795325112867385, 1.000000000000000000, 0.9238795325112867385, 1.000000000000000000, 0.9238795325112867385, 1.000000000000000000, 0.9238795325112867385, 1.000000000000000000, 0.9238795325112867385, 1.000000000000000000, 0.9238795325112867385, 1.000000000000000000, 0.9238795325112867385, 1.000000000000000000, 0.9238795325112867385, 1.000000000000000000, 0.9238795325112867385, 1.000000000000000000, 0.9238795325112867385, 1.000000000000000000, 0.9238795325112867385, 1.000000000000000000, 0.9238795325112867385, 1.000000000000000000, 0.9238795325112867385, 1.000000000000000000, 0.9238795325112867385, 1.000000000000000000, 0.9238795325112867385, 1.000000000000000000, 0.9238795325112867385, 1.000000000000000000, 0.9238795325112867385, 1.000000000000000000, 0.9238795325112867385, 1.000000000000000000, 0.9238795325112867385, 1.000000000000000000, 0.9238795325112867385, 1.000000000000000000, 0.9238795325112867385, 1.000000000000000000, 0.9238795325112867385, 1.000000000000000000, 0.9238795325112867385, 1.000000000000000000, 0.9238795325112867385, 1.000000000000000000, 0.9238795325112867385, 1.000000000000000000, 0.9238795325112867385, 1.000000000000000000, 0.9238795325112867385, 1.000000000000000000, 0.9238795325112867385, 1.000000000000000000, 0.9238795325112867385, 1.000000000000000000, 0.9238795325112867385, 1.000000000000000000, 0.9238795325112867385, 1.000000000000000000, 0.9238795325112867385, 1.000000000000000000, 0.9238795325112867385, 1.000000000000000000, 0.9238795325112867385, 1.000000000000000000, 0.9238795325112867385, 1.000000000000000000, 0.9238795325112867385, 1.000000000000000000, 0.9238795325112867385, 1.000000000000000000, 0.9238795325112867385, 1.000000000000000000, 0.9238795325112867385, 1.000000000000000000, 0.9238795325112867385, 1.000000000000000000, 0.9238795325112867385, 1.000000000000000000, 0.9238795325112867385, 1.000000000000000000, 0.9238795325112867385, 1.000000000000000000, 0.9238795325112867385, 1.000000000000000000, 0.9238795325112867385, 1.000000000000000000, 0.9238795325112867385, 1.000000000000000000, 0.9238795325112867385, 1.000000000000000000, 0.9238795325112867385, 1.000000000000000000, 0.9238795325112867385, 1.000000000000000000, 0.9238795325112867385, 1.000000000000000000, 0.9238795325112867385, 1.000000000000000000, 0.9238795325112867385, 1.000000000000000000, 0.9238795325112867385, 1.000000000000000000, 0.9238795325112867385, 1.000000000000000000, 0.9238795325112867385, 1.000000000000000000, 0.9238795325112867385, 1.000000000000000000, 0.9238795325112867385, 1.000000000000000000, 0.9238795325112867385, 1.000000000000000000, 0.9238795325112867385, 1.000000000000000000, 0.9238795325112867385, 1.000000000000000000, 0.9238795325112867385, 1.000000000000000000, 0.9238795325112867385, 1.000000000000000000, 0.9238795325112867385, 1.000000000000000000, 0.9238795325112867385, 1.000000000000000000, 0.9238795325112867385, 1.000000000000000000, 0.9238795325112867385, 1.000000000000000000, 0.9238795325112867385, 1.000000000000000000, 0.9238795325112867385, 1.000000000000000000, 0.9238795325112867385, 1.000000000000000000, 0.9238795325112867385, 1.000000000000000000, 0.9238795325112867385, 1.000000000000000000, 0.9238795325112867385, 1.000000000000000000, 0.9238795325112867385, 1.000000000000000000, 0.9238795325112867385, 1.000000000000000000, 0.9238795325112867385, 1.000000000000000000, 0.9238795325112867385, 1.000000000000000000, 0.9238795325112867385, 1.000000000000000000, 0.9238795325112867385, 1.000000000000000000, 0.9238795325112867385, 1.000000000000000000, 0.9238795325112867385, 1.000000000000000000, 0.9238795325112867385, 1.000000000000000000, 0.9238795325112867385, 1.000000000000000000, 0.9238795325112867385, 1.000000000000000000, 0.9238795325112867385, 1.000000000000000000, 0.9238795325112867385, 1.000000000000000000, 0.9238795325112867385, 1.000000000000000000, 0.9238795325112867385, 1.000000000000000000, 0.9238795325112867385, 1.000000000000000000, 0.9238795325112867385, 1.000000000000000000, 0.9238795325112867385, 1.000000000000000000, 0.9238795325112867385, 1.000000000000000000, 0.9238795325112867385, 1.000000000000000000, 0.9238795325112867385, 1.000000000000000000, 0.9238795325112867385, 1.000000000000000000, 0.9238795325112867385, 1.000000000000000000, 0.9238795325112867385, 1.000000000000000000, 0.9238795325112867385, 1.000000000000000000, 0.9238795325112867385, 1.000000000000000000, 0.9238795325112867385, 1.000000000000000000, 0.9238795325112867385, 1.000000000000000000) ) ) 
 REPRESENTATION_ITEM ( '' )  SURFACE ( )  );
#33645 = ORIENTED_EDGE ( 'NONE', *, *, #2713, .F. ) ;
#33646 = DIRECTION ( 'NONE',  ( 0.000000000000000000, 1.000000000000000000, 0.000000000000000000 ) ) ;
#33647 = CARTESIAN_POINT ( 'NONE',  ( -2.229367062499996610, -97.14583333196773651, 3.861377020970582219 ) ) ;
#33648 = CARTESIAN_POINT ( 'NONE',  ( 3.535533905932736864, -167.2500000027312126, 3.535533905932738641 ) ) ;
#33649 = CARTESIAN_POINT ( 'NONE',  ( -3.152548672688508926E-16, -92.81249999863439371, -5.148502694627439702 ) ) ;
#33650 = AXIS2_PLACEMENT_3D ( 'NONE', #17617, #18556, #3455 ) ;
#33651 = CARTESIAN_POINT ( 'NONE',  ( -2.499999999999996447, -54.70833333060213732, 4.330127018922195425 ) ) ;
#33652 = CARTESIAN_POINT ( 'NONE',  ( 2.500000000000002220, -5.666666666666666963, 4.330127018922192761 ) ) ;
#33653 = CARTESIAN_POINT ( 'NONE',  ( -59.29741812935640155, -131.6250000013655779, -2.196230717870135685 ) ) ;
#33654 = CARTESIAN_POINT ( 'NONE',  ( -53.51423613279429503, -147.2500000013656063, 4.591703134518083651 ) ) ;
#33655 = CARTESIAN_POINT ( 'NONE',  ( -2.229367062500000163, -15.47916666530107399, -3.861377020970580443 ) ) ;
#33656 = CARTESIAN_POINT ( 'NONE',  ( 4.458734125000001214, 9.854166668032263487, 2.574251347313718519 ) ) ;
#33657 = CARTESIAN_POINT ( 'NONE',  ( -4.458734124999999437, -60.56249999863440081, 0.000000000000000000 ) ) ;
#33658 = CARTESIAN_POINT ( 'NONE',  ( 0.000000000000000000, -120.0000000000000000, 0.000000000000000000 ) ) ;
#33659 = CARTESIAN_POINT ( 'NONE',  ( -4.458734124999999437, -15.31249999863440436, 0.000000000000000000 ) ) ;
#33660 = CARTESIAN_POINT ( 'NONE',  ( 5.000000000000000000, -71.50000000000000000, -6.123233995736766282E-16 ) ) ;
#33661 = ORIENTED_EDGE ( 'NONE', *, *, #30819, .F. ) ;
#33662 = CARTESIAN_POINT ( 'NONE',  ( -4.458734124999999437, -43.56249999863440081, 0.000000000000000000 ) ) ;
#33663 = CARTESIAN_POINT ( 'NONE',  ( -56.48576386720575471, -125.0000000013656205, -4.591703134518078322 ) ) ;
#33664 = CARTESIAN_POINT ( 'NONE',  ( -4.999999999999998224, -24.91666666666666430, 2.886751345948131764 ) ) ;
#33665 = CARTESIAN_POINT ( 'NONE',  ( 9.457646018065525792E-16, -84.06249999863439371, 5.148502694627439702 ) ) ;
#33666 = CARTESIAN_POINT ( 'NONE',  ( -4.458734124999999437, 19.35416666803225993, -2.574251347313719407 ) ) ;
#33667 = CARTESIAN_POINT ( 'NONE',  ( -2.229367062499996610, 10.85416666803225993, 3.861377020970582219 ) ) ;
#33668 = FACE_OUTER_BOUND ( 'NONE', #23732, .T. ) ;
#33669 = CARTESIAN_POINT ( 'NONE',  ( -2.500000000000000444, 11.83333333333333037, -4.330127018922193649 ) ) ;
#33670 = FACE_OUTER_BOUND ( 'NONE', #30291, .T. ) ;
#33671 = CARTESIAN_POINT ( 'NONE',  ( -2.500000000000000444, -68.16666666666667140, -4.330127018922193649 ) ) ;
#33672 = CARTESIAN_POINT ( 'NONE',  ( 5.000000000000000000, 14.62500000273118594, -6.123233995736766282E-16 ) ) ;
#33673 = ORIENTED_EDGE ( 'NONE', *, *, #26905, .F. ) ;
#33674 = CARTESIAN_POINT ( 'NONE',  ( 5.000000000000000000, -79.50000000000000000, -6.123233995736766282E-16 ) ) ;
#33675 = ORIENTED_EDGE ( 'NONE', *, *, #4797, .F. ) ;
#33676 = CARTESIAN_POINT ( 'NONE',  ( -51.75738570946856498, -144.8750000027312126, 3.805975901505576964 ) ) ;
#33678 = CARTESIAN_POINT ( 'NONE',  ( 2.499999999999998668, -28.33333333333333570, -4.330127018922193649 ) ) ;
#33677 = CARTESIAN_POINT ( 'NONE',  ( -1.339745962155610925, -103.7946581987385173, 5.000000000000000000 ) ) ;
#33679 = CARTESIAN_POINT ( 'NONE',  ( -2.229367062499996610, -31.14583333196773651, 3.861377020970582219 ) ) ;
#33680 = EDGE_CURVE ( 'NONE', #30949, #54038, #11982, .T. ) ;
#33681 = CARTESIAN_POINT ( 'NONE',  ( 1.060575238724906964E-15, -33.62499999726880873, 5.773502691896257311 ) ) ;
#33683 = VERTEX_POINT ( 'NONE', #41521 ) ;
#33682 = CARTESIAN_POINT ( 'NONE',  ( 9.457646018065525792E-16, -66.06249999863440792, 5.148502694627439702 ) ) ;
#33684 = CARTESIAN_POINT ( 'NONE',  ( -54.64476657466781973, -152.0625000013656063, -4.444560631937228834 ) ) ;
#33686 = VERTEX_POINT ( 'NONE', #11305 ) ;
#33685 = CARTESIAN_POINT ( 'NONE',  ( -2.229367062499996610, -14.39583333196774184, 3.861377020970582219 ) ) ;
#33687 = CARTESIAN_POINT ( 'NONE',  ( 5.000000000000000000, -75.50000000000000000, -6.123233995736766282E-16 ) ) ;
#33688 = DIRECTION ( 'NONE',  ( 7.709882115452476194E-16, -0.000000000000000000, 1.000000000000000000 ) ) ;
#33689 = CARTESIAN_POINT ( 'NONE',  ( 2.229367062500001939, -59.22916666530106511, 3.861377020970579999 ) ) ;
#33690 = VECTOR ( 'NONE', #52566, 1000.000000000000000 ) ;
#33691 =( BOUNDED_CURVE ( )  B_SPLINE_CURVE ( 2, ( #58395, #49371, #49044, #4667, #38757, #20430, #497, #14323, #14633 ),
 .UNSPECIFIED., .F., .F. ) 
 B_SPLINE_CURVE_WITH_KNOTS ( ( 3, 2, 2, 2, 3 ),
 ( 0.7562499999999999778, 0.7569444444444444198, 0.7583333333333333037, 0.7597222222222221877, 0.7604166666666666297 ),
 .UNSPECIFIED. ) 
 CURVE ( )  GEOMETRIC_REPRESENTATION_ITEM ( )  RATIONAL_B_SPLINE_CURVE ( ( 0.9330127018922194093, 0.9330127018922194093, 1.000000000000000000, 0.8660254037844387076, 1.000000000000000000, 0.8660254037844387076, 1.000000000000000000, 0.9330127018922194093, 0.9330127018922194093 ) ) 
 REPRESENTATION_ITEM ( '' )  );
#33692 = CARTESIAN_POINT ( 'NONE',  ( 2.499999999999998668, -84.20833333060214443, -4.330127018922193649 ) ) ;
#33694 = ORIENTED_EDGE ( 'NONE', *, *, #13101, .F. ) ;
#33693 = CARTESIAN_POINT ( 'NONE',  ( -1.339745962155610925, 10.33034180399266333, 5.000000000000000000 ) ) ;
#33695 = CARTESIAN_POINT ( 'NONE',  ( -55.39835681537999790, -146.8750000000000284, 4.984105922594378235 ) ) ;
#33696 = VECTOR ( 'NONE', #53358, 1000.000000000000000 ) ;
#33697 = CARTESIAN_POINT ( 'NONE',  ( 4.458734125000001214, -22.14583333196773296, 2.574251347313718519 ) ) ;
#33699 = ORIENTED_EDGE ( 'NONE', *, *, #34579, .F. ) ;
#33698 = CARTESIAN_POINT ( 'NONE',  ( 4.458734124999998549, -59.97916666530107221, -2.574251347313721627 ) ) ;
#33700 = CARTESIAN_POINT ( 'NONE',  ( 1.846868145590736310, -164.8750000013655779, 4.458734124999999437 ) ) ;
#33701 = CARTESIAN_POINT ( 'NONE',  ( 4.458734125000001214, -105.1458333319677365, 2.574251347313718519 ) ) ;
#33702 = CARTESIAN_POINT ( 'NONE',  ( -60.14911071818854538, -135.1875000027312126, 1.666127454062681146 ) ) ;
#33703 = ORIENTED_EDGE ( 'NONE', *, *, #29034, .T. ) ;
#33704 = CARTESIAN_POINT ( 'NONE',  ( -50.40829686548195099, -152.2500000013656063, -1.485763867205728284 ) ) ;
#33705 = CARTESIAN_POINT ( 'NONE',  ( -58.80597590150559739, -138.1250000027312410, 3.242614290531460330 ) ) ;
#33706 = CARTESIAN_POINT ( 'NONE',  ( -2.229367062499996610, -36.14583333196773651, 3.861377020970582219 ) ) ;
#33707 = CARTESIAN_POINT ( 'NONE',  ( 5.000000000000000000, -83.41666666666667140, -2.886751345948130876 ) ) ;
#33708 = CARTESIAN_POINT ( 'NONE',  ( -4.458734124999999437, -15.31249999863440436, 0.000000000000000000 ) ) ;
#33709 = VECTOR ( 'NONE', #38690, 1000.000000000000000 ) ;
#33710 = CARTESIAN_POINT ( 'NONE',  ( 4.458734125000000326, -102.1458333319677365, 2.574251347313718519 ) ) ;
#33711 = CARTESIAN_POINT ( 'NONE',  ( -8.190561711645485556E-16, -145.9375000013656063, 4.458734124999999437 ) ) ;
#33712 = CARTESIAN_POINT ( 'NONE',  ( -4.458734124999998549, -27.47916666530106866, 2.574251347313722516 ) ) ;
#33713 = CARTESIAN_POINT ( 'NONE',  ( 1.975475456537005874E-15, 12.24999999999999822, 5.000000000000000000 ) ) ;
#33714 = CARTESIAN_POINT ( 'NONE',  ( -55.35523342533222291, -131.3125000013656063, 4.444560631937231499 ) ) ;
#33715 = CARTESIAN_POINT ( 'NONE',  ( 4.458734125000001214, -68.14583333196773651, 2.574251347313718519 ) ) ;
#33716 = CARTESIAN_POINT ( 'NONE',  ( -4.999999999999998224, -15.91666666666666963, 2.886751345948131764 ) ) ;
#33717 = CARTESIAN_POINT ( 'NONE',  ( -6.972266317189433020E-16, -4.249999999999997335, -5.000000000000000000 ) ) ;
#33718 = CARTESIAN_POINT ( 'NONE',  ( 3.152801135295367541, -142.3125000013655779, -3.152801135295367541 ) ) ;
#33719 = CARTESIAN_POINT ( 'NONE',  ( -4.458734124999999437, 6.437500001365593860, 0.000000000000000000 ) ) ;
#33720 = VERTEX_POINT ( 'NONE', #26425 ) ;
#33721 = SURFACE_STYLE_FILL_AREA ( #44311 ) ;
#33722 = CARTESIAN_POINT ( 'NONE',  ( -6.972266317189433020E-16, 0.7499999999999996669, -5.000000000000000000 ) ) ;
#33724 = CARTESIAN_POINT ( 'NONE',  ( 4.458734124999999437, -29.81249999863440436, -5.460374474430324690E-16 ) ) ;
#33723 = CARTESIAN_POINT ( 'NONE',  ( 2.499999999999998668, -93.33333333333332860, -4.330127018922193649 ) ) ;
#33725 = DIRECTION ( 'NONE',  ( -0.000000000000000000, 1.000000000000000000, -0.000000000000000000 ) ) ;
#33726 = CARTESIAN_POINT ( 'NONE',  ( 2.229367062499998831, -77.89583333196773651, -3.861377020970580887 ) ) ;
#33727 = CARTESIAN_POINT ( 'NONE',  ( -3.152548672688508926E-16, 21.18750000136559208, -5.148502694627439702 ) ) ;
#33728 = CYLINDRICAL_SURFACE ( 'NONE', #47929, 5.000000000000000000 ) ;
#33729 = CARTESIAN_POINT ( 'NONE',  ( -51.60603307380591787, -139.9375000013656063, -2.891590998281053704 ) ) ;
#33730 = CARTESIAN_POINT ( 'NONE',  ( -3.152548672688508926E-16, 5.437500001365592084, -5.148502694627439702 ) ) ;
#33731 = CARTESIAN_POINT ( 'NONE',  ( 2.229367062499998831, 28.10416666803225993, -3.861377020970580887 ) ) ;
#33732 = CARTESIAN_POINT ( 'NONE',  ( 4.458734124999998549, -42.97916666530107932, -2.574251347313721627 ) ) ;
#33733 = CARTESIAN_POINT ( 'NONE',  ( 5.000000000000000888, -80.58333333333332860, 2.886751345948126879 ) ) ;
#33734 = CARTESIAN_POINT ( 'NONE',  ( 4.458734125000000326, 3.104166668032260379, 2.574251347313718519 ) ) ;
#33735 = CARTESIAN_POINT ( 'NONE',  ( -3.152548672688508926E-16, -23.81249999863440792, -5.148502694627439702 ) ) ;
#33736 = AXIS2_PLACEMENT_3D ( 'NONE', #43659, #22257, #8098 ) ;
#33737 = CARTESIAN_POINT ( 'NONE',  ( 2.730187237215162345E-16, -157.1875000013655779, -4.458734124999999437 ) ) ;
#33738 = CARTESIAN_POINT ( 'NONE',  ( 2.229367062500001939, -68.97916666530107932, 3.861377020970579999 ) ) ;
#33739 = CARTESIAN_POINT ( 'NONE',  ( 5.000000000000000000, -107.3749999972687874, -6.123233995736766282E-16 ) ) ;
#33740 = AXIS2_PLACEMENT_3D ( 'NONE', #2545, #26664, #42946 ) ;
#33741 = CARTESIAN_POINT ( 'NONE',  ( -53.33387254593725402, -148.8125000000000000, 5.149110718188524949 ) ) ;
#33742 = CARTESIAN_POINT ( 'NONE',  ( -55.00000000000001421, -155.0000000000000284, -8.082903768654752241 ) ) ;
#33743 = CARTESIAN_POINT ( 'NONE',  ( -4.458734124999999437, -104.6458333319677365, -2.574251347313719407 ) ) ;
#33744 = CARTESIAN_POINT ( 'NONE',  ( -4.458734124999999437, -74.56249999863440792, 0.000000000000000000 ) ) ;
#33745 = CARTESIAN_POINT ( 'NONE',  ( -2.500000000000000444, -52.16666666666666430, -4.330127018922193649 ) ) ;
#33746 = CARTESIAN_POINT ( 'NONE',  ( 2.499999999999998668, -73.33333333333332860, -4.330127018922193649 ) ) ;
#33747 = CARTESIAN_POINT ( 'NONE',  ( 1.062108568985190270E-13, -11.12499999726881761, -4.999999999999999112 ) ) ;
#33748 = ORIENTED_EDGE ( 'NONE', *, *, #21656, .T. ) ;
#33749 = CYLINDRICAL_SURFACE ( 'NONE', #21221, 5.000000000000000000 ) ;
#33750 = CARTESIAN_POINT ( 'NONE',  ( 1.339745962155615144, -27.58034179853028789, 4.999999999999999112 ) ) ;
#33751 = CARTESIAN_POINT ( 'NONE',  ( -2.499999999999996447, -10.83333333333333393, 4.330127018922195425 ) ) ;
#33752 = CARTESIAN_POINT ( 'NONE',  ( -2.229367062500000163, -19.47916666530106866, -3.861377020970580443 ) ) ;
#33753 = ADVANCED_FACE ( 'NONE', ( #55389 ), #32196, .T. ) ;
#33754 = CARTESIAN_POINT ( 'NONE',  ( -3.152548672688508926E-16, -75.56249999863440792, -5.148502694627439702 ) ) ;
#33755 = CARTESIAN_POINT ( 'NONE',  ( 3.152801135295367541, -168.5625000013656063, -3.152801135295367541 ) ) ;
#33756 = CARTESIAN_POINT ( 'NONE',  ( -3.535250795749689387E-16, -19.12499999726881228, -5.773502691896257311 ) ) ;
#33758 = ORIENTED_EDGE ( 'NONE', *, *, #5250, .F. ) ;
#33757 = CARTESIAN_POINT ( 'NONE',  ( 4.458734124999998549, -43.72916666530106511, -2.574251347313721627 ) ) ;
#33759 = CARTESIAN_POINT ( 'NONE',  ( -6.972266317189433020E-16, -45.12499999726880162, -5.000000000000000000 ) ) ;
#33761 = ORIENTED_EDGE ( 'NONE', *, *, #52869, .T. ) ;
#33760 = CARTESIAN_POINT ( 'NONE',  ( 4.458734124999999437, 2.937500001365594304, -5.460374474430324690E-16 ) ) ;
#33762 = CARTESIAN_POINT ( 'NONE',  ( -50.70258187064364108, -154.1250000013656063, 2.196230717870141014 ) ) ;
#33763 = CARTESIAN_POINT ( 'NONE',  ( -4.999999999999999112, -62.91666666666667140, 2.886751345948131764 ) ) ;
#33764 = CARTESIAN_POINT ( 'NONE',  ( 2.730187237215162345E-16, -154.4375000013655779, -4.458734124999999437 ) ) ;
#33765 = CARTESIAN_POINT ( 'NONE',  ( 2.229367062499998831, -42.89583333196773651, -3.861377020970580887 ) ) ;
#33766 = CARTESIAN_POINT ( 'NONE',  ( -1.339745962155613812, -79.20534180126146850, -5.000000000000000000 ) ) ;
#33767 = CARTESIAN_POINT ( 'NONE',  ( 3.535533905932738197, -160.8750000000000284, -3.535533905932738197 ) ) ;
#33768 = EDGE_CURVE ( 'NONE', #7216, #33686, #41100, .T. ) ;
#33769 = CARTESIAN_POINT ( 'NONE',  ( -4.458734124999998549, -90.22916666530106511, 2.574251347313722516 ) ) ;
#33770 = CARTESIAN_POINT ( 'NONE',  ( -53.51423613279429503, -125.5000000013656205, 4.591703134518082763 ) ) ;
#33771 = CARTESIAN_POINT ( 'NONE',  ( -2.229367062499996610, -7.395833331967735624, 3.861377020970582219 ) ) ;
#33772 = CARTESIAN_POINT ( 'NONE',  ( -4.458734124999999437, -43.64583333196774362, -2.574251347313719407 ) ) ;
#33773 =( BOUNDED_CURVE ( )  B_SPLINE_CURVE ( 2, ( #48888, #57623, #14161, #63076, #63387, #58554, #28642, #14474, #4833 ),
 .UNSPECIFIED., .F., .F. ) 
 B_SPLINE_CURVE_WITH_KNOTS ( ( 3, 2, 2, 2, 3 ),
 ( 0.9589285714285714635, 0.9595238095238095566, 0.9607142857142857428, 0.9619047619047619291, 0.9625000000000000222 ),
 .UNSPECIFIED. ) 
 CURVE ( )  GEOMETRIC_REPRESENTATION_ITEM ( )  RATIONAL_B_SPLINE_CURVE ( ( 0.9330127018922194093, 0.9330127018922194093, 1.000000000000000000, 0.8660254037844387076, 1.000000000000000000, 0.8660254037844387076, 1.000000000000000000, 0.9330127018922194093, 0.9330127018922194093 ) ) 
 REPRESENTATION_ITEM ( '' )  );
#33774 = LINE ( 'NONE', #37345, #55259 ) ;
#33775 = CARTESIAN_POINT ( 'NONE',  ( 4.458734124999999437, -147.4375000013656063, 0.000000000000000000 ) ) ;
#33776 = EDGE_CURVE ( 'NONE', #25237, #47640, #40721, .T. ) ;
#33777 = CARTESIAN_POINT ( 'NONE',  ( -2.229367062499996610, -88.39583333196773651, 3.861377020970582219 ) ) ;
#33778 = CARTESIAN_POINT ( 'NONE',  ( 2.500000000000002220, -34.54166666393547303, 4.330127018922192761 ) ) ;
#33779 = ORIENTED_EDGE ( 'NONE', *, *, #31305, .T. ) ;
#33780 = CARTESIAN_POINT ( 'NONE',  ( -5.000000000000000000, -47.08333333333333570, -2.886751345948128211 ) ) ;
#33781 = PRODUCT_DEFINITION_SHAPE ( 'NONE', 'NONE',  #50832 ) ;
#33782 = CARTESIAN_POINT ( 'NONE',  ( -52.53715891517739323, -152.5625000027312126, -4.819101127000233298 ) ) ;
#33783 = AXIS2_PLACEMENT_3D ( 'NONE', #48693, #49658, #24580 ) ;
#33784 = FACE_OUTER_BOUND ( 'NONE', #26026, .T. ) ;
#33785 = VECTOR ( 'NONE', #27616, 1000.000000000000000 ) ;
#33786 = VERTEX_POINT ( 'NONE', #6819 ) ;
#33787 = FACE_OUTER_BOUND ( 'NONE', #8299, .T. ) ;
#33788 = CARTESIAN_POINT ( 'NONE',  ( 2.229367062500001939, -10.22916666530106866, 3.861377020970579999 ) ) ;
#33789 = CARTESIAN_POINT ( 'NONE',  ( -6.972266317189433020E-16, -35.25000000000000000, -5.000000000000000000 ) ) ;
#33790 = CARTESIAN_POINT ( 'NONE',  ( 4.458734124999999437, -3.812499998634408360, -5.460374474430324690E-16 ) ) ;
#33791 = CARTESIAN_POINT ( 'NONE',  ( 2.500000000000002220, -30.54166666393548013, 4.330127018922192761 ) ) ;
#33792 = CARTESIAN_POINT ( 'NONE',  ( 4.458734124999999437, -152.3750000013655779, -1.846868145590734978 ) ) ;
#33793 = CARTESIAN_POINT ( 'NONE',  ( -4.458734124999997661, 23.52083333469892779, 2.574251347313722516 ) ) ;
#33794 = ORIENTED_EDGE ( 'NONE', *, *, #24697, .F. ) ;
#33795 = CARTESIAN_POINT ( 'NONE',  ( -2.229367062500000163, -91.47916666530106511, -3.861377020970580443 ) ) ;
#33796 = DIRECTION ( 'NONE',  ( 0.000000000000000000, 0.000000000000000000, -1.000000000000000000 ) ) ;
#33797 = CARTESIAN_POINT ( 'NONE',  ( 9.457646018065525792E-16, -14.06249999863440259, 5.148502694627439702 ) ) ;
#33798 = CARTESIAN_POINT ( 'NONE',  ( 0.000000000000000000, -170.0000000000000000, 0.000000000000000000 ) ) ;
#33799 = CARTESIAN_POINT ( 'NONE',  ( -1.339745962155613812, -13.20534180126147916, -5.000000000000000000 ) ) ;
#33800 = CARTESIAN_POINT ( 'NONE',  ( -59.59170313451811296, -153.5000000013656063, 1.485763867205729394 ) ) ;
#33801 = EDGE_CURVE ( 'NONE', #25201, #26022, #55960, .T. ) ;
#33802 = CARTESIAN_POINT ( 'NONE',  ( 2.500000000000002220, -43.54166666393548013, 4.330127018922192761 ) ) ;
#33803 = CARTESIAN_POINT ( 'NONE',  ( 0.000000000000000000, -170.0000000000000000, 5.000000000000000000 ) ) ;
#33804 = CARTESIAN_POINT ( 'NONE',  ( 4.458734125000000326, 17.10416666803225993, 2.574251347313718519 ) ) ;
#33805 = CARTESIAN_POINT ( 'NONE',  ( -4.999999999999998224, 12.20833333606451632, 2.886751345948131764 ) ) ;
#33806 = ORIENTED_EDGE ( 'NONE', *, *, #14941, .T. ) ;
#33807 = CARTESIAN_POINT ( 'NONE',  ( -4.458734124999999437, 19.68750000136559208, 0.000000000000000000 ) ) ;
#33808 = CARTESIAN_POINT ( 'NONE',  ( -2.229367062499996610, -61.14583333196774362, 3.861377020970582219 ) ) ;
#33809 = CARTESIAN_POINT ( 'NONE',  ( 9.457646018065525792E-16, -9.312499998634406140, 5.148502694627439702 ) ) ;
#33810 = DIRECTION ( 'NONE',  ( 0.000000000000000000, 0.000000000000000000, 1.000000000000000000 ) ) ;
#33811 = CARTESIAN_POINT ( 'NONE',  ( -5.000000000000000000, 9.916666666666667851, -2.886751345948128211 ) ) ;
#33812 = CARTESIAN_POINT ( 'NONE',  ( -3.152801135295367096, -166.0625000013656063, -3.152801135295367541 ) ) ;
#33813 = CARTESIAN_POINT ( 'NONE',  ( -2.229367062500000163, -53.47916666530107221, -3.861377020970580443 ) ) ;
#33814 = CARTESIAN_POINT ( 'NONE',  ( -5.000000000000000000, -86.87499999726880162, 0.000000000000000000 ) ) ;
#33815 = CARTESIAN_POINT ( 'NONE',  ( -50.55543936806279248, -136.3125000013656063, 0.3552334253322060320 ) ) ;
#33816 = CARTESIAN_POINT ( 'NONE',  ( 0.000000000000000000, -120.0000000000000000, 0.000000000000000000 ) ) ;
#33817 = CYLINDRICAL_SURFACE ( 'NONE', #40858, 5.000000000000000000 ) ;
#33818 = CARTESIAN_POINT ( 'NONE',  ( -4.458734124999999437, -88.64583333196773651, -2.574251347313719407 ) ) ;
#33819 = CARTESIAN_POINT ( 'NONE',  ( -8.190561711645485556E-16, -152.9375000013655779, 4.458734124999999437 ) ) ;
#33820 =( BOUNDED_CURVE ( )  B_SPLINE_CURVE ( 2, ( #32526, #37047, #27073, #56676, #52154, #32847, #56361, #52475, #51835 ),
 .UNSPECIFIED., .F., .F. ) 
 B_SPLINE_CURVE_WITH_KNOTS ( ( 3, 2, 2, 2, 3 ),
 ( 0.6083333333333329485, 0.6124999999999997113, 0.6166666666666663632, 0.6208333333333330151, 0.6249999999999996669 ),
 .UNSPECIFIED. ) 
 CURVE ( )  GEOMETRIC_REPRESENTATION_ITEM ( )  RATIONAL_B_SPLINE_CURVE ( ( 1.000000000000005995, 0.9238795325112806323, 1.000000000000000000, 0.9238795325112867385, 1.000000000000000000, 0.9238795325112867385, 1.000000000000000000, 0.9238795325112928447, 0.9999999999999938938 ) ) 
 REPRESENTATION_ITEM ( '' )  );
#33821 = CARTESIAN_POINT ( 'NONE',  ( -3.535250795749689387E-16, -37.25000000000001421, -5.773502691896257311 ) ) ;
#33822 = CARTESIAN_POINT ( 'NONE',  ( -53.33387254593710480, -139.8125000000000284, 5.149110718188539160 ) ) ;
#33823 = CARTESIAN_POINT ( 'NONE',  ( -6.972266317189433020E-16, -22.24999999999999645, -5.000000000000000000 ) ) ;
#33824 = ORIENTED_EDGE ( 'NONE', *, *, #3224, .T. ) ;
#33825 = CARTESIAN_POINT ( 'NONE',  ( 4.458734125000001214, -99.89583333196772230, 2.574251347313718519 ) ) ;
#33826 = CARTESIAN_POINT ( 'NONE',  ( -3.152548672688508926E-16, 10.18750000136559564, -5.148502694627439702 ) ) ;
#33827 = CONICAL_SURFACE ( 'NONE', #61582, 5.000000000000001776, 0.9599310885968795892 ) ;
#33828 = CARTESIAN_POINT ( 'NONE',  ( 2.071067811865391572, -161.8125000000000568, -5.000000000000086153 ) ) ;
#33829 = CARTESIAN_POINT ( 'NONE',  ( -2.500000000000000444, 2.833333333333333481, -4.330127018922193649 ) ) ;
#33830 = AXIS2_PLACEMENT_3D ( 'NONE', #14903, #54477, #15228 ) ;
#33831 = CARTESIAN_POINT ( 'NONE',  ( -4.458734124999997661, -62.22916666530105090, 2.574251347313722516 ) ) ;
#33832 = DIRECTION ( 'NONE',  ( 0.000000000000000000, 0.000000000000000000, 1.000000000000000000 ) ) ;
#33833 = EDGE_CURVE ( 'NONE', #58981, #50402, #5788, .T. ) ;
#33834 = EDGE_CURVE ( 'NONE', #49482, #44442, #23461, .T. ) ;
#33835 = CARTESIAN_POINT ( 'NONE',  ( -5.000000000000000000, -0.9583333306021485365, -2.886751345948128211 ) ) ;
#33836 = CARTESIAN_POINT ( 'NONE',  ( 2.229367062499998831, -28.64583333196774007, -3.861377020970580887 ) ) ;
#33837 = CARTESIAN_POINT ( 'NONE',  ( -2.500000000000000444, -48.04166666393547303, -4.330127018922193649 ) ) ;
#33838 = CARTESIAN_POINT ( 'NONE',  ( 5.000000000000000888, -19.58333333333333215, 2.886751345948126879 ) ) ;
#33839 = CARTESIAN_POINT ( 'NONE',  ( 1.060575238724906964E-15, -45.75000000000000000, 5.773502691896257311 ) ) ;
#33841 = CARTESIAN_POINT ( 'NONE',  ( -2.229367062500000163, -24.72916666530106866, -3.861377020970580443 ) ) ;
#33840 = CARTESIAN_POINT ( 'NONE',  ( -2.500000000000000444, 23.95833333606451987, -4.330127018922193649 ) ) ;
#33842 = CARTESIAN_POINT ( 'NONE',  ( -62.00000000000001421, -135.0000000000000284, -4.041451884327373456 ) ) ;
#33843 = CARTESIAN_POINT ( 'NONE',  ( -3.152548672688508926E-16, -69.56249999863439371, -5.148502694627439702 ) ) ;
#33844 = CARTESIAN_POINT ( 'NONE',  ( 3.152801135295366208, -143.8125000013655779, 3.152801135295367985 ) ) ;
#33845 = CARTESIAN_POINT ( 'NONE',  ( 9.457646018065525792E-16, -74.06249999863440792, 5.148502694627439702 ) ) ;
#33846 = CARTESIAN_POINT ( 'NONE',  ( -53.51423613279429503, -138.5000000013656347, 4.591703134518082763 ) ) ;
#33847 = EDGE_CURVE ( 'NONE', #29077, #2195, #18566, .T. ) ;
#33848 = CARTESIAN_POINT ( 'NONE',  ( 9.457646018065525792E-16, -23.31249999863440436, 5.148502694627439702 ) ) ;
#33849 = CARTESIAN_POINT ( 'NONE',  ( 2.499999999999998668, -67.20833333060214443, -4.330127018922193649 ) ) ;
#33850 = ORIENTED_EDGE ( 'NONE', *, *, #59513, .F. ) ;
#33851 = CARTESIAN_POINT ( 'NONE',  ( -58.80597590150559739, -148.1250000027312126, 3.242614290531460330 ) ) ;
#33853 = VERTEX_POINT ( 'NONE', #27691 ) ;
#33852 = EDGE_CURVE ( 'NONE', #19310, #54895, #56350, .T. ) ;
#33854 = CARTESIAN_POINT ( 'NONE',  ( 4.458734124999998549, -70.97916666530107932, -2.574251347313721627 ) ) ;
#33855 = DIRECTION ( 'NONE',  ( -0.000000000000000000, 1.000000000000000000, -0.000000000000000000 ) ) ;
#33856 = ORIENTED_EDGE ( 'NONE', *, *, #44875, .T. ) ;
#33857 = CARTESIAN_POINT ( 'NONE',  ( -6.972266317189433020E-16, 16.74999999999999645, -5.000000000000000000 ) ) ;
#33858 = CARTESIAN_POINT ( 'NONE',  ( -6.972266317189433020E-16, -83.24999999999998579, -5.000000000000000000 ) ) ;
#33859 = CARTESIAN_POINT ( 'NONE',  ( -4.458734124999999437, -61.56249999863440081, 0.000000000000000000 ) ) ;
#33860 = CARTESIAN_POINT ( 'NONE',  ( 9.457646018065525792E-16, 1.687500001365593194, 5.148502694627439702 ) ) ;
#33861 = ORIENTED_EDGE ( 'NONE', *, *, #51246, .T. ) ;
#33862 = CARTESIAN_POINT ( 'NONE',  ( -1.339745962155613812, -20.20534180126147916, -5.000000000000000000 ) ) ;
#33863 = CARTESIAN_POINT ( 'NONE',  ( -5.000000000000000000, -22.95833333060214798, -2.886751345948128211 ) ) ;
#33864 = CARTESIAN_POINT ( 'NONE',  ( 2.229367062499998831, 12.35416666803226171, -3.861377020970580887 ) ) ;
#33865 = CARTESIAN_POINT ( 'NONE',  ( -52.80376928212989185, -143.8750000013655779, -4.297418129356379346 ) ) ;
#33866 = CARTESIAN_POINT ( 'NONE',  ( 5.000000000000000888, 20.54166666939784847, 2.886751345948126879 ) ) ;
#33867 = CARTESIAN_POINT ( 'NONE',  ( -3.152801135295367985, -164.8125000013656063, 3.152801135295367096 ) ) ;
#33868 =( BOUNDED_CURVE ( )  B_SPLINE_CURVE ( 2, ( #45747, #11637, #31258, #50892, #57934, #9339, #52159, #62450, #28953 ),
 .UNSPECIFIED., .F., .F. ) 
 B_SPLINE_CURVE_WITH_KNOTS ( ( 3, 2, 2, 2, 3 ),
 ( 0.2910714285714285920, 0.2916666666666666852, 0.2928571428571428714, 0.2940476190476190577, 0.2946428571428571508 ),
 .UNSPECIFIED. ) 
 CURVE ( )  GEOMETRIC_REPRESENTATION_ITEM ( )  RATIONAL_B_SPLINE_CURVE ( ( 0.9330127018922194093, 0.9330127018922194093, 1.000000000000000000, 0.8660254037844387076, 1.000000000000000000, 0.8660254037844387076, 1.000000000000000000, 0.9330127018922194093, 0.9330127018922194093 ) ) 
 REPRESENTATION_ITEM ( '' )  );
#33869 = ORIENTED_EDGE ( 'NONE', *, *, #25268, .T. ) ;
#33870 = CARTESIAN_POINT ( 'NONE',  ( -4.458734124999997661, -74.22916666530106511, 2.574251347313722516 ) ) ;
#33871 = CARTESIAN_POINT ( 'NONE',  ( -5.000000000000000000, -69.95833333060214443, -2.886751345948128211 ) ) ;
#33872 = CARTESIAN_POINT ( 'NONE',  ( -2.229367062500000163, 4.520833334698926897, -3.861377020970580443 ) ) ;
#33873 = CYLINDRICAL_SURFACE ( 'NONE', #56216, 5.000000000000000000 ) ;
#33874 = CARTESIAN_POINT ( 'NONE',  ( 2.229367062499998831, -64.89583333196773651, -3.861377020970580887 ) ) ;
#33875 = CARTESIAN_POINT ( 'NONE',  ( -2.500000000000000444, -25.04166666393547658, -4.330127018922193649 ) ) ;
#33876 = CARTESIAN_POINT ( 'NONE',  ( -52.53715891517739323, -142.5625000027311557, -4.819101127000233298 ) ) ;
#33877 = CARTESIAN_POINT ( 'NONE',  ( 1.975475456537005874E-15, -44.62499999726880162, 5.000000000000000000 ) ) ;
#33878 = CARTESIAN_POINT ( 'NONE',  ( -1.339745962155613812, -59.20534180126148271, -5.000000000000000000 ) ) ;
#33879 = CARTESIAN_POINT ( 'NONE',  ( 3.061616997868383141E-16, -156.7500000000000000, -5.000000000000000000 ) ) ;
#33880 = CARTESIAN_POINT ( 'NONE',  ( 4.458734125000001214, -39.89583333196772941, 2.574251347313718519 ) ) ;
#33881 = CARTESIAN_POINT ( 'NONE',  ( -4.458734124999997661, -25.47916666530106866, 2.574251347313722516 ) ) ;
#33882 = CARTESIAN_POINT ( 'NONE',  ( 4.458734124999999437, 7.937500001365595637, -5.460374474430324690E-16 ) ) ;
#33883 = CARTESIAN_POINT ( 'NONE',  ( 0.000000000000000000, -120.0000000000000000, 0.000000000000000000 ) ) ;
#33884 = CARTESIAN_POINT ( 'NONE',  ( 2.500000000000002220, 23.33333333333333215, 4.330127018922192761 ) ) ;
#33885 = CARTESIAN_POINT ( 'NONE',  ( -2.071067811865478170, -150.4375000027312126, 5.000000000000000000 ) ) ;
#33886 = CARTESIAN_POINT ( 'NONE',  ( 1.162044386198238837E-16, 29.25000000000000000, 5.000000000000000000 ) ) ;
#33887 = CARTESIAN_POINT ( 'NONE',  ( 4.458734124999999437, -37.81249999863440792, -5.460374474430324690E-16 ) ) ;
#33888 = CARTESIAN_POINT ( 'NONE',  ( -2.499999999999996447, -66.70833333060214443, 4.330127018922195425 ) ) ;
#33889 = CARTESIAN_POINT ( 'NONE',  ( -51.60603307380591787, -148.1875000013656063, -2.891590998281053704 ) ) ;
#33890 = CARTESIAN_POINT ( 'NONE',  ( 5.000000000000000000, -142.0625000000000000, 2.071067811865478614 ) ) ;
#33891 = CARTESIAN_POINT ( 'NONE',  ( 2.229367062499998831, -75.89583333196773651, -3.861377020970580887 ) ) ;
#33892 = CARTESIAN_POINT ( 'NONE',  ( 1.846868145590735200, -166.5000000013655779, -4.458734124999999437 ) ) ;
#33893 = CARTESIAN_POINT ( 'NONE',  ( 2.229367062499998831, -28.64583333196774007, -3.861377020970580887 ) ) ;
#33894 = CYLINDRICAL_SURFACE ( 'NONE', #48171, 5.000000000000000000 ) ;
#33895 = CARTESIAN_POINT ( 'NONE',  ( -1.336351044127974539E-14, 22.37500000273118417, 5.000000000000000000 ) ) ;
#33896 = CARTESIAN_POINT ( 'NONE',  ( 1.060575238724906964E-15, -20.74999999999999645, 5.773502691896257311 ) ) ;
#33897 = CARTESIAN_POINT ( 'NONE',  ( 1.846868145590735200, -145.2500000013655779, -4.458734125000000326 ) ) ;
#33898 = ORIENTED_EDGE ( 'NONE', *, *, #23689, .F. ) ;
#33899 = CARTESIAN_POINT ( 'NONE',  ( -4.458734124999998549, 27.52083333469892779, 2.574251347313722516 ) ) ;
#33900 = CARTESIAN_POINT ( 'NONE',  ( 1.975475456537005874E-15, 8.249999999999998224, 5.000000000000000000 ) ) ;
#33901 = CARTESIAN_POINT ( 'NONE',  ( 9.457646018065525792E-16, -54.31249999863440792, 5.148502694627439702 ) ) ;
#33902 = CARTESIAN_POINT ( 'NONE',  ( -6.972266317189433020E-16, -27.12499999726881228, -5.000000000000000000 ) ) ;
#33903 = CARTESIAN_POINT ( 'NONE',  ( 3.061616997868383141E-16, -162.7500000000000000, -5.000000000000000000 ) ) ;
#33904 = CARTESIAN_POINT ( 'NONE',  ( 2.499999999999998668, 20.66666666666666785, -4.330127018922193649 ) ) ;
#33905 = LINE ( 'NONE', #48384, #50970 ) ;
#33906 = CARTESIAN_POINT ( 'NONE',  ( 9.457646018065525792E-16, -8.062499998634404363, 5.148502694627439702 ) ) ;
#33907 = CARTESIAN_POINT ( 'NONE',  ( -4.999999999999998224, 4.083333333333334814, 2.886751345948131764 ) ) ;
#33908 = EDGE_CURVE ( 'NONE', #51679, #35740, #63061, .T. ) ;
#33909 = LINE ( 'NONE', #19747, #48151 ) ;
#33910 = FACE_OUTER_BOUND ( 'NONE', #60038, .T. ) ;
#33911 = VECTOR ( 'NONE', #30711, 1000.000000000000000 ) ;
#33912 = CARTESIAN_POINT ( 'NONE',  ( -2.229367062499996610, -20.14583333196774007, 3.861377020970582219 ) ) ;
#33913 = CARTESIAN_POINT ( 'NONE',  ( 2.500000000000002220, 0.3333333333333348136, 4.330127018922192761 ) ) ;
#33914 = CARTESIAN_POINT ( 'NONE',  ( -4.458734124999999437, -52.39583333196773651, -2.574251347313719407 ) ) ;
#33915 = CARTESIAN_POINT ( 'NONE',  ( -4.458734124999999437, -155.1875000013655779, -5.460374474430324690E-16 ) ) ;
#33916 = VECTOR ( 'NONE', #35489, 1000.000000000000000 ) ;
#33917 = CARTESIAN_POINT ( 'NONE',  ( -4.999999999999999112, -50.79166666393547303, 2.886751345948131764 ) ) ;
#33918 = ORIENTED_EDGE ( 'NONE', *, *, #46424, .T. ) ;
#33919 = CARTESIAN_POINT ( 'NONE',  ( 9.457646018065525792E-16, 4.687500001365596525, 5.148502694627439702 ) ) ;
#33920 = ORIENTED_EDGE ( 'NONE', *, *, #18499, .T. ) ;
#33922 = CARTESIAN_POINT ( 'NONE',  ( 1.339745962155670655, -9.169658196007338447, -4.999999999999966249 ) ) ;
#33921 = CARTESIAN_POINT ( 'NONE',  ( 1.975475456537005874E-15, -4.749999999999999112, 5.000000000000000000 ) ) ;
#33923 = CARTESIAN_POINT ( 'NONE',  ( -3.152801135295367985, -159.8125000013656063, 3.152801135295367096 ) ) ;
#33924 = EDGE_CURVE ( 'NONE', #32996, #27913, #28628, .T. ) ;
#33925 = VERTEX_POINT ( 'NONE', #18973 ) ;
#33926 = UNCERTAINTY_MEASURE_WITH_UNIT (LENGTH_MEASURE( 1.000000000000000082E-05 ), #27925, 'distance_accuracy_value', 'NONE');
#33927 = EDGE_CURVE ( 'NONE', #3130, #13190, #33774, .T. ) ;
#33928 = CARTESIAN_POINT ( 'NONE',  ( 0.000000000000000000, -120.0000000000000000, 0.000000000000000000 ) ) ;
#33929 = CARTESIAN_POINT ( 'NONE',  ( -56.66612745406270335, -132.3125000000000284, -5.149110718188516067 ) ) ;
#33930 = CARTESIAN_POINT ( 'NONE',  ( 1.975475456537005874E-15, -47.62499999726880873, 5.000000000000000000 ) ) ;
#33931 = CARTESIAN_POINT ( 'NONE',  ( -4.458734124999998549, -43.47916666530106511, 2.574251347313722516 ) ) ;
#33932 = VERTEX_POINT ( 'NONE', #8087 ) ;
#33933 = EDGE_CURVE ( 'NONE', #733, #54901, #48562, .T. ) ;
#33934 = CARTESIAN_POINT ( 'NONE',  ( 1.339745962155612702, -103.1696581960073331, -5.000000000000000000 ) ) ;
#33935 = CARTESIAN_POINT ( 'NONE',  ( 2.229367062500001939, 19.02083333469892779, 3.861377020970579999 ) ) ;
#33936 = LINE ( 'NONE', #28164, #3007 ) ;
#33937 = EDGE_LOOP ( 'NONE', ( #14279, #34001, #28557, #8268 ) ) ;
#33938 = CARTESIAN_POINT ( 'NONE',  ( -2.229367062500000163, -85.72916666530107932, -3.861377020970580443 ) ) ;
#33939 = CARTESIAN_POINT ( 'NONE',  ( -57.46284108482265651, -126.0625000027312268, 4.819101127000239515 ) ) ;
#33940 = CARTESIAN_POINT ( 'NONE',  ( 1.339745962155615144, -35.58034179853028434, 4.999999999999999112 ) ) ;
#33941 = CARTESIAN_POINT ( 'NONE',  ( -6.972266317189433020E-16, -100.2499999999999858, -5.000000000000000000 ) ) ;
#33942 = CARTESIAN_POINT ( 'NONE',  ( 3.535533905932738197, -168.8750000000000284, -3.535533905932738197 ) ) ;
#33943 = CARTESIAN_POINT ( 'NONE',  ( -4.458734124999999437, -61.31249999863440081, 0.000000000000000000 ) ) ;
#33944 = CARTESIAN_POINT ( 'NONE',  ( 0.000000000000000000, -170.0000000000000000, 0.000000000000000000 ) ) ;
#33945 = CARTESIAN_POINT ( 'NONE',  ( 4.458734124999999437, 18.18750000136559564, -5.460374474430324690E-16 ) ) ;
#33946 =( BOUNDED_CURVE ( )  B_SPLINE_CURVE ( 2, ( #12354, #9645, #63067, #38592, #53712, #33780, #37125, #63379, #48567 ),
 .UNSPECIFIED., .F., .F. ) 
 B_SPLINE_CURVE_WITH_KNOTS ( ( 3, 2, 2, 2, 3 ),
 ( 0.5482142857142857650, 0.5488095238095238582, 0.5500000000000000444, 0.5511904761904762307, 0.5517857142857143238 ),
 .UNSPECIFIED. ) 
 CURVE ( )  GEOMETRIC_REPRESENTATION_ITEM ( )  RATIONAL_B_SPLINE_CURVE ( ( 0.9330127018922194093, 0.9330127018922194093, 1.000000000000000000, 0.8660254037844387076, 1.000000000000000000, 0.8660254037844387076, 1.000000000000000000, 0.9330127018922194093, 0.9330127018922194093 ) ) 
 REPRESENTATION_ITEM ( '' )  );
#33947 = CARTESIAN_POINT ( 'NONE',  ( 2.500000000000002220, -102.5416666639354588, 4.330127018922192761 ) ) ;
#33948 = CARTESIAN_POINT ( 'NONE',  ( -1.339745962155610925, -81.79465819873850307, 5.000000000000000000 ) ) ;
#33949 = CARTESIAN_POINT ( 'NONE',  ( -4.458734124999999437, -50.64583333196773651, -2.574251347313719407 ) ) ;
#33950 = CARTESIAN_POINT ( 'NONE',  ( -5.000000000000000000, -1.874999997268814944, 0.000000000000000000 ) ) ;
#33951 = DIRECTION ( 'NONE',  ( -0.000000000000000000, 1.000000000000000000, -0.000000000000000000 ) ) ;
#33952 = CYLINDRICAL_SURFACE ( 'NONE', #21424, 5.000000000000000000 ) ;
#33953 = CARTESIAN_POINT ( 'NONE',  ( 4.458734124999999437, -86.06249999863439371, -5.460374474430324690E-16 ) ) ;
#33954 = CARTESIAN_POINT ( 'NONE',  ( 9.457646018065525792E-16, -110.0624999986343937, 5.148502694627439702 ) ) ;
#33955 = CARTESIAN_POINT ( 'NONE',  ( -4.458734124999999437, -10.56249999863440792, 0.000000000000000000 ) ) ;
#33956 = EDGE_LOOP ( 'NONE', ( #43963, #30774, #37190, #11529 ) ) ;
#33957 = CARTESIAN_POINT ( 'NONE',  ( -5.000000000000000888, -155.5625000027311842, 2.071067811865474617 ) ) ;
#33958 = CARTESIAN_POINT ( 'NONE',  ( 2.229367062500001939, -95.97916666530105090, 3.861377020970579999 ) ) ;
#33959 = CARTESIAN_POINT ( 'NONE',  ( 5.000000000000000888, -163.0625000027311842, -2.071067811865475505 ) ) ;
#33960 = CARTESIAN_POINT ( 'NONE',  ( 4.458734124999998549, -90.97916666530106511, -2.574251347313721627 ) ) ;
#33961 = CARTESIAN_POINT ( 'NONE',  ( -5.000000000000000000, 21.91666666666666785, -2.886751345948128211 ) ) ;
#33962 = CARTESIAN_POINT ( 'NONE',  ( -2.500000000000000444, -53.04166666393548013, -4.330127018922193649 ) ) ;
#33963 = CARTESIAN_POINT ( 'NONE',  ( -5.000000000000000000, -30.08333333333332860, -2.886751345948128211 ) ) ;
#33964 = CARTESIAN_POINT ( 'NONE',  ( -51.60603307380591787, -128.9375000013656063, -2.891590998281053704 ) ) ;
#33965 =( BOUNDED_CURVE ( )  B_SPLINE_CURVE ( 2, ( #55805, #45827, #11721, #36492, #50653, #8726, #31338, #47643, #57631 ),
 .UNSPECIFIED., .F., .F. ) 
 B_SPLINE_CURVE_WITH_KNOTS ( ( 3, 2, 2, 2, 3 ),
 ( 0.1517857142857143016, 0.1523809523809523947, 0.1535714285714285809, 0.1547619047619047672, 0.1553571428571428603 ),
 .UNSPECIFIED. ) 
 CURVE ( )  GEOMETRIC_REPRESENTATION_ITEM ( )  RATIONAL_B_SPLINE_CURVE ( ( 0.9330127018922194093, 0.9330127018922209636, 1.000000000000000000, 0.8660254037844387076, 1.000000000000000000, 0.8660254037844387076, 1.000000000000000000, 0.9330127018922194093, 0.9330127018922194093 ) ) 
 REPRESENTATION_ITEM ( '' )  );
#33966 = CARTESIAN_POINT ( 'NONE',  ( -51.60603307380591787, -144.9375000013656063, -2.891590998281053704 ) ) ;
#33967 = CARTESIAN_POINT ( 'NONE',  ( -3.152548672688508926E-16, -16.56249999863440436, -5.148502694627439702 ) ) ;
#33968 = CARTESIAN_POINT ( 'NONE',  ( 2.229367062500001939, 13.77083333469892779, 3.861377020970579999 ) ) ;
#33969 = CARTESIAN_POINT ( 'NONE',  ( -4.458734124999999437, -56.64583333196773651, -2.574251347313719407 ) ) ;
#33970 = CARTESIAN_POINT ( 'NONE',  ( -2.500000000000000444, -20.16666666666666430, -4.330127018922193649 ) ) ;
#33971 = CARTESIAN_POINT ( 'NONE',  ( -4.458734124999999437, -16.31249999863440436, 0.000000000000000000 ) ) ;
#33972 = DIRECTION ( 'NONE',  ( 0.000000000000000000, 0.000000000000000000, 1.000000000000000000 ) ) ;
#33973 = CARTESIAN_POINT ( 'NONE',  ( 3.535533905932738197, -156.8750000000000284, -3.535533905932738197 ) ) ;
#33974 = EDGE_LOOP ( 'NONE', ( #39938, #47942, #31004, #57829 ) ) ;
#33975 = CARTESIAN_POINT ( 'NONE',  ( -2.229367062499996610, -40.39583333196773651, 3.861377020970582219 ) ) ;
#33976 = DIRECTION ( 'NONE',  ( -0.000000000000000000, 1.000000000000000000, -0.000000000000000000 ) ) ;
#33977 = CARTESIAN_POINT ( 'NONE',  ( 0.3470952277635277472, 8.860649561028097310, -7.493596212620242447 ) ) ;
#33978 = CARTESIAN_POINT ( 'NONE',  ( -6.972266317189433020E-16, -25.24999999999999645, -5.000000000000000000 ) ) ;
#33979 = CARTESIAN_POINT ( 'NONE',  ( 4.458734125000001214, -85.89583333196773651, 2.574251347313718519 ) ) ;
#33980 = CARTESIAN_POINT ( 'NONE',  ( 2.229367062499998831, 18.10416666803225993, -3.861377020970580887 ) ) ;
#33982 = EDGE_CURVE ( 'NONE', #15736, #41952, #30009, .T. ) ;
#33981 = CARTESIAN_POINT ( 'NONE',  ( 4.458734124999999437, 8.187500001365595637, -5.460374474430324690E-16 ) ) ;
#33983 = CARTESIAN_POINT ( 'NONE',  ( 6.123233995736766282E-16, -120.0000000000000000, -5.000000000000000000 ) ) ;
#33984 = CYLINDRICAL_SURFACE ( 'NONE', #3994, 5.000000000000000000 ) ;
#33985 = CARTESIAN_POINT ( 'NONE',  ( -6.972266317189433020E-16, 20.87500000273118062, -5.000000000000000000 ) ) ;
#33986 = CARTESIAN_POINT ( 'NONE',  ( -3.152548672688508926E-16, 18.18750000136559564, -5.148502694627439702 ) ) ;
#33987 = CARTESIAN_POINT ( 'NONE',  ( 5.000000000000000888, -72.58333333333334281, 2.886751345948126879 ) ) ;
#33988 = CARTESIAN_POINT ( 'NONE',  ( -3.535250795749689387E-16, 15.87500000273118417, -5.773502691896257311 ) ) ;
#33989 = VERTEX_POINT ( 'NONE', #54986 ) ;
#33990 = CARTESIAN_POINT ( 'NONE',  ( 1.975475456537005874E-15, -102.7499999999999858, 5.000000000000000000 ) ) ;
#33991 = ORIENTED_EDGE ( 'NONE', *, *, #43570, .F. ) ;
#33993 = CARTESIAN_POINT ( 'NONE',  ( 5.000000000000000888, -32.58333333333333570, 2.886751345948126879 ) ) ;
#33992 = FACE_OUTER_BOUND ( 'NONE', #10877, .T. ) ;
#33994 = CARTESIAN_POINT ( 'NONE',  ( 2.229367062499998831, -37.64583333196773651, -3.861377020970580887 ) ) ;
#33995 = CARTESIAN_POINT ( 'NONE',  ( -5.000000000000000000, -36.87499999726881583, 0.000000000000000000 ) ) ;
#33997 = ORIENTED_EDGE ( 'NONE', *, *, #5436, .T. ) ;
#33996 = CARTESIAN_POINT ( 'NONE',  ( -4.458734124999999437, -64.31249999863440792, 0.000000000000000000 ) ) ;
#33998 = CARTESIAN_POINT ( 'NONE',  ( -51.60603307380591787, -153.1875000013656063, -2.891590998281053704 ) ) ;
#33999 = CARTESIAN_POINT ( 'NONE',  ( -2.229367062499996610, -13.14583333196774007, 3.861377020970582219 ) ) ;
#34001 = ORIENTED_EDGE ( 'NONE', *, *, #41324, .T. ) ;
#34000 = CARTESIAN_POINT ( 'NONE',  ( 2.229367062500001939, -16.22916666530107577, 3.861377020970579999 ) ) ;
#34002 = CARTESIAN_POINT ( 'NONE',  ( 2.500000000000002220, -76.66666666666665719, 4.330127018922192761 ) ) ;
#34003 = CARTESIAN_POINT ( 'NONE',  ( -6.972266317189433020E-16, -83.12499999726878741, -5.000000000000000000 ) ) ;
#34004 = CARTESIAN_POINT ( 'NONE',  ( -4.458734124999999437, -55.56249999863440081, 0.000000000000000000 ) ) ;
#34005 = CARTESIAN_POINT ( 'NONE',  ( 2.500000000000002220, -84.54166666393547303, 4.330127018922192761 ) ) ;
#34007 = ORIENTED_EDGE ( 'NONE', *, *, #28709, .F. ) ;
#34006 = DIRECTION ( 'NONE',  ( 0.000000000000000000, 0.000000000000000000, 1.000000000000000000 ) ) ;
#34008 = CARTESIAN_POINT ( 'NONE',  ( -52.53715891517739323, -144.4375000000000284, -4.819101127000233298 ) ) ;
#34009 = CARTESIAN_POINT ( 'NONE',  ( 4.458734125000001214, -27.14583333196774717, 2.574251347313718519 ) ) ;
#34010 = VERTEX_POINT ( 'NONE', #10914 ) ;
#34011 = CARTESIAN_POINT ( 'NONE',  ( -4.458734124999999437, -167.1875000013655779, -5.460374474430324690E-16 ) ) ;
#34012 = CARTESIAN_POINT ( 'NONE',  ( 9.457646018065525792E-16, -107.3124999986343937, 5.148502694627439702 ) ) ;
#34013 = CARTESIAN_POINT ( 'NONE',  ( 5.000000000000000888, -50.45833333060213732, 2.886751345948126879 ) ) ;
#34014 = VERTEX_POINT ( 'NONE', #39855 ) ;
#34015 = CARTESIAN_POINT ( 'NONE',  ( -56.48576386720575471, -146.0000000013656347, -4.591703134518078322 ) ) ;
#34016 = CARTESIAN_POINT ( 'NONE',  ( -58.80597590150559739, -140.1250000027312126, 3.242614290531460330 ) ) ;
#34017 = CARTESIAN_POINT ( 'NONE',  ( -3.152548672688508926E-16, -38.56249999863440081, -5.148502694627439702 ) ) ;
#34018 =( BOUNDED_CURVE ( )  B_SPLINE_CURVE ( 2, ( #22144, #57514, #56562, #12165, #13430, #7672, #31784, #47220, #12797 ),
 .UNSPECIFIED., .F., .F. ) 
 B_SPLINE_CURVE_WITH_KNOTS ( ( 3, 2, 2, 2, 3 ),
 ( 0.6482142857142857428, 0.6488095238095238360, 0.6500000000000000222, 0.6511904761904762085, 0.6517857142857143016 ),
 .UNSPECIFIED. ) 
 CURVE ( )  GEOMETRIC_REPRESENTATION_ITEM ( )  RATIONAL_B_SPLINE_CURVE ( ( 0.9330127018922194093, 0.9330127018922194093, 1.000000000000000000, 0.8660254037844387076, 1.000000000000000000, 0.8660254037844387076, 1.000000000000000000, 0.9330127018922194093, 0.9330127018922194093 ) ) 
 REPRESENTATION_ITEM ( '' )  );
#34019 = CARTESIAN_POINT ( 'NONE',  ( -7.922798540899431252, 4.627424769998836673, -8.057412477672047046 ) ) ;
#34020 = CARTESIAN_POINT ( 'NONE',  ( -5.000000000000000000, -2.000000000000001776, 0.000000000000000000 ) ) ;
#34021 = CARTESIAN_POINT ( 'NONE',  ( -4.458734124999999437, -12.31249999863440259, 0.000000000000000000 ) ) ;
#34022 = CARTESIAN_POINT ( 'NONE',  ( -4.458734124999999437, -98.56249999863440792, 0.000000000000000000 ) ) ;
#34023 = VERTEX_POINT ( 'NONE', #14462 ) ;
#34024 = CARTESIAN_POINT ( 'NONE',  ( -3.152801135295367096, -142.3125000013655779, -3.152801135295367541 ) ) ;
#34025 = CARTESIAN_POINT ( 'NONE',  ( -4.458734124999999437, -29.64583333196773651, -2.574251347313719407 ) ) ;
#34026 = CARTESIAN_POINT ( 'NONE',  ( 1.339745962155612702, -70.29465819873850307, -5.000000000000000000 ) ) ;
#34027 = CARTESIAN_POINT ( 'NONE',  ( -56.48576386720575471, -132.7500000013656063, -4.591703134518078322 ) ) ;
#34028 = CARTESIAN_POINT ( 'NONE',  ( 4.458734125000001214, -66.14583333196772230, 2.574251347313718519 ) ) ;
#34029 = CARTESIAN_POINT ( 'NONE',  ( -5.000000000000000000, -91.08333333333334281, -2.886751345948128211 ) ) ;
#34030 = CARTESIAN_POINT ( 'NONE',  ( -50.01589407740564042, -146.7500000027312126, 0.3983568153799778022 ) ) ;
#34031 = CARTESIAN_POINT ( 'NONE',  ( 3.152801135295367541, -140.3125000013655779, -3.152801135295367541 ) ) ;
#34032 = CARTESIAN_POINT ( 'NONE',  ( -4.458734124999997661, 2.520833334698928230, 2.574251347313722516 ) ) ;
#34033 = EDGE_LOOP ( 'NONE', ( #56997, #3254, #57483, #648 ) ) ;
#34034 = LINE ( 'NONE', #24707, #60353 ) ;
#34035 = CARTESIAN_POINT ( 'NONE',  ( 1.975475456537005874E-15, 2.249999999999999556, 5.000000000000000000 ) ) ;
#34037 = CARTESIAN_POINT ( 'NONE',  ( 2.229367062499998831, -28.64583333196774007, -3.861377020970580887 ) ) ;
#34036 = CARTESIAN_POINT ( 'NONE',  ( 5.000000000000000000, -97.41666666666665719, -2.886751345948129988 ) ) ;
#34038 = CARTESIAN_POINT ( 'NONE',  ( 5.000000000000000000, -9.500000000000001776, -6.123233995736766282E-16 ) ) ;
#34039 = CARTESIAN_POINT ( 'NONE',  ( 4.458734125000001214, -77.14583333196775072, 2.574251347313718519 ) ) ;
#34040 = CARTESIAN_POINT ( 'NONE',  ( -2.229367062500000163, 23.27083333469892779, -3.861377020970580443 ) ) ;
#34041 = CARTESIAN_POINT ( 'NONE',  ( -6.972266317189433020E-16, -56.25000000000000000, -5.000000000000000000 ) ) ;
#34042 = CARTESIAN_POINT ( 'NONE',  ( -50.55543936806279248, -142.0625000013656063, 0.3552334253322060320 ) ) ;
#34043 = CARTESIAN_POINT ( 'NONE',  ( -2.229367062499996610, -4.145833331967739177, 3.861377020970582219 ) ) ;
#34044 = CARTESIAN_POINT ( 'NONE',  ( 2.229367062499998831, 25.10416666803225993, -3.861377020970580887 ) ) ;
#34045 = CARTESIAN_POINT ( 'NONE',  ( -4.458734124999997661, -45.47916666530106511, 2.574251347313722516 ) ) ;
#34046 = CARTESIAN_POINT ( 'NONE',  ( -52.53715891517739323, -144.4375000000000000, -4.819101127000233298 ) ) ;
#34047 = CARTESIAN_POINT ( 'NONE',  ( 4.458734124999999437, 3.187500001365594304, -5.460374474430324690E-16 ) ) ;
#34048 = CARTESIAN_POINT ( 'NONE',  ( 4.458734125000000326, -23.14583333196772941, 2.574251347313718519 ) ) ;
#34049 =( BOUNDED_CURVE ( )  B_SPLINE_CURVE ( 2, ( #19990, #19671, #14522, #28687, #38349, #9697, #43790, #24504, #19352 ),
 .UNSPECIFIED., .F., .F. ) 
 B_SPLINE_CURVE_WITH_KNOTS ( ( 3, 2, 2, 2, 3 ),
 ( 0.09375000000000000000, 0.09444444444444444198, 0.09583333333333333981, 0.09722222222222222376, 0.09791666666666666574 ),
 .UNSPECIFIED. ) 
 CURVE ( )  GEOMETRIC_REPRESENTATION_ITEM ( )  RATIONAL_B_SPLINE_CURVE ( ( 0.9330127018922194093, 0.9330127018922194093, 1.000000000000000000, 0.8660254037844387076, 1.000000000000000000, 0.8660254037844387076, 1.000000000000000000, 0.9330127018922194093, 0.9330127018922194093 ) ) 
 REPRESENTATION_ITEM ( '' )  );
#34050 = VECTOR ( 'NONE', #58795, 1000.000000000000000 ) ;
#34051 = CARTESIAN_POINT ( 'NONE',  ( -4.458734124999998549, -67.22916666530106511, 2.574251347313722516 ) ) ;
#34052 = CARTESIAN_POINT ( 'NONE',  ( -2.500000000000000444, -106.0416666639354730, -4.330127018922193649 ) ) ;
#34053 = CARTESIAN_POINT ( 'NONE',  ( 4.458734125000001214, 26.10416666803225993, 2.574251347313718519 ) ) ;
#34054 = DIRECTION ( 'NONE',  ( 0.000000000000000000, 0.000000000000000000, 1.000000000000000000 ) ) ;
#34055 = FACE_OUTER_BOUND ( 'NONE', #59058, .T. ) ;
#34056 = CARTESIAN_POINT ( 'NONE',  ( 4.458734124999998549, -73.97916666530106511, -2.574251347313721627 ) ) ;
#34057 = CARTESIAN_POINT ( 'NONE',  ( 5.000000000000000888, -52.58333333333332860, 2.886751345948126879 ) ) ;
#34058 = FACE_OUTER_BOUND ( 'NONE', #28161, .T. ) ;
#34059 = CARTESIAN_POINT ( 'NONE',  ( -4.999999999999999112, 28.20833333606451632, 2.886751345948131764 ) ) ;
#34060 = ORIENTED_EDGE ( 'NONE', *, *, #28398, .F. ) ;
#34061 = CARTESIAN_POINT ( 'NONE',  ( -2.500000000000000444, -27.16666666666666430, -4.330127018922193649 ) ) ;
#34062 = CARTESIAN_POINT ( 'NONE',  ( 1.975475456537005874E-15, -6.624999997268813168, 5.000000000000000000 ) ) ;
#34063 = CARTESIAN_POINT ( 'NONE',  ( -5.000000000000000000, -16.00000000000000000, 0.000000000000000000 ) ) ;
#34064 = CARTESIAN_POINT ( 'NONE',  ( 2.229367062499998831, -24.64583333196773651, -3.861377020970580887 ) ) ;
#34065 = CARTESIAN_POINT ( 'NONE',  ( 4.458734125000000326, -83.89583333196773651, 2.574251347313718519 ) ) ;
#34066 = CARTESIAN_POINT ( 'NONE',  ( -4.458734125000000326, -168.2500000013656063, -1.846868145590735644 ) ) ;
#34067 = CARTESIAN_POINT ( 'NONE',  ( 2.499999999999998668, -16.20833333060214443, -4.330127018922193649 ) ) ;
#34069 = VERTEX_POINT ( 'NONE', #44683 ) ;
#34068 = CARTESIAN_POINT ( 'NONE',  ( -2.229367062500000163, -52.47916666530107221, -3.861377020970580443 ) ) ;
#34070 = CARTESIAN_POINT ( 'NONE',  ( 1.975475456537005874E-15, -23.75000000000000000, 5.000000000000000000 ) ) ;
#34071 = CARTESIAN_POINT ( 'NONE',  ( 1.975475456537005874E-15, -27.62499999726881228, 5.000000000000000000 ) ) ;
#34073 = ORIENTED_EDGE ( 'NONE', *, *, #42411, .T. ) ;
#34072 = CARTESIAN_POINT ( 'NONE',  ( 2.229367062499998831, 1.104166668032261711, -3.861377020970580887 ) ) ;
#34074 = CARTESIAN_POINT ( 'NONE',  ( -57.89159099828107458, -151.6875000013656063, -3.393966926194107447 ) ) ;
#34075 = CARTESIAN_POINT ( 'NONE',  ( 5.000000000000000000, -59.50000000000000000, -6.123233995736766282E-16 ) ) ;
#34076 = CARTESIAN_POINT ( 'NONE',  ( 1.846868145590735200, -157.5000000013656063, -4.458734125000000326 ) ) ;
#34077 = CARTESIAN_POINT ( 'NONE',  ( -4.458734124999998549, -43.47916666530106511, 2.574251347313722516 ) ) ;
#34078 = DIRECTION ( 'NONE',  ( 0.000000000000000000, -1.000000000000000000, 0.000000000000000000 ) ) ;
#34079 = CARTESIAN_POINT ( 'NONE',  ( -5.000000000000000888, -163.5625000000000284, -2.071067811865475949 ) ) ;
#34080 = DIRECTION ( 'NONE',  ( 0.6485228581062915110, 0.000000000000000000, 0.7611951803011149931 ) ) ;
#34081 = CARTESIAN_POINT ( 'NONE',  ( -52.10840900171896806, -125.4375000013656063, 3.393966926194110556 ) ) ;
#34082 = CARTESIAN_POINT ( 'NONE',  ( 4.458734124999998549, -6.979166665301073103, -2.574251347313721627 ) ) ;
#34083 = CARTESIAN_POINT ( 'NONE',  ( 9.457646018065525792E-16, -48.31249999863440081, 5.148502694627439702 ) ) ;
#34084 = CARTESIAN_POINT ( 'NONE',  ( 2.499999999999998668, -89.33333333333332860, -4.330127018922193649 ) ) ;
#34085 = CARTESIAN_POINT ( 'NONE',  ( -1.846868145590734756, -149.1250000013656063, -4.458734125000000326 ) ) ;
#34086 = CARTESIAN_POINT ( 'NONE',  ( 4.458734125000001214, -89.14583333196775072, 2.574251347313718519 ) ) ;
#34087 = ORIENTED_EDGE ( 'NONE', *, *, #2066, .T. ) ;
#34088 = CARTESIAN_POINT ( 'NONE',  ( -59.81910112700026616, -152.1875000000000568, -2.462841084822585014 ) ) ;
#34089 = CARTESIAN_POINT ( 'NONE',  ( 1.975475456537005874E-15, 11.37500000273118239, 5.000000000000000000 ) ) ;
#34090 = CARTESIAN_POINT ( 'NONE',  ( -59.81910112700025905, -149.3125000027312126, -2.462841084822630311 ) ) ;
#34091 = CARTESIAN_POINT ( 'NONE',  ( 6.123233995736766282E-16, -120.0000000000000000, -5.000000000000000000 ) ) ;
#34092 = ORIENTED_EDGE ( 'NONE', *, *, #22111, .T. ) ;
#34093 = CYLINDRICAL_SURFACE ( 'NONE', #6179, 5.000000000000000000 ) ;
#34094 = CARTESIAN_POINT ( 'NONE',  ( -2.229367062500000163, -13.72916666530107221, -3.861377020970580443 ) ) ;
#34095 = CARTESIAN_POINT ( 'NONE',  ( 1.975475456537005874E-15, -50.75000000000000000, 5.000000000000000000 ) ) ;
#34096 = CARTESIAN_POINT ( 'NONE',  ( 4.458734124999998549, -2.729166665301069550, -2.574251347313721627 ) ) ;
#34097 = CARTESIAN_POINT ( 'NONE',  ( 5.000000000000000000, -55.37499999726880162, -6.123233995736766282E-16 ) ) ;
#34098 = CARTESIAN_POINT ( 'NONE',  ( 1.846868145590736310, -153.6250000013655779, 4.458734124999997661 ) ) ;
#34099 = CARTESIAN_POINT ( 'NONE',  ( -4.458734124999999437, 18.35416666803225993, -2.574251347313719407 ) ) ;
#34100 = ORIENTED_EDGE ( 'NONE', *, *, #6641, .T. ) ;
#34101 = CARTESIAN_POINT ( 'NONE',  ( 9.457646018065525792E-16, -90.06249999863440792, 5.148502694627439702 ) ) ;
#34102 = CARTESIAN_POINT ( 'NONE',  ( 10.39117206796836079, 1.272551561242683567E-15, -8.499999999999998224 ) ) ;
#34103 = CARTESIAN_POINT ( 'NONE',  ( 2.623433461001182909, -7.604994000793866782, -7.633824513837117465 ) ) ;
#34104 = CARTESIAN_POINT ( 'NONE',  ( -2.229367062500000163, -15.47916666530107399, -3.861377020970580443 ) ) ;
#34105 = EDGE_CURVE ( 'NONE', #3623, #22435, #47317, .T. ) ;
#34106 = FACE_OUTER_BOUND ( 'NONE', #63468, .T. ) ;
#34107 = CARTESIAN_POINT ( 'NONE',  ( -2.500000000000000444, -73.16666666666665719, -4.330127018922193649 ) ) ;
#34108 = CARTESIAN_POINT ( 'NONE',  ( -56.48576386720575471, -153.7500000013656063, -4.591703134518078322 ) ) ;
#34109 = CARTESIAN_POINT ( 'NONE',  ( 1.060575238724906964E-15, -42.62499999726880162, 5.773502691896257311 ) ) ;
#34110 = CARTESIAN_POINT ( 'NONE',  ( 0.000000000000000000, -170.0000000000000000, 5.000000000000000000 ) ) ;
#34111 = CARTESIAN_POINT ( 'NONE',  ( 2.229367062499998831, 16.35416666803225993, -3.861377020970580887 ) ) ;
#34112 = CARTESIAN_POINT ( 'NONE',  ( 7.500000000000000000, -4.330127018922199866, -7.422398894150035176 ) ) ;
#34113 = VECTOR ( 'NONE', #43923, 1000.000000000000000 ) ;
#34114 = ORIENTED_EDGE ( 'NONE', *, *, #35116, .T. ) ;
#34115 = CARTESIAN_POINT ( 'NONE',  ( 4.458734124999999437, 18.18750000136559564, -5.460374474430324690E-16 ) ) ;
#34116 = CARTESIAN_POINT ( 'NONE',  ( -4.458734124999999437, -63.39583333196772941, -2.574251347313719407 ) ) ;
#34117 = CARTESIAN_POINT ( 'NONE',  ( 4.458734124999999437, -7.062499998634404363, -5.460374474430324690E-16 ) ) ;
#34118 = CARTESIAN_POINT ( 'NONE',  ( -2.499999999999996447, 8.166666666666666075, 4.330127018922195425 ) ) ;
#34119 = CARTESIAN_POINT ( 'NONE',  ( 1.846868145590736310, -166.6250000013656063, 4.458734124999999437 ) ) ;
#34120 = CARTESIAN_POINT ( 'NONE',  ( 0.000000000000000000, -120.0000000000000000, 0.000000000000000000 ) ) ;
#34121 = CARTESIAN_POINT ( 'NONE',  ( 4.458734125000001214, -54.89583333196773651, 2.574251347313718519 ) ) ;
#34122 = CARTESIAN_POINT ( 'NONE',  ( -3.535250795749689387E-16, -87.12499999726880162, -5.773502691896257311 ) ) ;
#34123 = CYLINDRICAL_SURFACE ( 'NONE', #16483, 5.000000000000000000 ) ;
#34124 = EDGE_CURVE ( 'NONE', #37292, #49211, #34724, .T. ) ;
#34125 = CARTESIAN_POINT ( 'NONE',  ( 5.000000000000000888, 25.54166666939784847, 2.886751345948126879 ) ) ;
#34126 = CARTESIAN_POINT ( 'NONE',  ( 1.975475456537005874E-15, -69.74999999999998579, 5.000000000000000000 ) ) ;
#34127 = EDGE_CURVE ( 'NONE', #59631, #16288, #52197, .T. ) ;
#34128 = CARTESIAN_POINT ( 'NONE',  ( -1.846868145590737420, -152.0000000013656063, 4.458734124999997661 ) ) ;
#34129 = CARTESIAN_POINT ( 'NONE',  ( -5.000000000000000000, -39.99999999999999289, 0.000000000000000000 ) ) ;
#34130 = CARTESIAN_POINT ( 'NONE',  ( 1.339745962155612702, -46.29465819873851729, -5.000000000000000000 ) ) ;
#34131 = CARTESIAN_POINT ( 'NONE',  ( 5.000000000000000888, -162.9375000000000000, -2.071067811865475505 ) ) ;
#34132 = VERTEX_POINT ( 'NONE', #15437 ) ;
#34133 = CARTESIAN_POINT ( 'NONE',  ( 9.457646018065525792E-16, -101.0624999986344079, 5.148502694627439702 ) ) ;
#34134 = CARTESIAN_POINT ( 'NONE',  ( -4.458734124999998549, 2.520833334698928674, 2.574251347313722516 ) ) ;
#34135 = FACE_OUTER_BOUND ( 'NONE', #55005, .T. ) ;
#34136 = CARTESIAN_POINT ( 'NONE',  ( -3.535250795749689387E-16, 4.750000000000000888, -5.773502691896257311 ) ) ;
#34137 = ADVANCED_FACE ( 'NONE', ( #5456 ), #58846, .T. ) ;
#34138 = CARTESIAN_POINT ( 'NONE',  ( 4.458734124999998549, -67.72916666530106511, -2.574251347313721627 ) ) ;
#34139 =( BOUNDED_CURVE ( )  B_SPLINE_CURVE ( 2, ( #56351, #51518, #47003, #27064, #31242, #12581, #41844, #55709, #7456 ),
 .UNSPECIFIED., .F., .F. ) 
 B_SPLINE_CURVE_WITH_KNOTS ( ( 3, 2, 2, 2, 3 ),
 ( 0.8520833333333333037, 0.8527777777777777457, 0.8541666666666666297, 0.8555555555555555136, 0.8562499999999999556 ),
 .UNSPECIFIED. ) 
 CURVE ( )  GEOMETRIC_REPRESENTATION_ITEM ( )  RATIONAL_B_SPLINE_CURVE ( ( 0.9330127018922194093, 0.9330127018922194093, 1.000000000000000000, 0.8660254037844387076, 1.000000000000000000, 0.8660254037844387076, 1.000000000000000000, 0.9330127018922194093, 0.9330127018922194093 ) ) 
 REPRESENTATION_ITEM ( '' )  );
#34140 = CARTESIAN_POINT ( 'NONE',  ( -51.75738570946856498, -153.8750000027312126, 3.805975901505576964 ) ) ;
#34141 = CARTESIAN_POINT ( 'NONE',  ( 5.000000000000000000, -3.291666663935477910, -2.886751345948129988 ) ) ;
#34143 = ORIENTED_EDGE ( 'NONE', *, *, #13457, .F. ) ;
#34142 = CARTESIAN_POINT ( 'NONE',  ( 2.229367062499998831, -33.64583333196772941, -3.861377020970580887 ) ) ;
#34144 = DIRECTION ( 'NONE',  ( -0.000000000000000000, -0.000000000000000000, 1.000000000000000000 ) ) ;
#34145 = CARTESIAN_POINT ( 'NONE',  ( -50.01589407740564042, -136.6250000000000284, 0.3983568153799778022 ) ) ;
#34146 = CARTESIAN_POINT ( 'NONE',  ( 2.499999999999998668, -47.33333333333333570, -4.330127018922193649 ) ) ;
#34148 = CARTESIAN_POINT ( 'NONE',  ( 4.458734124999999437, -26.06249999863440792, -5.460374474430324690E-16 ) ) ;
#34147 = CARTESIAN_POINT ( 'NONE',  ( 1.339745962155615144, 6.419658201469706782, 4.999999999999999112 ) ) ;
#34149 = CARTESIAN_POINT ( 'NONE',  ( 1.339745962155612702, -4.169658196007335782, -5.000000000000000000 ) ) ;
#34150 = CARTESIAN_POINT ( 'NONE',  ( 2.229367062499998831, -69.64583333196773651, -3.861377020970580887 ) ) ;
#34151 = CARTESIAN_POINT ( 'NONE',  ( -8.190561711645485556E-16, -145.9375000013656063, 4.458734124999999437 ) ) ;
#34152 = CARTESIAN_POINT ( 'NONE',  ( 4.458734125000001214, -76.89583333196775072, 2.574251347313718519 ) ) ;
#34153 = CARTESIAN_POINT ( 'NONE',  ( -59.29741812935640155, -138.8750000013655779, -2.196230717870135685 ) ) ;
#34154 = CARTESIAN_POINT ( 'NONE',  ( 2.229367062500001939, -31.22916666530107221, 3.861377020970579999 ) ) ;
#34155 = CARTESIAN_POINT ( 'NONE',  ( -4.999999999999999112, -68.79166666393547303, 2.886751345948131764 ) ) ;
#34156 = VERTEX_POINT ( 'NONE', #9640 ) ;
#34157 = EDGE_CURVE ( 'NONE', #50070, #328, #62535, .T. ) ;
#34158 = CARTESIAN_POINT ( 'NONE',  ( -60.14911071818854538, -148.1875000027312126, 1.666127454062681146 ) ) ;
#34159 = ORIENTED_EDGE ( 'NONE', *, *, #22394, .F. ) ;
#34160 = CARTESIAN_POINT ( 'NONE',  ( -2.229367062499996610, -75.39583333196773651, 3.861377020970582219 ) ) ;
#34161 = CARTESIAN_POINT ( 'NONE',  ( -2.499999999999996447, 29.16666666666666785, 4.330127018922195425 ) ) ;
#34162 = ORIENTED_EDGE ( 'NONE', *, *, #22058, .F. ) ;
#34163 = CARTESIAN_POINT ( 'NONE',  ( -1.339745962155613812, 16.79465819873852084, -5.000000000000000000 ) ) ;
#34164 = CARTESIAN_POINT ( 'NONE',  ( -5.000000000000000000, -77.95833333060214443, -2.886751345948128211 ) ) ;
#34165 = CARTESIAN_POINT ( 'NONE',  ( 9.457646018065525792E-16, -58.31249999863440792, 5.148502694627439702 ) ) ;
#34166 = CARTESIAN_POINT ( 'NONE',  ( -3.152548672688508926E-16, 2.187500001365593416, -5.148502694627439702 ) ) ;
#34167 = ORIENTED_EDGE ( 'NONE', *, *, #62612, .F. ) ;
#34168 = CARTESIAN_POINT ( 'NONE',  ( 1.975475456537005874E-15, -67.74999999999998579, 5.000000000000000000 ) ) ;
#34169 = CARTESIAN_POINT ( 'NONE',  ( -6.972266317189433020E-16, -69.12499999726880162, -5.000000000000000000 ) ) ;
#34170 = CARTESIAN_POINT ( 'NONE',  ( 4.458734124999999437, 14.18750000136559386, -5.460374474430324690E-16 ) ) ;
#34171 = CARTESIAN_POINT ( 'NONE',  ( -56.48576386720575471, -144.7500000013656063, -4.591703134518078322 ) ) ;
#34172 = CARTESIAN_POINT ( 'NONE',  ( -6.972266317189433020E-16, -32.24999999999999289, -5.000000000000000000 ) ) ;
#34173 = CARTESIAN_POINT ( 'NONE',  ( -4.458734125000000326, -164.8750000013656063, 1.846868145590734089 ) ) ;
#34174 = ORIENTED_EDGE ( 'NONE', *, *, #35304, .F. ) ;
#34175 = CARTESIAN_POINT ( 'NONE',  ( -2.229367062500000163, -73.47916666530106511, -3.861377020970580443 ) ) ;
#34176 = CARTESIAN_POINT ( 'NONE',  ( -2.071067811865686448, -153.6874999999999716, -4.999999999999789502 ) ) ;
#34177 = CARTESIAN_POINT ( 'NONE',  ( -4.458734124999999437, 2.687500001365593860, 0.000000000000000000 ) ) ;
#34178 = EDGE_CURVE ( 'NONE', #4714, #6601, #54020, .T. ) ;
#34179 = ADVANCED_FACE ( 'NONE', ( #29569 ), #10282, .T. ) ;
#34180 = CARTESIAN_POINT ( 'NONE',  ( -5.000000000000000888, -162.5625000027312126, 2.071067811865474617 ) ) ;
#34181 = ADVANCED_FACE ( 'NONE', ( #35055 ), #49831, .T. ) ;
#34182 = CARTESIAN_POINT ( 'NONE',  ( -4.458734124999998549, -65.47916666530107932, 2.574251347313722516 ) ) ;
#34183 = CARTESIAN_POINT ( 'NONE',  ( 1.060575238724906964E-15, -26.62499999726881228, 5.773502691896257311 ) ) ;
#34184 = CARTESIAN_POINT ( 'NONE',  ( -59.98410592259440222, -142.1250000000000284, -0.3983568153799752487 ) ) ;
#34185 = CARTESIAN_POINT ( 'NONE',  ( 2.499999999999998668, -44.20833333060214443, -4.330127018922193649 ) ) ;
#34186 = CARTESIAN_POINT ( 'NONE',  ( 1.975475456537005874E-15, -72.62499999726878741, 5.000000000000000000 ) ) ;
#34187 =( BOUNDED_CURVE ( )  B_SPLINE_CURVE ( 2, ( #60702, #41686, #16310, #6982, #36243, #26593, #35931, #55559, #11473 ),
 .UNSPECIFIED., .F., .F. ) 
 B_SPLINE_CURVE_WITH_KNOTS ( ( 3, 2, 2, 2, 3 ),
 ( 0.5583333333333337922, 0.5625000000000004441, 0.5666666666666670960, 0.5708333333333338588, 0.5750000000000005107 ),
 .UNSPECIFIED. ) 
 CURVE ( )  GEOMETRIC_REPRESENTATION_ITEM ( )  RATIONAL_B_SPLINE_CURVE ( ( 0.9999999999999918954, 0.9238795325112948431, 1.000000000000000000, 0.9238795325112867385, 1.000000000000000000, 0.9238795325112867385, 1.000000000000000000, 0.9238795325112766355, 1.000000000000010214 ) ) 
 REPRESENTATION_ITEM ( '' )  );
#34188 = CARTESIAN_POINT ( 'NONE',  ( -4.458734124999998549, -47.22916666530106511, 2.574251347313722516 ) ) ;
#34189 = CARTESIAN_POINT ( 'NONE',  ( -4.458734124999997661, -28.47916666530107221, 2.574251347313722516 ) ) ;
#34190 = CARTESIAN_POINT ( 'NONE',  ( 9.457646018065525792E-16, 5.687500001365592972, 5.148502694627439702 ) ) ;
#34191 = DIRECTION ( 'NONE',  ( 0.000000000000000000, 0.000000000000000000, 1.000000000000000000 ) ) ;
#34192 = CARTESIAN_POINT ( 'NONE',  ( 5.000000000000000000, 26.50000000000000000, -6.123233995736766282E-16 ) ) ;
#34193 = CARTESIAN_POINT ( 'NONE',  ( -9.184850993605147944E-16, -148.3750000027312126, 5.000000000000000000 ) ) ;
#34194 = DIRECTION ( 'NONE',  ( -0.000000000000000000, 1.000000000000000000, -0.000000000000000000 ) ) ;
#34195 = CARTESIAN_POINT ( 'NONE',  ( -4.458734124999999437, -39.39583333196773651, -2.574251347313719407 ) ) ;
#34196 = CARTESIAN_POINT ( 'NONE',  ( 5.000000000000000000, -74.37499999726880162, -6.123233995736766282E-16 ) ) ;
#34197 = CARTESIAN_POINT ( 'NONE',  ( -53.51423613279429503, -143.5000000013656347, 4.591703134518082763 ) ) ;
#34198 = CARTESIAN_POINT ( 'NONE',  ( 3.061616997868383141E-16, -142.7500000000000284, -5.000000000000000000 ) ) ;
#34199 = EDGE_CURVE ( 'NONE', #7022, #26835, #10293, .T. ) ;
#34200 = CARTESIAN_POINT ( 'NONE',  ( -4.458734124999999437, -76.64583333196775072, -2.574251347313719407 ) ) ;
#34201 = CARTESIAN_POINT ( 'NONE',  ( 3.152801135295367541, -167.5625000013656063, -3.152801135295367541 ) ) ;
#34202 = CARTESIAN_POINT ( 'NONE',  ( 4.458734124999998549, -31.72916666530107577, -2.574251347313721627 ) ) ;
#34203 = LINE ( 'NONE', #24243, #34818 ) ;
#34204 = CARTESIAN_POINT ( 'NONE',  ( 5.000000000000000000, -21.41666666666666430, -2.886751345948129988 ) ) ;
#34205 = CARTESIAN_POINT ( 'NONE',  ( -8.190561711645485556E-16, -145.6875000013656063, 4.458734124999999437 ) ) ;
#34206 = ORIENTED_EDGE ( 'NONE', *, *, #12848, .T. ) ;
#34207 = CARTESIAN_POINT ( 'NONE',  ( -5.000000000000000000, -89.87499999726880162, 0.000000000000000000 ) ) ;
#34208 = CARTESIAN_POINT ( 'NONE',  ( -4.458734124999999437, -54.64583333196773651, -2.574251347313719407 ) ) ;
#34209 = CARTESIAN_POINT ( 'NONE',  ( -4.999999999999999112, 27.20833333606451987, 2.886751345948131764 ) ) ;
#34210 = CARTESIAN_POINT ( 'NONE',  ( -5.000000000000000888, -162.5625000000000000, -2.071067811865475949 ) ) ;
#34211 = CARTESIAN_POINT ( 'NONE',  ( 5.000000000000000000, 16.58333333333333215, -2.886751345948129988 ) ) ;
#34212 = DIRECTION ( 'NONE',  ( -0.000000000000000000, 1.000000000000000000, -0.000000000000000000 ) ) ;
#34213 = CARTESIAN_POINT ( 'NONE',  ( 4.458734124999999437, -3.812499998634408360, -5.460374474430324690E-16 ) ) ;
#34214 = CARTESIAN_POINT ( 'NONE',  ( -6.972266317189433020E-16, 3.749999999999999556, -5.000000000000000000 ) ) ;
#34215 = CARTESIAN_POINT ( 'NONE',  ( -5.000000000000000000, -40.95833333060215153, -2.886751345948128211 ) ) ;
#34216 = CARTESIAN_POINT ( 'NONE',  ( -4.999999999999998224, 0.08333333333333454995, 2.886751345948131764 ) ) ;
#34217 = CYLINDRICAL_SURFACE ( 'NONE', #22284, 5.000000000000000000 ) ;
#34219 = CARTESIAN_POINT ( 'NONE',  ( -4.458734124999999437, -23.39583333196773296, -2.574251347313719407 ) ) ;
#34218 = DIRECTION ( 'NONE',  ( -0.000000000000000000, 1.000000000000000000, -0.000000000000000000 ) ) ;
#34220 = CARTESIAN_POINT ( 'NONE',  ( 5.000000000000000000, 0.5833333333333314830, -2.886751345948130876 ) ) ;
#34221 = CARTESIAN_POINT ( 'NONE',  ( -4.458734124999998549, -56.22916666530107221, 2.574251347313722516 ) ) ;
#34222 = CARTESIAN_POINT ( 'NONE',  ( -4.458734124999999437, -154.1875000013656063, -5.460374474430324690E-16 ) ) ;
#34223 = CARTESIAN_POINT ( 'NONE',  ( 5.000000000000000000, -50.29166666393548013, -2.886751345948129988 ) ) ;
#34224 = VERTEX_POINT ( 'NONE', #12506 ) ;
#34225 = CARTESIAN_POINT ( 'NONE',  ( -4.458734124999999437, 3.437500001365594748, 0.000000000000000000 ) ) ;
#34226 = EDGE_LOOP ( 'NONE', ( #56354, #55816, #16221, #29789 ) ) ;
#34227 = CARTESIAN_POINT ( 'NONE',  ( 5.000000000000000000, -56.49999999999999289, -6.123233995736766282E-16 ) ) ;
#34228 = CARTESIAN_POINT ( 'NONE',  ( 4.458734124999999437, -157.5000000013656063, 1.846868145590737864 ) ) ;
#34229 = VERTEX_POINT ( 'NONE', #41447 ) ;
#34230 =( BOUNDED_CURVE ( )  B_SPLINE_CURVE ( 2, ( #45766, #41556, #31924, #2661, #60574, #51552, #59941, #55428, #21328 ),
 .UNSPECIFIED., .F., .F. ) 
 B_SPLINE_CURVE_WITH_KNOTS ( ( 3, 2, 2, 2, 3 ),
 ( 0.3583333333333336146, 0.3625000000000002665, 0.3666666666666669183, 0.3708333333333336257, 0.3750000000000002776 ),
 .UNSPECIFIED. ) 
 CURVE ( )  GEOMETRIC_REPRESENTATION_ITEM ( )  RATIONAL_B_SPLINE_CURVE ( ( 0.9999999999999948930, 0.9238795325112918455, 1.000000000000000000, 0.9238795325112867385, 1.000000000000000000, 0.9238795325112867385, 1.000000000000000000, 0.9238795325112816315, 1.000000000000005107 ) ) 
 REPRESENTATION_ITEM ( '' )  );
#34231 = CARTESIAN_POINT ( 'NONE',  ( -6.972266317189433020E-16, -72.25000000000000000, -5.000000000000000000 ) ) ;
#34232 = CARTESIAN_POINT ( 'NONE',  ( -57.46284108482265651, -133.9375000000000000, 4.819101127000239515 ) ) ;
#34233 = CARTESIAN_POINT ( 'NONE',  ( -55.00000000000002132, 0.000000000000000000, -5.000000000000000000 ) ) ;
#34234 = CARTESIAN_POINT ( 'NONE',  ( 2.229367062500001939, -42.22916666530107932, 3.861377020970579999 ) ) ;
#34235 = ORIENTED_EDGE ( 'NONE', *, *, #59690, .F. ) ;
#34236 = AXIS2_PLACEMENT_3D ( 'NONE', #9261, #32447, #38232 ) ;
#34237 = CARTESIAN_POINT ( 'NONE',  ( -6.972266317189433020E-16, -46.24999999999999289, -5.000000000000000000 ) ) ;
#34238 = CARTESIAN_POINT ( 'NONE',  ( 9.457646018065525792E-16, 18.93750000136559208, 5.148502694627439702 ) ) ;
#34239 = LINE ( 'NONE', #5307, #47159 ) ;
#34240 = ORIENTED_EDGE ( 'NONE', *, *, #21125, .F. ) ;
#34241 = CARTESIAN_POINT ( 'NONE',  ( -4.458734124999999437, 26.60416666803225993, -2.574251347313719407 ) ) ;
#34242 = CARTESIAN_POINT ( 'NONE',  ( -56.66612745406270335, -127.4375000027312126, -5.149110718188516067 ) ) ;
#34243 = CARTESIAN_POINT ( 'NONE',  ( -6.972266317189433020E-16, -4.124999997268814056, -5.000000000000000000 ) ) ;
#34244 = CARTESIAN_POINT ( 'NONE',  ( -2.500000000000000444, -7.166666666666668739, -4.330127018922193649 ) ) ;
#34245 = CARTESIAN_POINT ( 'NONE',  ( -5.000000000000000000, -103.0000000000000142, 0.000000000000000000 ) ) ;
#34246 = CARTESIAN_POINT ( 'NONE',  ( 4.458734124999998549, -60.72916666530106511, -2.574251347313721627 ) ) ;
#34247 = DIRECTION ( 'NONE',  ( 0.000000000000000000, 0.000000000000000000, 1.000000000000000000 ) ) ;
#34248 = CARTESIAN_POINT ( 'NONE',  ( -2.229367062500000163, 16.52083333469892779, -3.861377020970580443 ) ) ;
#34249 = CARTESIAN_POINT ( 'NONE',  ( -2.499999999999996447, 7.166666666666665186, 4.330127018922195425 ) ) ;
#34250 = EDGE_CURVE ( 'NONE', #2012, #16047, #36601, .T. ) ;
#34251 = EDGE_CURVE ( 'NONE', #1553, #48706, #53863, .T. ) ;
#34252 = CARTESIAN_POINT ( 'NONE',  ( -2.229367062499996610, -51.39583333196773651, 3.861377020970582219 ) ) ;
#34253 = CARTESIAN_POINT ( 'NONE',  ( 1.060575238724906964E-15, -9.624999997268814056, 5.773502691896257311 ) ) ;
#34254 = FACE_OUTER_BOUND ( 'NONE', #35497, .T. ) ;
#34255 = CARTESIAN_POINT ( 'NONE',  ( -4.999999999999998224, -19.79166666393548013, 2.886751345948131764 ) ) ;
#34256 = FACE_OUTER_BOUND ( 'NONE', #4697, .T. ) ;
#34257 = ADVANCED_FACE ( 'NONE', ( #36635 ), #1610, .T. ) ;
#34258 = CARTESIAN_POINT ( 'NONE',  ( 4.458734124999998549, -108.7291666653010651, -2.574251347313721627 ) ) ;
#34259 = CARTESIAN_POINT ( 'NONE',  ( -3.152548672688508926E-16, -10.81249999863440792, -5.148502694627439702 ) ) ;
#34260 = ORIENTED_EDGE ( 'NONE', *, *, #30358, .F. ) ;
#34261 = CARTESIAN_POINT ( 'NONE',  ( -6.972266317189433020E-16, -17.12499999726881583, -5.000000000000000000 ) ) ;
#34262 = CARTESIAN_POINT ( 'NONE',  ( 4.458734124999998549, -97.72916666530106511, -2.574251347313721627 ) ) ;
#34263 = CARTESIAN_POINT ( 'NONE',  ( 3.061616997868383141E-16, -160.8750000027311842, -5.000000000000000000 ) ) ;
#34264 = CARTESIAN_POINT ( 'NONE',  ( -3.152548672688508926E-16, -97.81249999863439371, -5.148502694627439702 ) ) ;
#34265 = CARTESIAN_POINT ( 'NONE',  ( 1.975475456537005874E-15, -94.62499999726880162, 5.000000000000000000 ) ) ;
#34267 = EDGE_CURVE ( 'NONE', #41892, #9483, #60474, .T. ) ;
#34266 = CARTESIAN_POINT ( 'NONE',  ( 2.500000000000002220, -56.54166666393548013, 4.330127018922192761 ) ) ;
#34268 = CARTESIAN_POINT ( 'NONE',  ( 2.499999999999998668, -5.333333333333335702, -4.330127018922193649 ) ) ;
#34269 = ADVANCED_FACE ( 'NONE', ( #26671 ), #16388, .T. ) ;
#34270 = CARTESIAN_POINT ( 'NONE',  ( -59.29741812935640155, -128.6250000013656063, -2.196230717870135685 ) ) ;
#34271 = CARTESIAN_POINT ( 'NONE',  ( -54.64476657466781973, -146.8125000013656063, -4.444560631937228834 ) ) ;
#34272 = CARTESIAN_POINT ( 'NONE',  ( -4.458734124999997661, -17.22916666530106866, 2.574251347313722516 ) ) ;
#34273 = CARTESIAN_POINT ( 'NONE',  ( -2.229367062499996610, 4.604166668032261711, 3.861377020970582219 ) ) ;
#34274 = CARTESIAN_POINT ( 'NONE',  ( 4.458734125000000326, -59.14583333196772230, 2.574251347313718519 ) ) ;
#34275 = CARTESIAN_POINT ( 'NONE',  ( -7.500000000000000000, -4.330127018922198090, -10.00000000000000000 ) ) ;
#34276 = CARTESIAN_POINT ( 'NONE',  ( 2.229367062500001939, -14.97916666530107399, 3.861377020970579999 ) ) ;
#34277 = CARTESIAN_POINT ( 'NONE',  ( 0.000000000000000000, -170.0000000000000000, 0.000000000000000000 ) ) ;
#34278 = CARTESIAN_POINT ( 'NONE',  ( -2.071067811865478170, -153.3125000000000000, 5.000000000000000000 ) ) ;
#34279 = CARTESIAN_POINT ( 'NONE',  ( 2.500000000000002220, -5.666666666666666963, 4.330127018922192761 ) ) ;
#34280 = ADVANCED_FACE ( 'NONE', ( #17336 ), #20898, .T. ) ;
#34281 = VERTEX_POINT ( 'NONE', #21535 ) ;
#34282 = CARTESIAN_POINT ( 'NONE',  ( 4.458734124999998549, -41.97916666530107932, -2.574251347313721627 ) ) ;
#34283 = CARTESIAN_POINT ( 'NONE',  ( -59.59170313451811296, -125.7500000013656347, 1.485763867205729394 ) ) ;
#34284 = EDGE_CURVE ( 'NONE', #32107, #41628, #38291, .T. ) ;
#34285 = CARTESIAN_POINT ( 'NONE',  ( -5.000000000000000000, -9.000000000000001776, 0.000000000000000000 ) ) ;
#34286 = CARTESIAN_POINT ( 'NONE',  ( -5.000000000000000000, -90.87499999726880162, 0.000000000000000000 ) ) ;
#34287 = CARTESIAN_POINT ( 'NONE',  ( -4.458734124999999437, -85.39583333196773651, -2.574251347313719407 ) ) ;
#34288 = CARTESIAN_POINT ( 'NONE',  ( -4.458734124999999437, 20.35416666803225993, -2.574251347313719407 ) ) ;
#34289 = AXIS2_PLACEMENT_3D ( 'NONE', #31582, #47331, #17435 ) ;
#34290 = CARTESIAN_POINT ( 'NONE',  ( 2.229367062500001939, 8.020833334698926009, 3.861377020970579999 ) ) ;
#34291 = CARTESIAN_POINT ( 'NONE',  ( -2.499999999999996447, -43.83333333333333570, 4.330127018922195425 ) ) ;
#34292 = CARTESIAN_POINT ( 'NONE',  ( -6.972266317189433020E-16, -37.12499999726881583, -5.000000000000000000 ) ) ;
#34293 = CARTESIAN_POINT ( 'NONE',  ( -2.229367062500000163, -89.72916666530106511, -3.861377020970580443 ) ) ;
#34294 = CARTESIAN_POINT ( 'NONE',  ( -4.458734124999999437, 23.43750000136559564, 0.000000000000000000 ) ) ;
#34295 = CARTESIAN_POINT ( 'NONE',  ( -5.000000000000000000, -77.08333333333334281, -2.886751345948128211 ) ) ;
#34296 = CARTESIAN_POINT ( 'NONE',  ( -4.999999999999999112, 14.20833333606451809, 2.886751345948131764 ) ) ;
#34297 = EDGE_LOOP ( 'NONE', ( #63313, #24656, #38440, #62596 ) ) ;
#34298 = FACE_OUTER_BOUND ( 'NONE', #11703, .T. ) ;
#34299 = ORIENTED_EDGE ( 'NONE', *, *, #44502, .F. ) ;
#34301 = CARTESIAN_POINT ( 'NONE',  ( 2.499999999999998668, -35.33333333333332860, -4.330127018922193649 ) ) ;
#34300 = CARTESIAN_POINT ( 'NONE',  ( -58.24261429053147765, -148.3750000027312126, -3.805975901505573855 ) ) ;
#34302 = CARTESIAN_POINT ( 'NONE',  ( -4.458734124999999437, -39.39583333196773651, -2.574251347313719407 ) ) ;
#34303 = CARTESIAN_POINT ( 'NONE',  ( -3.535250795749689387E-16, -32.12499999726880873, -5.773502691896257311 ) ) ;
#34305 = ORIENTED_EDGE ( 'NONE', *, *, #38902, .F. ) ;
#34304 = CARTESIAN_POINT ( 'NONE',  ( 4.458734124999998549, -63.72916666530107221, -2.574251347313721627 ) ) ;
#34306 = CARTESIAN_POINT ( 'NONE',  ( -55.35523342533222291, -152.5625000013656063, 4.444560631937231499 ) ) ;
#34307 = CARTESIAN_POINT ( 'NONE',  ( 9.457646018065525792E-16, -15.06249999863440259, 5.148502694627439702 ) ) ;
#34309 = VERTEX_POINT ( 'NONE', #4654 ) ;
#34308 = CARTESIAN_POINT ( 'NONE',  ( -2.229367062499996610, -16.39583333196773651, 3.861377020970582219 ) ) ;
#34310 = CARTESIAN_POINT ( 'NONE',  ( 5.000000000000000888, -80.58333333333332860, 2.886751345948126879 ) ) ;
#34311 = CARTESIAN_POINT ( 'NONE',  ( 1.975475456537005874E-15, 1.375000002731185500, 5.000000000000000000 ) ) ;
#34312 = CARTESIAN_POINT ( 'NONE',  ( 4.458734125000001214, -59.14583333196773651, 2.574251347313718519 ) ) ;
#34313 = CARTESIAN_POINT ( 'NONE',  ( 2.500000000000002220, -81.54166666393547303, 4.330127018922192761 ) ) ;
#34314 = ORIENTED_EDGE ( 'NONE', *, *, #29028, .F. ) ;
#34315 = CARTESIAN_POINT ( 'NONE',  ( -54.60164318462004474, -144.3750000000000284, -4.984105922594373794 ) ) ;
#34316 = CARTESIAN_POINT ( 'NONE',  ( -2.229367062499996610, -26.39583333196774007, 3.861377020970582219 ) ) ;
#34317 = VERTEX_POINT ( 'NONE', #58061 ) ;
#34318 =( BOUNDED_CURVE ( )  B_SPLINE_CURVE ( 2, ( #12669, #34088, #14154, #53398, #7849, #24134, #28633, #42249, #56745 ),
 .UNSPECIFIED., .F., .F. ) 
 B_SPLINE_CURVE_WITH_KNOTS ( ( 3, 2, 2, 2, 3 ),
 ( 0.09166666666666674346, 0.09583333333333342308, 0.1000000000000000888, 0.1041666666666667546, 0.1083333333333334203 ),
 .UNSPECIFIED. ) 
 CURVE ( )  GEOMETRIC_REPRESENTATION_ITEM ( )  RATIONAL_B_SPLINE_CURVE ( ( 0.9999999999999984457, 0.9238795325112882928, 1.000000000000000000, 0.9238795325112867385, 1.000000000000000000, 0.9238795325112867385, 1.000000000000000000, 0.9238795325112851842, 1.000000000000001554 ) ) 
 REPRESENTATION_ITEM ( '' )  );
#34319 = ITEM_DEFINED_TRANSFORMATION ( 'NONE', 'NONE', #25663,  #43054 ) ;
#34320 = CARTESIAN_POINT ( 'NONE',  ( -3.152801135295367985, -167.0625000013656063, 3.152801135295367096 ) ) ;
#34321 = CARTESIAN_POINT ( 'NONE',  ( 2.229367062499998831, -105.8958333319677365, -3.861377020970580887 ) ) ;
#34322 = CARTESIAN_POINT ( 'NONE',  ( 1.339745962155612702, -55.16965819600732601, -5.000000000000000000 ) ) ;
#34323 = ORIENTED_EDGE ( 'NONE', *, *, #48785, .T. ) ;
#34324 = CARTESIAN_POINT ( 'NONE',  ( -55.35523342533222291, -146.5625000013656063, 4.444560631937231499 ) ) ;
#34325 = CARTESIAN_POINT ( 'NONE',  ( -55.39835681537999790, -140.0000000027312126, 4.984105922594378235 ) ) ;
#34326 = CARTESIAN_POINT ( 'NONE',  ( -4.458734124999999437, -37.39583333196773651, -2.574251347313719407 ) ) ;
#34327 = CARTESIAN_POINT ( 'NONE',  ( -3.152801135295367096, -147.3125000013655779, -3.152801135295367541 ) ) ;
#34328 = CARTESIAN_POINT ( 'NONE',  ( -5.000000000000000000, 0.000000000000000000, 0.000000000000000000 ) ) ;
#34329 = CARTESIAN_POINT ( 'NONE',  ( 2.229367062499998831, -11.64583333196774007, -3.861377020970580887 ) ) ;
#34330 = CARTESIAN_POINT ( 'NONE',  ( 2.229367062500001939, -101.2291666653010651, 3.861377020970579999 ) ) ;
#34331 = VERTEX_POINT ( 'NONE', #53553 ) ;
#34332 = VECTOR ( 'NONE', #25060, 1000.000000000000000 ) ;
#34333 =( BOUNDED_CURVE ( )  B_SPLINE_CURVE ( 2, ( #20638, #40244, #59882, #15803, #10966, #50537, #25776, #11602, #20954 ),
 .UNSPECIFIED., .F., .F. ) 
 B_SPLINE_CURVE_WITH_KNOTS ( ( 3, 2, 2, 2, 3 ),
 ( 0.8982142857142857428, 0.8988095238095238360, 0.9000000000000000222, 0.9011904761904762085, 0.9017857142857143016 ),
 .UNSPECIFIED. ) 
 CURVE ( )  GEOMETRIC_REPRESENTATION_ITEM ( )  RATIONAL_B_SPLINE_CURVE ( ( 0.9330127018922194093, 0.9330127018922194093, 1.000000000000000000, 0.8660254037844387076, 1.000000000000000000, 0.8660254037844387076, 1.000000000000000000, 0.9330127018922194093, 0.9330127018922194093 ) ) 
 REPRESENTATION_ITEM ( '' )  );
#34334 = CARTESIAN_POINT ( 'NONE',  ( 4.458734125000000326, -143.6250000013656347, -1.846868145590734978 ) ) ;
#34335 = CARTESIAN_POINT ( 'NONE',  ( -4.458734124999999437, -33.64583333196772941, -2.574251347313719407 ) ) ;
#34336 = CARTESIAN_POINT ( 'NONE',  ( -3.535250795749689387E-16, 6.875000002731186832, -5.773502691896257311 ) ) ;
#34337 = LINE ( 'NONE', #8640, #51985 ) ;
#34338 = CARTESIAN_POINT ( 'NONE',  ( -55.35523342533222291, -134.3125000013656063, 4.444560631937231499 ) ) ;
#34339 = CARTESIAN_POINT ( 'NONE',  ( -3.152548672688508926E-16, -73.81249999863440792, -5.148502694627439702 ) ) ;
#34340 = CARTESIAN_POINT ( 'NONE',  ( 3.061616997868383141E-16, -144.8750000027312126, -5.000000000000000000 ) ) ;
#34341 = LINE ( 'NONE', #38848, #37744 ) ;
#34342 = CARTESIAN_POINT ( 'NONE',  ( 1.339745962155615144, -68.70534180126148271, 4.999999999999999112 ) ) ;
#34343 = CARTESIAN_POINT ( 'NONE',  ( -4.458734124999997661, 6.520833334698930450, 2.574251347313722516 ) ) ;
#34344 = ORIENTED_EDGE ( 'NONE', *, *, #5515, .T. ) ;
#34345 = CARTESIAN_POINT ( 'NONE',  ( 0.000000000000000000, 15.00000000000000000, 0.000000000000000000 ) ) ;
#34347 = CARTESIAN_POINT ( 'NONE',  ( -4.458734124999999437, -30.39583333196773651, -2.574251347313719407 ) ) ;
#34346 = CARTESIAN_POINT ( 'NONE',  ( -2.499999999999996447, -95.83333333333332860, 4.330127018922195425 ) ) ;
#34348 = CARTESIAN_POINT ( 'NONE',  ( 9.457646018065525792E-16, -80.31249999863440792, 5.148502694627439702 ) ) ;
#34349 = CARTESIAN_POINT ( 'NONE',  ( 4.458734125000000326, 24.85416666803225993, 2.574251347313718519 ) ) ;
#34350 = CARTESIAN_POINT ( 'NONE',  ( -2.499999999999996447, 23.29166666939785202, 4.330127018922195425 ) ) ;
#34351 = CARTESIAN_POINT ( 'NONE',  ( -50.70258187064364108, -140.1250000013655779, 2.196230717870141014 ) ) ;
#34352 = CARTESIAN_POINT ( 'NONE',  ( -4.458734124999997661, -0.2291666653010705768, 2.574251347313722516 ) ) ;
#34353 = DIRECTION ( 'NONE',  ( -0.000000000000000000, 1.000000000000000000, -0.000000000000000000 ) ) ;
#34354 = CARTESIAN_POINT ( 'NONE',  ( -4.458734124999999437, -45.64583333196774362, -2.574251347313719407 ) ) ;
#34355 = CARTESIAN_POINT ( 'NONE',  ( 2.229367062500001939, 4.020833334698926009, 3.861377020970579999 ) ) ;
#34356 = ORIENTED_EDGE ( 'NONE', *, *, #51074, .F. ) ;
#34357 = CARTESIAN_POINT ( 'NONE',  ( -4.458734124999999437, -24.56249999863440436, 0.000000000000000000 ) ) ;
#34358 = CARTESIAN_POINT ( 'NONE',  ( -2.229367062499996610, -70.14583333196773651, 3.861377020970582219 ) ) ;
#34359 = CARTESIAN_POINT ( 'NONE',  ( 5.000000000000000888, -103.4583333306021444, 2.886751345948126879 ) ) ;
#34360 = CARTESIAN_POINT ( 'NONE',  ( -3.152548672688508926E-16, 25.43750000136559208, -5.148502694627439702 ) ) ;
#34361 = EDGE_CURVE ( 'NONE', #50557, #60346, #29627, .T. ) ;
#34362 = CARTESIAN_POINT ( 'NONE',  ( -5.000000000000000000, -65.08333333333332860, -2.886751345948128211 ) ) ;
#34363 = DIRECTION ( 'NONE',  ( 0.000000000000000000, -0.000000000000000000, -1.000000000000000000 ) ) ;
#34364 = CARTESIAN_POINT ( 'NONE',  ( -4.458734124999997661, -72.47916666530107932, 2.574251347313722516 ) ) ;
#34365 = CARTESIAN_POINT ( 'NONE',  ( -5.000000000000000000, -58.08333333333332860, -2.886751345948128211 ) ) ;
#34366 = LINE ( 'NONE', #14435, #21313 ) ;
#34367 = CARTESIAN_POINT ( 'NONE',  ( 0.000000000000000000, -170.0000000000000000, 0.000000000000000000 ) ) ;
#34368 = ORIENTED_EDGE ( 'NONE', *, *, #47833, .F. ) ;
#34369 = CYLINDRICAL_SURFACE ( 'NONE', #33522, 5.000000000000000000 ) ;
#34370 = CARTESIAN_POINT ( 'NONE',  ( 5.000000000000000000, 2.708333336064520314, -2.886751345948130876 ) ) ;
#34371 = CARTESIAN_POINT ( 'NONE',  ( 1.060575238724906964E-15, -19.74999999999999645, 5.773502691896257311 ) ) ;
#34372 = CARTESIAN_POINT ( 'NONE',  ( -3.152548672688508926E-16, -20.56249999863440081, -5.148502694627439702 ) ) ;
#34373 = CARTESIAN_POINT ( 'NONE',  ( -2.229367062499996610, -82.14583333196773651, 3.861377020970582219 ) ) ;
#34374 = AXIS2_PLACEMENT_3D ( 'NONE', #15432, #54663, #6103 ) ;
#34375 = CARTESIAN_POINT ( 'NONE',  ( -4.458734124999999437, -166.1875000013655779, -5.460374474430324690E-16 ) ) ;
#34376 = CARTESIAN_POINT ( 'NONE',  ( 1.060575238724906964E-15, -16.62499999726881583, 5.773502691896257311 ) ) ;
#34378 = ORIENTED_EDGE ( 'NONE', *, *, #56762, .T. ) ;
#34377 = CARTESIAN_POINT ( 'NONE',  ( -4.458734124999999437, -48.39583333196772941, -2.574251347313719407 ) ) ;
#34379 = CARTESIAN_POINT ( 'NONE',  ( 1.975475456537005874E-15, -91.62499999726878741, 5.000000000000000000 ) ) ;
#34380 = CARTESIAN_POINT ( 'NONE',  ( -6.972266317189433020E-16, -62.24999999999999289, -5.000000000000000000 ) ) ;
#34382 = EDGE_LOOP ( 'NONE', ( #46474, #50958, #22264, #194 ) ) ;
#34381 = CARTESIAN_POINT ( 'NONE',  ( -4.458734124999999437, -0.6458333319677399542, -2.574251347313719407 ) ) ;
#34383 = CARTESIAN_POINT ( 'NONE',  ( -50.40829686548195099, -154.0000000013656063, -1.485763867205728284 ) ) ;
#34384 = CARTESIAN_POINT ( 'NONE',  ( 5.000000000000000888, -65.58333333333332860, 2.886751345948126879 ) ) ;
#34385 = CARTESIAN_POINT ( 'NONE',  ( -3.152801135295367985, -156.0625000013656063, 3.152801135295367096 ) ) ;
#34386 = CARTESIAN_POINT ( 'NONE',  ( -2.229367062500000163, -40.72916666530107221, -3.861377020970580443 ) ) ;
#34387 = CARTESIAN_POINT ( 'NONE',  ( 1.975475456537005874E-15, -68.62499999726881583, 5.000000000000000000 ) ) ;
#34388 =( BOUNDED_CURVE ( )  B_SPLINE_CURVE ( 2, ( #42195, #37071, #27719, #36747, #8430, #23212, #2344, #61837, #17121 ),
 .UNSPECIFIED., .F., .F. ) 
 B_SPLINE_CURVE_WITH_KNOTS ( ( 3, 2, 2, 2, 3 ),
 ( 0.3354166666666666963, 0.3361111111111111382, 0.3375000000000000222, 0.3388888888888889062, 0.3395833333333333481 ),
 .UNSPECIFIED. ) 
 CURVE ( )  GEOMETRIC_REPRESENTATION_ITEM ( )  RATIONAL_B_SPLINE_CURVE ( ( 0.9330127018922194093, 0.9330127018922220739, 1.000000000000000000, 0.8660254037844387076, 1.000000000000000000, 0.8660254037844387076, 1.000000000000000000, 0.9330127018922194093, 0.9330127018922194093 ) ) 
 REPRESENTATION_ITEM ( '' )  );
#34389 = CARTESIAN_POINT ( 'NONE',  ( -2.071067811865478170, -164.3125000000000000, 5.000000000000000000 ) ) ;
#34390 = CARTESIAN_POINT ( 'NONE',  ( -4.999999999999998224, 7.208333336064517205, 2.886751345948131764 ) ) ;
#34391 = CARTESIAN_POINT ( 'NONE',  ( -56.48576386720575471, -126.0000000013656063, -4.591703134518078322 ) ) ;
#34392 = CARTESIAN_POINT ( 'NONE',  ( -4.458734124999999437, -8.645833331967736513, -2.574251347313719407 ) ) ;
#34393 = CARTESIAN_POINT ( 'NONE',  ( 2.229367062499998831, -43.89583333196774362, -3.861377020970580887 ) ) ;
#34394 = CARTESIAN_POINT ( 'NONE',  ( -8.190561711645485556E-16, -146.6875000013656063, 4.458734124999999437 ) ) ;
#34395 = CARTESIAN_POINT ( 'NONE',  ( 2.229367062499998831, -88.89583333196773651, -3.861377020970580887 ) ) ;
#34396 = ORIENTED_EDGE ( 'NONE', *, *, #59883, .F. ) ;
#34397 = CARTESIAN_POINT ( 'NONE',  ( 1.975475456537005874E-15, 14.37500000273118417, 5.000000000000000000 ) ) ;
#34398 = CARTESIAN_POINT ( 'NONE',  ( 4.458734125000001214, 28.85416666803225993, 2.574251347313718519 ) ) ;
#34399 = CARTESIAN_POINT ( 'NONE',  ( -59.81910112700025905, -151.3125000027312126, -2.462841084822630311 ) ) ;
#34400 = ORIENTED_EDGE ( 'NONE', *, *, #56758, .F. ) ;
#34401 = CARTESIAN_POINT ( 'NONE',  ( 4.458734124999999437, 1.187500001365596081, -5.460374474430324690E-16 ) ) ;
#34402 = DIRECTION ( 'NONE',  ( -0.000000000000000000, 1.000000000000000000, -0.000000000000000000 ) ) ;
#34403 = CARTESIAN_POINT ( 'NONE',  ( 4.458734124999999437, -18.06249999863440792, -5.460374474430324690E-16 ) ) ;
#34404 = CARTESIAN_POINT ( 'NONE',  ( -4.999999999999998224, 2.208333336064519870, 2.886751345948131764 ) ) ;
#34405 = CARTESIAN_POINT ( 'NONE',  ( -4.458734124999998549, -3.229166665301069994, 2.574251347313722516 ) ) ;
#34406 = CARTESIAN_POINT ( 'NONE',  ( -6.972266317189433020E-16, -73.12499999726878741, -5.000000000000000000 ) ) ;
#34407 = CARTESIAN_POINT ( 'NONE',  ( -4.458734124999999437, -153.9375000013655779, -5.460374474430324690E-16 ) ) ;
#34408 = CARTESIAN_POINT ( 'NONE',  ( -2.229367062499996610, 20.60416666803225993, 3.861377020970582219 ) ) ;
#34409 = ORIENTED_EDGE ( 'NONE', *, *, #42806, .F. ) ;
#34410 = CARTESIAN_POINT ( 'NONE',  ( -2.229367062500000163, -99.47916666530106511, -3.861377020970580443 ) ) ;
#34411 = CARTESIAN_POINT ( 'NONE',  ( -6.972266317189433020E-16, -26.25000000000000355, -5.000000000000000000 ) ) ;
#34412 = CARTESIAN_POINT ( 'NONE',  ( -55.39835681537999790, -154.0000000027312410, 4.984105922594378235 ) ) ;
#34413 = CARTESIAN_POINT ( 'NONE',  ( -4.458734124999999437, -15.31249999863440436, 0.000000000000000000 ) ) ;
#34414 = CARTESIAN_POINT ( 'NONE',  ( 1.975475456537005874E-15, -49.74999999999999289, 5.000000000000000000 ) ) ;
#34415 = CARTESIAN_POINT ( 'NONE',  ( 2.500000000000002220, 29.33333333333333215, 4.330127018922192761 ) ) ;
#34416 = AXIS2_PLACEMENT_3D ( 'NONE', #49836, #60148, #45019 ) ;
#34417 = CARTESIAN_POINT ( 'NONE',  ( -52.10840900171896806, -153.1875000013656063, 3.393966926194110556 ) ) ;
#34418 = CARTESIAN_POINT ( 'NONE',  ( 5.000000000000000000, -39.37499999726880162, -6.123233995736766282E-16 ) ) ;
#34419 = DIRECTION ( 'NONE',  ( -0.6485228581062915110, 0.000000000000000000, -0.7611951803011149931 ) ) ;
#34420 = CARTESIAN_POINT ( 'NONE',  ( -4.458734124999997661, 15.77083333469892601, 2.574251347313722516 ) ) ;
#34421 = CARTESIAN_POINT ( 'NONE',  ( 5.000000000000000000, -51.29166666393547303, -2.886751345948130876 ) ) ;
#34422 = ORIENTED_EDGE ( 'NONE', *, *, #60151, .F. ) ;
#34423 = CARTESIAN_POINT ( 'NONE',  ( -2.229367062499996610, 15.85416666803226171, 3.861377020970582219 ) ) ;
#34424 = CARTESIAN_POINT ( 'NONE',  ( -2.229367062499996610, -64.14583333196773651, 3.861377020970582219 ) ) ;
#34425 = ORIENTED_EDGE ( 'NONE', *, *, #29931, .F. ) ;
#34426 = CARTESIAN_POINT ( 'NONE',  ( -4.458734124999997661, -10.47916666530106866, 2.574251347313722516 ) ) ;
#34427 = LINE ( 'NONE', #11196, #3178 ) ;
#34428 = CARTESIAN_POINT ( 'NONE',  ( -3.535250795749689387E-16, 6.749999999999999112, -5.773502691896257311 ) ) ;
#34429 = CARTESIAN_POINT ( 'NONE',  ( 3.152801135295366208, -168.5625000013656063, 3.152801135295367985 ) ) ;
#34430 = CARTESIAN_POINT ( 'NONE',  ( -1.339745962155613812, -21.08034179853029144, -5.000000000000000000 ) ) ;
#34431 = CARTESIAN_POINT ( 'NONE',  ( -4.458734124999999437, -52.39583333196773651, -2.574251347313719407 ) ) ;
#34432 = CARTESIAN_POINT ( 'NONE',  ( 2.500000000000002220, -89.54166666393547303, 4.330127018922192761 ) ) ;
#34433 = CARTESIAN_POINT ( 'NONE',  ( 2.229367062500001939, -34.97916666530107221, 3.861377020970579999 ) ) ;
#34434 = CARTESIAN_POINT ( 'NONE',  ( 1.339745962155612702, -38.29465819873851729, -5.000000000000000000 ) ) ;
#34435 = CARTESIAN_POINT ( 'NONE',  ( 7.204675194429079505E-15, 25.87500000273118062, -5.000000000000000000 ) ) ;
#34436 = CARTESIAN_POINT ( 'NONE',  ( 0.000000000000000000, -120.0000000000000000, 5.000000000000000000 ) ) ;
#34437 = CARTESIAN_POINT ( 'NONE',  ( 4.458734124999999437, -154.6875000013656063, 0.000000000000000000 ) ) ;
#34438 = CARTESIAN_POINT ( 'NONE',  ( 5.000000000000000888, -40.58333333333333570, 2.886751345948126879 ) ) ;
#34439 = CARTESIAN_POINT ( 'NONE',  ( 1.339745962155615144, -98.58034179853029855, 4.999999999999999112 ) ) ;
#34440 = CARTESIAN_POINT ( 'NONE',  ( -59.04365660845520836, -135.0000000000000284, 2.932170451817831758 ) ) ;
#34441 = ORIENTED_EDGE ( 'NONE', *, *, #38398, .F. ) ;
#34442 = CARTESIAN_POINT ( 'NONE',  ( -4.458734124999999437, -99.39583333196772230, -2.574251347313719407 ) ) ;
#34443 = CARTESIAN_POINT ( 'NONE',  ( -2.229367062500000163, 1.270833334698927342, -3.861377020970580443 ) ) ;
#34444 = CARTESIAN_POINT ( 'NONE',  ( -4.999999999999998224, -87.79166666393547303, 2.886751345948131764 ) ) ;
#34445 = CARTESIAN_POINT ( 'NONE',  ( -2.499999999999996447, 0.1666666666666656582, 4.330127018922195425 ) ) ;
#34446 = CARTESIAN_POINT ( 'NONE',  ( -2.229367062500000163, -66.47916666530106511, -3.861377020970580443 ) ) ;
#34447 = CARTESIAN_POINT ( 'NONE',  ( -4.729367062499999719, -90.15624999931721106, 0.000000000000000000 ) ) ;
#34448 = CARTESIAN_POINT ( 'NONE',  ( -3.535250795749689387E-16, -3.124999997268815832, -5.773502691896257311 ) ) ;
#34450 = ORIENTED_EDGE ( 'NONE', *, *, #36265, .F. ) ;
#34449 = CARTESIAN_POINT ( 'NONE',  ( 2.229367062500001939, -31.97916666530106866, 3.861377020970579999 ) ) ;
#34451 = DIRECTION ( 'NONE',  ( -0.9396926207859143121, 0.000000000000000000, -0.3420201433256525592 ) ) ;
#34452 = CARTESIAN_POINT ( 'NONE',  ( 1.339745962155615144, 19.29465819873852439, 4.999999999999999112 ) ) ;
#34453 = CARTESIAN_POINT ( 'NONE',  ( 1.339745962155615144, -20.70534180126147916, 4.999999999999999112 ) ) ;
#34454 = CARTESIAN_POINT ( 'NONE',  ( -4.999999999999999112, -48.91666666666666430, 2.886751345948131764 ) ) ;
#34456 = CARTESIAN_POINT ( 'NONE',  ( 4.458734125000001214, -26.14583333196774007, 2.574251347313718519 ) ) ;
#34455 = DIRECTION ( 'NONE',  ( 0.000000000000000000, 0.000000000000000000, 1.000000000000000000 ) ) ;
#34457 = CARTESIAN_POINT ( 'NONE',  ( 1.339745962155615144, -64.70534180126146850, 4.999999999999999112 ) ) ;
#34458 = CARTESIAN_POINT ( 'NONE',  ( 4.458734124999998549, -68.72916666530106511, -2.574251347313721627 ) ) ;
#34459 = CARTESIAN_POINT ( 'NONE',  ( -1.846868145590737420, -143.0000000013655779, 4.458734124999999437 ) ) ;
#34461 = EDGE_CURVE ( 'NONE', #55487, #19063, #25888, .T. ) ;
#34460 = CARTESIAN_POINT ( 'NONE',  ( -4.458734124999998549, -81.22916666530106511, 2.574251347313722516 ) ) ;
#34462 = CARTESIAN_POINT ( 'NONE',  ( -50.55543936806279248, -139.3125000013656063, 0.3552334253322060320 ) ) ;
#34463 = CARTESIAN_POINT ( 'NONE',  ( -2.229367062500000163, -32.72916666530106511, -3.861377020970580443 ) ) ;
#34464 = CARTESIAN_POINT ( 'NONE',  ( -5.000000000000000000, -69.95833333060214443, -2.886751345948128211 ) ) ;
#34465 = VERTEX_POINT ( 'NONE', #29085 ) ;
#34466 = ORIENTED_EDGE ( 'NONE', *, *, #43719, .F. ) ;
#34467 = CARTESIAN_POINT ( 'NONE',  ( -3.152548672688508926E-16, -70.81249999863440792, -5.148502694627439702 ) ) ;
#34468 = CARTESIAN_POINT ( 'NONE',  ( -6.972266317189433020E-16, -17.25000000000000000, -5.000000000000000000 ) ) ;
#34469 = ORIENTED_EDGE ( 'NONE', *, *, #54759, .T. ) ;
#34470 = CARTESIAN_POINT ( 'NONE',  ( 1.975475456537005874E-15, -61.74999999999999289, 5.000000000000000000 ) ) ;
#34471 = CARTESIAN_POINT ( 'NONE',  ( -1.339745962155610925, 8.205341801261479162, 5.000000000000000000 ) ) ;
#34472 = CARTESIAN_POINT ( 'NONE',  ( -4.458734124999999437, -60.64583333196774362, -2.574251347313719407 ) ) ;
#34473 = CARTESIAN_POINT ( 'NONE',  ( 2.229367062500001939, -2.229166665301068662, 3.861377020970579999 ) ) ;
#34474 = ORIENTED_EDGE ( 'NONE', *, *, #59883, .T. ) ;
#34475 = DIRECTION ( 'NONE',  ( -0.000000000000000000, 1.000000000000000000, -0.000000000000000000 ) ) ;
#34476 = DIRECTION ( 'NONE',  ( 0.000000000000000000, 0.000000000000000000, -1.000000000000000000 ) ) ;
#34477 = CARTESIAN_POINT ( 'NONE',  ( 2.229367062500001939, 15.02083333469892779, 3.861377020970579999 ) ) ;
#34478 = CARTESIAN_POINT ( 'NONE',  ( -51.60603307380591787, -140.9375000013656063, -2.891590998281053704 ) ) ;
#34479 = CARTESIAN_POINT ( 'NONE',  ( -4.999999999999998224, -0.9166666666666664076, 2.886751345948131764 ) ) ;
#34480 = CARTESIAN_POINT ( 'NONE',  ( 4.458734124999997661, -163.5000000013655779, 1.846868145590737864 ) ) ;
#34481 = VERTEX_POINT ( 'NONE', #9173 ) ;
#34482 = CARTESIAN_POINT ( 'NONE',  ( 2.229367062499998831, -80.64583333196773651, -3.861377020970580887 ) ) ;
#34483 = CARTESIAN_POINT ( 'NONE',  ( -6.972266317189433020E-16, -39.25000000000000000, -5.000000000000000000 ) ) ;
#34484 = CARTESIAN_POINT ( 'NONE',  ( 9.457646018065525792E-16, 0.9375000013655959696, 5.148502694627439702 ) ) ;
#34485 = CARTESIAN_POINT ( 'NONE',  ( -5.000000000000000000, -84.08333333333332860, -2.886751345948128211 ) ) ;
#34486 = CARTESIAN_POINT ( 'NONE',  ( -2.500000000000000444, -43.04166666393548013, -4.330127018922193649 ) ) ;
#34487 = CARTESIAN_POINT ( 'NONE',  ( 4.458734124999999437, -63.06249999863440792, -5.460374474430324690E-16 ) ) ;
#34488 = CARTESIAN_POINT ( 'NONE',  ( 5.000000000000000000, -23.29166666393548368, -2.886751345948129988 ) ) ;
#34489 = CARTESIAN_POINT ( 'NONE',  ( -4.999999999999998224, -72.79166666393548724, 2.886751345948131764 ) ) ;
#34490 = CARTESIAN_POINT ( 'NONE',  ( -4.458734124999997661, 27.77083333469892423, 2.574251347313722516 ) ) ;
#34491 = CARTESIAN_POINT ( 'NONE',  ( 2.499999999999998668, -61.33333333333333570, -4.330127018922193649 ) ) ;
#34492 = CARTESIAN_POINT ( 'NONE',  ( -2.229367062500000163, -48.47916666530106511, -3.861377020970580443 ) ) ;
#34493 = CARTESIAN_POINT ( 'NONE',  ( 2.229367062499998831, -31.89583333196773651, -3.861377020970580887 ) ) ;
#34494 = CARTESIAN_POINT ( 'NONE',  ( -4.458734124999999437, 8.437500001365595637, 0.000000000000000000 ) ) ;
#34495 = VECTOR ( 'NONE', #23945, 1000.000000000000000 ) ;
#34496 = CARTESIAN_POINT ( 'NONE',  ( 0.000000000000000000, -120.0000000000000000, 0.000000000000000000 ) ) ;
#34497 = CARTESIAN_POINT ( 'NONE',  ( 5.000000000000000888, 21.41666666666666430, 2.886751345948126879 ) ) ;
#34498 = CARTESIAN_POINT ( 'NONE',  ( 3.535533905932736864, -150.2500000027312126, 3.535533905932738641 ) ) ;
#34499 = CARTESIAN_POINT ( 'NONE',  ( -5.000000000000000000, 28.99999999999999645, 0.000000000000000000 ) ) ;
#34500 = CARTESIAN_POINT ( 'NONE',  ( 2.229367062500001939, -36.97916666530107221, 3.861377020970579999 ) ) ;
#34501 = CARTESIAN_POINT ( 'NONE',  ( 5.000000000000000000, -73.29166666393548724, -2.886751345948129988 ) ) ;
#34502 = VECTOR ( 'NONE', #46321, 1000.000000000000000 ) ;
#34503 = VECTOR ( 'NONE', #4526, 1000.000000000000000 ) ;
#34504 = CARTESIAN_POINT ( 'NONE',  ( -50.70258187064364108, -143.3750000013656063, 2.196230717870141014 ) ) ;
#34505 =( BOUNDED_CURVE ( )  B_SPLINE_CURVE ( 2, ( #1846, #2167, #41678, #17251, #52307, #36875, #32674, #12427, #7615 ),
 .UNSPECIFIED., .F., .F. ) 
 B_SPLINE_CURVE_WITH_KNOTS ( ( 3, 2, 2, 2, 3 ),
 ( 0.7083333333333329263, 0.7124999999999995781, 0.7166666666666663410, 0.7208333333333329929, 0.7249999999999996447 ),
 .UNSPECIFIED. ) 
 CURVE ( )  GEOMETRIC_REPRESENTATION_ITEM ( )  RATIONAL_B_SPLINE_CURVE ( ( 1.000000000000008216, 0.9238795325112786339, 1.000000000000000000, 0.9238795325112867385, 1.000000000000000000, 0.9238795325112867385, 1.000000000000000000, 0.9238795325112928447, 0.9999999999999938938 ) ) 
 REPRESENTATION_ITEM ( '' )  );
#34506 = CARTESIAN_POINT ( 'NONE',  ( 3.535533905932738197, -142.8750000000000000, -3.535533905932738197 ) ) ;
#34507 = LINE ( 'NONE', #45451, #11064 ) ;
#34508 = CARTESIAN_POINT ( 'NONE',  ( -4.458734124999999437, -80.56249999863440792, 0.000000000000000000 ) ) ;
#34509 = CARTESIAN_POINT ( 'NONE',  ( 3.152801135295366208, -163.8125000013656063, 3.152801135295367985 ) ) ;
#34510 = CARTESIAN_POINT ( 'NONE',  ( -2.229367062500000163, -36.47916666530107221, -3.861377020970580443 ) ) ;
#34511 = FACE_OUTER_BOUND ( 'NONE', #33065, .T. ) ;
#34512 = LINE ( 'NONE', #39033, #39973 ) ;
#34513 = CARTESIAN_POINT ( 'NONE',  ( 1.060575238724906964E-15, -19.74999999999999645, 5.773502691896257311 ) ) ;
#34514 = CARTESIAN_POINT ( 'NONE',  ( 3.152801135295366208, -144.5625000013655779, 3.152801135295367985 ) ) ;
#34515 = ORIENTED_EDGE ( 'NONE', *, *, #28773, .F. ) ;
#34516 = CARTESIAN_POINT ( 'NONE',  ( 9.457646018065525792E-16, 28.68750000136559208, 5.148502694627439702 ) ) ;
#34517 = ORIENTED_EDGE ( 'NONE', *, *, #20854, .F. ) ;
#34518 = CARTESIAN_POINT ( 'NONE',  ( 4.458734124999998549, -63.97916666530106511, -2.574251347313721627 ) ) ;
#34519 = CARTESIAN_POINT ( 'NONE',  ( 2.499999999999998668, 22.79166666939785202, -4.330127018922193649 ) ) ;
#34520 = CARTESIAN_POINT ( 'NONE',  ( 5.000000000000000000, -90.37499999726880162, -6.123233995736766282E-16 ) ) ;
#34521 = CARTESIAN_POINT ( 'NONE',  ( 1.060575238724906964E-15, 13.24999999999999822, 5.773502691896257311 ) ) ;
#34522 = CARTESIAN_POINT ( 'NONE',  ( 2.229367062500001939, -51.97916666530107221, 3.861377020970579999 ) ) ;
#34523 = CARTESIAN_POINT ( 'NONE',  ( 2.229367062500001939, -4.979166665301071326, 3.861377020970579999 ) ) ;
#34524 = CARTESIAN_POINT ( 'NONE',  ( -5.000000000000000000, 4.125000002731186832, 0.000000000000000000 ) ) ;
#34525 = CARTESIAN_POINT ( 'NONE',  ( -2.499999999999996447, -76.83333333333334281, 4.330127018922195425 ) ) ;
#34526 = CARTESIAN_POINT ( 'NONE',  ( -2.352990130084580066E-16, 8.660254037844390851, -7.422398894150034288 ) ) ;
#34528 = CARTESIAN_POINT ( 'NONE',  ( -4.458734124999999437, -20.39583333196774362, -2.574251347313719407 ) ) ;
#34527 = CARTESIAN_POINT ( 'NONE',  ( -2.499999999999996447, 5.166666666666666963, 4.330127018922195425 ) ) ;
#34529 = CARTESIAN_POINT ( 'NONE',  ( -6.972266317189433020E-16, 0.7499999999999996669, -5.000000000000000000 ) ) ;
#34530 = CARTESIAN_POINT ( 'NONE',  ( -4.458734124999998549, -53.22916666530107932, 2.574251347313722516 ) ) ;
#34531 = CARTESIAN_POINT ( 'NONE',  ( 4.458734124999999437, -157.6875000013655779, 0.000000000000000000 ) ) ;
#34532 = ADVANCED_FACE ( 'NONE', ( #19769 ), #19449, .T. ) ;
#34533 = CARTESIAN_POINT ( 'NONE',  ( -4.999999999999999112, -55.79166666393548013, 2.886751345948131764 ) ) ;
#34534 = ORIENTED_EDGE ( 'NONE', *, *, #11766, .F. ) ;
#34535 = CARTESIAN_POINT ( 'NONE',  ( -5.000000000000000000, 25.04166666939785202, -2.886751345948128211 ) ) ;
#34536 = CARTESIAN_POINT ( 'NONE',  ( -4.458734124999998549, 6.520833334698930450, 2.574251347313722516 ) ) ;
#34537 = ORIENTED_EDGE ( 'NONE', *, *, #21754, .T. ) ;
#34539 = CARTESIAN_POINT ( 'NONE',  ( -6.972266317189433020E-16, -68.12499999726881583, -5.000000000000000000 ) ) ;
#34538 = DIRECTION ( 'NONE',  ( -0.000000000000000000, 1.000000000000000000, -0.000000000000000000 ) ) ;
#34540 = CARTESIAN_POINT ( 'NONE',  ( -3.152801135295367985, -156.8125000013656063, 3.152801135295367096 ) ) ;
#34541 = ORIENTED_EDGE ( 'NONE', *, *, #16874, .T. ) ;
#34542 = AXIS2_PLACEMENT_3D ( 'NONE', #23556, #63111, #14197 ) ;
#34543 = EDGE_CURVE ( 'NONE', #36547, #16762, #32469, .T. ) ;
#34544 = CARTESIAN_POINT ( 'NONE',  ( 0.000000000000000000, 0.000000000000000000, -0.5776712190230133270 ) ) ;
#34545 = CARTESIAN_POINT ( 'NONE',  ( -54.60164318462004474, -134.3750000000000284, -4.984105922594373794 ) ) ;
#34546 = CARTESIAN_POINT ( 'NONE',  ( 5.000000000000000888, -53.45833333060213732, 2.886751345948126879 ) ) ;
#34547 = CARTESIAN_POINT ( 'NONE',  ( 2.229367062500001939, -41.22916666530107932, 3.861377020970579999 ) ) ;
#34548 = VECTOR ( 'NONE', #61946, 1000.000000000000000 ) ;
#34549 = VERTEX_POINT ( 'NONE', #34233 ) ;
#34550 = AXIS2_PLACEMENT_3D ( 'NONE', #4156, #43064, #49149 ) ;
#34551 = CARTESIAN_POINT ( 'NONE',  ( -3.535533905932737309, -145.6250000000000000, -3.535533905932738197 ) ) ;
#34552 = EDGE_CURVE ( 'NONE', #44876, #24978, #14308, .T. ) ;
#34553 = CARTESIAN_POINT ( 'NONE',  ( 4.458734124999999437, 17.18750000136559564, -5.460374474430324690E-16 ) ) ;
#34554 = CARTESIAN_POINT ( 'NONE',  ( -5.000000000000000000, -84.99999999999998579, 0.000000000000000000 ) ) ;
#34555 =( BOUNDED_CURVE ( )  B_SPLINE_CURVE ( 2, ( #52147, #60853, #2320, #37348, #47005, #62119, #56667, #47321, #7458 ),
 .UNSPECIFIED., .F., .F. ) 
 B_SPLINE_CURVE_WITH_KNOTS ( ( 3, 2, 2, 2, 3 ),
 ( 0.9687500000000000000, 0.9694444444444444420, 0.9708333333333333259, 0.9722222222222222099, 0.9729166666666666519 ),
 .UNSPECIFIED. ) 
 CURVE ( )  GEOMETRIC_REPRESENTATION_ITEM ( )  RATIONAL_B_SPLINE_CURVE ( ( 0.9330127018922194093, 0.9330127018922194093, 1.000000000000000000, 0.8660254037844387076, 1.000000000000000000, 0.8660254037844387076, 1.000000000000000000, 0.9330127018922194093, 0.9330127018922194093 ) ) 
 REPRESENTATION_ITEM ( '' )  );
#34556 = ORIENTED_EDGE ( 'NONE', *, *, #54679, .T. ) ;
#34557 = CARTESIAN_POINT ( 'NONE',  ( -4.458734124999998549, 28.77083333469892779, 2.574251347313722516 ) ) ;
#34558 = CARTESIAN_POINT ( 'NONE',  ( -51.60603307380591787, -153.9375000013656063, -2.891590998281053704 ) ) ;
#34559 = CYLINDRICAL_SURFACE ( 'NONE', #11059, 5.000000000000000000 ) ;
#34560 = CARTESIAN_POINT ( 'NONE',  ( -51.14619162160809651, -135.0000000000000284, 2.724453935955323480 ) ) ;
#34561 =( BOUNDED_CURVE ( )  B_SPLINE_CURVE ( 2, ( #30655, #50278, #6223, #18853, #25835, #37087, #36762, #40933, #26152 ),
 .UNSPECIFIED., .F., .F. ) 
 B_SPLINE_CURVE_WITH_KNOTS ( ( 3, 2, 2, 2, 3 ),
 ( 0.2187500000000000000, 0.2194444444444444420, 0.2208333333333333259, 0.2222222222222222099, 0.2229166666666666796 ),
 .UNSPECIFIED. ) 
 CURVE ( )  GEOMETRIC_REPRESENTATION_ITEM ( )  RATIONAL_B_SPLINE_CURVE ( ( 0.9330127018922194093, 0.9330127018922194093, 1.000000000000000000, 0.8660254037844387076, 1.000000000000000000, 0.8660254037844387076, 1.000000000000000000, 0.9330127018922180770, 0.9330127018922194093 ) ) 
 REPRESENTATION_ITEM ( '' )  );
#34562 = CARTESIAN_POINT ( 'NONE',  ( -6.972266317189433020E-16, 1.750000000000000444, -5.000000000000000000 ) ) ;
#34563 = CARTESIAN_POINT ( 'NONE',  ( -2.229367062499996610, -66.14583333196773651, 3.861377020970582219 ) ) ;
#34564 = FACE_OUTER_BOUND ( 'NONE', #60741, .T. ) ;
#34565 = CARTESIAN_POINT ( 'NONE',  ( -2.229367062500000163, 18.52083333469892779, -3.861377020970580443 ) ) ;
#34566 = CYLINDRICAL_SURFACE ( 'NONE', #13398, 5.000000000000000000 ) ;
#34567 = CARTESIAN_POINT ( 'NONE',  ( 4.458734125000001214, -52.14583333196772941, 2.574251347313718519 ) ) ;
#34568 = CARTESIAN_POINT ( 'NONE',  ( -2.499999999999996447, -11.70833333060214798, 4.330127018922195425 ) ) ;
#34569 = CARTESIAN_POINT ( 'NONE',  ( 1.975475456537005874E-15, -108.7499999999999858, 5.000000000000000000 ) ) ;
#34570 = FACE_OUTER_BOUND ( 'NONE', #57701, .T. ) ;
#34571 = CARTESIAN_POINT ( 'NONE',  ( -4.458734124999999437, -87.56249999863439371, 0.000000000000000000 ) ) ;
#34572 = CARTESIAN_POINT ( 'NONE',  ( -2.229367062499996610, -110.1458333319677365, 3.861377020970582219 ) ) ;
#34573 = CARTESIAN_POINT ( 'NONE',  ( -4.458734124999997661, -16.47916666530107577, 2.574251347313722516 ) ) ;
#34574 = VERTEX_POINT ( 'NONE', #29397 ) ;
#34575 = DIRECTION ( 'NONE',  ( 0.000000000000000000, 0.000000000000000000, 1.000000000000000000 ) ) ;
#34576 = CARTESIAN_POINT ( 'NONE',  ( -4.458734124999998549, -97.22916666530105090, 2.574251347313722516 ) ) ;
#34577 = CARTESIAN_POINT ( 'NONE',  ( -9.184850993605147944E-16, -163.3750000027311842, 5.000000000000000000 ) ) ;
#34578 = CARTESIAN_POINT ( 'NONE',  ( 4.458734124999999437, -100.0624999986344079, -5.460374474430324690E-16 ) ) ;
#34579 = EDGE_CURVE ( 'NONE', #25841, #54515, #23079, .T. ) ;
#34580 = CARTESIAN_POINT ( 'NONE',  ( 0.000000000000000000, -120.0000000000000000, 0.000000000000000000 ) ) ;
#34581 = CARTESIAN_POINT ( 'NONE',  ( 5.000000000000000000, -59.29166666393547303, -2.886751345948129988 ) ) ;
#34582 = CARTESIAN_POINT ( 'NONE',  ( -2.500000000000000444, 18.95833333606451632, -4.330127018922193649 ) ) ;
#34583 = CARTESIAN_POINT ( 'NONE',  ( -58.39396692619412477, -124.4375000013656063, 2.891590998281057701 ) ) ;
#34584 = CARTESIAN_POINT ( 'NONE',  ( -57.89159099828107458, -147.6875000013656063, -3.393966926194107447 ) ) ;
#34585 = CARTESIAN_POINT ( 'NONE',  ( -4.458734124999999437, -19.31249999863440081, 0.000000000000000000 ) ) ;
#34586 = CARTESIAN_POINT ( 'NONE',  ( -4.458734124999999437, 8.354166668032261711, -2.574251347313719407 ) ) ;
#34587 =( BOUNDED_CURVE ( )  B_SPLINE_CURVE ( 2, ( #41726, #14820, #10001, #50527, #688, #26078, #35410, #1652, #29614 ),
 .UNSPECIFIED., .F., .F. ) 
 B_SPLINE_CURVE_WITH_KNOTS ( ( 3, 2, 2, 2, 3 ),
 ( 0.8895833333333332815, 0.8902777777777777235, 0.8916666666666667185, 0.8930555555555556024, 0.8937500000000000444 ),
 .UNSPECIFIED. ) 
 CURVE ( )  GEOMETRIC_REPRESENTATION_ITEM ( )  RATIONAL_B_SPLINE_CURVE ( ( 0.9330127018922194093, 0.9330127018922194093, 1.000000000000000000, 0.8660254037844387076, 1.000000000000000000, 0.8660254037844387076, 1.000000000000000000, 0.9330127018922194093, 0.9330127018922194093 ) ) 
 REPRESENTATION_ITEM ( '' )  );
#34588 = CARTESIAN_POINT ( 'NONE',  ( -4.458734124999997661, -56.47916666530107221, 2.574251347313722516 ) ) ;
#34589 = FACE_OUTER_BOUND ( 'NONE', #12745, .T. ) ;
#34590 = CARTESIAN_POINT ( 'NONE',  ( -3.152548672688508926E-16, -21.56249999863440792, -5.148502694627439702 ) ) ;
#34591 = DIRECTION ( 'NONE',  ( 0.000000000000000000, 0.000000000000000000, -1.000000000000000000 ) ) ;
#34592 = CARTESIAN_POINT ( 'NONE',  ( 3.061616997868383141E-16, -156.7500000000000000, -5.000000000000000000 ) ) ;
#34593 = CARTESIAN_POINT ( 'NONE',  ( -2.499999999999996447, -5.833333333333336590, 4.330127018922195425 ) ) ;
#34594 = ORIENTED_EDGE ( 'NONE', *, *, #44166, .F. ) ;
#34595 = CARTESIAN_POINT ( 'NONE',  ( 2.229367062499998831, -44.89583333196774362, -3.861377020970580887 ) ) ;
#34596 = AXIS2_PLACEMENT_3D ( 'NONE', #46212, #21780, #36881 ) ;
#34597 = CARTESIAN_POINT ( 'NONE',  ( -4.999999999999998224, 26.08333333333332860, 2.886751345948131764 ) ) ;
#34598 = CARTESIAN_POINT ( 'NONE',  ( -6.439685834476978954, 4.942299687812971243, -7.659344964963200830 ) ) ;
#34599 = CARTESIAN_POINT ( 'NONE',  ( -1.510657702057710340E-15, 27.37500000273118417, 5.000000000000000000 ) ) ;
#34600 = CARTESIAN_POINT ( 'NONE',  ( -4.458734124999999437, -92.39583333196773651, -2.574251347313719407 ) ) ;
#34601 = CARTESIAN_POINT ( 'NONE',  ( 4.458734124999998549, 19.02083333469892779, -2.574251347313721627 ) ) ;
#34602 = AXIS2_PLACEMENT_3D ( 'NONE', #43776, #48294, #24489 ) ;
#34603 = VECTOR ( 'NONE', #27469, 1000.000000000000000 ) ;
#34604 = CARTESIAN_POINT ( 'NONE',  ( 4.458734124999998549, 9.270833334698927786, -2.574251347313721627 ) ) ;
#34605 = CARTESIAN_POINT ( 'NONE',  ( 5.000000000000000000, -93.41666666666667140, -2.886751345948130876 ) ) ;
#34606 = AXIS2_PLACEMENT_3D ( 'NONE', #50112, #6067, #60100 ) ;
#34607 = CARTESIAN_POINT ( 'NONE',  ( -1.339745962155610925, 12.20534180126148094, 5.000000000000000000 ) ) ;
#34608 = CARTESIAN_POINT ( 'NONE',  ( -2.229367062499996610, -89.39583333196773651, 3.861377020970582219 ) ) ;
#34609 = CARTESIAN_POINT ( 'NONE',  ( -4.458734124999998549, 19.52083333469893134, 2.574251347313722516 ) ) ;
#34610 = CARTESIAN_POINT ( 'NONE',  ( 2.500000000000002220, -74.66666666666665719, 4.330127018922192761 ) ) ;
#34611 = CARTESIAN_POINT ( 'NONE',  ( -3.535250795749689387E-16, 9.875000002731184168, -5.773502691896257311 ) ) ;
#34612 = VERTEX_POINT ( 'NONE', #32440 ) ;
#34613 = CARTESIAN_POINT ( 'NONE',  ( 0.000000000000000000, -120.0000000000000000, 5.000000000000000000 ) ) ;
#34614 = ORIENTED_EDGE ( 'NONE', *, *, #22892, .T. ) ;
#34615 =( BOUNDED_CURVE ( )  B_SPLINE_CURVE ( 2, ( #25433, #16426, #55675, #49867, #21248, #50839, #10949, #61138, #16103 ),
 .UNSPECIFIED., .F., .F. ) 
 B_SPLINE_CURVE_WITH_KNOTS ( ( 3, 2, 2, 2, 3 ),
 ( 0.01964285714285714593, 0.02023809523809523905, 0.02142857142857142877, 0.02261904761904761849, 0.02321428571428571508 ),
 .UNSPECIFIED. ) 
 CURVE ( )  GEOMETRIC_REPRESENTATION_ITEM ( )  RATIONAL_B_SPLINE_CURVE ( ( 0.9330127018922194093, 0.9330127018922195203, 1.000000000000000000, 0.8660254037844387076, 1.000000000000000000, 0.8660254037844387076, 1.000000000000000000, 0.9330127018922191873, 0.9330127018922194093 ) ) 
 REPRESENTATION_ITEM ( '' )  );
#34617 = CARTESIAN_POINT ( 'NONE',  ( -4.999999999999999112, -34.91666666666666430, 2.886751345948131764 ) ) ;
#34616 = CARTESIAN_POINT ( 'NONE',  ( 0.000000000000000000, -170.0000000000000000, 0.000000000000000000 ) ) ;
#34618 = CARTESIAN_POINT ( 'NONE',  ( -4.458734124999999437, -37.39583333196773651, -2.574251347313719407 ) ) ;
#34619 = ADVANCED_FACE ( 'NONE', ( #3190 ), #52069, .T. ) ;
#34620 = CARTESIAN_POINT ( 'NONE',  ( -2.500000000000000444, -38.04166666393548013, -4.330127018922193649 ) ) ;
#34621 = ADVANCED_FACE ( 'NONE', ( #45812 ), #59333, .T. ) ;
#34622 = VERTEX_POINT ( 'NONE', #54513 ) ;
#34623 = CARTESIAN_POINT ( 'NONE',  ( -59.59170313451811296, -149.7500000013656063, 1.485763867205729394 ) ) ;
#34624 = CARTESIAN_POINT ( 'NONE',  ( -2.229367062500000163, -13.47916666530107221, -3.861377020970580443 ) ) ;
#34626 = VERTEX_POINT ( 'NONE', #40662 ) ;
#34625 = CARTESIAN_POINT ( 'NONE',  ( -3.152548672688508926E-16, -16.81249999863440436, -5.148502694627439702 ) ) ;
#34627 = EDGE_CURVE ( 'NONE', #60995, #45777, #16875, .T. ) ;
#34628 = CARTESIAN_POINT ( 'NONE',  ( -3.535250795749689387E-16, -84.24999999999998579, -5.773502691896257311 ) ) ;
#34629 = CARTESIAN_POINT ( 'NONE',  ( -1.846868145590737420, -166.7500000013655779, 4.458734124999999437 ) ) ;
#34630 = CARTESIAN_POINT ( 'NONE',  ( 4.458734124999998549, -55.97916666530107932, -2.574251347313721627 ) ) ;
#34631 = CARTESIAN_POINT ( 'NONE',  ( -2.499999999999996447, -79.70833333060213022, 4.330127018922195425 ) ) ;
#34633 = ORIENTED_EDGE ( 'NONE', *, *, #48085, .F. ) ;
#34632 = FACE_OUTER_BOUND ( 'NONE', #54887, .T. ) ;
#34634 = CARTESIAN_POINT ( 'NONE',  ( -58.80597590150559739, -144.0000000000000284, 3.242614290531460330 ) ) ;
#34635 = CARTESIAN_POINT ( 'NONE',  ( -4.458734124999999437, -24.56249999863440436, 0.000000000000000000 ) ) ;
#34636 = CARTESIAN_POINT ( 'NONE',  ( 5.000000000000000888, -41.45833333060214443, 2.886751345948126879 ) ) ;
#34637 = EDGE_CURVE ( 'NONE', #8866, #11945, #12370, .T. ) ;
#34638 = ORIENTED_EDGE ( 'NONE', *, *, #4704, .T. ) ;
#34639 = ITEM_DEFINED_TRANSFORMATION ( 'NONE', 'NONE', #22602,  #43054 ) ;
#34640 = CARTESIAN_POINT ( 'NONE',  ( 1.846868145590736310, -163.8750000013655779, 4.458734124999999437 ) ) ;
#34641 = EDGE_CURVE ( 'NONE', #36504, #50783, #39027, .T. ) ;
#34642 = CARTESIAN_POINT ( 'NONE',  ( 4.458734124999999437, -106.0624999986344221, -5.460374474430324690E-16 ) ) ;
#34643 = CARTESIAN_POINT ( 'NONE',  ( 3.535533905932736864, -148.1250000000000000, 3.535533905932738641 ) ) ;
#34644 = ORIENTED_EDGE ( 'NONE', *, *, #16228, .F. ) ;
#34645 = CARTESIAN_POINT ( 'NONE',  ( -59.44456063193725015, -146.8125000013656063, -0.3552334253322034230 ) ) ;
#34646 = CARTESIAN_POINT ( 'NONE',  ( -4.458734124999999437, -73.64583333196773651, -2.574251347313719407 ) ) ;
#34647 = CARTESIAN_POINT ( 'NONE',  ( -57.46284108482265651, -138.0625000027311842, 4.819101127000239515 ) ) ;
#34648 = CARTESIAN_POINT ( 'NONE',  ( -4.458734124999999437, -44.39583333196774362, -2.574251347313719407 ) ) ;
#34649 = CARTESIAN_POINT ( 'NONE',  ( -1.846868145590734756, -144.3750000013656063, -4.458734124999999437 ) ) ;
#34650 = CIRCLE ( 'NONE', #32599, 11.00000000000000000 ) ;
#34651 = EDGE_CURVE ( 'NONE', #25000, #47748, #36226, .T. ) ;
#34652 = CARTESIAN_POINT ( 'NONE',  ( -7.500000000000698996, 1.613867362005801054, -7.450195926347907616 ) ) ;
#34653 = CARTESIAN_POINT ( 'NONE',  ( -6.972266317189433020E-16, -0.2500000000000001665, -5.000000000000000000 ) ) ;
#34654 = VECTOR ( 'NONE', #57340, 1000.000000000000000 ) ;
#34655 = CARTESIAN_POINT ( 'NONE',  ( -4.458734124999998549, -11.22916666530106866, 2.574251347313722516 ) ) ;
#34656 = AXIS2_PLACEMENT_3D ( 'NONE', #393, #5524, #34455 ) ;
#34657 = CARTESIAN_POINT ( 'NONE',  ( 2.500000000000002220, -99.66666666666665719, 4.330127018922192761 ) ) ;
#34658 = ORIENTED_EDGE ( 'NONE', *, *, #19239, .F. ) ;
#34659 = CARTESIAN_POINT ( 'NONE',  ( -5.000000000000000888, -167.5625000000000284, -2.071067811865475949 ) ) ;
#34660 = CARTESIAN_POINT ( 'NONE',  ( -4.458734124999999437, -35.64583333196772941, -2.574251347313719407 ) ) ;
#34661 = AXIS2_PLACEMENT_3D ( 'NONE', #40380, #60021, #15944 ) ;
#34662 = CARTESIAN_POINT ( 'NONE',  ( 1.060575238724906964E-15, 8.375000002731187720, 5.773502691896257311 ) ) ;
#34663 = CARTESIAN_POINT ( 'NONE',  ( 6.123233995736766282E-16, -120.0000000000000000, -5.000000000000000000 ) ) ;
#34664 = CARTESIAN_POINT ( 'NONE',  ( -54.64476657466781973, -132.8125000013656063, -4.444560631937228834 ) ) ;
#34665 = CARTESIAN_POINT ( 'NONE',  ( -4.458734124999999437, -71.56249999863439371, 0.000000000000000000 ) ) ;
#34666 = FACE_OUTER_BOUND ( 'NONE', #32205, .T. ) ;
#34667 = DIRECTION ( 'NONE',  ( -0.000000000000000000, 1.000000000000000000, -0.000000000000000000 ) ) ;
#34668 = CARTESIAN_POINT ( 'NONE',  ( 2.500000000000002220, -68.66666666666667140, 4.330127018922192761 ) ) ;
#34669 = CARTESIAN_POINT ( 'NONE',  ( -4.458734124999997661, 5.520833334698926009, 2.574251347313722516 ) ) ;
#34670 = ORIENTED_EDGE ( 'NONE', *, *, #41385, .T. ) ;
#34671 = CARTESIAN_POINT ( 'NONE',  ( 2.499999999999998668, -30.33333333333332860, -4.330127018922193649 ) ) ;
#34672 = CARTESIAN_POINT ( 'NONE',  ( -6.972266317189433020E-16, -15.25000000000000000, -5.000000000000000000 ) ) ;
#34674 = CARTESIAN_POINT ( 'NONE',  ( 4.458734125000001214, -29.89583333196773651, 2.574251347313718519 ) ) ;
#34673 = CARTESIAN_POINT ( 'NONE',  ( 5.000000000000000000, -93.50000000000000000, -6.123233995736766282E-16 ) ) ;
#34675 = CARTESIAN_POINT ( 'NONE',  ( -5.000000000000000000, -22.95833333060214798, -2.886751345948128211 ) ) ;
#34676 = CARTESIAN_POINT ( 'NONE',  ( 4.458734124999999437, -79.06249999863440792, -5.460374474430324690E-16 ) ) ;
#34677 = CARTESIAN_POINT ( 'NONE',  ( -2.229367062499996610, 18.60416666803225993, 3.861377020970582219 ) ) ;
#34678 = CARTESIAN_POINT ( 'NONE',  ( 1.339745962155612702, -18.29465819873851729, -5.000000000000000000 ) ) ;
#34679 = CARTESIAN_POINT ( 'NONE',  ( -59.59170313451811296, -136.5000000013656347, 1.485763867205729394 ) ) ;
#34680 = CARTESIAN_POINT ( 'NONE',  ( -2.229367062500000163, -3.479166665301069994, -3.861377020970580443 ) ) ;
#34681 = CARTESIAN_POINT ( 'NONE',  ( 2.229367062499998831, 22.10416666803225993, -3.861377020970580887 ) ) ;
#34682 = CARTESIAN_POINT ( 'NONE',  ( 4.458734125000000326, -43.14583333196773651, 2.574251347313718519 ) ) ;
#34683 = CARTESIAN_POINT ( 'NONE',  ( 5.000000000000000000, -15.50000000000000000, -6.123233995736766282E-16 ) ) ;
#34684 = CARTESIAN_POINT ( 'NONE',  ( -3.152548672688508926E-16, 2.437500001365593860, -5.148502694627439702 ) ) ;
#34685 = CARTESIAN_POINT ( 'NONE',  ( -4.458734124999997661, -26.47916666530107221, 2.574251347313722516 ) ) ;
#34686 = CARTESIAN_POINT ( 'NONE',  ( -4.458734124999998549, -68.22916666530107932, 2.574251347313722516 ) ) ;
#34687 = CARTESIAN_POINT ( 'NONE',  ( -2.500000000000000444, -103.0416666639354730, -4.330127018922193649 ) ) ;
#34688 = CARTESIAN_POINT ( 'NONE',  ( -4.458734124999998549, 26.77083333469893134, 2.574251347313722516 ) ) ;
#34689 = CYLINDRICAL_SURFACE ( 'NONE', #31774, 5.000000000000000000 ) ;
#34690 = CARTESIAN_POINT ( 'NONE',  ( -2.229367062500000163, -109.7291666653010651, -3.861377020970580443 ) ) ;
#34691 = CARTESIAN_POINT ( 'NONE',  ( 9.457646018065525792E-16, -75.31249999863440792, 5.148502694627439702 ) ) ;
#34692 = CARTESIAN_POINT ( 'NONE',  ( -5.000000000000000000, -59.00000000000000000, 0.000000000000000000 ) ) ;
#34693 = PRODUCT_DEFINITION ( 'UNKNOWN', '', #20526, #11896 ) ;
#34694 = CARTESIAN_POINT ( 'NONE',  ( -1.339745962155610925, -31.66965819600733312, 5.000000000000000000 ) ) ;
#34695 = CARTESIAN_POINT ( 'NONE',  ( -5.000000000000000000, 26.04166666939784847, -2.886751345948128211 ) ) ;
#34696 = VERTEX_POINT ( 'NONE', #10760 ) ;
#34697 = CARTESIAN_POINT ( 'NONE',  ( 2.500000000000002220, 6.333333333333333037, 4.330127018922192761 ) ) ;
#34698 = AXIS2_PLACEMENT_3D ( 'NONE', #63161, #43515, #14254 ) ;
#34699 = CARTESIAN_POINT ( 'NONE',  ( -2.499999999999996447, -98.83333333333332860, 4.330127018922195425 ) ) ;
#34700 = CARTESIAN_POINT ( 'NONE',  ( 5.000000000000000000, -19.49999999999999645, -6.123233995736766282E-16 ) ) ;
#34701 = CARTESIAN_POINT ( 'NONE',  ( -2.229367062500000163, -24.47916666530106866, -3.861377020970580443 ) ) ;
#34702 = AXIS2_PLACEMENT_3D ( 'NONE', #23412, #62656, #17936 ) ;
#34703 = CARTESIAN_POINT ( 'NONE',  ( 9.457646018065525792E-16, -82.06249999863440792, 5.148502694627439702 ) ) ;
#34704 =( BOUNDED_CURVE ( )  B_SPLINE_CURVE ( 2, ( #5924, #14919, #54157, #29707, #35193, #44504, #54491, #14599, #43551 ),
 .UNSPECIFIED., .F., .F. ) 
 B_SPLINE_CURVE_WITH_KNOTS ( ( 3, 2, 2, 2, 3 ),
 ( 0.3583333333333336146, 0.3625000000000002665, 0.3666666666666669183, 0.3708333333333336257, 0.3750000000000002776 ),
 .UNSPECIFIED. ) 
 CURVE ( )  GEOMETRIC_REPRESENTATION_ITEM ( )  RATIONAL_B_SPLINE_CURVE ( ( 0.9999999999999948930, 0.9238795325112918455, 1.000000000000000000, 0.9238795325112867385, 1.000000000000000000, 0.9238795325112867385, 1.000000000000000000, 0.9238795325112816315, 1.000000000000005107 ) ) 
 REPRESENTATION_ITEM ( '' )  );
#34705 = EDGE_CURVE ( 'NONE', #49354, #19379, #45620, .T. ) ;
#34706 = CARTESIAN_POINT ( 'NONE',  ( 5.000000000000000000, -18.37499999726881583, -6.123233995736766282E-16 ) ) ;
#34708 = EDGE_LOOP ( 'NONE', ( #28199, #36532, #29942, #39613 ) ) ;
#34707 = CARTESIAN_POINT ( 'NONE',  ( -4.458734124999999437, -50.31249999863440792, 0.000000000000000000 ) ) ;
#34709 = CARTESIAN_POINT ( 'NONE',  ( -10.12668159690567649, 1.240160820363494356E-15, -9.226681596905677907 ) ) ;
#34710 = CARTESIAN_POINT ( 'NONE',  ( 1.975475456537005874E-15, -15.62499999726881406, 5.000000000000000000 ) ) ;
#34712 = ORIENTED_EDGE ( 'NONE', *, *, #8713, .F. ) ;
#34711 = CARTESIAN_POINT ( 'NONE',  ( -2.229367062499996610, 0.6041666680322611560, 3.861377020970582219 ) ) ;
#34713 = CARTESIAN_POINT ( 'NONE',  ( -52.10840900171896806, -149.1875000013656063, 3.393966926194110556 ) ) ;
#34714 = CARTESIAN_POINT ( 'NONE',  ( -3.535250795749689387E-16, -67.25000000000000000, -5.773502691896257311 ) ) ;
#34715 = CARTESIAN_POINT ( 'NONE',  ( 3.152801135295366208, -153.8125000013656063, 3.152801135295367985 ) ) ;
#34716 = CARTESIAN_POINT ( 'NONE',  ( 9.457646018065525792E-16, -41.31249999863440081, 5.148502694627439702 ) ) ;
#34717 = CARTESIAN_POINT ( 'NONE',  ( 1.975475456537005874E-15, -23.75000000000000000, 5.000000000000000000 ) ) ;
#34718 = CARTESIAN_POINT ( 'NONE',  ( -2.071067811865475061, -161.6875000000000000, -5.000000000000000888 ) ) ;
#34719 = CARTESIAN_POINT ( 'NONE',  ( -4.999999999999998224, -56.79166666393547303, 2.886751345948131764 ) ) ;
#34720 = CARTESIAN_POINT ( 'NONE',  ( -57.89159099828107458, -127.9375000013656063, -3.393966926194107447 ) ) ;
#34721 = CARTESIAN_POINT ( 'NONE',  ( -2.229367062500000163, -8.729166665301073991, -3.861377020970580443 ) ) ;
#34722 = CARTESIAN_POINT ( 'NONE',  ( 4.458734124999999437, -48.06249999863440792, -5.460374474430324690E-16 ) ) ;
#34723 =( BOUNDED_CURVE ( )  B_SPLINE_CURVE ( 2, ( #7432, #7112, #37015, #52443, #37634, #31862, #42143, #21902, #17399 ),
 .UNSPECIFIED., .F., .F. ) 
 B_SPLINE_CURVE_WITH_KNOTS ( ( 3, 2, 2, 2, 3 ),
 ( 0.8249999999999997335, 0.8291666666666664964, 0.8333333333333331483, 0.8374999999999998002, 0.8416666666666664520 ),
 .UNSPECIFIED. ) 
 CURVE ( )  GEOMETRIC_REPRESENTATION_ITEM ( )  RATIONAL_B_SPLINE_CURVE ( ( 1.000000000000003997, 0.9238795325112826307, 1.000000000000000000, 0.9238795325112867385, 1.000000000000000000, 0.9238795325112867385, 1.000000000000000000, 0.9238795325112908463, 0.9999999999999958922 ) ) 
 REPRESENTATION_ITEM ( '' )  );
#34724 = LINE ( 'NONE', #15748, #45142 ) ;
#34725 = CARTESIAN_POINT ( 'NONE',  ( -1.846868145590734756, -148.1250000013655779, -4.458734125000000326 ) ) ;
#34726 = CARTESIAN_POINT ( 'NONE',  ( 4.458734124999999437, -91.06249999863440792, -5.460374474430324690E-16 ) ) ;
#34727 = CARTESIAN_POINT ( 'NONE',  ( -60.14911071818854538, -150.0625000000000000, 1.666127454062681146 ) ) ;
#34728 = ORIENTED_EDGE ( 'NONE', *, *, #1720, .F. ) ;
#34729 = EDGE_CURVE ( 'NONE', #23099, #39107, #25875, .T. ) ;
#34730 = FACE_OUTER_BOUND ( 'NONE', #20665, .T. ) ;
#34731 = CARTESIAN_POINT ( 'NONE',  ( 4.458734124999998549, 29.02083333469893134, -2.574251347313721627 ) ) ;
#34732 = CARTESIAN_POINT ( 'NONE',  ( -60.14911071818854538, -151.1875000027312126, 1.666127454062681368 ) ) ;
#34733 = ADVANCED_FACE ( 'NONE', ( #50640 ), #45172, .T. ) ;
#34734 = CARTESIAN_POINT ( 'NONE',  ( -1.339745962155613812, -62.20534180126146850, -5.000000000000000000 ) ) ;
#34735 = VERTEX_POINT ( 'NONE', #56434 ) ;
#34736 = CARTESIAN_POINT ( 'NONE',  ( -2.229367062499996610, 2.854166668032259935, 3.861377020970582219 ) ) ;
#34737 = EDGE_CURVE ( 'NONE', #26750, #2325, #58754, .T. ) ;
#34738 = CARTESIAN_POINT ( 'NONE',  ( -1.336351044127974539E-14, 21.37500000273118417, 5.000000000000000000 ) ) ;
#34739 = CARTESIAN_POINT ( 'NONE',  ( 4.458734124999999437, -19.06249999863440792, -5.460374474430324690E-16 ) ) ;
#34740 = DIRECTION ( 'NONE',  ( -0.000000000000000000, 1.000000000000000000, -0.000000000000000000 ) ) ;
#34741 = CARTESIAN_POINT ( 'NONE',  ( -4.458734124999998549, -4.229166665301070438, 2.574251347313722516 ) ) ;
#34742 = CARTESIAN_POINT ( 'NONE',  ( 0.000000000000000000, -120.0000000000000000, 5.000000000000000000 ) ) ;
#34743 = CARTESIAN_POINT ( 'NONE',  ( 2.730187237215162345E-16, -150.1875000013656063, -4.458734124999999437 ) ) ;
#34744 = VECTOR ( 'NONE', #44654, 1000.000000000000000 ) ;
#34745 = CARTESIAN_POINT ( 'NONE',  ( -4.458734124999999437, 20.43750000136559208, 0.000000000000000000 ) ) ;
#34746 = EDGE_LOOP ( 'NONE', ( #44286, #16573, #12150, #45354 ) ) ;
#34747 = CARTESIAN_POINT ( 'NONE',  ( 4.458734124999999437, -97.81249999863440792, -5.460374474430324690E-16 ) ) ;
#34748 = CARTESIAN_POINT ( 'NONE',  ( -2.500000000000000444, -75.16666666666665719, -4.330127018922193649 ) ) ;
#34749 = CARTESIAN_POINT ( 'NONE',  ( -1.339745962155613812, -104.0803417985302701, -5.000000000000000000 ) ) ;
#34750 = CARTESIAN_POINT ( 'NONE',  ( -4.458734124999998549, -14.22916666530107221, 2.574251347313722516 ) ) ;
#34751 = AXIS2_PLACEMENT_3D ( 'NONE', #27281, #8303, #12800 ) ;
#34752 = CARTESIAN_POINT ( 'NONE',  ( 7.500000000000002665, 3.988838049906435312, -0.8529248949437669980 ) ) ;
#34753 = DIRECTION ( 'NONE',  ( 0.000000000000000000, 0.000000000000000000, 1.000000000000000000 ) ) ;
#34754 = CARTESIAN_POINT ( 'NONE',  ( -59.29741812935640155, -149.6250000013655779, -2.196230717870135685 ) ) ;
#34755 = CARTESIAN_POINT ( 'NONE',  ( -2.500000000000000444, -41.04166666393548013, -4.330127018922193649 ) ) ;
#34756 = FACE_OUTER_BOUND ( 'NONE', #19943, .T. ) ;
#34757 = CARTESIAN_POINT ( 'NONE',  ( -4.458734124999999437, 13.60416666803226171, -2.574251347313719407 ) ) ;
#34758 = FACE_OUTER_BOUND ( 'NONE', #43804, .T. ) ;
#34759 = DIRECTION ( 'NONE',  ( -0.000000000000000000, 1.000000000000000000, -0.000000000000000000 ) ) ;
#34760 = CARTESIAN_POINT ( 'NONE',  ( 2.229367062500001939, 18.02083333469892779, 3.861377020970579999 ) ) ;
#34761 = CARTESIAN_POINT ( 'NONE',  ( 4.458734124999999437, -63.81249999863440792, -5.460374474430324690E-16 ) ) ;
#34762 = VERTEX_POINT ( 'NONE', #26515 ) ;
#34763 = CARTESIAN_POINT ( 'NONE',  ( -3.152548672688508926E-16, -7.812499998634405252, -5.148502694627439702 ) ) ;
#34764 = CARTESIAN_POINT ( 'NONE',  ( -5.000000000000000000, 1.916666666666667407, -2.886751345948128211 ) ) ;
#34765 = CARTESIAN_POINT ( 'NONE',  ( 3.152801135295366208, -166.5625000013656063, 3.152801135295367985 ) ) ;
#34766 = CARTESIAN_POINT ( 'NONE',  ( 5.000000000000000000, -63.37499999726880873, -6.123233995736766282E-16 ) ) ;
#34767 = CARTESIAN_POINT ( 'NONE',  ( 9.457646018065525792E-16, -51.06249999863440792, 5.148502694627439702 ) ) ;
#34768 = CARTESIAN_POINT ( 'NONE',  ( 1.060575238724906964E-15, -91.62499999726880162, 5.773502691896257311 ) ) ;
#34769 = CARTESIAN_POINT ( 'NONE',  ( 2.229367062499998831, -31.64583333196773651, -3.861377020970580887 ) ) ;
#34770 = CIRCLE ( 'NONE', #48125, 5.000000000000000000 ) ;
#34771 = CARTESIAN_POINT ( 'NONE',  ( 0.000000000000000000, -120.0000000000000000, 0.000000000000000000 ) ) ;
#34772 = CARTESIAN_POINT ( 'NONE',  ( 2.500000000000002220, -8.666666666666669627, 4.330127018922192761 ) ) ;
#34773 = CARTESIAN_POINT ( 'NONE',  ( 0.000000000000000000, 30.00000000000000000, 5.000000000000000000 ) ) ;
#34774 = CARTESIAN_POINT ( 'NONE',  ( 3.152801135295367541, -154.5625000013656063, -3.152801135295367541 ) ) ;
#34775 = CARTESIAN_POINT ( 'NONE',  ( 2.499999999999998668, -43.33333333333333570, -4.330127018922193649 ) ) ;
#34776 = DIRECTION ( 'NONE',  ( 1.000000000000000000, 0.000000000000000000, -0.000000000000000000 ) ) ;
#34777 = CARTESIAN_POINT ( 'NONE',  ( 0.000000000000000000, -170.0000000000000000, 5.000000000000000000 ) ) ;
#34778 = ORIENTED_EDGE ( 'NONE', *, *, #2715, .T. ) ;
#34779 = CARTESIAN_POINT ( 'NONE',  ( 4.458734124999998549, -100.7291666653010651, -2.574251347313721627 ) ) ;
#34780 = CARTESIAN_POINT ( 'NONE',  ( 4.458734124999998549, 1.020833334698927120, -2.574251347313721627 ) ) ;
#34781 =( BOUNDED_CURVE ( )  B_SPLINE_CURVE ( 2, ( #47066, #27433, #2689, #56086, #3331, #41583, #6882, #37412, #36459 ),
 .UNSPECIFIED., .F., .F. ) 
 B_SPLINE_CURVE_WITH_KNOTS ( ( 3, 2, 2, 2, 3 ),
 ( 0.6916666666666663188, 0.6958333333333329707, 0.6999999999999995115, 0.7041666666666662744, 0.7083333333333329263 ),
 .UNSPECIFIED. ) 
 CURVE ( )  GEOMETRIC_REPRESENTATION_ITEM ( )  RATIONAL_B_SPLINE_CURVE ( ( 1.000000000000005995, 0.9238795325112806323, 1.000000000000000000, 0.9238795325112867385, 1.000000000000000000, 0.9238795325112867385, 1.000000000000000000, 0.9238795325112948431, 0.9999999999999918954 ) ) 
 REPRESENTATION_ITEM ( '' )  );
#34782 = CARTESIAN_POINT ( 'NONE',  ( 1.975475456537005874E-15, -68.74999999999998579, 5.000000000000000000 ) ) ;
#34783 = CARTESIAN_POINT ( 'NONE',  ( 2.499999999999998668, -3.333333333333333925, -4.330127018922193649 ) ) ;
#34784 = CARTESIAN_POINT ( 'NONE',  ( 4.458734125000000326, -64.89583333196773651, 2.574251347313718519 ) ) ;
#34785 = ADVANCED_FACE ( 'NONE', ( #61573 ), #42251, .T. ) ;
#34786 = DIRECTION ( 'NONE',  ( 0.000000000000000000, 0.000000000000000000, 1.000000000000000000 ) ) ;
#34787 = B_SPLINE_CURVE_WITH_KNOTS ( 'NONE', 3,
 ( #24930, #14950, #14319, #53562, #43890, #63538, #9185, #18825, #58071, #59019, #29098, #38444, #34560, #14003, #14631, #33630, #48413, #54191, #48724, #19780, #53249, #52934, #44215, #53873, #63222 ),
 .UNSPECIFIED., .F., .F.,
 ( 4, 2, 2, 2, 2, 1, 2, 2, 2, 2, 2, 2, 4 ),
 ( 1.525486860402933621E-14, 0.001159901942158824556, 0.001739852913230607954, 0.002319803884302391352, 0.002899754855374174316, 0.003479705826445958147, 0.004059656797517741111, 0.004639607768589523208, 0.005799509710733074391, 0.006959411652876625574, 0.007539362623948399865, 0.008119313595020176758, 0.009279215537163704522 ),
 .UNSPECIFIED. ) ;
#34788 = CARTESIAN_POINT ( 'NONE',  ( -4.999999999999999112, -0.7916666639354794643, 2.886751345948131764 ) ) ;
#34790 = ORIENTED_EDGE ( 'NONE', *, *, #2880, .T. ) ;
#34789 = CARTESIAN_POINT ( 'NONE',  ( -2.229367062499996610, -35.14583333196772941, 3.861377020970582219 ) ) ;
#34791 = CARTESIAN_POINT ( 'NONE',  ( -6.972266317189433020E-16, 19.75000000000000000, -5.000000000000000000 ) ) ;
#34792 = CARTESIAN_POINT ( 'NONE',  ( 2.071067811865327624, -156.8125000000000284, -5.000000000000148326 ) ) ;
#34793 = ORIENTED_EDGE ( 'NONE', *, *, #14068, .F. ) ;
#34794 = CARTESIAN_POINT ( 'NONE',  ( 3.044556291839386294E-14, 12.75000000000000000, -5.000000000000000000 ) ) ;
#34795 = CARTESIAN_POINT ( 'NONE',  ( 2.500000000000002220, -51.66666666666666430, 4.330127018922192761 ) ) ;
#34797 = CARTESIAN_POINT ( 'NONE',  ( 2.229367062499998831, -25.89583333196773651, -3.861377020970580887 ) ) ;
#34796 = FACE_OUTER_BOUND ( 'NONE', #23889, .T. ) ;
#34798 = CARTESIAN_POINT ( 'NONE',  ( 5.000000000000000888, -32.45833333060215153, 2.886751345948126879 ) ) ;
#34799 = CARTESIAN_POINT ( 'NONE',  ( -2.229367062499996610, -72.14583333196773651, 3.861377020970582219 ) ) ;
#34800 = CARTESIAN_POINT ( 'NONE',  ( 3.152801135295367541, -142.5625000013655779, -3.152801135295367541 ) ) ;
#34801 = CARTESIAN_POINT ( 'NONE',  ( 9.457646018065525792E-16, -84.06249999863439371, 5.148502694627439702 ) ) ;
#34802 = VECTOR ( 'NONE', #14139, 1000.000000000000000 ) ;
#34803 = CARTESIAN_POINT ( 'NONE',  ( -59.59170313451811296, -139.7500000013656347, 1.485763867205729394 ) ) ;
#34804 = CARTESIAN_POINT ( 'NONE',  ( 4.458734124999998549, -29.97916666530107577, -2.574251347313721627 ) ) ;
#34805 = CARTESIAN_POINT ( 'NONE',  ( 5.000000000000000000, -70.29166666393547303, -2.886751345948129988 ) ) ;
#34806 = ORIENTED_EDGE ( 'NONE', *, *, #57825, .T. ) ;
#34807 = DIRECTION ( 'NONE',  ( -0.000000000000000000, 1.000000000000000000, -0.000000000000000000 ) ) ;
#34808 = ORIENTED_EDGE ( 'NONE', *, *, #31816, .T. ) ;
#34809 = CARTESIAN_POINT ( 'NONE',  ( -3.152548672688508926E-16, -73.81249999863440792, -5.148502694627439702 ) ) ;
#34810 = CARTESIAN_POINT ( 'NONE',  ( 0.000000000000000000, -120.0000000000000000, 0.000000000000000000 ) ) ;
#34811 = VERTEX_POINT ( 'NONE', #7851 ) ;
#34812 = CARTESIAN_POINT ( 'NONE',  ( 1.339745962155627135, 12.70534180126147739, -4.999999999999991118 ) ) ;
#34813 =( BOUNDED_CURVE ( )  B_SPLINE_CURVE ( 2, ( #30829, #31140, #46259, #2218, #26317, #41733, #56238, #21179, #60748 ),
 .UNSPECIFIED., .F., .F. ) 
 B_SPLINE_CURVE_WITH_KNOTS ( ( 3, 2, 2, 2, 3 ),
 ( 0.2354166666666666630, 0.2361111111111111049, 0.2374999999999999889, 0.2388888888888889006, 0.2395833333333333426 ),
 .UNSPECIFIED. ) 
 CURVE ( )  GEOMETRIC_REPRESENTATION_ITEM ( )  RATIONAL_B_SPLINE_CURVE ( ( 0.9330127018922194093, 0.9330127018922194093, 1.000000000000000000, 0.8660254037844387076, 1.000000000000000000, 0.8660254037844387076, 1.000000000000000000, 0.9330127018922194093, 0.9330127018922194093 ) ) 
 REPRESENTATION_ITEM ( '' )  );
#34814 = CARTESIAN_POINT ( 'NONE',  ( -9.184850993605147944E-16, -160.2500000000000000, 5.000000000000000000 ) ) ;
#34815 = CARTESIAN_POINT ( 'NONE',  ( 4.458734124999998549, -58.97916666530105800, -2.574251347313721627 ) ) ;
#34816 = CARTESIAN_POINT ( 'NONE',  ( -2.229367062500000163, -3.729166665301070438, -3.861377020970580443 ) ) ;
#34817 = ORIENTED_EDGE ( 'NONE', *, *, #33339, .F. ) ;
#34818 = VECTOR ( 'NONE', #19090, 1000.000000000000000 ) ;
#34819 = CARTESIAN_POINT ( 'NONE',  ( 1.975475456537005874E-15, -19.75000000000000000, 5.000000000000000000 ) ) ;
#34820 = CARTESIAN_POINT ( 'NONE',  ( 5.000000000000000000, -91.50000000000000000, -6.123233995736766282E-16 ) ) ;
#34821 = CARTESIAN_POINT ( 'NONE',  ( -4.458734124999999437, 11.60416666803225993, -2.574251347313719407 ) ) ;
#34822 = CARTESIAN_POINT ( 'NONE',  ( -59.44456063193725015, -140.5625000013656063, -0.3552334253322034230 ) ) ;
#34823 = CARTESIAN_POINT ( 'NONE',  ( 1.975475456537005874E-15, -73.75000000000000000, 5.000000000000000000 ) ) ;
#34824 = CARTESIAN_POINT ( 'NONE',  ( 2.730187237215162345E-16, -161.1875000013655779, -4.458734124999999437 ) ) ;
#34825 = EDGE_LOOP ( 'NONE', ( #47022, #27763, #52820, #20117 ) ) ;
#34826 = CARTESIAN_POINT ( 'NONE',  ( 4.458734124999998549, -80.72916666530106511, -2.574251347313721627 ) ) ;
#34827 = CARTESIAN_POINT ( 'NONE',  ( -6.972266317189433020E-16, -70.12499999726880162, -5.000000000000000000 ) ) ;
#34828 = CARTESIAN_POINT ( 'NONE',  ( -4.458734124999999437, 1.687500001365593194, 0.000000000000000000 ) ) ;
#34829 = CARTESIAN_POINT ( 'NONE',  ( 1.060575238724906964E-15, -86.75000000000000000, 5.773502691896257311 ) ) ;
#34830 = CARTESIAN_POINT ( 'NONE',  ( -1.339745962155610925, -42.66965819600731891, 5.000000000000000000 ) ) ;
#34831 = CARTESIAN_POINT ( 'NONE',  ( 2.229367062500001939, -63.22916666530106511, 3.861377020970579999 ) ) ;
#34832 = CARTESIAN_POINT ( 'NONE',  ( 2.499999999999998668, -26.20833333060214798, -4.330127018922193649 ) ) ;
#34833 = DIRECTION ( 'NONE',  ( -0.000000000000000000, 1.000000000000000000, -0.000000000000000000 ) ) ;
#34834 = CARTESIAN_POINT ( 'NONE',  ( 1.975475456537005874E-15, -46.62499999726880873, 5.000000000000000000 ) ) ;
#34835 = CARTESIAN_POINT ( 'NONE',  ( 1.339745962155615144, -61.70534180126146850, 4.999999999999999112 ) ) ;
#34836 = DIRECTION ( 'NONE',  ( 0.000000000000000000, 0.000000000000000000, 1.000000000000000000 ) ) ;
#34837 = CARTESIAN_POINT ( 'NONE',  ( 2.229367062500001939, -45.97916666530106511, 3.861377020970579999 ) ) ;
#34838 = PRODUCT_DEFINITION_SHAPE ( 'NONE', 'NONE',  #32748 ) ;
#34839 = CARTESIAN_POINT ( 'NONE',  ( -4.458734124999997661, -31.47916666530107577, 2.574251347313722516 ) ) ;
#34840 = CARTESIAN_POINT ( 'NONE',  ( -2.229367062499996610, 7.604166668032260823, 3.861377020970582219 ) ) ;
#34841 = VECTOR ( 'NONE', #6473, 1000.000000000000000 ) ;
#34842 = CARTESIAN_POINT ( 'NONE',  ( 5.000000000000000000, -146.1875000027312126, 2.071067811865478614 ) ) ;
#34843 = CARTESIAN_POINT ( 'NONE',  ( 5.000000000000000000, 20.49999999999999645, -6.123233995736766282E-16 ) ) ;
#34844 = CARTESIAN_POINT ( 'NONE',  ( -5.000000000000000000, -149.6250000027312126, -6.123233995736766282E-16 ) ) ;
#34845 = LINE ( 'NONE', #53817, #22327 ) ;
#34846 = EDGE_CURVE ( 'NONE', #50991, #63425, #42796, .T. ) ;
#34847 = VECTOR ( 'NONE', #49909, 1000.000000000000000 ) ;
#34848 = CARTESIAN_POINT ( 'NONE',  ( -4.458734124999999437, -35.39583333196773651, -2.574251347313719407 ) ) ;
#34849 = CARTESIAN_POINT ( 'NONE',  ( -2.500000000000000444, -72.04166666393548724, -4.330127018922193649 ) ) ;
#34850 = CARTESIAN_POINT ( 'NONE',  ( -59.59170313451811296, -145.7500000013655779, 1.485763867205729394 ) ) ;
#34851 = CARTESIAN_POINT ( 'NONE',  ( 1.975475456537005874E-15, -90.62499999726880162, 5.000000000000000000 ) ) ;
#34852 = CARTESIAN_POINT ( 'NONE',  ( 5.000000000000000888, -37.58333333333332860, 2.886751345948126879 ) ) ;
#34853 = CARTESIAN_POINT ( 'NONE',  ( 9.457646018065525792E-16, -82.31249999863440792, 5.148502694627439702 ) ) ;
#34854 = CARTESIAN_POINT ( 'NONE',  ( -1.846868145590737420, -167.0000000013655779, 4.458734124999997661 ) ) ;
#34855 = DIRECTION ( 'NONE',  ( -0.000000000000000000, 1.000000000000000000, -0.000000000000000000 ) ) ;
#34856 = DIRECTION ( 'NONE',  ( 0.000000000000000000, 1.000000000000000000, 0.000000000000000000 ) ) ;
#34857 = CARTESIAN_POINT ( 'NONE',  ( -5.000000000000000000, -25.00000000000000000, 0.000000000000000000 ) ) ;
#34858 = CARTESIAN_POINT ( 'NONE',  ( 3.152801135295367541, -144.3125000013655779, -3.152801135295367541 ) ) ;
#34859 = ORIENTED_EDGE ( 'NONE', *, *, #11469, .F. ) ;
#34860 = CARTESIAN_POINT ( 'NONE',  ( -3.535250795749689387E-16, -90.12499999726881583, -5.773502691896257311 ) ) ;
#34861 = ORIENTED_EDGE ( 'NONE', *, *, #63263, .T. ) ;
#34862 = CARTESIAN_POINT ( 'NONE',  ( 4.458734125000000326, -60.14583333196774362, 2.574251347313718519 ) ) ;
#34863 = CARTESIAN_POINT ( 'NONE',  ( 5.000000000000000000, 23.70833333606451632, -2.886751345948129988 ) ) ;
#34864 = CARTESIAN_POINT ( 'NONE',  ( 0.000000000000000000, -170.0000000000000000, 5.000000000000000000 ) ) ;
#34865 = CARTESIAN_POINT ( 'NONE',  ( 2.500000000000002220, 14.33333333333333393, 4.330127018922192761 ) ) ;
#34866 = AXIS2_PLACEMENT_3D ( 'NONE', #35493, #55111, #10081 ) ;
#34867 = CARTESIAN_POINT ( 'NONE',  ( -4.458734124999999437, -53.39583333196773651, -2.574251347313719407 ) ) ;
#34868 = CARTESIAN_POINT ( 'NONE',  ( 2.229367062500001939, -3.979166665301070438, 3.861377020970579999 ) ) ;
#34869 = CARTESIAN_POINT ( 'NONE',  ( 0.000000000000000000, -170.0000000000000000, 0.000000000000000000 ) ) ;
#34870 = CARTESIAN_POINT ( 'NONE',  ( -50.18089887299977647, -145.8125000027311842, 2.462841084822515292 ) ) ;
#34871 = DIRECTION ( 'NONE',  ( -0.000000000000000000, 1.000000000000000000, -0.000000000000000000 ) ) ;
#34872 = CARTESIAN_POINT ( 'NONE',  ( 5.000000000000000888, -166.9375000000000284, -2.071067811865475505 ) ) ;
#34873 = CARTESIAN_POINT ( 'NONE',  ( -6.972266317189433020E-16, -21.24999999999999289, -5.000000000000000000 ) ) ;
#34875 = CARTESIAN_POINT ( 'NONE',  ( 4.458734124999998549, -20.72916666530106866, -2.574251347313721627 ) ) ;
#34874 = CARTESIAN_POINT ( 'NONE',  ( -55.39835681537999790, -150.8750000000000284, 4.984105922594378235 ) ) ;
#34876 = CARTESIAN_POINT ( 'NONE',  ( 2.500000000000002220, 17.45833333606451987, 4.330127018922192761 ) ) ;
#34877 = CARTESIAN_POINT ( 'NONE',  ( 4.458734124999998549, -51.72916666530107221, -2.574251347313721627 ) ) ;
#34878 = CARTESIAN_POINT ( 'NONE',  ( 4.458734125000000326, -154.6250000013655779, -1.846868145590734978 ) ) ;
#34879 = CARTESIAN_POINT ( 'NONE',  ( -3.535250795749689387E-16, -54.12499999726880162, -5.773502691896257311 ) ) ;
#34880 = ORIENTED_EDGE ( 'NONE', *, *, #24937, .T. ) ;
#34881 = CARTESIAN_POINT ( 'NONE',  ( 1.975475456537005874E-15, -47.62499999726880873, 5.000000000000000000 ) ) ;
#34882 = CARTESIAN_POINT ( 'NONE',  ( 4.458734124999998549, 5.020833334698926897, -2.574251347313721627 ) ) ;
#34883 = VERTEX_POINT ( 'NONE', #46131 ) ;
#34885 = DIRECTION ( 'NONE',  ( -0.000000000000000000, 1.000000000000000000, -0.000000000000000000 ) ) ;
#34884 = DIRECTION ( 'NONE',  ( 0.000000000000000000, 0.000000000000000000, 1.000000000000000000 ) ) ;
#34886 = CARTESIAN_POINT ( 'NONE',  ( -1.846868145590734756, -155.1250000013655779, -4.458734125000000326 ) ) ;
#34887 = ORIENTED_EDGE ( 'NONE', *, *, #17311, .F. ) ;
#34888 = CARTESIAN_POINT ( 'NONE',  ( 5.000000000000000000, -23.37499999726881228, -6.123233995736766282E-16 ) ) ;
#34889 = CARTESIAN_POINT ( 'NONE',  ( -50.18089887299979068, -128.6875000000000284, 2.462841084822635640 ) ) ;
#34891 = AXIS2_PLACEMENT_3D ( 'NONE', #53359, #42761, #58187 ) ;
#34890 = CARTESIAN_POINT ( 'NONE',  ( 2.071067811865645591, -153.1875000000000000, 4.999999999999830358 ) ) ;
#34892 = CARTESIAN_POINT ( 'NONE',  ( 2.229367062499998831, -43.89583333196774362, -3.861377020970580887 ) ) ;
#34893 = EDGE_LOOP ( 'NONE', ( #20795, #10121, #20571, #62979 ) ) ;
#34894 = CARTESIAN_POINT ( 'NONE',  ( 2.499999999999998668, -103.2083333306021444, -4.330127018922193649 ) ) ;
#34895 = CARTESIAN_POINT ( 'NONE',  ( 4.458734124999999437, 11.18750000136559386, -5.460374474430324690E-16 ) ) ;
#34896 = CARTESIAN_POINT ( 'NONE',  ( -4.458734124999998549, -90.47916666530106511, 2.574251347313722516 ) ) ;
#34897 = CARTESIAN_POINT ( 'NONE',  ( -59.44456063193725015, -151.5625000013656063, -0.3552334253322034230 ) ) ;
#34898 = DIRECTION ( 'NONE',  ( 0.000000000000000000, 0.000000000000000000, 1.000000000000000000 ) ) ;
#34899 = PLANE ( 'NONE',  #10004 ) ;
#34900 = CARTESIAN_POINT ( 'NONE',  ( -75.00000000000002842, 0.000000000000000000, 5.000000000000000000 ) ) ;
#34901 = CARTESIAN_POINT ( 'NONE',  ( -4.458734124999999437, -63.31249999863440792, 0.000000000000000000 ) ) ;
#34902 = CARTESIAN_POINT ( 'NONE',  ( -5.000000000000000000, 10.04166666939785024, -2.886751345948128211 ) ) ;
#34903 = CARTESIAN_POINT ( 'NONE',  ( 2.229367062500001939, 18.02083333469892779, 3.861377020970579999 ) ) ;
#34904 =( BOUNDED_CURVE ( )  B_SPLINE_CURVE ( 2, ( #43847, #63493, #48995, #47744, #33274, #3700, #23315, #62563, #8829 ),
 .UNSPECIFIED., .F., .T. ) 
 B_SPLINE_CURVE_WITH_KNOTS ( ( 3, 2, 2, 2, 3 ),
 ( 0.2250000000000001998, 0.2291666666666668517, 0.2333333333333335313, 0.2375000000000001832, 0.2416666666666668628 ),
 .UNSPECIFIED. ) 
 CURVE ( )  GEOMETRIC_REPRESENTATION_ITEM ( )  RATIONAL_B_SPLINE_CURVE ( ( 0.9999999999999964473, 0.9238795325112902912, 1.000000000000000000, 0.9238795325112867385, 1.000000000000000000, 0.9238795325112867385, 1.000000000000000000, 0.9238795325112831858, 1.000000000000003553 ) ) 
 REPRESENTATION_ITEM ( '' )  );
#34905 = CARTESIAN_POINT ( 'NONE',  ( 2.500000000000002220, -33.66666666666666430, 4.330127018922192761 ) ) ;
#34906 = CARTESIAN_POINT ( 'NONE',  ( -2.229367062499996610, -49.39583333196772941, 3.861377020970582219 ) ) ;
#34907 = CARTESIAN_POINT ( 'NONE',  ( 2.499999999999998668, -7.208333330602150646, -4.330127018922193649 ) ) ;
#34908 = CARTESIAN_POINT ( 'NONE',  ( -5.000000000000000000, 24.99999999999999645, 0.000000000000000000 ) ) ;
#34909 = DIRECTION ( 'NONE',  ( -0.000000000000000000, 1.000000000000000000, -0.000000000000000000 ) ) ;
#34910 = CYLINDRICAL_SURFACE ( 'NONE', #51019, 5.000000000000000000 ) ;
#34911 = CARTESIAN_POINT ( 'NONE',  ( -55.00000000000001421, -135.0000000000000284, 8.082903768654762899 ) ) ;
#34912 = CARTESIAN_POINT ( 'NONE',  ( -4.458734124999999437, -15.56249999863440436, 0.000000000000000000 ) ) ;
#34913 = ORIENTED_EDGE ( 'NONE', *, *, #58518, .T. ) ;
#34914 = FACE_OUTER_BOUND ( 'NONE', #27191, .T. ) ;
#34915 = CARTESIAN_POINT ( 'NONE',  ( 4.458734124999999437, -102.8124999986344079, -5.460374474430324690E-16 ) ) ;
#34916 = CARTESIAN_POINT ( 'NONE',  ( 5.000000000000000888, -160.0625000027312126, -2.071067811865475505 ) ) ;
#34917 = CARTESIAN_POINT ( 'NONE',  ( -3.152548672688508926E-16, -95.81249999863440792, -5.148502694627439702 ) ) ;
#34918 = ADVANCED_FACE ( 'NONE', ( #32601 ), #8171, .F. ) ;
#34919 = CARTESIAN_POINT ( 'NONE',  ( -5.000000000000000000, -8.000000000000000000, 0.000000000000000000 ) ) ;
#34920 = CARTESIAN_POINT ( 'NONE',  ( 5.000000000000000000, -56.37499999726880162, -6.123233995736766282E-16 ) ) ;
#34921 = CARTESIAN_POINT ( 'NONE',  ( 5.000000000000000000, -62.29166666393547303, -2.886751345948130876 ) ) ;
#34922 = CARTESIAN_POINT ( 'NONE',  ( -54.64476657466781973, -154.0625000013656347, -4.444560631937228834 ) ) ;
#34923 = CARTESIAN_POINT ( 'NONE',  ( -51.60603307380591787, -143.9375000013656063, -2.891590998281053704 ) ) ;
#34924 = CARTESIAN_POINT ( 'NONE',  ( 2.229367062499998831, -16.64583333196773651, -3.861377020970580887 ) ) ;
#34925 = CARTESIAN_POINT ( 'NONE',  ( -4.458734124999999437, 7.437500001365594748, 0.000000000000000000 ) ) ;
#34926 = CARTESIAN_POINT ( 'NONE',  ( 4.458734125000000326, -64.14583333196773651, 2.574251347313718519 ) ) ;
#34927 = LINE ( 'NONE', #49397, #6956 ) ;
#34928 = CARTESIAN_POINT ( 'NONE',  ( -2.229367062500000163, -18.47916666530106866, -3.861377020970580443 ) ) ;
#34929 = CARTESIAN_POINT ( 'NONE',  ( -1.339745962155613812, -80.08034179853028434, -5.000000000000000000 ) ) ;
#34930 = CARTESIAN_POINT ( 'NONE',  ( -3.535533905932738641, -154.3750000000000000, 3.535533905932737309 ) ) ;
#34931 = CARTESIAN_POINT ( 'NONE',  ( -5.000000000000000000, -6.999999999999999112, 0.000000000000000000 ) ) ;
#34932 = CARTESIAN_POINT ( 'NONE',  ( -3.152801135295367096, -156.0625000013656063, -3.152801135295367541 ) ) ;
#34933 = EDGE_LOOP ( 'NONE', ( #30943, #23344, #30919, #22572 ) ) ;
#34934 = CARTESIAN_POINT ( 'NONE',  ( -4.458734124999999437, -45.56249999863440081, 0.000000000000000000 ) ) ;
#34935 = CARTESIAN_POINT ( 'NONE',  ( 5.000000000000000000, -44.29166666393546592, -2.886751345948130876 ) ) ;
#34936 = CARTESIAN_POINT ( 'NONE',  ( -6.972266317189433020E-16, -66.24999999999998579, -5.000000000000000000 ) ) ;
#34937 = CARTESIAN_POINT ( 'NONE',  ( -2.229367062500000163, -88.47916666530106511, -3.861377020970580443 ) ) ;
#34938 = CARTESIAN_POINT ( 'NONE',  ( -3.152548672688508926E-16, -90.56249999863440792, -5.148502694627439702 ) ) ;
#34939 = CARTESIAN_POINT ( 'NONE',  ( 2.229367062500001939, 13.77083333469892779, 3.861377020970579999 ) ) ;
#34940 = CARTESIAN_POINT ( 'NONE',  ( 4.458734125000001214, 7.104166668032259047, 2.574251347313718519 ) ) ;
#34941 = EDGE_CURVE ( 'NONE', #11847, #24623, #12027, .T. ) ;
#34942 = CARTESIAN_POINT ( 'NONE',  ( 5.000000000000000000, -82.50000000000000000, -6.123233995736766282E-16 ) ) ;
#34943 = EDGE_CURVE ( 'NONE', #33786, #11102, #1684, .T. ) ;
#34944 = CARTESIAN_POINT ( 'NONE',  ( -6.972266317189433020E-16, -68.12499999726881583, -5.000000000000000000 ) ) ;
#34945 = CYLINDRICAL_SURFACE ( 'NONE', #53990, 5.000000000000000000 ) ;
#34946 = CARTESIAN_POINT ( 'NONE',  ( 9.457646018065525792E-16, 18.68750000136559208, 5.148502694627439702 ) ) ;
#34947 = CARTESIAN_POINT ( 'NONE',  ( 2.499999999999998668, -75.33333333333332860, -4.330127018922193649 ) ) ;
#34948 = CARTESIAN_POINT ( 'NONE',  ( -2.500000000000000444, 6.958333336064520758, -4.330127018922193649 ) ) ;
#34949 = VERTEX_POINT ( 'NONE', #32283 ) ;
#34950 = CARTESIAN_POINT ( 'NONE',  ( 0.000000000000000000, -170.0000000000000000, 0.000000000000000000 ) ) ;
#34951 = VERTEX_POINT ( 'NONE', #61892 ) ;
#34952 = DIRECTION ( 'NONE',  ( 0.000000000000000000, 0.000000000000000000, 1.000000000000000000 ) ) ;
#34953 = CARTESIAN_POINT ( 'NONE',  ( 2.229367062500001939, -36.97916666530107221, 3.861377020970579999 ) ) ;
#34954 = EDGE_CURVE ( 'NONE', #5308, #37292, #51291, .T. ) ;
#34955 = CARTESIAN_POINT ( 'NONE',  ( -4.999999999999999112, -37.79166666393547303, 2.886751345948131764 ) ) ;
#34956 = EDGE_LOOP ( 'NONE', ( #45657, #31965, #55754, #4477 ) ) ;
#34957 = CARTESIAN_POINT ( 'NONE',  ( -58.39396692619412477, -146.6875000013656063, 2.891590998281057701 ) ) ;
#34958 = CARTESIAN_POINT ( 'NONE',  ( 9.457646018065525792E-16, -10.06249999863440792, 5.148502694627439702 ) ) ;
#34960 = ORIENTED_EDGE ( 'NONE', *, *, #50629, .T. ) ;
#34959 = CARTESIAN_POINT ( 'NONE',  ( 4.458734124999999437, -20.06249999863440081, -5.460374474430324690E-16 ) ) ;
#34961 =( BOUNDED_CURVE ( )  B_SPLINE_CURVE ( 2, ( #5940, #41284, #2090, #20410, #11700, #30364, #45806, #25546, #21694 ),
 .UNSPECIFIED., .F., .F. ) 
 B_SPLINE_CURVE_WITH_KNOTS ( ( 3, 2, 2, 2, 3 ),
 ( 0.3750000000000002776, 0.3791666666666669294, 0.3833333333333336368, 0.3875000000000003442, 0.3916666666666669960 ),
 .UNSPECIFIED. ) 
 CURVE ( )  GEOMETRIC_REPRESENTATION_ITEM ( )  RATIONAL_B_SPLINE_CURVE ( ( 0.9999999999999948930, 0.9238795325112918455, 1.000000000000000000, 0.9238795325112867385, 1.000000000000000000, 0.9238795325112867385, 1.000000000000000000, 0.9238795325112806323, 1.000000000000005995 ) ) 
 REPRESENTATION_ITEM ( '' )  );
#34962 = CARTESIAN_POINT ( 'NONE',  ( -4.999999999999999112, -83.91666666666667140, 2.886751345948131764 ) ) ;
#34963 = DIRECTION ( 'NONE',  ( 0.000000000000000000, 0.000000000000000000, 1.000000000000000000 ) ) ;
#34964 = CARTESIAN_POINT ( 'NONE',  ( 4.458734124999998549, -64.97916666530106511, -2.574251347313721627 ) ) ;
#34965 =( BOUNDED_CURVE ( )  B_SPLINE_CURVE ( 2, ( #26246, #6015, #40079, #21112, #6326, #20798, #36223, #26574, #55215 ),
 .UNSPECIFIED., .F., .F. ) 
 B_SPLINE_CURVE_WITH_KNOTS ( ( 3, 2, 2, 2, 3 ),
 ( 0.5910714285714285809, 0.5916666666666666741, 0.5928571428571428603, 0.5940476190476190466, 0.5946428571428571397 ),
 .UNSPECIFIED. ) 
 CURVE ( )  GEOMETRIC_REPRESENTATION_ITEM ( )  RATIONAL_B_SPLINE_CURVE ( ( 0.9330127018922194093, 0.9330127018922194093, 1.000000000000000000, 0.8660254037844387076, 1.000000000000000000, 0.8660254037844387076, 1.000000000000000000, 0.9330127018922194093, 0.9330127018922194093 ) ) 
 REPRESENTATION_ITEM ( '' )  );
#34966 = CARTESIAN_POINT ( 'NONE',  ( 2.499999999999998668, -86.20833333060214443, -4.330127018922193649 ) ) ;
#34968 = ORIENTED_EDGE ( 'NONE', *, *, #20327, .T. ) ;
#34967 = CARTESIAN_POINT ( 'NONE',  ( -5.000000000000000000, -18.00000000000000355, 0.000000000000000000 ) ) ;
#34969 = CARTESIAN_POINT ( 'NONE',  ( -50.01589407740564042, -140.6250000000000284, 0.3983568153799778022 ) ) ;
#34970 = CARTESIAN_POINT ( 'NONE',  ( 2.229367062499998831, -26.89583333196774007, -3.861377020970580887 ) ) ;
#34971 = CARTESIAN_POINT ( 'NONE',  ( 1.339745962155615144, -41.58034179853029144, 4.999999999999999112 ) ) ;
#34972 = ORIENTED_EDGE ( 'NONE', *, *, #14939, .T. ) ;
#34973 = CARTESIAN_POINT ( 'NONE',  ( -4.458734125000001214, -163.1250000013656063, 1.846868145590734089 ) ) ;
#34974 = ADVANCED_FACE ( 'NONE', ( #56106 ), #57066, .T. ) ;
#34975 = CARTESIAN_POINT ( 'NONE',  ( -3.152548672688508926E-16, -109.8124999986343795, -5.148502694627439702 ) ) ;
#34976 = DIRECTION ( 'NONE',  ( -0.000000000000000000, 1.000000000000000000, -0.000000000000000000 ) ) ;
#34977 = VERTEX_POINT ( 'NONE', #41291 ) ;
#34978 = CARTESIAN_POINT ( 'NONE',  ( -50.70258187064364108, -147.3750000013656063, 2.196230717870141014 ) ) ;
#34979=STYLED_ITEM('',(#63698),#28816);
#34980 = CARTESIAN_POINT ( 'NONE',  ( -2.229367062500000163, -73.72916666530106511, -3.861377020970580443 ) ) ;
#34981 = CARTESIAN_POINT ( 'NONE',  ( -56.66612745406270335, -133.4375000027312126, -5.149110718188516067 ) ) ;
#34982 = CARTESIAN_POINT ( 'NONE',  ( 4.458734124999999437, -42.81249999863440081, -5.460374474430324690E-16 ) ) ;
#34983 = CARTESIAN_POINT ( 'NONE',  ( 4.458734124999999437, -147.6875000013656063, 0.000000000000000000 ) ) ;
#34984 = CARTESIAN_POINT ( 'NONE',  ( 0.000000000000000000, -170.0000000000000000, 5.000000000000000000 ) ) ;
#34985 = CARTESIAN_POINT ( 'NONE',  ( -4.458734124999999437, -49.31249999863440792, 0.000000000000000000 ) ) ;
#34986 = CARTESIAN_POINT ( 'NONE',  ( -59.98410592259440222, -135.1250000000000284, -0.3983568153799752487 ) ) ;
#34987 = CARTESIAN_POINT ( 'NONE',  ( -3.152548672688508926E-16, -14.56249999863440436, -5.148502694627439702 ) ) ;
#34988 = CARTESIAN_POINT ( 'NONE',  ( 5.000000000000000888, -100.5833333333333144, 2.886751345948126879 ) ) ;
#34989 = CARTESIAN_POINT ( 'NONE',  ( -8.190561711645485556E-16, -141.9375000013656063, 4.458734124999999437 ) ) ;
#34990 = CARTESIAN_POINT ( 'NONE',  ( -4.458734124999999437, -31.56249999863440436, 0.000000000000000000 ) ) ;
#34991 = CARTESIAN_POINT ( 'NONE',  ( 5.000000000000000000, 4.625000002731187720, -6.123233995736766282E-16 ) ) ;
#34992 = CARTESIAN_POINT ( 'NONE',  ( -5.000000000000000000, -52.99999999999999289, 0.000000000000000000 ) ) ;
#34993 = CARTESIAN_POINT ( 'NONE',  ( -59.29741812935640155, -130.6250000013656347, -2.196230717870135685 ) ) ;
#34994 = CARTESIAN_POINT ( 'NONE',  ( 2.229367062500001939, -76.22916666530106511, 3.861377020970579999 ) ) ;
#34995 = CARTESIAN_POINT ( 'NONE',  ( 0.000000000000000000, -120.0000000000000000, 0.000000000000000000 ) ) ;
#34996 = CARTESIAN_POINT ( 'NONE',  ( 0.000000000000000000, -120.0000000000000000, 5.000000000000000000 ) ) ;
#34997 = CARTESIAN_POINT ( 'NONE',  ( -7.263825692932299738, -4.945657111639584436, -7.907570769506049757 ) ) ;
#34998 = CARTESIAN_POINT ( 'NONE',  ( -4.458734124999999437, 0.3541666680322609340, -2.574251347313719407 ) ) ;
#34999 = VERTEX_POINT ( 'NONE', #16858 ) ;
#35000 = CARTESIAN_POINT ( 'NONE',  ( 5.000000000000000000, -146.0000000000000284, 0.000000000000000000 ) ) ;
#35001 = LINE ( 'NONE', #10230, #14393 ) ;
#35003 = CARTESIAN_POINT ( 'NONE',  ( -2.229367062499996610, -36.14583333196773651, 3.861377020970582219 ) ) ;
#35002 = CARTESIAN_POINT ( 'NONE',  ( -4.458734124999999437, -86.31249999863439371, 0.000000000000000000 ) ) ;
#35004 = CARTESIAN_POINT ( 'NONE',  ( -54.60164318462004474, -143.5000000027312126, -4.984105922594373794 ) ) ;
#35005 = CARTESIAN_POINT ( 'NONE',  ( 2.229367062499998831, -81.89583333196773651, -3.861377020970580887 ) ) ;
#35006 = EDGE_CURVE ( 'NONE', #50566, #14032, #43162, .T. ) ;
#35007 = CARTESIAN_POINT ( 'NONE',  ( -4.458734124999997661, 18.52083333469892779, 2.574251347313722516 ) ) ;
#35008 = CARTESIAN_POINT ( 'NONE',  ( 0.000000000000000000, -170.0000000000000000, 0.000000000000000000 ) ) ;
#35009 = CARTESIAN_POINT ( 'NONE',  ( -52.10840900171896806, -137.1875000013656063, 3.393966926194110556 ) ) ;
#35010 = ADVANCED_FACE ( 'NONE', ( #8787 ), #4582, .T. ) ;
#35011 = EDGE_CURVE ( 'NONE', #141, #11953, #18927, .T. ) ;
#35012 = CARTESIAN_POINT ( 'NONE',  ( -3.152548672688508926E-16, 0.4375000013655955255, -5.148502694627439702 ) ) ;
#35013 = CARTESIAN_POINT ( 'NONE',  ( -4.458734124999999437, 21.35416666803225993, -2.574251347313719407 ) ) ;
#35014 = CARTESIAN_POINT ( 'NONE',  ( 2.229367062500001939, -48.22916666530106511, 3.861377020970579999 ) ) ;
#35015 = CARTESIAN_POINT ( 'NONE',  ( 0.000000000000000000, -120.0000000000000000, 0.000000000000000000 ) ) ;
#35016 = CARTESIAN_POINT ( 'NONE',  ( 4.458734125000000326, -5.895833331967740953, 2.574251347313718519 ) ) ;
#35017 = CARTESIAN_POINT ( 'NONE',  ( 9.457646018065525792E-16, -29.31249999863440436, 5.148502694627439702 ) ) ;
#35018 =( BOUNDED_CURVE ( )  B_SPLINE_CURVE ( 2, ( #16409, #50175, #40521, #11884, #5797, #6127, #35710, #11572, #36026 ),
 .UNSPECIFIED., .F., .F. ) 
 B_SPLINE_CURVE_WITH_KNOTS ( ( 3, 2, 2, 2, 3 ),
 ( 0.3053571428571428825, 0.3059523809523809756, 0.3071428571428571619, 0.3083333333333333481, 0.3089285714285714413 ),
 .UNSPECIFIED. ) 
 CURVE ( )  GEOMETRIC_REPRESENTATION_ITEM ( )  RATIONAL_B_SPLINE_CURVE ( ( 0.9330127018922194093, 0.9330127018922194093, 1.000000000000000000, 0.8660254037844387076, 1.000000000000000000, 0.8660254037844387076, 1.000000000000000000, 0.9330127018922194093, 0.9330127018922194093 ) ) 
 REPRESENTATION_ITEM ( '' )  );
#35019 = CARTESIAN_POINT ( 'NONE',  ( -53.51423613279429503, -130.5000000013656063, 4.591703134518082763 ) ) ;
#35020 = CARTESIAN_POINT ( 'NONE',  ( 4.458734125000001214, -73.89583333196773651, 2.574251347313718519 ) ) ;
#35021 = CARTESIAN_POINT ( 'NONE',  ( -4.999999999999999112, -104.7916666639354730, 2.886751345948131764 ) ) ;
#35022 = EDGE_CURVE ( 'NONE', #592, #17293, #24206, .T. ) ;
#35023 = CARTESIAN_POINT ( 'NONE',  ( 2.229367062500001939, 25.02083333469892779, 3.861377020970579999 ) ) ;
#35024 = DIRECTION ( 'NONE',  ( -0.000000000000000000, 1.000000000000000000, -0.000000000000000000 ) ) ;
#35025 = EDGE_CURVE ( 'NONE', #24115, #17875, #9101, .T. ) ;
#35026 = DIRECTION ( 'NONE',  ( -0.000000000000000000, 1.000000000000000000, -0.000000000000000000 ) ) ;
#35027 = CARTESIAN_POINT ( 'NONE',  ( 4.458734124999998549, -78.97916666530106511, -2.574251347313721627 ) ) ;
#35028 = CARTESIAN_POINT ( 'NONE',  ( -4.999999999999999112, -60.91666666666666430, 2.886751345948131764 ) ) ;
#35029 = CARTESIAN_POINT ( 'NONE',  ( 1.339745962155612702, -36.16965819600732601, -5.000000000000000000 ) ) ;
#35030 = CARTESIAN_POINT ( 'NONE',  ( 1.060575238724906964E-15, 22.37500000273118772, 5.773502691896257311 ) ) ;
#35031 = ORIENTED_EDGE ( 'NONE', *, *, #23550, .F. ) ;
#35032 = CARTESIAN_POINT ( 'NONE',  ( -6.972266317189433020E-16, -1.124999997268814278, -5.000000000000000000 ) ) ;
#35033 = DIRECTION ( 'NONE',  ( -0.000000000000000000, 1.000000000000000000, -0.000000000000000000 ) ) ;
#35034 = CARTESIAN_POINT ( 'NONE',  ( 2.499999999999998668, -17.33333333333333215, -4.330127018922193649 ) ) ;
#35035 = CARTESIAN_POINT ( 'NONE',  ( -4.458734124999999437, -21.39583333196774007, -2.574251347313719407 ) ) ;
#35036 = VECTOR ( 'NONE', #62251, 1000.000000000000114 ) ;
#35037 = CARTESIAN_POINT ( 'NONE',  ( 2.229367062499998831, -80.64583333196773651, -3.861377020970580887 ) ) ;
#35038 = CARTESIAN_POINT ( 'NONE',  ( -3.535250795749689387E-16, -22.12499999726881228, -5.773502691896257311 ) ) ;
#35040 = ORIENTED_EDGE ( 'NONE', *, *, #62642, .F. ) ;
#35039 = CARTESIAN_POINT ( 'NONE',  ( 4.458734124999999437, -51.81249999863440792, -5.460374474430324690E-16 ) ) ;
#35041 = CARTESIAN_POINT ( 'NONE',  ( -4.999999999999998224, -75.79166666393547303, 2.886751345948131764 ) ) ;
#35042 = CARTESIAN_POINT ( 'NONE',  ( 5.000000000000000000, 27.70833333606451987, -2.886751345948130876 ) ) ;
#35044 = ORIENTED_EDGE ( 'NONE', *, *, #46061, .T. ) ;
#35043 = CARTESIAN_POINT ( 'NONE',  ( 4.458734124999998549, 3.020833334698928674, -2.574251347313721627 ) ) ;
#35045 = CARTESIAN_POINT ( 'NONE',  ( -56.48576386720575471, -150.7500000013655779, -4.591703134518078322 ) ) ;
#35046 = CARTESIAN_POINT ( 'NONE',  ( -2.500000000000000444, -67.16666666666667140, -4.330127018922193649 ) ) ;
#35047 = CARTESIAN_POINT ( 'NONE',  ( -4.458734124999999437, -152.1875000013656063, -5.460374474430324690E-16 ) ) ;
#35048 = CARTESIAN_POINT ( 'NONE',  ( 2.229367062500001939, -46.22916666530106511, 3.861377020970579999 ) ) ;
#35049 = CARTESIAN_POINT ( 'NONE',  ( -1.339745962155610925, -76.66965819600731891, 5.000000000000000000 ) ) ;
#35050 = CARTESIAN_POINT ( 'NONE',  ( -5.000000000000000000, -158.5000000000000000, -6.123233995736766282E-16 ) ) ;
#35051 = DIRECTION ( 'NONE',  ( -0.000000000000000000, 1.000000000000000000, -0.000000000000000000 ) ) ;
#35052 = CARTESIAN_POINT ( 'NONE',  ( -52.80376928212989185, -126.1250000013656205, -4.297418129356379346 ) ) ;
#35053 = CARTESIAN_POINT ( 'NONE',  ( 2.229367062500001939, -11.22916666530107044, 3.861377020970579999 ) ) ;
#35054 = CARTESIAN_POINT ( 'NONE',  ( -4.458734124999999437, -46.56249999863440792, 0.000000000000000000 ) ) ;
#35055 = FACE_OUTER_BOUND ( 'NONE', #33956, .T. ) ;
#35056 = CARTESIAN_POINT ( 'NONE',  ( -1.846868145590737420, -143.7500000013655779, 4.458734124999999437 ) ) ;
#35057 = CARTESIAN_POINT ( 'NONE',  ( 9.457646018065525792E-16, -89.31249999863440792, 5.148502694627439702 ) ) ;
#35058 = CARTESIAN_POINT ( 'NONE',  ( -7.500000000000000000, -4.330127018922199866, -1.000000000000000888 ) ) ;
#35059 = VERTEX_POINT ( 'NONE', #52546 ) ;
#35060 = FACE_OUTER_BOUND ( 'NONE', #59074, .T. ) ;
#35061 = DIRECTION ( 'NONE',  ( 0.4999999999999951150, 0.000000000000000000, -0.8660254037844414832 ) ) ;
#35062 = CARTESIAN_POINT ( 'NONE',  ( -50.01589407740564042, -147.7500000027312126, 0.3983568153799778022 ) ) ;
#35063 = CARTESIAN_POINT ( 'NONE',  ( -5.000000000000000000, -62.08333333333332860, -2.886751345948128211 ) ) ;
#35064 = ORIENTED_EDGE ( 'NONE', *, *, #8612, .T. ) ;
#35065 = CARTESIAN_POINT ( 'NONE',  ( 4.458734125000001214, 3.104166668032260379, 2.574251347313718519 ) ) ;
#35066 = CARTESIAN_POINT ( 'NONE',  ( -1.049326080737009628E-13, -19.75000000000000000, 5.000000000000000000 ) ) ;
#35067 = CARTESIAN_POINT ( 'NONE',  ( 4.458734125000001214, -20.14583333196774007, 2.574251347313718519 ) ) ;
#35068 = CARTESIAN_POINT ( 'NONE',  ( 4.458734124999999437, -4.812499998634402587, -5.460374474430324690E-16 ) ) ;
#35069 = CARTESIAN_POINT ( 'NONE',  ( 5.000000000000000000, -73.37499999726880162, -6.123233995736766282E-16 ) ) ;
#35070 = CARTESIAN_POINT ( 'NONE',  ( 4.458734124999997661, -147.5000000013656063, 1.846868145590737864 ) ) ;
#35071 = CARTESIAN_POINT ( 'NONE',  ( -2.229367062500000163, 17.27083333469892779, -3.861377020970580443 ) ) ;
#35072 = VERTEX_POINT ( 'NONE', #23272 ) ;
#35073 = CARTESIAN_POINT ( 'NONE',  ( 2.229367062500001939, -95.97916666530105090, 3.861377020970579999 ) ) ;
#35074 = CARTESIAN_POINT ( 'NONE',  ( 2.499999999999998668, -71.20833333060214443, -4.330127018922193649 ) ) ;
#35075 = CARTESIAN_POINT ( 'NONE',  ( -4.458734124999999437, -21.31249999863440436, 0.000000000000000000 ) ) ;
#35076 = CARTESIAN_POINT ( 'NONE',  ( 7.499999999999999112, 0.7513028741560161539, -0.02472015219302839059 ) ) ;
#35077 = CARTESIAN_POINT ( 'NONE',  ( 1.339745962155612702, -3.294658198738522170, -5.000000000000000000 ) ) ;
#35078 = CARTESIAN_POINT ( 'NONE',  ( -57.89159099828107458, -148.6875000013656063, -3.393966926194107447 ) ) ;
#35079 = EDGE_CURVE ( 'NONE', #57060, #31680, #13617, .T. ) ;
#35080 = CARTESIAN_POINT ( 'NONE',  ( -5.000000000000000000, -43.87499999726880873, 0.000000000000000000 ) ) ;
#35081 = CARTESIAN_POINT ( 'NONE',  ( -6.972266317189433020E-16, 12.87500000273118417, -5.000000000000000000 ) ) ;
#35082 = CARTESIAN_POINT ( 'NONE',  ( -4.458734124999999437, 14.60416666803226171, -2.574251347313719407 ) ) ;
#35083 = CARTESIAN_POINT ( 'NONE',  ( -4.999999999999998224, -8.791666663935483683, 2.886751345948131764 ) ) ;
#35084 = FACE_OUTER_BOUND ( 'NONE', #12585, .T. ) ;
#35085 = CARTESIAN_POINT ( 'NONE',  ( 9.457646018065525792E-16, 14.93750000136559386, 5.148502694627439702 ) ) ;
#35086 = CARTESIAN_POINT ( 'NONE',  ( -3.152548672688508926E-16, -61.56249999863440792, -5.148502694627439702 ) ) ;
#35087 = ORIENTED_EDGE ( 'NONE', *, *, #43472, .T. ) ;
#35088 = CARTESIAN_POINT ( 'NONE',  ( -4.458734124999997661, -12.47916666530107044, 2.574251347313722516 ) ) ;
#35089 = EDGE_CURVE ( 'NONE', #27389, #28458, #8244, .T. ) ;
#35090 = CARTESIAN_POINT ( 'NONE',  ( -2.500000000000000444, 5.833333333333333037, -4.330127018922193649 ) ) ;
#35091 = CARTESIAN_POINT ( 'NONE',  ( -4.458734125000001214, -161.8750000013656063, 1.846868145590734089 ) ) ;
#35092 = CARTESIAN_POINT ( 'NONE',  ( 4.458734124999998549, -57.72916666530107221, -2.574251347313721627 ) ) ;
#35093 = CARTESIAN_POINT ( 'NONE',  ( -3.535250795749689387E-16, -89.12499999726880162, -5.773502691896257311 ) ) ;
#35094 = CARTESIAN_POINT ( 'NONE',  ( 2.229367062499998831, -33.64583333196772941, -3.861377020970580887 ) ) ;
#35095 = ADVANCED_FACE ( 'NONE', ( #18744 ), #62521, .T. ) ;
#35096 = ADVANCED_FACE ( 'NONE', ( #33235 ), #13922, .T. ) ;
#35097 =( BOUNDED_CURVE ( )  B_SPLINE_CURVE ( 2, ( #58852, #9330, #24765, #28943, #49837, #4508, #4825, #44369, #15 ),
 .UNSPECIFIED., .F., .F. ) 
 B_SPLINE_CURVE_WITH_KNOTS ( ( 3, 2, 2, 2, 3 ),
 ( 0.8145833333333333259, 0.8152777777777777679, 0.8166666666666666519, 0.8180555555555555358, 0.8187499999999999778 ),
 .UNSPECIFIED. ) 
 CURVE ( )  GEOMETRIC_REPRESENTATION_ITEM ( )  RATIONAL_B_SPLINE_CURVE ( ( 0.9330127018922194093, 0.9330127018922194093, 1.000000000000000000, 0.8660254037844387076, 1.000000000000000000, 0.8660254037844387076, 1.000000000000000000, 0.9330127018922194093, 0.9330127018922194093 ) ) 
 REPRESENTATION_ITEM ( '' )  );
#35098 = CYLINDRICAL_SURFACE ( 'NONE', #36003, 5.000000000000000000 ) ;
#35099 = CARTESIAN_POINT ( 'NONE',  ( -5.000000000000000000, -54.95833333060214443, -2.886751345948128211 ) ) ;
#35100 = CARTESIAN_POINT ( 'NONE',  ( -1.339745962155610925, -107.6696581960073189, 5.000000000000000000 ) ) ;
#35101 = CARTESIAN_POINT ( 'NONE',  ( 1.339745962155615144, -16.58034179853029499, 4.999999999999999112 ) ) ;
#35102 = CARTESIAN_POINT ( 'NONE',  ( -3.152801135295367096, -154.3125000013656063, -3.152801135295367541 ) ) ;
#35103 = CARTESIAN_POINT ( 'NONE',  ( 5.000000000000000000, -44.50000000000000000, -6.123233995736766282E-16 ) ) ;
#35104 = DIRECTION ( 'NONE',  ( -0.000000000000000000, 1.000000000000000000, -0.000000000000000000 ) ) ;
#35105 = EDGE_CURVE ( 'NONE', #27768, #35769, #23895, .T. ) ;
#35106 = CARTESIAN_POINT ( 'NONE',  ( -6.031010364368858512E-14, 2.375000002731183280, 5.000000000000000000 ) ) ;
#35107 = VERTEX_POINT ( 'NONE', #57690 ) ;
#35108 = CARTESIAN_POINT ( 'NONE',  ( 4.458734124999999437, -98.81249999863440792, -5.460374474430324690E-16 ) ) ;
#35109 = CARTESIAN_POINT ( 'NONE',  ( 9.457646018065525792E-16, 0.6875000013655957476, 5.148502694627439702 ) ) ;
#35110 = CARTESIAN_POINT ( 'NONE',  ( -5.000000000000000000, -8.958333330602144429, -2.886751345948128211 ) ) ;
#35111 = EDGE_CURVE ( 'NONE', #25453, #44367, #14789, .T. ) ;
#35112 = CARTESIAN_POINT ( 'NONE',  ( -5.000000000000000000, -4.999999999999997335, 0.000000000000000000 ) ) ;
#35113 = CARTESIAN_POINT ( 'NONE',  ( 4.458734124999998549, -66.72916666530106511, -2.574251347313721627 ) ) ;
#35115 = CARTESIAN_POINT ( 'NONE',  ( 1.339745962155615144, -22.58034179853029144, 4.999999999999999112 ) ) ;
#35114 =( BOUNDED_CURVE ( )  B_SPLINE_CURVE ( 2, ( #45055, #1022, #50197, #6148, #60185, #25764, #20942, #45376, #35732 ),
 .UNSPECIFIED., .F., .F. ) 
 B_SPLINE_CURVE_WITH_KNOTS ( ( 3, 2, 2, 2, 3 ),
 ( 0.5053571428571428381, 0.5059523809523809312, 0.5071428571428571175, 0.5083333333333333037, 0.5089285714285713969 ),
 .UNSPECIFIED. ) 
 CURVE ( )  GEOMETRIC_REPRESENTATION_ITEM ( )  RATIONAL_B_SPLINE_CURVE ( ( 0.9330127018922194093, 0.9330127018922194093, 1.000000000000000000, 0.8660254037844387076, 1.000000000000000000, 0.8660254037844387076, 1.000000000000000000, 0.9330127018922194093, 0.9330127018922194093 ) ) 
 REPRESENTATION_ITEM ( '' )  );
#35116 = EDGE_CURVE ( 'NONE', #63012, #19213, #27953, .T. ) ;
#35117 = CARTESIAN_POINT ( 'NONE',  ( 5.000000000000000000, -6.291666663935480130, -2.886751345948129988 ) ) ;
#35119 = ORIENTED_EDGE ( 'NONE', *, *, #17017, .T. ) ;
#35118 = CARTESIAN_POINT ( 'NONE',  ( 4.458734124999999437, -32.81249999863440792, -5.460374474430324690E-16 ) ) ;
#35120 = CARTESIAN_POINT ( 'NONE',  ( 3.253724281355068545E-15, 27.87500000273118417, -5.000000000000000000 ) ) ;
#35121 = ORIENTED_EDGE ( 'NONE', *, *, #22380, .T. ) ;
#35122 = CARTESIAN_POINT ( 'NONE',  ( -6.972266317189433020E-16, -49.12499999726880162, -5.000000000000000000 ) ) ;
#35123 = CARTESIAN_POINT ( 'NONE',  ( -5.000000000000000000, -49.08333333333332860, -2.886751345948128211 ) ) ;
#35125 = CARTESIAN_POINT ( 'NONE',  ( 4.458734124999999437, -30.06249999863440436, -5.460374474430324690E-16 ) ) ;
#35124 = CARTESIAN_POINT ( 'NONE',  ( 0.000000000000000000, -120.0000000000000000, 0.000000000000000000 ) ) ;
#35126 = CARTESIAN_POINT ( 'NONE',  ( -2.500000000000000444, 13.95833333606451809, -4.330127018922193649 ) ) ;
#35127 = CARTESIAN_POINT ( 'NONE',  ( 2.229367062499998831, -76.64583333196773651, -3.861377020970580887 ) ) ;
#35128 = CARTESIAN_POINT ( 'NONE',  ( 1.846868145590735200, -143.5000000013656063, -4.458734125000000326 ) ) ;
#35129 = CARTESIAN_POINT ( 'NONE',  ( 4.458734124999999437, -83.81249999863439371, -5.460374474430324690E-16 ) ) ;
#35130 = CARTESIAN_POINT ( 'NONE',  ( -58.39396692619412477, -137.6875000013656063, 2.891590998281057701 ) ) ;
#35131 = CARTESIAN_POINT ( 'NONE',  ( -3.152548672688508926E-16, -30.81249999863440436, -5.148502694627439702 ) ) ;
#35132 = CARTESIAN_POINT ( 'NONE',  ( 2.499999999999998668, -74.20833333060214443, -4.330127018922193649 ) ) ;
#35133 = ORIENTED_EDGE ( 'NONE', *, *, #44884, .T. ) ;
#35134 = DIRECTION ( 'NONE',  ( 0.000000000000000000, -1.000000000000000000, 0.000000000000000000 ) ) ;
#35135 = VERTEX_POINT ( 'NONE', #44769 ) ;
#35136 = CARTESIAN_POINT ( 'NONE',  ( -4.458734124999999437, -74.56249999863440792, 0.000000000000000000 ) ) ;
#35137 = CYLINDRICAL_SURFACE ( 'NONE', #39929, 5.000000000000000000 ) ;
#35138 = ORIENTED_EDGE ( 'NONE', *, *, #52689, .T. ) ;
#35139 = CARTESIAN_POINT ( 'NONE',  ( 5.000000000000000888, 27.41666666666666430, 2.886751345948126879 ) ) ;
#35140 = LINE ( 'NONE', #6189, #54790 ) ;
#35141 = CARTESIAN_POINT ( 'NONE',  ( 4.458734124999998549, -66.97916666530107932, -2.574251347313721627 ) ) ;
#35142 = CARTESIAN_POINT ( 'NONE',  ( 2.229367062499998831, -4.895833331967740065, -3.861377020970580887 ) ) ;
#35143 = VERTEX_POINT ( 'NONE', #39940 ) ;
#35144 = CARTESIAN_POINT ( 'NONE',  ( 0.000000000000000000, -170.0000000000000000, 0.000000000000000000 ) ) ;
#35145 = FACE_OUTER_BOUND ( 'NONE', #11007, .T. ) ;
#35146 = CARTESIAN_POINT ( 'NONE',  ( 4.458734125000001214, 11.10416666803225993, 2.574251347313718519 ) ) ;
#35147 = CARTESIAN_POINT ( 'NONE',  ( -52.80376928212989185, -140.8750000013656063, -4.297418129356379346 ) ) ;
#35148 = CARTESIAN_POINT ( 'NONE',  ( 2.500000000000002220, -27.54166666393548013, 4.330127018922192761 ) ) ;
#35149 = CARTESIAN_POINT ( 'NONE',  ( 3.152801135295367541, -160.3125000013656063, -3.152801135295367541 ) ) ;
#35150 = CARTESIAN_POINT ( 'NONE',  ( 5.000000000000000000, -109.4999999999999858, -6.123233995736766282E-16 ) ) ;
#35151 = VERTEX_POINT ( 'NONE', #34814 ) ;
#35152 = CARTESIAN_POINT ( 'NONE',  ( -4.458734124999997661, -79.22916666530106511, 2.574251347313722516 ) ) ;
#35153 = DIRECTION ( 'NONE',  ( 0.000000000000000000, 0.000000000000000000, 1.000000000000000000 ) ) ;
#35154 = CARTESIAN_POINT ( 'NONE',  ( 4.458734124999999437, 2.187500001365593416, -5.460374474430324690E-16 ) ) ;
#35155 = DIRECTION ( 'NONE',  ( 0.000000000000000000, 0.000000000000000000, 1.000000000000000000 ) ) ;
#35156 = DIRECTION ( 'NONE',  ( 0.000000000000000000, 0.000000000000000000, 1.000000000000000000 ) ) ;
#35157 = CARTESIAN_POINT ( 'NONE',  ( -3.152548672688508926E-16, -67.81249999863440792, -5.148502694627439702 ) ) ;
#35158 = CARTESIAN_POINT ( 'NONE',  ( 1.060575238724906964E-15, -25.62499999726881583, 5.773502691896257311 ) ) ;
#35159 = CARTESIAN_POINT ( 'NONE',  ( -5.000000000000000000, -72.87499999726880162, 0.000000000000000000 ) ) ;
#35160 = CARTESIAN_POINT ( 'NONE',  ( 4.458734125000000326, 29.10416666803226349, 2.574251347313718519 ) ) ;
#35161 = CARTESIAN_POINT ( 'NONE',  ( 2.500000000000002220, -110.5416666639354730, 4.330127018922192761 ) ) ;
#35162 = CARTESIAN_POINT ( 'NONE',  ( -6.972266317189433020E-16, 25.74999999999999645, -5.000000000000000000 ) ) ;
#35163 = CARTESIAN_POINT ( 'NONE',  ( -4.458734124999999437, -47.31249999863440792, 0.000000000000000000 ) ) ;
#35164 = CARTESIAN_POINT ( 'NONE',  ( -2.229367062500000163, -29.72916666530107221, -3.861377020970580443 ) ) ;
#35165 = CARTESIAN_POINT ( 'NONE',  ( 4.458734125000000326, 2.854166668032259491, 2.574251347313718519 ) ) ;
#35166 =( BOUNDED_CURVE ( )  B_SPLINE_CURVE ( 2, ( #24959, #44564, #522, #20132, #54548, #30084, #49714, #44893, #17543 ),
 .UNSPECIFIED., .F., .F. ) 
 B_SPLINE_CURVE_WITH_KNOTS ( ( 3, 2, 2, 2, 3 ),
 ( 0.9083333333333332149, 0.9124999999999998668, 0.9166666666666665186, 0.9208333333333330595, 0.9249999999999998224 ),
 .UNSPECIFIED. ) 
 CURVE ( )  GEOMETRIC_REPRESENTATION_ITEM ( )  RATIONAL_B_SPLINE_CURVE ( ( 1.000000000000001998, 0.9238795325112847401, 1.000000000000000000, 0.9238795325112867385, 1.000000000000000000, 0.9238795325112867385, 1.000000000000000000, 0.9238795325112908463, 0.9999999999999958922 ) ) 
 REPRESENTATION_ITEM ( '' )  );
#35167 = CARTESIAN_POINT ( 'NONE',  ( -3.535533905932737309, -161.7500000027312126, -3.535533905932738197 ) ) ;
#35168 = CARTESIAN_POINT ( 'NONE',  ( 5.000000000000000000, 22.58333333333333570, -2.886751345948129988 ) ) ;
#35169 = CARTESIAN_POINT ( 'NONE',  ( -5.000000000000000888, -146.6875000027312126, -2.071067811865475949 ) ) ;
#35170 = CARTESIAN_POINT ( 'NONE',  ( -2.500000000000000444, 28.83333333333333215, -4.330127018922193649 ) ) ;
#35171 = CARTESIAN_POINT ( 'NONE',  ( 2.229367062499998831, -38.64583333196773651, -3.861377020970580887 ) ) ;
#35172 = CARTESIAN_POINT ( 'NONE',  ( -5.000000000000000000, -71.95833333060214443, -2.886751345948128211 ) ) ;
#35173 = CARTESIAN_POINT ( 'NONE',  ( -57.19623071787017210, -145.6250000013655779, 4.297418129356382899 ) ) ;
#35174 = CYLINDRICAL_SURFACE ( 'NONE', #1077, 5.000000000000000000 ) ;
#35175 = CARTESIAN_POINT ( 'NONE',  ( -9.184850993605147944E-16, -141.3750000027312126, 5.000000000000000000 ) ) ;
#35176 = CARTESIAN_POINT ( 'NONE',  ( -2.229367062499996610, -79.39583333196773651, 3.861377020970582219 ) ) ;
#35177 = CARTESIAN_POINT ( 'NONE',  ( 4.458734124999999437, -164.6250000013656063, -1.846868145590734978 ) ) ;
#35178 = CARTESIAN_POINT ( 'NONE',  ( 5.000000000000000000, 18.62500000273118772, -6.123233995736766282E-16 ) ) ;
#35179 = LINE ( 'NONE', #50281, #21545 ) ;
#35180 = CARTESIAN_POINT ( 'NONE',  ( 2.500000000000002220, -29.66666666666666785, 4.330127018922192761 ) ) ;
#35181 = CARTESIAN_POINT ( 'NONE',  ( 4.458734125000000326, -143.3750000013656063, -1.846868145590734978 ) ) ;
#35182 = EDGE_LOOP ( 'NONE', ( #7547, #55910, #2630, #43030 ) ) ;
#35183 = CARTESIAN_POINT ( 'NONE',  ( 9.457646018065525792E-16, 22.68750000136559564, 5.148502694627439702 ) ) ;
#35184 = VERTEX_POINT ( 'NONE', #45738 ) ;
#35185 = CARTESIAN_POINT ( 'NONE',  ( 9.457646018065525792E-16, -62.31249999863440792, 5.148502694627439702 ) ) ;
#35186 = CARTESIAN_POINT ( 'NONE',  ( -2.499999999999996447, 19.29166666939785202, 4.330127018922195425 ) ) ;
#35187 = CARTESIAN_POINT ( 'NONE',  ( -9.184850993605147944E-16, -139.3750000027312126, 5.000000000000000000 ) ) ;
#35188 = CARTESIAN_POINT ( 'NONE',  ( -5.000000000000000000, 12.91666666666666785, -2.886751345948128211 ) ) ;
#35189 = CARTESIAN_POINT ( 'NONE',  ( -2.229367062500000163, -51.47916666530107221, -3.861377020970580443 ) ) ;
#35190 = CARTESIAN_POINT ( 'NONE',  ( -2.229367062500000163, -13.47916666530107221, -3.861377020970580443 ) ) ;
#35191 = CARTESIAN_POINT ( 'NONE',  ( -5.000000000000000000, 3.916666666666665630, -2.886751345948128211 ) ) ;
#35192 = CARTESIAN_POINT ( 'NONE',  ( -6.972266317189433020E-16, -44.12499999726880162, -5.000000000000000000 ) ) ;
#35193 = CARTESIAN_POINT ( 'NONE',  ( 5.000000000000000000, -158.1250000027311842, 0.000000000000000000 ) ) ;
#35194 = CARTESIAN_POINT ( 'NONE',  ( 5.000000000000000000, 28.62500000273118417, -6.123233995736766282E-16 ) ) ;
#35195 = CARTESIAN_POINT ( 'NONE',  ( 1.975475456537005874E-15, -9.750000000000000000, 5.000000000000000000 ) ) ;
#35196 =( BOUNDED_CURVE ( )  B_SPLINE_CURVE ( 2, ( #24281, #54834, #58696, #43883, #63531, #4979, #53866, #10763, #34237 ),
 .UNSPECIFIED., .F., .F. ) 
 B_SPLINE_CURVE_WITH_KNOTS ( ( 3, 2, 2, 2, 3 ),
 ( 0.6312499999999999778, 0.6319444444444444198, 0.6333333333333333037, 0.6347222222222221877, 0.6354166666666666297 ),
 .UNSPECIFIED. ) 
 CURVE ( )  GEOMETRIC_REPRESENTATION_ITEM ( )  RATIONAL_B_SPLINE_CURVE ( ( 0.9330127018922194093, 0.9330127018922194093, 1.000000000000000000, 0.8660254037844387076, 1.000000000000000000, 0.8660254037844387076, 1.000000000000000000, 0.9330127018922194093, 0.9330127018922194093 ) ) 
 REPRESENTATION_ITEM ( '' )  );
#35198 = CARTESIAN_POINT ( 'NONE',  ( -2.229367062499996610, -22.14583333196773651, 3.861377020970582219 ) ) ;
#35197 = CARTESIAN_POINT ( 'NONE',  ( -1.339745962155610925, -78.79465819873851729, 5.000000000000000000 ) ) ;
#35199 = CARTESIAN_POINT ( 'NONE',  ( -51.19402409849444524, -135.6250000027312410, -3.242614290531456334 ) ) ;
#35200 = CARTESIAN_POINT ( 'NONE',  ( 4.458734124999998549, -57.72916666530107221, -2.574251347313721627 ) ) ;
#35201 = CARTESIAN_POINT ( 'NONE',  ( -1.846868145590737420, -156.0000000013656063, 4.458734124999999437 ) ) ;
#35202 = CARTESIAN_POINT ( 'NONE',  ( 5.000000000000000888, -55.45833333060214443, 2.886751345948126879 ) ) ;
#35203 = VERTEX_POINT ( 'NONE', #20340 ) ;
#35204 = CARTESIAN_POINT ( 'NONE',  ( 4.458734125000001214, -3.145833331967738733, 2.574251347313718519 ) ) ;
#35205 = ORIENTED_EDGE ( 'NONE', *, *, #16429, .T. ) ;
#35206 = CARTESIAN_POINT ( 'NONE',  ( 2.499999999999998668, -21.33333333333333570, -4.330127018922193649 ) ) ;
#35207 = CARTESIAN_POINT ( 'NONE',  ( -4.458734125000001214, -157.8750000013656063, 1.846868145590734089 ) ) ;
#35208 = VERTEX_POINT ( 'NONE', #15833 ) ;
#35209 = CARTESIAN_POINT ( 'NONE',  ( 0.000000000000000000, -170.0000000000000000, 0.000000000000000000 ) ) ;
#35210 = CARTESIAN_POINT ( 'NONE',  ( -55.39835681537999790, -129.8750000000000284, 4.984105922594378235 ) ) ;
#35211 = CARTESIAN_POINT ( 'NONE',  ( 5.000000000000000888, -152.9375000000000000, -2.071067811865475505 ) ) ;
#35212 = CARTESIAN_POINT ( 'NONE',  ( -3.152548672688508926E-16, -42.81249999863440081, -5.148502694627439702 ) ) ;
#35213 = EDGE_LOOP ( 'NONE', ( #20732, #45954, #53717, #50700 ) ) ;
#35214 = CARTESIAN_POINT ( 'NONE',  ( 2.071067811865517694, -142.9375000027312126, -4.999999999999958256 ) ) ;
#35215 = CARTESIAN_POINT ( 'NONE',  ( 4.458734124999999437, 16.18750000136559564, -5.460374474430324690E-16 ) ) ;
#35216 = CARTESIAN_POINT ( 'NONE',  ( -4.458734124999999437, 27.68750000136559208, 0.000000000000000000 ) ) ;
#35217 = CARTESIAN_POINT ( 'NONE',  ( -59.29741812935640155, -153.6250000013655779, -2.196230717870135685 ) ) ;
#35218 = CARTESIAN_POINT ( 'NONE',  ( 0.000000000000000000, -170.0000000000000000, 5.000000000000000000 ) ) ;
#35219 = CARTESIAN_POINT ( 'NONE',  ( -2.499999999999996447, -35.70833333060213732, 4.330127018922195425 ) ) ;
#35220 = DIRECTION ( 'NONE',  ( -0.000000000000000000, 1.000000000000000000, -0.000000000000000000 ) ) ;
#35221 = CARTESIAN_POINT ( 'NONE',  ( 4.458734125000000326, -67.89583333196773651, 2.574251347313718519 ) ) ;
#35222 = DIRECTION ( 'NONE',  ( -0.000000000000000000, 1.000000000000000000, -0.000000000000000000 ) ) ;
#35223 = CARTESIAN_POINT ( 'NONE',  ( -4.458734124999999437, 20.60416666803225993, -2.574251347313719407 ) ) ;
#35224 = CARTESIAN_POINT ( 'NONE',  ( 5.000000000000000000, -33.41666666666666430, -2.886751345948130876 ) ) ;
#35225 = CARTESIAN_POINT ( 'NONE',  ( -4.999999999999998224, -1.791666663935480353, 2.886751345948131764 ) ) ;
#35226 = CARTESIAN_POINT ( 'NONE',  ( -4.458734124999999437, -47.56249999863440792, 0.000000000000000000 ) ) ;
#35227 = CARTESIAN_POINT ( 'NONE',  ( -5.000000000000000000, -9.874999997268815832, 0.000000000000000000 ) ) ;
#35228 = CARTESIAN_POINT ( 'NONE',  ( -6.972266317189433020E-16, 4.749999999999999112, -5.000000000000000000 ) ) ;
#35229 = CARTESIAN_POINT ( 'NONE',  ( -5.000000000000000000, -65.95833333060213022, -2.886751345948128211 ) ) ;
#35230 = CARTESIAN_POINT ( 'NONE',  ( -4.458734124999999437, -88.56249999863439371, 0.000000000000000000 ) ) ;
#35231 = LINE ( 'NONE', #1159, #4905 ) ;
#35232 = CARTESIAN_POINT ( 'NONE',  ( -4.458734124999997661, -17.47916666530106866, 2.574251347313722516 ) ) ;
#35233 = ORIENTED_EDGE ( 'NONE', *, *, #27971, .T. ) ;
#35234 = CARTESIAN_POINT ( 'NONE',  ( -2.500000000000000444, -47.04166666393547303, -4.330127018922193649 ) ) ;
#35235 = CARTESIAN_POINT ( 'NONE',  ( 9.457646018065525792E-16, -103.0624999986344221, 5.148502694627439702 ) ) ;
#35236 = CARTESIAN_POINT ( 'NONE',  ( 5.000000000000000000, -162.1250000027311842, 0.000000000000000000 ) ) ;
#35237 = ORIENTED_EDGE ( 'NONE', *, *, #24754, .T. ) ;
#35238 = CARTESIAN_POINT ( 'NONE',  ( 4.458734124999998549, -98.97916666530105090, -2.574251347313721627 ) ) ;
#35239 = CARTESIAN_POINT ( 'NONE',  ( 3.535533905932736864, -163.2500000027312126, 3.535533905932738641 ) ) ;
#35240 = CARTESIAN_POINT ( 'NONE',  ( 5.000000000000000000, -55.29166666393548013, -2.886751345948129988 ) ) ;
#35241 = CARTESIAN_POINT ( 'NONE',  ( -6.972266317189433020E-16, 18.87500000273119127, -5.000000000000000000 ) ) ;
#35242 = CARTESIAN_POINT ( 'NONE',  ( -50.55543936806279248, -126.0625000013655921, 0.3552334253322060320 ) ) ;
#35243 = CARTESIAN_POINT ( 'NONE',  ( -57.89159099828107458, -143.6875000013656063, -3.393966926194107447 ) ) ;
#35244 = CARTESIAN_POINT ( 'NONE',  ( -3.152548672688508926E-16, -21.56249999863440792, -5.148502694627439702 ) ) ;
#35245 = CARTESIAN_POINT ( 'NONE',  ( 2.229367062500001939, 5.770833334698927786, 3.861377020970579999 ) ) ;
#35246 = CARTESIAN_POINT ( 'NONE',  ( 4.458734124999998549, -62.97916666530106511, -2.574251347313721627 ) ) ;
#35247 = CARTESIAN_POINT ( 'NONE',  ( 5.000000000000000000, -48.29166666393548724, -2.886751345948130876 ) ) ;
#35248 = CARTESIAN_POINT ( 'NONE',  ( -4.458734124999999437, -17.31249999863440792, 0.000000000000000000 ) ) ;
#35249 = CARTESIAN_POINT ( 'NONE',  ( 3.061616997868383141E-16, -154.7500000000000000, -5.000000000000000000 ) ) ;
#35250 = CARTESIAN_POINT ( 'NONE',  ( 5.000000000000000000, -13.49999999999999822, -6.123233995736766282E-16 ) ) ;
#35251 = CARTESIAN_POINT ( 'NONE',  ( -3.152801135295367096, -155.0625000013656063, -3.152801135295367541 ) ) ;
#35252 = ORIENTED_EDGE ( 'NONE', *, *, #56601, .T. ) ;
#35253 = CARTESIAN_POINT ( 'NONE',  ( -4.458734124999999437, -47.64583333196775072, -2.574251347313719407 ) ) ;
#35254 = CARTESIAN_POINT ( 'NONE',  ( 5.000000000000000000, 21.62500000273118417, -6.123233995736766282E-16 ) ) ;
#35255 = CARTESIAN_POINT ( 'NONE',  ( 5.000000000000000888, -38.45833333060213732, 2.886751345948126879 ) ) ;
#35256 = CARTESIAN_POINT ( 'NONE',  ( 2.499999999999998668, 28.66666666666666785, -4.330127018922193649 ) ) ;
#35257 = CARTESIAN_POINT ( 'NONE',  ( -4.458734124999999437, 3.604166668032260379, -2.574251347313719407 ) ) ;
#35258 = DIRECTION ( 'NONE',  ( -0.000000000000000000, 1.000000000000000000, -0.000000000000000000 ) ) ;
#35259 = CYLINDRICAL_SURFACE ( 'NONE', #31722, 5.000000000000000888 ) ;
#35260 = CARTESIAN_POINT ( 'NONE',  ( 1.339745962155612702, -82.29465819873851729, -5.000000000000000000 ) ) ;
#35261 = CARTESIAN_POINT ( 'NONE',  ( 4.458734124999998549, 19.02083333469892779, -2.574251347313721627 ) ) ;
#35262 = CARTESIAN_POINT ( 'NONE',  ( -2.499999999999996447, -76.83333333333334281, 4.330127018922195425 ) ) ;
#35263 = CARTESIAN_POINT ( 'NONE',  ( -2.499999999999996447, 7.291666669397852019, 4.330127018922195425 ) ) ;
#35264 = ORIENTED_EDGE ( 'NONE', *, *, #20959, .T. ) ;
#35265 = CARTESIAN_POINT ( 'NONE',  ( 0.000000000000000000, -120.0000000000000000, 5.000000000000000000 ) ) ;
#35266 = ORIENTED_EDGE ( 'NONE', *, *, #36996, .F. ) ;
#35267 = LINE ( 'NONE', #15965, #24515 ) ;
#35268 = CARTESIAN_POINT ( 'NONE',  ( 4.458734124999999437, -36.81249999863440792, -5.460374474430324690E-16 ) ) ;
#35269 = AXIS2_PLACEMENT_3D ( 'NONE', #4134, #13147, #62048 ) ;
#35270 = CARTESIAN_POINT ( 'NONE',  ( 5.000000000000000000, -41.29166666393548013, -2.886751345948129988 ) ) ;
#35271 = ORIENTED_EDGE ( 'NONE', *, *, #15773, .F. ) ;
#35272 = CARTESIAN_POINT ( 'NONE',  ( 4.458734125000001214, -11.89583333196774007, 2.574251347313718519 ) ) ;
#35273 = ORIENTED_EDGE ( 'NONE', *, *, #4031, .F. ) ;
#35274 = CARTESIAN_POINT ( 'NONE',  ( -2.500000000000000444, -84.16666666666667140, -4.330127018922193649 ) ) ;
#35275 = CARTESIAN_POINT ( 'NONE',  ( -5.000000000000000000, 1.041666669397853351, -2.886751345948128211 ) ) ;
#35276 = CARTESIAN_POINT ( 'NONE',  ( 4.458734125000001214, -62.14583333196774362, 2.574251347313718519 ) ) ;
#35277 = CARTESIAN_POINT ( 'NONE',  ( 5.000000000000000000, -89.29166666393545881, -2.886751345948129988 ) ) ;
#35279 = ORIENTED_EDGE ( 'NONE', *, *, #2009, .T. ) ;
#35278 = CARTESIAN_POINT ( 'NONE',  ( -6.972266317189433020E-16, -49.12499999726880162, -5.000000000000000000 ) ) ;
#35280 = CARTESIAN_POINT ( 'NONE',  ( -50.18089887299979068, -141.6875000000000000, 2.462841084822635640 ) ) ;
#35281 = EDGE_CURVE ( 'NONE', #30690, #42274, #54245, .T. ) ;
#35282 = CARTESIAN_POINT ( 'NONE',  ( 4.458734124999998549, -25.97916666530106866, -2.574251347313721627 ) ) ;
#35283 = CARTESIAN_POINT ( 'NONE',  ( 1.975475456537005874E-15, -49.74999999999999289, 5.000000000000000000 ) ) ;
#35284 = ORIENTED_EDGE ( 'NONE', *, *, #47992, .F. ) ;
#35285 =( BOUNDED_CURVE ( )  B_SPLINE_CURVE ( 2, ( #26464, #22278, #46081, #55738, #2040, #12307, #26144, #27404, #61204 ),
 .UNSPECIFIED., .F., .F. ) 
 B_SPLINE_CURVE_WITH_KNOTS ( ( 3, 2, 2, 2, 3 ),
 ( 0.2916666666666669072, 0.2958333333333335591, 0.3000000000000002665, 0.3041666666666669183, 0.3083333333333336257 ),
 .UNSPECIFIED. ) 
 CURVE ( )  GEOMETRIC_REPRESENTATION_ITEM ( )  RATIONAL_B_SPLINE_CURVE ( ( 0.9999999999999958922, 0.9238795325112908463, 1.000000000000000000, 0.9238795325112867385, 1.000000000000000000, 0.9238795325112867385, 1.000000000000000000, 0.9238795325112816315, 1.000000000000005107 ) ) 
 REPRESENTATION_ITEM ( '' )  );
#35286 = SHAPE_DEFINITION_REPRESENTATION ( #43011, #25037 ) ;
#35287 = CARTESIAN_POINT ( 'NONE',  ( 4.458734124999999437, -164.6875000013655779, 0.000000000000000000 ) ) ;
#35288 = CARTESIAN_POINT ( 'NONE',  ( -2.229367062499996610, 27.85416666803225993, 3.861377020970582219 ) ) ;
#35289 = CARTESIAN_POINT ( 'NONE',  ( -5.000000000000000000, -38.87499999726880162, 0.000000000000000000 ) ) ;
#35290 = ORIENTED_EDGE ( 'NONE', *, *, #49454, .F. ) ;
#35291 = CARTESIAN_POINT ( 'NONE',  ( -50.55543936806279248, -148.3125000013656063, 0.3552334253322060320 ) ) ;
#35292 = CARTESIAN_POINT ( 'NONE',  ( -3.152548672688508926E-16, -74.81249999863439371, -5.148502694627439702 ) ) ;
#35293 = CARTESIAN_POINT ( 'NONE',  ( -60.14911071818854538, -133.1875000027312126, 1.666127454062681368 ) ) ;
#35294 = CARTESIAN_POINT ( 'NONE',  ( 4.458734124999999437, -43.81249999863440081, -5.460374474430324690E-16 ) ) ;
#35295 = CARTESIAN_POINT ( 'NONE',  ( 3.152801135295366208, -142.8125000013655779, 3.152801135295367985 ) ) ;
#35296 = CARTESIAN_POINT ( 'NONE',  ( -7.500000000000000000, 3.202583086485915942, -7.213046687579523386 ) ) ;
#35297 = CARTESIAN_POINT ( 'NONE',  ( 9.457646018065525792E-16, -49.06249999863440792, 5.148502694627439702 ) ) ;
#35298 = CARTESIAN_POINT ( 'NONE',  ( -1.975475456537005874E-15, 29.25000000000000000, 5.000000000000000000 ) ) ;
#35299 = CARTESIAN_POINT ( 'NONE',  ( -3.152548672688508926E-16, -16.56249999863440792, -5.148502694627439702 ) ) ;
#35300 = CARTESIAN_POINT ( 'NONE',  ( 5.000000000000000000, -102.5000000000000142, -6.123233995736766282E-16 ) ) ;
#35301 = EDGE_CURVE ( 'NONE', #8786, #15905, #60849, .T. ) ;
#35302 = CARTESIAN_POINT ( 'NONE',  ( -5.000000000000000000, -167.5000000000000000, -6.123233995736766282E-16 ) ) ;
#35303 = CARTESIAN_POINT ( 'NONE',  ( -2.229367062499996610, -31.39583333196773651, 3.861377020970582219 ) ) ;
#35304 = EDGE_CURVE ( 'NONE', #44139, #47814, #35140, .T. ) ;
#35305 = CARTESIAN_POINT ( 'NONE',  ( -2.499999999999996447, 5.291666669397853795, 4.330127018922195425 ) ) ;
#35306 = DIRECTION ( 'NONE',  ( 1.000000000000000000, 0.000000000000000000, -0.000000000000000000 ) ) ;
#35307 = CARTESIAN_POINT ( 'NONE',  ( -59.44456063193725015, -129.5625000013656063, -0.3552334253322034230 ) ) ;
#35308 = CARTESIAN_POINT ( 'NONE',  ( -4.458734124999999437, -71.64583333196773651, -2.574251347313719407 ) ) ;
#35309 = DIRECTION ( 'NONE',  ( -0.000000000000000000, 1.000000000000000000, -0.000000000000000000 ) ) ;
#35310 = CARTESIAN_POINT ( 'NONE',  ( 0.000000000000000000, -120.0000000000000000, 5.000000000000000000 ) ) ;
#35311 = CARTESIAN_POINT ( 'NONE',  ( 2.626220312808019583E-14, 14.87500000273118239, -5.000000000000000000 ) ) ;
#35312 = CARTESIAN_POINT ( 'NONE',  ( 4.458734124999999437, 0.9375000013655959696, -5.460374474430324690E-16 ) ) ;
#35313 = ORIENTED_EDGE ( 'NONE', *, *, #59063, .F. ) ;
#35314 = CARTESIAN_POINT ( 'NONE',  ( 1.339745962155615144, 16.41965820146970501, 4.999999999999999112 ) ) ;
#35315 = CARTESIAN_POINT ( 'NONE',  ( -2.499999999999996447, -59.83333333333333570, 4.330127018922195425 ) ) ;
#35317 = CARTESIAN_POINT ( 'NONE',  ( 4.458734124999998549, -32.72916666530107221, -2.574251347313721627 ) ) ;
#35316 = CARTESIAN_POINT ( 'NONE',  ( -4.458734124999999437, -90.31249999863440792, 0.000000000000000000 ) ) ;
#35318 = CARTESIAN_POINT ( 'NONE',  ( -5.000000000000000000, -36.00000000000000711, 0.000000000000000000 ) ) ;
#35319 = CARTESIAN_POINT ( 'NONE',  ( -4.458734124999999437, -82.56249999863440792, 0.000000000000000000 ) ) ;
#35320 = CARTESIAN_POINT ( 'NONE',  ( 4.458734125000000326, 15.85416666803226171, 2.574251347313718519 ) ) ;
#35321 = CARTESIAN_POINT ( 'NONE',  ( -59.29741812935640155, -139.6250000013655779, -2.196230717870135685 ) ) ;
#35322 = CARTESIAN_POINT ( 'NONE',  ( -4.458734124999997661, -2.229166665301068662, 2.574251347313722516 ) ) ;
#35323 = CARTESIAN_POINT ( 'NONE',  ( -2.229367062499996610, 21.60416666803226349, 3.861377020970582219 ) ) ;
#35324 = CARTESIAN_POINT ( 'NONE',  ( -4.458734124999997661, -46.47916666530106511, 2.574251347313722516 ) ) ;
#35325 = CARTESIAN_POINT ( 'NONE',  ( 2.499999999999998668, -11.33333333333333393, -4.330127018922193649 ) ) ;
#35326 = CARTESIAN_POINT ( 'NONE',  ( 9.457646018065525792E-16, -84.06249999863439371, 5.148502694627439702 ) ) ;
#35327 = CARTESIAN_POINT ( 'NONE',  ( 4.458734124999999437, -3.812499998634408360, -5.460374474430324690E-16 ) ) ;
#35328 = EDGE_LOOP ( 'NONE', ( #26012, #20179, #57308, #56103 ) ) ;
#35329 = CARTESIAN_POINT ( 'NONE',  ( -4.458734124999999437, -31.56249999863440436, 0.000000000000000000 ) ) ;
#35330 = CARTESIAN_POINT ( 'NONE',  ( -51.60603307380591787, -132.1875000013656063, -2.891590998281053704 ) ) ;
#35331 = CARTESIAN_POINT ( 'NONE',  ( 2.229367062500001939, -72.97916666530107932, 3.861377020970579999 ) ) ;
#35332 = CARTESIAN_POINT ( 'NONE',  ( -5.000000000000000000, -109.8749999972688016, 0.000000000000000000 ) ) ;
#35333 = CARTESIAN_POINT ( 'NONE',  ( -3.152548672688508926E-16, 24.43750000136559564, -5.148502694627439702 ) ) ;
#35334 = CARTESIAN_POINT ( 'NONE',  ( -55.00000000000002132, -155.0000000000000284, 1.734723475976807094E-15 ) ) ;
#35335 = ADVANCED_FACE ( 'NONE', ( #30936 ), #15189, .T. ) ;
#35336 = CARTESIAN_POINT ( 'NONE',  ( -3.535533905932737309, -145.7500000027311842, -3.535533905932738197 ) ) ;
#35337 = CARTESIAN_POINT ( 'NONE',  ( -4.458734124999999437, -76.56249999863440792, 0.000000000000000000 ) ) ;
#35338 = CARTESIAN_POINT ( 'NONE',  ( 2.500000000000002220, -59.66666666666665719, 4.330127018922192761 ) ) ;
#35339 = CARTESIAN_POINT ( 'NONE',  ( 2.499999999999998668, -90.20833333060214443, -4.330127018922193649 ) ) ;
#35340 = CARTESIAN_POINT ( 'NONE',  ( 2.500000000000002220, 26.45833333606451632, 4.330127018922192761 ) ) ;
#35341 = VERTEX_POINT ( 'NONE', #54103 ) ;
#35342 = CARTESIAN_POINT ( 'NONE',  ( 1.339745962155615144, -1.580341798530293662, 4.999999999999999112 ) ) ;
#35343 =( BOUNDED_CURVE ( )  B_SPLINE_CURVE ( 2, ( #54718, #44092, #19974, #35411, #20301, #40235, #49874, #4866, #59546 ),
 .UNSPECIFIED., .F., .F. ) 
 B_SPLINE_CURVE_WITH_KNOTS ( ( 3, 2, 2, 2, 3 ),
 ( 0.07500000000000005274, 0.07916666666666671848, 0.08333333333333339810, 0.08750000000000007772, 0.09166666666666674346 ),
 .UNSPECIFIED. ) 
 CURVE ( )  GEOMETRIC_REPRESENTATION_ITEM ( )  RATIONAL_B_SPLINE_CURVE ( ( 0.9999999999999990008, 0.9238795325112877377, 1.000000000000000000, 0.9238795325112867385, 1.000000000000000000, 0.9238795325112867385, 1.000000000000000000, 0.9238795325112851842, 1.000000000000001554 ) ) 
 REPRESENTATION_ITEM ( '' )  );
#35344 = LINE ( 'NONE', #49176, #8320 ) ;
#35345 = CARTESIAN_POINT ( 'NONE',  ( -4.999999999999999112, -20.91666666666666785, 2.886751345948131764 ) ) ;
#35346 = CARTESIAN_POINT ( 'NONE',  ( 4.458734125000001214, -19.89583333196773651, 2.574251347313718519 ) ) ;
#35347 = CARTESIAN_POINT ( 'NONE',  ( 4.458734124999998549, -84.72916666530106511, -2.574251347313721627 ) ) ;
#35348 = CARTESIAN_POINT ( 'NONE',  ( -5.000000000000000000, -23.95833333060214443, -2.886751345948128211 ) ) ;
#35350 = ORIENTED_EDGE ( 'NONE', *, *, #40797, .F. ) ;
#35349 = CARTESIAN_POINT ( 'NONE',  ( 2.229367062500001939, -47.97916666530106511, 3.861377020970579999 ) ) ;
#35351 = CARTESIAN_POINT ( 'NONE',  ( 1.339745962155615144, -59.58034179853028434, 4.999999999999999112 ) ) ;
#35353 = ORIENTED_EDGE ( 'NONE', *, *, #13465, .T. ) ;
#35352 = CARTESIAN_POINT ( 'NONE',  ( 4.458734125000001214, -4.145833331967740065, 2.574251347313718519 ) ) ;
#35354 = CARTESIAN_POINT ( 'NONE',  ( -54.64476657466781973, -150.8125000013656063, -4.444560631937228834 ) ) ;
#35355 = CARTESIAN_POINT ( 'NONE',  ( -3.535250795749689387E-16, -68.25000000000000000, -5.773502691896257311 ) ) ;
#35356 = CARTESIAN_POINT ( 'NONE',  ( 4.458734124999999437, -153.7500000013656063, 1.846868145590737864 ) ) ;
#35357 = CARTESIAN_POINT ( 'NONE',  ( -2.229367062499996610, -47.39583333196774362, 3.861377020970582219 ) ) ;
#35358 = CARTESIAN_POINT ( 'NONE',  ( 5.000000000000000888, -158.9375000000000000, -2.071067811865475505 ) ) ;
#35359 = CARTESIAN_POINT ( 'NONE',  ( -57.46284108482265651, -151.9375000000000284, 4.819101127000239515 ) ) ;
#35360 = EDGE_CURVE ( 'NONE', #10208, #48999, #19881, .T. ) ;
#35361 = CARTESIAN_POINT ( 'NONE',  ( 2.229367062500001939, -13.22916666530107221, 3.861377020970579999 ) ) ;
#35362 = CARTESIAN_POINT ( 'NONE',  ( -2.229367062500000163, -49.72916666530107221, -3.861377020970580443 ) ) ;
#35363 = AXIS2_PLACEMENT_3D ( 'NONE', #50952, #12970, #7215 ) ;
#35364 = DIRECTION ( 'NONE',  ( 0.000000000000000000, 0.000000000000000000, 1.000000000000000000 ) ) ;
#35365 = CARTESIAN_POINT ( 'NONE',  ( 3.152801135295366208, -144.5625000013655779, 3.152801135295367985 ) ) ;
#35366 = CARTESIAN_POINT ( 'NONE',  ( 4.458734124999998549, -93.97916666530106511, -2.574251347313721627 ) ) ;
#35367 = CARTESIAN_POINT ( 'NONE',  ( 75.00000000000002842, 15.00000000000000000, 5.000000000000000000 ) ) ;
#35368 = VERTEX_POINT ( 'NONE', #60227 ) ;
#35369 = CARTESIAN_POINT ( 'NONE',  ( 2.500000000000002220, -19.54166666393548013, 4.330127018922192761 ) ) ;
#35370 = CARTESIAN_POINT ( 'NONE',  ( -3.152548672688508926E-16, 24.18750000136559564, -5.148502694627439702 ) ) ;
#35371 = CARTESIAN_POINT ( 'NONE',  ( -58.80597590150559739, -146.1250000027312126, 3.242614290531460330 ) ) ;
#35372 = EDGE_CURVE ( 'NONE', #17248, #20760, #3733, .T. ) ;
#35373 = CARTESIAN_POINT ( 'NONE',  ( -6.972266317189433020E-16, -65.12499999726880162, -5.000000000000000000 ) ) ;
#35374 = ORIENTED_EDGE ( 'NONE', *, *, #58542, .F. ) ;
#35375 = CARTESIAN_POINT ( 'NONE',  ( 4.458734124999998549, -3.729166665301070438, -2.574251347313721627 ) ) ;
#35376 = CARTESIAN_POINT ( 'NONE',  ( 1.339745962155612702, -1.169658196007335338, -5.000000000000000000 ) ) ;
#35377 = CARTESIAN_POINT ( 'NONE',  ( -4.458734124999999437, -18.56249999863440792, 0.000000000000000000 ) ) ;
#35378 = EDGE_CURVE ( 'NONE', #19379, #52091, #40274, .T. ) ;
#35379 = CARTESIAN_POINT ( 'NONE',  ( -1.339745962155613812, 1.919658201469706116, -5.000000000000000000 ) ) ;
#35381 = ADVANCED_FACE ( 'NONE', ( #7461 ), #17734, .T. ) ;
#35380 = CARTESIAN_POINT ( 'NONE',  ( -2.229367062500000163, -6.479166665301072214, -3.861377020970580443 ) ) ;
#35382 = CARTESIAN_POINT ( 'NONE',  ( -5.000000000000000000, -73.95833333060214443, -2.886751345948128211 ) ) ;
#35383 = CARTESIAN_POINT ( 'NONE',  ( 3.152801135295366208, -147.5625000013655779, 3.152801135295367985 ) ) ;
#35384 =( BOUNDED_CURVE ( )  B_SPLINE_CURVE ( 2, ( #61709, #19750, #34527, #37563, #47834, #62022, #17638, #58676, #37255 ),
 .UNSPECIFIED., .F., .F. ) 
 B_SPLINE_CURVE_WITH_KNOTS ( ( 3, 2, 2, 2, 3 ),
 ( 0.1767857142857142960, 0.1773809523809523891, 0.1785714285714285754, 0.1797619047619047616, 0.1803571428571428548 ),
 .UNSPECIFIED. ) 
 CURVE ( )  GEOMETRIC_REPRESENTATION_ITEM ( )  RATIONAL_B_SPLINE_CURVE ( ( 0.9330127018922194093, 0.9330127018922194093, 1.000000000000000000, 0.8660254037844387076, 1.000000000000000000, 0.8660254037844387076, 1.000000000000000000, 0.9330127018922194093, 0.9330127018922194093 ) ) 
 REPRESENTATION_ITEM ( '' )  );
#35385 = CARTESIAN_POINT ( 'NONE',  ( 2.229367062500001939, 13.77083333469892779, 3.861377020970579999 ) ) ;
#35386 = ORIENTED_EDGE ( 'NONE', *, *, #10205, .T. ) ;
#35387 = CARTESIAN_POINT ( 'NONE',  ( -6.972266317189433020E-16, -19.12499999726880873, -5.000000000000000000 ) ) ;
#35388 = CARTESIAN_POINT ( 'NONE',  ( 1.975475456537005874E-15, -3.750000000000001776, 5.000000000000000000 ) ) ;
#35389 = CARTESIAN_POINT ( 'NONE',  ( 9.457646018065525792E-16, -17.06249999863440792, 5.148502694627439702 ) ) ;
#35390 = DIRECTION ( 'NONE',  ( -0.000000000000000000, 1.000000000000000000, -0.000000000000000000 ) ) ;
#35391 = LINE ( 'NONE', #5802, #21177 ) ;
#35392 = CARTESIAN_POINT ( 'NONE',  ( -59.29741812935640155, -151.6250000013656063, -2.196230717870135685 ) ) ;
#35393 = CARTESIAN_POINT ( 'NONE',  ( -4.999999999999999112, -45.79166666393547303, 2.886751345948131764 ) ) ;
#35394 = CARTESIAN_POINT ( 'NONE',  ( 2.500000000000002220, -74.66666666666665719, 4.330127018922192761 ) ) ;
#35395 = CARTESIAN_POINT ( 'NONE',  ( 9.457646018065525792E-16, 15.93750000136559564, 5.148502694627439702 ) ) ;
#35396 = CARTESIAN_POINT ( 'NONE',  ( -5.000000000000000000, -89.87499999726880162, 0.000000000000000000 ) ) ;
#35397 = CARTESIAN_POINT ( 'NONE',  ( -55.00000000000002132, -155.0000000000000284, 1.734723475976807094E-15 ) ) ;
#35398 = CARTESIAN_POINT ( 'NONE',  ( -2.229367062499996610, 12.85416666803226171, 3.861377020970582219 ) ) ;
#35399 = CARTESIAN_POINT ( 'NONE',  ( -4.458734124999999437, -66.39583333196773651, -2.574251347313719407 ) ) ;
#35400 = ORIENTED_EDGE ( 'NONE', *, *, #57754, .F. ) ;
#35401 = CARTESIAN_POINT ( 'NONE',  ( 4.458734125000000326, -12.14583333196774007, 2.574251347313718519 ) ) ;
#35402 = CARTESIAN_POINT ( 'NONE',  ( 5.000000000000000000, 3.499999999999999556, -6.123233995736766282E-16 ) ) ;
#35403 = CARTESIAN_POINT ( 'NONE',  ( 4.458734124999999437, -164.5000000013655779, 1.846868145590737864 ) ) ;
#35404 = CARTESIAN_POINT ( 'NONE',  ( -2.499999999999996447, -37.83333333333332860, 4.330127018922195425 ) ) ;
#35405 = CARTESIAN_POINT ( 'NONE',  ( 4.458734125000001214, -57.89583333196773651, 2.574251347313718519 ) ) ;
#35406 = CARTESIAN_POINT ( 'NONE',  ( 1.060575238724906964E-15, -92.62499999726881583, 5.773502691896257311 ) ) ;
#35407 = EDGE_CURVE ( 'NONE', #23020, #35439, #36400, .T. ) ;
#35408 = CARTESIAN_POINT ( 'NONE',  ( 2.229367062499998831, -32.64583333196773651, -3.861377020970580887 ) ) ;
#35409 = AXIS2_PLACEMENT_3D ( 'NONE', #5762, #25707, #45318 ) ;
#35410 = CARTESIAN_POINT ( 'NONE',  ( -2.500000000000000444, -77.16666666666665719, -4.330127018922193649 ) ) ;
#35411 = CARTESIAN_POINT ( 'NONE',  ( -49.85088928181150436, -151.6875000027311842, -1.666127454062680480 ) ) ;
#35412 = CARTESIAN_POINT ( 'NONE',  ( -2.500000000000000444, -79.04166666393547303, -4.330127018922193649 ) ) ;
#35413 = CARTESIAN_POINT ( 'NONE',  ( -8.190561711645485556E-16, -148.9375000013656063, 4.458734124999999437 ) ) ;
#35414 = CARTESIAN_POINT ( 'NONE',  ( -5.000000000000000000, -44.08333333333334281, -2.886751345948128211 ) ) ;
#35415 = DIRECTION ( 'NONE',  ( 0.000000000000000000, 0.000000000000000000, 1.000000000000000000 ) ) ;
#35416 = CARTESIAN_POINT ( 'NONE',  ( 5.000000000000000000, -6.291666663935481019, -2.886751345948130876 ) ) ;
#35417 = ORIENTED_EDGE ( 'NONE', *, *, #8217, .T. ) ;
#35418 = CARTESIAN_POINT ( 'NONE',  ( 4.458734125000001214, -106.8958333319677649, 2.574251347313718519 ) ) ;
#35419 = CARTESIAN_POINT ( 'NONE',  ( -4.458734124999999437, 0.3541666680322609340, -2.574251347313719407 ) ) ;
#35420 = CARTESIAN_POINT ( 'NONE',  ( 1.339745962155615144, 12.29465819873851906, 4.999999999999999112 ) ) ;
#35421 = CARTESIAN_POINT ( 'NONE',  ( -2.499999999999996447, -1.833333333333332593, 4.330127018922195425 ) ) ;
#35422 = CARTESIAN_POINT ( 'NONE',  ( 2.229367062499998831, -64.64583333196773651, -3.861377020970580887 ) ) ;
#35423 = CARTESIAN_POINT ( 'NONE',  ( -1.339745962155669101, -25.79465819873852084, 4.999999999999966249 ) ) ;
#35424 = CARTESIAN_POINT ( 'NONE',  ( 2.499999999999998668, -6.208333330602149758, -4.330127018922193649 ) ) ;
#35426 = ORIENTED_EDGE ( 'NONE', *, *, #24137, .F. ) ;
#35425 = CARTESIAN_POINT ( 'NONE',  ( 2.229367062499998831, -35.64583333196772941, -3.861377020970580887 ) ) ;
#35427 = CARTESIAN_POINT ( 'NONE',  ( 1.975475456537005874E-15, -77.75000000000000000, 5.000000000000000000 ) ) ;
#35428 = CARTESIAN_POINT ( 'NONE',  ( 2.499999999999998668, -81.33333333333332860, -4.330127018922193649 ) ) ;
#35430 = ORIENTED_EDGE ( 'NONE', *, *, #16503, .F. ) ;
#35429 = CARTESIAN_POINT ( 'NONE',  ( -3.152548672688508926E-16, 12.18750000136559564, -5.148502694627439702 ) ) ;
#35431 = CARTESIAN_POINT ( 'NONE',  ( -3.535250795749689387E-16, -48.25000000000000000, -5.773502691896257311 ) ) ;
#35432 = CARTESIAN_POINT ( 'NONE',  ( -4.458734124999999437, -31.64583333196773651, -2.574251347313719407 ) ) ;
#35433 = CARTESIAN_POINT ( 'NONE',  ( -3.152548672688508926E-16, -73.56249999863440792, -5.148502694627439702 ) ) ;
#35434 = CARTESIAN_POINT ( 'NONE',  ( -2.071067811865478170, -169.3125000000000284, 5.000000000000000000 ) ) ;
#35435 = CARTESIAN_POINT ( 'NONE',  ( -3.152548672688508926E-16, -80.56249999863440792, -5.148502694627439702 ) ) ;
#35436 = CARTESIAN_POINT ( 'NONE',  ( -57.89159099828107458, -134.9375000013656063, -3.393966926194107447 ) ) ;
#35437 = CARTESIAN_POINT ( 'NONE',  ( -3.152548672688508926E-16, -27.81249999863440436, -5.148502694627439702 ) ) ;
#35439 = VERTEX_POINT ( 'NONE', #37352 ) ;
#35438 = EDGE_CURVE ( 'NONE', #43179, #48474, #7771, .T. ) ;
#35440 = EDGE_CURVE ( 'NONE', #35972, #35143, #1691, .T. ) ;
#35441 = DIRECTION ( 'NONE',  ( 0.000000000000000000, 0.000000000000000000, 1.000000000000000000 ) ) ;
#35442 = ORIENTED_EDGE ( 'NONE', *, *, #4022, .T. ) ;
#35443 = CARTESIAN_POINT ( 'NONE',  ( -4.458734124999999437, -76.56249999863440792, 0.000000000000000000 ) ) ;
#35444 = FACE_OUTER_BOUND ( 'NONE', #52988, .T. ) ;
#35445 = EDGE_CURVE ( 'NONE', #44005, #25400, #46373, .T. ) ;
#35446 = ORIENTED_EDGE ( 'NONE', *, *, #18517, .F. ) ;
#35447 = DIRECTION ( 'NONE',  ( 1.000000000000000000, 0.000000000000000000, -0.000000000000000000 ) ) ;
#35448 = CARTESIAN_POINT ( 'NONE',  ( 5.000000000000000000, -12.49999999999999645, -6.123233995736766282E-16 ) ) ;
#35449 = CARTESIAN_POINT ( 'NONE',  ( -2.229367062499996610, -62.39583333196774362, 3.861377020970582219 ) ) ;
#35450 = ADVANCED_FACE ( 'NONE', ( #47008 ), #40899, .T. ) ;
#35451 = CARTESIAN_POINT ( 'NONE',  ( 2.229367062500001939, -1.229166665301071548, 3.861377020970579999 ) ) ;
#35452 = ORIENTED_EDGE ( 'NONE', *, *, #58150, .T. ) ;
#35453 = EDGE_CURVE ( 'NONE', #8541, #20951, #15747, .T. ) ;
#35454 = VECTOR ( 'NONE', #15017, 1000.000000000000000 ) ;
#35455 = CARTESIAN_POINT ( 'NONE',  ( 1.339745962155612702, -62.29465819873851729, -5.000000000000000000 ) ) ;
#35456 = CARTESIAN_POINT ( 'NONE',  ( -4.729367062499999719, -110.1562499993171969, 0.000000000000000000 ) ) ;
#35457 = EDGE_CURVE ( 'NONE', #5644, #55393, #51208, .T. ) ;
#35458 = EDGE_CURVE ( 'NONE', #51028, #43336, #56357, .T. ) ;
#35459 = CARTESIAN_POINT ( 'NONE',  ( 9.457646018065525792E-16, 7.937500001365594748, 5.148502694627439702 ) ) ;
#35460 = CARTESIAN_POINT ( 'NONE',  ( -59.59170313451811296, -142.5000000013656347, 1.485763867205729394 ) ) ;
#35461 = CARTESIAN_POINT ( 'NONE',  ( 5.000000000000000000, -27.37499999726880873, -6.123233995736766282E-16 ) ) ;
#35462 = CARTESIAN_POINT ( 'NONE',  ( -4.458734125000000326, -162.8750000013655779, 1.846868145590734089 ) ) ;
#35463 = CARTESIAN_POINT ( 'NONE',  ( -6.972266317189433020E-16, -75.12499999726880162, -5.000000000000000000 ) ) ;
#35465 = ADVANCED_FACE ( 'NONE', ( #61497 ), #60544, .T. ) ;
#35464 = ORIENTED_EDGE ( 'NONE', *, *, #13866, .T. ) ;
#35466 = CARTESIAN_POINT ( 'NONE',  ( 2.229367062500001939, -81.97916666530106511, 3.861377020970579999 ) ) ;
#35467 = EDGE_CURVE ( 'NONE', #27870, #51343, #51072, .T. ) ;
#35468 = CARTESIAN_POINT ( 'NONE',  ( 1.975475456537005874E-15, -29.62499999726881228, 5.000000000000000000 ) ) ;
#35469 = CARTESIAN_POINT ( 'NONE',  ( 2.229367062499998831, -2.645833331967738289, -3.861377020970580887 ) ) ;
#35470 = CARTESIAN_POINT ( 'NONE',  ( 0.000000000000000000, -170.0000000000000000, 0.000000000000000000 ) ) ;
#35471 =( BOUNDED_CURVE ( )  B_SPLINE_CURVE ( 2, ( #4209, #52779, #57304, #23821, #47626, #19297, #33466, #8708, #23512 ),
 .UNSPECIFIED., .F., .F. ) 
 B_SPLINE_CURVE_WITH_KNOTS ( ( 3, 2, 2, 2, 3 ),
 ( 0.9625000000000000222, 0.9630952380952381153, 0.9642857142857143016, 0.9654761904761904878, 0.9660714285714285809 ),
 .UNSPECIFIED. ) 
 CURVE ( )  GEOMETRIC_REPRESENTATION_ITEM ( )  RATIONAL_B_SPLINE_CURVE ( ( 0.9330127018922194093, 0.9330127018922194093, 1.000000000000000000, 0.8660254037844387076, 1.000000000000000000, 0.8660254037844387076, 1.000000000000000000, 0.9330127018922194093, 0.9330127018922194093 ) ) 
 REPRESENTATION_ITEM ( '' )  );
#35472 = CARTESIAN_POINT ( 'NONE',  ( 1.975475456537005874E-15, 1.250000000000000000, 5.000000000000000000 ) ) ;
#35473 = CARTESIAN_POINT ( 'NONE',  ( 9.457646018065525792E-16, -69.31249999863440792, 5.148502694627439702 ) ) ;
#35474 = CARTESIAN_POINT ( 'NONE',  ( -2.500000000000000444, -30.04166666393548013, -4.330127018922193649 ) ) ;
#35475 = CARTESIAN_POINT ( 'NONE',  ( -2.500000000000000444, -15.16666666666666785, -4.330127018922193649 ) ) ;
#35476 = CARTESIAN_POINT ( 'NONE',  ( 4.458734124999999437, 28.18750000136559208, -5.460374474430324690E-16 ) ) ;
#35477 = CARTESIAN_POINT ( 'NONE',  ( -2.500000000000000444, -83.04166666393547303, -4.330127018922193649 ) ) ;
#35478 = CARTESIAN_POINT ( 'NONE',  ( 4.458734124999999437, 27.18750000136559564, -5.460374474430324690E-16 ) ) ;
#35479 = CARTESIAN_POINT ( 'NONE',  ( 4.458734124999999437, -52.81249999863440792, -5.460374474430324690E-16 ) ) ;
#35480 = CARTESIAN_POINT ( 'NONE',  ( -4.458734124999999437, -34.56249999863440792, 0.000000000000000000 ) ) ;
#35481 = CARTESIAN_POINT ( 'NONE',  ( -2.229367062499996610, 3.604166668032260379, 3.861377020970582219 ) ) ;
#35482 = CARTESIAN_POINT ( 'NONE',  ( 6.123233995736766282E-16, -170.0000000000000000, -5.000000000000000000 ) ) ;
#35483 = CARTESIAN_POINT ( 'NONE',  ( -2.499999999999996447, 23.16666666666666430, 4.330127018922195425 ) ) ;
#35484 = CARTESIAN_POINT ( 'NONE',  ( -3.535533905932737309, -145.7500000027311842, -3.535533905932738197 ) ) ;
#35485 = DIRECTION ( 'NONE',  ( -0.000000000000000000, -1.000000000000000000, -0.000000000000000000 ) ) ;
#35486 = CARTESIAN_POINT ( 'NONE',  ( -2.229367062499996610, -44.14583333196774362, 3.861377020970582219 ) ) ;
#35487 = CARTESIAN_POINT ( 'NONE',  ( -3.535250795749689387E-16, -71.12499999726880162, -5.773502691896257311 ) ) ;
#35488 = CARTESIAN_POINT ( 'NONE',  ( -58.39396692619412477, -142.6875000013656063, 2.891590998281057701 ) ) ;
#35489 = DIRECTION ( 'NONE',  ( -0.000000000000000000, 1.000000000000000000, -0.000000000000000000 ) ) ;
#35490 = CARTESIAN_POINT ( 'NONE',  ( 5.000000000000000888, -141.0625000027312410, -2.071067811865475505 ) ) ;
#35491 = CARTESIAN_POINT ( 'NONE',  ( -3.152548672688508926E-16, -79.81249999863440792, -5.148502694627439702 ) ) ;
#35492 = CARTESIAN_POINT ( 'NONE',  ( 1.846868145590735200, -160.5000000013656347, -4.458734124999999437 ) ) ;
#35493 = CARTESIAN_POINT ( 'NONE',  ( 0.000000000000000000, -114.9999999999999858, 0.000000000000000000 ) ) ;
#35494 = DIRECTION ( 'NONE',  ( 0.000000000000000000, 0.000000000000000000, 1.000000000000000000 ) ) ;
#35495 = CARTESIAN_POINT ( 'NONE',  ( 5.000000000000000000, -29.50000000000000000, -6.123233995736766282E-16 ) ) ;
#35496 = CARTESIAN_POINT ( 'NONE',  ( 3.152801135295366208, -141.5625000013655779, 3.152801135295367985 ) ) ;
#35497 = EDGE_LOOP ( 'NONE', ( #6292, #1380, #2939, #57755 ) ) ;
#35498 = CARTESIAN_POINT ( 'NONE',  ( -4.458734124999999437, 20.43750000136559208, 0.000000000000000000 ) ) ;
#35499 = EDGE_LOOP ( 'NONE', ( #48400, #53376, #61615, #40366 ) ) ;
#35500 = CARTESIAN_POINT ( 'NONE',  ( 2.229367062500001939, -60.22916666530106511, 3.861377020970579999 ) ) ;
#35501 = CARTESIAN_POINT ( 'NONE',  ( -3.535250795749689387E-16, 22.87500000273118772, -5.773502691896257311 ) ) ;
#35502 = CARTESIAN_POINT ( 'NONE',  ( -52.53715891517739323, -138.5625000027311842, -4.819101127000233298 ) ) ;
#35503 = CARTESIAN_POINT ( 'NONE',  ( 2.499999999999998668, 11.66666666666666607, -4.330127018922193649 ) ) ;
#35504 = CARTESIAN_POINT ( 'NONE',  ( -4.458734124999999437, -51.31249999863440792, 0.000000000000000000 ) ) ;
#35505 = CARTESIAN_POINT ( 'NONE',  ( 2.229367062500001939, -12.97916666530107221, 3.861377020970579999 ) ) ;
#35506 = LINE ( 'NONE', #50293, #19499 ) ;
#35507 = CARTESIAN_POINT ( 'NONE',  ( 1.339745962155612702, -99.16965819600733312, -5.000000000000000000 ) ) ;
#35508 = CARTESIAN_POINT ( 'NONE',  ( -1.339745962155613812, -0.08034179853029406460, -5.000000000000000000 ) ) ;
#35509 = CARTESIAN_POINT ( 'NONE',  ( 2.499999999999998668, -66.20833333060213022, -4.330127018922193649 ) ) ;
#35511 = CARTESIAN_POINT ( 'NONE',  ( 2.229367062500001939, -16.22916666530107577, 3.861377020970579999 ) ) ;
#35510 = DIRECTION ( 'NONE',  ( -0.000000000000000000, 1.000000000000000000, -0.000000000000000000 ) ) ;
#35512 = CARTESIAN_POINT ( 'NONE',  ( 1.339745962155627135, 17.83034180399266333, -4.999999999999991118 ) ) ;
#35513 = CARTESIAN_POINT ( 'NONE',  ( -4.458734124999998549, -58.22916666530105800, 2.574251347313722516 ) ) ;
#35514 = CARTESIAN_POINT ( 'NONE',  ( 4.458734124999999437, -151.6875000013656063, 0.000000000000000000 ) ) ;
#35515 = CARTESIAN_POINT ( 'NONE',  ( 2.229367062499998831, -65.64583333196773651, -3.861377020970580887 ) ) ;
#35516 = CARTESIAN_POINT ( 'NONE',  ( -2.499999999999996447, -53.70833333060213732, 4.330127018922195425 ) ) ;
#35517 = EDGE_LOOP ( 'NONE', ( #55524, #16192, #36861, #8833 ) ) ;
#35518 = CARTESIAN_POINT ( 'NONE',  ( -1.339745962155613812, 24.91965820146970501, -5.000000000000000000 ) ) ;
#35519 = CARTESIAN_POINT ( 'NONE',  ( 4.458734125000001214, 1.854166668032262155, 2.574251347313718519 ) ) ;
#35520 = ORIENTED_EDGE ( 'NONE', *, *, #33419, .T. ) ;
#35522 = LINE ( 'NONE', #1767, #8053 ) ;
#35521 = CARTESIAN_POINT ( 'NONE',  ( -59.81910112700027327, -149.3125000027312126, -2.462841084822540605 ) ) ;
#35523 = CARTESIAN_POINT ( 'NONE',  ( -8.190561711645485556E-16, -154.6875000013655779, 4.458734124999999437 ) ) ;
#35524 = ORIENTED_EDGE ( 'NONE', *, *, #57129, .T. ) ;
#35525 = AXIS2_PLACEMENT_3D ( 'NONE', #8113, #22913, #27398 ) ;
#35526 = CARTESIAN_POINT ( 'NONE',  ( 2.499999999999998668, -54.33333333333332860, -4.330127018922193649 ) ) ;
#35527 = CARTESIAN_POINT ( 'NONE',  ( -49.85088928181150436, -128.5625000000000568, -1.666127454062680702 ) ) ;
#35528 = CARTESIAN_POINT ( 'NONE',  ( 1.339745962155615144, -80.58034179853028434, 4.999999999999999112 ) ) ;
#35529 = CARTESIAN_POINT ( 'NONE',  ( 4.458734125000001214, -51.14583333196772941, 2.574251347313718519 ) ) ;
#35530 = ORIENTED_EDGE ( 'NONE', *, *, #4362, .T. ) ;
#35531 = CARTESIAN_POINT ( 'NONE',  ( 1.975475456537005874E-15, 11.24999999999999822, 5.000000000000000000 ) ) ;
#35532 = CARTESIAN_POINT ( 'NONE',  ( 2.229367062500001939, 14.02083333469892779, 3.861377020970579999 ) ) ;
#35533 = EDGE_CURVE ( 'NONE', #22435, #9796, #46685, .T. ) ;
#35534 = CARTESIAN_POINT ( 'NONE',  ( -2.229367062500000163, 27.52083333469892779, -3.861377020970580443 ) ) ;
#35535 = CARTESIAN_POINT ( 'NONE',  ( -56.48576386720575471, -151.7500000013655779, -4.591703134518078322 ) ) ;
#35536 = CARTESIAN_POINT ( 'NONE',  ( 5.000000000000000000, -44.50000000000000000, -6.123233995736766282E-16 ) ) ;
#35537 = CARTESIAN_POINT ( 'NONE',  ( 7.500000000000000888, -2.886751345948134873, -7.198902722707428481 ) ) ;
#35538 =( BOUNDED_CURVE ( )  B_SPLINE_CURVE ( 2, ( #20036, #19396, #24546, #63162, #121, #39641, #29675, #5246, #53187 ),
 .UNSPECIFIED., .F., .F. ) 
 B_SPLINE_CURVE_WITH_KNOTS ( ( 3, 2, 2, 2, 3 ),
 ( 0.6696428571428570953, 0.6702380952380951884, 0.6714285714285713746, 0.6726190476190476719, 0.6732142857142857650 ),
 .UNSPECIFIED. ) 
 CURVE ( )  GEOMETRIC_REPRESENTATION_ITEM ( )  RATIONAL_B_SPLINE_CURVE ( ( 0.9330127018922194093, 0.9330127018922194093, 1.000000000000000000, 0.8660254037844387076, 1.000000000000000000, 0.8660254037844387076, 1.000000000000000000, 0.9330127018922194093, 0.9330127018922194093 ) ) 
 REPRESENTATION_ITEM ( '' )  );
#35539 = CARTESIAN_POINT ( 'NONE',  ( 4.458734125000000326, -62.89583333196774362, 2.574251347313718519 ) ) ;
#35540 = CARTESIAN_POINT ( 'NONE',  ( 0.000000000000000000, -120.0000000000000000, 5.000000000000000000 ) ) ;
#35541 = CARTESIAN_POINT ( 'NONE',  ( -4.458734124999998549, 10.77083333469892956, 2.574251347313722516 ) ) ;
#35542 = VECTOR ( 'NONE', #12519, 1000.000000000000000 ) ;
#35543 = CARTESIAN_POINT ( 'NONE',  ( -2.499999999999996447, -78.70833333060214443, 4.330127018922195425 ) ) ;
#35544 = EDGE_CURVE ( 'NONE', #18022, #41008, #6738, .T. ) ;
#35545 = CARTESIAN_POINT ( 'NONE',  ( -9.184850993605147944E-16, -157.3750000027311842, 5.000000000000000000 ) ) ;
#35546 = CARTESIAN_POINT ( 'NONE',  ( -4.458734124999999437, -55.56249999863440081, 0.000000000000000000 ) ) ;
#35547 = CARTESIAN_POINT ( 'NONE',  ( -2.500000000000000444, -9.041666663935483683, -4.330127018922193649 ) ) ;
#35548 = CARTESIAN_POINT ( 'NONE',  ( -1.339745962155610925, -108.7946581987385315, 5.000000000000000000 ) ) ;
#35549 = FACE_OUTER_BOUND ( 'NONE', #29926, .T. ) ;
#35550 = CARTESIAN_POINT ( 'NONE',  ( -2.229367062499996610, -87.39583333196773651, 3.861377020970582219 ) ) ;
#35551 = CARTESIAN_POINT ( 'NONE',  ( 5.000000000000000000, -104.3749999972688158, -6.123233995736766282E-16 ) ) ;
#35552 = CARTESIAN_POINT ( 'NONE',  ( 2.229367062499998831, -18.89583333196774007, -3.861377020970580887 ) ) ;
#35553 = VERTEX_POINT ( 'NONE', #18039 ) ;
#35554 = CARTESIAN_POINT ( 'NONE',  ( 1.975475456537005874E-15, -31.75000000000000000, 5.000000000000000000 ) ) ;
#35555 = CARTESIAN_POINT ( 'NONE',  ( -2.229367062500000163, -105.4791666653010651, -3.861377020970580443 ) ) ;
#35556 = CARTESIAN_POINT ( 'NONE',  ( -2.071067811865475061, -155.8125000027311842, -5.000000000000000888 ) ) ;
#35557 = ORIENTED_EDGE ( 'NONE', *, *, #20106, .F. ) ;
#35558 = CARTESIAN_POINT ( 'NONE',  ( 2.229367062499998831, -98.89583333196773651, -3.861377020970580887 ) ) ;
#35559 = CARTESIAN_POINT ( 'NONE',  ( 2.229367062500001939, -25.97916666530106866, 3.861377020970579999 ) ) ;
#35560 = CARTESIAN_POINT ( 'NONE',  ( -3.535250795749689387E-16, -56.12499999726880162, -5.773502691896257311 ) ) ;
#35561 = CARTESIAN_POINT ( 'NONE',  ( -1.339745962155613812, -67.20534180126149693, -5.000000000000000000 ) ) ;
#35562 = CARTESIAN_POINT ( 'NONE',  ( -56.48576386720575471, -125.7500000013656347, -4.591703134518078322 ) ) ;
#35563 = CARTESIAN_POINT ( 'NONE',  ( -58.39396692619412477, -143.4375000013656063, 2.891590998281057701 ) ) ;
#35564 = CARTESIAN_POINT ( 'NONE',  ( 4.458734124999999437, -21.81249999863440436, -5.460374474430324690E-16 ) ) ;
#35565 = CARTESIAN_POINT ( 'NONE',  ( 4.458734124999998549, -63.97916666530106511, -2.574251347313721627 ) ) ;
#35566 = CARTESIAN_POINT ( 'NONE',  ( 5.000000000000000888, -94.45833333060211601, 2.886751345948126879 ) ) ;
#35567 = CARTESIAN_POINT ( 'NONE',  ( -4.458734124999997661, -20.22916666530107221, 2.574251347313722516 ) ) ;
#35568 = CARTESIAN_POINT ( 'NONE',  ( -6.972266317189433020E-16, -88.25000000000000000, -5.000000000000000000 ) ) ;
#35569 = CARTESIAN_POINT ( 'NONE',  ( -5.000000000000000000, -149.5000000000000284, -6.123233995736766282E-16 ) ) ;
#35570 = CARTESIAN_POINT ( 'NONE',  ( 2.499999999999998668, -9.333333333333332149, -4.330127018922193649 ) ) ;
#35571 = CARTESIAN_POINT ( 'NONE',  ( 1.846868145590735200, -150.2500000013656063, -4.458734125000000326 ) ) ;
#35572 = ORIENTED_EDGE ( 'NONE', *, *, #16560, .F. ) ;
#35573 = CARTESIAN_POINT ( 'NONE',  ( -3.152548672688508926E-16, -46.81249999863440792, -5.148502694627439702 ) ) ;
#35574 =( BOUNDED_CURVE ( )  B_SPLINE_CURVE ( 2, ( #34172, #10051, #59266, #9729, #1070, #107, #58633, #15198, #29332 ),
 .UNSPECIFIED., .F., .F. ) 
 B_SPLINE_CURVE_WITH_KNOTS ( ( 3, 2, 2, 2, 3 ),
 ( 0.5187500000000000444, 0.5194444444444444864, 0.5208333333333333703, 0.5222222222222222543, 0.5229166666666666963 ),
 .UNSPECIFIED. ) 
 CURVE ( )  GEOMETRIC_REPRESENTATION_ITEM ( )  RATIONAL_B_SPLINE_CURVE ( ( 0.9330127018922194093, 0.9330127018922194093, 1.000000000000000000, 0.8660254037844387076, 1.000000000000000000, 0.8660254037844387076, 1.000000000000000000, 0.9330127018922194093, 0.9330127018922194093 ) ) 
 REPRESENTATION_ITEM ( '' )  );
#35575 = CARTESIAN_POINT ( 'NONE',  ( -4.999999999999998224, -37.91666666666667851, 2.886751345948131764 ) ) ;
#35576 = CARTESIAN_POINT ( 'NONE',  ( 1.339745962155729053, -90.29465819873854571, -4.999999999999933387 ) ) ;
#35577 = CARTESIAN_POINT ( 'NONE',  ( 2.499999999999998668, 27.66666666666666430, -4.330127018922193649 ) ) ;
#35578 = CARTESIAN_POINT ( 'NONE',  ( -4.458734124999999437, 5.687500001365592972, 0.000000000000000000 ) ) ;
#35579 = CARTESIAN_POINT ( 'NONE',  ( 5.000000000000000000, 1.708333336064519425, -2.886751345948130876 ) ) ;
#35580 = CARTESIAN_POINT ( 'NONE',  ( 5.000000000000000888, -41.45833333060214443, 2.886751345948126879 ) ) ;
#35581 = CARTESIAN_POINT ( 'NONE',  ( -3.750000000000007105, -6.495190528383289141, 0.000000000000000000 ) ) ;
#35582 = CARTESIAN_POINT ( 'NONE',  ( -4.458734124999998549, 14.52083333469892779, 2.574251347313722516 ) ) ;
#35583 = CARTESIAN_POINT ( 'NONE',  ( -5.000000000000000000, -76.00000000000000000, 0.000000000000000000 ) ) ;
#35584 = CARTESIAN_POINT ( 'NONE',  ( 5.000000000000000000, 9.625000002731184168, -6.123233995736766282E-16 ) ) ;
#35585 = VERTEX_POINT ( 'NONE', #42483 ) ;
#35586 = CARTESIAN_POINT ( 'NONE',  ( 2.499999999999998668, -80.20833333060213022, -4.330127018922193649 ) ) ;
#35587 = EDGE_LOOP ( 'NONE', ( #16226, #779, #20333, #18920 ) ) ;
#35588 = AXIS2_PLACEMENT_3D ( 'NONE', #62574, #18494, #62877 ) ;
#35589 = CARTESIAN_POINT ( 'NONE',  ( 1.339745962155615144, -85.70534180126146850, 4.999999999999999112 ) ) ;
#35590 = CARTESIAN_POINT ( 'NONE',  ( -4.458734124999999437, -41.39583333196773651, -2.574251347313719407 ) ) ;
#35591 = CARTESIAN_POINT ( 'NONE',  ( -8.190561711645485556E-16, -168.9375000013656063, 4.458734124999999437 ) ) ;
#35592 = VECTOR ( 'NONE', #53366, 1000.000000000000000 ) ;
#35593 = AXIS2_PLACEMENT_3D ( 'NONE', #5166, #29594, #34753 ) ;
#35594 = CARTESIAN_POINT ( 'NONE',  ( -4.999999999999999112, -39.79166666393547303, 2.886751345948131764 ) ) ;
#35595 = VERTEX_POINT ( 'NONE', #18361 ) ;
#35596 = CARTESIAN_POINT ( 'NONE',  ( -4.458734124999999437, -20.39583333196774362, -2.574251347313719407 ) ) ;
#35597 = VERTEX_POINT ( 'NONE', #38299 ) ;
#35598 = CARTESIAN_POINT ( 'NONE',  ( 5.000000000000000888, -86.58333333333334281, 2.886751345948126879 ) ) ;
#35599 = DIRECTION ( 'NONE',  ( -0.000000000000000000, 1.000000000000000000, -0.000000000000000000 ) ) ;
#35600 = CARTESIAN_POINT ( 'NONE',  ( -2.499999999999996447, -88.70833333060214443, 4.330127018922195425 ) ) ;
#35602 = ORIENTED_EDGE ( 'NONE', *, *, #23969, .F. ) ;
#35601 = CARTESIAN_POINT ( 'NONE',  ( 1.975475456537005874E-15, -0.7499999999999996669, 5.000000000000000000 ) ) ;
#35603 = CARTESIAN_POINT ( 'NONE',  ( -59.98410592259440222, -142.1250000000000284, -0.3983568153799752487 ) ) ;
#35604 = CARTESIAN_POINT ( 'NONE',  ( 2.229367062500001939, -32.22916666530106511, 3.861377020970579999 ) ) ;
#35605 = DIRECTION ( 'NONE',  ( -0.000000000000000000, 1.000000000000000000, -0.000000000000000000 ) ) ;
#35606 = VERTEX_POINT ( 'NONE', #43113 ) ;
#35607 = CARTESIAN_POINT ( 'NONE',  ( 4.458734125000001214, -78.89583333196772230, 2.574251347313718519 ) ) ;
#35608 = CARTESIAN_POINT ( 'NONE',  ( -4.458734124999999437, -108.5624999986343937, 0.000000000000000000 ) ) ;
#35609 = CARTESIAN_POINT ( 'NONE',  ( 2.499999999999998668, 20.66666666666666785, -4.330127018922193649 ) ) ;
#35610 = ORIENTED_EDGE ( 'NONE', *, *, #31385, .T. ) ;
#35611 = CARTESIAN_POINT ( 'NONE',  ( 3.061616997868383141E-16, -166.8750000027312126, -5.000000000000000000 ) ) ;
#35612 = CARTESIAN_POINT ( 'NONE',  ( -52.10840900171896806, -142.4375000013656063, 3.393966926194110556 ) ) ;
#35613 = CARTESIAN_POINT ( 'NONE',  ( -4.458734124999999437, -76.64583333196775072, -2.574251347313719407 ) ) ;
#35614 = CARTESIAN_POINT ( 'NONE',  ( -50.18089887299979068, -132.8125000027312126, 2.462841084822635640 ) ) ;
#35615 = CARTESIAN_POINT ( 'NONE',  ( 4.458734125000000326, -43.89583333196773651, 2.574251347313718519 ) ) ;
#35616 = CARTESIAN_POINT ( 'NONE',  ( 3.152801135295367541, -142.5625000013655779, -3.152801135295367541 ) ) ;
#35617 = DIRECTION ( 'NONE',  ( 0.000000000000000000, 0.000000000000000000, 1.000000000000000000 ) ) ;
#35618 = CARTESIAN_POINT ( 'NONE',  ( 2.229367062500001939, -50.97916666530107221, 3.861377020970579999 ) ) ;
#35619 = CARTESIAN_POINT ( 'NONE',  ( -2.229367062500000163, -44.47916666530106511, -3.861377020970580443 ) ) ;
#35620 = CARTESIAN_POINT ( 'NONE',  ( 5.000000000000000000, 29.58333333333332860, -2.886751345948130876 ) ) ;
#35621 = CARTESIAN_POINT ( 'NONE',  ( -2.229367062500000163, -18.47916666530106866, -3.861377020970580443 ) ) ;
#35622 = CARTESIAN_POINT ( 'NONE',  ( -3.535250795749689387E-16, -101.2500000000000000, -5.773502691896257311 ) ) ;
#35623 = CARTESIAN_POINT ( 'NONE',  ( 3.152801135295366208, -140.8125000013655779, 3.152801135295367985 ) ) ;
#35624 = CARTESIAN_POINT ( 'NONE',  ( -2.229367062499996610, -35.39583333196772941, 3.861377020970582219 ) ) ;
#35625 = CARTESIAN_POINT ( 'NONE',  ( 5.000000000000000000, 5.625000002731185056, -6.123233995736766282E-16 ) ) ;
#35626 = CARTESIAN_POINT ( 'NONE',  ( 1.339745962155612702, -50.29465819873851729, -5.000000000000000000 ) ) ;
#35627 = CARTESIAN_POINT ( 'NONE',  ( -57.19623071787017210, -129.3750000013656347, 4.297418129356382899 ) ) ;
#35628 = CARTESIAN_POINT ( 'NONE',  ( -4.458734124999998549, -76.47916666530105090, 2.574251347313722516 ) ) ;
#35629 = CARTESIAN_POINT ( 'NONE',  ( 3.061616997868383141E-16, -166.7500000000000000, -5.000000000000000000 ) ) ;
#35630 = CARTESIAN_POINT ( 'NONE',  ( 2.500000000000002220, 14.45833333606451809, 4.330127018922192761 ) ) ;
#35631 = CARTESIAN_POINT ( 'NONE',  ( 4.458734125000000326, 0.8541666680322613781, 2.574251347313718519 ) ) ;
#35632 = EDGE_LOOP ( 'NONE', ( #18301, #31895, #42154, #44291 ) ) ;
#35633 = VECTOR ( 'NONE', #39625, 1000.000000000000000 ) ;
#35634 = CARTESIAN_POINT ( 'NONE',  ( 3.044556291839386294E-14, 16.87500000273118417, -5.000000000000000000 ) ) ;
#35635 = CARTESIAN_POINT ( 'NONE',  ( 5.000000000000000000, 23.70833333606451632, -2.886751345948130876 ) ) ;
#35637 = CARTESIAN_POINT ( 'NONE',  ( 2.229367062500001939, -35.97916666530107221, 3.861377020970579999 ) ) ;
#35636 = CARTESIAN_POINT ( 'NONE',  ( -2.229367062499996610, -89.14583333196773651, 3.861377020970582219 ) ) ;
#35638 = CARTESIAN_POINT ( 'NONE',  ( 0.000000000000000000, -120.0000000000000000, 0.000000000000000000 ) ) ;
#35639 = CARTESIAN_POINT ( 'NONE',  ( 2.229367062500001939, -83.22916666530106511, 3.861377020970579999 ) ) ;
#35640 = CIRCLE ( 'NONE', #14039, 5.000000000000000000 ) ;
#35641 = CARTESIAN_POINT ( 'NONE',  ( -2.229367062499996610, 15.60416666803225993, 3.861377020970582219 ) ) ;
#35642 = CARTESIAN_POINT ( 'NONE',  ( 0.000000000000000000, -120.0000000000000000, 0.000000000000000000 ) ) ;
#35643 = VECTOR ( 'NONE', #22421, 1000.000000000000000 ) ;
#35644 = CARTESIAN_POINT ( 'NONE',  ( -58.39396692619412477, -139.4375000013656063, 2.891590998281057701 ) ) ;
#35645 = CARTESIAN_POINT ( 'NONE',  ( -2.229367062500000163, -9.479166665301068662, -3.861377020970580443 ) ) ;
#35646 = CARTESIAN_POINT ( 'NONE',  ( 9.457646018065525792E-16, 19.68750000136559208, 5.148502694627439702 ) ) ;
#35647 = CARTESIAN_POINT ( 'NONE',  ( 4.458734124999999437, -48.06249999863440792, -5.460374474430324690E-16 ) ) ;
#35648 = CARTESIAN_POINT ( 'NONE',  ( 1.975475456537005874E-15, -50.62499999726881583, 5.000000000000000000 ) ) ;
#35649 = CARTESIAN_POINT ( 'NONE',  ( 2.229367062499998831, -83.64583333196773651, -3.861377020970580887 ) ) ;
#35650 = CARTESIAN_POINT ( 'NONE',  ( 4.458734124999998549, -3.729166665301070438, -2.574251347313721627 ) ) ;
#35651 = CARTESIAN_POINT ( 'NONE',  ( 0.000000000000000000, -120.0000000000000000, 0.000000000000000000 ) ) ;
#35652 = ORIENTED_EDGE ( 'NONE', *, *, #61301, .F. ) ;
#35653 = CARTESIAN_POINT ( 'NONE',  ( -4.458734124999999437, -29.56249999863440436, 0.000000000000000000 ) ) ;
#35654 = CARTESIAN_POINT ( 'NONE',  ( -51.60603307380591787, -130.1875000013656063, -2.891590998281053704 ) ) ;
#35655 = CARTESIAN_POINT ( 'NONE',  ( -3.152548672688508926E-16, -73.56249999863440792, -5.148502694627439702 ) ) ;
#35656 = CARTESIAN_POINT ( 'NONE',  ( -2.229367062500000163, 29.27083333469892779, -3.861377020970580443 ) ) ;
#35657 = EDGE_CURVE ( 'NONE', #55337, #37963, #26843, .T. ) ;
#35658 =( BOUNDED_CURVE ( )  B_SPLINE_CURVE ( 2, ( #51849, #42190, #52166, #7791, #21395, #22909, #52492, #42503, #12607 ),
 .UNSPECIFIED., .F., .F. ) 
 B_SPLINE_CURVE_WITH_KNOTS ( ( 3, 2, 2, 2, 3 ),
 ( 0.5589285714285714413, 0.5595238095238095344, 0.5607142857142857206, 0.5619047619047619069, 0.5625000000000000000 ),
 .UNSPECIFIED. ) 
 CURVE ( )  GEOMETRIC_REPRESENTATION_ITEM ( )  RATIONAL_B_SPLINE_CURVE ( ( 0.9330127018922194093, 0.9330127018922194093, 1.000000000000000000, 0.8660254037844387076, 1.000000000000000000, 0.8660254037844387076, 1.000000000000000000, 0.9330127018922194093, 0.9330127018922194093 ) ) 
 REPRESENTATION_ITEM ( '' )  );
#35659 = CARTESIAN_POINT ( 'NONE',  ( -4.458734124999998549, 18.77083333469893134, 2.574251347313722516 ) ) ;
#35660 = CARTESIAN_POINT ( 'NONE',  ( -6.972266317189433020E-16, -65.24999999999998579, -5.000000000000000000 ) ) ;
#35661 = CARTESIAN_POINT ( 'NONE',  ( 1.339745962155615144, -66.70534180126148271, 4.999999999999999112 ) ) ;
#35662 = CARTESIAN_POINT ( 'NONE',  ( -4.458734124999999437, -76.64583333196775072, -2.574251347313719407 ) ) ;
#35663 = CARTESIAN_POINT ( 'NONE',  ( 5.000000000000000000, -60.41666666666666430, -2.886751345948129988 ) ) ;
#35664 = CARTESIAN_POINT ( 'NONE',  ( -2.500000000000000444, -75.16666666666665719, -4.330127018922193649 ) ) ;
#35665 = CARTESIAN_POINT ( 'NONE',  ( 1.060575238724906964E-15, 24.37500000273118417, 5.773502691896257311 ) ) ;
#35666 = ORIENTED_EDGE ( 'NONE', *, *, #58695, .F. ) ;
#35667 = DIRECTION ( 'NONE',  ( -0.6485228581062915110, 0.000000000000000000, -0.7611951803011149931 ) ) ;
#35668 = CARTESIAN_POINT ( 'NONE',  ( 2.500000000000002220, -52.54166666393548013, 4.330127018922192761 ) ) ;
#35670 = CARTESIAN_POINT ( 'NONE',  ( 1.060575238724906964E-15, -23.75000000000000000, 5.773502691896257311 ) ) ;
#35669 = CARTESIAN_POINT ( 'NONE',  ( 1.975475456537005874E-15, -106.6249999972687874, 5.000000000000000000 ) ) ;
#35671 = CARTESIAN_POINT ( 'NONE',  ( -3.152548672688508926E-16, -27.56249999863440081, -5.148502694627439702 ) ) ;
#35672 = CARTESIAN_POINT ( 'NONE',  ( 9.457646018065525792E-16, -90.06249999863440792, 5.148502694627439702 ) ) ;
#35673 =( BOUNDED_CURVE ( )  B_SPLINE_CURVE ( 2, ( #15377, #5407, #1555, #16010, #21157, #59447, #55263, #60410, #44634 ),
 .UNSPECIFIED., .F., .F. ) 
 B_SPLINE_CURVE_WITH_KNOTS ( ( 3, 2, 2, 2, 3 ),
 ( 0.6232142857142857206, 0.6238095238095238138, 0.6250000000000000000, 0.6261904761904761862, 0.6267857142857142794 ),
 .UNSPECIFIED. ) 
 CURVE ( )  GEOMETRIC_REPRESENTATION_ITEM ( )  RATIONAL_B_SPLINE_CURVE ( ( 0.9330127018922194093, 0.9330127018922194093, 1.000000000000000000, 0.8660254037844387076, 1.000000000000000000, 0.8660254037844387076, 1.000000000000000000, 0.9330127018922194093, 0.9330127018922194093 ) ) 
 REPRESENTATION_ITEM ( '' )  );
#35674 = CARTESIAN_POINT ( 'NONE',  ( 5.000000000000000000, -25.29166666393547658, -2.886751345948129988 ) ) ;
#35676 = ORIENTED_EDGE ( 'NONE', *, *, #59400, .F. ) ;
#35675 = CARTESIAN_POINT ( 'NONE',  ( 2.229367062499998831, -54.64583333196773651, -3.861377020970580887 ) ) ;
#35677 = LINE ( 'NONE', #1597, #15062 ) ;
#35679 = ORIENTED_EDGE ( 'NONE', *, *, #3084, .F. ) ;
#35678 = CARTESIAN_POINT ( 'NONE',  ( -4.458734124999999437, -1.562499998634406140, 0.000000000000000000 ) ) ;
#35680 = CARTESIAN_POINT ( 'NONE',  ( -50.40829686548195099, -149.0000000013656063, -1.485763867205728284 ) ) ;
#35681 = CARTESIAN_POINT ( 'NONE',  ( 1.060575238724906964E-15, -64.75000000000000000, 5.773502691896257311 ) ) ;
#35682 = CARTESIAN_POINT ( 'NONE',  ( 2.730187237215162345E-16, -150.4375000013656063, -4.458734124999999437 ) ) ;
#35683 = CARTESIAN_POINT ( 'NONE',  ( -2.229367062500000163, -45.72916666530106511, -3.861377020970580443 ) ) ;
#35684 = CARTESIAN_POINT ( 'NONE',  ( -4.999999999999998224, -76.79166666393547303, 2.886751345948131764 ) ) ;
#35685 = AXIS2_PLACEMENT_3D ( 'NONE', #27941, #37596, #62059 ) ;
#35686 = CARTESIAN_POINT ( 'NONE',  ( -3.535533905932737309, -157.6250000000000284, -3.535533905932738197 ) ) ;
#35687 = DIRECTION ( 'NONE',  ( 0.000000000000000000, 0.000000000000000000, 1.000000000000000000 ) ) ;
#35688 = CARTESIAN_POINT ( 'NONE',  ( -58.24261429053147765, -152.2500000000000284, -3.805975901505573855 ) ) ;
#35689 = CARTESIAN_POINT ( 'NONE',  ( -3.152548672688508926E-16, -9.812499998634406140, -5.148502694627439702 ) ) ;
#35690 = AXIS2_PLACEMENT_3D ( 'NONE', #58164, #53024, #47874 ) ;
#35691 = CARTESIAN_POINT ( 'NONE',  ( 2.229367062500001939, -52.22916666530107221, 3.861377020970579999 ) ) ;
#35692 = CARTESIAN_POINT ( 'NONE',  ( 1.339745962155619807, 22.70534180126147561, -4.999999999999996447 ) ) ;
#35693 = CARTESIAN_POINT ( 'NONE',  ( -3.152801135295367985, -143.8125000013655779, 3.152801135295367096 ) ) ;
#35694 = CARTESIAN_POINT ( 'NONE',  ( 2.229367062499998831, -96.89583333196773651, -3.861377020970580887 ) ) ;
#35695 = CYLINDRICAL_SURFACE ( 'NONE', #24556, 5.000000000000000000 ) ;
#35696 = ORIENTED_EDGE ( 'NONE', *, *, #63342, .T. ) ;
#35697 = CARTESIAN_POINT ( 'NONE',  ( -1.339745962155610925, 14.33034180399266688, 5.000000000000000000 ) ) ;
#35698 = CARTESIAN_POINT ( 'NONE',  ( -4.458734124999999437, 27.35416666803225993, -2.574251347313719407 ) ) ;
#35699 = CARTESIAN_POINT ( 'NONE',  ( -52.53715891517739323, -147.5625000027312126, -4.819101127000233298 ) ) ;
#35700 = ORIENTED_EDGE ( 'NONE', *, *, #17254, .F. ) ;
#35701 = CARTESIAN_POINT ( 'NONE',  ( 4.458734124999998549, -2.729166665301069550, -2.574251347313721627 ) ) ;
#35702 = DIRECTION ( 'NONE',  ( -0.000000000000000000, 1.000000000000000000, -0.000000000000000000 ) ) ;
#35703 = CARTESIAN_POINT ( 'NONE',  ( 2.229367062499998831, -15.89583333196773651, -3.861377020970580887 ) ) ;
#35704 = CARTESIAN_POINT ( 'NONE',  ( 1.975475456537005874E-15, 9.250000000000000000, 5.000000000000000000 ) ) ;
#35705 = CARTESIAN_POINT ( 'NONE',  ( 9.457646018065525792E-16, -7.062499998634404363, 5.148502694627439702 ) ) ;
#35706 = CARTESIAN_POINT ( 'NONE',  ( 4.406466114817131796, -6.116179640279303165, -7.446478553994418270 ) ) ;
#35707 = CARTESIAN_POINT ( 'NONE',  ( -4.458734124999999437, -149.9375000013656063, -5.460374474430324690E-16 ) ) ;
#35708 = CARTESIAN_POINT ( 'NONE',  ( 2.229367062499998831, 17.10416666803225993, -3.861377020970580887 ) ) ;
#35709 = ORIENTED_EDGE ( 'NONE', *, *, #50275, .F. ) ;
#35710 = CARTESIAN_POINT ( 'NONE',  ( -2.500000000000000444, -14.04166666393548013, -4.330127018922193649 ) ) ;
#35711 = CARTESIAN_POINT ( 'NONE',  ( -4.999999999999998224, -12.91666666666666607, 2.886751345948131764 ) ) ;
#35712 = CARTESIAN_POINT ( 'NONE',  ( 4.458734124999999437, -21.81249999863440436, -5.460374474430324690E-16 ) ) ;
#35713 = DIRECTION ( 'NONE',  ( -0.000000000000000000, -0.000000000000000000, 1.000000000000000000 ) ) ;
#35714 = CARTESIAN_POINT ( 'NONE',  ( 5.000000000000000888, 1.541666669397853795, 2.886751345948126879 ) ) ;
#35715 = CARTESIAN_POINT ( 'NONE',  ( -59.59170313451811296, -150.5000000013655779, 1.485763867205729394 ) ) ;
#35716 = CARTESIAN_POINT ( 'NONE',  ( 2.499999999999998668, -49.20833333060213732, -4.330127018922193649 ) ) ;
#35717 = CARTESIAN_POINT ( 'NONE',  ( 0.000000000000000000, -170.0000000000000000, 5.000000000000000000 ) ) ;
#35718 = CARTESIAN_POINT ( 'NONE',  ( -4.458734124999999437, 9.687500001365593860, 0.000000000000000000 ) ) ;
#35719 = DIRECTION ( 'NONE',  ( 0.000000000000000000, 0.000000000000000000, 1.000000000000000000 ) ) ;
#35720 = DIRECTION ( 'NONE',  ( 0.000000000000000000, 0.000000000000000000, 1.000000000000000000 ) ) ;
#35721 = CARTESIAN_POINT ( 'NONE',  ( 9.457646018065525792E-16, 11.93750000136559564, 5.148502694627439702 ) ) ;
#35722 = CARTESIAN_POINT ( 'NONE',  ( -2.229367062500000163, -66.47916666530106511, -3.861377020970580443 ) ) ;
#35723 = CARTESIAN_POINT ( 'NONE',  ( -3.152548672688508926E-16, -12.81249999863440259, -5.148502694627439702 ) ) ;
#35724 =( BOUNDED_CURVE ( )  B_SPLINE_CURVE ( 2, ( #61217, #40628, #60271, #16189, #17142, #35816, #36766, #55440, #31933 ),
 .UNSPECIFIED., .F., .F. ) 
 B_SPLINE_CURVE_WITH_KNOTS ( ( 3, 2, 2, 2, 3 ),
 ( 0.7229166666666666519, 0.7236111111111110938, 0.7249999999999999778, 0.7263888888888888618, 0.7270833333333333037 ),
 .UNSPECIFIED. ) 
 CURVE ( )  GEOMETRIC_REPRESENTATION_ITEM ( )  RATIONAL_B_SPLINE_CURVE ( ( 0.9330127018922194093, 0.9330127018922194093, 1.000000000000000000, 0.8660254037844387076, 1.000000000000000000, 0.8660254037844387076, 1.000000000000000000, 0.9330127018922194093, 0.9330127018922194093 ) ) 
 REPRESENTATION_ITEM ( '' )  );
#35725 = CARTESIAN_POINT ( 'NONE',  ( 2.500000000000002220, 3.333333333333333925, 4.330127018922192761 ) ) ;
#35726 = CARTESIAN_POINT ( 'NONE',  ( -4.458734125000001214, -162.8750000013655779, 1.846868145590734089 ) ) ;
#35727 = CARTESIAN_POINT ( 'NONE',  ( -2.499999999999996447, -40.70833333060214443, 4.330127018922195425 ) ) ;
#35728 = CARTESIAN_POINT ( 'NONE',  ( 4.458734124999999437, -60.81249999863440081, -5.460374474430324690E-16 ) ) ;
#35729 = CARTESIAN_POINT ( 'NONE',  ( -5.000000000000000000, -94.87499999726881583, 0.000000000000000000 ) ) ;
#35730 = EDGE_CURVE ( 'NONE', #63287, #35203, #47613, .T. ) ;
#35731 = VECTOR ( 'NONE', #11351, 1000.000000000000000 ) ;
#35732 = CARTESIAN_POINT ( 'NONE',  ( -6.972266317189433020E-16, -42.12499999726880873, -5.000000000000000000 ) ) ;
#35733 = LINE ( 'NONE', #46333, #39836 ) ;
#35734 = CARTESIAN_POINT ( 'NONE',  ( 5.000000000000000888, 5.541666669397853795, 2.886751345948126879 ) ) ;
#35735 = CARTESIAN_POINT ( 'NONE',  ( 2.229367062499998831, -34.64583333196772941, -3.861377020970580887 ) ) ;
#35736 = CARTESIAN_POINT ( 'NONE',  ( 1.339745962155615144, -51.58034179853028434, 4.999999999999999112 ) ) ;
#35737 = CARTESIAN_POINT ( 'NONE',  ( 1.060575238724906964E-15, -45.75000000000000000, 5.773502691896257311 ) ) ;
#35738 = CARTESIAN_POINT ( 'NONE',  ( -6.972266317189433020E-16, -13.25000000000000000, -5.000000000000000000 ) ) ;
#35739 = CARTESIAN_POINT ( 'NONE',  ( 2.499999999999998668, -86.20833333060214443, -4.330127018922193649 ) ) ;
#35740 = VERTEX_POINT ( 'NONE', #47939 ) ;
#35741 = CARTESIAN_POINT ( 'NONE',  ( -4.458734124999999437, -104.3958333319677365, -2.574251347313719407 ) ) ;
#35742 = CARTESIAN_POINT ( 'NONE',  ( 4.458734124999999437, -2.062499998634406584, -5.460374474430324690E-16 ) ) ;
#35743 = CARTESIAN_POINT ( 'NONE',  ( 6.123233995736766282E-16, -170.0000000000000000, -5.000000000000000000 ) ) ;
#35744 = CARTESIAN_POINT ( 'NONE',  ( 5.000000000000000000, -3.500000000000003109, -6.123233995736766282E-16 ) ) ;
#35745 = EDGE_CURVE ( 'NONE', #21770, #969, #58549, .T. ) ;
#35746 = CARTESIAN_POINT ( 'NONE',  ( 2.229367062499998831, -69.64583333196773651, -3.861377020970580887 ) ) ;
#35747 = CARTESIAN_POINT ( 'NONE',  ( -4.999999999999999112, -5.791666663935480130, 2.886751345948131764 ) ) ;
#35749 = ORIENTED_EDGE ( 'NONE', *, *, #26466, .T. ) ;
#35748 = CARTESIAN_POINT ( 'NONE',  ( 4.458734125000001214, -40.89583333196773651, 2.574251347313718519 ) ) ;
#35750 = CARTESIAN_POINT ( 'NONE',  ( 5.000000000000000888, -33.58333333333332860, 2.886751345948126879 ) ) ;
#35751 = EDGE_CURVE ( 'NONE', #24823, #58440, #35471, .T. ) ;
#35753 = ORIENTED_EDGE ( 'NONE', *, *, #9074, .F. ) ;
#35752 = CARTESIAN_POINT ( 'NONE',  ( 9.457646018065525792E-16, 9.687500001365593860, 5.148502694627439702 ) ) ;
#35754 = CARTESIAN_POINT ( 'NONE',  ( -2.500000000000000444, -49.04166666393547303, -4.330127018922193649 ) ) ;
#35755 = CARTESIAN_POINT ( 'NONE',  ( -5.000000000000000000, -51.00000000000000711, 0.000000000000000000 ) ) ;
#35756 = CARTESIAN_POINT ( 'NONE',  ( 4.458734125000001214, -33.14583333196774362, 2.574251347313718519 ) ) ;
#35757 = CARTESIAN_POINT ( 'NONE',  ( -1.339745962155613812, -42.08034179853029144, -5.000000000000000000 ) ) ;
#35758 = CARTESIAN_POINT ( 'NONE',  ( 2.229367062500001939, -74.97916666530106511, 3.861377020970579999 ) ) ;
#35759 = CARTESIAN_POINT ( 'NONE',  ( -2.071067811865475061, -169.6875000000000284, -5.000000000000000888 ) ) ;
#35760 = CARTESIAN_POINT ( 'NONE',  ( 2.229367062500001939, -79.97916666530106511, 3.861377020970579999 ) ) ;
#35761 = CARTESIAN_POINT ( 'NONE',  ( -57.89159099828107458, -133.9375000013656063, -3.393966926194107447 ) ) ;
#35762 = ADVANCED_FACE ( 'NONE', ( #13221 ), #53400, .T. ) ;
#35763 = CARTESIAN_POINT ( 'NONE',  ( -4.458734124999998549, -35.47916666530107221, 2.574251347313722516 ) ) ;
#35764 = ORIENTED_EDGE ( 'NONE', *, *, #28667, .F. ) ;
#35765 = CARTESIAN_POINT ( 'NONE',  ( -1.339745962155608039, 23.91965820146970501, -5.000000000000004441 ) ) ;
#35766 = ORIENTED_EDGE ( 'NONE', *, *, #44364, .F. ) ;
#35767 = CARTESIAN_POINT ( 'NONE',  ( 2.229367062500001939, -80.22916666530106511, 3.861377020970579999 ) ) ;
#35768 = CARTESIAN_POINT ( 'NONE',  ( -6.972266317189433020E-16, 21.87500000273118417, -5.000000000000000000 ) ) ;
#35769 = VERTEX_POINT ( 'NONE', #52471 ) ;
#35770 = CARTESIAN_POINT ( 'NONE',  ( 0.000000000000000000, -120.0000000000000000, 0.000000000000000000 ) ) ;
#35771 = VECTOR ( 'NONE', #35026, 1000.000000000000000 ) ;
#35772 =( BOUNDED_CURVE ( )  B_SPLINE_CURVE ( 2, ( #53727, #9658, #19945, #14481, #48264, #49221, #29911, #58241, #24147 ),
 .UNSPECIFIED., .F., .F. ) 
 B_SPLINE_CURVE_WITH_KNOTS ( ( 3, 2, 2, 2, 3 ),
 ( 0.4482142857142857317, 0.4488095238095238249, 0.4500000000000000111, 0.4511904761904761973, 0.4517857142857142905 ),
 .UNSPECIFIED. ) 
 CURVE ( )  GEOMETRIC_REPRESENTATION_ITEM ( )  RATIONAL_B_SPLINE_CURVE ( ( 0.9330127018922194093, 0.9330127018922194093, 1.000000000000000000, 0.8660254037844387076, 1.000000000000000000, 0.8660254037844387076, 1.000000000000000000, 0.9330127018922194093, 0.9330127018922194093 ) ) 
 REPRESENTATION_ITEM ( '' )  );
#35773 = CARTESIAN_POINT ( 'NONE',  ( 2.229367062500001939, -65.22916666530106511, 3.861377020970579999 ) ) ;
#35774 = VECTOR ( 'NONE', #29615, 1000.000000000000000 ) ;
#35775 = CARTESIAN_POINT ( 'NONE',  ( -4.458734124999999437, -1.645833331967737401, -2.574251347313719407 ) ) ;
#35776 = ORIENTED_EDGE ( 'NONE', *, *, #17576, .F. ) ;
#35777 = CARTESIAN_POINT ( 'NONE',  ( 5.000000000000000888, 3.541666669397852019, 2.886751345948126879 ) ) ;
#35778 = CARTESIAN_POINT ( 'NONE',  ( -6.972266317189433020E-16, 2.875000002731185500, -5.000000000000000000 ) ) ;
#35779 = ORIENTED_EDGE ( 'NONE', *, *, #56962, .T. ) ;
#35780 = EDGE_CURVE ( 'NONE', #14985, #11315, #55204, .T. ) ;
#35781 = FACE_OUTER_BOUND ( 'NONE', #31008, .T. ) ;
#35782 = CARTESIAN_POINT ( 'NONE',  ( 9.457646018065525792E-16, 9.937500001365592084, 5.148502694627439702 ) ) ;
#35783 = CARTESIAN_POINT ( 'NONE',  ( 3.061616997868383141E-16, -153.7500000000000000, -5.000000000000000000 ) ) ;
#35784 = CARTESIAN_POINT ( 'NONE',  ( -1.846868145590734756, -162.1250000013656347, -4.458734124999999437 ) ) ;
#35785 = CARTESIAN_POINT ( 'NONE',  ( 2.500000000000002220, -75.54166666393547303, 4.330127018922192761 ) ) ;
#35786 = ORIENTED_EDGE ( 'NONE', *, *, #16092, .F. ) ;
#35787 = CARTESIAN_POINT ( 'NONE',  ( 9.457646018065525792E-16, -79.06249999863440792, 5.148502694627439702 ) ) ;
#35788 = CARTESIAN_POINT ( 'NONE',  ( 3.535533905932736864, -164.2500000027312126, 3.535533905932738641 ) ) ;
#35789 = CARTESIAN_POINT ( 'NONE',  ( -2.229367062500000163, -4.479166665301070438, -3.861377020970580443 ) ) ;
#35790 = CYLINDRICAL_SURFACE ( 'NONE', #4669, 5.000000000000000000 ) ;
#35791 = CARTESIAN_POINT ( 'NONE',  ( -2.500000000000000444, -68.16666666666667140, -4.330127018922193649 ) ) ;
#35792 = CARTESIAN_POINT ( 'NONE',  ( 2.229367062499998831, -72.89583333196773651, -3.861377020970580887 ) ) ;
#35793 = CARTESIAN_POINT ( 'NONE',  ( 5.000000000000000000, -29.37499999726881228, -6.123233995736766282E-16 ) ) ;
#35794 = CARTESIAN_POINT ( 'NONE',  ( 0.000000000000000000, -120.0000000000000000, 0.000000000000000000 ) ) ;
#35795 = CARTESIAN_POINT ( 'NONE',  ( -2.500000000000000444, -1.041666663935479686, -4.330127018922193649 ) ) ;
#35796 = CARTESIAN_POINT ( 'NONE',  ( 2.499999999999998668, -104.3333333333333286, -4.330127018922193649 ) ) ;
#35797 = CARTESIAN_POINT ( 'NONE',  ( 1.975475456537005874E-15, -82.62499999726878741, 5.000000000000000000 ) ) ;
#35798 = CARTESIAN_POINT ( 'NONE',  ( 2.229367062500001939, -49.97916666530107221, 3.861377020970579999 ) ) ;
#35799 = CARTESIAN_POINT ( 'NONE',  ( 4.458734124999999437, -34.06249999863440792, -5.460374474430324690E-16 ) ) ;
#35800 = CARTESIAN_POINT ( 'NONE',  ( 4.458734124999999437, 3.937500001365595192, -5.460374474430324690E-16 ) ) ;
#35801 = CARTESIAN_POINT ( 'NONE',  ( -5.000000000000000000, -18.08333333333333215, -2.886751345948128211 ) ) ;
#35802 = CARTESIAN_POINT ( 'NONE',  ( 2.500000000000002220, 20.33333333333333215, 4.330127018922192761 ) ) ;
#35803 = CARTESIAN_POINT ( 'NONE',  ( -5.000000000000000888, -143.6875000027312126, -2.071067811865475949 ) ) ;
#35804 = CARTESIAN_POINT ( 'NONE',  ( 2.499999999999998668, -26.20833333060214798, -4.330127018922193649 ) ) ;
#35805 = CARTESIAN_POINT ( 'NONE',  ( -2.229367062500000163, -43.47916666530106511, -3.861377020970580443 ) ) ;
#35806 = CARTESIAN_POINT ( 'NONE',  ( -2.499999999999996447, -80.70833333060213022, 4.330127018922195425 ) ) ;
#35807 = CARTESIAN_POINT ( 'NONE',  ( -50.70258187064364108, -138.3750000013656063, 2.196230717870141014 ) ) ;
#35808 = CARTESIAN_POINT ( 'NONE',  ( 2.071067811865475505, -140.8125000000000000, -5.000000000000000888 ) ) ;
#35809 = ADVANCED_FACE ( 'NONE', ( #33784 ), #47324, .T. ) ;
#35810 = CARTESIAN_POINT ( 'NONE',  ( -1.250000000000000444, -7.938566201357367902, -7.198902722707430257 ) ) ;
#35811 = EDGE_CURVE ( 'NONE', #14927, #49915, #16121, .T. ) ;
#35812 = CARTESIAN_POINT ( 'NONE',  ( -4.458734124999999437, -78.64583333196773651, -2.574251347313719407 ) ) ;
#35813 = CARTESIAN_POINT ( 'NONE',  ( -3.152801135295367096, -162.3125000013656063, -3.152801135295367541 ) ) ;
#35814 = CARTESIAN_POINT ( 'NONE',  ( 1.975475456537005874E-15, -59.62499999726880873, 5.000000000000000000 ) ) ;
#35815 = CARTESIAN_POINT ( 'NONE',  ( 5.000000000000000000, -27.41666666666666785, -2.886751345948129988 ) ) ;
#35816 = CARTESIAN_POINT ( 'NONE',  ( -5.000000000000000000, -57.08333333333333570, -2.886751345948128211 ) ) ;
#35817 = ORIENTED_EDGE ( 'NONE', *, *, #38479, .T. ) ;
#35818 = CARTESIAN_POINT ( 'NONE',  ( -3.152548672688508926E-16, 24.18750000136559564, -5.148502694627439702 ) ) ;
#35819 = ORIENTED_EDGE ( 'NONE', *, *, #37063, .F. ) ;
#35820 = VECTOR ( 'NONE', #2025, 1000.000000000000000 ) ;
#35821 = CARTESIAN_POINT ( 'NONE',  ( 5.000000000000000888, 22.54166666939784847, 2.886751345948126879 ) ) ;
#35822 = DIRECTION ( 'NONE',  ( 0.000000000000000000, 0.000000000000000000, 1.000000000000000000 ) ) ;
#35823 = CARTESIAN_POINT ( 'NONE',  ( 5.000000000000000000, 15.50000000000000000, -6.123233995736766282E-16 ) ) ;
#35824 = AXIS2_PLACEMENT_3D ( 'NONE', #164, #34884, #54506 ) ;
#35825 = EDGE_CURVE ( 'NONE', #11293, #32107, #44465, .T. ) ;
#35826 = CARTESIAN_POINT ( 'NONE',  ( 4.458734125000000326, -50.89583333196772230, 2.574251347313718519 ) ) ;
#35827 = CARTESIAN_POINT ( 'NONE',  ( -2.229367062499996610, -10.14583333196773829, 3.861377020970582219 ) ) ;
#35828 = CARTESIAN_POINT ( 'NONE',  ( -55.00000000000002132, -155.0000000000000284, 1.734723475976807094E-15 ) ) ;
#35829 = CARTESIAN_POINT ( 'NONE',  ( 1.975475456537005874E-15, -99.62499999726880162, 5.000000000000000000 ) ) ;
#35830 = CARTESIAN_POINT ( 'NONE',  ( -5.000000000000000000, -37.08333333333332860, -2.886751345948128211 ) ) ;
#35831 = EDGE_CURVE ( 'NONE', #17008, #50534, #57651, .T. ) ;
#35832 = CARTESIAN_POINT ( 'NONE',  ( -1.339745962155610925, -74.66965819600731891, 5.000000000000000000 ) ) ;
#35833 = CARTESIAN_POINT ( 'NONE',  ( -4.999999999999999112, -31.91666666666666430, 2.886751345948131764 ) ) ;
#35834 = FACE_OUTER_BOUND ( 'NONE', #50322, .T. ) ;
#35836 = CARTESIAN_POINT ( 'NONE',  ( -3.152548672688508926E-16, -13.81249999863440436, -5.148502694627439702 ) ) ;
#35835 = CARTESIAN_POINT ( 'NONE',  ( -4.999999999999998224, -33.91666666666666430, 2.886751345948131764 ) ) ;
#35837 = CARTESIAN_POINT ( 'NONE',  ( -3.535533905932737309, -140.7500000027311842, -3.535533905932738197 ) ) ;
#35838 = CARTESIAN_POINT ( 'NONE',  ( -4.458734124999998549, -61.22916666530106511, 2.574251347313722516 ) ) ;
#35839 = CARTESIAN_POINT ( 'NONE',  ( -1.846868145590737420, -151.0000000013656063, 4.458734124999999437 ) ) ;
#35840 = CARTESIAN_POINT ( 'NONE',  ( -3.152548672688508926E-16, -63.56249999863440792, -5.148502694627439702 ) ) ;
#35841 = CARTESIAN_POINT ( 'NONE',  ( 5.000000000000000000, -57.37499999726880162, -6.123233995736766282E-16 ) ) ;
#35842 = ORIENTED_EDGE ( 'NONE', *, *, #34943, .T. ) ;
#35843 = CARTESIAN_POINT ( 'NONE',  ( 5.000000000000000888, 13.41666666666666785, 2.886751345948126879 ) ) ;
#35844 = VERTEX_POINT ( 'NONE', #989 ) ;
#35846 = CARTESIAN_POINT ( 'NONE',  ( 5.000000000000000888, -103.5833333333333428, 2.886751345948126879 ) ) ;
#35845 = CARTESIAN_POINT ( 'NONE',  ( 2.500000000000002220, -21.66666666666666785, 4.330127018922192761 ) ) ;
#35847 = CARTESIAN_POINT ( 'NONE',  ( -3.152801135295367096, -153.0625000013656063, -3.152801135295367541 ) ) ;
#35848 = ORIENTED_EDGE ( 'NONE', *, *, #11054, .F. ) ;
#35849 = CARTESIAN_POINT ( 'NONE',  ( -9.184850993605147944E-16, -169.2500000000000000, 5.000000000000000000 ) ) ;
#35850 = CARTESIAN_POINT ( 'NONE',  ( -51.19402409849444524, -128.5000000000000284, -3.242614290531456334 ) ) ;
#35851 = CARTESIAN_POINT ( 'NONE',  ( 5.000000000000000888, -161.0625000027312126, -2.071067811865475505 ) ) ;
#35852 = CARTESIAN_POINT ( 'NONE',  ( -4.458734124999998549, -47.47916666530106511, 2.574251347313722516 ) ) ;
#35853 = EDGE_LOOP ( 'NONE', ( #58573, #11631, #61859, #24679 ) ) ;
#35854 =( BOUNDED_CURVE ( )  B_SPLINE_CURVE ( 2, ( #25325, #15359, #30459, #6041, #54599, #10521, #19540, #43973, #63619 ),
 .UNSPECIFIED., .F., .F. ) 
 B_SPLINE_CURVE_WITH_KNOTS ( ( 3, 2, 2, 2, 3 ),
 ( 0.05625000000000000139, 0.05694444444444444337, 0.05833333333333333426, 0.05972222222222222515, 0.06041666666666666713 ),
 .UNSPECIFIED. ) 
 CURVE ( )  GEOMETRIC_REPRESENTATION_ITEM ( )  RATIONAL_B_SPLINE_CURVE ( ( 0.9330127018922192983, 0.9330127018922196314, 1.000000000000000000, 0.8660254037844387076, 1.000000000000000000, 0.8660254037844387076, 1.000000000000000000, 0.9330127018922194093, 0.9330127018922194093 ) ) 
 REPRESENTATION_ITEM ( '' )  );
#35855 = CARTESIAN_POINT ( 'NONE',  ( -1.339745962155613812, 16.91965820146970145, -5.000000000000000000 ) ) ;
#35856 = CARTESIAN_POINT ( 'NONE',  ( -3.152548672688508926E-16, 11.43750000136559386, -5.148502694627439702 ) ) ;
#35857 = CARTESIAN_POINT ( 'NONE',  ( -4.458734124999999437, 22.60416666803225993, -2.574251347313719407 ) ) ;
#35858 = CARTESIAN_POINT ( 'NONE',  ( -55.35523342533222291, -154.3125000013656347, 4.444560631937231499 ) ) ;
#35859 = CARTESIAN_POINT ( 'NONE',  ( 5.000000000000000888, -44.58333333333333570, 2.886751345948126879 ) ) ;
#35860 = CARTESIAN_POINT ( 'NONE',  ( 1.975475456537005874E-15, -100.7499999999999858, 5.000000000000000000 ) ) ;
#35861 = AXIS2_PLACEMENT_3D ( 'NONE', #62951, #22460, #51726 ) ;
#35862 = EDGE_LOOP ( 'NONE', ( #37816, #42242, #9099, #32416 ) ) ;
#35863 = CARTESIAN_POINT ( 'NONE',  ( -4.458734124999999437, -66.31249999863440792, 0.000000000000000000 ) ) ;
#35864 = CARTESIAN_POINT ( 'NONE',  ( 1.975475456537005874E-15, -28.62499999726881583, 5.000000000000000000 ) ) ;
#35865 = CARTESIAN_POINT ( 'NONE',  ( -4.458734124999999437, 13.68750000136559386, 0.000000000000000000 ) ) ;
#35866 = CARTESIAN_POINT ( 'NONE',  ( -1.339745962155610925, -62.79465819873851729, 5.000000000000000000 ) ) ;
#35867 = CARTESIAN_POINT ( 'NONE',  ( 0.000000000000000000, -120.0000000000000000, 0.000000000000000000 ) ) ;
#35868 = CARTESIAN_POINT ( 'NONE',  ( -4.458734124999998549, -57.47916666530108643, 2.574251347313722516 ) ) ;
#35869 = CARTESIAN_POINT ( 'NONE',  ( 5.000000000000000000, -12.37499999726881050, -6.123233995736766282E-16 ) ) ;
#35870 = DIRECTION ( 'NONE',  ( 0.000000000000000000, 0.000000000000000000, 1.000000000000000000 ) ) ;
#35871 = CARTESIAN_POINT ( 'NONE',  ( 2.500000000000002220, -87.66666666666667140, 4.330127018922192761 ) ) ;
#35872 = CARTESIAN_POINT ( 'NONE',  ( 2.499999999999998668, -104.2083333306021444, -4.330127018922193649 ) ) ;
#35873 = CARTESIAN_POINT ( 'NONE',  ( 4.458734124999998549, -14.97916666530107399, -2.574251347313721627 ) ) ;
#35874 = VERTEX_POINT ( 'NONE', #35373 ) ;
#35875 = CARTESIAN_POINT ( 'NONE',  ( -3.535533905932738641, -143.5000000027311842, 3.535533905932737309 ) ) ;
#35876 = CARTESIAN_POINT ( 'NONE',  ( 4.458734124999998549, -105.7291666653010651, -2.574251347313721627 ) ) ;
#35877 = CARTESIAN_POINT ( 'NONE',  ( 5.000000000000000888, -158.0625000027312126, -2.071067811865475505 ) ) ;
#35878 = EDGE_LOOP ( 'NONE', ( #28811, #985, #11238, #23594 ) ) ;
#35879 = CARTESIAN_POINT ( 'NONE',  ( -3.152548672688508926E-16, -102.8124999986344221, -5.148502694627439702 ) ) ;
#35880 = CARTESIAN_POINT ( 'NONE',  ( -4.458734124999999437, -28.31249999863440081, 0.000000000000000000 ) ) ;
#35881 = CARTESIAN_POINT ( 'NONE',  ( 5.000000000000000000, -62.37499999726880873, -6.123233995736766282E-16 ) ) ;
#35882 = CARTESIAN_POINT ( 'NONE',  ( -56.48576386720575471, -152.0000000013655779, -4.591703134518078322 ) ) ;
#35883 = CARTESIAN_POINT ( 'NONE',  ( -51.60603307380591787, -140.9375000013656063, -2.891590998281053704 ) ) ;
#35884 = EDGE_CURVE ( 'NONE', #20081, #38026, #22713, .T. ) ;
#35885 = CARTESIAN_POINT ( 'NONE',  ( -3.152548672688508926E-16, -22.56249999863440436, -5.148502694627439702 ) ) ;
#35886 = CARTESIAN_POINT ( 'NONE',  ( 2.229367062499998831, -61.89583333196774362, -3.861377020970580887 ) ) ;
#35887 = CARTESIAN_POINT ( 'NONE',  ( -6.972266317189433020E-16, -40.12499999726880162, -5.000000000000000000 ) ) ;
#35888 = CARTESIAN_POINT ( 'NONE',  ( 9.457646018065525792E-16, -21.06249999863440436, 5.148502694627439702 ) ) ;
#35889 = DIRECTION ( 'NONE',  ( -1.000000000000000000, 0.000000000000000000, -7.709882115452477180E-16 ) ) ;
#35890 = CARTESIAN_POINT ( 'NONE',  ( -3.535533905932737309, -151.6250000000000000, -3.535533905932738197 ) ) ;
#35891 = CARTESIAN_POINT ( 'NONE',  ( 5.000000000000000888, -13.58333333333333570, 2.886751345948126879 ) ) ;
#35892 = CARTESIAN_POINT ( 'NONE',  ( -4.458734125000000326, -153.0000000013656063, -1.846868145590735644 ) ) ;
#35893 = ORIENTED_EDGE ( 'NONE', *, *, #5153, .F. ) ;
#35894 = CARTESIAN_POINT ( 'NONE',  ( 4.458734124999998549, -44.97916666530107221, -2.574251347313721627 ) ) ;
#35895 = CARTESIAN_POINT ( 'NONE',  ( 5.000000000000000000, -38.37499999726881583, -6.123233995736766282E-16 ) ) ;
#35896 = CARTESIAN_POINT ( 'NONE',  ( -5.000000000000000000, 27.00000000000000000, 0.000000000000000000 ) ) ;
#35897 = CARTESIAN_POINT ( 'NONE',  ( 4.458734125000001214, 6.104166668032262599, 2.574251347313718519 ) ) ;
#35898 = CARTESIAN_POINT ( 'NONE',  ( -6.972266317189433020E-16, -74.12499999726878741, -5.000000000000000000 ) ) ;
#35899 = CARTESIAN_POINT ( 'NONE',  ( 1.339745962155615144, -37.58034179853029144, 4.999999999999999112 ) ) ;
#35900 = CARTESIAN_POINT ( 'NONE',  ( -6.972266317189433020E-16, -82.24999999999998579, -5.000000000000000000 ) ) ;
#35901 = CARTESIAN_POINT ( 'NONE',  ( 2.229367062500001939, 13.77083333469892779, 3.861377020970579999 ) ) ;
#35902 = CARTESIAN_POINT ( 'NONE',  ( 2.500000000000002220, -81.66666666666667140, 4.330127018922192761 ) ) ;
#35903 =( BOUNDED_CURVE ( )  B_SPLINE_CURVE ( 2, ( #51338, #15957, #21102, #56158, #21749, #61304, #55839, #46505, #6628 ),
 .UNSPECIFIED., .F., .F. ) 
 B_SPLINE_CURVE_WITH_KNOTS ( ( 3, 2, 2, 2, 3 ),
 ( 0.9083333333333332149, 0.9124999999999998668, 0.9166666666666665186, 0.9208333333333330595, 0.9249999999999998224 ),
 .UNSPECIFIED. ) 
 CURVE ( )  GEOMETRIC_REPRESENTATION_ITEM ( )  RATIONAL_B_SPLINE_CURVE ( ( 1.000000000000001998, 0.9238795325112847401, 1.000000000000000000, 0.9238795325112867385, 1.000000000000000000, 0.9238795325112867385, 1.000000000000000000, 0.9238795325112908463, 0.9999999999999958922 ) ) 
 REPRESENTATION_ITEM ( '' )  );
#35904 = CARTESIAN_POINT ( 'NONE',  ( -5.000000000000000000, 10.12500000273118594, 0.000000000000000000 ) ) ;
#35906 = VERTEX_POINT ( 'NONE', #20264 ) ;
#35905 = EDGE_CURVE ( 'NONE', #19582, #45000, #39544, .T. ) ;
#35907 = CARTESIAN_POINT ( 'NONE',  ( 2.071067811865550556, -162.3125000027312410, 4.999999999999925393 ) ) ;
#35908 = ORIENTED_EDGE ( 'NONE', *, *, #42050, .F. ) ;
#35909 = CARTESIAN_POINT ( 'NONE',  ( 5.000000000000000000, 26.50000000000000000, -6.123233995736766282E-16 ) ) ;
#35910 = CARTESIAN_POINT ( 'NONE',  ( -2.229367062500000163, -45.47916666530106511, -3.861377020970580443 ) ) ;
#35911 = EDGE_CURVE ( 'NONE', #11571, #4948, #31329, .T. ) ;
#35912 = CARTESIAN_POINT ( 'NONE',  ( 2.730187237215162345E-16, -165.4375000013655779, -4.458734124999999437 ) ) ;
#35913 = VECTOR ( 'NONE', #39190, 1000.000000000000000 ) ;
#35914 = EDGE_CURVE ( 'NONE', #48710, #40464, #18816, .T. ) ;
#35915 = CARTESIAN_POINT ( 'NONE',  ( -2.500000000000000444, -42.04166666393548013, -4.330127018922193649 ) ) ;
#35916 = ORIENTED_EDGE ( 'NONE', *, *, #15431, .T. ) ;
#35917 = CARTESIAN_POINT ( 'NONE',  ( -4.458734124999999437, -16.31249999863440436, 0.000000000000000000 ) ) ;
#35918 = ORIENTED_EDGE ( 'NONE', *, *, #46347, .T. ) ;
#35919 = CARTESIAN_POINT ( 'NONE',  ( -3.535250795749689387E-16, -87.24999999999998579, -5.773502691896257311 ) ) ;
#35920 = CARTESIAN_POINT ( 'NONE',  ( 4.458734124999999437, -167.5000000013655779, 1.846868145590737864 ) ) ;
#35921 = CARTESIAN_POINT ( 'NONE',  ( 1.060575238724906964E-15, -86.62499999726881583, 5.773502691896257311 ) ) ;
#35923 = ORIENTED_EDGE ( 'NONE', *, *, #61113, .T. ) ;
#35922 = CARTESIAN_POINT ( 'NONE',  ( 5.000000000000000000, -20.29166666393548368, -2.886751345948130876 ) ) ;
#35924 = CARTESIAN_POINT ( 'NONE',  ( -49.85088928181150436, -142.5625000000000284, -1.666127454062680702 ) ) ;
#35925 = CARTESIAN_POINT ( 'NONE',  ( -4.458734124999999437, -30.56249999863440436, 0.000000000000000000 ) ) ;
#35926 = CARTESIAN_POINT ( 'NONE',  ( -1.049326080737009628E-13, -5.624999997268816720, 5.000000000000000000 ) ) ;
#35927 = ORIENTED_EDGE ( 'NONE', *, *, #24714, .F. ) ;
#35928 = ITEM_DEFINED_TRANSFORMATION ( 'NONE', 'NONE', #8225,  #43054 ) ;
#35929 = CARTESIAN_POINT ( 'NONE',  ( 2.229367062499998831, -79.64583333196773651, -3.861377020970580887 ) ) ;
#35930 = CARTESIAN_POINT ( 'NONE',  ( 4.458734125000001214, -109.1458333319677365, 2.574251347313718519 ) ) ;
#35931 = CARTESIAN_POINT ( 'NONE',  ( -55.39835681537999790, -137.0000000027312126, 4.984105922594378235 ) ) ;
#35932 = ORIENTED_EDGE ( 'NONE', *, *, #7570, .F. ) ;
#35933 = CARTESIAN_POINT ( 'NONE',  ( -2.500000000000000444, -26.16666666666666430, -4.330127018922193649 ) ) ;
#35934 = CARTESIAN_POINT ( 'NONE',  ( -50.70258187064364108, -143.3750000013656063, 2.196230717870141014 ) ) ;
#35935 = CARTESIAN_POINT ( 'NONE',  ( 4.458734124999998549, -81.97916666530106511, -2.574251347313721627 ) ) ;
#35936 = CARTESIAN_POINT ( 'NONE',  ( -49.85088928181150436, -132.6875000027312410, -1.666127454062680702 ) ) ;
#35937 = CARTESIAN_POINT ( 'NONE',  ( 4.458734125000000326, -44.89583333196774362, 2.574251347313718519 ) ) ;
#35938 = CARTESIAN_POINT ( 'NONE',  ( -3.152801135295367985, -143.0625000013655779, 3.152801135295367096 ) ) ;
#35939 = CARTESIAN_POINT ( 'NONE',  ( -1.339745962155613812, -58.20534180126147561, -5.000000000000000000 ) ) ;
#35940 = CARTESIAN_POINT ( 'NONE',  ( -2.229367062500000163, -48.47916666530106511, -3.861377020970580443 ) ) ;
#35941 = CARTESIAN_POINT ( 'NONE',  ( -3.152548672688508926E-16, -43.56249999863439371, -5.148502694627439702 ) ) ;
#35942 = CARTESIAN_POINT ( 'NONE',  ( -4.458734124999998549, 26.77083333469893134, 2.574251347313722516 ) ) ;
#35943 = CARTESIAN_POINT ( 'NONE',  ( 4.458734124999998549, -16.72916666530107577, -2.574251347313721627 ) ) ;
#35944 = CARTESIAN_POINT ( 'NONE',  ( -5.000000000000000000, -100.0000000000000000, 0.000000000000000000 ) ) ;
#35945 = CARTESIAN_POINT ( 'NONE',  ( 4.458734124999999437, -140.7500000013655779, 1.846868145590737864 ) ) ;
#35946 = CARTESIAN_POINT ( 'NONE',  ( -2.229367062499996610, -39.39583333196773651, 3.861377020970582219 ) ) ;
#35947 = CARTESIAN_POINT ( 'NONE',  ( 5.000000000000000000, 1.708333336064519425, -2.886751345948129988 ) ) ;
#35948 = CARTESIAN_POINT ( 'NONE',  ( -6.972266317189433020E-16, -50.24999999999999289, -5.000000000000000000 ) ) ;
#35949 = CARTESIAN_POINT ( 'NONE',  ( -50.40829686548195099, -130.0000000013656063, -1.485763867205728284 ) ) ;
#35950 = CARTESIAN_POINT ( 'NONE',  ( -3.152548672688508926E-16, -77.81249999863440792, -5.148502694627439702 ) ) ;
#35951 = CARTESIAN_POINT ( 'NONE',  ( -5.000000000000000000, 5.999999999999998224, 0.000000000000000000 ) ) ;
#35952 = CARTESIAN_POINT ( 'NONE',  ( 1.975475456537005874E-15, -76.75000000000000000, 5.000000000000000000 ) ) ;
#35953 = AXIS2_PLACEMENT_3D ( 'NONE', #9252, #14387, #23434 ) ;
#35954 =( BOUNDED_CURVE ( )  B_SPLINE_CURVE ( 2, ( #13067, #21462, #22093, #32687, #60709, #36561, #2480, #36250, #27540 ),
 .UNSPECIFIED., .F., .F. ) 
 B_SPLINE_CURVE_WITH_KNOTS ( ( 3, 2, 2, 2, 3 ),
 ( 0.2017857142857142905, 0.2023809523809523836, 0.2035714285714285698, 0.2047619047619047561, 0.2053571428571428492 ),
 .UNSPECIFIED. ) 
 CURVE ( )  GEOMETRIC_REPRESENTATION_ITEM ( )  RATIONAL_B_SPLINE_CURVE ( ( 0.9330127018922194093, 0.9330127018922194093, 1.000000000000000000, 0.8660254037844387076, 1.000000000000000000, 0.8660254037844387076, 1.000000000000000000, 0.9330127018922194093, 0.9330127018922194093 ) ) 
 REPRESENTATION_ITEM ( '' )  );
#35955 = CARTESIAN_POINT ( 'NONE',  ( 9.457646018065525792E-16, -0.3124999986344051961, 5.148502694627439702 ) ) ;
#35956 = ORIENTED_EDGE ( 'NONE', *, *, #46042, .F. ) ;
#35957 = CARTESIAN_POINT ( 'NONE',  ( -6.972266317189433020E-16, -89.12499999726880162, -5.000000000000000000 ) ) ;
#35958 = CARTESIAN_POINT ( 'NONE',  ( -1.339745962155613812, -60.20534180126147561, -5.000000000000000000 ) ) ;
#35959 = CARTESIAN_POINT ( 'NONE',  ( 2.229367062499998831, -87.64583333196773651, -3.861377020970580887 ) ) ;
#35960 = CARTESIAN_POINT ( 'NONE',  ( -2.499999999999996447, -4.833333333333335702, 4.330127018922195425 ) ) ;
#35961 = CARTESIAN_POINT ( 'NONE',  ( -4.458734124999999437, -84.56249999863439371, 0.000000000000000000 ) ) ;
#35962 = CARTESIAN_POINT ( 'NONE',  ( -4.458734124999999437, 18.35416666803225993, -2.574251347313719407 ) ) ;
#35963 = DIRECTION ( 'NONE',  ( 0.000000000000000000, 0.000000000000000000, 1.000000000000000000 ) ) ;
#35964 = CARTESIAN_POINT ( 'NONE',  ( -50.70258187064364108, -138.1250000013656063, 2.196230717870141014 ) ) ;
#35965 = CARTESIAN_POINT ( 'NONE',  ( -2.229367062500000163, -5.479166665301072214, -3.861377020970580443 ) ) ;
#35966 = CARTESIAN_POINT ( 'NONE',  ( -2.229367062499996610, 23.60416666803225993, 3.861377020970582219 ) ) ;
#35967 = CARTESIAN_POINT ( 'NONE',  ( -4.458734124999999437, -46.56249999863440792, 0.000000000000000000 ) ) ;
#35968 = CARTESIAN_POINT ( 'NONE',  ( 5.000000000000000000, -38.29166666393548013, -2.886751345948130876 ) ) ;
#35969 = CARTESIAN_POINT ( 'NONE',  ( 2.229367062499998831, -86.64583333196773651, -3.861377020970580887 ) ) ;
#35970 = CARTESIAN_POINT ( 'NONE',  ( 9.457646018065525792E-16, -5.062499998634402587, 5.148502694627439702 ) ) ;
#35971 = CARTESIAN_POINT ( 'NONE',  ( -2.500000000000000444, -31.16666666666666785, -4.330127018922193649 ) ) ;
#35972 = VERTEX_POINT ( 'NONE', #25082 ) ;
#35973 = CARTESIAN_POINT ( 'NONE',  ( -2.229367062500000163, -31.72916666530107577, -3.861377020970580443 ) ) ;
#35974 = CARTESIAN_POINT ( 'NONE',  ( -51.60603307380591787, -131.1875000013656063, -2.891590998281053704 ) ) ;
#35975 = CARTESIAN_POINT ( 'NONE',  ( 9.457646018065525792E-16, -74.06249999863440792, 5.148502694627439702 ) ) ;
#35976 = CARTESIAN_POINT ( 'NONE',  ( -4.458734124999999437, 28.43750000136559208, 0.000000000000000000 ) ) ;
#35977 = CARTESIAN_POINT ( 'NONE',  ( 4.458734124999999437, 22.18750000136559564, -5.460374474430324690E-16 ) ) ;
#35978 = CYLINDRICAL_SURFACE ( 'NONE', #12312, 5.000000000000000000 ) ;
#35979 = CARTESIAN_POINT ( 'NONE',  ( 5.000000000000000000, -28.41666666666666430, -2.886751345948130876 ) ) ;
#35980 = CARTESIAN_POINT ( 'NONE',  ( -4.458734124999997661, -79.47916666530106511, 2.574251347313722516 ) ) ;
#35981 = CARTESIAN_POINT ( 'NONE',  ( -3.535250795749689387E-16, -62.25000000000000000, -5.773502691896257311 ) ) ;
#35982 = CARTESIAN_POINT ( 'NONE',  ( -1.339745962155613812, -32.08034179853029855, -5.000000000000000000 ) ) ;
#35983 = CARTESIAN_POINT ( 'NONE',  ( 5.000000000000000888, 22.54166666939784847, 2.886751345948126879 ) ) ;
#35984 = ORIENTED_EDGE ( 'NONE', *, *, #47152, .F. ) ;
#35985 = CARTESIAN_POINT ( 'NONE',  ( -6.972266317189433020E-16, -83.24999999999998579, -5.000000000000000000 ) ) ;
#35986 = DIRECTION ( 'NONE',  ( -0.8660254037844384856, 0.000000000000000000, 0.5000000000000001110 ) ) ;
#35987 = CARTESIAN_POINT ( 'NONE',  ( 2.500000000000002220, -22.66666666666666785, 4.330127018922192761 ) ) ;
#35988 = CARTESIAN_POINT ( 'NONE',  ( 4.458734125000001214, -26.89583333196774007, 2.574251347313718519 ) ) ;
#35989 = CARTESIAN_POINT ( 'NONE',  ( 4.458734124999998549, -87.72916666530107932, -2.574251347313721627 ) ) ;
#35990 = CARTESIAN_POINT ( 'NONE',  ( -5.000000000000000000, -22.87499999726881228, 0.000000000000000000 ) ) ;
#35992 = VERTEX_POINT ( 'NONE', #16073 ) ;
#35991 = CARTESIAN_POINT ( 'NONE',  ( -4.458734124999998549, -54.22916666530107221, 2.574251347313722516 ) ) ;
#35993 = CARTESIAN_POINT ( 'NONE',  ( 1.062108568985190270E-13, -27.25000000000000000, -4.999999999999999112 ) ) ;
#35994 = CARTESIAN_POINT ( 'NONE',  ( 2.500000000000002220, 27.45833333606451632, 4.330127018922192761 ) ) ;
#35996 = VERTEX_POINT ( 'NONE', #54995 ) ;
#35995 = CARTESIAN_POINT ( 'NONE',  ( 2.229367062500001939, -2.229166665301068662, 3.861377020970579999 ) ) ;
#35997 = CARTESIAN_POINT ( 'NONE',  ( 5.000000000000000000, -71.50000000000000000, -6.123233995736766282E-16 ) ) ;
#35998 = CARTESIAN_POINT ( 'NONE',  ( 4.458734124999999437, -152.6875000013656063, 0.000000000000000000 ) ) ;
#35999 = VECTOR ( 'NONE', #1632, 1000.000000000000000 ) ;
#36000 = CARTESIAN_POINT ( 'NONE',  ( 4.458734124999999437, -47.06249999863440792, -5.460374474430324690E-16 ) ) ;
#36001 = CARTESIAN_POINT ( 'NONE',  ( -51.75738570946856498, -155.0000000000000284, 3.805975901505577408 ) ) ;
#36002 = CARTESIAN_POINT ( 'NONE',  ( 5.000000000000000000, -158.0000000000000000, 0.000000000000000000 ) ) ;
#36003 = AXIS2_PLACEMENT_3D ( 'NONE', #20627, #25115, #15150 ) ;
#36004 = CARTESIAN_POINT ( 'NONE',  ( -58.39396692619412477, -124.6875000013656063, 2.891590998281057701 ) ) ;
#36005 = CARTESIAN_POINT ( 'NONE',  ( -4.458734124999999437, -16.56249999863440436, 0.000000000000000000 ) ) ;
#36006 = CARTESIAN_POINT ( 'NONE',  ( 4.458734125000001214, -49.14583333196772941, 2.574251347313718519 ) ) ;
#36007 = CARTESIAN_POINT ( 'NONE',  ( 0.000000000000000000, -120.0000000000000000, 0.000000000000000000 ) ) ;
#36008 = CARTESIAN_POINT ( 'NONE',  ( 4.458734125000000326, -143.3750000013656063, -1.846868145590734978 ) ) ;
#36009 = CARTESIAN_POINT ( 'NONE',  ( -3.152548672688508926E-16, -94.81249999863442213, -5.148502694627439702 ) ) ;
#36010 = CARTESIAN_POINT ( 'NONE',  ( -5.000000000000000000, -106.9999999999999858, 0.000000000000000000 ) ) ;
#36011 = ORIENTED_EDGE ( 'NONE', *, *, #56752, .F. ) ;
#36012 = CARTESIAN_POINT ( 'NONE',  ( -53.51423613279429503, -152.5000000013655779, 4.591703134518083651 ) ) ;
#36013 = CARTESIAN_POINT ( 'NONE',  ( -2.229367062500000163, 27.27083333469892779, -3.861377020970580443 ) ) ;
#36014 = CARTESIAN_POINT ( 'NONE',  ( -52.53715891517739323, -148.5625000027312126, -4.819101127000233298 ) ) ;
#36015 = DIRECTION ( 'NONE',  ( -0.000000000000000000, 1.000000000000000000, -0.000000000000000000 ) ) ;
#36016 = VERTEX_POINT ( 'NONE', #10922 ) ;
#36017 = CARTESIAN_POINT ( 'NONE',  ( 4.458734124999998549, 0.2708333346989263979, -2.574251347313721627 ) ) ;
#36018 = CARTESIAN_POINT ( 'NONE',  ( 5.000000000000000000, -106.4166666666666572, -2.886751345948130876 ) ) ;
#36019 = CARTESIAN_POINT ( 'NONE',  ( -4.458734124999999437, -23.64583333196773651, -2.574251347313719407 ) ) ;
#36020 = CARTESIAN_POINT ( 'NONE',  ( 5.000000000000000000, -70.50000000000000000, -6.123233995736766282E-16 ) ) ;
#36021 = CARTESIAN_POINT ( 'NONE',  ( 4.458734124999998549, -7.729166665301073103, -2.574251347313721627 ) ) ;
#36022 = CARTESIAN_POINT ( 'NONE',  ( 1.339745962155615144, 6.419658201469706782, 4.999999999999999112 ) ) ;
#36023 = CARTESIAN_POINT ( 'NONE',  ( -1.846868145590737420, -144.7500000013655779, 4.458734124999997661 ) ) ;
#36024 = CARTESIAN_POINT ( 'NONE',  ( -2.229367062500000163, 16.27083333469892779, -3.861377020970580443 ) ) ;
#36025 = ORIENTED_EDGE ( 'NONE', *, *, #15318, .T. ) ;
#36026 = CARTESIAN_POINT ( 'NONE',  ( -6.972266317189433020E-16, -14.12499999726881228, -5.000000000000000000 ) ) ;
#36027 = CARTESIAN_POINT ( 'NONE',  ( 3.061616997868383141E-16, -168.8750000027312126, -5.000000000000000000 ) ) ;
#36029 = CARTESIAN_POINT ( 'NONE',  ( -4.458734124999999437, -20.39583333196774362, -2.574251347313719407 ) ) ;
#36028 = CARTESIAN_POINT ( 'NONE',  ( 2.500000000000002220, -82.66666666666667140, 4.330127018922192761 ) ) ;
#36030 = CARTESIAN_POINT ( 'NONE',  ( 2.500000000000002220, -25.54166666393547658, 4.330127018922192761 ) ) ;
#36031 = LINE ( 'NONE', #25419, #29356 ) ;
#36032 =( BOUNDED_CURVE ( )  B_SPLINE_CURVE ( 2, ( #30769, #17247, #45243, #20808, #40411, #55861, #60050, #11774, #26584 ),
 .UNSPECIFIED., .F., .F. ) 
 B_SPLINE_CURVE_WITH_KNOTS ( ( 3, 2, 2, 2, 3 ),
 ( 0.6089285714285714857, 0.6095238095238095788, 0.6107142857142857650, 0.6119047619047619513, 0.6125000000000000444 ),
 .UNSPECIFIED. ) 
 CURVE ( )  GEOMETRIC_REPRESENTATION_ITEM ( )  RATIONAL_B_SPLINE_CURVE ( ( 0.9330127018922194093, 0.9330127018922256266, 1.000000000000000000, 0.8660254037844387076, 1.000000000000000000, 0.8660254037844387076, 1.000000000000000000, 0.9330127018922194093, 0.9330127018922194093 ) ) 
 REPRESENTATION_ITEM ( '' )  );
#36033 = CARTESIAN_POINT ( 'NONE',  ( -53.51423613279429503, -150.2500000013656063, 4.591703134518082763 ) ) ;
#36034 = CARTESIAN_POINT ( 'NONE',  ( -5.000000000000000000, -44.87499999726880873, 0.000000000000000000 ) ) ;
#36035 = CARTESIAN_POINT ( 'NONE',  ( 5.000000000000000000, -150.1875000027312126, 2.071067811865478614 ) ) ;
#36036 = CARTESIAN_POINT ( 'NONE',  ( -2.229367062499996610, 10.85416666803225993, 3.861377020970582219 ) ) ;
#36037 = DIRECTION ( 'NONE',  ( 0.000000000000000000, 0.000000000000000000, -1.000000000000000000 ) ) ;
#36038 = CARTESIAN_POINT ( 'NONE',  ( 1.339745962155612702, 9.705341801261479162, -5.000000000000000000 ) ) ;
#36039 = CARTESIAN_POINT ( 'NONE',  ( 2.229367062499998831, 13.35416666803226171, -3.861377020970580887 ) ) ;
#36040 = CARTESIAN_POINT ( 'NONE',  ( -4.458734124999999437, -65.31249999863440792, 0.000000000000000000 ) ) ;
#36041 = AXIS2_PLACEMENT_3D ( 'NONE', #34277, #38475, #19807 ) ;
#36042 = CARTESIAN_POINT ( 'NONE',  ( 4.458734124999998549, -15.97916666530107221, -2.574251347313721627 ) ) ;
#36043 = CARTESIAN_POINT ( 'NONE',  ( -2.499999999999996447, 1.166666666666666519, 4.330127018922195425 ) ) ;
#36044 = CARTESIAN_POINT ( 'NONE',  ( 1.846868145590736310, -162.6250000013655779, 4.458734124999999437 ) ) ;
#36045 = FACE_OUTER_BOUND ( 'NONE', #26047, .T. ) ;
#36046 = VECTOR ( 'NONE', #20875, 1000.000000000000000 ) ;
#36047 = CARTESIAN_POINT ( 'NONE',  ( 2.229367062500001939, -60.97916666530106511, 3.861377020970579999 ) ) ;
#36048 = CARTESIAN_POINT ( 'NONE',  ( 2.499999999999998668, -95.20833333060213022, -4.330127018922193649 ) ) ;
#36049 =( BOUNDED_CURVE ( )  B_SPLINE_CURVE ( 2, ( #27481, #12053, #7878, #2422, #32307, #22034, #41005, #21722, #57088 ),
 .UNSPECIFIED., .F., .F. ) 
 B_SPLINE_CURVE_WITH_KNOTS ( ( 3, 2, 2, 2, 3 ),
 ( 0.9410714285714285587, 0.9416666666666666519, 0.9428571428571428381, 0.9440476190476190244, 0.9446428571428571175 ),
 .UNSPECIFIED. ) 
 CURVE ( )  GEOMETRIC_REPRESENTATION_ITEM ( )  RATIONAL_B_SPLINE_CURVE ( ( 0.9330127018922194093, 0.9330127018922194093, 1.000000000000000000, 0.8660254037844387076, 1.000000000000000000, 0.8660254037844387076, 1.000000000000000000, 0.9330127018922194093, 0.9330127018922194093 ) ) 
 REPRESENTATION_ITEM ( '' )  );
#36050 = CARTESIAN_POINT ( 'NONE',  ( -1.339745962155613812, -70.20534180126148271, -5.000000000000000000 ) ) ;
#36051 = CARTESIAN_POINT ( 'NONE',  ( -1.339745962155613812, -89.08034179853027013, -5.000000000000000000 ) ) ;
#36052 = CARTESIAN_POINT ( 'NONE',  ( 2.229367062499998831, -37.64583333196773651, -3.861377020970580887 ) ) ;
#36053 = DIRECTION ( 'NONE',  ( -0.000000000000000000, 1.000000000000000000, -0.000000000000000000 ) ) ;
#36054 = CARTESIAN_POINT ( 'NONE',  ( 1.060575238724906964E-15, -44.74999999999999289, 5.773502691896257311 ) ) ;
#36055 = CARTESIAN_POINT ( 'NONE',  ( 7.549006887134058985, -4.358421158401196926, -7.700127545397296380 ) ) ;
#36056 = CARTESIAN_POINT ( 'NONE',  ( 5.000000000000000000, -17.29166666393548368, -2.886751345948130876 ) ) ;
#36057 = ORIENTED_EDGE ( 'NONE', *, *, #26206, .T. ) ;
#36058 = CARTESIAN_POINT ( 'NONE',  ( -4.458734124999998549, -105.2291666653010651, 2.574251347313722516 ) ) ;
#36059 = CARTESIAN_POINT ( 'NONE',  ( -4.458734124999999437, -2.562499998634407028, 0.000000000000000000 ) ) ;
#36060 = CARTESIAN_POINT ( 'NONE',  ( 2.499999999999998668, -73.20833333060214443, -4.330127018922193649 ) ) ;
#36061 = CARTESIAN_POINT ( 'NONE',  ( -5.000000000000000000, -9.000000000000001776, 0.000000000000000000 ) ) ;
#36062 = CARTESIAN_POINT ( 'NONE',  ( -2.229367062500000163, -72.47916666530107932, -3.861377020970580443 ) ) ;
#36063 = CARTESIAN_POINT ( 'NONE',  ( -5.000000000000000000, -17.08333333333333215, -2.886751345948128211 ) ) ;
#36064 = CARTESIAN_POINT ( 'NONE',  ( 1.060575238724906964E-15, -6.624999997268813168, 5.773502691896257311 ) ) ;
#36066 = ORIENTED_EDGE ( 'NONE', *, *, #47312, .F. ) ;
#36065 = CARTESIAN_POINT ( 'NONE',  ( -4.458734124999999437, -39.31249999863440081, 0.000000000000000000 ) ) ;
#36067 = DIRECTION ( 'NONE',  ( 0.000000000000000000, 0.000000000000000000, 1.000000000000000000 ) ) ;
#36069 = VERTEX_POINT ( 'NONE', #30539 ) ;
#36068 = CARTESIAN_POINT ( 'NONE',  ( 4.458734124999998549, 13.02083333469892779, -2.574251347313721627 ) ) ;
#36070 = CARTESIAN_POINT ( 'NONE',  ( 1.975475456537005874E-15, -101.6249999972688158, 5.000000000000000000 ) ) ;
#36071 = CARTESIAN_POINT ( 'NONE',  ( -2.499999999999996447, -55.83333333333332860, 4.330127018922195425 ) ) ;
#36072 = CARTESIAN_POINT ( 'NONE',  ( 9.457646018065525792E-16, -29.31249999863440436, 5.148502694627439702 ) ) ;
#36073 = CARTESIAN_POINT ( 'NONE',  ( -6.972266317189433020E-16, -4.249999999999997335, -5.000000000000000000 ) ) ;
#36074 = CARTESIAN_POINT ( 'NONE',  ( 2.229367062500001939, -76.97916666530106511, 3.861377020970579999 ) ) ;
#36075 = CARTESIAN_POINT ( 'NONE',  ( 1.846868145590736310, -140.8750000013656063, 4.458734124999999437 ) ) ;
#36076 = CARTESIAN_POINT ( 'NONE',  ( -3.152548672688508926E-16, -88.56249999863439371, -5.148502694627439702 ) ) ;
#36077 = CARTESIAN_POINT ( 'NONE',  ( -59.29741812935640155, -134.8750000013656063, -2.196230717870135685 ) ) ;
#36078 = CARTESIAN_POINT ( 'NONE',  ( 4.458734124999999437, -38.06249999863440792, -5.460374474430324690E-16 ) ) ;
#36079 = CARTESIAN_POINT ( 'NONE',  ( -6.972266317189433020E-16, -94.12499999726880162, -5.000000000000000000 ) ) ;
#36080 = ORIENTED_EDGE ( 'NONE', *, *, #54346, .T. ) ;
#36081 = CARTESIAN_POINT ( 'NONE',  ( -2.229367062499996610, -80.39583333196773651, 3.861377020970582219 ) ) ;
#36082 = CARTESIAN_POINT ( 'NONE',  ( -53.50367810914265476, -135.0000000000000000, -4.210172938645351692 ) ) ;
#36083 = ORIENTED_EDGE ( 'NONE', *, *, #6265, .T. ) ;
#36084 = CARTESIAN_POINT ( 'NONE',  ( -6.972266317189433020E-16, -15.12499999726881050, -5.000000000000000000 ) ) ;
#36086 = AXIS2_PLACEMENT_3D ( 'NONE', #31873, #18023, #12259 ) ;
#36085 = DIRECTION ( 'NONE',  ( 0.000000000000000000, 0.000000000000000000, 1.000000000000000000 ) ) ;
#36088 = ADVANCED_FACE ( 'NONE', ( #39863 ), #25730, .T. ) ;
#36087 = CARTESIAN_POINT ( 'NONE',  ( -3.152548672688508926E-16, -62.81249999863440792, -5.148502694627439702 ) ) ;
#36089 = CARTESIAN_POINT ( 'NONE',  ( 9.457646018065525792E-16, -10.31249999863440614, 5.148502694627439702 ) ) ;
#36090 = ORIENTED_EDGE ( 'NONE', *, *, #63608, .T. ) ;
#36091 = CYLINDRICAL_SURFACE ( 'NONE', #8143, 5.000000000000000000 ) ;
#36092 = CARTESIAN_POINT ( 'NONE',  ( 1.975475456537005874E-15, -92.62499999726881583, 5.000000000000000000 ) ) ;
#36093 = ORIENTED_EDGE ( 'NONE', *, *, #26359, .T. ) ;
#36094 = CARTESIAN_POINT ( 'NONE',  ( 4.458734125000001214, -6.145833331967741842, 2.574251347313718519 ) ) ;
#36095 = CARTESIAN_POINT ( 'NONE',  ( -2.229367062500000163, 8.520833334698926009, -3.861377020970580443 ) ) ;
#36096 = CARTESIAN_POINT ( 'NONE',  ( -6.972266317189433020E-16, -33.12499999726880873, -5.000000000000000000 ) ) ;
#36097 = CARTESIAN_POINT ( 'NONE',  ( -1.846868145590737420, -162.7500000013655779, 4.458734124999997661 ) ) ;
#36098 =( BOUNDED_CURVE ( )  B_SPLINE_CURVE ( 2, ( #7968, #62313, #27258, #23392, #46569, #52961, #42674, #7654, #18238 ),
 .UNSPECIFIED., .F., .F. ) 
 B_SPLINE_CURVE_WITH_KNOTS ( ( 3, 2, 2, 2, 3 ),
 ( 0.1020833333333333315, 0.1027777777777777735, 0.1041666666666666713, 0.1055555555555555552, 0.1062499999999999972 ),
 .UNSPECIFIED. ) 
 CURVE ( )  GEOMETRIC_REPRESENTATION_ITEM ( )  RATIONAL_B_SPLINE_CURVE ( ( 0.9330127018922194093, 0.9330127018922194093, 1.000000000000000000, 0.8660254037844387076, 1.000000000000000000, 0.8660254037844387076, 1.000000000000000000, 0.9330127018922194093, 0.9330127018922194093 ) ) 
 REPRESENTATION_ITEM ( '' )  );
#36099 = CYLINDRICAL_SURFACE ( 'NONE', #47109, 5.000000000000000000 ) ;
#36100 = ORIENTED_EDGE ( 'NONE', *, *, #56294, .F. ) ;
#36101 = CARTESIAN_POINT ( 'NONE',  ( -3.152548672688508926E-16, -87.56249999863440792, -5.148502694627439702 ) ) ;
#36102 = CARTESIAN_POINT ( 'NONE',  ( 5.000000000000000888, -29.45833333060214443, 2.886751345948126879 ) ) ;
#36103 = CARTESIAN_POINT ( 'NONE',  ( -4.458734124999998549, -4.229166665301070438, 2.574251347313722516 ) ) ;
#36104 = CARTESIAN_POINT ( 'NONE',  ( 0.000000000000000000, -170.0000000000000000, 0.000000000000000000 ) ) ;
#36105 = ADVANCED_FACE ( 'NONE', ( #17345 ), #51132, .T. ) ;
#36106 = CARTESIAN_POINT ( 'NONE',  ( 2.499999999999998668, -29.20833333060214798, -4.330127018922193649 ) ) ;
#36107 = ADVANCED_FACE ( 'NONE', ( #7705 ), #26046, .T. ) ;
#36108 = DIRECTION ( 'NONE',  ( -0.000000000000000000, 1.000000000000000000, -0.000000000000000000 ) ) ;
#36109 = CARTESIAN_POINT ( 'NONE',  ( 2.229367062500001939, 22.02083333469892779, 3.861377020970579999 ) ) ;
#36110 = CARTESIAN_POINT ( 'NONE',  ( -2.499999999999996447, -82.70833333060214443, 4.330127018922195425 ) ) ;
#36111 = CARTESIAN_POINT ( 'NONE',  ( 2.229367062499998831, 26.35416666803225993, -3.861377020970580887 ) ) ;
#36112 = CARTESIAN_POINT ( 'NONE',  ( -3.152548672688508926E-16, -50.56249999863440792, -5.148502694627439702 ) ) ;
#36113 = CARTESIAN_POINT ( 'NONE',  ( -2.229367062499996610, -35.39583333196772941, 3.861377020970582219 ) ) ;
#36114 = CARTESIAN_POINT ( 'NONE',  ( 2.229367062499998831, 3.104166668032259935, -3.861377020970580887 ) ) ;
#36115 = CARTESIAN_POINT ( 'NONE',  ( -4.764381983412779477E-15, 25.37500000273118062, 5.000000000000000000 ) ) ;
#36116 = CARTESIAN_POINT ( 'NONE',  ( -5.000000000000000000, 13.91666666666666785, -2.886751345948128211 ) ) ;
#36117 = CARTESIAN_POINT ( 'NONE',  ( 5.000000000000000000, -145.1875000027312126, 2.071067811865478614 ) ) ;
#36118 = CARTESIAN_POINT ( 'NONE',  ( 1.975475456537005874E-15, 18.37500000273118062, 5.000000000000000000 ) ) ;
#36119 = CARTESIAN_POINT ( 'NONE',  ( -3.152548672688508926E-16, -44.56249999863440081, -5.148502694627439702 ) ) ;
#36120 = CARTESIAN_POINT ( 'NONE',  ( 5.000000000000000000, -78.29166666393547303, -2.886751345948129988 ) ) ;
#36121 = EDGE_CURVE ( 'NONE', #12871, #8173, #29247, .T. ) ;
#36122 = CARTESIAN_POINT ( 'NONE',  ( -52.10840900171896806, -140.4375000013656063, 3.393966926194110556 ) ) ;
#36123 = CARTESIAN_POINT ( 'NONE',  ( 1.339745962155612702, -24.16965819600733312, -5.000000000000000000 ) ) ;
#36124 = CARTESIAN_POINT ( 'NONE',  ( 1.975475456537005874E-15, -22.74999999999999645, 5.000000000000000000 ) ) ;
#36125 = CARTESIAN_POINT ( 'NONE',  ( 2.229367062499998831, -84.89583333196773651, -3.861377020970580887 ) ) ;
#36126 = CARTESIAN_POINT ( 'NONE',  ( -1.846868145590734756, -163.3750000013656347, -4.458734124999999437 ) ) ;
#36127 = CARTESIAN_POINT ( 'NONE',  ( -1.013163106016700565, -8.075304045852661261, -7.231838333420565590 ) ) ;
#36128 = CARTESIAN_POINT ( 'NONE',  ( 5.000000000000000000, -29.41666666666666785, -2.886751345948129988 ) ) ;
#36129 = CARTESIAN_POINT ( 'NONE',  ( 3.152801135295367541, -140.3125000013655779, -3.152801135295367541 ) ) ;
#36130 = VERTEX_POINT ( 'NONE', #6437 ) ;
#36131 = CARTESIAN_POINT ( 'NONE',  ( 4.458734124999999437, 24.93750000136559208, -5.460374474430324690E-16 ) ) ;
#36132 = ORIENTED_EDGE ( 'NONE', *, *, #40432, .T. ) ;
#36133 = CARTESIAN_POINT ( 'NONE',  ( -4.458734124999998549, -89.22916666530106511, 2.574251347313722516 ) ) ;
#36134 = CARTESIAN_POINT ( 'NONE',  ( -3.152548672688508926E-16, 14.18750000136559386, -5.148502694627439702 ) ) ;
#36135 =( BOUNDED_CURVE ( )  B_SPLINE_CURVE ( 2, ( #50295, #59965, #6878, #1433, #60602, #20395, #31300, #30347, #39994 ),
 .UNSPECIFIED., .F., .F. ) 
 B_SPLINE_CURVE_WITH_KNOTS ( ( 3, 2, 2, 2, 3 ),
 ( 0.1312500000000000056, 0.1319444444444444475, 0.1333333333333333315, 0.1347222222222222154, 0.1354166666666666574 ),
 .UNSPECIFIED. ) 
 CURVE ( )  GEOMETRIC_REPRESENTATION_ITEM ( )  RATIONAL_B_SPLINE_CURVE ( ( 0.9330127018922194093, 0.9330127018922194093, 1.000000000000000000, 0.8660254037844387076, 1.000000000000000000, 0.8660254037844387076, 1.000000000000000000, 0.9330127018922194093, 0.9330127018922194093 ) ) 
 REPRESENTATION_ITEM ( '' )  );
#36136 = CARTESIAN_POINT ( 'NONE',  ( -2.499999999999996447, 17.29166666939785557, 4.330127018922195425 ) ) ;
#36137 = FACE_OUTER_BOUND ( 'NONE', #41359, .T. ) ;
#36138 = CARTESIAN_POINT ( 'NONE',  ( -2.500000000000000444, 6.833333333333333925, -4.330127018922193649 ) ) ;
#36139 = CARTESIAN_POINT ( 'NONE',  ( 2.229367062499998831, -57.64583333196773651, -3.861377020970580887 ) ) ;
#36140 = CARTESIAN_POINT ( 'NONE',  ( -3.152548672688508926E-16, -13.56249999863440259, -5.148502694627439702 ) ) ;
#36141 = CARTESIAN_POINT ( 'NONE',  ( 2.499999999999998668, -61.20833333060214443, -4.330127018922193649 ) ) ;
#36142 = EDGE_CURVE ( 'NONE', #49141, #44569, #24375, .T. ) ;
#36143 = CARTESIAN_POINT ( 'NONE',  ( -57.19623071787016499, -136.6250000013656063, 4.297418129356382899 ) ) ;
#36144 = CARTESIAN_POINT ( 'NONE',  ( -5.000000000000000000, -63.95833333060213732, -2.886751345948128211 ) ) ;
#36145 = CARTESIAN_POINT ( 'NONE',  ( 1.975475456537005874E-15, -1.749999999999999334, 5.000000000000000000 ) ) ;
#36146 = LINE ( 'NONE', #6557, #26868 ) ;
#36147 = CARTESIAN_POINT ( 'NONE',  ( -4.999999999999999112, -36.91666666666667140, 2.886751345948131764 ) ) ;
#36148 = CARTESIAN_POINT ( 'NONE',  ( 5.000000000000000000, -96.41666666666667140, -2.886751345948130876 ) ) ;
#36150 = CARTESIAN_POINT ( 'NONE',  ( 2.229367062499998831, -12.89583333196774007, -3.861377020970580887 ) ) ;
#36149 = CARTESIAN_POINT ( 'NONE',  ( -2.499999999999996447, 15.16666666666666607, 4.330127018922195425 ) ) ;
#36151 = CARTESIAN_POINT ( 'NONE',  ( 0.000000000000000000, -120.0000000000000000, 5.000000000000000000 ) ) ;
#36152 = CARTESIAN_POINT ( 'NONE',  ( 9.457646018065525792E-16, -62.06249999863440792, 5.148502694627439702 ) ) ;
#36153 =( BOUNDED_CURVE ( )  B_SPLINE_CURVE ( 2, ( #54214, #30403, #24952, #514, #5982, #25589, #20769, #35561, #1169 ),
 .UNSPECIFIED., .F., .F. ) 
 B_SPLINE_CURVE_WITH_KNOTS ( ( 3, 2, 2, 2, 3 ),
 ( 0.8062500000000000222, 0.8069444444444444642, 0.8083333333333333481, 0.8097222222222222321, 0.8104166666666666741 ),
 .UNSPECIFIED. ) 
 CURVE ( )  GEOMETRIC_REPRESENTATION_ITEM ( )  RATIONAL_B_SPLINE_CURVE ( ( 0.9330127018922194093, 0.9330127018922194093, 1.000000000000000000, 0.8660254037844387076, 1.000000000000000000, 0.8660254037844387076, 1.000000000000000000, 0.9330127018922194093, 0.9330127018922194093 ) ) 
 REPRESENTATION_ITEM ( '' )  );
#36154 = CARTESIAN_POINT ( 'NONE',  ( -1.846868145590737420, -154.0000000013655779, 4.458734124999999437 ) ) ;
#36155 = CARTESIAN_POINT ( 'NONE',  ( 4.458734125000001214, -72.89583333196775072, 2.574251347313718519 ) ) ;
#36156 = CARTESIAN_POINT ( 'NONE',  ( -57.19623071787017210, -146.6250000013656063, 4.297418129356382899 ) ) ;
#36157 = CARTESIAN_POINT ( 'NONE',  ( -4.458734124999999437, -21.64583333196774362, -2.574251347313719407 ) ) ;
#36158 = CARTESIAN_POINT ( 'NONE',  ( 1.060575238724906964E-15, -58.62499999726880873, 5.773502691896257311 ) ) ;
#36159 = ORIENTED_EDGE ( 'NONE', *, *, #59338, .F. ) ;
#36160 = CARTESIAN_POINT ( 'NONE',  ( 1.975475456537005874E-15, -85.62499999726880162, 5.000000000000000000 ) ) ;
#36161 = ORIENTED_EDGE ( 'NONE', *, *, #62538, .T. ) ;
#36163 = DIRECTION ( 'NONE',  ( -0.000000000000000000, 1.000000000000000000, -0.000000000000000000 ) ) ;
#36162 = CARTESIAN_POINT ( 'NONE',  ( -2.500000000000000444, -28.16666666666666785, -4.330127018922193649 ) ) ;
#36164 = CARTESIAN_POINT ( 'NONE',  ( 4.458734124999999437, -152.4375000013655779, 0.000000000000000000 ) ) ;
#36165 = ORIENTED_EDGE ( 'NONE', *, *, #53981, .T. ) ;
#36166 = CARTESIAN_POINT ( 'NONE',  ( 1.975475456537005874E-15, -54.74999999999999289, 5.000000000000000000 ) ) ;
#36167 = CARTESIAN_POINT ( 'NONE',  ( -53.33387254593733928, -128.8125000000000568, 5.149110718188519620 ) ) ;
#36168 = DIRECTION ( 'NONE',  ( 0.000000000000000000, 0.000000000000000000, 1.000000000000000000 ) ) ;
#36170 = EDGE_CURVE ( 'NONE', #5308, #32593, #11871, .T. ) ;
#36169 = CARTESIAN_POINT ( 'NONE',  ( 2.229367062500001939, -46.22916666530106511, 3.861377020970579999 ) ) ;
#36171 = ORIENTED_EDGE ( 'NONE', *, *, #11000, .F. ) ;
#36172 = EDGE_CURVE ( 'NONE', #53443, #52361, #20641, .T. ) ;
#36173 = CARTESIAN_POINT ( 'NONE',  ( 1.339745962155612702, 11.70534180126147916, -5.000000000000000000 ) ) ;
#36174 = CARTESIAN_POINT ( 'NONE',  ( 4.458734125000001214, 14.10416666803225993, 2.574251347313718519 ) ) ;
#36175 = CARTESIAN_POINT ( 'NONE',  ( -4.458734124999999437, 24.60416666803225993, -2.574251347313719407 ) ) ;
#36176 = CARTESIAN_POINT ( 'NONE',  ( -50.55543936806279248, -148.0625000013656063, 0.3552334253322060320 ) ) ;
#36177 = CARTESIAN_POINT ( 'NONE',  ( 2.500000000000002220, -108.5416666639354730, 4.330127018922192761 ) ) ;
#36178 = CARTESIAN_POINT ( 'NONE',  ( 5.000000000000000000, -61.37499999726880873, -6.123233995736766282E-16 ) ) ;
#36179 = ORIENTED_EDGE ( 'NONE', *, *, #7957, .T. ) ;
#36180 = CARTESIAN_POINT ( 'NONE',  ( 4.458734125000000326, -70.89583333196773651, 2.574251347313718519 ) ) ;
#36181 = DIRECTION ( 'NONE',  ( -0.000000000000000000, 1.000000000000000000, -0.000000000000000000 ) ) ;
#36182 = CARTESIAN_POINT ( 'NONE',  ( -2.229367062500000163, 10.52083333469892779, -3.861377020970580443 ) ) ;
#36183 = CARTESIAN_POINT ( 'NONE',  ( 2.493747252781420335E-13, -78.12499999726881583, -5.000000000000000000 ) ) ;
#36184 = CARTESIAN_POINT ( 'NONE',  ( -5.000000000000000000, -157.5000000000000000, -6.123233995736766282E-16 ) ) ;
#36185 = CARTESIAN_POINT ( 'NONE',  ( -3.152548672688508926E-16, -56.81249999863439371, -5.148502694627439702 ) ) ;
#36186 = CARTESIAN_POINT ( 'NONE',  ( -5.000000000000000000, -12.95833333060214976, -2.886751345948128211 ) ) ;
#36187 = ADVANCED_FACE ( 'NONE', ( #1618 ), #16396, .T. ) ;
#36188 = LINE ( 'NONE', #39715, #25491 ) ;
#36189 = DIRECTION ( 'NONE',  ( -0.000000000000000000, 1.000000000000000000, -0.000000000000000000 ) ) ;
#36190 = CARTESIAN_POINT ( 'NONE',  ( -4.458734124999997661, -20.47916666530107577, 2.574251347313722516 ) ) ;
#36191 = ORIENTED_EDGE ( 'NONE', *, *, #9529, .T. ) ;
#36192 = CARTESIAN_POINT ( 'NONE',  ( -4.999999999999998224, -60.91666666666666430, 2.886751345948131764 ) ) ;
#36193 = CARTESIAN_POINT ( 'NONE',  ( -2.229367062499996610, -105.1458333319677365, 3.861377020970582219 ) ) ;
#36194 = CARTESIAN_POINT ( 'NONE',  ( -3.535533905932737309, -157.7500000027312126, -3.535533905932738197 ) ) ;
#36195 = ORIENTED_EDGE ( 'NONE', *, *, #2418, .F. ) ;
#36196 = CARTESIAN_POINT ( 'NONE',  ( 2.229367062499998831, -104.8958333319677365, -3.861377020970580887 ) ) ;
#36197 = CARTESIAN_POINT ( 'NONE',  ( -2.229367062499996610, -26.14583333196773651, 3.861377020970582219 ) ) ;
#36198 = CARTESIAN_POINT ( 'NONE',  ( -2.499999999999996447, -64.70833333060213022, 4.330127018922195425 ) ) ;
#36199 = CARTESIAN_POINT ( 'NONE',  ( -59.59170313451811296, -152.7500000013655779, 1.485763867205729394 ) ) ;
#36200 = CARTESIAN_POINT ( 'NONE',  ( -50.55543936806279248, -144.0625000013656063, 0.3552334253322060320 ) ) ;
#36201 = CARTESIAN_POINT ( 'NONE',  ( 2.229367062499998831, -22.64583333196773651, -3.861377020970580887 ) ) ;
#36202 = CARTESIAN_POINT ( 'NONE',  ( -4.458734124999999437, -66.56249999863440792, 0.000000000000000000 ) ) ;
#36203 = CARTESIAN_POINT ( 'NONE',  ( -52.53715891517739323, -153.5625000027312126, -4.819101127000233298 ) ) ;
#36204 = CARTESIAN_POINT ( 'NONE',  ( -4.458734124999997661, -24.22916666530107577, 2.574251347313722516 ) ) ;
#36205 = CARTESIAN_POINT ( 'NONE',  ( -6.972266317189433020E-16, -33.24999999999999289, -5.000000000000000000 ) ) ;
#36206 = CARTESIAN_POINT ( 'NONE',  ( 3.061616997868383141E-16, -150.7500000000000284, -5.000000000000000000 ) ) ;
#36207 = CARTESIAN_POINT ( 'NONE',  ( -4.999999999999999112, -11.91666666666666607, 2.886751345948131764 ) ) ;
#36208 = CARTESIAN_POINT ( 'NONE',  ( 3.152801135295366208, -151.5625000013655779, 3.152801135295367985 ) ) ;
#36209 = ORIENTED_EDGE ( 'NONE', *, *, #11470, .T. ) ;
#36210 = CARTESIAN_POINT ( 'NONE',  ( -2.229367062500000163, -51.72916666530107221, -3.861377020970580443 ) ) ;
#36211 = CARTESIAN_POINT ( 'NONE',  ( 5.000000000000000000, -92.41666666666665719, -2.886751345948130876 ) ) ;
#36212 = CARTESIAN_POINT ( 'NONE',  ( 5.000000000000000000, 29.58333333333332860, -2.886751345948129988 ) ) ;
#36213 = CARTESIAN_POINT ( 'NONE',  ( 1.339745962155612702, -76.16965819600731891, -5.000000000000000000 ) ) ;
#36214 = CARTESIAN_POINT ( 'NONE',  ( -4.458734124999998549, 4.770833334698926009, 2.574251347313722516 ) ) ;
#36215 = CARTESIAN_POINT ( 'NONE',  ( 1.975475456537005874E-15, -73.62499999726878741, 5.000000000000000000 ) ) ;
#36216 = DIRECTION ( 'NONE',  ( -0.000000000000000000, 1.000000000000000000, -0.000000000000000000 ) ) ;
#36217 = CARTESIAN_POINT ( 'NONE',  ( 5.000000000000000888, -17.58333333333333215, 2.886751345948126879 ) ) ;
#36218 = CARTESIAN_POINT ( 'NONE',  ( 4.458734125000001214, 12.85416666803226171, 2.574251347313718519 ) ) ;
#36219 = CARTESIAN_POINT ( 'NONE',  ( -5.000000000000000000, 1.125000002731184390, 0.000000000000000000 ) ) ;
#36220 = ORIENTED_EDGE ( 'NONE', *, *, #27521, .F. ) ;
#36221 = CARTESIAN_POINT ( 'NONE',  ( 1.975475456537005874E-15, -80.62499999726881583, 5.000000000000000000 ) ) ;
#36222 = EDGE_LOOP ( 'NONE', ( #55552, #2468, #27291, #24458 ) ) ;
#36223 = CARTESIAN_POINT ( 'NONE',  ( -2.500000000000000444, -54.04166666393548013, -4.330127018922193649 ) ) ;
#36224 = CARTESIAN_POINT ( 'NONE',  ( -4.458734124999998549, -46.22916666530106511, 2.574251347313722516 ) ) ;
#36225 = CARTESIAN_POINT ( 'NONE',  ( -1.846868145590737420, -163.0000000013655779, 4.458734124999999437 ) ) ;
#36226 =( BOUNDED_CURVE ( )  B_SPLINE_CURVE ( 2, ( #20739, #34890, #21055, #55476, #29725, #35211, #54829, #30049, #15908 ),
 .UNSPECIFIED., .F., .F. ) 
 B_SPLINE_CURVE_WITH_KNOTS ( ( 3, 2, 2, 2, 3 ),
 ( 0.5583333333333337922, 0.5625000000000004441, 0.5666666666666670960, 0.5708333333333338588, 0.5750000000000005107 ),
 .UNSPECIFIED. ) 
 CURVE ( )  GEOMETRIC_REPRESENTATION_ITEM ( )  RATIONAL_B_SPLINE_CURVE ( ( 0.9999999999999918954, 0.9238795325112948431, 1.000000000000000000, 0.9238795325112867385, 1.000000000000000000, 0.9238795325112867385, 1.000000000000000000, 0.9238795325112766355, 1.000000000000010214 ) ) 
 REPRESENTATION_ITEM ( '' )  );
#36227 = CARTESIAN_POINT ( 'NONE',  ( 5.000000000000000000, -42.37499999726880873, -6.123233995736766282E-16 ) ) ;
#36228 = ORIENTED_EDGE ( 'NONE', *, *, #14083, .F. ) ;
#36229 = CARTESIAN_POINT ( 'NONE',  ( 2.229367062499998831, -18.64583333196774007, -3.861377020970580887 ) ) ;
#36230 = ORIENTED_EDGE ( 'NONE', *, *, #31180, .T. ) ;
#36231 = CARTESIAN_POINT ( 'NONE',  ( 2.499999999999998668, -85.33333333333332860, -4.330127018922193649 ) ) ;
#36232 = CARTESIAN_POINT ( 'NONE',  ( 1.846868145590735200, -166.2500000013656347, -4.458734125000000326 ) ) ;
#36234 = ORIENTED_EDGE ( 'NONE', *, *, #32677, .T. ) ;
#36233 = CARTESIAN_POINT ( 'NONE',  ( -1.339745962155610925, -60.66965819600733312, 5.000000000000000000 ) ) ;
#36235 = CARTESIAN_POINT ( 'NONE',  ( -58.80597590150559739, -141.0000000000000000, 3.242614290531460330 ) ) ;
#36236 = CARTESIAN_POINT ( 'NONE',  ( -2.229367062500000163, -32.72916666530106511, -3.861377020970580443 ) ) ;
#36237 = CYLINDRICAL_SURFACE ( 'NONE', #38162, 5.000000000000000000 ) ;
#36238 = EDGE_LOOP ( 'NONE', ( #63268, #6448, #6412, #9603 ) ) ;
#36239 = EDGE_CURVE ( 'NONE', #38937, #58224, #11561, .T. ) ;
#36240 = ADVANCED_FACE ( 'NONE', ( #21544 ), #60788, .T. ) ;
#36241 = CARTESIAN_POINT ( 'NONE',  ( -4.458734124999998549, -79.22916666530107932, 2.574251347313722516 ) ) ;
#36242 = CARTESIAN_POINT ( 'NONE',  ( -2.229367062500000163, 28.52083333469892779, -3.861377020970580443 ) ) ;
#36243 = CARTESIAN_POINT ( 'NONE',  ( -58.80597590150559739, -137.1250000027312410, 3.242614290531460330 ) ) ;
#36244 = EDGE_CURVE ( 'NONE', #25625, #9714, #22334, .T. ) ;
#36245 = ORIENTED_EDGE ( 'NONE', *, *, #17302, .T. ) ;
#36246 = CARTESIAN_POINT ( 'NONE',  ( -2.071067811865446640, -166.4375000027311842, 5.000000000000031086 ) ) ;
#36247 = CARTESIAN_POINT ( 'NONE',  ( -54.64476657466781973, -141.0625000013656063, -4.444560631937228834 ) ) ;
#36248 = CARTESIAN_POINT ( 'NONE',  ( -4.458734124999998549, -82.47916666530106511, 2.574251347313722516 ) ) ;
#36249 = CARTESIAN_POINT ( 'NONE',  ( -55.39835681537999790, -134.0000000027312126, 4.984105922594378235 ) ) ;
#36250 = CARTESIAN_POINT ( 'NONE',  ( 1.339745962155615144, 0.4196582014697064489, 4.999999999999999112 ) ) ;
#36251 = CARTESIAN_POINT ( 'NONE',  ( 1.846868145590735200, -143.5000000013655779, -4.458734124999999437 ) ) ;
#36252 = CARTESIAN_POINT ( 'NONE',  ( 1.255007937094098239E-14, 24.75000000000000000, -4.999999999999999112 ) ) ;
#36253 = CARTESIAN_POINT ( 'NONE',  ( -2.229367062500000163, -51.47916666530107221, -3.861377020970580443 ) ) ;
#36254 = CARTESIAN_POINT ( 'NONE',  ( 2.229367062499998831, -43.64583333196773651, -3.861377020970580887 ) ) ;
#36255 = CARTESIAN_POINT ( 'NONE',  ( -4.458734124999999437, 29.60416666803225993, -2.574251347313719407 ) ) ;
#36256 = EDGE_CURVE ( 'NONE', #4410, #60061, #159, .T. ) ;
#36257 = ADVANCED_FACE ( 'NONE', ( #12827 ), #3197, .T. ) ;
#36258 = CARTESIAN_POINT ( 'NONE',  ( 5.000000000000000888, -105.5833333333333428, 2.886751345948126879 ) ) ;
#36259 = CARTESIAN_POINT ( 'NONE',  ( 1.975475456537005874E-15, -20.74999999999999645, 5.000000000000000000 ) ) ;
#36260 = CARTESIAN_POINT ( 'NONE',  ( 9.457646018065525792E-16, -37.31249999863440792, 5.148502694627439702 ) ) ;
#36261 = CARTESIAN_POINT ( 'NONE',  ( 5.000000000000000000, 0.6250000027311873874, -6.123233995736766282E-16 ) ) ;
#36262 = CARTESIAN_POINT ( 'NONE',  ( 2.500000000000002220, 16.45833333606451987, 4.330127018922192761 ) ) ;
#36263 = CARTESIAN_POINT ( 'NONE',  ( -57.19623071787017210, -130.3750000013656631, 4.297418129356382899 ) ) ;
#36264 = CARTESIAN_POINT ( 'NONE',  ( -3.152548672688508926E-16, -81.81249999863440792, -5.148502694627439702 ) ) ;
#36265 = EDGE_CURVE ( 'NONE', #8539, #19698, #27932, .T. ) ;
#36266 = CARTESIAN_POINT ( 'NONE',  ( -55.39835681537999790, -142.0000000027312126, 4.984105922594378235 ) ) ;
#36267 = CARTESIAN_POINT ( 'NONE',  ( -3.152548672688508926E-16, -97.56249999863440792, -5.148502694627439702 ) ) ;
#36268 = CARTESIAN_POINT ( 'NONE',  ( -3.152548672688508926E-16, -2.812499998634407472, -5.148502694627439702 ) ) ;
#36269 = EDGE_LOOP ( 'NONE', ( #39984, #42527, #37908, #33205 ) ) ;
#36270 = CARTESIAN_POINT ( 'NONE',  ( 0.000000000000000000, 0.000000000000000000, -8.499999999999998224 ) ) ;
#36271 = ADVANCED_FACE ( 'NONE', ( #62364 ), #23117, .T. ) ;
#36272 = CARTESIAN_POINT ( 'NONE',  ( 1.975475456537005874E-15, -47.74999999999999289, 5.000000000000000000 ) ) ;
#36273 = CARTESIAN_POINT ( 'NONE',  ( 4.458734124999999437, -87.81249999863439371, -5.460374474430324690E-16 ) ) ;
#36274 = EDGE_CURVE ( 'NONE', #49290, #21365, #48497, .T. ) ;
#36275 = CARTESIAN_POINT ( 'NONE',  ( 2.499999999999998668, 27.66666666666666430, -4.330127018922193649 ) ) ;
#36276 = CARTESIAN_POINT ( 'NONE',  ( -3.152548672688508926E-16, -87.81249999863439371, -5.148502694627439702 ) ) ;
#36277 = CARTESIAN_POINT ( 'NONE',  ( -4.458734124999997661, 11.52083333469892423, 2.574251347313722516 ) ) ;
#36278 = DIRECTION ( 'NONE',  ( 0.000000000000000000, 0.000000000000000000, 1.000000000000000000 ) ) ;
#36279 = CARTESIAN_POINT ( 'NONE',  ( -52.80376928212989185, -134.8750000013656063, -4.297418129356379346 ) ) ;
#36280 = CARTESIAN_POINT ( 'NONE',  ( -4.458734124999999437, -7.312499998634404363, 0.000000000000000000 ) ) ;
#36281 = CARTESIAN_POINT ( 'NONE',  ( 4.458734124999999437, 14.93750000136559386, -5.460374474430324690E-16 ) ) ;
#36282 = CARTESIAN_POINT ( 'NONE',  ( 9.457646018065525792E-16, -47.31249999863440792, 5.148502694627439702 ) ) ;
#36283 =( BOUNDED_CURVE ( )  B_SPLINE_CURVE ( 2, ( #1908, #55295, #6086, #60442, #55616, #16998, #21514, #60757, #45944 ),
 .UNSPECIFIED., .F., .F. ) 
 B_SPLINE_CURVE_WITH_KNOTS ( ( 3, 2, 2, 2, 3 ),
 ( 0.2520833333333333259, 0.2527777777777777679, 0.2541666666666666519, 0.2555555555555555358, 0.2562499999999999778 ),
 .UNSPECIFIED. ) 
 CURVE ( )  GEOMETRIC_REPRESENTATION_ITEM ( )  RATIONAL_B_SPLINE_CURVE ( ( 0.9330127018922194093, 0.9330127018922194093, 1.000000000000000000, 0.8660254037844387076, 1.000000000000000000, 0.8660254037844387076, 1.000000000000000000, 0.9330127018922194093, 0.9330127018922194093 ) ) 
 REPRESENTATION_ITEM ( '' )  );
#36284 = CARTESIAN_POINT ( 'NONE',  ( 0.000000000000000000, 0.000000000000000000, 0.000000000000000000 ) ) ;
#36285 = CARTESIAN_POINT ( 'NONE',  ( -4.458734124999999437, -85.31249999863439371, 0.000000000000000000 ) ) ;
#36286 = CARTESIAN_POINT ( 'NONE',  ( 9.457646018065525792E-16, -3.062499998634407472, 5.148502694627439702 ) ) ;
#36287 = ORIENTED_EDGE ( 'NONE', *, *, #1935, .F. ) ;
#36288 = CARTESIAN_POINT ( 'NONE',  ( -3.152548672688508926E-16, -36.81249999863440792, -5.148502694627439702 ) ) ;
#36289 = CARTESIAN_POINT ( 'NONE',  ( -50.55543936806279248, -133.3125000013656063, 0.3552334253322060320 ) ) ;
#36290 = CARTESIAN_POINT ( 'NONE',  ( 4.458734124999998549, -75.72916666530106511, -2.574251347313721627 ) ) ;
#36291 = CARTESIAN_POINT ( 'NONE',  ( 2.229367062500001939, 28.77083333469892779, 3.861377020970579999 ) ) ;
#36292 = CARTESIAN_POINT ( 'NONE',  ( 9.457646018065525792E-16, 22.93750000136559919, 5.148502694627439702 ) ) ;
#36293 = CARTESIAN_POINT ( 'NONE',  ( -6.972266317189433020E-16, -58.12499999726880162, -5.000000000000000000 ) ) ;
#36294 = CARTESIAN_POINT ( 'NONE',  ( -6.972266317189433020E-16, -40.12499999726880162, -5.000000000000000000 ) ) ;
#36295 = CARTESIAN_POINT ( 'NONE',  ( -2.229367062499996610, -80.39583333196773651, 3.861377020970582219 ) ) ;
#36296 = CARTESIAN_POINT ( 'NONE',  ( 5.000000000000000000, -66.50000000000000000, -6.123233995736766282E-16 ) ) ;
#36297 = CARTESIAN_POINT ( 'NONE',  ( -5.000000000000000000, -31.87499999726880873, 0.000000000000000000 ) ) ;
#36298 = CARTESIAN_POINT ( 'NONE',  ( 5.000000000000000888, 20.54166666939784847, 2.886751345948126879 ) ) ;
#36299 = ORIENTED_EDGE ( 'NONE', *, *, #37761, .F. ) ;
#36300 = CARTESIAN_POINT ( 'NONE',  ( -5.000000000000000000, -57.08333333333333570, -2.886751345948128211 ) ) ;
#36301 = CARTESIAN_POINT ( 'NONE',  ( -5.000000000000000888, -168.5625000027312410, 2.071067811865474617 ) ) ;
#36303 = CARTESIAN_POINT ( 'NONE',  ( -5.000000000000000000, -24.08333333333333215, -2.886751345948128211 ) ) ;
#36302 = CARTESIAN_POINT ( 'NONE',  ( 55.00000000000002132, 0.000000000000000000, 0.000000000000000000 ) ) ;
#36304 = CARTESIAN_POINT ( 'NONE',  ( 4.458734124999999437, -29.81249999863440436, -5.460374474430324690E-16 ) ) ;
#36305 = CARTESIAN_POINT ( 'NONE',  ( 2.499999999999998668, -62.33333333333333570, -4.330127018922193649 ) ) ;
#36306 = CARTESIAN_POINT ( 'NONE',  ( -2.499999999999996447, -25.70833333060214798, 4.330127018922195425 ) ) ;
#36308 = ORIENTED_EDGE ( 'NONE', *, *, #9152, .F. ) ;
#36307 = CARTESIAN_POINT ( 'NONE',  ( 4.458734124999998549, -52.72916666530107221, -2.574251347313721627 ) ) ;
#36309 = DIRECTION ( 'NONE',  ( -0.000000000000000000, 1.000000000000000000, -0.000000000000000000 ) ) ;
#36310 = CARTESIAN_POINT ( 'NONE',  ( -4.999999999999998224, 11.20833333606451809, 2.886751345948131764 ) ) ;
#36312 = ORIENTED_EDGE ( 'NONE', *, *, #60309, .F. ) ;
#36311 = CARTESIAN_POINT ( 'NONE',  ( 4.458734124999999437, -3.062499998634407472, -5.460374474430324690E-16 ) ) ;
#36313 = CARTESIAN_POINT ( 'NONE',  ( 1.060575238724906964E-15, -69.75000000000000000, 5.773502691896257311 ) ) ;
#36314 = CARTESIAN_POINT ( 'NONE',  ( -53.51423613279429503, -139.2500000013656063, 4.591703134518083651 ) ) ;
#36315 = CARTESIAN_POINT ( 'NONE',  ( 4.458734125000001214, -45.14583333196774362, 2.574251347313718519 ) ) ;
#36316 = LINE ( 'NONE', #18195, #27590 ) ;
#36317 = CARTESIAN_POINT ( 'NONE',  ( -2.071067811865478170, -159.3125000000000000, 5.000000000000000000 ) ) ;
#36318 = CARTESIAN_POINT ( 'NONE',  ( -2.500000000000000444, -70.04166666393547303, -4.330127018922193649 ) ) ;
#36319 = CARTESIAN_POINT ( 'NONE',  ( -59.98410592259440222, -153.1250000000000284, -0.3983568153799752487 ) ) ;
#36320 = CARTESIAN_POINT ( 'NONE',  ( 2.229367062499998831, -17.89583333196773651, -3.861377020970580887 ) ) ;
#36321 = CARTESIAN_POINT ( 'NONE',  ( -4.458734124999999437, -49.56249999863440792, 0.000000000000000000 ) ) ;
#36322 = CARTESIAN_POINT ( 'NONE',  ( 1.846868145590736310, -143.6250000013655779, 4.458734124999999437 ) ) ;
#36323 = CARTESIAN_POINT ( 'NONE',  ( 4.458734124999999437, -94.06249999863440792, -5.460374474430324690E-16 ) ) ;
#36324 = CARTESIAN_POINT ( 'NONE',  ( 2.499999999999998668, -8.208333330602144429, -4.330127018922193649 ) ) ;
#36325 = ORIENTED_EDGE ( 'NONE', *, *, #24754, .F. ) ;
#36326 = CARTESIAN_POINT ( 'NONE',  ( -53.51423613279429503, -154.5000000013655779, 4.591703134518083651 ) ) ;
#36327 = CARTESIAN_POINT ( 'NONE',  ( -4.458734124999999437, 24.35416666803225993, -2.574251347313719407 ) ) ;
#36328 = CARTESIAN_POINT ( 'NONE',  ( -51.19402409849444524, -145.6250000027312126, -3.242614290531456334 ) ) ;
#36329 =( BOUNDED_CURVE ( )  B_SPLINE_CURVE ( 2, ( #51481, #12860, #42755, #37944, #46646, #2591, #57261, #32479, #13180 ),
 .UNSPECIFIED., .F., .F. ) 
 B_SPLINE_CURVE_WITH_KNOTS ( ( 3, 2, 2, 2, 3 ),
 ( 0.1104166666666666630, 0.1111111111111111049, 0.1125000000000000028, 0.1138888888888888867, 0.1145833333333333426 ),
 .UNSPECIFIED. ) 
 CURVE ( )  GEOMETRIC_REPRESENTATION_ITEM ( )  RATIONAL_B_SPLINE_CURVE ( ( 0.9330127018922194093, 0.9330127018922194093, 1.000000000000000000, 0.8660254037844387076, 1.000000000000000000, 0.8660254037844387076, 1.000000000000000000, 0.9330127018922187432, 0.9330127018922194093 ) ) 
 REPRESENTATION_ITEM ( '' )  );
#36330 = DIRECTION ( 'NONE',  ( 0.000000000000000000, 0.000000000000000000, 1.000000000000000000 ) ) ;
#36331 = CARTESIAN_POINT ( 'NONE',  ( 2.229367062500001939, -1.979166665301068662, 3.861377020970579999 ) ) ;
#36332 = VECTOR ( 'NONE', #42875, 1000.000000000000000 ) ;
#36333 = CARTESIAN_POINT ( 'NONE',  ( 1.846868145590736310, -147.8750000013656063, 4.458734124999999437 ) ) ;
#36334 = CARTESIAN_POINT ( 'NONE',  ( -4.458734124999998549, -23.47916666530107577, 2.574251347313722516 ) ) ;
#36335 = CARTESIAN_POINT ( 'NONE',  ( 4.458734124999998549, -62.97916666530107221, -2.574251347313721627 ) ) ;
#36336 = CARTESIAN_POINT ( 'NONE',  ( -4.458734124999999437, -9.312499998634406140, 0.000000000000000000 ) ) ;
#36337 = CARTESIAN_POINT ( 'NONE',  ( -58.24261429053147765, -146.3750000027312126, -3.805975901505573855 ) ) ;
#36338 = CARTESIAN_POINT ( 'NONE',  ( 3.152801135295367541, -145.3125000013655779, -3.152801135295367541 ) ) ;
#36339 = CARTESIAN_POINT ( 'NONE',  ( 4.458734125000000326, 15.85416666803226171, 2.574251347313718519 ) ) ;
#36340 = ORIENTED_EDGE ( 'NONE', *, *, #18522, .F. ) ;
#36341 = CARTESIAN_POINT ( 'NONE',  ( -1.339745962155610925, -18.66965819600733312, 5.000000000000000000 ) ) ;
#36342 = CARTESIAN_POINT ( 'NONE',  ( -1.339745962155613812, -21.20534180126147561, -5.000000000000000000 ) ) ;
#36344 = CARTESIAN_POINT ( 'NONE',  ( 4.458734124999999437, -18.81249999863440792, -5.460374474430324690E-16 ) ) ;
#36343 = CARTESIAN_POINT ( 'NONE',  ( 5.000000000000000888, -84.58333333333332860, 2.886751345948126879 ) ) ;
#36345 = CARTESIAN_POINT ( 'NONE',  ( -4.458734124999999437, 26.35416666803225993, -2.574251347313719407 ) ) ;
#36346 = CARTESIAN_POINT ( 'NONE',  ( -57.46284108482265651, -137.9375000000000284, 4.819101127000238627 ) ) ;
#36347 = CARTESIAN_POINT ( 'NONE',  ( -59.59170313451811296, -146.5000000013656347, 1.485763867205729394 ) ) ;
#36348 = ADVANCED_FACE ( 'NONE', ( #48182 ), #53327, .T. ) ;
#36349 = CARTESIAN_POINT ( 'NONE',  ( -2.499999999999996447, -47.70833333060215153, 4.330127018922195425 ) ) ;
#36350 = CYLINDRICAL_SURFACE ( 'NONE', #21032, 5.000000000000000000 ) ;
#36351 = CARTESIAN_POINT ( 'NONE',  ( -4.458734124999999437, 10.68750000136559386, 0.000000000000000000 ) ) ;
#36352 = CARTESIAN_POINT ( 'NONE',  ( 5.000000000000000000, -56.29166666393548013, -2.886751345948130876 ) ) ;
#36353 = DIRECTION ( 'NONE',  ( -0.000000000000000000, 1.000000000000000000, -0.000000000000000000 ) ) ;
#36354 = CARTESIAN_POINT ( 'NONE',  ( -2.229367062499996610, 14.85416666803226171, 3.861377020970582219 ) ) ;
#36355 = CARTESIAN_POINT ( 'NONE',  ( 9.457646018065525792E-16, -67.06249999863440792, 5.148502694627439702 ) ) ;
#36356 = CARTESIAN_POINT ( 'NONE',  ( -4.458734124999997661, -14.47916666530107221, 2.574251347313722516 ) ) ;
#36357 = CARTESIAN_POINT ( 'NONE',  ( 2.499999999999998668, 0.6666666666666660745, -4.330127018922193649 ) ) ;
#36358 = CARTESIAN_POINT ( 'NONE',  ( 2.730187237215162345E-16, -163.1875000013655779, -4.458734124999999437 ) ) ;
#36359 = CARTESIAN_POINT ( 'NONE',  ( 6.123233995736766282E-16, -170.0000000000000000, -5.000000000000000000 ) ) ;
#36360 = CARTESIAN_POINT ( 'NONE',  ( 4.458734124999999437, -59.81249999863440081, -5.460374474430324690E-16 ) ) ;
#36361 = CARTESIAN_POINT ( 'NONE',  ( 2.500000000000002220, -92.54166666393547303, 4.330127018922192761 ) ) ;
#36362 = CARTESIAN_POINT ( 'NONE',  ( -5.000000000000000000, -70.08333333333332860, -2.886751345948128211 ) ) ;
#36363 = CARTESIAN_POINT ( 'NONE',  ( 2.071067811865434205, -139.3125000027311842, 5.000000000000041744 ) ) ;
#36364 = CARTESIAN_POINT ( 'NONE',  ( -4.458734124999999437, -33.31249999863440792, 0.000000000000000000 ) ) ;
#36365 = CARTESIAN_POINT ( 'NONE',  ( 1.975475456537005874E-15, -51.62499999726880873, 5.000000000000000000 ) ) ;
#36366 = CARTESIAN_POINT ( 'NONE',  ( 5.000000000000000888, -50.58333333333332860, 2.886751345948126879 ) ) ;
#36367 = LINE ( 'NONE', #51175, #52124 ) ;
#36368 = CARTESIAN_POINT ( 'NONE',  ( 1.975475456537005874E-15, -17.62499999726881938, 5.000000000000000000 ) ) ;
#36369 = ORIENTED_EDGE ( 'NONE', *, *, #24727, .F. ) ;
#36370 = CARTESIAN_POINT ( 'NONE',  ( 2.229367062500001939, -107.9791666653010651, 3.861377020970579999 ) ) ;
#36371 = CARTESIAN_POINT ( 'NONE',  ( 4.458734124999998549, 0.02083333469892617584, -2.574251347313721627 ) ) ;
#36372 = CARTESIAN_POINT ( 'NONE',  ( 5.000000000000000888, -89.45833333060215864, 2.886751345948126879 ) ) ;
#36373 = CARTESIAN_POINT ( 'NONE',  ( 2.500000000000002220, -9.666666666666664298, 4.330127018922192761 ) ) ;
#36374 = CARTESIAN_POINT ( 'NONE',  ( -2.229367062499996610, -72.14583333196773651, 3.861377020970582219 ) ) ;
#36375 = VECTOR ( 'NONE', #25244, 1000.000000000000000 ) ;
#36376 = CYLINDRICAL_SURFACE ( 'NONE', #32875, 5.000000000000000000 ) ;
#36377 = CARTESIAN_POINT ( 'NONE',  ( -5.000000000000000000, -6.958333330602150646, -2.886751345948128211 ) ) ;
#36379 = VERTEX_POINT ( 'NONE', #22814 ) ;
#36378 = CARTESIAN_POINT ( 'NONE',  ( 2.229367062500001939, -36.97916666530107221, 3.861377020970579999 ) ) ;
#36380 = CARTESIAN_POINT ( 'NONE',  ( -1.339745962155613812, -17.08034179853029144, -5.000000000000000000 ) ) ;
#36382 = ORIENTED_EDGE ( 'NONE', *, *, #48011, .F. ) ;
#36381 = CARTESIAN_POINT ( 'NONE',  ( 4.458734124999998549, 14.02083333469892779, -2.574251347313721627 ) ) ;
#36383 = CARTESIAN_POINT ( 'NONE',  ( 1.975475456537005874E-15, -108.7499999999999858, 5.000000000000000000 ) ) ;
#36384 = CARTESIAN_POINT ( 'NONE',  ( 5.000000000000000888, -53.58333333333333570, 2.886751345948126879 ) ) ;
#36385 = CARTESIAN_POINT ( 'NONE',  ( -4.458734125000001214, -159.1250000013656063, 1.846868145590734089 ) ) ;
#36386 = CARTESIAN_POINT ( 'NONE',  ( -4.458734124999999437, -31.56249999863440436, 0.000000000000000000 ) ) ;
#36387 = DIRECTION ( 'NONE',  ( -0.000000000000000000, 1.000000000000000000, -0.000000000000000000 ) ) ;
#36388 = CARTESIAN_POINT ( 'NONE',  ( -4.458734124999998549, -74.22916666530106511, 2.574251347313722516 ) ) ;
#36389 = CARTESIAN_POINT ( 'NONE',  ( -5.000000000000000888, -168.5625000000000000, -2.071067811865475949 ) ) ;
#36390 = CARTESIAN_POINT ( 'NONE',  ( 2.229367062500001939, -85.97916666530107932, 3.861377020970579999 ) ) ;
#36391 = CARTESIAN_POINT ( 'NONE',  ( -55.35523342533222291, -134.5625000013656063, 4.444560631937231499 ) ) ;
#36392 = CARTESIAN_POINT ( 'NONE',  ( 2.229367062500001939, -34.22916666530107221, 3.861377020970579999 ) ) ;
#36393 = CARTESIAN_POINT ( 'NONE',  ( -6.972266317189433020E-16, -83.12499999726878741, -5.000000000000000000 ) ) ;
#36394 = VERTEX_POINT ( 'NONE', #57852 ) ;
#36395 = CARTESIAN_POINT ( 'NONE',  ( 4.458734125000001214, -80.14583333196773651, 2.574251347313718519 ) ) ;
#36396 = CARTESIAN_POINT ( 'NONE',  ( -2.352990130084580066E-16, 8.660254037844390851, -7.422398894150034288 ) ) ;
#36397 = ORIENTED_EDGE ( 'NONE', *, *, #30283, .T. ) ;
#36398 = CARTESIAN_POINT ( 'NONE',  ( 5.000000000000000888, -16.58333333333333215, 2.886751345948126879 ) ) ;
#36399 =( REPRESENTATION_RELATIONSHIP ('NONE','NONE', #27855, #25037 ) REPRESENTATION_RELATIONSHIP_WITH_TRANSFORMATION ( #30776 )SHAPE_REPRESENTATION_RELATIONSHIP( ) );
#36400 = LINE ( 'NONE', #56982, #46617 ) ;
#36401 = CARTESIAN_POINT ( 'NONE',  ( -4.458734124999998549, -62.47916666530106511, 2.574251347313722516 ) ) ;
#36402 = CARTESIAN_POINT ( 'NONE',  ( -3.152548672688508926E-16, -7.812499998634405252, -5.148502694627439702 ) ) ;
#36403 = VERTEX_POINT ( 'NONE', #13772 ) ;
#36404 =( BOUNDED_CURVE ( )  B_SPLINE_CURVE ( 2, ( #55225, #50390, #31723, #35922, #6025, #46525, #2467, #15974, #11462 ),
 .UNSPECIFIED., .F., .F. ) 
 B_SPLINE_CURVE_WITH_KNOTS ( ( 3, 2, 2, 2, 3 ),
 ( 0.4104166666666666519, 0.4111111111111110938, 0.4124999999999999778, 0.4138888888888888618, 0.4145833333333333592 ),
 .UNSPECIFIED. ) 
 CURVE ( )  GEOMETRIC_REPRESENTATION_ITEM ( )  RATIONAL_B_SPLINE_CURVE ( ( 0.9330127018922194093, 0.9330127018922194093, 1.000000000000000000, 0.8660254037844387076, 1.000000000000000000, 0.8660254037844387076, 1.000000000000000000, 0.9330127018922167448, 0.9330127018922194093 ) ) 
 REPRESENTATION_ITEM ( '' )  );
#36405 = CARTESIAN_POINT ( 'NONE',  ( -4.999999999999998224, -84.91666666666667140, 2.886751345948131764 ) ) ;
#36406 = DIRECTION ( 'NONE',  ( -0.000000000000000000, -0.000000000000000000, 1.000000000000000000 ) ) ;
#36407 = ORIENTED_EDGE ( 'NONE', *, *, #36970, .F. ) ;
#36408 = CARTESIAN_POINT ( 'NONE',  ( 4.458734124999998549, -4.979166665301072214, -2.574251347313721627 ) ) ;
#36409 = FACE_OUTER_BOUND ( 'NONE', #29800, .T. ) ;
#36410 = CARTESIAN_POINT ( 'NONE',  ( 4.458734124999999437, 6.187500001365593860, -5.460374474430324690E-16 ) ) ;
#36411 = CARTESIAN_POINT ( 'NONE',  ( 2.499999999999998668, -64.33333333333332860, -4.330127018922193649 ) ) ;
#36412 = CARTESIAN_POINT ( 'NONE',  ( 4.458734124999997661, -156.5000000013656347, 1.846868145590737864 ) ) ;
#36413 = DIRECTION ( 'NONE',  ( -0.000000000000000000, 1.000000000000000000, -0.000000000000000000 ) ) ;
#36414 = ORIENTED_EDGE ( 'NONE', *, *, #28405, .F. ) ;
#36415 = CARTESIAN_POINT ( 'NONE',  ( -2.229367062500000163, -84.47916666530107932, -3.861377020970580443 ) ) ;
#36416 = CARTESIAN_POINT ( 'NONE',  ( 0.000000000000000000, -120.0000000000000000, 0.000000000000000000 ) ) ;
#36417 = CARTESIAN_POINT ( 'NONE',  ( -2.229367062499996610, -3.145833331967738733, 3.861377020970582219 ) ) ;
#36418 = LINE ( 'NONE', #39954, #12902 ) ;
#36419 = VECTOR ( 'NONE', #20317, 1000.000000000000000 ) ;
#36420 =( BOUNDED_CURVE ( )  B_SPLINE_CURVE ( 2, ( #50130, #25697, #45307, #1275, #40477, #60118, #35668, #55615, #17314 ),
 .UNSPECIFIED., .F., .F. ) 
 B_SPLINE_CURVE_WITH_KNOTS ( ( 3, 2, 2, 2, 3 ),
 ( 0.5803571428571429047, 0.5809523809523809978, 0.5821428571428571841, 0.5833333333333333703, 0.5839285714285714635 ),
 .UNSPECIFIED. ) 
 CURVE ( )  GEOMETRIC_REPRESENTATION_ITEM ( )  RATIONAL_B_SPLINE_CURVE ( ( 0.9330127018922194093, 0.9330127018922194093, 1.000000000000000000, 0.8660254037844387076, 1.000000000000000000, 0.8660254037844387076, 1.000000000000000000, 0.9330127018922194093, 0.9330127018922194093 ) ) 
 REPRESENTATION_ITEM ( '' )  );
#36421 = CARTESIAN_POINT ( 'NONE',  ( 5.000000000000000000, -28.29166666393548013, -2.886751345948129988 ) ) ;
#36422 = CARTESIAN_POINT ( 'NONE',  ( 0.000000000000000000, 0.000000000000000000, 0.000000000000000000 ) ) ;
#36423 = CARTESIAN_POINT ( 'NONE',  ( -3.152548672688508926E-16, 22.43750000136559564, -5.148502694627439702 ) ) ;
#36424 = CARTESIAN_POINT ( 'NONE',  ( 2.500000000000002220, -104.6666666666666572, 4.330127018922192761 ) ) ;
#36425 = CARTESIAN_POINT ( 'NONE',  ( -4.458734124999999437, 28.68750000136559208, 0.000000000000000000 ) ) ;
#36426 = CARTESIAN_POINT ( 'NONE',  ( -3.152548672688508926E-16, -49.56249999863440792, -5.148502694627439702 ) ) ;
#36427 = CARTESIAN_POINT ( 'NONE',  ( -4.458734124999997661, -38.47916666530107221, 2.574251347313722516 ) ) ;
#36428 = CARTESIAN_POINT ( 'NONE',  ( 9.457646018065525792E-16, 0.6875000013655957476, 5.148502694627439702 ) ) ;
#36429 = CARTESIAN_POINT ( 'NONE',  ( -2.499999999999996447, 9.291666669397853795, 4.330127018922195425 ) ) ;
#36430 = CARTESIAN_POINT ( 'NONE',  ( -5.000000000000000000, 16.91666666666666430, -2.886751345948128211 ) ) ;
#36431 = CARTESIAN_POINT ( 'NONE',  ( 3.535533905932738197, -145.0000000027311842, -3.535533905932738197 ) ) ;
#36432 = CARTESIAN_POINT ( 'NONE',  ( 9.457646018065525792E-16, -45.06249999863440792, 5.148502694627439702 ) ) ;
#36433 = CARTESIAN_POINT ( 'NONE',  ( 5.000000000000000000, -79.37499999726881583, -6.123233995736766282E-16 ) ) ;
#36434 = CARTESIAN_POINT ( 'NONE',  ( -53.51423613279429503, -140.5000000013656347, 4.591703134518082763 ) ) ;
#36435 = CARTESIAN_POINT ( 'NONE',  ( 6.123233995736766282E-16, -170.0000000000000000, -5.000000000000000000 ) ) ;
#36436 = CARTESIAN_POINT ( 'NONE',  ( 2.499999999999998668, -22.33333333333332860, -4.330127018922193649 ) ) ;
#36437 = CARTESIAN_POINT ( 'NONE',  ( -4.458734124999997661, -87.47916666530107932, 2.574251347313722516 ) ) ;
#36438 = CARTESIAN_POINT ( 'NONE',  ( -1.846868145590737420, -160.0000000013656063, 4.458734124999997661 ) ) ;
#36439 = CARTESIAN_POINT ( 'NONE',  ( -2.387978478801491278, -7.281554020289322970, -7.069802615102039667 ) ) ;
#36440 = CARTESIAN_POINT ( 'NONE',  ( 1.060575238724906964E-15, -32.75000000000000711, 5.773502691896257311 ) ) ;
#36441 = CARTESIAN_POINT ( 'NONE',  ( -8.190561711645485556E-16, -140.6875000013656063, 4.458734124999999437 ) ) ;
#36442 = ORIENTED_EDGE ( 'NONE', *, *, #48987, .F. ) ;
#36443 = CARTESIAN_POINT ( 'NONE',  ( -2.229367062500000163, 21.27083333469892779, -3.861377020970580443 ) ) ;
#36444 = VERTEX_POINT ( 'NONE', #43351 ) ;
#36445 = CARTESIAN_POINT ( 'NONE',  ( -4.458734124999999437, -93.31249999863440792, 0.000000000000000000 ) ) ;
#36446 = CARTESIAN_POINT ( 'NONE',  ( -2.229367062499996610, 13.60416666803226171, 3.861377020970582219 ) ) ;
#36447 = CARTESIAN_POINT ( 'NONE',  ( 5.000000000000000888, 14.54166666939785024, 2.886751345948126879 ) ) ;
#36448 = CARTESIAN_POINT ( 'NONE',  ( 1.339745962155615144, -16.70534180126147561, 4.999999999999999112 ) ) ;
#36449 = CARTESIAN_POINT ( 'NONE',  ( 5.000000000000000888, 10.41666666666666607, 2.886751345948126879 ) ) ;
#36450 = ADVANCED_FACE ( 'NONE', ( #62999 ), #47252, .F. ) ;
#36451 = CARTESIAN_POINT ( 'NONE',  ( 2.229367062499998831, -58.64583333196773651, -3.861377020970580887 ) ) ;
#36452 = CARTESIAN_POINT ( 'NONE',  ( -2.229367062499996610, -12.14583333196774007, 3.861377020970582219 ) ) ;
#36453 = FACE_OUTER_BOUND ( 'NONE', #59446, .T. ) ;
#36454 = CARTESIAN_POINT ( 'NONE',  ( -52.10840900171896806, -136.4375000013656063, 3.393966926194110556 ) ) ;
#36455 = CARTESIAN_POINT ( 'NONE',  ( 0.000000000000000000, -170.0000000000000000, 0.000000000000000000 ) ) ;
#36456 = CARTESIAN_POINT ( 'NONE',  ( -2.499999999999996447, 0.2916666693978525737, 4.330127018922195425 ) ) ;
#36457 = CARTESIAN_POINT ( 'NONE',  ( -1.339745962155610925, 18.33034180399266333, 5.000000000000000000 ) ) ;
#36458 = CARTESIAN_POINT ( 'NONE',  ( 5.000000000000000000, -40.49999999999999289, -6.123233995736766282E-16 ) ) ;
#36459 = CARTESIAN_POINT ( 'NONE',  ( 3.061616997868383141E-16, -148.7500000000000284, -5.000000000000000000 ) ) ;
#36461 = CARTESIAN_POINT ( 'NONE',  ( 2.229367062499998831, -15.89583333196773651, -3.861377020970580887 ) ) ;
#36460 = CARTESIAN_POINT ( 'NONE',  ( -57.46284108482265651, -138.9375000000000000, 4.819101127000238627 ) ) ;
#36462 = CARTESIAN_POINT ( 'NONE',  ( -5.000000000000000000, -58.08333333333333570, -2.886751345948128211 ) ) ;
#36463 = CARTESIAN_POINT ( 'NONE',  ( 2.229367062500001939, -61.97916666530106511, 3.861377020970579999 ) ) ;
#36464 = CARTESIAN_POINT ( 'NONE',  ( -3.152801135295367096, -151.3125000013655779, -3.152801135295367541 ) ) ;
#36465 = CARTESIAN_POINT ( 'NONE',  ( 4.458734124999998549, -69.72916666530107932, -2.574251347313721627 ) ) ;
#36466 = CARTESIAN_POINT ( 'NONE',  ( -57.89159099828107458, -145.9375000013656063, -3.393966926194107447 ) ) ;
#36467 = AXIS2_PLACEMENT_3D ( 'NONE', #6414, #20569, #55934 ) ;
#36468 = CARTESIAN_POINT ( 'NONE',  ( 2.229367062499998831, -17.89583333196773651, -3.861377020970580887 ) ) ;
#36469 = CARTESIAN_POINT ( 'NONE',  ( 2.499999999999998668, -63.20833333060215153, -4.330127018922193649 ) ) ;
#36470 = ORIENTED_EDGE ( 'NONE', *, *, #54778, .T. ) ;
#36471 = DIRECTION ( 'NONE',  ( -0.000000000000000000, 1.000000000000000000, -0.000000000000000000 ) ) ;
#36472 = ORIENTED_EDGE ( 'NONE', *, *, #4501, .T. ) ;
#36473 = CARTESIAN_POINT ( 'NONE',  ( 4.458734124999998549, -60.97916666530106511, -2.574251347313721627 ) ) ;
#36475 = CARTESIAN_POINT ( 'NONE',  ( -6.972266317189433020E-16, -103.2500000000000000, -5.000000000000000000 ) ) ;
#36474 = CARTESIAN_POINT ( 'NONE',  ( 1.339745962155612702, -21.29465819873852084, -5.000000000000000000 ) ) ;
#36476 = CARTESIAN_POINT ( 'NONE',  ( -4.458734125000000326, -153.0000000013656063, -1.846868145590735644 ) ) ;
#36477 = ORIENTED_EDGE ( 'NONE', *, *, #24697, .T. ) ;
#36478 =( BOUNDED_CURVE ( )  B_SPLINE_CURVE ( 2, ( #46709, #61521, #56052, #37375, #57008, #32544, #57640, #19640, #39250 ),
 .UNSPECIFIED., .F., .F. ) 
 B_SPLINE_CURVE_WITH_KNOTS ( ( 3, 2, 2, 2, 3 ),
 ( 0.8910714285714286254, 0.8916666666666667185, 0.8928571428571429047, 0.8940476190476190910, 0.8946428571428571841 ),
 .UNSPECIFIED. ) 
 CURVE ( )  GEOMETRIC_REPRESENTATION_ITEM ( )  RATIONAL_B_SPLINE_CURVE ( ( 0.9330127018922194093, 0.9330127018922256266, 1.000000000000000000, 0.8660254037844387076, 1.000000000000000000, 0.8660254037844387076, 1.000000000000000000, 0.9330127018922194093, 0.9330127018922194093 ) ) 
 REPRESENTATION_ITEM ( '' )  );
#36479 = CARTESIAN_POINT ( 'NONE',  ( -6.972266317189433020E-16, 25.74999999999999645, -5.000000000000000000 ) ) ;
#36480 = CARTESIAN_POINT ( 'NONE',  ( -56.66612745406270335, -127.3125000000000284, -5.149110718188516067 ) ) ;
#36481 = CARTESIAN_POINT ( 'NONE',  ( -4.999999999999998224, -74.79166666393547303, 2.886751345948131764 ) ) ;
#36482 = CARTESIAN_POINT ( 'NONE',  ( 2.229367062500001939, -47.22916666530106511, 3.861377020970579999 ) ) ;
#36483 = ORIENTED_EDGE ( 'NONE', *, *, #15856, .F. ) ;
#36484 = CARTESIAN_POINT ( 'NONE',  ( 4.458734124999999437, 7.187500001365594748, -5.460374474430324690E-16 ) ) ;
#36485 = CARTESIAN_POINT ( 'NONE',  ( -3.152548672688508926E-16, 22.43750000136559208, -5.148502694627439702 ) ) ;
#36486 = CARTESIAN_POINT ( 'NONE',  ( -50.40829686548195099, -151.0000000013656063, -1.485763867205728284 ) ) ;
#36487 = CARTESIAN_POINT ( 'NONE',  ( -1.846868145590734756, -169.1250000013656063, -4.458734124999999437 ) ) ;
#36488 = ORIENTED_EDGE ( 'NONE', *, *, #25746, .F. ) ;
#36489 = CARTESIAN_POINT ( 'NONE',  ( 9.457646018065525792E-16, -69.06249999863439371, 5.148502694627439702 ) ) ;
#36490 = LINE ( 'NONE', #31024, #36645 ) ;
#36491 = CARTESIAN_POINT ( 'NONE',  ( -2.229367062500000163, 13.52083333469892779, -3.861377020970580443 ) ) ;
#36492 = CARTESIAN_POINT ( 'NONE',  ( 5.000000000000000000, 7.708333336064518093, -2.886751345948130876 ) ) ;
#36493 = CARTESIAN_POINT ( 'NONE',  ( -5.000000000000000000, -27.08333333333333215, -2.886751345948128211 ) ) ;
#36494 = CARTESIAN_POINT ( 'NONE',  ( 4.458734124999999437, -57.06249999863440081, -5.460374474430324690E-16 ) ) ;
#36495 = CARTESIAN_POINT ( 'NONE',  ( 2.500000000000002220, -14.54166666393548191, 4.330127018922192761 ) ) ;
#36496 = CARTESIAN_POINT ( 'NONE',  ( -2.499999999999996447, -44.70833333060214443, 4.330127018922195425 ) ) ;
#36497 = CARTESIAN_POINT ( 'NONE',  ( 1.339745962155615144, -65.70534180126148271, 4.999999999999999112 ) ) ;
#36498 =( BOUNDED_CURVE ( )  B_SPLINE_CURVE ( 2, ( #16281, #16911, #6318, #59714, #6957, #16598, #30422, #50687, #51012 ),
 .UNSPECIFIED., .F., .F. ) 
 B_SPLINE_CURVE_WITH_KNOTS ( ( 3, 2, 2, 2, 3 ),
 ( 0.1354166666666666574, 0.1361111111111110994, 0.1375000000000000111, 0.1388888888888888951, 0.1395833333333333370 ),
 .UNSPECIFIED. ) 
 CURVE ( )  GEOMETRIC_REPRESENTATION_ITEM ( )  RATIONAL_B_SPLINE_CURVE ( ( 0.9330127018922194093, 0.9330127018922194093, 1.000000000000000000, 0.8660254037844387076, 1.000000000000000000, 0.8660254037844387076, 1.000000000000000000, 0.9330127018922194093, 0.9330127018922194093 ) ) 
 REPRESENTATION_ITEM ( '' )  );
#36499 = CARTESIAN_POINT ( 'NONE',  ( 4.458734125000000326, -21.14583333196774362, 2.574251347313718519 ) ) ;
#36500 = ORIENTED_EDGE ( 'NONE', *, *, #10187, .T. ) ;
#36501 = CARTESIAN_POINT ( 'NONE',  ( 1.975475456537005874E-15, -60.75000000000000000, 5.000000000000000000 ) ) ;
#36502 = CARTESIAN_POINT ( 'NONE',  ( 2.229367062500001939, -109.9791666653010651, 3.861377020970579999 ) ) ;
#36503 = CARTESIAN_POINT ( 'NONE',  ( -3.535533905932738641, -156.5000000027312126, 3.535533905932737309 ) ) ;
#36504 = VERTEX_POINT ( 'NONE', #18289 ) ;
#36505 = CARTESIAN_POINT ( 'NONE',  ( -4.458734124999998549, -102.4791666653010509, 2.574251347313722516 ) ) ;
#36506 = CARTESIAN_POINT ( 'NONE',  ( -3.152548672688508926E-16, -25.56249999863440436, -5.148502694627439702 ) ) ;
#36507 = CARTESIAN_POINT ( 'NONE',  ( 5.000000000000000000, -62.29166666393547303, -2.886751345948129988 ) ) ;
#36508 = CIRCLE ( 'NONE', #45742, 11.00000000000000000 ) ;
#36509 = CARTESIAN_POINT ( 'NONE',  ( -56.48576386720575471, -154.0000000013655779, -4.591703134518078322 ) ) ;
#36510 = CARTESIAN_POINT ( 'NONE',  ( 3.535533905932736864, -148.1250000000000000, 3.535533905932738641 ) ) ;
#36511 = CARTESIAN_POINT ( 'NONE',  ( 9.457646018065525792E-16, -25.06249999863440792, 5.148502694627439702 ) ) ;
#36512 = CARTESIAN_POINT ( 'NONE',  ( -2.229367062499996610, -70.39583333196773651, 3.861377020970582219 ) ) ;
#36513 = CARTESIAN_POINT ( 'NONE',  ( 2.499999999999998668, 8.666666666666666075, -4.330127018922193649 ) ) ;
#36514 = CARTESIAN_POINT ( 'NONE',  ( -4.458734124999999437, -23.31249999863440436, 0.000000000000000000 ) ) ;
#36515 = CARTESIAN_POINT ( 'NONE',  ( 2.500000000000002220, -32.54166666393547303, 4.330127018922192761 ) ) ;
#36516 = CARTESIAN_POINT ( 'NONE',  ( -5.000000000000000888, -152.5625000000000284, -2.071067811865475949 ) ) ;
#36517 = CARTESIAN_POINT ( 'NONE',  ( 5.000000000000000000, -16.50000000000000000, -6.123233995736766282E-16 ) ) ;
#36518 = CARTESIAN_POINT ( 'NONE',  ( -3.152801135295367985, -150.8125000013655779, 3.152801135295367096 ) ) ;
#36519 = ORIENTED_EDGE ( 'NONE', *, *, #53455, .T. ) ;
#36520 = CARTESIAN_POINT ( 'NONE',  ( 4.458734125000000326, -49.14583333196772941, 2.574251347313718519 ) ) ;
#36521 = DIRECTION ( 'NONE',  ( -0.000000000000000000, 1.000000000000000000, -0.000000000000000000 ) ) ;
#36522 = LINE ( 'NONE', #56152, #49345 ) ;
#36523 = CARTESIAN_POINT ( 'NONE',  ( -2.499999999999996447, 23.16666666666666430, 4.330127018922195425 ) ) ;
#36524 = EDGE_CURVE ( 'NONE', #25814, #22293, #534, .T. ) ;
#36525 = CARTESIAN_POINT ( 'NONE',  ( -54.60164318462004474, -152.3750000000000284, -4.984105922594373794 ) ) ;
#36526 = CARTESIAN_POINT ( 'NONE',  ( -4.458734124999999437, 6.687500001365593860, 0.000000000000000000 ) ) ;
#36527 = CARTESIAN_POINT ( 'NONE',  ( 5.000000000000000888, 1.541666669397853795, 2.886751345948126879 ) ) ;
#36528 = CARTESIAN_POINT ( 'NONE',  ( 2.500000000000002220, -95.54166666393547303, 4.330127018922192761 ) ) ;
#36529 = FACE_OUTER_BOUND ( 'NONE', #37822, .T. ) ;
#36530 = CARTESIAN_POINT ( 'NONE',  ( -4.458734124999998549, 16.52083333469892779, 2.574251347313722516 ) ) ;
#36531 = CARTESIAN_POINT ( 'NONE',  ( -2.500000000000000444, 4.958333336064518981, -4.330127018922193649 ) ) ;
#36532 = ORIENTED_EDGE ( 'NONE', *, *, #48322, .T. ) ;
#36533 = LINE ( 'NONE', #52599, #5835 ) ;
#36534 = ORIENTED_EDGE ( 'NONE', *, *, #35089, .T. ) ;
#36535 = CARTESIAN_POINT ( 'NONE',  ( -2.499999999999996447, -50.83333333333332860, 4.330127018922195425 ) ) ;
#36536 = CARTESIAN_POINT ( 'NONE',  ( -4.458734124999999437, -42.31249999863440081, 0.000000000000000000 ) ) ;
#36537 = CARTESIAN_POINT ( 'NONE',  ( 3.152801135295366208, -165.8125000013656063, 3.152801135295367985 ) ) ;
#36538 = EDGE_CURVE ( 'NONE', #47814, #25936, #53008, .T. ) ;
#36539 = CARTESIAN_POINT ( 'NONE',  ( -2.500000000000000444, -47.04166666393547303, -4.330127018922193649 ) ) ;
#36540 = ORIENTED_EDGE ( 'NONE', *, *, #28841, .T. ) ;
#36542 = EDGE_CURVE ( 'NONE', #3482, #32387, #18907, .T. ) ;
#36541 = CARTESIAN_POINT ( 'NONE',  ( -4.458734124999999437, -19.39583333196774007, -2.574251347313719407 ) ) ;
#36543 = ORIENTED_EDGE ( 'NONE', *, *, #54997, .T. ) ;
#36544 = CARTESIAN_POINT ( 'NONE',  ( -5.000000000000000000, -86.00000000000000000, 0.000000000000000000 ) ) ;
#36545 = CARTESIAN_POINT ( 'NONE',  ( 4.458734125000000326, -163.3750000013656347, -1.846868145590734978 ) ) ;
#36547 = VERTEX_POINT ( 'NONE', #28875 ) ;
#36546 = DIRECTION ( 'NONE',  ( 0.000000000000000000, 0.000000000000000000, 1.000000000000000000 ) ) ;
#36548 = CARTESIAN_POINT ( 'NONE',  ( -58.24261429053147765, -138.2500000000000000, -3.805975901505573855 ) ) ;
#36549 = CARTESIAN_POINT ( 'NONE',  ( -4.458734124999999437, -31.64583333196773651, -2.574251347313719407 ) ) ;
#36550 = CARTESIAN_POINT ( 'NONE',  ( -1.339745962155610925, 21.20534180126147561, 5.000000000000000000 ) ) ;
#36551 = ORIENTED_EDGE ( 'NONE', *, *, #26360, .T. ) ;
#36552 = VECTOR ( 'NONE', #7279, 1000.000000000000000 ) ;
#36553 = CARTESIAN_POINT ( 'NONE',  ( -2.229367062499996610, -75.14583333196773651, 3.861377020970582219 ) ) ;
#36554 = CARTESIAN_POINT ( 'NONE',  ( -3.152548672688508926E-16, 24.43750000136559564, -5.148502694627439702 ) ) ;
#36555 = CARTESIAN_POINT ( 'NONE',  ( 1.339745962155615144, -18.70534180126147916, 4.999999999999999112 ) ) ;
#36556 = ORIENTED_EDGE ( 'NONE', *, *, #52729, .F. ) ;
#36557 = CARTESIAN_POINT ( 'NONE',  ( 3.061616997868383141E-16, -161.7500000000000000, -5.000000000000000000 ) ) ;
#36558 = CARTESIAN_POINT ( 'NONE',  ( -53.51423613279429503, -142.5000000013656063, 4.591703134518083651 ) ) ;
#36559 = CARTESIAN_POINT ( 'NONE',  ( -4.458734124999999437, -80.56249999863440792, 0.000000000000000000 ) ) ;
#36560 = CARTESIAN_POINT ( 'NONE',  ( -58.24261429053147765, -129.3750000027312126, -3.805975901505573855 ) ) ;
#36561 = CARTESIAN_POINT ( 'NONE',  ( 5.000000000000000888, 0.5416666693978527958, 2.886751345948126879 ) ) ;
#36562 = CARTESIAN_POINT ( 'NONE',  ( 4.458734124999997661, -142.7500000013655779, 1.846868145590737864 ) ) ;
#36563 = CARTESIAN_POINT ( 'NONE',  ( 5.000000000000000888, 20.41666666666666785, 2.886751345948126879 ) ) ;
#36564 = CARTESIAN_POINT ( 'NONE',  ( -4.458734124999997661, -57.22916666530107932, 2.574251347313722516 ) ) ;
#36565 = CARTESIAN_POINT ( 'NONE',  ( -4.458734124999997661, -45.22916666530106511, 2.574251347313722516 ) ) ;
#36566 = CARTESIAN_POINT ( 'NONE',  ( -2.229367062500000163, 26.52083333469892779, -3.861377020970580443 ) ) ;
#36567 = CARTESIAN_POINT ( 'NONE',  ( 1.060575238724906964E-15, -108.7499999999999858, 5.773502691896257311 ) ) ;
#36568 = CARTESIAN_POINT ( 'NONE',  ( 2.071067811865645591, -154.3125000027311557, 4.999999999999830358 ) ) ;
#36569 = CARTESIAN_POINT ( 'NONE',  ( 4.458734125000001214, -37.14583333196773651, 2.574251347313718519 ) ) ;
#36570 = CARTESIAN_POINT ( 'NONE',  ( 2.500000000000002220, -0.5416666639354792423, 4.330127018922192761 ) ) ;
#36571 = DIRECTION ( 'NONE',  ( 0.000000000000000000, 0.000000000000000000, 1.000000000000000000 ) ) ;
#36572 = CARTESIAN_POINT ( 'NONE',  ( -5.000000000000000000, -45.87499999726880873, 0.000000000000000000 ) ) ;
#36573 = CARTESIAN_POINT ( 'NONE',  ( 4.458734125000001214, -79.14583333196772230, 2.574251347313718519 ) ) ;
#36574 = CARTESIAN_POINT ( 'NONE',  ( -1.339745962155610925, 6.205341801261478274, 5.000000000000000000 ) ) ;
#36575 = CARTESIAN_POINT ( 'NONE',  ( 2.229367062499998831, -103.6458333319677365, -3.861377020970580887 ) ) ;
#36576 = CARTESIAN_POINT ( 'NONE',  ( 2.229367062500001939, -4.229166665301070438, 3.861377020970579999 ) ) ;
#36577 = ORIENTED_EDGE ( 'NONE', *, *, #46332, .F. ) ;
#36578 = DIRECTION ( 'NONE',  ( 0.000000000000000000, 0.000000000000000000, 1.000000000000000000 ) ) ;
#36579 = CARTESIAN_POINT ( 'NONE',  ( 1.339745962155612702, -9.169658196007334894, -5.000000000000000000 ) ) ;
#36580 = CARTESIAN_POINT ( 'NONE',  ( 2.229367062500001939, -93.97916666530106511, 3.861377020970579999 ) ) ;
#36581 = CARTESIAN_POINT ( 'NONE',  ( -6.972266317189433020E-16, -5.249999999999998224, -5.000000000000000000 ) ) ;
#36582 = CARTESIAN_POINT ( 'NONE',  ( 4.458734125000001214, -87.14583333196772230, 2.574251347313718519 ) ) ;
#36583 = CARTESIAN_POINT ( 'NONE',  ( -2.229367062499996610, 10.60416666803225993, 3.861377020970582219 ) ) ;
#36584 = CARTESIAN_POINT ( 'NONE',  ( -75.00000000000001421, 15.00000000000000000, -9.000000000000001776 ) ) ;
#36585 = CARTESIAN_POINT ( 'NONE',  ( -59.44456063193725015, -133.5625000013656063, -0.3552334253322034230 ) ) ;
#36586 = CARTESIAN_POINT ( 'NONE',  ( 4.458734124999998549, -6.729166665301073103, -2.574251347313721627 ) ) ;
#36587 = CARTESIAN_POINT ( 'NONE',  ( 2.229367062500001939, 14.77083333469892779, 3.861377020970579999 ) ) ;
#36588 = CARTESIAN_POINT ( 'NONE',  ( 2.229367062500001939, -51.22916666530107221, 3.861377020970579999 ) ) ;
#36589 = CARTESIAN_POINT ( 'NONE',  ( -4.999999999999998224, 17.20833333606451987, 2.886751345948131764 ) ) ;
#36590 = CARTESIAN_POINT ( 'NONE',  ( -2.229367062499996610, -84.14583333196773651, 3.861377020970582219 ) ) ;
#36591 = CARTESIAN_POINT ( 'NONE',  ( -4.458734124999997661, -7.229166665301073103, 2.574251347313722516 ) ) ;
#36592 = CARTESIAN_POINT ( 'NONE',  ( 5.000000000000000000, -106.3749999972688158, -6.123233995736766282E-16 ) ) ;
#36593 = ORIENTED_EDGE ( 'NONE', *, *, #15239, .F. ) ;
#36594 = CARTESIAN_POINT ( 'NONE',  ( -4.458734124999999437, -33.56249999863440792, 0.000000000000000000 ) ) ;
#36595 = VECTOR ( 'NONE', #28380, 1000.000000000000000 ) ;
#36596 = CARTESIAN_POINT ( 'NONE',  ( -59.59170313451811296, -126.7500000013655921, 1.485763867205729394 ) ) ;
#36597 = CARTESIAN_POINT ( 'NONE',  ( 4.458734125000001214, -80.89583333196773651, 2.574251347313718519 ) ) ;
#36598 = CARTESIAN_POINT ( 'NONE',  ( 5.000000000000000000, -109.2916666639354872, -2.886751345948129988 ) ) ;
#36599 = AXIS2_PLACEMENT_3D ( 'NONE', #25750, #61446, #55982 ) ;
#36600 = AXIS2_PLACEMENT_3D ( 'NONE', #47027, #50657, #61516 ) ;
#36601 =( BOUNDED_CURVE ( )  B_SPLINE_CURVE ( 2, ( #11234, #2248, #31806, #60779, #16705, #51440, #6739, #16063, #1302 ),
 .UNSPECIFIED., .F., .F. ) 
 B_SPLINE_CURVE_WITH_KNOTS ( ( 3, 2, 2, 2, 3 ),
 ( 0.1604166666666666796, 0.1611111111111111216, 0.1625000000000000056, 0.1638888888888888895, 0.1645833333333333315 ),
 .UNSPECIFIED. ) 
 CURVE ( )  GEOMETRIC_REPRESENTATION_ITEM ( )  RATIONAL_B_SPLINE_CURVE ( ( 0.9330127018922194093, 0.9330127018922207416, 1.000000000000000000, 0.8660254037844387076, 1.000000000000000000, 0.8660254037844387076, 1.000000000000000000, 0.9330127018922194093, 0.9330127018922194093 ) ) 
 REPRESENTATION_ITEM ( '' )  );
#36602 = CARTESIAN_POINT ( 'NONE',  ( 4.458734124999999437, -148.6250000013655779, -1.846868145590734978 ) ) ;
#36603 = CARTESIAN_POINT ( 'NONE',  ( -2.229367062500000163, 20.52083333469892779, -3.861377020970580443 ) ) ;
#36604 = EDGE_CURVE ( 'NONE', #13010, #49422, #63299, .T. ) ;
#36605 = ADVANCED_FACE ( 'NONE', ( #30135 ), #30954, .F. ) ;
#36606 = CARTESIAN_POINT ( 'NONE',  ( -5.000000000000000000, -25.95833333060214798, -2.886751345948128211 ) ) ;
#36607 = CARTESIAN_POINT ( 'NONE',  ( 4.458734125000000326, -81.14583333196773651, 2.574251347313718519 ) ) ;
#36608 = CARTESIAN_POINT ( 'NONE',  ( 2.499999999999998668, -63.33333333333332149, -4.330127018922193649 ) ) ;
#36609 = EDGE_CURVE ( 'NONE', #21297, #11671, #29180, .T. ) ;
#36610 = FACE_OUTER_BOUND ( 'NONE', #23018, .T. ) ;
#36611 = CARTESIAN_POINT ( 'NONE',  ( 5.000000000000000000, 18.70833333606451632, -2.886751345948129988 ) ) ;
#36612 = EDGE_LOOP ( 'NONE', ( #61312, #30514, #36551, #7848 ) ) ;
#36614 = CARTESIAN_POINT ( 'NONE',  ( 2.499999999999998668, -26.33333333333333215, -4.330127018922193649 ) ) ;
#36613 = CARTESIAN_POINT ( 'NONE',  ( 1.975475456537005874E-15, -75.62499999726880162, 5.000000000000000000 ) ) ;
#36615 = CARTESIAN_POINT ( 'NONE',  ( 4.458734125000001214, -29.89583333196773651, 2.574251347313718519 ) ) ;
#36616 = CARTESIAN_POINT ( 'NONE',  ( 1.975475456537005874E-15, -86.75000000000001421, 5.000000000000000000 ) ) ;
#36617 = EDGE_CURVE ( 'NONE', #141, #37963, #59432, .T. ) ;
#36618 = CARTESIAN_POINT ( 'NONE',  ( 1.060575238724906964E-15, -29.62499999726881228, 5.773502691896257311 ) ) ;
#36620 = EDGE_LOOP ( 'NONE', ( #9991, #44658, #26257, #55196 ) ) ;
#36619 = CARTESIAN_POINT ( 'NONE',  ( -3.152548672688508926E-16, -53.56249999863439371, -5.148502694627439702 ) ) ;
#36621 = CARTESIAN_POINT ( 'NONE',  ( -59.59170313451811296, -153.7500000013656063, 1.485763867205729394 ) ) ;
#36622 = EDGE_CURVE ( 'NONE', #39380, #24136, #19856, .T. ) ;
#36624 = ORIENTED_EDGE ( 'NONE', *, *, #59057, .T. ) ;
#36623 = CARTESIAN_POINT ( 'NONE',  ( 2.229367062499998831, -4.895833331967740065, -3.861377020970580887 ) ) ;
#36625 = CARTESIAN_POINT ( 'NONE',  ( 5.000000000000000888, -70.58333333333332860, 2.886751345948126879 ) ) ;
#36626 = CARTESIAN_POINT ( 'NONE',  ( -59.29741812935640155, -139.6250000013655779, -2.196230717870135685 ) ) ;
#36627 = CARTESIAN_POINT ( 'NONE',  ( -4.458734124999999437, -50.56249999863440792, 0.000000000000000000 ) ) ;
#36628 = CARTESIAN_POINT ( 'NONE',  ( -6.972266317189433020E-16, -65.12499999726880162, -5.000000000000000000 ) ) ;
#36629 = EDGE_CURVE ( 'NONE', #29478, #37570, #35854, .T. ) ;
#36630 = CARTESIAN_POINT ( 'NONE',  ( 2.500000000000002220, -76.54166666393547303, 4.330127018922192761 ) ) ;
#36631 = LINE ( 'NONE', #40496, #40543 ) ;
#36632 = CARTESIAN_POINT ( 'NONE',  ( -53.33387254593733928, -152.8125000000000284, 5.149110718188519620 ) ) ;
#36633 = CARTESIAN_POINT ( 'NONE',  ( -4.458734124999999437, -17.56249999863440792, 0.000000000000000000 ) ) ;
#36634 = CARTESIAN_POINT ( 'NONE',  ( -4.458734124999999437, -53.64583333196772941, -2.574251347313719407 ) ) ;
#36635 = FACE_OUTER_BOUND ( 'NONE', #32138, .T. ) ;
#36636 = DIRECTION ( 'NONE',  ( 0.000000000000000000, 0.000000000000000000, 1.000000000000000000 ) ) ;
#36637 = CARTESIAN_POINT ( 'NONE',  ( -1.846868145590734756, -142.1250000013656063, -4.458734125000000326 ) ) ;
#36638 = CARTESIAN_POINT ( 'NONE',  ( -4.458734124999999437, -92.56249999863440792, 0.000000000000000000 ) ) ;
#36639 = LINE ( 'NONE', #41135, #2004 ) ;
#36640 = ORIENTED_EDGE ( 'NONE', *, *, #40533, .F. ) ;
#36641 = CYLINDRICAL_SURFACE ( 'NONE', #52940, 5.000000000000000000 ) ;
#36642 = CARTESIAN_POINT ( 'NONE',  ( -56.66612745406270335, -144.4375000027312410, -5.149110718188516067 ) ) ;
#36643 = AXIS2_PLACEMENT_3D ( 'NONE', #19470, #44548, #58714 ) ;
#36644 = CARTESIAN_POINT ( 'NONE',  ( 4.458734124999999437, -0.8124999986344055847, -5.460374474430324690E-16 ) ) ;
#36645 = VECTOR ( 'NONE', #61266, 1000.000000000000000 ) ;
#36646 = CARTESIAN_POINT ( 'NONE',  ( 9.457646018065525792E-16, -96.31249999863439371, 5.148502694627439702 ) ) ;
#36647 = CARTESIAN_POINT ( 'NONE',  ( -4.458734125000001214, -148.1250000013655779, 1.846868145590734089 ) ) ;
#36648 = CARTESIAN_POINT ( 'NONE',  ( 4.458734125000001214, -25.14583333196774007, 2.574251347313718519 ) ) ;
#36649 = AXIS2_PLACEMENT_3D ( 'NONE', #38782, #53276, #13097 ) ;
#36650 = CARTESIAN_POINT ( 'NONE',  ( -4.999999999999998224, -66.91666666666667140, 2.886751345948131764 ) ) ;
#36651 = CARTESIAN_POINT ( 'NONE',  ( -50.55543936806279248, -141.0625000013656063, 0.3552334253322060320 ) ) ;
#36652 =( BOUNDED_CURVE ( )  B_SPLINE_CURVE ( 2, ( #56979, #2953, #13217, #3271, #2629, #61494, #17425, #46370, #51827 ),
 .UNSPECIFIED., .F., .F. ) 
 B_SPLINE_CURVE_WITH_KNOTS ( ( 3, 2, 2, 2, 3 ),
 ( 0.1062499999999999972, 0.1069444444444444392, 0.1083333333333333370, 0.1097222222222222210, 0.1104166666666666630 ),
 .UNSPECIFIED. ) 
 CURVE ( )  GEOMETRIC_REPRESENTATION_ITEM ( )  RATIONAL_B_SPLINE_CURVE ( ( 0.9330127018922194093, 0.9330127018922194093, 1.000000000000000000, 0.8660254037844387076, 1.000000000000000000, 0.8660254037844387076, 1.000000000000000000, 0.9330127018922194093, 0.9330127018922194093 ) ) 
 REPRESENTATION_ITEM ( '' )  );
#36653 = CARTESIAN_POINT ( 'NONE',  ( -2.229367062499996610, -61.39583333196774362, 3.861377020970582219 ) ) ;
#36654 = CARTESIAN_POINT ( 'NONE',  ( 5.000000000000000000, -72.50000000000000000, -6.123233995736766282E-16 ) ) ;
#36655 = LINE ( 'NONE', #7397, #57274 ) ;
#36656 = CARTESIAN_POINT ( 'NONE',  ( -4.458734124999999437, -143.9375000013656063, -5.460374474430324690E-16 ) ) ;
#36657 =( BOUNDED_CURVE ( )  B_SPLINE_CURVE ( 2, ( #10745, #59315, #50301, #15250, #30354, #5604, #49978, #1121, #5930 ),
 .UNSPECIFIED., .F., .F. ) 
 B_SPLINE_CURVE_WITH_KNOTS ( ( 3, 2, 2, 2, 3 ),
 ( 0.7624999999999999556, 0.7630952380952380487, 0.7642857142857142350, 0.7654761904761904212, 0.7660714285714286254 ),
 .UNSPECIFIED. ) 
 CURVE ( )  GEOMETRIC_REPRESENTATION_ITEM ( )  RATIONAL_B_SPLINE_CURVE ( ( 0.9330127018922194093, 0.9330127018922194093, 1.000000000000000000, 0.8660254037844387076, 1.000000000000000000, 0.8660254037844387076, 1.000000000000000000, 0.9330127018922130810, 0.9330127018922194093 ) ) 
 REPRESENTATION_ITEM ( '' )  );
#36658 = CARTESIAN_POINT ( 'NONE',  ( 4.458734124999999437, 10.93750000136559386, -5.460374474430324690E-16 ) ) ;
#36659 = ORIENTED_EDGE ( 'NONE', *, *, #53167, .T. ) ;
#36660 = CARTESIAN_POINT ( 'NONE',  ( -3.535533905932738641, -164.5000000027312126, 3.535533905932737309 ) ) ;
#36661 = CARTESIAN_POINT ( 'NONE',  ( 5.000000000000000000, -66.37499999726881583, -6.123233995736766282E-16 ) ) ;
#36663 = CARTESIAN_POINT ( 'NONE',  ( 2.229367062500001939, -26.97916666530106866, 3.861377020970579999 ) ) ;
#36662 = CARTESIAN_POINT ( 'NONE',  ( -2.499999999999996447, -86.83333333333332860, 4.330127018922195425 ) ) ;
#36664 = CARTESIAN_POINT ( 'NONE',  ( -4.458734124999999437, 29.43750000136559208, 0.000000000000000000 ) ) ;
#36665 = DIRECTION ( 'NONE',  ( -0.000000000000000000, 1.000000000000000000, -0.000000000000000000 ) ) ;
#36666 = CARTESIAN_POINT ( 'NONE',  ( -56.48576386720575471, -144.7500000013656063, -4.591703134518078322 ) ) ;
#36667 = CARTESIAN_POINT ( 'NONE',  ( -5.000000000000000000, -46.87499999726880873, 0.000000000000000000 ) ) ;
#36668 = CARTESIAN_POINT ( 'NONE',  ( 1.975475456537005874E-15, -1.624999997268813834, 5.000000000000000000 ) ) ;
#36669 = CARTESIAN_POINT ( 'NONE',  ( 4.458734124999998549, 9.270833334698927786, -2.574251347313721627 ) ) ;
#36670 = CARTESIAN_POINT ( 'NONE',  ( 1.975475456537005874E-15, -21.62499999726880873, 5.000000000000000000 ) ) ;
#36671 = CARTESIAN_POINT ( 'NONE',  ( 2.500000000000002220, 21.33333333333333215, 4.330127018922192761 ) ) ;
#36672 = CARTESIAN_POINT ( 'NONE',  ( -4.458734124999999437, 9.604166668032259935, -2.574251347313719407 ) ) ;
#36673 = CARTESIAN_POINT ( 'NONE',  ( -3.152548672688508926E-16, -66.56249999863440792, -5.148502694627439702 ) ) ;
#36674 = CARTESIAN_POINT ( 'NONE',  ( -4.458734124999997661, -17.47916666530106866, 2.574251347313722516 ) ) ;
#36675 = CARTESIAN_POINT ( 'NONE',  ( 5.000000000000000000, -2.416666666666664298, -2.886751345948129988 ) ) ;
#36676 = CARTESIAN_POINT ( 'NONE',  ( 4.458734124999999437, -159.5000000013655779, 1.846868145590737864 ) ) ;
#36677 = CARTESIAN_POINT ( 'NONE',  ( -5.000000000000000000, 22.00000000000000000, 0.000000000000000000 ) ) ;
#36678 = CARTESIAN_POINT ( 'NONE',  ( -2.229367062499996610, -62.14583333196774362, 3.861377020970582219 ) ) ;
#36679 = CARTESIAN_POINT ( 'NONE',  ( -5.000000000000000000, -92.87499999726881583, 0.000000000000000000 ) ) ;
#36680 = CARTESIAN_POINT ( 'NONE',  ( -2.499999999999996447, -79.83333333333332860, 4.330127018922195425 ) ) ;
#36681 = CARTESIAN_POINT ( 'NONE',  ( 5.000000000000000000, -56.49999999999999289, -6.123233995736766282E-16 ) ) ;
#36682 = CARTESIAN_POINT ( 'NONE',  ( -2.229367062499996610, -35.14583333196772941, 3.861377020970582219 ) ) ;
#36683 = EDGE_CURVE ( 'NONE', #49700, #28303, #53953, .T. ) ;
#36684 = DIRECTION ( 'NONE',  ( 0.000000000000000000, 0.000000000000000000, 1.000000000000000000 ) ) ;
#36685 = CARTESIAN_POINT ( 'NONE',  ( 4.458734124999998549, -59.97916666530106511, -2.574251347313721627 ) ) ;
#36686 =( BOUNDED_CURVE ( )  B_SPLINE_CURVE ( 2, ( #30024, #1743, #5919, #15882, #6871, #35502, #782, #40635, #20389 ),
 .UNSPECIFIED., .F., .F. ) 
 B_SPLINE_CURVE_WITH_KNOTS ( ( 3, 2, 2, 2, 3 ),
 ( 0.5083333333333337478, 0.5125000000000003997, 0.5166666666666671626, 0.5208333333333338144, 0.5250000000000004663 ),
 .UNSPECIFIED. ) 
 CURVE ( )  GEOMETRIC_REPRESENTATION_ITEM ( )  RATIONAL_B_SPLINE_CURVE ( ( 0.9999999999999918954, 0.9238795325112948431, 1.000000000000000000, 0.9238795325112867385, 1.000000000000000000, 0.9238795325112867385, 1.000000000000000000, 0.9238795325112786339, 1.000000000000008216 ) ) 
 REPRESENTATION_ITEM ( '' )  );
#36687 = CARTESIAN_POINT ( 'NONE',  ( 2.500000000000002220, -46.66666666666666430, 4.330127018922192761 ) ) ;
#36688 = CARTESIAN_POINT ( 'NONE',  ( -55.00000000000002132, -155.0000000000000284, 1.734723475976807094E-15 ) ) ;
#36689 = CARTESIAN_POINT ( 'NONE',  ( 5.000000000000000888, -36.45833333060213732, 2.886751345948126879 ) ) ;
#36690 = VERTEX_POINT ( 'NONE', #38834 ) ;
#36691 = CARTESIAN_POINT ( 'NONE',  ( -4.458734124999998549, -106.2291666653010793, 2.574251347313722516 ) ) ;
#36692 = CARTESIAN_POINT ( 'NONE',  ( -4.458734124999998549, -3.479166665301069994, 2.574251347313722516 ) ) ;
#36693 = CARTESIAN_POINT ( 'NONE',  ( 1.339745962155499015, -73.58034179853028434, 5.000000000000065725 ) ) ;
#36694 = CARTESIAN_POINT ( 'NONE',  ( 2.500000000000002220, -7.666666666666668739, 4.330127018922192761 ) ) ;
#36695 = CARTESIAN_POINT ( 'NONE',  ( -4.458734124999999437, -70.39583333196773651, -2.574251347313719407 ) ) ;
#36696=STYLED_ITEM('',(#63719),#50087);
#36697 = LINE ( 'NONE', #3251, #54452 ) ;
#36698 = CARTESIAN_POINT ( 'NONE',  ( -3.535250795749689387E-16, -12.12499999726881761, -5.773502691896257311 ) ) ;
#36700 = ORIENTED_EDGE ( 'NONE', *, *, #12488, .T. ) ;
#36699 = CARTESIAN_POINT ( 'NONE',  ( -2.229367062500000163, -40.47916666530107221, -3.861377020970580443 ) ) ;
#36701 = VECTOR ( 'NONE', #40351, 1000.000000000000000 ) ;
#36702 = CARTESIAN_POINT ( 'NONE',  ( 5.000000000000000000, -100.2916666639354446, -2.886751345948130876 ) ) ;
#36704 = ORIENTED_EDGE ( 'NONE', *, *, #15780, .T. ) ;
#36703 = CARTESIAN_POINT ( 'NONE',  ( -4.458734124999998549, 12.52083333469892779, 2.574251347313722516 ) ) ;
#36705 = CARTESIAN_POINT ( 'NONE',  ( 2.500000000000002220, -81.66666666666667140, 4.330127018922192761 ) ) ;
#36706 = CARTESIAN_POINT ( 'NONE',  ( -2.499999999999996447, -57.83333333333333570, 4.330127018922195425 ) ) ;
#36707 = ADVANCED_FACE ( 'NONE', ( #39154 ), #10214, .T. ) ;
#36708 = CARTESIAN_POINT ( 'NONE',  ( -1.846868145590734756, -161.3750000013656063, -4.458734125000000326 ) ) ;
#36709 = CARTESIAN_POINT ( 'NONE',  ( -4.458734124999999437, -36.56249999863440792, 0.000000000000000000 ) ) ;
#36710 = CARTESIAN_POINT ( 'NONE',  ( -5.000000000000000000, -87.08333333333331439, -2.886751345948128211 ) ) ;
#36711 = CARTESIAN_POINT ( 'NONE',  ( -2.229367062499996610, -80.14583333196773651, 3.861377020970582219 ) ) ;
#36712 =( BOUNDED_CURVE ( )  B_SPLINE_CURVE ( 2, ( #43309, #58427, #62944, #35575, #30745, #11118, #21099, #20783, #39421 ),
 .UNSPECIFIED., .F., .F. ) 
 B_SPLINE_CURVE_WITH_KNOTS ( ( 3, 2, 2, 2, 3 ),
 ( 0.4839285714285714302, 0.4845238095238095233, 0.4857142857142857095, 0.4869047619047618958, 0.4874999999999999889 ),
 .UNSPECIFIED. ) 
 CURVE ( )  GEOMETRIC_REPRESENTATION_ITEM ( )  RATIONAL_B_SPLINE_CURVE ( ( 0.9330127018922194093, 0.9330127018922194093, 1.000000000000000000, 0.8660254037844387076, 1.000000000000000000, 0.8660254037844387076, 1.000000000000000000, 0.9330127018922194093, 0.9330127018922194093 ) ) 
 REPRESENTATION_ITEM ( '' )  );
#36713 = CARTESIAN_POINT ( 'NONE',  ( 3.152801135295366208, -139.8125000013655779, 3.152801135295367985 ) ) ;
#36714 = EDGE_CURVE ( 'NONE', #3623, #50310, #9885, .T. ) ;
#36715 = CARTESIAN_POINT ( 'NONE',  ( -2.229367062499996610, -87.14583333196773651, 3.861377020970582219 ) ) ;
#36716 = CARTESIAN_POINT ( 'NONE',  ( -55.35523342533222291, -136.5625000013656063, 4.444560631937231499 ) ) ;
#36717 = CARTESIAN_POINT ( 'NONE',  ( -4.458734124999999437, 1.354166668032261933, -2.574251347313719407 ) ) ;
#36718 = CARTESIAN_POINT ( 'NONE',  ( -4.458734124999999437, -33.64583333196772941, -2.574251347313719407 ) ) ;
#36719 = EDGE_CURVE ( 'NONE', #38746, #45557, #44296, .T. ) ;
#36720 = CARTESIAN_POINT ( 'NONE',  ( 0.000000000000000000, -120.0000000000000000, 0.000000000000000000 ) ) ;
#36721 = CARTESIAN_POINT ( 'NONE',  ( 4.458734124999998549, -75.97916666530106511, -2.574251347313721627 ) ) ;
#36722 = CARTESIAN_POINT ( 'NONE',  ( 5.000000000000000888, -84.58333333333332860, 2.886751345948126879 ) ) ;
#36723 = VERTEX_POINT ( 'NONE', #59107 ) ;
#36724 = CARTESIAN_POINT ( 'NONE',  ( -1.339745962155610925, -14.66965819600733667, 5.000000000000000000 ) ) ;
#36725 = CARTESIAN_POINT ( 'NONE',  ( -1.339745962155660663, -18.66965819600733667, 4.999999999999972466 ) ) ;
#36726 = CARTESIAN_POINT ( 'NONE',  ( -3.152548672688508926E-16, -70.81249999863440792, -5.148502694627439702 ) ) ;
#36727 = CARTESIAN_POINT ( 'NONE',  ( -3.152548672688508926E-16, -10.81249999863440792, -5.148502694627439702 ) ) ;
#36728 = EDGE_LOOP ( 'NONE', ( #5536, #51110, #5327, #19614 ) ) ;
#36729 = CARTESIAN_POINT ( 'NONE',  ( 1.339745962155612702, -3.169658196007334894, -5.000000000000000000 ) ) ;
#36730 = CARTESIAN_POINT ( 'NONE',  ( -4.458734124999999437, -5.562499998634402587, 0.000000000000000000 ) ) ;
#36731 = CARTESIAN_POINT ( 'NONE',  ( -59.81910112700026616, -147.3125000027311842, -2.462841084822525506 ) ) ;
#36732 = CARTESIAN_POINT ( 'NONE',  ( -2.229367062499996610, 8.854166668032261711, 3.861377020970582219 ) ) ;
#36733 = CARTESIAN_POINT ( 'NONE',  ( 5.000000000000000000, -64.41666666666665719, -2.886751345948130876 ) ) ;
#36734 = CARTESIAN_POINT ( 'NONE',  ( -3.152801135295367096, -159.0625000013656063, -3.152801135295367541 ) ) ;
#36735 = VECTOR ( 'NONE', #18128, 1000.000000000000000 ) ;
#36736 = CARTESIAN_POINT ( 'NONE',  ( -2.229367062500000163, 29.27083333469892779, -3.861377020970580443 ) ) ;
#36737 = ORIENTED_EDGE ( 'NONE', *, *, #41053, .T. ) ;
#36738 = CARTESIAN_POINT ( 'NONE',  ( 4.458734125000000326, -85.89583333196775072, 2.574251347313718519 ) ) ;
#36739 = CARTESIAN_POINT ( 'NONE',  ( -4.999999999999998224, -24.91666666666666430, 2.886751345948131764 ) ) ;
#36740 = CARTESIAN_POINT ( 'NONE',  ( -3.152548672688508926E-16, -4.562499998634401699, -5.148502694627439702 ) ) ;
#36741 = VECTOR ( 'NONE', #56449, 1000.000000000000000 ) ;
#36742 = CARTESIAN_POINT ( 'NONE',  ( 6.288404560131952259, 5.029641972278931839, -0.4504974108211943773 ) ) ;
#36743=STYLED_ITEM('',(#63705),#50626);
#36744 = CARTESIAN_POINT ( 'NONE',  ( -2.500000000000000444, -32.04166666393548724, -4.330127018922193649 ) ) ;
#36745 = CARTESIAN_POINT ( 'NONE',  ( -4.729367062499999719, -110.1562499993171969, 0.000000000000000000 ) ) ;
#36746 = CARTESIAN_POINT ( 'NONE',  ( -4.458734124999999437, 25.60416666803225638, -2.574251347313719407 ) ) ;
#36747 = CARTESIAN_POINT ( 'NONE',  ( 5.000000000000000000, -10.41666666666666607, -2.886751345948130876 ) ) ;
#36748 = CARTESIAN_POINT ( 'NONE',  ( -2.229367062500000163, 28.52083333469892779, -3.861377020970580443 ) ) ;
#36749 = CARTESIAN_POINT ( 'NONE',  ( -2.229367062500000163, -50.47916666530107221, -3.861377020970580443 ) ) ;
#36750 = CARTESIAN_POINT ( 'NONE',  ( -4.458734124999999437, -39.56249999863440081, 0.000000000000000000 ) ) ;
#36751 = CARTESIAN_POINT ( 'NONE',  ( 2.229367062499998831, -1.895833331967737623, -3.861377020970580887 ) ) ;
#36752 = CARTESIAN_POINT ( 'NONE',  ( 1.339745962155612702, -0.1696581960073343942, -5.000000000000000000 ) ) ;
#36753 = CARTESIAN_POINT ( 'NONE',  ( -2.500000000000000444, 13.83333333333333215, -4.330127018922193649 ) ) ;
#36754 = CARTESIAN_POINT ( 'NONE',  ( -2.071067811865475061, -141.8125000027311842, -5.000000000000000888 ) ) ;
#36755 = CYLINDRICAL_SURFACE ( 'NONE', #17174, 5.000000000000000000 ) ;
#36756 = CARTESIAN_POINT ( 'NONE',  ( 4.458734124999999437, -40.81249999863440081, -5.460374474430324690E-16 ) ) ;
#36757 = CARTESIAN_POINT ( 'NONE',  ( -4.999999999999999112, -80.79166666393547303, 2.886751345948131764 ) ) ;
#36758 = AXIS2_PLACEMENT_3D ( 'NONE', #26933, #17273, #36897 ) ;
#36759 = CARTESIAN_POINT ( 'NONE',  ( -59.59170313451811296, -139.7500000013656347, 1.485763867205729394 ) ) ;
#36760 = LINE ( 'NONE', #56389, #22653 ) ;
#36761 = EDGE_CURVE ( 'NONE', #19705, #32024, #27210, .T. ) ;
#36762 = CARTESIAN_POINT ( 'NONE',  ( 2.500000000000002220, 3.333333333333333925, 4.330127018922192761 ) ) ;
#36763 = CARTESIAN_POINT ( 'NONE',  ( 4.458734124999999437, -86.06249999863439371, -5.460374474430324690E-16 ) ) ;
#36764 = CARTESIAN_POINT ( 'NONE',  ( 2.730187237215162345E-16, -163.4375000013655779, -4.458734124999999437 ) ) ;
#36765 = CARTESIAN_POINT ( 'NONE',  ( -5.000000000000000000, -34.08333333333332860, -2.886751345948128211 ) ) ;
#36766 = CARTESIAN_POINT ( 'NONE',  ( -2.500000000000000444, -57.16666666666667140, -4.330127018922193649 ) ) ;
#36767 = ORIENTED_EDGE ( 'NONE', *, *, #1539, .T. ) ;
#36768 = CARTESIAN_POINT ( 'NONE',  ( 9.457646018065525792E-16, 18.68750000136559208, 5.148502694627439702 ) ) ;
#36769 = EDGE_LOOP ( 'NONE', ( #49863, #6140, #53264, #12094 ) ) ;
#36770 = CARTESIAN_POINT ( 'NONE',  ( -2.229367062499996610, -89.14583333196773651, 3.861377020970582219 ) ) ;
#36771 = CARTESIAN_POINT ( 'NONE',  ( 4.458734124999998549, 16.02083333469892423, -2.574251347313721627 ) ) ;
#36772 = CARTESIAN_POINT ( 'NONE',  ( -3.535250795749689387E-16, 13.87500000273118417, -5.773502691896257311 ) ) ;
#36773 = CARTESIAN_POINT ( 'NONE',  ( 1.975475456537005874E-15, -28.62499999726881583, 5.000000000000000000 ) ) ;
#36774 = CARTESIAN_POINT ( 'NONE',  ( -2.499999999999996447, 9.166666666666666075, 4.330127018922195425 ) ) ;
#36775 = CARTESIAN_POINT ( 'NONE',  ( -2.229367062500000163, -55.47916666530107221, -3.861377020970580443 ) ) ;
#36776 = CARTESIAN_POINT ( 'NONE',  ( 1.339745962155615144, -6.705341801261480050, 4.999999999999999112 ) ) ;
#36777 = CARTESIAN_POINT ( 'NONE',  ( -58.39396692619412477, -135.6875000013656063, 2.891590998281057701 ) ) ;
#36778 = CARTESIAN_POINT ( 'NONE',  ( 5.000000000000000000, 7.625000002731186832, -6.123233995736766282E-16 ) ) ;
#36779 = CARTESIAN_POINT ( 'NONE',  ( 0.000000000000000000, 0.000000000000000000, 0.000000000000000000 ) ) ;
#36780 = CARTESIAN_POINT ( 'NONE',  ( 5.000000000000000888, -39.58333333333333570, 2.886751345948126879 ) ) ;
#36781 = DIRECTION ( 'NONE',  ( -0.000000000000000000, 1.000000000000000000, -0.000000000000000000 ) ) ;
#36782 = CARTESIAN_POINT ( 'NONE',  ( -4.458734124999999437, -15.56249999863440436, 0.000000000000000000 ) ) ;
#36783 = AXIS2_PLACEMENT_3D ( 'NONE', #62224, #17528, #37453 ) ;
#36784 = CARTESIAN_POINT ( 'NONE',  ( 1.975475456537005874E-15, 13.24999999999999822, 5.000000000000000000 ) ) ;
#36785 = CARTESIAN_POINT ( 'NONE',  ( 2.229367062499998831, -64.64583333196773651, -3.861377020970580887 ) ) ;
#36786 = CARTESIAN_POINT ( 'NONE',  ( -1.846868145590737420, -152.0000000013655779, 4.458734124999999437 ) ) ;
#36787 = CARTESIAN_POINT ( 'NONE',  ( 4.458734125000001214, -70.89583333196773651, 2.574251347313718519 ) ) ;
#36788 = AXIS2_PLACEMENT_3D ( 'NONE', #49352, #5941, #25230 ) ;
#36789 = CARTESIAN_POINT ( 'NONE',  ( -52.10840900171896806, -147.4375000013656063, 3.393966926194110556 ) ) ;
#36790 =( BOUNDED_CURVE ( )  B_SPLINE_CURVE ( 2, ( #38350, #57976, #33529, #13902, #23874, #54414, #48621, #34452, #19991 ),
 .UNSPECIFIED., .F., .F. ) 
 B_SPLINE_CURVE_WITH_KNOTS ( ( 3, 2, 2, 2, 3 ),
 ( 0.07321428571428571785, 0.07380952380952381098, 0.07499999999999999722, 0.07619047619047619735, 0.07678571428571429047 ),
 .UNSPECIFIED. ) 
 CURVE ( )  GEOMETRIC_REPRESENTATION_ITEM ( )  RATIONAL_B_SPLINE_CURVE ( ( 0.9330127018922194093, 0.9330127018922194093, 1.000000000000000000, 0.8660254037844387076, 1.000000000000000000, 0.8660254037844387076, 1.000000000000000000, 0.9330127018922194093, 0.9330127018922194093 ) ) 
 REPRESENTATION_ITEM ( '' )  );
#36791 = CARTESIAN_POINT ( 'NONE',  ( 4.458734124999999437, -17.06249999863440792, -5.460374474430324690E-16 ) ) ;
#36792 = CARTESIAN_POINT ( 'NONE',  ( -5.000000000000000000, -59.95833333060215153, -2.886751345948128211 ) ) ;
#36793 = ORIENTED_EDGE ( 'NONE', *, *, #48929, .F. ) ;
#36794 = CARTESIAN_POINT ( 'NONE',  ( -2.500000000000000444, -49.16666666666666430, -4.330127018922193649 ) ) ;
#36795 = ORIENTED_EDGE ( 'NONE', *, *, #39788, .T. ) ;
#36796 = CARTESIAN_POINT ( 'NONE',  ( 2.229367062499998831, -62.89583333196774362, -3.861377020970580887 ) ) ;
#36797 = CARTESIAN_POINT ( 'NONE',  ( -9.184850993605147944E-16, -144.2500000000000284, 5.000000000000000000 ) ) ;
#36798 = CARTESIAN_POINT ( 'NONE',  ( 1.846868145590735200, -152.2500000013656347, -4.458734125000000326 ) ) ;
#36799 = ORIENTED_EDGE ( 'NONE', *, *, #16940, .T. ) ;
#36800 = CARTESIAN_POINT ( 'NONE',  ( -5.000000000000000000, 27.12500000273118772, 0.000000000000000000 ) ) ;
#36801 = CARTESIAN_POINT ( 'NONE',  ( -51.19402409849444524, -126.5000000000000284, -3.242614290531456334 ) ) ;
#36802 = CARTESIAN_POINT ( 'NONE',  ( 0.000000000000000000, -120.0000000000000000, 0.000000000000000000 ) ) ;
#36803 = CARTESIAN_POINT ( 'NONE',  ( -4.458734124999998549, -46.47916666530107221, 2.574251347313722516 ) ) ;
#36804 = VERTEX_POINT ( 'NONE', #26602 ) ;
#36805 = VECTOR ( 'NONE', #41872, 1000.000000000000000 ) ;
#36806 =( BOUNDED_CURVE ( )  B_SPLINE_CURVE ( 2, ( #29306, #48622, #34145, #19036, #59237, #24824, #48936, #24506, #9699 ),
 .UNSPECIFIED., .F., .F. ) 
 B_SPLINE_CURVE_WITH_KNOTS ( ( 3, 2, 2, 2, 3 ),
 ( 0.6083333333333329485, 0.6124999999999997113, 0.6166666666666663632, 0.6208333333333330151, 0.6249999999999996669 ),
 .UNSPECIFIED. ) 
 CURVE ( )  GEOMETRIC_REPRESENTATION_ITEM ( )  RATIONAL_B_SPLINE_CURVE ( ( 1.000000000000005995, 0.9238795325112806323, 1.000000000000000000, 0.9238795325112867385, 1.000000000000000000, 0.9238795325112867385, 1.000000000000000000, 0.9238795325112928447, 0.9999999999999938938 ) ) 
 REPRESENTATION_ITEM ( '' )  );
#36807 = CARTESIAN_POINT ( 'NONE',  ( -5.000000000000000000, -109.9583333306021444, -2.886751345948128211 ) ) ;
#36808 = CARTESIAN_POINT ( 'NONE',  ( -4.458734124999999437, 8.604166668032261711, -2.574251347313719407 ) ) ;
#36809 = CARTESIAN_POINT ( 'NONE',  ( -4.458734124999999437, 21.68750000136559208, 0.000000000000000000 ) ) ;
#36810 = CARTESIAN_POINT ( 'NONE',  ( -51.60603307380591787, -150.9375000013656063, -2.891590998281053704 ) ) ;
#36811 = CARTESIAN_POINT ( 'NONE',  ( -58.80597590150559739, -150.1250000027312126, 3.242614290531460330 ) ) ;
#36812 = CARTESIAN_POINT ( 'NONE',  ( -6.972266317189433020E-16, -25.12499999726881228, -5.000000000000000000 ) ) ;
#36813 = ORIENTED_EDGE ( 'NONE', *, *, #98, .T. ) ;
#36814 = CARTESIAN_POINT ( 'NONE',  ( -4.458734124999997661, -73.22916666530106511, 2.574251347313722516 ) ) ;
#36815 = DIRECTION ( 'NONE',  ( -0.000000000000000000, 1.000000000000000000, -0.000000000000000000 ) ) ;
#36816 = CARTESIAN_POINT ( 'NONE',  ( -2.229367062500000163, 14.52083333469892779, -3.861377020970580443 ) ) ;
#36817 = EDGE_CURVE ( 'NONE', #25520, #7918, #37913, .T. ) ;
#36818 = CARTESIAN_POINT ( 'NONE',  ( -2.500000000000000444, -89.16666666666665719, -4.330127018922193649 ) ) ;
#36819 = CARTESIAN_POINT ( 'NONE',  ( -2.229367062499996610, -57.39583333196773651, 3.861377020970582219 ) ) ;
#36820 = CARTESIAN_POINT ( 'NONE',  ( -4.999999999999999112, -15.79166666393548191, 2.886751345948131764 ) ) ;
#36821 = CARTESIAN_POINT ( 'NONE',  ( 0.000000000000000000, -170.0000000000000000, 0.000000000000000000 ) ) ;
#36822 = DIRECTION ( 'NONE',  ( 0.000000000000000000, 0.000000000000000000, 1.000000000000000000 ) ) ;
#36823 = CARTESIAN_POINT ( 'NONE',  ( -1.339745962155613812, 18.79465819873852084, -5.000000000000000000 ) ) ;
#36824 = CARTESIAN_POINT ( 'NONE',  ( 4.458734124999999437, -34.81249999863440792, -5.460374474430324690E-16 ) ) ;
#36825 = CARTESIAN_POINT ( 'NONE',  ( -2.229367062499996610, -19.39583333196774007, 3.861377020970582219 ) ) ;
#36826 = EDGE_LOOP ( 'NONE', ( #46143, #23105, #53957, #16943 ) ) ;
#36827 = VECTOR ( 'NONE', #21622, 1000.000000000000000 ) ;
#36828 = DIRECTION ( 'NONE',  ( 0.8660254037844347108, 0.000000000000000000, -0.5000000000000069944 ) ) ;
#36829 = CARTESIAN_POINT ( 'NONE',  ( -5.000000000000000000, 30.00000000000000000, 0.000000000000000000 ) ) ;
#36830 = CARTESIAN_POINT ( 'NONE',  ( -2.071067811865475061, -157.8125000027311842, -5.000000000000000888 ) ) ;
#36831 = ORIENTED_EDGE ( 'NONE', *, *, #24835, .T. ) ;
#36832 = CARTESIAN_POINT ( 'NONE',  ( -4.458734124999999437, -102.6458333319677507, -2.574251347313719407 ) ) ;
#36833 = CARTESIAN_POINT ( 'NONE',  ( -2.229367062499996610, -24.14583333196773651, 3.861377020970582219 ) ) ;
#36834 = CARTESIAN_POINT ( 'NONE',  ( 2.499999999999998668, -60.20833333060214443, -4.330127018922193649 ) ) ;
#36835 = CARTESIAN_POINT ( 'NONE',  ( -52.80376928212989185, -152.1250000013656063, -4.297418129356379346 ) ) ;
#36836 = CARTESIAN_POINT ( 'NONE',  ( 3.535533905932738197, -146.8750000000000000, -3.535533905932738197 ) ) ;
#36837 = CARTESIAN_POINT ( 'NONE',  ( 4.458734124999998549, -26.72916666530106866, -2.574251347313721627 ) ) ;
#36838 = CARTESIAN_POINT ( 'NONE',  ( -4.458734124999997661, -68.47916666530107932, 2.574251347313722516 ) ) ;
#36839 = DIRECTION ( 'NONE',  ( 1.000000000000000000, 0.000000000000000000, -3.305092117221761110E-15 ) ) ;
#36840 = CARTESIAN_POINT ( 'NONE',  ( -4.458734124999999437, -25.31249999863440792, 0.000000000000000000 ) ) ;
#36841 = CARTESIAN_POINT ( 'NONE',  ( 0.000000000000000000, 0.000000000000000000, -11.00000000000000000 ) ) ;
#36842 = CARTESIAN_POINT ( 'NONE',  ( 2.071067811865475505, -151.8125000000000284, -5.000000000000000888 ) ) ;
#36843 = CARTESIAN_POINT ( 'NONE',  ( -5.000000000000000000, -15.08333333333333215, -2.886751345948128211 ) ) ;
#36844 = CARTESIAN_POINT ( 'NONE',  ( -3.152801135295367985, -152.8125000013656063, 3.152801135295367096 ) ) ;
#36845 = ORIENTED_EDGE ( 'NONE', *, *, #31305, .F. ) ;
#36846 = CARTESIAN_POINT ( 'NONE',  ( -6.972266317189433020E-16, -66.12499999726881583, -5.000000000000000000 ) ) ;
#36847 = CARTESIAN_POINT ( 'NONE',  ( -2.229367062500000163, -52.72916666530107221, -3.861377020970580443 ) ) ;
#36848 = CARTESIAN_POINT ( 'NONE',  ( 0.000000000000000000, -120.0000000000000000, 5.000000000000000000 ) ) ;
#36849 = DIRECTION ( 'NONE',  ( 0.000000000000000000, 0.000000000000000000, 1.000000000000000000 ) ) ;
#36850 = CARTESIAN_POINT ( 'NONE',  ( -2.500000000000000444, 22.83333333333333215, -4.330127018922193649 ) ) ;
#36851 = VECTOR ( 'NONE', #19147, 1000.000000000000000 ) ;
#36852 = LINE ( 'NONE', #31369, #8857 ) ;
#36853 = CARTESIAN_POINT ( 'NONE',  ( 4.458734124999998549, -1.729166665301068440, -2.574251347313721627 ) ) ;
#36854 = DIRECTION ( 'NONE',  ( 0.000000000000000000, 1.000000000000000000, 0.000000000000000000 ) ) ;
#36855 = FACE_OUTER_BOUND ( 'NONE', #1181, .T. ) ;
#36856 = CARTESIAN_POINT ( 'NONE',  ( 2.499999999999998668, -7.333333333333330373, -4.330127018922193649 ) ) ;
#36857 = CARTESIAN_POINT ( 'NONE',  ( 4.458734125000001214, 15.85416666803226171, 2.574251347313718519 ) ) ;
#36858 = CARTESIAN_POINT ( 'NONE',  ( 5.000000000000000000, 0.6250000027311873874, -6.123233995736766282E-16 ) ) ;
#36859 = VERTEX_POINT ( 'NONE', #40745 ) ;
#36860 = CARTESIAN_POINT ( 'NONE',  ( 4.648177544792955347E-16, 29.75000000000000355, -5.000000000000000000 ) ) ;
#36861 = ORIENTED_EDGE ( 'NONE', *, *, #18629, .T. ) ;
#36862 =( BOUNDED_CURVE ( )  B_SPLINE_CURVE ( 2, ( #33186, #58252, #4850, #43135, #62775, #57949, #33493, #19003, #53112 ),
 .UNSPECIFIED., .F., .F. ) 
 B_SPLINE_CURVE_WITH_KNOTS ( ( 3, 2, 2, 2, 3 ),
 ( 0.6187500000000000222, 0.6194444444444444642, 0.6208333333333333481, 0.6222222222222222321, 0.6229166666666666741 ),
 .UNSPECIFIED. ) 
 CURVE ( )  GEOMETRIC_REPRESENTATION_ITEM ( )  RATIONAL_B_SPLINE_CURVE ( ( 0.9330127018922194093, 0.9330127018922194093, 1.000000000000000000, 0.8660254037844387076, 1.000000000000000000, 0.8660254037844387076, 1.000000000000000000, 0.9330127018922194093, 0.9330127018922194093 ) ) 
 REPRESENTATION_ITEM ( '' )  );
#36863 = CARTESIAN_POINT ( 'NONE',  ( 9.457646018065525792E-16, -45.06249999863440792, 5.148502694627439702 ) ) ;
#36864 = CARTESIAN_POINT ( 'NONE',  ( -4.458734124999999437, -165.1875000013655779, -5.460374474430324690E-16 ) ) ;
#36865 = CARTESIAN_POINT ( 'NONE',  ( -5.000000000000000000, -44.95833333060215153, -2.886751345948128211 ) ) ;
#36866 = ORIENTED_EDGE ( 'NONE', *, *, #12950, .T. ) ;
#36867 = CARTESIAN_POINT ( 'NONE',  ( 9.457646018065525792E-16, -20.06249999863440081, 5.148502694627439702 ) ) ;
#36868 = ORIENTED_EDGE ( 'NONE', *, *, #41984, .F. ) ;
#36869 = CARTESIAN_POINT ( 'NONE',  ( -5.000000000000000000, -89.00000000000000000, 0.000000000000000000 ) ) ;
#36870 = CARTESIAN_POINT ( 'NONE',  ( 4.458734124999999437, -163.4375000013655779, 0.000000000000000000 ) ) ;
#36871 = CARTESIAN_POINT ( 'NONE',  ( 0.000000000000000000, -120.0000000000000000, 0.000000000000000000 ) ) ;
#36872 = CARTESIAN_POINT ( 'NONE',  ( -55.39835681537999790, -136.8750000000000284, 4.984105922594378235 ) ) ;
#36873 = VECTOR ( 'NONE', #49520, 1000.000000000000000 ) ;
#36874 = CARTESIAN_POINT ( 'NONE',  ( 9.457646018065525792E-16, -31.31249999863440436, 5.148502694627439702 ) ) ;
#36875 = CARTESIAN_POINT ( 'NONE',  ( -5.000000000000000888, -147.5625000027311842, 2.071067811865474617 ) ) ;
#36876 = ORIENTED_EDGE ( 'NONE', *, *, #14223, .T. ) ;
#36877 = CARTESIAN_POINT ( 'NONE',  ( 9.457646018065525792E-16, -76.06249999863440792, 5.148502694627439702 ) ) ;
#36878 = CARTESIAN_POINT ( 'NONE',  ( -2.229367062500000163, 22.52083333469892423, -3.861377020970580443 ) ) ;
#36879 = CARTESIAN_POINT ( 'NONE',  ( 5.000000000000000888, 24.54166666939784847, 2.886751345948126879 ) ) ;
#36880 = ORIENTED_EDGE ( 'NONE', *, *, #33048, .T. ) ;
#36881 = DIRECTION ( 'NONE',  ( 0.000000000000000000, 0.000000000000000000, 1.000000000000000000 ) ) ;
#36882 = CARTESIAN_POINT ( 'NONE',  ( -50.55543936806279248, -143.3125000013656063, 0.3552334253322060320 ) ) ;
#36883 = CARTESIAN_POINT ( 'NONE',  ( -4.458734124999998549, -78.47916666530107932, 2.574251347313722516 ) ) ;
#36884 = CARTESIAN_POINT ( 'NONE',  ( -59.81910112700025905, -131.3125000027312694, -2.462841084822630311 ) ) ;
#36885 = DIRECTION ( 'NONE',  ( 0.000000000000000000, 1.000000000000000000, 0.000000000000000000 ) ) ;
#36886 = CARTESIAN_POINT ( 'NONE',  ( 2.499999999999998668, -9.333333333333332149, -4.330127018922193649 ) ) ;
#36887 =( BOUNDED_CURVE ( )  B_SPLINE_CURVE ( 2, ( #54516, #10439, #30052, #9480, #29401, #49361, #44531, #173, #816 ),
 .UNSPECIFIED., .F., .F. ) 
 B_SPLINE_CURVE_WITH_KNOTS ( ( 3, 2, 2, 2, 3 ),
 ( 0.1604166666666666796, 0.1611111111111111216, 0.1625000000000000056, 0.1638888888888888895, 0.1645833333333333315 ),
 .UNSPECIFIED. ) 
 CURVE ( )  GEOMETRIC_REPRESENTATION_ITEM ( )  RATIONAL_B_SPLINE_CURVE ( ( 0.9330127018922194093, 0.9330127018922207416, 1.000000000000000000, 0.8660254037844387076, 1.000000000000000000, 0.8660254037844387076, 1.000000000000000000, 0.9330127018922194093, 0.9330127018922194093 ) ) 
 REPRESENTATION_ITEM ( '' )  );
#36888 = CARTESIAN_POINT ( 'NONE',  ( -6.972266317189433020E-16, 5.875000002731184168, -5.000000000000000000 ) ) ;
#36889 = CARTESIAN_POINT ( 'NONE',  ( -4.458734124999997661, -54.22916666530107221, 2.574251347313722516 ) ) ;
#36890 = CARTESIAN_POINT ( 'NONE',  ( 4.458734124999999437, -47.81249999863440792, -5.460374474430324690E-16 ) ) ;
#36891 = CARTESIAN_POINT ( 'NONE',  ( -2.500000000000000444, 20.83333333333333215, -4.330127018922193649 ) ) ;
#36892 = EDGE_CURVE ( 'NONE', #52029, #53780, #2992, .T. ) ;
#36893 = CARTESIAN_POINT ( 'NONE',  ( 5.000000000000000000, -107.4999999999999858, -6.123233995736766282E-16 ) ) ;
#36894 = CARTESIAN_POINT ( 'NONE',  ( -4.458734124999998549, -39.47916666530107932, 2.574251347313722516 ) ) ;
#36895 = CARTESIAN_POINT ( 'NONE',  ( -3.535250795749689387E-16, 3.875000002731186832, -5.773502691896257311 ) ) ;
#36896 = DIRECTION ( 'NONE',  ( -0.000000000000000000, 1.000000000000000000, -0.000000000000000000 ) ) ;
#36897 = DIRECTION ( 'NONE',  ( 0.000000000000000000, 0.000000000000000000, 1.000000000000000000 ) ) ;
#36898 = CARTESIAN_POINT ( 'NONE',  ( 4.458734124999998549, -79.97916666530107932, -2.574251347313721627 ) ) ;
#36899 = DIRECTION ( 'NONE',  ( -0.000000000000000000, 1.000000000000000000, -0.000000000000000000 ) ) ;
#36900 = CARTESIAN_POINT ( 'NONE',  ( -4.458734124999999437, -105.3124999986344221, 0.000000000000000000 ) ) ;
#36901 = CARTESIAN_POINT ( 'NONE',  ( -4.458734124999999437, -6.562499998634403475, 0.000000000000000000 ) ) ;
#36902 = ORIENTED_EDGE ( 'NONE', *, *, #1200, .T. ) ;
#36903 = CYLINDRICAL_SURFACE ( 'NONE', #6340, 5.000000000000000000 ) ;
#36904 = CARTESIAN_POINT ( 'NONE',  ( -3.152548672688508926E-16, -94.56249999863440792, -5.148502694627439702 ) ) ;
#36905 = CARTESIAN_POINT ( 'NONE',  ( 3.535533905932738197, -168.0000000027312126, -3.535533905932738197 ) ) ;
#36906 = CARTESIAN_POINT ( 'NONE',  ( 2.229367062499998831, -85.89583333196773651, -3.861377020970580887 ) ) ;
#36907 = CARTESIAN_POINT ( 'NONE',  ( 2.229367062500001939, 10.77083333469892956, 3.861377020970579999 ) ) ;
#36908 = DIRECTION ( 'NONE',  ( -0.000000000000000000, 1.000000000000000000, -0.000000000000000000 ) ) ;
#36909 = CARTESIAN_POINT ( 'NONE',  ( -50.70258187064364108, -132.1250000013656347, 2.196230717870141014 ) ) ;
#36910 = EDGE_CURVE ( 'NONE', #37124, #30399, #30787, .T. ) ;
#36911 = CARTESIAN_POINT ( 'NONE',  ( 2.229367062500001939, -7.979166665301073991, 3.861377020970579999 ) ) ;
#36912 = CARTESIAN_POINT ( 'NONE',  ( -2.229367062500000163, 17.27083333469892779, -3.861377020970580443 ) ) ;
#36913 = ADVANCED_FACE ( 'NONE', ( #16631 ), #55567, .T. ) ;
#36914 = CARTESIAN_POINT ( 'NONE',  ( 9.457646018065525792E-16, -55.31249999863439371, 5.148502694627439702 ) ) ;
#36915 = CARTESIAN_POINT ( 'NONE',  ( -9.184850993605147944E-16, -146.3750000027312126, 5.000000000000000000 ) ) ;
#36916 = CARTESIAN_POINT ( 'NONE',  ( 2.229367062499998831, -6.645833331967741842, -3.861377020970580887 ) ) ;
#36917 = CARTESIAN_POINT ( 'NONE',  ( -9.184850993605147944E-16, -142.2500000000000284, 5.000000000000000000 ) ) ;
#36918 = ORIENTED_EDGE ( 'NONE', *, *, #51676, .T. ) ;
#36919 = CARTESIAN_POINT ( 'NONE',  ( 4.458734125000000326, -35.14583333196772941, 2.574251347313718519 ) ) ;
#36920 = COLOUR_RGB ( '',0.8941176470588234615, 0.8941176470588234615, 0.8941176470588234615 ) ;
#36921 = CARTESIAN_POINT ( 'NONE',  ( -57.89159099828107458, -129.9375000013656063, -3.393966926194107447 ) ) ;
#36922 = CARTESIAN_POINT ( 'NONE',  ( 1.339745962155612702, 0.8303418039926664385, -5.000000000000000000 ) ) ;
#36923 = CARTESIAN_POINT ( 'NONE',  ( 2.229367062499998831, -82.64583333196773651, -3.861377020970580887 ) ) ;
#36924 = CARTESIAN_POINT ( 'NONE',  ( -2.229367062499996610, 25.60416666803225993, 3.861377020970582219 ) ) ;
#36925 = VECTOR ( 'NONE', #51417, 1000.000000000000000 ) ;
#36926 = EDGE_CURVE ( 'NONE', #30862, #26215, #26453, .T. ) ;
#36927 = CARTESIAN_POINT ( 'NONE',  ( -3.152801135295367096, -149.3125000013655779, -3.152801135295367541 ) ) ;
#36928 = CARTESIAN_POINT ( 'NONE',  ( 2.229367062500001939, 21.02083333469892779, 3.861377020970579999 ) ) ;
#36929 = CARTESIAN_POINT ( 'NONE',  ( -4.764381983412779477E-15, 27.25000000000000000, 5.000000000000000000 ) ) ;
#36930 = DIRECTION ( 'NONE',  ( 0.000000000000000000, 0.000000000000000000, 1.000000000000000000 ) ) ;
#36931 = CARTESIAN_POINT ( 'NONE',  ( 4.458734124999999437, -82.06249999863440792, -5.460374474430324690E-16 ) ) ;
#36932 = CARTESIAN_POINT ( 'NONE',  ( -2.499999999999996447, -62.83333333333333570, 4.330127018922195425 ) ) ;
#36933 = CARTESIAN_POINT ( 'NONE',  ( 1.339745962155615144, -72.58034179853027013, 4.999999999999999112 ) ) ;
#36934 = CARTESIAN_POINT ( 'NONE',  ( -3.535250795749689387E-16, 19.87500000273118417, -5.773502691896257311 ) ) ;
#36935 = VERTEX_POINT ( 'NONE', #46853 ) ;
#36936 = CARTESIAN_POINT ( 'NONE',  ( 5.000000000000000000, -35.41666666666666430, -2.886751345948130876 ) ) ;
#36937 = CARTESIAN_POINT ( 'NONE',  ( -59.81910112700027327, -139.3125000027312126, -2.462841084822392279 ) ) ;
#36939 = CARTESIAN_POINT ( 'NONE',  ( 5.000000000000000000, -21.50000000000000000, -6.123233995736766282E-16 ) ) ;
#36938 = CARTESIAN_POINT ( 'NONE',  ( -4.999999999999998224, -71.91666666666667140, 2.886751345948131764 ) ) ;
#36940 = CARTESIAN_POINT ( 'NONE',  ( 4.458734124999998549, -29.72916666530107221, -2.574251347313721627 ) ) ;
#36941 = CARTESIAN_POINT ( 'NONE',  ( -4.458734124999997661, -89.22916666530107932, 2.574251347313722516 ) ) ;
#36942 = CARTESIAN_POINT ( 'NONE',  ( 5.000000000000000000, -28.29166666393548013, -2.886751345948129988 ) ) ;
#36943 = EDGE_CURVE ( 'NONE', #17113, #54593, #62157, .T. ) ;
#36945 = EDGE_LOOP ( 'NONE', ( #37169, #37894, #1838, #59159 ) ) ;
#36944 = CARTESIAN_POINT ( 'NONE',  ( 4.458734124999999437, -56.81249999863440081, -5.460374474430324690E-16 ) ) ;
#36947 = ORIENTED_EDGE ( 'NONE', *, *, #1296, .T. ) ;
#36946 = CARTESIAN_POINT ( 'NONE',  ( 4.458734124999999437, -8.062499998634404363, -5.460374474430324690E-16 ) ) ;
#36948 = CARTESIAN_POINT ( 'NONE',  ( 5.000000000000000888, -73.58333333333334281, 2.886751345948126879 ) ) ;
#36949 = CARTESIAN_POINT ( 'NONE',  ( -58.39396692619412477, -139.4375000013656063, 2.891590998281057701 ) ) ;
#36950 = CARTESIAN_POINT ( 'NONE',  ( 9.457646018065525792E-16, -50.31249999863440792, 5.148502694627439702 ) ) ;
#36951 = CARTESIAN_POINT ( 'NONE',  ( 5.000000000000000000, -76.29166666393547303, -2.886751345948129988 ) ) ;
#36953 = ORIENTED_EDGE ( 'NONE', *, *, #34641, .F. ) ;
#36952 = CARTESIAN_POINT ( 'NONE',  ( -4.999999999999998224, -53.79166666393548013, 2.886751345948131764 ) ) ;
#36954 = CARTESIAN_POINT ( 'NONE',  ( -49.85088928181150436, -148.5625000000000000, -1.666127454062680702 ) ) ;
#36955 = CARTESIAN_POINT ( 'NONE',  ( -2.229367062499996610, -14.39583333196774184, 3.861377020970582219 ) ) ;
#36956 = CARTESIAN_POINT ( 'NONE',  ( 4.458734124999998549, -57.97916666530107221, -2.574251347313721627 ) ) ;
#36957 = CARTESIAN_POINT ( 'NONE',  ( 2.499999999999998668, 22.66666666666666430, -4.330127018922193649 ) ) ;
#36958 = CARTESIAN_POINT ( 'NONE',  ( -1.846868145590737420, -139.7500000013655779, 4.458734124999999437 ) ) ;
#36959 = CARTESIAN_POINT ( 'NONE',  ( 2.229367062499998831, -98.89583333196773651, -3.861377020970580887 ) ) ;
#36960 = CARTESIAN_POINT ( 'NONE',  ( 0.000000000000000000, -120.0000000000000000, 0.000000000000000000 ) ) ;
#36961 = ORIENTED_EDGE ( 'NONE', *, *, #21760, .F. ) ;
#36962 = DIRECTION ( 'NONE',  ( -0.000000000000000000, 1.000000000000000000, -0.000000000000000000 ) ) ;
#36963 = CARTESIAN_POINT ( 'NONE',  ( -58.80597590150559739, -143.1250000027312126, 3.242614290531460330 ) ) ;
#36964 = CARTESIAN_POINT ( 'NONE',  ( -3.152548672688508926E-16, -0.8124999986344055847, -5.148502694627439702 ) ) ;
#36965 = CARTESIAN_POINT ( 'NONE',  ( 1.975475456537005874E-15, -12.62499999726881050, 5.000000000000000000 ) ) ;
#36966 = VECTOR ( 'NONE', #3945, 1000.000000000000000 ) ;
#36967 = EDGE_CURVE ( 'NONE', #56591, #47541, #45897, .T. ) ;
#36968 = CARTESIAN_POINT ( 'NONE',  ( -4.458734124999999437, -6.312499998634403475, 0.000000000000000000 ) ) ;
#36969 = CARTESIAN_POINT ( 'NONE',  ( -3.152548672688508926E-16, -94.81249999863439371, -5.148502694627439702 ) ) ;
#36970 = EDGE_CURVE ( 'NONE', #41833, #42072, #46563, .T. ) ;
#36971 = EDGE_CURVE ( 'NONE', #17887, #50557, #13301, .T. ) ;
#36972 = CARTESIAN_POINT ( 'NONE',  ( 1.846868145590735200, -147.5000000013656063, -4.458734125000000326 ) ) ;
#36973 = CARTESIAN_POINT ( 'NONE',  ( 2.229367062499998831, -21.89583333196774007, -3.861377020970580887 ) ) ;
#36974 = CARTESIAN_POINT ( 'NONE',  ( 0.000000000000000000, -170.0000000000000000, 5.000000000000000000 ) ) ;
#36975 = CARTESIAN_POINT ( 'NONE',  ( -56.48576386720575471, -137.7500000013656063, -4.591703134518078322 ) ) ;
#36976 = CARTESIAN_POINT ( 'NONE',  ( 4.458734124999998549, -60.97916666530106511, -2.574251347313721627 ) ) ;
#36977 = CARTESIAN_POINT ( 'NONE',  ( -6.972266317189433020E-16, -84.12499999726880162, -5.000000000000000000 ) ) ;
#36978 = CARTESIAN_POINT ( 'NONE',  ( -0.2779000157839473517, -8.820699686765063774, -7.928862157988305626 ) ) ;
#36979 = CARTESIAN_POINT ( 'NONE',  ( 2.730187237215162345E-16, -143.1875000013656063, -4.458734124999999437 ) ) ;
#36980 = CARTESIAN_POINT ( 'NONE',  ( 2.229367062500001939, 12.77083333469892779, 3.861377020970579999 ) ) ;
#36981 = EDGE_LOOP ( 'NONE', ( #60863, #25796, #16602, #63214 ) ) ;
#36982 = CARTESIAN_POINT ( 'NONE',  ( -5.000000000000000000, -4.999999999999997335, 0.000000000000000000 ) ) ;
#36983 = FACE_OUTER_BOUND ( 'NONE', #15418, .T. ) ;
#36985 = CARTESIAN_POINT ( 'NONE',  ( 2.229367062500001939, -24.97916666530106866, 3.861377020970579999 ) ) ;
#36984 = CARTESIAN_POINT ( 'NONE',  ( 5.000000000000000888, -92.58333333333332860, 2.886751345948126879 ) ) ;
#36986 = CARTESIAN_POINT ( 'NONE',  ( -7.500000000000000000, 4.330127018922191873, -7.422398894150032511 ) ) ;
#36987 = CARTESIAN_POINT ( 'NONE',  ( 9.457646018065525792E-16, -72.31249999863440792, 5.148502694627439702 ) ) ;
#36988 = CARTESIAN_POINT ( 'NONE',  ( 0.000000000000000000, -170.0000000000000000, 0.000000000000000000 ) ) ;
#36989 = DIRECTION ( 'NONE',  ( -0.000000000000000000, 1.000000000000000000, -0.000000000000000000 ) ) ;
#36990 =( BOUNDED_CURVE ( )  B_SPLINE_CURVE ( 2, ( #42974, #57784, #9499, #13704, #33326, #8881, #9809, #4066, #23685 ),
 .UNSPECIFIED., .F., .F. ) 
 B_SPLINE_CURVE_WITH_KNOTS ( ( 3, 2, 2, 2, 3 ),
 ( 0.7562499999999999778, 0.7569444444444444198, 0.7583333333333333037, 0.7597222222222221877, 0.7604166666666666297 ),
 .UNSPECIFIED. ) 
 CURVE ( )  GEOMETRIC_REPRESENTATION_ITEM ( )  RATIONAL_B_SPLINE_CURVE ( ( 0.9330127018922194093, 0.9330127018922194093, 1.000000000000000000, 0.8660254037844387076, 1.000000000000000000, 0.8660254037844387076, 1.000000000000000000, 0.9330127018922194093, 0.9330127018922194093 ) ) 
 REPRESENTATION_ITEM ( '' )  );
#36991 = CARTESIAN_POINT ( 'NONE',  ( -56.48576386720575471, -146.7500000013655495, -4.591703134518078322 ) ) ;
#36992 = CARTESIAN_POINT ( 'NONE',  ( 2.500000000000002220, -52.54166666393548013, 4.330127018922192761 ) ) ;
#36993 = CARTESIAN_POINT ( 'NONE',  ( -9.184850993605147944E-16, -150.3750000027312126, 5.000000000000000000 ) ) ;
#36994 = CARTESIAN_POINT ( 'NONE',  ( 9.457646018065525792E-16, 8.937500001365595637, 5.148502694627439702 ) ) ;
#36995 = CARTESIAN_POINT ( 'NONE',  ( 0.000000000000000000, -170.0000000000000000, 5.000000000000000000 ) ) ;
#36996 = EDGE_CURVE ( 'NONE', #34626, #29404, #7115, .T. ) ;
#36997 = CARTESIAN_POINT ( 'NONE',  ( -1.339745962155610925, -14.79465819873851729, 5.000000000000000000 ) ) ;
#36998 = CARTESIAN_POINT ( 'NONE',  ( 4.458734124999998549, 5.270833334698926897, -2.574251347313721627 ) ) ;
#36999 = CARTESIAN_POINT ( 'NONE',  ( -4.458734124999998549, -73.22916666530106511, 2.574251347313722516 ) ) ;
#37000 = CARTESIAN_POINT ( 'NONE',  ( -4.458734124999999437, -17.56249999863440792, 0.000000000000000000 ) ) ;
#37001 = CARTESIAN_POINT ( 'NONE',  ( -2.500000000000000444, 1.833333333333332593, -4.330127018922193649 ) ) ;
#37002 = CARTESIAN_POINT ( 'NONE',  ( 3.152801135295367541, -160.3125000013656063, -3.152801135295367541 ) ) ;
#37003 = CARTESIAN_POINT ( 'NONE',  ( -6.972266317189433020E-16, -109.2499999999999858, -5.000000000000000000 ) ) ;
#37004 = CARTESIAN_POINT ( 'NONE',  ( -4.458734124999999437, -65.39583333196773651, -2.574251347313719407 ) ) ;
#37005 = CARTESIAN_POINT ( 'NONE',  ( 2.499999999999998668, -101.2083333306021444, -4.330127018922193649 ) ) ;
#37006 = CARTESIAN_POINT ( 'NONE',  ( -4.458734124999999437, -41.39583333196773651, -2.574251347313719407 ) ) ;
#37007 = LINE ( 'NONE', #56636, #52349 ) ;
#37008 = CARTESIAN_POINT ( 'NONE',  ( -3.152548672688508926E-16, -68.81249999863439371, -5.148502694627439702 ) ) ;
#37009 = CARTESIAN_POINT ( 'NONE',  ( 2.499999999999998668, -50.33333333333332860, -4.330127018922193649 ) ) ;
#37010 = CARTESIAN_POINT ( 'NONE',  ( -6.972266317189433020E-16, 9.750000000000000000, -5.000000000000000000 ) ) ;
#37011 = CARTESIAN_POINT ( 'NONE',  ( 5.000000000000000888, -152.0625000027312410, -2.071067811865475505 ) ) ;
#37012 = EDGE_LOOP ( 'NONE', ( #21242, #52047, #8845, #13429 ) ) ;
#37013 = CARTESIAN_POINT ( 'NONE',  ( -6.972266317189433020E-16, -85.25000000000000000, -5.000000000000000000 ) ) ;
#37014 = AXIS2_PLACEMENT_3D ( 'NONE', #44220, #19785, #39393 ) ;
#37015 = CARTESIAN_POINT ( 'NONE',  ( 3.535533905932736864, -144.2500000027311842, 3.535533905932738641 ) ) ;
#37016 = CARTESIAN_POINT ( 'NONE',  ( -5.000000000000000000, -8.000000000000000000, 0.000000000000000000 ) ) ;
#37017 = AXIS2_PLACEMENT_3D ( 'NONE', #769, #54472, #15554 ) ;
#37018 = CARTESIAN_POINT ( 'NONE',  ( 4.458734125000000326, -69.89583333196773651, 2.574251347313718519 ) ) ;
#37019 = CARTESIAN_POINT ( 'NONE',  ( -1.339745962155610925, -30.66965819600732956, 5.000000000000000000 ) ) ;
#37020 = CARTESIAN_POINT ( 'NONE',  ( 2.500000000000002220, -15.54166666393548191, 4.330127018922192761 ) ) ;
#37022 = EDGE_LOOP ( 'NONE', ( #48644, #17661, #32920, #21024 ) ) ;
#37021 = CARTESIAN_POINT ( 'NONE',  ( 4.458734124999998549, -38.72916666530106511, -2.574251347313721627 ) ) ;
#37023 = CARTESIAN_POINT ( 'NONE',  ( 0.000000000000000000, -170.0000000000000000, 0.000000000000000000 ) ) ;
#37025 = VERTEX_POINT ( 'NONE', #22419 ) ;
#37024 = CARTESIAN_POINT ( 'NONE',  ( -4.458734124999999437, 5.437500001365592972, 0.000000000000000000 ) ) ;
#37026 = CARTESIAN_POINT ( 'NONE',  ( -9.184850993605147944E-16, -151.2500000000000284, 5.000000000000000000 ) ) ;
#37027 = CARTESIAN_POINT ( 'NONE',  ( 2.500000000000002220, -57.66666666666667140, 4.330127018922192761 ) ) ;
#37028 = CARTESIAN_POINT ( 'NONE',  ( -1.846868145590734756, -160.3750000013656063, -4.458734125000000326 ) ) ;
#37029 = CARTESIAN_POINT ( 'NONE',  ( 2.229367062499998831, -34.89583333196772941, -3.861377020970580887 ) ) ;
#37030 = FACE_OUTER_BOUND ( 'NONE', #5784, .T. ) ;
#37031 = CARTESIAN_POINT ( 'NONE',  ( 9.457646018065525792E-16, -82.06249999863442213, 5.148502694627439702 ) ) ;
#37032 = CARTESIAN_POINT ( 'NONE',  ( 2.071067811865475505, -164.8124999999999716, -5.000000000000000888 ) ) ;
#37033 = CARTESIAN_POINT ( 'NONE',  ( -2.229367062500000163, -87.47916666530107932, -3.861377020970580443 ) ) ;
#37034 = CARTESIAN_POINT ( 'NONE',  ( -52.10840900171896806, -130.4375000013656063, 3.393966926194110556 ) ) ;
#37035 = CARTESIAN_POINT ( 'NONE',  ( 9.457646018065525792E-16, 1.687500001365593194, 5.148502694627439702 ) ) ;
#37036 = CARTESIAN_POINT ( 'NONE',  ( 2.229367062499998831, -35.89583333196773651, -3.861377020970580887 ) ) ;
#37037 = DIRECTION ( 'NONE',  ( -0.000000000000000000, 1.000000000000000000, -0.000000000000000000 ) ) ;
#37038 = CARTESIAN_POINT ( 'NONE',  ( -4.458734124999999437, -81.56249999863440792, 0.000000000000000000 ) ) ;
#37039 = CARTESIAN_POINT ( 'NONE',  ( -6.031010364368858512E-14, 3.249999999999997335, 5.000000000000000000 ) ) ;
#37040 =( BOUNDED_CURVE ( )  B_SPLINE_CURVE ( 2, ( #26419, #16769, #31877, #41837, #61482, #51817, #7759, #13208, #58532 ),
 .UNSPECIFIED., .F., .F. ) 
 B_SPLINE_CURVE_WITH_KNOTS ( ( 3, 2, 2, 2, 3 ),
 ( 0.2874999999999999778, 0.2880952380952380709, 0.2892857142857143127, 0.2904761904761904989, 0.2910714285714285920 ),
 .UNSPECIFIED. ) 
 CURVE ( )  GEOMETRIC_REPRESENTATION_ITEM ( )  RATIONAL_B_SPLINE_CURVE ( ( 0.9330127018922194093, 0.9330127018922194093, 1.000000000000000000, 0.8660254037844387076, 1.000000000000000000, 0.8660254037844387076, 1.000000000000000000, 0.9330127018922194093, 0.9330127018922194093 ) ) 
 REPRESENTATION_ITEM ( '' )  );
#37041 = EDGE_LOOP ( 'NONE', ( #9722, #39689, #11942, #19273 ) ) ;
#37042 = CARTESIAN_POINT ( 'NONE',  ( -5.000000000000000000, -94.95833333060213022, -2.886751345948128211 ) ) ;
#37043 =( BOUNDED_CURVE ( )  B_SPLINE_CURVE ( 2, ( #27904, #56880, #52050, #47525, #62336, #18257, #2532, #23089, #7988 ),
 .UNSPECIFIED., .F., .F. ) 
 B_SPLINE_CURVE_WITH_KNOTS ( ( 3, 2, 2, 2, 3 ),
 ( 0.6854166666666666741, 0.6861111111111111160, 0.6875000000000000000, 0.6888888888888888840, 0.6895833333333333259 ),
 .UNSPECIFIED. ) 
 CURVE ( )  GEOMETRIC_REPRESENTATION_ITEM ( )  RATIONAL_B_SPLINE_CURVE ( ( 0.9330127018922194093, 0.9330127018922194093, 1.000000000000000000, 0.8660254037844387076, 1.000000000000000000, 0.8660254037844387076, 1.000000000000000000, 0.9330127018922194093, 0.9330127018922194093 ) ) 
 REPRESENTATION_ITEM ( '' )  );
#37044 = CARTESIAN_POINT ( 'NONE',  ( -4.458734124999999437, -71.56249999863439371, 0.000000000000000000 ) ) ;
#37045 = CARTESIAN_POINT ( 'NONE',  ( 9.457646018065525792E-16, -8.312499998634406140, 5.148502694627439702 ) ) ;
#37046 = ORIENTED_EDGE ( 'NONE', *, *, #57810, .F. ) ;
#37047 = CARTESIAN_POINT ( 'NONE',  ( -2.071067811865348496, -150.8125000027311842, -5.000000000000127898 ) ) ;
#37048 = EDGE_CURVE ( 'NONE', #62346, #36859, #19859, .T. ) ;
#37049 = CARTESIAN_POINT ( 'NONE',  ( -6.972266317189433020E-16, -3.124999997268813612, -5.000000000000000000 ) ) ;
#37050 = CARTESIAN_POINT ( 'NONE',  ( -4.458734124999999437, -4.562499998634401699, 0.000000000000000000 ) ) ;
#37051 = CARTESIAN_POINT ( 'NONE',  ( -5.147856630858197489E-14, 3.249999999999997335, 5.000000000000000000 ) ) ;
#37052 = CARTESIAN_POINT ( 'NONE',  ( 2.229367062500001939, 3.020833334698928674, 3.861377020970579999 ) ) ;
#37053 = AXIS2_PLACEMENT_3D ( 'NONE', #35651, #63410, #45614 ) ;
#37054 = CARTESIAN_POINT ( 'NONE',  ( -4.999999999999998224, -32.79166666393547303, 2.886751345948131764 ) ) ;
#37055 = CARTESIAN_POINT ( 'NONE',  ( 1.846868145590735200, -158.2500000013656063, -4.458734124999999437 ) ) ;
#37056 = EDGE_CURVE ( 'NONE', #9299, #17113, #37534, .T. ) ;
#37057 = CARTESIAN_POINT ( 'NONE',  ( 4.458734125000000326, 28.85416666803226704, 2.574251347313718519 ) ) ;
#37058 = EDGE_LOOP ( 'NONE', ( #40597, #10505, #2401, #29303 ) ) ;
#37059 = CARTESIAN_POINT ( 'NONE',  ( -4.458734124999999437, -87.31249999863439371, 0.000000000000000000 ) ) ;
#37060 = CARTESIAN_POINT ( 'NONE',  ( -1.339745962155613812, -78.20534180126146850, -5.000000000000000000 ) ) ;
#37061 = CARTESIAN_POINT ( 'NONE',  ( -4.458734124999999437, -6.395833331967740953, -2.574251347313719407 ) ) ;
#37062 = AXIS2_PLACEMENT_3D ( 'NONE', #30261, #49883, #50853 ) ;
#37063 = EDGE_CURVE ( 'NONE', #35844, #41033, #44089, .T. ) ;
#37065 = EDGE_CURVE ( 'NONE', #14611, #34762, #42017, .T. ) ;
#37064 = CARTESIAN_POINT ( 'NONE',  ( 0.000000000000000000, -170.0000000000000000, 0.000000000000000000 ) ) ;
#37066 = FACE_OUTER_BOUND ( 'NONE', #3580, .T. ) ;
#37067 = DIRECTION ( 'NONE',  ( 0.000000000000000000, 0.000000000000000000, 1.000000000000000000 ) ) ;
#37068 = CARTESIAN_POINT ( 'NONE',  ( -2.499999999999996447, -37.70833333060213732, 4.330127018922195425 ) ) ;
#37069 = CARTESIAN_POINT ( 'NONE',  ( 0.000000000000000000, -170.0000000000000000, 0.000000000000000000 ) ) ;
#37070 = CARTESIAN_POINT ( 'NONE',  ( 2.229367062500001939, 27.02083333469892423, 3.861377020970579999 ) ) ;
#37071 = CARTESIAN_POINT ( 'NONE',  ( 1.339745962155661996, -10.29465819873852261, -4.999999999999970690 ) ) ;
#37072 =( BOUNDED_CURVE ( )  B_SPLINE_CURVE ( 2, ( #49244, #44408, #21252, #20299, #368, #55030, #19971, #39581, #15792 ),
 .UNSPECIFIED., .F., .F. ) 
 B_SPLINE_CURVE_WITH_KNOTS ( ( 3, 2, 2, 2, 3 ),
 ( 0.06250000000000000000, 0.06309523809523809312, 0.06428571428571427937, 0.06547619047619047949, 0.06607142857142857262 ),
 .UNSPECIFIED. ) 
 CURVE ( )  GEOMETRIC_REPRESENTATION_ITEM ( )  RATIONAL_B_SPLINE_CURVE ( ( 0.9330127018922194093, 0.9330127018922194093, 1.000000000000000000, 0.8660254037844387076, 1.000000000000000000, 0.8660254037844387076, 1.000000000000000000, 0.9330127018922194093, 0.9330127018922194093 ) ) 
 REPRESENTATION_ITEM ( '' )  );
#37073 = CARTESIAN_POINT ( 'NONE',  ( -4.458734124999999437, 23.60416666803225993, -2.574251347313719407 ) ) ;
#37074 = EDGE_CURVE ( 'NONE', #21757, #16025, #57280, .T. ) ;
#37075 = CARTESIAN_POINT ( 'NONE',  ( -3.152548672688508926E-16, -54.56249999863439371, -5.148502694627439702 ) ) ;
#37076 = CARTESIAN_POINT ( 'NONE',  ( 4.458734124999999437, -2.062499998634406584, -5.460374474430324690E-16 ) ) ;
#37077 = CARTESIAN_POINT ( 'NONE',  ( -9.184850993605147944E-16, -161.3750000027311842, 5.000000000000000000 ) ) ;
#37078 = CARTESIAN_POINT ( 'NONE',  ( -2.500000000000000444, 16.83333333333333215, -4.330127018922193649 ) ) ;
#37079 = EDGE_CURVE ( 'NONE', #58923, #36394, #24931, .T. ) ;
#37080 = CARTESIAN_POINT ( 'NONE',  ( 2.071067811865476394, -141.3125000027312126, 5.000000000000000000 ) ) ;
#37081 = CARTESIAN_POINT ( 'NONE',  ( -4.999999999999998224, -51.91666666666666430, 2.886751345948131764 ) ) ;
#37082 = CARTESIAN_POINT ( 'NONE',  ( 2.229367062499998831, -45.64583333196774362, -3.861377020970580887 ) ) ;
#37083 = CARTESIAN_POINT ( 'NONE',  ( -3.535250795749689387E-16, -80.12499999726880162, -5.773502691896257311 ) ) ;
#37084 = CARTESIAN_POINT ( 'NONE',  ( -53.51423613279429503, -139.5000000013656063, 4.591703134518082763 ) ) ;
#37085 = DIRECTION ( 'NONE',  ( -0.000000000000000000, 1.000000000000000000, -0.000000000000000000 ) ) ;
#37086 = EDGE_CURVE ( 'NONE', #10357, #26556, #44539, .T. ) ;
#37087 = CARTESIAN_POINT ( 'NONE',  ( 5.000000000000000888, 3.416666666666665186, 2.886751345948126879 ) ) ;
#37088 = CARTESIAN_POINT ( 'NONE',  ( 4.458734124999998549, -87.97916666530107932, -2.574251347313721627 ) ) ;
#37089 = CARTESIAN_POINT ( 'NONE',  ( 2.730187237215162345E-16, -159.4375000013655779, -4.458734124999999437 ) ) ;
#37090 = CARTESIAN_POINT ( 'NONE',  ( 5.000000000000000000, -32.50000000000000000, -6.123233995736766282E-16 ) ) ;
#37091 = ORIENTED_EDGE ( 'NONE', *, *, #44530, .F. ) ;
#37092 = CARTESIAN_POINT ( 'NONE',  ( -2.229367062500000163, 15.27083333469892779, -3.861377020970580443 ) ) ;
#37093 = ORIENTED_EDGE ( 'NONE', *, *, #61227, .T. ) ;
#37094 = CARTESIAN_POINT ( 'NONE',  ( -2.229367062500000163, -94.47916666530106511, -3.861377020970580443 ) ) ;
#37095 = CARTESIAN_POINT ( 'NONE',  ( 9.457646018065525792E-16, 15.68750000136559386, 5.148502694627439702 ) ) ;
#37096 = CARTESIAN_POINT ( 'NONE',  ( 2.500000000000002220, 15.45833333606451987, 4.330127018922192761 ) ) ;
#37097 =( BOUNDED_CURVE ( )  B_SPLINE_CURVE ( 2, ( #36557, #45573, #60704, #6661, #56188, #51365, #16624, #26268, #30781 ),
 .UNSPECIFIED., .F., .T. ) 
 B_SPLINE_CURVE_WITH_KNOTS ( ( 3, 2, 2, 2, 3 ),
 ( 0.2750000000000002442, 0.2791666666666668961, 0.2833333333333335480, 0.2875000000000001998, 0.2916666666666669072 ),
 .UNSPECIFIED. ) 
 CURVE ( )  GEOMETRIC_REPRESENTATION_ITEM ( )  RATIONAL_B_SPLINE_CURVE ( ( 0.9999999999999958922, 0.9238795325112908463, 1.000000000000000000, 0.9238795325112867385, 1.000000000000000000, 0.9238795325112867385, 1.000000000000000000, 0.9238795325112826307, 1.000000000000003997 ) ) 
 REPRESENTATION_ITEM ( '' )  );
#37098 = CARTESIAN_POINT ( 'NONE',  ( 1.975475456537005874E-15, -16.74999999999999645, 5.000000000000000000 ) ) ;
#37099 = CARTESIAN_POINT ( 'NONE',  ( -5.000000000000000000, 5.999999999999998224, 0.000000000000000000 ) ) ;
#37100 = CARTESIAN_POINT ( 'NONE',  ( 4.458734125000000326, -55.89583333196773651, 2.574251347313718519 ) ) ;
#37101 = CARTESIAN_POINT ( 'NONE',  ( -1.339745962155613812, -53.08034179853029144, -5.000000000000000000 ) ) ;
#37102 = CARTESIAN_POINT ( 'NONE',  ( 5.000000000000000000, -80.41666666666667140, -2.886751345948129988 ) ) ;
#37103 = CYLINDRICAL_SURFACE ( 'NONE', #7777, 5.000000000000000000 ) ;
#37104 = DIRECTION ( 'NONE',  ( 0.000000000000000000, 0.000000000000000000, 1.000000000000000000 ) ) ;
#37105 = CARTESIAN_POINT ( 'NONE',  ( -5.000000000000000000, -25.87499999726881583, 0.000000000000000000 ) ) ;
#37106 = DIRECTION ( 'NONE',  ( 0.000000000000000000, 0.000000000000000000, 1.000000000000000000 ) ) ;
#37107 = CARTESIAN_POINT ( 'NONE',  ( -5.000000000000000000, -37.99999999999999289, 0.000000000000000000 ) ) ;
#37108 = CARTESIAN_POINT ( 'NONE',  ( 2.500000000000002220, -96.66666666666665719, 4.330127018922192761 ) ) ;
#37110 = CARTESIAN_POINT ( 'NONE',  ( -4.458734124999999437, -17.56249999863440792, 0.000000000000000000 ) ) ;
#37109 = CARTESIAN_POINT ( 'NONE',  ( -5.000000000000000000, 13.99999999999999822, 0.000000000000000000 ) ) ;
#37111 = CARTESIAN_POINT ( 'NONE',  ( -1.339745962155610925, 13.20534180126147916, 5.000000000000000000 ) ) ;
#37112 = CARTESIAN_POINT ( 'NONE',  ( 2.229367062499998831, -65.64583333196773651, -3.861377020970580887 ) ) ;
#37113 = CARTESIAN_POINT ( 'NONE',  ( 4.458734124999999437, -149.6875000013656063, 0.000000000000000000 ) ) ;
#37114 = AXIS2_PLACEMENT_3D ( 'NONE', #7319, #50729, #6673 ) ;
#37115 = CARTESIAN_POINT ( 'NONE',  ( -4.458734124999999437, -70.31249999863439371, 0.000000000000000000 ) ) ;
#37116 = CARTESIAN_POINT ( 'NONE',  ( -53.51423613279429503, -144.5000000013656063, 4.591703134518082763 ) ) ;
#37117 = CARTESIAN_POINT ( 'NONE',  ( 2.229367062499998831, -19.89583333196774007, -3.861377020970580887 ) ) ;
#37118 = CARTESIAN_POINT ( 'NONE',  ( -5.000000000000000000, -59.87499999726880873, 0.000000000000000000 ) ) ;
#37119 = ORIENTED_EDGE ( 'NONE', *, *, #4672, .T. ) ;
#37120 = DIRECTION ( 'NONE',  ( -0.000000000000000000, 1.000000000000000000, -0.000000000000000000 ) ) ;
#37121 = ORIENTED_EDGE ( 'NONE', *, *, #11984, .F. ) ;
#37122 = CARTESIAN_POINT ( 'NONE',  ( -3.152548672688508926E-16, -66.81249999863442213, -5.148502694627439702 ) ) ;
#37123 = CARTESIAN_POINT ( 'NONE',  ( 0.000000000000000000, -170.0000000000000000, 0.000000000000000000 ) ) ;
#37124 = VERTEX_POINT ( 'NONE', #48725 ) ;
#37125 = CARTESIAN_POINT ( 'NONE',  ( -2.500000000000000444, -47.16666666666666430, -4.330127018922193649 ) ) ;
#37126 = LINE ( 'NONE', #17176, #60074 ) ;
#37127 = DIRECTION ( 'NONE',  ( -7.709882115452477180E-16, 0.000000000000000000, -1.000000000000000000 ) ) ;
#37128 = CARTESIAN_POINT ( 'NONE',  ( 2.229367062500001939, -55.22916666530107221, 3.861377020970579999 ) ) ;
#37129 = AXIS2_PLACEMENT_3D ( 'NONE', #5151, #43117, #18677 ) ;
#37130 = ORIENTED_EDGE ( 'NONE', *, *, #51074, .T. ) ;
#37131 = LINE ( 'NONE', #56750, #39833 ) ;
#37132 = CARTESIAN_POINT ( 'NONE',  ( 4.458734124999998549, 6.270833334698928674, -2.574251347313721627 ) ) ;
#37133 = CARTESIAN_POINT ( 'NONE',  ( 2.229367062500001939, 16.02083333469892779, 3.861377020970579999 ) ) ;
#37134 = CARTESIAN_POINT ( 'NONE',  ( -55.35523342533222291, -147.3125000013656063, 4.444560631937231499 ) ) ;
#37135 = CARTESIAN_POINT ( 'NONE',  ( -60.14911071818854538, -150.1875000027312126, 1.666127454062681146 ) ) ;
#37136 = CARTESIAN_POINT ( 'NONE',  ( 4.458734124999999437, -167.4375000013655779, 0.000000000000000000 ) ) ;
#37137 = VERTEX_POINT ( 'NONE', #4988 ) ;
#37138 = CARTESIAN_POINT ( 'NONE',  ( 9.457646018065525792E-16, -68.06249999863440792, 5.148502694627439702 ) ) ;
#37139 = CARTESIAN_POINT ( 'NONE',  ( -5.000000000000000000, -85.87499999726880162, 0.000000000000000000 ) ) ;
#37140 = CARTESIAN_POINT ( 'NONE',  ( -2.229367062500000163, 5.520833334698927786, -3.861377020970580443 ) ) ;
#37141 = CARTESIAN_POINT ( 'NONE',  ( -1.339745962155497683, -42.20534180126147561, -5.000000000000066613 ) ) ;
#37142 = CARTESIAN_POINT ( 'NONE',  ( 4.458734124999999437, -61.06249999863440081, -5.460374474430324690E-16 ) ) ;
#37143 = CARTESIAN_POINT ( 'NONE',  ( 5.000000000000000000, -17.37499999726881583, -6.123233995736766282E-16 ) ) ;
#37144 = LINE ( 'NONE', #37767, #60461 ) ;
#37145 = CARTESIAN_POINT ( 'NONE',  ( 3.535533905932736864, -161.1250000000000284, 3.535533905932738641 ) ) ;
#37146 = CARTESIAN_POINT ( 'NONE',  ( -2.499999999999996447, -83.70833333060214443, 4.330127018922195425 ) ) ;
#37147 = CARTESIAN_POINT ( 'NONE',  ( -3.152548672688508926E-16, -35.56249999863440792, -5.148502694627439702 ) ) ;
#37148 = CARTESIAN_POINT ( 'NONE',  ( -4.458734124999997661, -21.47916666530107221, 2.574251347313722516 ) ) ;
#37149 = ORIENTED_EDGE ( 'NONE', *, *, #57099, .T. ) ;
#37150 = CARTESIAN_POINT ( 'NONE',  ( -6.972266317189433020E-16, -61.25000000000000000, -5.000000000000000000 ) ) ;
#37151 = CARTESIAN_POINT ( 'NONE',  ( -2.499999999999996447, 29.16666666666666785, 4.330127018922195425 ) ) ;
#37152 = CARTESIAN_POINT ( 'NONE',  ( -9.184850993605147944E-16, -153.3750000027311842, 5.000000000000000000 ) ) ;
#37153 = ORIENTED_EDGE ( 'NONE', *, *, #12228, .T. ) ;
#37154 = CARTESIAN_POINT ( 'NONE',  ( 4.458734124999998549, -104.9791666653010651, -2.574251347313721627 ) ) ;
#37155 = VECTOR ( 'NONE', #11809, 1000.000000000000000 ) ;
#37156 = CARTESIAN_POINT ( 'NONE',  ( -4.458734124999998549, -30.22916666530106866, 2.574251347313722516 ) ) ;
#37157 = CARTESIAN_POINT ( 'NONE',  ( 5.000000000000000000, -63.37499999726880873, -6.123233995736766282E-16 ) ) ;
#37158 = CARTESIAN_POINT ( 'NONE',  ( -59.29741812935640155, -152.8750000013656063, -2.196230717870135685 ) ) ;
#37159 = CARTESIAN_POINT ( 'NONE',  ( -2.071067811865475061, -145.6875000000000000, -5.000000000000000888 ) ) ;
#37160 = EDGE_CURVE ( 'NONE', #42868, #871, #20255, .T. ) ;
#37161 = CARTESIAN_POINT ( 'NONE',  ( -4.458734124999999437, -27.39583333196774007, -2.574251347313719407 ) ) ;
#37162 = CARTESIAN_POINT ( 'NONE',  ( 2.229367062500001939, -72.22916666530107932, 3.861377020970579999 ) ) ;
#37163 = LINE ( 'NONE', #26550, #17181 ) ;
#37164 = CARTESIAN_POINT ( 'NONE',  ( -4.458734124999999437, -25.39583333196773651, -2.574251347313719407 ) ) ;
#37165 = CARTESIAN_POINT ( 'NONE',  ( -4.999999999999998224, -32.91666666666666430, 2.886751345948131764 ) ) ;
#37166 = CARTESIAN_POINT ( 'NONE',  ( -2.499999999999996447, 9.291666669397853795, 4.330127018922195425 ) ) ;
#37167 = CARTESIAN_POINT ( 'NONE',  ( 5.000000000000000000, -17.41666666666666430, -2.886751345948129988 ) ) ;
#37168 = CARTESIAN_POINT ( 'NONE',  ( 2.730187237215162345E-16, -149.1875000013656063, -4.458734124999999437 ) ) ;
#37169 = ORIENTED_EDGE ( 'NONE', *, *, #42774, .F. ) ;
#37170 = CARTESIAN_POINT ( 'NONE',  ( 6.123233995736766282E-16, -120.0000000000000000, -5.000000000000000000 ) ) ;
#37171 = CARTESIAN_POINT ( 'NONE',  ( 2.229367062499998831, -53.89583333196773651, -3.861377020970580887 ) ) ;
#37172 = VECTOR ( 'NONE', #34807, 1000.000000000000000 ) ;
#37173 = FACE_OUTER_BOUND ( 'NONE', #29785, .T. ) ;
#37174 = CARTESIAN_POINT ( 'NONE',  ( -3.535250795749689387E-16, 25.74999999999999645, -5.773502691896257311 ) ) ;
#37175 =( BOUNDED_CURVE ( )  B_SPLINE_CURVE ( 2, ( #46108, #15888, #36456, #51267, #25533, #45791, #1750, #35508, #7200 ),
 .UNSPECIFIED., .F., .F. ) 
 B_SPLINE_CURVE_WITH_KNOTS ( ( 3, 2, 2, 2, 3 ),
 ( 0.2395833333333333426, 0.2402777777777777846, 0.2416666666666666685, 0.2430555555555555525, 0.2437499999999999944 ),
 .UNSPECIFIED. ) 
 CURVE ( )  GEOMETRIC_REPRESENTATION_ITEM ( )  RATIONAL_B_SPLINE_CURVE ( ( 0.9330127018922194093, 0.9330127018922194093, 1.000000000000000000, 0.8660254037844387076, 1.000000000000000000, 0.8660254037844387076, 1.000000000000000000, 0.9330127018922194093, 0.9330127018922194093 ) ) 
 REPRESENTATION_ITEM ( '' )  );
#37176 = CARTESIAN_POINT ( 'NONE',  ( -3.152548672688508926E-16, -1.562499998634406140, -5.148502694627439702 ) ) ;
#37177 = CARTESIAN_POINT ( 'NONE',  ( 1.975475456537005874E-15, -92.74999999999998579, 5.000000000000000000 ) ) ;
#37178 = CARTESIAN_POINT ( 'NONE',  ( 5.000000000000000000, -87.37499999726880162, -6.123233995736766282E-16 ) ) ;
#37179 = CARTESIAN_POINT ( 'NONE',  ( -4.458734124999999437, 11.35416666803225993, -2.574251347313719407 ) ) ;
#37180 = ORIENTED_EDGE ( 'NONE', *, *, #14593, .F. ) ;
#37181 = FACE_OUTER_BOUND ( 'NONE', #46755, .T. ) ;
#37182 = VERTEX_POINT ( 'NONE', #19461 ) ;
#37183 = CARTESIAN_POINT ( 'NONE',  ( 2.071067811865484387, -168.3125000027312126, 4.999999999999991118 ) ) ;
#37184 = CARTESIAN_POINT ( 'NONE',  ( -3.152548672688508926E-16, -47.56249999863440792, -5.148502694627439702 ) ) ;
#37185 = CARTESIAN_POINT ( 'NONE',  ( 4.458734124999999437, -163.7500000013655779, 1.846868145590737864 ) ) ;
#37186 =( BOUNDED_CURVE ( )  B_SPLINE_CURVE ( 2, ( #42769, #48851, #4792, #23793, #62413, #53684, #53055, #19585, #58823 ),
 .UNSPECIFIED., .F., .F. ) 
 B_SPLINE_CURVE_WITH_KNOTS ( ( 3, 2, 2, 2, 3 ),
 ( 0.1196428571428571480, 0.1202380952380952411, 0.1214285714285714274, 0.1226190476190476136, 0.1232142857142857206 ),
 .UNSPECIFIED. ) 
 CURVE ( )  GEOMETRIC_REPRESENTATION_ITEM ( )  RATIONAL_B_SPLINE_CURVE ( ( 0.9330127018922192983, 0.9330127018922200755, 1.000000000000000000, 0.8660254037844387076, 1.000000000000000000, 0.8660254037844387076, 1.000000000000000000, 0.9330127018922185211, 0.9330127018922192983 ) ) 
 REPRESENTATION_ITEM ( '' )  );
#37187 = CARTESIAN_POINT ( 'NONE',  ( -4.999999999999999112, -43.79166666393546592, 2.886751345948131764 ) ) ;
#37188 = VERTEX_POINT ( 'NONE', #54522 ) ;
#37189 = CARTESIAN_POINT ( 'NONE',  ( -3.152548672688508926E-16, -25.56249999863440436, -5.148502694627439702 ) ) ;
#37190 = ORIENTED_EDGE ( 'NONE', *, *, #28594, .T. ) ;
#37191 = CARTESIAN_POINT ( 'NONE',  ( -6.972266317189433020E-16, -53.24999999999999289, -5.000000000000000000 ) ) ;
#37192 = CARTESIAN_POINT ( 'NONE',  ( -4.458734125000000326, -165.0000000013655779, -1.846868145590735644 ) ) ;
#37193 = CARTESIAN_POINT ( 'NONE',  ( -2.500000000000000444, -51.04166666393547303, -4.330127018922193649 ) ) ;
#37194 = CARTESIAN_POINT ( 'NONE',  ( -50.01589407740564042, -135.6250000000000284, 0.3983568153799778022 ) ) ;
#37195 = CARTESIAN_POINT ( 'NONE',  ( 2.229367062500001939, -39.22916666530107221, 3.861377020970579999 ) ) ;
#37196 = CARTESIAN_POINT ( 'NONE',  ( 3.061616997868383141E-16, -163.7500000000000000, -5.000000000000000000 ) ) ;
#37197 = ORIENTED_EDGE ( 'NONE', *, *, #40175, .F. ) ;
#37198 = CARTESIAN_POINT ( 'NONE',  ( 4.458734124999998549, -81.72916666530106511, -2.574251347313721627 ) ) ;
#37199 = CARTESIAN_POINT ( 'NONE',  ( -4.458734124999998549, 24.77083333469893134, 2.574251347313722516 ) ) ;
#37200 = CARTESIAN_POINT ( 'NONE',  ( 2.500000000000002220, 24.45833333606451987, 4.330127018922192761 ) ) ;
#37201 = EDGE_LOOP ( 'NONE', ( #15757, #47096, #53948, #10039 ) ) ;
#37202 = CARTESIAN_POINT ( 'NONE',  ( 1.339745962155612702, -69.16965819600731891, -5.000000000000000000 ) ) ;
#37203 = CARTESIAN_POINT ( 'NONE',  ( -59.29741812935640155, -138.8750000013656063, -2.196230717870135685 ) ) ;
#37204 = CARTESIAN_POINT ( 'NONE',  ( -4.458734124999999437, -80.64583333196773651, -2.574251347313719407 ) ) ;
#37205 = CARTESIAN_POINT ( 'NONE',  ( -54.60164318462004474, -131.5000000027312126, -4.984105922594373794 ) ) ;
#37206 = CARTESIAN_POINT ( 'NONE',  ( 2.071067811865392461, -143.1875000000000568, 5.000000000000084377 ) ) ;
#37207 = CARTESIAN_POINT ( 'NONE',  ( -6.972266317189433020E-16, -83.24999999999998579, -5.000000000000000000 ) ) ;
#37208 = CARTESIAN_POINT ( 'NONE',  ( -5.000000000000000000, -44.95833333060214443, -2.886751345948128211 ) ) ;
#37209 = CARTESIAN_POINT ( 'NONE',  ( 9.457646018065525792E-16, -53.06249999863440792, 5.148502694627439702 ) ) ;
#37210 = CARTESIAN_POINT ( 'NONE',  ( -59.81910112700026616, -151.3125000027312410, -2.462841084822585014 ) ) ;
#37211 = CARTESIAN_POINT ( 'NONE',  ( -2.229367062499996610, 26.85416666803225993, 3.861377020970582219 ) ) ;
#37212 = CARTESIAN_POINT ( 'NONE',  ( 5.000000000000000000, -105.4166666666666572, -2.886751345948129988 ) ) ;
#37213 = LINE ( 'NONE', #51053, #33010 ) ;
#37214 = CARTESIAN_POINT ( 'NONE',  ( -2.229367062499996610, -43.39583333196773651, 3.861377020970582219 ) ) ;
#37215 = CARTESIAN_POINT ( 'NONE',  ( -2.500000000000000444, -1.041666663935479686, -4.330127018922193649 ) ) ;
#37216 = CARTESIAN_POINT ( 'NONE',  ( 1.975475456537005874E-15, -72.75000000000000000, 5.000000000000000000 ) ) ;
#37217 = CARTESIAN_POINT ( 'NONE',  ( -59.59170313451811296, -126.5000000013656063, 1.485763867205729394 ) ) ;
#37218 = CARTESIAN_POINT ( 'NONE',  ( -4.458734124999999437, -80.56249999863440792, 0.000000000000000000 ) ) ;
#37219 = CARTESIAN_POINT ( 'NONE',  ( -4.458734124999999437, -102.3124999986344079, 0.000000000000000000 ) ) ;
#37220 = CARTESIAN_POINT ( 'NONE',  ( 2.229367062499998831, -6.895833331967741842, -3.861377020970580887 ) ) ;
#37221 = ORIENTED_EDGE ( 'NONE', *, *, #16123, .T. ) ;
#37222 = CARTESIAN_POINT ( 'NONE',  ( -2.499999999999996447, -85.70833333060214443, 4.330127018922195425 ) ) ;
#37223 = CARTESIAN_POINT ( 'NONE',  ( -2.229367062499996610, -95.14583333196773651, 3.861377020970582219 ) ) ;
#37224 = CARTESIAN_POINT ( 'NONE',  ( 5.000000000000000000, -166.1250000027312126, 0.000000000000000000 ) ) ;
#37225 = CARTESIAN_POINT ( 'NONE',  ( 4.458734124999999437, -85.06249999863439371, -5.460374474430324690E-16 ) ) ;
#37226 = CARTESIAN_POINT ( 'NONE',  ( 2.229367062499998831, 14.10416666803226171, -3.861377020970580887 ) ) ;
#37227 = LINE ( 'NONE', #61362, #60306 ) ;
#37228 = CARTESIAN_POINT ( 'NONE',  ( -53.51423613279429503, -134.2500000013656063, 4.591703134518082763 ) ) ;
#37229 = CARTESIAN_POINT ( 'NONE',  ( -2.229367062500000163, -13.47916666530107221, -3.861377020970580443 ) ) ;
#37230 = CARTESIAN_POINT ( 'NONE',  ( -4.458734124999999437, 17.35416666803225993, -2.574251347313719407 ) ) ;
#37231 = CARTESIAN_POINT ( 'NONE',  ( 4.458734125000000326, -55.14583333196773651, 2.574251347313718519 ) ) ;
#37232 = DIRECTION ( 'NONE',  ( -1.000000000000000000, 0.000000000000000000, 0.000000000000000000 ) ) ;
#37233 = CARTESIAN_POINT ( 'NONE',  ( -5.000000000000000000, -21.95833333060214798, -2.886751345948128211 ) ) ;
#37234 = CARTESIAN_POINT ( 'NONE',  ( -4.458734124999999437, -8.312499998634406140, 0.000000000000000000 ) ) ;
#37235 = CARTESIAN_POINT ( 'NONE',  ( 75.00000000000000000, 15.00000000000000000, 8.999999999999998224 ) ) ;
#37236 = ORIENTED_EDGE ( 'NONE', *, *, #49609, .F. ) ;
#37237 = CARTESIAN_POINT ( 'NONE',  ( 4.458734125000000326, -36.14583333196773651, 2.574251347313718519 ) ) ;
#37238 =( BOUNDED_CURVE ( )  B_SPLINE_CURVE ( 2, ( #21413, #25909, #36513, #12391, #51639, #22045, #45527, #21091, #7573 ),
 .UNSPECIFIED., .F., .F. ) 
 B_SPLINE_CURVE_WITH_KNOTS ( ( 3, 2, 2, 2, 3 ),
 ( 0.1517857142857143016, 0.1523809523809523947, 0.1535714285714285809, 0.1547619047619047672, 0.1553571428571428603 ),
 .UNSPECIFIED. ) 
 CURVE ( )  GEOMETRIC_REPRESENTATION_ITEM ( )  RATIONAL_B_SPLINE_CURVE ( ( 0.9330127018922194093, 0.9330127018922209636, 1.000000000000000000, 0.8660254037844387076, 1.000000000000000000, 0.8660254037844387076, 1.000000000000000000, 0.9330127018922194093, 0.9330127018922194093 ) ) 
 REPRESENTATION_ITEM ( '' )  );
#37239 = CARTESIAN_POINT ( 'NONE',  ( -54.64476657466781973, -126.0625000013655921, -4.444560631937228834 ) ) ;
#37240 = CARTESIAN_POINT ( 'NONE',  ( 5.000000000000000888, 26.54166666939784847, 2.886751345948126879 ) ) ;
#37241 = CARTESIAN_POINT ( 'NONE',  ( 2.229367062500001939, -77.97916666530106511, 3.861377020970579999 ) ) ;
#37242 = CARTESIAN_POINT ( 'NONE',  ( -2.229367062500000163, 22.27083333469892423, -3.861377020970580443 ) ) ;
#37243 = CARTESIAN_POINT ( 'NONE',  ( 4.458734124999997661, -149.7500000013656063, 1.846868145590737864 ) ) ;
#37244 = CARTESIAN_POINT ( 'NONE',  ( 9.457646018065525792E-16, 14.93750000136559564, 5.148502694627439702 ) ) ;
#37245 = CARTESIAN_POINT ( 'NONE',  ( 0.000000000000000000, -120.0000000000000000, 5.000000000000000000 ) ) ;
#37246 = CARTESIAN_POINT ( 'NONE',  ( 2.229367062500001939, -83.22916666530106511, 3.861377020970579999 ) ) ;
#37247 = CARTESIAN_POINT ( 'NONE',  ( -5.000000000000000000, -65.08333333333332860, -2.886751345948128211 ) ) ;
#37248 = CARTESIAN_POINT ( 'NONE',  ( 1.975475456537005874E-15, -1.624999997268813834, 5.000000000000000000 ) ) ;
#37249 = CARTESIAN_POINT ( 'NONE',  ( 2.500000000000002220, 21.45833333606451987, 4.330127018922192761 ) ) ;
#37250 = ORIENTED_EDGE ( 'NONE', *, *, #25920, .T. ) ;
#37251 = CARTESIAN_POINT ( 'NONE',  ( 0.000000000000000000, -170.0000000000000000, 0.000000000000000000 ) ) ;
#37252 = CARTESIAN_POINT ( 'NONE',  ( -3.535250795749689387E-16, -28.24999999999999645, -5.773502691896257311 ) ) ;
#37253 = CARTESIAN_POINT ( 'NONE',  ( -4.458734124999999437, -34.39583333196772941, -2.574251347313719407 ) ) ;
#37254 = EDGE_CURVE ( 'NONE', #4410, #25201, #53563, .T. ) ;
#37255 = CARTESIAN_POINT ( 'NONE',  ( -6.972266317189433020E-16, 4.749999999999999112, -5.000000000000000000 ) ) ;
#37256 = CARTESIAN_POINT ( 'NONE',  ( -2.499999999999996447, -27.70833333060214798, 4.330127018922195425 ) ) ;
#37258 = ORIENTED_EDGE ( 'NONE', *, *, #49603, .F. ) ;
#37257 = CARTESIAN_POINT ( 'NONE',  ( 4.458734124999999437, -59.81249999863440081, -5.460374474430324690E-16 ) ) ;
#37259 = CARTESIAN_POINT ( 'NONE',  ( 6.123233995736766282E-16, -170.0000000000000000, -5.000000000000000000 ) ) ;
#37261 = ORIENTED_EDGE ( 'NONE', *, *, #7900, .F. ) ;
#37260 = CARTESIAN_POINT ( 'NONE',  ( 4.458734124999999437, -11.06249999863440792, -5.460374474430324690E-16 ) ) ;
#37262 = CARTESIAN_POINT ( 'NONE',  ( 1.060575238724906964E-15, -71.75000000000000000, 5.773502691896257311 ) ) ;
#37263 = CARTESIAN_POINT ( 'NONE',  ( -53.51423613279429503, -137.2500000013656063, 4.591703134518083651 ) ) ;
#37264 = CARTESIAN_POINT ( 'NONE',  ( -4.458734124999999437, -49.64583333196772941, -2.574251347313719407 ) ) ;
#37265 =( BOUNDED_CURVE ( )  B_SPLINE_CURVE ( 2, ( #29817, #49450, #5392, #25009, #1538, #12441, #11486, #21143, #27234 ),
 .UNSPECIFIED., .F., .F. ) 
 B_SPLINE_CURVE_WITH_KNOTS ( ( 3, 2, 2, 2, 3 ),
 ( 0.01458333333333333356, 0.01527777777777777728, 0.01666666666666666644, 0.01805555555555555386, 0.01874999999999999931 ),
 .UNSPECIFIED. ) 
 CURVE ( )  GEOMETRIC_REPRESENTATION_ITEM ( )  RATIONAL_B_SPLINE_CURVE ( ( 0.9330127018922192983, 0.9330127018922194093, 1.000000000000000000, 0.8660254037844387076, 1.000000000000000000, 0.8660254037844387076, 1.000000000000000000, 0.9330127018922194093, 0.9330127018922194093 ) ) 
 REPRESENTATION_ITEM ( '' )  );
#37266 = CARTESIAN_POINT ( 'NONE',  ( 2.500000000000002220, -78.54166666393547303, 4.330127018922192761 ) ) ;
#37268 = ORIENTED_EDGE ( 'NONE', *, *, #3313, .T. ) ;
#37267 = CARTESIAN_POINT ( 'NONE',  ( 2.499999999999998668, -13.33333333333333570, -4.330127018922193649 ) ) ;
#37269 = CARTESIAN_POINT ( 'NONE',  ( -55.39835681537999790, -149.8750000000000284, 4.984105922594378235 ) ) ;
#37270 = CARTESIAN_POINT ( 'NONE',  ( 2.229367062499998831, -18.89583333196774007, -3.861377020970580887 ) ) ;
#37271 = CARTESIAN_POINT ( 'NONE',  ( -3.152548672688508926E-16, -56.81249999863439371, -5.148502694627439702 ) ) ;
#37272 = EDGE_CURVE ( 'NONE', #11599, #14930, #50684, .T. ) ;
#37273 = CARTESIAN_POINT ( 'NONE',  ( -2.500000000000000444, -24.16666666666666430, -4.330127018922193649 ) ) ;
#37274 = CARTESIAN_POINT ( 'NONE',  ( -4.458734124999999437, -141.9375000013656063, -5.460374474430324690E-16 ) ) ;
#37275 = CARTESIAN_POINT ( 'NONE',  ( 2.229367062500001939, -100.2291666653010651, 3.861377020970579999 ) ) ;
#37276 = CARTESIAN_POINT ( 'NONE',  ( 1.975475456537005874E-15, -31.62499999726880873, 5.000000000000000000 ) ) ;
#37277 = VERTEX_POINT ( 'NONE', #29737 ) ;
#37278 = CARTESIAN_POINT ( 'NONE',  ( -56.48576386720575471, -153.0000000013656063, -4.591703134518078322 ) ) ;
#37279 = CARTESIAN_POINT ( 'NONE',  ( -49.85088928181150436, -141.6875000027312126, -1.666127454062680702 ) ) ;
#37280 = CARTESIAN_POINT ( 'NONE',  ( -1.339745962155564296, -13.08034179853029499, -5.000000000000028422 ) ) ;
#37281 = CARTESIAN_POINT ( 'NONE',  ( 9.457646018065525792E-16, -9.062499998634406140, 5.148502694627439702 ) ) ;
#37282 = CARTESIAN_POINT ( 'NONE',  ( 4.458734125000000326, -96.14583333196773651, 2.574251347313718519 ) ) ;
#37283 = CARTESIAN_POINT ( 'NONE',  ( -8.190561711645485556E-16, -149.9375000013656063, 4.458734124999999437 ) ) ;
#37284 = CARTESIAN_POINT ( 'NONE',  ( -4.458734124999998549, -22.47916666530107577, 2.574251347313722516 ) ) ;
#37285 = FACE_OUTER_BOUND ( 'NONE', #42699, .T. ) ;
#37286 = CARTESIAN_POINT ( 'NONE',  ( -59.29741812935640155, -137.6250000013655779, -2.196230717870135685 ) ) ;
#37287 = CARTESIAN_POINT ( 'NONE',  ( 2.229367062500001939, -64.22916666530106511, 3.861377020970579999 ) ) ;
#37288 = CYLINDRICAL_SURFACE ( 'NONE', #40455, 5.000000000000000000 ) ;
#37289 = CYLINDRICAL_SURFACE ( 'NONE', #63409, 5.000000000000000000 ) ;
#37290 = CARTESIAN_POINT ( 'NONE',  ( 2.730187237215162345E-16, -146.1875000013656063, -4.458734124999999437 ) ) ;
#37291 = CARTESIAN_POINT ( 'NONE',  ( 4.458734124999998549, 9.020833334698927786, -2.574251347313721627 ) ) ;
#37292 = VERTEX_POINT ( 'NONE', #34900 ) ;
#37293 = CARTESIAN_POINT ( 'NONE',  ( -5.000000000000000000, -5.083333333333334814, -2.886751345948128211 ) ) ;
#37294 = CARTESIAN_POINT ( 'NONE',  ( 2.500000000000002220, -66.54166666393547303, 4.330127018922192761 ) ) ;
#37296 = CARTESIAN_POINT ( 'NONE',  ( -2.229367062499996610, -26.14583333196773651, 3.861377020970582219 ) ) ;
#37295 = CARTESIAN_POINT ( 'NONE',  ( 5.000000000000000000, -89.41666666666667140, -2.886751345948129988 ) ) ;
#37297 = LINE ( 'NONE', #42424, #3820 ) ;
#37298 = CARTESIAN_POINT ( 'NONE',  ( -2.229367062499996610, -73.39583333196773651, 3.861377020970582219 ) ) ;
#37299 = CARTESIAN_POINT ( 'NONE',  ( 9.457646018065525792E-16, 26.68750000136559564, 5.148502694627439702 ) ) ;
#37300 = CARTESIAN_POINT ( 'NONE',  ( 1.339745962155612702, -79.16965819600730470, -5.000000000000000000 ) ) ;
#37301 = CARTESIAN_POINT ( 'NONE',  ( -59.59170313451811296, -145.5000000013656063, 1.485763867205729394 ) ) ;
#37302 = CARTESIAN_POINT ( 'NONE',  ( -4.458734124999997661, 1.770833334698928008, 2.574251347313722516 ) ) ;
#37303 = CARTESIAN_POINT ( 'NONE',  ( 1.339745962155612702, -56.16965819600733312, -5.000000000000000000 ) ) ;
#37304 = LINE ( 'NONE', #22524, #45922 ) ;
#37305 = CARTESIAN_POINT ( 'NONE',  ( 9.457646018065525792E-16, 5.937500001365593860, 5.148502694627439702 ) ) ;
#37306 = CARTESIAN_POINT ( 'NONE',  ( 4.458734124999998549, -70.72916666530107932, -2.574251347313721627 ) ) ;
#37307 = CARTESIAN_POINT ( 'NONE',  ( -4.458734124999997661, -20.47916666530107577, 2.574251347313722516 ) ) ;
#37308 = CARTESIAN_POINT ( 'NONE',  ( -2.500000000000000444, -1.166666666666666519, -4.330127018922193649 ) ) ;
#37309 = CARTESIAN_POINT ( 'NONE',  ( 2.730187237215162345E-16, -160.1875000013655779, -4.458734124999999437 ) ) ;
#37310 = CARTESIAN_POINT ( 'NONE',  ( 6.972266317189433020E-16, 28.87500000273118417, -5.000000000000000000 ) ) ;
#37311 = CARTESIAN_POINT ( 'NONE',  ( -3.152548672688508926E-16, -63.56249999863440792, -5.148502694627439702 ) ) ;
#37312 = CARTESIAN_POINT ( 'NONE',  ( 1.060575238724906964E-15, -102.6249999972688158, 5.773502691896257311 ) ) ;
#37313 = CARTESIAN_POINT ( 'NONE',  ( -6.972266317189433020E-16, -51.25000000000000000, -5.000000000000000000 ) ) ;
#37314 = CARTESIAN_POINT ( 'NONE',  ( -2.229367062499996610, -42.14583333196773651, 3.861377020970582219 ) ) ;
#37315 = CARTESIAN_POINT ( 'NONE',  ( 9.457646018065525792E-16, -108.3124999986343937, 5.148502694627439702 ) ) ;
#37316 = CARTESIAN_POINT ( 'NONE',  ( 4.458734124999999437, -69.06249999863439371, -5.460374474430324690E-16 ) ) ;
#37317 = CARTESIAN_POINT ( 'NONE',  ( 1.060575238724906964E-15, -49.75000000000000000, 5.773502691896257311 ) ) ;
#37318 = CARTESIAN_POINT ( 'NONE',  ( 5.000000000000000000, -57.29166666393548013, -2.886751345948130876 ) ) ;
#37319 = CARTESIAN_POINT ( 'NONE',  ( 6.123233995736766282E-16, -170.0000000000000000, -5.000000000000000000 ) ) ;
#37320 = ORIENTED_EDGE ( 'NONE', *, *, #18155, .F. ) ;
#37321 = CARTESIAN_POINT ( 'NONE',  ( -4.458734124999998549, -110.2291666653010651, 2.574251347313722516 ) ) ;
#37322 = CARTESIAN_POINT ( 'NONE',  ( 1.339745962155612702, -89.16965819600733312, -5.000000000000000000 ) ) ;
#37323 = CARTESIAN_POINT ( 'NONE',  ( -2.500000000000000444, -6.166666666666667851, -4.330127018922193649 ) ) ;
#37324 = EDGE_CURVE ( 'NONE', #5681, #34549, #58704, .T. ) ;
#37325 = CARTESIAN_POINT ( 'NONE',  ( -2.229367062499996610, -79.14583333196773651, 3.861377020970582219 ) ) ;
#37326 = LINE ( 'NONE', #56646, #46238 ) ;
#37327 = CARTESIAN_POINT ( 'NONE',  ( 5.000000000000000888, -12.45833333060214976, 2.886751345948126879 ) ) ;
#37329 = ORIENTED_EDGE ( 'NONE', *, *, #18947, .F. ) ;
#37328 = CARTESIAN_POINT ( 'NONE',  ( -3.152548672688508926E-16, -42.56249999863440792, -5.148502694627439702 ) ) ;
#37331 = VERTEX_POINT ( 'NONE', #34562 ) ;
#37330 = CARTESIAN_POINT ( 'NONE',  ( 9.457646018065525792E-16, 4.687500001365596525, 5.148502694627439702 ) ) ;
#37332 = CARTESIAN_POINT ( 'NONE',  ( -53.33387254593711901, -140.9375000027311842, 5.149110718188534719 ) ) ;
#37333 = CARTESIAN_POINT ( 'NONE',  ( 2.499999999999998668, -58.33333333333333570, -4.330127018922193649 ) ) ;
#37334 = CARTESIAN_POINT ( 'NONE',  ( 4.458734124999999437, -158.7500000013656063, 1.846868145590737864 ) ) ;
#37335 = CARTESIAN_POINT ( 'NONE',  ( -4.458734124999999437, -37.56249999863440792, 0.000000000000000000 ) ) ;
#37336 = CARTESIAN_POINT ( 'NONE',  ( -5.000000000000000000, -35.08333333333332860, -2.886751345948128211 ) ) ;
#37337 = CARTESIAN_POINT ( 'NONE',  ( 4.458734124999998549, -80.72916666530106511, -2.574251347313721627 ) ) ;
#37338 = CARTESIAN_POINT ( 'NONE',  ( -2.071067811865478170, -168.3125000000000000, 5.000000000000000000 ) ) ;
#37339 = EDGE_CURVE ( 'NONE', #26215, #9342, #33029, .T. ) ;
#37340 = CARTESIAN_POINT ( 'NONE',  ( 2.229367062500001939, -89.97916666530106511, 3.861377020970579999 ) ) ;
#37341 = CARTESIAN_POINT ( 'NONE',  ( -55.35523342533222291, -130.5625000013656063, 4.444560631937231499 ) ) ;
#37342 = CARTESIAN_POINT ( 'NONE',  ( 2.229367062500001939, -2.229166665301068662, 3.861377020970579999 ) ) ;
#37343 = CARTESIAN_POINT ( 'NONE',  ( -4.458734124999999437, -40.56249999863440081, 0.000000000000000000 ) ) ;
#37344 = AXIS2_PLACEMENT_3D ( 'NONE', #46052, #11947, #22574 ) ;
#37345 = CARTESIAN_POINT ( 'NONE',  ( 6.123233995736766282E-16, -170.0000000000000000, -5.000000000000000000 ) ) ;
#37346 = EDGE_CURVE ( 'NONE', #13129, #25936, #5633, .T. ) ;
#37347 = CARTESIAN_POINT ( 'NONE',  ( 2.229367062499998831, -82.89583333196773651, -3.861377020970580887 ) ) ;
#37348 = CARTESIAN_POINT ( 'NONE',  ( 5.000000000000000000, -86.41666666666667140, -2.886751345948130876 ) ) ;
#37349 = ORIENTED_EDGE ( 'NONE', *, *, #21984, .T. ) ;
#37350 = EDGE_CURVE ( 'NONE', #29768, #33407, #59671, .T. ) ;
#37351 = CARTESIAN_POINT ( 'NONE',  ( -6.972266317189433020E-16, -95.12499999726880162, -5.000000000000000000 ) ) ;
#37352 = CARTESIAN_POINT ( 'NONE',  ( 1.975475456537005874E-15, -68.62499999726881583, 5.000000000000000000 ) ) ;
#37353 = CARTESIAN_POINT ( 'NONE',  ( -4.458734124999998549, -72.47916666530107932, 2.574251347313722516 ) ) ;
#37354 = CARTESIAN_POINT ( 'NONE',  ( -4.458734124999999437, -38.39583333196773651, -2.574251347313719407 ) ) ;
#37355 = CARTESIAN_POINT ( 'NONE',  ( 9.457646018065525792E-16, -11.31249999863440792, 5.148502694627439702 ) ) ;
#37356 = ORIENTED_EDGE ( 'NONE', *, *, #34199, .F. ) ;
#37357 = CYLINDRICAL_SURFACE ( 'NONE', #16397, 5.000000000000000000 ) ;
#37358 =( BOUNDED_CURVE ( )  B_SPLINE_CURVE ( 2, ( #43205, #39322, #4297, #3679, #14253, #33876, #33565, #48976, #53495 ),
 .UNSPECIFIED., .F., .F. ) 
 B_SPLINE_CURVE_WITH_KNOTS ( ( 3, 2, 2, 2, 3 ),
 ( 0.3750000000000002776, 0.3791666666666669294, 0.3833333333333336368, 0.3875000000000003442, 0.3916666666666669960 ),
 .UNSPECIFIED. ) 
 CURVE ( )  GEOMETRIC_REPRESENTATION_ITEM ( )  RATIONAL_B_SPLINE_CURVE ( ( 0.9999999999999948930, 0.9238795325112918455, 1.000000000000000000, 0.9238795325112867385, 1.000000000000000000, 0.9238795325112867385, 1.000000000000000000, 0.9238795325112806323, 1.000000000000005995 ) ) 
 REPRESENTATION_ITEM ( '' )  );
#37359 = CARTESIAN_POINT ( 'NONE',  ( 5.000000000000000000, 2.708333336064520314, -2.886751345948130876 ) ) ;
#37360 = CARTESIAN_POINT ( 'NONE',  ( -4.458734124999999437, -5.645833331967740953, -2.574251347313719407 ) ) ;
#37361 = CARTESIAN_POINT ( 'NONE',  ( -49.85088928181150436, -148.6875000027312126, -1.666127454062680480 ) ) ;
#37362 = CARTESIAN_POINT ( 'NONE',  ( 4.458734125000001214, 5.104166668032261711, 2.574251347313718519 ) ) ;
#37363 = CARTESIAN_POINT ( 'NONE',  ( -5.000000000000000000, -80.00000000000000000, 0.000000000000000000 ) ) ;
#37364 = CARTESIAN_POINT ( 'NONE',  ( 2.730187237215162345E-16, -157.1875000013655779, -4.458734124999999437 ) ) ;
#37365 = CARTESIAN_POINT ( 'NONE',  ( 2.229367062499998831, 27.10416666803225993, -3.861377020970580887 ) ) ;
#37366 = VERTEX_POINT ( 'NONE', #54840 ) ;
#37367 = CARTESIAN_POINT ( 'NONE',  ( 4.458734124999999437, -88.81249999863439371, -5.460374474430324690E-16 ) ) ;
#37368 = CARTESIAN_POINT ( 'NONE',  ( -4.458734124999998549, -11.22916666530106866, 2.574251347313722516 ) ) ;
#37369 = ADVANCED_FACE ( 'NONE', ( #26763 ), #25566, .T. ) ;
#37370 = CYLINDRICAL_SURFACE ( 'NONE', #36600, 5.000000000000000000 ) ;
#37371 = CARTESIAN_POINT ( 'NONE',  ( -58.24261429053147765, -138.2500000000000000, -3.805975901505573855 ) ) ;
#37372 = CARTESIAN_POINT ( 'NONE',  ( 2.499999999999998668, -37.20833333060213732, -4.330127018922193649 ) ) ;
#37373 = CARTESIAN_POINT ( 'NONE',  ( -58.24261429053147765, -144.3750000027312126, -3.805975901505573855 ) ) ;
#37374 = CARTESIAN_POINT ( 'NONE',  ( 4.458734124999999437, 23.18750000136559564, -5.460374474430324690E-16 ) ) ;
#37375 = CARTESIAN_POINT ( 'NONE',  ( -4.999999999999998224, -94.91666666666667140, 2.886751345948131764 ) ) ;
#37376 = CARTESIAN_POINT ( 'NONE',  ( 2.229367062500001939, 21.02083333469892779, 3.861377020970579999 ) ) ;
#37377 = CARTESIAN_POINT ( 'NONE',  ( 4.458734124999998549, -57.72916666530107221, -2.574251347313721627 ) ) ;
#37378 = CARTESIAN_POINT ( 'NONE',  ( 4.458734125000000326, -1.145833331967740287, 2.574251347313718519 ) ) ;
#37379 = CARTESIAN_POINT ( 'NONE',  ( -2.499999999999996447, -33.70833333060213732, 4.330127018922195425 ) ) ;
#37380 = CARTESIAN_POINT ( 'NONE',  ( 2.500000000000002220, 13.33333333333333215, 4.330127018922192761 ) ) ;
#37381 = CARTESIAN_POINT ( 'NONE',  ( 3.535533905932736864, -141.2500000027311842, 3.535533905932738641 ) ) ;
#37382 = CARTESIAN_POINT ( 'NONE',  ( -1.339745962155610925, -45.79465819873851729, 5.000000000000000000 ) ) ;
#37383 = CARTESIAN_POINT ( 'NONE',  ( 4.458734124999998549, -49.72916666530106511, -2.574251347313721627 ) ) ;
#37384 = CARTESIAN_POINT ( 'NONE',  ( -3.535250795749689387E-16, -85.12499999726881583, -5.773502691896257311 ) ) ;
#37385 = CARTESIAN_POINT ( 'NONE',  ( -50.70258187064364108, -136.3750000013656063, 2.196230717870141014 ) ) ;
#37386 = AXIS2_PLACEMENT_3D ( 'NONE', #44837, #30040, #54820 ) ;
#37387 = DIRECTION ( 'NONE',  ( -0.000000000000000000, 1.000000000000000000, -0.000000000000000000 ) ) ;
#37388 = CARTESIAN_POINT ( 'NONE',  ( 0.000000000000000000, -170.0000000000000000, 5.000000000000000000 ) ) ;
#37389 = CARTESIAN_POINT ( 'NONE',  ( 9.457646018065525792E-16, -88.31249999863439371, 5.148502694627439702 ) ) ;
#37390 = CARTESIAN_POINT ( 'NONE',  ( 4.458734124999999437, -156.6875000013655779, 0.000000000000000000 ) ) ;
#37391 = CARTESIAN_POINT ( 'NONE',  ( 5.000000000000000000, -34.50000000000000000, -6.123233995736766282E-16 ) ) ;
#37392 = CARTESIAN_POINT ( 'NONE',  ( 5.000000000000000000, 8.625000002731184168, -6.123233995736766282E-16 ) ) ;
#37393 = VERTEX_POINT ( 'NONE', #22259 ) ;
#37394 = CARTESIAN_POINT ( 'NONE',  ( 4.458734125000001214, 18.85416666803226349, 2.574251347313718519 ) ) ;
#37395 = ORIENTED_EDGE ( 'NONE', *, *, #39355, .T. ) ;
#37396 = CARTESIAN_POINT ( 'NONE',  ( -2.229367062499996610, -97.14583333196773651, 3.861377020970582219 ) ) ;
#37397 = CARTESIAN_POINT ( 'NONE',  ( 4.458734125000001214, 8.854166668032261711, 2.574251347313718519 ) ) ;
#37398 = CARTESIAN_POINT ( 'NONE',  ( -4.999999999999999112, 17.20833333606451987, 2.886751345948131764 ) ) ;
#37399 = CARTESIAN_POINT ( 'NONE',  ( -5.000000000000000000, -28.87499999726881228, 0.000000000000000000 ) ) ;
#37400 = CARTESIAN_POINT ( 'NONE',  ( 1.060575238724906964E-15, 8.250000000000000000, 5.773502691896257311 ) ) ;
#37401 = CARTESIAN_POINT ( 'NONE',  ( 4.458734124999999437, -55.81249999863440081, -5.460374474430324690E-16 ) ) ;
#37402 = CARTESIAN_POINT ( 'NONE',  ( -4.999999999999998224, -7.916666666666668739, 2.886751345948131764 ) ) ;
#37403 = CARTESIAN_POINT ( 'NONE',  ( 2.499999999999998668, -79.33333333333332860, -4.330127018922193649 ) ) ;
#37404 = EDGE_CURVE ( 'NONE', #24529, #7439, #13674, .T. ) ;
#37405 = ADVANCED_FACE ( 'NONE', ( #51530 ), #41858, .T. ) ;
#37406 = CARTESIAN_POINT ( 'NONE',  ( 4.458734124999999437, -28.81249999863440436, -5.460374474430324690E-16 ) ) ;
#37407 = CARTESIAN_POINT ( 'NONE',  ( 2.071067811865645591, -153.3125000027311557, 4.999999999999830358 ) ) ;
#37408 = CARTESIAN_POINT ( 'NONE',  ( 1.975475456537005874E-15, -63.74999999999998579, 5.000000000000000000 ) ) ;
#37409 = EDGE_CURVE ( 'NONE', #39907, #40253, #933, .T. ) ;
#37410 = CARTESIAN_POINT ( 'NONE',  ( -58.24261429053147765, -151.2500000000000284, -3.805975901505573855 ) ) ;
#37411 = CARTESIAN_POINT ( 'NONE',  ( 2.499999999999998668, -41.33333333333333570, -4.330127018922193649 ) ) ;
#37412 = CARTESIAN_POINT ( 'NONE',  ( 2.071067811865644703, -148.8125000000000000, -4.999999999999831246 ) ) ;
#37415 = CARTESIAN_POINT ( 'NONE',  ( -2.229367062499996610, -17.39583333196773651, 3.861377020970582219 ) ) ;
#37414 =( BOUNDED_CURVE ( )  B_SPLINE_CURVE ( 2, ( #47976, #18707, #28981, #38332, #38630, #63106, #33510, #53127, #32560 ),
 .UNSPECIFIED., .F., .F. ) 
 B_SPLINE_CURVE_WITH_KNOTS ( ( 3, 2, 2, 2, 3 ),
 ( 0.8696428571428571619, 0.8702380952380952550, 0.8714285714285714413, 0.8726190476190476275, 0.8732142857142857206 ),
 .UNSPECIFIED. ) 
 CURVE ( )  GEOMETRIC_REPRESENTATION_ITEM ( )  RATIONAL_B_SPLINE_CURVE ( ( 0.9330127018922194093, 0.9330127018922194093, 1.000000000000000000, 0.8660254037844387076, 1.000000000000000000, 0.8660254037844387076, 1.000000000000000000, 0.9330127018922194093, 0.9330127018922194093 ) ) 
 REPRESENTATION_ITEM ( '' )  );
#37413 = CARTESIAN_POINT ( 'NONE',  ( -6.972266317189433020E-16, 13.74999999999999822, -5.000000000000000000 ) ) ;
#37416 = CARTESIAN_POINT ( 'NONE',  ( 1.975475456537005874E-15, -107.6249999972687874, 5.000000000000000000 ) ) ;
#37417 = CARTESIAN_POINT ( 'NONE',  ( 2.229367062500001939, -65.97916666530106511, 3.861377020970579999 ) ) ;
#37418 = CARTESIAN_POINT ( 'NONE',  ( -4.458734125000001214, -149.1250000013656063, 1.846868145590734089 ) ) ;
#37419 = CARTESIAN_POINT ( 'NONE',  ( -3.152548672688508926E-16, -72.56249999863439371, -5.148502694627439702 ) ) ;
#37420 = CARTESIAN_POINT ( 'NONE',  ( -52.80376928212989185, -145.1250000013655779, -4.297418129356379346 ) ) ;
#37421 = EDGE_CURVE ( 'NONE', #40520, #51921, #12596, .T. ) ;
#37422 = CARTESIAN_POINT ( 'NONE',  ( -4.458734124999999437, -25.56249999863440792, 0.000000000000000000 ) ) ;
#37423 = CARTESIAN_POINT ( 'NONE',  ( -2.500000000000000444, -59.04166666393546592, -4.330127018922193649 ) ) ;
#37424 = ORIENTED_EDGE ( 'NONE', *, *, #60243, .F. ) ;
#37425 = CARTESIAN_POINT ( 'NONE',  ( 1.339745962155612702, -85.16965819600733312, -5.000000000000000000 ) ) ;
#37427 = ORIENTED_EDGE ( 'NONE', *, *, #22815, .F. ) ;
#37426 = ADVANCED_FACE ( 'NONE', ( #7153 ), #7781, .T. ) ;
#37428 = CARTESIAN_POINT ( 'NONE',  ( 2.229367062500001939, -67.22916666530106511, 3.861377020970579999 ) ) ;
#37429 = CARTESIAN_POINT ( 'NONE',  ( 2.071067811865644703, -148.9375000027312410, -4.999999999999831246 ) ) ;
#37430 = ADVANCED_FACE ( 'NONE', ( #50004 ), #56680, .F. ) ;
#37431 = ORIENTED_EDGE ( 'NONE', *, *, #15862, .T. ) ;
#37432 = EDGE_CURVE ( 'NONE', #54748, #11960, #42038, .T. ) ;
#37433 = CARTESIAN_POINT ( 'NONE',  ( -75.00000000000000000, 15.00000000000000000, 8.999999999999998224 ) ) ;
#37434 = DIRECTION ( 'NONE',  ( 0.000000000000000000, -1.000000000000000000, 0.000000000000000000 ) ) ;
#37435 = CARTESIAN_POINT ( 'NONE',  ( 4.458734124999998549, -53.97916666530107221, -2.574251347313721627 ) ) ;
#37436 = EDGE_LOOP ( 'NONE', ( #27829, #1904, #51975, #53101 ) ) ;
#37437 = VECTOR ( 'NONE', #18098, 1000.000000000000000 ) ;
#37438 = CARTESIAN_POINT ( 'NONE',  ( 3.093157300003884558, 6.874418838041288282, 2.127746763502802452E-15 ) ) ;
#37439 = CARTESIAN_POINT ( 'NONE',  ( 9.457646018065525792E-16, 7.937500001365594748, 5.148502694627439702 ) ) ;
#37440 = CARTESIAN_POINT ( 'NONE',  ( -2.229367062500000163, 20.52083333469892779, -3.861377020970580443 ) ) ;
#37441 = CARTESIAN_POINT ( 'NONE',  ( -50.70258187064364108, -150.1250000013656063, 2.196230717870141014 ) ) ;
#37442 = CARTESIAN_POINT ( 'NONE',  ( 2.499999999999998668, -108.2083333306021444, -4.330127018922193649 ) ) ;
#37443 = CYLINDRICAL_SURFACE ( 'NONE', #38733, 5.000000000000000000 ) ;
#37444 = ORIENTED_EDGE ( 'NONE', *, *, #5255, .F. ) ;
#37445 = CARTESIAN_POINT ( 'NONE',  ( -2.229367062499996610, -72.14583333196773651, 3.861377020970582219 ) ) ;
#37446 = CARTESIAN_POINT ( 'NONE',  ( -5.000000000000000000, -85.95833333060214443, -2.886751345948128211 ) ) ;
#37447 = CARTESIAN_POINT ( 'NONE',  ( -2.229367062499996610, 6.854166668032259935, 3.861377020970582219 ) ) ;
#37448 = CARTESIAN_POINT ( 'NONE',  ( 5.000000000000000000, -69.37499999726880162, -6.123233995736766282E-16 ) ) ;
#37449 = CARTESIAN_POINT ( 'NONE',  ( -2.229367062500000163, -60.72916666530106511, -3.861377020970580443 ) ) ;
#37450 = CARTESIAN_POINT ( 'NONE',  ( 2.500000000000002220, -17.54166666393547658, 4.330127018922192761 ) ) ;
#37451 = DIRECTION ( 'NONE',  ( -0.000000000000000000, 1.000000000000000000, -0.000000000000000000 ) ) ;
#37452 = DIRECTION ( 'NONE',  ( -0.000000000000000000, 1.000000000000000000, -0.000000000000000000 ) ) ;
#37453 = DIRECTION ( 'NONE',  ( -0.6485228581062915110, 0.000000000000000000, -0.7611951803011149931 ) ) ;
#37454 = CARTESIAN_POINT ( 'NONE',  ( 4.458734124999998549, -40.72916666530107221, -2.574251347313721627 ) ) ;
#37455 = CARTESIAN_POINT ( 'NONE',  ( -4.458734124999997661, -19.47916666530107221, 2.574251347313722516 ) ) ;
#37456 = ORIENTED_EDGE ( 'NONE', *, *, #5153, .T. ) ;
#37457 =( BOUNDED_CURVE ( )  B_SPLINE_CURVE ( 2, ( #27391, #47024, #2973, #27711, #3288, #4522, #48581, #18686, #9978 ),
 .UNSPECIFIED., .F., .F. ) 
 B_SPLINE_CURVE_WITH_KNOTS ( ( 3, 2, 2, 2, 3 ),
 ( 0.6395833333333332815, 0.6402777777777777235, 0.6416666666666667185, 0.6430555555555556024, 0.6437500000000000444 ),
 .UNSPECIFIED. ) 
 CURVE ( )  GEOMETRIC_REPRESENTATION_ITEM ( )  RATIONAL_B_SPLINE_CURVE ( ( 0.9330127018922194093, 0.9330127018922194093, 1.000000000000000000, 0.8660254037844387076, 1.000000000000000000, 0.8660254037844387076, 1.000000000000000000, 0.9330127018922194093, 0.9330127018922194093 ) ) 
 REPRESENTATION_ITEM ( '' )  );
#37458 = FACE_OUTER_BOUND ( 'NONE', #3272, .T. ) ;
#37459 = CARTESIAN_POINT ( 'NONE',  ( 2.229367062500001939, -108.9791666653010651, 3.861377020970579999 ) ) ;
#37460 = CARTESIAN_POINT ( 'NONE',  ( 5.000000000000000000, -154.1875000027312126, 2.071067811865478614 ) ) ;
#37461 = VERTEX_POINT ( 'NONE', #16791 ) ;
#37462 = CARTESIAN_POINT ( 'NONE',  ( 4.458734125000001214, -109.1458333319677365, 2.574251347313718519 ) ) ;
#37463 = CARTESIAN_POINT ( 'NONE',  ( -4.458734124999999437, -34.31249999863440792, 0.000000000000000000 ) ) ;
#37464 = CARTESIAN_POINT ( 'NONE',  ( 2.500000000000002220, -67.54166666393547303, 4.330127018922192761 ) ) ;
#37465 = CARTESIAN_POINT ( 'NONE',  ( -50.55543936806279248, -149.3125000013656063, 0.3552334253322060320 ) ) ;
#37466 = CARTESIAN_POINT ( 'NONE',  ( -5.000000000000000888, -145.5625000000000568, -2.071067811865475949 ) ) ;
#37467 = CARTESIAN_POINT ( 'NONE',  ( 4.458734125000000326, -26.89583333196774007, 2.574251347313718519 ) ) ;
#37468 = CARTESIAN_POINT ( 'NONE',  ( -4.458734124999997661, -69.47916666530107932, 2.574251347313722516 ) ) ;
#37469 = CARTESIAN_POINT ( 'NONE',  ( -3.152801135295367985, -169.0625000013656063, 3.152801135295367096 ) ) ;
#37470 = CARTESIAN_POINT ( 'NONE',  ( -2.229367062500000163, -26.47916666530106866, -3.861377020970580443 ) ) ;
#37471 = CARTESIAN_POINT ( 'NONE',  ( 2.499999999999998668, 14.66666666666666607, -4.330127018922193649 ) ) ;
#37472 = CARTESIAN_POINT ( 'NONE',  ( -4.999999999999999112, -15.91666666666666963, 2.886751345948131764 ) ) ;
#37473 = CARTESIAN_POINT ( 'NONE',  ( -3.152801135295367096, -149.0625000013655779, -3.152801135295367541 ) ) ;
#37474 = ORIENTED_EDGE ( 'NONE', *, *, #53074, .F. ) ;
#37475 = CARTESIAN_POINT ( 'NONE',  ( -1.339745962155613812, -82.20534180126146850, -5.000000000000000000 ) ) ;
#37476 = CARTESIAN_POINT ( 'NONE',  ( -4.458734124999997661, -50.47916666530107221, 2.574251347313722516 ) ) ;
#37477 = FACE_OUTER_BOUND ( 'NONE', #15181, .T. ) ;
#37478 = CARTESIAN_POINT ( 'NONE',  ( 5.000000000000000000, 24.50000000000000000, -6.123233995736766282E-16 ) ) ;
#37479 = LINE ( 'NONE', #41651, #12078 ) ;
#37480 = VECTOR ( 'NONE', #50069, 1000.000000000000000 ) ;
#37481 = CARTESIAN_POINT ( 'NONE',  ( 2.229367062500001939, -2.979166665301069550, 3.861377020970579999 ) ) ;
#37482 = CARTESIAN_POINT ( 'NONE',  ( 1.975475456537005874E-15, 19.25000000000000000, 5.000000000000000000 ) ) ;
#37483 = CARTESIAN_POINT ( 'NONE',  ( 1.339745962155615144, -87.58034179853028434, 4.999999999999999112 ) ) ;
#37484 = CARTESIAN_POINT ( 'NONE',  ( -2.229367062499996610, 8.604166668032261711, 3.861377020970582219 ) ) ;
#37485 = ORIENTED_EDGE ( 'NONE', *, *, #27238, .F. ) ;
#37486 = CARTESIAN_POINT ( 'NONE',  ( -7.500000000000001776, 0.000000000000000000, 0.000000000000000000 ) ) ;
#37487 = VERTEX_POINT ( 'NONE', #17744 ) ;
#37488 = CARTESIAN_POINT ( 'NONE',  ( -6.972266317189433020E-16, -71.25000000000000000, -5.000000000000000000 ) ) ;
#37489 = CARTESIAN_POINT ( 'NONE',  ( 2.229367062500001939, -49.97916666530107221, 3.861377020970579999 ) ) ;
#37490 = CARTESIAN_POINT ( 'NONE',  ( -1.846868145590734756, -158.3750000013655779, -4.458734125000000326 ) ) ;
#37491 = CARTESIAN_POINT ( 'NONE',  ( 2.500000000000002220, -46.54166666393547303, 4.330127018922192761 ) ) ;
#37492 = ORIENTED_EDGE ( 'NONE', *, *, #41340, .F. ) ;
#37493 = CARTESIAN_POINT ( 'NONE',  ( 4.458734125000001214, -23.89583333196774007, 2.574251347313718519 ) ) ;
#37494 = ORIENTED_EDGE ( 'NONE', *, *, #32321, .F. ) ;
#37495 = CARTESIAN_POINT ( 'NONE',  ( -5.000000000000000000, -102.8749999972688158, 0.000000000000000000 ) ) ;
#37496 = CARTESIAN_POINT ( 'NONE',  ( 4.458734124999999437, -159.5000000013655779, 1.846868145590737864 ) ) ;
#37497 = ADVANCED_FACE ( 'NONE', ( #36409 ), #56991, .T. ) ;
#37498 = EDGE_CURVE ( 'NONE', #6296, #49700, #7492, .T. ) ;
#37499 = CARTESIAN_POINT ( 'NONE',  ( -1.339745962155613812, -51.08034179853027723, -5.000000000000000000 ) ) ;
#37500 = CARTESIAN_POINT ( 'NONE',  ( -58.24261429053147765, -137.2500000000000000, -3.805975901505573855 ) ) ;
#37501 = CARTESIAN_POINT ( 'NONE',  ( -3.152548672688508926E-16, -39.81249999863440081, -5.148502694627439702 ) ) ;
#37502 = DIRECTION ( 'NONE',  ( 0.000000000000000000, 0.000000000000000000, 1.000000000000000000 ) ) ;
#37503 = ORIENTED_EDGE ( 'NONE', *, *, #34846, .T. ) ;
#37504 = ADVANCED_FACE ( 'NONE', ( #53096 ), #19305, .T. ) ;
#37505 = CARTESIAN_POINT ( 'NONE',  ( -2.229367062500000163, -84.47916666530107932, -3.861377020970580443 ) ) ;
#37506 = CARTESIAN_POINT ( 'NONE',  ( -2.229367062500000163, 25.52083333469892779, -3.861377020970580443 ) ) ;
#37507 = CARTESIAN_POINT ( 'NONE',  ( 2.500000000000002220, -24.54166666393548368, 4.330127018922192761 ) ) ;
#37508 = ORIENTED_EDGE ( 'NONE', *, *, #35089, .F. ) ;
#37509 = CARTESIAN_POINT ( 'NONE',  ( -50.40829686548195099, -139.2500000013656063, -1.485763867205728284 ) ) ;
#37510 = CARTESIAN_POINT ( 'NONE',  ( 9.457646018065525792E-16, -87.31249999863440792, 5.148502694627439702 ) ) ;
#37511 = CARTESIAN_POINT ( 'NONE',  ( -49.85088928181150436, -129.6875000027312126, -1.666127454062680702 ) ) ;
#37512 = CYLINDRICAL_SURFACE ( 'NONE', #2864, 5.000000000000000000 ) ;
#37513 = CARTESIAN_POINT ( 'NONE',  ( -3.535533905932738641, -158.5000000027312126, 3.535533905932737309 ) ) ;
#37514 = CARTESIAN_POINT ( 'NONE',  ( 5.000000000000000000, 4.583333333333331261, -2.886751345948130876 ) ) ;
#37515 = CARTESIAN_POINT ( 'NONE',  ( 2.229367062500001939, -53.97916666530107221, 3.861377020970579999 ) ) ;
#37516 = CARTESIAN_POINT ( 'NONE',  ( -5.000000000000000000, -84.87499999726880162, 0.000000000000000000 ) ) ;
#37517 = CARTESIAN_POINT ( 'NONE',  ( 9.457646018065525792E-16, 24.93750000136559564, 5.148502694627439702 ) ) ;
#37518 = CARTESIAN_POINT ( 'NONE',  ( 5.000000000000000888, -106.5833333333333286, 2.886751345948126879 ) ) ;
#37519 = CARTESIAN_POINT ( 'NONE',  ( -6.972266317189433020E-16, -22.24999999999999645, -5.000000000000000000 ) ) ;
#37520 = CARTESIAN_POINT ( 'NONE',  ( 9.457646018065525792E-16, -44.31249999863440081, 5.148502694627439702 ) ) ;
#37521 = CARTESIAN_POINT ( 'NONE',  ( -4.999999999999999112, -4.791666663935479242, 2.886751345948131764 ) ) ;
#37522 = DIRECTION ( 'NONE',  ( 0.000000000000000000, 0.000000000000000000, 1.000000000000000000 ) ) ;
#37523 = CARTESIAN_POINT ( 'NONE',  ( 6.123233995736766282E-16, -170.0000000000000000, -5.000000000000000000 ) ) ;
#37524 = CARTESIAN_POINT ( 'NONE',  ( 2.229367062500001939, -84.22916666530107932, 3.861377020970579999 ) ) ;
#37525 = CARTESIAN_POINT ( 'NONE',  ( -4.458734124999997661, -103.2291666653010509, 2.574251347313722516 ) ) ;
#37526 = CARTESIAN_POINT ( 'NONE',  ( -4.458734124999999437, -5.562499998634402587, 0.000000000000000000 ) ) ;
#37527 = ORIENTED_EDGE ( 'NONE', *, *, #6767, .T. ) ;
#37528 = DIRECTION ( 'NONE',  ( -0.000000000000000000, 1.000000000000000000, -0.000000000000000000 ) ) ;
#37529 = CARTESIAN_POINT ( 'NONE',  ( 9.457646018065525792E-16, -93.06249999863440792, 5.148502694627439702 ) ) ;
#37530 = CARTESIAN_POINT ( 'NONE',  ( 2.071067811865475505, -164.9375000027312126, -5.000000000000000888 ) ) ;
#37531 = CARTESIAN_POINT ( 'NONE',  ( 2.229367062499998831, -90.89583333196773651, -3.861377020970580887 ) ) ;
#37532 = CARTESIAN_POINT ( 'NONE',  ( 2.229367062500001939, 12.77083333469892779, 3.861377020970579999 ) ) ;
#37533 = FACE_OUTER_BOUND ( 'NONE', #54707, .T. ) ;
#37534 =( BOUNDED_CURVE ( )  B_SPLINE_CURVE ( 2, ( #57467, #62290, #27542, #28170, #52625, #8558, #3743, #23365, #8255 ),
 .UNSPECIFIED., .F., .F. ) 
 B_SPLINE_CURVE_WITH_KNOTS ( ( 3, 2, 2, 2, 3 ),
 ( 0.7270833333333333037, 0.7277777777777777457, 0.7291666666666666297, 0.7305555555555555136, 0.7312499999999999556 ),
 .UNSPECIFIED. ) 
 CURVE ( )  GEOMETRIC_REPRESENTATION_ITEM ( )  RATIONAL_B_SPLINE_CURVE ( ( 0.9330127018922194093, 0.9330127018922194093, 1.000000000000000000, 0.8660254037844387076, 1.000000000000000000, 0.8660254037844387076, 1.000000000000000000, 0.9330127018922194093, 0.9330127018922194093 ) ) 
 REPRESENTATION_ITEM ( '' )  );
#37535 = CARTESIAN_POINT ( 'NONE',  ( -50.40829686548195099, -132.0000000013656063, -1.485763867205728284 ) ) ;
#37536 = CARTESIAN_POINT ( 'NONE',  ( 2.229367062500001939, -10.97916666530107044, 3.861377020970579999 ) ) ;
#37537 = B_SPLINE_CURVE_WITH_KNOTS ( 'NONE', 3,
 ( #30209, #50490, #26041, #45656, #5143, #24762 ),
 .UNSPECIFIED., .F., .F.,
 ( 4, 2, 4 ),
 ( 2.475503369438313607E-07, 0.002222330217055647119, 0.004444412883774350592 ),
 .UNSPECIFIED. ) ;
#37538 = CARTESIAN_POINT ( 'NONE',  ( -3.152548672688508926E-16, 14.18750000136559386, -5.148502694627439702 ) ) ;
#37539 = CARTESIAN_POINT ( 'NONE',  ( 4.458734124999998549, -55.97916666530107932, -2.574251347313721627 ) ) ;
#37540 = CARTESIAN_POINT ( 'NONE',  ( -2.500000000000000444, -22.04166666393548013, -4.330127018922193649 ) ) ;
#37541 = CARTESIAN_POINT ( 'NONE',  ( 2.229367062499998831, -9.645833331967738289, -3.861377020970580887 ) ) ;
#37542 = CARTESIAN_POINT ( 'NONE',  ( 1.975475456537005874E-15, -109.6249999972688158, 5.000000000000000000 ) ) ;
#37543 = ORIENTED_EDGE ( 'NONE', *, *, #54329, .F. ) ;
#37544 = CARTESIAN_POINT ( 'NONE',  ( -4.458734124999999437, -33.64583333196772941, -2.574251347313719407 ) ) ;
#37545 = CARTESIAN_POINT ( 'NONE',  ( -56.48576386720575471, -129.0000000013656063, -4.591703134518078322 ) ) ;
#37546 = CARTESIAN_POINT ( 'NONE',  ( 2.499999999999998668, -76.33333333333334281, -4.330127018922193649 ) ) ;
#37547 = CARTESIAN_POINT ( 'NONE',  ( -4.458734124999999437, -80.39583333196772230, -2.574251347313719407 ) ) ;
#37548 = CARTESIAN_POINT ( 'NONE',  ( 4.458734125000001214, 21.85416666803225993, 2.574251347313718519 ) ) ;
#37550 = EDGE_CURVE ( 'NONE', #27142, #8539, #33396, .T. ) ;
#37549 = CARTESIAN_POINT ( 'NONE',  ( -3.152548672688508926E-16, 13.43750000136559386, -5.148502694627439702 ) ) ;
#37551 = CARTESIAN_POINT ( 'NONE',  ( -2.499999999999996447, -47.83333333333332149, 4.330127018922195425 ) ) ;
#37552 = CARTESIAN_POINT ( 'NONE',  ( -58.80597590150559739, -135.0000000000000284, 3.242614290531460330 ) ) ;
#37553 = CARTESIAN_POINT ( 'NONE',  ( 4.458734124999998549, -80.97916666530106511, -2.574251347313721627 ) ) ;
#37554 = CARTESIAN_POINT ( 'NONE',  ( 1.060575238724906964E-15, -69.75000000000000000, 5.773502691896257311 ) ) ;
#37555 = CARTESIAN_POINT ( 'NONE',  ( 6.123233995736766282E-16, -170.0000000000000000, -5.000000000000000000 ) ) ;
#37556 = CARTESIAN_POINT ( 'NONE',  ( 2.499999999999998668, 19.79166666939785202, -4.330127018922193649 ) ) ;
#37557 = VERTEX_POINT ( 'NONE', #33171 ) ;
#37558 = CARTESIAN_POINT ( 'NONE',  ( -1.339745962155613812, -66.20534180126148271, -5.000000000000000000 ) ) ;
#37559 = CARTESIAN_POINT ( 'NONE',  ( -1.339745962155497683, -90.20534180126148271, -5.000000000000066613 ) ) ;
#37561 = CARTESIAN_POINT ( 'NONE',  ( -3.535250795749689387E-16, -27.24999999999999645, -5.773502691896257311 ) ) ;
#37560 = CARTESIAN_POINT ( 'NONE',  ( -5.000000000000000000, -108.8749999972688016, 0.000000000000000000 ) ) ;
#37562 = CARTESIAN_POINT ( 'NONE',  ( -2.229367062499996610, -34.14583333196772941, 3.861377020970582219 ) ) ;
#37563 = CARTESIAN_POINT ( 'NONE',  ( -4.999999999999998224, 5.083333333333332149, 2.886751345948131764 ) ) ;
#37564 = AXIS2_PLACEMENT_3D ( 'NONE', #39479, #53332, #33091 ) ;
#37565 = CARTESIAN_POINT ( 'NONE',  ( 2.499999999999998668, -29.20833333060214798, -4.330127018922193649 ) ) ;
#37567 = ORIENTED_EDGE ( 'NONE', *, *, #8025, .F. ) ;
#37566 = CARTESIAN_POINT ( 'NONE',  ( 2.229367062499998831, -61.64583333196774362, -3.861377020970580887 ) ) ;
#37568 = CARTESIAN_POINT ( 'NONE',  ( 1.975475456537005874E-15, -62.62499999726880873, 5.000000000000000000 ) ) ;
#37570 = VERTEX_POINT ( 'NONE', #48574 ) ;
#37569 = CARTESIAN_POINT ( 'NONE',  ( -2.229367062499996610, -11.39583333196773829, 3.861377020970582219 ) ) ;
#37571 = CARTESIAN_POINT ( 'NONE',  ( -5.000000000000000000, -77.00000000000000000, 0.000000000000000000 ) ) ;
#37572 = CARTESIAN_POINT ( 'NONE',  ( -52.10840900171896806, -137.1875000013656063, 3.393966926194110556 ) ) ;
#37573 = CARTESIAN_POINT ( 'NONE',  ( -2.229367062499996610, -50.39583333196772941, 3.861377020970582219 ) ) ;
#37574 = CARTESIAN_POINT ( 'NONE',  ( 5.000000000000000000, -78.29166666393547303, -2.886751345948129988 ) ) ;
#37576 = ORIENTED_EDGE ( 'NONE', *, *, #13377, .F. ) ;
#37575 = CARTESIAN_POINT ( 'NONE',  ( 1.339745962155612702, -65.16965819600733312, -5.000000000000000000 ) ) ;
#37577 = CARTESIAN_POINT ( 'NONE',  ( -56.66612745406270335, -148.3125000000000000, -5.149110718188516067 ) ) ;
#37578 = CARTESIAN_POINT ( 'NONE',  ( 2.229367062500001939, -21.22916666530107221, 3.861377020970579999 ) ) ;
#37580 = ORIENTED_EDGE ( 'NONE', *, *, #53528, .F. ) ;
#37579 = CARTESIAN_POINT ( 'NONE',  ( 4.458734125000001214, -56.14583333196774362, 2.574251347313718519 ) ) ;
#37581 = CARTESIAN_POINT ( 'NONE',  ( 1.846868145590735200, -141.2500000013656063, -4.458734125000000326 ) ) ;
#37582 = CARTESIAN_POINT ( 'NONE',  ( 2.229367062499998831, -101.8958333319677365, -3.861377020970580887 ) ) ;
#37583 = CARTESIAN_POINT ( 'NONE',  ( 6.158835246850667461E-14, -2.250000000000001776, -4.999999999999999112 ) ) ;
#37584 = ORIENTED_EDGE ( 'NONE', *, *, #7679, .F. ) ;
#37585 = CARTESIAN_POINT ( 'NONE',  ( -53.51423613279429503, -150.5000000013655779, 4.591703134518083651 ) ) ;
#37586 = CARTESIAN_POINT ( 'NONE',  ( -58.80597590150559739, -141.1250000027312126, 3.242614290531460330 ) ) ;
#37587 = CARTESIAN_POINT ( 'NONE',  ( 1.975475456537005874E-15, 18.24999999999999645, 5.000000000000000000 ) ) ;
#37588 = CARTESIAN_POINT ( 'NONE',  ( -2.229367062499996610, -6.145833331967740953, 3.861377020970582219 ) ) ;
#37589 = CARTESIAN_POINT ( 'NONE',  ( -2.229367062500000163, -96.72916666530105090, -3.861377020970580443 ) ) ;
#37590 = CARTESIAN_POINT ( 'NONE',  ( 3.152801135295366208, -148.8125000013655779, 3.152801135295367985 ) ) ;
#37591 = CARTESIAN_POINT ( 'NONE',  ( -4.458734124999999437, -26.64583333196773651, -2.574251347313719407 ) ) ;
#37592 = DIRECTION ( 'NONE',  ( 0.000000000000000000, 0.000000000000000000, 1.000000000000000000 ) ) ;
#37593 = CARTESIAN_POINT ( 'NONE',  ( -52.10840900171896806, -137.1875000013656063, 3.393966926194110556 ) ) ;
#37594 = CARTESIAN_POINT ( 'NONE',  ( 4.458734124999999437, -64.06249999863440792, -5.460374474430324690E-16 ) ) ;
#37595 = CARTESIAN_POINT ( 'NONE',  ( -6.972266317189433020E-16, -21.12499999726881228, -5.000000000000000000 ) ) ;
#37596 = DIRECTION ( 'NONE',  ( -0.000000000000000000, 1.000000000000000000, -0.000000000000000000 ) ) ;
#37597 = CARTESIAN_POINT ( 'NONE',  ( 2.730187237215162345E-16, -142.1875000013656063, -4.458734124999999437 ) ) ;
#37598 = CARTESIAN_POINT ( 'NONE',  ( 2.229367062499998831, 9.104166668032261711, -3.861377020970580887 ) ) ;
#37599 =( BOUNDED_CURVE ( )  B_SPLINE_CURVE ( 2, ( #207, #25596, #19805, #35247, #39102, #10797, #30409, #50033, #5991 ),
 .UNSPECIFIED., .F., .F. ) 
 B_SPLINE_CURVE_WITH_KNOTS ( ( 3, 2, 2, 2, 3 ),
 ( 0.6437500000000000444, 0.6444444444444444864, 0.6458333333333333703, 0.6472222222222222543, 0.6479166666666666963 ),
 .UNSPECIFIED. ) 
 CURVE ( )  GEOMETRIC_REPRESENTATION_ITEM ( )  RATIONAL_B_SPLINE_CURVE ( ( 0.9330127018922194093, 0.9330127018922194093, 1.000000000000000000, 0.8660254037844387076, 1.000000000000000000, 0.8660254037844387076, 1.000000000000000000, 0.9330127018922194093, 0.9330127018922194093 ) ) 
 REPRESENTATION_ITEM ( '' )  );
#37600 = EDGE_LOOP ( 'NONE', ( #31676, #8418, #10143, #8330 ) ) ;
#37601 = CARTESIAN_POINT ( 'NONE',  ( -6.972266317189433020E-16, -81.24999999999998579, -5.000000000000000000 ) ) ;
#37602 = DIRECTION ( 'NONE',  ( 0.000000000000000000, 0.000000000000000000, 1.000000000000000000 ) ) ;
#37604 = CARTESIAN_POINT ( 'NONE',  ( -2.229367062499996610, -25.14583333196773651, 3.861377020970582219 ) ) ;
#37603 = CARTESIAN_POINT ( 'NONE',  ( 1.060575238724906964E-15, -92.74999999999998579, 5.773502691896257311 ) ) ;
#37605 = CARTESIAN_POINT ( 'NONE',  ( 2.500000000000002220, -14.54166666393548191, 4.330127018922192761 ) ) ;
#37606 = CARTESIAN_POINT ( 'NONE',  ( 2.229367062499998831, -70.89583333196773651, -3.861377020970580887 ) ) ;
#37607 = ADVANCED_FACE ( 'NONE', ( #43743 ), #38601, .T. ) ;
#37608 = TOROIDAL_SURFACE ( 'NONE', #47880, 10.12668159690567649, 0.7733184030943209830 ) ;
#37609 = CARTESIAN_POINT ( 'NONE',  ( -2.229367062499996610, 26.60416666803225993, 3.861377020970582219 ) ) ;
#37610 = CARTESIAN_POINT ( 'NONE',  ( -2.499999999999996447, -17.70833333060214443, 4.330127018922195425 ) ) ;
#37611 = CARTESIAN_POINT ( 'NONE',  ( -59.29741812935640155, -146.6250000013656063, -2.196230717870135685 ) ) ;
#37612 = CARTESIAN_POINT ( 'NONE',  ( 4.458734124999998549, 5.270833334698926897, -2.574251347313721627 ) ) ;
#37613 = CARTESIAN_POINT ( 'NONE',  ( -4.999999999999998224, -62.79166666393546592, 2.886751345948131764 ) ) ;
#37614 = CYLINDRICAL_SURFACE ( 'NONE', #47977, 5.000000000000000000 ) ;
#37615 = CARTESIAN_POINT ( 'NONE',  ( 2.229367062500001939, 7.020833334698928674, 3.861377020970579999 ) ) ;
#37616 = CARTESIAN_POINT ( 'NONE',  ( 2.229367062499998831, -71.64583333196773651, -3.861377020970580887 ) ) ;
#37617 = CARTESIAN_POINT ( 'NONE',  ( -4.458734124999999437, -21.64583333196774007, -2.574251347313719407 ) ) ;
#37618 = CARTESIAN_POINT ( 'NONE',  ( -5.000000000000000000, -5.999999999999998224, 0.000000000000000000 ) ) ;
#37619 = CARTESIAN_POINT ( 'NONE',  ( 4.458734124999999437, -158.5000000013656631, 1.846868145590737864 ) ) ;
#37620 = LINE ( 'NONE', #61768, #9946 ) ;
#37621 = CARTESIAN_POINT ( 'NONE',  ( 4.458734124999999437, -61.81249999863440081, -5.460374474430324690E-16 ) ) ;
#37622 = CARTESIAN_POINT ( 'NONE',  ( -2.500000000000000444, -101.0416666639354588, -4.330127018922193649 ) ) ;
#37623 = CARTESIAN_POINT ( 'NONE',  ( 5.000000000000000888, 15.41666666666666607, 2.886751345948126879 ) ) ;
#37624 = CARTESIAN_POINT ( 'NONE',  ( -4.458734124999999437, -40.31249999863440081, 0.000000000000000000 ) ) ;
#37625 = CARTESIAN_POINT ( 'NONE',  ( -1.339745962155613812, -84.20534180126149693, -5.000000000000000000 ) ) ;
#37626 = CARTESIAN_POINT ( 'NONE',  ( -4.458734124999999437, -108.5624999986343937, 0.000000000000000000 ) ) ;
#37627 = CARTESIAN_POINT ( 'NONE',  ( 4.458734124999999437, -67.06249999863440792, -5.460374474430324690E-16 ) ) ;
#37628 = CARTESIAN_POINT ( 'NONE',  ( -5.000000000000000000, -53.99999999999999289, 0.000000000000000000 ) ) ;
#37629 = CARTESIAN_POINT ( 'NONE',  ( 1.339745962155615144, -57.58034179853029144, 4.999999999999999112 ) ) ;
#37630 = DIRECTION ( 'NONE',  ( 0.8660254037844415942, -0.000000000000000000, 0.4999999999999948930 ) ) ;
#37631 = ORIENTED_EDGE ( 'NONE', *, *, #49591, .F. ) ;
#37632 = CARTESIAN_POINT ( 'NONE',  ( -5.000000000000000000, -85.08333333333332860, -2.886751345948128211 ) ) ;
#37633 =( BOUNDED_CURVE ( )  B_SPLINE_CURVE ( 2, ( #50659, #6598, #26213, #5969, #60326, #41001, #45833, #5642, #505 ),
 .UNSPECIFIED., .F., .F. ) 
 B_SPLINE_CURVE_WITH_KNOTS ( ( 3, 2, 2, 2, 3 ),
 ( 0.6660714285714285365, 0.6666666666666666297, 0.6678571428571428159, 0.6690476190476190022, 0.6696428571428570953 ),
 .UNSPECIFIED. ) 
 CURVE ( )  GEOMETRIC_REPRESENTATION_ITEM ( )  RATIONAL_B_SPLINE_CURVE ( ( 0.9330127018922194093, 0.9330127018922194093, 1.000000000000000000, 0.8660254037844387076, 1.000000000000000000, 0.8660254037844387076, 1.000000000000000000, 0.9330127018922194093, 0.9330127018922194093 ) ) 
 REPRESENTATION_ITEM ( '' )  );
#37634 = CARTESIAN_POINT ( 'NONE',  ( 5.000000000000000000, -144.1250000027312126, 0.000000000000000000 ) ) ;
#37635 = CARTESIAN_POINT ( 'NONE',  ( 2.499999999999998668, -13.33333333333333570, -4.330127018922193649 ) ) ;
#37636 = CARTESIAN_POINT ( 'NONE',  ( 4.458734124999999437, -15.81249999863440436, -5.460374474430324690E-16 ) ) ;
#37637 = CARTESIAN_POINT ( 'NONE',  ( -2.229367062500000163, -79.47916666530106511, -3.861377020970580443 ) ) ;
#37638 = CARTESIAN_POINT ( 'NONE',  ( -6.972266317189433020E-16, -5.124999997268812280, -5.000000000000000000 ) ) ;
#37639 = CARTESIAN_POINT ( 'NONE',  ( 5.000000000000000888, -11.45833333060214798, 2.886751345948126879 ) ) ;
#37641 = EDGE_LOOP ( 'NONE', ( #12971, #34314, #18856, #34073 ) ) ;
#37640 = CARTESIAN_POINT ( 'NONE',  ( 2.229367062499998831, -44.64583333196774362, -3.861377020970580887 ) ) ;
#37642 = CARTESIAN_POINT ( 'NONE',  ( -2.500000000000000444, 29.83333333333333215, -4.330127018922193649 ) ) ;
#37644 = EDGE_LOOP ( 'NONE', ( #13083, #54570, #25382, #28704 ) ) ;
#37643 = CARTESIAN_POINT ( 'NONE',  ( -4.458734124999998549, 9.520833334698927786, 2.574251347313722516 ) ) ;
#37645 = CYLINDRICAL_SURFACE ( 'NONE', #16575, 5.000000000000000000 ) ;
#37646 = CARTESIAN_POINT ( 'NONE',  ( 5.000000000000000000, -62.41666666666666430, -2.886751345948129988 ) ) ;
#37647 = CARTESIAN_POINT ( 'NONE',  ( -3.152801135295367985, -162.0625000013656063, 3.152801135295367096 ) ) ;
#37648 = CARTESIAN_POINT ( 'NONE',  ( 4.458734125000001214, -38.14583333196773651, 2.574251347313718519 ) ) ;
#37649 = CARTESIAN_POINT ( 'NONE',  ( -1.339745962155613812, -11.08034179853029322, -5.000000000000000000 ) ) ;
#37650 = CARTESIAN_POINT ( 'NONE',  ( -4.458734124999999437, -81.39583333196773651, -2.574251347313719407 ) ) ;
#37651 = CARTESIAN_POINT ( 'NONE',  ( 5.000000000000000000, -165.0625000000000000, 2.071067811865478614 ) ) ;
#37652 = CARTESIAN_POINT ( 'NONE',  ( -5.000000000000000000, -30.08333333333332860, -2.886751345948128211 ) ) ;
#37653 = CARTESIAN_POINT ( 'NONE',  ( -58.39396692619412477, -132.6875000013656063, 2.891590998281057701 ) ) ;
#37654 = VECTOR ( 'NONE', #29784, 1000.000000000000000 ) ;
#37655 = CARTESIAN_POINT ( 'NONE',  ( 9.457646018065525792E-16, -7.312499998634405252, 5.148502694627439702 ) ) ;
#37656 = VECTOR ( 'NONE', #183, 1000.000000000000000 ) ;
#37657 = CARTESIAN_POINT ( 'NONE',  ( 4.458734124999999437, -43.06249999863440081, -5.460374474430324690E-16 ) ) ;
#37658 = CARTESIAN_POINT ( 'NONE',  ( 5.000000000000000000, -26.41666666666666430, -2.886751345948130876 ) ) ;
#37659 = CARTESIAN_POINT ( 'NONE',  ( 4.458734125000001214, -82.14583333196772230, 2.574251347313718519 ) ) ;
#37660 = CARTESIAN_POINT ( 'NONE',  ( 0.000000000000000000, -170.0000000000000000, 0.000000000000000000 ) ) ;
#37661 = ORIENTED_EDGE ( 'NONE', *, *, #50764, .F. ) ;
#37662 = CARTESIAN_POINT ( 'NONE',  ( -60.14911071818854538, -153.1875000027312410, 1.666127454062681368 ) ) ;
#37663 = CARTESIAN_POINT ( 'NONE',  ( -3.152548672688508926E-16, -68.81249999863439371, -5.148502694627439702 ) ) ;
#37664 = CARTESIAN_POINT ( 'NONE',  ( -8.190561711645485556E-16, -145.9375000013656063, 4.458734124999999437 ) ) ;
#37665 = VERTEX_POINT ( 'NONE', #8717 ) ;
#37666 = CARTESIAN_POINT ( 'NONE',  ( -9.184850993605147944E-16, -164.2500000000000000, 5.000000000000000000 ) ) ;
#37667 = CARTESIAN_POINT ( 'NONE',  ( 1.339745962155565406, -3.580341798530294550, 5.000000000000028422 ) ) ;
#37668 = CARTESIAN_POINT ( 'NONE',  ( 4.458734124999998549, -12.97916666530107044, -2.574251347313721627 ) ) ;
#37669 = CARTESIAN_POINT ( 'NONE',  ( -57.46284108482265651, -147.0625000027312126, 4.819101127000238627 ) ) ;
#37670 = CARTESIAN_POINT ( 'NONE',  ( 4.458734124999999437, 2.187500001365593416, -5.460374474430324690E-16 ) ) ;
#37671 = DIRECTION ( 'NONE',  ( 0.000000000000000000, 0.000000000000000000, 1.000000000000000000 ) ) ;
#37672 = CARTESIAN_POINT ( 'NONE',  ( 4.458734124999999437, -156.4375000013655779, 0.000000000000000000 ) ) ;
#37673 = CARTESIAN_POINT ( 'NONE',  ( 2.229367062500001939, 24.77083333469892779, 3.861377020970579999 ) ) ;
#37674 = ORIENTED_EDGE ( 'NONE', *, *, #42116, .F. ) ;
#37675 = CARTESIAN_POINT ( 'NONE',  ( 2.229367062500001939, -92.97916666530106511, 3.861377020970579999 ) ) ;
#37676 = CARTESIAN_POINT ( 'NONE',  ( -1.339745962155613812, -68.20534180126148271, -5.000000000000000000 ) ) ;
#37677 = CARTESIAN_POINT ( 'NONE',  ( -2.480964764533239819E-13, -95.62499999726883004, 5.000000000000000000 ) ) ;
#37678 = CARTESIAN_POINT ( 'NONE',  ( 4.458734125000001214, -6.895833331967734736, 2.574251347313718519 ) ) ;
#37679 = EDGE_CURVE ( 'NONE', #13190, #43260, #14041, .T. ) ;
#37680 = CARTESIAN_POINT ( 'NONE',  ( 2.499999999999998668, -51.33333333333332860, -4.330127018922193649 ) ) ;
#37681 = CARTESIAN_POINT ( 'NONE',  ( 1.339745962155612702, -23.16965819600733312, -5.000000000000000000 ) ) ;
#37682 = CARTESIAN_POINT ( 'NONE',  ( 2.499999999999998668, -67.33333333333332860, -4.330127018922193649 ) ) ;
#37683 = CARTESIAN_POINT ( 'NONE',  ( 2.499999999999998668, -36.20833333060213732, -4.330127018922193649 ) ) ;
#37684 = CARTESIAN_POINT ( 'NONE',  ( 5.000000000000000000, -49.37499999726880873, -6.123233995736766282E-16 ) ) ;
#37685 = CARTESIAN_POINT ( 'NONE',  ( -4.458734124999997661, 21.77083333469892779, 2.574251347313722516 ) ) ;
#37686 = CARTESIAN_POINT ( 'NONE',  ( -6.972266317189433020E-16, -4.249999999999997335, -5.000000000000000000 ) ) ;
#37687 = CARTESIAN_POINT ( 'NONE',  ( -2.229367062499996610, 24.85416666803225993, 3.861377020970582219 ) ) ;
#37688 = CARTESIAN_POINT ( 'NONE',  ( -4.458734124999999437, -57.39583333196773651, -2.574251347313719407 ) ) ;
#37689 = CARTESIAN_POINT ( 'NONE',  ( 2.229367062500001939, -4.229166665301070438, 3.861377020970579999 ) ) ;
#37690 = CARTESIAN_POINT ( 'NONE',  ( -2.500000000000000444, -34.04166666393547303, -4.330127018922193649 ) ) ;
#37691 = CARTESIAN_POINT ( 'NONE',  ( -4.999999999999999112, 11.08333333333333393, 2.886751345948131764 ) ) ;
#37692 = CARTESIAN_POINT ( 'NONE',  ( 5.000000000000000888, -143.0625000027312126, -2.071067811865475505 ) ) ;
#37693 = CARTESIAN_POINT ( 'NONE',  ( -57.46284108482265651, -145.0625000027312126, 4.819101127000238627 ) ) ;
#37694 = CARTESIAN_POINT ( 'NONE',  ( 4.458734124999999437, -45.81249999863440081, -5.460374474430324690E-16 ) ) ;
#37695 = CARTESIAN_POINT ( 'NONE',  ( -5.000000000000000000, -85.87499999726880162, 0.000000000000000000 ) ) ;
#37696 = VECTOR ( 'NONE', #28457, 1000.000000000000000 ) ;
#37697 = CARTESIAN_POINT ( 'NONE',  ( -56.48576386720575471, -135.0000000013656347, -4.591703134518078322 ) ) ;
#37698 = CARTESIAN_POINT ( 'NONE',  ( 6.123233995736766282E-16, -170.0000000000000000, -5.000000000000000000 ) ) ;
#37699 = ADVANCED_FACE ( 'NONE', ( #53405 ), #4514, .F. ) ;
#37700 = LINE ( 'NONE', #4242, #62416 ) ;
#37701 = VECTOR ( 'NONE', #19886, 1000.000000000000000 ) ;
#37702 = EDGE_CURVE ( 'NONE', #6256, #28617, #33773, .T. ) ;
#37703 = CARTESIAN_POINT ( 'NONE',  ( 2.229367062500001939, -91.22916666530106511, 3.861377020970579999 ) ) ;
#37704 = CARTESIAN_POINT ( 'NONE',  ( -4.458734125000000326, -156.1250000013655779, 1.846868145590734089 ) ) ;
#37705 = CARTESIAN_POINT ( 'NONE',  ( 2.499999999999998668, -32.33333333333332860, -4.330127018922193649 ) ) ;
#37706 = DIRECTION ( 'NONE',  ( 0.000000000000000000, 0.000000000000000000, 1.000000000000000000 ) ) ;
#37707 = VERTEX_POINT ( 'NONE', #48257 ) ;
#37708 = CARTESIAN_POINT ( 'NONE',  ( -2.229367062500000163, 17.27083333469892779, -3.861377020970580443 ) ) ;
#37709 = ORIENTED_EDGE ( 'NONE', *, *, #40979, .F. ) ;
#37710 = CARTESIAN_POINT ( 'NONE',  ( 4.458734124999998549, -98.72916666530105090, -2.574251347313721627 ) ) ;
#37711 = CARTESIAN_POINT ( 'NONE',  ( 2.229367062499998831, 9.104166668032261711, -3.861377020970580887 ) ) ;
#37712 = CARTESIAN_POINT ( 'NONE',  ( -2.500000000000000444, 9.958333336064519870, -4.330127018922193649 ) ) ;
#37713 = CARTESIAN_POINT ( 'NONE',  ( -1.339745962155727277, -59.79465819873853150, 4.999999999999933387 ) ) ;
#37714 = CARTESIAN_POINT ( 'NONE',  ( -5.000000000000000000, 1.999999999999998224, 0.000000000000000000 ) ) ;
#37716 = EDGE_CURVE ( 'NONE', #52361, #8855, #9534, .T. ) ;
#37715 =( BOUNDED_CURVE ( )  B_SPLINE_CURVE ( 2, ( #11889, #25744, #49854, #26377, #11258, #35714, #1960, #10936, #46317 ),
 .UNSPECIFIED., .F., .F. ) 
 B_SPLINE_CURVE_WITH_KNOTS ( ( 3, 2, 2, 2, 3 ),
 ( 0.2270833333333333315, 0.2277777777777777735, 0.2291666666666666574, 0.2305555555555555691, 0.2312500000000000111 ),
 .UNSPECIFIED. ) 
 CURVE ( )  GEOMETRIC_REPRESENTATION_ITEM ( )  RATIONAL_B_SPLINE_CURVE ( ( 0.9330127018922194093, 0.9330127018922194093, 1.000000000000000000, 0.8660254037844387076, 1.000000000000000000, 0.8660254037844387076, 1.000000000000000000, 0.9330127018922194093, 0.9330127018922194093 ) ) 
 REPRESENTATION_ITEM ( '' )  );
#37717 = CARTESIAN_POINT ( 'NONE',  ( -2.229367062499996610, -61.14583333196774362, 3.861377020970582219 ) ) ;
#37718 = CARTESIAN_POINT ( 'NONE',  ( -5.000000000000000000, -52.95833333060214443, -2.886751345948128211 ) ) ;
#37719 = CARTESIAN_POINT ( 'NONE',  ( -3.535250795749689387E-16, -80.25000000000000000, -5.773502691896257311 ) ) ;
#37720 = CARTESIAN_POINT ( 'NONE',  ( 4.458734124999999437, -27.81249999863440081, -5.460374474430324690E-16 ) ) ;
#37721 = DIRECTION ( 'NONE',  ( -0.000000000000000000, 1.000000000000000000, -0.000000000000000000 ) ) ;
#37722 = CARTESIAN_POINT ( 'NONE',  ( 2.500000000000002220, -63.66666666666666430, 4.330127018922192761 ) ) ;
#37723 = FACE_OUTER_BOUND ( 'NONE', #4318, .T. ) ;
#37724 = CARTESIAN_POINT ( 'NONE',  ( -2.499999999999996447, -39.83333333333332860, 4.330127018922195425 ) ) ;
#37725 = CARTESIAN_POINT ( 'NONE',  ( 1.975475456537005874E-15, -75.62499999726880162, 5.000000000000000000 ) ) ;
#37727 = CARTESIAN_POINT ( 'NONE',  ( -2.229367062500000163, -20.72916666530107221, -3.861377020970580443 ) ) ;
#37726 = CARTESIAN_POINT ( 'NONE',  ( 1.062108568985190270E-13, -26.12499999726881583, -4.999999999999999112 ) ) ;
#37728 = CARTESIAN_POINT ( 'NONE',  ( 5.000000000000000000, -107.2916666639354730, -2.886751345948130876 ) ) ;
#37729 = CARTESIAN_POINT ( 'NONE',  ( 4.458734125000001214, -64.89583333196773651, 2.574251347313718519 ) ) ;
#37730 = CARTESIAN_POINT ( 'NONE',  ( -3.152801135295367985, -148.0625000013655779, 3.152801135295367096 ) ) ;
#37731 = CARTESIAN_POINT ( 'NONE',  ( -4.458734124999999437, -75.39583333196773651, -2.574251347313719407 ) ) ;
#37732 = CARTESIAN_POINT ( 'NONE',  ( -58.39396692619412477, -142.6875000013656063, 2.891590998281057701 ) ) ;
#37733 = CARTESIAN_POINT ( 'NONE',  ( -4.458734124999999437, -26.64583333196773651, -2.574251347313719407 ) ) ;
#37734 =( BOUNDED_CURVE ( )  B_SPLINE_CURVE ( 2, ( #49373, #5318, #24936, #35224, #499, #59349, #34905, #15282, #5959 ),
 .UNSPECIFIED., .F., .F. ) 
 B_SPLINE_CURVE_WITH_KNOTS ( ( 3, 2, 2, 2, 3 ),
 ( 0.5270833333333333481, 0.5277777777777777901, 0.5291666666666666741, 0.5305555555555555580, 0.5312500000000000000 ),
 .UNSPECIFIED. ) 
 CURVE ( )  GEOMETRIC_REPRESENTATION_ITEM ( )  RATIONAL_B_SPLINE_CURVE ( ( 0.9330127018922194093, 0.9330127018922194093, 1.000000000000000000, 0.8660254037844387076, 1.000000000000000000, 0.8660254037844387076, 1.000000000000000000, 0.9330127018922194093, 0.9330127018922194093 ) ) 
 REPRESENTATION_ITEM ( '' )  );
#37735 = CARTESIAN_POINT ( 'NONE',  ( 5.000000000000000888, -68.45833333060214443, 2.886751345948126879 ) ) ;
#37736 = ORIENTED_EDGE ( 'NONE', *, *, #14103, .T. ) ;
#37737 = EDGE_CURVE ( 'NONE', #7641, #45160, #39955, .T. ) ;
#37738 = CARTESIAN_POINT ( 'NONE',  ( 5.000000000000000000, -1.500000000000001332, -6.123233995736766282E-16 ) ) ;
#37739 = EDGE_LOOP ( 'NONE', ( #52394, #34060, #8072, #40005 ) ) ;
#37740 = CARTESIAN_POINT ( 'NONE',  ( -4.458734124999999437, -66.64583333196773651, -2.574251347313719407 ) ) ;
#37741 = CARTESIAN_POINT ( 'NONE',  ( 1.975475456537005874E-15, -7.624999997268812280, 5.000000000000000000 ) ) ;
#37742 = CARTESIAN_POINT ( 'NONE',  ( 7.907996613752301229, 3.055722423191984838, -7.792112796859423263 ) ) ;
#37743 = ORIENTED_EDGE ( 'NONE', *, *, #34105, .F. ) ;
#37744 = VECTOR ( 'NONE', #24703, 1000.000000000000000 ) ;
#37745 = CARTESIAN_POINT ( 'NONE',  ( -56.66612745406270335, -125.3125000000000142, -5.149110718188516067 ) ) ;
#37746 = DIRECTION ( 'NONE',  ( -0.000000000000000000, 1.000000000000000000, -0.000000000000000000 ) ) ;
#37747 = CARTESIAN_POINT ( 'NONE',  ( 4.458734125000001214, -54.14583333196773651, 2.574251347313718519 ) ) ;
#37748 = AXIS2_PLACEMENT_3D ( 'NONE', #36688, #47596, #18329 ) ;
#37749 = EDGE_LOOP ( 'NONE', ( #8901, #52056, #7472, #51939 ) ) ;
#37750 = CARTESIAN_POINT ( 'NONE',  ( 1.975475456537005874E-15, -54.74999999999999289, 5.000000000000000000 ) ) ;
#37751 = VECTOR ( 'NONE', #25243, 1000.000000000000000 ) ;
#37752 = CARTESIAN_POINT ( 'NONE',  ( 2.229367062499998831, 10.35416666803225993, -3.861377020970580887 ) ) ;
#37753 = CARTESIAN_POINT ( 'NONE',  ( 9.457646018065525792E-16, 17.93750000136559208, 5.148502694627439702 ) ) ;
#37754 = CARTESIAN_POINT ( 'NONE',  ( -56.48576386720575471, -146.7500000013655495, -4.591703134518078322 ) ) ;
#37755 = CARTESIAN_POINT ( 'NONE',  ( -5.000000000000000000, -2.000000000000001776, 0.000000000000000000 ) ) ;
#37756 = CARTESIAN_POINT ( 'NONE',  ( 3.152801135295366208, -168.5625000013656063, 3.152801135295367985 ) ) ;
#37757 = ORIENTED_EDGE ( 'NONE', *, *, #42923, .T. ) ;
#37758 = CARTESIAN_POINT ( 'NONE',  ( -4.458734124999999437, -77.31249999863440792, 0.000000000000000000 ) ) ;
#37759 = CARTESIAN_POINT ( 'NONE',  ( -6.972266317189433020E-16, -40.24999999999999289, -5.000000000000000000 ) ) ;
#37760 = CARTESIAN_POINT ( 'NONE',  ( 4.458734124999998549, 8.270833334698926009, -2.574251347313721627 ) ) ;
#37761 = EDGE_CURVE ( 'NONE', #54515, #42874, #54368, .T. ) ;
#37762 = EDGE_CURVE ( 'NONE', #21496, #13829, #5029, .T. ) ;
#37763 = CARTESIAN_POINT ( 'NONE',  ( 2.071067811865392461, -140.3125000027312694, 5.000000000000084377 ) ) ;
#37764 = EDGE_CURVE ( 'NONE', #59122, #41205, #11233, .T. ) ;
#37765 = CARTESIAN_POINT ( 'NONE',  ( -4.458734124999998549, -62.47916666530106511, 2.574251347313722516 ) ) ;
#37766 = CARTESIAN_POINT ( 'NONE',  ( 2.500000000000002220, -22.54166666393548013, 4.330127018922192761 ) ) ;
#37767 = CARTESIAN_POINT ( 'NONE',  ( 0.000000000000000000, -120.0000000000000000, 5.000000000000000000 ) ) ;
#37768 = CARTESIAN_POINT ( 'NONE',  ( 5.000000000000000000, -28.29166666393548013, -2.886751345948130876 ) ) ;
#37769 = CARTESIAN_POINT ( 'NONE',  ( -75.00000000000002842, 0.000000000000000000, 5.000000000000000000 ) ) ;
#37770 = CARTESIAN_POINT ( 'NONE',  ( -5.000000000000000000, -83.95833333060214443, -2.886751345948128211 ) ) ;
#37771 = CARTESIAN_POINT ( 'NONE',  ( -50.01589407740564042, -139.6250000000000284, 0.3983568153799778022 ) ) ;
#37772 = CARTESIAN_POINT ( 'NONE',  ( 9.457646018065525792E-16, -39.06249999863440081, 5.148502694627439702 ) ) ;
#37773 = CARTESIAN_POINT ( 'NONE',  ( -2.229367062499996610, -27.39583333196774007, 3.861377020970582219 ) ) ;
#37774 = CARTESIAN_POINT ( 'NONE',  ( 0.000000000000000000, -170.0000000000000000, 5.000000000000000000 ) ) ;
#37775 = CARTESIAN_POINT ( 'NONE',  ( 2.499999999999998668, 29.66666666666666430, -4.330127018922193649 ) ) ;
#37776 = CARTESIAN_POINT ( 'NONE',  ( 5.000000000000000000, -153.1250000027312126, 0.000000000000000000 ) ) ;
#37777 = ORIENTED_EDGE ( 'NONE', *, *, #1935, .T. ) ;
#37778 = CARTESIAN_POINT ( 'NONE',  ( 2.229367062500001939, -110.2291666653010651, 3.861377020970579999 ) ) ;
#37779 = CARTESIAN_POINT ( 'NONE',  ( -3.152548672688508926E-16, -29.56249999863440436, -5.148502694627439702 ) ) ;
#37780 = CARTESIAN_POINT ( 'NONE',  ( -5.000000000000000000, -66.87499999726881583, 0.000000000000000000 ) ) ;
#37781 = ADVANCED_FACE ( 'NONE', ( #29903 ), #25735, .T. ) ;
#37782 = CARTESIAN_POINT ( 'NONE',  ( -59.59170313451811296, -147.7500000013655779, 1.485763867205729394 ) ) ;
#37783 = CARTESIAN_POINT ( 'NONE',  ( -3.535533905932738641, -146.3750000000000000, 3.535533905932737309 ) ) ;
#37784 = CARTESIAN_POINT ( 'NONE',  ( -2.229367062500000163, -31.47916666530107577, -3.861377020970580443 ) ) ;
#37785 = EDGE_CURVE ( 'NONE', #36016, #6026, #42407, .T. ) ;
#37786 = CARTESIAN_POINT ( 'NONE',  ( 2.229367062500001939, -71.22916666530107932, 3.861377020970579999 ) ) ;
#37787 = CARTESIAN_POINT ( 'NONE',  ( -3.152801135295367985, -168.0625000013656063, 3.152801135295367096 ) ) ;
#37788 = CARTESIAN_POINT ( 'NONE',  ( 4.458734125000000326, -29.89583333196773651, 2.574251347313718519 ) ) ;
#37789 = DIRECTION ( 'NONE',  ( 0.000000000000000000, 0.000000000000000000, -1.000000000000000000 ) ) ;
#37790 = CARTESIAN_POINT ( 'NONE',  ( 5.000000000000000000, -5.374999997268811391, -6.123233995736766282E-16 ) ) ;
#37791 = CARTESIAN_POINT ( 'NONE',  ( 5.000000000000000000, -18.50000000000000355, -6.123233995736766282E-16 ) ) ;
#37792 = CARTESIAN_POINT ( 'NONE',  ( 3.152801135295367541, -146.3125000013655779, -3.152801135295367541 ) ) ;
#37793 = EDGE_LOOP ( 'NONE', ( #13292, #24811, #14872, #56149 ) ) ;
#37794 = CARTESIAN_POINT ( 'NONE',  ( -5.000000000000000000, -82.08333333333332860, -2.886751345948128211 ) ) ;
#37795 = CARTESIAN_POINT ( 'NONE',  ( -4.458734124999999437, -56.56249999863440081, 0.000000000000000000 ) ) ;
#37796 =( BOUNDED_CURVE ( )  B_SPLINE_CURVE ( 2, ( #57657, #32565, #52187, #17773, #46725, #32244, #22292, #27735, #23554 ),
 .UNSPECIFIED., .F., .F. ) 
 B_SPLINE_CURVE_WITH_KNOTS ( ( 3, 2, 2, 2, 3 ),
 ( 0.04107142857142857123, 0.04166666666666666435, 0.04285714285714285754, 0.04404761904761905073, 0.04464285714285714385 ),
 .UNSPECIFIED. ) 
 CURVE ( )  GEOMETRIC_REPRESENTATION_ITEM ( )  RATIONAL_B_SPLINE_CURVE ( ( 0.9330127018922194093, 0.9330127018922194093, 1.000000000000000000, 0.8660254037844387076, 1.000000000000000000, 0.8660254037844387076, 1.000000000000000000, 0.9330127018922194093, 0.9330127018922194093 ) ) 
 REPRESENTATION_ITEM ( '' )  );
#37797 = AXIS2_PLACEMENT_3D ( 'NONE', #23914, #38083, #62222 ) ;
#37798 = CARTESIAN_POINT ( 'NONE',  ( 1.060575238724906964E-15, 25.37500000273118417, 5.773502691896257311 ) ) ;
#37799 = LINE ( 'NONE', #27503, #52490 ) ;
#37800 = CARTESIAN_POINT ( 'NONE',  ( 2.500000000000002220, 24.33333333333333215, 4.330127018922192761 ) ) ;
#37801 = VECTOR ( 'NONE', #28670, 1000.000000000000000 ) ;
#37802 = DIRECTION ( 'NONE',  ( -0.000000000000000000, 1.000000000000000000, -0.000000000000000000 ) ) ;
#37803 = CARTESIAN_POINT ( 'NONE',  ( -3.152548672688508926E-16, -0.5624999986344053626, -5.148502694627439702 ) ) ;
#37804 = CARTESIAN_POINT ( 'NONE',  ( -5.000000000000000000, -51.87499999726881583, 0.000000000000000000 ) ) ;
#37805 = CARTESIAN_POINT ( 'NONE',  ( -2.071067811865415109, -164.3125000000000000, 5.000000000000062172 ) ) ;
#37806 = CARTESIAN_POINT ( 'NONE',  ( -2.229367062499996610, 9.604166668032261711, 3.861377020970582219 ) ) ;
#37807 = ORIENTED_EDGE ( 'NONE', *, *, #49164, .T. ) ;
#37808 = CYLINDRICAL_SURFACE ( 'NONE', #28415, 5.000000000000000000 ) ;
#37809 = ORIENTED_EDGE ( 'NONE', *, *, #13455, .T. ) ;
#37810 = DIRECTION ( 'NONE',  ( -0.000000000000000000, 1.000000000000000000, -0.000000000000000000 ) ) ;
#37811 = CARTESIAN_POINT ( 'NONE',  ( 4.458734125000001214, -48.89583333196772941, 2.574251347313718519 ) ) ;
#37812 = CARTESIAN_POINT ( 'NONE',  ( 4.458734125000000326, -158.6250000013655779, -1.846868145590734978 ) ) ;
#37813 = CARTESIAN_POINT ( 'NONE',  ( 2.500000000000002220, -51.54166666393547303, 4.330127018922192761 ) ) ;
#37814 = VERTEX_POINT ( 'NONE', #16080 ) ;
#37815 = CARTESIAN_POINT ( 'NONE',  ( 2.229367062499998831, -24.64583333196773651, -3.861377020970580887 ) ) ;
#37816 = ORIENTED_EDGE ( 'NONE', *, *, #50866, .F. ) ;
#37817 = CARTESIAN_POINT ( 'NONE',  ( -5.000000000000000000, -96.08333333333331439, -2.886751345948128211 ) ) ;
#37818 = CARTESIAN_POINT ( 'NONE',  ( -1.846868145590737420, -161.7500000013655495, 4.458734124999999437 ) ) ;
#37819 = DIRECTION ( 'NONE',  ( -0.000000000000000000, 1.000000000000000000, -0.000000000000000000 ) ) ;
#37820 = CARTESIAN_POINT ( 'NONE',  ( -57.46284108482265651, -137.9375000000000284, 4.819101127000239515 ) ) ;
#37821 = CARTESIAN_POINT ( 'NONE',  ( -3.152548672688508926E-16, -38.81249999863440081, -5.148502694627439702 ) ) ;
#37822 = EDGE_LOOP ( 'NONE', ( #25782, #30270, #30907, #36171 ) ) ;
#37823 = CARTESIAN_POINT ( 'NONE',  ( 2.229367062499998831, -83.64583333196773651, -3.861377020970580887 ) ) ;
#37824 = CARTESIAN_POINT ( 'NONE',  ( 4.458734125000001214, 23.10416666803225993, 2.574251347313718519 ) ) ;
#37825 = DIRECTION ( 'NONE',  ( -0.000000000000000000, 1.000000000000000000, -0.000000000000000000 ) ) ;
#37826 = ORIENTED_EDGE ( 'NONE', *, *, #25646, .T. ) ;
#37827 = CARTESIAN_POINT ( 'NONE',  ( -5.000000000000000000, -59.87499999726880873, 0.000000000000000000 ) ) ;
#37828 = CARTESIAN_POINT ( 'NONE',  ( -56.48576386720575471, -140.0000000013656063, -4.591703134518078322 ) ) ;
#37829 = CARTESIAN_POINT ( 'NONE',  ( 4.458734124999999437, -85.06249999863439371, -5.460374474430324690E-16 ) ) ;
#37830 = CARTESIAN_POINT ( 'NONE',  ( -58.80597590150559739, -129.1250000027312126, 3.242614290531460330 ) ) ;
#37831 = DIRECTION ( 'NONE',  ( 0.000000000000000000, 0.000000000000000000, 1.000000000000000000 ) ) ;
#37832 = CARTESIAN_POINT ( 'NONE',  ( -2.500000000000000444, -83.16666666666667140, -4.330127018922193649 ) ) ;
#37833 = AXIS2_PLACEMENT_3D ( 'NONE', #2523, #50458, #45300 ) ;
#37834 =( BOUNDED_CURVE ( )  B_SPLINE_CURVE ( 2, ( #12339, #42544, #17790, #32263, #37109, #51892, #47067, #27434, #37413 ),
 .UNSPECIFIED., .F., .F. ) 
 B_SPLINE_CURVE_WITH_KNOTS ( ( 3, 2, 2, 2, 3 ),
 ( 0.1125000000000000028, 0.1130952380952380959, 0.1142857142857142821, 0.1154761904761904823, 0.1160714285714285754 ),
 .UNSPECIFIED. ) 
 CURVE ( )  GEOMETRIC_REPRESENTATION_ITEM ( )  RATIONAL_B_SPLINE_CURVE ( ( 0.9330127018922194093, 0.9330127018922194093, 1.000000000000000000, 0.8660254037844387076, 1.000000000000000000, 0.8660254037844387076, 1.000000000000000000, 0.9330127018922194093, 0.9330127018922194093 ) ) 
 REPRESENTATION_ITEM ( '' )  );
#37835 = CARTESIAN_POINT ( 'NONE',  ( -2.500000000000000444, -45.04166666393547303, -4.330127018922193649 ) ) ;
#37836 = CARTESIAN_POINT ( 'NONE',  ( -4.458734124999999437, -56.31249999863440081, 0.000000000000000000 ) ) ;
#37837 = CARTESIAN_POINT ( 'NONE',  ( 0.000000000000000000, -120.0000000000000000, 5.000000000000000000 ) ) ;
#37838 = CARTESIAN_POINT ( 'NONE',  ( -4.458734124999998549, 21.77083333469892779, 2.574251347313722516 ) ) ;
#37839 = VECTOR ( 'NONE', #19175, 1000.000000000000000 ) ;
#37840 = CARTESIAN_POINT ( 'NONE',  ( 5.000000000000000888, -42.58333333333334281, 2.886751345948126879 ) ) ;
#37841 = CARTESIAN_POINT ( 'NONE',  ( 1.975475456537005874E-15, 1.375000002731185500, 5.000000000000000000 ) ) ;
#37842 = EDGE_CURVE ( 'NONE', #59664, #37124, #40345, .T. ) ;
#37843 = CARTESIAN_POINT ( 'NONE',  ( -2.229367062499996610, -42.39583333196773651, 3.861377020970582219 ) ) ;
#37844 = CARTESIAN_POINT ( 'NONE',  ( -5.000000000000000000, -5.958333330602148870, -2.886751345948128211 ) ) ;
#37845 = CARTESIAN_POINT ( 'NONE',  ( 0.000000000000000000, -170.0000000000000000, 0.000000000000000000 ) ) ;
#37846 = CARTESIAN_POINT ( 'NONE',  ( -51.60603307380591787, -124.9375000013656063, -2.891590998281053704 ) ) ;
#37847 = CARTESIAN_POINT ( 'NONE',  ( 2.229367062500001939, -86.22916666530107932, 3.861377020970579999 ) ) ;
#37848 = CARTESIAN_POINT ( 'NONE',  ( 2.229367062500001939, -103.9791666653010651, 3.861377020970579999 ) ) ;
#37849 = CARTESIAN_POINT ( 'NONE',  ( 9.457646018065525792E-16, -3.312499998634407916, 5.148502694627439702 ) ) ;
#37851 = EDGE_CURVE ( 'NONE', #31664, #54505, #17811, .T. ) ;
#37850 = ORIENTED_EDGE ( 'NONE', *, *, #15258, .T. ) ;
#37852 = CARTESIAN_POINT ( 'NONE',  ( -2.071067811865622943, -155.8125000027310989, -4.999999999999850786 ) ) ;
#37853 = CARTESIAN_POINT ( 'NONE',  ( 4.458734125000001214, -91.89583333196773651, 2.574251347313718519 ) ) ;
#37854 = CARTESIAN_POINT ( 'NONE',  ( 2.071067811865475505, -166.9375000027312126, -5.000000000000000888 ) ) ;
#37855 = CARTESIAN_POINT ( 'NONE',  ( 9.457646018065525792E-16, -94.31249999863440792, 5.148502694627439702 ) ) ;
#37856 = EDGE_CURVE ( 'NONE', #37137, #12070, #11605, .T. ) ;
#37857 = CARTESIAN_POINT ( 'NONE',  ( -50.40829686548195099, -128.0000000013656063, -1.485763867205728284 ) ) ;
#37858 = CARTESIAN_POINT ( 'NONE',  ( 2.229367062499998831, -13.64583333196774184, -3.861377020970580887 ) ) ;
#37859 = CARTESIAN_POINT ( 'NONE',  ( -4.458734124999998549, 10.52083333469892779, 2.574251347313722516 ) ) ;
#37860 = CARTESIAN_POINT ( 'NONE',  ( -3.152548672688508926E-16, -53.81249999863439371, -5.148502694627439702 ) ) ;
#37861 = CARTESIAN_POINT ( 'NONE',  ( 5.000000000000000000, -86.29166666393547303, -2.886751345948130876 ) ) ;
#37862 = DIRECTION ( 'NONE',  ( -0.000000000000000000, 1.000000000000000000, -0.000000000000000000 ) ) ;
#37863 = CARTESIAN_POINT ( 'NONE',  ( -2.229367062499996610, -11.14583333196773829, 3.861377020970582219 ) ) ;
#37864 = CARTESIAN_POINT ( 'NONE',  ( -6.972266317189433020E-16, -39.25000000000000000, -5.000000000000000000 ) ) ;
#37865 = ADVANCED_FACE ( 'NONE', ( #60477 ), #27003, .T. ) ;
#37866 = VERTEX_POINT ( 'NONE', #42100 ) ;
#37867 = CARTESIAN_POINT ( 'NONE',  ( -4.458734124999999437, -38.56249999863440081, 0.000000000000000000 ) ) ;
#37868 = CARTESIAN_POINT ( 'NONE',  ( 0.000000000000000000, -120.0000000000000000, 0.000000000000000000 ) ) ;
#37869 = EDGE_CURVE ( 'NONE', #42628, #46066, #46937, .T. ) ;
#37870 = CARTESIAN_POINT ( 'NONE',  ( -6.972266317189433020E-16, 0.8750000027311866102, -5.000000000000000000 ) ) ;
#37871 = DIRECTION ( 'NONE',  ( -0.000000000000000000, 1.000000000000000000, -0.000000000000000000 ) ) ;
#37872 = CARTESIAN_POINT ( 'NONE',  ( 2.229367062500001939, -79.97916666530106511, 3.861377020970579999 ) ) ;
#37873 = CARTESIAN_POINT ( 'NONE',  ( -2.229367062500000163, 24.27083333469892779, -3.861377020970580443 ) ) ;
#37874 = CARTESIAN_POINT ( 'NONE',  ( -3.152548672688508926E-16, 15.43750000136559564, -5.148502694627439702 ) ) ;
#37875 = EDGE_CURVE ( 'NONE', #63081, #41892, #50815, .T. ) ;
#37876 = DIRECTION ( 'NONE',  ( 0.000000000000000000, 0.000000000000000000, 1.000000000000000000 ) ) ;
#37877 = LINE ( 'NONE', #52356, #51207 ) ;
#37878 = CARTESIAN_POINT ( 'NONE',  ( 2.229367062499998831, -82.89583333196773651, -3.861377020970580887 ) ) ;
#37879 = CARTESIAN_POINT ( 'NONE',  ( 5.000000000000000888, -67.58333333333332860, 2.886751345948126879 ) ) ;
#37880 = CARTESIAN_POINT ( 'NONE',  ( 5.000000000000000000, 15.62500000273118417, -6.123233995736766282E-16 ) ) ;
#37881 = EDGE_LOOP ( 'NONE', ( #31229, #61418, #3496, #16884 ) ) ;
#37882 = CARTESIAN_POINT ( 'NONE',  ( 1.339745962155615144, -35.70534180126148271, 4.999999999999999112 ) ) ;
#37883 = CARTESIAN_POINT ( 'NONE',  ( -2.500000000000000444, 15.83333333333333037, -4.330127018922193649 ) ) ;
#37885 = CARTESIAN_POINT ( 'NONE',  ( 2.499999999999998668, -27.33333333333333570, -4.330127018922193649 ) ) ;
#37884 = CARTESIAN_POINT ( 'NONE',  ( -6.972266317189433020E-16, -40.24999999999999289, -5.000000000000000000 ) ) ;
#37886 = CARTESIAN_POINT ( 'NONE',  ( 4.458734124999999437, -31.81249999863440436, -5.460374474430324690E-16 ) ) ;
#37887 = AXIS2_PLACEMENT_3D ( 'NONE', #28780, #34538, #10113 ) ;
#37888 = DIRECTION ( 'NONE',  ( -0.000000000000000000, 1.000000000000000000, -0.000000000000000000 ) ) ;
#37889 = CARTESIAN_POINT ( 'NONE',  ( -5.000000000000000000, -28.87499999726881228, 0.000000000000000000 ) ) ;
#37891 = EDGE_LOOP ( 'NONE', ( #21184, #51187, #45835, #343 ) ) ;
#37890 = CARTESIAN_POINT ( 'NONE',  ( -4.458734124999999437, -59.31249999863440081, 0.000000000000000000 ) ) ;
#37892 = FACE_OUTER_BOUND ( 'NONE', #42326, .T. ) ;
#37894 = ORIENTED_EDGE ( 'NONE', *, *, #42064, .T. ) ;
#37893 = CARTESIAN_POINT ( 'NONE',  ( 9.457646018065525792E-16, -8.312499998634406140, 5.148502694627439702 ) ) ;
#37895 = CARTESIAN_POINT ( 'NONE',  ( -5.000000000000000000, -76.08333333333332860, -2.886751345948128211 ) ) ;
#37896 = FACE_OUTER_BOUND ( 'NONE', #29509, .T. ) ;
#37897 = CARTESIAN_POINT ( 'NONE',  ( 4.458734124999999437, -50.06249999863440792, -5.460374474430324690E-16 ) ) ;
#37898 = CARTESIAN_POINT ( 'NONE',  ( -2.499999999999996447, -78.70833333060214443, 4.330127018922195425 ) ) ;
#37900 = EDGE_LOOP ( 'NONE', ( #17145, #12796, #31145, #26760 ) ) ;
#37899 = CARTESIAN_POINT ( 'NONE',  ( -6.972266317189433020E-16, 9.875000002731185944, -5.000000000000000000 ) ) ;
#37901 = CARTESIAN_POINT ( 'NONE',  ( -57.46284108482265651, -147.9375000000000000, 4.819101127000239515 ) ) ;
#37902 = CARTESIAN_POINT ( 'NONE',  ( -4.458734124999999437, -21.56249999863440436, 0.000000000000000000 ) ) ;
#37904 = VERTEX_POINT ( 'NONE', #51769 ) ;
#37903 = CARTESIAN_POINT ( 'NONE',  ( -4.458734124999999437, -54.56249999863440081, 0.000000000000000000 ) ) ;
#37905 = DIRECTION ( 'NONE',  ( 1.000000000000000000, 0.000000000000000000, 0.000000000000000000 ) ) ;
#37906 = CARTESIAN_POINT ( 'NONE',  ( 4.458734124999999437, -142.5000000013656347, 1.846868145590737864 ) ) ;
#37907 = CARTESIAN_POINT ( 'NONE',  ( -3.152548672688508926E-16, -101.8124999986344079, -5.148502694627439702 ) ) ;
#37908 = ORIENTED_EDGE ( 'NONE', *, *, #40980, .F. ) ;
#37909 = CARTESIAN_POINT ( 'NONE',  ( -59.44456063193725015, -148.8125000013656063, -0.3552334253322034230 ) ) ;
#37910 = CARTESIAN_POINT ( 'NONE',  ( -50.18089887299979068, -143.8125000027312126, 2.462841084822635640 ) ) ;
#37911 = CARTESIAN_POINT ( 'NONE',  ( -2.500000000000000444, 0.9583333360645186483, -4.330127018922193649 ) ) ;
#37912 = CARTESIAN_POINT ( 'NONE',  ( -2.229367062499996610, -7.145833331967735624, 3.861377020970582219 ) ) ;
#37913 =( BOUNDED_CURVE ( )  B_SPLINE_CURVE ( 2, ( #46218, #11483, #51686, #7627, #41379, #36563, #32050, #12115, #16318 ),
 .UNSPECIFIED., .F., .F. ) 
 B_SPLINE_CURVE_WITH_KNOTS ( ( 3, 2, 2, 2, 3 ),
 ( 0.07708333333333333703, 0.07777777777777777901, 0.07916666666666666297, 0.08055555555555556080, 0.08125000000000000278 ),
 .UNSPECIFIED. ) 
 CURVE ( )  GEOMETRIC_REPRESENTATION_ITEM ( )  RATIONAL_B_SPLINE_CURVE ( ( 0.9330127018922194093, 0.9330127018922194093, 1.000000000000000000, 0.8660254037844387076, 1.000000000000000000, 0.8660254037844387076, 1.000000000000000000, 0.9330127018922194093, 0.9330127018922194093 ) ) 
 REPRESENTATION_ITEM ( '' )  );
#37914 = CARTESIAN_POINT ( 'NONE',  ( 2.229367062499998831, -102.8958333319677365, -3.861377020970580887 ) ) ;
#37915 = CARTESIAN_POINT ( 'NONE',  ( 1.846868145590735200, -144.5000000013656063, -4.458734125000000326 ) ) ;
#37916 = CARTESIAN_POINT ( 'NONE',  ( -4.458734124999998549, -26.47916666530107221, 2.574251347313722516 ) ) ;
#37917 = DIRECTION ( 'NONE',  ( -0.000000000000000000, 1.000000000000000000, -0.000000000000000000 ) ) ;
#37918 = CARTESIAN_POINT ( 'NONE',  ( -50.70258187064364108, -135.1250000013656063, 2.196230717870141014 ) ) ;
#37919 = CARTESIAN_POINT ( 'NONE',  ( 4.458734124999998549, -66.97916666530107932, -2.574251347313721627 ) ) ;
#37920 = LINE ( 'NONE', #23448, #11710 ) ;
#37921 = CARTESIAN_POINT ( 'NONE',  ( -4.999999999999998224, -33.91666666666666430, 2.886751345948131764 ) ) ;
#37922 = CARTESIAN_POINT ( 'NONE',  ( -4.458734124999999437, -140.9375000013656063, -5.460374474430324690E-16 ) ) ;
#37923 = CARTESIAN_POINT ( 'NONE',  ( 4.458734124999998549, 8.020833334698926009, -2.574251347313721627 ) ) ;
#37924 = ORIENTED_EDGE ( 'NONE', *, *, #5458, .T. ) ;
#37925 = CARTESIAN_POINT ( 'NONE',  ( -4.999999999999998224, -4.916666666666666075, 2.886751345948131764 ) ) ;
#37926 = CARTESIAN_POINT ( 'NONE',  ( -2.071067811865562991, -144.3124999999999716, 4.999999999999913847 ) ) ;
#37928 = CARTESIAN_POINT ( 'NONE',  ( -2.229367062499996610, -24.14583333196773651, 3.861377020970582219 ) ) ;
#37927 = CARTESIAN_POINT ( 'NONE',  ( 5.000000000000000000, -88.41666666666665719, -2.886751345948129988 ) ) ;
#37929 = CARTESIAN_POINT ( 'NONE',  ( 1.975475456537005874E-15, -35.75000000000000711, 5.000000000000000000 ) ) ;
#37930 = CARTESIAN_POINT ( 'NONE',  ( -3.152548672688508926E-16, -75.81249999863440792, -5.148502694627439702 ) ) ;
#37931 = AXIS2_PLACEMENT_3D ( 'NONE', #32516, #8089, #27693 ) ;
#37932 = CARTESIAN_POINT ( 'NONE',  ( -2.229367062499996610, 22.60416666803225993, 3.861377020970582219 ) ) ;
#37933 = CARTESIAN_POINT ( 'NONE',  ( -6.972266317189433020E-16, -79.12499999726881583, -5.000000000000000000 ) ) ;
#37934 = CARTESIAN_POINT ( 'NONE',  ( -54.64476657466781973, -140.8125000013656063, -4.444560631937228834 ) ) ;
#37935 = CARTESIAN_POINT ( 'NONE',  ( 9.457646018065525792E-16, 2.937500001365594304, 5.148502694627439702 ) ) ;
#37936 = CARTESIAN_POINT ( 'NONE',  ( -4.458734124999998549, 28.52083333469892423, 2.574251347313722516 ) ) ;
#37937 = CARTESIAN_POINT ( 'NONE',  ( 2.229367062499998831, -36.89583333196773651, -3.861377020970580887 ) ) ;
#37938 = DIRECTION ( 'NONE',  ( -0.000000000000000000, 1.000000000000000000, -0.000000000000000000 ) ) ;
#37939 = CARTESIAN_POINT ( 'NONE',  ( -2.229367062499996610, 4.854166668032261711, 3.861377020970582219 ) ) ;
#37940 = CARTESIAN_POINT ( 'NONE',  ( -2.229367062500000163, -71.47916666530107932, -3.861377020970580443 ) ) ;
#37941 = CARTESIAN_POINT ( 'NONE',  ( -2.229367062500000163, -17.72916666530106866, -3.861377020970580443 ) ) ;
#37942 = CARTESIAN_POINT ( 'NONE',  ( 5.000000000000000000, -8.416666666666669627, -2.886751345948129988 ) ) ;
#37943 = CARTESIAN_POINT ( 'NONE',  ( 1.846868145590736310, -160.6250000013655779, 4.458734124999999437 ) ) ;
#37944 = CARTESIAN_POINT ( 'NONE',  ( 5.000000000000000000, 15.70833333606451809, -2.886751345948130876 ) ) ;
#37945 = CARTESIAN_POINT ( 'NONE',  ( 4.458734124999998549, -65.72916666530106511, -2.574251347313721627 ) ) ;
#37946 = CARTESIAN_POINT ( 'NONE',  ( -5.000000000000000000, -101.9583333306021444, -2.886751345948128211 ) ) ;
#37947 = CARTESIAN_POINT ( 'NONE',  ( 4.458734124999999437, 29.18750000136559208, -5.460374474430324690E-16 ) ) ;
#37948 = CARTESIAN_POINT ( 'NONE',  ( 4.458734124999998549, -40.72916666530107221, -2.574251347313721627 ) ) ;
#37949 = CARTESIAN_POINT ( 'NONE',  ( -5.000000000000000000, -83.99999999999998579, 0.000000000000000000 ) ) ;
#37950 = CARTESIAN_POINT ( 'NONE',  ( -4.458734124999999437, -104.5624999986344079, 0.000000000000000000 ) ) ;
#37951 = CARTESIAN_POINT ( 'NONE',  ( 2.229367062499998831, -68.89583333196773651, -3.861377020970580887 ) ) ;
#37952 = CARTESIAN_POINT ( 'NONE',  ( -4.999999999999999112, -54.91666666666667140, 2.886751345948131764 ) ) ;
#37953 = CARTESIAN_POINT ( 'NONE',  ( 5.000000000000000000, -72.37499999726880162, -6.123233995736766282E-16 ) ) ;
#37954 = CARTESIAN_POINT ( 'NONE',  ( 2.071067811865264563, -151.9375000027311842, -5.000000000000211386 ) ) ;
#37955 = ORIENTED_EDGE ( 'NONE', *, *, #38200, .F. ) ;
#37956 = CARTESIAN_POINT ( 'NONE',  ( -3.152548672688508926E-16, -109.5624999986344079, -5.148502694627439702 ) ) ;
#37957 = CARTESIAN_POINT ( 'NONE',  ( 5.000000000000000000, -14.41666666666666963, -2.886751345948129988 ) ) ;
#37958 = CARTESIAN_POINT ( 'NONE',  ( -4.458734124999999437, -17.31249999863440792, 0.000000000000000000 ) ) ;
#37959 = CARTESIAN_POINT ( 'NONE',  ( 2.229367062499998831, -75.64583333196773651, -3.861377020970580887 ) ) ;
#37960 = DIRECTION ( 'NONE',  ( 0.000000000000000000, 1.000000000000000000, 0.000000000000000000 ) ) ;
#37961 = CARTESIAN_POINT ( 'NONE',  ( 5.000000000000000000, -12.37499999726881050, -6.123233995736766282E-16 ) ) ;
#37963 = VERTEX_POINT ( 'NONE', #26364 ) ;
#37962 = CARTESIAN_POINT ( 'NONE',  ( 4.458734125000001214, -42.89583333196773651, 2.574251347313718519 ) ) ;
#37964 = CARTESIAN_POINT ( 'NONE',  ( 3.061616997868383141E-16, -143.7500000000000284, -5.000000000000000000 ) ) ;
#37966 = ORIENTED_EDGE ( 'NONE', *, *, #20699, .T. ) ;
#37965 = CARTESIAN_POINT ( 'NONE',  ( 4.458734124999998549, 7.020833334698929562, -2.574251347313721627 ) ) ;
#37967 =( BOUNDED_CURVE ( )  B_SPLINE_CURVE ( 2, ( #6955, #12081, #31704, #7277, #41653, #38118, #17860, #3085, #37482 ),
 .UNSPECIFIED., .F., .F. ) 
 B_SPLINE_CURVE_WITH_KNOTS ( ( 3, 2, 2, 2, 3 ),
 ( 0.08541666666666666852, 0.08611111111111111049, 0.08749999999999999445, 0.08888888888888889228, 0.08958333333333333426 ),
 .UNSPECIFIED. ) 
 CURVE ( )  GEOMETRIC_REPRESENTATION_ITEM ( )  RATIONAL_B_SPLINE_CURVE ( ( 0.9330127018922194093, 0.9330127018922194093, 1.000000000000000000, 0.8660254037844387076, 1.000000000000000000, 0.8660254037844387076, 1.000000000000000000, 0.9330127018922194093, 0.9330127018922194093 ) ) 
 REPRESENTATION_ITEM ( '' )  );
#37968 = CARTESIAN_POINT ( 'NONE',  ( -51.60603307380591787, -151.9375000013656063, -2.891590998281053704 ) ) ;
#37969 = CARTESIAN_POINT ( 'NONE',  ( -2.500000000000000444, -61.16666666666666430, -4.330127018922193649 ) ) ;
#37970 = CARTESIAN_POINT ( 'NONE',  ( 4.458734124999999437, -156.6875000013655779, 0.000000000000000000 ) ) ;
#37971 = CARTESIAN_POINT ( 'NONE',  ( 4.458734124999999437, -36.06249999863440792, -5.460374474430324690E-16 ) ) ;
#37972 = CARTESIAN_POINT ( 'NONE',  ( 1.339745962155612702, -45.16965819600733312, -5.000000000000000000 ) ) ;
#37973 = CARTESIAN_POINT ( 'NONE',  ( -52.53715891517739323, -149.5625000027312126, -4.819101127000233298 ) ) ;
#37974 = CARTESIAN_POINT ( 'NONE',  ( 3.535533905932738197, -166.8750000000000284, -3.535533905932738197 ) ) ;
#37975 = CARTESIAN_POINT ( 'NONE',  ( 0.000000000000000000, -170.0000000000000000, 5.000000000000000000 ) ) ;
#37976 = AXIS2_PLACEMENT_3D ( 'NONE', #29363, #13959, #5267 ) ;
#37977 = CARTESIAN_POINT ( 'NONE',  ( -55.35523342533222291, -132.5625000013656063, 4.444560631937231499 ) ) ;
#37978 = CARTESIAN_POINT ( 'NONE',  ( -4.458734124999999437, -5.562499998634402587, 0.000000000000000000 ) ) ;
#37979 = CARTESIAN_POINT ( 'NONE',  ( -3.152548672688508926E-16, -39.81249999863440081, -5.148502694627439702 ) ) ;
#37980 = CARTESIAN_POINT ( 'NONE',  ( 5.000000000000000888, -67.45833333060214443, 2.886751345948126879 ) ) ;
#37981 = CARTESIAN_POINT ( 'NONE',  ( 4.458734125000000326, -154.3750000013655779, -1.846868145590734978 ) ) ;
#37982 = CARTESIAN_POINT ( 'NONE',  ( 4.458734125000001214, -83.14583333196773651, 2.574251347313718519 ) ) ;
#37983 = ORIENTED_EDGE ( 'NONE', *, *, #30741, .F. ) ;
#37984 = CARTESIAN_POINT ( 'NONE',  ( -49.85088928181150436, -152.6875000027311842, -1.666127454062680702 ) ) ;
#37985 = CARTESIAN_POINT ( 'NONE',  ( 5.000000000000000888, -2.458333330602146205, 2.886751345948126879 ) ) ;
#37986 = CARTESIAN_POINT ( 'NONE',  ( -4.458734124999998549, -69.47916666530107932, 2.574251347313722516 ) ) ;
#37987 = CARTESIAN_POINT ( 'NONE',  ( 1.846868145590735200, -147.5000000013656063, -4.458734124999999437 ) ) ;
#37988 = ORIENTED_EDGE ( 'NONE', *, *, #38985, .F. ) ;
#37989 = CARTESIAN_POINT ( 'NONE',  ( -1.339745962155613812, -71.08034179853027013, -5.000000000000000000 ) ) ;
#37990 = CARTESIAN_POINT ( 'NONE',  ( 4.458734125000001214, -10.14583333196773829, 2.574251347313718519 ) ) ;
#37991 = DIRECTION ( 'NONE',  ( 0.000000000000000000, 1.000000000000000000, 0.000000000000000000 ) ) ;
#37992 = CARTESIAN_POINT ( 'NONE',  ( 2.229367062500001939, 1.020833334698927120, 3.861377020970579999 ) ) ;
#37993 = CARTESIAN_POINT ( 'NONE',  ( 5.000000000000000000, -77.29166666393547303, -2.886751345948130876 ) ) ;
#37994 = CARTESIAN_POINT ( 'NONE',  ( -1.846868145590737420, -151.7500000013656063, 4.458734124999997661 ) ) ;
#37995 = CARTESIAN_POINT ( 'NONE',  ( 4.458734124999999437, 28.93750000136559208, -5.460374474430324690E-16 ) ) ;
#37996 = ORIENTED_EDGE ( 'NONE', *, *, #50866, .T. ) ;
#37997 = CARTESIAN_POINT ( 'NONE',  ( -2.229367062500000163, -90.47916666530106511, -3.861377020970580443 ) ) ;
#37998 = FACE_OUTER_BOUND ( 'NONE', #17167, .T. ) ;
#37999 = CARTESIAN_POINT ( 'NONE',  ( -2.916731409357579869E-14, 17.37500000273118417, 5.000000000000000888 ) ) ;
#38000 = CARTESIAN_POINT ( 'NONE',  ( -2.229367062499996610, -9.145833331967736513, 3.861377020970582219 ) ) ;
#38001 = CARTESIAN_POINT ( 'NONE',  ( -5.000000000000000000, 19.91666666666666430, -2.886751345948128211 ) ) ;
#38002 = DIRECTION ( 'NONE',  ( -0.000000000000000000, 1.000000000000000000, -0.000000000000000000 ) ) ;
#38003 = CARTESIAN_POINT ( 'NONE',  ( 5.000000000000000000, -87.50000000000000000, -6.123233995736766282E-16 ) ) ;
#38004 = CARTESIAN_POINT ( 'NONE',  ( -5.000000000000000000, -37.87499999726881583, 0.000000000000000000 ) ) ;
#38005 = LINE ( 'NONE', #33803, #16445 ) ;
#38006 = CARTESIAN_POINT ( 'NONE',  ( 9.457646018065525792E-16, 20.93750000136558853, 5.148502694627439702 ) ) ;
#38007 = LINE ( 'NONE', #48905, #25297 ) ;
#38008 = CARTESIAN_POINT ( 'NONE',  ( 2.229367062500001939, 23.02083333469892423, 3.861377020970579999 ) ) ;
#38009 = CARTESIAN_POINT ( 'NONE',  ( 2.229367062500001939, -55.97916666530107221, 3.861377020970579999 ) ) ;
#38010 = CARTESIAN_POINT ( 'NONE',  ( -4.458734124999999437, -4.645833331967739177, -2.574251347313719407 ) ) ;
#38011 =( BOUNDED_CURVE ( )  B_SPLINE_CURVE ( 2, ( #3901, #13230, #23197, #37993, #23520, #43121, #62761, #25410, #30545 ),
 .UNSPECIFIED., .F., .F. ) 
 B_SPLINE_CURVE_WITH_KNOTS ( ( 3, 2, 2, 2, 3 ),
 ( 0.7589285714285713969, 0.7595238095238094900, 0.7607142857142856762, 0.7619047619047618625, 0.7624999999999999556 ),
 .UNSPECIFIED. ) 
 CURVE ( )  GEOMETRIC_REPRESENTATION_ITEM ( )  RATIONAL_B_SPLINE_CURVE ( ( 0.9330127018922194093, 0.9330127018922194093, 1.000000000000000000, 0.8660254037844387076, 1.000000000000000000, 0.8660254037844387076, 1.000000000000000000, 0.9330127018922194093, 0.9330127018922194093 ) ) 
 REPRESENTATION_ITEM ( '' )  );
#38012 = DIRECTION ( 'NONE',  ( -0.000000000000000000, 1.000000000000000000, -0.000000000000000000 ) ) ;
#38013 = CARTESIAN_POINT ( 'NONE',  ( 1.060575238724906964E-15, 12.25000000000000000, 5.773502691896257311 ) ) ;
#38014 = CARTESIAN_POINT ( 'NONE',  ( -5.000000000000000888, -139.5625000027311842, 2.071067811865474617 ) ) ;
#38015 = CARTESIAN_POINT ( 'NONE',  ( 5.000000000000000000, -75.29166666393548724, -2.886751345948130876 ) ) ;
#38016 = VECTOR ( 'NONE', #19348, 1000.000000000000227 ) ;
#38017 = CARTESIAN_POINT ( 'NONE',  ( 2.229367062499998831, -49.64583333196772941, -3.861377020970580887 ) ) ;
#38018 = CARTESIAN_POINT ( 'NONE',  ( 5.000000000000000888, -86.45833333060213022, 2.886751345948126879 ) ) ;
#38019 = CARTESIAN_POINT ( 'NONE',  ( -52.10840900171896806, -134.4375000013656063, 3.393966926194110556 ) ) ;
#38020 = FACE_OUTER_BOUND ( 'NONE', #27418, .T. ) ;
#38021 = CARTESIAN_POINT ( 'NONE',  ( 0.000000000000000000, -120.0000000000000000, 0.000000000000000000 ) ) ;
#38022 = CARTESIAN_POINT ( 'NONE',  ( -4.458734124999999437, -91.64583333196773651, -2.574251347313719407 ) ) ;
#38023 = CARTESIAN_POINT ( 'NONE',  ( -4.458734125000000326, -159.1250000013656063, 1.846868145590734089 ) ) ;
#38024 = CARTESIAN_POINT ( 'NONE',  ( -4.999999999999999112, -35.91666666666666430, 2.886751345948131764 ) ) ;
#38025 = CARTESIAN_POINT ( 'NONE',  ( 6.158835246850667461E-14, 8.875000002731182391, -4.999999999999999112 ) ) ;
#38026 = VERTEX_POINT ( 'NONE', #52087 ) ;
#38027 = CARTESIAN_POINT ( 'NONE',  ( 2.229367062499998831, 19.10416666803225993, -3.861377020970580887 ) ) ;
#38028 = ORIENTED_EDGE ( 'NONE', *, *, #35453, .T. ) ;
#38029 = CARTESIAN_POINT ( 'NONE',  ( -4.458734124999999437, -95.39583333196772230, -2.574251347313719407 ) ) ;
#38030 = CARTESIAN_POINT ( 'NONE',  ( 2.229367062500001939, 8.770833334698927786, 3.861377020970579999 ) ) ;
#38031 = CARTESIAN_POINT ( 'NONE',  ( -5.000000000000000000, 11.04166666939785202, -2.886751345948128211 ) ) ;
#38032 = CARTESIAN_POINT ( 'NONE',  ( 6.123233995736766282E-16, -170.0000000000000000, -5.000000000000000000 ) ) ;
#38033 = CARTESIAN_POINT ( 'NONE',  ( 5.000000000000000000, 5.500000000000001776, -6.123233995736766282E-16 ) ) ;
#38034 = CARTESIAN_POINT ( 'NONE',  ( -3.152548672688508926E-16, -61.56249999863440081, -5.148502694627439702 ) ) ;
#38035 = CARTESIAN_POINT ( 'NONE',  ( -1.339745962155610925, -52.66965819600733312, 5.000000000000000000 ) ) ;
#38036 = CARTESIAN_POINT ( 'NONE',  ( 5.000000000000000888, 5.541666669397854683, 2.886751345948126879 ) ) ;
#38037 = CARTESIAN_POINT ( 'NONE',  ( 4.458734125000001214, -29.89583333196773651, 2.574251347313718519 ) ) ;
#38038 = DIRECTION ( 'NONE',  ( -0.000000000000000000, 1.000000000000000000, -0.000000000000000000 ) ) ;
#38039 = LINE ( 'NONE', #57043, #47708 ) ;
#38040 = CARTESIAN_POINT ( 'NONE',  ( 1.975475456537005874E-15, -24.62499999726881583, 5.000000000000000000 ) ) ;
#38041 = CARTESIAN_POINT ( 'NONE',  ( 2.499999999999998668, -43.33333333333333570, -4.330127018922193649 ) ) ;
#38043 = CARTESIAN_POINT ( 'NONE',  ( -4.458734124999999437, -19.56249999863440081, 0.000000000000000000 ) ) ;
#38042 = CARTESIAN_POINT ( 'NONE',  ( 0.000000000000000000, 0.000000000000000000, 0.000000000000000000 ) ) ;
#38044 = CARTESIAN_POINT ( 'NONE',  ( 1.339745962155615144, -4.580341798530294994, 4.999999999999999112 ) ) ;
#38045 = CARTESIAN_POINT ( 'NONE',  ( -3.152548672688508926E-16, -65.56249999863440792, -5.148502694627439702 ) ) ;
#38046 = CARTESIAN_POINT ( 'NONE',  ( -1.846868145590737420, -150.0000000013655779, 4.458734124999999437 ) ) ;
#38048 = EDGE_CURVE ( 'NONE', #12482, #52029, #53491, .T. ) ;
#38047 = CARTESIAN_POINT ( 'NONE',  ( 4.458734125000001214, -75.89583333196775072, 2.574251347313718519 ) ) ;
#38049 = CARTESIAN_POINT ( 'NONE',  ( -57.19623071787017210, -141.6250000013656063, 4.297418129356382899 ) ) ;
#38050 = CARTESIAN_POINT ( 'NONE',  ( 9.457646018065525792E-16, -24.31249999863440792, 5.148502694627439702 ) ) ;
#38051 = CARTESIAN_POINT ( 'NONE',  ( -3.535250795749689387E-16, -65.12499999726881583, -5.773502691896257311 ) ) ;
#38052 = ORIENTED_EDGE ( 'NONE', *, *, #38998, .F. ) ;
#38053 = CARTESIAN_POINT ( 'NONE',  ( -3.535533905932738641, -152.5000000027312126, 3.535533905932737309 ) ) ;
#38054 = ORIENTED_EDGE ( 'NONE', *, *, #19301, .T. ) ;
#38055 = CARTESIAN_POINT ( 'NONE',  ( -4.458734124999999437, -67.64583333196773651, -2.574251347313719407 ) ) ;
#38056 = CARTESIAN_POINT ( 'NONE',  ( 1.339745962155615144, -7.580341798530293218, 4.999999999999999112 ) ) ;
#38057 = CARTESIAN_POINT ( 'NONE',  ( -4.729367062499999719, 29.28125000204839168, 0.000000000000000000 ) ) ;
#38058 = ORIENTED_EDGE ( 'NONE', *, *, #35111, .F. ) ;
#38059 = AXIS2_PLACEMENT_3D ( 'NONE', #19558, #48196, #58488 ) ;
#38061 = VECTOR ( 'NONE', #59870, 1000.000000000000000 ) ;
#38060 = CARTESIAN_POINT ( 'NONE',  ( 6.123233995736766282E-16, -120.0000000000000000, -5.000000000000000000 ) ) ;
#38062 = CARTESIAN_POINT ( 'NONE',  ( -2.229367062500000163, -52.72916666530107221, -3.861377020970580443 ) ) ;
#38063 = CARTESIAN_POINT ( 'NONE',  ( 2.229367062499998831, 3.104166668032259935, -3.861377020970580887 ) ) ;
#38064 = VERTEX_POINT ( 'NONE', #56605 ) ;
#38065 = ADVANCED_FACE ( 'NONE', ( #31496 ), #47260, .F. ) ;
#38066 = CARTESIAN_POINT ( 'NONE',  ( -5.000000000000000000, -55.08333333333332860, -2.886751345948128211 ) ) ;
#38067 = EDGE_CURVE ( 'NONE', #727, #36069, #41336, .T. ) ;
#38068 = CARTESIAN_POINT ( 'NONE',  ( -4.458734124999999437, 5.687500001365592972, 0.000000000000000000 ) ) ;
#38069 = CARTESIAN_POINT ( 'NONE',  ( 4.458734125000001214, 21.10416666803226349, 2.574251347313718519 ) ) ;
#38070 = CARTESIAN_POINT ( 'NONE',  ( -59.29741812935640155, -146.6250000013656063, -2.196230717870135685 ) ) ;
#38071 = CARTESIAN_POINT ( 'NONE',  ( -6.972266317189433020E-16, -104.1249999972688016, -5.000000000000000000 ) ) ;
#38072 = CARTESIAN_POINT ( 'NONE',  ( 3.152801135295367541, -165.3125000013656063, -3.152801135295367541 ) ) ;
#38073 = ORIENTED_EDGE ( 'NONE', *, *, #33470, .T. ) ;
#38074 = CARTESIAN_POINT ( 'NONE',  ( 2.229367062500001939, -76.97916666530106511, 3.861377020970579999 ) ) ;
#38075 = AXIS2_PLACEMENT_3D ( 'NONE', #36802, #6902, #2710 ) ;
#38076 = CARTESIAN_POINT ( 'NONE',  ( 0.000000000000000000, -170.0000000000000000, 0.000000000000000000 ) ) ;
#38077 = CARTESIAN_POINT ( 'NONE',  ( -4.458734124999999437, 9.604166668032259935, -2.574251347313719407 ) ) ;
#38078 = ADVANCED_FACE ( 'NONE', ( #61746 ), #37288, .F. ) ;
#38079 = CARTESIAN_POINT ( 'NONE',  ( 1.339745962155612702, -69.16965819600731891, -5.000000000000000000 ) ) ;
#38080 = CARTESIAN_POINT ( 'NONE',  ( 4.458734125000001214, -59.14583333196773651, 2.574251347313718519 ) ) ;
#38081 = CARTESIAN_POINT ( 'NONE',  ( 2.500000000000002220, -21.54166666393548013, 4.330127018922192761 ) ) ;
#38082 = CARTESIAN_POINT ( 'NONE',  ( 1.339745962155612702, -20.29465819873851729, -5.000000000000000000 ) ) ;
#38083 = DIRECTION ( 'NONE',  ( -0.000000000000000000, 1.000000000000000000, -0.000000000000000000 ) ) ;
#38084 = CARTESIAN_POINT ( 'NONE',  ( 5.000000000000000000, 19.62500000273118772, -6.123233995736766282E-16 ) ) ;
#38085 = CARTESIAN_POINT ( 'NONE',  ( -5.000000000000000000, -105.9583333306021586, -2.886751345948128211 ) ) ;
#38086 = CARTESIAN_POINT ( 'NONE',  ( -5.000000000000000000, -159.5000000000000000, -6.123233995736766282E-16 ) ) ;
#38087 = CARTESIAN_POINT ( 'NONE',  ( 4.458734125000001214, -40.89583333196773651, 2.574251347313718519 ) ) ;
#38088 = CARTESIAN_POINT ( 'NONE',  ( 2.229367062499998831, -28.89583333196774007, -3.861377020970580887 ) ) ;
#38089 = DIRECTION ( 'NONE',  ( -0.000000000000000000, 1.000000000000000000, -0.000000000000000000 ) ) ;
#38090 = CARTESIAN_POINT ( 'NONE',  ( 2.499999999999998668, 24.66666666666666785, -4.330127018922193649 ) ) ;
#38091 = CARTESIAN_POINT ( 'NONE',  ( 3.535533905932738197, -152.0000000027312126, -3.535533905932738197 ) ) ;
#38092 = ORIENTED_EDGE ( 'NONE', *, *, #46814, .F. ) ;
#38093 = CARTESIAN_POINT ( 'NONE',  ( 1.975475456537005874E-15, -49.74999999999999289, 5.000000000000000000 ) ) ;
#38094 = CARTESIAN_POINT ( 'NONE',  ( -4.458734124999999437, -31.31249999863440436, 0.000000000000000000 ) ) ;
#38095 = CARTESIAN_POINT ( 'NONE',  ( -4.999999999999999112, -67.79166666393547303, 2.886751345948131764 ) ) ;
#38096 =( BOUNDED_CURVE ( )  B_SPLINE_CURVE ( 2, ( #61252, #3032, #56432, #28942, #31967, #9329, #46763, #4507, #18979 ),
 .UNSPECIFIED., .F., .F. ) 
 B_SPLINE_CURVE_WITH_KNOTS ( ( 3, 2, 2, 2, 3 ),
 ( 0.4583333333333337589, 0.4625000000000004663, 0.4666666666666671182, 0.4708333333333337700, 0.4750000000000004219 ),
 .UNSPECIFIED. ) 
 CURVE ( )  GEOMETRIC_REPRESENTATION_ITEM ( )  RATIONAL_B_SPLINE_CURVE ( ( 0.9999999999999918954, 0.9238795325112948431, 1.000000000000000000, 0.9238795325112867385, 1.000000000000000000, 0.9238795325112867385, 1.000000000000000000, 0.9238795325112786339, 1.000000000000008216 ) ) 
 REPRESENTATION_ITEM ( '' )  );
#38097 = CARTESIAN_POINT ( 'NONE',  ( -55.35523342533222291, -147.5625000013656063, 4.444560631937231499 ) ) ;
#38098 = CARTESIAN_POINT ( 'NONE',  ( -9.184850993605147944E-16, -143.2500000000000284, 5.000000000000000000 ) ) ;
#38099 = EDGE_CURVE ( 'NONE', #34811, #30019, #60095, .T. ) ;
#38100 = CARTESIAN_POINT ( 'NONE',  ( 2.229367062500001939, -26.97916666530106866, 3.861377020970579999 ) ) ;
#38101 = CARTESIAN_POINT ( 'NONE',  ( -2.229367062499996610, -74.39583333196773651, 3.861377020970582219 ) ) ;
#38102 = CARTESIAN_POINT ( 'NONE',  ( -5.000000000000000000, -55.08333333333332860, -2.886751345948128211 ) ) ;
#38103 = CARTESIAN_POINT ( 'NONE',  ( -4.458734124999997661, -30.22916666530106866, 2.574251347313722516 ) ) ;
#38104 = CARTESIAN_POINT ( 'NONE',  ( 0.000000000000000000, -170.0000000000000000, 0.000000000000000000 ) ) ;
#38105 = CARTESIAN_POINT ( 'NONE',  ( 5.000000000000000000, 18.70833333606451632, -2.886751345948130876 ) ) ;
#38106 = CARTESIAN_POINT ( 'NONE',  ( -5.000000000000000000, -24.08333333333333215, -2.886751345948128211 ) ) ;
#38107 = CARTESIAN_POINT ( 'NONE',  ( 1.846868145590735200, -147.2500000013656063, -4.458734125000000326 ) ) ;
#38108 = ORIENTED_EDGE ( 'NONE', *, *, #60430, .F. ) ;
#38109 = VECTOR ( 'NONE', #10392, 1000.000000000000000 ) ;
#38110 = CARTESIAN_POINT ( 'NONE',  ( 6.123233995736766282E-16, -170.0000000000000000, -5.000000000000000000 ) ) ;
#38111 = CARTESIAN_POINT ( 'NONE',  ( 4.458734125000000326, -59.14583333196772230, 2.574251347313718519 ) ) ;
#38112 = CARTESIAN_POINT ( 'NONE',  ( -2.500000000000000444, 24.95833333606451987, -4.330127018922193649 ) ) ;
#38113 = CARTESIAN_POINT ( 'NONE',  ( 5.000000000000000000, -81.29166666393547303, -2.886751345948130876 ) ) ;
#38114 = CARTESIAN_POINT ( 'NONE',  ( 5.000000000000000000, 20.49999999999999645, -6.123233995736766282E-16 ) ) ;
#38115 = FACE_OUTER_BOUND ( 'NONE', #21721, .T. ) ;
#38116 = CARTESIAN_POINT ( 'NONE',  ( -2.229367062499996610, -2.145833331967737845, 3.861377020970582219 ) ) ;
#38117 =( BOUNDED_CURVE ( )  B_SPLINE_CURVE ( 2, ( #20919, #45674, #35074, #6759, #54693, #25416, #60166, #26372, #45034 ),
 .UNSPECIFIED., .F., .F. ) 
 B_SPLINE_CURVE_WITH_KNOTS ( ( 3, 2, 2, 2, 3 ),
 ( 0.7160714285714285809, 0.7166666666666666741, 0.7178571428571428603, 0.7190476190476190466, 0.7196428571428571397 ),
 .UNSPECIFIED. ) 
 CURVE ( )  GEOMETRIC_REPRESENTATION_ITEM ( )  RATIONAL_B_SPLINE_CURVE ( ( 0.9330127018922194093, 0.9330127018922194093, 1.000000000000000000, 0.8660254037844387076, 1.000000000000000000, 0.8660254037844387076, 1.000000000000000000, 0.9330127018922194093, 0.9330127018922194093 ) ) 
 REPRESENTATION_ITEM ( '' )  );
#38118 = CARTESIAN_POINT ( 'NONE',  ( 5.000000000000000888, 19.41666666666666785, 2.886751345948126879 ) ) ;
#38119 = CARTESIAN_POINT ( 'NONE',  ( -1.339745962155613812, -81.08034179853028434, -5.000000000000000000 ) ) ;
#38120 = CARTESIAN_POINT ( 'NONE',  ( -3.152548672688508926E-16, 12.18750000136559564, -5.148502694627439702 ) ) ;
#38121 = LINE ( 'NONE', #24582, #58216 ) ;
#38122 = VERTEX_POINT ( 'NONE', #43668 ) ;
#38123 = CARTESIAN_POINT ( 'NONE',  ( -51.75738570946856498, -135.7500000000000284, 3.805975901505576964 ) ) ;
#38124 = CARTESIAN_POINT ( 'NONE',  ( -4.458734124999999437, -51.31249999863440792, 0.000000000000000000 ) ) ;
#38125 = CARTESIAN_POINT ( 'NONE',  ( -3.152801135295367985, -158.0625000013656063, 3.152801135295367096 ) ) ;
#38126 = EDGE_CURVE ( 'NONE', #4186, #800, #37920, .T. ) ;
#38127 = CARTESIAN_POINT ( 'NONE',  ( -2.500000000000000444, -52.04166666393547303, -4.330127018922193649 ) ) ;
#38128 = ORIENTED_EDGE ( 'NONE', *, *, #23718, .T. ) ;
#38129 = CARTESIAN_POINT ( 'NONE',  ( 2.229367062500001939, -22.97916666530107221, 3.861377020970579999 ) ) ;
#38130 = ORIENTED_EDGE ( 'NONE', *, *, #22818, .F. ) ;
#38132 = CARTESIAN_POINT ( 'NONE',  ( -9.184850993605147944E-16, -142.3750000027312126, 5.000000000000000000 ) ) ;
#38131 = CARTESIAN_POINT ( 'NONE',  ( -1.339745962155610925, -95.79465819873851729, 5.000000000000000000 ) ) ;
#38133 = CARTESIAN_POINT ( 'NONE',  ( 4.458734125000000326, -160.3750000013656063, -1.846868145590734978 ) ) ;
#38134 = ORIENTED_EDGE ( 'NONE', *, *, #48929, .T. ) ;
#38135 = DIRECTION ( 'NONE',  ( 0.000000000000000000, 1.000000000000000000, 0.000000000000000000 ) ) ;
#38136 = CARTESIAN_POINT ( 'NONE',  ( -59.81910112700025905, -134.1875000000000284, -2.462841084822630311 ) ) ;
#38137 = CARTESIAN_POINT ( 'NONE',  ( -3.152548672688508926E-16, -36.81249999863440792, -5.148502694627439702 ) ) ;
#38138 = ORIENTED_EDGE ( 'NONE', *, *, #23832, .F. ) ;
#38139 = CARTESIAN_POINT ( 'NONE',  ( -4.458734124999998549, -82.22916666530107932, 2.574251347313722516 ) ) ;
#38140 = ADVANCED_FACE ( 'NONE', ( #27940 ), #13478, .T. ) ;
#38141 = CARTESIAN_POINT ( 'NONE',  ( 4.458734125000001214, 19.10416666803225638, 2.574251347313718519 ) ) ;
#38142 = CARTESIAN_POINT ( 'NONE',  ( 0.000000000000000000, -170.0000000000000000, 5.000000000000000000 ) ) ;
#38143 = ORIENTED_EDGE ( 'NONE', *, *, #39695, .F. ) ;
#38144 = CARTESIAN_POINT ( 'NONE',  ( -50.70258187064364108, -138.3750000013656063, 2.196230717870141014 ) ) ;
#38145 = CARTESIAN_POINT ( 'NONE',  ( -4.458734124999999437, -86.56249999863439371, 0.000000000000000000 ) ) ;
#38146 = CARTESIAN_POINT ( 'NONE',  ( -49.85088928181150436, -125.6875000027311984, -1.666127454062680702 ) ) ;
#38147 = CARTESIAN_POINT ( 'NONE',  ( 2.500000000000002220, -4.541666663935479242, 4.330127018922192761 ) ) ;
#38148 = CARTESIAN_POINT ( 'NONE',  ( 5.000000000000000000, -9.500000000000001776, -6.123233995736766282E-16 ) ) ;
#38149 = CARTESIAN_POINT ( 'NONE',  ( -5.000000000000000000, -46.87499999726880873, 0.000000000000000000 ) ) ;
#38150 = CARTESIAN_POINT ( 'NONE',  ( 2.229367062500001939, -60.97916666530106511, 3.861377020970579999 ) ) ;
#38151 = CARTESIAN_POINT ( 'NONE',  ( 2.499999999999998668, 10.66666666666666430, -4.330127018922193649 ) ) ;
#38152 = VECTOR ( 'NONE', #8564, 1000.000000000000000 ) ;
#38153 = CARTESIAN_POINT ( 'NONE',  ( 4.458734124999999437, 24.18750000136559564, -5.460374474430324690E-16 ) ) ;
#38154 = CARTESIAN_POINT ( 'NONE',  ( 1.975475456537005874E-15, -102.6249999972688158, 5.000000000000000000 ) ) ;
#38155 = DIRECTION ( 'NONE',  ( 0.000000000000000000, 1.000000000000000000, 0.000000000000000000 ) ) ;
#38156 = CARTESIAN_POINT ( 'NONE',  ( -3.152548672688508926E-16, -44.81249999863440792, -5.148502694627439702 ) ) ;
#38157 = CARTESIAN_POINT ( 'NONE',  ( 5.000000000000000888, -4.458333330602148870, 2.886751345948126879 ) ) ;
#38158 = CARTESIAN_POINT ( 'NONE',  ( -6.972266317189433020E-16, 2.750000000000000000, -5.000000000000000000 ) ) ;
#38159 = CARTESIAN_POINT ( 'NONE',  ( -2.500000000000000444, -67.04166666393547303, -4.330127018922193649 ) ) ;
#38160 = CARTESIAN_POINT ( 'NONE',  ( -2.229367062500000163, -86.72916666530107932, -3.861377020970580443 ) ) ;
#38161 = CARTESIAN_POINT ( 'NONE',  ( -2.229367062500000163, -106.4791666653010651, -3.861377020970580443 ) ) ;
#38162 = AXIS2_PLACEMENT_3D ( 'NONE', #55865, #41366, #37502 ) ;
#38163 = CARTESIAN_POINT ( 'NONE',  ( -4.458734124999997661, -8.479166665301073991, 2.574251347313722516 ) ) ;
#38164 =( BOUNDED_CURVE ( )  B_SPLINE_CURVE ( 2, ( #14099, #52096, #22834, #48514, #4453, #24082, #43677, #63319, #8035 ),
 .UNSPECIFIED., .F., .F. ) 
 B_SPLINE_CURVE_WITH_KNOTS ( ( 3, 2, 2, 2, 3 ),
 ( 0.7375000000000000444, 0.7380952380952381375, 0.7392857142857143238, 0.7404761904761905100, 0.7410714285714286031 ),
 .UNSPECIFIED. ) 
 CURVE ( )  GEOMETRIC_REPRESENTATION_ITEM ( )  RATIONAL_B_SPLINE_CURVE ( ( 0.9330127018922194093, 0.9330127018922194093, 1.000000000000000000, 0.8660254037844387076, 1.000000000000000000, 0.8660254037844387076, 1.000000000000000000, 0.9330127018922194093, 0.9330127018922194093 ) ) 
 REPRESENTATION_ITEM ( '' )  );
#38165 = ORIENTED_EDGE ( 'NONE', *, *, #19048, .F. ) ;
#38166 = CARTESIAN_POINT ( 'NONE',  ( -2.499999999999996447, -80.83333333333332860, 4.330127018922195425 ) ) ;
#38167 = CARTESIAN_POINT ( 'NONE',  ( -2.229367062499996610, -99.14583333196773651, 3.861377020970582219 ) ) ;
#38168 = CARTESIAN_POINT ( 'NONE',  ( 2.071067811865475505, -165.9375000027311842, -5.000000000000000888 ) ) ;
#38169 = CARTESIAN_POINT ( 'NONE',  ( -2.229367062499996610, -94.39583333196773651, 3.861377020970582219 ) ) ;
#38170 = EDGE_CURVE ( 'NONE', #52469, #16995, #52709, .T. ) ;
#38171 = CARTESIAN_POINT ( 'NONE',  ( -2.499999999999996447, -53.70833333060213732, 4.330127018922195425 ) ) ;
#38172 = CARTESIAN_POINT ( 'NONE',  ( -6.972266317189433020E-16, -37.12499999726881583, -5.000000000000000000 ) ) ;
#38173 = CARTESIAN_POINT ( 'NONE',  ( -57.89159099828107458, -129.6875000013656063, -3.393966926194107447 ) ) ;
#38174 = CARTESIAN_POINT ( 'NONE',  ( -4.458734124999997661, -15.22916666530107754, 2.574251347313722516 ) ) ;
#38175 = CARTESIAN_POINT ( 'NONE',  ( 2.229367062499998831, 12.10416666803226171, -3.861377020970580887 ) ) ;
#38176 = CARTESIAN_POINT ( 'NONE',  ( 4.458734125000000326, -61.14583333196773651, 2.574251347313718519 ) ) ;
#38177 = FACE_OUTER_BOUND ( 'NONE', #9247, .T. ) ;
#38178 = LINE ( 'NONE', #13413, #16215 ) ;
#38179 = CARTESIAN_POINT ( 'NONE',  ( 4.458734124999999437, -15.81249999863440436, -5.460374474430324690E-16 ) ) ;
#38180 = CARTESIAN_POINT ( 'NONE',  ( 1.975475456537005874E-15, -21.75000000000000000, 5.000000000000000000 ) ) ;
#38181 = ORIENTED_EDGE ( 'NONE', *, *, #40150, .F. ) ;
#38182 = CARTESIAN_POINT ( 'NONE',  ( 2.229367062500001939, -39.22916666530107221, 3.861377020970579999 ) ) ;
#38183 = UNCERTAINTY_MEASURE_WITH_UNIT (LENGTH_MEASURE( 1.000000000000000082E-05 ), #22932, 'distance_accuracy_value', 'NONE');
#38184 = CARTESIAN_POINT ( 'NONE',  ( -59.59170313451811296, -124.7500000013655921, 1.485763867205729394 ) ) ;
#38185 = CARTESIAN_POINT ( 'NONE',  ( 1.975475456537005874E-15, 0.3750000027311862216, 5.000000000000000000 ) ) ;
#38186 = CARTESIAN_POINT ( 'NONE',  ( -6.972266317189433020E-16, 26.87500000273118417, -5.000000000000000000 ) ) ;
#38187 = CARTESIAN_POINT ( 'NONE',  ( -2.229367062499996610, -87.14583333196773651, 3.861377020970582219 ) ) ;
#38188 = CARTESIAN_POINT ( 'NONE',  ( -3.152548672688508926E-16, 26.18750000136559564, -5.148502694627439702 ) ) ;
#38189 = CARTESIAN_POINT ( 'NONE',  ( 2.229367062500001939, 15.02083333469892779, 3.861377020970579999 ) ) ;
#38190 = CARTESIAN_POINT ( 'NONE',  ( -4.999999999999998224, -64.79166666393547303, 2.886751345948131764 ) ) ;
#38191 = CARTESIAN_POINT ( 'NONE',  ( 4.458734125000000326, -87.14583333196773651, 2.574251347313718519 ) ) ;
#38192 = CARTESIAN_POINT ( 'NONE',  ( -5.000000000000000000, -69.99999999999998579, 0.000000000000000000 ) ) ;
#38193 = CARTESIAN_POINT ( 'NONE',  ( -4.999999999999999112, 11.20833333606451632, 2.886751345948131764 ) ) ;
#38194 = EDGE_LOOP ( 'NONE', ( #25695, #6184, #5704, #26827 ) ) ;
#38195 = CARTESIAN_POINT ( 'NONE',  ( 2.500000000000002220, -79.66666666666665719, 4.330127018922192761 ) ) ;
#38196 = CARTESIAN_POINT ( 'NONE',  ( -4.999999999999998224, -89.91666666666667140, 2.886751345948131764 ) ) ;
#38198 = CARTESIAN_POINT ( 'NONE',  ( -5.000000000000000000, -27.08333333333333215, -2.886751345948128211 ) ) ;
#38197 = CARTESIAN_POINT ( 'NONE',  ( -2.500000000000000444, -109.0416666639354730, -4.330127018922193649 ) ) ;
#38199 = CARTESIAN_POINT ( 'NONE',  ( -4.458734124999998549, -34.22916666530107221, 2.574251347313722516 ) ) ;
#38200 = EDGE_CURVE ( 'NONE', #53062, #63665, #48971, .T. ) ;
#38201 = CARTESIAN_POINT ( 'NONE',  ( 2.500000000000002220, -33.54166666393547303, 4.330127018922192761 ) ) ;
#38202 = EDGE_CURVE ( 'NONE', #15910, #60851, #53125, .T. ) ;
#38204 = VERTEX_POINT ( 'NONE', #13781 ) ;
#38203 = CARTESIAN_POINT ( 'NONE',  ( -4.458734124999998549, -62.22916666530106511, 2.574251347313722516 ) ) ;
#38205 = CARTESIAN_POINT ( 'NONE',  ( -50.55543936806279248, -150.3125000013656063, 0.3552334253322060320 ) ) ;
#38207 = EDGE_LOOP ( 'NONE', ( #18042, #9845, #33362, #10246 ) ) ;
#38206 = CARTESIAN_POINT ( 'NONE',  ( 4.458734124999998549, -8.979166665301073991, -2.574251347313721627 ) ) ;
#38208 = EDGE_CURVE ( 'NONE', #62028, #14857, #61783, .T. ) ;
#38209 = CARTESIAN_POINT ( 'NONE',  ( -5.000000000000000000, -77.08333333333334281, -2.886751345948128211 ) ) ;
#38210 = CARTESIAN_POINT ( 'NONE',  ( -51.60603307380591787, -135.9375000013656063, -2.891590998281053704 ) ) ;
#38211 = CARTESIAN_POINT ( 'NONE',  ( -4.458734124999999437, -58.56249999863440081, 0.000000000000000000 ) ) ;
#38212 = EDGE_CURVE ( 'NONE', #54588, #56025, #55589, .T. ) ;
#38213 =( BOUNDED_CURVE ( )  B_SPLINE_CURVE ( 2, ( #25098, #28962, #59526, #43443, #63087, #28653, #34107, #18997, #24151 ),
 .UNSPECIFIED., .F., .F. ) 
 B_SPLINE_CURVE_WITH_KNOTS ( ( 3, 2, 2, 2, 3 ),
 ( 0.7339285714285714857, 0.7345238095238095788, 0.7357142857142857650, 0.7369047619047619513, 0.7375000000000000444 ),
 .UNSPECIFIED. ) 
 CURVE ( )  GEOMETRIC_REPRESENTATION_ITEM ( )  RATIONAL_B_SPLINE_CURVE ( ( 0.9330127018922194093, 0.9330127018922256266, 1.000000000000000000, 0.8660254037844387076, 1.000000000000000000, 0.8660254037844387076, 1.000000000000000000, 0.9330127018922194093, 0.9330127018922194093 ) ) 
 REPRESENTATION_ITEM ( '' )  );
#38214 = CARTESIAN_POINT ( 'NONE',  ( -5.000000000000000000, -81.95833333060213022, -2.886751345948128211 ) ) ;
#38216 = ORIENTED_EDGE ( 'NONE', *, *, #54428, .T. ) ;
#38215 = FACE_OUTER_BOUND ( 'NONE', #27795, .T. ) ;
#38217 = CARTESIAN_POINT ( 'NONE',  ( -50.18089887299979068, -143.6875000000000284, 2.462841084822635640 ) ) ;
#38218 = ADVANCED_FACE ( 'NONE', ( #59763 ), #39165, .T. ) ;
#38219 = CARTESIAN_POINT ( 'NONE',  ( -3.152548672688508926E-16, -20.81249999863440081, -5.148502694627439702 ) ) ;
#38220 = EDGE_CURVE ( 'NONE', #57381, #39445, #18190, .T. ) ;
#38222 = ORIENTED_EDGE ( 'NONE', *, *, #49885, .T. ) ;
#38221 = CARTESIAN_POINT ( 'NONE',  ( 2.229367062499998831, -57.89583333196773651, -3.861377020970580887 ) ) ;
#38223 = SHAPE_REPRESENTATION_RELATIONSHIP ( 'NONE' , 'NONE' ,  #14320, #57040 ) ;
#38224 = CARTESIAN_POINT ( 'NONE',  ( -4.458734125000001214, -165.1250000013656063, 1.846868145590734089 ) ) ;
#38225 = CARTESIAN_POINT ( 'NONE',  ( -2.229367062499996610, -103.3958333319677365, 3.861377020970582219 ) ) ;
#38226 = ORIENTED_EDGE ( 'NONE', *, *, #46381, .T. ) ;
#38227 = EDGE_CURVE ( 'NONE', #43422, #43716, #59709, .T. ) ;
#38228 = CARTESIAN_POINT ( 'NONE',  ( -58.39396692619412477, -148.6875000013656063, 2.891590998281057701 ) ) ;
#38229 = CARTESIAN_POINT ( 'NONE',  ( -60.14911071818854538, -139.1875000027312126, 1.666127454062681368 ) ) ;
#38230 = EDGE_CURVE ( 'NONE', #41293, #63519, #18910, .T. ) ;
#38231 = EDGE_CURVE ( 'NONE', #62831, #27835, #29829, .T. ) ;
#38232 = DIRECTION ( 'NONE',  ( 0.000000000000000000, 0.000000000000000000, 1.000000000000000000 ) ) ;
#38233 = CARTESIAN_POINT ( 'NONE',  ( -3.152548672688508926E-16, -7.562499998634404363, -5.148502694627439702 ) ) ;
#38234 = CARTESIAN_POINT ( 'NONE',  ( -2.229367062499996610, -102.3958333319677365, 3.861377020970582219 ) ) ;
#38235 = CARTESIAN_POINT ( 'NONE',  ( -3.152801135295367096, -143.3125000013655779, -3.152801135295367541 ) ) ;
#38236 = CARTESIAN_POINT ( 'NONE',  ( 2.229367062500001939, -28.22916666530107221, 3.861377020970579999 ) ) ;
#38237 = CARTESIAN_POINT ( 'NONE',  ( -50.01589407740564042, -139.7500000027312126, 0.3983568153799778022 ) ) ;
#38238 = CARTESIAN_POINT ( 'NONE',  ( -54.64476657466781973, -136.8125000013656063, -4.444560631937228834 ) ) ;
#38239 = CARTESIAN_POINT ( 'NONE',  ( 4.458734124999999437, -66.06249999863440792, -5.460374474430324690E-16 ) ) ;
#38240 = CARTESIAN_POINT ( 'NONE',  ( 1.339745962155615144, -43.70534180126147561, 4.999999999999999112 ) ) ;
#38241 = CARTESIAN_POINT ( 'NONE',  ( -5.000000000000000000, -34.08333333333332860, -2.886751345948128211 ) ) ;
#38242 = CARTESIAN_POINT ( 'NONE',  ( 5.000000000000000000, -68.41666666666667140, -2.886751345948130876 ) ) ;
#38243 = CARTESIAN_POINT ( 'NONE',  ( 4.458734125000000326, 6.854166668032259935, 2.574251347313718519 ) ) ;
#38244 = EDGE_LOOP ( 'NONE', ( #41194, #7228, #16293, #28861 ) ) ;
#38246 = CARTESIAN_POINT ( 'NONE',  ( -2.229367062499996610, -28.14583333196774007, 3.861377020970582219 ) ) ;
#38245 = CARTESIAN_POINT ( 'NONE',  ( -2.499999999999996447, -92.83333333333334281, 4.330127018922195425 ) ) ;
#38247 = CARTESIAN_POINT ( 'NONE',  ( -6.972266317189433020E-16, -77.12499999726881583, -5.000000000000000000 ) ) ;
#38248 = CARTESIAN_POINT ( 'NONE',  ( 9.457646018065525792E-16, -75.31249999863440792, 5.148502694627439702 ) ) ;
#38249 = CARTESIAN_POINT ( 'NONE',  ( 9.457646018065525792E-16, 25.68750000136559208, 5.148502694627439702 ) ) ;
#38250 = CARTESIAN_POINT ( 'NONE',  ( -5.000000000000000000, -101.9583333306021444, -2.886751345948128211 ) ) ;
#38251 = CARTESIAN_POINT ( 'NONE',  ( -53.51423613279429503, -142.2500000013656063, 4.591703134518082763 ) ) ;
#38252 = CARTESIAN_POINT ( 'NONE',  ( -2.229367062500000163, 0.5208333346989266754, -3.861377020970580443 ) ) ;
#38253 = CARTESIAN_POINT ( 'NONE',  ( -4.458734124999999437, 26.43750000136559564, 0.000000000000000000 ) ) ;
#38254 = CARTESIAN_POINT ( 'NONE',  ( -3.152548672688508926E-16, -36.81249999863440792, -5.148502694627439702 ) ) ;
#38255 = FACE_OUTER_BOUND ( 'NONE', #20384, .T. ) ;
#38256 = CARTESIAN_POINT ( 'NONE',  ( 4.458734125000000326, 0.1041666680322607674, 2.574251347313718519 ) ) ;
#38257 = CARTESIAN_POINT ( 'NONE',  ( 2.229367062500001939, -25.22916666530106866, 3.861377020970579999 ) ) ;
#38258 = CARTESIAN_POINT ( 'NONE',  ( 1.846868145590736310, -154.6250000013655779, 4.458734124999999437 ) ) ;
#38259 = CARTESIAN_POINT ( 'NONE',  ( 2.229367062499998831, -69.64583333196773651, -3.861377020970580887 ) ) ;
#38260 = CARTESIAN_POINT ( 'NONE',  ( 5.000000000000000000, -99.37499999726881583, -6.123233995736766282E-16 ) ) ;
#38261 = CARTESIAN_POINT ( 'NONE',  ( -2.229367062499996610, 28.85416666803226349, 3.861377020970582219 ) ) ;
#38262 = LINE ( 'NONE', #13809, #26682 ) ;
#38263 = CARTESIAN_POINT ( 'NONE',  ( -3.152548672688508926E-16, -106.8124999986343937, -5.148502694627439702 ) ) ;
#38264 = CARTESIAN_POINT ( 'NONE',  ( 4.458734124999999437, -72.06249999863439371, -5.460374474430324690E-16 ) ) ;
#38265 = CARTESIAN_POINT ( 'NONE',  ( -2.499999999999996447, -52.83333333333332860, 4.330127018922195425 ) ) ;
#38266 = CARTESIAN_POINT ( 'NONE',  ( -2.499999999999996447, -21.83333333333332860, 4.330127018922195425 ) ) ;
#38267 = CYLINDRICAL_SURFACE ( 'NONE', #18130, 5.000000000000000000 ) ;
#38268 = ORIENTED_EDGE ( 'NONE', *, *, #2434, .T. ) ;
#38269 = CARTESIAN_POINT ( 'NONE',  ( 0.000000000000000000, -170.0000000000000000, 0.000000000000000000 ) ) ;
#38270 = CARTESIAN_POINT ( 'NONE',  ( -2.499999999999996447, 12.29166666939785202, 4.330127018922195425 ) ) ;
#38271 = CARTESIAN_POINT ( 'NONE',  ( 5.000000000000000000, -11.41666666666666607, -2.886751345948129988 ) ) ;
#38272 = CARTESIAN_POINT ( 'NONE',  ( 2.229367062500001939, -15.97916666530107399, 3.861377020970579999 ) ) ;
#38273 = CARTESIAN_POINT ( 'NONE',  ( 2.229367062500001939, -78.97916666530106511, 3.861377020970579999 ) ) ;
#38274 = FACE_OUTER_BOUND ( 'NONE', #61218, .T. ) ;
#38275 = CARTESIAN_POINT ( 'NONE',  ( 5.000000000000000888, -18.45833333060214798, 2.886751345948126879 ) ) ;
#38277 = ORIENTED_EDGE ( 'NONE', *, *, #19414, .F. ) ;
#38276 = CARTESIAN_POINT ( 'NONE',  ( 9.457646018065525792E-16, -44.06249999863439371, 5.148502694627439702 ) ) ;
#38278 = DIRECTION ( 'NONE',  ( -0.000000000000000000, 1.000000000000000000, -0.000000000000000000 ) ) ;
#38280 = VERTEX_POINT ( 'NONE', #40122 ) ;
#38279 = CARTESIAN_POINT ( 'NONE',  ( 4.458734124999999437, 5.937500001365593860, -5.460374474430324690E-16 ) ) ;
#38281 = CARTESIAN_POINT ( 'NONE',  ( 1.975475456537005874E-15, -86.62499999726880162, 5.000000000000000000 ) ) ;
#38282 = CARTESIAN_POINT ( 'NONE',  ( -2.499999999999996447, -62.83333333333333570, 4.330127018922195425 ) ) ;
#38283 = CARTESIAN_POINT ( 'NONE',  ( 4.458734125000000326, -155.6250000013656063, -1.846868145590734978 ) ) ;
#38284 = CARTESIAN_POINT ( 'NONE',  ( 4.458734125000001214, -39.14583333196773651, 2.574251347313718519 ) ) ;
#38285 = CARTESIAN_POINT ( 'NONE',  ( 1.975475456537005874E-15, -64.74999999999998579, 5.000000000000000000 ) ) ;
#38286 = CARTESIAN_POINT ( 'NONE',  ( -9.184850993605147944E-16, -168.2500000000000000, 5.000000000000000000 ) ) ;
#38287 = DIRECTION ( 'NONE',  ( 0.000000000000000000, 0.000000000000000000, 1.000000000000000000 ) ) ;
#38288 = CARTESIAN_POINT ( 'NONE',  ( -57.19623071787017210, -129.6250000013655779, 4.297418129356382899 ) ) ;
#38289 = CARTESIAN_POINT ( 'NONE',  ( 4.458734124999998549, -4.979166665301072214, -2.574251347313721627 ) ) ;
#38290 = CARTESIAN_POINT ( 'NONE',  ( -4.458734124999999437, -40.64583333196773651, -2.574251347313719407 ) ) ;
#38291 =( BOUNDED_CURVE ( )  B_SPLINE_CURVE ( 2, ( #61096, #26988, #46607, #56586, #32117, #7697, #47243, #63528, #49032 ),
 .UNSPECIFIED., .F., .F. ) 
 B_SPLINE_CURVE_WITH_KNOTS ( ( 3, 2, 2, 2, 3 ),
 ( 0.4895833333333333148, 0.4902777777777777568, 0.4916666666666666408, 0.4930555555555555802, 0.4937500000000000222 ),
 .UNSPECIFIED. ) 
 CURVE ( )  GEOMETRIC_REPRESENTATION_ITEM ( )  RATIONAL_B_SPLINE_CURVE ( ( 0.9330127018922194093, 0.9330127018922194093, 1.000000000000000000, 0.8660254037844387076, 1.000000000000000000, 0.8660254037844387076, 1.000000000000000000, 0.9330127018922194093, 0.9330127018922194093 ) ) 
 REPRESENTATION_ITEM ( '' )  );
#38292 = CARTESIAN_POINT ( 'NONE',  ( 6.123233995736766282E-16, -120.0000000000000000, -5.000000000000000000 ) ) ;
#38293 = CARTESIAN_POINT ( 'NONE',  ( 2.730187237215162345E-16, -148.1875000013656063, -4.458734124999999437 ) ) ;
#38294 = CARTESIAN_POINT ( 'NONE',  ( 9.457646018065525792E-16, -82.31249999863440792, 5.148502694627439702 ) ) ;
#38295 = CARTESIAN_POINT ( 'NONE',  ( 2.499999999999998668, -34.20833333060213732, -4.330127018922193649 ) ) ;
#38296 = ORIENTED_EDGE ( 'NONE', *, *, #56183, .T. ) ;
#38297 = ADVANCED_FACE ( 'NONE', ( #15372 ), #1239, .T. ) ;
#38298 = CARTESIAN_POINT ( 'NONE',  ( -5.000000000000000888, -148.6875000027312126, -2.071067811865475949 ) ) ;
#38299 = CARTESIAN_POINT ( 'NONE',  ( -6.972266317189433020E-16, -96.25000000000000000, -5.000000000000000000 ) ) ;
#38300 = CARTESIAN_POINT ( 'NONE',  ( 4.458734124999998549, -73.97916666530106511, -2.574251347313721627 ) ) ;
#38301 = VERTEX_POINT ( 'NONE', #10534 ) ;
#38302 = ADVANCED_FACE ( 'NONE', ( #34666 ), #40441, .T. ) ;
#38303 = CARTESIAN_POINT ( 'NONE',  ( -6.972266317189433020E-16, 3.749999999999999556, -5.000000000000000000 ) ) ;
#38304 = CARTESIAN_POINT ( 'NONE',  ( -2.229367062499996610, -12.39583333196774007, 3.861377020970582219 ) ) ;
#38305 = CARTESIAN_POINT ( 'NONE',  ( -50.01589407740564042, -150.7500000027312410, 0.3983568153799778022 ) ) ;
#38306 = CARTESIAN_POINT ( 'NONE',  ( -3.152548672688508926E-16, 1.437500001365596525, -5.148502694627439702 ) ) ;
#38307 = CARTESIAN_POINT ( 'NONE',  ( -5.000000000000000000, -95.87499999726881583, 0.000000000000000000 ) ) ;
#38308 = CARTESIAN_POINT ( 'NONE',  ( 1.846868145590735200, -151.2500000013656063, -4.458734124999999437 ) ) ;
#38309 = CARTESIAN_POINT ( 'NONE',  ( -2.229367062500000163, 27.27083333469892779, -3.861377020970580443 ) ) ;
#38310 = ORIENTED_EDGE ( 'NONE', *, *, #55804, .T. ) ;
#38311 = CARTESIAN_POINT ( 'NONE',  ( -2.229367062499996610, -92.14583333196773651, 3.861377020970582219 ) ) ;
#38312 = CARTESIAN_POINT ( 'NONE',  ( 1.975475456537005874E-15, -57.62499999726880873, 5.000000000000000000 ) ) ;
#38313 = CARTESIAN_POINT ( 'NONE',  ( -51.75738570946856498, -153.8750000027312126, 3.805975901505576964 ) ) ;
#38314 = CARTESIAN_POINT ( 'NONE',  ( -4.458734124999999437, -9.312499998634406140, 0.000000000000000000 ) ) ;
#38315 = CARTESIAN_POINT ( 'NONE',  ( -5.000000000000000000, 28.04166666939785202, -2.886751345948128211 ) ) ;
#38316 = CARTESIAN_POINT ( 'NONE',  ( 6.123233995736766282E-16, -170.0000000000000000, -5.000000000000000000 ) ) ;
#38317 = CARTESIAN_POINT ( 'NONE',  ( -50.40829686548195099, -152.0000000013655779, -1.485763867205728284 ) ) ;
#38318 = CARTESIAN_POINT ( 'NONE',  ( 5.000000000000000000, -35.37499999726881583, -6.123233995736766282E-16 ) ) ;
#38319 = CARTESIAN_POINT ( 'NONE',  ( 0.000000000000000000, -170.0000000000000000, 0.000000000000000000 ) ) ;
#38320 = CARTESIAN_POINT ( 'NONE',  ( -2.229367062500000163, 18.52083333469892779, -3.861377020970580443 ) ) ;
#38321 = CARTESIAN_POINT ( 'NONE',  ( 4.458734124999999437, 22.18750000136559564, -5.460374474430324690E-16 ) ) ;
#38322 = CARTESIAN_POINT ( 'NONE',  ( 9.457646018065525792E-16, -56.06249999863440792, 5.148502694627439702 ) ) ;
#38323 = CARTESIAN_POINT ( 'NONE',  ( -2.229367062499996610, -11.39583333196773829, 3.861377020970582219 ) ) ;
#38324 = CARTESIAN_POINT ( 'NONE',  ( -4.999999999999998224, -62.91666666666665719, 2.886751345948131764 ) ) ;
#38325 = CARTESIAN_POINT ( 'NONE',  ( -2.500000000000000444, 11.83333333333333037, -4.330127018922193649 ) ) ;
#38326 = CARTESIAN_POINT ( 'NONE',  ( -8.190561711645485556E-16, -166.6875000013655779, 4.458734124999999437 ) ) ;
#38327 = LINE ( 'NONE', #8123, #40761 ) ;
#38328 = CARTESIAN_POINT ( 'NONE',  ( -2.229367062500000163, -47.47916666530106511, -3.861377020970580443 ) ) ;
#38329 = CARTESIAN_POINT ( 'NONE',  ( 2.499999999999998668, -83.20833333060214443, -4.330127018922193649 ) ) ;
#38330 = CARTESIAN_POINT ( 'NONE',  ( -57.19623071787017210, -134.6250000013656347, 4.297418129356382899 ) ) ;
#38331 = DIRECTION ( 'NONE',  ( -0.8191520442889907994, 1.003171929053523514E-16, 0.5735764363510474917 ) ) ;
#38332 = CARTESIAN_POINT ( 'NONE',  ( -4.999999999999998224, -91.91666666666667140, 2.886751345948131764 ) ) ;
#38333 = CARTESIAN_POINT ( 'NONE',  ( -4.458734124999999437, -91.56249999863440792, 0.000000000000000000 ) ) ;
#38334 = CARTESIAN_POINT ( 'NONE',  ( -1.846868145590734756, -157.3750000013655779, -4.458734124999999437 ) ) ;
#38335 =( BOUNDED_CURVE ( )  B_SPLINE_CURVE ( 2, ( #52041, #58112, #62950, #52355, #4096, #57191, #48460, #52972, #7980 ),
 .UNSPECIFIED., .F., .F. ) 
 B_SPLINE_CURVE_WITH_KNOTS ( ( 3, 2, 2, 2, 3 ),
 ( 0.9229166666666667185, 0.9236111111111111605, 0.9250000000000000444, 0.9263888888888889284, 0.9270833333333333703 ),
 .UNSPECIFIED. ) 
 CURVE ( )  GEOMETRIC_REPRESENTATION_ITEM ( )  RATIONAL_B_SPLINE_CURVE ( ( 0.9330127018922194093, 0.9330127018922194093, 1.000000000000000000, 0.8660254037844387076, 1.000000000000000000, 0.8660254037844387076, 1.000000000000000000, 0.9330127018922194093, 0.9330127018922194093 ) ) 
 REPRESENTATION_ITEM ( '' )  );
#38336 = CARTESIAN_POINT ( 'NONE',  ( -4.999999999999999112, -37.91666666666666430, 2.886751345948131764 ) ) ;
#38337 = CARTESIAN_POINT ( 'NONE',  ( 5.000000000000000000, 8.708333336064518093, -2.886751345948130876 ) ) ;
#38338 = CARTESIAN_POINT ( 'NONE',  ( 5.000000000000000000, -163.0625000000000000, 2.071067811865478614 ) ) ;
#38339 = ORIENTED_EDGE ( 'NONE', *, *, #36542, .F. ) ;
#38340 = CARTESIAN_POINT ( 'NONE',  ( 9.457646018065525792E-16, -95.06249999863440792, 5.148502694627439702 ) ) ;
#38341 = CARTESIAN_POINT ( 'NONE',  ( -4.458734124999999437, 8.354166668032261711, -2.574251347313719407 ) ) ;
#38342 = CARTESIAN_POINT ( 'NONE',  ( 1.060575238724906964E-15, 9.375000002731184168, 5.773502691896257311 ) ) ;
#38343 = CARTESIAN_POINT ( 'NONE',  ( 5.000000000000000000, -80.50000000000000000, -6.123233995736766282E-16 ) ) ;
#38344 = CARTESIAN_POINT ( 'NONE',  ( 5.000000000000000000, 3.499999999999999556, -6.123233995736766282E-16 ) ) ;
#38345 = CARTESIAN_POINT ( 'NONE',  ( 2.229367062500001939, -58.97916666530106511, 3.861377020970579999 ) ) ;
#38346 = CARTESIAN_POINT ( 'NONE',  ( -2.499999999999996447, -39.83333333333332860, 4.330127018922195425 ) ) ;
#38347 = CARTESIAN_POINT ( 'NONE',  ( 1.060575238724906964E-15, 1.375000002731184834, 5.773502691896257311 ) ) ;
#38348 = CARTESIAN_POINT ( 'NONE',  ( 2.229367062500001939, -29.97916666530107221, 3.861377020970579999 ) ) ;
#38349 = CARTESIAN_POINT ( 'NONE',  ( 5.000000000000000000, 17.62500000273118417, -6.123233995736766282E-16 ) ) ;
#38350 = CARTESIAN_POINT ( 'NONE',  ( -6.972266317189433020E-16, 19.75000000000000000, -5.000000000000000000 ) ) ;
#38351 = CARTESIAN_POINT ( 'NONE',  ( 6.123233995736766282E-16, -170.0000000000000000, -5.000000000000000000 ) ) ;
#38352 = CARTESIAN_POINT ( 'NONE',  ( -3.535250795749689387E-16, -45.25000000000000000, -5.773502691896257311 ) ) ;
#38354 = CARTESIAN_POINT ( 'NONE',  ( -3.152548672688508926E-16, -21.81249999863440436, -5.148502694627439702 ) ) ;
#38353 = CARTESIAN_POINT ( 'NONE',  ( 1.975475456537005874E-15, -72.75000000000000000, 5.000000000000000000 ) ) ;
#38355 = CARTESIAN_POINT ( 'NONE',  ( 3.535533905932736864, -155.1250000000000000, 3.535533905932738641 ) ) ;
#38356 = CARTESIAN_POINT ( 'NONE',  ( 2.229367062499998831, -71.64583333196773651, -3.861377020970580887 ) ) ;
#38357 = CARTESIAN_POINT ( 'NONE',  ( 1.846868145590735200, -149.5000000013655779, -4.458734125000000326 ) ) ;
#38358 = CARTESIAN_POINT ( 'NONE',  ( 9.457646018065525792E-16, -76.06249999863440792, 5.148502694627439702 ) ) ;
#38359 = CARTESIAN_POINT ( 'NONE',  ( -53.51423613279429503, -141.5000000013656063, 4.591703134518082763 ) ) ;
#38360 = CARTESIAN_POINT ( 'NONE',  ( 4.458734125000001214, -24.14583333196773651, 2.574251347313718519 ) ) ;
#38361 = CARTESIAN_POINT ( 'NONE',  ( 1.060575238724906964E-15, -66.62499999726881583, 5.773502691896257311 ) ) ;
#38362 = VERTEX_POINT ( 'NONE', #4755 ) ;
#38363 = CARTESIAN_POINT ( 'NONE',  ( 2.499999999999998668, -93.20833333060214443, -4.330127018922193649 ) ) ;
#38364 = ORIENTED_EDGE ( 'NONE', *, *, #10634, .F. ) ;
#38365 = CARTESIAN_POINT ( 'NONE',  ( 4.458734124999999437, -67.06249999863440792, -5.460374474430324690E-16 ) ) ;
#38366 = CARTESIAN_POINT ( 'NONE',  ( -5.000000000000000000, 8.041666669397852019, -2.886751345948128211 ) ) ;
#38367 = DIRECTION ( 'NONE',  ( 0.000000000000000000, 0.000000000000000000, 1.000000000000000000 ) ) ;
#38368 = ORIENTED_EDGE ( 'NONE', *, *, #35533, .F. ) ;
#38369 = CARTESIAN_POINT ( 'NONE',  ( -1.339745962155610925, -82.79465819873851729, 5.000000000000000000 ) ) ;
#38370 = CARTESIAN_POINT ( 'NONE',  ( -4.458734124999999437, -55.64583333196773651, -2.574251347313719407 ) ) ;
#38371 = CARTESIAN_POINT ( 'NONE',  ( -4.458734124999999437, 0.3541666680322609340, -2.574251347313719407 ) ) ;
#38372 = ORIENTED_EDGE ( 'NONE', *, *, #47180, .T. ) ;
#38373 = CARTESIAN_POINT ( 'NONE',  ( 5.000000000000000000, -45.50000000000000000, -6.123233995736766282E-16 ) ) ;
#38374 = CARTESIAN_POINT ( 'NONE',  ( 2.229367062499998831, 18.35416666803225993, -3.861377020970580887 ) ) ;
#38375 = CARTESIAN_POINT ( 'NONE',  ( -50.55543936806279248, -145.0625000013656063, 0.3552334253322060320 ) ) ;
#38376 = CARTESIAN_POINT ( 'NONE',  ( -6.972266317189433020E-16, -2.250000000000000000, -5.000000000000000000 ) ) ;
#38377 = CARTESIAN_POINT ( 'NONE',  ( 1.846868145590735200, -164.2500000013656063, -4.458734124999999437 ) ) ;
#38378 =( BOUNDED_CURVE ( )  B_SPLINE_CURVE ( 2, ( #27465, #61261, #2106, #37135, #36811, #1782, #26522, #55798, #57073 ),
 .UNSPECIFIED., .F., .T. ) 
 B_SPLINE_CURVE_WITH_KNOTS ( ( 3, 2, 2, 2, 3 ),
 ( 0.1250000000000001110, 0.1291666666666667906, 0.1333333333333334425, 0.1375000000000001221, 0.1416666666666667740 ),
 .UNSPECIFIED. ) 
 CURVE ( )  GEOMETRIC_REPRESENTATION_ITEM ( )  RATIONAL_B_SPLINE_CURVE ( ( 0.9999999999999980016, 0.9238795325112887369, 1.000000000000000000, 0.9238795325112867385, 1.000000000000000000, 0.9238795325112867385, 1.000000000000000000, 0.9238795325112847401, 1.000000000000001998 ) ) 
 REPRESENTATION_ITEM ( '' )  );
#38379 = ORIENTED_EDGE ( 'NONE', *, *, #17743, .F. ) ;
#38380 = CARTESIAN_POINT ( 'NONE',  ( -4.458734124999999437, -75.39583333196773651, -2.574251347313719407 ) ) ;
#38381 = CARTESIAN_POINT ( 'NONE',  ( 5.000000000000000000, 14.62500000273118594, -6.123233995736766282E-16 ) ) ;
#38382 = CARTESIAN_POINT ( 'NONE',  ( -4.458734124999998549, 7.770833334698925121, 2.574251347313722516 ) ) ;
#38383 = CARTESIAN_POINT ( 'NONE',  ( -2.071067811865538566, -162.8125000027311842, -4.999999999999937828 ) ) ;
#38384 = CARTESIAN_POINT ( 'NONE',  ( -3.152548672688508926E-16, -59.81249999863440792, -5.148502694627439702 ) ) ;
#38385 = CARTESIAN_POINT ( 'NONE',  ( 1.060575238724906964E-15, -21.62499999726881228, 5.773502691896257311 ) ) ;
#38386 = CARTESIAN_POINT ( 'NONE',  ( -57.46284108482265651, -141.9375000000000284, 4.819101127000238627 ) ) ;
#38387 = CARTESIAN_POINT ( 'NONE',  ( 1.975475456537005874E-15, -45.74999999999999289, 5.000000000000000000 ) ) ;
#38388 = CARTESIAN_POINT ( 'NONE',  ( 5.000000000000000000, -61.41666666666665719, -2.886751345948130876 ) ) ;
#38389 = CARTESIAN_POINT ( 'NONE',  ( 6.123233995736766282E-16, -120.0000000000000000, -5.000000000000000000 ) ) ;
#38390 = FACE_OUTER_BOUND ( 'NONE', #20635, .T. ) ;
#38391 = CARTESIAN_POINT ( 'NONE',  ( -4.458734124999999437, -41.31249999863440081, 0.000000000000000000 ) ) ;
#38392 = PRODUCT_DEFINITION_SHAPE ( 'NONE', 'NONE',  #63676 ) ;
#38393 = CARTESIAN_POINT ( 'NONE',  ( 4.458734124999998549, -27.97916666530107221, -2.574251347313721627 ) ) ;
#38394 = CARTESIAN_POINT ( 'NONE',  ( -58.80597590150559739, -144.0000000000000284, 3.242614290531460330 ) ) ;
#38395 = CARTESIAN_POINT ( 'NONE',  ( -3.535250795749689387E-16, 23.75000000000000000, -5.773502691896257311 ) ) ;
#38396 = CARTESIAN_POINT ( 'NONE',  ( -2.071067811865475061, -150.8125000027311842, -5.000000000000000888 ) ) ;
#38397 = CARTESIAN_POINT ( 'NONE',  ( 4.458734124999998549, -105.9791666653010651, -2.574251347313721627 ) ) ;
#38398 = EDGE_CURVE ( 'NONE', #19213, #53853, #59443, .T. ) ;
#38399 = CARTESIAN_POINT ( 'NONE',  ( 4.458734125000001214, -32.89583333196774362, 2.574251347313718519 ) ) ;
#38400 = CARTESIAN_POINT ( 'NONE',  ( 5.000000000000000000, -68.29166666393547303, -2.886751345948129988 ) ) ;
#38401 = CARTESIAN_POINT ( 'NONE',  ( -50.40829686548195099, -148.2500000013656063, -1.485763867205728284 ) ) ;
#38402 = CARTESIAN_POINT ( 'NONE',  ( -5.000000000000000888, -143.4375000000000284, 2.071067811865474617 ) ) ;
#38403 = CARTESIAN_POINT ( 'NONE',  ( -3.152548672688508926E-16, -75.81249999863440792, -5.148502694627439702 ) ) ;
#38404 = DIRECTION ( 'NONE',  ( -0.000000000000000000, 1.000000000000000000, -0.000000000000000000 ) ) ;
#38405 = CARTESIAN_POINT ( 'NONE',  ( -2.229367062500000163, -29.47916666530107221, -3.861377020970580443 ) ) ;
#38406 = CARTESIAN_POINT ( 'NONE',  ( -60.14911071818854538, -136.1875000027312126, 1.666127454062681146 ) ) ;
#38407 = CARTESIAN_POINT ( 'NONE',  ( 1.339745962155612702, -45.16965819600733312, -5.000000000000000000 ) ) ;
#38408 = CARTESIAN_POINT ( 'NONE',  ( 5.000000000000000888, -24.58333333333333215, 2.886751345948126879 ) ) ;
#38409 = CARTESIAN_POINT ( 'NONE',  ( -4.458734125000000326, -149.0000000013656063, -1.846868145590735644 ) ) ;
#38410 = ORIENTED_EDGE ( 'NONE', *, *, #11047, .F. ) ;
#38411 = CARTESIAN_POINT ( 'NONE',  ( -3.152548672688508926E-16, -55.81249999863440081, -5.148502694627439702 ) ) ;
#38412 = CARTESIAN_POINT ( 'NONE',  ( 1.060575238724906964E-15, 28.37500000273118417, 5.773502691896257311 ) ) ;
#38413 = CARTESIAN_POINT ( 'NONE',  ( 1.339745962155615144, -90.58034179853029855, 4.999999999999999112 ) ) ;
#38414 = CARTESIAN_POINT ( 'NONE',  ( -5.000000000000000000, 20.99999999999999645, 0.000000000000000000 ) ) ;
#38415 = DIRECTION ( 'NONE',  ( -0.000000000000000000, 1.000000000000000000, -0.000000000000000000 ) ) ;
#38416 = CARTESIAN_POINT ( 'NONE',  ( 4.458734124999999437, -4.812499998634402587, -5.460374474430324690E-16 ) ) ;
#38417 = CARTESIAN_POINT ( 'NONE',  ( -5.000000000000000000, -11.00000000000000355, 0.000000000000000000 ) ) ;
#38418 = CARTESIAN_POINT ( 'NONE',  ( -4.458734124999999437, 12.35416666803225993, -2.574251347313719407 ) ) ;
#38419 = CARTESIAN_POINT ( 'NONE',  ( 6.972266317189433020E-16, 28.87500000273118417, -5.000000000000000000 ) ) ;
#38420 = ORIENTED_EDGE ( 'NONE', *, *, #19666, .T. ) ;
#38421 = CARTESIAN_POINT ( 'NONE',  ( -6.972266317189433020E-16, -97.12499999726880162, -5.000000000000000000 ) ) ;
#38422 = CARTESIAN_POINT ( 'NONE',  ( -3.152548672688508926E-16, -49.56249999863440792, -5.148502694627439702 ) ) ;
#38423 = CARTESIAN_POINT ( 'NONE',  ( 2.730187237215162345E-16, -159.4375000013655779, -4.458734124999999437 ) ) ;
#38424 = CARTESIAN_POINT ( 'NONE',  ( 2.499999999999998668, -48.20833333060215153, -4.330127018922193649 ) ) ;
#38425 = ORIENTED_EDGE ( 'NONE', *, *, #12931, .T. ) ;
#38426 = CARTESIAN_POINT ( 'NONE',  ( 4.458734124999999437, -23.81249999863440436, -5.460374474430324690E-16 ) ) ;
#38427 = ORIENTED_EDGE ( 'NONE', *, *, #13364, .F. ) ;
#38429 = CARTESIAN_POINT ( 'NONE',  ( 0.000000000000000000, 0.000000000000000000, -8.499999999999998224 ) ) ;
#38428 = CARTESIAN_POINT ( 'NONE',  ( 1.339745962155612702, -56.29465819873852439, -5.000000000000000000 ) ) ;
#38430 = CARTESIAN_POINT ( 'NONE',  ( -4.458734125000000326, -159.0000000013656063, -1.846868145590735644 ) ) ;
#38431 = VERTEX_POINT ( 'NONE', #54929 ) ;
#38432 = CARTESIAN_POINT ( 'NONE',  ( 1.975475456537005874E-15, -50.62499999726881583, 5.000000000000000000 ) ) ;
#38433 = CARTESIAN_POINT ( 'NONE',  ( -59.81910112700025905, -132.1875000000000568, -2.462841084822630311 ) ) ;
#38434 = CARTESIAN_POINT ( 'NONE',  ( -4.999999999999998224, -23.91666666666666785, 2.886751345948131764 ) ) ;
#38435 = CARTESIAN_POINT ( 'NONE',  ( -3.152548672688508926E-16, -37.81249999863440792, -5.148502694627439702 ) ) ;
#38436 = VERTEX_POINT ( 'NONE', #10223 ) ;
#38437 = CARTESIAN_POINT ( 'NONE',  ( -3.152548672688508926E-16, -84.56249999863439371, -5.148502694627439702 ) ) ;
#38438 = CARTESIAN_POINT ( 'NONE',  ( -3.152548672688508926E-16, 20.43750000136559208, -5.148502694627439702 ) ) ;
#38439 = CARTESIAN_POINT ( 'NONE',  ( 5.000000000000000888, -59.58333333333335702, 2.886751345948126879 ) ) ;
#38440 = ORIENTED_EDGE ( 'NONE', *, *, #32984, .T. ) ;
#38441 = CARTESIAN_POINT ( 'NONE',  ( -3.152548672688508926E-16, -85.81249999863440792, -5.148502694627439702 ) ) ;
#38442 = CARTESIAN_POINT ( 'NONE',  ( -59.81910112700025905, -127.3125000027312552, -2.462841084822630311 ) ) ;
#38443 = CARTESIAN_POINT ( 'NONE',  ( 5.000000000000000888, -35.45833333060213732, 2.886751345948126879 ) ) ;
#38444 = CARTESIAN_POINT ( 'NONE',  ( -50.95487605259684472, -135.0000000000000853, 2.386008429272880704 ) ) ;
#38445 = CARTESIAN_POINT ( 'NONE',  ( 5.000000000000000888, -145.0625000027311842, -2.071067811865475505 ) ) ;
#38446 = CARTESIAN_POINT ( 'NONE',  ( -2.229367062500000163, -62.47916666530106511, -3.861377020970580443 ) ) ;
#38447 = CARTESIAN_POINT ( 'NONE',  ( 6.123233995736766282E-16, -170.0000000000000000, -5.000000000000000000 ) ) ;
#38448 = CARTESIAN_POINT ( 'NONE',  ( 2.229367062500001939, 24.02083333469892779, 3.861377020970579999 ) ) ;
#38449 =( BOUNDED_CURVE ( )  B_SPLINE_CURVE ( 2, ( #22063, #17560, #61625, #41655, #37178, #57121, #61943, #37483, #61306 ),
 .UNSPECIFIED., .F., .F. ) 
 B_SPLINE_CURVE_WITH_KNOTS ( ( 3, 2, 2, 2, 3 ),
 ( 0.8303571428571429047, 0.8309523809523809978, 0.8321428571428571841, 0.8333333333333333703, 0.8339285714285714635 ),
 .UNSPECIFIED. ) 
 CURVE ( )  GEOMETRIC_REPRESENTATION_ITEM ( )  RATIONAL_B_SPLINE_CURVE ( ( 0.9330127018922194093, 0.9330127018922194093, 1.000000000000000000, 0.8660254037844387076, 1.000000000000000000, 0.8660254037844387076, 1.000000000000000000, 0.9330127018922194093, 0.9330127018922194093 ) ) 
 REPRESENTATION_ITEM ( '' )  );
#38450 = DIRECTION ( 'NONE',  ( 0.5000000000000001110, 0.000000000000000000, -0.8660254037844387076 ) ) ;
#38451 = CARTESIAN_POINT ( 'NONE',  ( -4.458734124999999437, -45.64583333196774362, -2.574251347313719407 ) ) ;
#38452 = CARTESIAN_POINT ( 'NONE',  ( 5.000000000000000000, -2.374999997268815388, -6.123233995736766282E-16 ) ) ;
#38453 = FACE_OUTER_BOUND ( 'NONE', #161, .T. ) ;
#38454 = DIRECTION ( 'NONE',  ( -0.000000000000000000, 1.000000000000000000, -0.000000000000000000 ) ) ;
#38455 = CARTESIAN_POINT ( 'NONE',  ( -3.152548672688508926E-16, -83.81249999863439371, -5.148502694627439702 ) ) ;
#38456 = CARTESIAN_POINT ( 'NONE',  ( -3.152548672688508926E-16, -109.5624999986344079, -5.148502694627439702 ) ) ;
#38457 = CARTESIAN_POINT ( 'NONE',  ( -4.458734124999999437, -9.645833331967738289, -2.574251347313719407 ) ) ;
#38458 = ORIENTED_EDGE ( 'NONE', *, *, #45601, .F. ) ;
#38459 = CARTESIAN_POINT ( 'NONE',  ( -2.071067811865538566, -163.8125000027312126, -4.999999999999937828 ) ) ;
#38460 = CARTESIAN_POINT ( 'NONE',  ( -4.458734124999999437, -97.39583333196773651, -2.574251347313719407 ) ) ;
#38461 = CARTESIAN_POINT ( 'NONE',  ( 3.535533905932738197, -165.0000000027312126, -3.535533905932738197 ) ) ;
#38462 = CARTESIAN_POINT ( 'NONE',  ( -4.458734124999999437, -92.64583333196773651, -2.574251347313719407 ) ) ;
#38463 = EDGE_CURVE ( 'NONE', #42072, #26895, #28877, .T. ) ;
#38464 = CARTESIAN_POINT ( 'NONE',  ( 2.500000000000002220, -54.54166666393548013, 4.330127018922192761 ) ) ;
#38465 = CARTESIAN_POINT ( 'NONE',  ( 5.000000000000000000, -5.416666666666666963, -2.886751345948130876 ) ) ;
#38466 = CIRCLE ( 'NONE', #24066, 5.000000000000000888 ) ;
#38467 = CARTESIAN_POINT ( 'NONE',  ( -50.70258187064364108, -130.1250000013656347, 2.196230717870141014 ) ) ;
#38468 =( BOUNDED_CURVE ( )  B_SPLINE_CURVE ( 2, ( #41396, #36579, #57484, #58718, #4680, #14644, #28500, #3444, #48119 ),
 .UNSPECIFIED., .F., .F. ) 
 B_SPLINE_CURVE_WITH_KNOTS ( ( 3, 2, 2, 2, 3 ),
 ( 0.3187499999999999778, 0.3194444444444444198, 0.3208333333333333592, 0.3222222222222222432, 0.3229166666666666852 ),
 .UNSPECIFIED. ) 
 CURVE ( )  GEOMETRIC_REPRESENTATION_ITEM ( )  RATIONAL_B_SPLINE_CURVE ( ( 0.9330127018922194093, 0.9330127018922194093, 1.000000000000000000, 0.8660254037844387076, 1.000000000000000000, 0.8660254037844387076, 1.000000000000000000, 0.9330127018922194093, 0.9330127018922194093 ) ) 
 REPRESENTATION_ITEM ( '' )  );
#38469 = CARTESIAN_POINT ( 'NONE',  ( -56.48576386720575471, -145.7500000013656063, -4.591703134518078322 ) ) ;
#38470 = CARTESIAN_POINT ( 'NONE',  ( -4.458734124999999437, -14.31249999863440436, 0.000000000000000000 ) ) ;
#38471 = CARTESIAN_POINT ( 'NONE',  ( 2.229367062500001939, 11.77083333469892601, 3.861377020970579999 ) ) ;
#38472 = CARTESIAN_POINT ( 'NONE',  ( -2.229367062499996610, -60.39583333196774362, 3.861377020970582219 ) ) ;
#38473 = CARTESIAN_POINT ( 'NONE',  ( 0.000000000000000000, -170.0000000000000000, 0.000000000000000000 ) ) ;
#38474 = CARTESIAN_POINT ( 'NONE',  ( -4.458734124999999437, -14.39583333196773474, -2.574251347313719407 ) ) ;
#38475 = DIRECTION ( 'NONE',  ( -0.000000000000000000, 1.000000000000000000, -0.000000000000000000 ) ) ;
#38476 = ORIENTED_EDGE ( 'NONE', *, *, #7236, .F. ) ;
#38477 = CARTESIAN_POINT ( 'NONE',  ( -2.229367062499996610, -43.39583333196773651, 3.861377020970582219 ) ) ;
#38478 = CARTESIAN_POINT ( 'NONE',  ( -5.000000000000000000, -11.99999999999999645, 0.000000000000000000 ) ) ;
#38479 = EDGE_CURVE ( 'NONE', #43626, #46822, #24757, .T. ) ;
#38480 = CARTESIAN_POINT ( 'NONE',  ( -6.972266317189433020E-16, -30.25000000000000000, -5.000000000000000000 ) ) ;
#38481 = CARTESIAN_POINT ( 'NONE',  ( 2.229367062500001939, -87.97916666530107932, 3.861377020970579999 ) ) ;
#38482 = CARTESIAN_POINT ( 'NONE',  ( -4.458734124999999437, 17.35416666803225993, -2.574251347313719407 ) ) ;
#38483 = CARTESIAN_POINT ( 'NONE',  ( -4.458734124999998549, 14.77083333469892779, 2.574251347313722516 ) ) ;
#38484 = CARTESIAN_POINT ( 'NONE',  ( -2.500000000000000444, -48.16666666666666430, -4.330127018922193649 ) ) ;
#38485 = EDGE_CURVE ( 'NONE', #2538, #58058, #2607, .T. ) ;
#38486 = CARTESIAN_POINT ( 'NONE',  ( -56.66612745406293783, -137.4375000027312126, -5.149110718188535607 ) ) ;
#38487 = CARTESIAN_POINT ( 'NONE',  ( -3.152548672688508926E-16, -89.81249999863440792, -5.148502694627439702 ) ) ;
#38488 = CARTESIAN_POINT ( 'NONE',  ( -3.535250795749689387E-16, -70.25000000000000000, -5.773502691896257311 ) ) ;
#38489 = CARTESIAN_POINT ( 'NONE',  ( 1.060575238724906964E-15, 13.37500000273118594, 5.773502691896257311 ) ) ;
#38490 = ORIENTED_EDGE ( 'NONE', *, *, #12576, .T. ) ;
#38491 = CARTESIAN_POINT ( 'NONE',  ( 6.123233995736766282E-16, -120.0000000000000000, -5.000000000000000000 ) ) ;
#38492 = ORIENTED_EDGE ( 'NONE', *, *, #6766, .T. ) ;
#38493 = CARTESIAN_POINT ( 'NONE',  ( 1.975475456537005874E-15, -79.62499999726881583, 5.000000000000000000 ) ) ;
#38495 = CARTESIAN_POINT ( 'NONE',  ( 5.000000000000000000, -26.49999999999999645, -6.123233995736766282E-16 ) ) ;
#38494 = CARTESIAN_POINT ( 'NONE',  ( -6.972266317189433020E-16, -85.25000000000000000, -5.000000000000000000 ) ) ;
#38496 = CARTESIAN_POINT ( 'NONE',  ( 4.458734124999999437, -32.81249999863440792, -5.460374474430324690E-16 ) ) ;
#38497 = CARTESIAN_POINT ( 'NONE',  ( 5.000000000000000000, -36.37499999726881583, -6.123233995736766282E-16 ) ) ;
#38499 = ORIENTED_EDGE ( 'NONE', *, *, #26451, .T. ) ;
#38498 = CARTESIAN_POINT ( 'NONE',  ( -4.458734124999999437, -68.31249999863439371, 0.000000000000000000 ) ) ;
#38500 = CARTESIAN_POINT ( 'NONE',  ( -53.51423613279429503, -150.5000000013655779, 4.591703134518082763 ) ) ;
#38502 = ORIENTED_EDGE ( 'NONE', *, *, #33570, .F. ) ;
#38501 = CARTESIAN_POINT ( 'NONE',  ( 9.457646018065525792E-16, -15.31249999863440436, 5.148502694627439702 ) ) ;
#38503 = CARTESIAN_POINT ( 'NONE',  ( 2.500000000000002220, -77.66666666666665719, 4.330127018922192761 ) ) ;
#38504 = CARTESIAN_POINT ( 'NONE',  ( 2.499999999999998668, 28.79166666939784847, -4.330127018922193649 ) ) ;
#38505 = CARTESIAN_POINT ( 'NONE',  ( 4.458734125000001214, -57.14583333196773651, 2.574251347313718519 ) ) ;
#38506 = CARTESIAN_POINT ( 'NONE',  ( -2.500000000000000444, -84.04166666393547303, -4.330127018922193649 ) ) ;
#38508 = ORIENTED_EDGE ( 'NONE', *, *, #44508, .T. ) ;
#38507 = DIRECTION ( 'NONE',  ( 0.000000000000000000, 0.000000000000000000, 1.000000000000000000 ) ) ;
#38509 = CARTESIAN_POINT ( 'NONE',  ( -54.60164318462004474, -146.3750000000000284, -4.984105922594373794 ) ) ;
#38510 = CARTESIAN_POINT ( 'NONE',  ( -4.458734124999998549, -23.47916666530107577, 2.574251347313722516 ) ) ;
#38512 = ORIENTED_EDGE ( 'NONE', *, *, #56329, .F. ) ;
#38511 = CARTESIAN_POINT ( 'NONE',  ( 4.458734125000001214, -60.14583333196774362, 2.574251347313718519 ) ) ;
#38513 = DIRECTION ( 'NONE',  ( 0.7611951803011147710, 0.000000000000000000, 0.6485228581062916220 ) ) ;
#38514 = CARTESIAN_POINT ( 'NONE',  ( -3.152801135295367096, -168.3125000013656063, -3.152801135295367541 ) ) ;
#38515 = EDGE_CURVE ( 'NONE', #27636, #29896, #9159, .T. ) ;
#38516 = CARTESIAN_POINT ( 'NONE',  ( -4.458734124999998549, -103.4791666653010509, 2.574251347313722516 ) ) ;
#38517 = VERTEX_POINT ( 'NONE', #26612 ) ;
#38518 = CARTESIAN_POINT ( 'NONE',  ( -57.19623071787016499, -150.6250000013656063, 4.297418129356382899 ) ) ;
#38519 = CARTESIAN_POINT ( 'NONE',  ( -49.85088928181150436, -136.6875000027312126, -1.666127454062680702 ) ) ;
#38520 = CARTESIAN_POINT ( 'NONE',  ( 2.229367062500001939, -39.97916666530107221, 3.861377020970579999 ) ) ;
#38521 =( BOUNDED_CURVE ( )  B_SPLINE_CURVE ( 2, ( #50773, #6715, #60439, #1274, #30178, #25371, #30507, #16364, #26324 ),
 .UNSPECIFIED., .F., .F. ) 
 B_SPLINE_CURVE_WITH_KNOTS ( ( 3, 2, 2, 2, 3 ),
 ( 0.7267857142857142572, 0.7273809523809523503, 0.7285714285714285365, 0.7297619047619047228, 0.7303571428571428159 ),
 .UNSPECIFIED. ) 
 CURVE ( )  GEOMETRIC_REPRESENTATION_ITEM ( )  RATIONAL_B_SPLINE_CURVE ( ( 0.9330127018922194093, 0.9330127018922194093, 1.000000000000000000, 0.8660254037844387076, 1.000000000000000000, 0.8660254037844387076, 1.000000000000000000, 0.9330127018922194093, 0.9330127018922194093 ) ) 
 REPRESENTATION_ITEM ( '' )  );
#38522 = CARTESIAN_POINT ( 'NONE',  ( 0.000000000000000000, -120.0000000000000000, 5.000000000000000000 ) ) ;
#38523 = CARTESIAN_POINT ( 'NONE',  ( 2.229367062499998831, -10.64583333196773829, -3.861377020970580887 ) ) ;
#38524 = CARTESIAN_POINT ( 'NONE',  ( 4.458734125000000326, -100.1458333319677365, 2.574251347313718519 ) ) ;
#38525 = CARTESIAN_POINT ( 'NONE',  ( -4.458734125000001214, -145.1250000013655779, 1.846868145590734089 ) ) ;
#38526 = CARTESIAN_POINT ( 'NONE',  ( 4.458734124999998549, -26.97916666530107221, -2.574251347313721627 ) ) ;
#38527 = CARTESIAN_POINT ( 'NONE',  ( -52.53715891517739323, -153.4375000000000284, -4.819101127000233298 ) ) ;
#38528 = CARTESIAN_POINT ( 'NONE',  ( -50.55543936806279248, -133.0625000013656063, 0.3552334253322060320 ) ) ;
#38529 = CARTESIAN_POINT ( 'NONE',  ( 2.229367062499998831, -70.89583333196773651, -3.861377020970580887 ) ) ;
#38530 = DIRECTION ( 'NONE',  ( -0.000000000000000000, 1.000000000000000000, -0.000000000000000000 ) ) ;
#38531 = CARTESIAN_POINT ( 'NONE',  ( -6.972266317189433020E-16, -88.12499999726880162, -5.000000000000000000 ) ) ;
#38532 = CARTESIAN_POINT ( 'NONE',  ( 1.846868145590735200, -141.2500000013656063, -4.458734124999999437 ) ) ;
#38533 = CARTESIAN_POINT ( 'NONE',  ( -4.458734124999999437, 3.437500001365594748, 0.000000000000000000 ) ) ;
#38534 = EDGE_LOOP ( 'NONE', ( #36161, #15008, #8405, #21438 ) ) ;
#38535 = CARTESIAN_POINT ( 'NONE',  ( 1.975475456537005874E-15, 2.249999999999999556, 5.000000000000000000 ) ) ;
#38536 = CARTESIAN_POINT ( 'NONE',  ( 0.000000000000000000, -120.0000000000000000, 5.000000000000000000 ) ) ;
#38538 = CARTESIAN_POINT ( 'NONE',  ( 4.458734124999998549, -27.72916666530107221, -2.574251347313721627 ) ) ;
#38537 = CARTESIAN_POINT ( 'NONE',  ( 2.499999999999998668, -97.33333333333332860, -4.330127018922193649 ) ) ;
#38539 = CARTESIAN_POINT ( 'NONE',  ( 4.458734124999998549, -76.97916666530106511, -2.574251347313721627 ) ) ;
#38540 = CARTESIAN_POINT ( 'NONE',  ( -2.229367062499996610, 24.60416666803225993, 3.861377020970582219 ) ) ;
#38541 = FACE_OUTER_BOUND ( 'NONE', #39434, .T. ) ;
#38542 = CARTESIAN_POINT ( 'NONE',  ( -56.48576386720575471, -140.7500000013655779, -4.591703134518078322 ) ) ;
#38543 = EDGE_CURVE ( 'NONE', #7250, #17309, #48602, .T. ) ;
#38544 = EDGE_CURVE ( 'NONE', #31572, #14198, #4641, .T. ) ;
#38545 = CARTESIAN_POINT ( 'NONE',  ( -4.458734124999999437, 2.604166668032263043, -2.574251347313719407 ) ) ;
#38546 = CARTESIAN_POINT ( 'NONE',  ( 9.457646018065525792E-16, 25.68750000136559208, 5.148502694627439702 ) ) ;
#38547 = CARTESIAN_POINT ( 'NONE',  ( -4.458734124999999437, -44.64583333196773651, -2.574251347313719407 ) ) ;
#38548 = CARTESIAN_POINT ( 'NONE',  ( 1.975475456537005874E-15, -3.624999997268814056, 5.000000000000000000 ) ) ;
#38549 = CARTESIAN_POINT ( 'NONE',  ( -3.152548672688508926E-16, -0.5624999986344053626, -5.148502694627439702 ) ) ;
#38550 = CARTESIAN_POINT ( 'NONE',  ( 4.458734124999998549, -22.97916666530107221, -2.574251347313721627 ) ) ;
#38551 = CARTESIAN_POINT ( 'NONE',  ( -1.846868145590734756, -155.1250000013655779, -4.458734125000000326 ) ) ;
#38552 = CARTESIAN_POINT ( 'NONE',  ( 2.229367062500001939, -69.97916666530107932, 3.861377020970579999 ) ) ;
#38553 = CARTESIAN_POINT ( 'NONE',  ( -5.000000000000000000, -104.8749999972688158, 0.000000000000000000 ) ) ;
#38554 = ADVANCED_FACE ( 'NONE', ( #61352 ), #41704, .T. ) ;
#38555 = VECTOR ( 'NONE', #46392, 1000.000000000000000 ) ;
#38556 = CARTESIAN_POINT ( 'NONE',  ( -55.39835681537999790, -148.8750000000000284, 4.984105922594378235 ) ) ;
#38557 = CARTESIAN_POINT ( 'NONE',  ( -2.499999999999996447, -83.83333333333332860, 4.330127018922195425 ) ) ;
#38558 = ADVANCED_FACE ( 'NONE', ( #7638 ), #6370, .T. ) ;
#38559 = CARTESIAN_POINT ( 'NONE',  ( 2.229367062499998831, -106.8958333319677365, -3.861377020970580887 ) ) ;
#38560 = CARTESIAN_POINT ( 'NONE',  ( 9.457646018065525792E-16, -71.31249999863439371, 5.148502694627439702 ) ) ;
#38561 = CARTESIAN_POINT ( 'NONE',  ( 5.000000000000000000, -56.49999999999999289, -6.123233995736766282E-16 ) ) ;
#38562 = CARTESIAN_POINT ( 'NONE',  ( -5.000000000000000000, -22.08333333333333215, -2.886751345948128211 ) ) ;
#38563 = CARTESIAN_POINT ( 'NONE',  ( -3.535250795749689387E-16, 27.87500000273118417, -5.773502691896257311 ) ) ;
#38564 = ORIENTED_EDGE ( 'NONE', *, *, #32329, .F. ) ;
#38565 = CARTESIAN_POINT ( 'NONE',  ( 1.975475456537005874E-15, -7.750000000000000000, 5.000000000000000000 ) ) ;
#38566 = CARTESIAN_POINT ( 'NONE',  ( 5.000000000000000000, -27.29166666393548013, -2.886751345948130876 ) ) ;
#38567 = CARTESIAN_POINT ( 'NONE',  ( -2.499999999999996447, -11.83333333333333393, 4.330127018922195425 ) ) ;
#38568 = CARTESIAN_POINT ( 'NONE',  ( 2.229367062500001939, -18.97916666530106866, 3.861377020970579999 ) ) ;
#38569 = CARTESIAN_POINT ( 'NONE',  ( -3.152548672688508926E-16, -77.56249999863440792, -5.148502694627439702 ) ) ;
#38570 = CARTESIAN_POINT ( 'NONE',  ( 4.458734125000000326, -169.6250000013656063, -1.846868145590734978 ) ) ;
#38571 = CARTESIAN_POINT ( 'NONE',  ( 5.000000000000000888, -19.45833333060214798, 2.886751345948126879 ) ) ;
#38573 = ORIENTED_EDGE ( 'NONE', *, *, #46048, .T. ) ;
#38572 = CARTESIAN_POINT ( 'NONE',  ( -2.229367062499996610, -44.14583333196774362, 3.861377020970582219 ) ) ;
#38574 = CARTESIAN_POINT ( 'NONE',  ( 5.000000000000000888, -15.45833333060214443, 2.886751345948126879 ) ) ;
#38576 = ORIENTED_EDGE ( 'NONE', *, *, #56679, .T. ) ;
#38575 = CARTESIAN_POINT ( 'NONE',  ( -2.229367062500000163, 1.270833334698927342, -3.861377020970580443 ) ) ;
#38577 = CARTESIAN_POINT ( 'NONE',  ( -4.999999999999998224, -86.79166666393547303, 2.886751345948131764 ) ) ;
#38578 = CARTESIAN_POINT ( 'NONE',  ( -3.535250795749689387E-16, -63.25000000000000000, -5.773502691896257311 ) ) ;
#38579 = CARTESIAN_POINT ( 'NONE',  ( 4.458734125000000326, -154.6250000013655779, -1.846868145590734978 ) ) ;
#38580 = CARTESIAN_POINT ( 'NONE',  ( 4.458734124999999437, -39.06249999863440081, -5.460374474430324690E-16 ) ) ;
#38581 = CARTESIAN_POINT ( 'NONE',  ( -2.500000000000000444, -79.16666666666665719, -4.330127018922193649 ) ) ;
#38582 = CARTESIAN_POINT ( 'NONE',  ( -5.000000000000000888, -161.5625000000000568, -2.071067811865475949 ) ) ;
#38583 = CARTESIAN_POINT ( 'NONE',  ( -9.184850993605147944E-16, -168.2500000000000000, 5.000000000000000000 ) ) ;
#38584 = CARTESIAN_POINT ( 'NONE',  ( -59.59170313451811296, -127.7500000013655921, 1.485763867205729394 ) ) ;
#38585 = CARTESIAN_POINT ( 'NONE',  ( -4.458734124999999437, -4.562499998634401699, 0.000000000000000000 ) ) ;
#38586 = CARTESIAN_POINT ( 'NONE',  ( -4.458734124999998549, -38.47916666530107221, 2.574251347313722516 ) ) ;
#38587 = CARTESIAN_POINT ( 'NONE',  ( 1.339745962155612702, -26.29465819873852084, -5.000000000000000000 ) ) ;
#38588 = CARTESIAN_POINT ( 'NONE',  ( 4.458734124999999437, -148.5000000013656347, 1.846868145590737864 ) ) ;
#38589 = CARTESIAN_POINT ( 'NONE',  ( 2.229367062500001939, -87.22916666530107932, 3.861377020970579999 ) ) ;
#38590 = CARTESIAN_POINT ( 'NONE',  ( 2.499999999999998668, -108.3333333333333428, -4.330127018922193649 ) ) ;
#38591 = ORIENTED_EDGE ( 'NONE', *, *, #37404, .F. ) ;
#38592 = CARTESIAN_POINT ( 'NONE',  ( -4.999999999999998224, -46.91666666666666430, 2.886751345948131764 ) ) ;
#38593 = CARTESIAN_POINT ( 'NONE',  ( -58.24261429053147765, -149.3750000027312126, -3.805975901505573855 ) ) ;
#38594 = CARTESIAN_POINT ( 'NONE',  ( 2.499999999999998668, -2.208333330602146205, -4.330127018922193649 ) ) ;
#38595 = CARTESIAN_POINT ( 'NONE',  ( 9.457646018065525792E-16, -75.31249999863440792, 5.148502694627439702 ) ) ;
#38596 = ORIENTED_EDGE ( 'NONE', *, *, #18020, .F. ) ;
#38597 = VECTOR ( 'NONE', #26890, 1000.000000000000000 ) ;
#38598 = CARTESIAN_POINT ( 'NONE',  ( -1.339745962155610925, -13.79465819873852261, 5.000000000000000000 ) ) ;
#38599 = CARTESIAN_POINT ( 'NONE',  ( -3.152548672688508926E-16, -13.81249999863440436, -5.148502694627439702 ) ) ;
#38600 = PRODUCT_DEFINITION_CONTEXT ( 'detailed design', #51998, 'design' ) ;
#38601 = CYLINDRICAL_SURFACE ( 'NONE', #55902, 5.000000000000000000 ) ;
#38602 = CARTESIAN_POINT ( 'NONE',  ( -4.458734124999998549, -0.2291666653010705768, 2.574251347313722516 ) ) ;
#38603 = CARTESIAN_POINT ( 'NONE',  ( 5.000000000000000888, -30.45833333060214443, 2.886751345948126879 ) ) ;
#38604 = CARTESIAN_POINT ( 'NONE',  ( 4.458734124999999437, -154.3750000013655779, -1.846868145590734978 ) ) ;
#38605 = CARTESIAN_POINT ( 'NONE',  ( 4.458734124999998549, 21.02083333469892779, -2.574251347313721627 ) ) ;
#38606 = ORIENTED_EDGE ( 'NONE', *, *, #41769, .F. ) ;
#38607 = CARTESIAN_POINT ( 'NONE',  ( -4.458734124999999437, -93.39583333196772230, -2.574251347313719407 ) ) ;
#38608 = CARTESIAN_POINT ( 'NONE',  ( -62.00000000000001421, -135.0000000000000284, 4.041451884327384114 ) ) ;
#38609 = LINE ( 'NONE', #19947, #16475 ) ;
#38610 = CARTESIAN_POINT ( 'NONE',  ( 4.458734124999999437, -12.81249999863440259, -5.460374474430324690E-16 ) ) ;
#38611 = CYLINDRICAL_SURFACE ( 'NONE', #24280, 5.000000000000000000 ) ;
#38612 = CARTESIAN_POINT ( 'NONE',  ( -52.80376928212989185, -153.8750000013655779, -4.297418129356379346 ) ) ;
#38613 = EDGE_CURVE ( 'NONE', #26042, #46511, #61031, .T. ) ;
#38614 = CARTESIAN_POINT ( 'NONE',  ( 5.000000000000000000, -39.29166666393548724, -2.886751345948129988 ) ) ;
#38615 = FACE_OUTER_BOUND ( 'NONE', #11468, .T. ) ;
#38616 = CARTESIAN_POINT ( 'NONE',  ( 4.458734125000000326, 19.10416666803225638, 2.574251347313718519 ) ) ;
#38617 = CARTESIAN_POINT ( 'NONE',  ( -1.339745962155613812, -72.20534180126148271, -5.000000000000000000 ) ) ;
#38618 = VERTEX_POINT ( 'NONE', #30691 ) ;
#38619 = CARTESIAN_POINT ( 'NONE',  ( 2.229367062499998831, 19.35416666803225993, -3.861377020970580887 ) ) ;
#38620 = CARTESIAN_POINT ( 'NONE',  ( 2.229367062499998831, -63.64583333196772941, -3.861377020970580887 ) ) ;
#38621 = CARTESIAN_POINT ( 'NONE',  ( -3.152548672688508926E-16, -8.812499998634406140, -5.148502694627439702 ) ) ;
#38622 = CARTESIAN_POINT ( 'NONE',  ( 1.975475456537005874E-15, -15.62499999726881406, 5.000000000000000000 ) ) ;
#38623 = CARTESIAN_POINT ( 'NONE',  ( 1.060575238724906964E-15, 9.250000000000001776, 5.773502691896257311 ) ) ;
#38624 = CARTESIAN_POINT ( 'NONE',  ( 2.730187237215162345E-16, -166.1875000013655779, -4.458734124999999437 ) ) ;
#38625 = CARTESIAN_POINT ( 'NONE',  ( -5.000000000000000000, -98.87499999726881583, 0.000000000000000000 ) ) ;
#38626 = CARTESIAN_POINT ( 'NONE',  ( 2.229367062500001939, -55.97916666530107221, 3.861377020970579999 ) ) ;
#38627 = CARTESIAN_POINT ( 'NONE',  ( 5.000000000000000000, -83.29166666393547303, -2.886751345948129988 ) ) ;
#38628 = CARTESIAN_POINT ( 'NONE',  ( -59.44456063193725015, -136.8125000013656063, -0.3552334253322034230 ) ) ;
#38629 = CARTESIAN_POINT ( 'NONE',  ( -5.000000000000000000, -17.00000000000000000, 0.000000000000000000 ) ) ;
#38630 = CARTESIAN_POINT ( 'NONE',  ( -5.000000000000000000, -92.00000000000000000, 0.000000000000000000 ) ) ;
#38631 = CARTESIAN_POINT ( 'NONE',  ( 4.458734124999998549, -88.97916666530106511, -2.574251347313721627 ) ) ;
#38632 = CARTESIAN_POINT ( 'NONE',  ( -1.846868145590734756, -155.3750000013656063, -4.458734124999999437 ) ) ;
#38633 = CARTESIAN_POINT ( 'NONE',  ( -2.499999999999996447, -39.83333333333332860, 4.330127018922195425 ) ) ;
#38634 = CARTESIAN_POINT ( 'NONE',  ( -55.39835681537999790, -139.8750000000000284, 4.984105922594378235 ) ) ;
#38635 = EDGE_CURVE ( 'NONE', #1769, #7560, #63088, .T. ) ;
#38636 = CARTESIAN_POINT ( 'NONE',  ( 5.000000000000000888, -22.58333333333332860, 2.886751345948126879 ) ) ;
#38637 = ORIENTED_EDGE ( 'NONE', *, *, #27086, .F. ) ;
#38638 = CARTESIAN_POINT ( 'NONE',  ( -2.229367062500000163, -103.4791666653010651, -3.861377020970580443 ) ) ;
#38639 = CARTESIAN_POINT ( 'NONE',  ( -2.229367062500000163, 6.270833334698928674, -3.861377020970580443 ) ) ;
#38640 = CARTESIAN_POINT ( 'NONE',  ( -4.999999999999999112, 12.20833333606451632, 2.886751345948131764 ) ) ;
#38641 = DIRECTION ( 'NONE',  ( -0.000000000000000000, 1.000000000000000000, -0.000000000000000000 ) ) ;
#38642 = ADVANCED_FACE ( 'NONE', ( #55467 ), #25543, .T. ) ;
#38643 = CARTESIAN_POINT ( 'NONE',  ( 1.060575238724906964E-15, 4.250000000000000000, 5.773502691896257311 ) ) ;
#38644 = AXIS2_PLACEMENT_3D ( 'NONE', #59532, #16419, #36037 ) ;
#38645 = CARTESIAN_POINT ( 'NONE',  ( 2.229367062499998831, -61.64583333196774362, -3.861377020970580887 ) ) ;
#38646 =( BOUNDED_CURVE ( )  B_SPLINE_CURVE ( 2, ( #44767, #10678, #3418, #54436, #24526, #728, #94, #54754, #29973 ),
 .UNSPECIFIED., .F., .F. ) 
 B_SPLINE_CURVE_WITH_KNOTS ( ( 3, 2, 2, 2, 3 ),
 ( 0.4750000000000004219, 0.4791666666666671293, 0.4833333333333337811, 0.4875000000000004330, 0.4916666666666670849 ),
 .UNSPECIFIED. ) 
 CURVE ( )  GEOMETRIC_REPRESENTATION_ITEM ( )  RATIONAL_B_SPLINE_CURVE ( ( 0.9999999999999918954, 0.9238795325112948431, 1.000000000000000000, 0.9238795325112867385, 1.000000000000000000, 0.9238795325112867385, 1.000000000000000000, 0.9238795325112786339, 1.000000000000008216 ) ) 
 REPRESENTATION_ITEM ( '' )  );
#38647 = CARTESIAN_POINT ( 'NONE',  ( -2.500000000000000444, 2.833333333333333481, -4.330127018922193649 ) ) ;
#38648 = EDGE_CURVE ( 'NONE', #35135, #19195, #49916, .T. ) ;
#38649 = CARTESIAN_POINT ( 'NONE',  ( -2.500000000000000444, -2.041666663935480575, -4.330127018922193649 ) ) ;
#38650 = CARTESIAN_POINT ( 'NONE',  ( -4.458734124999999437, -26.31249999863440792, 0.000000000000000000 ) ) ;
#38651 = CARTESIAN_POINT ( 'NONE',  ( -51.75738570946856498, -143.8750000027312126, 3.805975901505576964 ) ) ;
#38652 = CARTESIAN_POINT ( 'NONE',  ( -6.972266317189433020E-16, -48.12499999726880873, -5.000000000000000000 ) ) ;
#38653 = DIRECTION ( 'NONE',  ( -0.000000000000000000, 1.000000000000000000, -0.000000000000000000 ) ) ;
#38654 = CARTESIAN_POINT ( 'NONE',  ( -4.999999999999999112, -43.91666666666665719, 2.886751345948131764 ) ) ;
#38656 = CARTESIAN_POINT ( 'NONE',  ( -3.152548672688508926E-16, -27.81249999863440436, -5.148502694627439702 ) ) ;
#38655 = DIRECTION ( 'NONE',  ( -1.000000000000000000, 0.000000000000000000, -0.000000000000000000 ) ) ;
#38657 = CARTESIAN_POINT ( 'NONE',  ( -2.498395430326213474E-14, 15.37500000273118239, 5.000000000000000000 ) ) ;
#38658 = CARTESIAN_POINT ( 'NONE',  ( -4.458734124999999437, -68.39583333196773651, -2.574251347313719407 ) ) ;
#38659 = CARTESIAN_POINT ( 'NONE',  ( 4.458734125000000326, -144.6250000013655779, -1.846868145590734978 ) ) ;
#38660 = CARTESIAN_POINT ( 'NONE',  ( 2.229367062499998831, -78.64583333196773651, -3.861377020970580887 ) ) ;
#38661 = CARTESIAN_POINT ( 'NONE',  ( -57.19623071787017210, -139.6250000013655779, 4.297418129356382899 ) ) ;
#38662 = CARTESIAN_POINT ( 'NONE',  ( -4.458734124999999437, -23.64583333196773651, -2.574251347313719407 ) ) ;
#38663 = CARTESIAN_POINT ( 'NONE',  ( -5.000000000000000000, -66.87499999726881583, 0.000000000000000000 ) ) ;
#38664 = ORIENTED_EDGE ( 'NONE', *, *, #7236, .T. ) ;
#38665 = CARTESIAN_POINT ( 'NONE',  ( 5.000000000000000000, -93.37499999726881583, -6.123233995736766282E-16 ) ) ;
#38666 = ORIENTED_EDGE ( 'NONE', *, *, #56989, .F. ) ;
#38667 = CARTESIAN_POINT ( 'NONE',  ( 9.457646018065525792E-16, -71.31249999863439371, 5.148502694627439702 ) ) ;
#38668 = CARTESIAN_POINT ( 'NONE',  ( 5.000000000000000888, -165.9375000000000000, -2.071067811865475505 ) ) ;
#38669 =( NAMED_UNIT ( * ) SI_UNIT ( $, .STERADIAN. ) SOLID_ANGLE_UNIT ( ) );
#38670 = ORIENTED_EDGE ( 'NONE', *, *, #34651, .T. ) ;
#38671 = CARTESIAN_POINT ( 'NONE',  ( 5.000000000000000000, 12.50000000000000000, -6.123233995736766282E-16 ) ) ;
#38672 = CARTESIAN_POINT ( 'NONE',  ( -58.80597590150559739, -143.1250000027312126, 3.242614290531460330 ) ) ;
#38673 = CARTESIAN_POINT ( 'NONE',  ( 2.229367062500001939, -61.22916666530106511, 3.861377020970579999 ) ) ;
#38674 = CARTESIAN_POINT ( 'NONE',  ( -2.229367062500000163, 2.270833334698928230, -3.861377020970580443 ) ) ;
#38675 = ORIENTED_EDGE ( 'NONE', *, *, #23973, .F. ) ;
#38676 = CARTESIAN_POINT ( 'NONE',  ( 0.000000000000000000, -120.0000000000000000, 0.000000000000000000 ) ) ;
#38677 = CARTESIAN_POINT ( 'NONE',  ( 2.229367062499998831, 13.35416666803226171, -3.861377020970580887 ) ) ;
#38678 = CARTESIAN_POINT ( 'NONE',  ( -52.80376928212989185, -146.8750000013656063, -4.297418129356379346 ) ) ;
#38679 = CARTESIAN_POINT ( 'NONE',  ( -2.500000000000000444, -2.166666666666663854, -4.330127018922193649 ) ) ;
#38680 = CARTESIAN_POINT ( 'NONE',  ( -1.846868145590734756, -163.1250000013656347, -4.458734124999999437 ) ) ;
#38681 = ORIENTED_EDGE ( 'NONE', *, *, #10688, .T. ) ;
#38682 = CARTESIAN_POINT ( 'NONE',  ( 2.229367062499998831, -78.64583333196773651, -3.861377020970580887 ) ) ;
#38683 = CARTESIAN_POINT ( 'NONE',  ( -2.071067811865308972, -153.3125000000000284, 5.000000000000169642 ) ) ;
#38684 = CARTESIAN_POINT ( 'NONE',  ( 9.457646018065525792E-16, -0.06249999863440491854, 5.148502694627439702 ) ) ;
#38685 = AXIS2_PLACEMENT_3D ( 'NONE', #55129, #44505, #30350 ) ;
#38686 = CARTESIAN_POINT ( 'NONE',  ( 2.500000000000002220, -19.54166666393548013, 4.330127018922192761 ) ) ;
#38687 = CARTESIAN_POINT ( 'NONE',  ( -2.229367062499996610, -63.39583333196774362, 3.861377020970582219 ) ) ;
#38688 = AXIS2_PLACEMENT_3D ( 'NONE', #59856, #30237, #5808 ) ;
#38689 = CARTESIAN_POINT ( 'NONE',  ( -3.535250795749689387E-16, -19.12499999726881228, -5.773502691896257311 ) ) ;
#38690 = DIRECTION ( 'NONE',  ( -0.000000000000000000, 1.000000000000000000, -0.000000000000000000 ) ) ;
#38691 = CYLINDRICAL_SURFACE ( 'NONE', #46005, 5.000000000000000000 ) ;
#38692 = CARTESIAN_POINT ( 'NONE',  ( -4.999999999999998224, -58.91666666666665009, 2.886751345948131764 ) ) ;
#38693 =( BOUNDED_CURVE ( )  B_SPLINE_CURVE ( 2, ( #44366, #39858, #15111, #34727, #44686, #60466, #40193, #54355, #25399 ),
 .UNSPECIFIED., .F., .F. ) 
 B_SPLINE_CURVE_WITH_KNOTS ( ( 3, 2, 2, 2, 3 ),
 ( 0.1583333333333334925, 0.1625000000000001721, 0.1666666666666668239, 0.1708333333333335036, 0.1750000000000001554 ),
 .UNSPECIFIED. ) 
 CURVE ( )  GEOMETRIC_REPRESENTATION_ITEM ( )  RATIONAL_B_SPLINE_CURVE ( ( 0.9999999999999970024, 0.9238795325112897361, 1.000000000000000000, 0.9238795325112867385, 1.000000000000000000, 0.9238795325112867385, 1.000000000000000000, 0.9238795325112837409, 1.000000000000003109 ) ) 
 REPRESENTATION_ITEM ( '' )  );
#38694 = LINE ( 'NONE', #38389, #16210 ) ;
#38695 = CARTESIAN_POINT ( 'NONE',  ( 2.229367062499998831, -41.64583333196773651, -3.861377020970580887 ) ) ;
#38696 = CARTESIAN_POINT ( 'NONE',  ( 4.458734124999998549, -25.97916666530107221, -2.574251347313721627 ) ) ;
#38697 = CARTESIAN_POINT ( 'NONE',  ( 2.229367062499998831, 6.104166668032262599, -3.861377020970580887 ) ) ;
#38698 = FACE_OUTER_BOUND ( 'NONE', #27484, .T. ) ;
#38699 = CARTESIAN_POINT ( 'NONE',  ( 5.000000000000000888, 23.41666666666666785, 2.886751345948126879 ) ) ;
#38700 = CARTESIAN_POINT ( 'NONE',  ( -3.535533905932737309, -148.7500000027311842, -3.535533905932738197 ) ) ;
#38701 = CARTESIAN_POINT ( 'NONE',  ( -4.458734124999999437, -107.6458333319677365, -2.574251347313719407 ) ) ;
#38702 = CARTESIAN_POINT ( 'NONE',  ( 4.458734125000001214, -36.89583333196773651, 2.574251347313718519 ) ) ;
#38703 = CARTESIAN_POINT ( 'NONE',  ( -4.999999999999999112, -65.79166666393547303, 2.886751345948131764 ) ) ;
#38704 = CARTESIAN_POINT ( 'NONE',  ( -53.51423613279429503, -147.5000000013656063, 4.591703134518082763 ) ) ;
#38705 = CARTESIAN_POINT ( 'NONE',  ( -5.000000000000000000, -141.5000000000000284, -6.123233995736766282E-16 ) ) ;
#38706 = CARTESIAN_POINT ( 'NONE',  ( 9.457646018065525792E-16, -75.31249999863440792, 5.148502694627439702 ) ) ;
#38707 = CARTESIAN_POINT ( 'NONE',  ( 9.457646018065525792E-16, -31.06249999863440436, 5.148502694627439702 ) ) ;
#38708 = CARTESIAN_POINT ( 'NONE',  ( -57.46284108482265651, -136.0625000027312126, 4.819101127000238627 ) ) ;
#38709 = DIRECTION ( 'NONE',  ( 0.000000000000000000, 0.000000000000000000, 1.000000000000000000 ) ) ;
#38710 = CARTESIAN_POINT ( 'NONE',  ( -5.000000000000000000, -22.08333333333333215, -2.886751345948128211 ) ) ;
#38711 = CARTESIAN_POINT ( 'NONE',  ( 4.458734124999999437, -143.5000000013656063, 1.846868145590737864 ) ) ;
#38712 = ORIENTED_EDGE ( 'NONE', *, *, #28051, .F. ) ;
#38713 = CARTESIAN_POINT ( 'NONE',  ( -4.458734124999999437, 26.43750000136559564, 0.000000000000000000 ) ) ;
#38714 = CARTESIAN_POINT ( 'NONE',  ( -57.46284108482265651, -140.9375000000000000, 4.819101127000238627 ) ) ;
#38715 = CARTESIAN_POINT ( 'NONE',  ( -4.458734124999997661, -57.47916666530108643, 2.574251347313722516 ) ) ;
#38716 = CARTESIAN_POINT ( 'NONE',  ( 2.499999999999998668, 26.79166666939785202, -4.330127018922193649 ) ) ;
#38717 = CARTESIAN_POINT ( 'NONE',  ( 1.975475456537005874E-15, -48.62499999726880162, 5.000000000000000000 ) ) ;
#38718 = CARTESIAN_POINT ( 'NONE',  ( 2.499999999999998668, 16.66666666666666785, -4.330127018922193649 ) ) ;
#38719 = CARTESIAN_POINT ( 'NONE',  ( 4.769696007084727185, -120.0000000000000000, 1.500000000000000000 ) ) ;
#38720 = CARTESIAN_POINT ( 'NONE',  ( -4.458734124999998549, -6.229166665301072214, 2.574251347313722516 ) ) ;
#38721 = CARTESIAN_POINT ( 'NONE',  ( -2.071067811865459518, -168.3125000000000284, 5.000000000000019540 ) ) ;
#38722 = CARTESIAN_POINT ( 'NONE',  ( -5.000000000000000000, -77.00000000000000000, 0.000000000000000000 ) ) ;
#38723 = CARTESIAN_POINT ( 'NONE',  ( 6.901579824520443829, -4.675625068323827627, -0.7022220667781372549 ) ) ;
#38724 =( BOUNDED_CURVE ( )  B_SPLINE_CURVE ( 2, ( #23323, #18491, #7272, #46499, #4323 ),
 .UNSPECIFIED., .F., .F. ) 
 B_SPLINE_CURVE_WITH_KNOTS ( ( 3, 2, 3 ),
 ( 0.9982142857142857206, 0.9988095238095238138, 1.000000000000000000 ),
 .UNSPECIFIED. ) 
 CURVE ( )  GEOMETRIC_REPRESENTATION_ITEM ( )  RATIONAL_B_SPLINE_CURVE ( ( 0.9330127018922194093, 0.9330127018922194093, 1.000000000000000000, 0.8660254037844387076, 1.000000000000000000 ) ) 
 REPRESENTATION_ITEM ( '' )  );
#38725 = CARTESIAN_POINT ( 'NONE',  ( 1.339745962155612702, -12.29465819873851906, -5.000000000000000000 ) ) ;
#38726 = CARTESIAN_POINT ( 'NONE',  ( 2.229367062500001939, -19.97916666530107221, 3.861377020970579999 ) ) ;
#38727 = VECTOR ( 'NONE', #61207, 1000.000000000000000 ) ;
#38728 = CARTESIAN_POINT ( 'NONE',  ( 2.500000000000002220, -97.54166666393545881, 4.330127018922192761 ) ) ;
#38729 = CARTESIAN_POINT ( 'NONE',  ( 2.229367062500001939, -55.97916666530107221, 3.861377020970579999 ) ) ;
#38730 = CARTESIAN_POINT ( 'NONE',  ( 1.846868145590735200, -160.5000000013656347, -4.458734125000000326 ) ) ;
#38731 = CARTESIAN_POINT ( 'NONE',  ( -3.535250795749689387E-16, -50.12499999726881583, -5.773502691896257311 ) ) ;
#38732 = ORIENTED_EDGE ( 'NONE', *, *, #26024, .F. ) ;
#38733 = AXIS2_PLACEMENT_3D ( 'NONE', #47095, #22973, #42259 ) ;
#38734 = CARTESIAN_POINT ( 'NONE',  ( -4.458734124999999437, 7.437500001365594748, 0.000000000000000000 ) ) ;
#38735 = ORIENTED_EDGE ( 'NONE', *, *, #3572, .F. ) ;
#38737 = CARTESIAN_POINT ( 'NONE',  ( 1.975475456537005874E-15, -9.624999997268814056, 5.000000000000000000 ) ) ;
#38736 = CARTESIAN_POINT ( 'NONE',  ( 5.000000000000000888, -87.58333333333332860, 2.886751345948126879 ) ) ;
#38738 = CARTESIAN_POINT ( 'NONE',  ( 4.458734124999999437, -162.4375000013655779, 0.000000000000000000 ) ) ;
#38739 = EDGE_LOOP ( 'NONE', ( #58559, #5752, #47153, #19322 ) ) ;
#38740 =( BOUNDED_CURVE ( )  B_SPLINE_CURVE ( 2, ( #684, #53430, #48598, #30244, #9363, #39259, #28976, #54058, #29930 ),
 .UNSPECIFIED., .F., .F. ) 
 B_SPLINE_CURVE_WITH_KNOTS ( ( 3, 2, 2, 2, 3 ),
 ( 0.9854166666666667185, 0.9861111111111111605, 0.9875000000000000444, 0.9888888888888889284, 0.9895833333333333703 ),
 .UNSPECIFIED. ) 
 CURVE ( )  GEOMETRIC_REPRESENTATION_ITEM ( )  RATIONAL_B_SPLINE_CURVE ( ( 0.9330127018922194093, 0.9330127018922194093, 1.000000000000000000, 0.8660254037844387076, 1.000000000000000000, 0.8660254037844387076, 1.000000000000000000, 0.9330127018922194093, 0.9330127018922194093 ) ) 
 REPRESENTATION_ITEM ( '' )  );
#38741 = CARTESIAN_POINT ( 'NONE',  ( -6.972266317189433020E-16, -51.12499999726880873, -5.000000000000000000 ) ) ;
#38742 = CARTESIAN_POINT ( 'NONE',  ( -49.85088928181150436, -133.5625000000000284, -1.666127454062680702 ) ) ;
#38743 = EDGE_CURVE ( 'NONE', #31992, #4978, #54170, .T. ) ;
#38744 = CARTESIAN_POINT ( 'NONE',  ( -5.000000000000000000, -58.95833333060213732, -2.886751345948128211 ) ) ;
#38745 = CARTESIAN_POINT ( 'NONE',  ( 2.229367062500001939, -43.22916666530107932, 3.861377020970579999 ) ) ;
#38746 = VERTEX_POINT ( 'NONE', #24911 ) ;
#38747 = DIRECTION ( 'NONE',  ( -0.000000000000000000, 1.000000000000000000, -0.000000000000000000 ) ) ;
#38748 = CARTESIAN_POINT ( 'NONE',  ( -4.458734124999998549, 20.77083333469892779, 2.574251347313722516 ) ) ;
#38749 = CYLINDRICAL_SURFACE ( 'NONE', #14267, 5.000000000000000000 ) ;
#38750 = VERTEX_POINT ( 'NONE', #34881 ) ;
#38751 = CARTESIAN_POINT ( 'NONE',  ( -2.229367062499996610, -85.39583333196773651, 3.861377020970582219 ) ) ;
#38752 = CARTESIAN_POINT ( 'NONE',  ( -54.60164318462004474, -126.5000000027312126, -4.984105922594373794 ) ) ;
#38753 = CARTESIAN_POINT ( 'NONE',  ( 2.499999999999998668, -35.20833333060213732, -4.330127018922193649 ) ) ;
#38754 = CARTESIAN_POINT ( 'NONE',  ( 2.500000000000002220, -39.66666666666667140, 4.330127018922192761 ) ) ;
#38755 = CARTESIAN_POINT ( 'NONE',  ( -2.499999999999996447, 24.16666666666666785, 4.330127018922195425 ) ) ;
#38756 = CARTESIAN_POINT ( 'NONE',  ( -3.152548672688508926E-16, -60.56249999863440792, -5.148502694627439702 ) ) ;
#38757 = CARTESIAN_POINT ( 'NONE',  ( -5.000000000000000000, -61.87499999726880873, 0.000000000000000000 ) ) ;
#38758 = CARTESIAN_POINT ( 'NONE',  ( -3.152548672688508926E-16, 21.43750000136559564, -5.148502694627439702 ) ) ;
#38759 = CARTESIAN_POINT ( 'NONE',  ( 5.000000000000000000, -102.3749999972688158, -6.123233995736766282E-16 ) ) ;
#38760 = CARTESIAN_POINT ( 'NONE',  ( -1.339745962155610925, -43.79465819873851729, 5.000000000000000000 ) ) ;
#38761 = CARTESIAN_POINT ( 'NONE',  ( 2.229367062500001939, -48.22916666530106511, 3.861377020970579999 ) ) ;
#38762 = CARTESIAN_POINT ( 'NONE',  ( 5.000000000000000888, -1.458333330602149092, 2.886751345948126879 ) ) ;
#38763 = CARTESIAN_POINT ( 'NONE',  ( 6.123233995736766282E-16, -170.0000000000000000, -5.000000000000000000 ) ) ;
#38764 = DIRECTION ( 'NONE',  ( 0.000000000000000000, 0.000000000000000000, 1.000000000000000000 ) ) ;
#38765 = CARTESIAN_POINT ( 'NONE',  ( -3.152548672688508926E-16, -85.81249999863440792, -5.148502694627439702 ) ) ;
#38766 = CARTESIAN_POINT ( 'NONE',  ( -3.152548672688508926E-16, -105.5624999986344221, -5.148502694627439702 ) ) ;
#38767 = CARTESIAN_POINT ( 'NONE',  ( 2.229367062500001939, -13.22916666530107221, 3.861377020970579999 ) ) ;
#38768 = VERTEX_POINT ( 'NONE', #45161 ) ;
#38769 = AXIS2_PLACEMENT_3D ( 'NONE', #48576, #22584, #9032 ) ;
#38770 = CARTESIAN_POINT ( 'NONE',  ( -5.000000000000000000, -81.00000000000000000, 0.000000000000000000 ) ) ;
#38771 = CARTESIAN_POINT ( 'NONE',  ( -2.229367062500000163, -98.47916666530105090, -3.861377020970580443 ) ) ;
#38772 = CARTESIAN_POINT ( 'NONE',  ( -5.000000000000000888, -161.5625000027311842, 2.071067811865474617 ) ) ;
#38773 = CARTESIAN_POINT ( 'NONE',  ( -4.458734124999999437, -92.56249999863440792, 0.000000000000000000 ) ) ;
#38774 = VECTOR ( 'NONE', #10003, 1000.000000000000000 ) ;
#38775 = CARTESIAN_POINT ( 'NONE',  ( -5.000000000000000000, -49.95833333060213022, -2.886751345948128211 ) ) ;
#38776 = CARTESIAN_POINT ( 'NONE',  ( -2.499999999999996447, -36.70833333060213732, 4.330127018922195425 ) ) ;
#38777 = CARTESIAN_POINT ( 'NONE',  ( -50.70258187064364108, -129.1250000013655779, 2.196230717870141014 ) ) ;
#38778 = CARTESIAN_POINT ( 'NONE',  ( -50.70258187064364108, -145.1250000013656063, 2.196230717870141014 ) ) ;
#38779 = CARTESIAN_POINT ( 'NONE',  ( -2.229367062499996610, -17.14583333196773651, 3.861377020970582219 ) ) ;
#38780 = CARTESIAN_POINT ( 'NONE',  ( -2.229367062500000163, 12.27083333469892601, -3.861377020970580443 ) ) ;
#38781 = CARTESIAN_POINT ( 'NONE',  ( 9.457646018065525792E-16, -57.31249999863440081, 5.148502694627439702 ) ) ;
#38782 = CARTESIAN_POINT ( 'NONE',  ( 0.000000000000000000, -120.0000000000000000, 0.000000000000000000 ) ) ;
#38783 = CARTESIAN_POINT ( 'NONE',  ( 9.457646018065525792E-16, -16.06249999863440436, 5.148502694627439702 ) ) ;
#38784 = CARTESIAN_POINT ( 'NONE',  ( 6.123233995736766282E-16, -170.0000000000000000, -5.000000000000000000 ) ) ;
#38785 = CARTESIAN_POINT ( 'NONE',  ( -3.535533905932737309, -153.6250000000000000, -3.535533905932738197 ) ) ;
#38786 = ORIENTED_EDGE ( 'NONE', *, *, #39359, .F. ) ;
#38787 = CARTESIAN_POINT ( 'NONE',  ( -3.152548672688508926E-16, -42.81249999863440081, -5.148502694627439702 ) ) ;
#38788 = CARTESIAN_POINT ( 'NONE',  ( 1.975475456537005874E-15, -83.62499999726878741, 5.000000000000000000 ) ) ;
#38789 = CYLINDRICAL_SURFACE ( 'NONE', #5183, 5.000000000000000000 ) ;
#38790 = CARTESIAN_POINT ( 'NONE',  ( -1.339745962155610925, -66.66965819600733312, 5.000000000000000000 ) ) ;
#38791 = CARTESIAN_POINT ( 'NONE',  ( -4.458734124999999437, -85.31249999863439371, 0.000000000000000000 ) ) ;
#38792 = CARTESIAN_POINT ( 'NONE',  ( 4.458734124999999437, 18.93750000136559564, -5.460374474430324690E-16 ) ) ;
#38793 = CARTESIAN_POINT ( 'NONE',  ( 4.458734124999999437, 11.18750000136559386, -5.460374474430324690E-16 ) ) ;
#38794 = CARTESIAN_POINT ( 'NONE',  ( -5.000000000000000000, 30.00000000000000000, 0.000000000000000000 ) ) ;
#38795 = CARTESIAN_POINT ( 'NONE',  ( -5.000000000000000000, -165.6250000027312126, -6.123233995736766282E-16 ) ) ;
#38796 = CARTESIAN_POINT ( 'NONE',  ( 2.229367062499998831, -88.89583333196773651, -3.861377020970580887 ) ) ;
#38797 = CARTESIAN_POINT ( 'NONE',  ( -3.535250795749689387E-16, -71.25000000000000000, -5.773502691896257311 ) ) ;
#38798 = CARTESIAN_POINT ( 'NONE',  ( -5.000000000000000000, 15.04166666939785202, -2.886751345948128211 ) ) ;
#38799 = ORIENTED_EDGE ( 'NONE', *, *, #61301, .T. ) ;
#38800 = CARTESIAN_POINT ( 'NONE',  ( 5.000000000000000888, -79.58333333333332860, 2.886751345948126879 ) ) ;
#38801 = ORIENTED_EDGE ( 'NONE', *, *, #19663, .T. ) ;
#38802 = CARTESIAN_POINT ( 'NONE',  ( -56.66612745406286678, -144.4375000027312126, -5.149110718188528502 ) ) ;
#38804 = CARTESIAN_POINT ( 'NONE',  ( 5.000000000000000888, -33.58333333333332860, 2.886751345948126879 ) ) ;
#38803 = FACE_OUTER_BOUND ( 'NONE', #20230, .T. ) ;
#38805 = CARTESIAN_POINT ( 'NONE',  ( 4.458734125000001214, -36.89583333196773651, 2.574251347313718519 ) ) ;
#38806 = CARTESIAN_POINT ( 'NONE',  ( -4.999999999999999112, -31.79166666393548724, 2.886751345948131764 ) ) ;
#38808 = ORIENTED_EDGE ( 'NONE', *, *, #44705, .F. ) ;
#38807 = CARTESIAN_POINT ( 'NONE',  ( -2.229367062500000163, -65.47916666530106511, -3.861377020970580443 ) ) ;
#38809 = CARTESIAN_POINT ( 'NONE',  ( -59.44456063193725015, -151.8125000013656063, -0.3552334253322034230 ) ) ;
#38810 = CARTESIAN_POINT ( 'NONE',  ( 4.458734124999999437, -11.81249999863440081, -5.460374474430324690E-16 ) ) ;
#38812 = EDGE_LOOP ( 'NONE', ( #34305, #62552, #20199, #56098 ) ) ;
#38811 = CARTESIAN_POINT ( 'NONE',  ( 4.458734125000001214, -15.14583333196773651, 2.574251347313718519 ) ) ;
#38813 = CARTESIAN_POINT ( 'NONE',  ( 5.000000000000000000, -76.41666666666665719, -2.886751345948129988 ) ) ;
#38814 = DIRECTION ( 'NONE',  ( 0.000000000000000000, 0.000000000000000000, 1.000000000000000000 ) ) ;
#38815 = CARTESIAN_POINT ( 'NONE',  ( -2.229367062499996610, -57.39583333196773651, 3.861377020970582219 ) ) ;
#38817 = CARTESIAN_POINT ( 'NONE',  ( -5.000000000000000000, -79.87499999726881583, 0.000000000000000000 ) ) ;
#38816 = APPLICATION_CONTEXT ( 'automotive_design' ) ;
#38819 = ORIENTED_EDGE ( 'NONE', *, *, #36604, .F. ) ;
#38818 = LINE ( 'NONE', #39456, #35454 ) ;
#38820 = CARTESIAN_POINT ( 'NONE',  ( -51.19402409849444524, -145.5000000000000284, -3.242614290531456334 ) ) ;
#38821 = ADVANCED_FACE ( 'NONE', ( #11383 ), #26091, .F. ) ;
#38822 = AXIS2_PLACEMENT_3D ( 'NONE', #49094, #54571, #34952 ) ;
#38823 = CARTESIAN_POINT ( 'NONE',  ( 9.457646018065525792E-16, -24.31249999863440792, 5.148502694627439702 ) ) ;
#38824 = VERTEX_POINT ( 'NONE', #39369 ) ;
#38825 =( BOUNDED_CURVE ( )  B_SPLINE_CURVE ( 2, ( #47617, #3265, #47926, #57607, #43413, #3570, #18665, #62433, #32833 ),
 .UNSPECIFIED., .F., .F. ) 
 B_SPLINE_CURVE_WITH_KNOTS ( ( 3, 2, 2, 2, 3 ),
 ( 0.3437500000000000000, 0.3444444444444444420, 0.3458333333333333259, 0.3472222222222222099, 0.3479166666666666519 ),
 .UNSPECIFIED. ) 
 CURVE ( )  GEOMETRIC_REPRESENTATION_ITEM ( )  RATIONAL_B_SPLINE_CURVE ( ( 0.9330127018922194093, 0.9330127018922194093, 1.000000000000000000, 0.8660254037844387076, 1.000000000000000000, 0.8660254037844387076, 1.000000000000000000, 0.9330127018922194093, 0.9330127018922194093 ) ) 
 REPRESENTATION_ITEM ( '' )  );
#38826 = DIRECTION ( 'NONE',  ( -1.000000000000000000, 0.000000000000000000, 0.000000000000000000 ) ) ;
#38827 = CARTESIAN_POINT ( 'NONE',  ( 4.458734125000000326, -168.6250000013655779, -1.846868145590734978 ) ) ;
#38828 = CARTESIAN_POINT ( 'NONE',  ( -2.229367062499996610, -104.3958333319677365, 3.861377020970582219 ) ) ;
#38829 = CARTESIAN_POINT ( 'NONE',  ( -2.500000000000000444, -69.04166666393547303, -4.330127018922193649 ) ) ;
#38830 = ORIENTED_EDGE ( 'NONE', *, *, #62480, .T. ) ;
#38831 = CARTESIAN_POINT ( 'NONE',  ( -57.89159099828107458, -150.9375000013656063, -3.393966926194107447 ) ) ;
#38832 = CARTESIAN_POINT ( 'NONE',  ( -58.24261429053147765, -138.3750000027312126, -3.805975901505573855 ) ) ;
#38833 = CARTESIAN_POINT ( 'NONE',  ( 4.458734124999999437, -36.81249999863440792, -5.460374474430324690E-16 ) ) ;
#38834 = CARTESIAN_POINT ( 'NONE',  ( 1.975475456537005874E-15, -56.75000000000000000, 5.000000000000000000 ) ) ;
#38835 = DIRECTION ( 'NONE',  ( -0.000000000000000000, 1.000000000000000000, -0.000000000000000000 ) ) ;
#38836 = CARTESIAN_POINT ( 'NONE',  ( -4.458734124999999437, -14.31249999863440436, 0.000000000000000000 ) ) ;
#38837 = CARTESIAN_POINT ( 'NONE',  ( -2.229367062499996610, -98.39583333196773651, 3.861377020970582219 ) ) ;
#38838 = VERTEX_POINT ( 'NONE', #49348 ) ;
#38839 =( BOUNDED_CURVE ( )  B_SPLINE_CURVE ( 2, ( #51734, #36937, #22783, #55924, #56879, #56563, #7987, #1907, #11839 ),
 .UNSPECIFIED., .F., .F. ) 
 B_SPLINE_CURVE_WITH_KNOTS ( ( 3, 2, 2, 2, 3 ),
 ( 0.4916666666666670849, 0.4958333333333337922, 0.5000000000000004441, 0.5041666666666670960, 0.5083333333333337478 ),
 .UNSPECIFIED. ) 
 CURVE ( )  GEOMETRIC_REPRESENTATION_ITEM ( )  RATIONAL_B_SPLINE_CURVE ( ( 0.9999999999999918954, 0.9238795325112948431, 1.000000000000000000, 0.9238795325112867385, 1.000000000000000000, 0.9238795325112867385, 1.000000000000000000, 0.9238795325112786339, 1.000000000000008216 ) ) 
 REPRESENTATION_ITEM ( '' )  );
#38840 = EDGE_CURVE ( 'NONE', #1445, #14167, #50305, .T. ) ;
#38841 = CARTESIAN_POINT ( 'NONE',  ( 1.846868145590735200, -142.5000000013656347, -4.458734125000000326 ) ) ;
#38842 = CARTESIAN_POINT ( 'NONE',  ( -4.458734124999999437, -28.64583333196774007, -2.574251347313719407 ) ) ;
#38843 = EDGE_CURVE ( 'NONE', #49754, #19960, #43709, .T. ) ;
#38844 = CARTESIAN_POINT ( 'NONE',  ( -5.000000000000000000, 12.00000000000000000, 0.000000000000000000 ) ) ;
#38845 = CARTESIAN_POINT ( 'NONE',  ( -50.55543936806279248, -134.0625000013656063, 0.3552334253322060320 ) ) ;
#38846 = CARTESIAN_POINT ( 'NONE',  ( 2.229367062499998831, -66.89583333196773651, -3.861377020970580887 ) ) ;
#38847 = CARTESIAN_POINT ( 'NONE',  ( 1.339745962155612702, -17.29465819873852084, -5.000000000000000000 ) ) ;
#38848 = CARTESIAN_POINT ( 'NONE',  ( 6.123233995736766282E-16, -170.0000000000000000, -5.000000000000000000 ) ) ;
#38849 = CARTESIAN_POINT ( 'NONE',  ( -3.152801135295367985, -141.8125000013655779, 3.152801135295367096 ) ) ;
#38850 = CARTESIAN_POINT ( 'NONE',  ( 9.457646018065525792E-16, 2.687500001365593860, 5.148502694627439702 ) ) ;
#38851 = ORIENTED_EDGE ( 'NONE', *, *, #61048, .F. ) ;
#38852 = CARTESIAN_POINT ( 'NONE',  ( 5.000000000000000888, 9.416666666666666075, 2.886751345948126879 ) ) ;
#38854 = CARTESIAN_POINT ( 'NONE',  ( -2.229367062499996610, -31.14583333196773651, 3.861377020970582219 ) ) ;
#38853 = CARTESIAN_POINT ( 'NONE',  ( -5.000000000000000000, -94.08333333333332860, -2.886751345948128211 ) ) ;
#38855 = CARTESIAN_POINT ( 'NONE',  ( -1.339745962155610925, -22.66965819600732956, 5.000000000000000000 ) ) ;
#38856 = CARTESIAN_POINT ( 'NONE',  ( -4.458734124999999437, -75.56249999863440792, 0.000000000000000000 ) ) ;
#38857 = CARTESIAN_POINT ( 'NONE',  ( -2.229367062500000163, 25.27083333469892779, -3.861377020970580443 ) ) ;
#38858 = CARTESIAN_POINT ( 'NONE',  ( -4.764381983412779477E-15, 27.25000000000000000, 5.000000000000000000 ) ) ;
#38859 = EDGE_CURVE ( 'NONE', #37487, #52254, #19482, .T. ) ;
#38860 = CARTESIAN_POINT ( 'NONE',  ( -59.44456063193725015, -142.5625000013656063, -0.3552334253322034230 ) ) ;
#38861 = CARTESIAN_POINT ( 'NONE',  ( -2.229367062500000163, -4.479166665301070438, -3.861377020970580443 ) ) ;
#38862 = CARTESIAN_POINT ( 'NONE',  ( 2.229367062500001939, 27.77083333469892779, 3.861377020970579999 ) ) ;
#38863 = CARTESIAN_POINT ( 'NONE',  ( -2.229367062500000163, -43.72916666530106511, -3.861377020970580443 ) ) ;
#38864 = CARTESIAN_POINT ( 'NONE',  ( -4.458734124999997661, -0.2291666653010705768, 2.574251347313722516 ) ) ;
#38865 = EDGE_LOOP ( 'NONE', ( #23724, #22967, #61716, #2026 ) ) ;
#38866 = CARTESIAN_POINT ( 'NONE',  ( 2.229367062499998831, -26.89583333196774007, -3.861377020970580887 ) ) ;
#38867 = AXIS2_PLACEMENT_3D ( 'NONE', #5553, #52629, #25165 ) ;
#38868 = CARTESIAN_POINT ( 'NONE',  ( 2.229367062500001939, -71.97916666530107932, 3.861377020970579999 ) ) ;
#38869 = CARTESIAN_POINT ( 'NONE',  ( 5.000000000000000000, -103.3749999972688158, -6.123233995736766282E-16 ) ) ;
#38870 = VECTOR ( 'NONE', #34078, 1000.000000000000000 ) ;
#38871 = CARTESIAN_POINT ( 'NONE',  ( 4.458734124999999437, 27.18750000136559564, -5.460374474430324690E-16 ) ) ;
#38872 = CARTESIAN_POINT ( 'NONE',  ( -58.24261429053147765, -139.2500000000000000, -3.805975901505573855 ) ) ;
#38873 = EDGE_CURVE ( 'NONE', #30395, #49021, #58936, .T. ) ;
#38874 = DIRECTION ( 'NONE',  ( -0.000000000000000000, 1.000000000000000000, -0.000000000000000000 ) ) ;
#38875 = CARTESIAN_POINT ( 'NONE',  ( 4.458734124999998549, -70.97916666530107932, -2.574251347313721627 ) ) ;
#38876 = CARTESIAN_POINT ( 'NONE',  ( 5.000000000000000000, -54.49999999999999289, -6.123233995736766282E-16 ) ) ;
#38877 = LINE ( 'NONE', #4788, #6951 ) ;
#38878 = CARTESIAN_POINT ( 'NONE',  ( 2.499999999999998668, 28.79166666939784847, -4.330127018922193649 ) ) ;
#38879 = ORIENTED_EDGE ( 'NONE', *, *, #48019, .F. ) ;
#38880 = CARTESIAN_POINT ( 'NONE',  ( -6.972266317189433020E-16, -56.25000000000000000, -5.000000000000000000 ) ) ;
#38881 = CARTESIAN_POINT ( 'NONE',  ( 1.339745962155612702, 2.830341803992664662, -5.000000000000000000 ) ) ;
#38882 = CARTESIAN_POINT ( 'NONE',  ( 5.000000000000000000, -14.49999999999999822, -6.123233995736766282E-16 ) ) ;
#38883 = CARTESIAN_POINT ( 'NONE',  ( 4.458734124999998549, -14.72916666530107399, -2.574251347313721627 ) ) ;
#38884 = CARTESIAN_POINT ( 'NONE',  ( -4.458734124999999437, -83.31249999863439371, 0.000000000000000000 ) ) ;
#38885 = VECTOR ( 'NONE', #11036, 1000.000000000000000 ) ;
#38886 = CARTESIAN_POINT ( 'NONE',  ( 1.846868145590736310, -166.8750000013655779, 4.458734124999999437 ) ) ;
#38887 = CARTESIAN_POINT ( 'NONE',  ( -5.000000000000000000, -15.95833333060214443, -2.886751345948128211 ) ) ;
#38889 = EDGE_LOOP ( 'NONE', ( #55472, #34817, #63295, #29386 ) ) ;
#38888 = CARTESIAN_POINT ( 'NONE',  ( 2.229367062500001939, -50.97916666530107221, 3.861377020970579999 ) ) ;
#38890 = CARTESIAN_POINT ( 'NONE',  ( -2.499999999999996447, -27.70833333060214798, 4.330127018922195425 ) ) ;
#38892 = ORIENTED_EDGE ( 'NONE', *, *, #16043, .F. ) ;
#38891 = CARTESIAN_POINT ( 'NONE',  ( -3.152548672688508926E-16, 1.187500001365596081, -5.148502694627439702 ) ) ;
#38893 = CARTESIAN_POINT ( 'NONE',  ( 1.975475456537005874E-15, -34.62499999726880873, 5.000000000000000000 ) ) ;
#38894 = CARTESIAN_POINT ( 'NONE',  ( 5.000000000000000000, -63.41666666666665719, -2.886751345948129988 ) ) ;
#38895 = CARTESIAN_POINT ( 'NONE',  ( 4.458734124999999437, -156.7500000013656063, 1.846868145590737864 ) ) ;
#38896 = CARTESIAN_POINT ( 'NONE',  ( -4.458734124999999437, -39.56249999863440081, 0.000000000000000000 ) ) ;
#38897 = CARTESIAN_POINT ( 'NONE',  ( 2.500000000000002220, -14.66666666666666785, 4.330127018922192761 ) ) ;
#38898 =( BOUNDED_CURVE ( )  B_SPLINE_CURVE ( 2, ( #42140, #3244, #62092, #57273, #13191, #47598, #28292, #23481, #39831 ),
 .UNSPECIFIED., .F., .F. ) 
 B_SPLINE_CURVE_WITH_KNOTS ( ( 3, 2, 2, 2, 3 ),
 ( 0.1145833333333333426, 0.1152777777777777846, 0.1166666666666666685, 0.1180555555555555525, 0.1187500000000000083 ),
 .UNSPECIFIED. ) 
 CURVE ( )  GEOMETRIC_REPRESENTATION_ITEM ( )  RATIONAL_B_SPLINE_CURVE ( ( 0.9330127018922194093, 0.9330127018922200755, 1.000000000000000000, 0.8660254037844387076, 1.000000000000000000, 0.8660254037844387076, 1.000000000000000000, 0.9330127018922187432, 0.9330127018922194093 ) ) 
 REPRESENTATION_ITEM ( '' )  );
#38899 = CARTESIAN_POINT ( 'NONE',  ( -2.071067811865475061, -160.6875000000000284, -5.000000000000000888 ) ) ;
#38900 = CARTESIAN_POINT ( 'NONE',  ( -5.000000000000000000, -30.00000000000000000, 0.000000000000000000 ) ) ;
#38901 = CARTESIAN_POINT ( 'NONE',  ( -50.40829686548195099, -126.2500000013656063, -1.485763867205728284 ) ) ;
#38902 = EDGE_CURVE ( 'NONE', #14226, #33989, #40971, .T. ) ;
#38903 = CARTESIAN_POINT ( 'NONE',  ( -3.152548672688508926E-16, -4.812499998634402587, -5.148502694627439702 ) ) ;
#38904 = CARTESIAN_POINT ( 'NONE',  ( 4.458734124999998549, -47.97916666530107221, -2.574251347313721627 ) ) ;
#38905 = ADVANCED_FACE ( 'NONE', ( #1763 ), #12348, .T. ) ;
#38906 = ADVANCED_FACE ( 'NONE', ( #41922 ), #61564, .T. ) ;
#38907 = CARTESIAN_POINT ( 'NONE',  ( 3.535533905932738197, -151.0000000027312126, -3.535533905932738197 ) ) ;
#38908 = CARTESIAN_POINT ( 'NONE',  ( 3.152801135295367541, -147.3125000013655779, -3.152801135295367541 ) ) ;
#38909 = CARTESIAN_POINT ( 'NONE',  ( 9.457646018065525792E-16, -87.31249999863440792, 5.148502694627439702 ) ) ;
#38910 = CARTESIAN_POINT ( 'NONE',  ( -58.80597590150559739, -143.0000000000000284, 3.242614290531460330 ) ) ;
#38911 = ORIENTED_EDGE ( 'NONE', *, *, #30374, .F. ) ;
#38912 = CARTESIAN_POINT ( 'NONE',  ( -6.972266317189433020E-16, 2.875000002731185500, -5.000000000000000000 ) ) ;
#38913 = CARTESIAN_POINT ( 'NONE',  ( -2.229367062500000163, 28.27083333469892779, -3.861377020970580443 ) ) ;
#38914 = CARTESIAN_POINT ( 'NONE',  ( -50.18089887299979068, -149.8125000027312126, 2.462841084822635640 ) ) ;
#38915 = DIRECTION ( 'NONE',  ( 0.000000000000000000, 0.000000000000000000, 1.000000000000000000 ) ) ;
#38916 = ORIENTED_EDGE ( 'NONE', *, *, #28411, .F. ) ;
#38917 = CARTESIAN_POINT ( 'NONE',  ( -6.972266317189433020E-16, -78.24999999999998579, -5.000000000000000000 ) ) ;
#38918 = CARTESIAN_POINT ( 'NONE',  ( -3.152548672688508926E-16, -12.81249999863440259, -5.148502694627439702 ) ) ;
#38919 = EDGE_CURVE ( 'NONE', #2786, #30395, #46445, .T. ) ;
#38920 = CARTESIAN_POINT ( 'NONE',  ( -4.458734124999999437, -0.3124999986344051406, 0.000000000000000000 ) ) ;
#38921 = CARTESIAN_POINT ( 'NONE',  ( -6.972266317189433020E-16, -74.12499999726878741, -5.000000000000000000 ) ) ;
#38922 = CARTESIAN_POINT ( 'NONE',  ( -4.458734125000000326, -154.8750000013655779, 1.846868145590734089 ) ) ;
#38923 =( BOUNDED_CURVE ( )  B_SPLINE_CURVE ( 2, ( #9460, #23644, #10098, #151, #33600, #34215, #29706, #28764, #62880 ),
 .UNSPECIFIED., .F., .F. ) 
 B_SPLINE_CURVE_WITH_KNOTS ( ( 3, 2, 2, 2, 3 ),
 ( 0.4982142857142857206, 0.4988095238095238138, 0.5000000000000000000, 0.5011904761904761862, 0.5017857142857142794 ),
 .UNSPECIFIED. ) 
 CURVE ( )  GEOMETRIC_REPRESENTATION_ITEM ( )  RATIONAL_B_SPLINE_CURVE ( ( 0.9330127018922194093, 0.9330127018922194093, 1.000000000000000000, 0.8660254037844387076, 1.000000000000000000, 0.8660254037844387076, 1.000000000000000000, 0.9330127018922194093, 0.9330127018922194093 ) ) 
 REPRESENTATION_ITEM ( '' )  );
#38924 = CARTESIAN_POINT ( 'NONE',  ( -2.229367062500000163, 21.27083333469892779, -3.861377020970580443 ) ) ;
#38925 = ORIENTED_EDGE ( 'NONE', *, *, #26009, .F. ) ;
#38926 = CARTESIAN_POINT ( 'NONE',  ( -2.229367062500000163, -93.47916666530106511, -3.861377020970580443 ) ) ;
#38927 = CARTESIAN_POINT ( 'NONE',  ( 0.000000000000000000, -120.0000000000000000, 0.000000000000000000 ) ) ;
#38928 = CARTESIAN_POINT ( 'NONE',  ( 1.339745962155612702, -40.29465819873851729, -5.000000000000000000 ) ) ;
#38929 = CARTESIAN_POINT ( 'NONE',  ( -3.152548672688508926E-16, -16.56249999863440792, -5.148502694627439702 ) ) ;
#38930 = CARTESIAN_POINT ( 'NONE',  ( 5.000000000000000000, -39.29166666393548724, -2.886751345948130876 ) ) ;
#38931 = CARTESIAN_POINT ( 'NONE',  ( -5.000000000000000000, -12.99999999999999822, 0.000000000000000000 ) ) ;
#38932 = CARTESIAN_POINT ( 'NONE',  ( -51.60603307380591787, -153.9375000013656063, -2.891590998281053704 ) ) ;
#38933 = CARTESIAN_POINT ( 'NONE',  ( -2.500000000000000444, -43.04166666393548013, -4.330127018922193649 ) ) ;
#38934 = CARTESIAN_POINT ( 'NONE',  ( 1.975475456537005874E-15, -41.62499999726880162, 5.000000000000000000 ) ) ;
#38935 = CARTESIAN_POINT ( 'NONE',  ( 4.458734124999999437, 18.18750000136559564, -5.460374474430324690E-16 ) ) ;
#38936 = CARTESIAN_POINT ( 'NONE',  ( -2.500000000000000444, 11.95833333606451809, -4.330127018922193649 ) ) ;
#38937 = VERTEX_POINT ( 'NONE', #56739 ) ;
#38938 = CARTESIAN_POINT ( 'NONE',  ( 4.458734124999999437, 19.18750000136559564, -5.460374474430324690E-16 ) ) ;
#38939 = CARTESIAN_POINT ( 'NONE',  ( -2.229367062499996610, -63.14583333196774362, 3.861377020970582219 ) ) ;
#38940 = CARTESIAN_POINT ( 'NONE',  ( -4.458734124999999437, -8.562499998634406140, 0.000000000000000000 ) ) ;
#38941 = CARTESIAN_POINT ( 'NONE',  ( -6.972266317189433020E-16, -31.24999999999999645, -5.000000000000000000 ) ) ;
#38942 = CARTESIAN_POINT ( 'NONE',  ( -2.500000000000000444, 10.83333333333333393, -4.330127018922193649 ) ) ;
#38943 = CARTESIAN_POINT ( 'NONE',  ( 4.458734125000000326, -169.3750000013656347, -1.846868145590734978 ) ) ;
#38944 = CARTESIAN_POINT ( 'NONE',  ( -5.000000000000000000, -98.95833333060214443, -2.886751345948128211 ) ) ;
#38945 = CARTESIAN_POINT ( 'NONE',  ( 4.458734125000001214, -50.89583333196772230, 2.574251347313718519 ) ) ;
#38946 = CARTESIAN_POINT ( 'NONE',  ( -5.000000000000000000, -90.95833333060213022, -2.886751345948128211 ) ) ;
#38947 = CARTESIAN_POINT ( 'NONE',  ( -6.972266317189433020E-16, -38.25000000000000000, -5.000000000000000000 ) ) ;
#38948 = CARTESIAN_POINT ( 'NONE',  ( 5.000000000000000000, 25.70833333606452342, -2.886751345948130876 ) ) ;
#38949 = DIRECTION ( 'NONE',  ( -0.000000000000000000, 1.000000000000000000, -0.000000000000000000 ) ) ;
#38950 = CARTESIAN_POINT ( 'NONE',  ( -4.458734124999999437, -152.1875000013656063, -5.460374474430324690E-16 ) ) ;
#38951 = CARTESIAN_POINT ( 'NONE',  ( -5.000000000000000000, -37.00000000000000711, 0.000000000000000000 ) ) ;
#38952 = CARTESIAN_POINT ( 'NONE',  ( 5.000000000000000000, -98.29166666393545881, -2.886751345948130876 ) ) ;
#38953 = CARTESIAN_POINT ( 'NONE',  ( 0.000000000000000000, -170.0000000000000000, 5.000000000000000000 ) ) ;
#38954 = ORIENTED_EDGE ( 'NONE', *, *, #13436, .F. ) ;
#38955 = CARTESIAN_POINT ( 'NONE',  ( -3.152548672688508926E-16, -100.5624999986344079, -5.148502694627439702 ) ) ;
#38956 = CARTESIAN_POINT ( 'NONE',  ( 2.229367062500001939, 2.770833334698928674, 3.861377020970579999 ) ) ;
#38957 =( GEOMETRIC_REPRESENTATION_CONTEXT ( 3 ) GLOBAL_UNCERTAINTY_ASSIGNED_CONTEXT ( ( #19121 ) ) GLOBAL_UNIT_ASSIGNED_CONTEXT ( ( #4901, #5540, #38669 ) ) REPRESENTATION_CONTEXT ( 'NONE', 'WORKASPACE' ) );
#38958 = CARTESIAN_POINT ( 'NONE',  ( 3.535533905932738197, -161.8750000000000284, -3.535533905932738197 ) ) ;
#38959 = CARTESIAN_POINT ( 'NONE',  ( 1.060575238724906964E-15, 2.249999999999998668, 5.773502691896257311 ) ) ;
#38960 = VECTOR ( 'NONE', #57729, 1000.000000000000000 ) ;
#38961 = CARTESIAN_POINT ( 'NONE',  ( 4.458734124999999437, -62.81249999863440792, -5.460374474430324690E-16 ) ) ;
#38962 = LINE ( 'NONE', #28684, #38016 ) ;
#38963 = CARTESIAN_POINT ( 'NONE',  ( 2.500000000000002220, -2.541666663935477466, 4.330127018922192761 ) ) ;
#38965 = ORIENTED_EDGE ( 'NONE', *, *, #1280, .F. ) ;
#38964 = CARTESIAN_POINT ( 'NONE',  ( -4.458734124999999437, -31.39583333196773296, -2.574251347313719407 ) ) ;
#38966 = FACE_OUTER_BOUND ( 'NONE', #36620, .T. ) ;
#38967 = CARTESIAN_POINT ( 'NONE',  ( -1.339745962155613812, -48.08034179853029144, -5.000000000000000000 ) ) ;
#38968 = CARTESIAN_POINT ( 'NONE',  ( -5.000000000000000000, 24.99999999999999645, 0.000000000000000000 ) ) ;
#38969 = CARTESIAN_POINT ( 'NONE',  ( 2.500000000000002220, -45.66666666666666430, 4.330127018922192761 ) ) ;
#38971 = CARTESIAN_POINT ( 'NONE',  ( 4.458734124999999437, -27.06249999863440081, -5.460374474430324690E-16 ) ) ;
#38970 = CARTESIAN_POINT ( 'NONE',  ( 0.000000000000000000, -170.0000000000000000, 5.000000000000000000 ) ) ;
#38972 = CARTESIAN_POINT ( 'NONE',  ( 2.500000000000002220, -4.541666663935479242, 4.330127018922192761 ) ) ;
#38973 = CARTESIAN_POINT ( 'NONE',  ( 9.457646018065525792E-16, -68.06249999863440792, 5.148502694627439702 ) ) ;
#38974 = CARTESIAN_POINT ( 'NONE',  ( -3.152801135295367985, -145.0625000013655779, 3.152801135295367096 ) ) ;
#38975 = CARTESIAN_POINT ( 'NONE',  ( -3.152548672688508926E-16, -74.56249999863440792, -5.148502694627439702 ) ) ;
#38976 = CARTESIAN_POINT ( 'NONE',  ( -57.89159099828107458, -137.9375000013656063, -3.393966926194107447 ) ) ;
#38977 = CARTESIAN_POINT ( 'NONE',  ( 2.229367062499998831, -29.89583333196773296, -3.861377020970580887 ) ) ;
#38978 = CARTESIAN_POINT ( 'NONE',  ( -3.535250795749689387E-16, -68.12499999726881583, -5.773502691896257311 ) ) ;
#38980 = VERTEX_POINT ( 'NONE', #31647 ) ;
#38979 = EDGE_CURVE ( 'NONE', #53169, #53313, #6363, .T. ) ;
#38981 = ADVANCED_FACE ( 'NONE', ( #16537 ), #17801, .T. ) ;
#38982 = ORIENTED_EDGE ( 'NONE', *, *, #48346, .F. ) ;
#38983 = CARTESIAN_POINT ( 'NONE',  ( -3.152548672688508926E-16, -72.81249999863439371, -5.148502694627439702 ) ) ;
#38984 = CARTESIAN_POINT ( 'NONE',  ( -1.339745962155612258, 28.79465819873852084, -5.000000000000000888 ) ) ;
#38985 = EDGE_CURVE ( 'NONE', #12164, #7641, #52219, .T. ) ;
#38986 = SURFACE_STYLE_FILL_AREA ( #48327 ) ;
#38987 = ORIENTED_EDGE ( 'NONE', *, *, #55706, .F. ) ;
#38988 = CARTESIAN_POINT ( 'NONE',  ( 1.339745962155615144, 12.29465819873851906, 4.999999999999999112 ) ) ;
#38989 = EDGE_CURVE ( 'NONE', #29232, #25897, #47852, .T. ) ;
#38990 = DIRECTION ( 'NONE',  ( -0.000000000000000000, 1.000000000000000000, -0.000000000000000000 ) ) ;
#38991 = CARTESIAN_POINT ( 'NONE',  ( -4.458734124999999437, -61.64583333196773651, -2.574251347313719407 ) ) ;
#38992 = ADVANCED_FACE ( 'NONE', ( #22958 ), #42555, .T. ) ;
#38993 = CARTESIAN_POINT ( 'NONE',  ( -2.229367062500000163, 1.270833334698927342, -3.861377020970580443 ) ) ;
#38994 = VERTEX_POINT ( 'NONE', #57685 ) ;
#38995 = EDGE_CURVE ( 'NONE', #57302, #25237, #28136, .T. ) ;
#38996 = CARTESIAN_POINT ( 'NONE',  ( 5.000000000000000000, -142.0000000000000284, 0.000000000000000000 ) ) ;
#38997 = CARTESIAN_POINT ( 'NONE',  ( 1.339745962155615144, -69.58034179853028434, 4.999999999999999112 ) ) ;
#38998 = EDGE_CURVE ( 'NONE', #15810, #50806, #30184, .T. ) ;
#38999 = CARTESIAN_POINT ( 'NONE',  ( 4.458734124999998549, 14.27083333469892779, -2.574251347313721627 ) ) ;
#39000 = CARTESIAN_POINT ( 'NONE',  ( -54.64476657466781973, -145.8125000013656063, -4.444560631937228834 ) ) ;
#39001 = CARTESIAN_POINT ( 'NONE',  ( -1.339745962155610925, -1.794658198738520616, 5.000000000000000000 ) ) ;
#39002 = CARTESIAN_POINT ( 'NONE',  ( -8.190561711645485556E-16, -166.6875000013655779, 4.458734124999999437 ) ) ;
#39003 = PRESENTATION_LAYER_ASSIGNMENT (  '', '', ( #28718 ) ) ;
#39005 = EDGE_CURVE ( 'NONE', #11960, #32525, #21946, .T. ) ;
#39004 = ORIENTED_EDGE ( 'NONE', *, *, #51159, .F. ) ;
#39006 = CARTESIAN_POINT ( 'NONE',  ( -3.152548672688508926E-16, -75.56249999863440792, -5.148502694627439702 ) ) ;
#39007 = CARTESIAN_POINT ( 'NONE',  ( -4.764381983412779477E-15, 26.25000000000000000, 5.000000000000000000 ) ) ;
#39008 = CARTESIAN_POINT ( 'NONE',  ( -3.152548672688508926E-16, 0.4375000013655955255, -5.148502694627439702 ) ) ;
#39009 = VECTOR ( 'NONE', #29628, 1000.000000000000114 ) ;
#39010 = EDGE_CURVE ( 'NONE', #38431, #35874, #52539, .T. ) ;
#39011 = CARTESIAN_POINT ( 'NONE',  ( -5.000000000000000000, 1.916666666666667407, -2.886751345948128211 ) ) ;
#39012 = CARTESIAN_POINT ( 'NONE',  ( 4.458734125000001214, -65.14583333196773651, 2.574251347313718519 ) ) ;
#39013 = CARTESIAN_POINT ( 'NONE',  ( 2.499999999999998668, -24.20833333060214443, -4.330127018922193649 ) ) ;
#39014 = CARTESIAN_POINT ( 'NONE',  ( -5.000000000000000000, 5.916666666666666963, -2.886751345948128211 ) ) ;
#39015 = CARTESIAN_POINT ( 'NONE',  ( 2.500000000000002220, -45.66666666666666430, 4.330127018922192761 ) ) ;
#39016 = CYLINDRICAL_SURFACE ( 'NONE', #21316, 5.000000000000000000 ) ;
#39017 = CARTESIAN_POINT ( 'NONE',  ( 9.457646018065525792E-16, -47.06249999863440792, 5.148502694627439702 ) ) ;
#39018 = CARTESIAN_POINT ( 'NONE',  ( 2.229367062499998831, -27.89583333196774007, -3.861377020970580887 ) ) ;
#39019 = CARTESIAN_POINT ( 'NONE',  ( -4.458734124999999437, 5.354166668032261711, -2.574251347313719407 ) ) ;
#39020 = CARTESIAN_POINT ( 'NONE',  ( -57.46284108482265651, -140.0625000027312126, 4.819101127000238627 ) ) ;
#39021 = CARTESIAN_POINT ( 'NONE',  ( 1.060575238724906964E-15, 25.25000000000000355, 5.773502691896257311 ) ) ;
#39022 = CARTESIAN_POINT ( 'NONE',  ( -2.071067811865478170, -148.4375000027312126, 5.000000000000000000 ) ) ;
#39023 = DIRECTION ( 'NONE',  ( -0.000000000000000000, 1.000000000000000000, -0.000000000000000000 ) ) ;
#39024 = CARTESIAN_POINT ( 'NONE',  ( 2.229367062499998831, -39.64583333196773651, -3.861377020970580887 ) ) ;
#39025 = CARTESIAN_POINT ( 'NONE',  ( -5.000000000000000000, -74.87499999726880162, 0.000000000000000000 ) ) ;
#39026 = CARTESIAN_POINT ( 'NONE',  ( -57.19623071787017210, -144.6250000013656063, 4.297418129356382899 ) ) ;
#39027 =( BOUNDED_CURVE ( )  B_SPLINE_CURVE ( 2, ( #10436, #44526, #486, #20088, #49678, #21374, #50318, #5623, #39693 ),
 .UNSPECIFIED., .F., .F. ) 
 B_SPLINE_CURVE_WITH_KNOTS ( ( 3, 2, 2, 2, 3 ),
 ( 0.8303571428571429047, 0.8309523809523809978, 0.8321428571428571841, 0.8333333333333333703, 0.8339285714285714635 ),
 .UNSPECIFIED. ) 
 CURVE ( )  GEOMETRIC_REPRESENTATION_ITEM ( )  RATIONAL_B_SPLINE_CURVE ( ( 0.9330127018922194093, 0.9330127018922194093, 1.000000000000000000, 0.8660254037844387076, 1.000000000000000000, 0.8660254037844387076, 1.000000000000000000, 0.9330127018922194093, 0.9330127018922194093 ) ) 
 REPRESENTATION_ITEM ( '' )  );
#39028 = CARTESIAN_POINT ( 'NONE',  ( 2.071067811865476394, -143.1875000000000000, 5.000000000000000000 ) ) ;
#39029 = CARTESIAN_POINT ( 'NONE',  ( 4.458734125000000326, -74.14583333196773651, 2.574251347313718519 ) ) ;
#39030 = CARTESIAN_POINT ( 'NONE',  ( -3.152801135295367096, -167.3125000013656063, -3.152801135295367541 ) ) ;
#39031 = CARTESIAN_POINT ( 'NONE',  ( 4.458734124999999437, -31.81249999863440436, -5.460374474430324690E-16 ) ) ;
#39032 = FACE_OUTER_BOUND ( 'NONE', #57409, .T. ) ;
#39033 = CARTESIAN_POINT ( 'NONE',  ( 0.000000000000000000, -120.0000000000000000, 5.000000000000000000 ) ) ;
#39034 = CARTESIAN_POINT ( 'NONE',  ( -4.999999999999999112, -23.91666666666667140, 2.886751345948131764 ) ) ;
#39035 = CARTESIAN_POINT ( 'NONE',  ( 4.458734125000000326, -145.3750000013656347, -1.846868145590734978 ) ) ;
#39036 = ORIENTED_EDGE ( 'NONE', *, *, #58244, .T. ) ;
#39037 = CARTESIAN_POINT ( 'NONE',  ( 2.229367062499998831, 26.10416666803225993, -3.861377020970580887 ) ) ;
#39038 = CARTESIAN_POINT ( 'NONE',  ( 4.458734124999999437, -56.06249999863440081, -5.460374474430324690E-16 ) ) ;
#39039 = CARTESIAN_POINT ( 'NONE',  ( 0.000000000000000000, -120.0000000000000000, 5.000000000000000000 ) ) ;
#39040 = CARTESIAN_POINT ( 'NONE',  ( -2.500000000000000444, 18.83333333333333215, -4.330127018922193649 ) ) ;
#39041 = CARTESIAN_POINT ( 'NONE',  ( -9.184850993605147944E-16, -168.2500000000000000, 5.000000000000000000 ) ) ;
#39042 = CARTESIAN_POINT ( 'NONE',  ( 2.229367062499998831, -5.645833331967740953, -3.861377020970580887 ) ) ;
#39043 = DIRECTION ( 'NONE',  ( 0.000000000000000000, 0.000000000000000000, 1.000000000000000000 ) ) ;
#39044 = CARTESIAN_POINT ( 'NONE',  ( -58.24261429053147765, -145.3750000027312126, -3.805975901505573855 ) ) ;
#39045 = LINE ( 'NONE', #30030, #5608 ) ;
#39046 = CARTESIAN_POINT ( 'NONE',  ( -2.352990130084580066E-16, 8.660254037844390851, -7.564335161054483336 ) ) ;
#39048 = CARTESIAN_POINT ( 'NONE',  ( -4.458734124999998549, -22.22916666530107221, 2.574251347313722516 ) ) ;
#39047 = CARTESIAN_POINT ( 'NONE',  ( 2.499999999999998668, 18.66666666666666430, -4.330127018922193649 ) ) ;
#39049 = CARTESIAN_POINT ( 'NONE',  ( 2.500000000000002220, 10.45833333606451987, 4.330127018922192761 ) ) ;
#39050 = CARTESIAN_POINT ( 'NONE',  ( 4.458734124999998549, -55.72916666530107221, -2.574251347313721627 ) ) ;
#39051 = CARTESIAN_POINT ( 'NONE',  ( -3.152801135295367096, -154.3125000013656063, -3.152801135295367541 ) ) ;
#39052 = AXIS2_PLACEMENT_3D ( 'NONE', #58271, #19335, #8441 ) ;
#39053 = CARTESIAN_POINT ( 'NONE',  ( -5.000000000000000000, -49.95833333060213022, -2.886751345948128211 ) ) ;
#39054 = ORIENTED_EDGE ( 'NONE', *, *, #1931, .T. ) ;
#39055 = CARTESIAN_POINT ( 'NONE',  ( 2.229367062499998831, 4.104166668032260823, -3.861377020970580887 ) ) ;
#39056 = ORIENTED_EDGE ( 'NONE', *, *, #48085, .T. ) ;
#39058 = CARTESIAN_POINT ( 'NONE',  ( -1.339745962155613812, -3.205341801261480938, -5.000000000000000000 ) ) ;
#39057 = CARTESIAN_POINT ( 'NONE',  ( 2.499999999999998668, -4.333333333333334814, -4.330127018922193649 ) ) ;
#39059 = CARTESIAN_POINT ( 'NONE',  ( -3.152801135295367096, -157.0625000013656063, -3.152801135295367541 ) ) ;
#39060 = ORIENTED_EDGE ( 'NONE', *, *, #18161, .T. ) ;
#39061 = PRODUCT_DEFINITION_CONTEXT ( 'detailed design', #242, 'design' ) ;
#39062 = FACE_OUTER_BOUND ( 'NONE', #4047, .T. ) ;
#39063 = CARTESIAN_POINT ( 'NONE',  ( -50.18089887299979068, -132.6875000000000284, 2.462841084822635640 ) ) ;
#39064 = CARTESIAN_POINT ( 'NONE',  ( 2.500000000000002220, -53.54166666393548013, 4.330127018922192761 ) ) ;
#39065 = CARTESIAN_POINT ( 'NONE',  ( -4.458734124999998549, -42.47916666530107932, 2.574251347313722516 ) ) ;
#39066 = ORIENTED_EDGE ( 'NONE', *, *, #51943, .F. ) ;
#39067 = CARTESIAN_POINT ( 'NONE',  ( -4.330127018922205195, 45.00000000000000000, -7.499999999999943157 ) ) ;
#39068 = CARTESIAN_POINT ( 'NONE',  ( 4.458734124999998549, 19.27083333469893134, -2.574251347313721627 ) ) ;
#39069 = DIRECTION ( 'NONE',  ( -0.000000000000000000, 1.000000000000000000, -0.000000000000000000 ) ) ;
#39070 =( BOUNDED_CURVE ( )  B_SPLINE_CURVE ( 2, ( #15428, #40494, #11227, #1294, #637, #39849, #6101, #60135, #34717 ),
 .UNSPECIFIED., .F., .F. ) 
 B_SPLINE_CURVE_WITH_KNOTS ( ( 3, 2, 2, 2, 3 ),
 ( 0.3803571428571428381, 0.3809523809523809312, 0.3821428571428571175, 0.3833333333333333592, 0.3839285714285714524 ),
 .UNSPECIFIED. ) 
 CURVE ( )  GEOMETRIC_REPRESENTATION_ITEM ( )  RATIONAL_B_SPLINE_CURVE ( ( 0.9330127018922194093, 0.9330127018922194093, 1.000000000000000000, 0.8660254037844387076, 1.000000000000000000, 0.8660254037844387076, 1.000000000000000000, 0.9330127018922194093, 0.9330127018922194093 ) ) 
 REPRESENTATION_ITEM ( '' )  );
#39071 = ORIENTED_EDGE ( 'NONE', *, *, #56737, .F. ) ;
#39072 = CARTESIAN_POINT ( 'NONE',  ( 9.457646018065525792E-16, 27.93750000136559208, 5.148502694627439702 ) ) ;
#39073 = CARTESIAN_POINT ( 'NONE',  ( -51.19402409849444524, -126.6250000027312126, -3.242614290531456334 ) ) ;
#39074 = CARTESIAN_POINT ( 'NONE',  ( -5.000000000000000000, 25.04166666939785202, -2.886751345948128211 ) ) ;
#39075 = CARTESIAN_POINT ( 'NONE',  ( 2.499999999999998668, -100.3333333333333286, -4.330127018922193649 ) ) ;
#39076 =( BOUNDED_CURVE ( )  B_SPLINE_CURVE ( 2, ( #30365, #33922, #49027, #25547, #40011, #29081, #15589, #48708, #38737 ),
 .UNSPECIFIED., .F., .F. ) 
 B_SPLINE_CURVE_WITH_KNOTS ( ( 3, 2, 2, 2, 3 ),
 ( 0.2732142857142857428, 0.2738095238095238360, 0.2750000000000000222, 0.2761904761904762085, 0.2767857142857143016 ),
 .UNSPECIFIED. ) 
 CURVE ( )  GEOMETRIC_REPRESENTATION_ITEM ( )  RATIONAL_B_SPLINE_CURVE ( ( 0.9330127018922194093, 0.9330127018922225179, 1.000000000000000000, 0.8660254037844387076, 1.000000000000000000, 0.8660254037844387076, 1.000000000000000000, 0.9330127018922194093, 0.9330127018922194093 ) ) 
 REPRESENTATION_ITEM ( '' )  );
#39077 = CARTESIAN_POINT ( 'NONE',  ( 2.229367062499998831, -58.64583333196773651, -3.861377020970580887 ) ) ;
#39078 = CARTESIAN_POINT ( 'NONE',  ( 1.975475456537005874E-15, 10.37500000273118417, 5.000000000000000000 ) ) ;
#39079 = CARTESIAN_POINT ( 'NONE',  ( -4.458734124999999437, 18.68750000136559564, 0.000000000000000000 ) ) ;
#39080 = EDGE_CURVE ( 'NONE', #25339, #44494, #21576, .T. ) ;
#39081 = CARTESIAN_POINT ( 'NONE',  ( -4.458734124999998549, -49.47916666530106511, 2.574251347313722516 ) ) ;
#39082 = CARTESIAN_POINT ( 'NONE',  ( -2.499999999999996447, -8.708333330602144429, 4.330127018922195425 ) ) ;
#39083 = CARTESIAN_POINT ( 'NONE',  ( 0.000000000000000000, -170.0000000000000000, 0.000000000000000000 ) ) ;
#39084 = CARTESIAN_POINT ( 'NONE',  ( -3.152548672688508926E-16, -87.81249999863439371, -5.148502694627439702 ) ) ;
#39085 = CARTESIAN_POINT ( 'NONE',  ( -3.152548672688508926E-16, -108.5624999986343937, -5.148502694627439702 ) ) ;
#39086 = CARTESIAN_POINT ( 'NONE',  ( 4.458734125000000326, -10.14583333196773829, 2.574251347313718519 ) ) ;
#39087 = ORIENTED_EDGE ( 'NONE', *, *, #4010, .T. ) ;
#39088 = CARTESIAN_POINT ( 'NONE',  ( -2.500000000000000444, -17.04166666393548368, -4.330127018922193649 ) ) ;
#39089 = CARTESIAN_POINT ( 'NONE',  ( -3.152548672688508926E-16, -98.56249999863442213, -5.148502694627439702 ) ) ;
#39090 = CARTESIAN_POINT ( 'NONE',  ( 5.000000000000000000, -163.1875000027312410, 2.071067811865478614 ) ) ;
#39091 = CARTESIAN_POINT ( 'NONE',  ( -4.458734124999999437, -98.56249999863440792, 0.000000000000000000 ) ) ;
#39092 = VECTOR ( 'NONE', #45783, 1000.000000000000000 ) ;
#39093 = CARTESIAN_POINT ( 'NONE',  ( 1.339745962155612702, -49.16965819600731891, -5.000000000000000000 ) ) ;
#39094 = CARTESIAN_POINT ( 'NONE',  ( -2.499999999999996447, -49.70833333060213732, 4.330127018922195425 ) ) ;
#39095 = CARTESIAN_POINT ( 'NONE',  ( 1.975475456537005874E-15, -84.62499999726880162, 5.000000000000000000 ) ) ;
#39096 = CARTESIAN_POINT ( 'NONE',  ( -53.51423613279429503, -129.2500000013656347, 4.591703134518082763 ) ) ;
#39097 = CARTESIAN_POINT ( 'NONE',  ( -52.80376928212989185, -146.8750000013656063, -4.297418129356378458 ) ) ;
#39098 = CARTESIAN_POINT ( 'NONE',  ( 4.458734124999998549, -20.72916666530107221, -2.574251347313721627 ) ) ;
#39099 = CARTESIAN_POINT ( 'NONE',  ( 4.458734124999998549, 5.020833334698926897, -2.574251347313721627 ) ) ;
#39100 =( BOUNDED_CURVE ( )  B_SPLINE_CURVE ( 2, ( #27818, #3395, #52278, #38113, #27195, #28134, #32648, #62571, #56479 ),
 .UNSPECIFIED., .F., .F. ) 
 B_SPLINE_CURVE_WITH_KNOTS ( ( 3, 2, 2, 2, 3 ),
 ( 0.7874999999999999778, 0.7880952380952380709, 0.7892857142857142572, 0.7904761904761904434, 0.7910714285714285365 ),
 .UNSPECIFIED. ) 
 CURVE ( )  GEOMETRIC_REPRESENTATION_ITEM ( )  RATIONAL_B_SPLINE_CURVE ( ( 0.9330127018922194093, 0.9330127018922194093, 1.000000000000000000, 0.8660254037844387076, 1.000000000000000000, 0.8660254037844387076, 1.000000000000000000, 0.9330127018922194093, 0.9330127018922194093 ) ) 
 REPRESENTATION_ITEM ( '' )  );
#39101 = CARTESIAN_POINT ( 'NONE',  ( -3.152548672688508926E-16, -57.81249999863440081, -5.148502694627439702 ) ) ;
#39102 = CARTESIAN_POINT ( 'NONE',  ( 5.000000000000000000, -48.37499999726880873, -6.123233995736766282E-16 ) ) ;
#39103 = CARTESIAN_POINT ( 'NONE',  ( -4.458734124999999437, -12.31249999863440259, 0.000000000000000000 ) ) ;
#39104 = CARTESIAN_POINT ( 'NONE',  ( 1.975475456537005874E-15, -21.75000000000000000, 5.000000000000000000 ) ) ;
#39105 = CARTESIAN_POINT ( 'NONE',  ( 5.000000000000000888, -156.9375000000000284, -2.071067811865475505 ) ) ;
#39106 = CARTESIAN_POINT ( 'NONE',  ( 2.500000000000002220, -8.666666666666669627, 4.330127018922192761 ) ) ;
#39107 = VERTEX_POINT ( 'NONE', #14538 ) ;
#39108 = CARTESIAN_POINT ( 'NONE',  ( -2.229367062500000163, -41.72916666530107932, -3.861377020970580443 ) ) ;
#39109 = LINE ( 'NONE', #18858, #4759 ) ;
#39110 = CARTESIAN_POINT ( 'NONE',  ( -4.419133455862249704, 6.108866147517435508, -7.026396753507433424 ) ) ;
#39111 = CARTESIAN_POINT ( 'NONE',  ( -5.000000000000000000, -66.87499999726881583, 0.000000000000000000 ) ) ;
#39112 = CARTESIAN_POINT ( 'NONE',  ( 4.458734124999999437, -87.81249999863439371, -5.460374474430324690E-16 ) ) ;
#39113 = CARTESIAN_POINT ( 'NONE',  ( 2.229367062500001939, 18.77083333469892779, 3.861377020970579999 ) ) ;
#39114 = CARTESIAN_POINT ( 'NONE',  ( -2.229367062500000163, 11.52083333469892601, -3.861377020970580443 ) ) ;
#39115 = CARTESIAN_POINT ( 'NONE',  ( -6.972266317189433020E-16, -82.24999999999998579, -5.000000000000000000 ) ) ;
#39116 = LINE ( 'NONE', #19182, #19402 ) ;
#39117 = CARTESIAN_POINT ( 'NONE',  ( -4.458734124999999437, -87.64583333196773651, -2.574251347313719407 ) ) ;
#39118 = CARTESIAN_POINT ( 'NONE',  ( 4.458734125000001214, 22.85416666803225993, 2.574251347313718519 ) ) ;
#39119 = CARTESIAN_POINT ( 'NONE',  ( 1.060575238724906964E-15, -77.75000000000000000, 5.773502691896257311 ) ) ;
#39120 = CARTESIAN_POINT ( 'NONE',  ( -5.000000000000000000, 14.04166666939785202, -2.886751345948128211 ) ) ;
#39121 = ORIENTED_EDGE ( 'NONE', *, *, #11395, .T. ) ;
#39122 = CARTESIAN_POINT ( 'NONE',  ( -6.972266317189433020E-16, -7.124999997268814056, -5.000000000000000000 ) ) ;
#39123 = VERTEX_POINT ( 'NONE', #3964 ) ;
#39124 =( BOUNDED_CURVE ( )  B_SPLINE_CURVE ( 2, ( #61527, #57956, #18702, #17765, #47039, #48281, #62475, #52808, #13877 ),
 .UNSPECIFIED., .F., .F. ) 
 B_SPLINE_CURVE_WITH_KNOTS ( ( 3, 2, 2, 2, 3 ),
 ( 0.7089285714285714635, 0.7095238095238095566, 0.7107142857142857428, 0.7119047619047619291, 0.7125000000000000222 ),
 .UNSPECIFIED. ) 
 CURVE ( )  GEOMETRIC_REPRESENTATION_ITEM ( )  RATIONAL_B_SPLINE_CURVE ( ( 0.9330127018922194093, 0.9330127018922194093, 1.000000000000000000, 0.8660254037844387076, 1.000000000000000000, 0.8660254037844387076, 1.000000000000000000, 0.9330127018922194093, 0.9330127018922194093 ) ) 
 REPRESENTATION_ITEM ( '' )  );
#39126 = CARTESIAN_POINT ( 'NONE',  ( -2.500000000000000444, -34.16666666666666430, -4.330127018922193649 ) ) ;
#39125 = LINE ( 'NONE', #44588, #17267 ) ;
#39127 = CARTESIAN_POINT ( 'NONE',  ( 4.458734124999998549, -38.72916666530106511, -2.574251347313721627 ) ) ;
#39128 = CARTESIAN_POINT ( 'NONE',  ( -4.999999999999999112, -33.79166666393547303, 2.886751345948131764 ) ) ;
#39130 = ORIENTED_EDGE ( 'NONE', *, *, #36172, .T. ) ;
#39129 = CARTESIAN_POINT ( 'NONE',  ( 4.458734124999999437, -63.81249999863440792, -5.460374474430324690E-16 ) ) ;
#39131 = CARTESIAN_POINT ( 'NONE',  ( -57.89159099828107458, -152.9375000013656063, -3.393966926194107447 ) ) ;
#39132 = CARTESIAN_POINT ( 'NONE',  ( 4.458734125000001214, -13.89583333196774007, 2.574251347313718519 ) ) ;
#39134 = EDGE_LOOP ( 'NONE', ( #1509, #19757, #54146, #36230 ) ) ;
#39133 = CARTESIAN_POINT ( 'NONE',  ( 4.458734125000001214, -16.14583333196773651, 2.574251347313718519 ) ) ;
#39135 = CARTESIAN_POINT ( 'NONE',  ( 2.499999999999998668, -80.33333333333332860, -4.330127018922193649 ) ) ;
#39136 = CARTESIAN_POINT ( 'NONE',  ( -56.48576386720575471, -136.7500000013655779, -4.591703134518078322 ) ) ;
#39137 = CARTESIAN_POINT ( 'NONE',  ( -2.229367062499996610, -58.39583333196773651, 3.861377020970582219 ) ) ;
#39138 = CARTESIAN_POINT ( 'NONE',  ( 5.000000000000000000, -81.37499999726881583, -6.123233995736766282E-16 ) ) ;
#39140 = ORIENTED_EDGE ( 'NONE', *, *, #2339, .T. ) ;
#39139 = CARTESIAN_POINT ( 'NONE',  ( -1.049326080737009628E-13, -17.75000000000000355, 5.000000000000000000 ) ) ;
#39141 = VECTOR ( 'NONE', #26739, 1000.000000000000000 ) ;
#39142 = CARTESIAN_POINT ( 'NONE',  ( -56.66612745406270335, -147.3125000000000284, -5.149110718188516067 ) ) ;
#39143 = CARTESIAN_POINT ( 'NONE',  ( -2.229367062500000163, -25.72916666530106866, -3.861377020970580443 ) ) ;
#39144 = EDGE_LOOP ( 'NONE', ( #29696, #7034, #32274, #30273 ) ) ;
#39145 = CARTESIAN_POINT ( 'NONE',  ( 1.846868145590735200, -165.5000000013655779, -4.458734125000000326 ) ) ;
#39146 = CARTESIAN_POINT ( 'NONE',  ( 2.229367062500001939, -106.2291666653010651, 3.861377020970579999 ) ) ;
#39147 = CARTESIAN_POINT ( 'NONE',  ( -1.339745962155613812, -69.08034179853028434, -5.000000000000000000 ) ) ;
#39148 = VERTEX_POINT ( 'NONE', #43180 ) ;
#39149 = CARTESIAN_POINT ( 'NONE',  ( -53.51423613279429503, -145.5000000013656063, 4.591703134518083651 ) ) ;
#39150 = AXIS2_PLACEMENT_3D ( 'NONE', #1215, #35605, #49437 ) ;
#39151 = CARTESIAN_POINT ( 'NONE',  ( -60.14911071818854538, -138.1875000027312126, 1.666127454062681368 ) ) ;
#39152 = CARTESIAN_POINT ( 'NONE',  ( 2.229367062499998831, -39.64583333196773651, -3.861377020970580887 ) ) ;
#39153 = CARTESIAN_POINT ( 'NONE',  ( 4.458734124999997661, -144.7500000013655779, 1.846868145590737864 ) ) ;
#39154 = FACE_OUTER_BOUND ( 'NONE', #10182, .T. ) ;
#39155 = CARTESIAN_POINT ( 'NONE',  ( 5.000000000000000000, 29.50000000000000000, -6.123233995736766282E-16 ) ) ;
#39156 = CARTESIAN_POINT ( 'NONE',  ( -4.458734124999998549, -15.22916666530107754, 2.574251347313722516 ) ) ;
#39157 = CARTESIAN_POINT ( 'NONE',  ( 4.458734125000000326, -101.1458333319677365, 2.574251347313718519 ) ) ;
#39158 = ORIENTED_EDGE ( 'NONE', *, *, #57204, .T. ) ;
#39159 = CARTESIAN_POINT ( 'NONE',  ( 3.152801135295366208, -143.8125000013655779, 3.152801135295367985 ) ) ;
#39160 = CARTESIAN_POINT ( 'NONE',  ( -4.458734124999998549, -35.47916666530107221, 2.574251347313722516 ) ) ;
#39161 = CARTESIAN_POINT ( 'NONE',  ( 1.060575238724906964E-15, 5.375000002731184168, 5.773502691896257311 ) ) ;
#39162 = CARTESIAN_POINT ( 'NONE',  ( -54.60164318462004474, -139.5000000027312126, -4.984105922594373794 ) ) ;
#39163 = CARTESIAN_POINT ( 'NONE',  ( -53.51423613279429503, -134.2500000013656063, 4.591703134518082763 ) ) ;
#39164 = CARTESIAN_POINT ( 'NONE',  ( 2.229367062500001939, -67.22916666530106511, 3.861377020970579999 ) ) ;
#39165 = CYLINDRICAL_SURFACE ( 'NONE', #18864, 5.000000000000000000 ) ;
#39166 = CARTESIAN_POINT ( 'NONE',  ( 5.000000000000000000, -54.29166666393549434, -2.886751345948130876 ) ) ;
#39167 = CARTESIAN_POINT ( 'NONE',  ( -2.621086668468698644, -7.606368536631371136, -7.634085501268427443 ) ) ;
#39168 = CARTESIAN_POINT ( 'NONE',  ( -4.458734124999999437, 6.354166668032259047, -2.574251347313719407 ) ) ;
#39169 = ORIENTED_EDGE ( 'NONE', *, *, #18881, .T. ) ;
#39170 = CARTESIAN_POINT ( 'NONE',  ( -5.000000000000000000, 16.04166666939785202, -2.886751345948128211 ) ) ;
#39172 = CARTESIAN_POINT ( 'NONE',  ( 9.457646018065525792E-16, -28.06249999863440081, 5.148502694627439702 ) ) ;
#39171 = CARTESIAN_POINT ( 'NONE',  ( 5.000000000000000888, -93.58333333333332860, 2.886751345948126879 ) ) ;
#39173 = CARTESIAN_POINT ( 'NONE',  ( 1.339745962155612702, -95.29465819873851729, -5.000000000000000000 ) ) ;
#39174 = CARTESIAN_POINT ( 'NONE',  ( 4.458734125000001214, -82.14583333196772230, 2.574251347313718519 ) ) ;
#39175 = CARTESIAN_POINT ( 'NONE',  ( -4.458734124999997661, 25.52083333469892423, 2.574251347313722516 ) ) ;
#39176 = CARTESIAN_POINT ( 'NONE',  ( 2.500000000000002220, -18.66666666666666430, 4.330127018922192761 ) ) ;
#39177 = CARTESIAN_POINT ( 'NONE',  ( -59.59170313451811296, -140.5000000013656347, 1.485763867205729394 ) ) ;
#39178 = CARTESIAN_POINT ( 'NONE',  ( -2.229367062499996610, -1.145833331967736957, 3.861377020970582219 ) ) ;
#39179 = CARTESIAN_POINT ( 'NONE',  ( -2.229367062500000163, 27.27083333469892779, -3.861377020970580443 ) ) ;
#39180 = CARTESIAN_POINT ( 'NONE',  ( 2.229367062499998831, -41.89583333196773651, -3.861377020970580887 ) ) ;
#39181 = CARTESIAN_POINT ( 'NONE',  ( -1.339745962155613812, -51.08034179853027723, -5.000000000000000000 ) ) ;
#39182 = CARTESIAN_POINT ( 'NONE',  ( -2.229367062500000163, 0.5208333346989266754, -3.861377020970580443 ) ) ;
#39183 = ORIENTED_EDGE ( 'NONE', *, *, #29558, .F. ) ;
#39184 = CARTESIAN_POINT ( 'NONE',  ( -4.458734124999999437, -23.64583333196773651, -2.574251347313719407 ) ) ;
#39185 = AXIS2_PLACEMENT_3D ( 'NONE', #44386, #4841, #44066 ) ;
#39186 = CARTESIAN_POINT ( 'NONE',  ( 2.229367062500001939, -66.97916666530106511, 3.861377020970579999 ) ) ;
#39187 = CARTESIAN_POINT ( 'NONE',  ( -3.535250795749689387E-16, -106.1249999972688300, -5.773502691896257311 ) ) ;
#39188 = EDGE_CURVE ( 'NONE', #13925, #60011, #13915, .T. ) ;
#39189 = CARTESIAN_POINT ( 'NONE',  ( 2.229367062499998831, 25.35416666803225993, -3.861377020970580887 ) ) ;
#39190 = DIRECTION ( 'NONE',  ( -0.000000000000000000, 1.000000000000000000, -0.000000000000000000 ) ) ;
#39191 = CARTESIAN_POINT ( 'NONE',  ( 6.123233995736766282E-16, -170.0000000000000000, -5.000000000000000000 ) ) ;
#39192 = CARTESIAN_POINT ( 'NONE',  ( -3.152548672688508926E-16, -71.81249999863439371, -5.148502694627439702 ) ) ;
#39193 = CARTESIAN_POINT ( 'NONE',  ( -2.499999999999996447, -60.83333333333333570, 4.330127018922195425 ) ) ;
#39194 = CARTESIAN_POINT ( 'NONE',  ( -1.339745962155613812, -22.20534180126147561, -5.000000000000000000 ) ) ;
#39195 = CARTESIAN_POINT ( 'NONE',  ( -2.499999999999996447, 28.29166666939785202, 4.330127018922195425 ) ) ;
#39196 = EDGE_LOOP ( 'NONE', ( #8850, #40386, #6486, #62621 ) ) ;
#39197 = DIRECTION ( 'NONE',  ( -0.000000000000000000, -0.000000000000000000, 1.000000000000000000 ) ) ;
#39198 = CARTESIAN_POINT ( 'NONE',  ( 5.000000000000000888, -16.58333333333333215, 2.886751345948126879 ) ) ;
#39199 = CARTESIAN_POINT ( 'NONE',  ( -2.229367062499996610, -24.14583333196773651, 3.861377020970582219 ) ) ;
#39200 = CARTESIAN_POINT ( 'NONE',  ( -3.152548672688508926E-16, -84.56249999863439371, -5.148502694627439702 ) ) ;
#39201 =( BOUNDED_CURVE ( )  B_SPLINE_CURVE ( 2, ( #27430, #12643, #8149, #47063, #32580, #41905, #27125, #62178, #47377 ),
 .UNSPECIFIED., .F., .F. ) 
 B_SPLINE_CURVE_WITH_KNOTS ( ( 3, 2, 2, 2, 3 ),
 ( 0.2982142857142857095, 0.2988095238095238027, 0.2999999999999999889, 0.3011904761904761751, 0.3017857142857142683 ),
 .UNSPECIFIED. ) 
 CURVE ( )  GEOMETRIC_REPRESENTATION_ITEM ( )  RATIONAL_B_SPLINE_CURVE ( ( 0.9330127018922194093, 0.9330127018922194093, 1.000000000000000000, 0.8660254037844387076, 1.000000000000000000, 0.8660254037844387076, 1.000000000000000000, 0.9330127018922194093, 0.9330127018922194093 ) ) 
 REPRESENTATION_ITEM ( '' )  );
#39202 = CARTESIAN_POINT ( 'NONE',  ( -1.846868145590737420, -168.0000000013655779, 4.458734124999999437 ) ) ;
#39203 = EDGE_CURVE ( 'NONE', #19510, #57924, #61413, .T. ) ;
#39204 = CARTESIAN_POINT ( 'NONE',  ( 2.500000000000002220, -18.54166666393547658, 4.330127018922192761 ) ) ;
#39206 = ORIENTED_EDGE ( 'NONE', *, *, #24500, .T. ) ;
#39205 = CARTESIAN_POINT ( 'NONE',  ( -4.458734124999999437, -48.31249999863440792, 0.000000000000000000 ) ) ;
#39207 = CARTESIAN_POINT ( 'NONE',  ( -6.972266317189433020E-16, -24.24999999999999645, -5.000000000000000000 ) ) ;
#39208 = CARTESIAN_POINT ( 'NONE',  ( -75.00000000000000000, 15.00000000000000000, 8.999999999999998224 ) ) ;
#39210 = VERTEX_POINT ( 'NONE', #59310 ) ;
#39209 = CARTESIAN_POINT ( 'NONE',  ( -4.458734124999999437, 2.437500001365593860, 0.000000000000000000 ) ) ;
#39211 = CARTESIAN_POINT ( 'NONE',  ( -58.39396692619412477, -154.4375000013656063, 2.891590998281057701 ) ) ;
#39212 = CARTESIAN_POINT ( 'NONE',  ( -5.000000000000000000, -68.99999999999998579, 0.000000000000000000 ) ) ;
#39213 = CARTESIAN_POINT ( 'NONE',  ( 1.846868145590735200, -154.5000000013656347, -4.458734125000000326 ) ) ;
#39214 = CARTESIAN_POINT ( 'NONE',  ( -4.458734124999999437, -41.64583333196773651, -2.574251347313719407 ) ) ;
#39215 = DIRECTION ( 'NONE',  ( -0.000000000000000000, 1.000000000000000000, -0.000000000000000000 ) ) ;
#39216 = CARTESIAN_POINT ( 'NONE',  ( -5.000000000000000888, -160.4375000000000568, 2.071067811865474617 ) ) ;
#39217 = CARTESIAN_POINT ( 'NONE',  ( 1.975475456537005874E-15, -51.62499999726880873, 5.000000000000000000 ) ) ;
#39218 = CARTESIAN_POINT ( 'NONE',  ( -59.44456063193725015, -127.8125000013655921, -0.3552334253322034230 ) ) ;
#39219 = CARTESIAN_POINT ( 'NONE',  ( -4.458734124999999437, -10.56249999863440792, 0.000000000000000000 ) ) ;
#39220 = CARTESIAN_POINT ( 'NONE',  ( 4.458734124999998549, -48.97916666530107221, -2.574251347313721627 ) ) ;
#39221 =( BOUNDED_CURVE ( )  B_SPLINE_CURVE ( 2, ( #59642, #35832, #41267, #25534, #16837, #50297, #46109, #21677, #45151 ),
 .UNSPECIFIED., .F., .F. ) 
 B_SPLINE_CURVE_WITH_KNOTS ( ( 3, 2, 2, 2, 3 ),
 ( 0.7410714285714286031, 0.7416666666666666963, 0.7428571428571428825, 0.7440476190476190688, 0.7446428571428571619 ),
 .UNSPECIFIED. ) 
 CURVE ( )  GEOMETRIC_REPRESENTATION_ITEM ( )  RATIONAL_B_SPLINE_CURVE ( ( 0.9330127018922194093, 0.9330127018922194093, 1.000000000000000000, 0.8660254037844387076, 1.000000000000000000, 0.8660254037844387076, 1.000000000000000000, 0.9330127018922194093, 0.9330127018922194093 ) ) 
 REPRESENTATION_ITEM ( '' )  );
#39222 = DIRECTION ( 'NONE',  ( 0.000000000000000000, 0.000000000000000000, 1.000000000000000000 ) ) ;
#39223 = CARTESIAN_POINT ( 'NONE',  ( 4.458734124999999437, -148.4375000013656063, 0.000000000000000000 ) ) ;
#39224 = CARTESIAN_POINT ( 'NONE',  ( -4.458734124999999437, -87.64583333196773651, -2.574251347313719407 ) ) ;
#39225 = CARTESIAN_POINT ( 'NONE',  ( -55.39835681537999790, -142.8750000000000284, 4.984105922594378235 ) ) ;
#39226 = ORIENTED_EDGE ( 'NONE', *, *, #42264, .T. ) ;
#39227 = CARTESIAN_POINT ( 'NONE',  ( 1.339745962155615144, -19.58034179853029499, 4.999999999999999112 ) ) ;
#39228 = CARTESIAN_POINT ( 'NONE',  ( -5.000000000000000000, -5.874999997268811391, 0.000000000000000000 ) ) ;
#39229 = CARTESIAN_POINT ( 'NONE',  ( -53.33387254593733928, -149.9375000027312126, 5.149110718188519620 ) ) ;
#39230 = CARTESIAN_POINT ( 'NONE',  ( 5.000000000000000000, -29.37499999726881228, -6.123233995736766282E-16 ) ) ;
#39231 = VERTEX_POINT ( 'NONE', #49972 ) ;
#39232 = CARTESIAN_POINT ( 'NONE',  ( -4.458734124999999437, 0.6875000013655957476, 0.000000000000000000 ) ) ;
#39233 = CARTESIAN_POINT ( 'NONE',  ( 1.339745962155615144, -78.70534180126148271, 4.999999999999999112 ) ) ;
#39234 = CARTESIAN_POINT ( 'NONE',  ( 4.458734124999998549, -14.97916666530107221, -2.574251347313721627 ) ) ;
#39235 = CARTESIAN_POINT ( 'NONE',  ( -2.229367062500000163, -2.479166665301069106, -3.861377020970580443 ) ) ;
#39236 = LINE ( 'NONE', #10609, #30565 ) ;
#39237 = CARTESIAN_POINT ( 'NONE',  ( -4.458734125000000326, -153.8750000013655779, 1.846868145590734089 ) ) ;
#39238 = CARTESIAN_POINT ( 'NONE',  ( -4.458734124999999437, 21.43750000136559208, 0.000000000000000000 ) ) ;
#39239 = VERTEX_POINT ( 'NONE', #29071 ) ;
#39240 = CARTESIAN_POINT ( 'NONE',  ( -4.458734124999999437, -99.39583333196772230, -2.574251347313719407 ) ) ;
#39241 = DIRECTION ( 'NONE',  ( -0.000000000000000000, 1.000000000000000000, -0.000000000000000000 ) ) ;
#39242 = CARTESIAN_POINT ( 'NONE',  ( 5.000000000000000000, -12.29166666393547835, -2.886751345948130876 ) ) ;
#39243 = CARTESIAN_POINT ( 'NONE',  ( -3.152548672688508926E-16, -13.56249999863440259, -5.148502694627439702 ) ) ;
#39244 = CARTESIAN_POINT ( 'NONE',  ( 1.975475456537005874E-15, -39.62499999726880162, 5.000000000000000000 ) ) ;
#39245 = CARTESIAN_POINT ( 'NONE',  ( 5.000000000000000000, 29.50000000000000000, -6.123233995736766282E-16 ) ) ;
#39246 = CARTESIAN_POINT ( 'NONE',  ( -55.35523342533222291, -154.3125000013656347, 4.444560631937231499 ) ) ;
#39247 = CARTESIAN_POINT ( 'NONE',  ( -5.000000000000000000, -39.87499999726880162, 0.000000000000000000 ) ) ;
#39248 = CARTESIAN_POINT ( 'NONE',  ( 2.499999999999998668, -67.20833333060214443, -4.330127018922193649 ) ) ;
#39249 = CARTESIAN_POINT ( 'NONE',  ( -2.229367062500000163, 12.52083333469892601, -3.861377020970580443 ) ) ;
#39250 = CARTESIAN_POINT ( 'NONE',  ( -6.972266317189433020E-16, -95.25000000000000000, -5.000000000000000000 ) ) ;
#39251 = VERTEX_POINT ( 'NONE', #20396 ) ;
#39252 = CARTESIAN_POINT ( 'NONE',  ( 4.458734124999998549, 16.27083333469892779, -2.574251347313721627 ) ) ;
#39253 = CARTESIAN_POINT ( 'NONE',  ( -2.229367062500000163, -59.47916666530106511, -3.861377020970580443 ) ) ;
#39254 = VERTEX_POINT ( 'NONE', #44186 ) ;
#39255 = CARTESIAN_POINT ( 'NONE',  ( -2.229367062500000163, -10.72916666530106866, -3.861377020970580443 ) ) ;
#39256 = SURFACE_SIDE_STYLE ('',( #11516 ) ) ;
#39257 = CARTESIAN_POINT ( 'NONE',  ( 5.000000000000000888, 6.416666666666666963, 2.886751345948126879 ) ) ;
#39258 = CARTESIAN_POINT ( 'NONE',  ( -4.458734124999999437, -167.9375000013655779, -5.460374474430324690E-16 ) ) ;
#39259 = CARTESIAN_POINT ( 'NONE',  ( 5.000000000000000888, -88.58333333333332860, 2.886751345948126879 ) ) ;
#39260 = CARTESIAN_POINT ( 'NONE',  ( 4.458734124999999437, -51.81249999863440792, -5.460374474430324690E-16 ) ) ;
#39261 = CARTESIAN_POINT ( 'NONE',  ( 5.000000000000000000, -87.37499999726880162, -6.123233995736766282E-16 ) ) ;
#39262 = EDGE_CURVE ( 'NONE', #17113, #49521, #58990, .T. ) ;
#39263 = CARTESIAN_POINT ( 'NONE',  ( -2.229367062499996610, -32.14583333196773651, 3.861377020970582219 ) ) ;
#39264 = FACE_OUTER_BOUND ( 'NONE', #58942, .T. ) ;
#39265 = DIRECTION ( 'NONE',  ( 0.000000000000000000, 1.000000000000000000, 0.000000000000000000 ) ) ;
#39266 = CARTESIAN_POINT ( 'NONE',  ( 3.152801135295366208, -151.8125000013655779, 3.152801135295367985 ) ) ;
#39267 = CARTESIAN_POINT ( 'NONE',  ( -3.535250795749689387E-16, -40.24999999999998579, -5.773502691896257311 ) ) ;
#39268 = CARTESIAN_POINT ( 'NONE',  ( 2.500000000000002220, -46.66666666666666430, 4.330127018922192761 ) ) ;
#39269 = CARTESIAN_POINT ( 'NONE',  ( 6.123233995736766282E-16, -120.0000000000000000, -5.000000000000000000 ) ) ;
#39270 = VERTEX_POINT ( 'NONE', #39995 ) ;
#39271 = CARTESIAN_POINT ( 'NONE',  ( -4.458734124999998549, -99.22916666530105090, 2.574251347313722516 ) ) ;
#39272 = CARTESIAN_POINT ( 'NONE',  ( -4.458734124999998549, 0.5208333346989265644, 2.574251347313722516 ) ) ;
#39273 =( BOUNDED_CURVE ( )  B_SPLINE_CURVE ( 2, ( #17830, #6681, #26288, #8189, #3681, #23295, #40758, #27791, #35952 ),
 .UNSPECIFIED., .F., .F. ) 
 B_SPLINE_CURVE_WITH_KNOTS ( ( 3, 2, 2, 2, 3 ),
 ( 0.8854166666666666297, 0.8861111111111110716, 0.8874999999999999556, 0.8888888888888888395, 0.8895833333333332815 ),
 .UNSPECIFIED. ) 
 CURVE ( )  GEOMETRIC_REPRESENTATION_ITEM ( )  RATIONAL_B_SPLINE_CURVE ( ( 0.9330127018922194093, 0.9330127018922194093, 1.000000000000000000, 0.8660254037844387076, 1.000000000000000000, 0.8660254037844387076, 1.000000000000000000, 0.9330127018922194093, 0.9330127018922194093 ) ) 
 REPRESENTATION_ITEM ( '' )  );
#39274 = DIRECTION ( 'NONE',  ( -0.000000000000000000, 1.000000000000000000, -0.000000000000000000 ) ) ;
#39275 = CARTESIAN_POINT ( 'NONE',  ( 5.000000000000000000, -0.5000000000000004441, -6.123233995736766282E-16 ) ) ;
#39276 = ADVANCED_FACE ( 'NONE', ( #20070 ), #58364, .T. ) ;
#39277 = CARTESIAN_POINT ( 'NONE',  ( 2.229367062500001939, -68.97916666530107932, 3.861377020970579999 ) ) ;
#39278 = LINE ( 'NONE', #34447, #39009 ) ;
#39279 = CARTESIAN_POINT ( 'NONE',  ( -3.535250795749689387E-16, -0.1249999972688133065, -5.773502691896257311 ) ) ;
#39281 = ORIENTED_EDGE ( 'NONE', *, *, #10240, .T. ) ;
#39280 = CARTESIAN_POINT ( 'NONE',  ( 2.229367062499998831, -31.64583333196773651, -3.861377020970580887 ) ) ;
#39282 = CARTESIAN_POINT ( 'NONE',  ( 1.975475456537005874E-15, -10.75000000000000000, 5.000000000000000000 ) ) ;
#39283 = FACE_OUTER_BOUND ( 'NONE', #54819, .T. ) ;
#39284 = EDGE_CURVE ( 'NONE', #19571, #6165, #25702, .T. ) ;
#39285 = DIRECTION ( 'NONE',  ( -0.000000000000000000, 1.000000000000000000, -0.000000000000000000 ) ) ;
#39286 = CARTESIAN_POINT ( 'NONE',  ( 5.000000000000000000, -43.50000000000000000, -6.123233995736766282E-16 ) ) ;
#39288 = CARTESIAN_POINT ( 'NONE',  ( -4.458734124999998549, -24.47916666530107577, 2.574251347313722516 ) ) ;
#39287 = DIRECTION ( 'NONE',  ( -0.000000000000000000, 1.000000000000000000, -0.000000000000000000 ) ) ;
#39289 = CARTESIAN_POINT ( 'NONE',  ( -1.336351044127974539E-14, 22.37500000273118417, 5.000000000000000000 ) ) ;
#39290 = CARTESIAN_POINT ( 'NONE',  ( 2.229367062500001939, -71.97916666530107932, 3.861377020970579999 ) ) ;
#39291 = CARTESIAN_POINT ( 'NONE',  ( 2.730187237215162345E-16, -143.4375000013656063, -4.458734124999999437 ) ) ;
#39292 = CARTESIAN_POINT ( 'NONE',  ( 4.458734124999998549, -80.72916666530106511, -2.574251347313721627 ) ) ;
#39293 = CARTESIAN_POINT ( 'NONE',  ( -59.59170313451811296, -137.7500000013656063, 1.485763867205729394 ) ) ;
#39294 = CARTESIAN_POINT ( 'NONE',  ( 2.229367062500001939, -29.22916666530107221, 3.861377020970579999 ) ) ;
#39295 = CARTESIAN_POINT ( 'NONE',  ( 1.060575238724906964E-15, -73.62499999726881583, 5.773502691896257311 ) ) ;
#39296 = ORIENTED_EDGE ( 'NONE', *, *, #60597, .T. ) ;
#39297 = CARTESIAN_POINT ( 'NONE',  ( 0.000000000000000000, 15.00000000000000000, -11.00000000000000000 ) ) ;
#39298 = ORIENTED_EDGE ( 'NONE', *, *, #767, .F. ) ;
#39299 = CARTESIAN_POINT ( 'NONE',  ( 4.458734124999998549, -73.97916666530106511, -2.574251347313721627 ) ) ;
#39300 = CARTESIAN_POINT ( 'NONE',  ( -1.127183054612291972E-14, 22.37500000273118417, 4.999999999999999112 ) ) ;
#39301 = ORIENTED_EDGE ( 'NONE', *, *, #57129, .F. ) ;
#39302 = CARTESIAN_POINT ( 'NONE',  ( -6.000000000000000000, -114.9999999999999858, -1.500000000000000000 ) ) ;
#39303 =( BOUNDED_CURVE ( )  B_SPLINE_CURVE ( 2, ( #41314, #47417, #7873, #46472, #52250, #21719, #32942, #36497, #51623 ),
 .UNSPECIFIED., .F., .F. ) 
 B_SPLINE_CURVE_WITH_KNOTS ( ( 3, 2, 2, 2, 3 ),
 ( 0.6803571428571428825, 0.6809523809523809756, 0.6821428571428571619, 0.6833333333333333481, 0.6839285714285714413 ),
 .UNSPECIFIED. ) 
 CURVE ( )  GEOMETRIC_REPRESENTATION_ITEM ( )  RATIONAL_B_SPLINE_CURVE ( ( 0.9330127018922194093, 0.9330127018922194093, 1.000000000000000000, 0.8660254037844387076, 1.000000000000000000, 0.8660254037844387076, 1.000000000000000000, 0.9330127018922194093, 0.9330127018922194093 ) ) 
 REPRESENTATION_ITEM ( '' )  );
#39304 = CARTESIAN_POINT ( 'NONE',  ( -53.33387254593719717, -142.9375000027312410, 5.149110718188530278 ) ) ;
#39305 = EDGE_CURVE ( 'NONE', #27512, #42376, #4959, .T. ) ;
#39306 = CARTESIAN_POINT ( 'NONE',  ( -2.229367062499996610, -59.39583333196773651, 3.861377020970582219 ) ) ;
#39307 = CARTESIAN_POINT ( 'NONE',  ( -4.458734124999999437, 2.437500001365593860, 0.000000000000000000 ) ) ;
#39308 = ORIENTED_EDGE ( 'NONE', *, *, #11795, .F. ) ;
#39309 = CARTESIAN_POINT ( 'NONE',  ( 3.535533905932736864, -142.1250000000000000, 3.535533905932738641 ) ) ;
#39310 = CARTESIAN_POINT ( 'NONE',  ( -6.972266317189433020E-16, -108.2499999999999858, -5.000000000000000000 ) ) ;
#39311 = CARTESIAN_POINT ( 'NONE',  ( 4.458734125000001214, 12.10416666803226171, 2.574251347313718519 ) ) ;
#39312 = CARTESIAN_POINT ( 'NONE',  ( -52.10840900171896806, -142.1875000013656063, 3.393966926194110556 ) ) ;
#39313 = CARTESIAN_POINT ( 'NONE',  ( 3.152801135295366208, -164.5625000013656063, 3.152801135295367985 ) ) ;
#39314 = ORIENTED_EDGE ( 'NONE', *, *, #10669, .F. ) ;
#39315 = CARTESIAN_POINT ( 'NONE',  ( -4.458734124999999437, -81.31249999863440792, 0.000000000000000000 ) ) ;
#39316 = CARTESIAN_POINT ( 'NONE',  ( -1.339745962155613812, -52.08034179853028434, -5.000000000000000000 ) ) ;
#39317 = CARTESIAN_POINT ( 'NONE',  ( -4.458734124999999437, 0.6875000013655957476, 0.000000000000000000 ) ) ;
#39318 = CARTESIAN_POINT ( 'NONE',  ( -5.000000000000000000, -86.08333333333334281, -2.886751345948128211 ) ) ;
#39319 = CARTESIAN_POINT ( 'NONE',  ( 0.000000000000000000, -170.0000000000000000, 0.000000000000000000 ) ) ;
#39320 = CARTESIAN_POINT ( 'NONE',  ( -3.152548672688508926E-16, -65.81249999863440792, -5.148502694627439702 ) ) ;
#39321 = CARTESIAN_POINT ( 'NONE',  ( -2.499999999999996447, -23.70833333060214443, 4.330127018922195425 ) ) ;
#39322 = CARTESIAN_POINT ( 'NONE',  ( -50.18089887299977647, -142.8125000027311557, 2.462841084822486426 ) ) ;
#39323 = CARTESIAN_POINT ( 'NONE',  ( -1.339745962155610925, -40.79465819873852439, 5.000000000000000000 ) ) ;
#39324 = FACE_OUTER_BOUND ( 'NONE', #46494, .T. ) ;
#39325 = CARTESIAN_POINT ( 'NONE',  ( 1.339745962155612702, -58.29465819873852439, -5.000000000000000000 ) ) ;
#39326 = CARTESIAN_POINT ( 'NONE',  ( -4.458734124999999437, -48.31249999863440792, 0.000000000000000000 ) ) ;
#39327 = CARTESIAN_POINT ( 'NONE',  ( -4.458734124999997661, -33.47916666530107221, 2.574251347313722516 ) ) ;
#39328 = CARTESIAN_POINT ( 'NONE',  ( -2.229367062499996610, 6.604166668032259935, 3.861377020970582219 ) ) ;
#39329 = CARTESIAN_POINT ( 'NONE',  ( -9.184850993605147944E-16, -146.3750000027312126, 5.000000000000000000 ) ) ;
#39330 = CARTESIAN_POINT ( 'NONE',  ( -4.999999999999999112, 25.08333333333333215, 2.886751345948131764 ) ) ;
#39331 = CARTESIAN_POINT ( 'NONE',  ( -5.000000000000000000, -148.6250000027312126, -6.123233995736766282E-16 ) ) ;
#39332 = CARTESIAN_POINT ( 'NONE',  ( 6.123233995736766282E-16, -170.0000000000000000, -5.000000000000000000 ) ) ;
#39333 = CARTESIAN_POINT ( 'NONE',  ( -4.458734124999999437, -36.39583333196772941, -2.574251347313719407 ) ) ;
#39334 = CARTESIAN_POINT ( 'NONE',  ( 1.060575238724906964E-15, -74.62499999726880162, 5.773502691896257311 ) ) ;
#39335 = CARTESIAN_POINT ( 'NONE',  ( -54.64476657466781973, -142.0625000013656063, -4.444560631937228834 ) ) ;
#39336 = CARTESIAN_POINT ( 'NONE',  ( 5.000000000000000000, -144.0625000000000284, 2.071067811865478614 ) ) ;
#39337 = B_SPLINE_CURVE_WITH_KNOTS ( 'NONE', 3,
 ( #56743, #2705, #37742, #62519, #3030, #41926 ),
 .UNSPECIFIED., .F., .F.,
 ( 4, 2, 4 ),
 ( 0.000000000000000000, 0.002307655110370371299, 0.004615310220740742597 ),
 .UNSPECIFIED. ) ;
#39338 = EDGE_CURVE ( 'NONE', #23654, #29728, #34704, .T. ) ;
#39339 = CARTESIAN_POINT ( 'NONE',  ( 5.000000000000000000, -37.50000000000000711, -6.123233995736766282E-16 ) ) ;
#39340 = EDGE_CURVE ( 'NONE', #47522, #42641, #39045, .T. ) ;
#39341 = CARTESIAN_POINT ( 'NONE',  ( -2.229367062499996610, -75.39583333196773651, 3.861377020970582219 ) ) ;
#39342 = CARTESIAN_POINT ( 'NONE',  ( 1.846868145590735200, -164.5000000013655779, -4.458734124999999437 ) ) ;
#39343 = CARTESIAN_POINT ( 'NONE',  ( 9.457646018065525792E-16, -35.06249999863440792, 5.148502694627439702 ) ) ;
#39344 = EDGE_CURVE ( 'NONE', #1507, #48710, #46266, .T. ) ;
#39345 = CARTESIAN_POINT ( 'NONE',  ( 3.061616997868383141E-16, -160.7500000000000000, -5.000000000000000000 ) ) ;
#39346 = CARTESIAN_POINT ( 'NONE',  ( -6.972266317189433020E-16, 7.750000000000000000, -5.000000000000000000 ) ) ;
#39347 = CARTESIAN_POINT ( 'NONE',  ( 2.500000000000002220, -21.66666666666666785, 4.330127018922192761 ) ) ;
#39348 = CARTESIAN_POINT ( 'NONE',  ( 2.730187237215162345E-16, -142.1875000013656063, -4.458734124999999437 ) ) ;
#39349 = ORIENTED_EDGE ( 'NONE', *, *, #28053, .T. ) ;
#39350 = CARTESIAN_POINT ( 'NONE',  ( -4.458734124999999437, 28.43750000136559208, 0.000000000000000000 ) ) ;
#39351 = ORIENTED_EDGE ( 'NONE', *, *, #58568, .F. ) ;
#39352 = CARTESIAN_POINT ( 'NONE',  ( 4.458734124999998549, -61.97916666530106511, -2.574251347313721627 ) ) ;
#39353 = CARTESIAN_POINT ( 'NONE',  ( -2.499999999999996447, 24.29166666939785202, 4.330127018922195425 ) ) ;
#39354 = CARTESIAN_POINT ( 'NONE',  ( 5.000000000000000888, 16.41666666666666785, 2.886751345948126879 ) ) ;
#39355 = EDGE_CURVE ( 'NONE', #50310, #9796, #56899, .T. ) ;
#39356 = CARTESIAN_POINT ( 'NONE',  ( 4.458734125000000326, -52.89583333196772941, 2.574251347313718519 ) ) ;
#39357 = CARTESIAN_POINT ( 'NONE',  ( 4.458734124999998549, -6.729166665301073103, -2.574251347313721627 ) ) ;
#39358 = CARTESIAN_POINT ( 'NONE',  ( -2.499999999999996447, 4.166666666666666075, 4.330127018922195425 ) ) ;
#39359 = EDGE_CURVE ( 'NONE', #733, #22693, #1483, .T. ) ;
#39360 = CARTESIAN_POINT ( 'NONE',  ( 2.493747252781420335E-13, -56.12499999726880873, -5.000000000000000000 ) ) ;
#39362 = CARTESIAN_POINT ( 'NONE',  ( 9.457646018065525792E-16, -20.06249999863440081, 5.148502694627439702 ) ) ;
#39361 = CARTESIAN_POINT ( 'NONE',  ( 5.000000000000000000, 0.5000000000000004441, -6.123233995736766282E-16 ) ) ;
#39363 = DIRECTION ( 'NONE',  ( 0.000000000000000000, 1.000000000000000000, 0.000000000000000000 ) ) ;
#39364 = CARTESIAN_POINT ( 'NONE',  ( -4.458734124999999437, -53.39583333196773651, -2.574251347313719407 ) ) ;
#39365 = CARTESIAN_POINT ( 'NONE',  ( -1.846868145590734756, -156.3750000013655779, -4.458734125000000326 ) ) ;
#39366 = EDGE_CURVE ( 'NONE', #40791, #7933, #12918, .T. ) ;
#39367 = CARTESIAN_POINT ( 'NONE',  ( 5.000000000000000000, -54.29166666393549434, -2.886751345948129988 ) ) ;
#39368 = ORIENTED_EDGE ( 'NONE', *, *, #53512, .F. ) ;
#39369 = CARTESIAN_POINT ( 'NONE',  ( 3.061616997868383141E-16, -142.7500000000000284, -5.000000000000000000 ) ) ;
#39370 = CARTESIAN_POINT ( 'NONE',  ( 4.458734125000001214, 6.854166668032259935, 2.574251347313718519 ) ) ;
#39371 = EDGE_LOOP ( 'NONE', ( #18770, #57863, #53797, #47167 ) ) ;
#39373 = CARTESIAN_POINT ( 'NONE',  ( -5.000000000000000000, -67.95833333060214443, -2.886751345948128211 ) ) ;
#39372 = CARTESIAN_POINT ( 'NONE',  ( -6.972266317189433020E-16, -56.25000000000000000, -5.000000000000000000 ) ) ;
#39374 = CARTESIAN_POINT ( 'NONE',  ( 3.152801135295367541, -155.3125000013656063, -3.152801135295367541 ) ) ;
#39375 = ORIENTED_EDGE ( 'NONE', *, *, #53840, .F. ) ;
#39376 = CARTESIAN_POINT ( 'NONE',  ( -6.972266317189433020E-16, 10.75000000000000000, -5.000000000000000000 ) ) ;
#39377 = CARTESIAN_POINT ( 'NONE',  ( -58.80597590150559739, -133.0000000000000284, 3.242614290531460330 ) ) ;
#39378 = CARTESIAN_POINT ( 'NONE',  ( -2.499999999999996447, -58.70833333060214443, 4.330127018922195425 ) ) ;
#39379 = CARTESIAN_POINT ( 'NONE',  ( -4.458734124999999437, -42.56249999863440081, 0.000000000000000000 ) ) ;
#39380 = VERTEX_POINT ( 'NONE', #55452 ) ;
#39381 = AXIS2_PLACEMENT_3D ( 'NONE', #32125, #26356, #36330 ) ;
#39382 = CARTESIAN_POINT ( 'NONE',  ( -4.458734124999999437, 17.60416666803225993, -2.574251347313719407 ) ) ;
#39383 = CARTESIAN_POINT ( 'NONE',  ( -5.000000000000000000, -85.08333333333332860, -2.886751345948128211 ) ) ;
#39384 = ORIENTED_EDGE ( 'NONE', *, *, #58518, .F. ) ;
#39385 = CARTESIAN_POINT ( 'NONE',  ( -4.458734124999999437, -89.64583333196773651, -2.574251347313719407 ) ) ;
#39386 = CARTESIAN_POINT ( 'NONE',  ( -58.80597590150559739, -125.1250000027312126, 3.242614290531460330 ) ) ;
#39387 = CARTESIAN_POINT ( 'NONE',  ( 6.324555320336756381, 15.00000000000000000, -9.000000000000001776 ) ) ;
#39388 = CARTESIAN_POINT ( 'NONE',  ( -5.000000000000000000, -7.083333333333330373, -2.886751345948128211 ) ) ;
#39389 = CARTESIAN_POINT ( 'NONE',  ( 5.000000000000000888, -52.45833333060213732, 2.886751345948126879 ) ) ;
#39390 = CARTESIAN_POINT ( 'NONE',  ( 2.229367062500001939, -59.97916666530106511, 3.861377020970579999 ) ) ;
#39391 = CARTESIAN_POINT ( 'NONE',  ( 4.458734124999998549, 20.27083333469892779, -2.574251347313721627 ) ) ;
#39392 =( BOUNDED_CURVE ( )  B_SPLINE_CURVE ( 2, ( #42199, #23540, #28349, #38324, #53117, #8434, #28662, #9360, #47966 ),
 .UNSPECIFIED., .F., .F. ) 
 B_SPLINE_CURVE_WITH_KNOTS ( ( 3, 2, 2, 2, 3 ),
 ( 0.7729166666666666963, 0.7736111111111111382, 0.7750000000000000222, 0.7763888888888889062, 0.7770833333333333481 ),
 .UNSPECIFIED. ) 
 CURVE ( )  GEOMETRIC_REPRESENTATION_ITEM ( )  RATIONAL_B_SPLINE_CURVE ( ( 0.9330127018922194093, 0.9330127018922194093, 1.000000000000000000, 0.8660254037844387076, 1.000000000000000000, 0.8660254037844387076, 1.000000000000000000, 0.9330127018922194093, 0.9330127018922194093 ) ) 
 REPRESENTATION_ITEM ( '' )  );
#39393 = DIRECTION ( 'NONE',  ( 0.000000000000000000, 0.000000000000000000, 1.000000000000000000 ) ) ;
#39394 = CARTESIAN_POINT ( 'NONE',  ( -2.229367062499996610, -48.39583333196772941, 3.861377020970582219 ) ) ;
#39395 = CARTESIAN_POINT ( 'NONE',  ( -4.999999999999999112, -7.791666663935482795, 2.886751345948131764 ) ) ;
#39396 = CARTESIAN_POINT ( 'NONE',  ( -1.339745962155610925, -66.66965819600733312, 5.000000000000000000 ) ) ;
#39397 = FACE_OUTER_BOUND ( 'NONE', #57530, .T. ) ;
#39398 = CARTESIAN_POINT ( 'NONE',  ( 4.458734124999998549, -106.7291666653010509, -2.574251347313721627 ) ) ;
#39399 = CARTESIAN_POINT ( 'NONE',  ( 9.457646018065525792E-16, -9.312499998634406140, 5.148502694627439702 ) ) ;
#39400 = VERTEX_POINT ( 'NONE', #11683 ) ;
#39401 = CARTESIAN_POINT ( 'NONE',  ( 1.975475456537005874E-15, -46.62499999726880873, 5.000000000000000000 ) ) ;
#39402 = CARTESIAN_POINT ( 'NONE',  ( 4.458734124999998549, -96.72916666530105090, -2.574251347313721627 ) ) ;
#39403 = CARTESIAN_POINT ( 'NONE',  ( -5.000000000000000888, -162.5625000027312126, 2.071067811865474617 ) ) ;
#39404 = CARTESIAN_POINT ( 'NONE',  ( 4.458734124999998549, -99.97916666530106511, -2.574251347313721627 ) ) ;
#39405 = CARTESIAN_POINT ( 'NONE',  ( -5.000000000000000000, -8.083333333333332149, -2.886751345948128211 ) ) ;
#39406 = CARTESIAN_POINT ( 'NONE',  ( -3.535250795749689387E-16, -59.12499999726880873, -5.773502691896257311 ) ) ;
#39407 = CYLINDRICAL_SURFACE ( 'NONE', #20209, 5.000000000000000000 ) ;
#39408 = CARTESIAN_POINT ( 'NONE',  ( -58.39396692619412477, -154.6875000013656063, 2.891590998281057701 ) ) ;
#39409 = CARTESIAN_POINT ( 'NONE',  ( -51.60603307380591787, -147.9375000013656063, -2.891590998281053704 ) ) ;
#39410 = ADVANCED_FACE ( 'NONE', ( #41266 ), #6556, .T. ) ;
#39411 = CARTESIAN_POINT ( 'NONE',  ( 4.458734124999998549, -15.72916666530107399, -2.574251347313721627 ) ) ;
#39412 = CARTESIAN_POINT ( 'NONE',  ( -3.152548672688508926E-16, 8.187500001365595637, -5.148502694627439702 ) ) ;
#39413 = CARTESIAN_POINT ( 'NONE',  ( 9.457646018065525792E-16, -58.31249999863440792, 5.148502694627439702 ) ) ;
#39414 = CARTESIAN_POINT ( 'NONE',  ( 2.493747252781420335E-13, -56.12499999726880873, -5.000000000000000000 ) ) ;
#39415 = CARTESIAN_POINT ( 'NONE',  ( -3.152548672688508926E-16, -16.56249999863440436, -5.148502694627439702 ) ) ;
#39416 = CARTESIAN_POINT ( 'NONE',  ( 2.499999999999998668, -8.208333330602144429, -4.330127018922193649 ) ) ;
#39417 = CARTESIAN_POINT ( 'NONE',  ( 5.000000000000000888, -153.9375000000000000, -2.071067811865475505 ) ) ;
#39418 = CARTESIAN_POINT ( 'NONE',  ( 5.000000000000000000, -6.499999999999999112, -6.123233995736766282E-16 ) ) ;
#39419 = ORIENTED_EDGE ( 'NONE', *, *, #59779, .T. ) ;
#39420 = CARTESIAN_POINT ( 'NONE',  ( -2.229367062500000163, -48.72916666530106511, -3.861377020970580443 ) ) ;
#39421 = CARTESIAN_POINT ( 'NONE',  ( -6.972266317189433020E-16, -38.25000000000000000, -5.000000000000000000 ) ) ;
#39422 = DIRECTION ( 'NONE',  ( 0.000000000000000000, 0.000000000000000000, 1.000000000000000000 ) ) ;
#39423 = CARTESIAN_POINT ( 'NONE',  ( 4.458734125000001214, -84.89583333196773651, 2.574251347313718519 ) ) ;
#39424 = CARTESIAN_POINT ( 'NONE',  ( 2.229367062499998831, 21.10416666803226349, -3.861377020970580887 ) ) ;
#39425 = AXIS2_PLACEMENT_3D ( 'NONE', #13228, #43119, #18679 ) ;
#39426 = CARTESIAN_POINT ( 'NONE',  ( -2.229367062500000163, 10.52083333469892779, -3.861377020970580443 ) ) ;
#39427 = CARTESIAN_POINT ( 'NONE',  ( -5.000000000000000000, -88.95833333060214443, -2.886751345948128211 ) ) ;
#39428 = CARTESIAN_POINT ( 'NONE',  ( 5.000000000000000888, -37.45833333060213732, 2.886751345948126879 ) ) ;
#39429 = DIRECTION ( 'NONE',  ( 0.000000000000000000, 0.000000000000000000, -1.000000000000000000 ) ) ;
#39430 = CARTESIAN_POINT ( 'NONE',  ( -3.152548672688508926E-16, 20.18750000136559208, -5.148502694627439702 ) ) ;
#39431 = CARTESIAN_POINT ( 'NONE',  ( 5.000000000000000000, -73.41666666666665719, -2.886751345948129988 ) ) ;
#39432 = CARTESIAN_POINT ( 'NONE',  ( 2.500000000000002220, 8.458333336064518093, 4.330127018922192761 ) ) ;
#39434 = EDGE_LOOP ( 'NONE', ( #3485, #29968, #47128, #54652 ) ) ;
#39433 = EDGE_CURVE ( 'NONE', #42937, #21194, #41650, .T. ) ;
#39435 = CARTESIAN_POINT ( 'NONE',  ( 1.975475456537005874E-15, -96.62499999726880162, 5.000000000000000000 ) ) ;
#39436 = ADVANCED_FACE ( 'NONE', ( #50296 ), #50938, .T. ) ;
#39437 = ORIENTED_EDGE ( 'NONE', *, *, #40150, .T. ) ;
#39439 = CARTESIAN_POINT ( 'NONE',  ( -3.535250795749689387E-16, -32.25000000000000000, -5.773502691896257311 ) ) ;
#39438 = CARTESIAN_POINT ( 'NONE',  ( 1.975475456537005874E-15, -103.7500000000000000, 5.000000000000000000 ) ) ;
#39440 = CARTESIAN_POINT ( 'NONE',  ( -4.458734124999999437, -40.31249999863440081, 0.000000000000000000 ) ) ;
#39441 = EDGE_CURVE ( 'NONE', #1762, #3107, #37175, .T. ) ;
#39442 = EDGE_CURVE ( 'NONE', #28553, #40991, #3912, .T. ) ;
#39443 = CARTESIAN_POINT ( 'NONE',  ( 5.000000000000000888, -34.45833333060213732, 2.886751345948126879 ) ) ;
#39445 = VERTEX_POINT ( 'NONE', #61552 ) ;
#39444 = CARTESIAN_POINT ( 'NONE',  ( -4.458734124999999437, -66.31249999863440792, 0.000000000000000000 ) ) ;
#39446 = CARTESIAN_POINT ( 'NONE',  ( -52.10840900171896806, -151.4375000013656063, 3.393966926194110556 ) ) ;
#39447 = CARTESIAN_POINT ( 'NONE',  ( -4.458734124999998549, -11.22916666530106866, 2.574251347313722516 ) ) ;
#39449 = ORIENTED_EDGE ( 'NONE', *, *, #2521, .T. ) ;
#39448 = CARTESIAN_POINT ( 'NONE',  ( -3.152548672688508926E-16, -12.81249999863440259, -5.148502694627439702 ) ) ;
#39450 =( BOUNDED_CURVE ( )  B_SPLINE_CURVE ( 2, ( #17960, #61100, #55951, #2878, #56590, #22809, #32443, #31810, #51445 ),
 .UNSPECIFIED., .F., .F. ) 
 B_SPLINE_CURVE_WITH_KNOTS ( ( 3, 2, 2, 2, 3 ),
 ( 0.6916666666666663188, 0.6958333333333329707, 0.6999999999999995115, 0.7041666666666662744, 0.7083333333333329263 ),
 .UNSPECIFIED. ) 
 CURVE ( )  GEOMETRIC_REPRESENTATION_ITEM ( )  RATIONAL_B_SPLINE_CURVE ( ( 1.000000000000005995, 0.9238795325112806323, 1.000000000000000000, 0.9238795325112867385, 1.000000000000000000, 0.9238795325112867385, 1.000000000000000000, 0.9238795325112948431, 0.9999999999999918954 ) ) 
 REPRESENTATION_ITEM ( '' )  );
#39451 = CARTESIAN_POINT ( 'NONE',  ( -3.535250795749689387E-16, -82.25000000000000000, -5.773502691896257311 ) ) ;
#39452 = CARTESIAN_POINT ( 'NONE',  ( -1.339745962155613812, 0.9196582014697067819, -5.000000000000000000 ) ) ;
#39453 = CARTESIAN_POINT ( 'NONE',  ( -4.458734124999998549, -56.47916666530107221, 2.574251347313722516 ) ) ;
#39454 =( BOUNDED_CURVE ( )  B_SPLINE_CURVE ( 2, ( #40546, #41489, #16107, #11274, #61141, #36362, #23076, #36050, #31213 ),
 .UNSPECIFIED., .F., .F. ) 
 B_SPLINE_CURVE_WITH_KNOTS ( ( 3, 2, 2, 2, 3 ),
 ( 0.7125000000000000222, 0.7130952380952381153, 0.7142857142857143016, 0.7154761904761904878, 0.7160714285714285809 ),
 .UNSPECIFIED. ) 
 CURVE ( )  GEOMETRIC_REPRESENTATION_ITEM ( )  RATIONAL_B_SPLINE_CURVE ( ( 0.9330127018922194093, 0.9330127018922194093, 1.000000000000000000, 0.8660254037844387076, 1.000000000000000000, 0.8660254037844387076, 1.000000000000000000, 0.9330127018922194093, 0.9330127018922194093 ) ) 
 REPRESENTATION_ITEM ( '' )  );
#39455 = CARTESIAN_POINT ( 'NONE',  ( 2.499999999999998668, -82.20833333060214443, -4.330127018922193649 ) ) ;
#39457 = ORIENTED_EDGE ( 'NONE', *, *, #59143, .F. ) ;
#39456 = CARTESIAN_POINT ( 'NONE',  ( 6.123233995736766282E-16, -170.0000000000000000, -5.000000000000000000 ) ) ;
#39458 = CARTESIAN_POINT ( 'NONE',  ( -59.98410592259440222, -144.1250000000000284, -0.3983568153799752487 ) ) ;
#39459 = CARTESIAN_POINT ( 'NONE',  ( 4.458734124999998549, -28.97916666530107577, -2.574251347313721627 ) ) ;
#39460 = FACE_BOUND ( 'NONE', #6961, .T. ) ;
#39461 = EDGE_LOOP ( 'NONE', ( #37567, #43809, #51360, #45950 ) ) ;
#39462 = CARTESIAN_POINT ( 'NONE',  ( 2.730187237215162345E-16, -164.4375000013655779, -4.458734124999999437 ) ) ;
#39463 = CARTESIAN_POINT ( 'NONE',  ( -2.229367062500000163, -105.7291666653010651, -3.861377020970580443 ) ) ;
#39464 = CARTESIAN_POINT ( 'NONE',  ( 2.071067811865349828, -148.1874999999999716, 5.000000000000126121 ) ) ;
#39465 = ORIENTED_EDGE ( 'NONE', *, *, #51869, .F. ) ;
#39466 = CARTESIAN_POINT ( 'NONE',  ( -50.55543936806279248, -147.3125000013656063, 0.3552334253322060320 ) ) ;
#39467 = CARTESIAN_POINT ( 'NONE',  ( -58.80597590150559739, -139.1250000027312410, 3.242614290531460330 ) ) ;
#39468 = CARTESIAN_POINT ( 'NONE',  ( -3.152548672688508926E-16, -43.56249999863439371, -5.148502694627439702 ) ) ;
#39469 = CARTESIAN_POINT ( 'NONE',  ( 3.152801135295366208, -145.8125000013655779, 3.152801135295367985 ) ) ;
#39470 = DIRECTION ( 'NONE',  ( -0.000000000000000000, 1.000000000000000000, -0.000000000000000000 ) ) ;
#39471 = CARTESIAN_POINT ( 'NONE',  ( -2.500000000000000444, -71.16666666666667140, -4.330127018922193649 ) ) ;
#39472 = CARTESIAN_POINT ( 'NONE',  ( -4.458734124999999437, -12.39583333196774184, -2.574251347313719407 ) ) ;
#39473 = CARTESIAN_POINT ( 'NONE',  ( 5.000000000000000000, -101.5000000000000000, -6.123233995736766282E-16 ) ) ;
#39474 = ORIENTED_EDGE ( 'NONE', *, *, #14144, .T. ) ;
#39475 = VECTOR ( 'NONE', #6893, 1000.000000000000000 ) ;
#39476 = CARTESIAN_POINT ( 'NONE',  ( 3.152801135295366208, -139.8125000013655779, 3.152801135295367985 ) ) ;
#39477 = CARTESIAN_POINT ( 'NONE',  ( -4.458734124999999437, -34.56249999863440792, 0.000000000000000000 ) ) ;
#39478 = CARTESIAN_POINT ( 'NONE',  ( 2.500000000000002220, 8.458333336064518093, 4.330127018922192761 ) ) ;
#39479 = CARTESIAN_POINT ( 'NONE',  ( 0.000000000000000000, -170.0000000000000000, 0.000000000000000000 ) ) ;
#39480 = CARTESIAN_POINT ( 'NONE',  ( -52.80376928212989185, -134.8750000013656063, -4.297418129356379346 ) ) ;
#39481 = CARTESIAN_POINT ( 'NONE',  ( -4.458734124999998549, -72.47916666530107932, 2.574251347313722516 ) ) ;
#39482 = CARTESIAN_POINT ( 'NONE',  ( -57.46284108482265651, -146.0625000027312126, 4.819101127000238627 ) ) ;
#39483 = CARTESIAN_POINT ( 'NONE',  ( -4.999999999999998224, -69.91666666666667140, 2.886751345948131764 ) ) ;
#39484 = DIRECTION ( 'NONE',  ( 1.000000000000000000, 0.000000000000000000, -3.614007241618347908E-17 ) ) ;
#39485 = CARTESIAN_POINT ( 'NONE',  ( 4.458734124999998549, 5.020833334698926897, -2.574251347313721627 ) ) ;
#39486 = ORIENTED_EDGE ( 'NONE', *, *, #20596, .T. ) ;
#39487 = CARTESIAN_POINT ( 'NONE',  ( -1.339745962155613812, -71.08034179853027013, -5.000000000000000000 ) ) ;
#39488 = CARTESIAN_POINT ( 'NONE',  ( -5.000000000000000000, -76.08333333333334281, -2.886751345948128211 ) ) ;
#39490 = CARTESIAN_POINT ( 'NONE',  ( -4.458734124999999437, -29.39583333196773296, -2.574251347313719407 ) ) ;
#39489 = CARTESIAN_POINT ( 'NONE',  ( -3.535250795749689387E-16, -96.25000000000000000, -5.773502691896257311 ) ) ;
#39491 = CARTESIAN_POINT ( 'NONE',  ( 0.000000000000000000, -120.0000000000000000, 0.000000000000000000 ) ) ;
#39492 = CARTESIAN_POINT ( 'NONE',  ( -3.152548672688508926E-16, -81.81249999863440792, -5.148502694627439702 ) ) ;
#39493 = CARTESIAN_POINT ( 'NONE',  ( 4.458734124999998549, 16.02083333469892779, -2.574251347313721627 ) ) ;
#39494 = DIRECTION ( 'NONE',  ( 0.000000000000000000, 0.000000000000000000, 1.000000000000000000 ) ) ;
#39495 = CARTESIAN_POINT ( 'NONE',  ( -50.55543936806279248, -138.0625000013656063, 0.3552334253322060320 ) ) ;
#39496 = CARTESIAN_POINT ( 'NONE',  ( 2.229367062500001939, -1.979166665301068662, 3.861377020970579999 ) ) ;
#39497 = CARTESIAN_POINT ( 'NONE',  ( -2.229367062500000163, 23.27083333469892779, -3.861377020970580443 ) ) ;
#39498 = CARTESIAN_POINT ( 'NONE',  ( -2.229367062499996610, -43.39583333196773651, 3.861377020970582219 ) ) ;
#39499 = CARTESIAN_POINT ( 'NONE',  ( -1.339745962155610925, -50.66965819600732601, 5.000000000000000000 ) ) ;
#39500 = CARTESIAN_POINT ( 'NONE',  ( -4.458734124999999437, -0.3958333319677397322, -2.574251347313719407 ) ) ;
#39501 = ORIENTED_EDGE ( 'NONE', *, *, #54619, .T. ) ;
#39502 = CARTESIAN_POINT ( 'NONE',  ( 4.458734124999999437, -26.06249999863440792, -5.460374474430324690E-16 ) ) ;
#39503 =( BOUNDED_CURVE ( )  B_SPLINE_CURVE ( 2, ( #26695, #3210, #47265, #56610, #46628, #17678, #21873, #12527, #22830 ),
 .UNSPECIFIED., .F., .F. ) 
 B_SPLINE_CURVE_WITH_KNOTS ( ( 3, 2, 2, 2, 3 ),
 ( 0.5839285714285714635, 0.5845238095238095566, 0.5857142857142857428, 0.5869047619047619291, 0.5875000000000000222 ),
 .UNSPECIFIED. ) 
 CURVE ( )  GEOMETRIC_REPRESENTATION_ITEM ( )  RATIONAL_B_SPLINE_CURVE ( ( 0.9330127018922194093, 0.9330127018922194093, 1.000000000000000000, 0.8660254037844387076, 1.000000000000000000, 0.8660254037844387076, 1.000000000000000000, 0.9330127018922194093, 0.9330127018922194093 ) ) 
 REPRESENTATION_ITEM ( '' )  );
#39504 = CARTESIAN_POINT ( 'NONE',  ( -4.458734124999999437, -67.39583333196773651, -2.574251347313719407 ) ) ;
#39505 = CARTESIAN_POINT ( 'NONE',  ( 2.499999999999998668, -106.2083333306021444, -4.330127018922193649 ) ) ;
#39506 = CARTESIAN_POINT ( 'NONE',  ( -4.458734124999999437, 26.60416666803225993, -2.574251347313719407 ) ) ;
#39507 = CARTESIAN_POINT ( 'NONE',  ( 5.000000000000000000, -58.37499999726880873, -6.123233995736766282E-16 ) ) ;
#39508 = CARTESIAN_POINT ( 'NONE',  ( 0.000000000000000000, -170.0000000000000000, 5.000000000000000000 ) ) ;
#39509 = CARTESIAN_POINT ( 'NONE',  ( 4.458734124999998549, -74.97916666530106511, -2.574251347313721627 ) ) ;
#39510 = CARTESIAN_POINT ( 'NONE',  ( 5.000000000000000000, -58.50000000000000000, -6.123233995736766282E-16 ) ) ;
#39511 = CARTESIAN_POINT ( 'NONE',  ( 5.000000000000000000, -73.50000000000000000, -6.123233995736766282E-16 ) ) ;
#39512 = CARTESIAN_POINT ( 'NONE',  ( -5.000000000000000000, -10.95833333060214621, -2.886751345948128211 ) ) ;
#39513 = ORIENTED_EDGE ( 'NONE', *, *, #55598, .F. ) ;
#39514 = CARTESIAN_POINT ( 'NONE',  ( -2.500000000000000444, -57.04166666393548013, -4.330127018922193649 ) ) ;
#39515 = CARTESIAN_POINT ( 'NONE',  ( -5.000000000000000000, -18.99999999999999645, 0.000000000000000000 ) ) ;
#39516 = CARTESIAN_POINT ( 'NONE',  ( 9.457646018065525792E-16, -21.06249999863440436, 5.148502694627439702 ) ) ;
#39517 = CARTESIAN_POINT ( 'NONE',  ( -2.229367062500000163, -82.47916666530106511, -3.861377020970580443 ) ) ;
#39518 = AXIS2_PLACEMENT_3D ( 'NONE', #31157, #50139, #60766 ) ;
#39519 = CARTESIAN_POINT ( 'NONE',  ( 1.846868145590735200, -167.5000000013655779, -4.458734125000000326 ) ) ;
#39520 = CARTESIAN_POINT ( 'NONE',  ( 5.000000000000000000, -20.29166666393548368, -2.886751345948129988 ) ) ;
#39522 = ORIENTED_EDGE ( 'NONE', *, *, #46945, .T. ) ;
#39521 = CARTESIAN_POINT ( 'NONE',  ( -2.229367062499996610, -49.14583333196772941, 3.861377020970582219 ) ) ;
#39523 = CARTESIAN_POINT ( 'NONE',  ( 1.339745962155615144, -45.58034179853028434, 4.999999999999999112 ) ) ;
#39525 = ORIENTED_EDGE ( 'NONE', *, *, #5485, .F. ) ;
#39524 = CARTESIAN_POINT ( 'NONE',  ( 2.229367062499998831, 3.104166668032259935, -3.861377020970580887 ) ) ;
#39526 = CARTESIAN_POINT ( 'NONE',  ( -50.70258187064364108, -151.1250000013656347, 2.196230717870141014 ) ) ;
#39527 = CARTESIAN_POINT ( 'NONE',  ( 2.500000000000002220, -66.66666666666667140, 4.330127018922192761 ) ) ;
#39528 = CARTESIAN_POINT ( 'NONE',  ( -4.458734124999999437, -154.1875000013656063, -5.460374474430324690E-16 ) ) ;
#39529 = CARTESIAN_POINT ( 'NONE',  ( -3.152548672688508926E-16, -43.81249999863440081, -5.148502694627439702 ) ) ;
#39530 = CARTESIAN_POINT ( 'NONE',  ( 5.000000000000000000, -68.29166666393547303, -2.886751345948130876 ) ) ;
#39531 = CARTESIAN_POINT ( 'NONE',  ( 3.061616997868383141E-16, -163.7500000000000000, -5.000000000000000000 ) ) ;
#39532 = DIRECTION ( 'NONE',  ( -0.000000000000000000, 1.000000000000000000, -0.000000000000000000 ) ) ;
#39533 = CARTESIAN_POINT ( 'NONE',  ( -55.35523342533222291, -128.5625000013656063, 4.444560631937231499 ) ) ;
#39534 = CARTESIAN_POINT ( 'NONE',  ( -2.229367062500000163, -11.72916666530107044, -3.861377020970580443 ) ) ;
#39535 = CARTESIAN_POINT ( 'NONE',  ( -3.152548672688508926E-16, -43.81249999863440081, -5.148502694627439702 ) ) ;
#39536 = CARTESIAN_POINT ( 'NONE',  ( 5.000000000000000000, -89.50000000000000000, -6.123233995736766282E-16 ) ) ;
#39537 = CARTESIAN_POINT ( 'NONE',  ( -4.458734125000001214, -148.8750000013655495, 1.846868145590734089 ) ) ;
#39538 = CARTESIAN_POINT ( 'NONE',  ( -3.152548672688508926E-16, -90.81249999863440792, -5.148502694627439702 ) ) ;
#39539 = CARTESIAN_POINT ( 'NONE',  ( 1.975475456537005874E-15, -17.62499999726881583, 5.000000000000000000 ) ) ;
#39540 = ORIENTED_EDGE ( 'NONE', *, *, #52384, .F. ) ;
#39541 = CARTESIAN_POINT ( 'NONE',  ( -6.972266317189433020E-16, -32.24999999999999289, -5.000000000000000000 ) ) ;
#39542 = FACE_OUTER_BOUND ( 'NONE', #62062, .T. ) ;
#39543 = CARTESIAN_POINT ( 'NONE',  ( -58.24261429053147765, -152.3750000027312126, -3.805975901505573855 ) ) ;
#39544 = LINE ( 'NONE', #60152, #10602 ) ;
#39545 = ADVANCED_FACE ( 'NONE', ( #47684 ), #33216, .T. ) ;
#39546 = ORIENTED_EDGE ( 'NONE', *, *, #48422, .F. ) ;
#39547 = CARTESIAN_POINT ( 'NONE',  ( 2.229367062500001939, 1.020833334698927120, 3.861377020970579999 ) ) ;
#39548 = CYLINDRICAL_SURFACE ( 'NONE', #26569, 5.000000000000000000 ) ;
#39549 = CARTESIAN_POINT ( 'NONE',  ( -4.458734124999999437, -18.64583333196774007, -2.574251347313719407 ) ) ;
#39550 = CARTESIAN_POINT ( 'NONE',  ( -5.000000000000000000, 9.000000000000001776, 0.000000000000000000 ) ) ;
#39551 = CARTESIAN_POINT ( 'NONE',  ( -2.229367062500000163, -4.479166665301070438, -3.861377020970580443 ) ) ;
#39552 = CARTESIAN_POINT ( 'NONE',  ( -6.972266317189433020E-16, -54.24999999999999289, -5.000000000000000000 ) ) ;
#39553 = CARTESIAN_POINT ( 'NONE',  ( 3.152801135295367541, -148.3125000013655779, -3.152801135295367541 ) ) ;
#39554 = CARTESIAN_POINT ( 'NONE',  ( 9.457646018065525792E-16, 20.68750000136559208, 5.148502694627439702 ) ) ;
#39555 = ORIENTED_EDGE ( 'NONE', *, *, #19324, .T. ) ;
#39556 = CARTESIAN_POINT ( 'NONE',  ( 4.458734124999998549, -99.72916666530106511, -2.574251347313721627 ) ) ;
#39557 = LINE ( 'NONE', #34102, #27458 ) ;
#39558 = CARTESIAN_POINT ( 'NONE',  ( -57.46284108482265651, -154.0625000027312126, 4.819101127000238627 ) ) ;
#39559 = CARTESIAN_POINT ( 'NONE',  ( 4.458734124999998549, -13.72916666530107399, -2.574251347313721627 ) ) ;
#39560 = CARTESIAN_POINT ( 'NONE',  ( -4.999999999999998224, 28.20833333606451987, 2.886751345948131764 ) ) ;
#39561 = LINE ( 'NONE', #54379, #34503 ) ;
#39562 = AXIS2_PLACEMENT_3D ( 'NONE', #56818, #51980, #48088 ) ;
#39563 = CARTESIAN_POINT ( 'NONE',  ( -53.51423613279429503, -153.2500000013655779, 4.591703134518082763 ) ) ;
#39564 = CARTESIAN_POINT ( 'NONE',  ( -2.500000000000000444, -40.04166666393548013, -4.330127018922193649 ) ) ;
#39565 = DIRECTION ( 'NONE',  ( -0.000000000000000000, 1.000000000000000000, -0.000000000000000000 ) ) ;
#39566 = CARTESIAN_POINT ( 'NONE',  ( 2.229367062499998831, 11.35416666803225993, -3.861377020970580887 ) ) ;
#39567 = CARTESIAN_POINT ( 'NONE',  ( -6.972266317189433020E-16, -35.25000000000000000, -5.000000000000000000 ) ) ;
#39568 = LINE ( 'NONE', #11264, #55159 ) ;
#39569 = CARTESIAN_POINT ( 'NONE',  ( 9.457646018065525792E-16, 16.93750000136559564, 5.148502694627439702 ) ) ;
#39570 = CARTESIAN_POINT ( 'NONE',  ( -4.458734124999999437, -62.39583333196774362, -2.574251347313719407 ) ) ;
#39571 = VERTEX_POINT ( 'NONE', #13597 ) ;
#39572 = CARTESIAN_POINT ( 'NONE',  ( 4.458734125000000326, -10.14583333196773829, 2.574251347313718519 ) ) ;
#39573 = CARTESIAN_POINT ( 'NONE',  ( 5.000000000000000888, -169.0625000027312126, -2.071067811865475505 ) ) ;
#39574 = CARTESIAN_POINT ( 'NONE',  ( 5.000000000000000000, 3.583333333333333925, -2.886751345948129988 ) ) ;
#39575 = CARTESIAN_POINT ( 'NONE',  ( 4.458734124999999437, -169.4375000013656063, 0.000000000000000000 ) ) ;
#39576 = CARTESIAN_POINT ( 'NONE',  ( -9.184850993605147944E-16, -154.3750000027311842, 5.000000000000000000 ) ) ;
#39577 = CARTESIAN_POINT ( 'NONE',  ( 4.458734124999998549, -53.72916666530106511, -2.574251347313721627 ) ) ;
#39578 = CARTESIAN_POINT ( 'NONE',  ( -4.999999999999999112, -89.79166666393547303, 2.886751345948131764 ) ) ;
#39579 = CARTESIAN_POINT ( 'NONE',  ( 4.458734124999999437, -34.81249999863440792, -5.460374474430324690E-16 ) ) ;
#39580 =( BOUNDED_CURVE ( )  B_SPLINE_CURVE ( 2, ( #4496, #8083, #43725, #63369, #38900, #37652, #32509, #52141, #62112 ),
 .UNSPECIFIED., .F., .F. ) 
 B_SPLINE_CURVE_WITH_KNOTS ( ( 3, 2, 2, 2, 3 ),
 ( 0.4267857142857142683, 0.4273809523809523614, 0.4285714285714285476, 0.4297619047619047894, 0.4303571428571428825 ),
 .UNSPECIFIED. ) 
 CURVE ( )  GEOMETRIC_REPRESENTATION_ITEM ( )  RATIONAL_B_SPLINE_CURVE ( ( 0.9330127018922194093, 0.9330127018922194093, 1.000000000000000000, 0.8660254037844387076, 1.000000000000000000, 0.8660254037844387076, 1.000000000000000000, 0.9330127018922194093, 0.9330127018922194093 ) ) 
 REPRESENTATION_ITEM ( '' )  );
#39581 = CARTESIAN_POINT ( 'NONE',  ( -1.339745962155613812, 19.91965820146970501, -5.000000000000000000 ) ) ;
#39582 = CARTESIAN_POINT ( 'NONE',  ( 3.535533905932738197, -142.0000000027311842, -3.535533905932738197 ) ) ;
#39583 = CARTESIAN_POINT ( 'NONE',  ( -1.339745962155613812, -108.0803417985302985, -5.000000000000000000 ) ) ;
#39584 = CARTESIAN_POINT ( 'NONE',  ( 2.730187237215162345E-16, -153.4375000013655779, -4.458734124999999437 ) ) ;
#39585 = CARTESIAN_POINT ( 'NONE',  ( -5.000000000000000000, -45.00000000000000000, 0.000000000000000000 ) ) ;
#39586 = CARTESIAN_POINT ( 'NONE',  ( 2.788906526875773208E-15, 27.87500000273118772, -5.000000000000000000 ) ) ;
#39587 = CARTESIAN_POINT ( 'NONE',  ( -59.24072208773964832, -135.0000000000000568, 2.598697453439798188 ) ) ;
#39588 = ORIENTED_EDGE ( 'NONE', *, *, #59338, .T. ) ;
#39589 = CARTESIAN_POINT ( 'NONE',  ( 4.458734124999999437, -99.81249999863440792, -5.460374474430324690E-16 ) ) ;
#39590 = CARTESIAN_POINT ( 'NONE',  ( -2.229367062499996610, 2.604166668032259491, 3.861377020970582219 ) ) ;
#39591 = CARTESIAN_POINT ( 'NONE',  ( 1.975475456537005874E-15, -76.75000000000000000, 5.000000000000000000 ) ) ;
#39592 = CARTESIAN_POINT ( 'NONE',  ( -5.000000000000000000, -3.000000000000002665, 0.000000000000000000 ) ) ;
#39593 = CARTESIAN_POINT ( 'NONE',  ( -4.458734124999997661, -68.22916666530106511, 2.574251347313722516 ) ) ;
#39594 = CARTESIAN_POINT ( 'NONE',  ( -8.660254037844341113, 45.00000000000000000, 6.047423072554883697E-14 ) ) ;
#39595 = CARTESIAN_POINT ( 'NONE',  ( 5.000000000000000000, -0.2916666639354824619, -2.886751345948129988 ) ) ;
#39597 = ORIENTED_EDGE ( 'NONE', *, *, #60075, .F. ) ;
#39596 = CARTESIAN_POINT ( 'NONE',  ( 4.458734125000001214, -31.89583333196773651, 2.574251347313718519 ) ) ;
#39598 = CARTESIAN_POINT ( 'NONE',  ( -2.500000000000000444, -11.16666666666666430, -4.330127018922193649 ) ) ;
#39599 = CARTESIAN_POINT ( 'NONE',  ( 3.535533905932736864, -157.1250000000000284, 3.535533905932738641 ) ) ;
#39600 = VERTEX_POINT ( 'NONE', #52834 ) ;
#39601 = LINE ( 'NONE', #38351, #44283 ) ;
#39602 = CARTESIAN_POINT ( 'NONE',  ( -2.500000000000000444, -52.16666666666666430, -4.330127018922193649 ) ) ;
#39604 = CARTESIAN_POINT ( 'NONE',  ( 4.458734124999998549, -23.97916666530107221, -2.574251347313721627 ) ) ;
#39603 = CARTESIAN_POINT ( 'NONE',  ( 5.000000000000000000, -17.29166666393548368, -2.886751345948130876 ) ) ;
#39605 = CARTESIAN_POINT ( 'NONE',  ( -6.972266317189433020E-16, -4.249999999999997335, -5.000000000000000000 ) ) ;
#39606 = CARTESIAN_POINT ( 'NONE',  ( 9.457646018065525792E-16, -72.06249999863439371, 5.148502694627439702 ) ) ;
#39607 = CARTESIAN_POINT ( 'NONE',  ( 4.458734124999999437, -142.6875000013656063, 0.000000000000000000 ) ) ;
#39608 = CARTESIAN_POINT ( 'NONE',  ( 4.458734124999999437, -82.81249999863440792, -5.460374474430324690E-16 ) ) ;
#39609 = CARTESIAN_POINT ( 'NONE',  ( -54.64476657466781973, -139.0625000013656063, -4.444560631937228834 ) ) ;
#39610 = VECTOR ( 'NONE', #56914, 1000.000000000000000 ) ;
#39611 = CARTESIAN_POINT ( 'NONE',  ( 2.229367062499998831, -27.89583333196774007, -3.861377020970580887 ) ) ;
#39612 = CARTESIAN_POINT ( 'NONE',  ( -2.500000000000000444, -74.04166666393547303, -4.330127018922193649 ) ) ;
#39613 = ORIENTED_EDGE ( 'NONE', *, *, #17664, .F. ) ;
#39614 = CARTESIAN_POINT ( 'NONE',  ( 0.000000000000000000, -170.0000000000000000, 5.000000000000000000 ) ) ;
#39615 = EDGE_LOOP ( 'NONE', ( #30598, #51731, #62736, #45929 ) ) ;
#39616 = CARTESIAN_POINT ( 'NONE',  ( -2.229367062500000163, -71.72916666530107932, -3.861377020970580443 ) ) ;
#39617 = ORIENTED_EDGE ( 'NONE', *, *, #58150, .F. ) ;
#39618 = CARTESIAN_POINT ( 'NONE',  ( -5.000000000000000000, 17.00000000000000000, 0.000000000000000000 ) ) ;
#39619 = CARTESIAN_POINT ( 'NONE',  ( 1.975475456537005874E-15, -12.74999999999999822, 5.000000000000000000 ) ) ;
#39621 = EDGE_CURVE ( 'NONE', #49284, #25405, #3635, .T. ) ;
#39620 = CARTESIAN_POINT ( 'NONE',  ( -4.458734124999998549, -58.47916666530106511, 2.574251347313722516 ) ) ;
#39622 = CARTESIAN_POINT ( 'NONE',  ( -4.458734124999999437, -5.645833331967740953, -2.574251347313719407 ) ) ;
#39623 = ORIENTED_EDGE ( 'NONE', *, *, #57558, .F. ) ;
#39624 = CARTESIAN_POINT ( 'NONE',  ( 5.000000000000000000, -142.0625000000000000, 2.071067811865478614 ) ) ;
#39625 = DIRECTION ( 'NONE',  ( -0.000000000000000000, 1.000000000000000000, -0.000000000000000000 ) ) ;
#39626 = CARTESIAN_POINT ( 'NONE',  ( 2.229367062499998831, 14.35416666803226171, -3.861377020970580887 ) ) ;
#39627 = CARTESIAN_POINT ( 'NONE',  ( -50.55543936806279248, -139.0625000013656063, 0.3552334253322060320 ) ) ;
#39628 = CARTESIAN_POINT ( 'NONE',  ( 5.000000000000000888, -24.58333333333333215, 2.886751345948126879 ) ) ;
#39629 = CARTESIAN_POINT ( 'NONE',  ( -4.458734124999999437, -159.9375000013655779, -5.460374474430324690E-16 ) ) ;
#39630 = ORIENTED_EDGE ( 'NONE', *, *, #21654, .F. ) ;
#39631 = CARTESIAN_POINT ( 'NONE',  ( 2.229367062499998831, -81.64583333196773651, -3.861377020970580887 ) ) ;
#39632 = CARTESIAN_POINT ( 'NONE',  ( 2.229367062499998831, 3.354166668032259935, -3.861377020970580887 ) ) ;
#39633 = CARTESIAN_POINT ( 'NONE',  ( 5.000000000000000888, -86.58333333333334281, 2.886751345948126879 ) ) ;
#39634 = EDGE_CURVE ( 'NONE', #59356, #41437, #43341, .T. ) ;
#39635 = FACE_OUTER_BOUND ( 'NONE', #14780, .T. ) ;
#39636 = CARTESIAN_POINT ( 'NONE',  ( 2.229367062500001939, -64.22916666530106511, 3.861377020970579999 ) ) ;
#39637 = CARTESIAN_POINT ( 'NONE',  ( -2.499999999999996447, -27.70833333060214798, 4.330127018922195425 ) ) ;
#39638 = ADVANCED_FACE ( 'NONE', ( #2686 ), #23246, .T. ) ;
#39639 = CARTESIAN_POINT ( 'NONE',  ( -4.999999999999998224, -14.91666666666666785, 2.886751345948131764 ) ) ;
#39640 = CARTESIAN_POINT ( 'NONE',  ( -6.972266317189433020E-16, -1.124999997268814278, -5.000000000000000000 ) ) ;
#39641 = CARTESIAN_POINT ( 'NONE',  ( -5.000000000000000000, -64.95833333060213022, -2.886751345948128211 ) ) ;
#39642 = CARTESIAN_POINT ( 'NONE',  ( -2.229367062500000163, -46.47916666530106511, -3.861377020970580443 ) ) ;
#39643 = CARTESIAN_POINT ( 'NONE',  ( -4.458734124999997661, -34.47916666530107221, 2.574251347313722516 ) ) ;
#39644 = CARTESIAN_POINT ( 'NONE',  ( 4.458734124999998549, 7.020833334698928674, -2.574251347313721627 ) ) ;
#39645 =( BOUNDED_CURVE ( )  B_SPLINE_CURVE ( 2, ( #11499, #42270, #61910, #61593, #38084, #32622, #18141, #17527, #52565 ),
 .UNSPECIFIED., .F., .F. ) 
 B_SPLINE_CURVE_WITH_KNOTS ( ( 3, 2, 2, 2, 3 ),
 ( 0.06607142857142857262, 0.06666666666666666574, 0.06785714285714285199, 0.06904761904761905211, 0.06964285714285714524 ),
 .UNSPECIFIED. ) 
 CURVE ( )  GEOMETRIC_REPRESENTATION_ITEM ( )  RATIONAL_B_SPLINE_CURVE ( ( 0.9330127018922194093, 0.9330127018922194093, 1.000000000000000000, 0.8660254037844387076, 1.000000000000000000, 0.8660254037844387076, 1.000000000000000000, 0.9330127018922194093, 0.9330127018922194093 ) ) 
 REPRESENTATION_ITEM ( '' )  );
#39646 = CARTESIAN_POINT ( 'NONE',  ( -2.500000000000000444, -10.04166666393547658, -4.330127018922193649 ) ) ;
#39647 = CARTESIAN_POINT ( 'NONE',  ( -4.999999999999999112, 22.08333333333333215, 2.886751345948131764 ) ) ;
#39648 = CARTESIAN_POINT ( 'NONE',  ( 2.071067811865476394, -149.3125000027311842, 5.000000000000000000 ) ) ;
#39649 = CARTESIAN_POINT ( 'NONE',  ( 0.000000000000000000, -170.0000000000000000, 5.000000000000000000 ) ) ;
#39650 = CARTESIAN_POINT ( 'NONE',  ( 2.229367062499998831, -35.64583333196772941, -3.861377020970580887 ) ) ;
#39651 = CARTESIAN_POINT ( 'NONE',  ( -2.500000000000000444, -76.04166666393547303, -4.330127018922193649 ) ) ;
#39652 = EDGE_CURVE ( 'NONE', #53365, #62346, #39201, .T. ) ;
#39653 = CARTESIAN_POINT ( 'NONE',  ( -50.40829686548195099, -145.2500000013656347, -1.485763867205728284 ) ) ;
#39654 = CARTESIAN_POINT ( 'NONE',  ( -5.000000000000000888, -140.4375000000000000, 2.071067811865474617 ) ) ;
#39655 = CARTESIAN_POINT ( 'NONE',  ( 0.5974722283283632196, -8.315303285985693904, -0.7026937717022971874 ) ) ;
#39656 = CARTESIAN_POINT ( 'NONE',  ( -2.229367062500000163, -77.72916666530106511, -3.861377020970580443 ) ) ;
#39657 = CARTESIAN_POINT ( 'NONE',  ( -4.458734124999999437, -165.2500000013655779, -1.846868145590735644 ) ) ;
#39658 = CARTESIAN_POINT ( 'NONE',  ( 5.000000000000000888, 18.54166666939785202, 2.886751345948126879 ) ) ;
#39659 = DIRECTION ( 'NONE',  ( -0.000000000000000000, 1.000000000000000000, -0.000000000000000000 ) ) ;
#39660 = CARTESIAN_POINT ( 'NONE',  ( -3.535250795749689387E-16, -26.25000000000000355, -5.773502691896257311 ) ) ;
#39661 = CARTESIAN_POINT ( 'NONE',  ( -1.846868145590734756, -145.1250000013655779, -4.458734125000000326 ) ) ;
#39662 = ORIENTED_EDGE ( 'NONE', *, *, #58551, .T. ) ;
#39663 = CARTESIAN_POINT ( 'NONE',  ( 2.229367062500001939, 28.77083333469892779, 3.861377020970579999 ) ) ;
#39664 = ORIENTED_EDGE ( 'NONE', *, *, #58125, .T. ) ;
#39665 = CARTESIAN_POINT ( 'NONE',  ( -4.458734124999999437, -63.64583333196773651, -2.574251347313719407 ) ) ;
#39666 = CARTESIAN_POINT ( 'NONE',  ( 2.500000000000002220, 22.45833333606451987, 4.330127018922192761 ) ) ;
#39667 = CARTESIAN_POINT ( 'NONE',  ( 5.000000000000000888, -90.45833333060214443, 2.886751345948126879 ) ) ;
#39668 = CARTESIAN_POINT ( 'NONE',  ( 5.000000000000000000, 15.58333333333333215, -2.886751345948129988 ) ) ;
#39669 = CARTESIAN_POINT ( 'NONE',  ( 4.458734125000000326, -51.89583333196773651, 2.574251347313718519 ) ) ;
#39670 = CARTESIAN_POINT ( 'NONE',  ( -4.458734124999999437, -5.312499998634402587, 0.000000000000000000 ) ) ;
#39671 = CARTESIAN_POINT ( 'NONE',  ( -3.535533905932737309, -168.6250000000000284, -3.535533905932738197 ) ) ;
#39672 = EDGE_CURVE ( 'NONE', #36130, #29318, #26077, .T. ) ;
#39673 = CARTESIAN_POINT ( 'NONE',  ( -6.972266317189433020E-16, -9.250000000000000000, -5.000000000000000000 ) ) ;
#39674 = CARTESIAN_POINT ( 'NONE',  ( -1.339745962155613812, -0.2053418012614791066, -5.000000000000000000 ) ) ;
#39675 = FACE_OUTER_BOUND ( 'NONE', #22411, .T. ) ;
#39676 =( BOUNDED_CURVE ( )  B_SPLINE_CURVE ( 2, ( #31972, #51608, #17812, #52231, #13303, #22656, #57694, #13621, #52859 ),
 .UNSPECIFIED., .F., .F. ) 
 B_SPLINE_CURVE_WITH_KNOTS ( ( 3, 2, 2, 2, 3 ),
 ( 0.1910714285714285865, 0.1916666666666666796, 0.1928571428571428659, 0.1940476190476190521, 0.1946428571428571452 ),
 .UNSPECIFIED. ) 
 CURVE ( )  GEOMETRIC_REPRESENTATION_ITEM ( )  RATIONAL_B_SPLINE_CURVE ( ( 0.9330127018922194093, 0.9330127018922209636, 1.000000000000000000, 0.8660254037844387076, 1.000000000000000000, 0.8660254037844387076, 1.000000000000000000, 0.9330127018922194093, 0.9330127018922194093 ) ) 
 REPRESENTATION_ITEM ( '' )  );
#39678 = CARTESIAN_POINT ( 'NONE',  ( -3.152548672688508926E-16, -21.56249999863440081, -5.148502694627439702 ) ) ;
#39677 = DIRECTION ( 'NONE',  ( -0.000000000000000000, 1.000000000000000000, -0.000000000000000000 ) ) ;
#39679 = CARTESIAN_POINT ( 'NONE',  ( -5.000000000000000000, -31.95833333060214443, -2.886751345948128211 ) ) ;
#39680 = CARTESIAN_POINT ( 'NONE',  ( 2.229367062499998831, -54.64583333196773651, -3.861377020970580887 ) ) ;
#39681 = CARTESIAN_POINT ( 'NONE',  ( 4.458734124999999437, -154.7500000013656063, 1.846868145590737864 ) ) ;
#39682 = CARTESIAN_POINT ( 'NONE',  ( 2.499999999999998668, -54.20833333060213732, -4.330127018922193649 ) ) ;
#39683 = EDGE_LOOP ( 'NONE', ( #24209, #27664, #19689, #3286 ) ) ;
#39684 = CARTESIAN_POINT ( 'NONE',  ( 1.975475456537005874E-15, -26.74999999999999645, 5.000000000000000000 ) ) ;
#39685 = CARTESIAN_POINT ( 'NONE',  ( 4.458734124999999437, 3.937500001365595192, -5.460374474430324690E-16 ) ) ;
#39686 = ORIENTED_EDGE ( 'NONE', *, *, #32676, .F. ) ;
#39687 = CARTESIAN_POINT ( 'NONE',  ( 1.975475456537005874E-15, -28.74999999999999645, 5.000000000000000000 ) ) ;
#39688 = CARTESIAN_POINT ( 'NONE',  ( -8.190561711645485556E-16, -155.6875000013655779, 4.458734124999999437 ) ) ;
#39689 = ORIENTED_EDGE ( 'NONE', *, *, #42145, .T. ) ;
#39690 = CONICAL_SURFACE ( 'NONE', #54073, 10.39117206796836079, 1.221730476396047926 ) ;
#39691 = CARTESIAN_POINT ( 'NONE',  ( 1.975475456537005874E-15, -23.62499999726880873, 5.000000000000000000 ) ) ;
#39692 = CARTESIAN_POINT ( 'NONE',  ( -58.80597590150559739, -131.0000000000000284, 3.242614290531460330 ) ) ;
#39693 = CARTESIAN_POINT ( 'NONE',  ( 1.975475456537005874E-15, -86.75000000000001421, 5.000000000000000000 ) ) ;
#39695 = EDGE_CURVE ( 'NONE', #27676, #51084, #38039, .T. ) ;
#39694 = CARTESIAN_POINT ( 'NONE',  ( -2.229367062499996610, -43.39583333196773651, 3.861377020970582219 ) ) ;
#39696 = ORIENTED_EDGE ( 'NONE', *, *, #53011, .F. ) ;
#39697 = EDGE_CURVE ( 'NONE', #41789, #2557, #58566, .T. ) ;
#39698 = EDGE_CURVE ( 'NONE', #6727, #52469, #36790, .T. ) ;
#39699 = CARTESIAN_POINT ( 'NONE',  ( 2.229367062499998831, 14.35416666803226171, -3.861377020970580887 ) ) ;
#39700 = ORIENTED_EDGE ( 'NONE', *, *, #56215, .T. ) ;
#39701 = CARTESIAN_POINT ( 'NONE',  ( 4.458734124999999437, -90.06249999863440792, -5.460374474430324690E-16 ) ) ;
#39702 = CARTESIAN_POINT ( 'NONE',  ( -54.64476657466781973, -153.8125000013656347, -4.444560631937228834 ) ) ;
#39703 = CARTESIAN_POINT ( 'NONE',  ( -2.071067811865415109, -165.3125000000000284, 5.000000000000062172 ) ) ;
#39704 = CARTESIAN_POINT ( 'NONE',  ( 5.000000000000000000, -39.49999999999999289, -6.123233995736766282E-16 ) ) ;
#39705 = CARTESIAN_POINT ( 'NONE',  ( 6.123233995736766282E-16, -120.0000000000000000, -5.000000000000000000 ) ) ;
#39706 = CARTESIAN_POINT ( 'NONE',  ( -4.458734124999999437, -64.31249999863440792, 0.000000000000000000 ) ) ;
#39707 = CARTESIAN_POINT ( 'NONE',  ( 6.523606932381168733, 4.893847819346807348, -7.213065638943126245 ) ) ;
#39708 = CARTESIAN_POINT ( 'NONE',  ( 2.229367062499998831, 20.35416666803225993, -3.861377020970580887 ) ) ;
#39709 = EDGE_CURVE ( 'NONE', #59564, #46451, #30573, .T. ) ;
#39710 = CARTESIAN_POINT ( 'NONE',  ( 1.975475456537005874E-15, -83.62499999726878741, 5.000000000000000000 ) ) ;
#39711 = CARTESIAN_POINT ( 'NONE',  ( -3.152548672688508926E-16, -48.81249999863440792, -5.148502694627439702 ) ) ;
#39712 = CARTESIAN_POINT ( 'NONE',  ( 5.000000000000000888, -7.458333330602143540, 2.886751345948126879 ) ) ;
#39713 = CARTESIAN_POINT ( 'NONE',  ( -6.972266317189433020E-16, -109.2499999999999716, -5.000000000000000000 ) ) ;
#39714 = EDGE_CURVE ( 'NONE', #60346, #32427, #10847, .T. ) ;
#39715 = CARTESIAN_POINT ( 'NONE',  ( 0.000000000000000000, -170.0000000000000000, 5.000000000000000000 ) ) ;
#39716 = CARTESIAN_POINT ( 'NONE',  ( 1.975475456537005874E-15, -73.75000000000000000, 5.000000000000000000 ) ) ;
#39717 = CARTESIAN_POINT ( 'NONE',  ( -1.339745962155610925, 11.33034180399266511, 5.000000000000000000 ) ) ;
#39718 = CARTESIAN_POINT ( 'NONE',  ( -2.229367062499996610, -16.39583333196773651, 3.861377020970582219 ) ) ;
#39719 = ORIENTED_EDGE ( 'NONE', *, *, #40185, .F. ) ;
#39720 = CARTESIAN_POINT ( 'NONE',  ( 5.000000000000000888, -31.58333333333333215, 2.886751345948126879 ) ) ;
#39721 = CARTESIAN_POINT ( 'NONE',  ( -4.458734124999999437, -101.3124999986344079, 0.000000000000000000 ) ) ;
#39722 = CARTESIAN_POINT ( 'NONE',  ( -2.071067811865475061, -161.8125000027311842, -5.000000000000000888 ) ) ;
#39723 = CARTESIAN_POINT ( 'NONE',  ( -4.458734124999998549, -96.47916666530105090, 2.574251347313722516 ) ) ;
#39724 = CARTESIAN_POINT ( 'NONE',  ( -1.339745962155555858, -8.205341801261482715, -5.000000000000032863 ) ) ;
#39725 = CARTESIAN_POINT ( 'NONE',  ( 2.499999999999998668, -58.20833333060214443, -4.330127018922193649 ) ) ;
#39726 = CYLINDRICAL_SURFACE ( 'NONE', #9908, 5.000000000000000000 ) ;
#39727 = CARTESIAN_POINT ( 'NONE',  ( -50.40829686548195099, -154.2500000013656063, -1.485763867205728284 ) ) ;
#39728 = CARTESIAN_POINT ( 'NONE',  ( -57.19623071787016499, -147.3750000013656063, 4.297418129356382899 ) ) ;
#39729 = CARTESIAN_POINT ( 'NONE',  ( 4.458734125000000326, -17.89583333196773651, 2.574251347313718519 ) ) ;
#39730 = CARTESIAN_POINT ( 'NONE',  ( -4.458734124999998549, 4.520833334698926009, 2.574251347313722516 ) ) ;
#39731 = CARTESIAN_POINT ( 'NONE',  ( -4.458734124999999437, -64.56249999863440792, 0.000000000000000000 ) ) ;
#39732 = CARTESIAN_POINT ( 'NONE',  ( 2.229367062499998831, -19.64583333196774007, -3.861377020970580887 ) ) ;
#39733 = CARTESIAN_POINT ( 'NONE',  ( -2.500000000000000444, -80.04166666393547303, -4.330127018922193649 ) ) ;
#39734 = CARTESIAN_POINT ( 'NONE',  ( -3.535533905932737309, -154.6250000000000000, -3.535533905932738197 ) ) ;
#39735 = CARTESIAN_POINT ( 'NONE',  ( -5.000000000000000000, -7.083333333333330373, -2.886751345948128211 ) ) ;
#39736 = CARTESIAN_POINT ( 'NONE',  ( -4.458734124999999437, -156.9375000013655779, -5.460374474430324690E-16 ) ) ;
#39737 = ORIENTED_EDGE ( 'NONE', *, *, #18620, .F. ) ;
#39738 = CARTESIAN_POINT ( 'NONE',  ( -3.152548672688508926E-16, -44.81249999863439371, -5.148502694627439702 ) ) ;
#39739 = CARTESIAN_POINT ( 'NONE',  ( -1.339745962155564296, -12.20534180126147916, -5.000000000000028422 ) ) ;
#39740 = CARTESIAN_POINT ( 'NONE',  ( -4.458734124999998549, -89.22916666530106511, 2.574251347313722516 ) ) ;
#39741 = CARTESIAN_POINT ( 'NONE',  ( 2.229367062500001939, -90.97916666530106511, 3.861377020970579999 ) ) ;
#39742 = CARTESIAN_POINT ( 'NONE',  ( 9.457646018065525792E-16, 17.68750000136559564, 5.148502694627439702 ) ) ;
#39743 = CARTESIAN_POINT ( 'NONE',  ( 9.457646018065525792E-16, 9.937500001365592084, 5.148502694627439702 ) ) ;
#39744 = CARTESIAN_POINT ( 'NONE',  ( 2.500000000000002220, -82.66666666666667140, 4.330127018922192761 ) ) ;
#39745 = CARTESIAN_POINT ( 'NONE',  ( -5.000000000000000000, -69.08333333333332860, -2.886751345948128211 ) ) ;
#39746 = CARTESIAN_POINT ( 'NONE',  ( 1.975475456537005874E-15, -67.62499999726881583, 5.000000000000000000 ) ) ;
#39747 = CARTESIAN_POINT ( 'NONE',  ( 2.229367062499998831, 21.10416666803226349, -3.861377020970580887 ) ) ;
#39748 = CARTESIAN_POINT ( 'NONE',  ( -2.500000000000000444, -75.16666666666665719, -4.330127018922193649 ) ) ;
#39749 = CARTESIAN_POINT ( 'NONE',  ( 5.000000000000000888, 6.541666669397851130, 2.886751345948126879 ) ) ;
#39750 = VERTEX_POINT ( 'NONE', #44746 ) ;
#39751 = VERTEX_POINT ( 'NONE', #707 ) ;
#39752 = CARTESIAN_POINT ( 'NONE',  ( 2.499999999999998668, -85.33333333333332860, -4.330127018922193649 ) ) ;
#39753 = CARTESIAN_POINT ( 'NONE',  ( 4.458734124999999437, -37.81249999863440792, -5.460374474430324690E-16 ) ) ;
#39754 =( BOUNDED_CURVE ( )  B_SPLINE_CURVE ( 2, ( #42984, #62628, #18550, #15624, #44885, #44558, #34582, #50026, #35241 ),
 .UNSPECIFIED., .F., .F. ) 
 B_SPLINE_CURVE_WITH_KNOTS ( ( 3, 2, 2, 2, 3 ),
 ( 0.06964285714285714524, 0.07023809523809523836, 0.07142857142857142461, 0.07261904761904762473, 0.07321428571428571785 ),
 .UNSPECIFIED. ) 
 CURVE ( )  GEOMETRIC_REPRESENTATION_ITEM ( )  RATIONAL_B_SPLINE_CURVE ( ( 0.9330127018922194093, 0.9330127018922194093, 1.000000000000000000, 0.8660254037844387076, 1.000000000000000000, 0.8660254037844387076, 1.000000000000000000, 0.9330127018922194093, 0.9330127018922194093 ) ) 
 REPRESENTATION_ITEM ( '' )  );
#39755 = CARTESIAN_POINT ( 'NONE',  ( -4.999999999999999112, -40.79166666393548724, 2.886751345948131764 ) ) ;
#39756 = ORIENTED_EDGE ( 'NONE', *, *, #29529, .F. ) ;
#39757 = CARTESIAN_POINT ( 'NONE',  ( -59.44456063193725015, -147.8125000013656063, -0.3552334253322034230 ) ) ;
#39758 = CARTESIAN_POINT ( 'NONE',  ( -3.152548672688508926E-16, -13.56249999863440259, -5.148502694627439702 ) ) ;
#39760 = ORIENTED_EDGE ( 'NONE', *, *, #44512, .F. ) ;
#39759 = CARTESIAN_POINT ( 'NONE',  ( -2.229367062500000163, -13.72916666530107221, -3.861377020970580443 ) ) ;
#39761 = CARTESIAN_POINT ( 'NONE',  ( -4.999999999999999112, -80.91666666666667140, 2.886751345948131764 ) ) ;
#39762 = CARTESIAN_POINT ( 'NONE',  ( 4.458734124999999437, -169.4375000013656063, 0.000000000000000000 ) ) ;
#39763 = CARTESIAN_POINT ( 'NONE',  ( -3.152548672688508926E-16, -64.81249999863440792, -5.148502694627439702 ) ) ;
#39764 = CARTESIAN_POINT ( 'NONE',  ( 5.000000000000000000, -87.29166666393548724, -2.886751345948129988 ) ) ;
#39766 = ORIENTED_EDGE ( 'NONE', *, *, #548, .T. ) ;
#39765 = CARTESIAN_POINT ( 'NONE',  ( 1.975475456537005874E-15, -48.62499999726880162, 5.000000000000000000 ) ) ;
#39767 = CARTESIAN_POINT ( 'NONE',  ( -52.53715891517739323, -142.4375000000000000, -4.819101127000233298 ) ) ;
#39768 = CARTESIAN_POINT ( 'NONE',  ( -4.458734124999999437, -29.64583333196773651, -2.574251347313719407 ) ) ;
#39769 = CARTESIAN_POINT ( 'NONE',  ( -5.000000000000000000, -50.08333333333332860, -2.886751345948128211 ) ) ;
#39770 = ORIENTED_EDGE ( 'NONE', *, *, #53455, .F. ) ;
#39771 =( BOUNDED_CURVE ( )  B_SPLINE_CURVE ( 2, ( #8281, #7021, #7656, #62315, #22448, #27569, #7342, #18240, #26629 ),
 .UNSPECIFIED., .F., .F. ) 
 B_SPLINE_CURVE_WITH_KNOTS ( ( 3, 2, 2, 2, 3 ),
 ( 0.8160714285714285587, 0.8166666666666666519, 0.8178571428571428381, 0.8190476190476190244, 0.8196428571428571175 ),
 .UNSPECIFIED. ) 
 CURVE ( )  GEOMETRIC_REPRESENTATION_ITEM ( )  RATIONAL_B_SPLINE_CURVE ( ( 0.9330127018922194093, 0.9330127018922194093, 1.000000000000000000, 0.8660254037844387076, 1.000000000000000000, 0.8660254037844387076, 1.000000000000000000, 0.9330127018922194093, 0.9330127018922194093 ) ) 
 REPRESENTATION_ITEM ( '' )  );
#39772 = ADVANCED_FACE ( 'NONE', ( #49578 ), #71, .T. ) ;
#39773 = CONTEXT_DEPENDENT_SHAPE_REPRESENTATION ( #19946, #23509 ) ;
#39774 = CARTESIAN_POINT ( 'NONE',  ( 3.152801135295366208, -163.8125000013656063, 3.152801135295367985 ) ) ;
#39775 = CARTESIAN_POINT ( 'NONE',  ( 4.458734125000001214, -110.1458333319677507, 2.574251347313718519 ) ) ;
#39776 = CARTESIAN_POINT ( 'NONE',  ( 5.000000000000000888, -23.58333333333333215, 2.886751345948126879 ) ) ;
#39777 = ORIENTED_EDGE ( 'NONE', *, *, #47515, .T. ) ;
#39778 = CARTESIAN_POINT ( 'NONE',  ( -57.19623071787016499, -144.6250000013656063, 4.297418129356382899 ) ) ;
#39779 = CARTESIAN_POINT ( 'NONE',  ( 4.458734124999999437, -76.06249999863440792, -5.460374474430324690E-16 ) ) ;
#39780 = CARTESIAN_POINT ( 'NONE',  ( -49.85088928181150436, -133.6875000027312126, -1.666127454062680702 ) ) ;
#39781 = CARTESIAN_POINT ( 'NONE',  ( -3.152548672688508926E-16, -46.56249999863440792, -5.148502694627439702 ) ) ;
#39782 = CARTESIAN_POINT ( 'NONE',  ( -4.458734125000000326, -145.1250000013656063, 1.846868145590734089 ) ) ;
#39783 = EDGE_CURVE ( 'NONE', #11315, #28751, #63438, .T. ) ;
#39784 = CARTESIAN_POINT ( 'NONE',  ( -7.908219015560238319, -3.084967917785936820, -7.795665562178438535 ) ) ;
#39785 = CARTESIAN_POINT ( 'NONE',  ( -4.458734124999999437, -47.31249999863440792, 0.000000000000000000 ) ) ;
#39786 = CARTESIAN_POINT ( 'NONE',  ( -5.000000000000000000, -0.08333333333333454995, -2.886751345948128211 ) ) ;
#39787 = VECTOR ( 'NONE', #42060, 1000.000000000000000 ) ;
#39788 = EDGE_CURVE ( 'NONE', #26290, #37707, #38466, .T. ) ;
#39789 = CARTESIAN_POINT ( 'NONE',  ( 4.458734124999999437, -12.81249999863440259, -5.460374474430324690E-16 ) ) ;
#39790 = CARTESIAN_POINT ( 'NONE',  ( -5.000000000000000000, -100.0833333333333286, -2.886751345948128211 ) ) ;
#39791 = CARTESIAN_POINT ( 'NONE',  ( -3.152801135295367985, -142.0625000013655779, 3.152801135295367096 ) ) ;
#39792 = CARTESIAN_POINT ( 'NONE',  ( 9.457646018065525792E-16, -31.31249999863440436, 5.148502694627439702 ) ) ;
#39793 = CARTESIAN_POINT ( 'NONE',  ( -5.000000000000000000, 7.041666669397851130, -2.886751345948128211 ) ) ;
#39794 = FACE_OUTER_BOUND ( 'NONE', #53692, .T. ) ;
#39795 = CARTESIAN_POINT ( 'NONE',  ( -54.64476657466781973, -133.8125000013656063, -4.444560631937228834 ) ) ;
#39796 = CARTESIAN_POINT ( 'NONE',  ( -3.152548672688508926E-16, -74.81249999863439371, -5.148502694627439702 ) ) ;
#39797 = ADVANCED_FACE ( 'NONE', ( #39283 ), #58290, .T. ) ;
#39798 = CARTESIAN_POINT ( 'NONE',  ( -6.972266317189433020E-16, -34.25000000000000000, -5.000000000000000000 ) ) ;
#39799 = DIRECTION ( 'NONE',  ( 0.000000000000000000, 0.000000000000000000, 1.000000000000000000 ) ) ;
#39800 = CARTESIAN_POINT ( 'NONE',  ( -1.306442393143578462, -8.377108146505394259, -7.792327460285862983 ) ) ;
#39801 = CARTESIAN_POINT ( 'NONE',  ( 4.458734124999999437, -0.06249999863440491854, -5.460374474430324690E-16 ) ) ;
#39802 = VERTEX_POINT ( 'NONE', #19353 ) ;
#39803 = CARTESIAN_POINT ( 'NONE',  ( 2.500000000000002220, 16.45833333606451987, 4.330127018922192761 ) ) ;
#39804 = EDGE_CURVE ( 'NONE', #21365, #28539, #12771, .T. ) ;
#39805 = CARTESIAN_POINT ( 'NONE',  ( 1.975475456537005874E-15, -14.62499999726881228, 5.000000000000000000 ) ) ;
#39807 = CARTESIAN_POINT ( 'NONE',  ( 4.458734125000001214, -34.89583333196772941, 2.574251347313718519 ) ) ;
#39806 = CARTESIAN_POINT ( 'NONE',  ( -5.000000000000000000, -96.08333333333331439, -2.886751345948128211 ) ) ;
#39808 = CARTESIAN_POINT ( 'NONE',  ( 1.975475456537005874E-15, 9.250000000000000000, 5.000000000000000000 ) ) ;
#39809 = CARTESIAN_POINT ( 'NONE',  ( 4.458734125000001214, -80.14583333196773651, 2.574251347313718519 ) ) ;
#39810 = CARTESIAN_POINT ( 'NONE',  ( 2.229367062500001939, 17.77083333469892779, 3.861377020970579999 ) ) ;
#39811 = CARTESIAN_POINT ( 'NONE',  ( -6.972266317189433020E-16, -53.24999999999999289, -5.000000000000000000 ) ) ;
#39812 = CARTESIAN_POINT ( 'NONE',  ( -51.60603307380591787, -136.9375000013655779, -2.891590998281053704 ) ) ;
#39813 = ADVANCED_FACE ( 'NONE', ( #15498 ), #53144, .T. ) ;
#39814 = CARTESIAN_POINT ( 'NONE',  ( -4.458734124999997661, -4.229166665301070438, 2.574251347313722516 ) ) ;
#39815 = CARTESIAN_POINT ( 'NONE',  ( -3.152548672688508926E-16, 23.18750000136559208, -5.148502694627439702 ) ) ;
#39816 = CARTESIAN_POINT ( 'NONE',  ( 2.229367062499998831, -42.89583333196773651, -3.861377020970580887 ) ) ;
#39817 = DIRECTION ( 'NONE',  ( -0.000000000000000000, 1.000000000000000000, -0.000000000000000000 ) ) ;
#39818 = CARTESIAN_POINT ( 'NONE',  ( -4.458734124999999437, -1.312499998634406140, 0.000000000000000000 ) ) ;
#39819 = CARTESIAN_POINT ( 'NONE',  ( 9.457646018065525792E-16, -30.31249999863440436, 5.148502694627439702 ) ) ;
#39820 = CARTESIAN_POINT ( 'NONE',  ( -59.44456063193725015, -131.8125000013656063, -0.3552334253322034230 ) ) ;
#39821 = CARTESIAN_POINT ( 'NONE',  ( 9.457646018065525792E-16, -75.06249999863439371, 5.148502694627439702 ) ) ;
#39822 = CARTESIAN_POINT ( 'NONE',  ( 1.060575238724906964E-15, -107.6249999972687874, 5.773502691896257311 ) ) ;
#39823 = CARTESIAN_POINT ( 'NONE',  ( -2.229367062500000163, 25.52083333469892779, -3.861377020970580443 ) ) ;
#39824 = CARTESIAN_POINT ( 'NONE',  ( 6.123233995736766282E-16, -170.0000000000000000, -5.000000000000000000 ) ) ;
#39825 = CARTESIAN_POINT ( 'NONE',  ( -57.46284108482265651, -153.0625000027312126, 4.819101127000238627 ) ) ;
#39826 = CARTESIAN_POINT ( 'NONE',  ( 9.457646018065525792E-16, -76.31249999863440792, 5.148502694627439702 ) ) ;
#39827 = CARTESIAN_POINT ( 'NONE',  ( -3.535250795749689387E-16, -61.25000000000000000, -5.773502691896257311 ) ) ;
#39828 = CARTESIAN_POINT ( 'NONE',  ( 0.000000000000000000, -120.0000000000000000, 0.000000000000000000 ) ) ;
#39829 = CARTESIAN_POINT ( 'NONE',  ( 2.500000000000002220, 22.45833333606451987, 4.330127018922192761 ) ) ;
#39830 = ORIENTED_EDGE ( 'NONE', *, *, #2066, .F. ) ;
#39831 = CARTESIAN_POINT ( 'NONE',  ( 2.626220312808019583E-14, 14.87500000273118239, -5.000000000000000000 ) ) ;
#39832 =( BOUNDED_CURVE ( )  B_SPLINE_CURVE ( 2, ( #20633, #11279, #55036, #15798, #40864, #45382, #10960, #1347, #60192 ),
 .UNSPECIFIED., .F., .F. ) 
 B_SPLINE_CURVE_WITH_KNOTS ( ( 3, 2, 2, 2, 3 ),
 ( 0.7229166666666666519, 0.7236111111111110938, 0.7249999999999999778, 0.7263888888888888618, 0.7270833333333333037 ),
 .UNSPECIFIED. ) 
 CURVE ( )  GEOMETRIC_REPRESENTATION_ITEM ( )  RATIONAL_B_SPLINE_CURVE ( ( 0.9330127018922194093, 0.9330127018922194093, 1.000000000000000000, 0.8660254037844387076, 1.000000000000000000, 0.8660254037844387076, 1.000000000000000000, 0.9330127018922194093, 0.9330127018922194093 ) ) 
 REPRESENTATION_ITEM ( '' )  );
#39833 = VECTOR ( 'NONE', #12674, 1000.000000000000000 ) ;
#39834 = CARTESIAN_POINT ( 'NONE',  ( 2.499999999999998668, -16.33333333333333215, -4.330127018922193649 ) ) ;
#39835 = CARTESIAN_POINT ( 'NONE',  ( -4.458734124999999437, -22.31249999863440436, 0.000000000000000000 ) ) ;
#39836 = VECTOR ( 'NONE', #28204, 1000.000000000000000 ) ;
#39837 = CARTESIAN_POINT ( 'NONE',  ( -2.229367062500000163, -83.47916666530106511, -3.861377020970580443 ) ) ;
#39838 = CARTESIAN_POINT ( 'NONE',  ( -4.999999999999999112, -21.79166666393547658, 2.886751345948131764 ) ) ;
#39840 = ORIENTED_EDGE ( 'NONE', *, *, #62274, .T. ) ;
#39839 = CARTESIAN_POINT ( 'NONE',  ( 9.457646018065525792E-16, -48.06249999863440081, 5.148502694627439702 ) ) ;
#39841 = CARTESIAN_POINT ( 'NONE',  ( -5.000000000000000000, -24.00000000000000000, 0.000000000000000000 ) ) ;
#39842 = CARTESIAN_POINT ( 'NONE',  ( -5.000000000000000000, 11.04166666939785202, -2.886751345948128211 ) ) ;
#39844 = ORIENTED_EDGE ( 'NONE', *, *, #21206, .F. ) ;
#39843 = CARTESIAN_POINT ( 'NONE',  ( 9.457646018065525792E-16, 2.687500001365594304, 5.148502694627439702 ) ) ;
#39845 = CARTESIAN_POINT ( 'NONE',  ( -50.40829686548195099, -151.0000000013656063, -1.485763867205728284 ) ) ;
#39846 = CARTESIAN_POINT ( 'NONE',  ( 5.000000000000000888, -64.58333333333332860, 2.886751345948126879 ) ) ;
#39847 = CARTESIAN_POINT ( 'NONE',  ( 3.152801135295366208, -150.8125000013655779, 3.152801135295367985 ) ) ;
#39848 = CARTESIAN_POINT ( 'NONE',  ( -4.458734124999998549, -48.47916666530106511, 2.574251347313722516 ) ) ;
#39849 = CARTESIAN_POINT ( 'NONE',  ( 5.000000000000000888, -23.58333333333333215, 2.886751345948126879 ) ) ;
#39850 = CARTESIAN_POINT ( 'NONE',  ( 3.535533905932738197, -161.8750000000000284, -3.535533905932738197 ) ) ;
#39851 = CARTESIAN_POINT ( 'NONE',  ( -5.000000000000000000, 11.00000000000000000, 0.000000000000000000 ) ) ;
#39852 = CARTESIAN_POINT ( 'NONE',  ( -51.60603307380591787, -128.1875000013656063, -2.891590998281053704 ) ) ;
#39853 = CARTESIAN_POINT ( 'NONE',  ( -4.458734124999999437, -10.64583333196773829, -2.574251347313719407 ) ) ;
#39854 = CARTESIAN_POINT ( 'NONE',  ( 4.458734125000001214, -47.14583333196774362, 2.574251347313718519 ) ) ;
#39855 = CARTESIAN_POINT ( 'NONE',  ( 3.061616997868383141E-16, -165.8750000027312126, -5.000000000000000000 ) ) ;
#39856 = CARTESIAN_POINT ( 'NONE',  ( -4.458734124999999437, -144.9375000013656063, -5.460374474430324690E-16 ) ) ;
#39857 = CARTESIAN_POINT ( 'NONE',  ( -4.458734124999999437, -86.56249999863439371, 0.000000000000000000 ) ) ;
#39858 = CARTESIAN_POINT ( 'NONE',  ( -59.81910112700027327, -150.1875000000000000, -2.462841084822540605 ) ) ;
#39859 = EDGE_LOOP ( 'NONE', ( #40903, #61914, #2094, #13762 ) ) ;
#39860 = CARTESIAN_POINT ( 'NONE',  ( -6.972266317189433020E-16, 13.87500000273118594, -5.000000000000000000 ) ) ;
#39861 = DIRECTION ( 'NONE',  ( 0.000000000000000000, 0.000000000000000000, 1.000000000000000000 ) ) ;
#39862 = CARTESIAN_POINT ( 'NONE',  ( -58.24261429053147765, -146.3750000027312126, -3.805975901505573855 ) ) ;
#39863 = FACE_OUTER_BOUND ( 'NONE', #3001, .T. ) ;
#39864 = ORIENTED_EDGE ( 'NONE', *, *, #42915, .T. ) ;
#39865 = CARTESIAN_POINT ( 'NONE',  ( 2.229367062499998831, 5.354166668032261711, -3.861377020970580887 ) ) ;
#39866 = CARTESIAN_POINT ( 'NONE',  ( 1.339745962155612702, -50.16965819600732601, -5.000000000000000000 ) ) ;
#39867 = CARTESIAN_POINT ( 'NONE',  ( 4.458734125000001214, -16.14583333196773651, 2.574251347313718519 ) ) ;
#39868 = CARTESIAN_POINT ( 'NONE',  ( -5.000000000000000000, -100.8749999972688158, 0.000000000000000000 ) ) ;
#39869 = CARTESIAN_POINT ( 'NONE',  ( -4.458734124999999437, -1.395833331967737179, -2.574251347313719407 ) ) ;
#39870 = CARTESIAN_POINT ( 'NONE',  ( 6.123233995736766282E-16, -120.0000000000000000, -5.000000000000000000 ) ) ;
#39871 = CARTESIAN_POINT ( 'NONE',  ( 1.846868145590736310, -147.6250000013655779, 4.458734124999997661 ) ) ;
#39872 = VECTOR ( 'NONE', #8563, 1000.000000000000000 ) ;
#39873 =( BOUNDED_CURVE ( )  B_SPLINE_CURVE ( 2, ( #42615, #29065, #48690, #13350, #9765, #24255, #43858, #53837, #63505 ),
 .UNSPECIFIED., .F., .F. ) 
 B_SPLINE_CURVE_WITH_KNOTS ( ( 3, 2, 2, 2, 3 ),
 ( 0.1482142857142857151, 0.1488095238095238082, 0.1499999999999999944, 0.1511904761904761807, 0.1517857142857143016 ),
 .UNSPECIFIED. ) 
 CURVE ( )  GEOMETRIC_REPRESENTATION_ITEM ( )  RATIONAL_B_SPLINE_CURVE ( ( 0.9330127018922194093, 0.9330127018922194093, 1.000000000000000000, 0.8660254037844387076, 1.000000000000000000, 0.8660254037844387076, 1.000000000000000000, 0.9330127018922178550, 0.9330127018922194093 ) ) 
 REPRESENTATION_ITEM ( '' )  );
#39874 = CARTESIAN_POINT ( 'NONE',  ( 2.229367062499998831, 13.10416666803226171, -3.861377020970580887 ) ) ;
#39875 = VERTEX_POINT ( 'NONE', #58605 ) ;
#39876 = CARTESIAN_POINT ( 'NONE',  ( -4.458734124999999437, -96.31249999863440792, 0.000000000000000000 ) ) ;
#39877 = CARTESIAN_POINT ( 'NONE',  ( -5.000000000000000000, -18.87499999726881583, 0.000000000000000000 ) ) ;
#39878 = CARTESIAN_POINT ( 'NONE',  ( 2.500000000000000444, 7.216878364870322748, -7.063244554130000630 ) ) ;
#39879 = CARTESIAN_POINT ( 'NONE',  ( 9.457646018065525792E-16, -16.06249999863440436, 5.148502694627439702 ) ) ;
#39880 = AXIS2_PLACEMENT_3D ( 'NONE', #28145, #37810, #17565 ) ;
#39881 = CARTESIAN_POINT ( 'NONE',  ( -49.85088928181150436, -143.5625000000000568, -1.666127454062680480 ) ) ;
#39882 = DIRECTION ( 'NONE',  ( 0.000000000000000000, 0.000000000000000000, 1.000000000000000000 ) ) ;
#39883 = CARTESIAN_POINT ( 'NONE',  ( -57.19623071787017210, -151.3750000013656063, 4.297418129356382899 ) ) ;
#39884 = CARTESIAN_POINT ( 'NONE',  ( 5.000000000000000000, -43.37499999726880873, -6.123233995736766282E-16 ) ) ;
#39885 = CARTESIAN_POINT ( 'NONE',  ( 1.339745962155612702, -74.29465819873853150, -5.000000000000000000 ) ) ;
#39886 = CARTESIAN_POINT ( 'NONE',  ( -2.229367062499996610, 15.85416666803226171, 3.861377020970582219 ) ) ;
#39887 = CARTESIAN_POINT ( 'NONE',  ( -5.000000000000000000, -89.95833333060214443, -2.886751345948128211 ) ) ;
#39888 = CARTESIAN_POINT ( 'NONE',  ( 4.458734124999999437, 15.18750000136559564, -5.460374474430324690E-16 ) ) ;
#39889 = CARTESIAN_POINT ( 'NONE',  ( -4.458734124999998549, -61.22916666530106511, 2.574251347313722516 ) ) ;
#39890 = VERTEX_POINT ( 'NONE', #9079 ) ;
#39891 = CARTESIAN_POINT ( 'NONE',  ( 2.229367062499998831, -13.89583333196774184, -3.861377020970580887 ) ) ;
#39892 = CARTESIAN_POINT ( 'NONE',  ( -5.000000000000000000, 2.999999999999999112, 0.000000000000000000 ) ) ;
#39893 = CARTESIAN_POINT ( 'NONE',  ( 3.152801135295366208, -163.5625000013656063, 3.152801135295367985 ) ) ;
#39894 = CARTESIAN_POINT ( 'NONE',  ( 1.975475456537005874E-15, -63.62499999726880873, 5.000000000000000000 ) ) ;
#39895 = CARTESIAN_POINT ( 'NONE',  ( -4.458734124999998549, -51.22916666530107221, 2.574251347313722516 ) ) ;
#39896 = CARTESIAN_POINT ( 'NONE',  ( -2.499999999999996447, -88.70833333060214443, 4.330127018922195425 ) ) ;
#39897 = CARTESIAN_POINT ( 'NONE',  ( -3.152548672688508926E-16, -31.56249999863440436, -5.148502694627439702 ) ) ;
#39898 = AXIS2_PLACEMENT_3D ( 'NONE', #12921, #17449, #17757 ) ;
#39899 = FACE_OUTER_BOUND ( 'NONE', #30722, .T. ) ;
#39900 = DIRECTION ( 'NONE',  ( -0.000000000000000000, -1.000000000000000000, -0.000000000000000000 ) ) ;
#39901 = CARTESIAN_POINT ( 'NONE',  ( 0.000000000000000000, 0.000000000000000000, -9.999999999999998224 ) ) ;
#39902 = DIRECTION ( 'NONE',  ( -0.000000000000000000, 1.000000000000000000, -0.000000000000000000 ) ) ;
#39903 = CARTESIAN_POINT ( 'NONE',  ( -3.152801135295367985, -153.0625000013656063, 3.152801135295367096 ) ) ;
#39904 = CARTESIAN_POINT ( 'NONE',  ( -4.999999999999999112, -43.91666666666665719, 2.886751345948131764 ) ) ;
#39905 = CARTESIAN_POINT ( 'NONE',  ( 5.000000000000000888, -46.58333333333334991, 2.886751345948126879 ) ) ;
#39906 = CARTESIAN_POINT ( 'NONE',  ( 5.000000000000000888, -6.458333330602150646, 2.886751345948126879 ) ) ;
#39907 = VERTEX_POINT ( 'NONE', #28688 ) ;
#39908 = CARTESIAN_POINT ( 'NONE',  ( -3.152548672688508926E-16, -101.5624999986344221, -5.148502694627439702 ) ) ;
#39909 = CARTESIAN_POINT ( 'NONE',  ( -2.229367062499996610, 3.604166668032260379, 3.861377020970582219 ) ) ;
#39910 = CARTESIAN_POINT ( 'NONE',  ( -1.339745962155610925, -8.669658196007331341, 5.000000000000000000 ) ) ;
#39911 = CARTESIAN_POINT ( 'NONE',  ( 1.060575238724906964E-15, -4.749999999999997335, 5.773502691896257311 ) ) ;
#39912 = CARTESIAN_POINT ( 'NONE',  ( 2.229367062499998831, -65.64583333196773651, -3.861377020970580887 ) ) ;
#39913 = CARTESIAN_POINT ( 'NONE',  ( -5.000000000000000000, -30.87499999726881228, 0.000000000000000000 ) ) ;
#39914 = CARTESIAN_POINT ( 'NONE',  ( 2.500000000000002220, -4.541666663935479242, 4.330127018922192761 ) ) ;
#39916 = VERTEX_POINT ( 'NONE', #48308 ) ;
#39915 = CARTESIAN_POINT ( 'NONE',  ( -4.458734124999998549, -32.22916666530106511, 2.574251347313722516 ) ) ;
#39917 = CARTESIAN_POINT ( 'NONE',  ( -1.339745962155610925, -81.79465819873850307, 5.000000000000000000 ) ) ;
#39918 = CARTESIAN_POINT ( 'NONE',  ( 0.000000000000000000, 0.000000000000000000, 0.000000000000000000 ) ) ;
#39919 = ORIENTED_EDGE ( 'NONE', *, *, #39366, .T. ) ;
#39920 = CARTESIAN_POINT ( 'NONE',  ( 1.339745962155612702, -101.2946581987385031, -5.000000000000000000 ) ) ;
#39921 = CARTESIAN_POINT ( 'NONE',  ( 5.000000000000000000, -48.50000000000000000, -6.123233995736766282E-16 ) ) ;
#39923 = CARTESIAN_POINT ( 'NONE',  ( -4.458734124999999437, -23.64583333196773651, -2.574251347313719407 ) ) ;
#39922 = CARTESIAN_POINT ( 'NONE',  ( -6.972266317189433020E-16, -46.12499999726880873, -5.000000000000000000 ) ) ;
#39924 = VECTOR ( 'NONE', #13036, 1000.000000000000000 ) ;
#39925 = CARTESIAN_POINT ( 'NONE',  ( -1.339745962155613812, -4.205341801261476498, -5.000000000000000000 ) ) ;
#39926 = CARTESIAN_POINT ( 'NONE',  ( -2.229367062500000163, -75.47916666530106511, -3.861377020970580443 ) ) ;
#39927 = CARTESIAN_POINT ( 'NONE',  ( -4.458734125000001214, -142.1250000013656063, 1.846868145590734089 ) ) ;
#39928 = CARTESIAN_POINT ( 'NONE',  ( 9.457646018065525792E-16, -81.06249999863440792, 5.148502694627439702 ) ) ;
#39929 = AXIS2_PLACEMENT_3D ( 'NONE', #1058, #6186, #10361 ) ;
#39930 = CARTESIAN_POINT ( 'NONE',  ( -53.51423613279429503, -139.5000000013656063, 4.591703134518082763 ) ) ;
#39931 = CARTESIAN_POINT ( 'NONE',  ( -4.458734124999999437, -29.56249999863440436, 0.000000000000000000 ) ) ;
#39932 = CARTESIAN_POINT ( 'NONE',  ( 1.060575238724906964E-15, -69.62499999726880162, 5.773502691896257311 ) ) ;
#39933 = ORIENTED_EDGE ( 'NONE', *, *, #4706, .T. ) ;
#39934 = CARTESIAN_POINT ( 'NONE',  ( -6.972266317189433020E-16, -83.12499999726878741, -5.000000000000000000 ) ) ;
#39935 = ORIENTED_EDGE ( 'NONE', *, *, #21651, .F. ) ;
#39936 = CARTESIAN_POINT ( 'NONE',  ( -2.229367062500000163, -70.72916666530107932, -3.861377020970580443 ) ) ;
#39937 = CARTESIAN_POINT ( 'NONE',  ( -50.75781946612335105, -135.0000000000005969, -1.372666862511563224 ) ) ;
#39938 = ORIENTED_EDGE ( 'NONE', *, *, #18881, .F. ) ;
#39939 = CARTESIAN_POINT ( 'NONE',  ( -6.972266317189433020E-16, 27.74999999999999645, -5.000000000000000000 ) ) ;
#39940 = CARTESIAN_POINT ( 'NONE',  ( 1.975475456537005874E-15, -65.62499999726881583, 5.000000000000000000 ) ) ;
#39941 = CARTESIAN_POINT ( 'NONE',  ( 4.458734124999999437, -60.06249999863440081, -5.460374474430324690E-16 ) ) ;
#39942 = CARTESIAN_POINT ( 'NONE',  ( 2.229367062500001939, -5.229166665301071326, 3.861377020970579999 ) ) ;
#39943 = ORIENTED_EDGE ( 'NONE', *, *, #51470, .T. ) ;
#39944 = CARTESIAN_POINT ( 'NONE',  ( -1.339745962155610925, -44.79465819873851018, 5.000000000000000000 ) ) ;
#39945 = CARTESIAN_POINT ( 'NONE',  ( -4.458734124999999437, 14.68750000136559386, 0.000000000000000000 ) ) ;
#39946 = CARTESIAN_POINT ( 'NONE',  ( -56.48576386720575471, -142.7500000013656063, -4.591703134518078322 ) ) ;
#39947 = CARTESIAN_POINT ( 'NONE',  ( 1.339745962155612702, -24.29465819873852084, -5.000000000000000000 ) ) ;
#39948 = CARTESIAN_POINT ( 'NONE',  ( 3.152801135295367541, -162.3125000013656063, -3.152801135295367541 ) ) ;
#39949 = LINE ( 'NONE', #59597, #39872 ) ;
#39950 = ORIENTED_EDGE ( 'NONE', *, *, #20766, .F. ) ;
#39951 = CARTESIAN_POINT ( 'NONE',  ( -4.458734124999999437, -79.31249999863440792, 0.000000000000000000 ) ) ;
#39952 = CARTESIAN_POINT ( 'NONE',  ( 6.123233995736766282E-16, -170.0000000000000000, -5.000000000000000000 ) ) ;
#39953 = CARTESIAN_POINT ( 'NONE',  ( 4.458734125000001214, 1.104166668032261711, 2.574251347313718519 ) ) ;
#39954 = CARTESIAN_POINT ( 'NONE',  ( 6.123233995736766282E-16, -170.0000000000000000, -5.000000000000000000 ) ) ;
#39955 =( BOUNDED_CURVE ( )  B_SPLINE_CURVE ( 2, ( #338, #54684, #5154, #34404, #10928, #1316, #5791, #35379, #14792 ),
 .UNSPECIFIED., .F., .F. ) 
 B_SPLINE_CURVE_WITH_KNOTS ( ( 3, 2, 2, 2, 3 ),
 ( 0.2229166666666666796, 0.2236111111111111216, 0.2250000000000000056, 0.2263888888888888895, 0.2270833333333333315 ),
 .UNSPECIFIED. ) 
 CURVE ( )  GEOMETRIC_REPRESENTATION_ITEM ( )  RATIONAL_B_SPLINE_CURVE ( ( 0.9330127018922194093, 0.9330127018922207416, 1.000000000000000000, 0.8660254037844387076, 1.000000000000000000, 0.8660254037844387076, 1.000000000000000000, 0.9330127018922194093, 0.9330127018922194093 ) ) 
 REPRESENTATION_ITEM ( '' )  );
#39956 = CARTESIAN_POINT ( 'NONE',  ( 1.060575238724906964E-15, -87.75000000000000000, 5.773502691896257311 ) ) ;
#39957 = CYLINDRICAL_SURFACE ( 'NONE', #45965, 5.000000000000000000 ) ;
#39958 = CARTESIAN_POINT ( 'NONE',  ( -4.458734124999999437, -67.56249999863440792, 0.000000000000000000 ) ) ;
#39959 = CARTESIAN_POINT ( 'NONE',  ( -5.000000000000000000, -23.95833333060214443, -2.886751345948128211 ) ) ;
#39960 = CARTESIAN_POINT ( 'NONE',  ( -5.000000000000000000, -15.08333333333333215, -2.886751345948128211 ) ) ;
#39961 = CARTESIAN_POINT ( 'NONE',  ( -3.152548672688508926E-16, 28.43750000136559564, -5.148502694627439702 ) ) ;
#39962 = CARTESIAN_POINT ( 'NONE',  ( 2.499999999999998668, -110.2083333306021444, -4.330127018922193649 ) ) ;
#39963 = CARTESIAN_POINT ( 'NONE',  ( 1.339745962155641346, -3.169658196007335782, -4.999999999999983125 ) ) ;
#39964 = CARTESIAN_POINT ( 'NONE',  ( 4.458734125000001214, -45.89583333196774362, 2.574251347313718519 ) ) ;
#39965 = PRODUCT_DEFINITION_SHAPE ( 'NONE', 'NONE',  #63678 ) ;
#39966 = CARTESIAN_POINT ( 'NONE',  ( -4.458734124999999437, -31.64583333196773651, -2.574251347313719407 ) ) ;
#39967 = CARTESIAN_POINT ( 'NONE',  ( -4.458734124999997661, 4.520833334698926897, 2.574251347313722516 ) ) ;
#39968 = VECTOR ( 'NONE', #42559, 1000.000000000000114 ) ;
#39969 = DIRECTION ( 'NONE',  ( 0.000000000000000000, 0.000000000000000000, 1.000000000000000000 ) ) ;
#39970 = CARTESIAN_POINT ( 'NONE',  ( -3.535250795749689387E-16, 19.74999999999999645, -5.773502691896257311 ) ) ;
#39971 = CARTESIAN_POINT ( 'NONE',  ( 3.535533905932738197, -144.0000000027311842, -3.535533905932738197 ) ) ;
#39972 = CARTESIAN_POINT ( 'NONE',  ( 5.000000000000000888, -54.45833333060214443, 2.886751345948126879 ) ) ;
#39973 = VECTOR ( 'NONE', #39659, 1000.000000000000000 ) ;
#39974 = CARTESIAN_POINT ( 'NONE',  ( -2.229367062500000163, -38.47916666530107221, -3.861377020970580443 ) ) ;
#39975 = CARTESIAN_POINT ( 'NONE',  ( -5.000000000000000000, -73.87499999726880162, 0.000000000000000000 ) ) ;
#39976 = CARTESIAN_POINT ( 'NONE',  ( -56.48576386720575471, -146.0000000013656347, -4.591703134518078322 ) ) ;
#39977 = CARTESIAN_POINT ( 'NONE',  ( 2.071067811865476394, -140.1875000000000000, 5.000000000000000000 ) ) ;
#39978 = CARTESIAN_POINT ( 'NONE',  ( -2.229367062499996610, -78.39583333196773651, 3.861377020970582219 ) ) ;
#39979 = CARTESIAN_POINT ( 'NONE',  ( 1.846868145590736310, -165.8750000013656063, 4.458734124999997661 ) ) ;
#39980 = CARTESIAN_POINT ( 'NONE',  ( 5.000000000000000000, 18.70833333606451632, -2.886751345948130876 ) ) ;
#39981 = CARTESIAN_POINT ( 'NONE',  ( 1.339745962155612702, 7.705341801261479162, -5.000000000000000000 ) ) ;
#39982 = CARTESIAN_POINT ( 'NONE',  ( -3.535250795749689387E-16, -29.25000000000000000, -5.773502691896257311 ) ) ;
#39983 = CARTESIAN_POINT ( 'NONE',  ( 4.458734125000000326, -144.3750000013656063, -1.846868145590734978 ) ) ;
#39984 = ORIENTED_EDGE ( 'NONE', *, *, #56157, .T. ) ;
#39985 = CARTESIAN_POINT ( 'NONE',  ( 2.229367062499998831, 25.10416666803225993, -3.861377020970580887 ) ) ;
#39986 = VERTEX_POINT ( 'NONE', #53764 ) ;
#39987 = CARTESIAN_POINT ( 'NONE',  ( -2.229367062500000163, -64.72916666530106511, -3.861377020970580443 ) ) ;
#39988 = CARTESIAN_POINT ( 'NONE',  ( 1.060575238724906964E-15, 22.37500000273118772, 5.773502691896257311 ) ) ;
#39989 = CARTESIAN_POINT ( 'NONE',  ( -6.324555320336760822, 15.00000000000000000, 8.999999999999998224 ) ) ;
#39990 = CARTESIAN_POINT ( 'NONE',  ( 1.060575238724906964E-15, 14.25000000000000178, 5.773502691896257311 ) ) ;
#39991 = ADVANCED_FACE ( 'NONE', ( #43479 ), #9386, .T. ) ;
#39992 = CARTESIAN_POINT ( 'NONE',  ( 4.458734125000000326, -48.89583333196772941, 2.574251347313718519 ) ) ;
#39993 = CARTESIAN_POINT ( 'NONE',  ( 9.457646018065525792E-16, -10.06249999863440792, 5.148502694627439702 ) ) ;
#39994 = CARTESIAN_POINT ( 'NONE',  ( -6.972266317189433020E-16, 13.74999999999999822, -5.000000000000000000 ) ) ;
#39995 = CARTESIAN_POINT ( 'NONE',  ( -6.972266317189433020E-16, -60.12499999726880162, -5.000000000000000000 ) ) ;
#39996 = CARTESIAN_POINT ( 'NONE',  ( -1.339745962155610925, -61.79465819873851729, 5.000000000000000000 ) ) ;
#39997 = CARTESIAN_POINT ( 'NONE',  ( 5.000000000000000000, -66.37499999726881583, -6.123233995736766282E-16 ) ) ;
#39999 = CARTESIAN_POINT ( 'NONE',  ( 4.458734125000001214, -23.89583333196774007, 2.574251347313718519 ) ) ;
#39998 = CARTESIAN_POINT ( 'NONE',  ( -2.498395430326213474E-14, 15.25000000000000000, 5.000000000000000000 ) ) ;
#40000 = CARTESIAN_POINT ( 'NONE',  ( 1.975475456537005874E-15, -32.74999999999999289, 5.000000000000000000 ) ) ;
#40001 = CARTESIAN_POINT ( 'NONE',  ( -2.229367062499996610, -52.14583333196773651, 3.861377020970582219 ) ) ;
#40002 = CARTESIAN_POINT ( 'NONE',  ( 3.152801135295366208, -157.8125000013656063, 3.152801135295367985 ) ) ;
#40003 = ADVANCED_FACE ( 'NONE', ( #4883 ), #24505, .T. ) ;
#40004 = CARTESIAN_POINT ( 'NONE',  ( -2.500000000000000444, -54.04166666393548013, -4.330127018922193649 ) ) ;
#40005 = ORIENTED_EDGE ( 'NONE', *, *, #16664, .T. ) ;
#40006 = CARTESIAN_POINT ( 'NONE',  ( 2.500000000000002220, 13.33333333333333215, 4.330127018922192761 ) ) ;
#40008 = ADVANCED_FACE ( 'NONE', ( #11610 ), #25784, .T. ) ;
#40007 = CARTESIAN_POINT ( 'NONE',  ( 2.229367062499998831, 6.104166668032262599, -3.861377020970580887 ) ) ;
#40009 = ORIENTED_EDGE ( 'NONE', *, *, #39634, .F. ) ;
#40011 = CARTESIAN_POINT ( 'NONE',  ( 5.000000000000000000, -9.374999997268814056, -6.123233995736766282E-16 ) ) ;
#40010 = CARTESIAN_POINT ( 'NONE',  ( -5.000000000000000000, -28.08333333333333925, -2.886751345948128211 ) ) ;
#40012 = CARTESIAN_POINT ( 'NONE',  ( -1.846868145590734756, -157.1250000013656063, -4.458734125000000326 ) ) ;
#40013 = ORIENTED_EDGE ( 'NONE', *, *, #47653, .T. ) ;
#40014 =( GEOMETRIC_REPRESENTATION_CONTEXT ( 3 ) GLOBAL_UNCERTAINTY_ASSIGNED_CONTEXT ( ( #24272 ) ) GLOBAL_UNIT_ASSIGNED_CONTEXT ( ( #7698, #27301, #21852 ) ) REPRESENTATION_CONTEXT ( 'NONE', 'WORKASPACE' ) );
#40015 = CARTESIAN_POINT ( 'NONE',  ( 5.000000000000000000, -87.37499999726880162, -6.123233995736766282E-16 ) ) ;
#40016 = CARTESIAN_POINT ( 'NONE',  ( -50.01589407740564042, -129.6250000000000284, 0.3983568153799778022 ) ) ;
#40018 = VECTOR ( 'NONE', #27122, 1000.000000000000227 ) ;
#40017 = CARTESIAN_POINT ( 'NONE',  ( 2.071067811865391572, -160.9375000027312126, -5.000000000000086153 ) ) ;
#40019 = CARTESIAN_POINT ( 'NONE',  ( 4.458734125000001214, -42.14583333196773651, 2.574251347313718519 ) ) ;
#40020 = ORIENTED_EDGE ( 'NONE', *, *, #37079, .F. ) ;
#40021 = DIRECTION ( 'NONE',  ( -0.000000000000000000, 1.000000000000000000, -0.000000000000000000 ) ) ;
#40022 = CARTESIAN_POINT ( 'NONE',  ( -3.152548672688508926E-16, 15.43750000136559564, -5.148502694627439702 ) ) ;
#40023 = CARTESIAN_POINT ( 'NONE',  ( 2.229367062500001939, -89.22916666530106511, 3.861377020970579999 ) ) ;
#40024 = CARTESIAN_POINT ( 'NONE',  ( -54.60164318462004474, -124.5000000027311984, -4.984105922594373794 ) ) ;
#40025 = CARTESIAN_POINT ( 'NONE',  ( 1.339745962155612702, 12.83034180399266511, -5.000000000000000000 ) ) ;
#40026 = CARTESIAN_POINT ( 'NONE',  ( 1.339745962155612702, -61.16965819600733312, -5.000000000000000000 ) ) ;
#40027 =( BOUNDED_CURVE ( )  B_SPLINE_CURVE ( 2, ( #29848, #16021, #49480, #25992, #40139, #54946, #25681, #6387, #11193 ),
 .UNSPECIFIED., .F., .F. ) 
 B_SPLINE_CURVE_WITH_KNOTS ( ( 3, 2, 2, 2, 3 ),
 ( 0.9660714285714285809, 0.9666666666666666741, 0.9678571428571428603, 0.9690476190476190466, 0.9696428571428571397 ),
 .UNSPECIFIED. ) 
 CURVE ( )  GEOMETRIC_REPRESENTATION_ITEM ( )  RATIONAL_B_SPLINE_CURVE ( ( 0.9330127018922194093, 0.9330127018922194093, 1.000000000000000000, 0.8660254037844387076, 1.000000000000000000, 0.8660254037844387076, 1.000000000000000000, 0.9330127018922194093, 0.9330127018922194093 ) ) 
 REPRESENTATION_ITEM ( '' )  );
#40028 = DIRECTION ( 'NONE',  ( -0.000000000000000000, 1.000000000000000000, -0.000000000000000000 ) ) ;
#40029 = CARTESIAN_POINT ( 'NONE',  ( 4.458734124999999437, -67.81249999863440792, -5.460374474430324690E-16 ) ) ;
#40030 = CARTESIAN_POINT ( 'NONE',  ( -1.339745962155589165, 9.919658201469706782, -5.000000000000014211 ) ) ;
#40031 = CARTESIAN_POINT ( 'NONE',  ( -3.152548672688508926E-16, 17.43750000136559564, -5.148502694627439702 ) ) ;
#40032 = CARTESIAN_POINT ( 'NONE',  ( -1.339745962155613812, 6.794658198738520838, -5.000000000000000000 ) ) ;
#40033 = CARTESIAN_POINT ( 'NONE',  ( 2.229367062499998831, -46.89583333196774362, -3.861377020970580887 ) ) ;
#40034 = ADVANCED_FACE ( 'NONE', ( #45395 ), #5844, .T. ) ;
#40035 = CARTESIAN_POINT ( 'NONE',  ( -4.999999999999999112, -10.79166666393547658, 2.886751345948131764 ) ) ;
#40036 = CARTESIAN_POINT ( 'NONE',  ( -60.14911071818854538, -145.0625000000000284, 1.666127454062681146 ) ) ;
#40037 = DIRECTION ( 'NONE',  ( -0.000000000000000000, 1.000000000000000000, -0.000000000000000000 ) ) ;
#40038 = CARTESIAN_POINT ( 'NONE',  ( -4.458734124999998549, -88.47916666530107932, 2.574251347313722516 ) ) ;
#40039 = DIRECTION ( 'NONE',  ( 0.000000000000000000, 0.000000000000000000, 1.000000000000000000 ) ) ;
#40040 = CARTESIAN_POINT ( 'NONE',  ( -4.458734124999999437, -16.56249999863440436, 0.000000000000000000 ) ) ;
#40041 = ORIENTED_EDGE ( 'NONE', *, *, #23178, .F. ) ;
#40042 = DIRECTION ( 'NONE',  ( -0.000000000000000000, 1.000000000000000000, -0.000000000000000000 ) ) ;
#40043 = CARTESIAN_POINT ( 'NONE',  ( 2.229367062500001939, -101.9791666653010651, 3.861377020970579999 ) ) ;
#40044 = CARTESIAN_POINT ( 'NONE',  ( -9.184850993605147944E-16, -161.3750000027311842, 5.000000000000000000 ) ) ;
#40045 = ORIENTED_EDGE ( 'NONE', *, *, #18522, .T. ) ;
#40046 = CARTESIAN_POINT ( 'NONE',  ( -2.229367062500000163, -96.72916666530105090, -3.861377020970580443 ) ) ;
#40047 = CARTESIAN_POINT ( 'NONE',  ( -1.049326080737009628E-13, -19.75000000000000000, 5.000000000000000000 ) ) ;
#40048 = CARTESIAN_POINT ( 'NONE',  ( 5.000000000000000000, -59.37499999726880873, -6.123233995736766282E-16 ) ) ;
#40049 = CARTESIAN_POINT ( 'NONE',  ( 1.339745962155615144, -62.58034179853028434, 4.999999999999999112 ) ) ;
#40050 = CARTESIAN_POINT ( 'NONE',  ( -50.70258187064364108, -126.1250000013656205, 2.196230717870141014 ) ) ;
#40051 = CARTESIAN_POINT ( 'NONE',  ( -56.48576386720575471, -141.7500000013656063, -4.591703134518078322 ) ) ;
#40052 = CARTESIAN_POINT ( 'NONE',  ( 4.458734125000000326, -16.89583333196773651, 2.574251347313718519 ) ) ;
#40053 = CARTESIAN_POINT ( 'NONE',  ( -2.229367062500000163, 6.270833334698928674, -3.861377020970580443 ) ) ;
#40054 = CARTESIAN_POINT ( 'NONE',  ( 4.458734124999998549, -65.97916666530106511, -2.574251347313721627 ) ) ;
#40055 = LINE ( 'NONE', #34275, #7964 ) ;
#40056 = CARTESIAN_POINT ( 'NONE',  ( -4.458734124999999437, -19.31249999863440081, 0.000000000000000000 ) ) ;
#40057 = CARTESIAN_POINT ( 'NONE',  ( 6.123233995736766282E-16, -120.0000000000000000, -5.000000000000000000 ) ) ;
#40058 = CARTESIAN_POINT ( 'NONE',  ( 5.000000000000000000, -155.0000000000000284, 0.000000000000000000 ) ) ;
#40059 = CARTESIAN_POINT ( 'NONE',  ( -3.535250795749689387E-16, -13.24999999999999822, -5.773502691896257311 ) ) ;
#40060 = CARTESIAN_POINT ( 'NONE',  ( 4.458734125000000326, -154.3750000013655779, -1.846868145590734978 ) ) ;
#40061 = ORIENTED_EDGE ( 'NONE', *, *, #41769, .T. ) ;
#40062 = CARTESIAN_POINT ( 'NONE',  ( -2.229367062499996610, -44.39583333196774362, 3.861377020970582219 ) ) ;
#40063 =( BOUNDED_CURVE ( )  B_SPLINE_CURVE ( 2, ( #44629, #14721, #589, #39166, #4756, #15373, #9897, #5081, #48506 ),
 .UNSPECIFIED., .F., .F. ) 
 B_SPLINE_CURVE_WITH_KNOTS ( ( 3, 2, 2, 2, 3 ),
 ( 0.6937499999999999778, 0.6944444444444444198, 0.6958333333333333037, 0.6972222222222221877, 0.6979166666666666297 ),
 .UNSPECIFIED. ) 
 CURVE ( )  GEOMETRIC_REPRESENTATION_ITEM ( )  RATIONAL_B_SPLINE_CURVE ( ( 0.9330127018922194093, 0.9330127018922194093, 1.000000000000000000, 0.8660254037844387076, 1.000000000000000000, 0.8660254037844387076, 1.000000000000000000, 0.9330127018922194093, 0.9330127018922194093 ) ) 
 REPRESENTATION_ITEM ( '' )  );
#40064 = CARTESIAN_POINT ( 'NONE',  ( 1.975475456537005874E-15, -66.74999999999998579, 5.000000000000000000 ) ) ;
#40065 = CARTESIAN_POINT ( 'NONE',  ( 1.975475456537005874E-15, -38.62499999726880873, 5.000000000000000000 ) ) ;
#40066 = CARTESIAN_POINT ( 'NONE',  ( -2.499999999999996447, 29.16666666666666785, 4.330127018922195425 ) ) ;
#40067 = AXIS2_PLACEMENT_3D ( 'NONE', #1727, #25512, #11350 ) ;
#40068 = EDGE_CURVE ( 'NONE', #25319, #40086, #17446, .T. ) ;
#40069 = CARTESIAN_POINT ( 'NONE',  ( 9.457646018065525792E-16, 4.937500001365596525, 5.148502694627439702 ) ) ;
#40070 = FACE_OUTER_BOUND ( 'NONE', #62823, .T. ) ;
#40071 = CARTESIAN_POINT ( 'NONE',  ( -5.000000000000000888, -165.5625000027312126, 2.071067811865474617 ) ) ;
#40072 = CARTESIAN_POINT ( 'NONE',  ( -1.339745962155610925, -73.79465819873853150, 5.000000000000000000 ) ) ;
#40073 = CARTESIAN_POINT ( 'NONE',  ( -2.229367062500000163, 21.27083333469892779, -3.861377020970580443 ) ) ;
#40074 = CARTESIAN_POINT ( 'NONE',  ( 1.060575238724906964E-15, -75.75000000000000000, 5.773502691896257311 ) ) ;
#40075 = CARTESIAN_POINT ( 'NONE',  ( 5.000000000000000888, 8.541666669397853795, 2.886751345948126879 ) ) ;
#40076 = ORIENTED_EDGE ( 'NONE', *, *, #20596, .F. ) ;
#40077 = DIRECTION ( 'NONE',  ( -0.000000000000000000, 1.000000000000000000, -0.000000000000000000 ) ) ;
#40078 = ORIENTED_EDGE ( 'NONE', *, *, #5119, .F. ) ;
#40079 = CARTESIAN_POINT ( 'NONE',  ( -2.499999999999996447, -53.70833333060213732, 4.330127018922195425 ) ) ;
#40080 = CARTESIAN_POINT ( 'NONE',  ( 4.458734124999999437, -40.81249999863440081, -5.460374474430324690E-16 ) ) ;
#40081 = CARTESIAN_POINT ( 'NONE',  ( 2.500000000000002220, -38.54166666393548013, 4.330127018922192761 ) ) ;
#40082 = ORIENTED_EDGE ( 'NONE', *, *, #91, .F. ) ;
#40084 = EDGE_CURVE ( 'NONE', #10009, #22588, #41278, .T. ) ;
#40083 = CARTESIAN_POINT ( 'NONE',  ( 4.458734125000001214, -10.89583333196773651, 2.574251347313718519 ) ) ;
#40086 = VERTEX_POINT ( 'NONE', #1670 ) ;
#40085 = CARTESIAN_POINT ( 'NONE',  ( 9.457646018065525792E-16, -21.31249999863440081, 5.148502694627439702 ) ) ;
#40087 = CARTESIAN_POINT ( 'NONE',  ( 2.500000000000002220, -82.66666666666667140, 4.330127018922192761 ) ) ;
#40088 = CARTESIAN_POINT ( 'NONE',  ( 3.152801135295366208, -166.5625000013656063, 3.152801135295367985 ) ) ;
#40089 = EDGE_CURVE ( 'NONE', #57423, #62194, #8054, .T. ) ;
#40090 = CARTESIAN_POINT ( 'NONE',  ( -4.458734124999999437, -61.64583333196773651, -2.574251347313719407 ) ) ;
#40091 = CARTESIAN_POINT ( 'NONE',  ( -3.535250795749689387E-16, -89.12499999726880162, -5.773502691896257311 ) ) ;
#40093 = ORIENTED_EDGE ( 'NONE', *, *, #39338, .T. ) ;
#40092 = CYLINDRICAL_SURFACE ( 'NONE', #2594, 5.000000000000000000 ) ;
#40094 = CARTESIAN_POINT ( 'NONE',  ( -57.46284108482265651, -139.9375000000000284, 4.819101127000239515 ) ) ;
#40095 = CARTESIAN_POINT ( 'NONE',  ( -4.458734124999998549, -25.47916666530106866, 2.574251347313722516 ) ) ;
#40096 = FACE_OUTER_BOUND ( 'NONE', #27420, .T. ) ;
#40097 = ORIENTED_EDGE ( 'NONE', *, *, #23930, .F. ) ;
#40098 = SHAPE_DEFINITION_REPRESENTATION ( #14783, #21293 ) ;
#40099 = CARTESIAN_POINT ( 'NONE',  ( 1.846868145590735200, -164.5000000013655779, -4.458734125000000326 ) ) ;
#40100 = CARTESIAN_POINT ( 'NONE',  ( 4.458734125000001214, 29.10416666803225993, 2.574251347313718519 ) ) ;
#40101 = CARTESIAN_POINT ( 'NONE',  ( 5.000000000000000888, -155.9375000000000000, -2.071067811865475505 ) ) ;
#40102 = ORIENTED_EDGE ( 'NONE', *, *, #12586, .F. ) ;
#40103 = CARTESIAN_POINT ( 'NONE',  ( -57.19623071787016499, -145.6250000013655779, 4.297418129356382899 ) ) ;
#40104 =( GEOMETRIC_REPRESENTATION_CONTEXT ( 3 ) GLOBAL_UNCERTAINTY_ASSIGNED_CONTEXT ( ( #43308 ) ) GLOBAL_UNIT_ASSIGNED_CONTEXT ( ( #13100, #23071, #61061 ) ) REPRESENTATION_CONTEXT ( 'NONE', 'WORKASPACE' ) );
#40105 = CARTESIAN_POINT ( 'NONE',  ( -4.458734124999999437, -76.56249999863440792, 0.000000000000000000 ) ) ;
#40106 = CARTESIAN_POINT ( 'NONE',  ( -57.46284108482265651, -136.0625000027311842, 4.819101127000239515 ) ) ;
#40107 = CARTESIAN_POINT ( 'NONE',  ( -2.229367062500000163, -44.47916666530106511, -3.861377020970580443 ) ) ;
#40108 = CARTESIAN_POINT ( 'NONE',  ( 4.458734124999999437, -140.6250000013656063, -1.846868145590734978 ) ) ;
#40109 = DIRECTION ( 'NONE',  ( 0.000000000000000000, 0.000000000000000000, 1.000000000000000000 ) ) ;
#40110 = CARTESIAN_POINT ( 'NONE',  ( -4.458734124999999437, -50.39583333196772941, -2.574251347313719407 ) ) ;
#40111 = VECTOR ( 'NONE', #47817, 1000.000000000000000 ) ;
#40112 = LINE ( 'NONE', #6043, #3955 ) ;
#40113 = EDGE_CURVE ( 'NONE', #1919, #19582, #63462, .T. ) ;
#40114 = CARTESIAN_POINT ( 'NONE',  ( 4.458734124999998549, -15.72916666530107399, -2.574251347313721627 ) ) ;
#40115 = CARTESIAN_POINT ( 'NONE',  ( -4.999999999999999112, -102.9166666666666714, 2.886751345948131764 ) ) ;
#40116 = CARTESIAN_POINT ( 'NONE',  ( 3.061616997868383141E-16, -167.7500000000000000, -5.000000000000000000 ) ) ;
#40117 = CARTESIAN_POINT ( 'NONE',  ( 4.458734124999998549, -32.97916666530106511, -2.574251347313721627 ) ) ;
#40118 = CARTESIAN_POINT ( 'NONE',  ( 2.500000000000002220, 4.458333336064518093, 4.330127018922192761 ) ) ;
#40119 = CARTESIAN_POINT ( 'NONE',  ( -4.999999999999998224, -52.91666666666666430, 2.886751345948131764 ) ) ;
#40120 = CARTESIAN_POINT ( 'NONE',  ( -57.89159099828107458, -127.6875000013656063, -3.393966926194107447 ) ) ;
#40121 = CARTESIAN_POINT ( 'NONE',  ( -2.229367062499996610, -76.39583333196773651, 3.861377020970582219 ) ) ;
#40122 = CARTESIAN_POINT ( 'NONE',  ( -58.24261429053147765, -154.2500000000000284, -3.805975901505573855 ) ) ;
#40123 = CARTESIAN_POINT ( 'NONE',  ( -4.999999999999998224, -0.7916666639354794643, 2.886751345948131764 ) ) ;
#40124 = DIRECTION ( 'NONE',  ( 0.000000000000000000, 0.000000000000000000, 1.000000000000000000 ) ) ;
#40125 = CARTESIAN_POINT ( 'NONE',  ( 4.458734124999999437, -1.062499998634405696, -5.460374474430324690E-16 ) ) ;
#40126 = ORIENTED_EDGE ( 'NONE', *, *, #56171, .F. ) ;
#40127 = DIRECTION ( 'NONE',  ( 0.000000000000000000, 1.000000000000000000, 0.000000000000000000 ) ) ;
#40128 = LINE ( 'NONE', #49781, #27769 ) ;
#40130 = CARTESIAN_POINT ( 'NONE',  ( 4.458734124999999437, -35.81249999863440792, -5.460374474430324690E-16 ) ) ;
#40129 = CARTESIAN_POINT ( 'NONE',  ( -4.458734124999999437, -85.39583333196773651, -2.574251347313719407 ) ) ;
#40131 = CARTESIAN_POINT ( 'NONE',  ( 1.339745962155612702, -9.294658198738520838, -5.000000000000000000 ) ) ;
#40132 = CARTESIAN_POINT ( 'NONE',  ( -3.152548672688508926E-16, -83.81249999863439371, -5.148502694627439702 ) ) ;
#40133 = CARTESIAN_POINT ( 'NONE',  ( 2.229367062499998831, 16.10416666803225993, -3.861377020970580887 ) ) ;
#40134 = CARTESIAN_POINT ( 'NONE',  ( 2.499999999999998668, -77.20833333060214443, -4.330127018922193649 ) ) ;
#40135 = CARTESIAN_POINT ( 'NONE',  ( -51.60603307380591787, -137.9375000013656063, -2.891590998281053704 ) ) ;
#40136 = CARTESIAN_POINT ( 'NONE',  ( -3.152548672688508926E-16, -0.5624999986344053626, -5.148502694627439702 ) ) ;
#40137 = CARTESIAN_POINT ( 'NONE',  ( 4.458734125000001214, 22.85416666803225993, 2.574251347313718519 ) ) ;
#40138 = CARTESIAN_POINT ( 'NONE',  ( 2.229367062500001939, -46.22916666530106511, 3.861377020970579999 ) ) ;
#40139 = CARTESIAN_POINT ( 'NONE',  ( 5.000000000000000000, -105.5000000000000142, -6.123233995736766282E-16 ) ) ;
#40140 = CARTESIAN_POINT ( 'NONE',  ( -2.229367062500000163, -83.47916666530106511, -3.861377020970580443 ) ) ;
#40141 = CARTESIAN_POINT ( 'NONE',  ( -4.458734124999999437, -6.312499998634403475, 0.000000000000000000 ) ) ;
#40142 = ORIENTED_EDGE ( 'NONE', *, *, #20488, .T. ) ;
#40143 = CARTESIAN_POINT ( 'NONE',  ( 4.458734124999998549, -30.97916666530106866, -2.574251347313721627 ) ) ;
#40144 = CARTESIAN_POINT ( 'NONE',  ( -50.40829686548195099, -132.2500000013656063, -1.485763867205728284 ) ) ;
#40145 = CARTESIAN_POINT ( 'NONE',  ( 4.458734124999998549, -73.72916666530106511, -2.574251347313721627 ) ) ;
#40146 = CARTESIAN_POINT ( 'NONE',  ( 5.000000000000000000, -108.3749999972688016, -6.123233995736766282E-16 ) ) ;
#40147 =( BOUNDED_CURVE ( )  B_SPLINE_CURVE ( 2, ( #59179, #14781, #59504, #5463, #10918, #15113, #10596, #10287, #39541 ),
 .UNSPECIFIED., .F., .F. ) 
 B_SPLINE_CURVE_WITH_KNOTS ( ( 3, 2, 2, 2, 3 ),
 ( 0.4410714285714285587, 0.4416666666666666519, 0.4428571428571428381, 0.4440476190476190244, 0.4446428571428571175 ),
 .UNSPECIFIED. ) 
 CURVE ( )  GEOMETRIC_REPRESENTATION_ITEM ( )  RATIONAL_B_SPLINE_CURVE ( ( 0.9330127018922194093, 0.9330127018922194093, 1.000000000000000000, 0.8660254037844387076, 1.000000000000000000, 0.8660254037844387076, 1.000000000000000000, 0.9330127018922194093, 0.9330127018922194093 ) ) 
 REPRESENTATION_ITEM ( '' )  );
#40148 = CARTESIAN_POINT ( 'NONE',  ( -3.152548672688508926E-16, 26.43750000136559208, -5.148502694627439702 ) ) ;
#40149 = EDGE_CURVE ( 'NONE', #14229, #30563, #46030, .T. ) ;
#40150 = EDGE_CURVE ( 'NONE', #37814, #45194, #31554, .T. ) ;
#40151 = FACE_OUTER_BOUND ( 'NONE', #52258, .T. ) ;
#40152 = CYLINDRICAL_SURFACE ( 'NONE', #8047, 5.000000000000000000 ) ;
#40153 = CARTESIAN_POINT ( 'NONE',  ( -4.458734124999999437, -78.64583333196773651, -2.574251347313719407 ) ) ;
#40154 = CARTESIAN_POINT ( 'NONE',  ( 5.000000000000000888, -58.58333333333333570, 2.886751345948126879 ) ) ;
#40155 = EDGE_CURVE ( 'NONE', #13355, #11557, #4282, .T. ) ;
#40156 = FACE_OUTER_BOUND ( 'NONE', #3026, .T. ) ;
#40157 = CARTESIAN_POINT ( 'NONE',  ( -4.999999999999999112, 26.20833333606451632, 2.886751345948131764 ) ) ;
#40158 = VERTEX_POINT ( 'NONE', #56650 ) ;
#40159 = CARTESIAN_POINT ( 'NONE',  ( 2.499999999999998668, -1.208333330602148870, -4.330127018922193649 ) ) ;
#40160 = EDGE_CURVE ( 'NONE', #2538, #14167, #31870, .T. ) ;
#40161 = CARTESIAN_POINT ( 'NONE',  ( -2.500000000000000444, -99.16666666666665719, -4.330127018922193649 ) ) ;
#40163 = CARTESIAN_POINT ( 'NONE',  ( 1.060575238724906964E-15, -17.75000000000000355, 5.773502691896257311 ) ) ;
#40162 = DIRECTION ( 'NONE',  ( -0.000000000000000000, 1.000000000000000000, -0.000000000000000000 ) ) ;
#40164 = CARTESIAN_POINT ( 'NONE',  ( -2.229367062499996610, -23.14583333196773651, 3.861377020970582219 ) ) ;
#40165 = EDGE_CURVE ( 'NONE', #52605, #39254, #23998, .T. ) ;
#40166 = CARTESIAN_POINT ( 'NONE',  ( -4.458734124999999437, -84.39583333196773651, -2.574251347313719407 ) ) ;
#40167 = EDGE_CURVE ( 'NONE', #14751, #51146, #32651, .T. ) ;
#40168 =( BOUNDED_CURVE ( )  B_SPLINE_CURVE ( 2, ( #59614, #15546, #35167, #54782, #10713, #30320, #49942, #40613, #37077 ),
 .UNSPECIFIED., .F., .F. ) 
 B_SPLINE_CURVE_WITH_KNOTS ( ( 3, 2, 2, 2, 3 ),
 ( 0.2416666666666668628, 0.2458333333333335147, 0.2500000000000002220, 0.2541666666666668739, 0.2583333333333335813 ),
 .UNSPECIFIED. ) 
 CURVE ( )  GEOMETRIC_REPRESENTATION_ITEM ( )  RATIONAL_B_SPLINE_CURVE ( ( 0.9999999999999964473, 0.9238795325112902912, 1.000000000000000000, 0.9238795325112867385, 1.000000000000000000, 0.9238795325112867385, 1.000000000000000000, 0.9238795325112826307, 1.000000000000003997 ) ) 
 REPRESENTATION_ITEM ( '' )  );
#40169 = CARTESIAN_POINT ( 'NONE',  ( 5.000000000000000888, -24.45833333060214088, 2.886751345948126879 ) ) ;
#40170 = VECTOR ( 'NONE', #44073, 1000.000000000000000 ) ;
#40172 = ORIENTED_EDGE ( 'NONE', *, *, #38919, .F. ) ;
#40171 = CARTESIAN_POINT ( 'NONE',  ( 2.229367062499998831, -51.64583333196773651, -3.861377020970580887 ) ) ;
#40173 = CARTESIAN_POINT ( 'NONE',  ( 5.000000000000000000, -65.50000000000000000, -6.123233995736766282E-16 ) ) ;
#40174 = CARTESIAN_POINT ( 'NONE',  ( -2.499999999999996447, 11.29166666939785202, 4.330127018922195425 ) ) ;
#40175 = EDGE_CURVE ( 'NONE', #18747, #53481, #5984, .T. ) ;
#40177 = ORIENTED_EDGE ( 'NONE', *, *, #41053, .F. ) ;
#40176 = CARTESIAN_POINT ( 'NONE',  ( -4.458734124999998549, -5.479166665301072214, 2.574251347313722516 ) ) ;
#40178 = CARTESIAN_POINT ( 'NONE',  ( -59.29741812935640155, -149.6250000013655779, -2.196230717870135685 ) ) ;
#40179 = CARTESIAN_POINT ( 'NONE',  ( -2.500000000000000444, -66.16666666666667140, -4.330127018922193649 ) ) ;
#40180 = ADVANCED_FACE ( 'NONE', ( #7440 ), #27988, .T. ) ;
#40181 = CARTESIAN_POINT ( 'NONE',  ( 1.846868145590736310, -153.8750000013655779, 4.458734124999999437 ) ) ;
#40182 = CARTESIAN_POINT ( 'NONE',  ( 2.229367062499998831, -46.89583333196774362, -3.861377020970580887 ) ) ;
#40183 = CARTESIAN_POINT ( 'NONE',  ( -5.000000000000000000, -76.95833333060214443, -2.886751345948128211 ) ) ;
#40184 = CARTESIAN_POINT ( 'NONE',  ( -5.000000000000000888, -157.5625000000000568, -2.071067811865475949 ) ) ;
#40185 = EDGE_CURVE ( 'NONE', #24668, #36016, #45801, .T. ) ;
#40186 = ADVANCED_FACE ( 'NONE', ( #43093 ), #41831, .T. ) ;
#40187 = CARTESIAN_POINT ( 'NONE',  ( -54.60164318462004474, -152.3750000000000284, -4.984105922594373794 ) ) ;
#40188 = CARTESIAN_POINT ( 'NONE',  ( 9.457646018065525792E-16, -12.31249999863440259, 5.148502694627439702 ) ) ;
#40189 = CARTESIAN_POINT ( 'NONE',  ( -2.229367062500000163, -47.72916666530106511, -3.861377020970580443 ) ) ;
#40190 = CARTESIAN_POINT ( 'NONE',  ( 5.000000000000000888, -89.58333333333332860, 2.886751345948126879 ) ) ;
#40191 = CARTESIAN_POINT ( 'NONE',  ( 1.846868145590735200, -146.2500000013656063, -4.458734125000000326 ) ) ;
#40192 = CARTESIAN_POINT ( 'NONE',  ( -2.229367062500000163, -92.72916666530106511, -3.861377020970580443 ) ) ;
#40193 = CARTESIAN_POINT ( 'NONE',  ( -55.39835681537999790, -149.8750000000000284, 4.984105922594378235 ) ) ;
#40194 = ORIENTED_EDGE ( 'NONE', *, *, #63242, .F. ) ;
#40195 = DIRECTION ( 'NONE',  ( -0.6485228581062915110, 0.000000000000000000, -0.7611951803011149931 ) ) ;
#40196 = CARTESIAN_POINT ( 'NONE',  ( 4.458734124999998549, 27.02083333469892423, -2.574251347313721627 ) ) ;
#40197 = CARTESIAN_POINT ( 'NONE',  ( -52.53715891517739323, -145.5625000027312126, -4.819101127000233298 ) ) ;
#40198 = CARTESIAN_POINT ( 'NONE',  ( 0.000000000000000000, 0.000000000000000000, 0.000000000000000000 ) ) ;
#40199 = ORIENTED_EDGE ( 'NONE', *, *, #59045, .F. ) ;
#40200 = CARTESIAN_POINT ( 'NONE',  ( 2.229367062499998831, -0.6458333319677399542, -3.861377020970580887 ) ) ;
#40201 = CARTESIAN_POINT ( 'NONE',  ( 1.339745962155612702, 6.705341801261480050, -5.000000000000000000 ) ) ;
#40202 = CARTESIAN_POINT ( 'NONE',  ( 4.458734124999998549, -17.97916666530106866, -2.574251347313721627 ) ) ;
#40203 = CARTESIAN_POINT ( 'NONE',  ( -1.339745962155613812, -101.2053418012614827, -5.000000000000000000 ) ) ;
#40204 = CARTESIAN_POINT ( 'NONE',  ( 4.458734124999999437, -9.812499998634406140, -5.460374474430324690E-16 ) ) ;
#40205 = LINE ( 'NONE', #39870, #5929 ) ;
#40206 = CARTESIAN_POINT ( 'NONE',  ( -8.190561711645485556E-16, -147.6875000013656063, 4.458734124999999437 ) ) ;
#40207 = CARTESIAN_POINT ( 'NONE',  ( -2.229367062499996610, 17.60416666803225993, 3.861377020970582219 ) ) ;
#40208 = ORIENTED_EDGE ( 'NONE', *, *, #33158, .T. ) ;
#40209 = CARTESIAN_POINT ( 'NONE',  ( -2.499999999999996447, -26.70833333060214798, 4.330127018922195425 ) ) ;
#40210 = CARTESIAN_POINT ( 'NONE',  ( 6.123233995736766282E-16, -120.0000000000000000, -5.000000000000000000 ) ) ;
#40211 = CARTESIAN_POINT ( 'NONE',  ( 9.457646018065525792E-16, -20.06249999863440081, 5.148502694627439702 ) ) ;
#40212 = AXIS2_PLACEMENT_3D ( 'NONE', #36779, #56412, #37106 ) ;
#40213 = CARTESIAN_POINT ( 'NONE',  ( 5.000000000000000000, -25.37499999726881583, -6.123233995736766282E-16 ) ) ;
#40214 = CARTESIAN_POINT ( 'NONE',  ( -6.972266317189433020E-16, -6.249999999999999112, -5.000000000000000000 ) ) ;
#40215 = CARTESIAN_POINT ( 'NONE',  ( -54.64476657466781973, -147.8125000013656063, -4.444560631937228834 ) ) ;
#40216 = CARTESIAN_POINT ( 'NONE',  ( 1.060575238724906964E-15, -48.62499999726881583, 5.773502691896257311 ) ) ;
#40217 = CARTESIAN_POINT ( 'NONE',  ( 5.000000000000000000, -74.41666666666665719, -2.886751345948130876 ) ) ;
#40218 = CARTESIAN_POINT ( 'NONE',  ( -2.229367062499996610, 14.85416666803226171, 3.861377020970582219 ) ) ;
#40219 = DIRECTION ( 'NONE',  ( -0.000000000000000000, 1.000000000000000000, -0.000000000000000000 ) ) ;
#40220 = PRODUCT_DEFINITION ( 'UNKNOWN', '', #56491, #23827 ) ;
#40221 = DIRECTION ( 'NONE',  ( -0.000000000000000000, 1.000000000000000000, -0.000000000000000000 ) ) ;
#40222 = CARTESIAN_POINT ( 'NONE',  ( 4.458734124999999437, 13.18750000136559208, -5.460374474430324690E-16 ) ) ;
#40223 = CARTESIAN_POINT ( 'NONE',  ( 4.458734124999999437, -64.81249999863440792, -5.460374474430324690E-16 ) ) ;
#40224 = ORIENTED_EDGE ( 'NONE', *, *, #28689, .T. ) ;
#40225 = CARTESIAN_POINT ( 'NONE',  ( 2.229367062499998831, -12.89583333196774007, -3.861377020970580887 ) ) ;
#40226 =( BOUNDED_CURVE ( )  B_SPLINE_CURVE ( 2, ( #28674, #23861, #43464, #19340, #53751, #9374, #38634, #33822, #53441 ),
 .UNSPECIFIED., .F., .F. ) 
 B_SPLINE_CURVE_WITH_KNOTS ( ( 3, 2, 2, 2, 3 ),
 ( 0.4916666666666670849, 0.4958333333333337922, 0.5000000000000004441, 0.5041666666666670960, 0.5083333333333337478 ),
 .UNSPECIFIED. ) 
 CURVE ( )  GEOMETRIC_REPRESENTATION_ITEM ( )  RATIONAL_B_SPLINE_CURVE ( ( 0.9999999999999918954, 0.9238795325112948431, 1.000000000000000000, 0.9238795325112867385, 1.000000000000000000, 0.9238795325112867385, 1.000000000000000000, 0.9238795325112786339, 1.000000000000008216 ) ) 
 REPRESENTATION_ITEM ( '' )  );
#40227 = CARTESIAN_POINT ( 'NONE',  ( -4.999999999999999112, 6.083333333333333037, 2.886751345948131764 ) ) ;
#40228 = CARTESIAN_POINT ( 'NONE',  ( -4.458734124999999437, -163.9375000013655779, -5.460374474430324690E-16 ) ) ;
#40229 = CARTESIAN_POINT ( 'NONE',  ( -5.000000000000000000, -37.99999999999999289, 0.000000000000000000 ) ) ;
#40230 = CARTESIAN_POINT ( 'NONE',  ( -4.458734124999998549, -56.22916666530107221, 2.574251347313722516 ) ) ;
#40231 = CARTESIAN_POINT ( 'NONE',  ( 2.499999999999998668, -91.20833333060214443, -4.330127018922193649 ) ) ;
#40232 = CARTESIAN_POINT ( 'NONE',  ( 4.458734124999998549, -34.72916666530107221, -2.574251347313721627 ) ) ;
#40233 = FACE_OUTER_BOUND ( 'NONE', #172, .T. ) ;
#40234 = CARTESIAN_POINT ( 'NONE',  ( 0.000000000000000000, -120.0000000000000000, 0.000000000000000000 ) ) ;
#40235 = CARTESIAN_POINT ( 'NONE',  ( -52.53715891517739323, -151.5625000027312126, -4.819101127000233298 ) ) ;
#40236 = CARTESIAN_POINT ( 'NONE',  ( -6.972266317189433020E-16, -83.12499999726878741, -5.000000000000000000 ) ) ;
#40237 = CARTESIAN_POINT ( 'NONE',  ( 3.152801135295367541, -149.5625000013655779, -3.152801135295367541 ) ) ;
#40238 = CARTESIAN_POINT ( 'NONE',  ( 5.000000000000000000, -42.41666666666667140, -2.886751345948129988 ) ) ;
#40239 = CARTESIAN_POINT ( 'NONE',  ( 1.975475456537005874E-15, 20.24999999999999645, 5.000000000000000000 ) ) ;
#40240 = CARTESIAN_POINT ( 'NONE',  ( -57.11050704595625405, -135.0000000000000000, -4.001714258895231247 ) ) ;
#40241 = EDGE_LOOP ( 'NONE', ( #22295, #1377, #56431, #24589 ) ) ;
#40242 = CARTESIAN_POINT ( 'NONE',  ( -4.458734124999999437, -107.3124999986343937, 0.000000000000000000 ) ) ;
#40243 = CARTESIAN_POINT ( 'NONE',  ( -2.229367062499996610, 4.604166668032261711, 3.861377020970582219 ) ) ;
#40244 = CARTESIAN_POINT ( 'NONE',  ( -1.339745962155610925, -96.66965819600731891, 5.000000000000000000 ) ) ;
#40245 = CARTESIAN_POINT ( 'NONE',  ( -2.500000000000000444, -1.166666666666666519, -4.330127018922193649 ) ) ;
#40246 = CARTESIAN_POINT ( 'NONE',  ( -3.152548672688508926E-16, -64.56249999863440792, -5.148502694627439702 ) ) ;
#40247 = DIRECTION ( 'NONE',  ( -0.000000000000000000, 1.000000000000000000, -0.000000000000000000 ) ) ;
#40248 = CARTESIAN_POINT ( 'NONE',  ( 5.000000000000000000, -6.374999997268812280, -6.123233995736766282E-16 ) ) ;
#40250 = VERTEX_POINT ( 'NONE', #12881 ) ;
#40249 = CARTESIAN_POINT ( 'NONE',  ( -4.458734124999999437, -34.39583333196772941, -2.574251347313719407 ) ) ;
#40251 = CYLINDRICAL_SURFACE ( 'NONE', #28635, 5.000000000000000000 ) ;
#40252 = CARTESIAN_POINT ( 'NONE',  ( 1.339745962155615144, -6.705341801261480050, 4.999999999999999112 ) ) ;
#40253 = VERTEX_POINT ( 'NONE', #23491 ) ;
#40254 = CARTESIAN_POINT ( 'NONE',  ( -6.972266317189433020E-16, -101.2499999999999858, -5.000000000000000000 ) ) ;
#40255 = CARTESIAN_POINT ( 'NONE',  ( 1.060575238724906964E-15, -47.75000000000000000, 5.773502691896257311 ) ) ;
#40256 = ADVANCED_FACE ( 'NONE', ( #17082 ), #61474, .T. ) ;
#40257 = CARTESIAN_POINT ( 'NONE',  ( -3.152548672688508926E-16, -31.81249999863440792, -5.148502694627439702 ) ) ;
#40258 = CARTESIAN_POINT ( 'NONE',  ( 2.500000000000002220, -32.54166666393547303, 4.330127018922192761 ) ) ;
#40259 = CARTESIAN_POINT ( 'NONE',  ( -2.229367062500000163, -73.47916666530106511, -3.861377020970580443 ) ) ;
#40260 = CARTESIAN_POINT ( 'NONE',  ( 3.152801135295367541, -141.5625000013655779, -3.152801135295367541 ) ) ;
#40261 = CARTESIAN_POINT ( 'NONE',  ( -4.458734124999998549, -82.22916666530107932, 2.574251347313722516 ) ) ;
#40262 = CARTESIAN_POINT ( 'NONE',  ( -59.59170313451811296, -134.7500000013656063, 1.485763867205729394 ) ) ;
#40263 = CARTESIAN_POINT ( 'NONE',  ( -2.229367062500000163, -27.72916666530107221, -3.861377020970580443 ) ) ;
#40264 = EDGE_CURVE ( 'NONE', #62694, #54373, #52131, .T. ) ;
#40265 = VERTEX_POINT ( 'NONE', #24427 ) ;
#40266 = LINE ( 'NONE', #6183, #23830 ) ;
#40267 = ORIENTED_EDGE ( 'NONE', *, *, #35281, .T. ) ;
#40268 = CARTESIAN_POINT ( 'NONE',  ( 2.229367062500001939, -79.22916666530106511, 3.861377020970579999 ) ) ;
#40269 = CARTESIAN_POINT ( 'NONE',  ( 2.499999999999998668, -21.33333333333333570, -4.330127018922193649 ) ) ;
#40270 = ORIENTED_EDGE ( 'NONE', *, *, #35079, .F. ) ;
#40271 = VECTOR ( 'NONE', #35134, 1000.000000000000000 ) ;
#40272 = DIRECTION ( 'NONE',  ( 0.000000000000000000, 1.000000000000000000, 0.000000000000000000 ) ) ;
#40273 =( BOUNDED_CURVE ( )  B_SPLINE_CURVE ( 2, ( #24218, #43825, #14557, #5556, #29029, #53489, #24862, #48653, #113 ),
 .UNSPECIFIED., .F., .F. ) 
 B_SPLINE_CURVE_WITH_KNOTS ( ( 3, 2, 2, 2, 3 ),
 ( 0.2089285714285714357, 0.2095238095238095288, 0.2107142857142857151, 0.2119047619047619013, 0.2124999999999999944 ),
 .UNSPECIFIED. ) 
 CURVE ( )  GEOMETRIC_REPRESENTATION_ITEM ( )  RATIONAL_B_SPLINE_CURVE ( ( 0.9330127018922194093, 0.9330127018922194093, 1.000000000000000000, 0.8660254037844387076, 1.000000000000000000, 0.8660254037844387076, 1.000000000000000000, 0.9330127018922194093, 0.9330127018922194093 ) ) 
 REPRESENTATION_ITEM ( '' )  );
#40274 = LINE ( 'NONE', #19695, #56869 ) ;
#40275 = CARTESIAN_POINT ( 'NONE',  ( -2.229367062500000163, -66.72916666530106511, -3.861377020970580443 ) ) ;
#40276 = CARTESIAN_POINT ( 'NONE',  ( 9.457646018065525792E-16, -1.312499998634405918, 5.148502694627439702 ) ) ;
#40277 = ORIENTED_EDGE ( 'NONE', *, *, #13801, .T. ) ;
#40278 = CARTESIAN_POINT ( 'NONE',  ( -6.972266317189433020E-16, -45.24999999999999289, -5.000000000000000000 ) ) ;
#40279 = CARTESIAN_POINT ( 'NONE',  ( 0.000000000000000000, -170.0000000000000000, 0.000000000000000000 ) ) ;
#40280 = CARTESIAN_POINT ( 'NONE',  ( 4.458734125000001214, 10.10416666803226171, 2.574251347313718519 ) ) ;
#40281 = CARTESIAN_POINT ( 'NONE',  ( -52.10840900171896806, -140.1875000013656063, 3.393966926194110556 ) ) ;
#40282 = CYLINDRICAL_SURFACE ( 'NONE', #41862, 5.000000000000000000 ) ;
#40283 = CARTESIAN_POINT ( 'NONE',  ( 3.152801135295367541, -161.3125000013656063, -3.152801135295367541 ) ) ;
#40284 = CARTESIAN_POINT ( 'NONE',  ( 1.975475456537005874E-15, -21.62499999726880873, 5.000000000000000000 ) ) ;
#40285 = ORIENTED_EDGE ( 'NONE', *, *, #7942, .F. ) ;
#40286 = CARTESIAN_POINT ( 'NONE',  ( 4.458734124999999437, -80.81249999863440792, -5.460374474430324690E-16 ) ) ;
#40287 = CARTESIAN_POINT ( 'NONE',  ( -6.972266317189433020E-16, -60.24999999999999289, -5.000000000000000000 ) ) ;
#40288 = CARTESIAN_POINT ( 'NONE',  ( 9.457646018065525792E-16, -5.062499998634401699, 5.148502694627439702 ) ) ;
#40289 = DIRECTION ( 'NONE',  ( -0.000000000000000000, 1.000000000000000000, -0.000000000000000000 ) ) ;
#40290 = DIRECTION ( 'NONE',  ( 0.000000000000000000, 0.000000000000000000, 1.000000000000000000 ) ) ;
#40291 = CARTESIAN_POINT ( 'NONE',  ( 2.229367062500001939, -72.22916666530107932, 3.861377020970579999 ) ) ;
#40292 = CARTESIAN_POINT ( 'NONE',  ( 2.499999999999998668, -31.20833333060214443, -4.330127018922193649 ) ) ;
#40293 = DIRECTION ( 'NONE',  ( -0.000000000000000000, 1.000000000000000000, -0.000000000000000000 ) ) ;
#40294 = CARTESIAN_POINT ( 'NONE',  ( 1.339745962155615144, -78.58034179853028434, 4.999999999999999112 ) ) ;
#40295 = CARTESIAN_POINT ( 'NONE',  ( -6.972266317189433020E-16, -45.24999999999999289, -5.000000000000000000 ) ) ;
#40296 = CARTESIAN_POINT ( 'NONE',  ( 5.000000000000000000, -82.37499999726881583, -6.123233995736766282E-16 ) ) ;
#40297 = CARTESIAN_POINT ( 'NONE',  ( -4.458734124999998549, -44.22916666530106511, 2.574251347313722516 ) ) ;
#40298 = CARTESIAN_POINT ( 'NONE',  ( -4.458734124999999437, -33.56249999863440792, 0.000000000000000000 ) ) ;
#40299 = CARTESIAN_POINT ( 'NONE',  ( -3.152548672688508926E-16, 2.187500001365593416, -5.148502694627439702 ) ) ;
#40300 = CARTESIAN_POINT ( 'NONE',  ( 3.535533905932738197, -150.8750000000000000, -3.535533905932738197 ) ) ;
#40301 = CARTESIAN_POINT ( 'NONE',  ( 1.060575238724906964E-15, 20.24999999999999645, 5.773502691896257311 ) ) ;
#40302 = CARTESIAN_POINT ( 'NONE',  ( -9.184850993605147944E-16, -146.3750000027312126, 5.000000000000000000 ) ) ;
#40303 = CARTESIAN_POINT ( 'NONE',  ( -6.972266317189433020E-16, -84.24999999999998579, -5.000000000000000000 ) ) ;
#40304 = CARTESIAN_POINT ( 'NONE',  ( -4.458734124999999437, -43.31249999863440081, 0.000000000000000000 ) ) ;
#40305 = CARTESIAN_POINT ( 'NONE',  ( 5.000000000000000000, -72.29166666393547303, -2.886751345948129988 ) ) ;
#40306 = CARTESIAN_POINT ( 'NONE',  ( -57.89159099828107458, -142.9375000013656063, -3.393966926194107447 ) ) ;
#40307 = CARTESIAN_POINT ( 'NONE',  ( -6.972266317189433020E-16, -70.12499999726880162, -5.000000000000000000 ) ) ;
#40308 = EDGE_CURVE ( 'NONE', #32593, #58460, #49503, .T. ) ;
#40309 = DIRECTION ( 'NONE',  ( -0.000000000000000000, 1.000000000000000000, -0.000000000000000000 ) ) ;
#40310 = CARTESIAN_POINT ( 'NONE',  ( -2.229367062499996610, -81.39583333196773651, 3.861377020970582219 ) ) ;
#40311 = CARTESIAN_POINT ( 'NONE',  ( 3.152801135295366208, -160.8125000013656063, 3.152801135295367985 ) ) ;
#40312 = CARTESIAN_POINT ( 'NONE',  ( -5.000000000000000888, -160.4375000000000568, 2.071067811865474617 ) ) ;
#40313 = CARTESIAN_POINT ( 'NONE',  ( -3.093533885184598375, -6.874201416485457017, -7.446478553994068328 ) ) ;
#40314 = CARTESIAN_POINT ( 'NONE',  ( -5.000000000000000000, -25.08333333333333215, -2.886751345948128211 ) ) ;
#40315 = CARTESIAN_POINT ( 'NONE',  ( 4.458734125000000326, -140.3750000013656063, -1.846868145590734978 ) ) ;
#40316 = ORIENTED_EDGE ( 'NONE', *, *, #2776, .F. ) ;
#40317 = CARTESIAN_POINT ( 'NONE',  ( -2.229367062500000163, 23.27083333469892779, -3.861377020970580443 ) ) ;
#40318 = ORIENTED_EDGE ( 'NONE', *, *, #38227, .T. ) ;
#40319 = CARTESIAN_POINT ( 'NONE',  ( -4.458734124999997661, -60.47916666530106511, 2.574251347313722516 ) ) ;
#40320 = CARTESIAN_POINT ( 'NONE',  ( 2.500000000000002220, 21.45833333606451987, 4.330127018922192761 ) ) ;
#40321 = CARTESIAN_POINT ( 'NONE',  ( -1.339745962155727277, -60.66965819600734022, 4.999999999999933387 ) ) ;
#40322 = CARTESIAN_POINT ( 'NONE',  ( -5.000000000000000000, 11.91666666666666607, -2.886751345948128211 ) ) ;
#40323 = CARTESIAN_POINT ( 'NONE',  ( -3.152548672688508926E-16, -48.56249999863440792, -5.148502694627439702 ) ) ;
#40324 = CARTESIAN_POINT ( 'NONE',  ( -4.458734124999999437, -12.31249999863440259, 0.000000000000000000 ) ) ;
#40325 = CARTESIAN_POINT ( 'NONE',  ( 7.894705354777835637, 0.7527931906242791849, -7.590204373988219011 ) ) ;
#40326 = CARTESIAN_POINT ( 'NONE',  ( 1.975475456537005874E-15, -66.74999999999998579, 5.000000000000000000 ) ) ;
#40327 = DIRECTION ( 'NONE',  ( 0.000000000000000000, 0.000000000000000000, 1.000000000000000000 ) ) ;
#40328 = CARTESIAN_POINT ( 'NONE',  ( -2.229367062499996610, -13.39583333196774007, 3.861377020970582219 ) ) ;
#40329 = CARTESIAN_POINT ( 'NONE',  ( 5.000000000000000000, -139.1250000027312126, 0.000000000000000000 ) ) ;
#40330 = CARTESIAN_POINT ( 'NONE',  ( -2.229367062499996610, -60.14583333196774362, 3.861377020970582219 ) ) ;
#40331 = CARTESIAN_POINT ( 'NONE',  ( 1.846868145590735200, -157.5000000013656063, -4.458734125000000326 ) ) ;
#40332 = CARTESIAN_POINT ( 'NONE',  ( 2.499999999999998668, -55.20833333060214443, -4.330127018922193649 ) ) ;
#40333 = ORIENTED_EDGE ( 'NONE', *, *, #27967, .F. ) ;
#40334 = DIRECTION ( 'NONE',  ( 1.000000000000000000, 0.000000000000000000, 0.000000000000000000 ) ) ;
#40335 = CARTESIAN_POINT ( 'NONE',  ( 2.229367062499998831, -0.8958333319677401763, -3.861377020970580887 ) ) ;
#40336 = ORIENTED_EDGE ( 'NONE', *, *, #53716, .F. ) ;
#40337 = CARTESIAN_POINT ( 'NONE',  ( -6.972266317189433020E-16, -4.124999997268814056, -5.000000000000000000 ) ) ;
#40338 = CARTESIAN_POINT ( 'NONE',  ( 1.846868145590735200, -155.2500000013656063, -4.458734125000000326 ) ) ;
#40339 = ORIENTED_EDGE ( 'NONE', *, *, #53535, .F. ) ;
#40340 = CARTESIAN_POINT ( 'NONE',  ( 1.339745962155612702, 25.70534180126147916, -5.000000000000000000 ) ) ;
#40341 = CARTESIAN_POINT ( 'NONE',  ( -58.24261429053147765, -129.2500000000000284, -3.805975901505573855 ) ) ;
#40342 = CARTESIAN_POINT ( 'NONE',  ( 1.339745962155612702, -80.16965819600733312, -5.000000000000000000 ) ) ;
#40343 = CARTESIAN_POINT ( 'NONE',  ( -3.152548672688508926E-16, -50.81249999863440792, -5.148502694627439702 ) ) ;
#40344 = EDGE_LOOP ( 'NONE', ( #49402, #25166, #30257, #35374 ) ) ;
#40345 =( BOUNDED_CURVE ( )  B_SPLINE_CURVE ( 2, ( #35704, #1625, #19938, #55331, #39550, #59191, #11248, #660, #20269 ),
 .UNSPECIFIED., .F., .F. ) 
 B_SPLINE_CURVE_WITH_KNOTS ( ( 3, 2, 2, 2, 3 ),
 ( 0.1729166666666666630, 0.1736111111111111049, 0.1749999999999999889, 0.1763888888888889006, 0.1770833333333333426 ),
 .UNSPECIFIED. ) 
 CURVE ( )  GEOMETRIC_REPRESENTATION_ITEM ( )  RATIONAL_B_SPLINE_CURVE ( ( 0.9330127018922194093, 0.9330127018922194093, 1.000000000000000000, 0.8660254037844387076, 1.000000000000000000, 0.8660254037844387076, 1.000000000000000000, 0.9330127018922194093, 0.9330127018922194093 ) ) 
 REPRESENTATION_ITEM ( '' )  );
#40346 = CARTESIAN_POINT ( 'NONE',  ( 75.00000000000000000, 0.000000000000000000, 8.999999999999998224 ) ) ;
#40347 = CARTESIAN_POINT ( 'NONE',  ( 9.457646018065525792E-16, 14.93750000136559564, 5.148502694627439702 ) ) ;
#40348 = CARTESIAN_POINT ( 'NONE',  ( -4.458734124999998549, 27.77083333469892423, 2.574251347313722516 ) ) ;
#40349 = CARTESIAN_POINT ( 'NONE',  ( -55.35523342533222291, -153.3125000013656063, 4.444560631937231499 ) ) ;
#40350 = CARTESIAN_POINT ( 'NONE',  ( 3.061616997868383141E-16, -146.7500000000000284, -5.000000000000000000 ) ) ;
#40351 = DIRECTION ( 'NONE',  ( -0.000000000000000000, 1.000000000000000000, -0.000000000000000000 ) ) ;
#40352 = DIRECTION ( 'NONE',  ( 0.000000000000000000, 0.000000000000000000, 1.000000000000000000 ) ) ;
#40353 = CARTESIAN_POINT ( 'NONE',  ( 9.457646018065525792E-16, -65.06249999863440792, 5.148502694627439702 ) ) ;
#40354 = CARTESIAN_POINT ( 'NONE',  ( -2.499999999999996447, 1.166666666666666519, 4.330127018922195425 ) ) ;
#40355 = CARTESIAN_POINT ( 'NONE',  ( -2.229367062500000163, 20.52083333469892779, -3.861377020970580443 ) ) ;
#40356 = EDGE_CURVE ( 'NONE', #51312, #55230, #9626, .T. ) ;
#40357 = CARTESIAN_POINT ( 'NONE',  ( -2.500000000000000444, 17.83333333333333215, -4.330127018922193649 ) ) ;
#40358 = DIRECTION ( 'NONE',  ( -0.000000000000000000, 1.000000000000000000, -0.000000000000000000 ) ) ;
#40359 = CARTESIAN_POINT ( 'NONE',  ( -4.458734124999999437, -54.64583333196774362, -2.574251347313719407 ) ) ;
#40360 = CARTESIAN_POINT ( 'NONE',  ( -5.000000000000000000, -6.958333330602150646, -2.886751345948128211 ) ) ;
#40361 = CARTESIAN_POINT ( 'NONE',  ( -2.499999999999996447, 25.16666666666666430, 4.330127018922195425 ) ) ;
#40362 = CARTESIAN_POINT ( 'NONE',  ( -6.000000000000000000, -114.9999999999999858, 1.499999999999999556 ) ) ;
#40363 = CARTESIAN_POINT ( 'NONE',  ( 4.458734124999999437, -90.06249999863440792, -5.460374474430324690E-16 ) ) ;
#40364 = CYLINDRICAL_SURFACE ( 'NONE', #61451, 5.000000000000000000 ) ;
#40365 = CARTESIAN_POINT ( 'NONE',  ( -4.458734124999999437, -18.64583333196774362, -2.574251347313719407 ) ) ;
#40366 = ORIENTED_EDGE ( 'NONE', *, *, #25351, .F. ) ;
#40367 = CARTESIAN_POINT ( 'NONE',  ( 5.000000000000000000, -31.50000000000000000, -6.123233995736766282E-16 ) ) ;
#40368 = CARTESIAN_POINT ( 'NONE',  ( 9.457646018065525792E-16, -106.0624999986343795, 5.148502694627439702 ) ) ;
#40369 = CARTESIAN_POINT ( 'NONE',  ( 2.071067811865475505, -155.9375000027312126, -5.000000000000000888 ) ) ;
#40370 = ORIENTED_EDGE ( 'NONE', *, *, #21609, .F. ) ;
#40371 = CARTESIAN_POINT ( 'NONE',  ( -4.458734124999998549, -98.47916666530105090, 2.574251347313722516 ) ) ;
#40372 = CARTESIAN_POINT ( 'NONE',  ( 2.229367062499998831, -28.64583333196774007, -3.861377020970580887 ) ) ;
#40373 = CARTESIAN_POINT ( 'NONE',  ( -5.000000000000000000, -58.87499999726880873, 0.000000000000000000 ) ) ;
#40374 = CARTESIAN_POINT ( 'NONE',  ( 5.000000000000000888, -62.45833333060213732, 2.886751345948126879 ) ) ;
#40375 = CARTESIAN_POINT ( 'NONE',  ( -50.40829686548195099, -127.0000000013656063, -1.485763867205728284 ) ) ;
#40376 = CARTESIAN_POINT ( 'NONE',  ( -59.59170313451810586, -144.5000000013656063, 1.485763867205729394 ) ) ;
#40377 = CARTESIAN_POINT ( 'NONE',  ( -2.229367062500000163, -24.47916666530106866, -3.861377020970580443 ) ) ;
#40378 = CARTESIAN_POINT ( 'NONE',  ( -4.458734124999999437, 6.354166668032259047, -2.574251347313719407 ) ) ;
#40379 = CARTESIAN_POINT ( 'NONE',  ( 4.458734125000000326, -63.14583333196774362, 2.574251347313718519 ) ) ;
#40380 = CARTESIAN_POINT ( 'NONE',  ( 0.000000000000000000, -120.0000000000000000, 0.000000000000000000 ) ) ;
#40381 = CARTESIAN_POINT ( 'NONE',  ( 4.458734124999999437, -17.81249999863440792, -5.460374474430324690E-16 ) ) ;
#40382 = FACE_OUTER_BOUND ( 'NONE', #37012, .T. ) ;
#40383 = CARTESIAN_POINT ( 'NONE',  ( -2.071067811865478170, -152.3125000000000000, 5.000000000000000000 ) ) ;
#40384 = CARTESIAN_POINT ( 'NONE',  ( -4.999999999999999112, -13.91666666666666785, 2.886751345948131764 ) ) ;
#40385 = CARTESIAN_POINT ( 'NONE',  ( -4.458734125000000326, -151.0000000013656063, -1.846868145590735644 ) ) ;
#40386 = ORIENTED_EDGE ( 'NONE', *, *, #49918, .F. ) ;
#40387 = CARTESIAN_POINT ( 'NONE',  ( 2.229367062500001939, -47.22916666530106511, 3.861377020970579999 ) ) ;
#40388 = CARTESIAN_POINT ( 'NONE',  ( 5.000000000000000000, -38.29166666393548013, -2.886751345948130876 ) ) ;
#40389 = CARTESIAN_POINT ( 'NONE',  ( -2.500000000000000444, 28.83333333333333215, -4.330127018922193649 ) ) ;
#40390 = CARTESIAN_POINT ( 'NONE',  ( -4.458734124999999437, 6.604166668032259047, -2.574251347313719407 ) ) ;
#40391 = CARTESIAN_POINT ( 'NONE',  ( 1.975475456537005874E-15, 1.375000002731185500, 5.000000000000000000 ) ) ;
#40392 = CARTESIAN_POINT ( 'NONE',  ( -2.480964764533239819E-13, -95.62499999726883004, 5.000000000000000000 ) ) ;
#40393 = CARTESIAN_POINT ( 'NONE',  ( -5.926426369611017623E-15, 26.25000000000000000, 5.000000000000000000 ) ) ;
#40394 = CARTESIAN_POINT ( 'NONE',  ( 2.229367062500001939, 18.77083333469892779, 3.861377020970579999 ) ) ;
#40395 = CARTESIAN_POINT ( 'NONE',  ( 5.000000000000000000, -75.41666666666667140, -2.886751345948129988 ) ) ;
#40396 =( BOUNDED_CURVE ( )  B_SPLINE_CURVE ( 2, ( #24650, #58432, #44256, #220, #19818, #39427, #44909, #59386, #865 ),
 .UNSPECIFIED., .F., .F. ) 
 B_SPLINE_CURVE_WITH_KNOTS ( ( 3, 2, 2, 2, 3 ),
 ( 0.8410714285714285809, 0.8416666666666666741, 0.8428571428571428603, 0.8440476190476190466, 0.8446428571428571397 ),
 .UNSPECIFIED. ) 
 CURVE ( )  GEOMETRIC_REPRESENTATION_ITEM ( )  RATIONAL_B_SPLINE_CURVE ( ( 0.9330127018922194093, 0.9330127018922194093, 1.000000000000000000, 0.8660254037844387076, 1.000000000000000000, 0.8660254037844387076, 1.000000000000000000, 0.9330127018922194093, 0.9330127018922194093 ) ) 
 REPRESENTATION_ITEM ( '' )  );
#40397 = CARTESIAN_POINT ( 'NONE',  ( -2.499999999999996447, 10.29166666939785024, 4.330127018922195425 ) ) ;
#40398 = ORIENTED_EDGE ( 'NONE', *, *, #22697, .F. ) ;
#40399 = CARTESIAN_POINT ( 'NONE',  ( -2.499999999999996447, -97.83333333333332860, 4.330127018922195425 ) ) ;
#40400 = ORIENTED_EDGE ( 'NONE', *, *, #30369, .T. ) ;
#40401 = CARTESIAN_POINT ( 'NONE',  ( -1.339745962155613812, -51.20534180126148271, -5.000000000000000000 ) ) ;
#40402 = CARTESIAN_POINT ( 'NONE',  ( 9.457646018065525792E-16, -42.06249999863440081, 5.148502694627439702 ) ) ;
#40403 = VECTOR ( 'NONE', #49764, 1000.000000000000000 ) ;
#40404 = CARTESIAN_POINT ( 'NONE',  ( 1.060575238724906964E-15, -41.62499999726880162, 5.773502691896257311 ) ) ;
#40405 = EDGE_LOOP ( 'NONE', ( #62679, #7579, #45458, #5869 ) ) ;
#40406 = CARTESIAN_POINT ( 'NONE',  ( -4.458734124999999437, -18.31249999863440792, 0.000000000000000000 ) ) ;
#40407 = ORIENTED_EDGE ( 'NONE', *, *, #14577, .T. ) ;
#40408 = CARTESIAN_POINT ( 'NONE',  ( 5.000000000000000000, -80.50000000000000000, -6.123233995736766282E-16 ) ) ;
#40409 = FACE_OUTER_BOUND ( 'NONE', #41253, .T. ) ;
#40410 = CARTESIAN_POINT ( 'NONE',  ( 1.060575238724906964E-15, -88.62499999726880162, 5.773502691896257311 ) ) ;
#40412 = ORIENTED_EDGE ( 'NONE', *, *, #63257, .T. ) ;
#40411 = CARTESIAN_POINT ( 'NONE',  ( 5.000000000000000000, -55.49999999999999289, -6.123233995736766282E-16 ) ) ;
#40413 = CARTESIAN_POINT ( 'NONE',  ( -50.18089887299979068, -139.6875000000000284, 2.462841084822635640 ) ) ;
#40414 = CARTESIAN_POINT ( 'NONE',  ( 4.458734124999999437, -25.06249999863440792, -5.460374474430324690E-16 ) ) ;
#40415 = EDGE_LOOP ( 'NONE', ( #41894, #46930, #47951, #26902 ) ) ;
#40416 = ITEM_DEFINED_TRANSFORMATION ( 'NONE', 'NONE', #1033,  #43054 ) ;
#40417 = CARTESIAN_POINT ( 'NONE',  ( 4.458734125000000326, -163.6250000013656063, -1.846868145590734978 ) ) ;
#40418 = CARTESIAN_POINT ( 'NONE',  ( -3.152548672688508926E-16, -74.56249999863440792, -5.148502694627439702 ) ) ;
#40419 = CARTESIAN_POINT ( 'NONE',  ( 4.458734124999998549, 27.27083333469892423, -2.574251347313721627 ) ) ;
#40420 = CARTESIAN_POINT ( 'NONE',  ( 5.000000000000000000, -55.37499999726880162, -6.123233995736766282E-16 ) ) ;
#40421 = EDGE_LOOP ( 'NONE', ( #28336, #23938, #38830, #61221 ) ) ;
#40422 = CARTESIAN_POINT ( 'NONE',  ( -2.500000000000000444, 4.958333336064518981, -4.330127018922193649 ) ) ;
#40423 = CARTESIAN_POINT ( 'NONE',  ( -55.35523342533222291, -145.5625000013656063, 4.444560631937231499 ) ) ;
#40424 = CARTESIAN_POINT ( 'NONE',  ( -4.458734124999999437, -75.56249999863440792, 0.000000000000000000 ) ) ;
#40425 = CARTESIAN_POINT ( 'NONE',  ( -51.75738570946856498, -132.8750000027312126, 3.805975901505576964 ) ) ;
#40426 = CARTESIAN_POINT ( 'NONE',  ( 2.229367062499998831, -43.64583333196773651, -3.861377020970580887 ) ) ;
#40427 = CARTESIAN_POINT ( 'NONE',  ( 4.458734124999999437, -142.6250000013656063, -1.846868145590734978 ) ) ;
#40428 = CARTESIAN_POINT ( 'NONE',  ( -1.339745962155610925, 6.330341803992665106, 5.000000000000000000 ) ) ;
#40429 = CARTESIAN_POINT ( 'NONE',  ( -4.458734124999997661, -50.22916666530107221, 2.574251347313722516 ) ) ;
#40430 = CARTESIAN_POINT ( 'NONE',  ( 4.458734124999998549, -43.72916666530106511, -2.574251347313721627 ) ) ;
#40431 = CARTESIAN_POINT ( 'NONE',  ( 6.123233995736766282E-16, -170.0000000000000000, -5.000000000000000000 ) ) ;
#40432 = EDGE_CURVE ( 'NONE', #23954, #60539, #29234, .T. ) ;
#40433 = CARTESIAN_POINT ( 'NONE',  ( 4.458734125000001214, -17.89583333196774007, 2.574251347313718519 ) ) ;
#40434 = CARTESIAN_POINT ( 'NONE',  ( -2.500000000000000444, -100.1666666666666572, -4.330127018922193649 ) ) ;
#40435 = CARTESIAN_POINT ( 'NONE',  ( -4.458734125000001214, -140.1250000013655779, 1.846868145590734089 ) ) ;
#40436 = CARTESIAN_POINT ( 'NONE',  ( 2.229367062499998831, -35.89583333196773651, -3.861377020970580887 ) ) ;
#40437 = CARTESIAN_POINT ( 'NONE',  ( -2.500000000000000444, 3.958333336064518093, -4.330127018922193649 ) ) ;
#40438 = CARTESIAN_POINT ( 'NONE',  ( -1.339745962155613812, -7.080341798530293218, -5.000000000000000000 ) ) ;
#40439 = CARTESIAN_POINT ( 'NONE',  ( -56.48576386720575471, -128.7500000013656063, -4.591703134518078322 ) ) ;
#40440 = CARTESIAN_POINT ( 'NONE',  ( -4.458734124999999437, -75.64583333196775072, -2.574251347313719407 ) ) ;
#40441 = CYLINDRICAL_SURFACE ( 'NONE', #4500, 5.000000000000000000 ) ;
#40442 = DIRECTION ( 'NONE',  ( -0.000000000000000000, 1.000000000000000000, -0.000000000000000000 ) ) ;
#40443 =( BOUNDED_CURVE ( )  B_SPLINE_CURVE ( 2, ( #13940, #53807, #34185, #53496, #9119, #48353, #19071, #58644, #33877 ),
 .UNSPECIFIED., .F., .F. ) 
 B_SPLINE_CURVE_WITH_KNOTS ( ( 3, 2, 2, 2, 3 ),
 ( 0.5232142857142857428, 0.5238095238095238360, 0.5250000000000000222, 0.5261904761904762085, 0.5267857142857143016 ),
 .UNSPECIFIED. ) 
 CURVE ( )  GEOMETRIC_REPRESENTATION_ITEM ( )  RATIONAL_B_SPLINE_CURVE ( ( 0.9330127018922194093, 0.9330127018922194093, 1.000000000000000000, 0.8660254037844387076, 1.000000000000000000, 0.8660254037844387076, 1.000000000000000000, 0.9330127018922194093, 0.9330127018922194093 ) ) 
 REPRESENTATION_ITEM ( '' )  );
#40444 = CARTESIAN_POINT ( 'NONE',  ( -2.229367062499996610, 1.604166668032262155, 3.861377020970582219 ) ) ;
#40445 = ORIENTED_EDGE ( 'NONE', *, *, #19247, .F. ) ;
#40446 = CARTESIAN_POINT ( 'NONE',  ( 1.975475456537005874E-15, -30.74999999999999645, 5.000000000000000000 ) ) ;
#40447 = CARTESIAN_POINT ( 'NONE',  ( -1.127183054612291972E-14, 23.37500000273118772, 4.999999999999999112 ) ) ;
#40449 = CARTESIAN_POINT ( 'NONE',  ( 2.229367062500001939, -36.97916666530107221, 3.861377020970579999 ) ) ;
#40448 = CARTESIAN_POINT ( 'NONE',  ( -3.152548672688508926E-16, -86.56249999863440792, -5.148502694627439702 ) ) ;
#40450 = EDGE_CURVE ( 'NONE', #19298, #43561, #56521, .T. ) ;
#40451 = CARTESIAN_POINT ( 'NONE',  ( 1.339745962155616255, 27.70534180126147916, -4.999999999999997335 ) ) ;
#40452 = CARTESIAN_POINT ( 'NONE',  ( 4.458734125000001214, -84.14583333196772230, 2.574251347313718519 ) ) ;
#40453 = CARTESIAN_POINT ( 'NONE',  ( -4.458734124999997661, 17.52083333469892779, 2.574251347313722516 ) ) ;
#40454 = CARTESIAN_POINT ( 'NONE',  ( 0.000000000000000000, -120.0000000000000000, 5.000000000000000000 ) ) ;
#40455 = AXIS2_PLACEMENT_3D ( 'NONE', #56917, #58481, #48505 ) ;
#40456 = CARTESIAN_POINT ( 'NONE',  ( -58.39396692619412477, -137.4375000013656063, 2.891590998281057701 ) ) ;
#40457 = CARTESIAN_POINT ( 'NONE',  ( -4.458734124999999437, -8.312499998634406140, 0.000000000000000000 ) ) ;
#40458 = CARTESIAN_POINT ( 'NONE',  ( 4.458734124999999437, 19.93750000136559208, -5.460374474430324690E-16 ) ) ;
#40459 = EDGE_CURVE ( 'NONE', #23800, #27082, #4187, .T. ) ;
#40460 = CARTESIAN_POINT ( 'NONE',  ( 4.458734124999998549, -47.97916666530106511, -2.574251347313721627 ) ) ;
#40461 = CARTESIAN_POINT ( 'NONE',  ( 5.000000000000000000, -11.49999999999999645, -6.123233995736766282E-16 ) ) ;
#40462 = CARTESIAN_POINT ( 'NONE',  ( 4.458734125000001214, -85.89583333196773651, 2.574251347313718519 ) ) ;
#40463 = CARTESIAN_POINT ( 'NONE',  ( 2.229367062499998831, -2.645833331967738289, -3.861377020970580887 ) ) ;
#40464 = VERTEX_POINT ( 'NONE', #13827 ) ;
#40465 = CARTESIAN_POINT ( 'NONE',  ( 2.229367062499998831, -30.89583333196773651, -3.861377020970580887 ) ) ;
#40466 = CARTESIAN_POINT ( 'NONE',  ( -50.55543936806279248, -132.3125000013656063, 0.3552334253322060320 ) ) ;
#40467 = CARTESIAN_POINT ( 'NONE',  ( -4.458734124999999437, -77.39583333196772230, -2.574251347313719407 ) ) ;
#40468 = CARTESIAN_POINT ( 'NONE',  ( -4.458734124999999437, 29.35416666803225993, -2.574251347313719407 ) ) ;
#40469 = CARTESIAN_POINT ( 'NONE',  ( 4.458734124999998549, 22.27083333469893134, -2.574251347313721627 ) ) ;
#40470 = CARTESIAN_POINT ( 'NONE',  ( 1.975475456537005874E-15, -77.75000000000000000, 5.000000000000000000 ) ) ;
#40471 = CARTESIAN_POINT ( 'NONE',  ( -6.972266317189433020E-16, -66.24999999999998579, -5.000000000000000000 ) ) ;
#40472 = CARTESIAN_POINT ( 'NONE',  ( 2.229367062500001939, -80.22916666530106511, 3.861377020970579999 ) ) ;
#40473 = CARTESIAN_POINT ( 'NONE',  ( -5.000000000000000000, -56.99999999999999289, 0.000000000000000000 ) ) ;
#40474 = CARTESIAN_POINT ( 'NONE',  ( 1.060575238724906964E-15, 26.37500000273118417, 5.773502691896257311 ) ) ;
#40475 = EDGE_LOOP ( 'NONE', ( #30335, #58117, #42010, #22486 ) ) ;
#40476 = CARTESIAN_POINT ( 'NONE',  ( -1.339745962155610925, -65.79465819873851729, 5.000000000000000000 ) ) ;
#40477 = CARTESIAN_POINT ( 'NONE',  ( 5.000000000000000000, -52.37499999726881583, -6.123233995736766282E-16 ) ) ;
#40479 = CARTESIAN_POINT ( 'NONE',  ( 2.500000000000002220, -18.66666666666666430, 4.330127018922192761 ) ) ;
#40478 = DIRECTION ( 'NONE',  ( -0.000000000000000000, 1.000000000000000000, -0.000000000000000000 ) ) ;
#40480 = CARTESIAN_POINT ( 'NONE',  ( 4.458734125000001214, -22.89583333196773651, 2.574251347313718519 ) ) ;
#40481 = CARTESIAN_POINT ( 'NONE',  ( 2.229367062500001939, -85.97916666530107932, 3.861377020970579999 ) ) ;
#40482 = CARTESIAN_POINT ( 'NONE',  ( 2.500000000000002220, -24.54166666393548368, 4.330127018922192761 ) ) ;
#40483 = EDGE_CURVE ( 'NONE', #27765, #42211, #52389, .T. ) ;
#40485 = ORIENTED_EDGE ( 'NONE', *, *, #22896, .T. ) ;
#40484 = CARTESIAN_POINT ( 'NONE',  ( -4.458734124999999437, -56.31249999863440081, 0.000000000000000000 ) ) ;
#40486 = CARTESIAN_POINT ( 'NONE',  ( 2.499999999999998668, -27.33333333333333570, -4.330127018922193649 ) ) ;
#40487 = CARTESIAN_POINT ( 'NONE',  ( 1.975475456537005874E-15, 11.37500000273118239, 5.000000000000000000 ) ) ;
#40489 = ORIENTED_EDGE ( 'NONE', *, *, #16118, .T. ) ;
#40488 = CARTESIAN_POINT ( 'NONE',  ( 9.457646018065525792E-16, -6.312499998634404363, 5.148502694627439702 ) ) ;
#40490 = CARTESIAN_POINT ( 'NONE',  ( -51.60603307380591787, -148.9375000013656063, -2.891590998281053704 ) ) ;
#40491 = CARTESIAN_POINT ( 'NONE',  ( -5.000000000000000000, -64.00000000000000000, 0.000000000000000000 ) ) ;
#40492 = CARTESIAN_POINT ( 'NONE',  ( 4.458734124999999437, -150.6875000013656063, 0.000000000000000000 ) ) ;
#40493 = CARTESIAN_POINT ( 'NONE',  ( -4.458734124999999437, -45.56249999863440081, 0.000000000000000000 ) ) ;
#40494 = CARTESIAN_POINT ( 'NONE',  ( 1.339745962155612702, -23.29465819873851729, -5.000000000000000000 ) ) ;
#40495 = CARTESIAN_POINT ( 'NONE',  ( -5.000000000000000888, -159.4375000000000284, 2.071067811865474617 ) ) ;
#40496 = CARTESIAN_POINT ( 'NONE',  ( -4.250000000000000000, 5.204748896376250699E-16, -10.00000000000000000 ) ) ;
#40497 = CARTESIAN_POINT ( 'NONE',  ( -58.80597590150559739, -154.0000000000000284, 3.242614290531460330 ) ) ;
#40498 = CARTESIAN_POINT ( 'NONE',  ( -4.458734124999999437, -13.56249999863440259, 0.000000000000000000 ) ) ;
#40499 = CARTESIAN_POINT ( 'NONE',  ( 4.458734125000001214, -53.14583333196773651, 2.574251347313718519 ) ) ;
#40500 = VECTOR ( 'NONE', #46351, 1000.000000000000000 ) ;
#40501 = CARTESIAN_POINT ( 'NONE',  ( 0.000000000000000000, -120.0000000000000000, 0.000000000000000000 ) ) ;
#40502 = CARTESIAN_POINT ( 'NONE',  ( 3.152801135295366208, -143.5625000013655779, 3.152801135295367985 ) ) ;
#40503 = CARTESIAN_POINT ( 'NONE',  ( -4.458734124999998549, -96.47916666530105090, 2.574251347313722516 ) ) ;
#40504 = FACE_OUTER_BOUND ( 'NONE', #63461, .T. ) ;
#40505 = VERTEX_POINT ( 'NONE', #34380 ) ;
#40506 = CARTESIAN_POINT ( 'NONE',  ( 1.975475456537005874E-15, -79.62499999726881583, 5.000000000000000000 ) ) ;
#40507 = CARTESIAN_POINT ( 'NONE',  ( 9.457646018065525792E-16, 25.68750000136559208, 5.148502694627439702 ) ) ;
#40508 = CARTESIAN_POINT ( 'NONE',  ( -58.80597590150559739, -147.1250000027312126, 3.242614290531460330 ) ) ;
#40509 = CARTESIAN_POINT ( 'NONE',  ( 5.000000000000000000, -38.41666666666667140, -2.886751345948130876 ) ) ;
#40510 = ORIENTED_EDGE ( 'NONE', *, *, #13795, .F. ) ;
#40511 = CARTESIAN_POINT ( 'NONE',  ( -3.152548672688508926E-16, -4.562499998634401699, -5.148502694627439702 ) ) ;
#40512 = EDGE_CURVE ( 'NONE', #38980, #8862, #9311, .T. ) ;
#40513 = EDGE_CURVE ( 'NONE', #48010, #28481, #1863, .T. ) ;
#40514 = CARTESIAN_POINT ( 'NONE',  ( 5.000000000000000000, 6.499999999999999112, -6.123233995736766282E-16 ) ) ;
#40515 = CARTESIAN_POINT ( 'NONE',  ( -4.458734124999999437, -17.64583333196773651, -2.574251347313719407 ) ) ;
#40516 = CARTESIAN_POINT ( 'NONE',  ( -5.000000000000000000, -100.9583333306021444, -2.886751345948128211 ) ) ;
#40517 = CARTESIAN_POINT ( 'NONE',  ( 9.457646018065525792E-16, -8.062499998634404363, 5.148502694627439702 ) ) ;
#40518 = CARTESIAN_POINT ( 'NONE',  ( -4.458734124999999437, -148.0000000013656063, -1.846868145590735644 ) ) ;
#40519 = CARTESIAN_POINT ( 'NONE',  ( -4.458734124999999437, 15.43750000136559386, 0.000000000000000000 ) ) ;
#40520 = VERTEX_POINT ( 'NONE', #58525 ) ;
#40521 = CARTESIAN_POINT ( 'NONE',  ( -2.499999999999996447, -13.70833333060214976, 4.330127018922195425 ) ) ;
#40522 = CARTESIAN_POINT ( 'NONE',  ( -4.999999999999998224, -20.91666666666666785, 2.886751345948131764 ) ) ;
#40523 = CARTESIAN_POINT ( 'NONE',  ( -2.229367062500000163, -19.47916666530106866, -3.861377020970580443 ) ) ;
#40525 = EDGE_CURVE ( 'NONE', #40939, #26042, #54335, .T. ) ;
#40524 = CARTESIAN_POINT ( 'NONE',  ( -51.19402409849444524, -143.5000000000000284, -3.242614290531456334 ) ) ;
#40526 = CARTESIAN_POINT ( 'NONE',  ( 1.162044386198238837E-16, 29.25000000000000000, 5.000000000000000000 ) ) ;
#40527 =( BOUNDED_CURVE ( )  B_SPLINE_CURVE ( 2, ( #51227, #56372, #27713, #7475, #3290 ),
 .UNSPECIFIED., .F., .F. ) 
 B_SPLINE_CURVE_WITH_KNOTS ( ( 3, 2, 3 ),
 ( 0.9916666666666665853, 0.9958333333333333481, 1.000000000000000000 ),
 .UNSPECIFIED. ) 
 CURVE ( )  GEOMETRIC_REPRESENTATION_ITEM ( )  RATIONAL_B_SPLINE_CURVE ( ( 1.000000000000001998, 0.9238795325112847401, 1.000000000000000000, 0.9238795325112867385, 1.000000000000000000 ) ) 
 REPRESENTATION_ITEM ( '' )  );
#40528 = CARTESIAN_POINT ( 'NONE',  ( -52.80376928212989185, -148.8750000013655779, -4.297418129356379346 ) ) ;
#40529 = CARTESIAN_POINT ( 'NONE',  ( -3.535250795749689387E-16, -49.12499999726881583, -5.773502691896257311 ) ) ;
#40530 = CARTESIAN_POINT ( 'NONE',  ( 0.000000000000000000, -170.0000000000000000, 0.000000000000000000 ) ) ;
#40531 = CARTESIAN_POINT ( 'NONE',  ( -4.458734124999997661, 13.77083333469892779, 2.574251347313722516 ) ) ;
#40532 = CARTESIAN_POINT ( 'NONE',  ( 1.339745962155615144, -35.70534180126148271, 4.999999999999999112 ) ) ;
#40533 = EDGE_CURVE ( 'NONE', #57369, #26645, #19101, .T. ) ;
#40534 = FACE_OUTER_BOUND ( 'NONE', #14542, .T. ) ;
#40535 = CARTESIAN_POINT ( 'NONE',  ( -4.458734124999999437, 9.687500001365593860, 0.000000000000000000 ) ) ;
#40536 = CARTESIAN_POINT ( 'NONE',  ( 4.458734124999998549, -66.72916666530106511, -2.574251347313721627 ) ) ;
#40537 = CARTESIAN_POINT ( 'NONE',  ( -2.229367062499996610, -15.39583333196773651, 3.861377020970582219 ) ) ;
#40538 = CARTESIAN_POINT ( 'NONE',  ( 1.060575238724906964E-15, 2.249999999999998668, 5.773502691896257311 ) ) ;
#40539 = CARTESIAN_POINT ( 'NONE',  ( -3.152801135295367985, -165.8125000013656063, 3.152801135295367096 ) ) ;
#40540 = CARTESIAN_POINT ( 'NONE',  ( 1.339745962155618697, 23.70534180126147916, -4.999999999999998224 ) ) ;
#40541 = CARTESIAN_POINT ( 'NONE',  ( 9.457646018065525792E-16, -57.06249999863440081, 5.148502694627439702 ) ) ;
#40542 = CARTESIAN_POINT ( 'NONE',  ( -2.500000000000000444, -96.04166666393548724, -4.330127018922193649 ) ) ;
#40543 = VECTOR ( 'NONE', #51748, 1000.000000000000000 ) ;
#40544 = CARTESIAN_POINT ( 'NONE',  ( 0.000000000000000000, -120.0000000000000000, 5.000000000000000000 ) ) ;
#40545 =( BOUNDED_CURVE ( )  B_SPLINE_CURVE ( 2, ( #63395, #57941, #23837, #39242, #28650, #49222, #24461, #23526, #5162 ),
 .UNSPECIFIED., .F., .F. ) 
 B_SPLINE_CURVE_WITH_KNOTS ( ( 3, 2, 2, 2, 3 ),
 ( 0.3437500000000000000, 0.3444444444444444420, 0.3458333333333333259, 0.3472222222222222099, 0.3479166666666666519 ),
 .UNSPECIFIED. ) 
 CURVE ( )  GEOMETRIC_REPRESENTATION_ITEM ( )  RATIONAL_B_SPLINE_CURVE ( ( 0.9330127018922194093, 0.9330127018922194093, 1.000000000000000000, 0.8660254037844387076, 1.000000000000000000, 0.8660254037844387076, 1.000000000000000000, 0.9330127018922194093, 0.9330127018922194093 ) ) 
 REPRESENTATION_ITEM ( '' )  );
#40546 = CARTESIAN_POINT ( 'NONE',  ( 1.975475456537005874E-15, -69.74999999999998579, 5.000000000000000000 ) ) ;
#40547 = CARTESIAN_POINT ( 'NONE',  ( -4.458734124999999437, -33.39583333196772941, -2.574251347313719407 ) ) ;
#40548 = CARTESIAN_POINT ( 'NONE',  ( 0.000000000000000000, -170.0000000000000000, 0.000000000000000000 ) ) ;
#40549 = CARTESIAN_POINT ( 'NONE',  ( -4.458734125000000326, -151.1250000013656347, 1.846868145590734089 ) ) ;
#40550 = CARTESIAN_POINT ( 'NONE',  ( -3.535250795749689387E-16, -42.24999999999999289, -5.773502691896257311 ) ) ;
#40551 = CARTESIAN_POINT ( 'NONE',  ( -1.339745962155613812, -14.20534180126148094, -5.000000000000000000 ) ) ;
#40552 = CARTESIAN_POINT ( 'NONE',  ( -2.500000000000000444, -108.1666666666666572, -4.330127018922193649 ) ) ;
#40553 = ORIENTED_EDGE ( 'NONE', *, *, #40979, .T. ) ;
#40554 = CARTESIAN_POINT ( 'NONE',  ( -2.229367062499996610, -109.1458333319677365, 3.861377020970582219 ) ) ;
#40555 = CARTESIAN_POINT ( 'NONE',  ( 2.229367062499998831, -1.895833331967737623, -3.861377020970580887 ) ) ;
#40556 = LINE ( 'NONE', #35743, #9305 ) ;
#40557 = CARTESIAN_POINT ( 'NONE',  ( 5.000000000000000000, -3.416666666666665186, -2.886751345948129988 ) ) ;
#40558 = CARTESIAN_POINT ( 'NONE',  ( -3.152548672688508926E-16, -68.56249999863439371, -5.148502694627439702 ) ) ;
#40559 = CARTESIAN_POINT ( 'NONE',  ( 1.975475456537005874E-15, -16.74999999999999645, 5.000000000000000000 ) ) ;
#40560 = CARTESIAN_POINT ( 'NONE',  ( 1.060575238724906964E-15, -5.624999997268811391, 5.773502691896257311 ) ) ;
#40562 = EDGE_LOOP ( 'NONE', ( #6477, #49807, #15591, #20992 ) ) ;
#40561 = CARTESIAN_POINT ( 'NONE',  ( 9.457646018065525792E-16, -40.06249999863439371, 5.148502694627439702 ) ) ;
#40563 = CARTESIAN_POINT ( 'NONE',  ( 0.000000000000000000, -170.0000000000000000, 0.000000000000000000 ) ) ;
#40564 = CARTESIAN_POINT ( 'NONE',  ( -2.499999999999996447, 28.29166666939785202, 4.330127018922195425 ) ) ;
#40566 = ORIENTED_EDGE ( 'NONE', *, *, #59724, .F. ) ;
#40565 = CARTESIAN_POINT ( 'NONE',  ( -4.458734124999999437, 10.43750000136559386, 0.000000000000000000 ) ) ;
#40567 = CARTESIAN_POINT ( 'NONE',  ( 5.000000000000000000, -101.4166666666666572, -2.886751345948130876 ) ) ;
#40568 = CARTESIAN_POINT ( 'NONE',  ( -2.500000000000000444, -50.16666666666666430, -4.330127018922193649 ) ) ;
#40569 = CARTESIAN_POINT ( 'NONE',  ( -2.229367062499996610, -31.39583333196773651, 3.861377020970582219 ) ) ;
#40570 = CARTESIAN_POINT ( 'NONE',  ( 1.975475456537005874E-15, -34.75000000000000000, 5.000000000000000000 ) ) ;
#40571 = CARTESIAN_POINT ( 'NONE',  ( -4.458734124999999437, -76.39583333196775072, -2.574251347313719407 ) ) ;
#40572 = CARTESIAN_POINT ( 'NONE',  ( -1.846868145590737420, -140.0000000013655779, 4.458734124999999437 ) ) ;
#40573 = CARTESIAN_POINT ( 'NONE',  ( -4.458734124999999437, -82.31249999863440792, 0.000000000000000000 ) ) ;
#40574 = CARTESIAN_POINT ( 'NONE',  ( -59.59170313451811296, -136.7500000013655779, 1.485763867205729394 ) ) ;
#40575 = CARTESIAN_POINT ( 'NONE',  ( -4.458734124999999437, -34.56249999863440792, 0.000000000000000000 ) ) ;
#40576 = ORIENTED_EDGE ( 'NONE', *, *, #32988, .T. ) ;
#40577 = CARTESIAN_POINT ( 'NONE',  ( -2.499999999999996447, -82.70833333060214443, 4.330127018922195425 ) ) ;
#40578 = VERTEX_POINT ( 'NONE', #50475 ) ;
#40579 = CARTESIAN_POINT ( 'NONE',  ( 4.458734124999998549, -78.97916666530106511, -2.574251347313721627 ) ) ;
#40580 = CARTESIAN_POINT ( 'NONE',  ( 5.000000000000000888, -21.58333333333332860, 2.886751345948126879 ) ) ;
#40581 = ORIENTED_EDGE ( 'NONE', *, *, #47998, .T. ) ;
#40582 = LINE ( 'NONE', #11946, #16234 ) ;
#40583 = CARTESIAN_POINT ( 'NONE',  ( -6.972266317189433020E-16, -31.12499999726880873, -5.000000000000000000 ) ) ;
#40584 = CARTESIAN_POINT ( 'NONE',  ( 2.229367062500001939, -62.22916666530106511, 3.861377020970579999 ) ) ;
#40585 = CARTESIAN_POINT ( 'NONE',  ( -4.458734124999999437, -4.645833331967739177, -2.574251347313719407 ) ) ;
#40586 = ORIENTED_EDGE ( 'NONE', *, *, #27521, .T. ) ;
#40587 = CARTESIAN_POINT ( 'NONE',  ( 5.000000000000000000, 3.708333336064517649, -2.886751345948130876 ) ) ;
#40588 = ADVANCED_FACE ( 'NONE', ( #49817 ), #21196, .T. ) ;
#40589 = DIRECTION ( 'NONE',  ( 0.000000000000000000, 0.000000000000000000, 1.000000000000000000 ) ) ;
#40590 = CARTESIAN_POINT ( 'NONE',  ( 1.339745962155612702, -27.29465819873852084, -5.000000000000000000 ) ) ;
#40591 = CARTESIAN_POINT ( 'NONE',  ( -3.152548672688508926E-16, 5.437500001365592084, -5.148502694627439702 ) ) ;
#40592 = CARTESIAN_POINT ( 'NONE',  ( -54.64476657466781973, -142.8125000013656063, -4.444560631937228834 ) ) ;
#40593 = CARTESIAN_POINT ( 'NONE',  ( 6.123233995736766282E-16, -170.0000000000000000, -5.000000000000000000 ) ) ;
#40594 = CARTESIAN_POINT ( 'NONE',  ( 4.458734124999997661, -159.5000000013656063, 1.846868145590737864 ) ) ;
#40595 =( BOUNDED_CURVE ( )  B_SPLINE_CURVE ( 2, ( #48073, #53843, #23646, #62882, #153, #58045, #33602, #58365, #19749 ),
 .UNSPECIFIED., .F., .F. ) 
 B_SPLINE_CURVE_WITH_KNOTS ( ( 3, 2, 2, 2, 3 ),
 ( 0.6854166666666666741, 0.6861111111111111160, 0.6875000000000000000, 0.6888888888888888840, 0.6895833333333333259 ),
 .UNSPECIFIED. ) 
 CURVE ( )  GEOMETRIC_REPRESENTATION_ITEM ( )  RATIONAL_B_SPLINE_CURVE ( ( 0.9330127018922194093, 0.9330127018922194093, 1.000000000000000000, 0.8660254037844387076, 1.000000000000000000, 0.8660254037844387076, 1.000000000000000000, 0.9330127018922194093, 0.9330127018922194093 ) ) 
 REPRESENTATION_ITEM ( '' )  );
#40596 = FACE_OUTER_BOUND ( 'NONE', #15653, .T. ) ;
#40597 = ORIENTED_EDGE ( 'NONE', *, *, #48531, .F. ) ;
#40598 = CARTESIAN_POINT ( 'NONE',  ( -3.152548672688508926E-16, -82.56249999863440792, -5.148502694627439702 ) ) ;
#40599 = CARTESIAN_POINT ( 'NONE',  ( 3.061616997868383141E-16, -163.8750000027311842, -5.000000000000000000 ) ) ;
#40600 = CARTESIAN_POINT ( 'NONE',  ( -2.229367062500000163, -5.479166665301072214, -3.861377020970580443 ) ) ;
#40601 = CARTESIAN_POINT ( 'NONE',  ( -51.19402409849444524, -147.5000000000000284, -3.242614290531456334 ) ) ;
#40602 = CYLINDRICAL_SURFACE ( 'NONE', #25391, 5.000000000000000000 ) ;
#40603 = CARTESIAN_POINT ( 'NONE',  ( -4.458734124999998549, -69.47916666530107932, 2.574251347313722516 ) ) ;
#40604 = CARTESIAN_POINT ( 'NONE',  ( -2.499999999999996447, -28.70833333060214798, 4.330127018922195425 ) ) ;
#40605 = CARTESIAN_POINT ( 'NONE',  ( -6.972266317189433020E-16, -29.25000000000000000, -5.000000000000000000 ) ) ;
#40606 = CARTESIAN_POINT ( 'NONE',  ( -2.499999999999996447, -0.7083333306021483144, 4.330127018922195425 ) ) ;
#40607 = CARTESIAN_POINT ( 'NONE',  ( -2.500000000000000444, 22.83333333333333215, -4.330127018922193649 ) ) ;
#40608 = CARTESIAN_POINT ( 'NONE',  ( -4.458734124999999437, 26.60416666803225993, -2.574251347313719407 ) ) ;
#40609 = EDGE_CURVE ( 'NONE', #39239, #33786, #12547, .T. ) ;
#40610 = CARTESIAN_POINT ( 'NONE',  ( 4.458734124999999437, -53.81249999863439371, -5.460374474430324690E-16 ) ) ;
#40611 = CARTESIAN_POINT ( 'NONE',  ( -2.229367062500000163, -32.72916666530106511, -3.861377020970580443 ) ) ;
#40612 = CARTESIAN_POINT ( 'NONE',  ( -4.458734124999997661, 2.520833334698928230, 2.574251347313722516 ) ) ;
#40613 = CARTESIAN_POINT ( 'NONE',  ( -2.071067811865394237, -161.4375000027312410, 5.000000000000084377 ) ) ;
#40614 = CARTESIAN_POINT ( 'NONE',  ( 5.000000000000000000, 21.58333333333333215, -2.886751345948129988 ) ) ;
#40615 = EDGE_CURVE ( 'NONE', #9483, #39986, #8425, .T. ) ;
#40616 = CARTESIAN_POINT ( 'NONE',  ( -5.000000000000000000, -143.6250000027312126, -6.123233995736766282E-16 ) ) ;
#40617 = CARTESIAN_POINT ( 'NONE',  ( -6.972266317189433020E-16, -26.12499999726881583, -5.000000000000000000 ) ) ;
#40618 = CARTESIAN_POINT ( 'NONE',  ( -2.229367062500000163, -40.47916666530107221, -3.861377020970580443 ) ) ;
#40619 = CARTESIAN_POINT ( 'NONE',  ( -2.500000000000000444, -80.04166666393547303, -4.330127018922193649 ) ) ;
#40620 = CARTESIAN_POINT ( 'NONE',  ( -59.59170313451811296, -140.7500000013655779, 1.485763867205729394 ) ) ;
#40621 = CARTESIAN_POINT ( 'NONE',  ( 0.000000000000000000, -170.0000000000000000, 5.000000000000000000 ) ) ;
#40622 = EDGE_CURVE ( 'NONE', #40086, #16789, #14974, .T. ) ;
#40623 = CARTESIAN_POINT ( 'NONE',  ( 1.339745962155612702, -15.16965819600733134, -5.000000000000000000 ) ) ;
#40624 = CARTESIAN_POINT ( 'NONE',  ( -2.229367062499996610, -80.39583333196773651, 3.861377020970582219 ) ) ;
#40625 = CARTESIAN_POINT ( 'NONE',  ( 3.152801135295367541, -161.5625000013656063, -3.152801135295367541 ) ) ;
#40626 = CARTESIAN_POINT ( 'NONE',  ( 5.000000000000000000, 13.62500000273118417, -6.123233995736766282E-16 ) ) ;
#40627 = CARTESIAN_POINT ( 'NONE',  ( -5.000000000000000000, -28.08333333333333925, -2.886751345948128211 ) ) ;
#40628 = CARTESIAN_POINT ( 'NONE',  ( -1.339745962155610925, -56.79465819873851729, 5.000000000000000000 ) ) ;
#40629 = ORIENTED_EDGE ( 'NONE', *, *, #11470, .F. ) ;
#40630 = CARTESIAN_POINT ( 'NONE',  ( -2.229367062500000163, 25.27083333469892779, -3.861377020970580443 ) ) ;
#40631 = ORIENTED_EDGE ( 'NONE', *, *, #7231, .F. ) ;
#40632 = CARTESIAN_POINT ( 'NONE',  ( 2.229367062500001939, -61.22916666530106511, 3.861377020970579999 ) ) ;
#40633 =( BOUNDED_CURVE ( )  B_SPLINE_CURVE ( 2, ( #14598, #63508, #54490, #13973, #43239, #44503, #53532, #63195, #20069 ),
 .UNSPECIFIED., .F., .F. ) 
 B_SPLINE_CURVE_WITH_KNOTS ( ( 3, 2, 2, 2, 3 ),
 ( 0.1250000000000001110, 0.1291666666666667906, 0.1333333333333334425, 0.1375000000000001221, 0.1416666666666667740 ),
 .UNSPECIFIED. ) 
 CURVE ( )  GEOMETRIC_REPRESENTATION_ITEM ( )  RATIONAL_B_SPLINE_CURVE ( ( 0.9999999999999980016, 0.9238795325112887369, 1.000000000000000000, 0.9238795325112867385, 1.000000000000000000, 0.9238795325112867385, 1.000000000000000000, 0.9238795325112847401, 1.000000000000001998 ) ) 
 REPRESENTATION_ITEM ( '' )  );
#40634 = CARTESIAN_POINT ( 'NONE',  ( -2.499999999999996447, 23.29166666939785202, 4.330127018922195425 ) ) ;
#40635 = CARTESIAN_POINT ( 'NONE',  ( -56.66612745406293783, -138.4375000027312126, -5.149110718188535607 ) ) ;
#40636 = CARTESIAN_POINT ( 'NONE',  ( 2.499999999999998668, 13.66666666666666785, -4.330127018922193649 ) ) ;
#40637 = CARTESIAN_POINT ( 'NONE',  ( 2.229367062500001939, -48.97916666530107221, 3.861377020970579999 ) ) ;
#40638 = VECTOR ( 'NONE', #5884, 1000.000000000000000 ) ;
#40639 = CARTESIAN_POINT ( 'NONE',  ( 2.229367062500001939, -11.97916666530107044, 3.861377020970579999 ) ) ;
#40640 = CARTESIAN_POINT ( 'NONE',  ( 1.339745962155612702, -6.294658198738520838, -5.000000000000000000 ) ) ;
#40641 = CARTESIAN_POINT ( 'NONE',  ( -6.972266317189433020E-16, -99.12499999726880162, -5.000000000000000000 ) ) ;
#40642 = CARTESIAN_POINT ( 'NONE',  ( -2.499999999999996447, -36.83333333333332860, 4.330127018922195425 ) ) ;
#40643 = DIRECTION ( 'NONE',  ( -0.000000000000000000, 1.000000000000000000, -0.000000000000000000 ) ) ;
#40644 = CARTESIAN_POINT ( 'NONE',  ( 5.000000000000000888, -35.58333333333332860, 2.886751345948126879 ) ) ;
#40645 = CARTESIAN_POINT ( 'NONE',  ( 5.000000000000000000, -74.41666666666665719, -2.886751345948130876 ) ) ;
#40647 = CARTESIAN_POINT ( 'NONE',  ( 9.457646018065525792E-16, -15.31249999863440436, 5.148502694627439702 ) ) ;
#40646 = CARTESIAN_POINT ( 'NONE',  ( -2.498395430326213474E-14, 21.37500000273118062, 5.000000000000000000 ) ) ;
#40648 = DIRECTION ( 'NONE',  ( -0.000000000000000000, 1.000000000000000000, -0.000000000000000000 ) ) ;
#40649 = CARTESIAN_POINT ( 'NONE',  ( 4.458734124999998549, -59.72916666530106511, -2.574251347313721627 ) ) ;
#40650 = CARTESIAN_POINT ( 'NONE',  ( -4.458734125000000326, -152.2500000013656347, -1.846868145590735644 ) ) ;
#40651 = CARTESIAN_POINT ( 'NONE',  ( -4.458734124999998549, -64.22916666530107932, 2.574251347313722516 ) ) ;
#40652 = CARTESIAN_POINT ( 'NONE',  ( -3.535250795749689387E-16, -57.12499999726880873, -5.773502691896257311 ) ) ;
#40653 = ORIENTED_EDGE ( 'NONE', *, *, #8243, .F. ) ;
#40654 = CARTESIAN_POINT ( 'NONE',  ( -58.24261429053147765, -137.2500000000000000, -3.805975901505573855 ) ) ;
#40655 = ORIENTED_EDGE ( 'NONE', *, *, #51089, .T. ) ;
#40657 = DIRECTION ( 'NONE',  ( -0.000000000000000000, 1.000000000000000000, -0.000000000000000000 ) ) ;
#40656 = CARTESIAN_POINT ( 'NONE',  ( -51.19402409849444524, -141.5000000000000284, -3.242614290531456334 ) ) ;
#40658 = CARTESIAN_POINT ( 'NONE',  ( -4.458734125000001214, -153.8750000013655779, 1.846868145590734089 ) ) ;
#40659 = ORIENTED_EDGE ( 'NONE', *, *, #11829, .F. ) ;
#40660 = CARTESIAN_POINT ( 'NONE',  ( -1.339745962155613812, -10.20534180126147739, -5.000000000000000000 ) ) ;
#40661 = CARTESIAN_POINT ( 'NONE',  ( -55.39835681537999790, -128.8750000000000284, 4.984105922594378235 ) ) ;
#40662 = CARTESIAN_POINT ( 'NONE',  ( -6.972266317189433020E-16, 4.749999999999999112, -5.000000000000000000 ) ) ;
#40663 = CARTESIAN_POINT ( 'NONE',  ( 2.229367062499998831, -47.89583333196774362, -3.861377020970580887 ) ) ;
#40664 = ORIENTED_EDGE ( 'NONE', *, *, #14955, .F. ) ;
#40665 = CARTESIAN_POINT ( 'NONE',  ( 4.458734124999999437, 14.18750000136559386, -5.460374474430324690E-16 ) ) ;
#40666 = CARTESIAN_POINT ( 'NONE',  ( 2.229367062500001939, 24.02083333469892779, 3.861377020970579999 ) ) ;
#40667 = CARTESIAN_POINT ( 'NONE',  ( -59.44456063193725015, -152.5625000013656063, -0.3552334253322034230 ) ) ;
#40668 = LINE ( 'NONE', #60312, #54161 ) ;
#40669 = CARTESIAN_POINT ( 'NONE',  ( 5.000000000000000888, -61.45833333060214443, 2.886751345948126879 ) ) ;
#40670 = EDGE_LOOP ( 'NONE', ( #51492, #38379 ) ) ;
#40671 = CARTESIAN_POINT ( 'NONE',  ( 9.457646018065525792E-16, -64.06249999863440792, 5.148502694627439702 ) ) ;
#40672 = CARTESIAN_POINT ( 'NONE',  ( 1.062108568985190270E-13, -28.12499999726880873, -4.999999999999999112 ) ) ;
#40673 = CARTESIAN_POINT ( 'NONE',  ( -3.152548672688508926E-16, 14.43750000136559386, -5.148502694627439702 ) ) ;
#40674 = CARTESIAN_POINT ( 'NONE',  ( -2.499999999999996447, -69.70833333060214443, 4.330127018922195425 ) ) ;
#40675 = CARTESIAN_POINT ( 'NONE',  ( -5.000000000000000000, -26.99999999999999645, 0.000000000000000000 ) ) ;
#40676 = CARTESIAN_POINT ( 'NONE',  ( 2.229367062499998831, -56.89583333196773651, -3.861377020970580887 ) ) ;
#40677 = CARTESIAN_POINT ( 'NONE',  ( -2.500000000000000444, -17.04166666393548368, -4.330127018922193649 ) ) ;
#40678 = CARTESIAN_POINT ( 'NONE',  ( -1.975475456537005874E-15, 29.25000000000000000, 5.000000000000000000 ) ) ;
#40679 = FACE_OUTER_BOUND ( 'NONE', #6012, .T. ) ;
#40680 = CARTESIAN_POINT ( 'NONE',  ( -8.660254037844341113, 45.00000000000000000, 6.047423072554883697E-14 ) ) ;
#40681 = DIRECTION ( 'NONE',  ( -0.000000000000000000, 1.000000000000000000, -0.000000000000000000 ) ) ;
#40682 = CARTESIAN_POINT ( 'NONE',  ( 4.458734124999998549, -18.97916666530106511, -2.574251347313721627 ) ) ;
#40683 = EDGE_LOOP ( 'NONE', ( #45638, #23863, #43760, #58307 ) ) ;
#40684 = CARTESIAN_POINT ( 'NONE',  ( 2.500000000000002220, 23.33333333333333215, 4.330127018922192761 ) ) ;
#40685 = CARTESIAN_POINT ( 'NONE',  ( 2.229367062499998831, -102.6458333319677365, -3.861377020970580887 ) ) ;
#40686 = CARTESIAN_POINT ( 'NONE',  ( 3.061616997868383141E-16, -158.8750000027311842, -5.000000000000000000 ) ) ;
#40687 = ORIENTED_EDGE ( 'NONE', *, *, #16123, .F. ) ;
#40688 = CARTESIAN_POINT ( 'NONE',  ( -2.229367062500000163, -101.7291666653010651, -3.861377020970580443 ) ) ;
#40689 = CARTESIAN_POINT ( 'NONE',  ( 4.458734124999998549, -26.72916666530106866, -2.574251347313721627 ) ) ;
#40690 = CARTESIAN_POINT ( 'NONE',  ( 5.000000000000000000, -56.29166666393548013, -2.886751345948129988 ) ) ;
#40691 = CARTESIAN_POINT ( 'NONE',  ( -52.80376928212989185, -124.8750000013656205, -4.297418129356379346 ) ) ;
#40692 = CARTESIAN_POINT ( 'NONE',  ( -51.60603307380591787, -142.9375000013656063, -2.891590998281053704 ) ) ;
#40693 = CARTESIAN_POINT ( 'NONE',  ( -2.229367062499996610, -26.14583333196773651, 3.861377020970582219 ) ) ;
#40694 = CARTESIAN_POINT ( 'NONE',  ( -2.229367062499996610, -64.39583333196773651, 3.861377020970582219 ) ) ;
#40695 = CARTESIAN_POINT ( 'NONE',  ( -1.339745962155610925, -39.66965819600733312, 5.000000000000000000 ) ) ;
#40696 = CARTESIAN_POINT ( 'NONE',  ( -4.458734124999999437, -20.31249999863440081, 0.000000000000000000 ) ) ;
#40697 = FACE_OUTER_BOUND ( 'NONE', #11732, .T. ) ;
#40698 = CARTESIAN_POINT ( 'NONE',  ( -9.184850993605147944E-16, -150.2500000000000284, 5.000000000000000000 ) ) ;
#40699 = CARTESIAN_POINT ( 'NONE',  ( 2.499999999999998668, -13.33333333333333570, -4.330127018922193649 ) ) ;
#40700 = CARTESIAN_POINT ( 'NONE',  ( -4.458734124999999437, -151.9375000013655779, -5.460374474430324690E-16 ) ) ;
#40701 = ORIENTED_EDGE ( 'NONE', *, *, #1374, .T. ) ;
#40702 = CARTESIAN_POINT ( 'NONE',  ( -4.458734124999999437, -47.56249999863440792, 0.000000000000000000 ) ) ;
#40703 = FACE_OUTER_BOUND ( 'NONE', #37900, .T. ) ;
#40704 = CARTESIAN_POINT ( 'NONE',  ( 1.975475456537005874E-15, -90.74999999999998579, 5.000000000000000000 ) ) ;
#40705 = CARTESIAN_POINT ( 'NONE',  ( -5.000000000000000000, 27.91666666666666430, -2.886751345948128211 ) ) ;
#40706 = CARTESIAN_POINT ( 'NONE',  ( -4.458734124999998549, 3.770833334698929562, 2.574251347313722516 ) ) ;
#40707 = DIRECTION ( 'NONE',  ( 0.000000000000000000, 0.000000000000000000, 1.000000000000000000 ) ) ;
#40708 = DIRECTION ( 'NONE',  ( 1.000000000000000000, 0.000000000000000000, 0.000000000000000000 ) ) ;
#40709 = FACE_OUTER_BOUND ( 'NONE', #41120, .T. ) ;
#40710 = CARTESIAN_POINT ( 'NONE',  ( 2.229367062500001939, 16.77083333469892779, 3.861377020970579999 ) ) ;
#40711 = CARTESIAN_POINT ( 'NONE',  ( -5.000000000000000000, -80.08333333333332860, -2.886751345948128211 ) ) ;
#40712 = CARTESIAN_POINT ( 'NONE',  ( 5.000000000000000888, 10.54166666939785202, 2.886751345948126879 ) ) ;
#40713 = ORIENTED_EDGE ( 'NONE', *, *, #57831, .F. ) ;
#40714 = CARTESIAN_POINT ( 'NONE',  ( -3.750000000000004885, 6.495190528383289141, 0.000000000000000000 ) ) ;
#40715 = ORIENTED_EDGE ( 'NONE', *, *, #9853, .T. ) ;
#40716 = AXIS2_PLACEMENT_3D ( 'NONE', #26399, #11914, #5505 ) ;
#40717 = LINE ( 'NONE', #59722, #59415 ) ;
#40718 = CARTESIAN_POINT ( 'NONE',  ( 2.229367062499998831, -44.64583333196774362, -3.861377020970580887 ) ) ;
#40719 = CARTESIAN_POINT ( 'NONE',  ( 1.846868145590736310, -162.8750000013655779, 4.458734124999999437 ) ) ;
#40720 = VECTOR ( 'NONE', #58706, 1000.000000000000000 ) ;
#40721 =( BOUNDED_CURVE ( )  B_SPLINE_CURVE ( 2, ( #26113, #50876, #45732, #1685, #11622, #22569, #21286, #60538, #36079 ),
 .UNSPECIFIED., .F., .F. ) 
 B_SPLINE_CURVE_WITH_KNOTS ( ( 3, 2, 2, 2, 3 ),
 ( 0.8767857142857142794, 0.8773809523809523725, 0.8785714285714285587, 0.8797619047619047450, 0.8803571428571428381 ),
 .UNSPECIFIED. ) 
 CURVE ( )  GEOMETRIC_REPRESENTATION_ITEM ( )  RATIONAL_B_SPLINE_CURVE ( ( 0.9330127018922194093, 0.9330127018922194093, 1.000000000000000000, 0.8660254037844387076, 1.000000000000000000, 0.8660254037844387076, 1.000000000000000000, 0.9330127018922194093, 0.9330127018922194093 ) ) 
 REPRESENTATION_ITEM ( '' )  );
#40722 = CARTESIAN_POINT ( 'NONE',  ( 2.500000000000002220, -41.54166666393548013, 4.330127018922192761 ) ) ;
#40723 = ORIENTED_EDGE ( 'NONE', *, *, #18493, .T. ) ;
#40724 = CARTESIAN_POINT ( 'NONE',  ( -4.458734124999998549, -17.22916666530106866, 2.574251347313722516 ) ) ;
#40725 = VERTEX_POINT ( 'NONE', #51108 ) ;
#40726 = CARTESIAN_POINT ( 'NONE',  ( 5.000000000000000000, -89.41666666666667140, -2.886751345948129988 ) ) ;
#40727 = CARTESIAN_POINT ( 'NONE',  ( 4.458734124999999437, -168.5000000013656063, 1.846868145590737864 ) ) ;
#40728 = CARTESIAN_POINT ( 'NONE',  ( 2.500000000000002220, -85.54166666393547303, 4.330127018922192761 ) ) ;
#40730 = ORIENTED_EDGE ( 'NONE', *, *, #41605, .T. ) ;
#40729 = CARTESIAN_POINT ( 'NONE',  ( -2.500000000000000444, -61.04166666393547303, -4.330127018922193649 ) ) ;
#40731 = CARTESIAN_POINT ( 'NONE',  ( -51.75738570946856498, -140.7500000000000000, 3.805975901505576964 ) ) ;
#40732 = CARTESIAN_POINT ( 'NONE',  ( 4.458734124999999437, -35.06249999863440792, -5.460374474430324690E-16 ) ) ;
#40733 = CARTESIAN_POINT ( 'NONE',  ( 2.500000000000002220, -41.54166666393548013, 4.330127018922192761 ) ) ;
#40734 = ORIENTED_EDGE ( 'NONE', *, *, #55138, .F. ) ;
#40735 = CARTESIAN_POINT ( 'NONE',  ( -2.229367062500000163, -79.47916666530106511, -3.861377020970580443 ) ) ;
#40736 = CARTESIAN_POINT ( 'NONE',  ( 2.229367062500001939, -108.2291666653010651, 3.861377020970579999 ) ) ;
#40737 = CARTESIAN_POINT ( 'NONE',  ( 5.000000000000000000, -23.41666666666667140, -2.886751345948130876 ) ) ;
#40738 = ORIENTED_EDGE ( 'NONE', *, *, #21436, .F. ) ;
#40739 = CARTESIAN_POINT ( 'NONE',  ( 0.000000000000000000, -120.0000000000000000, 5.000000000000000000 ) ) ;
#40740 = CARTESIAN_POINT ( 'NONE',  ( -57.19623071787016499, -142.6250000013656063, 4.297418129356382899 ) ) ;
#40741 = CARTESIAN_POINT ( 'NONE',  ( -2.229367062500000163, -81.72916666530106511, -3.861377020970580443 ) ) ;
#40742 = CARTESIAN_POINT ( 'NONE',  ( -58.24261429053147765, -133.3750000027312126, -3.805975901505573855 ) ) ;
#40743 = CARTESIAN_POINT ( 'NONE',  ( -2.229367062499996610, -45.14583333196774362, 3.861377020970582219 ) ) ;
#40744 = CARTESIAN_POINT ( 'NONE',  ( -4.458734124999999437, -144.2500000013656063, -1.846868145590735644 ) ) ;
#40745 = CARTESIAN_POINT ( 'NONE',  ( 1.975475456537005874E-15, -13.62499999726881228, 5.000000000000000000 ) ) ;
#40746 = CARTESIAN_POINT ( 'NONE',  ( -2.229367062499996610, -50.14583333196772941, 3.861377020970582219 ) ) ;
#40747 = CARTESIAN_POINT ( 'NONE',  ( 2.229367062500001939, -45.97916666530106511, 3.861377020970579999 ) ) ;
#40748 = CARTESIAN_POINT ( 'NONE',  ( -3.152548672688508926E-16, 29.43750000136559564, -5.148502694627439702 ) ) ;
#40749 = CARTESIAN_POINT ( 'NONE',  ( -4.458734124999999437, -16.31249999863440436, 0.000000000000000000 ) ) ;
#40750 = CARTESIAN_POINT ( 'NONE',  ( -3.535250795749689387E-16, -102.2500000000000000, -5.773502691896257311 ) ) ;
#40751 = CARTESIAN_POINT ( 'NONE',  ( -2.071067811865496378, -167.6875000000000284, -4.999999999999979572 ) ) ;
#40752 = CARTESIAN_POINT ( 'NONE',  ( -2.229367062500000163, -37.72916666530107221, -3.861377020970580443 ) ) ;
#40753 = CARTESIAN_POINT ( 'NONE',  ( 1.060575238724906964E-15, 3.375000002731186388, 5.773502691896257311 ) ) ;
#40754 = CARTESIAN_POINT ( 'NONE',  ( -5.000000000000000000, -39.95833333060214443, -2.886751345948128211 ) ) ;
#40755 = CARTESIAN_POINT ( 'NONE',  ( -52.80376928212989185, -127.8750000013656063, -4.297418129356379346 ) ) ;
#40756 = CARTESIAN_POINT ( 'NONE',  ( -4.458734124999999437, -72.56249999863439371, 0.000000000000000000 ) ) ;
#40757 = CARTESIAN_POINT ( 'NONE',  ( 2.499999999999998668, -71.33333333333332860, -4.330127018922193649 ) ) ;
#40758 = CARTESIAN_POINT ( 'NONE',  ( 2.500000000000002220, -76.66666666666665719, 4.330127018922192761 ) ) ;
#40759 = CARTESIAN_POINT ( 'NONE',  ( -4.458734124999997661, 1.520833334698927564, 2.574251347313722516 ) ) ;
#40760 = ORIENTED_EDGE ( 'NONE', *, *, #57812, .T. ) ;
#40761 = VECTOR ( 'NONE', #18071, 1000.000000000000000 ) ;
#40762 = LINE ( 'NONE', #15694, #56219 ) ;
#40763 = CARTESIAN_POINT ( 'NONE',  ( 1.339745962155612702, -15.29465819873851906, -5.000000000000000000 ) ) ;
#40765 = CARTESIAN_POINT ( 'NONE',  ( -4.458734124999998549, -37.22916666530107221, 2.574251347313722516 ) ) ;
#40764 = CARTESIAN_POINT ( 'NONE',  ( -2.229367062500000163, -90.47916666530106511, -3.861377020970580443 ) ) ;
#40766 = CARTESIAN_POINT ( 'NONE',  ( -6.972266317189433020E-16, 2.750000000000000000, -5.000000000000000000 ) ) ;
#40767 = CARTESIAN_POINT ( 'NONE',  ( -2.229367062499996610, -86.39583333196773651, 3.861377020970582219 ) ) ;
#40768 = VECTOR ( 'NONE', #5124, 1000.000000000000000 ) ;
#40769 = CARTESIAN_POINT ( 'NONE',  ( 2.229367062499998831, 15.10416666803225993, -3.861377020970580887 ) ) ;
#40770 = DIRECTION ( 'NONE',  ( -0.000000000000000000, 1.000000000000000000, -0.000000000000000000 ) ) ;
#40771 = CARTESIAN_POINT ( 'NONE',  ( -51.60603307380591787, -135.9375000013656063, -2.891590998281053704 ) ) ;
#40772 = CARTESIAN_POINT ( 'NONE',  ( -2.229367062499996610, -8.145833331967736513, 3.861377020970582219 ) ) ;
#40773 = CARTESIAN_POINT ( 'NONE',  ( 4.458734124999999437, 23.93750000136559564, -5.460374474430324690E-16 ) ) ;
#40774 = CARTESIAN_POINT ( 'NONE',  ( 4.458734125000000326, -50.14583333196772230, 2.574251347313718519 ) ) ;
#40775 =( BOUNDED_CURVE ( )  B_SPLINE_CURVE ( 2, ( #28443, #41970, #18163, #38105, #23632, #17546, #12707, #47125, #56789 ),
 .UNSPECIFIED., .F., .F. ) 
 B_SPLINE_CURVE_WITH_KNOTS ( ( 3, 2, 2, 2, 3 ),
 ( 0.08541666666666666852, 0.08611111111111111049, 0.08749999999999999445, 0.08888888888888889228, 0.08958333333333333426 ),
 .UNSPECIFIED. ) 
 CURVE ( )  GEOMETRIC_REPRESENTATION_ITEM ( )  RATIONAL_B_SPLINE_CURVE ( ( 0.9330127018922194093, 0.9330127018922194093, 1.000000000000000000, 0.8660254037844387076, 1.000000000000000000, 0.8660254037844387076, 1.000000000000000000, 0.9330127018922194093, 0.9330127018922194093 ) ) 
 REPRESENTATION_ITEM ( '' )  );
#40776 = CARTESIAN_POINT ( 'NONE',  ( 1.975475456537005874E-15, -15.62499999726881406, 5.000000000000000000 ) ) ;
#40777 = CARTESIAN_POINT ( 'NONE',  ( -3.152548672688508926E-16, -86.56249999863440792, -5.148502694627439702 ) ) ;
#40778 = CARTESIAN_POINT ( 'NONE',  ( -4.458734124999999437, -1.395833331967737179, -2.574251347313719407 ) ) ;
#40779 = ORIENTED_EDGE ( 'NONE', *, *, #57123, .T. ) ;
#40780 = CARTESIAN_POINT ( 'NONE',  ( -2.229367062500000163, -30.72916666530107221, -3.861377020970580443 ) ) ;
#40781 = CARTESIAN_POINT ( 'NONE',  ( -58.39396692619412477, -131.6875000013656063, 2.891590998281057701 ) ) ;
#40782 = CARTESIAN_POINT ( 'NONE',  ( 4.458734124999999437, -72.81249999863439371, -5.460374474430324690E-16 ) ) ;
#40783 = CARTESIAN_POINT ( 'NONE',  ( -4.458734124999999437, 27.35416666803225993, -2.574251347313719407 ) ) ;
#40784 = CARTESIAN_POINT ( 'NONE',  ( 2.229367062499998831, 21.35416666803226349, -3.861377020970580887 ) ) ;
#40785 = CARTESIAN_POINT ( 'NONE',  ( 5.000000000000000000, -53.49999999999999289, -6.123233995736766282E-16 ) ) ;
#40786 = CARTESIAN_POINT ( 'NONE',  ( 1.339745962155612702, -28.29465819873851729, -5.000000000000000000 ) ) ;
#40787 = CARTESIAN_POINT ( 'NONE',  ( -3.152548672688508926E-16, -75.81249999863440792, -5.148502694627439702 ) ) ;
#40788 = CARTESIAN_POINT ( 'NONE',  ( -4.999999999999999112, -62.91666666666667140, 2.886751345948131764 ) ) ;
#40789 = FACE_OUTER_BOUND ( 'NONE', #47532, .T. ) ;
#40790 = CARTESIAN_POINT ( 'NONE',  ( -5.000000000000000000, 23.12500000273118417, 0.000000000000000000 ) ) ;
#40791 = VERTEX_POINT ( 'NONE', #10901 ) ;
#40792 = CYLINDRICAL_SURFACE ( 'NONE', #9851, 5.000000000000000000 ) ;
#40793 = CARTESIAN_POINT ( 'NONE',  ( -6.972266317189433020E-16, -67.25000000000000000, -5.000000000000000000 ) ) ;
#40795 = CARTESIAN_POINT ( 'NONE',  ( 5.000000000000000000, -21.41666666666666430, -2.886751345948129988 ) ) ;
#40794 = CARTESIAN_POINT ( 'NONE',  ( -59.98410592259440222, -138.2500000027312126, -0.3983568153799752487 ) ) ;
#40796 = CARTESIAN_POINT ( 'NONE',  ( 4.458734124999999437, -28.81249999863440436, -5.460374474430324690E-16 ) ) ;
#40797 = EDGE_CURVE ( 'NONE', #55752, #14724, #54441, .T. ) ;
#40798 = CARTESIAN_POINT ( 'NONE',  ( 4.458734124999999437, -87.81249999863439371, -5.460374474430324690E-16 ) ) ;
#40799 = CARTESIAN_POINT ( 'NONE',  ( 2.499999999999998668, -22.20833333060215153, -4.330127018922193649 ) ) ;
#40801 = EDGE_LOOP ( 'NONE', ( #61476, #3723, #36813, #18405 ) ) ;
#40800 = CARTESIAN_POINT ( 'NONE',  ( 4.458734124999999437, -57.81249999863440081, -5.460374474430324690E-16 ) ) ;
#40802 = CARTESIAN_POINT ( 'NONE',  ( 2.500000000000002220, -74.54166666393547303, 4.330127018922192761 ) ) ;
#40804 = ORIENTED_EDGE ( 'NONE', *, *, #20940, .T. ) ;
#40803 = CARTESIAN_POINT ( 'NONE',  ( 4.458734125000001214, -5.145833331967740065, 2.574251347313718519 ) ) ;
#40805 = CARTESIAN_POINT ( 'NONE',  ( -5.000000000000000000, -69.08333333333332860, -2.886751345948128211 ) ) ;
#40806 = CARTESIAN_POINT ( 'NONE',  ( -3.152801135295367985, -151.0625000013655779, 3.152801135295367096 ) ) ;
#40807 = CARTESIAN_POINT ( 'NONE',  ( 4.458734125000001214, -46.14583333196773651, 2.574251347313718519 ) ) ;
#40808 = LINE ( 'NONE', #36001, #63544 ) ;
#40809 = CARTESIAN_POINT ( 'NONE',  ( -5.000000000000000888, -159.5625000000000568, -2.071067811865475949 ) ) ;
#40810 = CARTESIAN_POINT ( 'NONE',  ( 1.975475456537005874E-15, -21.62499999726880873, 5.000000000000000000 ) ) ;
#40811 = CARTESIAN_POINT ( 'NONE',  ( -50.18089887299979068, -153.6875000000000284, 2.462841084822635640 ) ) ;
#40812 = VECTOR ( 'NONE', #6475, 1000.000000000000000 ) ;
#40813 = CARTESIAN_POINT ( 'NONE',  ( -4.458734124999998549, -14.47916666530107221, 2.574251347313722516 ) ) ;
#40814 = CARTESIAN_POINT ( 'NONE',  ( 4.458734124999998549, -52.97916666530107932, -2.574251347313721627 ) ) ;
#40815 = EDGE_CURVE ( 'NONE', #897, #27765, #967, .T. ) ;
#40816 = CARTESIAN_POINT ( 'NONE',  ( -5.000000000000000000, -58.87499999726880873, 0.000000000000000000 ) ) ;
#40817 = CARTESIAN_POINT ( 'NONE',  ( -8.190561711645485556E-16, -142.6875000013656063, 4.458734124999999437 ) ) ;
#40818 = ADVANCED_FACE ( 'NONE', ( #44670 ), #54654, .T. ) ;
#40819 = CARTESIAN_POINT ( 'NONE',  ( 2.229367062499998831, -94.89583333196773651, -3.861377020970580887 ) ) ;
#40820 = CARTESIAN_POINT ( 'NONE',  ( -2.500000000000000444, 20.95833333606451987, -4.330127018922193649 ) ) ;
#40821 = ORIENTED_EDGE ( 'NONE', *, *, #10507, .F. ) ;
#40822 = CARTESIAN_POINT ( 'NONE',  ( -55.35523342533222291, -153.5625000013656063, 4.444560631937231499 ) ) ;
#40823 = CARTESIAN_POINT ( 'NONE',  ( -2.229367062499996610, 27.60416666803225993, 3.861377020970582219 ) ) ;
#40824 = CARTESIAN_POINT ( 'NONE',  ( -59.81910112700025905, -145.3125000027312126, -2.462841084822630311 ) ) ;
#40825 =( BOUNDED_CURVE ( )  B_SPLINE_CURVE ( 2, ( #42831, #42516, #33504, #62783, #8437, #37693, #43142, #32874, #12619 ),
 .UNSPECIFIED., .F., .F. ) 
 B_SPLINE_CURVE_WITH_KNOTS ( ( 3, 2, 2, 2, 3 ),
 ( 0.2916666666666669072, 0.2958333333333335591, 0.3000000000000002665, 0.3041666666666669183, 0.3083333333333336257 ),
 .UNSPECIFIED. ) 
 CURVE ( )  GEOMETRIC_REPRESENTATION_ITEM ( )  RATIONAL_B_SPLINE_CURVE ( ( 0.9999999999999958922, 0.9238795325112908463, 1.000000000000000000, 0.9238795325112867385, 1.000000000000000000, 0.9238795325112867385, 1.000000000000000000, 0.9238795325112816315, 1.000000000000005107 ) ) 
 REPRESENTATION_ITEM ( '' )  );
#40826 = CARTESIAN_POINT ( 'NONE',  ( 1.339745962155612702, -50.29465819873851729, -5.000000000000000000 ) ) ;
#40827 = ORIENTED_EDGE ( 'NONE', *, *, #3219, .T. ) ;
#40828 = EDGE_CURVE ( 'NONE', #45244, #8687, #26335, .T. ) ;
#40829 = CARTESIAN_POINT ( 'NONE',  ( 2.229367062499998831, -4.645833331967740065, -3.861377020970580887 ) ) ;
#40830 = CARTESIAN_POINT ( 'NONE',  ( 2.499999999999998668, -1.208333330602148870, -4.330127018922193649 ) ) ;
#40831 = CARTESIAN_POINT ( 'NONE',  ( 2.229367062500001939, -23.22916666530107221, 3.861377020970579999 ) ) ;
#40832 = CARTESIAN_POINT ( 'NONE',  ( 1.339745962155615144, -70.70534180126148271, 4.999999999999999112 ) ) ;
#40833 = CARTESIAN_POINT ( 'NONE',  ( -4.458734124999998549, -8.229166665301073991, 2.574251347313722516 ) ) ;
#40834 = CARTESIAN_POINT ( 'NONE',  ( 5.276498195232308674, -6.073236878017951312, -7.633618187056764981 ) ) ;
#40835 = CARTESIAN_POINT ( 'NONE',  ( 3.152801135295367541, -150.3125000013655779, -3.152801135295367541 ) ) ;
#40836 = CARTESIAN_POINT ( 'NONE',  ( -4.458734124999999437, 16.35416666803225993, -2.574251347313719407 ) ) ;
#40837 = ORIENTED_EDGE ( 'NONE', *, *, #19300, .F. ) ;
#40838 = CARTESIAN_POINT ( 'NONE',  ( -6.972266317189433020E-16, -63.12499999726880162, -5.000000000000000000 ) ) ;
#40839 = CARTESIAN_POINT ( 'NONE',  ( 1.975475456537005874E-15, -98.74999999999998579, 5.000000000000000000 ) ) ;
#40840 = CARTESIAN_POINT ( 'NONE',  ( 4.458734124999999437, -17.81249999863440792, -5.460374474430324690E-16 ) ) ;
#40841 = CARTESIAN_POINT ( 'NONE',  ( -6.972266317189433020E-16, -85.12499999726880162, -5.000000000000000000 ) ) ;
#40842 = FACE_OUTER_BOUND ( 'NONE', #58592, .T. ) ;
#40843 = CARTESIAN_POINT ( 'NONE',  ( -58.39396692619412477, -151.4375000013656063, 2.891590998281057701 ) ) ;
#40844 = ADVANCED_FACE ( 'NONE', ( #1285 ), #30189, .T. ) ;
#40845 = CARTESIAN_POINT ( 'NONE',  ( 5.000000000000000888, -44.45833333060214443, 2.886751345948126879 ) ) ;
#40846 = CARTESIAN_POINT ( 'NONE',  ( 0.000000000000000000, -120.0000000000000000, 0.000000000000000000 ) ) ;
#40847 = CARTESIAN_POINT ( 'NONE',  ( -4.458734124999999437, 6.687500001365593860, 0.000000000000000000 ) ) ;
#40848 = DIRECTION ( 'NONE',  ( 0.000000000000000000, 0.000000000000000000, 1.000000000000000000 ) ) ;
#40849 = CYLINDRICAL_SURFACE ( 'NONE', #21272, 5.000000000000000000 ) ;
#40850 = CARTESIAN_POINT ( 'NONE',  ( 4.458734124999998549, 11.27083333469893134, -2.574251347313721627 ) ) ;
#40851 = CARTESIAN_POINT ( 'NONE',  ( 4.458734124999999437, -67.81249999863440792, -5.460374474430324690E-16 ) ) ;
#40852 = CARTESIAN_POINT ( 'NONE',  ( -4.458734124999997661, -13.47916666530107221, 2.574251347313722516 ) ) ;
#40853 = CARTESIAN_POINT ( 'NONE',  ( -3.535250795749689387E-16, -3.250000000000003109, -5.773502691896257311 ) ) ;
#40854 = CARTESIAN_POINT ( 'NONE',  ( -3.152801135295367096, -164.0625000013656063, -3.152801135295367541 ) ) ;
#40855 = CARTESIAN_POINT ( 'NONE',  ( 0.000000000000000000, 0.000000000000000000, 0.000000000000000000 ) ) ;
#40856 = CARTESIAN_POINT ( 'NONE',  ( -4.458734124999999437, -61.31249999863440081, 0.000000000000000000 ) ) ;
#40857 = CARTESIAN_POINT ( 'NONE',  ( 1.060575238724906964E-15, -96.62499999726880162, 5.773502691896257311 ) ) ;
#40858 = AXIS2_PLACEMENT_3D ( 'NONE', #38021, #57653, #13579 ) ;
#40859 = CARTESIAN_POINT ( 'NONE',  ( -1.339745962155613812, -80.20534180126148271, -5.000000000000000000 ) ) ;
#40860 = DIRECTION ( 'NONE',  ( -0.000000000000000000, 1.000000000000000000, -0.000000000000000000 ) ) ;
#40861 = CARTESIAN_POINT ( 'NONE',  ( -4.458734124999999437, -35.39583333196772941, -2.574251347313719407 ) ) ;
#40862 = CARTESIAN_POINT ( 'NONE',  ( 1.975475456537005874E-15, -60.75000000000000000, 5.000000000000000000 ) ) ;
#40863 = CARTESIAN_POINT ( 'NONE',  ( -2.499999999999996447, -45.83333333333333570, 4.330127018922195425 ) ) ;
#40864 = CARTESIAN_POINT ( 'NONE',  ( -5.000000000000000000, -57.87499999726880873, 0.000000000000000000 ) ) ;
#40865 = DIRECTION ( 'NONE',  ( -1.000000000000000000, 0.000000000000000000, 0.000000000000000000 ) ) ;
#40866 = EDGE_LOOP ( 'NONE', ( #37743, #11991, #37395, #38368 ) ) ;
#40867 = CARTESIAN_POINT ( 'NONE',  ( 4.458734124999999437, -108.8124999986343937, -5.460374474430324690E-16 ) ) ;
#40868 = CARTESIAN_POINT ( 'NONE',  ( 2.229367062499998831, -3.895833331967739177, -3.861377020970580887 ) ) ;
#40869 = CARTESIAN_POINT ( 'NONE',  ( 2.500000000000002220, -59.66666666666665719, 4.330127018922192761 ) ) ;
#40870 = CARTESIAN_POINT ( 'NONE',  ( 5.000000000000000000, -9.416666666666662522, -2.886751345948129988 ) ) ;
#40871 = EDGE_CURVE ( 'NONE', #42718, #7443, #46181, .T. ) ;
#40872 = CARTESIAN_POINT ( 'NONE',  ( -3.152548672688508926E-16, -70.56249999863439371, -5.148502694627439702 ) ) ;
#40873 = CARTESIAN_POINT ( 'NONE',  ( 6.123233995736766282E-16, -170.0000000000000000, -5.000000000000000000 ) ) ;
#40874 = EDGE_CURVE ( 'NONE', #62900, #45629, #10465, .T. ) ;
#40875 = EDGE_CURVE ( 'NONE', #4851, #60221, #46914, .T. ) ;
#40876 = CARTESIAN_POINT ( 'NONE',  ( 2.500000000000002220, -5.541666663935480130, 4.330127018922192761 ) ) ;
#40878 = VERTEX_POINT ( 'NONE', #61714 ) ;
#40877 = CARTESIAN_POINT ( 'NONE',  ( -2.229367062500000163, -38.47916666530107221, -3.861377020970580443 ) ) ;
#40879 = CARTESIAN_POINT ( 'NONE',  ( 1.975475456537005874E-15, -22.62499999726880873, 5.000000000000000000 ) ) ;
#40881 = ORIENTED_EDGE ( 'NONE', *, *, #10072, .T. ) ;
#40880 = CARTESIAN_POINT ( 'NONE',  ( -4.458734124999999437, 11.43750000136559564, 0.000000000000000000 ) ) ;
#40882 = CARTESIAN_POINT ( 'NONE',  ( 1.975475456537005874E-15, -39.75000000000000000, 5.000000000000000000 ) ) ;
#40883 = CARTESIAN_POINT ( 'NONE',  ( 2.500000000000002220, -49.66666666666666430, 4.330127018922192761 ) ) ;
#40884 = CARTESIAN_POINT ( 'NONE',  ( 4.458734124999998549, -29.97916666530107577, -2.574251347313721627 ) ) ;
#40885 = CARTESIAN_POINT ( 'NONE',  ( 1.975475456537005874E-15, -32.62499999726880873, 5.000000000000000000 ) ) ;
#40886 = CARTESIAN_POINT ( 'NONE',  ( 4.458734124999998549, -74.72916666530106511, -2.574251347313721627 ) ) ;
#40887 = CARTESIAN_POINT ( 'NONE',  ( 5.000000000000000888, -168.9375000000000284, -2.071067811865475505 ) ) ;
#40888 = CARTESIAN_POINT ( 'NONE',  ( -2.229367062500000163, -88.47916666530106511, -3.861377020970580443 ) ) ;
#40889 = CARTESIAN_POINT ( 'NONE',  ( -50.55543936806279248, -133.3125000013656063, 0.3552334253322060320 ) ) ;
#40890 = CARTESIAN_POINT ( 'NONE',  ( 4.458734125000001214, -38.14583333196773651, 2.574251347313718519 ) ) ;
#40891 = CARTESIAN_POINT ( 'NONE',  ( -6.972266317189433020E-16, -70.12499999726880162, -5.000000000000000000 ) ) ;
#40893 = ADVANCED_FACE ( 'NONE', ( #3483 ), #52373, .T. ) ;
#40892 = ORIENTED_EDGE ( 'NONE', *, *, #13548, .F. ) ;
#40894 = CARTESIAN_POINT ( 'NONE',  ( 2.229367062499998831, -80.89583333196773651, -3.861377020970580887 ) ) ;
#40895 = CARTESIAN_POINT ( 'NONE',  ( 1.339745962155612702, -21.29465819873852084, -5.000000000000000000 ) ) ;
#40896 = ORIENTED_EDGE ( 'NONE', *, *, #62201, .T. ) ;
#40897 = CARTESIAN_POINT ( 'NONE',  ( -1.339745962155613812, -4.080341798530293218, -5.000000000000000000 ) ) ;
#40898 = VECTOR ( 'NONE', #15525, 1000.000000000000000 ) ;
#40899 = CYLINDRICAL_SURFACE ( 'NONE', #37344, 5.000000000000000000 ) ;
#40900 = CARTESIAN_POINT ( 'NONE',  ( 4.458734124999999437, -63.06249999863440792, -5.460374474430324690E-16 ) ) ;
#40901 = VECTOR ( 'NONE', #25870, 1000.000000000000000 ) ;
#40902 = CARTESIAN_POINT ( 'NONE',  ( -2.229367062499996610, -2.395833331967737845, 3.861377020970582219 ) ) ;
#40903 = ORIENTED_EDGE ( 'NONE', *, *, #61227, .F. ) ;
#40904 =( BOUNDED_CURVE ( )  B_SPLINE_CURVE ( 2, ( #50615, #41264, #11681, #60914, #2375, #12001, #41578, #17153, #56409 ),
 .UNSPECIFIED., .F., .F. ) 
 B_SPLINE_CURVE_WITH_KNOTS ( ( 3, 2, 2, 2, 3 ),
 ( 0.5839285714285714635, 0.5845238095238095566, 0.5857142857142857428, 0.5869047619047619291, 0.5875000000000000222 ),
 .UNSPECIFIED. ) 
 CURVE ( )  GEOMETRIC_REPRESENTATION_ITEM ( )  RATIONAL_B_SPLINE_CURVE ( ( 0.9330127018922194093, 0.9330127018922194093, 1.000000000000000000, 0.8660254037844387076, 1.000000000000000000, 0.8660254037844387076, 1.000000000000000000, 0.9330127018922194093, 0.9330127018922194093 ) ) 
 REPRESENTATION_ITEM ( '' )  );
#40905 = CARTESIAN_POINT ( 'NONE',  ( 1.975475456537005874E-15, -9.624999997268814056, 5.000000000000000000 ) ) ;
#40906 = EDGE_LOOP ( 'NONE', ( #2149, #33228, #4338, #59629 ) ) ;
#40907 = CARTESIAN_POINT ( 'NONE',  ( 1.975475456537005874E-15, -91.74999999999998579, 5.000000000000000000 ) ) ;
#40908 = CARTESIAN_POINT ( 'NONE',  ( 2.229367062499998831, 5.354166668032261711, -3.861377020970580887 ) ) ;
#40909 = CARTESIAN_POINT ( 'NONE',  ( 1.975475456537005874E-15, -32.62499999726880873, 5.000000000000000000 ) ) ;
#40910 = CARTESIAN_POINT ( 'NONE',  ( -4.458734125000000326, -160.8750000013656063, 1.846868145590734089 ) ) ;
#40911 = CARTESIAN_POINT ( 'NONE',  ( -2.500000000000000444, 18.95833333606451632, -4.330127018922193649 ) ) ;
#40912 = ORIENTED_EDGE ( 'NONE', *, *, #4646, .F. ) ;
#40913 = CARTESIAN_POINT ( 'NONE',  ( -4.458734124999999437, -86.39583333196772230, -2.574251347313719407 ) ) ;
#40914 = CARTESIAN_POINT ( 'NONE',  ( 1.339745962155615144, -75.70534180126148271, 4.999999999999999112 ) ) ;
#40915 = CARTESIAN_POINT ( 'NONE',  ( -2.229367062499996610, -2.145833331967737845, 3.861377020970582219 ) ) ;
#40916 = FACE_OUTER_BOUND ( 'NONE', #43095, .T. ) ;
#40917 =( BOUNDED_CURVE ( )  B_SPLINE_CURVE ( 2, ( #48309, #43792, #63439, #19355, #38968, #58606, #50863, #11613, #49580 ),
 .UNSPECIFIED., .F., .F. ) 
 B_SPLINE_CURVE_WITH_KNOTS ( ( 3, 2, 2, 2, 3 ),
 ( 0.03392857142857143293, 0.03452380952380952606, 0.03571428571428571230, 0.03690476190476190549, 0.03750000000000000555 ),
 .UNSPECIFIED. ) 
 CURVE ( )  GEOMETRIC_REPRESENTATION_ITEM ( )  RATIONAL_B_SPLINE_CURVE ( ( 0.9330127018922194093, 0.9330127018922197424, 1.000000000000000000, 0.8660254037844387076, 1.000000000000000000, 0.8660254037844387076, 1.000000000000000000, 0.9330127018922189652, 0.9330127018922194093 ) ) 
 REPRESENTATION_ITEM ( '' )  );
#40918 = CARTESIAN_POINT ( 'NONE',  ( 2.499999999999998668, -30.20833333060214443, -4.330127018922193649 ) ) ;
#40919 = CYLINDRICAL_SURFACE ( 'NONE', #7057, 5.000000000000000000 ) ;
#40920 = CARTESIAN_POINT ( 'NONE',  ( -4.458734124999997661, 23.77083333469892423, 2.574251347313722516 ) ) ;
#40921 = CARTESIAN_POINT ( 'NONE',  ( -4.999999999999998224, -82.79166666393547303, 2.886751345948131764 ) ) ;
#40922 = CARTESIAN_POINT ( 'NONE',  ( 2.229367062500001939, 26.02083333469892779, 3.861377020970579999 ) ) ;
#40923 = CARTESIAN_POINT ( 'NONE',  ( 4.458734124999998549, -48.72916666530107221, -2.574251347313721627 ) ) ;
#40924 = CARTESIAN_POINT ( 'NONE',  ( -2.229367062499996610, -38.39583333196773651, 3.861377020970582219 ) ) ;
#40925 = CARTESIAN_POINT ( 'NONE',  ( -2.229367062499996610, 0.6041666680322611560, 3.861377020970582219 ) ) ;
#40926 = CARTESIAN_POINT ( 'NONE',  ( -5.000000000000000000, 19.91666666666666785, -2.886751345948128211 ) ) ;
#40927 = CARTESIAN_POINT ( 'NONE',  ( 5.000000000000000000, -147.1875000027312126, 2.071067811865478614 ) ) ;
#40928 = CARTESIAN_POINT ( 'NONE',  ( 0.000000000000000000, -120.0000000000000000, 0.000000000000000000 ) ) ;
#40929 = CARTESIAN_POINT ( 'NONE',  ( -4.458734124999999437, -40.39583333196773651, -2.574251347313719407 ) ) ;
#40930 = CARTESIAN_POINT ( 'NONE',  ( -2.499999999999996447, -78.70833333060214443, 4.330127018922195425 ) ) ;
#40931 = CARTESIAN_POINT ( 'NONE',  ( -59.29741812935640155, -141.8750000013655779, -2.196230717870135685 ) ) ;
#40932 = CARTESIAN_POINT ( 'NONE',  ( -2.071067811865478170, -140.3125000000000284, 5.000000000000000000 ) ) ;
#40933 = CARTESIAN_POINT ( 'NONE',  ( 1.339745962155590275, 3.294658198738519950, 5.000000000000013323 ) ) ;
#40934 = CARTESIAN_POINT ( 'NONE',  ( -4.458734124999999437, -82.64583333196773651, -2.574251347313719407 ) ) ;
#40935 = CARTESIAN_POINT ( 'NONE',  ( -1.846868145590737420, -163.0000000013655779, 4.458734124999997661 ) ) ;
#40936 = CARTESIAN_POINT ( 'NONE',  ( 1.339745962155615144, 7.294658198738519950, 4.999999999999999112 ) ) ;
#40937 = CARTESIAN_POINT ( 'NONE',  ( -4.999999999999999112, -28.91666666666666430, 2.886751345948131764 ) ) ;
#40938 = CARTESIAN_POINT ( 'NONE',  ( -3.152801135295367985, -139.8125000013655779, 3.152801135295367096 ) ) ;
#40939 = VERTEX_POINT ( 'NONE', #2539 ) ;
#40940 = CARTESIAN_POINT ( 'NONE',  ( 9.457646018065525792E-16, 23.68750000136559564, 5.148502694627439702 ) ) ;
#40941 = ORIENTED_EDGE ( 'NONE', *, *, #22117, .T. ) ;
#40942 = CARTESIAN_POINT ( 'NONE',  ( -3.152548672688508926E-16, -89.56249999863439371, -5.148502694627439702 ) ) ;
#40943 = CARTESIAN_POINT ( 'NONE',  ( -4.458734124999998549, 12.52083333469892779, 2.574251347313722516 ) ) ;
#40944 = CARTESIAN_POINT ( 'NONE',  ( -2.500000000000000444, 15.95833333606451809, -4.330127018922193649 ) ) ;
#40945 = CYLINDRICAL_SURFACE ( 'NONE', #16530, 5.000000000000000000 ) ;
#40946 = CARTESIAN_POINT ( 'NONE',  ( -5.000000000000000000, 6.916666666666664298, -2.886751345948128211 ) ) ;
#40947 = AXIS2_PLACEMENT_3D ( 'NONE', #53547, #58685, #30043 ) ;
#40948 = CARTESIAN_POINT ( 'NONE',  ( -4.458734124999999437, -55.31249999863440081, 0.000000000000000000 ) ) ;
#40949 = CARTESIAN_POINT ( 'NONE',  ( -4.458734124999998549, -12.22916666530106866, 2.574251347313722516 ) ) ;
#40950 = CARTESIAN_POINT ( 'NONE',  ( -6.972266317189433020E-16, -61.12499999726880162, -5.000000000000000000 ) ) ;
#40951 = EDGE_CURVE ( 'NONE', #53830, #46451, #51741, .T. ) ;
#40952 = ADVANCED_FACE ( 'NONE', ( #62344 ), #18265, .T. ) ;
#40953 = CARTESIAN_POINT ( 'NONE',  ( -53.51423613279429503, -135.5000000013656063, 4.591703134518083651 ) ) ;
#40954 = CYLINDRICAL_SURFACE ( 'NONE', #51258, 5.000000000000000000 ) ;
#40955 = CARTESIAN_POINT ( 'NONE',  ( -4.999999999999998224, -36.91666666666667140, 2.886751345948131764 ) ) ;
#40956 = ADVANCED_FACE ( 'NONE', ( #37892 ), #17063, .F. ) ;
#40957 = CARTESIAN_POINT ( 'NONE',  ( -5.000000000000000000, -62.08333333333332860, -2.886751345948128211 ) ) ;
#40958 = CARTESIAN_POINT ( 'NONE',  ( 1.060575238724906964E-15, -34.75000000000000711, 5.773502691896257311 ) ) ;
#40959 = CARTESIAN_POINT ( 'NONE',  ( 5.000000000000000888, -74.58333333333332860, 2.886751345948126879 ) ) ;
#40961 = CARTESIAN_POINT ( 'NONE',  ( 2.229367062499998831, -13.89583333196774184, -3.861377020970580887 ) ) ;
#40960 = CARTESIAN_POINT ( 'NONE',  ( -59.98410592259440222, -151.1250000000000284, -0.3983568153799752487 ) ) ;
#40962 = LINE ( 'NONE', #59647, #54310 ) ;
#40963 = CARTESIAN_POINT ( 'NONE',  ( 4.458734124999998549, -61.72916666530106511, -2.574251347313721627 ) ) ;
#40964 = CARTESIAN_POINT ( 'NONE',  ( 1.846868145590735200, -153.5000000013656063, -4.458734125000000326 ) ) ;
#40965 = CARTESIAN_POINT ( 'NONE',  ( -2.229367062500000163, -70.47916666530107932, -3.861377020970580443 ) ) ;
#40966 = CARTESIAN_POINT ( 'NONE',  ( -56.48576386720575471, -148.0000000013655779, -4.591703134518078322 ) ) ;
#40967 = ADVANCED_FACE ( 'NONE', ( #27148 ), #27770, .T. ) ;
#40968 = ADVANCED_FACE ( 'NONE', ( #50960 ), #61891, .F. ) ;
#40969 = CARTESIAN_POINT ( 'NONE',  ( -2.499999999999996447, -61.70833333060214443, 4.330127018922195425 ) ) ;
#40970 = ORIENTED_EDGE ( 'NONE', *, *, #13335, .T. ) ;
#40971 = LINE ( 'NONE', #2701, #53801 ) ;
#40972 = ORIENTED_EDGE ( 'NONE', *, *, #34250, .T. ) ;
#40974 = CARTESIAN_POINT ( 'NONE',  ( 1.339745962155615144, -58.70534180126147561, 4.999999999999999112 ) ) ;
#40973 = CARTESIAN_POINT ( 'NONE',  ( -54.60164318462004474, -141.3750000000000284, -4.984105922594373794 ) ) ;
#40975 = CARTESIAN_POINT ( 'NONE',  ( -1.846868145590737420, -151.7500000013655779, 4.458734124999999437 ) ) ;
#40976 = EDGE_CURVE ( 'NONE', #53762, #36069, #29493, .T. ) ;
#40977 = ORIENTED_EDGE ( 'NONE', *, *, #56305, .T. ) ;
#40978 =( BOUNDED_CURVE ( )  B_SPLINE_CURVE ( 2, ( #47346, #42823, #8115, #47031, #22598, #42508, #27400, #18388, #12611 ),
 .UNSPECIFIED., .F., .F. ) 
 B_SPLINE_CURVE_WITH_KNOTS ( ( 3, 2, 2, 2, 3 ),
 ( 0.9053571428571428603, 0.9059523809523809534, 0.9071428571428571397, 0.9083333333333333259, 0.9089285714285714191 ),
 .UNSPECIFIED. ) 
 CURVE ( )  GEOMETRIC_REPRESENTATION_ITEM ( )  RATIONAL_B_SPLINE_CURVE ( ( 0.9330127018922194093, 0.9330127018922194093, 1.000000000000000000, 0.8660254037844387076, 1.000000000000000000, 0.8660254037844387076, 1.000000000000000000, 0.9330127018922194093, 0.9330127018922194093 ) ) 
 REPRESENTATION_ITEM ( '' )  );
#40979 = EDGE_CURVE ( 'NONE', #8963, #12432, #37126, .T. ) ;
#40980 = EDGE_CURVE ( 'NONE', #63269, #17397, #15442, .T. ) ;
#40981 = CARTESIAN_POINT ( 'NONE',  ( 5.000000000000000888, -54.58333333333332860, 2.886751345948126879 ) ) ;
#40982 = CARTESIAN_POINT ( 'NONE',  ( -49.85088928181150436, -129.5625000000000284, -1.666127454062680702 ) ) ;
#40983 = CARTESIAN_POINT ( 'NONE',  ( 4.458734124999999437, -47.06249999863440792, -5.460374474430324690E-16 ) ) ;
#40984 = VERTEX_POINT ( 'NONE', #48879 ) ;
#40985 = CARTESIAN_POINT ( 'NONE',  ( -4.999999999999998224, 17.20833333606451987, 2.886751345948131764 ) ) ;
#40986 = CARTESIAN_POINT ( 'NONE',  ( -3.152548672688508926E-16, 12.43750000136559564, -5.148502694627439702 ) ) ;
#40987 = CARTESIAN_POINT ( 'NONE',  ( 4.458734124999998549, 24.27083333469892779, -2.574251347313721627 ) ) ;
#40988 = CARTESIAN_POINT ( 'NONE',  ( -52.10840900171896806, -150.1875000013656063, 3.393966926194110556 ) ) ;
#40989 = CARTESIAN_POINT ( 'NONE',  ( 2.499999999999998668, -78.20833333060214443, -4.330127018922193649 ) ) ;
#40990 = FACE_OUTER_BOUND ( 'NONE', #3278, .T. ) ;
#40991 = VERTEX_POINT ( 'NONE', #20590 ) ;
#40992 = CARTESIAN_POINT ( 'NONE',  ( -3.152548672688508926E-16, -65.56249999863440792, -5.148502694627439702 ) ) ;
#40993 = CARTESIAN_POINT ( 'NONE',  ( 6.123233995736766282E-16, -120.0000000000000000, -5.000000000000000000 ) ) ;
#40994 = CARTESIAN_POINT ( 'NONE',  ( -2.229367062500000163, 12.52083333469892601, -3.861377020970580443 ) ) ;
#40995 = CARTESIAN_POINT ( 'NONE',  ( -6.972266317189433020E-16, -75.25000000000000000, -5.000000000000000000 ) ) ;
#40996 = CARTESIAN_POINT ( 'NONE',  ( -49.85088928181150436, -152.6875000027312126, -1.666127454062680480 ) ) ;
#40997 = CARTESIAN_POINT ( 'NONE',  ( -2.229367062500000163, -55.72916666530107221, -3.861377020970580443 ) ) ;
#40998 = CARTESIAN_POINT ( 'NONE',  ( 1.060575238724906964E-15, -12.62499999726881050, 5.773502691896257311 ) ) ;
#40999 = CARTESIAN_POINT ( 'NONE',  ( 0.000000000000000000, -120.0000000000000000, 0.000000000000000000 ) ) ;
#41000 = CARTESIAN_POINT ( 'NONE',  ( -6.972266317189433020E-16, -20.12499999726881228, -5.000000000000000000 ) ) ;
#41001 = CARTESIAN_POINT ( 'NONE',  ( 5.000000000000000888, -64.45833333060213022, 2.886751345948126879 ) ) ;
#41002 =( BOUNDED_CURVE ( )  B_SPLINE_CURVE ( 2, ( #55996, #7106, #26720, #16433, #27343, #11595, #31216, #50846, #26396 ),
 .UNSPECIFIED., .F., .F. ) 
 B_SPLINE_CURVE_WITH_KNOTS ( ( 3, 2, 2, 2, 3 ),
 ( 0.8553571428571428159, 0.8559523809523809090, 0.8571428571428570953, 0.8583333333333332815, 0.8589285714285714857 ),
 .UNSPECIFIED. ) 
 CURVE ( )  GEOMETRIC_REPRESENTATION_ITEM ( )  RATIONAL_B_SPLINE_CURVE ( ( 0.9330127018922194093, 0.9330127018922194093, 1.000000000000000000, 0.8660254037844387076, 1.000000000000000000, 0.8660254037844387076, 1.000000000000000000, 0.9330127018922130810, 0.9330127018922194093 ) ) 
 REPRESENTATION_ITEM ( '' )  );
#41003 = CARTESIAN_POINT ( 'NONE',  ( -3.152548672688508926E-16, -22.81249999863440436, -5.148502694627439702 ) ) ;
#41004 = VERTEX_POINT ( 'NONE', #53713 ) ;
#41005 = CARTESIAN_POINT ( 'NONE',  ( -2.500000000000000444, -102.1666666666666572, -4.330127018922193649 ) ) ;
#41006 = CARTESIAN_POINT ( 'NONE',  ( 4.458734124999998549, -103.7291666653010651, -2.574251347313721627 ) ) ;
#41007 = CARTESIAN_POINT ( 'NONE',  ( 3.535533905932738197, -158.0000000027312126, -3.535533905932738197 ) ) ;
#41008 = VERTEX_POINT ( 'NONE', #650 ) ;
#41009 = CARTESIAN_POINT ( 'NONE',  ( 9.457646018065525792E-16, -100.3124999986344079, 5.148502694627439702 ) ) ;
#41010 = CARTESIAN_POINT ( 'NONE',  ( -4.458734124999999437, -29.31249999863440436, 0.000000000000000000 ) ) ;
#41011 = CARTESIAN_POINT ( 'NONE',  ( 5.000000000000000000, -64.37499999726881583, -6.123233995736766282E-16 ) ) ;
#41012 = CARTESIAN_POINT ( 'NONE',  ( -57.89159099828107458, -151.9375000013656063, -3.393966926194107447 ) ) ;
#41013 = CARTESIAN_POINT ( 'NONE',  ( -52.10840900171896806, -144.1875000013656063, 3.393966926194110556 ) ) ;
#41014 = CARTESIAN_POINT ( 'NONE',  ( -4.458734124999999437, -23.39583333196773651, -2.574251347313719407 ) ) ;
#41015 = CARTESIAN_POINT ( 'NONE',  ( -3.152548672688508926E-16, -63.81249999863440792, -5.148502694627439702 ) ) ;
#41016 = CARTESIAN_POINT ( 'NONE',  ( -51.75738570946856498, -153.8750000027312126, 3.805975901505576964 ) ) ;
#41017 = CARTESIAN_POINT ( 'NONE',  ( -2.229367062500000163, -21.47916666530107221, -3.861377020970580443 ) ) ;
#41018 = CARTESIAN_POINT ( 'NONE',  ( 5.000000000000000000, -75.50000000000000000, -6.123233995736766282E-16 ) ) ;
#41019 = CARTESIAN_POINT ( 'NONE',  ( 3.535533905932736864, -149.1250000000000000, 3.535533905932738641 ) ) ;
#41020 = CARTESIAN_POINT ( 'NONE',  ( 1.060575238724906964E-15, -11.74999999999999467, 5.773502691896257311 ) ) ;
#41021 = CARTESIAN_POINT ( 'NONE',  ( 3.152801135295367541, -153.3125000013656063, -3.152801135295367541 ) ) ;
#41022 = ORIENTED_EDGE ( 'NONE', *, *, #33982, .F. ) ;
#41023 = CARTESIAN_POINT ( 'NONE',  ( -3.152548672688508926E-16, -53.81249999863439371, -5.148502694627439702 ) ) ;
#41024 = CARTESIAN_POINT ( 'NONE',  ( -6.972266317189433020E-16, -58.12499999726880162, -5.000000000000000000 ) ) ;
#41025 = CARTESIAN_POINT ( 'NONE',  ( 5.000000000000000000, -90.41666666666667140, -2.886751345948130876 ) ) ;
#41026 = CARTESIAN_POINT ( 'NONE',  ( -3.152548672688508926E-16, -89.56249999863439371, -5.148502694627439702 ) ) ;
#41027 = CARTESIAN_POINT ( 'NONE',  ( -2.229367062500000163, 5.520833334698927786, -3.861377020970580443 ) ) ;
#41028 = CARTESIAN_POINT ( 'NONE',  ( -5.000000000000000000, -160.6250000027311842, -6.123233995736766282E-16 ) ) ;
#41029 = LINE ( 'NONE', #10810, #53295 ) ;
#41030 = CARTESIAN_POINT ( 'NONE',  ( -2.500000000000000444, 25.83333333333333215, -4.330127018922193649 ) ) ;
#41031 = CARTESIAN_POINT ( 'NONE',  ( -3.152548672688508926E-16, 17.18750000136559919, -5.148502694627439702 ) ) ;
#41032 = CARTESIAN_POINT ( 'NONE',  ( 5.000000000000000000, 1.708333336064519425, -2.886751345948129988 ) ) ;
#41033 = VERTEX_POINT ( 'NONE', #29575 ) ;
#41034 = LINE ( 'NONE', #60681, #23288 ) ;
#41035 = EDGE_LOOP ( 'NONE', ( #38052, #39501, #23027, #16870 ) ) ;
#41036 = MECHANICAL_DESIGN_GEOMETRIC_PRESENTATION_REPRESENTATION (  '', ( #28718 ), #40014 ) ;
#41037 = CARTESIAN_POINT ( 'NONE',  ( 5.000000000000000000, -85.49999999999998579, -6.123233995736766282E-16 ) ) ;
#41038 = CARTESIAN_POINT ( 'NONE',  ( 4.458734124999998549, -45.72916666530106511, -2.574251347313721627 ) ) ;
#41039 = CARTESIAN_POINT ( 'NONE',  ( -3.152801135295367096, -162.3125000013656063, -3.152801135295367541 ) ) ;
#41040 = VECTOR ( 'NONE', #41428, 1000.000000000000000 ) ;
#41041 = CARTESIAN_POINT ( 'NONE',  ( -3.535250795749689387E-16, -37.12499999726881583, -5.773502691896257311 ) ) ;
#41042 = ORIENTED_EDGE ( 'NONE', *, *, #11047, .T. ) ;
#41043 = CARTESIAN_POINT ( 'NONE',  ( -4.458734124999998549, -16.22916666530107577, 2.574251347313722516 ) ) ;
#41044 = ORIENTED_EDGE ( 'NONE', *, *, #44341, .F. ) ;
#41045 = CARTESIAN_POINT ( 'NONE',  ( 0.000000000000000000, -120.0000000000000000, 0.000000000000000000 ) ) ;
#41046 = CARTESIAN_POINT ( 'NONE',  ( 2.730187237215162345E-16, -165.1875000013655779, -4.458734124999999437 ) ) ;
#41048 = ORIENTED_EDGE ( 'NONE', *, *, #53478, .T. ) ;
#41047 = CARTESIAN_POINT ( 'NONE',  ( -1.339745962155610925, -34.66965819600733312, 5.000000000000000000 ) ) ;
#41049 = CARTESIAN_POINT ( 'NONE',  ( -56.66612745406270335, -142.3125000000000000, -5.149110718188516067 ) ) ;
#41050 = CARTESIAN_POINT ( 'NONE',  ( 2.229367062499998831, -32.89583333196773651, -3.861377020970580887 ) ) ;
#41051 = CARTESIAN_POINT ( 'NONE',  ( -1.339745962155613812, 22.91965820146970501, -5.000000000000000000 ) ) ;
#41052 = ORIENTED_EDGE ( 'NONE', *, *, #35438, .T. ) ;
#41053 = EDGE_CURVE ( 'NONE', #41004, #14852, #23641, .T. ) ;
#41054 = CARTESIAN_POINT ( 'NONE',  ( -4.458734124999999437, -77.39583333196772230, -2.574251347313719407 ) ) ;
#41055 = CARTESIAN_POINT ( 'NONE',  ( -4.458734124999999437, -109.5624999986343937, 0.000000000000000000 ) ) ;
#41056 = CARTESIAN_POINT ( 'NONE',  ( 6.123233995736766282E-16, 15.00000000000000000, -5.000000000000000000 ) ) ;
#41057 = EDGE_LOOP ( 'NONE', ( #22707, #51828, #6156, #17179, #60724 ) ) ;
#41058 = CARTESIAN_POINT ( 'NONE',  ( 1.975475456537005874E-15, 5.375000002731185944, 5.000000000000000000 ) ) ;
#41059 = CARTESIAN_POINT ( 'NONE',  ( -54.64476657466781973, -142.0625000013656063, -4.444560631937228834 ) ) ;
#41060 = CARTESIAN_POINT ( 'NONE',  ( -4.458734124999999437, -78.56249999863440792, 0.000000000000000000 ) ) ;
#41061 = CARTESIAN_POINT ( 'NONE',  ( -50.01589407740564042, -135.7500000027312126, 0.3983568153799778022 ) ) ;
#41062 = DIRECTION ( 'NONE',  ( -0.000000000000000000, 1.000000000000000000, -0.000000000000000000 ) ) ;
#41063 = CARTESIAN_POINT ( 'NONE',  ( -1.846868145590734756, -141.3750000013656063, -4.458734124999999437 ) ) ;
#41064 = CARTESIAN_POINT ( 'NONE',  ( 4.458734125000000326, -50.89583333196772230, 2.574251347313718519 ) ) ;
#41065 = CARTESIAN_POINT ( 'NONE',  ( -2.229367062500000163, -46.47916666530106511, -3.861377020970580443 ) ) ;
#41066 = CARTESIAN_POINT ( 'NONE',  ( -2.229367062500000163, 29.52083333469892779, -3.861377020970580443 ) ) ;
#41067 = CARTESIAN_POINT ( 'NONE',  ( 5.000000000000000000, -108.4999999999999858, -6.123233995736766282E-16 ) ) ;
#41068 = CARTESIAN_POINT ( 'NONE',  ( 6.158835246850666199E-14, 9.749999999999996447, -4.999999999999999112 ) ) ;
#41069 = CARTESIAN_POINT ( 'NONE',  ( 2.229367062500001939, -40.22916666530107221, 3.861377020970579999 ) ) ;
#41070 = CARTESIAN_POINT ( 'NONE',  ( 1.060575238724906964E-15, -0.6249999972688138339, 5.773502691896257311 ) ) ;
#41071 = CARTESIAN_POINT ( 'NONE',  ( -5.000000000000000000, -73.00000000000000000, 0.000000000000000000 ) ) ;
#41072 = CARTESIAN_POINT ( 'NONE',  ( -58.39396692619412477, -128.4375000013656063, 2.891590998281057701 ) ) ;
#41073 = CARTESIAN_POINT ( 'NONE',  ( -2.229367062500000163, -81.72916666530106511, -3.861377020970580443 ) ) ;
#41074 = CARTESIAN_POINT ( 'NONE',  ( 1.975475456537005874E-15, 6.249999999999998224, 5.000000000000000000 ) ) ;
#41075 = CARTESIAN_POINT ( 'NONE',  ( -4.458734124999999437, -95.31249999863440792, 0.000000000000000000 ) ) ;
#41076 = CARTESIAN_POINT ( 'NONE',  ( 1.975475456537005874E-15, -30.62499999726881583, 5.000000000000000000 ) ) ;
#41077 = CARTESIAN_POINT ( 'NONE',  ( 4.458734125000000326, -1.145833331967740287, 2.574251347313718519 ) ) ;
#41078 = ORIENTED_EDGE ( 'NONE', *, *, #31889, .T. ) ;
#41079 = FACE_OUTER_BOUND ( 'NONE', #30878, .T. ) ;
#41080 = CARTESIAN_POINT ( 'NONE',  ( 0.000000000000000000, -120.0000000000000000, 5.000000000000000000 ) ) ;
#41081 = CARTESIAN_POINT ( 'NONE',  ( -4.458734124999998549, -85.22916666530107932, 2.574251347313722516 ) ) ;
#41082 = CARTESIAN_POINT ( 'NONE',  ( 1.339745962155611592, 27.29465819873851729, 5.000000000000000888 ) ) ;
#41083 = CARTESIAN_POINT ( 'NONE',  ( -2.229367062500000163, -84.72916666530107932, -3.861377020970580443 ) ) ;
#41084 = CARTESIAN_POINT ( 'NONE',  ( 4.458734125000000326, 12.85416666803226171, 2.574251347313718519 ) ) ;
#41085 = CARTESIAN_POINT ( 'NONE',  ( -2.500000000000000444, -53.16666666666666430, -4.330127018922193649 ) ) ;
#41086 = CARTESIAN_POINT ( 'NONE',  ( -52.10840900171896806, -135.1875000013656063, 3.393966926194110556 ) ) ;
#41087 = CARTESIAN_POINT ( 'NONE',  ( -4.458734124999997661, -8.229166665301073991, 2.574251347313722516 ) ) ;
#41088 = CARTESIAN_POINT ( 'NONE',  ( -3.152548672688508926E-16, 17.18750000136559919, -5.148502694627439702 ) ) ;
#41089 = CARTESIAN_POINT ( 'NONE',  ( 4.458734125000000326, -46.14583333196773651, 2.574251347313718519 ) ) ;
#41090 = CARTESIAN_POINT ( 'NONE',  ( 5.000000000000000888, -11.58333333333333393, 2.886751345948126879 ) ) ;
#41091 = CARTESIAN_POINT ( 'NONE',  ( 9.457646018065525792E-16, -88.06249999863439371, 5.148502694627439702 ) ) ;
#41092 = CARTESIAN_POINT ( 'NONE',  ( -4.458734124999999437, -2.395833331967737845, -2.574251347313719407 ) ) ;
#41093 =( LENGTH_UNIT ( ) NAMED_UNIT ( * ) SI_UNIT ( .MILLI., .METRE. ) );
#41094 = ORIENTED_EDGE ( 'NONE', *, *, #9370, .F. ) ;
#41095 = CARTESIAN_POINT ( 'NONE',  ( -4.458734124999999437, -30.56249999863440436, 0.000000000000000000 ) ) ;
#41096 = CARTESIAN_POINT ( 'NONE',  ( -58.39396692619412477, -132.6875000013656063, 2.891590998281057701 ) ) ;
#41097 = CARTESIAN_POINT ( 'NONE',  ( 2.229367062500001939, -76.97916666530106511, 3.861377020970579999 ) ) ;
#41098 = CARTESIAN_POINT ( 'NONE',  ( -2.499999999999996447, -109.7083333306021444, 4.330127018922195425 ) ) ;
#41099 = VECTOR ( 'NONE', #9649, 1000.000000000000114 ) ;
#41100 =( BOUNDED_CURVE ( )  B_SPLINE_CURVE ( 2, ( #17096, #61173, #22247, #61492, #21611, #51825, #7766, #12272, #42166 ),
 .UNSPECIFIED., .F., .F. ) 
 B_SPLINE_CURVE_WITH_KNOTS ( ( 3, 2, 2, 2, 3 ),
 ( 0.3770833333333333259, 0.3777777777777777679, 0.3791666666666666519, 0.3805555555555555358, 0.3812499999999999778 ),
 .UNSPECIFIED. ) 
 CURVE ( )  GEOMETRIC_REPRESENTATION_ITEM ( )  RATIONAL_B_SPLINE_CURVE ( ( 0.9330127018922194093, 0.9330127018922194093, 1.000000000000000000, 0.8660254037844387076, 1.000000000000000000, 0.8660254037844387076, 1.000000000000000000, 0.9330127018922194093, 0.9330127018922194093 ) ) 
 REPRESENTATION_ITEM ( '' )  );
#41101 = CARTESIAN_POINT ( 'NONE',  ( -2.229367062500000163, 22.52083333469892423, -3.861377020970580443 ) ) ;
#41102 = DIRECTION ( 'NONE',  ( -0.6485228581062915110, 0.000000000000000000, -0.7611951803011149931 ) ) ;
#41103 = CARTESIAN_POINT ( 'NONE',  ( -4.999999999999998224, -25.79166666393547658, 2.886751345948131764 ) ) ;
#41104 = CARTESIAN_POINT ( 'NONE',  ( -4.458734124999997661, -77.47916666530106511, 2.574251347313722516 ) ) ;
#41105 = CARTESIAN_POINT ( 'NONE',  ( -5.000000000000000000, -66.00000000000000000, 0.000000000000000000 ) ) ;
#41106 = CARTESIAN_POINT ( 'NONE',  ( -54.60164318462004474, -151.3750000000000284, -4.984105922594373794 ) ) ;
#41107 = CARTESIAN_POINT ( 'NONE',  ( -2.500000000000000444, 19.95833333606451987, -4.330127018922193649 ) ) ;
#41108 = ORIENTED_EDGE ( 'NONE', *, *, #54683, .T. ) ;
#41109 = CARTESIAN_POINT ( 'NONE',  ( -3.535533905932737309, -168.7500000027312126, -3.535533905932738197 ) ) ;
#41111 = CARTESIAN_POINT ( 'NONE',  ( 1.060575238724906964E-15, -22.75000000000000000, 5.773502691896257311 ) ) ;
#41110 = DIRECTION ( 'NONE',  ( -0.000000000000000000, 1.000000000000000000, -0.000000000000000000 ) ) ;
#41112 = CARTESIAN_POINT ( 'NONE',  ( -2.229367062500000163, -29.47916666530107221, -3.861377020970580443 ) ) ;
#41113 = CARTESIAN_POINT ( 'NONE',  ( -4.458734124999999437, -89.31249999863440792, 0.000000000000000000 ) ) ;
#41114 = CARTESIAN_POINT ( 'NONE',  ( 5.000000000000000888, -25.45833333060214443, 2.886751345948126879 ) ) ;
#41116 = ORIENTED_EDGE ( 'NONE', *, *, #44419, .F. ) ;
#41115 = CARTESIAN_POINT ( 'NONE',  ( 2.229367062499998831, -56.64583333196773651, -3.861377020970580887 ) ) ;
#41117 = CARTESIAN_POINT ( 'NONE',  ( 0.000000000000000000, -170.0000000000000000, 5.000000000000000000 ) ) ;
#41118 = CARTESIAN_POINT ( 'NONE',  ( -6.972266317189433020E-16, 10.87500000273118417, -5.000000000000000000 ) ) ;
#41120 = EDGE_LOOP ( 'NONE', ( #46162, #30916, #39486, #63523 ) ) ;
#41119 = CARTESIAN_POINT ( 'NONE',  ( 4.458734124999999437, -4.062499998634408804, -5.460374474430324690E-16 ) ) ;
#41121 = CARTESIAN_POINT ( 'NONE',  ( -2.500000000000000444, -71.16666666666667140, -4.330127018922193649 ) ) ;
#41122 = CARTESIAN_POINT ( 'NONE',  ( -52.10840900171896806, -140.1875000013656063, 3.393966926194110556 ) ) ;
#41123 = CARTESIAN_POINT ( 'NONE',  ( 2.229367062499998831, -43.89583333196774362, -3.861377020970580887 ) ) ;
#41124 = CARTESIAN_POINT ( 'NONE',  ( 5.000000000000000000, -34.50000000000000000, -6.123233995736766282E-16 ) ) ;
#41125 = CARTESIAN_POINT ( 'NONE',  ( 3.061616997868383141E-16, -159.7500000000000000, -5.000000000000000000 ) ) ;
#41126 = CARTESIAN_POINT ( 'NONE',  ( 2.500000000000002220, -72.54166666393548724, 4.330127018922192761 ) ) ;
#41127 = CARTESIAN_POINT ( 'NONE',  ( -5.000000000000000000, -81.87499999726881583, 0.000000000000000000 ) ) ;
#41128 = AXIS2_PLACEMENT_3D ( 'NONE', #34771, #10636, #30249 ) ;
#41129 = CARTESIAN_POINT ( 'NONE',  ( -59.29741812935640155, -124.8750000013656205, -2.196230717870135685 ) ) ;
#41130 = CARTESIAN_POINT ( 'NONE',  ( -3.152548672688508926E-16, -16.81249999863440436, -5.148502694627439702 ) ) ;
#41131 = CARTESIAN_POINT ( 'NONE',  ( 4.458734124999999437, -54.06249999863440081, -5.460374474430324690E-16 ) ) ;
#41132 = CARTESIAN_POINT ( 'NONE',  ( -5.000000000000000000, 0.9166666666666664076, -2.886751345948128211 ) ) ;
#41133 = CARTESIAN_POINT ( 'NONE',  ( -4.458734125000000326, -144.0000000013655779, -1.846868145590735644 ) ) ;
#41134 = CARTESIAN_POINT ( 'NONE',  ( -2.229367062500000163, -93.72916666530106511, -3.861377020970580443 ) ) ;
#41135 = CARTESIAN_POINT ( 'NONE',  ( 6.123233995736766282E-16, -170.0000000000000000, -5.000000000000000000 ) ) ;
#41136 = ORIENTED_EDGE ( 'NONE', *, *, #11033, .T. ) ;
#41137 = CARTESIAN_POINT ( 'NONE',  ( -9.184850993605147944E-16, -155.2500000000000000, 5.000000000000000000 ) ) ;
#41138 = CARTESIAN_POINT ( 'NONE',  ( -4.458734124999999437, 27.43750000136559208, 0.000000000000000000 ) ) ;
#41139 = CARTESIAN_POINT ( 'NONE',  ( -60.14911071818854538, -148.1875000027312126, 1.666127454062681368 ) ) ;
#41140 = CARTESIAN_POINT ( 'NONE',  ( 5.000000000000000000, -60.50000000000000000, -6.123233995736766282E-16 ) ) ;
#41141 = CARTESIAN_POINT ( 'NONE',  ( 4.458734124999999437, -3.812499998634408360, -5.460374474430324690E-16 ) ) ;
#41142 = CARTESIAN_POINT ( 'NONE',  ( -4.458734125000001214, -149.1250000013656063, 1.846868145590734089 ) ) ;
#41143 = CARTESIAN_POINT ( 'NONE',  ( 4.458734125000001214, -24.14583333196773651, 2.574251347313718519 ) ) ;
#41144 =( BOUNDED_CURVE ( )  B_SPLINE_CURVE ( 2, ( #31963, #17501, #22646, #57688, #61567, #56742, #8167, #47701, #8476 ),
 .UNSPECIFIED., .F., .F. ) 
 B_SPLINE_CURVE_WITH_KNOTS ( ( 3, 2, 2, 2, 3 ),
 ( 0.4187500000000000111, 0.4194444444444444531, 0.4208333333333333370, 0.4222222222222222210, 0.4229166666666666630 ),
 .UNSPECIFIED. ) 
 CURVE ( )  GEOMETRIC_REPRESENTATION_ITEM ( )  RATIONAL_B_SPLINE_CURVE ( ( 0.9330127018922194093, 0.9330127018922194093, 1.000000000000000000, 0.8660254037844387076, 1.000000000000000000, 0.8660254037844387076, 1.000000000000000000, 0.9330127018922194093, 0.9330127018922194093 ) ) 
 REPRESENTATION_ITEM ( '' )  );
#41145 = CARTESIAN_POINT ( 'NONE',  ( -4.458734124999999437, -65.56249999863440792, 0.000000000000000000 ) ) ;
#41146 = CARTESIAN_POINT ( 'NONE',  ( -1.339745962155613812, -84.08034179853027013, -5.000000000000000000 ) ) ;
#41147 = CARTESIAN_POINT ( 'NONE',  ( 2.229367062499998831, -6.645833331967741842, -3.861377020970580887 ) ) ;
#41148 = CARTESIAN_POINT ( 'NONE',  ( 7.169303301815196150, -4.521054846639319003, -7.349897473155491134 ) ) ;
#41149 = CARTESIAN_POINT ( 'NONE',  ( 4.458734124999999437, -146.3750000013655779, -1.846868145590734978 ) ) ;
#41150 =( BOUNDED_CURVE ( )  B_SPLINE_CURVE ( 2, ( #42522, #24168, #47666, #9060, #52508, #3618, #27731, #3931, #58272 ),
 .UNSPECIFIED., .F., .F. ) 
 B_SPLINE_CURVE_WITH_KNOTS ( ( 3, 2, 2, 2, 3 ),
 ( 0.9553571428571429047, 0.9559523809523809978, 0.9571428571428571841, 0.9583333333333333703, 0.9589285714285714635 ),
 .UNSPECIFIED. ) 
 CURVE ( )  GEOMETRIC_REPRESENTATION_ITEM ( )  RATIONAL_B_SPLINE_CURVE ( ( 0.9330127018922194093, 0.9330127018922194093, 1.000000000000000000, 0.8660254037844387076, 1.000000000000000000, 0.8660254037844387076, 1.000000000000000000, 0.9330127018922194093, 0.9330127018922194093 ) ) 
 REPRESENTATION_ITEM ( '' )  );
#41151 = CARTESIAN_POINT ( 'NONE',  ( 2.229367062499998831, 15.10416666803225993, -3.861377020970580887 ) ) ;
#41152 = EDGE_LOOP ( 'NONE', ( #12944, #26121, #59236, #16825 ) ) ;
#41153 = CARTESIAN_POINT ( 'NONE',  ( 0.6250000000000013323, 8.299410119600871383, -7.298562697733108173 ) ) ;
#41155 = CARTESIAN_POINT ( 'NONE',  ( 9.457646018065525792E-16, -18.06249999863440436, 5.148502694627439702 ) ) ;
#41154 = CARTESIAN_POINT ( 'NONE',  ( 5.000000000000000000, -87.41666666666667140, -2.886751345948129988 ) ) ;
#41156 = EDGE_CURVE ( 'NONE', #35439, #44817, #35097, .T. ) ;
#41157 = DIRECTION ( 'NONE',  ( 0.000000000000000000, 0.000000000000000000, 1.000000000000000000 ) ) ;
#41158 = CARTESIAN_POINT ( 'NONE',  ( -58.80597590150559739, -138.0000000000000284, 3.242614290531460330 ) ) ;
#41159 = CARTESIAN_POINT ( 'NONE',  ( -52.10840900171896806, -151.1875000013656063, 3.393966926194110556 ) ) ;
#41160 = CARTESIAN_POINT ( 'NONE',  ( -2.499999999999996447, -44.70833333060214443, 4.330127018922195425 ) ) ;
#41161 = CARTESIAN_POINT ( 'NONE',  ( -6.972266317189433020E-16, -41.12499999726880162, -5.000000000000000000 ) ) ;
#41162 = CARTESIAN_POINT ( 'NONE',  ( 4.458734125000000326, 9.104166668032261711, 2.574251347313718519 ) ) ;
#41163 = CARTESIAN_POINT ( 'NONE',  ( 1.975475456537005874E-15, -62.62499999726880873, 5.000000000000000000 ) ) ;
#41164 = CARTESIAN_POINT ( 'NONE',  ( 4.458734124999999437, 12.18750000136559564, -5.460374474430324690E-16 ) ) ;
#41165 = CARTESIAN_POINT ( 'NONE',  ( 4.458734124999998549, -64.72916666530106511, -2.574251347313721627 ) ) ;
#41166 = VECTOR ( 'NONE', #19720, 1000.000000000000000 ) ;
#41167 = CARTESIAN_POINT ( 'NONE',  ( 2.229367062500001939, -15.22916666530107399, 3.861377020970579999 ) ) ;
#41168 = CARTESIAN_POINT ( 'NONE',  ( -4.999999999999999112, -2.916666666666664742, 2.886751345948131764 ) ) ;
#41169 = CARTESIAN_POINT ( 'NONE',  ( -4.458734125000000326, -162.0000000013655779, -1.846868145590735644 ) ) ;
#41170 = CARTESIAN_POINT ( 'NONE',  ( -1.339745962155613812, -38.20534180126147561, -5.000000000000000000 ) ) ;
#41171 = VECTOR ( 'NONE', #43782, 1000.000000000000000 ) ;
#41172 = CARTESIAN_POINT ( 'NONE',  ( -4.458734124999999437, -58.31249999863440081, 0.000000000000000000 ) ) ;
#41173 = CARTESIAN_POINT ( 'NONE',  ( 5.000000000000000000, -97.29166666393547303, -2.886751345948129988 ) ) ;
#41174 = DIRECTION ( 'NONE',  ( -0.000000000000000000, 1.000000000000000000, -0.000000000000000000 ) ) ;
#41175 = CARTESIAN_POINT ( 'NONE',  ( -6.972266317189433020E-16, -56.25000000000000000, -5.000000000000000000 ) ) ;
#41176 = CARTESIAN_POINT ( 'NONE',  ( -2.229367062499996610, -33.14583333196772941, 3.861377020970582219 ) ) ;
#41177 = LINE ( 'NONE', #60189, #59507 ) ;
#41178 =( BOUNDED_CURVE ( )  B_SPLINE_CURVE ( 2, ( #2933, #8383, #62419, #2608, #47603, #22546, #32495, #12252, #42148 ),
 .UNSPECIFIED., .F., .F. ) 
 B_SPLINE_CURVE_WITH_KNOTS ( ( 3, 2, 2, 2, 3 ),
 ( 0.2553571428571428381, 0.2559523809523809312, 0.2571428571428571175, 0.2583333333333333592, 0.2589285714285714524 ),
 .UNSPECIFIED. ) 
 CURVE ( )  GEOMETRIC_REPRESENTATION_ITEM ( )  RATIONAL_B_SPLINE_CURVE ( ( 0.9330127018922194093, 0.9330127018922194093, 1.000000000000000000, 0.8660254037844387076, 1.000000000000000000, 0.8660254037844387076, 1.000000000000000000, 0.9330127018922194093, 0.9330127018922194093 ) ) 
 REPRESENTATION_ITEM ( '' )  );
#41179 = CARTESIAN_POINT ( 'NONE',  ( 5.000000000000000888, -47.58333333333333570, 2.886751345948126879 ) ) ;
#41180 = DIRECTION ( 'NONE',  ( -0.000000000000000000, 1.000000000000000000, -0.000000000000000000 ) ) ;
#41181 = FACE_OUTER_BOUND ( 'NONE', #4347, .T. ) ;
#41182 = ORIENTED_EDGE ( 'NONE', *, *, #60184, .F. ) ;
#41183 = CARTESIAN_POINT ( 'NONE',  ( 2.229367062500001939, -104.9791666653010651, 3.861377020970579999 ) ) ;
#41184 = CARTESIAN_POINT ( 'NONE',  ( -4.458734124999998549, -1.479166665301071770, 2.574251347313722516 ) ) ;
#41185 = DIRECTION ( 'NONE',  ( -0.000000000000000000, 1.000000000000000000, -0.000000000000000000 ) ) ;
#41186 = CARTESIAN_POINT ( 'NONE',  ( -2.500000000000000444, -9.166666666666662522, -4.330127018922193649 ) ) ;
#41187 = CARTESIAN_POINT ( 'NONE',  ( -2.229367062499996610, -74.14583333196773651, 3.861377020970582219 ) ) ;
#41188 = FACE_OUTER_BOUND ( 'NONE', #61778, .T. ) ;
#41189 = CARTESIAN_POINT ( 'NONE',  ( -4.999999999999999112, -9.791666663935476578, 2.886751345948131764 ) ) ;
#41191 = ORIENTED_EDGE ( 'NONE', *, *, #36524, .F. ) ;
#41190 = CARTESIAN_POINT ( 'NONE',  ( 4.458734124999998549, -40.72916666530107221, -2.574251347313721627 ) ) ;
#41192 = DIRECTION ( 'NONE',  ( 0.000000000000000000, 0.000000000000000000, 1.000000000000000000 ) ) ;
#41194 = ORIENTED_EDGE ( 'NONE', *, *, #20950, .F. ) ;
#41193 = CARTESIAN_POINT ( 'NONE',  ( -3.152548672688508926E-16, 13.18750000136559208, -5.148502694627439702 ) ) ;
#41195 = LINE ( 'NONE', #55699, #28907 ) ;
#41196 = CARTESIAN_POINT ( 'NONE',  ( -3.535250795749689387E-16, -55.24999999999998579, -5.773502691896257311 ) ) ;
#41197 = CARTESIAN_POINT ( 'NONE',  ( 4.458734124999998549, -30.97916666530107577, -2.574251347313721627 ) ) ;
#41198 = CARTESIAN_POINT ( 'NONE',  ( 75.00000000000002842, 15.00000000000000000, 5.000000000000000000 ) ) ;
#41199 = CARTESIAN_POINT ( 'NONE',  ( -2.229367062499996610, -78.14583333196773651, 3.861377020970582219 ) ) ;
#41200 =( BOUNDED_CURVE ( )  B_SPLINE_CURVE ( 2, ( #861, #20464, #11748, #61618, #32330, #57112, #12713, #60668, #42296 ),
 .UNSPECIFIED., .F., .F. ) 
 B_SPLINE_CURVE_WITH_KNOTS ( ( 3, 2, 2, 2, 3 ),
 ( 0.2687499999999999889, 0.2694444444444444309, 0.2708333333333333148, 0.2722222222222221988, 0.2729166666666666963 ),
 .UNSPECIFIED. ) 
 CURVE ( )  GEOMETRIC_REPRESENTATION_ITEM ( )  RATIONAL_B_SPLINE_CURVE ( ( 0.9330127018922194093, 0.9330127018922194093, 1.000000000000000000, 0.8660254037844387076, 1.000000000000000000, 0.8660254037844387076, 1.000000000000000000, 0.9330127018922167448, 0.9330127018922194093 ) ) 
 REPRESENTATION_ITEM ( '' )  );
#41201 = CARTESIAN_POINT ( 'NONE',  ( -1.846868145590737420, -142.0000000013655495, 4.458734124999999437 ) ) ;
#41202 = CARTESIAN_POINT ( 'NONE',  ( 9.457646018065525792E-16, -88.06249999863439371, 5.148502694627439702 ) ) ;
#41203 = CARTESIAN_POINT ( 'NONE',  ( -56.48576386720575471, -135.0000000013656347, -4.591703134518078322 ) ) ;
#41204 = CARTESIAN_POINT ( 'NONE',  ( 2.229367062499998831, -33.89583333196772941, -3.861377020970580887 ) ) ;
#41205 = VERTEX_POINT ( 'NONE', #34089 ) ;
#41206 = CARTESIAN_POINT ( 'NONE',  ( 4.458734124999999437, -80.06249999863440792, -5.460374474430324690E-16 ) ) ;
#41207 = CARTESIAN_POINT ( 'NONE',  ( 1.975475456537005874E-15, -84.74999999999998579, 5.000000000000000000 ) ) ;
#41208 = ORIENTED_EDGE ( 'NONE', *, *, #1962, .T. ) ;
#41209 = CARTESIAN_POINT ( 'NONE',  ( -2.499999999999996447, -3.708333330602147537, 4.330127018922195425 ) ) ;
#41211 = VECTOR ( 'NONE', #40643, 1000.000000000000000 ) ;
#41210 = CARTESIAN_POINT ( 'NONE',  ( -4.999999999999998224, -11.79166666393547835, 2.886751345948131764 ) ) ;
#41212 = CARTESIAN_POINT ( 'NONE',  ( 4.458734125000001214, -66.14583333196772230, 2.574251347313718519 ) ) ;
#41213 = CARTESIAN_POINT ( 'NONE',  ( -4.458734124999999437, -11.64583333196773829, -2.574251347313719407 ) ) ;
#41214 = ORIENTED_EDGE ( 'NONE', *, *, #16200, .F. ) ;
#41215 = CARTESIAN_POINT ( 'NONE',  ( -52.53715891517739323, -149.4375000000000000, -4.819101127000233298 ) ) ;
#41216 = CARTESIAN_POINT ( 'NONE',  ( -6.972266317189433020E-16, -93.12499999726881583, -5.000000000000000000 ) ) ;
#41217 = ORIENTED_EDGE ( 'NONE', *, *, #32650, .T. ) ;
#41218 = CARTESIAN_POINT ( 'NONE',  ( 4.458734124999998549, -7.979166665301073991, -2.574251347313721627 ) ) ;
#41219 = CARTESIAN_POINT ( 'NONE',  ( -3.152548672688508926E-16, 9.437500001365593860, -5.148502694627439702 ) ) ;
#41220 = CARTESIAN_POINT ( 'NONE',  ( 1.975475456537005874E-15, -15.75000000000000000, 5.000000000000000000 ) ) ;
#41221 = CARTESIAN_POINT ( 'NONE',  ( -4.458734124999999437, -157.0000000013655779, -1.846868145590735644 ) ) ;
#41222 = CARTESIAN_POINT ( 'NONE',  ( -55.00000000000002132, -155.0000000000000284, 1.734723475976807094E-15 ) ) ;
#41223 = ORIENTED_EDGE ( 'NONE', *, *, #33470, .F. ) ;
#41224 = CARTESIAN_POINT ( 'NONE',  ( 2.229367062500001939, -84.97916666530107932, 3.861377020970579999 ) ) ;
#41225 = CARTESIAN_POINT ( 'NONE',  ( 5.000000000000000000, -164.1250000027311842, 0.000000000000000000 ) ) ;
#41226 = CARTESIAN_POINT ( 'NONE',  ( 4.458734124999999437, -0.8124999986344055847, -5.460374474430324690E-16 ) ) ;
#41227 = ADVANCED_FACE ( 'NONE', ( #330 ), #19616, .T. ) ;
#41228 = CARTESIAN_POINT ( 'NONE',  ( -56.66612745406283125, -147.3125000000000284, -5.149110718188525837 ) ) ;
#41229 = CARTESIAN_POINT ( 'NONE',  ( 2.499999999999998668, -32.20833333060215153, -4.330127018922193649 ) ) ;
#41230 = LINE ( 'NONE', #27090, #7806 ) ;
#41231 = CARTESIAN_POINT ( 'NONE',  ( 2.229367062499998831, 23.35416666803225993, -3.861377020970580887 ) ) ;
#41232 = CARTESIAN_POINT ( 'NONE',  ( -2.499999999999996447, 23.16666666666666430, 4.330127018922195425 ) ) ;
#41233 = CARTESIAN_POINT ( 'NONE',  ( -2.229367062499996610, 28.85416666803226349, 3.861377020970582219 ) ) ;
#41234 = CARTESIAN_POINT ( 'NONE',  ( 9.457646018065525792E-16, -49.06249999863440792, 5.148502694627439702 ) ) ;
#41235 = CARTESIAN_POINT ( 'NONE',  ( 2.229367062500001939, -35.22916666530107221, 3.861377020970579999 ) ) ;
#41236 = CARTESIAN_POINT ( 'NONE',  ( -4.458734124999999437, 2.354166668032262599, -2.574251347313719407 ) ) ;
#41237 = CARTESIAN_POINT ( 'NONE',  ( 1.975475456537005874E-15, -17.75000000000000355, 5.000000000000000000 ) ) ;
#41238 = CARTESIAN_POINT ( 'NONE',  ( -2.499999999999996447, 17.16666666666666430, 4.330127018922195425 ) ) ;
#41239 = CARTESIAN_POINT ( 'NONE',  ( 5.000000000000000888, -145.0625000027311842, -2.071067811865475505 ) ) ;
#41241 = ADVANCED_FACE ( 'NONE', ( #44048 ), #48568, .T. ) ;
#41240 = CARTESIAN_POINT ( 'NONE',  ( 1.339745962155557191, -26.58034179853029499, 5.000000000000032863 ) ) ;
#41242 = CARTESIAN_POINT ( 'NONE',  ( -4.458734124999998549, -41.22916666530107221, 2.574251347313722516 ) ) ;
#41243 = CARTESIAN_POINT ( 'NONE',  ( -5.000000000000000000, -78.87499999726881583, 0.000000000000000000 ) ) ;
#41244 = CARTESIAN_POINT ( 'NONE',  ( -51.60603307380591787, -140.1875000013656063, -2.891590998281053704 ) ) ;
#41245 = CARTESIAN_POINT ( 'NONE',  ( -6.972266317189433020E-16, -93.24999999999998579, -5.000000000000000000 ) ) ;
#41246 = DIRECTION ( 'NONE',  ( -0.000000000000000000, 1.000000000000000000, -0.000000000000000000 ) ) ;
#41247 = EDGE_CURVE ( 'NONE', #57124, #60836, #32921, .T. ) ;
#41248 = CARTESIAN_POINT ( 'NONE',  ( 2.229367062500001939, -87.22916666530107932, 3.861377020970579999 ) ) ;
#41249 = CARTESIAN_POINT ( 'NONE',  ( -8.190561711645485556E-16, -160.9375000013655779, 4.458734124999999437 ) ) ;
#41250 = CARTESIAN_POINT ( 'NONE',  ( 5.000000000000000000, 7.583333333333333925, -2.886751345948130876 ) ) ;
#41251 = CARTESIAN_POINT ( 'NONE',  ( -4.999999999999999112, -30.91666666666666785, 2.886751345948131764 ) ) ;
#41252 = CARTESIAN_POINT ( 'NONE',  ( 2.730187237215162345E-16, -140.1875000013656063, -4.458734124999999437 ) ) ;
#41253 = EDGE_LOOP ( 'NONE', ( #35530, #51843, #40804, #42075 ) ) ;
#41254 = CARTESIAN_POINT ( 'NONE',  ( 4.458734125000001214, 21.85416666803225993, 2.574251347313718519 ) ) ;
#41255 = VERTEX_POINT ( 'NONE', #25401 ) ;
#41256 = CARTESIAN_POINT ( 'NONE',  ( -2.229367062500000163, -92.47916666530106511, -3.861377020970580443 ) ) ;
#41257 = CARTESIAN_POINT ( 'NONE',  ( 2.229367062499998831, 14.10416666803226171, -3.861377020970580887 ) ) ;
#41258 = CARTESIAN_POINT ( 'NONE',  ( 5.000000000000000000, 14.70833333606451987, -2.886751345948129988 ) ) ;
#41259 = FACE_OUTER_BOUND ( 'NONE', #58303, .T. ) ;
#41260 = CARTESIAN_POINT ( 'NONE',  ( -3.535250795749689387E-16, 7.749999999999999112, -5.773502691896257311 ) ) ;
#41261 = CARTESIAN_POINT ( 'NONE',  ( -3.152548672688508926E-16, -58.56249999863439371, -5.148502694627439702 ) ) ;
#41262 = CARTESIAN_POINT ( 'NONE',  ( 4.458734124999998549, -10.72916666530106866, -2.574251347313721627 ) ) ;
#41263 = CARTESIAN_POINT ( 'NONE',  ( 7.499999999997997158, -3.157198044624895061, -7.642795354507847527 ) ) ;
#41264 = CARTESIAN_POINT ( 'NONE',  ( -1.339745962155610925, -51.79465819873851729, 5.000000000000000000 ) ) ;
#41265 = CARTESIAN_POINT ( 'NONE',  ( 2.499999999999998668, -99.20833333060214443, -4.330127018922193649 ) ) ;
#41266 = FACE_OUTER_BOUND ( 'NONE', #61062, .T. ) ;
#41267 = CARTESIAN_POINT ( 'NONE',  ( -2.499999999999996447, -74.70833333060214443, 4.330127018922195425 ) ) ;
#41268 = CARTESIAN_POINT ( 'NONE',  ( -3.535250795749689387E-16, -41.25000000000000000, -5.773502691896257311 ) ) ;
#41269 = CARTESIAN_POINT ( 'NONE',  ( 2.499999999999998668, -107.3333333333333428, -4.330127018922193649 ) ) ;
#41271 = CARTESIAN_POINT ( 'NONE',  ( -4.458734124999998549, -12.47916666530107221, 2.574251347313722516 ) ) ;
#41270 = LINE ( 'NONE', #61874, #3865 ) ;
#41272 = CARTESIAN_POINT ( 'NONE',  ( -4.999999999999998224, 13.08333333333333215, 2.886751345948131764 ) ) ;
#41273 = CARTESIAN_POINT ( 'NONE',  ( 9.457646018065525792E-16, -61.06249999863440081, 5.148502694627439702 ) ) ;
#41274 = CARTESIAN_POINT ( 'NONE',  ( 4.458734124999999437, -150.7500000013655779, 1.846868145590737864 ) ) ;
#41275 = ADVANCED_FACE ( 'NONE', ( #39542 ), #32271, .T. ) ;
#41276 = CARTESIAN_POINT ( 'NONE',  ( -4.458734124999998549, -70.22916666530107932, 2.574251347313722516 ) ) ;
#41277 = CARTESIAN_POINT ( 'NONE',  ( -57.19623071787017210, -145.6250000013655779, 4.297418129356382899 ) ) ;
#41278 =( BOUNDED_CURVE ( )  B_SPLINE_CURVE ( 2, ( #45075, #10656, #31230, #60837, #45718, #6804, #54735, #36380, #56010 ),
 .UNSPECIFIED., .F., .F. ) 
 B_SPLINE_CURVE_WITH_KNOTS ( ( 3, 2, 2, 2, 3 ),
 ( 0.3267857142857142905, 0.3273809523809523836, 0.3285714285714285698, 0.3297619047619047561, 0.3303571428571428492 ),
 .UNSPECIFIED. ) 
 CURVE ( )  GEOMETRIC_REPRESENTATION_ITEM ( )  RATIONAL_B_SPLINE_CURVE ( ( 0.9330127018922194093, 0.9330127018922194093, 1.000000000000000000, 0.8660254037844387076, 1.000000000000000000, 0.8660254037844387076, 1.000000000000000000, 0.9330127018922194093, 0.9330127018922194093 ) ) 
 REPRESENTATION_ITEM ( '' )  );
#41279 = CARTESIAN_POINT ( 'NONE',  ( -4.458734124999998549, -21.47916666530107221, 2.574251347313722516 ) ) ;
#41280 = CARTESIAN_POINT ( 'NONE',  ( -2.499999999999996447, -62.70833333060214443, 4.330127018922195425 ) ) ;
#41281 = ORIENTED_EDGE ( 'NONE', *, *, #17576, .T. ) ;
#41282 = ORIENTED_EDGE ( 'NONE', *, *, #60517, .T. ) ;
#41283 = CARTESIAN_POINT ( 'NONE',  ( -2.229367062499996610, -61.39583333196774362, 3.861377020970582219 ) ) ;
#41285 = CARTESIAN_POINT ( 'NONE',  ( 5.000000000000000000, -8.416666666666669627, -2.886751345948130876 ) ) ;
#41284 = CARTESIAN_POINT ( 'NONE',  ( -2.071067811865580754, -157.8125000027312126, -4.999999999999894307 ) ) ;
#41286 = ADVANCED_FACE ( 'NONE', ( #58214 ), #14142, .T. ) ;
#41287 = CARTESIAN_POINT ( 'NONE',  ( 1.846868145590736310, -150.6250000013655779, 4.458734124999999437 ) ) ;
#41288 = ORIENTED_EDGE ( 'NONE', *, *, #18953, .T. ) ;
#41289 = CARTESIAN_POINT ( 'NONE',  ( 7.500000000000000000, 4.330127018922190096, -10.00000000000000000 ) ) ;
#41290 = CARTESIAN_POINT ( 'NONE',  ( -55.39835681537999790, -125.8750000000000142, 4.984105922594378235 ) ) ;
#41291 = CARTESIAN_POINT ( 'NONE',  ( -6.972266317189433020E-16, -53.12499999726880162, -5.000000000000000000 ) ) ;
#41292 = CARTESIAN_POINT ( 'NONE',  ( 9.457646018065525792E-16, -49.31249999863441502, 5.148502694627439702 ) ) ;
#41293 = VERTEX_POINT ( 'NONE', #8398 ) ;
#41294 =( BOUNDED_CURVE ( )  B_SPLINE_CURVE ( 2, ( #40793, #30836, #302, #26014, #30179, #5433, #49495, #59475, #9928 ),
 .UNSPECIFIED., .F., .F. ) 
 B_SPLINE_CURVE_WITH_KNOTS ( ( 3, 2, 2, 2, 3 ),
 ( 0.6946428571428571175, 0.6952380952380952106, 0.6964285714285713969, 0.6976190476190475831, 0.6982142857142856762 ),
 .UNSPECIFIED. ) 
 CURVE ( )  GEOMETRIC_REPRESENTATION_ITEM ( )  RATIONAL_B_SPLINE_CURVE ( ( 0.9330127018922194093, 0.9330127018922194093, 1.000000000000000000, 0.8660254037844387076, 1.000000000000000000, 0.8660254037844387076, 1.000000000000000000, 0.9330127018922194093, 0.9330127018922194093 ) ) 
 REPRESENTATION_ITEM ( '' )  );
#41295 = CARTESIAN_POINT ( 'NONE',  ( -5.000000000000000000, -145.5000000000000284, -6.123233995736766282E-16 ) ) ;
#41296 = CARTESIAN_POINT ( 'NONE',  ( 4.458734124999999437, 10.18750000136559386, -5.460374474430324690E-16 ) ) ;
#41297 = CARTESIAN_POINT ( 'NONE',  ( 2.229367062499998831, 24.35416666803225993, -3.861377020970580887 ) ) ;
#41298 = CARTESIAN_POINT ( 'NONE',  ( -59.29741812935640155, -150.6250000013656063, -2.196230717870135685 ) ) ;
#41299 = CARTESIAN_POINT ( 'NONE',  ( -5.000000000000000000, -23.87499999726881228, 0.000000000000000000 ) ) ;
#41300 = CARTESIAN_POINT ( 'NONE',  ( 5.000000000000000000, -61.29166666393548013, -2.886751345948130876 ) ) ;
#41301 = VERTEX_POINT ( 'NONE', #13211 ) ;
#41302 = CARTESIAN_POINT ( 'NONE',  ( -2.229367062499996610, -73.14583333196773651, 3.861377020970582219 ) ) ;
#41303 = CARTESIAN_POINT ( 'NONE',  ( -4.999999999999998224, 1.083333333333331927, 2.886751345948131764 ) ) ;
#41304 = CARTESIAN_POINT ( 'NONE',  ( 4.458734125000001214, 10.10416666803226171, 2.574251347313718519 ) ) ;
#41305 = CARTESIAN_POINT ( 'NONE',  ( -1.127183054612291972E-14, 24.25000000000000000, 4.999999999999999112 ) ) ;
#41306 = EDGE_CURVE ( 'NONE', #8603, #21511, #38825, .T. ) ;
#41307 = CYLINDRICAL_SURFACE ( 'NONE', #51118, 5.000000000000000000 ) ;
#41308 = EDGE_CURVE ( 'NONE', #34317, #42312, #23179, .T. ) ;
#41309 = CARTESIAN_POINT ( 'NONE',  ( -2.229367062500000163, -54.72916666530107221, -3.861377020970580443 ) ) ;
#41310 = CARTESIAN_POINT ( 'NONE',  ( 5.000000000000000000, -13.29166666393548191, -2.886751345948129988 ) ) ;
#41311 = CARTESIAN_POINT ( 'NONE',  ( 1.975475456537005874E-15, -99.74999999999998579, 5.000000000000000000 ) ) ;
#41312 = DIRECTION ( 'NONE',  ( -0.000000000000000000, 1.000000000000000000, -0.000000000000000000 ) ) ;
#41313 = EDGE_CURVE ( 'NONE', #4948, #48755, #18351, .T. ) ;
#41314 = CARTESIAN_POINT ( 'NONE',  ( -6.972266317189433020E-16, -65.24999999999998579, -5.000000000000000000 ) ) ;
#41315 = CARTESIAN_POINT ( 'NONE',  ( 9.457646018065525792E-16, -19.31249999863440792, 5.148502694627439702 ) ) ;
#41316 = ORIENTED_EDGE ( 'NONE', *, *, #36910, .F. ) ;
#41317 = DIRECTION ( 'NONE',  ( -0.5000000000000068834, 0.000000000000000000, -0.8660254037844345998 ) ) ;
#41318 = CARTESIAN_POINT ( 'NONE',  ( 4.458734124999999437, -107.8124999986343937, -5.460374474430324690E-16 ) ) ;
#41319 = CARTESIAN_POINT ( 'NONE',  ( -3.535533905932737309, -158.7500000027312126, -3.535533905932738197 ) ) ;
#41320 = ORIENTED_EDGE ( 'NONE', *, *, #17333, .T. ) ;
#41321 = CARTESIAN_POINT ( 'NONE',  ( 4.458734125000001214, -104.1458333319677365, 2.574251347313718519 ) ) ;
#41322 = CARTESIAN_POINT ( 'NONE',  ( -3.152548672688508926E-16, -24.56249999863440792, -5.148502694627439702 ) ) ;
#41323 = CARTESIAN_POINT ( 'NONE',  ( 2.499999999999998668, -61.20833333060214443, -4.330127018922193649 ) ) ;
#41324 = EDGE_CURVE ( 'NONE', #942, #43496, #9013, .T. ) ;
#41325 = CARTESIAN_POINT ( 'NONE',  ( -55.35523342533222291, -151.5625000013656063, 4.444560631937231499 ) ) ;
#41326 = CARTESIAN_POINT ( 'NONE',  ( -5.000000000000000888, -148.5625000000000000, -2.071067811865475949 ) ) ;
#41327 = CARTESIAN_POINT ( 'NONE',  ( -4.458734124999999437, -24.39583333196773651, -2.574251347313719407 ) ) ;
#41328 = EDGE_CURVE ( 'NONE', #51921, #25405, #45419, .T. ) ;
#41329 = CARTESIAN_POINT ( 'NONE',  ( -2.229367062500000163, -68.72916666530107932, -3.861377020970580443 ) ) ;
#41330 = DIRECTION ( 'NONE',  ( -0.000000000000000000, 1.000000000000000000, -0.000000000000000000 ) ) ;
#41331 = CARTESIAN_POINT ( 'NONE',  ( 9.457646018065525792E-16, -27.06249999863440081, 5.148502694627439702 ) ) ;
#41332 = CARTESIAN_POINT ( 'NONE',  ( -2.071067811865475061, -152.6875000000000284, -5.000000000000000888 ) ) ;
#41333 = CARTESIAN_POINT ( 'NONE',  ( -3.535250795749689387E-16, -10.25000000000000355, -5.773502691896257311 ) ) ;
#41334 = CARTESIAN_POINT ( 'NONE',  ( 3.152801135295367541, -151.3125000013655779, -3.152801135295367541 ) ) ;
#41335 = EDGE_LOOP ( 'NONE', ( #59923, #58130, #15752, #47399 ) ) ;
#41336 = B_SPLINE_CURVE_WITH_KNOTS ( 'NONE', 3,
 ( #26690, #46307, #12522, #27317, #2893, #22505 ),
 .UNSPECIFIED., .F., .F.,
 ( 4, 2, 4 ),
 ( 0.000000000000000000, 0.0004189869898913742632, 0.0008379739797827464665 ),
 .UNSPECIFIED. ) ;
#41337 = CARTESIAN_POINT ( 'NONE',  ( -4.458734124999997661, -51.47916666530107932, 2.574251347313722516 ) ) ;
#41338 = CARTESIAN_POINT ( 'NONE',  ( 0.000000000000000000, -170.0000000000000000, 0.000000000000000000 ) ) ;
#41339 = CARTESIAN_POINT ( 'NONE',  ( -7.169303301815100227, 4.521054846639364300, -7.349897473154783256 ) ) ;
#41340 = EDGE_CURVE ( 'NONE', #32024, #25786, #52001, .T. ) ;
#41341 = CARTESIAN_POINT ( 'NONE',  ( -5.000000000000000000, 26.00000000000000000, 0.000000000000000000 ) ) ;
#41342 = LINE ( 'NONE', #56154, #13988 ) ;
#41343 = CARTESIAN_POINT ( 'NONE',  ( 2.229367062500001939, 3.020833334698928674, 3.861377020970579999 ) ) ;
#41344 = PLANE ( 'NONE',  #55477 ) ;
#41345 = CARTESIAN_POINT ( 'NONE',  ( 2.499999999999998668, -41.20833333060214443, -4.330127018922193649 ) ) ;
#41346 = LINE ( 'NONE', #51340, #36552 ) ;
#41347 = CARTESIAN_POINT ( 'NONE',  ( 4.458734124999998549, 14.02083333469892779, -2.574251347313721627 ) ) ;
#41348 = CARTESIAN_POINT ( 'NONE',  ( 5.000000000000000000, 2.625000002731185500, -6.123233995736766282E-16 ) ) ;
#41349 = ORIENTED_EDGE ( 'NONE', *, *, #61815, .F. ) ;
#41350 = CARTESIAN_POINT ( 'NONE',  ( 1.339745962155615588, 26.70534180126147561, -4.999999999999997335 ) ) ;
#41351 = ORIENTED_EDGE ( 'NONE', *, *, #24496, .T. ) ;
#41352 =( BOUNDED_CURVE ( )  B_SPLINE_CURVE ( 2, ( #62182, #8152, #41269, #51891, #57047, #60919, #17158, #7203, #27752 ),
 .UNSPECIFIED., .F., .F. ) 
 B_SPLINE_CURVE_WITH_KNOTS ( ( 3, 2, 2, 2, 3 ),
 ( 0.9803571428571428159, 0.9809523809523809090, 0.9821428571428570953, 0.9833333333333332815, 0.9839285714285714857 ),
 .UNSPECIFIED. ) 
 CURVE ( )  GEOMETRIC_REPRESENTATION_ITEM ( )  RATIONAL_B_SPLINE_CURVE ( ( 0.9330127018922194093, 0.9330127018922194093, 1.000000000000000000, 0.8660254037844387076, 1.000000000000000000, 0.8660254037844387076, 1.000000000000000000, 0.9330127018922130810, 0.9330127018922194093 ) ) 
 REPRESENTATION_ITEM ( '' )  );
#41353 = CARTESIAN_POINT ( 'NONE',  ( 1.975475456537005874E-15, -50.75000000000000000, 5.000000000000000000 ) ) ;
#41354 = CARTESIAN_POINT ( 'NONE',  ( 4.458734124999998549, -42.72916666530107221, -2.574251347313721627 ) ) ;
#41355 = CARTESIAN_POINT ( 'NONE',  ( -4.458734124999999437, -162.1875000013655779, -5.460374474430324690E-16 ) ) ;
#41356 = CARTESIAN_POINT ( 'NONE',  ( -2.500000000000000444, -46.04166666393547303, -4.330127018922193649 ) ) ;
#41357 = ORIENTED_EDGE ( 'NONE', *, *, #5458, .F. ) ;
#41358 = CARTESIAN_POINT ( 'NONE',  ( 9.457646018065525792E-16, -19.06249999863440792, 5.148502694627439702 ) ) ;
#41359 = EDGE_LOOP ( 'NONE', ( #26337, #4982, #31859, #49466 ) ) ;
#41360 = CARTESIAN_POINT ( 'NONE',  ( -4.999999999999999112, -88.91666666666667140, 2.886751345948131764 ) ) ;
#41361 = CARTESIAN_POINT ( 'NONE',  ( -3.152801135295367096, -165.0625000013656063, -3.152801135295367541 ) ) ;
#41363 = ORIENTED_EDGE ( 'NONE', *, *, #13304, .T. ) ;
#41362 = CARTESIAN_POINT ( 'NONE',  ( 0.000000000000000000, -170.0000000000000000, 5.000000000000000000 ) ) ;
#41364 = CARTESIAN_POINT ( 'NONE',  ( -57.46284108482265651, -136.9375000000000000, 4.819101127000239515 ) ) ;
#41365 = CARTESIAN_POINT ( 'NONE',  ( -3.152548672688508926E-16, -33.81249999863440792, -5.148502694627439702 ) ) ;
#41366 = DIRECTION ( 'NONE',  ( -0.000000000000000000, 1.000000000000000000, -0.000000000000000000 ) ) ;
#41367 = ORIENTED_EDGE ( 'NONE', *, *, #44726, .F. ) ;
#41368 = CARTESIAN_POINT ( 'NONE',  ( -3.152548672688508926E-16, -78.56249999863440792, -5.148502694627439702 ) ) ;
#41369 = CARTESIAN_POINT ( 'NONE',  ( -2.229367062499996610, 26.85416666803225993, 3.861377020970582219 ) ) ;
#41370 = CARTESIAN_POINT ( 'NONE',  ( -1.339745962155610925, -53.79465819873851018, 5.000000000000000000 ) ) ;
#41371 = EDGE_LOOP ( 'NONE', ( #54115, #32841, #30443, #45555 ) ) ;
#41372 = LINE ( 'NONE', #60386, #19172 ) ;
#41373 = CARTESIAN_POINT ( 'NONE',  ( -59.44456063193725015, -142.8125000013656063, -0.3552334253322034230 ) ) ;
#41374 = CARTESIAN_POINT ( 'NONE',  ( -3.152548672688508926E-16, -78.81249999863440792, -5.148502694627439702 ) ) ;
#41375 = CARTESIAN_POINT ( 'NONE',  ( -56.66612745406270335, -131.4375000027312126, -5.149110718188516067 ) ) ;
#41376 = CARTESIAN_POINT ( 'NONE',  ( 2.071067811865517694, -142.8124999999999716, -4.999999999999958256 ) ) ;
#41377 = CARTESIAN_POINT ( 'NONE',  ( 4.458734124999997661, -141.7500000013655779, 1.846868145590737864 ) ) ;
#41378 =( BOUNDED_CURVE ( )  B_SPLINE_CURVE ( 2, ( #21377, #36173, #55793, #1458, #21058, #46457, #26196, #21703, #35531 ),
 .UNSPECIFIED., .F., .F. ) 
 B_SPLINE_CURVE_WITH_KNOTS ( ( 3, 2, 2, 2, 3 ),
 ( 0.1303571428571428659, 0.1309523809523809590, 0.1321428571428571452, 0.1333333333333333315, 0.1339285714285714246 ),
 .UNSPECIFIED. ) 
 CURVE ( )  GEOMETRIC_REPRESENTATION_ITEM ( )  RATIONAL_B_SPLINE_CURVE ( ( 0.9330127018922194093, 0.9330127018922194093, 1.000000000000000000, 0.8660254037844387076, 1.000000000000000000, 0.8660254037844387076, 1.000000000000000000, 0.9330127018922194093, 0.9330127018922194093 ) ) 
 REPRESENTATION_ITEM ( '' )  );
#41379 = CARTESIAN_POINT ( 'NONE',  ( 5.000000000000000000, 20.49999999999999645, -6.123233995736766282E-16 ) ) ;
#41380 = CARTESIAN_POINT ( 'NONE',  ( -4.458734124999997661, -55.22916666530107932, 2.574251347313722516 ) ) ;
#41381 = CARTESIAN_POINT ( 'NONE',  ( -2.229367062499996610, -45.14583333196774362, 3.861377020970582219 ) ) ;
#41382 = CARTESIAN_POINT ( 'NONE',  ( -4.999999999999998224, 21.08333333333333215, 2.886751345948131764 ) ) ;
#41383 = CARTESIAN_POINT ( 'NONE',  ( 1.060575238724906964E-15, -104.7500000000000142, 5.773502691896257311 ) ) ;
#41384 = CARTESIAN_POINT ( 'NONE',  ( 5.000000000000000888, -154.0625000027312126, -2.071067811865475505 ) ) ;
#41385 = EDGE_CURVE ( 'NONE', #22249, #11403, #39580, .T. ) ;
#41386 = CARTESIAN_POINT ( 'NONE',  ( -3.152548672688508926E-16, -36.81249999863440792, -5.148502694627439702 ) ) ;
#41387 = CARTESIAN_POINT ( 'NONE',  ( -3.535250795749689387E-16, 0.8750000027311874984, -5.773502691896257311 ) ) ;
#41388 = CARTESIAN_POINT ( 'NONE',  ( -5.000000000000000888, -153.6875000027312126, -2.071067811865475949 ) ) ;
#41389 = CARTESIAN_POINT ( 'NONE',  ( -54.64476657466781973, -128.8125000013656063, -4.444560631937228834 ) ) ;
#41390 = CARTESIAN_POINT ( 'NONE',  ( 4.458734124999999437, -77.06249999863440792, -5.460374474430324690E-16 ) ) ;
#41391 = CARTESIAN_POINT ( 'NONE',  ( 2.500000000000002220, -34.66666666666666430, 4.330127018922192761 ) ) ;
#41392 = CARTESIAN_POINT ( 'NONE',  ( 4.458734124999999437, -95.81249999863440792, -5.460374474430324690E-16 ) ) ;
#41393 = CARTESIAN_POINT ( 'NONE',  ( -2.229367062500000163, -6.729166665301073103, -3.861377020970580443 ) ) ;
#41394 = ORIENTED_EDGE ( 'NONE', *, *, #60217, .F. ) ;
#41395 = DIRECTION ( 'NONE',  ( -0.000000000000000000, 1.000000000000000000, -0.000000000000000000 ) ) ;
#41396 = CARTESIAN_POINT ( 'NONE',  ( -6.972266317189433020E-16, -9.124999997268814056, -5.000000000000000000 ) ) ;
#41397 = CARTESIAN_POINT ( 'NONE',  ( 9.457646018065525792E-16, -90.06249999863440792, 5.148502694627439702 ) ) ;
#41398 = CARTESIAN_POINT ( 'NONE',  ( -5.000000000000000888, -168.5625000027312410, 2.071067811865474617 ) ) ;
#41399 = CARTESIAN_POINT ( 'NONE',  ( -2.229367062499996610, -84.39583333196773651, 3.861377020970582219 ) ) ;
#41400 = CARTESIAN_POINT ( 'NONE',  ( -2.229367062499996610, 14.60416666803226171, 3.861377020970582219 ) ) ;
#41401 = CARTESIAN_POINT ( 'NONE',  ( 0.000000000000000000, -170.0000000000000000, 0.000000000000000000 ) ) ;
#41402 = CARTESIAN_POINT ( 'NONE',  ( -59.44456063193725015, -132.5625000013656063, -0.3552334253322034230 ) ) ;
#41403 = CARTESIAN_POINT ( 'NONE',  ( 2.229367062500001939, -4.979166665301071326, 3.861377020970579999 ) ) ;
#41404 = CARTESIAN_POINT ( 'NONE',  ( 4.458734125000001214, 15.85416666803226171, 2.574251347313718519 ) ) ;
#41405 = CARTESIAN_POINT ( 'NONE',  ( -3.152548672688508926E-16, -47.81249999863440792, -5.148502694627439702 ) ) ;
#41406 = CARTESIAN_POINT ( 'NONE',  ( 1.339745962155612702, -38.16965819600732601, -5.000000000000000000 ) ) ;
#41407 = CARTESIAN_POINT ( 'NONE',  ( 4.458734125000001214, -84.89583333196773651, 2.574251347313718519 ) ) ;
#41408 = CARTESIAN_POINT ( 'NONE',  ( -3.152548672688508926E-16, -10.56249999863440792, -5.148502694627439702 ) ) ;
#41409 = CARTESIAN_POINT ( 'NONE',  ( -5.000000000000000000, -38.99999999999999289, 0.000000000000000000 ) ) ;
#41410 = ADVANCED_FACE ( 'NONE', ( #27686 ), #47313, .T. ) ;
#41411 = ORIENTED_EDGE ( 'NONE', *, *, #62460, .F. ) ;
#41412 = CARTESIAN_POINT ( 'NONE',  ( -2.229367062499996610, -33.39583333196772941, 3.861377020970582219 ) ) ;
#41413 = CARTESIAN_POINT ( 'NONE',  ( -57.89159099828107458, -127.9375000013656063, -3.393966926194107447 ) ) ;
#41414 = EDGE_CURVE ( 'NONE', #32917, #29720, #52754, .T. ) ;
#41415 = CARTESIAN_POINT ( 'NONE',  ( 4.458734125000001214, -77.89583333196773651, 2.574251347313718519 ) ) ;
#41416 = CARTESIAN_POINT ( 'NONE',  ( -5.000000000000000000, -108.8749999972688016, 0.000000000000000000 ) ) ;
#41417 = CARTESIAN_POINT ( 'NONE',  ( 9.457646018065525792E-16, 17.93750000136559208, 5.148502694627439702 ) ) ;
#41418 = ADVANCED_FACE ( 'NONE', ( #30525 ), #29243, .T. ) ;
#41419 = CARTESIAN_POINT ( 'NONE',  ( 6.123233995736766282E-16, -170.0000000000000000, -5.000000000000000000 ) ) ;
#41420 = CARTESIAN_POINT ( 'NONE',  ( -5.000000000000000000, -145.6250000027312126, -6.123233995736766282E-16 ) ) ;
#41421 = CARTESIAN_POINT ( 'NONE',  ( 4.458734125000000326, -85.14583333196773651, 2.574251347313718519 ) ) ;
#41422 = CARTESIAN_POINT ( 'NONE',  ( -3.535250795749689387E-16, -63.25000000000000000, -5.773502691896257311 ) ) ;
#41423 = DIRECTION ( 'NONE',  ( -0.000000000000000000, 1.000000000000000000, -0.000000000000000000 ) ) ;
#41424 = CARTESIAN_POINT ( 'NONE',  ( -5.000000000000000000, 21.12500000273118417, 0.000000000000000000 ) ) ;
#41425 = VERTEX_POINT ( 'NONE', #10277 ) ;
#41426 = FACE_OUTER_BOUND ( 'NONE', #35213, .T. ) ;
#41427 = CARTESIAN_POINT ( 'NONE',  ( -3.535533905932738641, -168.5000000027312126, 3.535533905932737309 ) ) ;
#41429 = CARTESIAN_POINT ( 'NONE',  ( -3.535250795749689387E-16, -26.25000000000000355, -5.773502691896257311 ) ) ;
#41428 = DIRECTION ( 'NONE',  ( -0.000000000000000000, -1.000000000000000000, -0.000000000000000000 ) ) ;
#41430 = CARTESIAN_POINT ( 'NONE',  ( -2.229367062499996610, -29.14583333196774007, 3.861377020970582219 ) ) ;
#41431 = CARTESIAN_POINT ( 'NONE',  ( -3.152548672688508926E-16, -87.56249999863440792, -5.148502694627439702 ) ) ;
#41432 = CARTESIAN_POINT ( 'NONE',  ( -5.000000000000000000, -30.87499999726881228, 0.000000000000000000 ) ) ;
#41434 = ORIENTED_EDGE ( 'NONE', *, *, #50790, .F. ) ;
#41433 = CARTESIAN_POINT ( 'NONE',  ( -4.458734124999998549, -53.22916666530107932, 2.574251347313722516 ) ) ;
#41435 = CARTESIAN_POINT ( 'NONE',  ( -57.89159099828107458, -153.9375000013656063, -3.393966926194107447 ) ) ;
#41437 = VERTEX_POINT ( 'NONE', #29565 ) ;
#41436 = CARTESIAN_POINT ( 'NONE',  ( -4.458734124999998549, -1.479166665301071770, 2.574251347313722516 ) ) ;
#41438 = CARTESIAN_POINT ( 'NONE',  ( 1.060575238724906964E-15, -73.75000000000000000, 5.773502691896257311 ) ) ;
#41439 = CARTESIAN_POINT ( 'NONE',  ( -59.59170313451810586, -139.5000000013656063, 1.485763867205729394 ) ) ;
#41440 = CARTESIAN_POINT ( 'NONE',  ( -4.458734124999999437, -51.56249999863440792, 0.000000000000000000 ) ) ;
#41441 = CARTESIAN_POINT ( 'NONE',  ( 1.975475456537005874E-15, -34.75000000000000000, 5.000000000000000000 ) ) ;
#41442 = CARTESIAN_POINT ( 'NONE',  ( 5.000000000000000888, -71.45833333060214443, 2.886751345948126879 ) ) ;
#41443 = CARTESIAN_POINT ( 'NONE',  ( -2.500000000000000444, -82.04166666393547303, -4.330127018922193649 ) ) ;
#41444 = CARTESIAN_POINT ( 'NONE',  ( -59.81910112700025905, -152.1875000000000284, -2.462841084822630311 ) ) ;
#41445 = CARTESIAN_POINT ( 'NONE',  ( -4.458734124999999437, -16.64583333196773651, -2.574251347313719407 ) ) ;
#41446 = CARTESIAN_POINT ( 'NONE',  ( -4.458734124999999437, -49.64583333196772941, -2.574251347313719407 ) ) ;
#41447 = CARTESIAN_POINT ( 'NONE',  ( -6.972266317189433020E-16, -50.12499999726881583, -5.000000000000000000 ) ) ;
#41448 = CARTESIAN_POINT ( 'NONE',  ( 3.152801135295367541, -141.3125000013655779, -3.152801135295367541 ) ) ;
#41449 = CARTESIAN_POINT ( 'NONE',  ( -4.458734124999999437, -96.64583333196773651, -2.574251347313719407 ) ) ;
#41450 = CARTESIAN_POINT ( 'NONE',  ( 3.535533905932738197, -157.8750000000000284, -3.535533905932738197 ) ) ;
#41451 = ORIENTED_EDGE ( 'NONE', *, *, #22380, .F. ) ;
#41452 = LINE ( 'NONE', #46612, #56034 ) ;
#41453 = CARTESIAN_POINT ( 'NONE',  ( 2.229367062500001939, 25.77083333469892779, 3.861377020970579999 ) ) ;
#41454 = CARTESIAN_POINT ( 'NONE',  ( -51.19402409849444524, -141.6250000027312126, -3.242614290531456334 ) ) ;
#41455 = CARTESIAN_POINT ( 'NONE',  ( -1.339745962155610925, -12.66965819600733134, 5.000000000000000000 ) ) ;
#41456 = CARTESIAN_POINT ( 'NONE',  ( -2.229367062499996610, -3.145833331967738733, 3.861377020970582219 ) ) ;
#41457 = CARTESIAN_POINT ( 'NONE',  ( 4.458734124999998549, -92.97916666530106511, -2.574251347313721627 ) ) ;
#41458 = EDGE_CURVE ( 'NONE', #27288, #49758, #44679, .T. ) ;
#41459 = CARTESIAN_POINT ( 'NONE',  ( 1.846868145590736310, -148.8750000013655495, 4.458734124999999437 ) ) ;
#41460 = CARTESIAN_POINT ( 'NONE',  ( 2.229367062499998831, -24.89583333196773651, -3.861377020970580887 ) ) ;
#41461 = CARTESIAN_POINT ( 'NONE',  ( 5.000000000000000000, -46.41666666666666430, -2.886751345948130876 ) ) ;
#41462 = CARTESIAN_POINT ( 'NONE',  ( 2.229367062499998831, -64.89583333196773651, -3.861377020970580887 ) ) ;
#41463 = CARTESIAN_POINT ( 'NONE',  ( -3.535533905932737309, -154.7500000027312126, -3.535533905932738197 ) ) ;
#41464 = CARTESIAN_POINT ( 'NONE',  ( 6.123233995736766282E-16, -120.0000000000000000, -5.000000000000000000 ) ) ;
#41465 = CARTESIAN_POINT ( 'NONE',  ( -8.190561711645485556E-16, -143.6875000013656063, 4.458734124999999437 ) ) ;
#41466 = CARTESIAN_POINT ( 'NONE',  ( -3.152548672688508926E-16, 9.187500001365592084, -5.148502694627439702 ) ) ;
#41467 = ORIENTED_EDGE ( 'NONE', *, *, #48806, .T. ) ;
#41468 = FACE_OUTER_BOUND ( 'NONE', #44120, .T. ) ;
#41469 = CARTESIAN_POINT ( 'NONE',  ( 2.500000000000002220, 16.33333333333333215, 4.330127018922192761 ) ) ;
#41471 = CARTESIAN_POINT ( 'NONE',  ( 2.229367062499998831, -20.64583333196774007, -3.861377020970580887 ) ) ;
#41470 = CARTESIAN_POINT ( 'NONE',  ( 5.000000000000000888, -85.58333333333332860, 2.886751345948126879 ) ) ;
#41472 = CARTESIAN_POINT ( 'NONE',  ( -4.458734124999999437, 29.35416666803225993, -2.574251347313719407 ) ) ;
#41473 = CARTESIAN_POINT ( 'NONE',  ( -5.000000000000000000, -5.999999999999998224, 0.000000000000000000 ) ) ;
#41474 =( BOUNDED_CURVE ( )  B_SPLINE_CURVE ( 2, ( #4675, #24297, #63549, #34255, #53884, #54848, #6596, #16565, #41000 ),
 .UNSPECIFIED., .F., .F. ) 
 B_SPLINE_CURVE_WITH_KNOTS ( ( 3, 2, 2, 2, 3 ),
 ( 0.4062500000000000000, 0.4069444444444444420, 0.4083333333333333259, 0.4097222222222222099, 0.4104166666666666519 ),
 .UNSPECIFIED. ) 
 CURVE ( )  GEOMETRIC_REPRESENTATION_ITEM ( )  RATIONAL_B_SPLINE_CURVE ( ( 0.9330127018922194093, 0.9330127018922194093, 1.000000000000000000, 0.8660254037844387076, 1.000000000000000000, 0.8660254037844387076, 1.000000000000000000, 0.9330127018922194093, 0.9330127018922194093 ) ) 
 REPRESENTATION_ITEM ( '' )  );
#41475 = CARTESIAN_POINT ( 'NONE',  ( -59.29741812935640155, -144.6250000013656063, -2.196230717870135685 ) ) ;
#41476 = CARTESIAN_POINT ( 'NONE',  ( 5.000000000000000888, -46.45833333060214443, 2.886751345948126879 ) ) ;
#41477 = CARTESIAN_POINT ( 'NONE',  ( 3.535533905932738197, -150.0000000027312126, -3.535533905932738197 ) ) ;
#41478 = CARTESIAN_POINT ( 'NONE',  ( -4.458734124999999437, 8.687500001365595637, 0.000000000000000000 ) ) ;
#41479 = CARTESIAN_POINT ( 'NONE',  ( 7.922281120364393914, -4.573931137438282057, -8.047472243342932430 ) ) ;
#41480 = DIRECTION ( 'NONE',  ( 0.000000000000000000, 0.000000000000000000, 1.000000000000000000 ) ) ;
#41481 = CARTESIAN_POINT ( 'NONE',  ( -2.229367062499996610, 13.85416666803226171, 3.861377020970582219 ) ) ;
#41482 = CARTESIAN_POINT ( 'NONE',  ( 9.457646018065525792E-16, -66.06249999863440792, 5.148502694627439702 ) ) ;
#41483 = CARTESIAN_POINT ( 'NONE',  ( 2.229367062500001939, -21.22916666530107221, 3.861377020970579999 ) ) ;
#41484 = CARTESIAN_POINT ( 'NONE',  ( 5.000000000000000000, -2.500000000000002220, -6.123233995736766282E-16 ) ) ;
#41485 = CARTESIAN_POINT ( 'NONE',  ( -4.458734125000000326, -160.0000000013656063, -1.846868145590735644 ) ) ;
#41486 = CARTESIAN_POINT ( 'NONE',  ( -1.339745962155613812, -41.08034179853029144, -5.000000000000000000 ) ) ;
#41487 = CARTESIAN_POINT ( 'NONE',  ( -4.458734124999998549, -63.22916666530106511, 2.574251347313722516 ) ) ;
#41488 = CARTESIAN_POINT ( 'NONE',  ( 2.499999999999998668, -94.20833333060213022, -4.330127018922193649 ) ) ;
#41489 = CARTESIAN_POINT ( 'NONE',  ( -1.339745962155610925, -69.79465819873850307, 5.000000000000000000 ) ) ;
#41490 = CARTESIAN_POINT ( 'NONE',  ( -5.000000000000000000, -36.08333333333332860, -2.886751345948128211 ) ) ;
#41491 = CARTESIAN_POINT ( 'NONE',  ( -4.458734124999997661, -34.22916666530107221, 2.574251347313722516 ) ) ;
#41492 = DIRECTION ( 'NONE',  ( -0.000000000000000000, 1.000000000000000000, -0.000000000000000000 ) ) ;
#41493 = CARTESIAN_POINT ( 'NONE',  ( -3.535250795749689387E-16, -51.25000000000000000, -5.773502691896257311 ) ) ;
#41494 = CARTESIAN_POINT ( 'NONE',  ( -1.339745962155614700, 27.20534180126147916, 4.999999999999999112 ) ) ;
#41495 = CARTESIAN_POINT ( 'NONE',  ( 5.000000000000000000, -152.1250000027312126, 0.000000000000000000 ) ) ;
#41496 = EDGE_LOOP ( 'NONE', ( #2164, #42879, #29079, #58794 ) ) ;
#41497 = CARTESIAN_POINT ( 'NONE',  ( -4.458734124999999437, -105.3958333319677365, -2.574251347313719407 ) ) ;
#41498 = CARTESIAN_POINT ( 'NONE',  ( -4.458734124999999437, -2.645833331967737845, -2.574251347313719407 ) ) ;
#41499 = CYLINDRICAL_SURFACE ( 'NONE', #3183, 5.000000000000000000 ) ;
#41500 = CARTESIAN_POINT ( 'NONE',  ( 5.000000000000000888, -5.583333333333336590, 2.886751345948126879 ) ) ;
#41501 = CARTESIAN_POINT ( 'NONE',  ( 2.229367062499998831, -73.64583333196773651, -3.861377020970580887 ) ) ;
#41502 = CARTESIAN_POINT ( 'NONE',  ( -5.000000000000000000, -30.95833333060214443, -2.886751345948128211 ) ) ;
#41503 = CARTESIAN_POINT ( 'NONE',  ( -3.535250795749689387E-16, -8.124999997268814056, -5.773502691896257311 ) ) ;
#41505 = EDGE_LOOP ( 'NONE', ( #26099, #226, #51989, #19907 ) ) ;
#41504 = CARTESIAN_POINT ( 'NONE',  ( 2.229367062500001939, -38.97916666530107221, 3.861377020970579999 ) ) ;
#41506 = CARTESIAN_POINT ( 'NONE',  ( 1.339745962155612702, -81.29465819873850307, -5.000000000000000000 ) ) ;
#41508 = ORIENTED_EDGE ( 'NONE', *, *, #56265, .T. ) ;
#41507 = CARTESIAN_POINT ( 'NONE',  ( -2.229367062499996610, 12.60416666803226171, 3.861377020970582219 ) ) ;
#41509 = CARTESIAN_POINT ( 'NONE',  ( -55.00000000000002132, 15.00000000000000000, 5.000000000000000000 ) ) ;
#41510 = CARTESIAN_POINT ( 'NONE',  ( 5.000000000000000000, -57.49999999999999289, -6.123233995736766282E-16 ) ) ;
#41511 = CARTESIAN_POINT ( 'NONE',  ( -1.846868145590734756, -159.3750000013656347, -4.458734125000000326 ) ) ;
#41512 = CARTESIAN_POINT ( 'NONE',  ( 2.229367062499998831, -30.89583333196773651, -3.861377020970580887 ) ) ;
#41513 = DIRECTION ( 'NONE',  ( 1.000000000000000000, 0.000000000000000000, 0.000000000000000000 ) ) ;
#41514 = CARTESIAN_POINT ( 'NONE',  ( -4.458734124999999437, -80.39583333196772230, -2.574251347313719407 ) ) ;
#41515 = CARTESIAN_POINT ( 'NONE',  ( -3.152801135295367096, -141.3125000013655779, -3.152801135295367541 ) ) ;
#41517 = ADVANCED_FACE ( 'NONE', ( #20249 ), #25717, .F. ) ;
#41516 = CARTESIAN_POINT ( 'NONE',  ( 4.458734124999999437, -85.81249999863439371, -5.460374474430324690E-16 ) ) ;
#41518 = CARTESIAN_POINT ( 'NONE',  ( -50.70258187064364108, -134.3750000013656347, 2.196230717870141014 ) ) ;
#41519 = CARTESIAN_POINT ( 'NONE',  ( -4.458734124999998549, -2.479166665301069550, 2.574251347313722516 ) ) ;
#41520 = CARTESIAN_POINT ( 'NONE',  ( -2.229367062500000163, -33.72916666530107221, -3.861377020970580443 ) ) ;
#41521 = CARTESIAN_POINT ( 'NONE',  ( 1.975475456537005874E-15, -24.74999999999999645, 5.000000000000000000 ) ) ;
#41522 = CARTESIAN_POINT ( 'NONE',  ( 9.457646018065525792E-16, -79.31249999863439371, 5.148502694627439702 ) ) ;
#41523 = CARTESIAN_POINT ( 'NONE',  ( 5.000000000000000000, -84.41666666666667140, -2.886751345948130876 ) ) ;
#41524 =( BOUNDED_CURVE ( )  B_SPLINE_CURVE ( 2, ( #13368, #45958, #42631, #21528, #41124, #52608, #21845, #23345, #41441 ),
 .UNSPECIFIED., .F., .F. ) 
 B_SPLINE_CURVE_WITH_KNOTS ( ( 3, 2, 2, 2, 3 ),
 ( 0.4589285714285714080, 0.4595238095238095011, 0.4607142857142856873, 0.4619047619047619291, 0.4625000000000000222 ),
 .UNSPECIFIED. ) 
 CURVE ( )  GEOMETRIC_REPRESENTATION_ITEM ( )  RATIONAL_B_SPLINE_CURVE ( ( 0.9330127018922194093, 0.9330127018922194093, 1.000000000000000000, 0.8660254037844387076, 1.000000000000000000, 0.8660254037844387076, 1.000000000000000000, 0.9330127018922194093, 0.9330127018922194093 ) ) 
 REPRESENTATION_ITEM ( '' )  );
#41525 = ORIENTED_EDGE ( 'NONE', *, *, #389, .T. ) ;
#41526 = LINE ( 'NONE', #61177, #8018 ) ;
#41527 =( BOUNDED_CURVE ( )  B_SPLINE_CURVE ( 2, ( #41353, #25294, #36535, #10493, #30107, #45550, #49737, #40401, #11763 ),
 .UNSPECIFIED., .F., .F. ) 
 B_SPLINE_CURVE_WITH_KNOTS ( ( 3, 2, 2, 2, 3 ),
 ( 0.5767857142857142350, 0.5773809523809523281, 0.5785714285714286254, 0.5797619047619048116, 0.5803571428571429047 ),
 .UNSPECIFIED. ) 
 CURVE ( )  GEOMETRIC_REPRESENTATION_ITEM ( )  RATIONAL_B_SPLINE_CURVE ( ( 0.9330127018922194093, 0.9330127018922194093, 1.000000000000000000, 0.8660254037844387076, 1.000000000000000000, 0.8660254037844387076, 1.000000000000000000, 0.9330127018922194093, 0.9330127018922194093 ) ) 
 REPRESENTATION_ITEM ( '' )  );
#41528 = DIRECTION ( 'NONE',  ( -0.000000000000000000, 1.000000000000000000, -0.000000000000000000 ) ) ;
#41529 = CARTESIAN_POINT ( 'NONE',  ( -4.458734124999999437, -66.56249999863440792, 0.000000000000000000 ) ) ;
#41530 = CARTESIAN_POINT ( 'NONE',  ( 2.229367062499998831, -8.895833331967736513, -3.861377020970580887 ) ) ;
#41531 = ORIENTED_EDGE ( 'NONE', *, *, #32613, .T. ) ;
#41532 = CARTESIAN_POINT ( 'NONE',  ( 1.975475456537005874E-15, 17.25000000000000000, 5.000000000000000000 ) ) ;
#41533 = CARTESIAN_POINT ( 'NONE',  ( 4.458734124999999437, -5.062499998634402587, -5.460374474430324690E-16 ) ) ;
#41534 = CARTESIAN_POINT ( 'NONE',  ( -1.339745962155636017, 3.205341801261477386, 4.999999999999985789 ) ) ;
#41535 = CARTESIAN_POINT ( 'NONE',  ( 4.458734125000001214, 8.104166668032261711, 2.574251347313718519 ) ) ;
#41536 = CARTESIAN_POINT ( 'NONE',  ( 3.535533905932738197, -153.8750000000000000, -3.535533905932738197 ) ) ;
#41537 = CARTESIAN_POINT ( 'NONE',  ( 3.152801135295367541, -156.3125000013656063, -3.152801135295367541 ) ) ;
#41538 = CARTESIAN_POINT ( 'NONE',  ( 0.000000000000000000, -170.0000000000000000, 0.000000000000000000 ) ) ;
#41539 = ORIENTED_EDGE ( 'NONE', *, *, #41607, .T. ) ;
#41540 = CARTESIAN_POINT ( 'NONE',  ( 9.457646018065525792E-16, -85.06249999863440792, 5.148502694627439702 ) ) ;
#41541 = CARTESIAN_POINT ( 'NONE',  ( -1.339745962155610925, -77.79465819873853150, 5.000000000000000000 ) ) ;
#41542 = CARTESIAN_POINT ( 'NONE',  ( 2.229367062500001939, -0.9791666653010712151, 3.861377020970579999 ) ) ;
#41543 = CARTESIAN_POINT ( 'NONE',  ( 0.000000000000000000, -120.0000000000000000, 0.000000000000000000 ) ) ;
#41544 = AXIS2_PLACEMENT_3D ( 'NONE', #14290, #19433, #59641 ) ;
#41545 = CARTESIAN_POINT ( 'NONE',  ( 2.500000000000002220, -28.54166666393548013, 4.330127018922192761 ) ) ;
#41546 = PLANE ( 'NONE',  #910 ) ;
#41547 = CARTESIAN_POINT ( 'NONE',  ( 4.458734125000000326, 25.10416666803225993, 2.574251347313718519 ) ) ;
#41548 = CARTESIAN_POINT ( 'NONE',  ( 0.000000000000000000, -120.0000000000000000, 0.000000000000000000 ) ) ;
#41549 = CARTESIAN_POINT ( 'NONE',  ( 9.457646018065525792E-16, 28.93750000136558853, 5.148502694627439702 ) ) ;
#41550 = CARTESIAN_POINT ( 'NONE',  ( -4.458734124999998549, -49.22916666530106511, 2.574251347313722516 ) ) ;
#41551 = CARTESIAN_POINT ( 'NONE',  ( 4.458734125000000326, -36.14583333196773651, 2.574251347313718519 ) ) ;
#41552 = CARTESIAN_POINT ( 'NONE',  ( -2.229367062500000163, 2.270833334698928230, -3.861377020970580443 ) ) ;
#41553 = CARTESIAN_POINT ( 'NONE',  ( -5.000000000000000000, 9.041666669397853795, -2.886751345948128211 ) ) ;
#41554 = CARTESIAN_POINT ( 'NONE',  ( -3.535250795749689387E-16, 17.75000000000000355, -5.773502691896257311 ) ) ;
#41555 = CARTESIAN_POINT ( 'NONE',  ( 3.535533905932738197, -141.0000000027311842, -3.535533905932738197 ) ) ;
#41556 = CARTESIAN_POINT ( 'NONE',  ( 2.071067811865582087, -159.1875000000000000, 4.999999999999894307 ) ) ;
#41557 = CARTESIAN_POINT ( 'NONE',  ( 4.458734124999998549, -41.72916666530107932, -2.574251347313721627 ) ) ;
#41558 = CARTESIAN_POINT ( 'NONE',  ( 2.500000000000002220, -76.54166666393547303, 4.330127018922192761 ) ) ;
#41559 = CARTESIAN_POINT ( 'NONE',  ( -57.19623071787017210, -139.6250000013655779, 4.297418129356382899 ) ) ;
#41560 = CARTESIAN_POINT ( 'NONE',  ( 2.500000000000002220, -65.54166666393547303, 4.330127018922192761 ) ) ;
#41561 = CARTESIAN_POINT ( 'NONE',  ( -5.000000000000000000, -88.00000000000000000, 0.000000000000000000 ) ) ;
#41562 = CARTESIAN_POINT ( 'NONE',  ( -3.152548672688508926E-16, -83.81249999863437949, -5.148502694627439702 ) ) ;
#41563 = CARTESIAN_POINT ( 'NONE',  ( -1.846868145590734756, -160.3750000013655779, -4.458734124999999437 ) ) ;
#41564 = CARTESIAN_POINT ( 'NONE',  ( 1.339745962155612702, 9.830341803992665106, -5.000000000000000000 ) ) ;
#41565 = CARTESIAN_POINT ( 'NONE',  ( 2.500000000000002220, -34.66666666666666430, 4.330127018922192761 ) ) ;
#41566 = ORIENTED_EDGE ( 'NONE', *, *, #59421, .T. ) ;
#41567 = CARTESIAN_POINT ( 'NONE',  ( 4.458734125000001214, 16.85416666803225638, 2.574251347313718519 ) ) ;
#41568 = ORIENTED_EDGE ( 'NONE', *, *, #16235, .T. ) ;
#41569 = B_SPLINE_CURVE_WITH_KNOTS ( 'NONE', 3,
 ( #55347, #352, #9985, #30885, #38, #30234 ),
 .UNSPECIFIED., .F., .F.,
 ( 4, 2, 4 ),
 ( -5.145455527297706927E-06, 0.0004153350442917481326, 0.0008358155441107939163 ),
 .UNSPECIFIED. ) ;
#41570 = CARTESIAN_POINT ( 'NONE',  ( -4.458734124999999437, -91.31249999863440792, 0.000000000000000000 ) ) ;
#41571 = CARTESIAN_POINT ( 'NONE',  ( 2.229367062499998831, 11.10416666803225993, -3.861377020970580887 ) ) ;
#41572 = CARTESIAN_POINT ( 'NONE',  ( 2.499999999999998668, 17.79166666939785557, -4.330127018922193649 ) ) ;
#41573 =( BOUNDED_CURVE ( )  B_SPLINE_CURVE ( 2, ( #51232, #46077, #6846, #21640, #16805, #60880, #7169, #2035, #25499, #41549, #41233, #26778, #36425, #46396, #36748, #55420, #31917, #56053, #60565, #45439, #55094, #31599, #2345, #59934, #56378, #21953, #61200, #1083, #15855, #1402, #35478, #30641, #50263, #6211, #25824, #26140, #21003, #40608, #60253, #11338, #36111, #30961, #1712, #21321, #40922, #16490, #55734, #11650, #50904, #46710, #3918, #17759, #47032, #12612, #13871, #28035, #52497, #51856, #37687, #47963, #27093, #7480, #23537, #47652, #8738, #3606, #52802, #18696, #61838, #51544, #23214, #42509, #27401, #37073, #27720, #43136, #18389, #7799, #57009, #42824, #38008, #62469, #2982, #28346, #57641, #62776, #13569, #33187, #52172, #41875, #38321, #2655, #22274, #18065, #57950, #61522, #13245, #17452, #57329, #22916, #56696, #32225, #22599, #42196, #37376, #12924, #32546, #8116, #47347, #8431, #3296, #32868, #62147, #9049, #29924, #25105, #29277, #48907, #49549, #63406, #33807, #15138, #43761, #28659, #38619, #14493, #38938, #29602, #48592, #4852, #24472, #19323, #19006, #44078, #356, #58574, #4533, #33495, #34115, #49232, #34760, #48275, #19642, #59534, #44397, #19958, #53736, #54052, #5174, #43449, #24791, #9989, #4231, #39569, #59209, #9669, #54386, #678, #14180, #10311, #5491, #39252, #42, #58878, #14809, #23846, #34423, #63094, #58255, #53423, #53113, #9357, #44715, #20287, #39888, #28969, #24158, #35085, #36354, #16098, #26708, #31204, #26385, #6774, #16737, #16421, #31518, #6460, #59857, #60811, #41481, #6138, #60176, #15782, #49861, #50520, #36039, #26069, #40222, #15467, #46002, #1967, #35398, #20930, #11585, #21568, #2281, #20615, #45687, #10625, #41164, #1644, #5809, #35721, #55670, #55984, #54705, #55351, #11898, #30238, #51161, #40850, #25426, #21243, #60493, #7094, #45045, #50834, #1012, #46323, #21885, #55020, #11265, #10942, #30561, #50186, #25752, #45366, #1333, #30889, #40535, #36672, #22843, #17989, #61132, #2586, #42750, #7729, #56302, #22205, #42121, #2910, #57256, #12538, #12855, #52103, #27334, #46641, #56934, #27959, #22525, #47582, #52730, #8358, #12230, #41804, #31844, #47276, #23467, #3533, #23142, #46965, #37615, #13173, #7413, #32797, #52426, #51476, #62393, #18314, #61763, #32151, #17377, #51787, #3225, #37305, #42433, #17690, #32474, #8044, #27023, #27649, #61448, #36998, #56624, #17055, #62075, #8662, #37939, #57571, #13497, #33113, #3846, #28274, #47889, #44004, #58808, #53986, #34355, #44324, #63651, #57877, #49157, #48209, #13802, #54304, #49481, #53352, #34047, #33734, #33422, #43686, #15071, #62708, #288, #63333, #10245, #34684, #9914, #53669, #29210, #48835, #59136, #9602, #23779, #24720, #5419, #9287, #24091, #43381, #53040, #19570, #4775, #18933, #28588, #19250, #29849, #29523, #63026, #48523, #39182, #5102, #43070, #4163, #24402, #38256, #19887, #14425, #8978, #38864, #14739, #39500, #18634, #38549, #58180, #14109, #28903, #4464, #58501, #30817, #60102, #31131, #39818, #40778, #606, #60423, #11195, #26305, #1257, #25357, #45613, #44975, #50449, #21494, #20216, #41092, #16660, #20860, #40463, #60739, #54948, #941, #11515, #36286, #25035, #16023, #16348, #20544, #55276, #10875, #30492, #35650, #35327, #10554, #6389, #55596, #50114, #59785, #44646, #6069, #21169, #6699, #55909, #15710, #59459, #25683, #25994, #35970, #50754, #1569, #45928, #1890, #11820, #15391, #31439, #51082, #45292, #35016, #54630, #5739, #30164, #49794, #40141, #27259, #7655, #51714, #36916, #27568, #22766, #16980, #42361, #8280, #22127, #36591, #62000, #17618, #41720, #26953, #61370, #12778, #46885, #32400, #32077, #2829, #22447, #46248, #37234, #56227, #12148, #46570, #26628, #61687, #17292, #21813, #56860, #31768, #42045, #13414, #52346, #47201, #7969, #17920, #37541, #57180, #27884, #3145, #2209, #42675, #13099, #47506, #32717, #52026, #7341, #41408, #3456, #23070, #62314, #51400, #7020, #18239, #37863, #61060, #57496, #33036, #2510, #56547, #12466, #48133, #9827, #58731, #53901, #23393, #9212, #53591, #39103, #52652, #28825, #49071, #3769, #29438, #8899, #9521, #43304, #24637, #5018, #19166, #14657, #47812, #44244, #18854, #4084, #48446, #52962, #29128, #8587, #208, #62940, #4693, #4386, #38474, #23707, #28197, #14349, #48751, #42993, #57801, #34276, #58101, #62635, #13723, #33659, #24315, #14030, #24005, #43608, #53277, #38179, #63250, #19489, #38783, #58422, #18557, #33971, #43922, #19806, #39415, #63569, #33347, #59053, #14981, #28515, #6615, #54221, #55518, #35248, #45848, #26228, #45528, #45210, #20776, #40381, #50673, #25597, #15306, #16269, #60660, #25273, #15631, #34928, #5342, #5992, #1176, #10472, #20133, #10798, #1810, #1489, #54549, #40056, #30737, #21092, #21414, #39732, #60022, #29764, #25910, #15945, #24960, #54867, #35567, #40696, #10159, #44565, #55191, #60341, #11112, #50358, #49398, #6306, #35888, #11432, #523, #31050, #59372, #41017, #34590, #30085, #30410, #49715, #5660, #44894, #854, #20457, #59699, #50034, #8206, #12392, #32006, #32639, #46489, #16898, #3071, #13021, #16584, #51640, #32320, #36514, #46802, #2437, #22046, #61610, #26876, #2132, #7574, #47123, #41639, #51325, #36204, #61291, #12705, #61928, #52269, #7263, #51000, #17213, #2749, #27494, #51951, #27186, #22368, #36840, #37164, #11741, #7890, #56787, #56470, #22688, #47434, #60977, #42288, #27809, #41968, #17544, #17847, #37470, #31359, #57103, #21735, #6940, #3386, #23003, #41331, #42604, #55826, #26551, #46171, #56145, #12065, #31690, #57418, #47743, #13339, #48371, #24564, #9444, #29053, #28441, #19089, #14274, #8515, #33893, #63492, #13653, #28125, #53515, #9137, #33273, #18481, #52892, #4313, #38405, #23933, #23630, #43225, #18778, #37788, #28745, #3699, #23314, #38103, #18160, #53203, #8828, #32959, #43534, #42914, #58028, #4941, #43846, #38707, #63178, #48677, #4617, #24242, #19417, #58346, #52584, #34202, #39031, #58658, #14580, #62866, #62562, #57727, #33584, #53825, #9754, #48056, #62242, #29361, #48994, #4009, #13957, #1978, #41176, #56316, #36364, #40547, #2292, #51172, #46335, #14901, #1655, #46015, #31532, #44169, #21255, #41491, #58974, #21894, #448, #21579, #35735, #17065, #61143, #11594, #7105, #39343, #36682, #11276, #60188, #40861, #44487, #60822, #136, #12240, #55363, #16747, #60505, #30902, #16109, #19730, #6786, #55995, #34510, #49322, #26719, #50529, #54141, #5266, #26080, #31215, #6472, #45699, #26395, #10080, #16432, #31852, #36052, #51486, #50844, #11909, #7424, #55680, #24886, #29691, #20945, #22535, #56944, #51796, #41812, #13183, #47285, #27342, #56634, #52112, #57581, #27969, #7738, #17699, #32806, #47591, #8670, #12549, #3235, #2596, #52435, #27658, #61458, #32483, #37624, #27033, #8056, #13508, #17390, #37948, #46973, #57265, #42131, #33123, #52740, #42442, #42760, #37006, #28283, #61773, #2921, #32161, #46650, #8368, #3543, #47896, #37314, #23151, #22852, #12865, #62085, #18001, #62402, #18324, #22215, #25964, #2485, #31104, #15995, #45581, #1860, #26276, #16952, #35941, #36254, #40430, #16320, #56519, #60712, #41695, #50725, #51374, #12440, #31742, #35619, #6360, #55246, #6994, #46855, #7314, #26926, #6669, #41381, #36565, #30789, #11793, #22098, #55569, #50414, #56196, #31411, #11485, #40747, #45899, #26604, #16633, #46220, #21466, #41065, #55882, #60070, #51049, #1537, #21142, #60395, #2183, #21787, #61027, #11166, #12117, #46543, #61343, #27233, #17265, #36890, #32052, #51688, #7629, #20829, #50291, #55447, #25529, #10095, #40323, #784, #16196, #20392, #39992, #40637, #54487, #24898, #11048, #21029, #24576, #59637, #59961, #44499, #54807, #10415, #30026, #5921, #44182, #20064, #60278, #15570, #49655, #59306, #148, #5593, #20718, #6239, #35826, #15241, #58986, #25209, #10736, #35504, #15884, #35189, #30342, #44822, #49968, #25849, #39669, #34522, #45146, #30673, #11362, #5278, #55123, #30986, #1111, #45465, #1430, #50612, #39356, #19743, #29703, #14913, #54154, #49334, #34867, #463, #60909, #21346, #7196, #42221, #26166, #27426, #26803, #17782, #61866, #17478, #17151, #56406, #12331, #22624, #61228, #50932, #51883, #32575, #16831, #51263, #6873, #40948, #46735, #36775, #46104, #55761, #46425, #37401, #37100, #26488, #11999, #2680, #56718, #57037, #11678, #31942, #1745, #61547, #41576, #60598, #2373, #7510, #12636, #45785, #16517, #51570, #32253, #22301, #27121, #36139, #41900, #7823, #47058, #31296, #3008, #2062, #12951, #6551, #21671, #21982, #41261, #36451, #56079, #31626, #47373, #38345, #14517, #63118, #19030, #18414, #9072, #4254, #62171, #23869, #28683, #3322, #43473, #48303, #13592, #58285, #19347, #32895, #57972, #28370, #13896, #33211, #52828, #8763, #27744, #18721, #18093, #37717, #8456, #8144, #13271, #63431, #38034, #38645, #47990, #24178, #22941, #9381, #14204, #53139, #33831, #53449, #28991, #48615, #4554, #42535, #43785, #38961, #58597, #52196, #57353, #52521, #62496, #28062, #47679, #43161, #3631, #23239, #42852, #57667, #3944, #23567, #62801, #33523, #45388, #25449, #29626, #55044, #40246, #35422, #30264, #45069, #34784, #24498, #20640, #53757, #4877, #701, #10649, #59559, #48928, #39912, #5513, #59885, #44102, #49886, #9692, #5836, #20312, #10970, #10337, #34446, #15805, #1354, #35113, #19664, #1036, #29947, #25778, #49572, #25127, #50211, #381, #54077, #30589, #6162, #34138, #44740, #20957, #10015, #15492, #19985, #39593, #54729, #29299, #49260, #40558, #60201, #59230, #5198, #66, #39277, #58904, #14832, #24816, #44420, #15162, #54408, #17076, #35746, #51805, #12251, #37018, #31865, #17403, #46984, #26406, #42147, #36695, #51183, #40872, #16119, #27044, #56330, #50539, #2931, #51498, #7434, #27350, #46661, #11604, #56645, #22225, #12560, #2606, #41824, #16758, #6482, #55371, #36374, #32172, #30912, #7747, #36062, #61469, #6799, #22545, #11286, #46345, #26090, #45712, #1665, #46025, #31224, #60515, #21266, #16442, #41501, #55691, #50855, #1988, #56005, #21590, #41187, #60832, #61154, #11919, #31547, #7114, #26731, #2302, #21904, #3250, #42772, #3555, #57898, #13195, #13521, #17710, #57278, #33754, #37959, #18952, #27983, #28608, #53371, #8997, #56955, #47297, #12876, #47909, #24110, #48224, #4182, #47602, #18651, #13822, #8067, #52753, #63043, #32818, #27669, #33441, #23164, #38569, #9306, #61782, #14127, #62417, #18336, #57593, #33139, #32494, #23796, #22863, #52125, #28920, #4482, #42454, #48543, #8683, #38273, #28296, #37325, #62097, #43398, #18013, #37637, #52447, #3864, #8382, #58199, #23485, #43088, #53058, #62728, #53687, #15414, #44997, #58826, #9620, #35037, #54648, #58519, #29868, #44023, #49498, #19903, #5437, #5120, #24739, #305, #19269, #10264, #29227, #48854, #63670, #63353, #34703, #34373, #14443, #25055, #4796, #39517, #50134, #25375, #625, #44664, #59478, #10573, #30183, #962, #20235, #38884, #15728, #39837, #20563, #49812, #44342, #19590, #34065, #15088, #5757, #54328, #24421, #43707, #40166, #59807, #39200, #10896, #35347, #54967, #30511, #6089, #14756, #54002, #9931, #29546, #49179, #59155, #26652, #12172, #25701, #45947, #22149, #40481, #2535, #45635, #46271, #16370, #61393, #41744, #55928, #51421, #20879, #17319, #55620, #21190, #1912, #26018, #7364, #56567, #2230, #11216, #41431, #21517, #35989, #40798, #1279, #51102, #21834, #45312, #30840, #26972, #11535, #60122, #50470, #6719, #11843, #31150, #50778, #7041, #16044, #60445, #36941, #41113, #46591, #26329, #56250, #31789, #12489, #61080, #17001, #60761, #35672, #32101, #55300, #6408 ),
 .UNSPECIFIED., .F., .F. ) 
 B_SPLINE_CURVE_WITH_KNOTS ( ( 3, 2, 2, 2, 2, 2, 2, 2, 2, 2, 2, 2, 2, 2, 2, 2, 2, 2, 2, 2, 2, 2, 2, 2, 2, 2, 2, 2, 2, 2, 2, 2, 2, 2, 2, 2, 2, 2, 2, 2, 2, 2, 2, 2, 2, 2, 2, 2, 2, 2, 2, 2, 2, 2, 2, 2, 2, 2, 2, 2, 2, 2, 2, 2, 2, 2, 2, 2, 2, 2, 2, 2, 2, 2, 2, 2, 2, 2, 2, 2, 2, 2, 2, 2, 2, 2, 2, 2, 2, 2, 2, 2, 2, 2, 2, 2, 2, 2, 2, 2, 2, 2, 2, 2, 2, 2, 2, 2, 2, 2, 2, 2, 2, 2, 2, 2, 2, 2, 2, 2, 2, 2, 2, 2, 2, 2, 2, 2, 2, 2, 2, 2, 2, 2, 2, 2, 2, 2, 2, 2, 2, 2, 2, 2, 2, 2, 2, 2, 2, 2, 2, 2, 2, 2, 2, 2, 2, 2, 2, 2, 2, 2, 2, 2, 2, 2, 2, 2, 2, 2, 2, 2, 2, 2, 2, 2, 2, 2, 2, 2, 2, 2, 2, 2, 2, 2, 2, 2, 2, 2, 2, 2, 2, 2, 2, 2, 2, 2, 2, 2, 2, 2, 2, 2, 2, 2, 2, 2, 2, 2, 2, 2, 2, 2, 2, 2, 2, 2, 2, 2, 2, 2, 2, 2, 2, 2, 2, 2, 2, 2, 2, 2, 2, 2, 2, 2, 2, 2, 2, 2, 2, 2, 2, 2, 2, 2, 2, 2, 2, 2, 2, 2, 2, 2, 2, 2, 2, 2, 2, 2, 2, 2, 2, 2, 2, 2, 2, 2, 2, 2, 2, 2, 2, 2, 2, 2, 2, 2, 2, 2, 2, 2, 2, 2, 2, 2, 2, 2, 2, 2, 2, 2, 2, 2, 2, 2, 2, 2, 2, 2, 2, 2, 2, 2, 2, 2, 2, 2, 2, 2, 2, 2, 2, 2, 2, 2, 2, 2, 2, 2, 2, 2, 2, 2, 2, 2, 2, 2, 2, 2, 2, 2, 2, 2, 2, 2, 2, 2, 2, 2, 2, 2, 2, 2, 2, 2, 2, 2, 2, 2, 2, 2, 2, 2, 2, 2, 2, 2, 2, 2, 2, 2, 2, 2, 2, 2, 2, 2, 2, 2, 2, 2, 2, 2, 2, 2, 2, 2, 2, 2, 2, 2, 2, 2, 2, 2, 2, 2, 2, 2, 2, 2, 2, 2, 2, 2, 2, 2, 2, 2, 2, 2, 2, 2, 2, 2, 2, 2, 2, 2, 2, 2, 2, 2, 2, 2, 2, 2, 2, 2, 2, 2, 2, 2, 2, 2, 2, 2, 2, 2, 2, 2, 2, 2, 2, 2, 2, 2, 2, 2, 2, 2, 2, 2, 2, 2, 2, 2, 2, 2, 2, 2, 2, 2, 2, 2, 2, 2, 2, 2, 2, 2, 2, 2, 2, 2, 2, 2, 2, 2, 2, 2, 2, 2, 2, 2, 2, 2, 2, 2, 2, 2, 2, 2, 2, 2, 2, 2, 2, 2, 2, 2, 2, 2, 2, 2, 2, 2, 2, 2, 2, 2, 2, 2, 2, 2, 2, 2, 2, 2, 2, 2, 2, 2, 2, 2, 2, 2, 2, 2, 2, 2, 2, 2, 2, 2, 2, 2, 2, 2, 2, 2, 2, 2, 2, 2, 2, 2, 2, 2, 2, 2, 2, 2, 2, 2, 2, 2, 2, 2, 2, 2, 2, 2, 2, 2, 2, 2, 2, 2, 2, 2, 2, 2, 2, 2, 2, 2, 2, 2, 2, 2, 2, 2, 2, 2, 2, 2, 2, 2, 2, 2, 2, 2, 2, 2, 2, 2, 2, 2, 2, 2, 2, 2, 2, 2, 2, 2, 2, 2, 2, 2, 2, 2, 2, 2, 2, 2, 2, 2, 2, 2, 2, 2, 2, 2, 2, 2, 2, 2, 2, 2, 2, 2, 2, 2, 2, 2, 2, 2, 2, 2, 2, 2, 2, 2, 2, 2, 2, 2, 2, 2, 2, 2, 2, 2, 2, 2, 2, 2, 2, 2, 2, 2, 2, 2, 2, 2, 2, 2, 2, 2, 2, 2, 2, 2, 2, 2, 2, 2, 2, 2, 2, 2, 2, 2, 2, 2, 2, 2, 2, 2, 2, 2, 2, 2, 2, 2, 2, 2, 2, 2, 2, 2, 2, 2, 2, 2, 2, 2, 2, 2, 2, 2, 2, 2, 2, 2, 2, 2, 2, 2, 2, 2, 2, 2, 2, 2, 2, 2, 3 ),
 ( 0.000000000000000000, 0.001388888888888888942, 0.002777777777777777884, 0.004166666666666666609, 0.005555555555555555768, 0.006944444444444444059, 0.008333333333333333218, 0.009722222222222222376, 0.01111111111111111154, 0.01250000000000000069, 0.01388888888888888812, 0.01527777777777777728, 0.01666666666666666644, 0.01805555555555555386, 0.01944444444444444475, 0.02083333333333333218, 0.02222222222222222307, 0.02361111111111111049, 0.02500000000000000139, 0.02638888888888888881, 0.02777777777777777624, 0.02916666666666666713, 0.03055555555555555455, 0.03194444444444444198, 0.03333333333333333287, 0.03472222222222222376, 0.03611111111111110772, 0.03749999999999999861, 0.03888888888888888951, 0.04027777777777778040, 0.04166666666666666435, 0.04305555555555555525, 0.04444444444444444614, 0.04583333333333333010, 0.04722222222222222099, 0.04861111111111111188, 0.05000000000000000278, 0.05138888888888888673, 0.05277777777777777762, 0.05416666666666666852, 0.05555555555555555247, 0.05694444444444444337, 0.05833333333333333426, 0.05972222222222222515, 0.06111111111111110911, 0.06250000000000000000, 0.06388888888888888395, 0.06527777777777778179, 0.06666666666666666574, 0.06805555555555554970, 0.06944444444444444753, 0.07083333333333333148, 0.07222222222222221544, 0.07361111111111111327, 0.07499999999999999722, 0.07638888888888889506, 0.07777777777777777901, 0.07916666666666666297, 0.08055555555555556080, 0.08194444444444444475, 0.08333333333333332871, 0.08472222222222222654, 0.08611111111111111049, 0.08749999999999999445, 0.08888888888888889228, 0.09027777777777777624, 0.09166666666666666019, 0.09305555555555555802, 0.09444444444444444198, 0.09583333333333333981, 0.09722222222222222376, 0.09861111111111110772, 0.1000000000000000056, 0.1013888888888888895, 0.1027777777777777735, 0.1041666666666666713, 0.1055555555555555552, 0.1069444444444444392, 0.1083333333333333370, 0.1097222222222222210, 0.1111111111111111049, 0.1125000000000000028, 0.1138888888888888867, 0.1152777777777777846, 0.1166666666666666685, 0.1180555555555555525, 0.1194444444444444503, 0.1208333333333333343, 0.1222222222222222182, 0.1236111111111111160, 0.1250000000000000000, 0.1263888888888888840, 0.1277777777777777679, 0.1291666666666666796, 0.1305555555555555636, 0.1319444444444444475, 0.1333333333333333315, 0.1347222222222222154, 0.1361111111111110994, 0.1375000000000000111, 0.1388888888888888951, 0.1402777777777777790, 0.1416666666666666630, 0.1430555555555555469, 0.1444444444444444309, 0.1458333333333333426, 0.1472222222222222265, 0.1486111111111111105, 0.1499999999999999944, 0.1513888888888888784, 0.1527777777777777901, 0.1541666666666666741, 0.1555555555555555580, 0.1569444444444444420, 0.1583333333333333259, 0.1597222222222222099, 0.1611111111111111216, 0.1625000000000000056, 0.1638888888888888895, 0.1652777777777777735, 0.1666666666666666574, 0.1680555555555555691, 0.1694444444444444531, 0.1708333333333333370, 0.1722222222222222210, 0.1736111111111111049, 0.1749999999999999889, 0.1763888888888889006, 0.1777777777777777846, 0.1791666666666666685, 0.1805555555555555525, 0.1819444444444444364, 0.1833333333333333204, 0.1847222222222222321, 0.1861111111111111160, 0.1875000000000000000, 0.1888888888888888840, 0.1902777777777777679, 0.1916666666666666796, 0.1930555555555555636, 0.1944444444444444475, 0.1958333333333333315, 0.1972222222222222154, 0.1986111111111110994, 0.2000000000000000111, 0.2013888888888888951, 0.2027777777777777790, 0.2041666666666666630, 0.2055555555555555469, 0.2069444444444444309, 0.2083333333333333426, 0.2097222222222222265, 0.2111111111111111105, 0.2124999999999999944, 0.2138888888888888784, 0.2152777777777777901, 0.2166666666666666741, 0.2180555555555555580, 0.2194444444444444420, 0.2208333333333333259, 0.2222222222222222099, 0.2236111111111111216, 0.2250000000000000056, 0.2263888888888888895, 0.2277777777777777735, 0.2291666666666666574, 0.2305555555555555691, 0.2319444444444444531, 0.2333333333333333370, 0.2347222222222222210, 0.2361111111111111049, 0.2374999999999999889, 0.2388888888888889006, 0.2402777777777777846, 0.2416666666666666685, 0.2430555555555555525, 0.2444444444444444364, 0.2458333333333333204, 0.2472222222222222321, 0.2486111111111111160, 0.2500000000000000000, 0.2513888888888888840, 0.2527777777777777679, 0.2541666666666666519, 0.2555555555555555358, 0.2569444444444444198, 0.2583333333333333592, 0.2597222222222222432, 0.2611111111111111271, 0.2625000000000000111, 0.2638888888888888951, 0.2652777777777777790, 0.2666666666666666630, 0.2680555555555555469, 0.2694444444444444309, 0.2708333333333333148, 0.2722222222222221988, 0.2736111111111111382, 0.2750000000000000222, 0.2763888888888889062, 0.2777777777777777901, 0.2791666666666666741, 0.2805555555555555580, 0.2819444444444444420, 0.2833333333333333259, 0.2847222222222222099, 0.2861111111111110938, 0.2874999999999999778, 0.2888888888888888618, 0.2902777777777778012, 0.2916666666666666852, 0.2930555555555555691, 0.2944444444444444531, 0.2958333333333333370, 0.2972222222222222210, 0.2986111111111111049, 0.2999999999999999889, 0.3013888888888888729, 0.3027777777777777568, 0.3041666666666666408, 0.3055555555555555802, 0.3069444444444444642, 0.3083333333333333481, 0.3097222222222222321, 0.3111111111111111160, 0.3125000000000000000, 0.3138888888888888840, 0.3152777777777777679, 0.3166666666666666519, 0.3180555555555555358, 0.3194444444444444198, 0.3208333333333333592, 0.3222222222222222432, 0.3236111111111111271, 0.3250000000000000111, 0.3263888888888888951, 0.3277777777777777790, 0.3291666666666666630, 0.3305555555555555469, 0.3319444444444444309, 0.3333333333333333148, 0.3347222222222221988, 0.3361111111111111382, 0.3375000000000000222, 0.3388888888888889062, 0.3402777777777777901, 0.3416666666666666741, 0.3430555555555555580, 0.3444444444444444420, 0.3458333333333333259, 0.3472222222222222099, 0.3486111111111110938, 0.3499999999999999778, 0.3513888888888888618, 0.3527777777777778012, 0.3541666666666666852, 0.3555555555555555691, 0.3569444444444444531, 0.3583333333333333370, 0.3597222222222222210, 0.3611111111111111049, 0.3624999999999999889, 0.3638888888888888729, 0.3652777777777777568, 0.3666666666666666408, 0.3680555555555555802, 0.3694444444444444642, 0.3708333333333333481, 0.3722222222222222321, 0.3736111111111111160, 0.3750000000000000000, 0.3763888888888888840, 0.3777777777777777679, 0.3791666666666666519, 0.3805555555555555358, 0.3819444444444444198, 0.3833333333333333592, 0.3847222222222222432, 0.3861111111111111271, 0.3875000000000000111, 0.3888888888888888951, 0.3902777777777777790, 0.3916666666666666630, 0.3930555555555555469, 0.3944444444444444309, 0.3958333333333333148, 0.3972222222222221988, 0.3986111111111111382, 0.4000000000000000222, 0.4013888888888889062, 0.4027777777777777901, 0.4041666666666666741, 0.4055555555555555580, 0.4069444444444444420, 0.4083333333333333259, 0.4097222222222222099, 0.4111111111111110938, 0.4124999999999999778, 0.4138888888888888618, 0.4152777777777778012, 0.4166666666666666852, 0.4180555555555555691, 0.4194444444444444531, 0.4208333333333333370, 0.4222222222222222210, 0.4236111111111111049, 0.4249999999999999889, 0.4263888888888888729, 0.4277777777777777568, 0.4291666666666666408, 0.4305555555555555802, 0.4319444444444444642, 0.4333333333333333481, 0.4347222222222222321, 0.4361111111111111160, 0.4375000000000000000, 0.4388888888888888840, 0.4402777777777777679, 0.4416666666666666519, 0.4430555555555555358, 0.4444444444444444198, 0.4458333333333333592, 0.4472222222222222432, 0.4486111111111111271, 0.4500000000000000111, 0.4513888888888888951, 0.4527777777777777790, 0.4541666666666666630, 0.4555555555555555469, 0.4569444444444444309, 0.4583333333333333148, 0.4597222222222221988, 0.4611111111111111382, 0.4625000000000000222, 0.4638888888888889062, 0.4652777777777777901, 0.4666666666666666741, 0.4680555555555555580, 0.4694444444444444420, 0.4708333333333333259, 0.4722222222222222099, 0.4736111111111110938, 0.4749999999999999778, 0.4763888888888888618, 0.4777777777777778012, 0.4791666666666666852, 0.4805555555555555691, 0.4819444444444444531, 0.4833333333333333370, 0.4847222222222222210, 0.4861111111111111049, 0.4874999999999999889, 0.4888888888888888729, 0.4902777777777777568, 0.4916666666666666408, 0.4930555555555555802, 0.4944444444444444642, 0.4958333333333333481, 0.4972222222222222321, 0.4986111111111111160, 0.5000000000000000000, 0.5013888888888888840, 0.5027777777777777679, 0.5041666666666666519, 0.5055555555555555358, 0.5069444444444444198, 0.5083333333333333037, 0.5097222222222221877, 0.5111111111111110716, 0.5124999999999999556, 0.5138888888888888395, 0.5152777777777777235, 0.5166666666666667185, 0.5180555555555556024, 0.5194444444444444864, 0.5208333333333333703, 0.5222222222222222543, 0.5236111111111111382, 0.5250000000000000222, 0.5263888888888889062, 0.5277777777777777901, 0.5291666666666666741, 0.5305555555555555580, 0.5319444444444444420, 0.5333333333333333259, 0.5347222222222222099, 0.5361111111111110938, 0.5374999999999999778, 0.5388888888888888618, 0.5402777777777777457, 0.5416666666666666297, 0.5430555555555555136, 0.5444444444444443976, 0.5458333333333332815, 0.5472222222222222765, 0.5486111111111111605, 0.5500000000000000444, 0.5513888888888889284, 0.5527777777777778123, 0.5541666666666666963, 0.5555555555555555802, 0.5569444444444444642, 0.5583333333333333481, 0.5597222222222222321, 0.5611111111111111160, 0.5625000000000000000, 0.5638888888888888840, 0.5652777777777777679, 0.5666666666666666519, 0.5680555555555555358, 0.5694444444444444198, 0.5708333333333333037, 0.5722222222222221877, 0.5736111111111110716, 0.5749999999999999556, 0.5763888888888888395, 0.5777777777777777235, 0.5791666666666667185, 0.5805555555555556024, 0.5819444444444444864, 0.5833333333333333703, 0.5847222222222222543, 0.5861111111111111382, 0.5875000000000000222, 0.5888888888888889062, 0.5902777777777777901, 0.5916666666666666741, 0.5930555555555555580, 0.5944444444444444420, 0.5958333333333333259, 0.5972222222222222099, 0.5986111111111110938, 0.5999999999999999778, 0.6013888888888888618, 0.6027777777777777457, 0.6041666666666666297, 0.6055555555555555136, 0.6069444444444443976, 0.6083333333333332815, 0.6097222222222222765, 0.6111111111111111605, 0.6125000000000000444, 0.6138888888888889284, 0.6152777777777778123, 0.6166666666666666963, 0.6180555555555555802, 0.6194444444444444642, 0.6208333333333333481, 0.6222222222222222321, 0.6236111111111111160, 0.6250000000000000000, 0.6263888888888888840, 0.6277777777777777679, 0.6291666666666666519, 0.6305555555555555358, 0.6319444444444444198, 0.6333333333333333037, 0.6347222222222221877, 0.6361111111111110716, 0.6374999999999999556, 0.6388888888888888395, 0.6402777777777777235, 0.6416666666666667185, 0.6430555555555556024, 0.6444444444444444864, 0.6458333333333333703, 0.6472222222222222543, 0.6486111111111111382, 0.6500000000000000222, 0.6513888888888889062, 0.6527777777777777901, 0.6541666666666666741, 0.6555555555555555580, 0.6569444444444444420, 0.6583333333333333259, 0.6597222222222222099, 0.6611111111111110938, 0.6624999999999999778, 0.6638888888888888618, 0.6652777777777777457, 0.6666666666666666297, 0.6680555555555555136, 0.6694444444444443976, 0.6708333333333332815, 0.6722222222222222765, 0.6736111111111111605, 0.6750000000000000444, 0.6763888888888889284, 0.6777777777777778123, 0.6791666666666666963, 0.6805555555555555802, 0.6819444444444444642, 0.6833333333333333481, 0.6847222222222222321, 0.6861111111111111160, 0.6875000000000000000, 0.6888888888888888840, 0.6902777777777777679, 0.6916666666666666519, 0.6930555555555555358, 0.6944444444444444198, 0.6958333333333333037, 0.6972222222222221877, 0.6986111111111110716, 0.6999999999999999556, 0.7013888888888888395, 0.7027777777777777235, 0.7041666666666667185, 0.7055555555555556024, 0.7069444444444444864, 0.7083333333333333703, 0.7097222222222222543, 0.7111111111111111382, 0.7125000000000000222, 0.7138888888888889062, 0.7152777777777777901, 0.7166666666666666741, 0.7180555555555555580, 0.7194444444444444420, 0.7208333333333333259, 0.7222222222222222099, 0.7236111111111110938, 0.7249999999999999778, 0.7263888888888888618, 0.7277777777777777457, 0.7291666666666666297, 0.7305555555555555136, 0.7319444444444443976, 0.7333333333333332815, 0.7347222222222222765, 0.7361111111111111605, 0.7375000000000000444, 0.7388888888888889284, 0.7402777777777778123, 0.7416666666666666963, 0.7430555555555555802, 0.7444444444444444642, 0.7458333333333333481, 0.7472222222222222321, 0.7486111111111111160, 0.7500000000000000000, 0.7513888888888888840, 0.7527777777777777679, 0.7541666666666666519, 0.7555555555555555358, 0.7569444444444444198, 0.7583333333333333037, 0.7597222222222221877, 0.7611111111111110716, 0.7624999999999999556, 0.7638888888888888395, 0.7652777777777777235, 0.7666666666666667185, 0.7680555555555556024, 0.7694444444444444864, 0.7708333333333333703, 0.7722222222222222543, 0.7736111111111111382, 0.7750000000000000222, 0.7763888888888889062, 0.7777777777777777901, 0.7791666666666666741, 0.7805555555555555580, 0.7819444444444444420, 0.7833333333333333259, 0.7847222222222222099, 0.7861111111111110938, 0.7874999999999999778, 0.7888888888888888618, 0.7902777777777777457, 0.7916666666666666297, 0.7930555555555555136, 0.7944444444444443976, 0.7958333333333332815, 0.7972222222222222765, 0.7986111111111111605, 0.8000000000000000444, 0.8013888888888889284, 0.8027777777777778123, 0.8041666666666666963, 0.8055555555555555802, 0.8069444444444444642, 0.8083333333333333481, 0.8097222222222222321, 0.8111111111111111160, 0.8125000000000000000, 0.8138888888888888840, 0.8152777777777777679, 0.8166666666666666519, 0.8180555555555555358, 0.8194444444444444198, 0.8208333333333333037, 0.8222222222222221877, 0.8236111111111110716, 0.8249999999999999556, 0.8263888888888888395, 0.8277777777777777235, 0.8291666666666667185, 0.8305555555555556024, 0.8319444444444444864, 0.8333333333333333703, 0.8347222222222222543, 0.8361111111111111382, 0.8375000000000000222, 0.8388888888888889062, 0.8402777777777777901, 0.8416666666666666741, 0.8430555555555555580, 0.8444444444444444420, 0.8458333333333333259, 0.8472222222222222099, 0.8486111111111110938, 0.8499999999999999778, 0.8513888888888888618, 0.8527777777777777457, 0.8541666666666666297, 0.8555555555555555136, 0.8569444444444443976, 0.8583333333333332815, 0.8597222222222222765, 0.8611111111111111605, 0.8625000000000000444, 0.8638888888888889284, 0.8652777777777778123, 0.8666666666666666963, 0.8680555555555555802, 0.8694444444444444642, 0.8708333333333333481, 0.8722222222222222321, 0.8736111111111111160, 0.8750000000000000000, 0.8763888888888888840, 0.8777777777777777679, 0.8791666666666666519, 0.8805555555555555358, 0.8819444444444444198, 0.8833333333333333037, 0.8847222222222221877, 0.8861111111111110716, 0.8874999999999999556, 0.8888888888888888395, 0.8902777777777777235, 0.8916666666666667185, 0.8930555555555556024, 0.8944444444444444864, 0.8958333333333333703, 0.8972222222222222543, 0.8986111111111111382, 0.9000000000000000222, 0.9013888888888889062, 0.9027777777777777901, 0.9041666666666666741, 0.9055555555555555580, 0.9069444444444444420, 0.9083333333333333259, 0.9097222222222222099, 0.9111111111111110938, 0.9124999999999999778, 0.9138888888888888618, 0.9152777777777777457, 0.9166666666666666297, 0.9180555555555555136, 0.9194444444444443976, 0.9208333333333332815, 0.9222222222222222765, 0.9236111111111111605, 0.9250000000000000444, 0.9263888888888889284, 0.9277777777777778123, 0.9291666666666666963, 0.9305555555555555802, 0.9319444444444444642, 0.9333333333333333481, 0.9347222222222222321, 0.9361111111111111160, 0.9375000000000000000, 0.9388888888888888840, 0.9402777777777777679, 0.9416666666666666519, 0.9430555555555555358, 0.9444444444444444198, 0.9458333333333333037, 0.9472222222222221877, 0.9486111111111110716, 0.9499999999999999556, 0.9513888888888888395, 0.9527777777777777235, 0.9541666666666667185, 0.9555555555555556024, 0.9569444444444444864, 0.9583333333333333703, 0.9597222222222222543, 0.9611111111111111382, 0.9625000000000000222, 0.9638888888888889062, 0.9652777777777777901, 0.9666666666666666741, 0.9680555555555555580, 0.9694444444444444420, 0.9708333333333333259, 0.9722222222222222099, 0.9736111111111110938, 0.9749999999999999778, 0.9763888888888888618, 0.9777777777777777457, 0.9791666666666666297, 0.9805555555555555136, 0.9819444444444443976, 0.9833333333333332815, 0.9847222222222222765, 0.9861111111111111605, 0.9875000000000000444, 0.9888888888888889284, 0.9902777777777778123, 0.9916666666666666963, 0.9930555555555555802, 0.9944444444444444642, 0.9958333333333333481, 0.9972222222222222321, 0.9986111111111111160, 1.000000000000000000 ),
 .UNSPECIFIED. ) 
 CURVE ( )  GEOMETRIC_REPRESENTATION_ITEM ( )  RATIONAL_B_SPLINE_CURVE ( ( 1.000000000000000000, 0.8660254037844387076, 1.000000000000000000, 0.8660254037844387076, 1.000000000000000000, 0.8660254037844387076, 1.000000000000000000, 0.8660254037844387076, 1.000000000000000000, 0.8660254037844387076, 1.000000000000000000, 0.8660254037844387076, 1.000000000000000000, 0.8660254037844387076, 1.000000000000000000, 0.8660254037844387076, 1.000000000000000000, 0.8660254037844387076, 1.000000000000000000, 0.8660254037844387076, 1.000000000000000000, 0.8660254037844387076, 1.000000000000000000, 0.8660254037844387076, 1.000000000000000000, 0.8660254037844387076, 1.000000000000000000, 0.8660254037844387076, 1.000000000000000000, 0.8660254037844387076, 1.000000000000000000, 0.8660254037844387076, 1.000000000000000000, 0.8660254037844387076, 1.000000000000000000, 0.8660254037844387076, 1.000000000000000000, 0.8660254037844387076, 1.000000000000000000, 0.8660254037844387076, 1.000000000000000000, 0.8660254037844387076, 1.000000000000000000, 0.8660254037844387076, 1.000000000000000000, 0.8660254037844387076, 1.000000000000000000, 0.8660254037844387076, 1.000000000000000000, 0.8660254037844387076, 1.000000000000000000, 0.8660254037844387076, 1.000000000000000000, 0.8660254037844387076, 1.000000000000000000, 0.8660254037844387076, 1.000000000000000000, 0.8660254037844387076, 1.000000000000000000, 0.8660254037844387076, 1.000000000000000000, 0.8660254037844387076, 1.000000000000000000, 0.8660254037844387076, 1.000000000000000000, 0.8660254037844387076, 1.000000000000000000, 0.8660254037844387076, 1.000000000000000000, 0.8660254037844387076, 1.000000000000000000, 0.8660254037844387076, 1.000000000000000000, 0.8660254037844387076, 1.000000000000000000, 0.8660254037844387076, 1.000000000000000000, 0.8660254037844387076, 1.000000000000000000, 0.8660254037844387076, 1.000000000000000000, 0.8660254037844387076, 1.000000000000000000, 0.8660254037844387076, 1.000000000000000000, 0.8660254037844387076, 1.000000000000000000, 0.8660254037844387076, 1.000000000000000000, 0.8660254037844387076, 1.000000000000000000, 0.8660254037844387076, 1.000000000000000000, 0.8660254037844387076, 1.000000000000000000, 0.8660254037844387076, 1.000000000000000000, 0.8660254037844387076, 1.000000000000000000, 0.8660254037844387076, 1.000000000000000000, 0.8660254037844387076, 1.000000000000000000, 0.8660254037844387076, 1.000000000000000000, 0.8660254037844387076, 1.000000000000000000, 0.8660254037844387076, 1.000000000000000000, 0.8660254037844387076, 1.000000000000000000, 0.8660254037844387076, 1.000000000000000000, 0.8660254037844387076, 1.000000000000000000, 0.8660254037844387076, 1.000000000000000000, 0.8660254037844387076, 1.000000000000000000, 0.8660254037844387076, 1.000000000000000000, 0.8660254037844387076, 1.000000000000000000, 0.8660254037844387076, 1.000000000000000000, 0.8660254037844387076, 1.000000000000000000, 0.8660254037844387076, 1.000000000000000000, 0.8660254037844387076, 1.000000000000000000, 0.8660254037844387076, 1.000000000000000000, 0.8660254037844387076, 1.000000000000000000, 0.8660254037844387076, 1.000000000000000000, 0.8660254037844387076, 1.000000000000000000, 0.8660254037844387076, 1.000000000000000000, 0.8660254037844387076, 1.000000000000000000, 0.8660254037844387076, 1.000000000000000000, 0.8660254037844387076, 1.000000000000000000, 0.8660254037844387076, 1.000000000000000000, 0.8660254037844387076, 1.000000000000000000, 0.8660254037844387076, 1.000000000000000000, 0.8660254037844387076, 1.000000000000000000, 0.8660254037844387076, 1.000000000000000000, 0.8660254037844387076, 1.000000000000000000, 0.8660254037844387076, 1.000000000000000000, 0.8660254037844387076, 1.000000000000000000, 0.8660254037844387076, 1.000000000000000000, 0.8660254037844387076, 1.000000000000000000, 0.8660254037844387076, 1.000000000000000000, 0.8660254037844387076, 1.000000000000000000, 0.8660254037844387076, 1.000000000000000000, 0.8660254037844387076, 1.000000000000000000, 0.8660254037844387076, 1.000000000000000000, 0.8660254037844387076, 1.000000000000000000, 0.8660254037844387076, 1.000000000000000000, 0.8660254037844387076, 1.000000000000000000, 0.8660254037844387076, 1.000000000000000000, 0.8660254037844387076, 1.000000000000000000, 0.8660254037844387076, 1.000000000000000000, 0.8660254037844387076, 1.000000000000000000, 0.8660254037844387076, 1.000000000000000000, 0.8660254037844387076, 1.000000000000000000, 0.8660254037844387076, 1.000000000000000000, 0.8660254037844387076, 1.000000000000000000, 0.8660254037844387076, 1.000000000000000000, 0.8660254037844387076, 1.000000000000000000, 0.8660254037844387076, 1.000000000000000000, 0.8660254037844387076, 1.000000000000000000, 0.8660254037844387076, 1.000000000000000000, 0.8660254037844387076, 1.000000000000000000, 0.8660254037844387076, 1.000000000000000000, 0.8660254037844387076, 1.000000000000000000, 0.8660254037844387076, 1.000000000000000000, 0.8660254037844387076, 1.000000000000000000, 0.8660254037844387076, 1.000000000000000000, 0.8660254037844387076, 1.000000000000000000, 0.8660254037844387076, 1.000000000000000000, 0.8660254037844387076, 1.000000000000000000, 0.8660254037844387076, 1.000000000000000000, 0.8660254037844387076, 1.000000000000000000, 0.8660254037844387076, 1.000000000000000000, 0.8660254037844387076, 1.000000000000000000, 0.8660254037844387076, 1.000000000000000000, 0.8660254037844387076, 1.000000000000000000, 0.8660254037844387076, 1.000000000000000000, 0.8660254037844387076, 1.000000000000000000, 0.8660254037844387076, 1.000000000000000000, 0.8660254037844387076, 1.000000000000000000, 0.8660254037844387076, 1.000000000000000000, 0.8660254037844387076, 1.000000000000000000, 0.8660254037844387076, 1.000000000000000000, 0.8660254037844387076, 1.000000000000000000, 0.8660254037844387076, 1.000000000000000000, 0.8660254037844387076, 1.000000000000000000, 0.8660254037844387076, 1.000000000000000000, 0.8660254037844387076, 1.000000000000000000, 0.8660254037844387076, 1.000000000000000000, 0.8660254037844387076, 1.000000000000000000, 0.8660254037844387076, 1.000000000000000000, 0.8660254037844387076, 1.000000000000000000, 0.8660254037844387076, 1.000000000000000000, 0.8660254037844387076, 1.000000000000000000, 0.8660254037844387076, 1.000000000000000000, 0.8660254037844387076, 1.000000000000000000, 0.8660254037844387076, 1.000000000000000000, 0.8660254037844387076, 1.000000000000000000, 0.8660254037844387076, 1.000000000000000000, 0.8660254037844387076, 1.000000000000000000, 0.8660254037844387076, 1.000000000000000000, 0.8660254037844387076, 1.000000000000000000, 0.8660254037844387076, 1.000000000000000000, 0.8660254037844387076, 1.000000000000000000, 0.8660254037844387076, 1.000000000000000000, 0.8660254037844387076, 1.000000000000000000, 0.8660254037844387076, 1.000000000000000000, 0.8660254037844387076, 1.000000000000000000, 0.8660254037844387076, 1.000000000000000000, 0.8660254037844387076, 1.000000000000000000, 0.8660254037844387076, 1.000000000000000000, 0.8660254037844387076, 1.000000000000000000, 0.8660254037844387076, 1.000000000000000000, 0.8660254037844387076, 1.000000000000000000, 0.8660254037844387076, 1.000000000000000000, 0.8660254037844387076, 1.000000000000000000, 0.8660254037844387076, 1.000000000000000000, 0.8660254037844387076, 1.000000000000000000, 0.8660254037844387076, 1.000000000000000000, 0.8660254037844387076, 1.000000000000000000, 0.8660254037844387076, 1.000000000000000000, 0.8660254037844387076, 1.000000000000000000, 0.8660254037844387076, 1.000000000000000000, 0.8660254037844387076, 1.000000000000000000, 0.8660254037844387076, 1.000000000000000000, 0.8660254037844387076, 1.000000000000000000, 0.8660254037844387076, 1.000000000000000000, 0.8660254037844387076, 1.000000000000000000, 0.8660254037844387076, 1.000000000000000000, 0.8660254037844387076, 1.000000000000000000, 0.8660254037844387076, 1.000000000000000000, 0.8660254037844387076, 1.000000000000000000, 0.8660254037844387076, 1.000000000000000000, 0.8660254037844387076, 1.000000000000000000, 0.8660254037844387076, 1.000000000000000000, 0.8660254037844387076, 1.000000000000000000, 0.8660254037844387076, 1.000000000000000000, 0.8660254037844387076, 1.000000000000000000, 0.8660254037844387076, 1.000000000000000000, 0.8660254037844387076, 1.000000000000000000, 0.8660254037844387076, 1.000000000000000000, 0.8660254037844387076, 1.000000000000000000, 0.8660254037844387076, 1.000000000000000000, 0.8660254037844387076, 1.000000000000000000, 0.8660254037844387076, 1.000000000000000000, 0.8660254037844387076, 1.000000000000000000, 0.8660254037844387076, 1.000000000000000000, 0.8660254037844387076, 1.000000000000000000, 0.8660254037844387076, 1.000000000000000000, 0.8660254037844387076, 1.000000000000000000, 0.8660254037844387076, 1.000000000000000000, 0.8660254037844387076, 1.000000000000000000, 0.8660254037844387076, 1.000000000000000000, 0.8660254037844387076, 1.000000000000000000, 0.8660254037844387076, 1.000000000000000000, 0.8660254037844387076, 1.000000000000000000, 0.8660254037844387076, 1.000000000000000000, 0.8660254037844387076, 1.000000000000000000, 0.8660254037844387076, 1.000000000000000000, 0.8660254037844387076, 1.000000000000000000, 0.8660254037844387076, 1.000000000000000000, 0.8660254037844387076, 1.000000000000000000, 0.8660254037844387076, 1.000000000000000000, 0.8660254037844387076, 1.000000000000000000, 0.8660254037844387076, 1.000000000000000000, 0.8660254037844387076, 1.000000000000000000, 0.8660254037844387076, 1.000000000000000000, 0.8660254037844387076, 1.000000000000000000, 0.8660254037844387076, 1.000000000000000000, 0.8660254037844387076, 1.000000000000000000, 0.8660254037844387076, 1.000000000000000000, 0.8660254037844387076, 1.000000000000000000, 0.8660254037844387076, 1.000000000000000000, 0.8660254037844387076, 1.000000000000000000, 0.8660254037844387076, 1.000000000000000000, 0.8660254037844387076, 1.000000000000000000, 0.8660254037844387076, 1.000000000000000000, 0.8660254037844387076, 1.000000000000000000, 0.8660254037844387076, 1.000000000000000000, 0.8660254037844387076, 1.000000000000000000, 0.8660254037844387076, 1.000000000000000000, 0.8660254037844387076, 1.000000000000000000, 0.8660254037844387076, 1.000000000000000000, 0.8660254037844387076, 1.000000000000000000, 0.8660254037844387076, 1.000000000000000000, 0.8660254037844387076, 1.000000000000000000, 0.8660254037844387076, 1.000000000000000000, 0.8660254037844387076, 1.000000000000000000, 0.8660254037844387076, 1.000000000000000000, 0.8660254037844387076, 1.000000000000000000, 0.8660254037844387076, 1.000000000000000000, 0.8660254037844387076, 1.000000000000000000, 0.8660254037844387076, 1.000000000000000000, 0.8660254037844387076, 1.000000000000000000, 0.8660254037844387076, 1.000000000000000000, 0.8660254037844387076, 1.000000000000000000, 0.8660254037844387076, 1.000000000000000000, 0.8660254037844387076, 1.000000000000000000, 0.8660254037844387076, 1.000000000000000000, 0.8660254037844387076, 1.000000000000000000, 0.8660254037844387076, 1.000000000000000000, 0.8660254037844387076, 1.000000000000000000, 0.8660254037844387076, 1.000000000000000000, 0.8660254037844387076, 1.000000000000000000, 0.8660254037844387076, 1.000000000000000000, 0.8660254037844387076, 1.000000000000000000, 0.8660254037844387076, 1.000000000000000000, 0.8660254037844387076, 1.000000000000000000, 0.8660254037844387076, 1.000000000000000000, 0.8660254037844387076, 1.000000000000000000, 0.8660254037844387076, 1.000000000000000000, 0.8660254037844387076, 1.000000000000000000, 0.8660254037844387076, 1.000000000000000000, 0.8660254037844387076, 1.000000000000000000, 0.8660254037844387076, 1.000000000000000000, 0.8660254037844387076, 1.000000000000000000, 0.8660254037844387076, 1.000000000000000000, 0.8660254037844387076, 1.000000000000000000, 0.8660254037844387076, 1.000000000000000000, 0.8660254037844387076, 1.000000000000000000, 0.8660254037844387076, 1.000000000000000000, 0.8660254037844387076, 1.000000000000000000, 0.8660254037844387076, 1.000000000000000000, 0.8660254037844387076, 1.000000000000000000, 0.8660254037844387076, 1.000000000000000000, 0.8660254037844387076, 1.000000000000000000, 0.8660254037844387076, 1.000000000000000000, 0.8660254037844387076, 1.000000000000000000, 0.8660254037844387076, 1.000000000000000000, 0.8660254037844387076, 1.000000000000000000, 0.8660254037844387076, 1.000000000000000000, 0.8660254037844387076, 1.000000000000000000, 0.8660254037844387076, 1.000000000000000000, 0.8660254037844387076, 1.000000000000000000, 0.8660254037844387076, 1.000000000000000000, 0.8660254037844387076, 1.000000000000000000, 0.8660254037844387076, 1.000000000000000000, 0.8660254037844387076, 1.000000000000000000, 0.8660254037844387076, 1.000000000000000000, 0.8660254037844387076, 1.000000000000000000, 0.8660254037844387076, 1.000000000000000000, 0.8660254037844387076, 1.000000000000000000, 0.8660254037844387076, 1.000000000000000000, 0.8660254037844387076, 1.000000000000000000, 0.8660254037844387076, 1.000000000000000000, 0.8660254037844387076, 1.000000000000000000, 0.8660254037844387076, 1.000000000000000000, 0.8660254037844387076, 1.000000000000000000, 0.8660254037844387076, 1.000000000000000000, 0.8660254037844387076, 1.000000000000000000, 0.8660254037844387076, 1.000000000000000000, 0.8660254037844387076, 1.000000000000000000, 0.8660254037844387076, 1.000000000000000000, 0.8660254037844387076, 1.000000000000000000, 0.8660254037844387076, 1.000000000000000000, 0.8660254037844387076, 1.000000000000000000, 0.8660254037844387076, 1.000000000000000000, 0.8660254037844387076, 1.000000000000000000, 0.8660254037844387076, 1.000000000000000000, 0.8660254037844387076, 1.000000000000000000, 0.8660254037844387076, 1.000000000000000000, 0.8660254037844387076, 1.000000000000000000, 0.8660254037844387076, 1.000000000000000000, 0.8660254037844387076, 1.000000000000000000, 0.8660254037844387076, 1.000000000000000000, 0.8660254037844387076, 1.000000000000000000, 0.8660254037844387076, 1.000000000000000000, 0.8660254037844387076, 1.000000000000000000, 0.8660254037844387076, 1.000000000000000000, 0.8660254037844387076, 1.000000000000000000, 0.8660254037844387076, 1.000000000000000000, 0.8660254037844387076, 1.000000000000000000, 0.8660254037844387076, 1.000000000000000000, 0.8660254037844387076, 1.000000000000000000, 0.8660254037844387076, 1.000000000000000000, 0.8660254037844387076, 1.000000000000000000, 0.8660254037844387076, 1.000000000000000000, 0.8660254037844387076, 1.000000000000000000, 0.8660254037844387076, 1.000000000000000000, 0.8660254037844387076, 1.000000000000000000, 0.8660254037844387076, 1.000000000000000000, 0.8660254037844387076, 1.000000000000000000, 0.8660254037844387076, 1.000000000000000000, 0.8660254037844387076, 1.000000000000000000, 0.8660254037844387076, 1.000000000000000000, 0.8660254037844387076, 1.000000000000000000, 0.8660254037844387076, 1.000000000000000000, 0.8660254037844387076, 1.000000000000000000, 0.8660254037844387076, 1.000000000000000000, 0.8660254037844387076, 1.000000000000000000, 0.8660254037844387076, 1.000000000000000000, 0.8660254037844387076, 1.000000000000000000, 0.8660254037844387076, 1.000000000000000000, 0.8660254037844387076, 1.000000000000000000, 0.8660254037844387076, 1.000000000000000000, 0.8660254037844387076, 1.000000000000000000, 0.8660254037844387076, 1.000000000000000000, 0.8660254037844387076, 1.000000000000000000, 0.8660254037844387076, 1.000000000000000000, 0.8660254037844387076, 1.000000000000000000, 0.8660254037844387076, 1.000000000000000000, 0.8660254037844387076, 1.000000000000000000, 0.8660254037844387076, 1.000000000000000000, 0.8660254037844387076, 1.000000000000000000, 0.8660254037844387076, 1.000000000000000000, 0.8660254037844387076, 1.000000000000000000, 0.8660254037844387076, 1.000000000000000000, 0.8660254037844387076, 1.000000000000000000, 0.8660254037844387076, 1.000000000000000000, 0.8660254037844387076, 1.000000000000000000, 0.8660254037844387076, 1.000000000000000000, 0.8660254037844387076, 1.000000000000000000, 0.8660254037844387076, 1.000000000000000000, 0.8660254037844387076, 1.000000000000000000, 0.8660254037844387076, 1.000000000000000000, 0.8660254037844387076, 1.000000000000000000, 0.8660254037844387076, 1.000000000000000000, 0.8660254037844387076, 1.000000000000000000, 0.8660254037844387076, 1.000000000000000000, 0.8660254037844387076, 1.000000000000000000, 0.8660254037844387076, 1.000000000000000000, 0.8660254037844387076, 1.000000000000000000, 0.8660254037844387076, 1.000000000000000000, 0.8660254037844387076, 1.000000000000000000, 0.8660254037844387076, 1.000000000000000000, 0.8660254037844387076, 1.000000000000000000, 0.8660254037844387076, 1.000000000000000000, 0.8660254037844387076, 1.000000000000000000, 0.8660254037844387076, 1.000000000000000000, 0.8660254037844387076, 1.000000000000000000, 0.8660254037844387076, 1.000000000000000000, 0.8660254037844387076, 1.000000000000000000, 0.8660254037844387076, 1.000000000000000000, 0.8660254037844387076, 1.000000000000000000, 0.8660254037844387076, 1.000000000000000000, 0.8660254037844387076, 1.000000000000000000, 0.8660254037844387076, 1.000000000000000000, 0.8660254037844387076, 1.000000000000000000, 0.8660254037844387076, 1.000000000000000000, 0.8660254037844387076, 1.000000000000000000, 0.8660254037844387076, 1.000000000000000000, 0.8660254037844387076, 1.000000000000000000, 0.8660254037844387076, 1.000000000000000000, 0.8660254037844387076, 1.000000000000000000, 0.8660254037844387076, 1.000000000000000000, 0.8660254037844387076, 1.000000000000000000, 0.8660254037844387076, 1.000000000000000000, 0.8660254037844387076, 1.000000000000000000, 0.8660254037844387076, 1.000000000000000000, 0.8660254037844387076, 1.000000000000000000, 0.8660254037844387076, 1.000000000000000000, 0.8660254037844387076, 1.000000000000000000, 0.8660254037844387076, 1.000000000000000000, 0.8660254037844387076, 1.000000000000000000, 0.8660254037844387076, 1.000000000000000000, 0.8660254037844387076, 1.000000000000000000, 0.8660254037844387076, 1.000000000000000000, 0.8660254037844387076, 1.000000000000000000, 0.8660254037844387076, 1.000000000000000000, 0.8660254037844387076, 1.000000000000000000, 0.8660254037844387076, 1.000000000000000000, 0.8660254037844387076, 1.000000000000000000, 0.8660254037844387076, 1.000000000000000000, 0.8660254037844387076, 1.000000000000000000, 0.8660254037844387076, 1.000000000000000000, 0.8660254037844387076, 1.000000000000000000, 0.8660254037844387076, 1.000000000000000000, 0.8660254037844387076, 1.000000000000000000, 0.8660254037844387076, 1.000000000000000000, 0.8660254037844387076, 1.000000000000000000, 0.8660254037844387076, 1.000000000000000000, 0.8660254037844387076, 1.000000000000000000, 0.8660254037844387076, 1.000000000000000000, 0.8660254037844387076, 1.000000000000000000, 0.8660254037844387076, 1.000000000000000000, 0.8660254037844387076, 1.000000000000000000, 0.8660254037844387076, 1.000000000000000000, 0.8660254037844387076, 1.000000000000000000, 0.8660254037844387076, 1.000000000000000000, 0.8660254037844387076, 1.000000000000000000, 0.8660254037844387076, 1.000000000000000000, 0.8660254037844387076, 1.000000000000000000, 0.8660254037844387076, 1.000000000000000000, 0.8660254037844387076, 1.000000000000000000, 0.8660254037844387076, 1.000000000000000000, 0.8660254037844387076, 1.000000000000000000, 0.8660254037844387076, 1.000000000000000000, 0.8660254037844387076, 1.000000000000000000, 0.8660254037844387076, 1.000000000000000000, 0.8660254037844387076, 1.000000000000000000, 0.8660254037844387076, 1.000000000000000000, 0.8660254037844387076, 1.000000000000000000, 0.8660254037844387076, 1.000000000000000000, 0.8660254037844387076, 1.000000000000000000, 0.8660254037844387076, 1.000000000000000000, 0.8660254037844387076, 1.000000000000000000, 0.8660254037844387076, 1.000000000000000000, 0.8660254037844387076, 1.000000000000000000, 0.8660254037844387076, 1.000000000000000000, 0.8660254037844387076, 1.000000000000000000, 0.8660254037844387076, 1.000000000000000000, 0.8660254037844387076, 1.000000000000000000, 0.8660254037844387076, 1.000000000000000000, 0.8660254037844387076, 1.000000000000000000, 0.8660254037844387076, 1.000000000000000000, 0.8660254037844387076, 1.000000000000000000, 0.8660254037844387076, 1.000000000000000000, 0.8660254037844387076, 1.000000000000000000, 0.8660254037844387076, 1.000000000000000000, 0.8660254037844387076, 1.000000000000000000, 0.8660254037844387076, 1.000000000000000000, 0.8660254037844387076, 1.000000000000000000, 0.8660254037844387076, 1.000000000000000000, 0.8660254037844387076, 1.000000000000000000, 0.8660254037844387076, 1.000000000000000000, 0.8660254037844387076, 1.000000000000000000, 0.8660254037844387076, 1.000000000000000000, 0.8660254037844387076, 1.000000000000000000, 0.8660254037844387076, 1.000000000000000000, 0.8660254037844387076, 1.000000000000000000, 0.8660254037844387076, 1.000000000000000000, 0.8660254037844387076, 1.000000000000000000, 0.8660254037844387076, 1.000000000000000000, 0.8660254037844387076, 1.000000000000000000, 0.8660254037844387076, 1.000000000000000000, 0.8660254037844387076, 1.000000000000000000, 0.8660254037844387076, 1.000000000000000000, 0.8660254037844387076, 1.000000000000000000, 0.8660254037844387076, 1.000000000000000000, 0.8660254037844387076, 1.000000000000000000, 0.8660254037844387076, 1.000000000000000000, 0.8660254037844387076, 1.000000000000000000, 0.8660254037844387076, 1.000000000000000000, 0.8660254037844387076, 1.000000000000000000, 0.8660254037844387076, 1.000000000000000000, 0.8660254037844387076, 1.000000000000000000, 0.8660254037844387076, 1.000000000000000000, 0.8660254037844387076, 1.000000000000000000, 0.8660254037844387076, 1.000000000000000000, 0.8660254037844387076, 1.000000000000000000, 0.8660254037844387076, 1.000000000000000000, 0.8660254037844387076, 1.000000000000000000, 0.8660254037844387076, 1.000000000000000000, 0.8660254037844387076, 1.000000000000000000, 0.8660254037844387076, 1.000000000000000000, 0.8660254037844387076, 1.000000000000000000, 0.8660254037844387076, 1.000000000000000000, 0.8660254037844387076, 1.000000000000000000, 0.8660254037844387076, 1.000000000000000000, 0.8660254037844387076, 1.000000000000000000, 0.8660254037844387076, 1.000000000000000000, 0.8660254037844387076, 1.000000000000000000, 0.8660254037844387076, 1.000000000000000000, 0.8660254037844387076, 1.000000000000000000, 0.8660254037844387076, 1.000000000000000000, 0.8660254037844387076, 1.000000000000000000, 0.8660254037844387076, 1.000000000000000000, 0.8660254037844387076, 1.000000000000000000, 0.8660254037844387076, 1.000000000000000000, 0.8660254037844387076, 1.000000000000000000, 0.8660254037844387076, 1.000000000000000000, 0.8660254037844387076, 1.000000000000000000, 0.8660254037844387076, 1.000000000000000000, 0.8660254037844387076, 1.000000000000000000, 0.8660254037844387076, 1.000000000000000000, 0.8660254037844387076, 1.000000000000000000, 0.8660254037844387076, 1.000000000000000000, 0.8660254037844387076, 1.000000000000000000, 0.8660254037844387076, 1.000000000000000000, 0.8660254037844387076, 1.000000000000000000, 0.8660254037844387076, 1.000000000000000000, 0.8660254037844387076, 1.000000000000000000, 0.8660254037844387076, 1.000000000000000000, 0.8660254037844387076, 1.000000000000000000, 0.8660254037844387076, 1.000000000000000000, 0.8660254037844387076, 1.000000000000000000, 0.8660254037844387076, 1.000000000000000000, 0.8660254037844387076, 1.000000000000000000, 0.8660254037844387076, 1.000000000000000000, 0.8660254037844387076, 1.000000000000000000, 0.8660254037844387076, 1.000000000000000000, 0.8660254037844387076, 1.000000000000000000, 0.8660254037844387076, 1.000000000000000000, 0.8660254037844387076, 1.000000000000000000, 0.8660254037844387076, 1.000000000000000000, 0.8660254037844387076, 1.000000000000000000, 0.8660254037844387076, 1.000000000000000000, 0.8660254037844387076, 1.000000000000000000, 0.8660254037844387076, 1.000000000000000000, 0.8660254037844387076, 1.000000000000000000, 0.8660254037844387076, 1.000000000000000000, 0.8660254037844387076, 1.000000000000000000, 0.8660254037844387076, 1.000000000000000000, 0.8660254037844387076, 1.000000000000000000, 0.8660254037844387076, 1.000000000000000000, 0.8660254037844387076, 1.000000000000000000, 0.8660254037844387076, 1.000000000000000000, 0.8660254037844387076, 1.000000000000000000, 0.8660254037844387076, 1.000000000000000000, 0.8660254037844387076, 1.000000000000000000, 0.8660254037844387076, 1.000000000000000000, 0.8660254037844387076, 1.000000000000000000, 0.8660254037844387076, 1.000000000000000000, 0.8660254037844387076, 1.000000000000000000, 0.8660254037844387076, 1.000000000000000000, 0.8660254037844387076, 1.000000000000000000, 0.8660254037844387076, 1.000000000000000000, 0.8660254037844387076, 1.000000000000000000, 0.8660254037844387076, 1.000000000000000000, 0.8660254037844387076, 1.000000000000000000, 0.8660254037844387076, 1.000000000000000000, 0.8660254037844387076, 1.000000000000000000, 0.8660254037844387076, 1.000000000000000000, 0.8660254037844387076, 1.000000000000000000, 0.8660254037844387076, 1.000000000000000000, 0.8660254037844387076, 1.000000000000000000, 0.8660254037844387076, 1.000000000000000000, 0.8660254037844387076, 1.000000000000000000, 0.8660254037844387076, 1.000000000000000000, 0.8660254037844387076, 1.000000000000000000, 0.8660254037844387076, 1.000000000000000000, 0.8660254037844387076, 1.000000000000000000, 0.8660254037844387076, 1.000000000000000000, 0.8660254037844387076, 1.000000000000000000, 0.8660254037844387076, 1.000000000000000000, 0.8660254037844387076, 1.000000000000000000, 0.8660254037844387076, 1.000000000000000000, 0.8660254037844387076, 1.000000000000000000, 0.8660254037844387076, 1.000000000000000000, 0.8660254037844387076, 1.000000000000000000, 0.8660254037844387076, 1.000000000000000000, 0.8660254037844387076, 1.000000000000000000, 0.8660254037844387076, 1.000000000000000000, 0.8660254037844387076, 1.000000000000000000, 0.8660254037844387076, 1.000000000000000000, 0.8660254037844387076, 1.000000000000000000, 0.8660254037844387076, 1.000000000000000000, 0.8660254037844387076, 1.000000000000000000, 0.8660254037844387076, 1.000000000000000000, 0.8660254037844387076, 1.000000000000000000, 0.8660254037844387076, 1.000000000000000000, 0.8660254037844387076, 1.000000000000000000, 0.8660254037844387076, 1.000000000000000000, 0.8660254037844387076, 1.000000000000000000, 0.8660254037844387076, 1.000000000000000000, 0.8660254037844387076, 1.000000000000000000, 0.8660254037844387076, 1.000000000000000000, 0.8660254037844387076, 1.000000000000000000, 0.8660254037844387076, 1.000000000000000000, 0.8660254037844387076, 1.000000000000000000, 0.8660254037844387076, 1.000000000000000000, 0.8660254037844387076, 1.000000000000000000, 0.8660254037844387076, 1.000000000000000000, 0.8660254037844387076, 1.000000000000000000, 0.8660254037844387076, 1.000000000000000000, 0.8660254037844387076, 1.000000000000000000, 0.8660254037844387076, 1.000000000000000000, 0.8660254037844387076, 1.000000000000000000, 0.8660254037844387076, 1.000000000000000000, 0.8660254037844387076, 1.000000000000000000, 0.8660254037844387076, 1.000000000000000000, 0.8660254037844387076, 1.000000000000000000, 0.8660254037844387076, 1.000000000000000000, 0.8660254037844387076, 1.000000000000000000, 0.8660254037844387076, 1.000000000000000000, 0.8660254037844387076, 1.000000000000000000, 0.8660254037844387076, 1.000000000000000000, 0.8660254037844387076, 1.000000000000000000, 0.8660254037844387076, 1.000000000000000000, 0.8660254037844387076, 1.000000000000000000, 0.8660254037844387076, 1.000000000000000000, 0.8660254037844387076, 1.000000000000000000, 0.8660254037844387076, 1.000000000000000000, 0.8660254037844387076, 1.000000000000000000, 0.8660254037844387076, 1.000000000000000000, 0.8660254037844387076, 1.000000000000000000, 0.8660254037844387076, 1.000000000000000000, 0.8660254037844387076, 1.000000000000000000, 0.8660254037844387076, 1.000000000000000000, 0.8660254037844387076, 1.000000000000000000, 0.8660254037844387076, 1.000000000000000000, 0.8660254037844387076, 1.000000000000000000, 0.8660254037844387076, 1.000000000000000000, 0.8660254037844387076, 1.000000000000000000, 0.8660254037844387076, 1.000000000000000000, 0.8660254037844387076, 1.000000000000000000, 0.8660254037844387076, 1.000000000000000000, 0.8660254037844387076, 1.000000000000000000, 0.8660254037844387076, 1.000000000000000000, 0.8660254037844387076, 1.000000000000000000, 0.8660254037844387076, 1.000000000000000000, 0.8660254037844387076, 1.000000000000000000, 0.8660254037844387076, 1.000000000000000000, 0.8660254037844387076, 1.000000000000000000, 0.8660254037844387076, 1.000000000000000000, 0.8660254037844387076, 1.000000000000000000, 0.8660254037844387076, 1.000000000000000000, 0.8660254037844387076, 1.000000000000000000, 0.8660254037844387076, 1.000000000000000000, 0.8660254037844387076, 1.000000000000000000, 0.8660254037844387076, 1.000000000000000000, 0.8660254037844387076, 1.000000000000000000, 0.8660254037844387076, 1.000000000000000000, 0.8660254037844387076, 1.000000000000000000, 0.8660254037844387076, 1.000000000000000000, 0.8660254037844387076, 1.000000000000000000, 0.8660254037844387076, 1.000000000000000000, 0.8660254037844387076, 1.000000000000000000, 0.8660254037844387076, 1.000000000000000000, 0.8660254037844387076, 1.000000000000000000, 0.8660254037844387076, 1.000000000000000000, 0.8660254037844387076, 1.000000000000000000, 0.8660254037844387076, 1.000000000000000000, 0.8660254037844387076, 1.000000000000000000, 0.8660254037844387076, 1.000000000000000000, 0.8660254037844387076, 1.000000000000000000, 0.8660254037844387076, 1.000000000000000000, 0.8660254037844387076, 1.000000000000000000, 0.8660254037844387076, 1.000000000000000000, 0.8660254037844387076, 1.000000000000000000, 0.8660254037844387076, 1.000000000000000000, 0.8660254037844387076, 1.000000000000000000, 0.8660254037844387076, 1.000000000000000000, 0.8660254037844387076, 1.000000000000000000, 0.8660254037844387076, 1.000000000000000000, 0.8660254037844387076, 1.000000000000000000, 0.8660254037844387076, 1.000000000000000000, 0.8660254037844387076, 1.000000000000000000, 0.8660254037844387076, 1.000000000000000000, 0.8660254037844387076, 1.000000000000000000, 0.8660254037844387076, 1.000000000000000000, 0.8660254037844387076, 1.000000000000000000, 0.8660254037844387076, 1.000000000000000000, 0.8660254037844387076, 1.000000000000000000, 0.8660254037844387076, 1.000000000000000000, 0.8660254037844387076, 1.000000000000000000, 0.8660254037844387076, 1.000000000000000000, 0.8660254037844387076, 1.000000000000000000, 0.8660254037844387076, 1.000000000000000000, 0.8660254037844387076, 1.000000000000000000, 0.8660254037844387076, 1.000000000000000000, 0.8660254037844387076, 1.000000000000000000, 0.8660254037844387076, 1.000000000000000000, 0.8660254037844387076, 1.000000000000000000, 0.8660254037844387076, 1.000000000000000000, 0.8660254037844387076, 1.000000000000000000, 0.8660254037844387076, 1.000000000000000000, 0.8660254037844387076, 1.000000000000000000, 0.8660254037844387076, 1.000000000000000000, 0.8660254037844387076, 1.000000000000000000, 0.8660254037844387076, 1.000000000000000000, 0.8660254037844387076, 1.000000000000000000, 0.8660254037844387076, 1.000000000000000000, 0.8660254037844387076, 1.000000000000000000, 0.8660254037844387076, 1.000000000000000000, 0.8660254037844387076, 1.000000000000000000, 0.8660254037844387076, 1.000000000000000000, 0.8660254037844387076, 1.000000000000000000, 0.8660254037844387076, 1.000000000000000000, 0.8660254037844387076, 1.000000000000000000, 0.8660254037844387076, 1.000000000000000000, 0.8660254037844387076, 1.000000000000000000, 0.8660254037844387076, 1.000000000000000000, 0.8660254037844387076, 1.000000000000000000, 0.8660254037844387076, 1.000000000000000000, 0.8660254037844387076, 1.000000000000000000, 0.8660254037844387076, 1.000000000000000000, 0.8660254037844387076, 1.000000000000000000, 0.8660254037844387076, 1.000000000000000000, 0.8660254037844387076, 1.000000000000000000, 0.8660254037844387076, 1.000000000000000000, 0.8660254037844387076, 1.000000000000000000, 0.8660254037844387076, 1.000000000000000000, 0.8660254037844387076, 1.000000000000000000, 0.8660254037844387076, 1.000000000000000000, 0.8660254037844387076, 1.000000000000000000, 0.8660254037844387076, 1.000000000000000000 ) ) 
 REPRESENTATION_ITEM ( '' )  );
#41574 = CARTESIAN_POINT ( 'NONE',  ( -6.972266317189433020E-16, -17.12499999726881583, -5.000000000000000000 ) ) ;
#41575 = CARTESIAN_POINT ( 'NONE',  ( -2.500000000000000444, 7.833333333333334814, -4.330127018922193649 ) ) ;
#41576 = CARTESIAN_POINT ( 'NONE',  ( 4.458734124999998549, -56.72916666530107932, -2.574251347313721627 ) ) ;
#41577 = CARTESIAN_POINT ( 'NONE',  ( 7.894958282449824338, -1.603399432398892266, -7.593838100136980351 ) ) ;
#41578 = CARTESIAN_POINT ( 'NONE',  ( -2.500000000000000444, -52.16666666666666430, -4.330127018922193649 ) ) ;
#41579 = CARTESIAN_POINT ( 'NONE',  ( -5.000000000000000000, -37.95833333060213022, -2.886751345948128211 ) ) ;
#41580 = CARTESIAN_POINT ( 'NONE',  ( 6.158835246850667461E-14, -1.250000000000002442, -4.999999999999999112 ) ) ;
#41581 = CARTESIAN_POINT ( 'NONE',  ( -9.184850993605147944E-16, -151.3750000027311842, 5.000000000000000000 ) ) ;
#41582 = CARTESIAN_POINT ( 'NONE',  ( 5.000000000000000000, -38.41666666666667140, -2.886751345948129988 ) ) ;
#41583 = CARTESIAN_POINT ( 'NONE',  ( 5.000000000000000888, -148.9375000000000000, -2.071067811865475505 ) ) ;
#41585 = CARTESIAN_POINT ( 'NONE',  ( -3.152548672688508926E-16, -16.81249999863440436, -5.148502694627439702 ) ) ;
#41584 = CARTESIAN_POINT ( 'NONE',  ( 3.061616997868383141E-16, -143.7500000000000284, -5.000000000000000000 ) ) ;
#41586 = FACE_OUTER_BOUND ( 'NONE', #965, .T. ) ;
#41587 = CARTESIAN_POINT ( 'NONE',  ( -3.152548672688508926E-16, -57.56249999863439371, -5.148502694627439702 ) ) ;
#41588 = CARTESIAN_POINT ( 'NONE',  ( -3.152801135295367096, -150.3125000013655779, -3.152801135295367541 ) ) ;
#41590 = EDGE_CURVE ( 'NONE', #31117, #19049, #54817, .T. ) ;
#41589 = CARTESIAN_POINT ( 'NONE',  ( 2.229367062500001939, -71.97916666530107932, 3.861377020970579999 ) ) ;
#41591 = CARTESIAN_POINT ( 'NONE',  ( -51.60603307380591787, -146.1875000013656063, -2.891590998281053704 ) ) ;
#41592 = AXIS2_PLACEMENT_3D ( 'NONE', #28548, #48167, #38507 ) ;
#41593 = CARTESIAN_POINT ( 'NONE',  ( 4.458734125000001214, -22.14583333196773296, 2.574251347313718519 ) ) ;
#41594 = CARTESIAN_POINT ( 'NONE',  ( -2.500000000000000444, -61.04166666393547303, -4.330127018922193649 ) ) ;
#41595 = ORIENTED_EDGE ( 'NONE', *, *, #41773, .F. ) ;
#41596 = ORIENTED_EDGE ( 'NONE', *, *, #28667, .T. ) ;
#41597 = CARTESIAN_POINT ( 'NONE',  ( 4.458734124999998549, -62.97916666530107221, -2.574251347313721627 ) ) ;
#41598 = DIRECTION ( 'NONE',  ( -0.000000000000000000, 0.000000000000000000, 1.000000000000000000 ) ) ;
#41599 = CARTESIAN_POINT ( 'NONE',  ( 3.152801135295367541, -153.3125000013656063, -3.152801135295367541 ) ) ;
#41600 = ORIENTED_EDGE ( 'NONE', *, *, #41762, .F. ) ;
#41601 = CARTESIAN_POINT ( 'NONE',  ( -2.500000000000000444, 2.958333336064520314, -4.330127018922193649 ) ) ;
#41602 = CARTESIAN_POINT ( 'NONE',  ( 7.922281120364393914, 4.573931137438269623, -8.047472243342930653 ) ) ;
#41603 = CARTESIAN_POINT ( 'NONE',  ( -4.458734124999999437, -50.56249999863440792, 0.000000000000000000 ) ) ;
#41604 = ORIENTED_EDGE ( 'NONE', *, *, #37764, .F. ) ;
#41605 = EDGE_CURVE ( 'NONE', #36935, #52748, #515, .T. ) ;
#41606 = CARTESIAN_POINT ( 'NONE',  ( -75.00000000000002842, 0.000000000000000000, -5.000000000000000000 ) ) ;
#41607 = EDGE_CURVE ( 'NONE', #11132, #2012, #59320, .T. ) ;
#41608 = CARTESIAN_POINT ( 'NONE',  ( 4.458734124999998549, 9.270833334698927786, -2.574251347313721627 ) ) ;
#41609 = CARTESIAN_POINT ( 'NONE',  ( 9.457646018065525792E-16, 21.93750000136559208, 5.148502694627439702 ) ) ;
#41610 = CARTESIAN_POINT ( 'NONE',  ( -53.51423613279429503, -149.2500000013655779, 4.591703134518082763 ) ) ;
#41611 = CARTESIAN_POINT ( 'NONE',  ( -4.999999999999998224, -23.79166666393548368, 2.886751345948131764 ) ) ;
#41612 = CARTESIAN_POINT ( 'NONE',  ( 2.730187237215162345E-16, -168.1875000013655779, -4.458734124999999437 ) ) ;
#41613 = VERTEX_POINT ( 'NONE', #39217 ) ;
#41614 = CARTESIAN_POINT ( 'NONE',  ( 9.457646018065525792E-16, -71.06249999863439371, 5.148502694627439702 ) ) ;
#41615 = CARTESIAN_POINT ( 'NONE',  ( 2.499999999999998668, -28.20833333060214798, -4.330127018922193649 ) ) ;
#41616 = CARTESIAN_POINT ( 'NONE',  ( -4.458734124999998549, 11.77083333469892601, 2.574251347313722516 ) ) ;
#41617 = ADVANCED_FACE ( 'NONE', ( #20578 ), #24752, .T. ) ;
#41618 = CYLINDRICAL_SURFACE ( 'NONE', #43911, 5.000000000000000000 ) ;
#41619 = CARTESIAN_POINT ( 'NONE',  ( -2.229367062500000163, -53.72916666530107221, -3.861377020970580443 ) ) ;
#41620 = CARTESIAN_POINT ( 'NONE',  ( 1.060575238724906964E-15, -14.62499999726881228, 5.773502691896257311 ) ) ;
#41621 = DIRECTION ( 'NONE',  ( -0.000000000000000000, 1.000000000000000000, -0.000000000000000000 ) ) ;
#41622 = CARTESIAN_POINT ( 'NONE',  ( -2.071067811865432873, -139.8125000027311842, -5.000000000000041744 ) ) ;
#41623 = CARTESIAN_POINT ( 'NONE',  ( 9.457646018065525792E-16, -21.31249999863440081, 5.148502694627439702 ) ) ;
#41624 = ORIENTED_EDGE ( 'NONE', *, *, #61814, .F. ) ;
#41625 = DIRECTION ( 'NONE',  ( 0.5000000000000003331, 0.000000000000000000, 0.8660254037844385966 ) ) ;
#41626 = CARTESIAN_POINT ( 'NONE',  ( -2.500000000000000444, 28.83333333333333215, -4.330127018922193649 ) ) ;
#41627 = CARTESIAN_POINT ( 'NONE',  ( -5.000000000000000000, -158.6250000027311842, -6.123233995736766282E-16 ) ) ;
#41628 = VERTEX_POINT ( 'NONE', #58842 ) ;
#41629 = CARTESIAN_POINT ( 'NONE',  ( -4.458734124999998549, -100.4791666653010509, 2.574251347313722516 ) ) ;
#41630 = CARTESIAN_POINT ( 'NONE',  ( 4.458734124999999437, -26.81249999863440081, -5.460374474430324690E-16 ) ) ;
#41631 = CARTESIAN_POINT ( 'NONE',  ( 5.000000000000000000, -65.37499999726881583, -6.123233995736766282E-16 ) ) ;
#41632 = CIRCLE ( 'NONE', #63228, 5.000000000000000000 ) ;
#41633 = CARTESIAN_POINT ( 'NONE',  ( -50.70258187064364108, -153.3750000013656347, 2.196230717870141014 ) ) ;
#41634 = CARTESIAN_POINT ( 'NONE',  ( -2.071067811865475061, -146.6875000000000568, -5.000000000000000888 ) ) ;
#41635 = ADVANCED_FACE ( 'NONE', ( #320 ), #15743, .T. ) ;
#41636 = CARTESIAN_POINT ( 'NONE',  ( 4.458734124999999437, -25.81249999863440792, -5.460374474430324690E-16 ) ) ;
#41637 = CARTESIAN_POINT ( 'NONE',  ( 9.457646018065525792E-16, -70.31249999863439371, 5.148502694627439702 ) ) ;
#41638 = FACE_OUTER_BOUND ( 'NONE', #628, .T. ) ;
#41639 = CARTESIAN_POINT ( 'NONE',  ( 9.457646018065525792E-16, -24.06249999863440436, 5.148502694627439702 ) ) ;
#41640 = LINE ( 'NONE', #32640, #49180 ) ;
#41641 = CARTESIAN_POINT ( 'NONE',  ( -3.535533905932737309, -150.6250000000000000, -3.535533905932738197 ) ) ;
#41642 = CARTESIAN_POINT ( 'NONE',  ( -3.535250795749689387E-16, -19.24999999999999645, -5.773502691896257311 ) ) ;
#41643 = CARTESIAN_POINT ( 'NONE',  ( 4.458734124999999437, -152.5000000013656347, 1.846868145590737864 ) ) ;
#41644 = ORIENTED_EDGE ( 'NONE', *, *, #2169, .T. ) ;
#41645 = DIRECTION ( 'NONE',  ( -0.000000000000000000, 1.000000000000000000, -0.000000000000000000 ) ) ;
#41646 = CARTESIAN_POINT ( 'NONE',  ( -4.458734124999997661, -52.47916666530107221, 2.574251347313722516 ) ) ;
#41647 = CARTESIAN_POINT ( 'NONE',  ( -5.000000000000000000, -86.95833333060214443, -2.886751345948128211 ) ) ;
#41648 = CARTESIAN_POINT ( 'NONE',  ( -53.33387254593758087, -135.8125000000000284, 5.149110718188498304 ) ) ;
#41649 = CARTESIAN_POINT ( 'NONE',  ( 5.000000000000000888, 23.41666666666666785, 2.886751345948126879 ) ) ;
#41650 =( BOUNDED_CURVE ( )  B_SPLINE_CURVE ( 2, ( #60916, #31631, #31301, #16836, #1115, #26809, #46429, #31946, #51576 ),
 .UNSPECIFIED., .F., .F. ) 
 B_SPLINE_CURVE_WITH_KNOTS ( ( 3, 2, 2, 2, 3 ),
 ( 0.4446428571428571175, 0.4452380952380952106, 0.4464285714285714524, 0.4476190476190476386, 0.4482142857142857317 ),
 .UNSPECIFIED. ) 
 CURVE ( )  GEOMETRIC_REPRESENTATION_ITEM ( )  RATIONAL_B_SPLINE_CURVE ( ( 0.9330127018922194093, 0.9330127018922194093, 1.000000000000000000, 0.8660254037844387076, 1.000000000000000000, 0.8660254037844387076, 1.000000000000000000, 0.9330127018922194093, 0.9330127018922194093 ) ) 
 REPRESENTATION_ITEM ( '' )  );
#41651 = CARTESIAN_POINT ( 'NONE',  ( 0.000000000000000000, -120.0000000000000000, 5.000000000000000000 ) ) ;
#41652 = CARTESIAN_POINT ( 'NONE',  ( -3.152548672688508926E-16, 1.437500001365596525, -5.148502694627439702 ) ) ;
#41653 = CARTESIAN_POINT ( 'NONE',  ( 5.000000000000000000, 19.50000000000000000, -6.123233995736766282E-16 ) ) ;
#41654 = DIRECTION ( 'NONE',  ( -0.000000000000000000, 1.000000000000000000, -0.000000000000000000 ) ) ;
#41655 = CARTESIAN_POINT ( 'NONE',  ( 5.000000000000000000, -87.29166666393547303, -2.886751345948130876 ) ) ;
#41656 = CARTESIAN_POINT ( 'NONE',  ( 4.458734125000001214, 17.85416666803225993, 2.574251347313718519 ) ) ;
#41657 = CARTESIAN_POINT ( 'NONE',  ( -3.535250795749689387E-16, 3.875000002731186832, -5.773502691896257311 ) ) ;
#41658 = ORIENTED_EDGE ( 'NONE', *, *, #55511, .T. ) ;
#41659 = CARTESIAN_POINT ( 'NONE',  ( -5.000000000000000000, -29.95833333060214443, -2.886751345948128211 ) ) ;
#41660 = ORIENTED_EDGE ( 'NONE', *, *, #42264, .F. ) ;
#41661 = CARTESIAN_POINT ( 'NONE',  ( 5.000000000000000888, -168.0625000027312410, -2.071067811865475505 ) ) ;
#41662 = CARTESIAN_POINT ( 'NONE',  ( 2.229367062500001939, -44.97916666530106511, 3.861377020970579999 ) ) ;
#41663 = CARTESIAN_POINT ( 'NONE',  ( 4.458734125000000326, -163.6250000013656063, -1.846868145590734978 ) ) ;
#41664 = EDGE_CURVE ( 'NONE', #3938, #14927, #2247, .T. ) ;
#41665 =( BOUNDED_CURVE ( )  B_SPLINE_CURVE ( 2, ( #32082, #23398, #13728, #47511, #47207, #57806, #51719, #17924, #62320 ),
 .UNSPECIFIED., .F., .F. ) 
 B_SPLINE_CURVE_WITH_KNOTS ( ( 3, 2, 2, 2, 3 ),
 ( 0.7017857142857142350, 0.7023809523809523281, 0.7035714285714286254, 0.7047619047619048116, 0.7053571428571429047 ),
 .UNSPECIFIED. ) 
 CURVE ( )  GEOMETRIC_REPRESENTATION_ITEM ( )  RATIONAL_B_SPLINE_CURVE ( ( 0.9330127018922194093, 0.9330127018922194093, 1.000000000000000000, 0.8660254037844387076, 1.000000000000000000, 0.8660254037844387076, 1.000000000000000000, 0.9330127018922194093, 0.9330127018922194093 ) ) 
 REPRESENTATION_ITEM ( '' )  );
#41666 = EDGE_CURVE ( 'NONE', #19824, #29058, #36631, .T. ) ;
#41667 = CARTESIAN_POINT ( 'NONE',  ( 2.500000000000002220, -44.54166666393547303, 4.330127018922192761 ) ) ;
#41668 = EDGE_CURVE ( 'NONE', #60851, #57423, #8791, .T. ) ;
#41669 = ORIENTED_EDGE ( 'NONE', *, *, #35079, .T. ) ;
#41670 = CARTESIAN_POINT ( 'NONE',  ( 4.458734124999999437, -17.81249999863440792, -5.460374474430324690E-16 ) ) ;
#41671 = VERTEX_POINT ( 'NONE', #30853 ) ;
#41672 = CARTESIAN_POINT ( 'NONE',  ( 5.000000000000000000, -88.50000000000000000, -6.123233995736766282E-16 ) ) ;
#41673 = CARTESIAN_POINT ( 'NONE',  ( 1.846868145590736310, -164.6250000013655779, 4.458734124999999437 ) ) ;
#41675 = ORIENTED_EDGE ( 'NONE', *, *, #33067, .T. ) ;
#41674 = CARTESIAN_POINT ( 'NONE',  ( -2.500000000000000444, -19.16666666666666430, -4.330127018922193649 ) ) ;
#41676 = CARTESIAN_POINT ( 'NONE',  ( -51.75738570946856498, -138.7500000000000000, 3.805975901505576964 ) ) ;
#41677 = CARTESIAN_POINT ( 'NONE',  ( -4.458734124999999437, -33.64583333196772941, -2.574251347313719407 ) ) ;
#41678 = CARTESIAN_POINT ( 'NONE',  ( -3.535533905932737309, -147.7500000027311842, -3.535533905932738197 ) ) ;
#41679 = ADVANCED_FACE ( 'NONE', ( #11549 ), #21847, .T. ) ;
#41680 = ORIENTED_EDGE ( 'NONE', *, *, #3660, .F. ) ;
#41681 = VECTOR ( 'NONE', #60486, 1000.000000000000000 ) ;
#41682 = ITEM_DEFINED_TRANSFORMATION ( 'NONE', 'NONE', #49255,  #43054 ) ;
#41683 = CARTESIAN_POINT ( 'NONE',  ( 9.457646018065525792E-16, -79.06249999863440792, 5.148502694627439702 ) ) ;
#41684 = EDGE_CURVE ( 'NONE', #52679, #34612, #28507, .T. ) ;
#41685 = CARTESIAN_POINT ( 'NONE',  ( 2.229367062499998831, 23.35416666803225993, -3.861377020970580887 ) ) ;
#41686 = CARTESIAN_POINT ( 'NONE',  ( -59.81910112700027327, -137.3125000027312126, -2.462841084822392279 ) ) ;
#41687 = VERTEX_POINT ( 'NONE', #46285 ) ;
#41688 = CARTESIAN_POINT ( 'NONE',  ( -1.339745962155610925, -25.79465819873852084, 5.000000000000000000 ) ) ;
#41689 = CARTESIAN_POINT ( 'NONE',  ( -58.39396692619412477, -140.6875000013656063, 2.891590998281057701 ) ) ;
#41690 = CARTESIAN_POINT ( 'NONE',  ( 9.457646018065525792E-16, -78.31249999863442213, 5.148502694627439702 ) ) ;
#41691 = CARTESIAN_POINT ( 'NONE',  ( -51.75738570946856498, -131.8750000027312126, 3.805975901505576964 ) ) ;
#41692 = CARTESIAN_POINT ( 'NONE',  ( 1.339745962155612702, 22.70534180126147916, -5.000000000000000000 ) ) ;
#41693 = CARTESIAN_POINT ( 'NONE',  ( -1.339745962155613812, -83.20534180126146850, -5.000000000000000000 ) ) ;
#41694 = CARTESIAN_POINT ( 'NONE',  ( -3.152548672688508926E-16, -54.56249999863439371, -5.148502694627439702 ) ) ;
#41695 = CARTESIAN_POINT ( 'NONE',  ( 9.457646018065525792E-16, -44.06249999863439371, 5.148502694627439702 ) ) ;
#41696 = CARTESIAN_POINT ( 'NONE',  ( -5.000000000000000000, 20.99999999999999645, 0.000000000000000000 ) ) ;
#41697 = CARTESIAN_POINT ( 'NONE',  ( -2.499999999999996447, -108.8333333333333428, 4.330127018922195425 ) ) ;
#41698 = DIRECTION ( 'NONE',  ( -0.000000000000000000, 1.000000000000000000, -0.000000000000000000 ) ) ;
#41699 = CARTESIAN_POINT ( 'NONE',  ( -2.229367062499996610, -40.39583333196773651, 3.861377020970582219 ) ) ;
#41700 = CARTESIAN_POINT ( 'NONE',  ( -2.500000000000000444, 1.958333336064519647, -4.330127018922193649 ) ) ;
#41701 = DIRECTION ( 'NONE',  ( 0.000000000000000000, 0.000000000000000000, 1.000000000000000000 ) ) ;
#41702 = CARTESIAN_POINT ( 'NONE',  ( -57.89159099828107458, -126.6875000013656063, -3.393966926194107447 ) ) ;
#41703 = CARTESIAN_POINT ( 'NONE',  ( -2.229367062499996610, -79.39583333196773651, 3.861377020970582219 ) ) ;
#41704 = CYLINDRICAL_SURFACE ( 'NONE', #48655, 5.000000000000000000 ) ;
#41705 = CARTESIAN_POINT ( 'NONE',  ( -4.458734124999997661, -102.2291666653010793, 2.574251347313722516 ) ) ;
#41706 = CARTESIAN_POINT ( 'NONE',  ( 4.458734124999999437, -8.062499998634404363, -5.460374474430324690E-16 ) ) ;
#41707 = ORIENTED_EDGE ( 'NONE', *, *, #60320, .F. ) ;
#41708 = CARTESIAN_POINT ( 'NONE',  ( -2.500000000000000444, -36.04166666393547303, -4.330127018922193649 ) ) ;
#41709 = CARTESIAN_POINT ( 'NONE',  ( 4.458734125000001214, -92.89583333196775072, 2.574251347313718519 ) ) ;
#41710 = CARTESIAN_POINT ( 'NONE',  ( -1.336351044127974539E-14, 23.24999999999999645, 5.000000000000000000 ) ) ;
#41711 = CARTESIAN_POINT ( 'NONE',  ( -3.152548672688508926E-16, -84.81249999863439371, -5.148502694627439702 ) ) ;
#41712 = CARTESIAN_POINT ( 'NONE',  ( -4.458734124999999437, 13.43750000136559386, 0.000000000000000000 ) ) ;
#41713 = DIRECTION ( 'NONE',  ( -0.000000000000000000, 1.000000000000000000, -0.000000000000000000 ) ) ;
#41714 = CARTESIAN_POINT ( 'NONE',  ( -59.59170313451811296, -132.5000000013656063, 1.485763867205729394 ) ) ;
#41715 = CARTESIAN_POINT ( 'NONE',  ( 2.229367062500001939, -6.979166665301073103, 3.861377020970579999 ) ) ;
#41716 = CARTESIAN_POINT ( 'NONE',  ( -2.229367062499996610, 18.60416666803225993, 3.861377020970582219 ) ) ;
#41717 = CARTESIAN_POINT ( 'NONE',  ( 4.458734124999998549, -51.97916666530107221, -2.574251347313721627 ) ) ;
#41718 = CARTESIAN_POINT ( 'NONE',  ( 5.000000000000000000, -38.37499999726881583, -6.123233995736766282E-16 ) ) ;
#41719 = CARTESIAN_POINT ( 'NONE',  ( -5.000000000000000000, -37.08333333333332860, -2.886751345948128211 ) ) ;
#41720 = CARTESIAN_POINT ( 'NONE',  ( -2.229367062500000163, -7.479166665301073991, -3.861377020970580443 ) ) ;
#41721 = SURFACE_STYLE_FILL_AREA ( #51715 ) ;
#41722 = ORIENTED_EDGE ( 'NONE', *, *, #13736, .T. ) ;
#41723 = CARTESIAN_POINT ( 'NONE',  ( -2.229367062500000163, -35.72916666530107221, -3.861377020970580443 ) ) ;
#41724 =( BOUNDED_CURVE ( )  B_SPLINE_CURVE ( 2, ( #8514, #51950, #3070, #47122, #27493, #8827, #52583, #22687, #43224 ),
 .UNSPECIFIED., .F., .F. ) 
 B_SPLINE_CURVE_WITH_KNOTS ( ( 3, 2, 2, 2, 3 ),
 ( 0.05208333333333333565, 0.05277777777777777762, 0.05416666666666666852, 0.05555555555555555247, 0.05625000000000000139 ),
 .UNSPECIFIED. ) 
 CURVE ( )  GEOMETRIC_REPRESENTATION_ITEM ( )  RATIONAL_B_SPLINE_CURVE ( ( 0.9330127018922192983, 0.9330127018922196314, 1.000000000000000000, 0.8660254037844387076, 1.000000000000000000, 0.8660254037844387076, 1.000000000000000000, 0.9330127018922189652, 0.9330127018922192983 ) ) 
 REPRESENTATION_ITEM ( '' )  );
#41725 = CARTESIAN_POINT ( 'NONE',  ( -50.70258187064364108, -126.3750000013656489, 2.196230717870141014 ) ) ;
#41726 = CARTESIAN_POINT ( 'NONE',  ( 1.975475456537005874E-15, -76.75000000000000000, 5.000000000000000000 ) ) ;
#41727 = CARTESIAN_POINT ( 'NONE',  ( -3.152548672688508926E-16, -82.56249999863442213, -5.148502694627439702 ) ) ;
#41728 = CARTESIAN_POINT ( 'NONE',  ( -2.229367062500000163, 26.27083333469892779, -3.861377020970580443 ) ) ;
#41729 = VECTOR ( 'NONE', #36896, 1000.000000000000000 ) ;
#41730 = CARTESIAN_POINT ( 'NONE',  ( -3.152801135295367096, -148.3125000013655779, -3.152801135295367541 ) ) ;
#41731 = CARTESIAN_POINT ( 'NONE',  ( 4.458734124999999437, 21.18750000136559208, -5.460374474430324690E-16 ) ) ;
#41732 = DIRECTION ( 'NONE',  ( -1.000000000000000000, -0.000000000000000000, -0.000000000000000000 ) ) ;
#41733 = CARTESIAN_POINT ( 'NONE',  ( 5.000000000000000888, 1.416666666666666741, 2.886751345948126879 ) ) ;
#41734 = CARTESIAN_POINT ( 'NONE',  ( 4.458734124999999437, -85.06249999863439371, -5.460374474430324690E-16 ) ) ;
#41735 = CARTESIAN_POINT ( 'NONE',  ( 5.000000000000000000, -66.41666666666667140, -2.886751345948129988 ) ) ;
#41736 = CARTESIAN_POINT ( 'NONE',  ( 2.499999999999998668, -72.20833333060214443, -4.330127018922193649 ) ) ;
#41737 = CARTESIAN_POINT ( 'NONE',  ( 5.000000000000000000, 16.70833333606451987, -2.886751345948129988 ) ) ;
#41738 = VERTEX_POINT ( 'NONE', #2243 ) ;
#41739 = DIRECTION ( 'NONE',  ( 0.000000000000000000, 0.000000000000000000, 1.000000000000000000 ) ) ;
#41740 = CARTESIAN_POINT ( 'NONE',  ( -1.339745962155585168, 8.794658198738517285, -5.000000000000015987 ) ) ;
#41742 = CARTESIAN_POINT ( 'NONE',  ( 2.499999999999998668, -23.33333333333333215, -4.330127018922193649 ) ) ;
#41741 = CARTESIAN_POINT ( 'NONE',  ( 0.000000000000000000, -170.0000000000000000, 0.000000000000000000 ) ) ;
#41743 = CARTESIAN_POINT ( 'NONE',  ( 4.458734124999998549, -28.72916666530107221, -2.574251347313721627 ) ) ;
#41744 = CARTESIAN_POINT ( 'NONE',  ( -2.229367062500000163, -86.47916666530107932, -3.861377020970580443 ) ) ;
#41745 = EDGE_CURVE ( 'NONE', #54676, #38746, #48225, .T. ) ;
#41746 = CARTESIAN_POINT ( 'NONE',  ( 5.000000000000000000, -31.37499999726880873, -6.123233995736766282E-16 ) ) ;
#41748 = ORIENTED_EDGE ( 'NONE', *, *, #12644, .F. ) ;
#41747 = CARTESIAN_POINT ( 'NONE',  ( 9.457646018065525792E-16, -55.06249999863439371, 5.148502694627439702 ) ) ;
#41749 = CARTESIAN_POINT ( 'NONE',  ( -52.10840900171896806, -154.4375000013656063, 3.393966926194110556 ) ) ;
#41751 = VERTEX_POINT ( 'NONE', #45648 ) ;
#41750 = CARTESIAN_POINT ( 'NONE',  ( 4.458734124999998549, -9.979166665301068662, -2.574251347313721627 ) ) ;
#41752 = CARTESIAN_POINT ( 'NONE',  ( 5.000000000000000000, -69.41666666666667140, -2.886751345948129988 ) ) ;
#41753 = CARTESIAN_POINT ( 'NONE',  ( -50.40829686548195099, -140.0000000013656063, -1.485763867205728284 ) ) ;
#41754 = CARTESIAN_POINT ( 'NONE',  ( 2.229367062500001939, -50.22916666530107221, 3.861377020970579999 ) ) ;
#41755 =( BOUNDED_CURVE ( )  B_SPLINE_CURVE ( 2, ( #53188, #48355, #23613, #62544, #58329, #48661, #28109, #9121, #43209 ),
 .UNSPECIFIED., .F., .F. ) 
 B_SPLINE_CURVE_WITH_KNOTS ( ( 3, 2, 2, 2, 3 ),
 ( 0.3937499999999999889, 0.3944444444444444309, 0.3958333333333333148, 0.3972222222222221988, 0.3979166666666666963 ),
 .UNSPECIFIED. ) 
 CURVE ( )  GEOMETRIC_REPRESENTATION_ITEM ( )  RATIONAL_B_SPLINE_CURVE ( ( 0.9330127018922194093, 0.9330127018922194093, 1.000000000000000000, 0.8660254037844387076, 1.000000000000000000, 0.8660254037844387076, 1.000000000000000000, 0.9330127018922167448, 0.9330127018922194093 ) ) 
 REPRESENTATION_ITEM ( '' )  );
#41756 = EDGE_CURVE ( 'NONE', #43111, #7190, #15364, .T. ) ;
#41757 = CARTESIAN_POINT ( 'NONE',  ( -5.000000000000000000, -78.95833333060213022, -2.886751345948128211 ) ) ;
#41758 = EDGE_LOOP ( 'NONE', ( #39760, #59721, #52398, #27048 ) ) ;
#41759 = CARTESIAN_POINT ( 'NONE',  ( -56.66612745406270335, -149.3125000000000000, -5.149110718188516067 ) ) ;
#41760 = ADVANCED_FACE ( 'NONE', ( #45962 ), #46921, .T. ) ;
#41761 = CARTESIAN_POINT ( 'NONE',  ( -3.152548672688508926E-16, -18.81249999863440792, -5.148502694627439702 ) ) ;
#41762 = EDGE_CURVE ( 'NONE', #11950, #62422, #5214, .T. ) ;
#41763 = CARTESIAN_POINT ( 'NONE',  ( -4.458734124999999437, -51.56249999863440792, 0.000000000000000000 ) ) ;
#41764 = CARTESIAN_POINT ( 'NONE',  ( -1.339745962155613812, 0.7946581987385198387, -5.000000000000000000 ) ) ;
#41765 = CARTESIAN_POINT ( 'NONE',  ( -8.190561711645485556E-16, -139.6875000013656063, 4.458734124999999437 ) ) ;
#41766 = CARTESIAN_POINT ( 'NONE',  ( 9.457646018065525792E-16, -102.3124999986344221, 5.148502694627439702 ) ) ;
#41767 = CYLINDRICAL_SURFACE ( 'NONE', #25570, 5.000000000000000000 ) ;
#41768 = ORIENTED_EDGE ( 'NONE', *, *, #22758, .F. ) ;
#41769 = EDGE_CURVE ( 'NONE', #47799, #55067, #53674, .T. ) ;
#41770 = CARTESIAN_POINT ( 'NONE',  ( -5.000000000000000888, -155.5625000000000853, -2.071067811865475949 ) ) ;
#41771 = CARTESIAN_POINT ( 'NONE',  ( -58.80597590150559739, -144.1250000027312126, 3.242614290531460330 ) ) ;
#41772 = AXIS2_PLACEMENT_3D ( 'NONE', #24643, #33976, #58737 ) ;
#41773 = EDGE_CURVE ( 'NONE', #35874, #34281, #13848, .T. ) ;
#41774 = CARTESIAN_POINT ( 'NONE',  ( 1.062108568985190270E-13, -13.12499999726881583, -4.999999999999999112 ) ) ;
#41775 = VECTOR ( 'NONE', #60363, 1000.000000000000000 ) ;
#41776 = CARTESIAN_POINT ( 'NONE',  ( -2.229367062499996610, -5.145833331967740065, 3.861377020970582219 ) ) ;
#41777 = CARTESIAN_POINT ( 'NONE',  ( 4.458734124999999437, -98.06249999863440792, -5.460374474430324690E-16 ) ) ;
#41778 = EDGE_CURVE ( 'NONE', #37182, #24836, #4120, .T. ) ;
#41779 = CARTESIAN_POINT ( 'NONE',  ( -4.458734125000001214, -150.1250000013655779, 1.846868145590734089 ) ) ;
#41780 = CARTESIAN_POINT ( 'NONE',  ( -4.458734124999999437, -20.56249999863440081, 0.000000000000000000 ) ) ;
#41781 = AXIS2_PLACEMENT_3D ( 'NONE', #55350, #40221, #16097 ) ;
#41782 = CARTESIAN_POINT ( 'NONE',  ( -6.972266317189433020E-16, -67.25000000000000000, -5.000000000000000000 ) ) ;
#41783 = CARTESIAN_POINT ( 'NONE',  ( -57.19623071787017210, -137.3750000013656063, 4.297418129356382899 ) ) ;
#41784 = CARTESIAN_POINT ( 'NONE',  ( -4.458734124999998549, -61.47916666530107221, 2.574251347313722516 ) ) ;
#41785 = DIRECTION ( 'NONE',  ( 0.000000000000000000, 0.000000000000000000, 1.000000000000000000 ) ) ;
#41786 = CARTESIAN_POINT ( 'NONE',  ( 7.970070017554212960, -4.546953124339766283, -8.057670357645358550 ) ) ;
#41787 = CARTESIAN_POINT ( 'NONE',  ( 4.458734124999999437, -143.3750000013656063, -1.846868145590734978 ) ) ;
#41788 = CARTESIAN_POINT ( 'NONE',  ( -4.458734124999997661, 11.52083333469892423, 2.574251347313722516 ) ) ;
#41789 = VERTEX_POINT ( 'NONE', #42393 ) ;
#41790 = CARTESIAN_POINT ( 'NONE',  ( -9.184850993605147944E-16, -164.3750000027311842, 5.000000000000000000 ) ) ;
#41791 = DIRECTION ( 'NONE',  ( -0.000000000000000000, 1.000000000000000000, -0.000000000000000000 ) ) ;
#41793 = CARTESIAN_POINT ( 'NONE',  ( -4.458734124999998549, -24.22916666530107577, 2.574251347313722516 ) ) ;
#41792 = CARTESIAN_POINT ( 'NONE',  ( 2.499999999999998668, -91.33333333333334281, -4.330127018922193649 ) ) ;
#41794 = CARTESIAN_POINT ( 'NONE',  ( -7.500000000000000888, -1.443375672974068769, -7.063244554130002406 ) ) ;
#41795 = CARTESIAN_POINT ( 'NONE',  ( 2.229367062499998831, -68.89583333196773651, -3.861377020970580887 ) ) ;
#41796 = CARTESIAN_POINT ( 'NONE',  ( 4.458734124999999437, 27.93750000136559208, -5.460374474430324690E-16 ) ) ;
#41797 = FACE_OUTER_BOUND ( 'NONE', #28151, .T. ) ;
#41798 = CARTESIAN_POINT ( 'NONE',  ( -57.19623071787017210, -146.3750000013655779, 4.297418129356382899 ) ) ;
#41799 = CARTESIAN_POINT ( 'NONE',  ( 2.499999999999998668, -52.20833333060213732, -4.330127018922193649 ) ) ;
#41800 = CARTESIAN_POINT ( 'NONE',  ( -54.60164318462004474, -148.3750000000000284, -4.984105922594373794 ) ) ;
#41801 = CARTESIAN_POINT ( 'NONE',  ( -4.458734124999997661, 10.77083333469892956, 2.574251347313722516 ) ) ;
#41802 = CARTESIAN_POINT ( 'NONE',  ( 6.123233995736766282E-16, -170.0000000000000000, -5.000000000000000000 ) ) ;
#41803 = CARTESIAN_POINT ( 'NONE',  ( -2.498395430326213474E-14, 21.24999999999999289, 5.000000000000000000 ) ) ;
#41804 = CARTESIAN_POINT ( 'NONE',  ( -4.458734124999999437, 7.604166668032259935, -2.574251347313719407 ) ) ;
#41805 = CARTESIAN_POINT ( 'NONE',  ( -4.458734124999999437, -71.39583333196773651, -2.574251347313719407 ) ) ;
#41806 = CARTESIAN_POINT ( 'NONE',  ( 2.229367062499998831, -19.89583333196774007, -3.861377020970580887 ) ) ;
#41807 = CARTESIAN_POINT ( 'NONE',  ( 2.500000000000002220, 1.333333333333332149, 4.330127018922192761 ) ) ;
#41808 = CARTESIAN_POINT ( 'NONE',  ( 1.846868145590735200, -161.2500000013655779, -4.458734125000000326 ) ) ;
#41809 = CARTESIAN_POINT ( 'NONE',  ( 9.457646018065525792E-16, -66.06249999863440792, 5.148502694627439702 ) ) ;
#41810 = CARTESIAN_POINT ( 'NONE',  ( 5.000000000000000000, -93.29166666393547303, -2.886751345948129988 ) ) ;
#41811 = CARTESIAN_POINT ( 'NONE',  ( 2.499999999999998668, 5.791666669397853795, -4.330127018922193649 ) ) ;
#41812 = CARTESIAN_POINT ( 'NONE',  ( 2.229367062499998831, -38.64583333196773651, -3.861377020970580887 ) ) ;
#41813 = CARTESIAN_POINT ( 'NONE',  ( 5.000000000000000000, -60.50000000000000000, -6.123233995736766282E-16 ) ) ;
#41814 = CARTESIAN_POINT ( 'NONE',  ( 2.229367062500001939, -67.22916666530106511, 3.861377020970579999 ) ) ;
#41815 = CARTESIAN_POINT ( 'NONE',  ( -2.500000000000000444, -50.16666666666666430, -4.330127018922193649 ) ) ;
#41816 = CARTESIAN_POINT ( 'NONE',  ( 5.000000000000000888, -72.45833333060213022, 2.886751345948126879 ) ) ;
#41817 = CARTESIAN_POINT ( 'NONE',  ( 1.339745962155615144, -36.58034179853029855, 4.999999999999999112 ) ) ;
#41818 = EDGE_LOOP ( 'NONE', ( #1197, #39935, #42920, #9555 ) ) ;
#41819 = FACE_OUTER_BOUND ( 'NONE', #52790, .T. ) ;
#41820 = VECTOR ( 'NONE', #2287, 1000.000000000000000 ) ;
#41821 = CARTESIAN_POINT ( 'NONE',  ( 0.000000000000000000, -120.0000000000000000, 0.000000000000000000 ) ) ;
#41822 = CARTESIAN_POINT ( 'NONE',  ( -2.500000000000000444, -5.166666666666666963, -4.330127018922193649 ) ) ;
#41823 = VECTOR ( 'NONE', #4922, 1000.000000000000000 ) ;
#41824 = CARTESIAN_POINT ( 'NONE',  ( 4.458734124999999437, -71.81249999863439371, -5.460374474430324690E-16 ) ) ;
#41825 = PRESENTATION_LAYER_ASSIGNMENT (  '', '', ( #36696 ) ) ;
#41826 = CARTESIAN_POINT ( 'NONE',  ( -1.339745962155613812, -5.080341798530291442, -5.000000000000000000 ) ) ;
#41827 = CARTESIAN_POINT ( 'NONE',  ( -2.500000000000000444, -15.04166666393548191, -4.330127018922193649 ) ) ;
#41829 = ORIENTED_EDGE ( 'NONE', *, *, #3867, .T. ) ;
#41828 = CARTESIAN_POINT ( 'NONE',  ( -4.458734124999998549, -40.22916666530107932, 2.574251347313722516 ) ) ;
#41830 = VECTOR ( 'NONE', #8178, 1000.000000000000000 ) ;
#41831 = CYLINDRICAL_SURFACE ( 'NONE', #45652, 5.000000000000000000 ) ;
#41833 = VERTEX_POINT ( 'NONE', #17951 ) ;
#41832 = CARTESIAN_POINT ( 'NONE',  ( -4.458734124999998549, 6.520833334698930450, 2.574251347313722516 ) ) ;
#41834 = CARTESIAN_POINT ( 'NONE',  ( -4.999999999999999112, -53.91666666666667140, 2.886751345948131764 ) ) ;
#41835 = CARTESIAN_POINT ( 'NONE',  ( -4.458734125000000326, -160.2500000013656063, -1.846868145590735644 ) ) ;
#41836 = CARTESIAN_POINT ( 'NONE',  ( 4.458734125000001214, -34.14583333196772941, 2.574251347313718519 ) ) ;
#41837 = CARTESIAN_POINT ( 'NONE',  ( 5.000000000000000000, -10.41666666666666607, -2.886751345948130876 ) ) ;
#41838 = CARTESIAN_POINT ( 'NONE',  ( -2.229367062499996610, -81.14583333196773651, 3.861377020970582219 ) ) ;
#41839 = CARTESIAN_POINT ( 'NONE',  ( -5.000000000000000000, -166.5000000000000000, -6.123233995736766282E-16 ) ) ;
#41840 = CARTESIAN_POINT ( 'NONE',  ( 4.458734124999998549, -88.72916666530106511, -2.574251347313721627 ) ) ;
#41841 = CARTESIAN_POINT ( 'NONE',  ( -57.19623071787017210, -132.6250000013656347, 4.297418129356382899 ) ) ;
#41842 = CARTESIAN_POINT ( 'NONE',  ( -4.458734124999999437, -0.5624999986344053626, 0.000000000000000000 ) ) ;
#41843 = CARTESIAN_POINT ( 'NONE',  ( 4.458734124999999437, -37.06249999863440792, -5.460374474430324690E-16 ) ) ;
#41844 = CARTESIAN_POINT ( 'NONE',  ( 2.500000000000002220, -72.66666666666667140, 4.330127018922192761 ) ) ;
#41845 = CARTESIAN_POINT ( 'NONE',  ( -4.458734124999998549, -85.47916666530106511, 2.574251347313722516 ) ) ;
#41846 = CARTESIAN_POINT ( 'NONE',  ( -9.184850993605147944E-16, -145.2500000000000284, 5.000000000000000000 ) ) ;
#41847 = ORIENTED_EDGE ( 'NONE', *, *, #37762, .T. ) ;
#41848 = CARTESIAN_POINT ( 'NONE',  ( -5.000000000000000888, -141.5625000000000568, -2.071067811865475949 ) ) ;
#41849 = DIRECTION ( 'NONE',  ( -0.000000000000000000, 1.000000000000000000, -0.000000000000000000 ) ) ;
#41850 = CARTESIAN_POINT ( 'NONE',  ( -4.458734124999999437, -68.56249999863439371, 0.000000000000000000 ) ) ;
#41851 = CARTESIAN_POINT ( 'NONE',  ( -2.229367062500000163, -7.729166665301073991, -3.861377020970580443 ) ) ;
#41852 = ORIENTED_EDGE ( 'NONE', *, *, #1131, .F. ) ;
#41853 = CARTESIAN_POINT ( 'NONE',  ( 2.071067811865412445, -163.8125000000000000, -5.000000000000063949 ) ) ;
#41854 =( BOUNDED_CURVE ( )  B_SPLINE_CURVE ( 2, ( #49213, #38598, #47943, #29258, #13549, #4213, #24771, #14158, #57621 ),
 .UNSPECIFIED., .F., .F. ) 
 B_SPLINE_CURVE_WITH_KNOTS ( ( 3, 2, 2, 2, 3 ),
 ( 0.3125000000000000000, 0.3130952380952380931, 0.3142857142857142794, 0.3154761904761904656, 0.3160714285714285587 ),
 .UNSPECIFIED. ) 
 CURVE ( )  GEOMETRIC_REPRESENTATION_ITEM ( )  RATIONAL_B_SPLINE_CURVE ( ( 0.9330127018922194093, 0.9330127018922194093, 1.000000000000000000, 0.8660254037844387076, 1.000000000000000000, 0.8660254037844387076, 1.000000000000000000, 0.9330127018922194093, 0.9330127018922194093 ) ) 
 REPRESENTATION_ITEM ( '' )  );
#41855 = EDGE_CURVE ( 'NONE', #28232, #14051, #20814, .T. ) ;
#41856 = FACE_OUTER_BOUND ( 'NONE', #16823, .T. ) ;
#41857 = CARTESIAN_POINT ( 'NONE',  ( 9.457646018065525792E-16, -9.312499998634406140, 5.148502694627439702 ) ) ;
#41858 = CYLINDRICAL_SURFACE ( 'NONE', #19922, 5.000000000000000000 ) ;
#41859 = CARTESIAN_POINT ( 'NONE',  ( 4.458734125000001214, 1.104166668032261711, 2.574251347313718519 ) ) ;
#41860 = CARTESIAN_POINT ( 'NONE',  ( 1.975475456537005874E-15, -64.74999999999998579, 5.000000000000000000 ) ) ;
#41861 = CARTESIAN_POINT ( 'NONE',  ( -4.458734124999999437, -157.9375000013655779, -5.460374474430324690E-16 ) ) ;
#41862 = AXIS2_PLACEMENT_3D ( 'NONE', #53795, #24855, #45424 ) ;
#41863 = CARTESIAN_POINT ( 'NONE',  ( 9.457646018065525792E-16, 25.68750000136559208, 5.148502694627439702 ) ) ;
#41864 = VERTEX_POINT ( 'NONE', #62669 ) ;
#41865 = CARTESIAN_POINT ( 'NONE',  ( 2.229367062499998831, -85.64583333196773651, -3.861377020970580887 ) ) ;
#41866 = CARTESIAN_POINT ( 'NONE',  ( -4.999999999999998224, -77.91666666666665719, 2.886751345948131764 ) ) ;
#41867 = CARTESIAN_POINT ( 'NONE',  ( -4.458734124999999437, -10.39583333196773829, -2.574251347313719407 ) ) ;
#41868 = VECTOR ( 'NONE', #62481, 1000.000000000000000 ) ;
#41869 = DIRECTION ( 'NONE',  ( -0.000000000000000000, 1.000000000000000000, -0.000000000000000000 ) ) ;
#41870 = CARTESIAN_POINT ( 'NONE',  ( 0.000000000000000000, -120.0000000000000000, 0.000000000000000000 ) ) ;
#41871 = CARTESIAN_POINT ( 'NONE',  ( -2.500000000000000444, -34.04166666393547303, -4.330127018922193649 ) ) ;
#41872 = DIRECTION ( 'NONE',  ( -0.000000000000000000, 1.000000000000000000, -0.000000000000000000 ) ) ;
#41873 = CARTESIAN_POINT ( 'NONE',  ( -4.458734124999997661, 22.77083333469892068, 2.574251347313722516 ) ) ;
#41874 = FACE_OUTER_BOUND ( 'NONE', #37749, .T. ) ;
#41875 = CARTESIAN_POINT ( 'NONE',  ( 4.458734124999998549, 22.27083333469892779, -2.574251347313721627 ) ) ;
#41876 = CARTESIAN_POINT ( 'NONE',  ( -4.458734124999999437, -50.39583333196773651, -2.574251347313719407 ) ) ;
#41877 = CARTESIAN_POINT ( 'NONE',  ( -4.458734124999999437, -1.645833331967737401, -2.574251347313719407 ) ) ;
#41878 = CARTESIAN_POINT ( 'NONE',  ( -2.500000000000000444, 8.958333336064518093, -4.330127018922193649 ) ) ;
#41879 = CARTESIAN_POINT ( 'NONE',  ( -3.535250795749689387E-16, 12.75000000000000000, -5.773502691896257311 ) ) ;
#41880 = CARTESIAN_POINT ( 'NONE',  ( 2.071067811865476394, -142.3125000027312410, 5.000000000000000000 ) ) ;
#41881 = CARTESIAN_POINT ( 'NONE',  ( 1.975475456537005874E-15, -51.75000000000000000, 5.000000000000000000 ) ) ;
#41882 = CARTESIAN_POINT ( 'NONE',  ( 4.458734124999999437, -47.81249999863440792, -5.460374474430324690E-16 ) ) ;
#41883 = CARTESIAN_POINT ( 'NONE',  ( 5.000000000000000000, -81.29166666393547303, -2.886751345948129988 ) ) ;
#41884 = CARTESIAN_POINT ( 'NONE',  ( -50.40829686548195099, -139.2500000013656063, -1.485763867205728284 ) ) ;
#41885 = DIRECTION ( 'NONE',  ( 1.000000000000000000, 0.000000000000000000, 0.000000000000000000 ) ) ;
#41886 = CARTESIAN_POINT ( 'NONE',  ( 1.975475456537005874E-15, -27.74999999999999645, 5.000000000000000000 ) ) ;
#41887 = VECTOR ( 'NONE', #2322, 1000.000000000000000 ) ;
#41888 = CARTESIAN_POINT ( 'NONE',  ( 4.458734125000000326, -84.14583333196773651, 2.574251347313718519 ) ) ;
#41889 = CARTESIAN_POINT ( 'NONE',  ( 1.846868145590736310, -158.8750000013655779, 4.458734124999997661 ) ) ;
#41890 = CARTESIAN_POINT ( 'NONE',  ( 5.000000000000000000, -31.50000000000000000, -6.123233995736766282E-16 ) ) ;
#41891 = CARTESIAN_POINT ( 'NONE',  ( -5.000000000000000888, -147.5625000000000853, -2.071067811865475949 ) ) ;
#41892 = VERTEX_POINT ( 'NONE', #18589 ) ;
#41893 = CARTESIAN_POINT ( 'NONE',  ( -2.229367062499996610, 15.60416666803225993, 3.861377020970582219 ) ) ;
#41894 = ORIENTED_EDGE ( 'NONE', *, *, #16203, .F. ) ;
#41895 = CARTESIAN_POINT ( 'NONE',  ( -4.458734124999999437, -92.31249999863440792, 0.000000000000000000 ) ) ;
#41896 = CARTESIAN_POINT ( 'NONE',  ( -4.458734124999998549, 14.52083333469892779, 2.574251347313722516 ) ) ;
#41897 = CARTESIAN_POINT ( 'NONE',  ( 5.000000000000000000, 15.70833333606451809, -2.886751345948129988 ) ) ;
#41898 = CARTESIAN_POINT ( 'NONE',  ( 2.499999999999998668, -16.33333333333333215, -4.330127018922193649 ) ) ;
#41899 = CARTESIAN_POINT ( 'NONE',  ( 5.000000000000000000, 6.583333333333333037, -2.886751345948129988 ) ) ;
#41900 = CARTESIAN_POINT ( 'NONE',  ( 4.458734124999998549, -57.72916666530107932, -2.574251347313721627 ) ) ;
#41901 = CARTESIAN_POINT ( 'NONE',  ( -5.000000000000000000, -39.99999999999999289, 0.000000000000000000 ) ) ;
#41902 = CARTESIAN_POINT ( 'NONE',  ( -3.535250795749689387E-16, -82.25000000000000000, -5.773502691896257311 ) ) ;
#41903 = CARTESIAN_POINT ( 'NONE',  ( -57.19623071787016499, -135.6250000013655779, 4.297418129356382899 ) ) ;
#41904 = CARTESIAN_POINT ( 'NONE',  ( 6.123233995736766282E-16, -170.0000000000000000, -5.000000000000000000 ) ) ;
#41905 = CARTESIAN_POINT ( 'NONE',  ( -5.000000000000000000, -12.95833333060214798, -2.886751345948128211 ) ) ;
#41906 = CARTESIAN_POINT ( 'NONE',  ( 5.000000000000000888, -109.5833333333333428, 2.886751345948126879 ) ) ;
#41907 = CARTESIAN_POINT ( 'NONE',  ( 5.000000000000000000, -41.49999999999999289, -6.123233995736766282E-16 ) ) ;
#41908 = CARTESIAN_POINT ( 'NONE',  ( 0.000000000000000000, -170.0000000000000000, 0.000000000000000000 ) ) ;
#41911 = CARTESIAN_POINT ( 'NONE',  ( 2.229367062500001939, -18.22916666530106866, 3.861377020970579999 ) ) ;
#41910 =( BOUNDED_CURVE ( )  B_SPLINE_CURVE ( 2, ( #37191, #8236, #57757, #48083, #47770, #27838, #17572, #47460, #23346 ),
 .UNSPECIFIED., .F., .F. ) 
 B_SPLINE_CURVE_WITH_KNOTS ( ( 3, 2, 2, 2, 3 ),
 ( 0.5946428571428571397, 0.5952380952380952328, 0.5964285714285714191, 0.5976190476190476053, 0.5982142857142856984 ),
 .UNSPECIFIED. ) 
 CURVE ( )  GEOMETRIC_REPRESENTATION_ITEM ( )  RATIONAL_B_SPLINE_CURVE ( ( 0.9330127018922194093, 0.9330127018922194093, 1.000000000000000000, 0.8660254037844387076, 1.000000000000000000, 0.8660254037844387076, 1.000000000000000000, 0.9330127018922194093, 0.9330127018922194093 ) ) 
 REPRESENTATION_ITEM ( '' )  );
#41909 = CARTESIAN_POINT ( 'NONE',  ( -58.80597590150559739, -139.0000000000000284, 3.242614290531460330 ) ) ;
#41912 = AXIS2_PLACEMENT_3D ( 'NONE', #22352, #2118, #32303 ) ;
#41913 = DIRECTION ( 'NONE',  ( -0.000000000000000000, 1.000000000000000000, -0.000000000000000000 ) ) ;
#41914 = CARTESIAN_POINT ( 'NONE',  ( -3.152548672688508926E-16, -64.56249999863440792, -5.148502694627439702 ) ) ;
#41915 = CARTESIAN_POINT ( 'NONE',  ( 4.458734124999999437, -153.6875000013656063, 0.000000000000000000 ) ) ;
#41916 = CARTESIAN_POINT ( 'NONE',  ( 4.458734124999998549, -72.72916666530106511, -2.574251347313721627 ) ) ;
#41917 = AXIS2_PLACEMENT_3D ( 'NONE', #60503, #37871, #16745 ) ;
#41918 = CARTESIAN_POINT ( 'NONE',  ( -50.70258187064364108, -146.3750000013655779, 2.196230717870141014 ) ) ;
#41919 = CARTESIAN_POINT ( 'NONE',  ( 4.458734124999998549, -20.97916666530107221, -2.574251347313721627 ) ) ;
#41920 = CARTESIAN_POINT ( 'NONE',  ( 5.000000000000000000, -62.37499999726880873, -6.123233995736766282E-16 ) ) ;
#41921 = ORIENTED_EDGE ( 'NONE', *, *, #17799, .T. ) ;
#41922 = FACE_OUTER_BOUND ( 'NONE', #52758, .T. ) ;
#41923 = ORIENTED_EDGE ( 'NONE', *, *, #51925, .T. ) ;
#41924 = CARTESIAN_POINT ( 'NONE',  ( -2.229367062500000163, -62.72916666530106511, -3.861377020970580443 ) ) ;
#41925 = CARTESIAN_POINT ( 'NONE',  ( 2.499999999999998668, -7.208333330602150646, -4.330127018922193649 ) ) ;
#41926 = CARTESIAN_POINT ( 'NONE',  ( 7.894787914004607998, 1.243647571710251278E-13, -7.591390474663425536 ) ) ;
#41927 = CARTESIAN_POINT ( 'NONE',  ( 2.730187237215162345E-16, -153.1875000013656063, -4.458734124999999437 ) ) ;
#41928 = VERTEX_POINT ( 'NONE', #43335 ) ;
#41929 = CARTESIAN_POINT ( 'NONE',  ( -2.500000000000000444, 26.95833333606451632, -4.330127018922193649 ) ) ;
#41930 = CARTESIAN_POINT ( 'NONE',  ( -59.98410592259440222, -125.1250000000000142, -0.3983568153799752487 ) ) ;
#41931 = CARTESIAN_POINT ( 'NONE',  ( -2.499999999999996447, -55.70833333060214443, 4.330127018922195425 ) ) ;
#41932 = CARTESIAN_POINT ( 'NONE',  ( -4.458734124999999437, -51.64583333196773651, -2.574251347313719407 ) ) ;
#41933 = EDGE_LOOP ( 'NONE', ( #27827, #27245, #40779, #12039 ) ) ;
#41934 = AXIS2_PLACEMENT_3D ( 'NONE', #43285, #49050, #62616 ) ;
#41935 = CYLINDRICAL_SURFACE ( 'NONE', #47069, 5.000000000000000000 ) ;
#41936 = CARTESIAN_POINT ( 'NONE',  ( 4.458734124999998549, 8.270833334698926009, -2.574251347313721627 ) ) ;
#41937 = CARTESIAN_POINT ( 'NONE',  ( 4.458734124999998549, 21.27083333469892779, -2.574251347313721627 ) ) ;
#41938 = CARTESIAN_POINT ( 'NONE',  ( -57.19623071787017210, -147.3750000013656063, 4.297418129356382899 ) ) ;
#41939 = CARTESIAN_POINT ( 'NONE',  ( 2.499999999999998668, -77.33333333333334281, -4.330127018922193649 ) ) ;
#41940 = CARTESIAN_POINT ( 'NONE',  ( -4.458734124999999437, -167.9375000013655779, -5.460374474430324690E-16 ) ) ;
#41941 = VERTEX_POINT ( 'NONE', #58135 ) ;
#41942 = CARTESIAN_POINT ( 'NONE',  ( -3.152548672688508926E-16, -69.56249999863439371, -5.148502694627439702 ) ) ;
#41943 = CARTESIAN_POINT ( 'NONE',  ( 4.458734124999999437, 6.187500001365593860, -5.460374474430324690E-16 ) ) ;
#41944 = DIRECTION ( 'NONE',  ( -0.000000000000000000, 1.000000000000000000, -0.000000000000000000 ) ) ;
#41945 = CARTESIAN_POINT ( 'NONE',  ( -3.152548672688508926E-16, -60.81249999863440081, -5.148502694627439702 ) ) ;
#41946 = CARTESIAN_POINT ( 'NONE',  ( -5.000000000000000000, -16.87499999726881583, 0.000000000000000000 ) ) ;
#41947 = CARTESIAN_POINT ( 'NONE',  ( -1.339745962155610925, -99.79465819873853150, 5.000000000000000000 ) ) ;
#41948 = CARTESIAN_POINT ( 'NONE',  ( -2.500000000000000444, -45.04166666393547303, -4.330127018922193649 ) ) ;
#41949 = CARTESIAN_POINT ( 'NONE',  ( -2.500000000000000444, 18.83333333333333215, -4.330127018922193649 ) ) ;
#41950 = CARTESIAN_POINT ( 'NONE',  ( -3.152548672688508926E-16, -33.56249999863440792, -5.148502694627439702 ) ) ;
#41951 = CARTESIAN_POINT ( 'NONE',  ( 4.458734124999999437, -24.06249999863440436, -5.460374474430324690E-16 ) ) ;
#41952 = VERTEX_POINT ( 'NONE', #52064 ) ;
#41953 =( BOUNDED_CURVE ( )  B_SPLINE_CURVE ( 2, ( #13943, #55895, #18764, #61044, #62545, #3369, #7007, #51387, #57712 ),
 .UNSPECIFIED., .F., .F. ) 
 B_SPLINE_CURVE_WITH_KNOTS ( ( 3, 2, 2, 2, 3 ),
 ( 0.2750000000000002442, 0.2791666666666668961, 0.2833333333333335480, 0.2875000000000001998, 0.2916666666666669072 ),
 .UNSPECIFIED. ) 
 CURVE ( )  GEOMETRIC_REPRESENTATION_ITEM ( )  RATIONAL_B_SPLINE_CURVE ( ( 0.9999999999999958922, 0.9238795325112908463, 1.000000000000000000, 0.9238795325112867385, 1.000000000000000000, 0.9238795325112867385, 1.000000000000000000, 0.9238795325112826307, 1.000000000000003997 ) ) 
 REPRESENTATION_ITEM ( '' )  );
#41954 = CARTESIAN_POINT ( 'NONE',  ( 6.123233995736766282E-16, -170.0000000000000000, -5.000000000000000000 ) ) ;
#41955 = CARTESIAN_POINT ( 'NONE',  ( -2.229367062499996610, -107.1458333319677365, 3.861377020970582219 ) ) ;
#41956 = CARTESIAN_POINT ( 'NONE',  ( 2.071067811865476394, -154.3125000027312410, 5.000000000000000000 ) ) ;
#41957 = EDGE_LOOP ( 'NONE', ( #2601, #8163, #13263, #2766 ) ) ;
#41958 = CARTESIAN_POINT ( 'NONE',  ( 4.458734124999998549, -100.9791666653010509, -2.574251347313721627 ) ) ;
#41959 = ADVANCED_FACE ( 'NONE', ( #38215 ), #57838, .T. ) ;
#41960 = AXIS2_PLACEMENT_3D ( 'NONE', #21683, #61876, #32265 ) ;
#41961 = CARTESIAN_POINT ( 'NONE',  ( -4.458734124999998549, -33.22916666530107221, 2.574251347313722516 ) ) ;
#41962 = CARTESIAN_POINT ( 'NONE',  ( 5.000000000000000888, -62.45833333060214443, 2.886751345948126879 ) ) ;
#41963 = CARTESIAN_POINT ( 'NONE',  ( -50.40829686548195099, -153.2500000013655779, -1.485763867205728284 ) ) ;
#41964 = CARTESIAN_POINT ( 'NONE',  ( 3.061616997868383141E-16, -147.7500000000000284, -5.000000000000000000 ) ) ;
#41965 = CARTESIAN_POINT ( 'NONE',  ( -4.458734124999999437, -31.39583333196773296, -2.574251347313719407 ) ) ;
#41966 = CARTESIAN_POINT ( 'NONE',  ( -4.458734124999997661, -70.47916666530107932, 2.574251347313722516 ) ) ;
#41967 = DIRECTION ( 'NONE',  ( -0.000000000000000000, 1.000000000000000000, -0.000000000000000000 ) ) ;
#41968 = CARTESIAN_POINT ( 'NONE',  ( -4.458734124999997661, -26.22916666530106866, 2.574251347313722516 ) ) ;
#41969 = CARTESIAN_POINT ( 'NONE',  ( 1.339745962155612702, 14.70534180126147916, -5.000000000000000000 ) ) ;
#41970 = CARTESIAN_POINT ( 'NONE',  ( 1.339745962155612702, 18.83034180399265978, -5.000000000000000000 ) ) ;
#41971 = CARTESIAN_POINT ( 'NONE',  ( -5.000000000000000000, -17.00000000000000000, 0.000000000000000000 ) ) ;
#41972 = CARTESIAN_POINT ( 'NONE',  ( -1.846868145590737420, -148.7500000013656063, 4.458734124999999437 ) ) ;
#41973 = EDGE_LOOP ( 'NONE', ( #2457, #7357, #37527, #18991 ) ) ;
#41974 = CARTESIAN_POINT ( 'NONE',  ( -57.46284108482265651, -152.9375000000000000, 4.819101127000238627 ) ) ;
#41975 = CARTESIAN_POINT ( 'NONE',  ( -4.458734124999999437, -52.64583333196773651, -2.574251347313719407 ) ) ;
#41976 = CARTESIAN_POINT ( 'NONE',  ( -2.499999999999996447, -86.70833333060214443, 4.330127018922195425 ) ) ;
#41977 = FACE_OUTER_BOUND ( 'NONE', #44916, .T. ) ;
#41978 = CARTESIAN_POINT ( 'NONE',  ( -3.535250795749689387E-16, 21.75000000000000000, -5.773502691896257311 ) ) ;
#41979 = AXIS2_PLACEMENT_3D ( 'NONE', #60023, #15946, #6307 ) ;
#41980 = DIRECTION ( 'NONE',  ( -0.000000000000000000, 1.000000000000000000, -0.000000000000000000 ) ) ;
#41981 = CARTESIAN_POINT ( 'NONE',  ( 4.458734125000001214, -0.8958333319677401763, 2.574251347313718519 ) ) ;
#41982 = ADVANCED_FACE ( 'NONE', ( #27606 ), #3181, .T. ) ;
#41983 = CARTESIAN_POINT ( 'NONE',  ( 1.975475456537005874E-15, -0.7499999999999996669, 5.000000000000000000 ) ) ;
#41984 = EDGE_CURVE ( 'NONE', #26202, #2867, #16686, .T. ) ;
#41985 = DIRECTION ( 'NONE',  ( 0.000000000000000000, 0.000000000000000000, 1.000000000000000000 ) ) ;
#41986 = DIRECTION ( 'NONE',  ( 0.000000000000000000, 0.000000000000000000, 1.000000000000000000 ) ) ;
#41987 = CARTESIAN_POINT ( 'NONE',  ( -2.229367062499996610, 14.60416666803226171, 3.861377020970582219 ) ) ;
#41988 = CARTESIAN_POINT ( 'NONE',  ( -5.000000000000000000, 3.041666669397851130, -2.886751345948128211 ) ) ;
#41989 = EDGE_LOOP ( 'NONE', ( #53411, #39060, #21664, #25468 ) ) ;
#41990 = CARTESIAN_POINT ( 'NONE',  ( -55.00000000000002132, -135.0000000000000284, 1.734723475976807094E-15 ) ) ;
#41991 = ORIENTED_EDGE ( 'NONE', *, *, #3325, .T. ) ;
#41992 = CARTESIAN_POINT ( 'NONE',  ( -5.000000000000000000, -71.08333333333332860, -2.886751345948128211 ) ) ;
#41993 = CARTESIAN_POINT ( 'NONE',  ( -4.458734124999999437, -48.31249999863440792, 0.000000000000000000 ) ) ;
#41994 = CARTESIAN_POINT ( 'NONE',  ( 1.846868145590735200, -165.5000000013655779, -4.458734125000000326 ) ) ;
#41995 = CARTESIAN_POINT ( 'NONE',  ( 2.500000000000002220, -47.54166666393547303, 4.330127018922192761 ) ) ;
#41996 = ORIENTED_EDGE ( 'NONE', *, *, #2963, .F. ) ;
#41997 = CARTESIAN_POINT ( 'NONE',  ( -4.458734124999999437, -25.31249999863440792, 0.000000000000000000 ) ) ;
#41998 = ORIENTED_EDGE ( 'NONE', *, *, #14576, .T. ) ;
#41999 = CARTESIAN_POINT ( 'NONE',  ( 2.500000000000002220, -86.66666666666667140, 4.330127018922192761 ) ) ;
#42000 = CARTESIAN_POINT ( 'NONE',  ( 1.846868145590736310, -162.6250000013655779, 4.458734124999999437 ) ) ;
#42001 = CARTESIAN_POINT ( 'NONE',  ( -5.000000000000000000, -50.87499999726881583, 0.000000000000000000 ) ) ;
#42002 = CARTESIAN_POINT ( 'NONE',  ( -57.46284108482265651, -135.9375000000000000, 4.819101127000239515 ) ) ;
#42003 = CARTESIAN_POINT ( 'NONE',  ( -4.458734124999999437, -30.64583333196774007, -2.574251347313719407 ) ) ;
#42004 = CARTESIAN_POINT ( 'NONE',  ( -4.999999999999998224, 20.20833333606451987, 2.886751345948131764 ) ) ;
#42005 = ORIENTED_EDGE ( 'NONE', *, *, #44419, .T. ) ;
#42006 = ADVANCED_FACE ( 'NONE', ( #48790 ), #59091, .T. ) ;
#42007 = CARTESIAN_POINT ( 'NONE',  ( 9.457646018065525792E-16, -81.06249999863440792, 5.148502694627439702 ) ) ;
#42008 = CARTESIAN_POINT ( 'NONE',  ( 2.229367062499998831, 24.35416666803225993, -3.861377020970580887 ) ) ;
#42009 = CARTESIAN_POINT ( 'NONE',  ( -6.972266317189433020E-16, -59.25000000000000000, -5.000000000000000000 ) ) ;
#42010 = ORIENTED_EDGE ( 'NONE', *, *, #8635, .T. ) ;
#42011 = CARTESIAN_POINT ( 'NONE',  ( -1.339745962155610925, -59.66965819600732601, 5.000000000000000000 ) ) ;
#42012 = CARTESIAN_POINT ( 'NONE',  ( -52.10840900171896806, -140.4375000013656063, 3.393966926194110556 ) ) ;
#42013 = CARTESIAN_POINT ( 'NONE',  ( 4.458734124999999437, -80.06249999863440792, -5.460374474430324690E-16 ) ) ;
#42014 = CARTESIAN_POINT ( 'NONE',  ( -51.19402409849444524, -132.6250000027312126, -3.242614290531456334 ) ) ;
#42015 = CARTESIAN_POINT ( 'NONE',  ( 2.500000000000002220, -27.66666666666666430, 4.330127018922192761 ) ) ;
#42016 = CARTESIAN_POINT ( 'NONE',  ( 1.975475456537005874E-15, -82.74999999999998579, 5.000000000000000000 ) ) ;
#42017 = LINE ( 'NONE', #47173, #63060 ) ;
#42018 = CARTESIAN_POINT ( 'NONE',  ( 2.229367062500001939, -52.97916666530107221, 3.861377020970579999 ) ) ;
#42019 = LINE ( 'NONE', #37837, #5837 ) ;
#42020 = CARTESIAN_POINT ( 'NONE',  ( -4.458734124999999437, 27.68750000136559208, 0.000000000000000000 ) ) ;
#42021 = AXIS2_PLACEMENT_3D ( 'NONE', #19732, #34855, #1098 ) ;
#42022 = CARTESIAN_POINT ( 'NONE',  ( -4.999999999999999112, -104.9166666666666572, 2.886751345948131764 ) ) ;
#42023 = CARTESIAN_POINT ( 'NONE',  ( 5.000000000000000000, -154.1875000027312126, 2.071067811865478614 ) ) ;
#42024 = CARTESIAN_POINT ( 'NONE',  ( -3.152548672688508926E-16, -38.81249999863440081, -5.148502694627439702 ) ) ;
#42025 = CARTESIAN_POINT ( 'NONE',  ( -5.000000000000000000, 1.125000002731184390, 0.000000000000000000 ) ) ;
#42026 = DIRECTION ( 'NONE',  ( -0.000000000000000000, 1.000000000000000000, -0.000000000000000000 ) ) ;
#42027 = FACE_OUTER_BOUND ( 'NONE', #4273, .T. ) ;
#42028 = CARTESIAN_POINT ( 'NONE',  ( -2.229367062500000163, -76.72916666530106511, -3.861377020970580443 ) ) ;
#42029 = CARTESIAN_POINT ( 'NONE',  ( -4.458734124999999437, -102.3958333319677365, -2.574251347313719407 ) ) ;
#42030 = CARTESIAN_POINT ( 'NONE',  ( 4.458734124999998549, -4.979166665301071326, -2.574251347313721627 ) ) ;
#42031 = VERTEX_POINT ( 'NONE', #49749 ) ;
#42032 = CARTESIAN_POINT ( 'NONE',  ( 4.458734124999998549, -94.72916666530106511, -2.574251347313721627 ) ) ;
#42033 = CARTESIAN_POINT ( 'NONE',  ( -5.000000000000000000, -163.6250000027311842, -6.123233995736766282E-16 ) ) ;
#42034 = CARTESIAN_POINT ( 'NONE',  ( 4.458734124999998549, -88.97916666530107932, -2.574251347313721627 ) ) ;
#42035 = EDGE_CURVE ( 'NONE', #6571, #59835, #244, .T. ) ;
#42036 = CARTESIAN_POINT ( 'NONE',  ( 2.229367062499998831, 12.10416666803226171, -3.861377020970580887 ) ) ;
#42037 = CARTESIAN_POINT ( 'NONE',  ( 2.499999999999998668, -2.208333330602146205, -4.330127018922193649 ) ) ;
#42038 =( BOUNDED_CURVE ( )  B_SPLINE_CURVE ( 2, ( #47016, #61819, #27076, #37361, #3281, #2966, #60865, #46693, #2640 ),
 .UNSPECIFIED., .F., .F. ) 
 B_SPLINE_CURVE_WITH_KNOTS ( ( 3, 2, 2, 2, 3 ),
 ( 0.1750000000000001554, 0.1791666666666668351, 0.1833333333333334869, 0.1875000000000001665, 0.1916666666666668462 ),
 .UNSPECIFIED. ) 
 CURVE ( )  GEOMETRIC_REPRESENTATION_ITEM ( )  RATIONAL_B_SPLINE_CURVE ( ( 0.9999999999999970024, 0.9238795325112897361, 1.000000000000000000, 0.9238795325112867385, 1.000000000000000000, 0.9238795325112867385, 1.000000000000000000, 0.9238795325112837409, 1.000000000000003109 ) ) 
 REPRESENTATION_ITEM ( '' )  );
#42039 = CARTESIAN_POINT ( 'NONE',  ( -57.19623071787017210, -134.3750000013656347, 4.297418129356382899 ) ) ;
#42040 = CARTESIAN_POINT ( 'NONE',  ( -4.458734124999999437, -11.31249999863440792, 0.000000000000000000 ) ) ;
#42041 = CARTESIAN_POINT ( 'NONE',  ( 2.229367062499998831, 18.10416666803225993, -3.861377020970580887 ) ) ;
#42042 = CARTESIAN_POINT ( 'NONE',  ( -2.229367062499996610, -53.39583333196773651, 3.861377020970582219 ) ) ;
#42043 = CARTESIAN_POINT ( 'NONE',  ( -1.339745962155625802, 17.33034180399266688, 4.999999999999991118 ) ) ;
#42044 = CARTESIAN_POINT ( 'NONE',  ( -1.339745962155610925, -21.66965819600733312, 5.000000000000000000 ) ) ;
#42045 = CARTESIAN_POINT ( 'NONE',  ( -2.229367062499996610, -9.145833331967736513, 3.861377020970582219 ) ) ;
#42046 = ORIENTED_EDGE ( 'NONE', *, *, #63292, .T. ) ;
#42047 = CARTESIAN_POINT ( 'NONE',  ( 2.229367062499998831, -34.89583333196772941, -3.861377020970580887 ) ) ;
#42048 = CARTESIAN_POINT ( 'NONE',  ( -50.40829686548195099, -129.2500000013656347, -1.485763867205728284 ) ) ;
#42049 = CARTESIAN_POINT ( 'NONE',  ( 3.044556291839386294E-14, 11.87500000273118417, -5.000000000000000000 ) ) ;
#42050 = EDGE_CURVE ( 'NONE', #62343, #47452, #49543, .T. ) ;
#42051 = CARTESIAN_POINT ( 'NONE',  ( 2.229367062499998831, -78.64583333196773651, -3.861377020970580887 ) ) ;
#42052 = CARTESIAN_POINT ( 'NONE',  ( -4.458734124999999437, 22.43750000136559564, 0.000000000000000000 ) ) ;
#42053 = CARTESIAN_POINT ( 'NONE',  ( -8.190561711645485556E-16, -150.9375000013656063, 4.458734124999999437 ) ) ;
#42054 = CARTESIAN_POINT ( 'NONE',  ( -4.458734124999998549, 15.77083333469892601, 2.574251347313722516 ) ) ;
#42055 = CARTESIAN_POINT ( 'NONE',  ( 2.500000000000002220, -53.66666666666667140, 4.330127018922192761 ) ) ;
#42056 = ADVANCED_FACE ( 'NONE', ( #49431 ), #40092, .T. ) ;
#42057 = DIRECTION ( 'NONE',  ( -0.000000000000000000, 1.000000000000000000, -0.000000000000000000 ) ) ;
#42058 = CARTESIAN_POINT ( 'NONE',  ( 2.229367062500001939, -85.22916666530107932, 3.861377020970579999 ) ) ;
#42059 = CARTESIAN_POINT ( 'NONE',  ( 2.499999999999998668, -62.33333333333333570, -4.330127018922193649 ) ) ;
#42060 = DIRECTION ( 'NONE',  ( -0.000000000000000000, 1.000000000000000000, -0.000000000000000000 ) ) ;
#42061 = CARTESIAN_POINT ( 'NONE',  ( 5.000000000000000888, 21.54166666939785202, 2.886751345948126879 ) ) ;
#42062 = EDGE_LOOP ( 'NONE', ( #9241, #57788, #3662, #46044 ) ) ;
#42063 = CARTESIAN_POINT ( 'NONE',  ( 5.000000000000000000, -35.50000000000000711, -6.123233995736766282E-16 ) ) ;
#42064 = EDGE_CURVE ( 'NONE', #28458, #63093, #38818, .T. ) ;
#42065 = CARTESIAN_POINT ( 'NONE',  ( 7.204675194429079505E-15, 27.74999999999999645, -5.000000000000000000 ) ) ;
#42067 = CARTESIAN_POINT ( 'NONE',  ( 5.000000000000000000, -29.41666666666666785, -2.886751345948129988 ) ) ;
#42066 = CYLINDRICAL_SURFACE ( 'NONE', #47074, 5.000000000000000000 ) ;
#42068 = CARTESIAN_POINT ( 'NONE',  ( -4.458734124999999437, -30.39583333196773651, -2.574251347313719407 ) ) ;
#42069 = DIRECTION ( 'NONE',  ( 0.000000000000000000, 0.000000000000000000, 1.000000000000000000 ) ) ;
#42070 = CARTESIAN_POINT ( 'NONE',  ( 5.000000000000000888, -26.45833333060214443, 2.886751345948126879 ) ) ;
#42072 = VERTEX_POINT ( 'NONE', #30442 ) ;
#42071 = CARTESIAN_POINT ( 'NONE',  ( -4.458734124999998549, -60.22916666530106511, 2.574251347313722516 ) ) ;
#42073 = CARTESIAN_POINT ( 'NONE',  ( -57.19623071787017210, -153.6250000013655779, 4.297418129356382899 ) ) ;
#42075 = ORIENTED_EDGE ( 'NONE', *, *, #2339, .F. ) ;
#42074 = CARTESIAN_POINT ( 'NONE',  ( -2.229367062499996610, -10.39583333196773829, 3.861377020970582219 ) ) ;
#42076 = CARTESIAN_POINT ( 'NONE',  ( 1.060575238724906964E-15, -70.74999999999998579, 5.773502691896257311 ) ) ;
#42077 = CARTESIAN_POINT ( 'NONE',  ( -59.44456063193725015, -137.5625000013656063, -0.3552334253322034230 ) ) ;
#42078 = CARTESIAN_POINT ( 'NONE',  ( -2.229367062500000163, -53.72916666530107221, -3.861377020970580443 ) ) ;
#42079 = CARTESIAN_POINT ( 'NONE',  ( -5.000000000000000000, -76.95833333060214443, -2.886751345948128211 ) ) ;
#42081 = ORIENTED_EDGE ( 'NONE', *, *, #9423, .F. ) ;
#42080 = CARTESIAN_POINT ( 'NONE',  ( -2.500000000000000444, -55.04166666393548013, -4.330127018922193649 ) ) ;
#42082 = CARTESIAN_POINT ( 'NONE',  ( -57.46284108482265651, -149.9375000000000284, 4.819101127000239515 ) ) ;
#42083 = ADVANCED_FACE ( 'NONE', ( #34632 ), #10198, .T. ) ;
#42084 = CARTESIAN_POINT ( 'NONE',  ( -4.458734124999999437, -15.64583333196773474, -2.574251347313719407 ) ) ;
#42085 = CARTESIAN_POINT ( 'NONE',  ( -2.229367062500000163, -57.72916666530107932, -3.861377020970580443 ) ) ;
#42086 = CARTESIAN_POINT ( 'NONE',  ( -2.499999999999996447, -23.83333333333333215, 4.330127018922195425 ) ) ;
#42087 = CARTESIAN_POINT ( 'NONE',  ( -4.458734124999999437, -139.9375000013656063, -5.460374474430324690E-16 ) ) ;
#42088 = CARTESIAN_POINT ( 'NONE',  ( 2.229367062500001939, -101.2291666653010651, 3.861377020970579999 ) ) ;
#42089 = LINE ( 'NONE', #57224, #33785 ) ;
#42090 = ORIENTED_EDGE ( 'NONE', *, *, #25404, .F. ) ;
#42091 = CARTESIAN_POINT ( 'NONE',  ( 3.061616997868383141E-16, -166.7500000000000000, -5.000000000000000000 ) ) ;
#42092 = CARTESIAN_POINT ( 'NONE',  ( -58.24261429053147765, -141.3750000027312126, -3.805975901505573855 ) ) ;
#42093 = VECTOR ( 'NONE', #20788, 1000.000000000000000 ) ;
#42094 = CARTESIAN_POINT ( 'NONE',  ( -4.458734124999998549, -8.229166665301073991, 2.574251347313722516 ) ) ;
#42095 = CARTESIAN_POINT ( 'NONE',  ( -2.229367062499996610, -95.39583333196773651, 3.861377020970582219 ) ) ;
#42096 = CARTESIAN_POINT ( 'NONE',  ( -8.190561711645485556E-16, -147.9375000013656063, 4.458734124999999437 ) ) ;
#42097 = CARTESIAN_POINT ( 'NONE',  ( -2.229367062499996610, -22.39583333196773651, 3.861377020970582219 ) ) ;
#42098 = CARTESIAN_POINT ( 'NONE',  ( -52.10840900171896806, -138.1875000013656347, 3.393966926194110556 ) ) ;
#42099 = CARTESIAN_POINT ( 'NONE',  ( 2.229367062499998831, -61.89583333196774362, -3.861377020970580887 ) ) ;
#42100 = CARTESIAN_POINT ( 'NONE',  ( 1.975475456537005874E-15, -22.74999999999999645, 5.000000000000000000 ) ) ;
#42101 = CARTESIAN_POINT ( 'NONE',  ( -1.339745962155613812, -43.08034179853029144, -5.000000000000000000 ) ) ;
#42102 = CARTESIAN_POINT ( 'NONE',  ( -4.458734124999999437, -144.9375000013656063, -5.460374474430324690E-16 ) ) ;
#42103 = CARTESIAN_POINT ( 'NONE',  ( 4.458734125000000326, 12.85416666803226171, 2.574251347313718519 ) ) ;
#42104 =( BOUNDED_CURVE ( )  B_SPLINE_CURVE ( 2, ( #52344, #27882, #23068, #8898, #42673, #14348, #33970, #62312, #4385 ),
 .UNSPECIFIED., .F., .F. ) 
 B_SPLINE_CURVE_WITH_KNOTS ( ( 3, 2, 2, 2, 3 ),
 ( 0.4145833333333333592, 0.4152777777777778012, 0.4166666666666666852, 0.4180555555555555691, 0.4187500000000000111 ),
 .UNSPECIFIED. ) 
 CURVE ( )  GEOMETRIC_REPRESENTATION_ITEM ( )  RATIONAL_B_SPLINE_CURVE ( ( 0.9330127018922194093, 0.9330127018922220739, 1.000000000000000000, 0.8660254037844387076, 1.000000000000000000, 0.8660254037844387076, 1.000000000000000000, 0.9330127018922194093, 0.9330127018922194093 ) ) 
 REPRESENTATION_ITEM ( '' )  );
#42105 = ORIENTED_EDGE ( 'NONE', *, *, #38170, .F. ) ;
#42106 = CARTESIAN_POINT ( 'NONE',  ( -5.000000000000000000, -81.08333333333332860, -2.886751345948128211 ) ) ;
#42107 = FACE_OUTER_BOUND ( 'NONE', #55599, .T. ) ;
#42109 = CARTESIAN_POINT ( 'NONE',  ( 4.458734125000001214, -24.89583333196773651, 2.574251347313718519 ) ) ;
#42108 = CARTESIAN_POINT ( 'NONE',  ( 5.000000000000000000, -91.41666666666665719, -2.886751345948129988 ) ) ;
#42110 = CARTESIAN_POINT ( 'NONE',  ( 2.500000000000002220, 4.458333336064518093, 4.330127018922192761 ) ) ;
#42111 = CARTESIAN_POINT ( 'NONE',  ( -2.229367062500000163, -71.72916666530107932, -3.861377020970580443 ) ) ;
#42112 = CARTESIAN_POINT ( 'NONE',  ( 2.229367062499998831, 29.10416666803225993, -3.861377020970580887 ) ) ;
#42113 = FACE_OUTER_BOUND ( 'NONE', #45480, .T. ) ;
#42114 = CARTESIAN_POINT ( 'NONE',  ( -58.39396692619412477, -146.4375000013656063, 2.891590998281057701 ) ) ;
#42115 = EDGE_CURVE ( 'NONE', #45853, #40725, #11780, .T. ) ;
#42116 = EDGE_CURVE ( 'NONE', #18888, #49819, #56139, .T. ) ;
#42117 = CARTESIAN_POINT ( 'NONE',  ( -2.229367062499996610, 8.854166668032261711, 3.861377020970582219 ) ) ;
#42118 = CARTESIAN_POINT ( 'NONE',  ( -6.972266317189433020E-16, -63.12499999726880162, -5.000000000000000000 ) ) ;
#42120 = EDGE_CURVE ( 'NONE', #50022, #48710, #27236, .T. ) ;
#42119 = CARTESIAN_POINT ( 'NONE',  ( 0.000000000000000000, -120.0000000000000000, 0.000000000000000000 ) ) ;
#42121 = CARTESIAN_POINT ( 'NONE',  ( -2.229367062499996610, 8.854166668032261711, 3.861377020970582219 ) ) ;
#42122 = CARTESIAN_POINT ( 'NONE',  ( 4.458734124999998549, -71.72916666530107932, -2.574251347313721627 ) ) ;
#42123 = CARTESIAN_POINT ( 'NONE',  ( 4.458734124999998549, -19.97916666530107221, -2.574251347313721627 ) ) ;
#42124 = CARTESIAN_POINT ( 'NONE',  ( -3.535250795749689387E-16, -2.250000000000001776, -5.773502691896257311 ) ) ;
#42125 = CARTESIAN_POINT ( 'NONE',  ( 3.152801135295367541, -158.3125000013656063, -3.152801135295367541 ) ) ;
#42126 = CARTESIAN_POINT ( 'NONE',  ( -2.500000000000000444, 28.95833333606451987, -4.330127018922193649 ) ) ;
#42127 = CARTESIAN_POINT ( 'NONE',  ( 4.458734124999998549, -64.72916666530106511, -2.574251347313721627 ) ) ;
#42128 = CARTESIAN_POINT ( 'NONE',  ( 5.000000000000000888, -99.45833333060213022, 2.886751345948126879 ) ) ;
#42129 = EDGE_CURVE ( 'NONE', #2367, #24664, #21191, .T. ) ;
#42130 = CARTESIAN_POINT ( 'NONE',  ( 5.000000000000000000, -41.41666666666667140, -2.886751345948130876 ) ) ;
#42131 = CARTESIAN_POINT ( 'NONE',  ( 2.229367062500001939, -40.97916666530107221, 3.861377020970579999 ) ) ;
#42132 = ADVANCED_FACE ( 'NONE', ( #16614 ), #50707, .T. ) ;
#42133 = CARTESIAN_POINT ( 'NONE',  ( 9.457646018065525792E-16, -107.3124999986343937, 5.148502694627439702 ) ) ;
#42134 = CARTESIAN_POINT ( 'NONE',  ( -4.458734124999997661, -66.47916666530106511, 2.574251347313722516 ) ) ;
#42135 = CARTESIAN_POINT ( 'NONE',  ( 2.499999999999998668, -47.33333333333333570, -4.330127018922193649 ) ) ;
#42136 = CARTESIAN_POINT ( 'NONE',  ( -2.500000000000000444, -23.16666666666666785, -4.330127018922193649 ) ) ;
#42137 = EDGE_CURVE ( 'NONE', #11132, #41205, #2163, .T. ) ;
#42138 = CARTESIAN_POINT ( 'NONE',  ( -2.499999999999996447, 16.16666666666666430, 4.330127018922195425 ) ) ;
#42139 = ORIENTED_EDGE ( 'NONE', *, *, #37737, .F. ) ;
#42140 = CARTESIAN_POINT ( 'NONE',  ( -2.498395430326213474E-14, 15.37500000273118239, 5.000000000000000000 ) ) ;
#42141 = VECTOR ( 'NONE', #52879, 1000.000000000000000 ) ;
#42142 =( BOUNDED_CURVE ( )  B_SPLINE_CURVE ( 2, ( #12287, #12598, #50572, #2968, #21938, #22261, #6515, #16793, #16156 ),
 .UNSPECIFIED., .F., .F. ) 
 B_SPLINE_CURVE_WITH_KNOTS ( ( 3, 2, 2, 2, 3 ),
 ( 0.8812499999999999778, 0.8819444444444444198, 0.8833333333333333037, 0.8847222222222221877, 0.8854166666666666297 ),
 .UNSPECIFIED. ) 
 CURVE ( )  GEOMETRIC_REPRESENTATION_ITEM ( )  RATIONAL_B_SPLINE_CURVE ( ( 0.9330127018922194093, 0.9330127018922194093, 1.000000000000000000, 0.8660254037844387076, 1.000000000000000000, 0.8660254037844387076, 1.000000000000000000, 0.9330127018922194093, 0.9330127018922194093 ) ) 
 REPRESENTATION_ITEM ( '' )  );
#42143 = CARTESIAN_POINT ( 'NONE',  ( 3.535533905932738197, -144.0000000027311842, -3.535533905932738197 ) ) ;
#42144 = CARTESIAN_POINT ( 'NONE',  ( -4.999999999999999112, -7.916666666666668739, 2.886751345948131764 ) ) ;
#42145 = EDGE_CURVE ( 'NONE', #63665, #19571, #56178, .T. ) ;
#42146 = VECTOR ( 'NONE', #21653, 1000.000000000000000 ) ;
#42147 = CARTESIAN_POINT ( 'NONE',  ( -4.458734124999999437, -70.31249999863439371, 0.000000000000000000 ) ) ;
#42148 = CARTESIAN_POINT ( 'NONE',  ( -6.972266317189433020E-16, -6.249999999999999112, -5.000000000000000000 ) ) ;
#42149 = CARTESIAN_POINT ( 'NONE',  ( -2.500000000000000444, -14.04166666393548013, -4.330127018922193649 ) ) ;
#42151 = VERTEX_POINT ( 'NONE', #60376 ) ;
#42150 = CARTESIAN_POINT ( 'NONE',  ( 2.229367062500001939, -43.97916666530106511, 3.861377020970579999 ) ) ;
#42152 = CARTESIAN_POINT ( 'NONE',  ( 5.000000000000000000, -81.50000000000000000, -6.123233995736766282E-16 ) ) ;
#42154 = ORIENTED_EDGE ( 'NONE', *, *, #58181, .T. ) ;
#42153 = CARTESIAN_POINT ( 'NONE',  ( 4.458734125000001214, 5.854166668032262599, 2.574251347313718519 ) ) ;
#42155 = CARTESIAN_POINT ( 'NONE',  ( 1.339745962155615144, -81.70534180126146850, 4.999999999999999112 ) ) ;
#42156 = CARTESIAN_POINT ( 'NONE',  ( -2.499999999999996447, -53.83333333333332860, 4.330127018922195425 ) ) ;
#42157 = CARTESIAN_POINT ( 'NONE',  ( -8.190561711645485556E-16, -158.9375000013655779, 4.458734124999999437 ) ) ;
#42158 = CARTESIAN_POINT ( 'NONE',  ( 2.229367062500001939, -34.22916666530107221, 3.861377020970579999 ) ) ;
#42159 = CARTESIAN_POINT ( 'NONE',  ( -5.000000000000000000, -87.00000000000000000, 0.000000000000000000 ) ) ;
#42160 = CARTESIAN_POINT ( 'NONE',  ( -4.458734124999999437, -79.39583333196773651, -2.574251347313719407 ) ) ;
#42161 = CARTESIAN_POINT ( 'NONE',  ( 5.000000000000000000, -167.0000000000000000, 0.000000000000000000 ) ) ;
#42162 = CARTESIAN_POINT ( 'NONE',  ( 4.458734124999998549, -89.72916666530106511, -2.574251347313721627 ) ) ;
#42163 = CARTESIAN_POINT ( 'NONE',  ( -58.39396692619412477, -131.6875000013656063, 2.891590998281057701 ) ) ;
#42164 = CARTESIAN_POINT ( 'NONE',  ( 4.458734124999998549, -1.979166665301068662, -2.574251347313721627 ) ) ;
#42165 = CARTESIAN_POINT ( 'NONE',  ( -2.229367062499996610, -38.39583333196773651, 3.861377020970582219 ) ) ;
#42166 = CARTESIAN_POINT ( 'NONE',  ( 1.975475456537005874E-15, -16.62499999726881583, 5.000000000000000000 ) ) ;
#42167 = CARTESIAN_POINT ( 'NONE',  ( 4.458734124999999437, -82.06249999863440792, -5.460374474430324690E-16 ) ) ;
#42168 = CARTESIAN_POINT ( 'NONE',  ( -6.250000000000000888, 5.051814855409225480, -7.198902722707429369 ) ) ;
#42169 = ORIENTED_EDGE ( 'NONE', *, *, #7496, .T. ) ;
#42170 = CARTESIAN_POINT ( 'NONE',  ( -5.000000000000000000, -148.6250000027312126, -6.123233995736766282E-16 ) ) ;
#42171 = CARTESIAN_POINT ( 'NONE',  ( 0.000000000000000000, -170.0000000000000000, 5.000000000000000000 ) ) ;
#42172 = CARTESIAN_POINT ( 'NONE',  ( 4.458734125000001214, -68.14583333196773651, 2.574251347313718519 ) ) ;
#42173 = CARTESIAN_POINT ( 'NONE',  ( 4.458734125000000326, -40.89583333196773651, 2.574251347313718519 ) ) ;
#42174 = CARTESIAN_POINT ( 'NONE',  ( -4.458734124999999437, -9.645833331967738289, -2.574251347313719407 ) ) ;
#42175 = EDGE_LOOP ( 'NONE', ( #43320, #46211, #5405, #56668, #42781, #26911, #51901, #22510, #27321, #23039, #39864, #59335, #13051, #27910, #407, #50137, #60207, #49443, #62821, #62756, #16555, #23232, #28397, #56506, #53292, #32402, #58450, #42978, #50251, #46793, #18957, #15053, #50018, #21596, #14764, #44132, #9940, #48821, #35233, #41539, #40972, #1479, #45064, #42305, #47535, #15001, #50953, #14122, #51128, #55323, #41351, #1614, #53790, #27919, #9926, #28855, #20007, #44272, #35923, #56749, #45018, #62584, #57998, #60377, #21432, #58689, #17549, #33301, #22449, #6233, #6264, #26114, #6311, #48716, #30177, #52929, #30427, #44918, #12601, #44195, #62455, #52865, #43330, #61176, #50859, #33748, #40267, #33918, #32643, #27214, #40277, #48082, #6828, #21690, #21453, #3595, #48178, #62166, #39522, #2365, #6806, #51424, #27480, #28237, #289, #7671, #58930, #46444, #45779, #53468, #7534, #44262, #37119, #5586, #29276, #61433, #62446, #29810, #37093, #54577, #36880, #40013, #50986, #51202, #24891, #27139, #5943, #44492, #46522, #62101, #35817, #37809, #34638, #26158, #32104, #27172, #32660, #41108, #50772, #40208, #47857, #22648, #1515, #44668, #708, #49219, #19851, #63112, #45249, #15169, #28531, #16724, #7776, #53928, #13994, #26124, #10539, #2088, #58527, #19128, #36083, #57556, #39130, #63530, #61805, #63436, #17579, #27297, #21404, #20265, #9238, #36767, #48254, #52964, #13527, #18820, #58898, #48651, #60703, #40655, #33380, #26630, #42046, #18205, #56778, #53654, #49024, #41596, #56208, #4828, #16925, #41722, #49189, #63303, #58603, #40581, #15040, #7343, #44097, #29013, #40881, #11779, #11130, #49416, #24706, #37268, #54095, #48159, #3936, #12989, #48484, #60650, #54174, #38576, #20474, #17819, #59910, #18486, #49720, #35464, #23960, #35779, #39766, #49996, #34880, #52913, #9813, #36534, #52333, #27599, #17714, #5506, #53470, #15255, #37850, #15722, #46388, #3350, #36080, #17342, #28844, #55831, #45215, #4585 ) ) ;
#42176 = CARTESIAN_POINT ( 'NONE',  ( 1.339745962155612702, -5.294658198738519950, -5.000000000000000000 ) ) ;
#42177 = CARTESIAN_POINT ( 'NONE',  ( 1.339745962155612702, 2.830341803992664662, -5.000000000000000000 ) ) ;
#42178 = CARTESIAN_POINT ( 'NONE',  ( 2.229367062500001939, -4.229166665301070438, 3.861377020970579999 ) ) ;
#42179 = DIRECTION ( 'NONE',  ( -0.000000000000000000, 1.000000000000000000, -0.000000000000000000 ) ) ;
#42180 = CARTESIAN_POINT ( 'NONE',  ( -2.229367062499996610, 2.854166668032259935, 3.861377020970582219 ) ) ;
#42181 = VECTOR ( 'NONE', #9522, 1000.000000000000000 ) ;
#42182 = CARTESIAN_POINT ( 'NONE',  ( -2.499999999999996447, -95.70833333060213022, 4.330127018922195425 ) ) ;
#42183 = CARTESIAN_POINT ( 'NONE',  ( 3.152801135295366208, -156.5625000013656063, 3.152801135295367985 ) ) ;
#42184 = CARTESIAN_POINT ( 'NONE',  ( -4.458734124999999437, 26.35416666803225993, -2.574251347313719407 ) ) ;
#42185 = ORIENTED_EDGE ( 'NONE', *, *, #22536, .F. ) ;
#42186 = CARTESIAN_POINT ( 'NONE',  ( 9.457646018065525792E-16, -84.06249999863439371, 5.148502694627439702 ) ) ;
#42187 = DIRECTION ( 'NONE',  ( -0.000000000000000000, 1.000000000000000000, -0.000000000000000000 ) ) ;
#42188 = CARTESIAN_POINT ( 'NONE',  ( 9.457646018065525792E-16, -11.06249999863440969, 5.148502694627439702 ) ) ;
#42189 = CARTESIAN_POINT ( 'NONE',  ( -6.972266317189433020E-16, 19.75000000000000000, -5.000000000000000000 ) ) ;
#42190 = CARTESIAN_POINT ( 'NONE',  ( 1.339745962155612702, -48.29465819873851729, -5.000000000000000000 ) ) ;
#42191 = CARTESIAN_POINT ( 'NONE',  ( 1.975475456537005874E-15, -67.74999999999998579, 5.000000000000000000 ) ) ;
#42192 = CARTESIAN_POINT ( 'NONE',  ( -5.000000000000000000, -33.95833333060213732, -2.886751345948128211 ) ) ;
#42193 = FACE_OUTER_BOUND ( 'NONE', #58032, .T. ) ;
#42194 = CARTESIAN_POINT ( 'NONE',  ( 4.458734124999999437, 24.18750000136559564, -5.460374474430324690E-16 ) ) ;
#42195 = CARTESIAN_POINT ( 'NONE',  ( 1.062108568985190270E-13, -10.25000000000000355, -4.999999999999999112 ) ) ;
#42196 = CARTESIAN_POINT ( 'NONE',  ( 4.458734125000000326, 21.10416666803226704, 2.574251347313718519 ) ) ;
#42197 = CARTESIAN_POINT ( 'NONE',  ( -4.458734124999999437, -59.31249999863440081, 0.000000000000000000 ) ) ;
#42198 = CARTESIAN_POINT ( 'NONE',  ( -2.229367062500000163, -5.729166665301072214, -3.861377020970580443 ) ) ;
#42199 = CARTESIAN_POINT ( 'NONE',  ( 1.975475456537005874E-15, -62.74999999999998579, 5.000000000000000000 ) ) ;
#42200 = CARTESIAN_POINT ( 'NONE',  ( 1.060575238724906964E-15, 17.25000000000000000, 5.773502691896257311 ) ) ;
#42201 = CARTESIAN_POINT ( 'NONE',  ( 5.000000000000000000, -140.1875000027311842, 2.071067811865478614 ) ) ;
#42202 = CARTESIAN_POINT ( 'NONE',  ( -2.500000000000000444, -46.16666666666666430, -4.330127018922193649 ) ) ;
#42203 = CARTESIAN_POINT ( 'NONE',  ( 4.458734125000001214, -47.89583333196775072, 2.574251347313718519 ) ) ;
#42204 = CARTESIAN_POINT ( 'NONE',  ( -5.000000000000000000, -84.87499999726880162, 0.000000000000000000 ) ) ;
#42205 = CARTESIAN_POINT ( 'NONE',  ( -53.51423613279429503, -137.5000000013656063, 4.591703134518082763 ) ) ;
#42206 = CARTESIAN_POINT ( 'NONE',  ( 6.123233995736766282E-16, -120.0000000000000000, -5.000000000000000000 ) ) ;
#42207 = CARTESIAN_POINT ( 'NONE',  ( 9.457646018065525792E-16, -87.31249999863440792, 5.148502694627439702 ) ) ;
#42208 = CARTESIAN_POINT ( 'NONE',  ( -1.846868145590737420, -159.0000000013656063, 4.458734124999997661 ) ) ;
#42209 = CARTESIAN_POINT ( 'NONE',  ( 5.000000000000000000, -30.50000000000000000, -6.123233995736766282E-16 ) ) ;
#42210 = CYLINDRICAL_SURFACE ( 'NONE', #11011, 5.000000000000000000 ) ;
#42211 = VERTEX_POINT ( 'NONE', #31392 ) ;
#42212 = EDGE_CURVE ( 'NONE', #17071, #55117, #23260, .T. ) ;
#42213 = CARTESIAN_POINT ( 'NONE',  ( 2.229367062499998831, 20.10416666803225993, -3.861377020970580887 ) ) ;
#42214 = VERTEX_POINT ( 'NONE', #1842 ) ;
#42215 = CARTESIAN_POINT ( 'NONE',  ( -2.229367062499996610, -95.14583333196773651, 3.861377020970582219 ) ) ;
#42216 = CARTESIAN_POINT ( 'NONE',  ( -2.229367062500000163, 16.27083333469892779, -3.861377020970580443 ) ) ;
#42217 = CARTESIAN_POINT ( 'NONE',  ( 5.000000000000000888, 17.54166666939785557, 2.886751345948126879 ) ) ;
#42218 = EDGE_CURVE ( 'NONE', #42312, #2707, #36404, .T. ) ;
#42219 = CARTESIAN_POINT ( 'NONE',  ( -3.535250795749689387E-16, 5.749999999999998224, -5.773502691896257311 ) ) ;
#42220 =( BOUNDED_CURVE ( )  B_SPLINE_CURVE ( 2, ( #34569, #35548, #55173, #6287, #5965, #54530, #60323, #45508, #39713 ),
 .UNSPECIFIED., .F., .F. ) 
 B_SPLINE_CURVE_WITH_KNOTS ( ( 3, 2, 2, 2, 3 ),
 ( 0.9910714285714286031, 0.9916666666666666963, 0.9928571428571428825, 0.9940476190476190688, 0.9946428571428571619 ),
 .UNSPECIFIED. ) 
 CURVE ( )  GEOMETRIC_REPRESENTATION_ITEM ( )  RATIONAL_B_SPLINE_CURVE ( ( 0.9330127018922194093, 0.9330127018922194093, 1.000000000000000000, 0.8660254037844387076, 1.000000000000000000, 0.8660254037844387076, 1.000000000000000000, 0.9330127018922194093, 0.9330127018922194093 ) ) 
 REPRESENTATION_ITEM ( '' )  );
#42221 = CARTESIAN_POINT ( 'NONE',  ( 4.458734124999999437, -53.81249999863439371, -5.460374474430324690E-16 ) ) ;
#42222 = CYLINDRICAL_SURFACE ( 'NONE', #43143, 5.000000000000000000 ) ;
#42223 = CARTESIAN_POINT ( 'NONE',  ( 5.000000000000000000, -82.50000000000000000, -6.123233995736766282E-16 ) ) ;
#42224 = EDGE_CURVE ( 'NONE', #12246, #44127, #55760, .T. ) ;
#42225 = CARTESIAN_POINT ( 'NONE',  ( -57.89159099828107458, -135.9375000013656063, -3.393966926194107447 ) ) ;
#42226 = CARTESIAN_POINT ( 'NONE',  ( 4.250000000000000000, 0.000000000000000000, -10.00000000000000000 ) ) ;
#42227 = CARTESIAN_POINT ( 'NONE',  ( -2.499999999999996447, -25.70833333060214798, 4.330127018922195425 ) ) ;
#42228 = CARTESIAN_POINT ( 'NONE',  ( -2.499999999999996447, -24.70833333060214443, 4.330127018922195425 ) ) ;
#42229 = CARTESIAN_POINT ( 'NONE',  ( -2.500000000000000444, -37.16666666666666430, -4.330127018922193649 ) ) ;
#42230 = FACE_OUTER_BOUND ( 'NONE', #34893, .T. ) ;
#42232 = CARTESIAN_POINT ( 'NONE',  ( 2.229367062499998831, -21.89583333196774007, -3.861377020970580887 ) ) ;
#42231 = CARTESIAN_POINT ( 'NONE',  ( -6.972266317189433020E-16, -43.25000000000000000, -5.000000000000000000 ) ) ;
#42233 = CARTESIAN_POINT ( 'NONE',  ( -3.535533905932738641, -143.3750000000000000, 3.535533905932737309 ) ) ;
#42234 = CARTESIAN_POINT ( 'NONE',  ( -3.152548672688508926E-16, -62.56249999863440792, -5.148502694627439702 ) ) ;
#42235 = CARTESIAN_POINT ( 'NONE',  ( 3.152801135295367541, -147.5625000013655779, -3.152801135295367541 ) ) ;
#42236 = VECTOR ( 'NONE', #18216, 1000.000000000000000 ) ;
#42237 = CARTESIAN_POINT ( 'NONE',  ( 4.458734125000001214, -69.89583333196773651, 2.574251347313718519 ) ) ;
#42238 = CARTESIAN_POINT ( 'NONE',  ( -59.44456063193725015, -144.8125000013656063, -0.3552334253322034230 ) ) ;
#42239 = CARTESIAN_POINT ( 'NONE',  ( -2.229367062500000163, -17.72916666530106866, -3.861377020970580443 ) ) ;
#42240 =( BOUNDED_CURVE ( )  B_SPLINE_CURVE ( 2, ( #32461, #11885, #62380, #17361, #36661, #7402, #37294, #56923, #47266 ),
 .UNSPECIFIED., .F., .F. ) 
 B_SPLINE_CURVE_WITH_KNOTS ( ( 3, 2, 2, 2, 3 ),
 ( 0.6803571428571428825, 0.6809523809523809756, 0.6821428571428571619, 0.6833333333333333481, 0.6839285714285714413 ),
 .UNSPECIFIED. ) 
 CURVE ( )  GEOMETRIC_REPRESENTATION_ITEM ( )  RATIONAL_B_SPLINE_CURVE ( ( 0.9330127018922194093, 0.9330127018922194093, 1.000000000000000000, 0.8660254037844387076, 1.000000000000000000, 0.8660254037844387076, 1.000000000000000000, 0.9330127018922194093, 0.9330127018922194093 ) ) 
 REPRESENTATION_ITEM ( '' )  );
#42241 = CARTESIAN_POINT ( 'NONE',  ( 2.499999999999998668, -60.20833333060214443, -4.330127018922193649 ) ) ;
#42242 = ORIENTED_EDGE ( 'NONE', *, *, #32238, .T. ) ;
#42243 = CARTESIAN_POINT ( 'NONE',  ( -5.000000000000000888, -150.4375000000000000, 2.071067811865474617 ) ) ;
#42244 = ORIENTED_EDGE ( 'NONE', *, *, #7588, .T. ) ;
#42245 = CARTESIAN_POINT ( 'NONE',  ( -4.458734124999999437, -68.64583333196773651, -2.574251347313719407 ) ) ;
#42246 = DIRECTION ( 'NONE',  ( -0.000000000000000000, 1.000000000000000000, -0.000000000000000000 ) ) ;
#42247 = DIRECTION ( 'NONE',  ( -0.000000000000000000, 1.000000000000000000, -0.000000000000000000 ) ) ;
#42248 = VERTEX_POINT ( 'NONE', #6650 ) ;
#42249 = CARTESIAN_POINT ( 'NONE',  ( -53.33387254593728954, -151.8125000000000284, 5.149110718188522284 ) ) ;
#42250 = CARTESIAN_POINT ( 'NONE',  ( -57.46284108482265651, -125.9375000000000568, 4.819101127000239515 ) ) ;
#42251 = CYLINDRICAL_SURFACE ( 'NONE', #38075, 5.000000000000000000 ) ;
#42252 = CARTESIAN_POINT ( 'NONE',  ( -4.458734124999999437, -53.64583333196772941, -2.574251347313719407 ) ) ;
#42253 = ORIENTED_EDGE ( 'NONE', *, *, #46518, .T. ) ;
#42254 = CARTESIAN_POINT ( 'NONE',  ( 2.499999999999998668, -45.33333333333333570, -4.330127018922193649 ) ) ;
#42255 = CARTESIAN_POINT ( 'NONE',  ( -2.229367062500000163, 8.520833334698926009, -3.861377020970580443 ) ) ;
#42256 = CARTESIAN_POINT ( 'NONE',  ( 9.457646018065525792E-16, 19.93750000136559208, 5.148502694627439702 ) ) ;
#42257 = CARTESIAN_POINT ( 'NONE',  ( -58.39396692619412477, -150.4375000013656063, 2.891590998281057701 ) ) ;
#42258 = CARTESIAN_POINT ( 'NONE',  ( 1.339745962155661996, -13.16965819600733489, -4.999999999999970690 ) ) ;
#42259 = DIRECTION ( 'NONE',  ( 0.000000000000000000, 0.000000000000000000, 1.000000000000000000 ) ) ;
#42260 = VERTEX_POINT ( 'NONE', #35601 ) ;
#42261 = CARTESIAN_POINT ( 'NONE',  ( 2.229367062500001939, -71.97916666530107932, 3.861377020970579999 ) ) ;
#42262 = CARTESIAN_POINT ( 'NONE',  ( 1.339745962155615144, 14.41965820146970323, 4.999999999999999112 ) ) ;
#42263 = CARTESIAN_POINT ( 'NONE',  ( 4.458734124999998549, 9.270833334698927786, -2.574251347313721627 ) ) ;
#42264 = EDGE_CURVE ( 'NONE', #58314, #483, #36032, .T. ) ;
#42265 = CARTESIAN_POINT ( 'NONE',  ( 3.535533905932736864, -140.2500000027311842, 3.535533905932738641 ) ) ;
#42266 = CARTESIAN_POINT ( 'NONE',  ( -2.229367062499996610, -61.39583333196774362, 3.861377020970582219 ) ) ;
#42267 = CARTESIAN_POINT ( 'NONE',  ( 2.499999999999998668, -21.20833333060214798, -4.330127018922193649 ) ) ;
#42268 = CARTESIAN_POINT ( 'NONE',  ( -2.499999999999996447, -18.83333333333333215, 4.330127018922195425 ) ) ;
#42269 = CARTESIAN_POINT ( 'NONE',  ( 3.061616997868383141E-16, -162.7500000000000000, -5.000000000000000000 ) ) ;
#42270 = CARTESIAN_POINT ( 'NONE',  ( 1.339745962155612702, 19.83034180399266688, -5.000000000000000000 ) ) ;
#42271 = CYLINDRICAL_SURFACE ( 'NONE', #41912, 5.000000000000000000 ) ;
#42272 = CARTESIAN_POINT ( 'NONE',  ( 4.458734124999999437, -42.81249999863440081, -5.460374474430324690E-16 ) ) ;
#42273 = CARTESIAN_POINT ( 'NONE',  ( 2.229367062500001939, -24.22916666530107577, 3.861377020970579999 ) ) ;
#42274 = VERTEX_POINT ( 'NONE', #3103 ) ;
#42275 = CARTESIAN_POINT ( 'NONE',  ( -1.339745962155613812, -5.080341798530291442, -5.000000000000000000 ) ) ;
#42276 = CARTESIAN_POINT ( 'NONE',  ( 4.458734125000001214, -107.8958333319677365, 2.574251347313718519 ) ) ;
#42277 = CARTESIAN_POINT ( 'NONE',  ( 5.000000000000000888, -153.0625000027311842, -2.071067811865475505 ) ) ;
#42278 = EDGE_LOOP ( 'NONE', ( #2268, #52544, #55867, #59137 ) ) ;
#42279 = CARTESIAN_POINT ( 'NONE',  ( 4.458734124999999437, -106.0624999986344221, -5.460374474430324690E-16 ) ) ;
#42280 = VECTOR ( 'NONE', #42591, 1000.000000000000114 ) ;
#42281 = CARTESIAN_POINT ( 'NONE',  ( 2.229367062500001939, -29.97916666530107221, 3.861377020970579999 ) ) ;
#42282 = CARTESIAN_POINT ( 'NONE',  ( 1.060575238724906964E-15, -65.62499999726881583, 5.773502691896257311 ) ) ;
#42283 = CARTESIAN_POINT ( 'NONE',  ( -52.80376928212989185, -150.1250000013656063, -4.297418129356379346 ) ) ;
#42284 = CARTESIAN_POINT ( 'NONE',  ( 5.000000000000000000, -148.0625000000000284, 2.071067811865478614 ) ) ;
#42285 = CARTESIAN_POINT ( 'NONE',  ( -2.229367062499996610, -28.14583333196774007, 3.861377020970582219 ) ) ;
#42286 = CARTESIAN_POINT ( 'NONE',  ( 4.458734124999998549, -68.97916666530107932, -2.574251347313721627 ) ) ;
#42287 = CARTESIAN_POINT ( 'NONE',  ( 1.846868145590735200, -169.5000000013655495, -4.458734124999999437 ) ) ;
#42288 = CARTESIAN_POINT ( 'NONE',  ( 9.457646018065525792E-16, -26.06249999863440792, 5.148502694627439702 ) ) ;
#42289 = CARTESIAN_POINT ( 'NONE',  ( 1.975475456537005874E-15, -25.62499999726881228, 5.000000000000000000 ) ) ;
#42290 = CARTESIAN_POINT ( 'NONE',  ( 2.499999999999998668, -14.33333333333333037, -4.330127018922193649 ) ) ;
#42291 = CARTESIAN_POINT ( 'NONE',  ( 3.152801135295366208, -149.5625000013655779, 3.152801135295367985 ) ) ;
#42292 = ORIENTED_EDGE ( 'NONE', *, *, #53534, .T. ) ;
#42293 = CARTESIAN_POINT ( 'NONE',  ( -5.000000000000000000, -82.00000000000000000, 0.000000000000000000 ) ) ;
#42294 = CARTESIAN_POINT ( 'NONE',  ( -2.229367062499996610, -51.39583333196773651, 3.861377020970582219 ) ) ;
#42295 =( BOUNDED_CURVE ( )  B_SPLINE_CURVE ( 2, ( #2599, #2925, #22856, #33129, #3548, #22540, #42136, #27346, #31857 ),
 .UNSPECIFIED., .F., .F. ) 
 B_SPLINE_CURVE_WITH_KNOTS ( ( 3, 2, 2, 2, 3 ),
 ( 0.3767857142857142794, 0.3773809523809523725, 0.3785714285714285587, 0.3797619047619047450, 0.3803571428571428381 ),
 .UNSPECIFIED. ) 
 CURVE ( )  GEOMETRIC_REPRESENTATION_ITEM ( )  RATIONAL_B_SPLINE_CURVE ( ( 0.9330127018922194093, 0.9330127018922194093, 1.000000000000000000, 0.8660254037844387076, 1.000000000000000000, 0.8660254037844387076, 1.000000000000000000, 0.9330127018922194093, 0.9330127018922194093 ) ) 
 REPRESENTATION_ITEM ( '' )  );
#42296 = CARTESIAN_POINT ( 'NONE',  ( -1.049326080737009628E-13, -2.750000000000003109, 5.000000000000000000 ) ) ;
#42297 = DIRECTION ( 'NONE',  ( 0.000000000000000000, 1.000000000000000000, 0.000000000000000000 ) ) ;
#42298 = CARTESIAN_POINT ( 'NONE',  ( 2.499999999999998668, 25.66666666666666430, -4.330127018922193649 ) ) ;
#42299 = CARTESIAN_POINT ( 'NONE',  ( -1.336351044127974539E-14, 25.24999999999999645, 5.000000000000000000 ) ) ;
#42300 = CARTESIAN_POINT ( 'NONE',  ( -4.458734124999999437, -3.312499998634407916, 0.000000000000000000 ) ) ;
#42301 = CARTESIAN_POINT ( 'NONE',  ( -4.999999999999998224, -10.91666666666666607, 2.886751345948131764 ) ) ;
#42302 = CARTESIAN_POINT ( 'NONE',  ( 3.061616997868383141E-16, -164.7500000000000000, -5.000000000000000000 ) ) ;
#42303 = CARTESIAN_POINT ( 'NONE',  ( 6.123233995736766282E-16, -170.0000000000000000, -5.000000000000000000 ) ) ;
#42304 = CARTESIAN_POINT ( 'NONE',  ( -4.458734124999998549, 7.520833334698926009, 2.574251347313722516 ) ) ;
#42305 = ORIENTED_EDGE ( 'NONE', *, *, #37842, .T. ) ;
#42306 = CARTESIAN_POINT ( 'NONE',  ( -7.500000000000000888, -0.7512838658081441023, 1.307818870560639724E-15 ) ) ;
#42307 = EDGE_LOOP ( 'NONE', ( #16915, #10053, #1311, #14555 ) ) ;
#42308 = CARTESIAN_POINT ( 'NONE',  ( -6.972266317189433020E-16, -33.24999999999999289, -5.000000000000000000 ) ) ;
#42309 = CARTESIAN_POINT ( 'NONE',  ( 4.458734124999999437, -48.81249999863440792, -5.460374474430324690E-16 ) ) ;
#42310 = CARTESIAN_POINT ( 'NONE',  ( 4.458734124999999437, -158.6875000013655779, 0.000000000000000000 ) ) ;
#42311 = CARTESIAN_POINT ( 'NONE',  ( 5.000000000000000000, -45.37499999726880873, -6.123233995736766282E-16 ) ) ;
#42312 = VERTEX_POINT ( 'NONE', #42634 ) ;
#42313 = CARTESIAN_POINT ( 'NONE',  ( -4.458734124999998549, -25.22916666530106866, 2.574251347313722516 ) ) ;
#42314 = ORIENTED_EDGE ( 'NONE', *, *, #20787, .F. ) ;
#42315 = CARTESIAN_POINT ( 'NONE',  ( 2.071067811865472841, -169.8124999999999716, -5.000000000000002665 ) ) ;
#42316 = CARTESIAN_POINT ( 'NONE',  ( 4.458734124999999437, -164.4375000013655779, 0.000000000000000000 ) ) ;
#42317 = CARTESIAN_POINT ( 'NONE',  ( -6.972266317189433020E-16, -95.25000000000000000, -5.000000000000000000 ) ) ;
#42318 = CARTESIAN_POINT ( 'NONE',  ( -55.39835681537999790, -138.8750000000000284, 4.984105922594378235 ) ) ;
#42319 = ADVANCED_FACE ( 'NONE', ( #47773 ), #27527, .T. ) ;
#42320 = CARTESIAN_POINT ( 'NONE',  ( 2.229367062500001939, -40.22916666530107221, 3.861377020970579999 ) ) ;
#42321 = CARTESIAN_POINT ( 'NONE',  ( -5.000000000000000000, 23.04166666939784847, -2.886751345948128211 ) ) ;
#42322 = VERTEX_POINT ( 'NONE', #22403 ) ;
#42323 = CARTESIAN_POINT ( 'NONE',  ( 9.457646018065525792E-16, -84.06249999863439371, 5.148502694627439702 ) ) ;
#42324 = CARTESIAN_POINT ( 'NONE',  ( 9.457646018065525792E-16, 25.93750000136559564, 5.148502694627439702 ) ) ;
#42325 = LINE ( 'NONE', #43573, #26636 ) ;
#42326 = EDGE_LOOP ( 'NONE', ( #5725, #42767, #35087, #62351, #36312, #19670, #26866, #57686, #50384, #7006, #491, #51177, #9416, #18544, #56108, #30120, #32310, #9526, #11851, #55050, #6501, #33384, #38712, #18284, #46020, #10670, #26525, #32781, #30111, #32294, #58735, #21584, #50560, #24858, #42995, #44031, #18673, #9731, #9696, #48012, #27530, #28866, #16796, #39375 ) ) ;
#42327 = CARTESIAN_POINT ( 'NONE',  ( 2.500000000000002220, 14.33333333333333393, 4.330127018922192761 ) ) ;
#42328 = CARTESIAN_POINT ( 'NONE',  ( -55.35523342533222291, -139.5625000013656063, 4.444560631937231499 ) ) ;
#42329 = CARTESIAN_POINT ( 'NONE',  ( -2.229367062500000163, -84.72916666530107932, -3.861377020970580443 ) ) ;
#42330 = CARTESIAN_POINT ( 'NONE',  ( -52.53715891517739323, -132.5625000027312126, -4.819101127000233298 ) ) ;
#42331 = CARTESIAN_POINT ( 'NONE',  ( 5.000000000000000000, 22.50000000000000000, -6.123233995736766282E-16 ) ) ;
#42332 = CARTESIAN_POINT ( 'NONE',  ( -1.339745962155610925, -6.794658198738519062, 5.000000000000000000 ) ) ;
#42333 =( BOUNDED_CURVE ( )  B_SPLINE_CURVE ( 2, ( #38535, #13483, #4760, #24078, #48195, #62695, #53340, #29510, #43989 ),
 .UNSPECIFIED., .F., .F. ) 
 B_SPLINE_CURVE_WITH_KNOTS ( ( 3, 2, 2, 2, 3 ),
 ( 0.1982142857142857040, 0.1988095238095237971, 0.2000000000000000111, 0.2011904761904761973, 0.2017857142857142905 ),
 .UNSPECIFIED. ) 
 CURVE ( )  GEOMETRIC_REPRESENTATION_ITEM ( )  RATIONAL_B_SPLINE_CURVE ( ( 0.9330127018922194093, 0.9330127018922194093, 1.000000000000000000, 0.8660254037844387076, 1.000000000000000000, 0.8660254037844387076, 1.000000000000000000, 0.9330127018922194093, 0.9330127018922194093 ) ) 
 REPRESENTATION_ITEM ( '' )  );
#42334 = CARTESIAN_POINT ( 'NONE',  ( -6.972266317189433020E-16, -52.12499999726880873, -5.000000000000000000 ) ) ;
#42335 = CARTESIAN_POINT ( 'NONE',  ( 4.458734124999999437, -52.81249999863440792, -5.460374474430324690E-16 ) ) ;
#42336 = CARTESIAN_POINT ( 'NONE',  ( 2.500000000000002220, 10.33333333333333393, 4.330127018922192761 ) ) ;
#42337 = CARTESIAN_POINT ( 'NONE',  ( -2.229367062499996610, 20.85416666803226349, 3.861377020970582219 ) ) ;
#42338 = CARTESIAN_POINT ( 'NONE',  ( 2.500000000000002220, -105.6666666666666572, 4.330127018922192761 ) ) ;
#42339 = CARTESIAN_POINT ( 'NONE',  ( 5.000000000000000000, -154.1250000027312126, 0.000000000000000000 ) ) ;
#42340 = CARTESIAN_POINT ( 'NONE',  ( 2.229367062499998831, -41.89583333196773651, -3.861377020970580887 ) ) ;
#42341 = CARTESIAN_POINT ( 'NONE',  ( 5.000000000000000000, -4.374999997268816720, -6.123233995736766282E-16 ) ) ;
#42342 = CARTESIAN_POINT ( 'NONE',  ( -5.000000000000000888, -153.5625000027312126, 2.071067811865474617 ) ) ;
#42344 = CIRCLE ( 'NONE', #1330, 4.250000000000000000 ) ;
#42343 = CARTESIAN_POINT ( 'NONE',  ( -56.48576386720575471, -124.7500000013655921, -4.591703134518078322 ) ) ;
#42345 = CARTESIAN_POINT ( 'NONE',  ( 9.457646018065525792E-16, -83.31249999863440792, 5.148502694627439702 ) ) ;
#42346 = CARTESIAN_POINT ( 'NONE',  ( 9.457646018065525792E-16, -100.0624999986344221, 5.148502694627439702 ) ) ;
#42347 = CARTESIAN_POINT ( 'NONE',  ( 4.458734125000000326, -3.145833331967738289, 2.574251347313718519 ) ) ;
#42348 = VERTEX_POINT ( 'NONE', #62593 ) ;
#42349 = CARTESIAN_POINT ( 'NONE',  ( 1.975475456537005874E-15, -86.62499999726880162, 5.000000000000000000 ) ) ;
#42350 = CARTESIAN_POINT ( 'NONE',  ( 4.458734124999998549, -93.72916666530105090, -2.574251347313721627 ) ) ;
#42351 = CARTESIAN_POINT ( 'NONE',  ( 5.000000000000000000, -165.1875000027312126, 2.071067811865478614 ) ) ;
#42352 = CARTESIAN_POINT ( 'NONE',  ( -4.458734124999998549, -92.47916666530106511, 2.574251347313722516 ) ) ;
#42353 = CARTESIAN_POINT ( 'NONE',  ( 2.229367062500001939, 13.77083333469892779, 3.861377020970579999 ) ) ;
#42354 = DIRECTION ( 'NONE',  ( -0.000000000000000000, 1.000000000000000000, -0.000000000000000000 ) ) ;
#42355 = CARTESIAN_POINT ( 'NONE',  ( -59.29741812935640155, -132.6250000013656347, -2.196230717870135685 ) ) ;
#42356 = CARTESIAN_POINT ( 'NONE',  ( 2.229367062499998831, -14.64583333196773474, -3.861377020970580887 ) ) ;
#42357 = CARTESIAN_POINT ( 'NONE',  ( -4.458734124999998549, 14.52083333469892779, 2.574251347313722516 ) ) ;
#42358 = CARTESIAN_POINT ( 'NONE',  ( 4.458734125000000326, -52.14583333196773651, 2.574251347313718519 ) ) ;
#42359 = FACE_OUTER_BOUND ( 'NONE', #32276, .T. ) ;
#42360 = CARTESIAN_POINT ( 'NONE',  ( -1.339745962155613812, -22.08034179853029855, -5.000000000000000000 ) ) ;
#42361 = CARTESIAN_POINT ( 'NONE',  ( 2.229367062500001939, -6.979166665301073103, 3.861377020970579999 ) ) ;
#42362 = CARTESIAN_POINT ( 'NONE',  ( 5.000000000000000000, -106.2916666639354730, -2.886751345948130876 ) ) ;
#42363 = VERTEX_POINT ( 'NONE', #22720 ) ;
#42364 = CARTESIAN_POINT ( 'NONE',  ( -2.229367062499996610, -36.39583333196773651, 3.861377020970582219 ) ) ;
#42365 = CARTESIAN_POINT ( 'NONE',  ( -59.59170313451811296, -127.7500000013655921, 1.485763867205729394 ) ) ;
#42366 = CARTESIAN_POINT ( 'NONE',  ( 1.339745962155615144, 0.4196582014697064489, 4.999999999999999112 ) ) ;
#42367 = CARTESIAN_POINT ( 'NONE',  ( 9.457646018065525792E-16, -80.06249999863439371, 5.148502694627439702 ) ) ;
#42368 = CARTESIAN_POINT ( 'NONE',  ( 4.458734124999998549, 22.02083333469892779, -2.574251347313721627 ) ) ;
#42369 = CARTESIAN_POINT ( 'NONE',  ( 4.458734125000001214, 17.10416666803225993, 2.574251347313718519 ) ) ;
#42370 = CARTESIAN_POINT ( 'NONE',  ( -1.339745962155610925, 7.205341801261477386, 5.000000000000000000 ) ) ;
#42371 = CARTESIAN_POINT ( 'NONE',  ( 2.499999999999998668, -55.33333333333332860, -4.330127018922193649 ) ) ;
#42372 = CARTESIAN_POINT ( 'NONE',  ( -2.229367062500000163, -83.72916666530106511, -3.861377020970580443 ) ) ;
#42373 = CARTESIAN_POINT ( 'NONE',  ( 5.000000000000000000, -69.49999999999998579, -6.123233995736766282E-16 ) ) ;
#42374 = CARTESIAN_POINT ( 'NONE',  ( 1.975475456537005874E-15, -63.62499999726880873, 5.000000000000000000 ) ) ;
#42375 = CARTESIAN_POINT ( 'NONE',  ( -5.000000000000000000, 17.04166666939785202, -2.886751345948128211 ) ) ;
#42376 = VERTEX_POINT ( 'NONE', #3728 ) ;
#42377 = CARTESIAN_POINT ( 'NONE',  ( -6.972266317189433020E-16, -66.24999999999998579, -5.000000000000000000 ) ) ;
#42378 = CARTESIAN_POINT ( 'NONE',  ( 5.000000000000000000, 7.583333333333333925, -2.886751345948130876 ) ) ;
#42380 = CARTESIAN_POINT ( 'NONE',  ( -5.000000000000000000, -28.08333333333333925, -2.886751345948128211 ) ) ;
#42379 = FACE_OUTER_BOUND ( 'NONE', #54402, .T. ) ;
#42381 = CARTESIAN_POINT ( 'NONE',  ( 4.458734124999998549, -30.72916666530107221, -2.574251347313721627 ) ) ;
#42382 = CARTESIAN_POINT ( 'NONE',  ( 1.975475456537005874E-15, -33.75000000000000000, 5.000000000000000000 ) ) ;
#42383 = CARTESIAN_POINT ( 'NONE',  ( -2.499999999999996447, -29.70833333060215153, 4.330127018922195425 ) ) ;
#42385 = ORIENTED_EDGE ( 'NONE', *, *, #3416, .F. ) ;
#42384 = CARTESIAN_POINT ( 'NONE',  ( -4.458734124999999437, -61.39583333196774362, -2.574251347313719407 ) ) ;
#42386 = CARTESIAN_POINT ( 'NONE',  ( -50.40829686548195099, -154.2500000013656063, -1.485763867205728284 ) ) ;
#42388 = EDGE_LOOP ( 'NONE', ( #43558, #58086, #60205, #60682 ) ) ;
#42387 = CARTESIAN_POINT ( 'NONE',  ( 2.229367062500001939, -11.22916666530107044, 3.861377020970579999 ) ) ;
#42389 = CARTESIAN_POINT ( 'NONE',  ( 2.500000000000002220, -78.66666666666665719, 4.330127018922192761 ) ) ;
#42390 = CARTESIAN_POINT ( 'NONE',  ( -50.70258187064364108, -137.1250000013656063, 2.196230717870141014 ) ) ;
#42391 = CARTESIAN_POINT ( 'NONE',  ( 2.229367062499998831, -53.89583333196773651, -3.861377020970580887 ) ) ;
#42392 = CARTESIAN_POINT ( 'NONE',  ( 5.000000000000000888, -79.45833333060214443, 2.886751345948126879 ) ) ;
#42394 = ORIENTED_EDGE ( 'NONE', *, *, #7942, .T. ) ;
#42393 = CARTESIAN_POINT ( 'NONE',  ( -4.764381983412779477E-15, 26.37500000273118417, 5.000000000000000000 ) ) ;
#42395 = CARTESIAN_POINT ( 'NONE',  ( -57.46284108482265651, -148.9375000000000000, 4.819101127000239515 ) ) ;
#42396 = ADVANCED_FACE ( 'NONE', ( #62276 ), #62896, .T. ) ;
#42397 = CARTESIAN_POINT ( 'NONE',  ( 9.457646018065525792E-16, -21.31249999863440081, 5.148502694627439702 ) ) ;
#42399 = ORIENTED_EDGE ( 'NONE', *, *, #11487, .F. ) ;
#42398 = CARTESIAN_POINT ( 'NONE',  ( 4.458734125000001214, -59.14583333196773651, 2.574251347313718519 ) ) ;
#42400 = CARTESIAN_POINT ( 'NONE',  ( -8.190561711645485556E-16, -168.9375000013656063, 4.458734124999999437 ) ) ;
#42401 = CARTESIAN_POINT ( 'NONE',  ( 4.458734124999999437, -99.06249999863440792, -5.460374474430324690E-16 ) ) ;
#42402 = VERTEX_POINT ( 'NONE', #42317 ) ;
#42403 = CARTESIAN_POINT ( 'NONE',  ( -55.35523342533222291, -150.5625000013656063, 4.444560631937231499 ) ) ;
#42404 = CARTESIAN_POINT ( 'NONE',  ( -51.19402409849444524, -144.6250000027312126, -3.242614290531456334 ) ) ;
#42405 = DIRECTION ( 'NONE',  ( 0.000000000000000000, 0.000000000000000000, 1.000000000000000000 ) ) ;
#42406 = CARTESIAN_POINT ( 'NONE',  ( 4.458734124999999437, -6.812499998634404363, -5.460374474430324690E-16 ) ) ;
#42407 =( BOUNDED_CURVE ( )  B_SPLINE_CURVE ( 2, ( #20911, #5472, #44377, #44696, #39868, #40516, #60158, #30872, #15121 ),
 .UNSPECIFIED., .F., .F. ) 
 B_SPLINE_CURVE_WITH_KNOTS ( ( 3, 2, 2, 2, 3 ),
 ( 0.9267857142857143238, 0.9273809523809524169, 0.9285714285714286031, 0.9297619047619047894, 0.9303571428571428825 ),
 .UNSPECIFIED. ) 
 CURVE ( )  GEOMETRIC_REPRESENTATION_ITEM ( )  RATIONAL_B_SPLINE_CURVE ( ( 0.9330127018922194093, 0.9330127018922194093, 1.000000000000000000, 0.8660254037844387076, 1.000000000000000000, 0.8660254037844387076, 1.000000000000000000, 0.9330127018922194093, 0.9330127018922194093 ) ) 
 REPRESENTATION_ITEM ( '' )  );
#42408 = CARTESIAN_POINT ( 'NONE',  ( 4.458734124999999437, -93.06249999863440792, -5.460374474430324690E-16 ) ) ;
#42409 = CARTESIAN_POINT ( 'NONE',  ( -4.458734125000000326, -149.2500000013655779, -1.846868145590735644 ) ) ;
#42410 = CARTESIAN_POINT ( 'NONE',  ( 4.458734124999998549, -27.97916666530107577, -2.574251347313721627 ) ) ;
#42411 = EDGE_CURVE ( 'NONE', #5841, #34951, #14220, .T. ) ;
#42412 = CARTESIAN_POINT ( 'NONE',  ( -7.500000000000000888, 3.639598441879742907, -0.7155132341745253921 ) ) ;
#42413 = CARTESIAN_POINT ( 'NONE',  ( -54.64476657466781973, -137.8125000013656063, -4.444560631937228834 ) ) ;
#42414 = CARTESIAN_POINT ( 'NONE',  ( -4.458734124999999437, -63.64583333196773651, -2.574251347313719407 ) ) ;
#42415 = CARTESIAN_POINT ( 'NONE',  ( 2.499999999999998668, -43.33333333333333570, -4.330127018922193649 ) ) ;
#42416 = CYLINDRICAL_SURFACE ( 'NONE', #35685, 5.000000000000000000 ) ;
#42417 = CARTESIAN_POINT ( 'NONE',  ( -4.458734125000000326, -144.8750000013656063, 1.846868145590734089 ) ) ;
#42418 = CARTESIAN_POINT ( 'NONE',  ( -4.458734124999999437, 10.43750000136559386, 0.000000000000000000 ) ) ;
#42419 = VERTEX_POINT ( 'NONE', #13683 ) ;
#42420 = CARTESIAN_POINT ( 'NONE',  ( -6.972266317189433020E-16, -49.12499999726880162, -5.000000000000000000 ) ) ;
#42421 = CARTESIAN_POINT ( 'NONE',  ( 5.000000000000000888, -61.58333333333333570, 2.886751345948126879 ) ) ;
#42423 = CARTESIAN_POINT ( 'NONE',  ( 9.457646018065525792E-16, -22.06249999863440436, 5.148502694627439702 ) ) ;
#42422 = CARTESIAN_POINT ( 'NONE',  ( -3.535250795749689387E-16, -90.24999999999998579, -5.773502691896257311 ) ) ;
#42424 = CARTESIAN_POINT ( 'NONE',  ( 0.000000000000000000, -120.0000000000000000, 5.000000000000000000 ) ) ;
#42425 = CARTESIAN_POINT ( 'NONE',  ( 4.458734124999999437, -70.06249999863439371, -5.460374474430324690E-16 ) ) ;
#42426 = CARTESIAN_POINT ( 'NONE',  ( -6.972266317189433020E-16, -72.25000000000000000, -5.000000000000000000 ) ) ;
#42427 = CARTESIAN_POINT ( 'NONE',  ( -5.000000000000000000, -17.87499999726881583, 0.000000000000000000 ) ) ;
#42428 = EDGE_CURVE ( 'NONE', #11960, #35585, #23350, .T. ) ;
#42429 = CARTESIAN_POINT ( 'NONE',  ( -50.55543936806279248, -145.0625000013656063, 0.3552334253322060320 ) ) ;
#42430 = CARTESIAN_POINT ( 'NONE',  ( -4.458734124999999437, 2.687500001365593860, 0.000000000000000000 ) ) ;
#42431 = CARTESIAN_POINT ( 'NONE',  ( 6.123233995736766282E-16, -120.0000000000000000, -5.000000000000000000 ) ) ;
#42432 = DIRECTION ( 'NONE',  ( 0.000000000000000000, 0.000000000000000000, 1.000000000000000000 ) ) ;
#42433 = CARTESIAN_POINT ( 'NONE',  ( -2.229367062499996610, 5.854166668032262599, 3.861377020970582219 ) ) ;
#42434 = CARTESIAN_POINT ( 'NONE',  ( -4.458734124999999437, -74.31249999863440792, 0.000000000000000000 ) ) ;
#42435 = CARTESIAN_POINT ( 'NONE',  ( -4.458734124999999437, -21.56249999863440436, 0.000000000000000000 ) ) ;
#42436 = CARTESIAN_POINT ( 'NONE',  ( -3.535250795749689387E-16, -5.249999999999997335, -5.773502691896257311 ) ) ;
#42437 = CARTESIAN_POINT ( 'NONE',  ( 3.152801135295367541, -159.3125000013656063, -3.152801135295367541 ) ) ;
#42438 = CARTESIAN_POINT ( 'NONE',  ( 1.975475456537005874E-15, -36.62499999726880873, 5.000000000000000000 ) ) ;
#42439 = CARTESIAN_POINT ( 'NONE',  ( -2.229367062500000163, -62.47916666530106511, -3.861377020970580443 ) ) ;
#42440 = CARTESIAN_POINT ( 'NONE',  ( 5.000000000000000888, -100.4583333306021444, 2.886751345948126879 ) ) ;
#42441 = CYLINDRICAL_SURFACE ( 'NONE', #57365, 5.000000000000000000 ) ;
#42442 = CARTESIAN_POINT ( 'NONE',  ( -4.458734124999997661, -41.22916666530107932, 2.574251347313722516 ) ) ;
#42443 = ADVANCED_FACE ( 'NONE', ( #12735 ), #32993, .T. ) ;
#42444 = CARTESIAN_POINT ( 'NONE',  ( -4.458734124999999437, -107.5624999986343937, 0.000000000000000000 ) ) ;
#42445 = CARTESIAN_POINT ( 'NONE',  ( -4.458734124999999437, -65.64583333196773651, -2.574251347313719407 ) ) ;
#42446 = CARTESIAN_POINT ( 'NONE',  ( 5.000000000000000888, -48.58333333333332149, 2.886751345948126879 ) ) ;
#42447 = CARTESIAN_POINT ( 'NONE',  ( -1.339745962155613812, -41.20534180126147561, -5.000000000000000000 ) ) ;
#42448 = CARTESIAN_POINT ( 'NONE',  ( 2.500000000000002220, -68.54166666393547303, 4.330127018922192761 ) ) ;
#42449 = EDGE_LOOP ( 'NONE', ( #49579, #301, #31483, #13962 ) ) ;
#42450 = CARTESIAN_POINT ( 'NONE',  ( 1.975475456537005874E-15, -84.74999999999998579, 5.000000000000000000 ) ) ;
#42451 = CARTESIAN_POINT ( 'NONE',  ( -2.500000000000000444, -100.0416666639354588, -4.330127018922193649 ) ) ;
#42452 = CARTESIAN_POINT ( 'NONE',  ( 2.499999999999998668, -11.33333333333333393, -4.330127018922193649 ) ) ;
#42453 = CARTESIAN_POINT ( 'NONE',  ( -4.458734124999998549, -17.22916666530106866, 2.574251347313722516 ) ) ;
#42454 = CARTESIAN_POINT ( 'NONE',  ( 4.458734124999998549, -78.72916666530106511, -2.574251347313721627 ) ) ;
#42455 = DIRECTION ( 'NONE',  ( -0.6485228581062915110, 0.000000000000000000, -0.7611951803011149931 ) ) ;
#42456 = CARTESIAN_POINT ( 'NONE',  ( 5.000000000000000000, -13.37499999726881050, -6.123233995736766282E-16 ) ) ;
#42458 = ORIENTED_EDGE ( 'NONE', *, *, #41607, .F. ) ;
#42457 = CARTESIAN_POINT ( 'NONE',  ( -4.458734124999998549, -42.22916666530107932, 2.574251347313722516 ) ) ;
#42459 = CARTESIAN_POINT ( 'NONE',  ( 6.123233995736766282E-16, -120.0000000000000000, -5.000000000000000000 ) ) ;
#42461 = EDGE_LOOP ( 'NONE', ( #17866, #60293, #28291, #53323 ) ) ;
#42460 = CARTESIAN_POINT ( 'NONE',  ( -3.152548672688508926E-16, 9.187500001365593860, -5.148502694627439702 ) ) ;
#42462 =( BOUNDED_CURVE ( )  B_SPLINE_CURVE ( 2, ( #26005, #61698, #1898, #22459, #45935, #21506, #26639, #46580, #12477 ),
 .UNSPECIFIED., .F., .F. ) 
 B_SPLINE_CURVE_WITH_KNOTS ( ( 3, 2, 2, 2, 3 ),
 ( 0.6062499999999999556, 0.6069444444444443976, 0.6083333333333332815, 0.6097222222222222765, 0.6104166666666667185 ),
 .UNSPECIFIED. ) 
 CURVE ( )  GEOMETRIC_REPRESENTATION_ITEM ( )  RATIONAL_B_SPLINE_CURVE ( ( 0.9330127018922194093, 0.9330127018922194093, 1.000000000000000000, 0.8660254037844387076, 1.000000000000000000, 0.8660254037844387076, 1.000000000000000000, 0.9330127018922194093, 0.9330127018922194093 ) ) 
 REPRESENTATION_ITEM ( '' )  );
#42463 = LINE ( 'NONE', #41509, #17594 ) ;
#42464 = CARTESIAN_POINT ( 'NONE',  ( 5.000000000000000888, -55.58333333333333570, 2.886751345948126879 ) ) ;
#42465 = CARTESIAN_POINT ( 'NONE',  ( -3.152801135295367096, -158.3125000013656063, -3.152801135295367541 ) ) ;
#42466 = CARTESIAN_POINT ( 'NONE',  ( 2.229367062500001939, -38.22916666530107221, 3.861377020970579999 ) ) ;
#42467 = CARTESIAN_POINT ( 'NONE',  ( -6.324555320336756381, 15.00000000000000000, -9.000000000000001776 ) ) ;
#42468 = CARTESIAN_POINT ( 'NONE',  ( -3.152548672688508926E-16, -82.56249999863442213, -5.148502694627439702 ) ) ;
#42469 = CARTESIAN_POINT ( 'NONE',  ( 3.535533905932736864, -165.1250000000000284, 3.535533905932738641 ) ) ;
#42470 = CARTESIAN_POINT ( 'NONE',  ( 0.000000000000000000, -120.0000000000000000, 0.000000000000000000 ) ) ;
#42471 = CARTESIAN_POINT ( 'NONE',  ( -59.44456063193725015, -129.8125000013656063, -0.3552334253322034230 ) ) ;
#42472 = ADVANCED_FACE ( 'NONE', ( #13054 ), #18198, .T. ) ;
#42473 = CARTESIAN_POINT ( 'NONE',  ( -2.229367062499996610, -8.395833331967736513, 3.861377020970582219 ) ) ;
#42474 = CARTESIAN_POINT ( 'NONE',  ( -4.458734124999998549, -43.47916666530106511, 2.574251347313722516 ) ) ;
#42475 = VECTOR ( 'NONE', #41528, 1000.000000000000000 ) ;
#42476 = EDGE_CURVE ( 'NONE', #47715, #7044, #27760, .T. ) ;
#42477 = ADVANCED_FACE ( 'NONE', ( #32358 ), #1592, .T. ) ;
#42478 = CARTESIAN_POINT ( 'NONE',  ( 2.071067811865645591, -151.3125000027311842, 4.999999999999830358 ) ) ;
#42479 = CARTESIAN_POINT ( 'NONE',  ( 9.457646018065525792E-16, -84.31249999863437949, 5.148502694627439702 ) ) ;
#42480 = FACE_OUTER_BOUND ( 'NONE', #62426, .T. ) ;
#42481 = ORIENTED_EDGE ( 'NONE', *, *, #8230, .F. ) ;
#42482 = CARTESIAN_POINT ( 'NONE',  ( -4.999999999999998224, -94.79166666393547303, 2.886751345948131764 ) ) ;
#42483 = CARTESIAN_POINT ( 'NONE',  ( -58.24261429053147765, -148.2500000000000284, -3.805975901505573855 ) ) ;
#42484 = CARTESIAN_POINT ( 'NONE',  ( 9.457646018065525792E-16, -71.31249999863439371, 5.148502694627439702 ) ) ;
#42485 = CARTESIAN_POINT ( 'NONE',  ( -4.458734124999999437, -146.2500000013656347, -1.846868145590735644 ) ) ;
#42486 = EDGE_LOOP ( 'NONE', ( #34422, #31872, #54971, #5159 ) ) ;
#42487 = EDGE_CURVE ( 'NONE', #24623, #40250, #29805, .T. ) ;
#42488 = LINE ( 'NONE', #47013, #63593 ) ;
#42489 = CARTESIAN_POINT ( 'NONE',  ( 5.000000000000000000, 17.58333333333333215, -2.886751345948130876 ) ) ;
#42490 = CARTESIAN_POINT ( 'NONE',  ( -2.229367062499996610, -5.395833331967740953, 3.861377020970582219 ) ) ;
#42491 = EDGE_CURVE ( 'NONE', #5270, #36444, #29723, .T. ) ;
#42492 = CARTESIAN_POINT ( 'NONE',  ( -2.500000000000000444, 2.833333333333333481, -4.330127018922193649 ) ) ;
#42493 = CARTESIAN_POINT ( 'NONE',  ( -3.152548672688508926E-16, 3.437500001365594748, -5.148502694627439702 ) ) ;
#42494 = CARTESIAN_POINT ( 'NONE',  ( -5.000000000000000000, -95.95833333060213022, -2.886751345948128211 ) ) ;
#42495 = CARTESIAN_POINT ( 'NONE',  ( 3.152801135295367541, -155.3125000013656063, -3.152801135295367541 ) ) ;
#42496 = CARTESIAN_POINT ( 'NONE',  ( -4.458734124999999437, 27.43750000136559208, 0.000000000000000000 ) ) ;
#42497 = ORIENTED_EDGE ( 'NONE', *, *, #21676, .T. ) ;
#42498 = CARTESIAN_POINT ( 'NONE',  ( -4.458734124999997661, -93.22916666530107932, 2.574251347313722516 ) ) ;
#42499 = CARTESIAN_POINT ( 'NONE',  ( -4.999999999999998224, -67.91666666666667140, 2.886751345948131764 ) ) ;
#42500 = CARTESIAN_POINT ( 'NONE',  ( -4.999999999999998224, -69.79166666393547303, 2.886751345948131764 ) ) ;
#42501 = CARTESIAN_POINT ( 'NONE',  ( -2.229367062500000163, -7.479166665301073991, -3.861377020970580443 ) ) ;
#42502 = CARTESIAN_POINT ( 'NONE',  ( 0.000000000000000000, -120.0000000000000000, 5.000000000000000000 ) ) ;
#42503 = CARTESIAN_POINT ( 'NONE',  ( 1.339745962155615144, -48.70534180126148271, 4.999999999999999112 ) ) ;
#42504 = CARTESIAN_POINT ( 'NONE',  ( 5.000000000000000000, -67.41666666666667140, -2.886751345948130876 ) ) ;
#42505 = CARTESIAN_POINT ( 'NONE',  ( 2.500000000000002220, -33.54166666393547303, 4.330127018922192761 ) ) ;
#42506 = FACE_OUTER_BOUND ( 'NONE', #7367, .T. ) ;
#42507 = CARTESIAN_POINT ( 'NONE',  ( -3.152548672688508926E-16, 20.43750000136559208, -5.148502694627439702 ) ) ;
#42508 = CARTESIAN_POINT ( 'NONE',  ( -5.000000000000000000, -97.95833333060214443, -2.886751345948128211 ) ) ;
#42509 = CARTESIAN_POINT ( 'NONE',  ( -4.458734124999997661, 23.77083333469892423, 2.574251347313722516 ) ) ;
#42510 = CARTESIAN_POINT ( 'NONE',  ( 4.458734124999999437, -54.81249999863440081, -5.460374474430324690E-16 ) ) ;
#42511 = CARTESIAN_POINT ( 'NONE',  ( 9.457646018065525792E-16, -4.312499998634408804, 5.148502694627439702 ) ) ;
#42512 =( BOUNDED_CURVE ( )  B_SPLINE_CURVE ( 2, ( #51369, #56515, #27229, #46850, #2797, #18527, #18824, #58070, #13694 ),
 .UNSPECIFIED., .F., .F. ) 
 B_SPLINE_CURVE_WITH_KNOTS ( ( 3, 2, 2, 2, 3 ),
 ( 0.7375000000000000444, 0.7380952380952381375, 0.7392857142857143238, 0.7404761904761905100, 0.7410714285714286031 ),
 .UNSPECIFIED. ) 
 CURVE ( )  GEOMETRIC_REPRESENTATION_ITEM ( )  RATIONAL_B_SPLINE_CURVE ( ( 0.9330127018922194093, 0.9330127018922194093, 1.000000000000000000, 0.8660254037844387076, 1.000000000000000000, 0.8660254037844387076, 1.000000000000000000, 0.9330127018922194093, 0.9330127018922194093 ) ) 
 REPRESENTATION_ITEM ( '' )  );
#42513 = DIRECTION ( 'NONE',  ( -0.000000000000000000, 1.000000000000000000, -0.000000000000000000 ) ) ;
#42514 = CARTESIAN_POINT ( 'NONE',  ( -5.000000000000000000, 15.91666666666666430, -2.886751345948128211 ) ) ;
#42515 = CARTESIAN_POINT ( 'NONE',  ( -3.535533905932738641, -140.5000000027311842, 3.535533905932737309 ) ) ;
#42516 = CARTESIAN_POINT ( 'NONE',  ( -59.81910112700026616, -145.3125000027311842, -2.462841084822510851 ) ) ;
#42517 = CARTESIAN_POINT ( 'NONE',  ( -2.229367062499996610, -46.14583333196774362, 3.861377020970582219 ) ) ;
#42518 = CARTESIAN_POINT ( 'NONE',  ( -2.499999999999996447, -84.70833333060214443, 4.330127018922195425 ) ) ;
#42519 = CARTESIAN_POINT ( 'NONE',  ( -54.64476657466781973, -135.0625000013656063, -4.444560631937228834 ) ) ;
#42520 = VECTOR ( 'NONE', #38530, 1000.000000000000000 ) ;
#42521 = DIRECTION ( 'NONE',  ( -0.000000000000000000, 1.000000000000000000, -0.000000000000000000 ) ) ;
#42522 = CARTESIAN_POINT ( 'NONE',  ( 1.975475456537005874E-15, -104.6249999972688016, 5.000000000000000000 ) ) ;
#42523 = CARTESIAN_POINT ( 'NONE',  ( 4.458734124999998549, -83.97916666530106511, -2.574251347313721627 ) ) ;
#42524 = CARTESIAN_POINT ( 'NONE',  ( -3.152801135295367985, -157.0625000013656063, 3.152801135295367096 ) ) ;
#42525 = CARTESIAN_POINT ( 'NONE',  ( -3.535250795749689387E-16, -35.25000000000000000, -5.773502691896257311 ) ) ;
#42526 = DIRECTION ( 'NONE',  ( -0.000000000000000000, 1.000000000000000000, -0.000000000000000000 ) ) ;
#42527 = ORIENTED_EDGE ( 'NONE', *, *, #33478, .F. ) ;
#42528 = CARTESIAN_POINT ( 'NONE',  ( 4.458734125000001214, 19.85416666803226349, 2.574251347313718519 ) ) ;
#42529 = ORIENTED_EDGE ( 'NONE', *, *, #34705, .F. ) ;
#42530 = CARTESIAN_POINT ( 'NONE',  ( -4.458734124999998549, -98.22916666530105090, 2.574251347313722516 ) ) ;
#42531 = CARTESIAN_POINT ( 'NONE',  ( -4.458734124999998549, 7.520833334698926009, 2.574251347313722516 ) ) ;
#42532 = CARTESIAN_POINT ( 'NONE',  ( -3.535250795749689387E-16, 12.87500000273118417, -5.773502691896257311 ) ) ;
#42533 = LINE ( 'NONE', #11997, #48332 ) ;
#42534 = CARTESIAN_POINT ( 'NONE',  ( -4.999999999999999112, 3.083333333333333925, 2.886751345948131764 ) ) ;
#42535 = CARTESIAN_POINT ( 'NONE',  ( 2.229367062499998831, -62.64583333196774362, -3.861377020970580887 ) ) ;
#42536 = CARTESIAN_POINT ( 'NONE',  ( 4.729367062499999719, -139.2812500020483810, 0.000000000000000000 ) ) ;
#42537 = CARTESIAN_POINT ( 'NONE',  ( 1.060575238724906964E-15, -80.75000000000000000, 5.773502691896257311 ) ) ;
#42538 = CARTESIAN_POINT ( 'NONE',  ( 9.457646018065525792E-16, -26.06249999863440792, 5.148502694627439702 ) ) ;
#42539 = LINE ( 'NONE', #12334, #24510 ) ;
#42540 = CARTESIAN_POINT ( 'NONE',  ( -1.339745962155614034, 26.33034180399265978, 4.999999999999999112 ) ) ;
#42541 = CARTESIAN_POINT ( 'NONE',  ( 1.339745962155612702, -109.2946581987385315, -5.000000000000000000 ) ) ;
#42542 = CARTESIAN_POINT ( 'NONE',  ( 1.060575238724906964E-15, -37.75000000000000000, 5.773502691896257311 ) ) ;
#42543 = FACE_OUTER_BOUND ( 'NONE', #38739, .T. ) ;
#42545 = CARTESIAN_POINT ( 'NONE',  ( 2.229367062499998831, -20.89583333196774007, -3.861377020970580887 ) ) ;
#42544 = CARTESIAN_POINT ( 'NONE',  ( -1.339745962155610925, 14.20534180126148094, 5.000000000000000000 ) ) ;
#42546 = CARTESIAN_POINT ( 'NONE',  ( -2.499999999999996447, -57.83333333333333570, 4.330127018922195425 ) ) ;
#42547 = CARTESIAN_POINT ( 'NONE',  ( 4.458734124999999437, -64.81249999863440792, -5.460374474430324690E-16 ) ) ;
#42548 = CARTESIAN_POINT ( 'NONE',  ( 3.152801135295367541, -149.5625000013655779, -3.152801135295367541 ) ) ;
#42549 = CARTESIAN_POINT ( 'NONE',  ( -4.458734124999999437, -78.39583333196772230, -2.574251347313719407 ) ) ;
#42550 = CARTESIAN_POINT ( 'NONE',  ( -54.64476657466781973, -145.0625000013656063, -4.444560631937228834 ) ) ;
#42551 = CARTESIAN_POINT ( 'NONE',  ( -4.458734124999998549, -26.47916666530107221, 2.574251347313722516 ) ) ;
#42552 = CARTESIAN_POINT ( 'NONE',  ( 5.000000000000000000, -67.29166666393547303, -2.886751345948129988 ) ) ;
#42554 = ORIENTED_EDGE ( 'NONE', *, *, #25509, .F. ) ;
#42553 = ADVANCED_FACE ( 'NONE', ( #14306 ), #17998, .F. ) ;
#42555 = CYLINDRICAL_SURFACE ( 'NONE', #30248, 5.000000000000000000 ) ;
#42556 = ORIENTED_EDGE ( 'NONE', *, *, #49250, .F. ) ;
#42557 = CARTESIAN_POINT ( 'NONE',  ( 4.458734124999998549, -69.97916666530107932, -2.574251347313721627 ) ) ;
#42558 = CARTESIAN_POINT ( 'NONE',  ( 5.000000000000000000, -149.1250000027312126, 0.000000000000000000 ) ) ;
#42559 = DIRECTION ( 'NONE',  ( 0.8660254037844385966, 0.5000000000000001110, 0.000000000000000000 ) ) ;
#42560 = ORIENTED_EDGE ( 'NONE', *, *, #11395, .F. ) ;
#42561 = CARTESIAN_POINT ( 'NONE',  ( -58.80597590150559739, -127.0000000000000284, 3.242614290531460330 ) ) ;
#42562 = CARTESIAN_POINT ( 'NONE',  ( 5.000000000000000888, -8.583333333333332149, 2.886751345948126879 ) ) ;
#42563 = CARTESIAN_POINT ( 'NONE',  ( -2.229367062500000163, -51.72916666530107221, -3.861377020970580443 ) ) ;
#42564 = EDGE_CURVE ( 'NONE', #23493, #15636, #62713, .T. ) ;
#42565 = VERTEX_POINT ( 'NONE', #53237 ) ;
#42566 = VECTOR ( 'NONE', #53469, 1000.000000000000000 ) ;
#42567 = CARTESIAN_POINT ( 'NONE',  ( 2.500000000000002220, -45.66666666666666430, 4.330127018922192761 ) ) ;
#42568 = CARTESIAN_POINT ( 'NONE',  ( 2.229367062500001939, 10.02083333469892779, 3.861377020970579999 ) ) ;
#42569 = ADVANCED_FACE ( 'NONE', ( #39062 ), #59331, .T. ) ;
#42570 = CARTESIAN_POINT ( 'NONE',  ( 2.229367062500001939, 17.02083333469892779, 3.861377020970579999 ) ) ;
#42571 = CARTESIAN_POINT ( 'NONE',  ( -53.51423613279429503, -146.2500000013656063, 4.591703134518082763 ) ) ;
#42572 = CARTESIAN_POINT ( 'NONE',  ( -2.500000000000000444, 5.958333336064519870, -4.330127018922193649 ) ) ;
#42573 = CARTESIAN_POINT ( 'NONE',  ( -1.846868145590734756, -168.1250000013656063, -4.458734124999999437 ) ) ;
#42575 = EDGE_CURVE ( 'NONE', #28956, #23230, #43878, .T. ) ;
#42574 = ORIENTED_EDGE ( 'NONE', *, *, #6431, .T. ) ;
#42576 = CARTESIAN_POINT ( 'NONE',  ( 2.229367062499998831, -72.64583333196773651, -3.861377020970580887 ) ) ;
#42577 = LINE ( 'NONE', #32935, #34603 ) ;
#42578 = CARTESIAN_POINT ( 'NONE',  ( -4.458734124999999437, 8.687500001365595637, 0.000000000000000000 ) ) ;
#42579 = EDGE_CURVE ( 'NONE', #4978, #29860, #5592, .T. ) ;
#42580 = DIRECTION ( 'NONE',  ( 0.000000000000000000, 0.000000000000000000, 1.000000000000000000 ) ) ;
#42581 = CARTESIAN_POINT ( 'NONE',  ( 2.229367062500001939, -62.22916666530106511, 3.861377020970579999 ) ) ;
#42582 = CARTESIAN_POINT ( 'NONE',  ( -2.499999999999996447, -17.70833333060214443, 4.330127018922195425 ) ) ;
#42583 = CARTESIAN_POINT ( 'NONE',  ( -5.000000000000000000, -32.87499999726880873, 0.000000000000000000 ) ) ;
#42584 = CARTESIAN_POINT ( 'NONE',  ( 1.339745962155615144, -45.70534180126146850, 4.999999999999999112 ) ) ;
#42585 = DIRECTION ( 'NONE',  ( 1.000000000000000000, 0.000000000000000000, 0.000000000000000000 ) ) ;
#42586 = LINE ( 'NONE', #26860, #27541 ) ;
#42587 = CARTESIAN_POINT ( 'NONE',  ( -3.535533905932738641, -159.3750000000000284, 3.535533905932737309 ) ) ;
#42588 = CARTESIAN_POINT ( 'NONE',  ( 4.458734125000001214, -42.89583333196773651, 2.574251347313718519 ) ) ;
#42589 = CARTESIAN_POINT ( 'NONE',  ( -3.152548672688508926E-16, -25.81249999863440792, -5.148502694627439702 ) ) ;
#42590 = VERTEX_POINT ( 'NONE', #54511 ) ;
#42591 = DIRECTION ( 'NONE',  ( -0.8660254037844410391, 0.4999999999999958367, 0.000000000000000000 ) ) ;
#42592 = CARTESIAN_POINT ( 'NONE',  ( -4.458734124999999437, -108.3124999986343937, 0.000000000000000000 ) ) ;
#42593 = CARTESIAN_POINT ( 'NONE',  ( -3.535533905932738641, -152.5000000027312126, 3.535533905932737309 ) ) ;
#42594 = VERTEX_POINT ( 'NONE', #14619 ) ;
#42595 = CARTESIAN_POINT ( 'NONE',  ( 2.229367062499998831, -109.8958333319677365, -3.861377020970580887 ) ) ;
#42596 = CARTESIAN_POINT ( 'NONE',  ( -2.229367062499996610, -31.14583333196773651, 3.861377020970582219 ) ) ;
#42597 = CARTESIAN_POINT ( 'NONE',  ( -2.500000000000000444, -68.04166666393547303, -4.330127018922193649 ) ) ;
#42598 =( BOUNDED_CURVE ( )  B_SPLINE_CURVE ( 2, ( #28566, #24069, #38237, #53647, #9266, #58478, #39162, #62688, #28253 ),
 .UNSPECIFIED., .F., .F. ) 
 B_SPLINE_CURVE_WITH_KNOTS ( ( 3, 2, 2, 2, 3 ),
 ( 0.4750000000000004219, 0.4791666666666671293, 0.4833333333333337811, 0.4875000000000004330, 0.4916666666666670849 ),
 .UNSPECIFIED. ) 
 CURVE ( )  GEOMETRIC_REPRESENTATION_ITEM ( )  RATIONAL_B_SPLINE_CURVE ( ( 0.9999999999999918954, 0.9238795325112948431, 1.000000000000000000, 0.9238795325112867385, 1.000000000000000000, 0.9238795325112867385, 1.000000000000000000, 0.9238795325112786339, 1.000000000000008216 ) ) 
 REPRESENTATION_ITEM ( '' )  );
#42599 = CARTESIAN_POINT ( 'NONE',  ( -50.70258187064364108, -146.3750000013655779, 2.196230717870141014 ) ) ;
#42600 = CARTESIAN_POINT ( 'NONE',  ( 3.535533905932738197, -148.8750000000000000, -3.535533905932738197 ) ) ;
#42601 = CARTESIAN_POINT ( 'NONE',  ( 2.229367062500001939, -28.97916666530107221, 3.861377020970579999 ) ) ;
#42602 = CARTESIAN_POINT ( 'NONE',  ( 4.458734124999998549, -70.97916666530107932, -2.574251347313721627 ) ) ;
#42603 = CARTESIAN_POINT ( 'NONE',  ( 2.730187237215162345E-16, -168.4375000013656063, -4.458734124999999437 ) ) ;
#42604 = CARTESIAN_POINT ( 'NONE',  ( -2.229367062499996610, -27.14583333196774007, 3.861377020970582219 ) ) ;
#42605 = DIRECTION ( 'NONE',  ( -0.000000000000000000, 1.000000000000000000, -0.000000000000000000 ) ) ;
#42606 = FACE_OUTER_BOUND ( 'NONE', #31501, .T. ) ;
#42607 = CARTESIAN_POINT ( 'NONE',  ( -3.535250795749689387E-16, -18.25000000000000355, -5.773502691896257311 ) ) ;
#42608 = CARTESIAN_POINT ( 'NONE',  ( 4.458734124999999437, -147.5000000013656063, 1.846868145590737864 ) ) ;
#42609 = ORIENTED_EDGE ( 'NONE', *, *, #55776, .T. ) ;
#42610 = FACE_OUTER_BOUND ( 'NONE', #20902, .T. ) ;
#42611 = CARTESIAN_POINT ( 'NONE',  ( 4.458734125000000326, -58.14583333196773651, 2.574251347313718519 ) ) ;
#42612 = CARTESIAN_POINT ( 'NONE',  ( 5.000000000000000000, 28.62500000273118417, -6.123233995736766282E-16 ) ) ;
#42613 = DIRECTION ( 'NONE',  ( 0.000000000000000000, 0.000000000000000000, 1.000000000000000000 ) ) ;
#42614 = CARTESIAN_POINT ( 'NONE',  ( 5.000000000000000000, 23.50000000000000000, -6.123233995736766282E-16 ) ) ;
#42615 = CARTESIAN_POINT ( 'NONE',  ( 1.975475456537005874E-15, 8.375000002731187720, 5.000000000000000000 ) ) ;
#42616 = CARTESIAN_POINT ( 'NONE',  ( -2.229367062500000163, -0.4791666653010707710, -3.861377020970580443 ) ) ;
#42617 =( BOUNDED_CURVE ( )  B_SPLINE_CURVE ( 2, ( #16885, #3058, #26537, #26863, #2736, #56775, #17835, #42275, #60647 ),
 .UNSPECIFIED., .F., .F. ) 
 B_SPLINE_CURVE_WITH_KNOTS ( ( 3, 2, 2, 2, 3 ),
 ( 0.2812500000000000000, 0.2819444444444444420, 0.2833333333333333259, 0.2847222222222222099, 0.2854166666666666519 ),
 .UNSPECIFIED. ) 
 CURVE ( )  GEOMETRIC_REPRESENTATION_ITEM ( )  RATIONAL_B_SPLINE_CURVE ( ( 0.9330127018922194093, 0.9330127018922194093, 1.000000000000000000, 0.8660254037844387076, 1.000000000000000000, 0.8660254037844387076, 1.000000000000000000, 0.9330127018922194093, 0.9330127018922194093 ) ) 
 REPRESENTATION_ITEM ( '' )  );
#42618 = CARTESIAN_POINT ( 'NONE',  ( -1.339745962155613812, -11.20534180126147916, -5.000000000000000000 ) ) ;
#42619 = LINE ( 'NONE', #13353, #39924 ) ;
#42620 = CARTESIAN_POINT ( 'NONE',  ( -3.152548672688508926E-16, 10.18750000136559564, -5.148502694627439702 ) ) ;
#42621 = EDGE_LOOP ( 'NONE', ( #27555, #38508, #38801, #11281 ) ) ;
#42622 = CARTESIAN_POINT ( 'NONE',  ( 1.975475456537005874E-15, -65.74999999999998579, 5.000000000000000000 ) ) ;
#42623 = ORIENTED_EDGE ( 'NONE', *, *, #57131, .T. ) ;
#42624 = CARTESIAN_POINT ( 'NONE',  ( 2.071067811865459962, -167.9375000027312126, -5.000000000000015987 ) ) ;
#42625 = CARTESIAN_POINT ( 'NONE',  ( -2.229367062499996610, -47.14583333196774362, 3.861377020970582219 ) ) ;
#42626 = CARTESIAN_POINT ( 'NONE',  ( 3.152801135295367541, -160.5625000013656063, -3.152801135295367541 ) ) ;
#42627 = CARTESIAN_POINT ( 'NONE',  ( -4.999999999999999112, -44.79166666393547303, 2.886751345948131764 ) ) ;
#42628 = VERTEX_POINT ( 'NONE', #34231 ) ;
#42629 = CARTESIAN_POINT ( 'NONE',  ( 4.458734125000001214, -21.89583333196773296, 2.574251347313718519 ) ) ;
#42630 = ORIENTED_EDGE ( 'NONE', *, *, #29400, .T. ) ;
#42632 = DIRECTION ( 'NONE',  ( -1.000000000000000000, 0.000000000000000000, 0.000000000000000000 ) ) ;
#42631 = CARTESIAN_POINT ( 'NONE',  ( 2.499999999999998668, -34.33333333333332860, -4.330127018922193649 ) ) ;
#42633 = CARTESIAN_POINT ( 'NONE',  ( -1.846868145590737420, -159.7500000013656063, 4.458734124999999437 ) ) ;
#42634 = CARTESIAN_POINT ( 'NONE',  ( -6.972266317189433020E-16, -20.12499999726881228, -5.000000000000000000 ) ) ;
#42635 = CARTESIAN_POINT ( 'NONE',  ( -49.85088928181150436, -136.5625000000000284, -1.666127454062680702 ) ) ;
#42636 = CARTESIAN_POINT ( 'NONE',  ( 2.229367062499998831, -37.89583333196773651, -3.861377020970580887 ) ) ;
#42637 = EDGE_LOOP ( 'NONE', ( #44766, #50496, #53304, #30215, #17187, #6499, #49350, #5976, #59401, #42005, #56229, #12815, #52817, #17410, #8309, #8388, #31769, #21049, #11822, #48550, #1829, #13690, #17504, #4028, #37996, #51211, #29750, #53422, #59729, #50307, #16190, #14386, #55643, #51502, #16619, #18279, #18366, #21827, #24917, #8224, #55466, #58467, #19846, #6867, #28213, #34114, #49605, #59956, #23332, #22957, #43851, #52538, #17244, #39555, #28446, #17199, #12968, #26580, #24425, #26370, #30453, #18341, #3969, #46191, #39919, #22143, #45255, #43250, #15769, #28054, #8096, #18119, #5431, #30663, #15082, #24743, #33824, #8627, #50314, #43437, #60860, #11993, #48376, #3870, #31344, #62361, #52313, #62104, #36179, #29783, #55800, #58207, #18581, #31890, #53157, #35264, #45094, #3419, #31979, #32885, #62600, #488, #51521, #38499, #42709, #15268, #4511, #20528, #60153, #47567, #13058, #6182, #16259, #8248, #24092, #55648, #26975, #41998, #5127, #38681, #50055, #34670, #55143, #12214, #51253, #4872, #10429, #47459, #49741, #43306, #63587, #1847, #21520, #38664, #25425, #2308, #16450, #7986, #16981, #51040, #14411, #13311, #57929, #48017, #7620, #16145, #51749, #1801, #5614, #50756, #10359, #24045, #8677, #1349, #17203, #3343, #58193, #45814, #10627, #46176, #15846, #4661, #15662, #37153, #10492, #60130, #11456, #45750, #17169, #49252, #17510, #19842, #39226, #8232, #26842, #36472, #29573, #27709, #41042, #34790, #27204, #4389, #50788, #51758, #17864, #46870, #63237, #36057, #9551, #47203, #2712, #8817, #20155, #742, #63138, #632, #58103, #23508, #9328, #48023, #47766, #36209, #31795, #7328, #21480, #14627, #23600, #31085, #19447, #57833, #11290, #58909, #13708, #12088, #20242, #55375, #38296, #31254, #36397, #1456, #61, #19556, #48467, #31753, #26660, #43611, #39169, #59726, #52556, #58119, #52613, #52382, #59011, #23358, #10753, #5202, #15934, #32501, #24984, #6096, #245, #53397, #4374, #25772, #58383, #59579, #49704, #23710, #33264, #2831, #8798, #42870, #52882, #8004, #1195, #37807, #41282, #63606, #60550, #7109, #37757, #53905, #41208, #41847, #36831, #31717, #2297, #10695, #54431, #13365, #2455, #54872, #61355, #42886, #59987, #31469, #12661, #61318, #49744, #38573, #12379, #43181, #28924, #15233 ) ) ;
#42638 = CARTESIAN_POINT ( 'NONE',  ( 4.458734125000001214, -79.89583333196773651, 2.574251347313718519 ) ) ;
#42639 = CARTESIAN_POINT ( 'NONE',  ( 4.458734124999998549, 26.27083333469893134, -2.574251347313721627 ) ) ;
#42640 = CARTESIAN_POINT ( 'NONE',  ( 1.975475456537005874E-15, -12.62499999726881050, 5.000000000000000000 ) ) ;
#42641 = VERTEX_POINT ( 'NONE', #5300 ) ;
#42642 = AXIS2_PLACEMENT_3D ( 'NONE', #23662, #8009, #33620 ) ;
#42643 = FACE_OUTER_BOUND ( 'NONE', #11210, .T. ) ;
#42644 = CARTESIAN_POINT ( 'NONE',  ( -59.44456063193725015, -139.8125000013656063, -0.3552334253322034230 ) ) ;
#42645 = CARTESIAN_POINT ( 'NONE',  ( 2.229367062499998831, -84.89583333196773651, -3.861377020970580887 ) ) ;
#42646 = CARTESIAN_POINT ( 'NONE',  ( -55.39835681537999790, -132.0000000027312126, 4.984105922594378235 ) ) ;
#42647 = DIRECTION ( 'NONE',  ( 0.000000000000000000, 1.000000000000000000, 0.000000000000000000 ) ) ;
#42648 = CARTESIAN_POINT ( 'NONE',  ( 5.000000000000000000, -9.416666666666662522, -2.886751345948130876 ) ) ;
#42649 = CARTESIAN_POINT ( 'NONE',  ( 1.975475456537005874E-15, -44.62499999726880162, 5.000000000000000000 ) ) ;
#42650 = CARTESIAN_POINT ( 'NONE',  ( 4.458734124999999437, -54.81249999863440081, -5.460374474430324690E-16 ) ) ;
#42651 = CARTESIAN_POINT ( 'NONE',  ( 5.000000000000000000, 10.58333333333333393, -2.886751345948130876 ) ) ;
#42652 = CARTESIAN_POINT ( 'NONE',  ( -4.458734124999999437, 22.60416666803225993, -2.574251347313719407 ) ) ;
#42653 = CARTESIAN_POINT ( 'NONE',  ( 5.000000000000000888, -109.5833333333333286, 2.886751345948126879 ) ) ;
#42654 = AXIS2_PLACEMENT_3D ( 'NONE', #52610, #28157, #43256 ) ;
#42655 = CARTESIAN_POINT ( 'NONE',  ( -55.00000000000002132, -155.0000000000000284, 1.734723475976807094E-15 ) ) ;
#42656 = CARTESIAN_POINT ( 'NONE',  ( -4.458734124999998549, -42.47916666530107932, 2.574251347313722516 ) ) ;
#42657 = CARTESIAN_POINT ( 'NONE',  ( -2.500000000000000444, -5.041666663935480130, -4.330127018922193649 ) ) ;
#42658 = LINE ( 'NONE', #4065, #46895 ) ;
#42659 = CARTESIAN_POINT ( 'NONE',  ( -58.39396692619412477, -125.4375000013656063, 2.891590998281057701 ) ) ;
#42660 = CARTESIAN_POINT ( 'NONE',  ( -3.152548672688508926E-16, -82.81249999863442213, -5.148502694627439702 ) ) ;
#42661 = CARTESIAN_POINT ( 'NONE',  ( -4.458734124999997661, -100.2291666653010509, 2.574251347313722516 ) ) ;
#42662 = CARTESIAN_POINT ( 'NONE',  ( 2.229367062500001939, -7.229166665301073103, 3.861377020970579999 ) ) ;
#42663 =( BOUNDED_CURVE ( )  B_SPLINE_CURVE ( 2, ( #53132, #58896, #4246, #692, #14825, #20305, #13886, #48921, #9064 ),
 .UNSPECIFIED., .F., .F. ) 
 B_SPLINE_CURVE_WITH_KNOTS ( ( 3, 2, 2, 2, 3 ),
 ( 0.3482142857142856984, 0.3488095238095237915, 0.3499999999999999778, 0.3511904761904761640, 0.3517857142857143127 ),
 .UNSPECIFIED. ) 
 CURVE ( )  GEOMETRIC_REPRESENTATION_ITEM ( )  RATIONAL_B_SPLINE_CURVE ( ( 0.9330127018922194093, 0.9330127018922194093, 1.000000000000000000, 0.8660254037844387076, 1.000000000000000000, 0.8660254037844387076, 1.000000000000000000, 0.9330127018922163007, 0.9330127018922194093 ) ) 
 REPRESENTATION_ITEM ( '' )  );
#42664 = EDGE_LOOP ( 'NONE', ( #15963, #36488, #8548, #44759 ) ) ;
#42665 = CARTESIAN_POINT ( 'NONE',  ( -3.152548672688508926E-16, -92.56249999863439371, -5.148502694627439702 ) ) ;
#42666 = CARTESIAN_POINT ( 'NONE',  ( 5.000000000000000888, -167.0625000027311842, -2.071067811865475505 ) ) ;
#42667 = CARTESIAN_POINT ( 'NONE',  ( 4.458734125000001214, -94.14583333196773651, 2.574251347313718519 ) ) ;
#42668 = CARTESIAN_POINT ( 'NONE',  ( -2.500000000000000444, -16.16666666666666785, -4.330127018922193649 ) ) ;
#42669 = CARTESIAN_POINT ( 'NONE',  ( -57.19623071787017210, -128.3750000013656631, 4.297418129356382899 ) ) ;
#42670 = CARTESIAN_POINT ( 'NONE',  ( -4.458734124999997661, -13.22916666530107399, 2.574251347313722516 ) ) ;
#42671 = CARTESIAN_POINT ( 'NONE',  ( 2.229367062500001939, 10.77083333469892956, 3.861377020970579999 ) ) ;
#42672 = CARTESIAN_POINT ( 'NONE',  ( -4.458734124999997661, -54.47916666530107932, 2.574251347313722516 ) ) ;
#42673 = CARTESIAN_POINT ( 'NONE',  ( -5.000000000000000000, -19.99999999999999645, 0.000000000000000000 ) ) ;
#42674 = CARTESIAN_POINT ( 'NONE',  ( 2.500000000000002220, 17.33333333333333215, 4.330127018922192761 ) ) ;
#42675 = CARTESIAN_POINT ( 'NONE',  ( 9.457646018065525792E-16, -10.06249999863440614, 5.148502694627439702 ) ) ;
#42676 = VERTEX_POINT ( 'NONE', #58379 ) ;
#42677 = CARTESIAN_POINT ( 'NONE',  ( -2.229367062500000163, -37.72916666530107221, -3.861377020970580443 ) ) ;
#42678 = CARTESIAN_POINT ( 'NONE',  ( -50.40829686548195099, -127.2500000013656347, -1.485763867205728284 ) ) ;
#42679 = CARTESIAN_POINT ( 'NONE',  ( 1.339745962155615144, -76.70534180126148271, 4.999999999999999112 ) ) ;
#42680 = CARTESIAN_POINT ( 'NONE',  ( -6.972266317189433020E-16, 9.750000000000000000, -5.000000000000000000 ) ) ;
#42681 = CARTESIAN_POINT ( 'NONE',  ( 4.458734125000001214, -81.89583333196773651, 2.574251347313718519 ) ) ;
#42682 = CARTESIAN_POINT ( 'NONE',  ( -4.458734124999999437, 24.35416666803225993, -2.574251347313719407 ) ) ;
#42683 = CARTESIAN_POINT ( 'NONE',  ( -2.229367062499996610, 16.85416666803225993, 3.861377020970582219 ) ) ;
#42684 = DIRECTION ( 'NONE',  ( -0.000000000000000000, 1.000000000000000000, -0.000000000000000000 ) ) ;
#42685 = FACE_OUTER_BOUND ( 'NONE', #49383, .T. ) ;
#42686 = CARTESIAN_POINT ( 'NONE',  ( 4.458734124999998549, -81.97916666530106511, -2.574251347313721627 ) ) ;
#42687 = CARTESIAN_POINT ( 'NONE',  ( -5.000000000000000000, -69.08333333333332860, -2.886751345948128211 ) ) ;
#42688 = CARTESIAN_POINT ( 'NONE',  ( 2.500000000000002220, 11.45833333606451809, 4.330127018922192761 ) ) ;
#42689 = EDGE_LOOP ( 'NONE', ( #50642, #58545, #48780, #24429 ) ) ;
#42690 = CARTESIAN_POINT ( 'NONE',  ( 1.339745962155615144, -25.70534180126147916, 4.999999999999999112 ) ) ;
#42691 =( BOUNDED_CURVE ( )  B_SPLINE_CURVE ( 2, ( #21350, #1114, #788, #56082, #55765, #50616, #20721, #10739, #26169 ),
 .UNSPECIFIED., .F., .F. ) 
 B_SPLINE_CURVE_WITH_KNOTS ( ( 3, 2, 2, 2, 3 ),
 ( 0.09464285714285713969, 0.09523809523809523281, 0.09642857142857143293, 0.09761904761904761918, 0.09821428571428571230 ),
 .UNSPECIFIED. ) 
 CURVE ( )  GEOMETRIC_REPRESENTATION_ITEM ( )  RATIONAL_B_SPLINE_CURVE ( ( 0.9330127018922194093, 0.9330127018922194093, 1.000000000000000000, 0.8660254037844387076, 1.000000000000000000, 0.8660254037844387076, 1.000000000000000000, 0.9330127018922194093, 0.9330127018922194093 ) ) 
 REPRESENTATION_ITEM ( '' )  );
#42692 = DIRECTION ( 'NONE',  ( 0.000000000000000000, 0.000000000000000000, 1.000000000000000000 ) ) ;
#42694 = CARTESIAN_POINT ( 'NONE',  ( 5.000000000000000000, -31.41666666666667140, -2.886751345948129988 ) ) ;
#42693 = CARTESIAN_POINT ( 'NONE',  ( -1.339745962155727277, -108.6696581960073331, 4.999999999999933387 ) ) ;
#42695 = CARTESIAN_POINT ( 'NONE',  ( -4.458734124999999437, -31.39583333196773296, -2.574251347313719407 ) ) ;
#42696 = DIRECTION ( 'NONE',  ( -0.000000000000000000, 1.000000000000000000, -0.000000000000000000 ) ) ;
#42697 = CARTESIAN_POINT ( 'NONE',  ( -2.499999999999996447, -26.70833333060214798, 4.330127018922195425 ) ) ;
#42699 = EDGE_LOOP ( 'NONE', ( #19114, #7047, #39943, #60929 ) ) ;
#42698 = CARTESIAN_POINT ( 'NONE',  ( 4.458734125000001214, -59.89583333196774362, 2.574251347313718519 ) ) ;
#42700 = CARTESIAN_POINT ( 'NONE',  ( 1.339745962155612702, -62.16965819600734022, -5.000000000000000000 ) ) ;
#42702 = ORIENTED_EDGE ( 'NONE', *, *, #17376, .F. ) ;
#42701 = CARTESIAN_POINT ( 'NONE',  ( 4.458734124999999437, -7.062499998634404363, -5.460374474430324690E-16 ) ) ;
#42703 = CARTESIAN_POINT ( 'NONE',  ( -4.999999999999999112, -74.91666666666665719, 2.886751345948131764 ) ) ;
#42704 = CARTESIAN_POINT ( 'NONE',  ( 1.339745962155613146, 28.83034180399266688, -4.999999999999999112 ) ) ;
#42705 = CARTESIAN_POINT ( 'NONE',  ( -2.229367062500000163, -52.72916666530107221, -3.861377020970580443 ) ) ;
#42706 =( BOUNDED_CURVE ( )  B_SPLINE_CURVE ( 2, ( #51380, #17600, #7322, #17900, #26932, #46549, #57163, #62615, #43590 ),
 .UNSPECIFIED., .F., .F. ) 
 B_SPLINE_CURVE_WITH_KNOTS ( ( 3, 2, 2, 2, 3 ),
 ( 0.02500000000000002220, 0.02916666666666669488, 0.03333333333333336757, 0.03750000000000003331, 0.04166666666666670599 ),
 .UNSPECIFIED. ) 
 CURVE ( )  GEOMETRIC_REPRESENTATION_ITEM ( )  RATIONAL_B_SPLINE_CURVE ( ( 0.9999999999999996669, 0.9238795325112870716, 1.000000000000000000, 0.9238795325112867385, 1.000000000000000000, 0.9238795325112867385, 1.000000000000000000, 0.9238795325112859613, 1.000000000000000666 ) ) 
 REPRESENTATION_ITEM ( '' )  );
#42707 = CARTESIAN_POINT ( 'NONE',  ( 5.000000000000000000, -78.37499999726881583, -6.123233995736766282E-16 ) ) ;
#42709 = ORIENTED_EDGE ( 'NONE', *, *, #14593, .T. ) ;
#42708 = CARTESIAN_POINT ( 'NONE',  ( -6.972266317189433020E-16, -65.12499999726880162, -5.000000000000000000 ) ) ;
#42710 = CARTESIAN_POINT ( 'NONE',  ( -51.75738570946856498, -149.7500000000000284, 3.805975901505576964 ) ) ;
#42711 = CARTESIAN_POINT ( 'NONE',  ( 4.458734125000001214, -21.14583333196774362, 2.574251347313718519 ) ) ;
#42713 = ORIENTED_EDGE ( 'NONE', *, *, #21285, .F. ) ;
#42712 = CARTESIAN_POINT ( 'NONE',  ( -4.458734124999999437, -59.56249999863440081, 0.000000000000000000 ) ) ;
#42714 = FILL_AREA_STYLE_COLOUR ( '', #57500 ) ;
#42715 = CARTESIAN_POINT ( 'NONE',  ( -1.846868145590734756, -169.3750000013656347, -4.458734125000000326 ) ) ;
#42716 = CARTESIAN_POINT ( 'NONE',  ( 4.458734125000001214, -98.14583333196773651, 2.574251347313718519 ) ) ;
#42717 = CARTESIAN_POINT ( 'NONE',  ( -3.535533905932737309, -167.7500000027312126, -3.535533905932738197 ) ) ;
#42718 = VERTEX_POINT ( 'NONE', #48401 ) ;
#42719 = CARTESIAN_POINT ( 'NONE',  ( -51.60603307380591787, -150.1875000013656063, -2.891590998281053704 ) ) ;
#42720 = CARTESIAN_POINT ( 'NONE',  ( -55.39835681537999790, -144.0000000027312126, 4.984105922594378235 ) ) ;
#42721 = DIRECTION ( 'NONE',  ( -0.000000000000000000, 1.000000000000000000, -0.000000000000000000 ) ) ;
#42722 = CARTESIAN_POINT ( 'NONE',  ( 2.229367062500001939, -5.979166665301072214, 3.861377020970579999 ) ) ;
#42723 = CARTESIAN_POINT ( 'NONE',  ( 4.458734124999998549, -95.97916666530107932, -2.574251347313721627 ) ) ;
#42724 = CARTESIAN_POINT ( 'NONE',  ( 3.152801135295367541, -143.5625000013655779, -3.152801135295367541 ) ) ;
#42725 = CARTESIAN_POINT ( 'NONE',  ( 4.458734124999999437, -29.06249999863440436, -5.460374474430324690E-16 ) ) ;
#42726 = CARTESIAN_POINT ( 'NONE',  ( -9.184850993605147944E-16, -163.3750000027311842, 5.000000000000000000 ) ) ;
#42727 = CARTESIAN_POINT ( 'NONE',  ( -53.51423613279429503, -135.2500000013656347, 4.591703134518082763 ) ) ;
#42728 = CARTESIAN_POINT ( 'NONE',  ( 2.229367062500001939, -70.22916666530107932, 3.861377020970579999 ) ) ;
#42729 = CARTESIAN_POINT ( 'NONE',  ( -2.500000000000000444, -91.16666666666665719, -4.330127018922193649 ) ) ;
#42730 = CARTESIAN_POINT ( 'NONE',  ( 2.500000000000002220, -88.54166666393548724, 4.330127018922192761 ) ) ;
#42731 = CARTESIAN_POINT ( 'NONE',  ( -1.846868145590734756, -141.1250000013656063, -4.458734124999999437 ) ) ;
#42732 = CARTESIAN_POINT ( 'NONE',  ( 2.229367062499998831, 8.104166668032261711, -3.861377020970580887 ) ) ;
#42733 = EDGE_LOOP ( 'NONE', ( #62214, #48861, #31191, #58389 ) ) ;
#42734 = AXIS2_PLACEMENT_3D ( 'NONE', #6953, #51962, #17556 ) ;
#42735 = LINE ( 'NONE', #51463, #21267 ) ;
#42736 = CARTESIAN_POINT ( 'NONE',  ( -5.000000000000000888, -144.4375000000000000, 2.071067811865474617 ) ) ;
#42738 = CARTESIAN_POINT ( 'NONE',  ( 4.458734124999999437, -25.81249999863440792, -5.460374474430324690E-16 ) ) ;
#42737 = CARTESIAN_POINT ( 'NONE',  ( 5.000000000000000000, -90.50000000000000000, -6.123233995736766282E-16 ) ) ;
#42739 = DIRECTION ( 'NONE',  ( -0.6485228581062916220, 0.000000000000000000, -0.7611951803011147710 ) ) ;
#42740 = CARTESIAN_POINT ( 'NONE',  ( -3.152548672688508926E-16, -78.81249999863440792, -5.148502694627439702 ) ) ;
#42741 = VECTOR ( 'NONE', #7092, 1000.000000000000000 ) ;
#42742 = CARTESIAN_POINT ( 'NONE',  ( 4.458734124999999437, 22.93750000136559564, -5.460374474430324690E-16 ) ) ;
#42743 = CARTESIAN_POINT ( 'NONE',  ( 1.975475456537005874E-15, -34.75000000000000000, 5.000000000000000000 ) ) ;
#42744 = VECTOR ( 'NONE', #36665, 1000.000000000000000 ) ;
#42745 = CARTESIAN_POINT ( 'NONE',  ( -59.44456063193725015, -146.5625000013656063, -0.3552334253322034230 ) ) ;
#42746 = CARTESIAN_POINT ( 'NONE',  ( -4.458734124999999437, 4.687500001365595637, 0.000000000000000000 ) ) ;
#42747 = LINE ( 'NONE', #14106, #63321 ) ;
#42748 = CARTESIAN_POINT ( 'NONE',  ( 2.229367062500001939, -36.22916666530107221, 3.861377020970579999 ) ) ;
#42749 = CARTESIAN_POINT ( 'NONE',  ( -2.500000000000000444, -4.041666663935479242, -4.330127018922193649 ) ) ;
#42750 = CARTESIAN_POINT ( 'NONE',  ( 4.458734124999999437, 9.187500001365592084, -5.460374474430324690E-16 ) ) ;
#42751 = CARTESIAN_POINT ( 'NONE',  ( -4.458734124999998549, -71.22916666530106511, 2.574251347313722516 ) ) ;
#42752 = CARTESIAN_POINT ( 'NONE',  ( 4.458734124999998549, -21.97916666530107221, -2.574251347313721627 ) ) ;
#42753 = CARTESIAN_POINT ( 'NONE',  ( -2.500000000000000444, -8.166666666666669627, -4.330127018922193649 ) ) ;
#42754 = CARTESIAN_POINT ( 'NONE',  ( 4.458734125000000326, -161.3750000013656063, -1.846868145590734978 ) ) ;
#42755 = CARTESIAN_POINT ( 'NONE',  ( 2.499999999999998668, 15.79166666939785202, -4.330127018922193649 ) ) ;
#42756 = CARTESIAN_POINT ( 'NONE',  ( -3.152548672688508926E-16, -65.56249999863440792, -5.148502694627439702 ) ) ;
#42757 = CARTESIAN_POINT ( 'NONE',  ( 5.000000000000000888, -98.45833333060213022, 2.886751345948126879 ) ) ;
#42758 = EDGE_CURVE ( 'NONE', #16611, #15979, #42968, .T. ) ;
#42759 = CARTESIAN_POINT ( 'NONE',  ( 4.458734124999998549, 29.27083333469892423, -2.574251347313721627 ) ) ;
#42760 = CARTESIAN_POINT ( 'NONE',  ( -4.458734124999999437, -41.31249999863440081, 0.000000000000000000 ) ) ;
#42761 = DIRECTION ( 'NONE',  ( -0.000000000000000000, 1.000000000000000000, -0.000000000000000000 ) ) ;
#42762 = CARTESIAN_POINT ( 'NONE',  ( -2.229367062500000163, -103.7291666653010651, -3.861377020970580443 ) ) ;
#42763 = CARTESIAN_POINT ( 'NONE',  ( 4.458734125000000326, -67.14583333196773651, 2.574251347313718519 ) ) ;
#42764 = CARTESIAN_POINT ( 'NONE',  ( 2.499999999999998668, -53.33333333333332860, -4.330127018922193649 ) ) ;
#42765 = CARTESIAN_POINT ( 'NONE',  ( 2.500000000000002220, -57.54166666393548013, 4.330127018922192761 ) ) ;
#42766 = DIRECTION ( 'NONE',  ( 1.000000000000000000, 0.000000000000000000, 3.614007241618347908E-17 ) ) ;
#42767 = ORIENTED_EDGE ( 'NONE', *, *, #20327, .F. ) ;
#42768 = DIRECTION ( 'NONE',  ( -0.000000000000000000, 1.000000000000000000, -0.000000000000000000 ) ) ;
#42769 = CARTESIAN_POINT ( 'NONE',  ( -2.916731409357579869E-14, 13.25000000000000178, 5.000000000000000888 ) ) ;
#42770 = CARTESIAN_POINT ( 'NONE',  ( -5.000000000000000000, -14.08333333333333037, -2.886751345948128211 ) ) ;
#42771 = CARTESIAN_POINT ( 'NONE',  ( -2.229367062499996610, -18.14583333196773651, 3.861377020970582219 ) ) ;
#42772 = CARTESIAN_POINT ( 'NONE',  ( 2.229367062500001939, -74.97916666530106511, 3.861377020970579999 ) ) ;
#42773 = CARTESIAN_POINT ( 'NONE',  ( -6.972266317189433020E-16, 19.87500000273118417, -5.000000000000000000 ) ) ;
#42774 = EDGE_CURVE ( 'NONE', #28458, #55065, #24935, .T. ) ;
#42775 = CARTESIAN_POINT ( 'NONE',  ( -5.000000000000000000, -11.87499999726881761, 0.000000000000000000 ) ) ;
#42777 = ORIENTED_EDGE ( 'NONE', *, *, #51450, .T. ) ;
#42776 = CARTESIAN_POINT ( 'NONE',  ( -2.229367062499996610, -45.14583333196774362, 3.861377020970582219 ) ) ;
#42778 = CARTESIAN_POINT ( 'NONE',  ( 5.000000000000000888, -41.58333333333333570, 2.886751345948126879 ) ) ;
#42779 = ADVANCED_FACE ( 'NONE', ( #19123 ), #59983, .T. ) ;
#42781 = ORIENTED_EDGE ( 'NONE', *, *, #14917, .T. ) ;
#42780 = CARTESIAN_POINT ( 'NONE',  ( 9.457646018065525792E-16, 7.687500001365596525, 5.148502694627439702 ) ) ;
#42782 = CARTESIAN_POINT ( 'NONE',  ( 6.123233995736766282E-16, -170.0000000000000000, -5.000000000000000000 ) ) ;
#42783 = CARTESIAN_POINT ( 'NONE',  ( 2.500000000000002220, -63.66666666666666430, 4.330127018922192761 ) ) ;
#42784 = CARTESIAN_POINT ( 'NONE',  ( 4.458734124999999437, -158.6875000013655779, 0.000000000000000000 ) ) ;
#42785 = CARTESIAN_POINT ( 'NONE',  ( -4.458734124999998549, -34.47916666530107221, 2.574251347313722516 ) ) ;
#42786 = CARTESIAN_POINT ( 'NONE',  ( -58.24261429053147765, -149.3750000027312126, -3.805975901505573855 ) ) ;
#42787 = AXIS2_PLACEMENT_3D ( 'NONE', #49697, #5641, #8111 ) ;
#42788 = CARTESIAN_POINT ( 'NONE',  ( 5.000000000000000000, -165.0000000000000000, 0.000000000000000000 ) ) ;
#42789 = CARTESIAN_POINT ( 'NONE',  ( 6.123233995736766282E-16, -170.0000000000000000, -5.000000000000000000 ) ) ;
#42790 = CARTESIAN_POINT ( 'NONE',  ( -57.89159099828107458, -132.9375000013656063, -3.393966926194107447 ) ) ;
#42791 = VECTOR ( 'NONE', #16690, 1000.000000000000000 ) ;
#42792 = CARTESIAN_POINT ( 'NONE',  ( -2.229367062500000163, -6.729166665301073103, -3.861377020970580443 ) ) ;
#42793 = ADVANCED_FACE ( 'NONE', ( #25873 ), #31324, .T. ) ;
#42794 = AXIS2_PLACEMENT_3D ( 'NONE', #38076, #8800, #42888 ) ;
#42795 = CARTESIAN_POINT ( 'NONE',  ( 9.457646018065525792E-16, -40.31249999863440081, 5.148502694627439702 ) ) ;
#42796 =( BOUNDED_CURVE ( )  B_SPLINE_CURVE ( 2, ( #27149, #52226, #41931, #27454, #26840, #3348, #22965, #12978, #17508 ),
 .UNSPECIFIED., .F., .F. ) 
 B_SPLINE_CURVE_WITH_KNOTS ( ( 3, 2, 2, 2, 3 ),
 ( 0.7062500000000000444, 0.7069444444444444864, 0.7083333333333333703, 0.7097222222222222543, 0.7104166666666666963 ),
 .UNSPECIFIED. ) 
 CURVE ( )  GEOMETRIC_REPRESENTATION_ITEM ( )  RATIONAL_B_SPLINE_CURVE ( ( 0.9330127018922194093, 0.9330127018922194093, 1.000000000000000000, 0.8660254037844387076, 1.000000000000000000, 0.8660254037844387076, 1.000000000000000000, 0.9330127018922194093, 0.9330127018922194093 ) ) 
 REPRESENTATION_ITEM ( '' )  );
#42797 = CARTESIAN_POINT ( 'NONE',  ( -1.339745962155613812, -25.08034179853028789, -5.000000000000000000 ) ) ;
#42798 = CARTESIAN_POINT ( 'NONE',  ( 9.457646018065525792E-16, -86.31249999863440792, 5.148502694627439702 ) ) ;
#42799 = CARTESIAN_POINT ( 'NONE',  ( -6.972266317189433020E-16, -108.2499999999999858, -5.000000000000000000 ) ) ;
#42800 = VERTEX_POINT ( 'NONE', #16856 ) ;
#42801 = CARTESIAN_POINT ( 'NONE',  ( 1.975475456537005874E-15, -94.62499999726880162, 5.000000000000000000 ) ) ;
#42802 = CARTESIAN_POINT ( 'NONE',  ( -5.000000000000000000, -11.95833333060214798, -2.886751345948128211 ) ) ;
#42803 = CARTESIAN_POINT ( 'NONE',  ( -4.458734124999998549, -67.47916666530106511, 2.574251347313722516 ) ) ;
#42804 = CARTESIAN_POINT ( 'NONE',  ( -3.152801135295367985, -148.0625000013655779, 3.152801135295367096 ) ) ;
#42805 = ORIENTED_EDGE ( 'NONE', *, *, #12741, .T. ) ;
#42806 = EDGE_CURVE ( 'NONE', #727, #22078, #50316, .T. ) ;
#42807 = CARTESIAN_POINT ( 'NONE',  ( 4.458734125000001214, -11.14583333196774007, 2.574251347313718519 ) ) ;
#42808 = DIRECTION ( 'NONE',  ( 0.000000000000000000, 0.000000000000000000, 1.000000000000000000 ) ) ;
#42809 = CARTESIAN_POINT ( 'NONE',  ( -2.229367062499996610, 3.854166668032260823, 3.861377020970582219 ) ) ;
#42810 = CARTESIAN_POINT ( 'NONE',  ( 1.339745962155612702, -30.16965819600732956, -5.000000000000000000 ) ) ;
#42811 = CARTESIAN_POINT ( 'NONE',  ( 4.458734124999997661, -153.5000000013656063, 1.846868145590737864 ) ) ;
#42812 = CARTESIAN_POINT ( 'NONE',  ( 4.458734124999998549, 28.02083333469893134, -2.574251347313721627 ) ) ;
#42813 = ORIENTED_EDGE ( 'NONE', *, *, #42564, .T. ) ;
#42814 = CARTESIAN_POINT ( 'NONE',  ( 2.229367062499998831, -94.64583333196773651, -3.861377020970580887 ) ) ;
#42815 = CARTESIAN_POINT ( 'NONE',  ( -5.000000000000000000, -31.08333333333332860, -2.886751345948128211 ) ) ;
#42816 = CARTESIAN_POINT ( 'NONE',  ( -5.000000000000000000, -63.00000000000000000, 0.000000000000000000 ) ) ;
#42817 = CARTESIAN_POINT ( 'NONE',  ( 2.229367062500001939, -7.979166665301073991, 3.861377020970579999 ) ) ;
#42818 = CARTESIAN_POINT ( 'NONE',  ( 5.000000000000000000, -51.50000000000000711, -6.123233995736766282E-16 ) ) ;
#42819 = CARTESIAN_POINT ( 'NONE',  ( -6.972266317189433020E-16, 14.74999999999999822, -5.000000000000000000 ) ) ;
#42820 = CARTESIAN_POINT ( 'NONE',  ( 5.000000000000000000, -34.37499999726881583, -6.123233995736766282E-16 ) ) ;
#42821 = DIRECTION ( 'NONE',  ( 0.000000000000000000, 0.000000000000000000, 1.000000000000000000 ) ) ;
#42822 = CARTESIAN_POINT ( 'NONE',  ( 2.229367062499998831, 20.35416666803225993, -3.861377020970580887 ) ) ;
#42823 = CARTESIAN_POINT ( 'NONE',  ( -1.339745962155610925, -97.66965819600733312, 5.000000000000000000 ) ) ;
#42824 = CARTESIAN_POINT ( 'NONE',  ( 4.458734125000000326, 23.10416666803225993, 2.574251347313718519 ) ) ;
#42825 = CARTESIAN_POINT ( 'NONE',  ( 4.458734124999999437, -58.81249999863440081, -5.460374474430324690E-16 ) ) ;
#42826 = CARTESIAN_POINT ( 'NONE',  ( -4.458734124999997661, -5.479166665301072214, 2.574251347313722516 ) ) ;
#42827 = AXIS2_PLACEMENT_3D ( 'NONE', #1410, #21010, #55741 ) ;
#42828 = CARTESIAN_POINT ( 'NONE',  ( 6.123233995736766282E-16, -170.0000000000000000, -5.000000000000000000 ) ) ;
#42829 = CARTESIAN_POINT ( 'NONE',  ( 5.000000000000000888, 7.416666666666665186, 2.886751345948126879 ) ) ;
#42830 = CARTESIAN_POINT ( 'NONE',  ( -2.071067811865478170, -142.4375000027311842, 5.000000000000000000 ) ) ;
#42831 = CARTESIAN_POINT ( 'NONE',  ( -58.24261429053147765, -145.3750000027312126, -3.805975901505573855 ) ) ;
#42832 = CARTESIAN_POINT ( 'NONE',  ( 9.457646018065525792E-16, -49.06249999863440792, 5.148502694627439702 ) ) ;
#42833 = CARTESIAN_POINT ( 'NONE',  ( 5.000000000000000000, -86.29166666393547303, -2.886751345948129988 ) ) ;
#42834 = EDGE_CURVE ( 'NONE', #800, #22037, #49165, .T. ) ;
#42835 = VECTOR ( 'NONE', #17751, 1000.000000000000000 ) ;
#42836 = CARTESIAN_POINT ( 'NONE',  ( -56.48576386720575471, -136.0000000013656063, -4.591703134518078322 ) ) ;
#42837 = CARTESIAN_POINT ( 'NONE',  ( -4.999999999999998224, -16.91666666666666430, 2.886751345948131764 ) ) ;
#42838 = CARTESIAN_POINT ( 'NONE',  ( -51.19402409849444524, -145.5000000000000284, -3.242614290531456334 ) ) ;
#42839 = AXIS2_PLACEMENT_3D ( 'NONE', #53590, #48131, #18852 ) ;
#42840 = CARTESIAN_POINT ( 'NONE',  ( 4.458734124999999437, -89.06249999863439371, -5.460374474430324690E-16 ) ) ;
#42841 = CARTESIAN_POINT ( 'NONE',  ( -4.458734125000000326, -158.1250000013656063, 1.846868145590734089 ) ) ;
#42842 =( BOUNDED_CURVE ( )  B_SPLINE_CURVE ( 2, ( #54143, #38407, #49644, #4315, #28748, #44489, #58660, #5581, #59296 ),
 .UNSPECIFIED., .F., .F. ) 
 B_SPLINE_CURVE_WITH_KNOTS ( ( 3, 2, 2, 2, 3 ),
 ( 0.6187500000000000222, 0.6194444444444444642, 0.6208333333333333481, 0.6222222222222222321, 0.6229166666666666741 ),
 .UNSPECIFIED. ) 
 CURVE ( )  GEOMETRIC_REPRESENTATION_ITEM ( )  RATIONAL_B_SPLINE_CURVE ( ( 0.9330127018922194093, 0.9330127018922194093, 1.000000000000000000, 0.8660254037844387076, 1.000000000000000000, 0.8660254037844387076, 1.000000000000000000, 0.9330127018922194093, 0.9330127018922194093 ) ) 
 REPRESENTATION_ITEM ( '' )  );
#42843 = CARTESIAN_POINT ( 'NONE',  ( -4.999999999999999112, -38.91666666666667140, 2.886751345948131764 ) ) ;
#42844 = ORIENTED_EDGE ( 'NONE', *, *, #56295, .T. ) ;
#42845 = CARTESIAN_POINT ( 'NONE',  ( 4.458734124999998549, 20.02083333469892779, -2.574251347313721627 ) ) ;
#42846 = EDGE_LOOP ( 'NONE', ( #19836, #42458, #665, #34913 ) ) ;
#42847 = CARTESIAN_POINT ( 'NONE',  ( 9.457646018065525792E-16, -97.06249999863439371, 5.148502694627439702 ) ) ;
#42848 = CARTESIAN_POINT ( 'NONE',  ( -3.152548672688508926E-16, 6.187500001365593860, -5.148502694627439702 ) ) ;
#42849 = CARTESIAN_POINT ( 'NONE',  ( 5.000000000000000000, 9.625000002731184168, -6.123233995736766282E-16 ) ) ;
#42850 = CARTESIAN_POINT ( 'NONE',  ( -2.500000000000000444, -35.04166666393547303, -4.330127018922193649 ) ) ;
#42851 = CARTESIAN_POINT ( 'NONE',  ( 2.499999999999998668, 2.666666666666667851, -4.330127018922193649 ) ) ;
#42852 = CARTESIAN_POINT ( 'NONE',  ( 4.458734124999998549, -63.72916666530106511, -2.574251347313721627 ) ) ;
#42853 = DIRECTION ( 'NONE',  ( 0.000000000000000000, 0.000000000000000000, 1.000000000000000000 ) ) ;
#42854 = CARTESIAN_POINT ( 'NONE',  ( 4.458734124999998549, -26.72916666530106866, -2.574251347313721627 ) ) ;
#42855 = EDGE_CURVE ( 'NONE', #721, #53022, #31508, .T. ) ;
#42856 = FACE_OUTER_BOUND ( 'NONE', #38207, .T. ) ;
#42857 = CARTESIAN_POINT ( 'NONE',  ( 5.000000000000000000, -42.49999999999999289, -6.123233995736766282E-16 ) ) ;
#42858 = CARTESIAN_POINT ( 'NONE',  ( -6.972266317189433020E-16, 5.749999999999999112, -5.000000000000000000 ) ) ;
#42860 = CARTESIAN_POINT ( 'NONE',  ( -2.229367062500000163, -19.72916666530107221, -3.861377020970580443 ) ) ;
#42859 = CARTESIAN_POINT ( 'NONE',  ( 1.975475456537005874E-15, -9.750000000000000000, 5.000000000000000000 ) ) ;
#42861 = CARTESIAN_POINT ( 'NONE',  ( 5.000000000000000888, -154.9375000000000000, -2.071067811865475505 ) ) ;
#42862 = CARTESIAN_POINT ( 'NONE',  ( -4.458734124999998549, -63.22916666530106511, 2.574251347313722516 ) ) ;
#42863 = CARTESIAN_POINT ( 'NONE',  ( -4.458734124999999437, -147.1875000013656063, -5.460374474430324690E-16 ) ) ;
#42864 = CARTESIAN_POINT ( 'NONE',  ( -3.152548672688508926E-16, -76.56249999863440792, -5.148502694627439702 ) ) ;
#42865 = CARTESIAN_POINT ( 'NONE',  ( -56.48576386720575471, -144.0000000013656063, -4.591703134518078322 ) ) ;
#42866 = CARTESIAN_POINT ( 'NONE',  ( 4.458734124999999437, -24.06249999863440436, -5.460374474430324690E-16 ) ) ;
#42867 = CARTESIAN_POINT ( 'NONE',  ( 2.500000000000002220, -65.54166666393547303, 4.330127018922192761 ) ) ;
#42868 = VERTEX_POINT ( 'NONE', #35849 ) ;
#42869 = CARTESIAN_POINT ( 'NONE',  ( -6.972266317189433020E-16, -22.24999999999999645, -5.000000000000000000 ) ) ;
#42870 = ORIENTED_EDGE ( 'NONE', *, *, #3233, .T. ) ;
#42871 = CARTESIAN_POINT ( 'NONE',  ( -3.152548672688508926E-16, -68.81249999863439371, -5.148502694627439702 ) ) ;
#42872 = CARTESIAN_POINT ( 'NONE',  ( 3.535533905932738197, -149.0000000027311842, -3.535533905932738197 ) ) ;
#42873 = CARTESIAN_POINT ( 'NONE',  ( -1.339745962155610925, -5.669658196007334006, 5.000000000000000000 ) ) ;
#42874 = VERTEX_POINT ( 'NONE', #21698 ) ;
#42875 = DIRECTION ( 'NONE',  ( -0.000000000000000000, 1.000000000000000000, -0.000000000000000000 ) ) ;
#42876 = CARTESIAN_POINT ( 'NONE',  ( -3.152548672688508926E-16, -53.81249999863439371, -5.148502694627439702 ) ) ;
#42877 = VECTOR ( 'NONE', #17064, 1000.000000000000000 ) ;
#42878 = CARTESIAN_POINT ( 'NONE',  ( -4.458734124999999437, -0.5624999986344053626, 0.000000000000000000 ) ) ;
#42879 = ORIENTED_EDGE ( 'NONE', *, *, #10976, .T. ) ;
#42880 = DIRECTION ( 'NONE',  ( -0.000000000000000000, 1.000000000000000000, -0.000000000000000000 ) ) ;
#42881 = CARTESIAN_POINT ( 'NONE',  ( -4.458734124999999437, 4.604166668032261711, -2.574251347313719407 ) ) ;
#42882 = CARTESIAN_POINT ( 'NONE',  ( 4.458734124999998549, 18.27083333469893134, -2.574251347313721627 ) ) ;
#42883 = CARTESIAN_POINT ( 'NONE',  ( -57.19623071787017210, -143.3750000013656063, 4.297418129356382899 ) ) ;
#42884 = CARTESIAN_POINT ( 'NONE',  ( -4.458734125000000326, -167.8750000013656063, 1.846868145590734089 ) ) ;
#42885 =( BOUNDED_CURVE ( )  B_SPLINE_CURVE ( 2, ( #2023, #2331, #7783, #27386, #56041, #60238, #41536, #26441, #35783 ),
 .UNSPECIFIED., .F., .F. ) 
 B_SPLINE_CURVE_WITH_KNOTS ( ( 3, 2, 2, 2, 3 ),
 ( 0.5250000000000004663, 0.5291666666666671182, 0.5333333333333338810, 0.5375000000000005329, 0.5416666666666671848 ),
 .UNSPECIFIED. ) 
 CURVE ( )  GEOMETRIC_REPRESENTATION_ITEM ( )  RATIONAL_B_SPLINE_CURVE ( ( 0.9999999999999918954, 0.9238795325112948431, 1.000000000000000000, 0.9238795325112867385, 1.000000000000000000, 0.9238795325112867385, 1.000000000000000000, 0.9238795325112766355, 1.000000000000010214 ) ) 
 REPRESENTATION_ITEM ( '' )  );
#42886 = ORIENTED_EDGE ( 'NONE', *, *, #9170, .T. ) ;
#42887 = CARTESIAN_POINT ( 'NONE',  ( 4.458734124999999437, -74.81249999863440792, -5.460374474430324690E-16 ) ) ;
#42888 = DIRECTION ( 'NONE',  ( 0.000000000000000000, 0.000000000000000000, 1.000000000000000000 ) ) ;
#42889 = CARTESIAN_POINT ( 'NONE',  ( -4.458734124999999437, 9.687500001365593860, 0.000000000000000000 ) ) ;
#42890 = CARTESIAN_POINT ( 'NONE',  ( -2.499999999999996447, -88.83333333333332860, 4.330127018922195425 ) ) ;
#42891 = CARTESIAN_POINT ( 'NONE',  ( -3.152548672688508926E-16, -57.81249999863440081, -5.148502694627439702 ) ) ;
#42892 = CARTESIAN_POINT ( 'NONE',  ( 2.500000000000002220, -20.54166666393548013, 4.330127018922192761 ) ) ;
#42893 = CARTESIAN_POINT ( 'NONE',  ( -6.972266317189433020E-16, -96.12499999726880162, -5.000000000000000000 ) ) ;
#42894 = CARTESIAN_POINT ( 'NONE',  ( 5.000000000000000000, -45.41666666666665719, -2.886751345948130876 ) ) ;
#42895 = DIRECTION ( 'NONE',  ( 0.000000000000000000, 0.000000000000000000, 1.000000000000000000 ) ) ;
#42896 = CARTESIAN_POINT ( 'NONE',  ( -2.071067811865308972, -156.3125000000000568, 5.000000000000169642 ) ) ;
#42897 = FACE_OUTER_BOUND ( 'NONE', #20160, .T. ) ;
#42898 = CARTESIAN_POINT ( 'NONE',  ( -2.229367062500000163, -40.47916666530107221, -3.861377020970580443 ) ) ;
#42899 = CARTESIAN_POINT ( 'NONE',  ( -2.229367062499996610, -25.39583333196773651, 3.861377020970582219 ) ) ;
#42900 = CARTESIAN_POINT ( 'NONE',  ( -51.75738570946856498, -139.8750000027312126, 3.805975901505576964 ) ) ;
#42901 = CARTESIAN_POINT ( 'NONE',  ( -3.535250795749689387E-16, 26.75000000000000000, -5.773502691896257311 ) ) ;
#42902 = CARTESIAN_POINT ( 'NONE',  ( 5.000000000000000000, -152.1875000027312126, 2.071067811865478614 ) ) ;
#42903 = ORIENTED_EDGE ( 'NONE', *, *, #753, .F. ) ;
#42904 = CARTESIAN_POINT ( 'NONE',  ( -4.458734124999999437, -108.6458333319677365, -2.574251347313719407 ) ) ;
#42905 = CARTESIAN_POINT ( 'NONE',  ( 4.458734124999998549, -34.72916666530107221, -2.574251347313721627 ) ) ;
#42906 = CARTESIAN_POINT ( 'NONE',  ( 1.060575238724906964E-15, -70.62499999726881583, 5.773502691896257311 ) ) ;
#42907 = CARTESIAN_POINT ( 'NONE',  ( -52.80376928212989185, -146.1250000013656063, -4.297418129356379346 ) ) ;
#42908 = CARTESIAN_POINT ( 'NONE',  ( -5.000000000000000000, -144.5000000000000284, -6.123233995736766282E-16 ) ) ;
#42909 = EDGE_CURVE ( 'NONE', #42031, #42211, #7223, .T. ) ;
#42910 = EDGE_CURVE ( 'NONE', #57087, #33853, #18367, .T. ) ;
#42911 = CARTESIAN_POINT ( 'NONE',  ( 9.457646018065525792E-16, -28.06249999863440081, 5.148502694627439702 ) ) ;
#42912 = CARTESIAN_POINT ( 'NONE',  ( -4.458734124999997661, -75.47916666530106511, 2.574251347313722516 ) ) ;
#42913 = CARTESIAN_POINT ( 'NONE',  ( 4.458734124999999437, -169.6250000013656063, -1.846868145590734978 ) ) ;
#42914 = CARTESIAN_POINT ( 'NONE',  ( 4.458734124999998549, -30.72916666530107221, -2.574251347313721627 ) ) ;
#42915 = EDGE_CURVE ( 'NONE', #45427, #46757, #47117, .T. ) ;
#42916 = FACE_OUTER_BOUND ( 'NONE', #27886, .T. ) ;
#42917 = CARTESIAN_POINT ( 'NONE',  ( -53.33387254593703375, -137.9375000027311842, 5.149110718188541824 ) ) ;
#42918 = CARTESIAN_POINT ( 'NONE',  ( 5.000000000000000888, -15.58333333333333215, 2.886751345948126879 ) ) ;
#42919 = CARTESIAN_POINT ( 'NONE',  ( -4.458734125000001214, -146.8750000013656063, 1.846868145590734089 ) ) ;
#42920 = ORIENTED_EDGE ( 'NONE', *, *, #47530, .T. ) ;
#42921 = DIRECTION ( 'NONE',  ( -0.000000000000000000, 1.000000000000000000, -0.000000000000000000 ) ) ;
#42922 = CARTESIAN_POINT ( 'NONE',  ( -2.229367062500000163, -58.72916666530106511, -3.861377020970580443 ) ) ;
#42923 = EDGE_CURVE ( 'NONE', #8886, #4102, #12173, .T. ) ;
#42924 = CARTESIAN_POINT ( 'NONE',  ( 2.499999999999998668, 25.79166666939785202, -4.330127018922193649 ) ) ;
#42925 = CARTESIAN_POINT ( 'NONE',  ( 0.000000000000000000, -120.0000000000000000, 0.000000000000000000 ) ) ;
#42926 = CARTESIAN_POINT ( 'NONE',  ( 5.000000000000000000, 21.58333333333333215, -2.886751345948129988 ) ) ;
#42927 = AXIS2_PLACEMENT_3D ( 'NONE', #41741, #54242, #53923 ) ;
#42928 = EDGE_CURVE ( 'NONE', #38937, #33932, #33946, .T. ) ;
#42929 = EDGE_CURVE ( 'NONE', #53932, #31664, #38096, .T. ) ;
#42930 = CARTESIAN_POINT ( 'NONE',  ( 1.975475456537005874E-15, -36.62499999726880873, 5.000000000000000000 ) ) ;
#42931 = CARTESIAN_POINT ( 'NONE',  ( -4.458734124999999437, -2.312499998634407028, 0.000000000000000000 ) ) ;
#42932 = CARTESIAN_POINT ( 'NONE',  ( 3.061616997868383141E-16, -154.7500000000000000, -5.000000000000000000 ) ) ;
#42933 = CARTESIAN_POINT ( 'NONE',  ( -4.999999999999998224, -80.79166666393547303, 2.886751345948131764 ) ) ;
#42934 = CARTESIAN_POINT ( 'NONE',  ( 4.458734124999998549, 9.020833334698927786, -2.574251347313721627 ) ) ;
#42935 = EDGE_CURVE ( 'NONE', #27373, #58935, #7535, .T. ) ;
#42936 = CARTESIAN_POINT ( 'NONE',  ( 2.500000000000002220, -12.66666666666666607, 4.330127018922192761 ) ) ;
#42937 = VERTEX_POINT ( 'NONE', #58225 ) ;
#42938 = CARTESIAN_POINT ( 'NONE',  ( 4.458734124999998549, -46.72916666530106511, -2.574251347313721627 ) ) ;
#42939 = EDGE_CURVE ( 'NONE', #7158, #57284, #22650, .T. ) ;
#42940 = CARTESIAN_POINT ( 'NONE',  ( -4.458734125000001214, -158.1250000013656063, 1.846868145590734089 ) ) ;
#42941 = EDGE_CURVE ( 'NONE', #28080, #46979, #34318, .T. ) ;
#42942 = CARTESIAN_POINT ( 'NONE',  ( -5.000000000000000000, -51.95833333060213732, -2.886751345948128211 ) ) ;
#42943 = VERTEX_POINT ( 'NONE', #51603 ) ;
#42944 = CARTESIAN_POINT ( 'NONE',  ( -2.229367062499996610, -22.14583333196773651, 3.861377020970582219 ) ) ;
#42945 = EDGE_LOOP ( 'NONE', ( #16569, #20085, #55718, #45733 ) ) ;
#42947 = CARTESIAN_POINT ( 'NONE',  ( -6.972266317189433020E-16, -103.1249999972688158, -5.000000000000000000 ) ) ;
#42946 = DIRECTION ( 'NONE',  ( 0.000000000000000000, 0.000000000000000000, 1.000000000000000000 ) ) ;
#42948 = CARTESIAN_POINT ( 'NONE',  ( 1.846868145590736310, -160.6250000013655779, 4.458734124999999437 ) ) ;
#42949 = ORIENTED_EDGE ( 'NONE', *, *, #25351, .T. ) ;
#42950 = CARTESIAN_POINT ( 'NONE',  ( 1.339745962155612702, -39.16965819600733312, -5.000000000000000000 ) ) ;
#42951 = CARTESIAN_POINT ( 'NONE',  ( -51.75738570946856498, -132.7500000000000284, 3.805975901505576964 ) ) ;
#42952 = CARTESIAN_POINT ( 'NONE',  ( 4.458734125000001214, -39.14583333196773651, 2.574251347313718519 ) ) ;
#42953 = ORIENTED_EDGE ( 'NONE', *, *, #57558, .T. ) ;
#42954 = CARTESIAN_POINT ( 'NONE',  ( 4.458734125000001214, -82.89583333196772230, 2.574251347313718519 ) ) ;
#42955 = CARTESIAN_POINT ( 'NONE',  ( 4.458734124999999437, 19.18750000136559564, -5.460374474430324690E-16 ) ) ;
#42956 = CARTESIAN_POINT ( 'NONE',  ( -5.000000000000000000, -17.87499999726881583, 0.000000000000000000 ) ) ;
#42957 = ORIENTED_EDGE ( 'NONE', *, *, #57781, .T. ) ;
#42958 = CARTESIAN_POINT ( 'NONE',  ( -57.89159099828107458, -137.9375000013656063, -3.393966926194107447 ) ) ;
#42959 = CARTESIAN_POINT ( 'NONE',  ( -4.458734124999998549, -85.47916666530106511, 2.574251347313722516 ) ) ;
#42960 = CARTESIAN_POINT ( 'NONE',  ( -58.80597590150559739, -126.1250000027312126, 3.242614290531460330 ) ) ;
#42961 = CARTESIAN_POINT ( 'NONE',  ( 2.499999999999998668, -4.208333330602147981, -4.330127018922193649 ) ) ;
#42962 = CARTESIAN_POINT ( 'NONE',  ( -2.071067811865372921, -158.4375000027312126, 5.000000000000104805 ) ) ;
#42963 = CARTESIAN_POINT ( 'NONE',  ( 1.339745962155615144, -13.58034179853029322, 4.999999999999999112 ) ) ;
#42964 = CARTESIAN_POINT ( 'NONE',  ( -4.458734124999999437, -61.39583333196774362, -2.574251347313719407 ) ) ;
#42965 = CARTESIAN_POINT ( 'NONE',  ( 1.339745962155615144, -37.70534180126148271, 4.999999999999999112 ) ) ;
#42966 = CARTESIAN_POINT ( 'NONE',  ( -4.458734124999998549, 24.77083333469893134, 2.574251347313722516 ) ) ;
#42967 = VECTOR ( 'NONE', #3642, 1000.000000000000000 ) ;
#42968 =( BOUNDED_CURVE ( )  B_SPLINE_CURVE ( 2, ( #53857, #9787, #5621, #10434, #4974, #44203, #19767, #54178, #39376 ),
 .UNSPECIFIED., .F., .F. ) 
 B_SPLINE_CURVE_WITH_KNOTS ( ( 3, 2, 2, 2, 3 ),
 ( 0.1339285714285714246, 0.1345238095238095177, 0.1357142857142857040, 0.1369047619047619180, 0.1375000000000000111 ),
 .UNSPECIFIED. ) 
 CURVE ( )  GEOMETRIC_REPRESENTATION_ITEM ( )  RATIONAL_B_SPLINE_CURVE ( ( 0.9330127018922194093, 0.9330127018922194093, 1.000000000000000000, 0.8660254037844387076, 1.000000000000000000, 0.8660254037844387076, 1.000000000000000000, 0.9330127018922194093, 0.9330127018922194093 ) ) 
 REPRESENTATION_ITEM ( '' )  );
#42969 = CARTESIAN_POINT ( 'NONE',  ( 2.500000000000002220, -97.66666666666665719, 4.330127018922192761 ) ) ;
#42970 = CARTESIAN_POINT ( 'NONE',  ( -55.00000000000002132, -155.0000000000000284, 1.734723475976807094E-15 ) ) ;
#42971 = CARTESIAN_POINT ( 'NONE',  ( 4.458734124999999437, -44.06249999863440081, -5.460374474430324690E-16 ) ) ;
#42972 = CARTESIAN_POINT ( 'NONE',  ( 5.000000000000000888, -2.458333330602146205, 2.886751345948126879 ) ) ;
#42973 = CARTESIAN_POINT ( 'NONE',  ( 0.000000000000000000, -170.0000000000000000, 0.000000000000000000 ) ) ;
#42974 = CARTESIAN_POINT ( 'NONE',  ( 1.975475456537005874E-15, -60.75000000000000000, 5.000000000000000000 ) ) ;
#42975 = CARTESIAN_POINT ( 'NONE',  ( -4.458734124999999437, -84.56249999863439371, 0.000000000000000000 ) ) ;
#42976 = CARTESIAN_POINT ( 'NONE',  ( -4.458734124999997661, -101.2291666653010651, 2.574251347313722516 ) ) ;
#42977 = CARTESIAN_POINT ( 'NONE',  ( -2.229367062500000163, -12.72916666530107044, -3.861377020970580443 ) ) ;
#42978 = ORIENTED_EDGE ( 'NONE', *, *, #33339, .T. ) ;
#42979 = CARTESIAN_POINT ( 'NONE',  ( -5.000000000000000000, -16.87499999726881583, 0.000000000000000000 ) ) ;
#42980 = CARTESIAN_POINT ( 'NONE',  ( -2.229367062499996610, -98.14583333196773651, 3.861377020970582219 ) ) ;
#42981 = CARTESIAN_POINT ( 'NONE',  ( -2.071067811865475061, -164.8125000027312126, -5.000000000000000888 ) ) ;
#42982 = CARTESIAN_POINT ( 'NONE',  ( -4.458734124999999437, -91.64583333196773651, -2.574251347313719407 ) ) ;
#42983 = CARTESIAN_POINT ( 'NONE',  ( 5.000000000000000888, -53.45833333060213732, 2.886751345948126879 ) ) ;
#42984 = CARTESIAN_POINT ( 'NONE',  ( 1.975475456537005874E-15, 19.37500000273118772, 5.000000000000000000 ) ) ;
#42985 = AXIS2_PLACEMENT_3D ( 'NONE', #36422, #7165, #22271 ) ;
#42986 = CARTESIAN_POINT ( 'NONE',  ( -54.64476657466781973, -127.8125000013655921, -4.444560631937228834 ) ) ;
#42987 =( BOUNDED_CURVE ( )  B_SPLINE_CURVE ( 2, ( #12569, #32182, #51813, #7755, #27358, #22553, #12884, #33449, #38893 ),
 .UNSPECIFIED., .F., .F. ) 
 B_SPLINE_CURVE_WITH_KNOTS ( ( 3, 2, 2, 2, 3 ),
 ( 0.5270833333333333481, 0.5277777777777777901, 0.5291666666666666741, 0.5305555555555555580, 0.5312500000000000000 ),
 .UNSPECIFIED. ) 
 CURVE ( )  GEOMETRIC_REPRESENTATION_ITEM ( )  RATIONAL_B_SPLINE_CURVE ( ( 0.9330127018922194093, 0.9330127018922194093, 1.000000000000000000, 0.8660254037844387076, 1.000000000000000000, 0.8660254037844387076, 1.000000000000000000, 0.9330127018922194093, 0.9330127018922194093 ) ) 
 REPRESENTATION_ITEM ( '' )  );
#42988 = CARTESIAN_POINT ( 'NONE',  ( -2.229367062499996610, -15.14583333196773474, 3.861377020970582219 ) ) ;
#42989 = CARTESIAN_POINT ( 'NONE',  ( 4.458734124999998549, 11.02083333469892779, -2.574251347313721627 ) ) ;
#42990 = CARTESIAN_POINT ( 'NONE',  ( -4.458734124999999437, -58.56249999863440081, 0.000000000000000000 ) ) ;
#42991 = DIRECTION ( 'NONE',  ( 0.000000000000000000, 0.000000000000000000, 1.000000000000000000 ) ) ;
#42992 = CARTESIAN_POINT ( 'NONE',  ( 1.255007937094098239E-14, 23.75000000000000000, -4.999999999999999112 ) ) ;
#42993 = CARTESIAN_POINT ( 'NONE',  ( 4.458734124999999437, -14.81249999863440436, -5.460374474430324690E-16 ) ) ;
#42994 = CARTESIAN_POINT ( 'NONE',  ( 1.975475456537005874E-15, -24.62499999726881583, 5.000000000000000000 ) ) ;
#42995 = ORIENTED_EDGE ( 'NONE', *, *, #15698, .F. ) ;
#42996 = CARTESIAN_POINT ( 'NONE',  ( 2.229367062499998831, -40.89583333196773651, -3.861377020970580887 ) ) ;
#42997 = DIRECTION ( 'NONE',  ( 0.000000000000000000, 0.000000000000000000, 1.000000000000000000 ) ) ;
#42998 = CARTESIAN_POINT ( 'NONE',  ( 2.500000000000002220, 0.4583333360645182042, 4.330127018922192761 ) ) ;
#42999 = CARTESIAN_POINT ( 'NONE',  ( -7.922281120364393914, 4.573931137438271399, -8.047472243342930653 ) ) ;
#43000 = CARTESIAN_POINT ( 'NONE',  ( 4.458734124999998549, -86.72916666530107932, -2.574251347313721627 ) ) ;
#43001 = CARTESIAN_POINT ( 'NONE',  ( -2.229367062499996610, 24.60416666803225993, 3.861377020970582219 ) ) ;
#43002 = CARTESIAN_POINT ( 'NONE',  ( 4.458734124999999437, 15.18750000136559564, -5.460374474430324690E-16 ) ) ;
#43003 = CARTESIAN_POINT ( 'NONE',  ( -1.339745962155610925, -47.79465819873851729, 5.000000000000000000 ) ) ;
#43004 = CARTESIAN_POINT ( 'NONE',  ( -5.000000000000000000, -64.95833333060213022, -2.886751345948128211 ) ) ;
#43005 = CARTESIAN_POINT ( 'NONE',  ( -2.229367062499996610, -87.39583333196773651, 3.861377020970582219 ) ) ;
#43006 = CARTESIAN_POINT ( 'NONE',  ( 5.000000000000000000, -68.41666666666667140, -2.886751345948129988 ) ) ;
#43007 = CARTESIAN_POINT ( 'NONE',  ( 5.000000000000000000, 11.70833333606451809, -2.886751345948129988 ) ) ;
#43009 = ORIENTED_EDGE ( 'NONE', *, *, #38840, .F. ) ;
#43008 = EDGE_CURVE ( 'NONE', #31402, #12840, #60277, .T. ) ;
#43010 = CARTESIAN_POINT ( 'NONE',  ( 5.000000000000000000, -25.50000000000000355, -6.123233995736766282E-16 ) ) ;
#43011 = PRODUCT_DEFINITION_SHAPE ( 'NONE', 'NONE',  #40220 ) ;
#43012 = VECTOR ( 'NONE', #46185, 1000.000000000000000 ) ;
#43013 = CARTESIAN_POINT ( 'NONE',  ( -51.19402409849444524, -144.6250000027312126, -3.242614290531456334 ) ) ;
#43015 = CARTESIAN_POINT ( 'NONE',  ( -2.500000000000000444, -30.16666666666666785, -4.330127018922193649 ) ) ;
#43014 = CARTESIAN_POINT ( 'NONE',  ( 1.975475456537005874E-15, -71.75000000000000000, 5.000000000000000000 ) ) ;
#43016 = CARTESIAN_POINT ( 'NONE',  ( -4.458734124999998549, -33.22916666530107221, 2.574251347313722516 ) ) ;
#43017 = CARTESIAN_POINT ( 'NONE',  ( 1.339745962155600711, 18.29465819873852084, 5.000000000000007994 ) ) ;
#43018 = EDGE_CURVE ( 'NONE', #41687, #15898, #4206, .T. ) ;
#43019 = CARTESIAN_POINT ( 'NONE',  ( 5.000000000000000888, -35.45833333060213732, 2.886751345948126879 ) ) ;
#43021 = ORIENTED_EDGE ( 'NONE', *, *, #55147, .F. ) ;
#43020 = CARTESIAN_POINT ( 'NONE',  ( -3.152548672688508926E-16, -62.56249999863440792, -5.148502694627439702 ) ) ;
#43022 = CARTESIAN_POINT ( 'NONE',  ( -53.51423613279429503, -151.5000000013655779, 4.591703134518082763 ) ) ;
#43024 = ORIENTED_EDGE ( 'NONE', *, *, #10605, .F. ) ;
#43023 = CARTESIAN_POINT ( 'NONE',  ( 4.458734125000001214, -9.145833331967736513, 2.574251347313718519 ) ) ;
#43025 = CARTESIAN_POINT ( 'NONE',  ( 5.000000000000000000, -78.50000000000000000, -6.123233995736766282E-16 ) ) ;
#43026 = CARTESIAN_POINT ( 'NONE',  ( -59.59170313451810586, -136.5000000013656063, 1.485763867205729394 ) ) ;
#43027 = CARTESIAN_POINT ( 'NONE',  ( 9.457646018065525792E-16, -58.31249999863440792, 5.148502694627439702 ) ) ;
#43028 = CARTESIAN_POINT ( 'NONE',  ( 1.060575238724906964E-15, -75.62499999726880162, 5.773502691896257311 ) ) ;
#43030 = ORIENTED_EDGE ( 'NONE', *, *, #8682, .F. ) ;
#43029 = CARTESIAN_POINT ( 'NONE',  ( 5.000000000000000000, -65.37499999726881583, -6.123233995736766282E-16 ) ) ;
#43031 = CARTESIAN_POINT ( 'NONE',  ( -52.53715891517739323, -151.4375000000000284, -4.819101127000233298 ) ) ;
#43032 = CARTESIAN_POINT ( 'NONE',  ( -4.458734124999998549, -19.47916666530107221, 2.574251347313722516 ) ) ;
#43034 = ORIENTED_EDGE ( 'NONE', *, *, #7875, .F. ) ;
#43033 = CARTESIAN_POINT ( 'NONE',  ( 2.229367062499998831, -55.89583333196773651, -3.861377020970580887 ) ) ;
#43035 = DIRECTION ( 'NONE',  ( 0.000000000000000000, -1.000000000000000000, 0.000000000000000000 ) ) ;
#43036 = CARTESIAN_POINT ( 'NONE',  ( -4.458734125000001214, -167.1250000013656063, 1.846868145590734089 ) ) ;
#43037 = CARTESIAN_POINT ( 'NONE',  ( -3.152548672688508926E-16, -97.81249999863439371, -5.148502694627439702 ) ) ;
#43038 = CARTESIAN_POINT ( 'NONE',  ( -1.339745962155613812, -27.08034179853029499, -5.000000000000000000 ) ) ;
#43039 = ORIENTED_EDGE ( 'NONE', *, *, #19611, .F. ) ;
#43040 = CARTESIAN_POINT ( 'NONE',  ( -50.40829686548195099, -150.2500000013656347, -1.485763867205728284 ) ) ;
#43041 = CARTESIAN_POINT ( 'NONE',  ( -55.39835681537999790, -137.0000000027312126, 4.984105922594378235 ) ) ;
#43042 =( BOUNDED_CURVE ( )  B_SPLINE_CURVE ( 2, ( #62957, #14050, #15000, #19187, #29461, #24023, #43627, #14366, #33990 ),
 .UNSPECIFIED., .F., .F. ) 
 B_SPLINE_CURVE_WITH_KNOTS ( ( 3, 2, 2, 2, 3 ),
 ( 0.9446428571428571175, 0.9452380952380952106, 0.9464285714285713969, 0.9476190476190475831, 0.9482142857142856762 ),
 .UNSPECIFIED. ) 
 CURVE ( )  GEOMETRIC_REPRESENTATION_ITEM ( )  RATIONAL_B_SPLINE_CURVE ( ( 0.9330127018922194093, 0.9330127018922194093, 1.000000000000000000, 0.8660254037844387076, 1.000000000000000000, 0.8660254037844387076, 1.000000000000000000, 0.9330127018922194093, 0.9330127018922194093 ) ) 
 REPRESENTATION_ITEM ( '' )  );
#43043 = CARTESIAN_POINT ( 'NONE',  ( -1.339745962155613812, 0.9196582014697067819, -5.000000000000000000 ) ) ;
#43044 = CARTESIAN_POINT ( 'NONE',  ( 9.457646018065525792E-16, -10.06249999863440792, 5.148502694627439702 ) ) ;
#43045 = CARTESIAN_POINT ( 'NONE',  ( 2.229367062500001939, -102.2291666653010651, 3.861377020970579999 ) ) ;
#43046 = CARTESIAN_POINT ( 'NONE',  ( 2.730187237215162345E-16, -144.4375000013656063, -4.458734124999999437 ) ) ;
#43047 = CARTESIAN_POINT ( 'NONE',  ( -2.229367062500000163, -29.72916666530107221, -3.861377020970580443 ) ) ;
#43048 = CARTESIAN_POINT ( 'NONE',  ( -6.972266317189433020E-16, -80.24999999999998579, -5.000000000000000000 ) ) ;
#43049 = CARTESIAN_POINT ( 'NONE',  ( -56.48576386720575471, -138.7500000013656063, -4.591703134518078322 ) ) ;
#43050 = CARTESIAN_POINT ( 'NONE',  ( 9.457646018065525792E-16, -67.31249999863440792, 5.148502694627439702 ) ) ;
#43051 = CARTESIAN_POINT ( 'NONE',  ( 0.000000000000000000, -120.0000000000000000, 5.000000000000000000 ) ) ;
#43052 = CARTESIAN_POINT ( 'NONE',  ( -6.972266317189433020E-16, -22.12499999726881228, -5.000000000000000000 ) ) ;
#43053 = CARTESIAN_POINT ( 'NONE',  ( -1.846868145590734756, -140.1250000013656347, -4.458734124999999437 ) ) ;
#43054 = AXIS2_PLACEMENT_3D ( 'NONE', #62200, #38367, #13919 ) ;
#43055 = CARTESIAN_POINT ( 'NONE',  ( -4.458734124999999437, 4.437500001365595637, 0.000000000000000000 ) ) ;
#43056 = ORIENTED_EDGE ( 'NONE', *, *, #4706, .F. ) ;
#43057 = FILL_AREA_STYLE_COLOUR ( '', #5885 ) ;
#43058 = DIRECTION ( 'NONE',  ( 0.000000000000000000, -0.000000000000000000, -1.000000000000000000 ) ) ;
#43060 = CARTESIAN_POINT ( 'NONE',  ( 4.458734124999999437, -30.81249999863440436, -5.460374474430324690E-16 ) ) ;
#43059 = CARTESIAN_POINT ( 'NONE',  ( 5.000000000000000000, -91.50000000000000000, -6.123233995736766282E-16 ) ) ;
#43061 = CARTESIAN_POINT ( 'NONE',  ( 0.000000000000000000, -170.0000000000000000, 0.000000000000000000 ) ) ;
#43062 = CARTESIAN_POINT ( 'NONE',  ( -4.458734124999998549, -76.47916666530105090, 2.574251347313722516 ) ) ;
#43063 = CARTESIAN_POINT ( 'NONE',  ( -4.458734124999999437, 21.43750000136559208, 0.000000000000000000 ) ) ;
#43064 = DIRECTION ( 'NONE',  ( -0.000000000000000000, 1.000000000000000000, -0.000000000000000000 ) ) ;
#43065 = CARTESIAN_POINT ( 'NONE',  ( -59.44456063193725015, -143.5625000013656063, -0.3552334253322034230 ) ) ;
#43066 = CARTESIAN_POINT ( 'NONE',  ( -2.229367062499996610, 4.854166668032261711, 3.861377020970582219 ) ) ;
#43067 = CARTESIAN_POINT ( 'NONE',  ( 2.229367062500001939, 26.77083333469892423, 3.861377020970579999 ) ) ;
#43068 = CARTESIAN_POINT ( 'NONE',  ( 4.458734124999999437, -40.06249999863440081, -5.460374474430324690E-16 ) ) ;
#43069 = CARTESIAN_POINT ( 'NONE',  ( -6.972266317189433020E-16, -80.24999999999998579, -5.000000000000000000 ) ) ;
#43070 = CARTESIAN_POINT ( 'NONE',  ( 2.229367062499998831, 0.3541666680322609340, -3.861377020970580887 ) ) ;
#43071 = CARTESIAN_POINT ( 'NONE',  ( -4.458734124999997661, -22.47916666530107221, 2.574251347313722516 ) ) ;
#43072 =( BOUNDED_CURVE ( )  B_SPLINE_CURVE ( 2, ( #6555, #1749, #45468, #21674, #11682 ),
 .UNSPECIFIED., .F., .F. ) 
 B_SPLINE_CURVE_WITH_KNOTS ( ( 3, 2, 3 ),
 ( 0.9982142857142857206, 0.9988095238095238138, 1.000000000000000000 ),
 .UNSPECIFIED. ) 
 CURVE ( )  GEOMETRIC_REPRESENTATION_ITEM ( )  RATIONAL_B_SPLINE_CURVE ( ( 0.9330127018922194093, 0.9330127018922194093, 1.000000000000000000, 0.8660254037844387076, 1.000000000000000000 ) ) 
 REPRESENTATION_ITEM ( '' )  );
#43073 = CARTESIAN_POINT ( 'NONE',  ( -3.152801135295367985, -154.8125000013656063, 3.152801135295367096 ) ) ;
#43074 = CARTESIAN_POINT ( 'NONE',  ( -2.229367062499996610, -67.14583333196773651, 3.861377020970582219 ) ) ;
#43075 = CARTESIAN_POINT ( 'NONE',  ( -4.999999999999999112, -99.79166666393545881, 2.886751345948131764 ) ) ;
#43076 = CARTESIAN_POINT ( 'NONE',  ( 1.339745962155624914, 15.70534180126147561, -4.999999999999991118 ) ) ;
#43077 = CARTESIAN_POINT ( 'NONE',  ( 1.339745962155615144, 9.419658201469706782, 4.999999999999999112 ) ) ;
#43078 = CARTESIAN_POINT ( 'NONE',  ( 2.229367062500001939, -106.2291666653010651, 3.861377020970579999 ) ) ;
#43079 = CARTESIAN_POINT ( 'NONE',  ( -2.229367062500000163, -69.72916666530107932, -3.861377020970580443 ) ) ;
#43080 = CARTESIAN_POINT ( 'NONE',  ( 2.500000000000002220, -51.66666666666666430, 4.330127018922192761 ) ) ;
#43081 = CARTESIAN_POINT ( 'NONE',  ( 1.975475456537005874E-15, -73.75000000000000000, 5.000000000000000000 ) ) ;
#43082 = CARTESIAN_POINT ( 'NONE',  ( 2.500000000000002220, 27.45833333606451632, 4.330127018922192761 ) ) ;
#43083 = ORIENTED_EDGE ( 'NONE', *, *, #31000, .F. ) ;
#43084 = CARTESIAN_POINT ( 'NONE',  ( 4.458734125000001214, -109.8958333319677365, 2.574251347313718519 ) ) ;
#43085 = CARTESIAN_POINT ( 'NONE',  ( -1.339745962155613812, 11.91965820146970678, -5.000000000000000000 ) ) ;
#43086 = CARTESIAN_POINT ( 'NONE',  ( 2.500000000000002220, -13.66666666666666785, 4.330127018922192761 ) ) ;
#43087 = CARTESIAN_POINT ( 'NONE',  ( -4.458734124999999437, -16.31249999863440436, 0.000000000000000000 ) ) ;
#43088 = CARTESIAN_POINT ( 'NONE',  ( 2.229367062500001939, -79.97916666530106511, 3.861377020970579999 ) ) ;
#43089 = CARTESIAN_POINT ( 'NONE',  ( -4.458734124999999437, -169.1875000013656063, -5.460374474430324690E-16 ) ) ;
#43090 = CARTESIAN_POINT ( 'NONE',  ( -4.999999999999999112, -19.79166666393547658, 2.886751345948131764 ) ) ;
#43092 = ORIENTED_EDGE ( 'NONE', *, *, #46502, .F. ) ;
#43091 = CARTESIAN_POINT ( 'NONE',  ( -3.152548672688508926E-16, -43.56249999863440081, -5.148502694627439702 ) ) ;
#43093 = FACE_OUTER_BOUND ( 'NONE', #10762, .T. ) ;
#43095 = EDGE_LOOP ( 'NONE', ( #51427, #45805, #55582, #63050 ) ) ;
#43094 = CARTESIAN_POINT ( 'NONE',  ( -4.458734124999999437, 7.354166668032259935, -2.574251347313719407 ) ) ;
#43096 = CARTESIAN_POINT ( 'NONE',  ( -55.00000000000002132, -155.0000000000000284, 1.734723475976807094E-15 ) ) ;
#43097 = CARTESIAN_POINT ( 'NONE',  ( 5.000000000000000888, -60.58333333333332860, 2.886751345948126879 ) ) ;
#43098 = CARTESIAN_POINT ( 'NONE',  ( 1.846868145590735200, -156.5000000013656347, -4.458734125000000326 ) ) ;
#43099 = CARTESIAN_POINT ( 'NONE',  ( -2.229367062500000163, -35.72916666530107221, -3.861377020970580443 ) ) ;
#43100 = AXIS2_PLACEMENT_3D ( 'NONE', #5222, #36636, #5381 ) ;
#43101 = DIRECTION ( 'NONE',  ( -0.000000000000000000, 1.000000000000000000, -0.000000000000000000 ) ) ;
#43102 = CARTESIAN_POINT ( 'NONE',  ( -3.535533905932738641, -166.3750000000000284, 3.535533905932737309 ) ) ;
#43103 = AXIS2_PLACEMENT_3D ( 'NONE', #46378, #12593, #2326 ) ;
#43104 = CARTESIAN_POINT ( 'NONE',  ( -59.29741812935640155, -129.8750000013656063, -2.196230717870135685 ) ) ;
#43105 = CARTESIAN_POINT ( 'NONE',  ( 4.458734124999999437, -5.062499998634402587, -5.460374474430324690E-16 ) ) ;
#43106 = CARTESIAN_POINT ( 'NONE',  ( 2.229367062500001939, -39.22916666530107221, 3.861377020970579999 ) ) ;
#43107 = CARTESIAN_POINT ( 'NONE',  ( 1.339745962155615144, -54.70534180126148271, 4.999999999999999112 ) ) ;
#43108 = CARTESIAN_POINT ( 'NONE',  ( -1.846868145590737420, -148.7500000013656063, 4.458734124999999437 ) ) ;
#43109 = CARTESIAN_POINT ( 'NONE',  ( 2.229367062499998831, -81.89583333196773651, -3.861377020970580887 ) ) ;
#43110 = LINE ( 'NONE', #28940, #46148 ) ;
#43111 = VERTEX_POINT ( 'NONE', #51909 ) ;
#43112 = CARTESIAN_POINT ( 'NONE',  ( -3.535533905932738641, -141.3750000000000000, 3.535533905932737309 ) ) ;
#43113 = CARTESIAN_POINT ( 'NONE',  ( -6.972266317189433020E-16, -44.25000000000000000, -5.000000000000000000 ) ) ;
#43115 = EDGE_CURVE ( 'NONE', #16789, #49905, #44651, .T. ) ;
#43114 = CARTESIAN_POINT ( 'NONE',  ( -2.229367062500000163, -70.72916666530107932, -3.861377020970580443 ) ) ;
#43116 = EDGE_LOOP ( 'NONE', ( #43243, #309, #2528, #6926 ) ) ;
#43117 = DIRECTION ( 'NONE',  ( -0.000000000000000000, -1.000000000000000000, -0.000000000000000000 ) ) ;
#43118 = CARTESIAN_POINT ( 'NONE',  ( 4.458734125000001214, -13.14583333196774184, 2.574251347313718519 ) ) ;
#43119 = DIRECTION ( 'NONE',  ( -0.000000000000000000, 1.000000000000000000, -0.000000000000000000 ) ) ;
#43120 = CARTESIAN_POINT ( 'NONE',  ( -4.458734124999999437, 3.604166668032260379, -2.574251347313719407 ) ) ;
#43121 = CARTESIAN_POINT ( 'NONE',  ( 5.000000000000000888, -77.45833333060213022, 2.886751345948126879 ) ) ;
#43122 = CARTESIAN_POINT ( 'NONE',  ( 4.458734124999999437, -151.4375000013655779, 0.000000000000000000 ) ) ;
#43123 = CARTESIAN_POINT ( 'NONE',  ( 4.458734125000000326, 23.85416666803225993, 2.574251347313718519 ) ) ;
#43124 = VERTEX_POINT ( 'NONE', #30536 ) ;
#43125 = CARTESIAN_POINT ( 'NONE',  ( 4.458734124999999437, -91.81249999863440792, -5.460374474430324690E-16 ) ) ;
#43126 = CARTESIAN_POINT ( 'NONE',  ( 2.499999999999998668, -47.33333333333333570, -4.330127018922193649 ) ) ;
#43127 = CARTESIAN_POINT ( 'NONE',  ( 1.975475456537005874E-15, -103.6249999972687874, 5.000000000000000000 ) ) ;
#43128 = CARTESIAN_POINT ( 'NONE',  ( -2.229367062499996610, -8.145833331967736513, 3.861377020970582219 ) ) ;
#43129 = CARTESIAN_POINT ( 'NONE',  ( -1.339745962155610925, -84.66965819600731891, 5.000000000000000000 ) ) ;
#43130 = CARTESIAN_POINT ( 'NONE',  ( 4.769696007084728073, -120.0000000000000000, 1.500000000000000000 ) ) ;
#43131 = CARTESIAN_POINT ( 'NONE',  ( -50.70258187064364108, -152.1250000013656063, 2.196230717870141014 ) ) ;
#43132 = CARTESIAN_POINT ( 'NONE',  ( -2.499999999999996447, -34.70833333060213732, 4.330127018922195425 ) ) ;
#43133 = FACE_BOUND ( 'NONE', #59325, .T. ) ;
#43134 = CARTESIAN_POINT ( 'NONE',  ( -4.458734124999999437, 20.60416666803225993, -2.574251347313719407 ) ) ;
#43135 = CARTESIAN_POINT ( 'NONE',  ( 5.000000000000000000, -44.41666666666665719, -2.886751345948130876 ) ) ;
#43136 = CARTESIAN_POINT ( 'NONE',  ( -3.152548672688508926E-16, 23.43750000136559564, -5.148502694627439702 ) ) ;
#43137 = CARTESIAN_POINT ( 'NONE',  ( 4.458734125000001214, -56.89583333196774362, 2.574251347313718519 ) ) ;
#43138 = CARTESIAN_POINT ( 'NONE',  ( 2.229367062500001939, -6.229166665301072214, 3.861377020970579999 ) ) ;
#43139 = DIRECTION ( 'NONE',  ( 0.5000000000000005551, -0.8660254037844383745, 0.000000000000000000 ) ) ;
#43140 = CARTESIAN_POINT ( 'NONE',  ( 2.500000000000002220, 8.333333333333332149, 4.330127018922192761 ) ) ;
#43141 = CARTESIAN_POINT ( 'NONE',  ( -1.846868145590737420, -166.7500000013655779, 4.458734124999999437 ) ) ;
#43142 = CARTESIAN_POINT ( 'NONE',  ( -55.39835681537999790, -145.0000000027312126, 4.984105922594378235 ) ) ;
#43143 = AXIS2_PLACEMENT_3D ( 'NONE', #47374, #56720, #52198 ) ;
#43144 = CARTESIAN_POINT ( 'NONE',  ( -2.229367062499996610, -47.14583333196774362, 3.861377020970582219 ) ) ;
#43145 = CARTESIAN_POINT ( 'NONE',  ( -3.535250795749689387E-16, -83.12499999726880162, -5.773502691896257311 ) ) ;
#43146 = CARTESIAN_POINT ( 'NONE',  ( -53.51423613279429503, -136.5000000013656347, 4.591703134518082763 ) ) ;
#43147 = CARTESIAN_POINT ( 'NONE',  ( -2.500000000000000444, -17.16666666666666430, -4.330127018922193649 ) ) ;
#43148 = CARTESIAN_POINT ( 'NONE',  ( 0.000000000000000000, -120.0000000000000000, 5.000000000000000000 ) ) ;
#43149 = CARTESIAN_POINT ( 'NONE',  ( 4.458734125000000326, -89.14583333196773651, 2.574251347313718519 ) ) ;
#43150 = CARTESIAN_POINT ( 'NONE',  ( -3.152801135295367985, -159.0625000013656063, 3.152801135295367096 ) ) ;
#43151 = CARTESIAN_POINT ( 'NONE',  ( 2.499999999999998668, -37.33333333333332860, -4.330127018922193649 ) ) ;
#43152 = CARTESIAN_POINT ( 'NONE',  ( 0.000000000000000000, -170.0000000000000000, 0.000000000000000000 ) ) ;
#43153 = ORIENTED_EDGE ( 'NONE', *, *, #54428, .F. ) ;
#43154 = CARTESIAN_POINT ( 'NONE',  ( 5.000000000000000000, -22.41666666666666785, -2.886751345948130876 ) ) ;
#43155 = ORIENTED_EDGE ( 'NONE', *, *, #44875, .F. ) ;
#43156 = CARTESIAN_POINT ( 'NONE',  ( 4.458734124999998549, -96.72916666530105090, -2.574251347313721627 ) ) ;
#43157 = CARTESIAN_POINT ( 'NONE',  ( 2.229367062500001939, 10.77083333469892956, 3.861377020970579999 ) ) ;
#43158 = CARTESIAN_POINT ( 'NONE',  ( 5.000000000000000000, 12.70833333606451809, -2.886751345948129988 ) ) ;
#43159 = CYLINDRICAL_SURFACE ( 'NONE', #27820, 5.000000000000000000 ) ;
#43160 = CARTESIAN_POINT ( 'NONE',  ( -4.999999999999999112, 2.083333333333333037, 2.886751345948131764 ) ) ;
#43161 = CARTESIAN_POINT ( 'NONE',  ( -2.229367062500000163, -63.47916666530106511, -3.861377020970580443 ) ) ;
#43162 =( BOUNDED_CURVE ( )  B_SPLINE_CURVE ( 2, ( #46454, #2399, #14544, #32922, #14232, #34164, #28708, #13298, #29016 ),
 .UNSPECIFIED., .F., .F. ) 
 B_SPLINE_CURVE_WITH_KNOTS ( ( 3, 2, 2, 2, 3 ),
 ( 0.8895833333333332815, 0.8902777777777777235, 0.8916666666666667185, 0.8930555555555556024, 0.8937500000000000444 ),
 .UNSPECIFIED. ) 
 CURVE ( )  GEOMETRIC_REPRESENTATION_ITEM ( )  RATIONAL_B_SPLINE_CURVE ( ( 0.9330127018922194093, 0.9330127018922194093, 1.000000000000000000, 0.8660254037844387076, 1.000000000000000000, 0.8660254037844387076, 1.000000000000000000, 0.9330127018922194093, 0.9330127018922194093 ) ) 
 REPRESENTATION_ITEM ( '' )  );
#43163 = CARTESIAN_POINT ( 'NONE',  ( -2.499999999999996447, -7.833333333333331261, 4.330127018922195425 ) ) ;
#43164 = CARTESIAN_POINT ( 'NONE',  ( -5.000000000000000000, 4.125000002731186832, 0.000000000000000000 ) ) ;
#43165 = CARTESIAN_POINT ( 'NONE',  ( -3.152548672688508926E-16, -27.56249999863440081, -5.148502694627439702 ) ) ;
#43166 = CARTESIAN_POINT ( 'NONE',  ( -60.14911071818854538, -144.1875000027312410, 1.666127454062681146 ) ) ;
#43167 = CARTESIAN_POINT ( 'NONE',  ( -5.000000000000000000, 26.12500000273118417, 0.000000000000000000 ) ) ;
#43168 = CARTESIAN_POINT ( 'NONE',  ( 5.000000000000000000, -19.41666666666666785, -2.886751345948130876 ) ) ;
#43169 = CARTESIAN_POINT ( 'NONE',  ( 2.499999999999998668, -45.33333333333333570, -4.330127018922193649 ) ) ;
#43171 = CARTESIAN_POINT ( 'NONE',  ( 4.458734124999998549, -20.97916666530107221, -2.574251347313721627 ) ) ;
#43170 = CARTESIAN_POINT ( 'NONE',  ( -58.24261429053147765, -142.2500000000000284, -3.805975901505573855 ) ) ;
#43172 = CARTESIAN_POINT ( 'NONE',  ( 5.000000000000000000, -155.0000000000000284, 0.000000000000000000 ) ) ;
#43173 = CARTESIAN_POINT ( 'NONE',  ( -2.229367062500000163, -70.47916666530107932, -3.861377020970580443 ) ) ;
#43174 = CARTESIAN_POINT ( 'NONE',  ( 4.458734125000000326, -149.6250000013655779, -1.846868145590734978 ) ) ;
#43175 = CARTESIAN_POINT ( 'NONE',  ( -3.152548672688508926E-16, -75.56249999863439371, -5.148502694627439702 ) ) ;
#43176 = CARTESIAN_POINT ( 'NONE',  ( -55.35523342533222291, -144.5625000013656063, 4.444560631937231499 ) ) ;
#43177 = CARTESIAN_POINT ( 'NONE',  ( -4.458734124999999437, -27.64583333196774007, -2.574251347313719407 ) ) ;
#43178 = CARTESIAN_POINT ( 'NONE',  ( -3.535250795749689387E-16, -66.12499999726881583, -5.773502691896257311 ) ) ;
#43179 = VERTEX_POINT ( 'NONE', #25078 ) ;
#43180 = CARTESIAN_POINT ( 'NONE',  ( -6.972266317189433020E-16, -74.25000000000000000, -5.000000000000000000 ) ) ;
#43181 = ORIENTED_EDGE ( 'NONE', *, *, #62273, .T. ) ;
#43182 = CARTESIAN_POINT ( 'NONE',  ( -2.229367062499996610, -70.39583333196773651, 3.861377020970582219 ) ) ;
#43183 = CARTESIAN_POINT ( 'NONE',  ( -5.000000000000000000, 8.125000002731187720, 0.000000000000000000 ) ) ;
#43184 = CARTESIAN_POINT ( 'NONE',  ( -1.339745962155613812, -6.080341798530292330, -5.000000000000000000 ) ) ;
#43185 = ORIENTED_EDGE ( 'NONE', *, *, #44151, .F. ) ;
#43186 = AXIS2_PLACEMENT_3D ( 'NONE', #14889, #44798, #39969 ) ;
#43187 = DIRECTION ( 'NONE',  ( 0.000000000000000000, 0.000000000000000000, 1.000000000000000000 ) ) ;
#43189 = EDGE_CURVE ( 'NONE', #58460, #24525, #36508, .T. ) ;
#43188 = CARTESIAN_POINT ( 'NONE',  ( 9.457646018065525792E-16, -55.31249999863439371, 5.148502694627439702 ) ) ;
#43190 = CARTESIAN_POINT ( 'NONE',  ( 4.458734124999998549, 1.020833334698927120, -2.574251347313721627 ) ) ;
#43191 = ORIENTED_EDGE ( 'NONE', *, *, #39783, .T. ) ;
#43192 = CARTESIAN_POINT ( 'NONE',  ( -2.500000000000000444, -55.16666666666667140, -4.330127018922193649 ) ) ;
#43193 = CARTESIAN_POINT ( 'NONE',  ( 2.229367062500001939, 21.02083333469892779, 3.861377020970579999 ) ) ;
#43194 = CARTESIAN_POINT ( 'NONE',  ( -59.44456063193725015, -144.5625000013656063, -0.3552334253322034230 ) ) ;
#43195 = CARTESIAN_POINT ( 'NONE',  ( -5.000000000000000000, -2.083333333333333037, -2.886751345948128211 ) ) ;
#43196 = CARTESIAN_POINT ( 'NONE',  ( -3.152801135295367096, -167.0625000013656063, -3.152801135295367541 ) ) ;
#43197 = ORIENTED_EDGE ( 'NONE', *, *, #59421, .F. ) ;
#43198 = CARTESIAN_POINT ( 'NONE',  ( 2.229367062499998831, -73.64583333196773651, -3.861377020970580887 ) ) ;
#43199 = EDGE_CURVE ( 'NONE', #25684, #10189, #54672, .T. ) ;
#43200 = CARTESIAN_POINT ( 'NONE',  ( -4.999999999999998224, -39.91666666666667140, 2.886751345948131764 ) ) ;
#43201 = CARTESIAN_POINT ( 'NONE',  ( 2.229367062499998831, 8.354166668032261711, -3.861377020970580887 ) ) ;
#43202 = CARTESIAN_POINT ( 'NONE',  ( -2.229367062500000163, -59.72916666530106511, -3.861377020970580443 ) ) ;
#43203 = CARTESIAN_POINT ( 'NONE',  ( -5.000000000000000000, -19.95833333060214798, -2.886751345948128211 ) ) ;
#43204 = ADVANCED_FACE ( 'NONE', ( #35060 ), #59831, .F. ) ;
#43205 = CARTESIAN_POINT ( 'NONE',  ( -51.75738570946856498, -142.8750000027312126, 3.805975901505576964 ) ) ;
#43206 = FACE_OUTER_BOUND ( 'NONE', #37058, .T. ) ;
#43207 = CARTESIAN_POINT ( 'NONE',  ( 1.975475456537005874E-15, -61.74999999999999289, 5.000000000000000000 ) ) ;
#43208 =( BOUNDED_CURVE ( )  B_SPLINE_CURVE ( 2, ( #16779, #56353, #56027, #11944, #17098, #57301, #12584, #51204, #37039 ),
 .UNSPECIFIED., .F., .F. ) 
 B_SPLINE_CURVE_WITH_KNOTS ( ( 3, 2, 2, 2, 3 ),
 ( 0.1875000000000000000, 0.1880952380952380931, 0.1892857142857142794, 0.1904761904761904656, 0.1910714285714285865 ),
 .UNSPECIFIED. ) 
 CURVE ( )  GEOMETRIC_REPRESENTATION_ITEM ( )  RATIONAL_B_SPLINE_CURVE ( ( 0.9330127018922194093, 0.9330127018922194093, 1.000000000000000000, 0.8660254037844387076, 1.000000000000000000, 0.8660254037844387076, 1.000000000000000000, 0.9330127018922178550, 0.9330127018922194093 ) ) 
 REPRESENTATION_ITEM ( '' )  );
#43209 = CARTESIAN_POINT ( 'NONE',  ( -1.049326080737009628E-13, -18.62499999726881583, 5.000000000000000000 ) ) ;
#43210 = CARTESIAN_POINT ( 'NONE',  ( 6.123233995736766282E-16, -120.0000000000000000, -5.000000000000000000 ) ) ;
#43211 = CARTESIAN_POINT ( 'NONE',  ( 9.457646018065525792E-16, -38.06249999863441502, 5.148502694627439702 ) ) ;
#43212 = CARTESIAN_POINT ( 'NONE',  ( -4.458734124999997661, -26.47916666530107221, 2.574251347313722516 ) ) ;
#43213 =( BOUNDED_CURVE ( )  B_SPLINE_CURVE ( 2, ( #36784, #37111, #57361, #41272, #56417, #51894, #8156, #46747, #2383 ),
 .UNSPECIFIED., .F., .F. ) 
 B_SPLINE_CURVE_WITH_KNOTS ( ( 3, 2, 2, 2, 3 ),
 ( 0.1395833333333333370, 0.1402777777777777790, 0.1416666666666666630, 0.1430555555555555469, 0.1437499999999999889 ),
 .UNSPECIFIED. ) 
 CURVE ( )  GEOMETRIC_REPRESENTATION_ITEM ( )  RATIONAL_B_SPLINE_CURVE ( ( 0.9330127018922194093, 0.9330127018922194093, 1.000000000000000000, 0.8660254037844387076, 1.000000000000000000, 0.8660254037844387076, 1.000000000000000000, 0.9330127018922194093, 0.9330127018922194093 ) ) 
 REPRESENTATION_ITEM ( '' )  );
#43214 = CARTESIAN_POINT ( 'NONE',  ( 2.500000000000002220, 11.33333333333333393, 4.330127018922192761 ) ) ;
#43215 = CARTESIAN_POINT ( 'NONE',  ( 2.499999999999998668, 26.66666666666666430, -4.330127018922193649 ) ) ;
#43216 = CARTESIAN_POINT ( 'NONE',  ( -5.000000000000000888, -154.5625000027311842, 2.071067811865474617 ) ) ;
#43217 = EDGE_LOOP ( 'NONE', ( #12729, #36234, #9780, #16363, #63290, #23433, #62591, #45803 ) ) ;
#43218 = CARTESIAN_POINT ( 'NONE',  ( -4.458734124999999437, -106.5624999986343937, 0.000000000000000000 ) ) ;
#43219 = CARTESIAN_POINT ( 'NONE',  ( 9.457646018065525792E-16, -31.06249999863440436, 5.148502694627439702 ) ) ;
#43220 = CARTESIAN_POINT ( 'NONE',  ( -5.000000000000000000, -69.87499999726880162, 0.000000000000000000 ) ) ;
#43221 = CARTESIAN_POINT ( 'NONE',  ( -52.10840900171896806, -149.4375000013656063, 3.393966926194110556 ) ) ;
#43222 = CARTESIAN_POINT ( 'NONE',  ( 3.061616997868383141E-16, -143.7500000000000284, -5.000000000000000000 ) ) ;
#43223 = CARTESIAN_POINT ( 'NONE',  ( 2.229367062499998831, -72.89583333196773651, -3.861377020970580887 ) ) ;
#43224 = CARTESIAN_POINT ( 'NONE',  ( -1.127183054612291972E-14, 22.37500000273118417, 4.999999999999999112 ) ) ;
#43225 = CARTESIAN_POINT ( 'NONE',  ( 4.458734124999998549, -29.72916666530107221, -2.574251347313721627 ) ) ;
#43226 = CARTESIAN_POINT ( 'NONE',  ( -5.000000000000000000, -27.95833333060214798, -2.886751345948128211 ) ) ;
#43227 = DIRECTION ( 'NONE',  ( -0.000000000000000000, 1.000000000000000000, -0.000000000000000000 ) ) ;
#43228 = CARTESIAN_POINT ( 'NONE',  ( -5.000000000000000000, -19.99999999999999645, 0.000000000000000000 ) ) ;
#43229 = CARTESIAN_POINT ( 'NONE',  ( -4.458734125000001214, -145.8750000013656063, 1.846868145590734089 ) ) ;
#43230 = ORIENTED_EDGE ( 'NONE', *, *, #30367, .F. ) ;
#43231 = CARTESIAN_POINT ( 'NONE',  ( -4.458734124999997661, -59.47916666530106511, 2.574251347313722516 ) ) ;
#43232 = CARTESIAN_POINT ( 'NONE',  ( -5.000000000000000000, 27.12500000273118772, 0.000000000000000000 ) ) ;
#43233 = CARTESIAN_POINT ( 'NONE',  ( -2.071067811865394237, -162.3125000000000568, 5.000000000000084377 ) ) ;
#43234 = CARTESIAN_POINT ( 'NONE',  ( 1.060575238724906964E-15, 17.25000000000000000, 5.773502691896257311 ) ) ;
#43235 = FACE_OUTER_BOUND ( 'NONE', #59394, .T. ) ;
#43236 = CARTESIAN_POINT ( 'NONE',  ( -4.458734124999998549, -4.229166665301070438, 2.574251347313722516 ) ) ;
#43237 = CARTESIAN_POINT ( 'NONE',  ( -6.972266317189433020E-16, 7.750000000000000000, -5.000000000000000000 ) ) ;
#43238 = EDGE_CURVE ( 'NONE', #48396, #41928, #57826, .T. ) ;
#43239 = CARTESIAN_POINT ( 'NONE',  ( 5.000000000000000000, -165.1250000027311842, 0.000000000000000000 ) ) ;
#43240 = CARTESIAN_POINT ( 'NONE',  ( 4.458734124999998549, 11.02083333469892779, -2.574251347313721627 ) ) ;
#43241 =( BOUNDED_CURVE ( )  B_SPLINE_CURVE ( 2, ( #8841, #61941, #13666, #22704, #23643, #18496, #61623, #62879, #18791 ),
 .UNSPECIFIED., .F., .F. ) 
 B_SPLINE_CURVE_WITH_KNOTS ( ( 3, 2, 2, 2, 3 ),
 ( 0.008928571428571429811, 0.009523809523809524669, 0.01071428571428571438, 0.01190476190476190410, 0.01250000000000000069 ),
 .UNSPECIFIED. ) 
 CURVE ( )  GEOMETRIC_REPRESENTATION_ITEM ( )  RATIONAL_B_SPLINE_CURVE ( ( 0.9330127018922192983, 0.9330127018922194093, 1.000000000000000000, 0.8660254037844387076, 1.000000000000000000, 0.8660254037844387076, 1.000000000000000000, 0.9330127018922191873, 0.9330127018922192983 ) ) 
 REPRESENTATION_ITEM ( '' )  );
#43242 = CARTESIAN_POINT ( 'NONE',  ( 0.000000000000000000, -170.0000000000000000, 0.000000000000000000 ) ) ;
#43243 = ORIENTED_EDGE ( 'NONE', *, *, #7490, .F. ) ;
#43244 = CARTESIAN_POINT ( 'NONE',  ( 5.000000000000000000, 0.5000000000000004441, -6.123233995736766282E-16 ) ) ;
#43245 = CARTESIAN_POINT ( 'NONE',  ( 2.229367062499998831, -48.64583333196772941, -3.861377020970580887 ) ) ;
#43246 = CARTESIAN_POINT ( 'NONE',  ( 3.152801135295367541, -159.5625000013656063, -3.152801135295367541 ) ) ;
#43247 = CARTESIAN_POINT ( 'NONE',  ( -5.000000000000000000, -47.95833333060214443, -2.886751345948128211 ) ) ;
#43248 = ORIENTED_EDGE ( 'NONE', *, *, #20924, .F. ) ;
#43249 = CARTESIAN_POINT ( 'NONE',  ( 2.229367062499998831, -22.64583333196773651, -3.861377020970580887 ) ) ;
#43250 = ORIENTED_EDGE ( 'NONE', *, *, #10696, .T. ) ;
#43252 = CARTESIAN_POINT ( 'NONE',  ( -1.339745962155613812, -103.0803417985302843, -5.000000000000000000 ) ) ;
#43251 = CARTESIAN_POINT ( 'NONE',  ( 1.975475456537005874E-15, -87.75000000000001421, 5.000000000000000000 ) ) ;
#43253 = CARTESIAN_POINT ( 'NONE',  ( 1.846868145590735200, -159.2500000013656063, -4.458734125000000326 ) ) ;
#43254 = ORIENTED_EDGE ( 'NONE', *, *, #38463, .T. ) ;
#43255 =( BOUNDED_CURVE ( )  B_SPLINE_CURVE ( 2, ( #31366, #47131, #41976, #3079, #7583, #41647, #51007, #46498, #22698 ),
 .UNSPECIFIED., .F., .F. ) 
 B_SPLINE_CURVE_WITH_KNOTS ( ( 3, 2, 2, 2, 3 ),
 ( 0.8267857142857142350, 0.8273809523809523281, 0.8285714285714286254, 0.8297619047619048116, 0.8303571428571429047 ),
 .UNSPECIFIED. ) 
 CURVE ( )  GEOMETRIC_REPRESENTATION_ITEM ( )  RATIONAL_B_SPLINE_CURVE ( ( 0.9330127018922194093, 0.9330127018922194093, 1.000000000000000000, 0.8660254037844387076, 1.000000000000000000, 0.8660254037844387076, 1.000000000000000000, 0.9330127018922194093, 0.9330127018922194093 ) ) 
 REPRESENTATION_ITEM ( '' )  );
#43256 = DIRECTION ( 'NONE',  ( 0.000000000000000000, 0.000000000000000000, 1.000000000000000000 ) ) ;
#43257 = CARTESIAN_POINT ( 'NONE',  ( -60.14911071818854538, -134.0625000000000284, 1.666127454062681368 ) ) ;
#43258 = CARTESIAN_POINT ( 'NONE',  ( 1.339745962155612702, -53.16965819600733312, -5.000000000000000000 ) ) ;
#43259 = CARTESIAN_POINT ( 'NONE',  ( -3.152548672688508926E-16, -35.81249999863440792, -5.148502694627439702 ) ) ;
#43260 = VERTEX_POINT ( 'NONE', #40506 ) ;
#43261 = EDGE_CURVE ( 'NONE', #22693, #46689, #54992, .T. ) ;
#43262 = EDGE_CURVE ( 'NONE', #9578, #20024, #40147, .T. ) ;
#43263 = CARTESIAN_POINT ( 'NONE',  ( 4.458734125000001214, -83.89583333196773651, 2.574251347313718519 ) ) ;
#43264 = CARTESIAN_POINT ( 'NONE',  ( 9.457646018065525792E-16, 16.93750000136559564, 5.148502694627439702 ) ) ;
#43265 = CYLINDRICAL_SURFACE ( 'NONE', #6076, 5.000000000000000000 ) ;
#43266 = ADVANCED_FACE ( 'NONE', ( #34730 ), #25727, .T. ) ;
#43267 = ORIENTED_EDGE ( 'NONE', *, *, #17229, .F. ) ;
#43268 = CARTESIAN_POINT ( 'NONE',  ( -50.70258187064364108, -137.3750000013656063, 2.196230717870141014 ) ) ;
#43269 = CARTESIAN_POINT ( 'NONE',  ( 2.229367062500001939, -87.22916666530107932, 3.861377020970579999 ) ) ;
#43270 = CARTESIAN_POINT ( 'NONE',  ( -51.75738570946856498, -127.8750000027312268, 3.805975901505576964 ) ) ;
#43271 = CARTESIAN_POINT ( 'NONE',  ( 1.975475456537005874E-15, -4.624999997268815832, 5.000000000000000000 ) ) ;
#43272 = CARTESIAN_POINT ( 'NONE',  ( 1.975475456537005874E-15, -8.624999997268812280, 5.000000000000000000 ) ) ;
#43273 = CARTESIAN_POINT ( 'NONE',  ( 5.000000000000000000, -13.29166666393548191, -2.886751345948130876 ) ) ;
#43274 = CARTESIAN_POINT ( 'NONE',  ( -4.458734124999997661, -62.22916666530105090, 2.574251347313722516 ) ) ;
#43275 = CARTESIAN_POINT ( 'NONE',  ( -55.39835681537999790, -151.0000000027312410, 4.984105922594378235 ) ) ;
#43276 = AXIS2_PLACEMENT_3D ( 'NONE', #48479, #4416, #38814 ) ;
#43277 = CARTESIAN_POINT ( 'NONE',  ( 4.458734125000001214, 23.10416666803225993, 2.574251347313718519 ) ) ;
#43278 = ADVANCED_FACE ( 'NONE', ( #49522 ), #50492, .T. ) ;
#43279 = CARTESIAN_POINT ( 'NONE',  ( 1.339745962155615144, -42.70534180126148982, 4.999999999999999112 ) ) ;
#43280 = DIRECTION ( 'NONE',  ( -0.000000000000000000, 1.000000000000000000, -0.000000000000000000 ) ) ;
#43281 = CARTESIAN_POINT ( 'NONE',  ( -4.458734124999998549, -45.47916666530105800, 2.574251347313722516 ) ) ;
#43282 = CARTESIAN_POINT ( 'NONE',  ( -2.499999999999996447, -6.708333330602149758, 4.330127018922195425 ) ) ;
#43283 = DIRECTION ( 'NONE',  ( -0.000000000000000000, 1.000000000000000000, -0.000000000000000000 ) ) ;
#43284 = EDGE_CURVE ( 'NONE', #60011, #51908, #41632, .T. ) ;
#43285 = CARTESIAN_POINT ( 'NONE',  ( -7.500000000000000000, -4.330127018922198090, -10.00000000000000000 ) ) ;
#43286 = CARTESIAN_POINT ( 'NONE',  ( 2.229367062499998831, -85.89583333196773651, -3.861377020970580887 ) ) ;
#43287 = CARTESIAN_POINT ( 'NONE',  ( -4.458734124999999437, -105.3958333319677365, -2.574251347313719407 ) ) ;
#43288 = CARTESIAN_POINT ( 'NONE',  ( 4.458734124999998549, -8.979166665301075767, -2.574251347313721627 ) ) ;
#43289 = ORIENTED_EDGE ( 'NONE', *, *, #58542, .T. ) ;
#43290 = CARTESIAN_POINT ( 'NONE',  ( 1.339745962155615144, -52.70534180126147561, 4.999999999999999112 ) ) ;
#43291 = CARTESIAN_POINT ( 'NONE',  ( 9.457646018065525792E-16, -99.06249999863440792, 5.148502694627439702 ) ) ;
#43292 = EDGE_CURVE ( 'NONE', #58774, #9375, #18735, .T. ) ;
#43293 = CARTESIAN_POINT ( 'NONE',  ( 3.535533905932738197, -164.0000000027312126, -3.535533905932738197 ) ) ;
#43294 = CARTESIAN_POINT ( 'NONE',  ( -4.458734124999999437, -89.56249999863440792, 0.000000000000000000 ) ) ;
#43295 = CARTESIAN_POINT ( 'NONE',  ( 5.000000000000000888, -54.45833333060214443, 2.886751345948126879 ) ) ;
#43296 = CARTESIAN_POINT ( 'NONE',  ( -3.750000000000004885, 6.495190528383289141, 0.000000000000000000 ) ) ;
#43297 = CARTESIAN_POINT ( 'NONE',  ( -50.55543936806279248, -131.0625000013656063, 0.3552334253322060320 ) ) ;
#43298 = CARTESIAN_POINT ( 'NONE',  ( -57.89159099828107458, -146.6875000013656063, -3.393966926194107447 ) ) ;
#43299 = CARTESIAN_POINT ( 'NONE',  ( -2.229367062499996610, -13.14583333196774007, 3.861377020970582219 ) ) ;
#43300 = CARTESIAN_POINT ( 'NONE',  ( 9.457646018065525792E-16, 13.68750000136559208, 5.148502694627439702 ) ) ;
#43301 = CARTESIAN_POINT ( 'NONE',  ( 4.458734125000000326, -58.14583333196773651, 2.574251347313718519 ) ) ;
#43302 = CARTESIAN_POINT ( 'NONE',  ( -6.972266317189433020E-16, -76.24999999999998579, -5.000000000000000000 ) ) ;
#43303 = DIRECTION ( 'NONE',  ( -0.000000000000000000, 1.000000000000000000, -0.000000000000000000 ) ) ;
#43304 = CARTESIAN_POINT ( 'NONE',  ( 2.229367062500001939, -12.97916666530107221, 3.861377020970579999 ) ) ;
#43305 = CARTESIAN_POINT ( 'NONE',  ( 1.975475456537005874E-15, -71.75000000000000000, 5.000000000000000000 ) ) ;
#43306 = ORIENTED_EDGE ( 'NONE', *, *, #57454, .T. ) ;
#43307 = CARTESIAN_POINT ( 'NONE',  ( -4.458734124999999437, -42.56249999863440081, 0.000000000000000000 ) ) ;
#43308 = UNCERTAINTY_MEASURE_WITH_UNIT (LENGTH_MEASURE( 1.000000000000000082E-05 ), #13100, 'distance_accuracy_value', 'NONE');
#43309 = CARTESIAN_POINT ( 'NONE',  ( 1.975475456537005874E-15, -37.74999999999999289, 5.000000000000000000 ) ) ;
#43310 = CARTESIAN_POINT ( 'NONE',  ( 2.499999999999998668, -66.33333333333332860, -4.330127018922193649 ) ) ;
#43311 = CARTESIAN_POINT ( 'NONE',  ( -5.000000000000000000, -66.95833333060214443, -2.886751345948128211 ) ) ;
#43312 = CARTESIAN_POINT ( 'NONE',  ( 4.458734124999998549, -87.72916666530107932, -2.574251347313721627 ) ) ;
#43313 = CARTESIAN_POINT ( 'NONE',  ( -3.152548672688508926E-16, 18.18750000136559564, -5.148502694627439702 ) ) ;
#43314 = CARTESIAN_POINT ( 'NONE',  ( -4.458734124999999437, 16.60416666803225993, -2.574251347313719407 ) ) ;
#43315 = CARTESIAN_POINT ( 'NONE',  ( -5.000000000000000000, -48.08333333333332860, -2.886751345948128211 ) ) ;
#43316 = CARTESIAN_POINT ( 'NONE',  ( 0.000000000000000000, 0.000000000000000000, 4.999999999999999112 ) ) ;
#43317 = CARTESIAN_POINT ( 'NONE',  ( -2.229367062499996610, -88.39583333196773651, 3.861377020970582219 ) ) ;
#43318 = CARTESIAN_POINT ( 'NONE',  ( 5.000000000000000000, -69.41666666666667140, -2.886751345948129988 ) ) ;
#43319 = CARTESIAN_POINT ( 'NONE',  ( -2.500000000000000444, 13.95833333606451809, -4.330127018922193649 ) ) ;
#43320 = ORIENTED_EDGE ( 'NONE', *, *, #45337, .T. ) ;
#43321 = CARTESIAN_POINT ( 'NONE',  ( 1.975475456537005874E-15, -79.74999999999998579, 5.000000000000000000 ) ) ;
#43323 = CARTESIAN_POINT ( 'NONE',  ( 5.000000000000000888, -26.58333333333333570, 2.886751345948126879 ) ) ;
#43322 = CARTESIAN_POINT ( 'NONE',  ( -6.972266317189433020E-16, -3.250000000000001332, -5.000000000000000000 ) ) ;
#43324 = CARTESIAN_POINT ( 'NONE',  ( 2.229367062500001939, -32.97916666530106511, 3.861377020970579999 ) ) ;
#43325 = CARTESIAN_POINT ( 'NONE',  ( 1.060575238724906964E-15, -31.62499999726880873, 5.773502691896257311 ) ) ;
#43327 = VERTEX_POINT ( 'NONE', #30211 ) ;
#43326 = CARTESIAN_POINT ( 'NONE',  ( -4.458734124999998549, -63.22916666530106511, 2.574251347313722516 ) ) ;
#43328 = CARTESIAN_POINT ( 'NONE',  ( -56.48576386720575471, -153.0000000013656063, -4.591703134518078322 ) ) ;
#43330 = ORIENTED_EDGE ( 'NONE', *, *, #3220, .T. ) ;
#43329 = CARTESIAN_POINT ( 'NONE',  ( -4.458734124999999437, -13.64583333196774007, -2.574251347313719407 ) ) ;
#43331 = CARTESIAN_POINT ( 'NONE',  ( -2.500000000000000444, -79.16666666666665719, -4.330127018922193649 ) ) ;
#43332 = CARTESIAN_POINT ( 'NONE',  ( 6.972266317189433020E-16, 28.87500000273118417, -5.000000000000000000 ) ) ;
#43333 = CARTESIAN_POINT ( 'NONE',  ( -4.458734124999999437, -57.56249999863440081, 0.000000000000000000 ) ) ;
#43334 = CARTESIAN_POINT ( 'NONE',  ( -4.999999999999999112, -83.79166666393547303, 2.886751345948131764 ) ) ;
#43336 = VERTEX_POINT ( 'NONE', #5779 ) ;
#43335 = CARTESIAN_POINT ( 'NONE',  ( 1.975475456537005874E-15, -19.62499999726881228, 5.000000000000000000 ) ) ;
#43337 = CARTESIAN_POINT ( 'NONE',  ( -49.85088928181150436, -145.5625000000000568, -1.666127454062680702 ) ) ;
#43338 = CARTESIAN_POINT ( 'NONE',  ( -2.229367062500000163, -22.72916666530107221, -3.861377020970580443 ) ) ;
#43340 = ORIENTED_EDGE ( 'NONE', *, *, #22117, .F. ) ;
#43339 = CARTESIAN_POINT ( 'NONE',  ( -3.152548672688508926E-16, -57.81249999863440081, -5.148502694627439702 ) ) ;
#43341 =( BOUNDED_CURVE ( )  B_SPLINE_CURVE ( 2, ( #61871, #3013, #42227, #8460, #37105, #17484, #52525, #56724, #7514 ),
 .UNSPECIFIED., .F., .F. ) 
 B_SPLINE_CURVE_WITH_KNOTS ( ( 3, 2, 2, 2, 3 ),
 ( 0.3910714285714285698, 0.3916666666666666630, 0.3928571428571428492, 0.3940476190476190355, 0.3946428571428571286 ),
 .UNSPECIFIED. ) 
 CURVE ( )  GEOMETRIC_REPRESENTATION_ITEM ( )  RATIONAL_B_SPLINE_CURVE ( ( 0.9330127018922194093, 0.9330127018922194093, 1.000000000000000000, 0.8660254037844387076, 1.000000000000000000, 0.8660254037844387076, 1.000000000000000000, 0.9330127018922194093, 0.9330127018922194093 ) ) 
 REPRESENTATION_ITEM ( '' )  );
#43342 = EDGE_CURVE ( 'NONE', #18684, #61278, #16306, .T. ) ;
#43343 = DIRECTION ( 'NONE',  ( 1.000000000000000000, 0.000000000000000000, 0.000000000000000000 ) ) ;
#43344 = CARTESIAN_POINT ( 'NONE',  ( -3.152801135295367096, -166.3125000013656063, -3.152801135295367541 ) ) ;
#43345 = CARTESIAN_POINT ( 'NONE',  ( -3.152548672688508926E-16, -104.8124999986344079, -5.148502694627439702 ) ) ;
#43346 = CARTESIAN_POINT ( 'NONE',  ( -4.999999999999998224, 18.08333333333333215, 2.886751345948131764 ) ) ;
#43347 = ORIENTED_EDGE ( 'NONE', *, *, #15409, .F. ) ;
#43348 = CARTESIAN_POINT ( 'NONE',  ( -57.19623071787016499, -149.6250000013655779, 4.297418129356382899 ) ) ;
#43349 = CARTESIAN_POINT ( 'NONE',  ( -50.18089887299979068, -136.8125000027311842, 2.462841084822635640 ) ) ;
#43350 = CARTESIAN_POINT ( 'NONE',  ( 4.458734124999998549, -39.72916666530107221, -2.574251347313721627 ) ) ;
#43351 = CARTESIAN_POINT ( 'NONE',  ( 1.975475456537005874E-15, -32.62499999726880873, 5.000000000000000000 ) ) ;
#43352 = CARTESIAN_POINT ( 'NONE',  ( -4.458734124999998549, -14.22916666530107221, 2.574251347313722516 ) ) ;
#43353 = CARTESIAN_POINT ( 'NONE',  ( 2.229367062500001939, -99.22916666530105090, 3.861377020970579999 ) ) ;
#43354 =( BOUNDED_CURVE ( )  B_SPLINE_CURVE ( 2, ( #17718, #27991, #21912, #51507, #46670, #51191, #7123, #52134, #47610 ),
 .UNSPECIFIED., .F., .F. ) 
 B_SPLINE_CURVE_WITH_KNOTS ( ( 3, 2, 2, 2, 3 ),
 ( 0.9187499999999999556, 0.9194444444444443976, 0.9208333333333332815, 0.9222222222222222765, 0.9229166666666667185 ),
 .UNSPECIFIED. ) 
 CURVE ( )  GEOMETRIC_REPRESENTATION_ITEM ( )  RATIONAL_B_SPLINE_CURVE ( ( 0.9330127018922194093, 0.9330127018922194093, 1.000000000000000000, 0.8660254037844387076, 1.000000000000000000, 0.8660254037844387076, 1.000000000000000000, 0.9330127018922194093, 0.9330127018922194093 ) ) 
 REPRESENTATION_ITEM ( '' )  );
#43355 = CARTESIAN_POINT ( 'NONE',  ( -8.190561711645485556E-16, -143.9375000013656063, 4.458734124999999437 ) ) ;
#43356 = CARTESIAN_POINT ( 'NONE',  ( -3.152548672688508926E-16, -25.81249999863440792, -5.148502694627439702 ) ) ;
#43357 = CARTESIAN_POINT ( 'NONE',  ( 2.500000000000002220, -70.66666666666667140, 4.330127018922192761 ) ) ;
#43358 = CARTESIAN_POINT ( 'NONE',  ( -58.39396692619412477, -132.4375000013656063, 2.891590998281057701 ) ) ;
#43359 = CARTESIAN_POINT ( 'NONE',  ( -4.458734124999999437, -70.56249999863439371, 0.000000000000000000 ) ) ;
#43360 = EDGE_CURVE ( 'NONE', #59975, #22959, #41452, .T. ) ;
#43361 = DIRECTION ( 'NONE',  ( -0.000000000000000000, 1.000000000000000000, -0.000000000000000000 ) ) ;
#43362 = CARTESIAN_POINT ( 'NONE',  ( 0.000000000000000000, -170.0000000000000000, 0.000000000000000000 ) ) ;
#43363 = CARTESIAN_POINT ( 'NONE',  ( -4.458734124999999437, -141.0000000013655779, -1.846868145590735644 ) ) ;
#43364 = CARTESIAN_POINT ( 'NONE',  ( -4.458734124999999437, 5.437500001365592972, 0.000000000000000000 ) ) ;
#43365 = VERTEX_POINT ( 'NONE', #31484 ) ;
#43366 = CYLINDRICAL_SURFACE ( 'NONE', #35690, 5.000000000000000000 ) ;
#43367 = ADVANCED_FACE ( 'NONE', ( #26993 ), #36641, .T. ) ;
#43368 = CARTESIAN_POINT ( 'NONE',  ( -6.972266317189433020E-16, 15.87500000273118417, -5.000000000000000000 ) ) ;
#43370 = CARTESIAN_POINT ( 'NONE',  ( 4.458734124999998549, -31.72916666530107577, -2.574251347313721627 ) ) ;
#43369 = CARTESIAN_POINT ( 'NONE',  ( -2.500000000000000444, -97.16666666666665719, -4.330127018922193649 ) ) ;
#43371 = CARTESIAN_POINT ( 'NONE',  ( -4.999999999999998224, -76.79166666393547303, 2.886751345948131764 ) ) ;
#43372 = CARTESIAN_POINT ( 'NONE',  ( 4.458734125000001214, -74.14583333196773651, 2.574251347313718519 ) ) ;
#43373 = CARTESIAN_POINT ( 'NONE',  ( 2.229367062499998831, 24.10416666803225993, -3.861377020970580887 ) ) ;
#43374 = CARTESIAN_POINT ( 'NONE',  ( -51.75738570946856498, -151.7500000000000284, 3.805975901505576964 ) ) ;
#43375 = CARTESIAN_POINT ( 'NONE',  ( -55.35523342533222291, -143.3125000013656063, 4.444560631937231499 ) ) ;
#43376 = EDGE_CURVE ( 'NONE', #48933, #41789, #51129, .T. ) ;
#43377 = CARTESIAN_POINT ( 'NONE',  ( -3.152548672688508926E-16, 3.437500001365594748, -5.148502694627439702 ) ) ;
#43378 = CARTESIAN_POINT ( 'NONE',  ( -4.458734124999999437, 28.43750000136559208, 0.000000000000000000 ) ) ;
#43379 = CARTESIAN_POINT ( 'NONE',  ( 4.458734124999998549, -43.97916666530106511, -2.574251347313721627 ) ) ;
#43380 = DIRECTION ( 'NONE',  ( 0.000000000000000000, 0.000000000000000000, 1.000000000000000000 ) ) ;
#43381 = CARTESIAN_POINT ( 'NONE',  ( -3.152548672688508926E-16, 1.437500001365596525, -5.148502694627439702 ) ) ;
#43382 = CARTESIAN_POINT ( 'NONE',  ( 2.229367062500001939, -24.22916666530107577, 3.861377020970579999 ) ) ;
#43383 = CARTESIAN_POINT ( 'NONE',  ( -4.458734125000000326, -154.0000000013655779, -1.846868145590735644 ) ) ;
#43384 = CARTESIAN_POINT ( 'NONE',  ( 9.457646018065525792E-16, -68.06249999863440792, 5.148502694627439702 ) ) ;
#43385 = CARTESIAN_POINT ( 'NONE',  ( -4.999999999999999112, -106.7916666639354730, 2.886751345948131764 ) ) ;
#43386 = CARTESIAN_POINT ( 'NONE',  ( -3.152548672688508926E-16, 28.43750000136559208, -5.148502694627439702 ) ) ;
#43387 = DIRECTION ( 'NONE',  ( 0.000000000000000000, 0.000000000000000000, 1.000000000000000000 ) ) ;
#43388 = CARTESIAN_POINT ( 'NONE',  ( 4.458734124999999437, -104.0624999986344079, -5.460374474430324690E-16 ) ) ;
#43389 = CARTESIAN_POINT ( 'NONE',  ( -2.229367062500000163, -72.72916666530107932, -3.861377020970580443 ) ) ;
#43390 = CARTESIAN_POINT ( 'NONE',  ( -2.500000000000000444, -55.16666666666667140, -4.330127018922193649 ) ) ;
#43391 = CARTESIAN_POINT ( 'NONE',  ( -5.000000000000000000, -65.95833333060213022, -2.886751345948128211 ) ) ;
#43392 = LINE ( 'NONE', #28602, #26355 ) ;
#43393 = ORIENTED_EDGE ( 'NONE', *, *, #28841, .F. ) ;
#43394 = CARTESIAN_POINT ( 'NONE',  ( 0.000000000000000000, 0.000000000000000000, -9.226681596905677907 ) ) ;
#43395 = CARTESIAN_POINT ( 'NONE',  ( -6.972266317189433020E-16, -27.12499999726881228, -5.000000000000000000 ) ) ;
#43396 = CARTESIAN_POINT ( 'NONE',  ( 2.500000000000002220, -10.66666666666666430, 4.330127018922192761 ) ) ;
#43397 = CARTESIAN_POINT ( 'NONE',  ( 9.457646018065525792E-16, -16.06249999863440436, 5.148502694627439702 ) ) ;
#43398 = CARTESIAN_POINT ( 'NONE',  ( -4.458734124999999437, -79.31249999863440792, 0.000000000000000000 ) ) ;
#43399 = CARTESIAN_POINT ( 'NONE',  ( -3.152801135295367096, -166.3125000013656063, -3.152801135295367541 ) ) ;
#43400 = CARTESIAN_POINT ( 'NONE',  ( -5.000000000000000000, -16.87499999726881583, 0.000000000000000000 ) ) ;
#43402 = ORIENTED_EDGE ( 'NONE', *, *, #31536, .T. ) ;
#43401 = CARTESIAN_POINT ( 'NONE',  ( -4.458734124999998549, -47.22916666530106511, 2.574251347313722516 ) ) ;
#43403 = CARTESIAN_POINT ( 'NONE',  ( 1.339745962155612702, -15.16965819600733134, -5.000000000000000000 ) ) ;
#43405 = ORIENTED_EDGE ( 'NONE', *, *, #18804, .T. ) ;
#43404 = CARTESIAN_POINT ( 'NONE',  ( 4.458734124999999437, 1.937500001365593416, -5.460374474430324690E-16 ) ) ;
#43406 = CARTESIAN_POINT ( 'NONE',  ( -59.59170313451810586, -152.5000000013655779, 1.485763867205729394 ) ) ;
#43407 = CARTESIAN_POINT ( 'NONE',  ( 5.000000000000000000, -58.41666666666665719, -2.886751345948129988 ) ) ;
#43408 = CARTESIAN_POINT ( 'NONE',  ( 4.458734124999999437, -154.7500000013656063, 1.846868145590737864 ) ) ;
#43409 = CARTESIAN_POINT ( 'NONE',  ( -4.458734124999998549, -40.47916666530107221, 2.574251347313722516 ) ) ;
#43410 = CARTESIAN_POINT ( 'NONE',  ( -5.000000000000000000, -79.08333333333332860, -2.886751345948128211 ) ) ;
#43411 =( BOUNDED_CURVE ( )  B_SPLINE_CURVE ( 2, ( #21241, #1010, #15465, #35083, #19956, #45364, #49859, #55349, #11263 ),
 .UNSPECIFIED., .F., .F. ) 
 B_SPLINE_CURVE_WITH_KNOTS ( ( 3, 2, 2, 2, 3 ),
 ( 0.2696428571428571286, 0.2702380952380952217, 0.2714285714285714080, 0.2726190476190475942, 0.2732142857142857428 ),
 .UNSPECIFIED. ) 
 CURVE ( )  GEOMETRIC_REPRESENTATION_ITEM ( )  RATIONAL_B_SPLINE_CURVE ( ( 0.9330127018922194093, 0.9330127018922194093, 1.000000000000000000, 0.8660254037844387076, 1.000000000000000000, 0.8660254037844387076, 1.000000000000000000, 0.9330127018922163007, 0.9330127018922194093 ) ) 
 REPRESENTATION_ITEM ( '' )  );
#43412 = CARTESIAN_POINT ( 'NONE',  ( 2.071067811865475505, -163.8125000000000284, -5.000000000000000888 ) ) ;
#43413 = CARTESIAN_POINT ( 'NONE',  ( 5.000000000000000000, -11.49999999999999645, -6.123233995736766282E-16 ) ) ;
#43414 = CARTESIAN_POINT ( 'NONE',  ( -58.39396692619412477, -125.6875000013656063, 2.891590998281057701 ) ) ;
#43415 = CARTESIAN_POINT ( 'NONE',  ( -4.458734124999999437, -5.645833331967740953, -2.574251347313719407 ) ) ;
#43416 = CARTESIAN_POINT ( 'NONE',  ( 4.458734124999998549, -41.97916666530107932, -2.574251347313721627 ) ) ;
#43417 = EDGE_CURVE ( 'NONE', #58830, #39750, #2253, .T. ) ;
#43418 = CARTESIAN_POINT ( 'NONE',  ( -4.999999999999998224, -24.79166666393548368, 2.886751345948131764 ) ) ;
#43419 = CARTESIAN_POINT ( 'NONE',  ( -4.458734125000000326, -149.0000000013656063, -1.846868145590735644 ) ) ;
#43420 = CARTESIAN_POINT ( 'NONE',  ( 4.458734124999998549, -90.97916666530106511, -2.574251347313721627 ) ) ;
#43421 = CARTESIAN_POINT ( 'NONE',  ( 1.339745962155615144, -108.7053418012614543, 4.999999999999999112 ) ) ;
#43422 = VERTEX_POINT ( 'NONE', #42091 ) ;
#43423 = CARTESIAN_POINT ( 'NONE',  ( -2.499999999999996447, 27.29166666939785202, 4.330127018922195425 ) ) ;
#43424 = CARTESIAN_POINT ( 'NONE',  ( -55.39835681537999790, -150.0000000027312126, 4.984105922594378235 ) ) ;
#43425 = B_SPLINE_CURVE_WITH_KNOTS ( 'NONE', 3,
 ( #15870, #15223, #20050, #770, #39655, #44807 ),
 .UNSPECIFIED., .F., .F.,
 ( 4, 2, 4 ),
 ( 0.004444412883774326306, 0.006655097293744431999, 0.008865781703714537693 ),
 .UNSPECIFIED. ) ;
#43426 = CARTESIAN_POINT ( 'NONE',  ( -6.972266317189433020E-16, -2.124999997268814056, -5.000000000000000000 ) ) ;
#43427 = CARTESIAN_POINT ( 'NONE',  ( -3.152548672688508926E-16, -77.81249999863440792, -5.148502694627439702 ) ) ;
#43428 = ORIENTED_EDGE ( 'NONE', *, *, #59851, .T. ) ;
#43429 = FACE_OUTER_BOUND ( 'NONE', #37041, .T. ) ;
#43430 = CARTESIAN_POINT ( 'NONE',  ( 4.458734124999999437, -13.06249999863440259, -5.460374474430324690E-16 ) ) ;
#43431 = CARTESIAN_POINT ( 'NONE',  ( 2.499999999999998668, -79.20833333060213022, -4.330127018922193649 ) ) ;
#43432 = CARTESIAN_POINT ( 'NONE',  ( -2.229367062499996610, -2.145833331967737845, 3.861377020970582219 ) ) ;
#43433 = CARTESIAN_POINT ( 'NONE',  ( 2.499999999999998668, -30.20833333060214443, -4.330127018922193649 ) ) ;
#43434 = CARTESIAN_POINT ( 'NONE',  ( -1.846868145590734756, -151.1250000013656347, -4.458734124999999437 ) ) ;
#43435 =( BOUNDED_CURVE ( )  B_SPLINE_CURVE ( 2, ( #58780, #44948, #14710, #15036, #34328, #39786, #29494, #49766, #34653 ),
 .UNSPECIFIED., .F., .T. ) 
 B_SPLINE_CURVE_WITH_KNOTS ( ( 3, 2, 2, 2, 3 ),
 ( 0.2479166666666666741, 0.2486111111111111160, 0.2500000000000000000, 0.2513888888888888840, 0.2520833333333333259 ),
 .UNSPECIFIED. ) 
 CURVE ( )  GEOMETRIC_REPRESENTATION_ITEM ( )  RATIONAL_B_SPLINE_CURVE ( ( 0.9330127018922194093, 0.9330127018922194093, 1.000000000000000000, 0.8660254037844387076, 1.000000000000000000, 0.8660254037844387076, 1.000000000000000000, 0.9330127018922194093, 0.9330127018922194093 ) ) 
 REPRESENTATION_ITEM ( '' )  );
#43436 = CARTESIAN_POINT ( 'NONE',  ( -3.152548672688508926E-16, 21.18750000136559208, -5.148502694627439702 ) ) ;
#43437 = ORIENTED_EDGE ( 'NONE', *, *, #21651, .T. ) ;
#43438 = CARTESIAN_POINT ( 'NONE',  ( 2.229367062499998831, -93.64583333196772230, -3.861377020970580887 ) ) ;
#43439 = CARTESIAN_POINT ( 'NONE',  ( 1.975475456537005874E-15, -47.74999999999999289, 5.000000000000000000 ) ) ;
#43440 = CARTESIAN_POINT ( 'NONE',  ( 5.000000000000000888, 0.000000000000000000, 0.000000000000000000 ) ) ;
#43441 = CARTESIAN_POINT ( 'NONE',  ( 2.229367062500001939, -15.97916666530107399, 3.861377020970579999 ) ) ;
#43442 = CARTESIAN_POINT ( 'NONE',  ( -2.500000000000000444, -85.04166666393547303, -4.330127018922193649 ) ) ;
#43443 = CARTESIAN_POINT ( 'NONE',  ( -4.999999999999998224, -72.91666666666667140, 2.886751345948131764 ) ) ;
#43444 = CARTESIAN_POINT ( 'NONE',  ( -54.64476657466781973, -151.8125000013656063, -4.444560631937228834 ) ) ;
#43445 = CARTESIAN_POINT ( 'NONE',  ( -5.000000000000000000, -42.87499999726880873, 0.000000000000000000 ) ) ;
#43446 = DIRECTION ( 'NONE',  ( -0.000000000000000000, 1.000000000000000000, -0.000000000000000000 ) ) ;
#43447 = CARTESIAN_POINT ( 'NONE',  ( -2.229367062499996610, 17.85416666803225993, 3.861377020970582219 ) ) ;
#43448 = CARTESIAN_POINT ( 'NONE',  ( 2.499999999999998668, -51.20833333060213732, -4.330127018922193649 ) ) ;
#43449 = CARTESIAN_POINT ( 'NONE',  ( 4.458734124999998549, 17.27083333469892779, -2.574251347313721627 ) ) ;
#43450 = CARTESIAN_POINT ( 'NONE',  ( 2.229367062500001939, -58.97916666530106511, 3.861377020970579999 ) ) ;
#43451 = CARTESIAN_POINT ( 'NONE',  ( 2.229367062499998831, -7.895833331967735624, -3.861377020970580887 ) ) ;
#43452 = CARTESIAN_POINT ( 'NONE',  ( -6.972266317189433020E-16, -34.12499999726881583, -5.000000000000000000 ) ) ;
#43453 = CARTESIAN_POINT ( 'NONE',  ( 5.000000000000000000, 9.499999999999998224, -6.123233995736766282E-16 ) ) ;
#43454 = CARTESIAN_POINT ( 'NONE',  ( -8.190561711645485556E-16, -167.6875000013655779, 4.458734124999999437 ) ) ;
#43455 = CARTESIAN_POINT ( 'NONE',  ( -2.500000000000000444, -21.04166666393548013, -4.330127018922193649 ) ) ;
#43456 = CARTESIAN_POINT ( 'NONE',  ( 4.458734124999999437, -52.81249999863440792, -5.460374474430324690E-16 ) ) ;
#43457 = CARTESIAN_POINT ( 'NONE',  ( -4.999999999999999112, -83.79166666393547303, 2.886751345948131764 ) ) ;
#43458 = CARTESIAN_POINT ( 'NONE',  ( -52.80376928212989185, -137.1250000013655779, -4.297418129356379346 ) ) ;
#43459 = CARTESIAN_POINT ( 'NONE',  ( 1.975475456537005874E-15, -33.62499999726880873, 5.000000000000000000 ) ) ;
#43460 = CARTESIAN_POINT ( 'NONE',  ( 0.000000000000000000, -170.0000000000000000, 5.000000000000000000 ) ) ;
#43461 = CARTESIAN_POINT ( 'NONE',  ( -2.229367062500000163, -92.72916666530106511, -3.861377020970580443 ) ) ;
#43462 = CARTESIAN_POINT ( 'NONE',  ( 1.846868145590735200, -152.5000000013656347, -4.458734124999999437 ) ) ;
#43463 = CARTESIAN_POINT ( 'NONE',  ( 5.000000000000000000, -38.49999999999999289, -6.123233995736766282E-16 ) ) ;
#43464 = CARTESIAN_POINT ( 'NONE',  ( -59.98410592259440222, -140.1250000000000284, -0.3983568153799752487 ) ) ;
#43465 = CARTESIAN_POINT ( 'NONE',  ( 3.535533905932736864, -163.1250000000000284, 3.535533905932738641 ) ) ;
#43466 = ORIENTED_EDGE ( 'NONE', *, *, #40308, .T. ) ;
#43467 = CARTESIAN_POINT ( 'NONE',  ( 4.458734125000001214, -102.8958333319677365, 2.574251347313718519 ) ) ;
#43468 = CARTESIAN_POINT ( 'NONE',  ( -4.458734124999999437, 9.354166668032261711, -2.574251347313719407 ) ) ;
#43469 = CARTESIAN_POINT ( 'NONE',  ( 5.000000000000000888, 13.54166666939785202, 2.886751345948126879 ) ) ;
#43470 = CYLINDRICAL_SURFACE ( 'NONE', #20623, 5.000000000000000000 ) ;
#43471 = CARTESIAN_POINT ( 'NONE',  ( 5.000000000000000000, 0.5833333333333314830, -2.886751345948129988 ) ) ;
#43472 = EDGE_CURVE ( 'NONE', #12526, #55226, #51262, .T. ) ;
#43473 = CARTESIAN_POINT ( 'NONE',  ( 4.458734125000000326, -59.89583333196774362, 2.574251347313718519 ) ) ;
#43474 = VECTOR ( 'NONE', #58149, 1000.000000000000000 ) ;
#43475 = CARTESIAN_POINT ( 'NONE',  ( -1.339745962155613812, 19.79465819873851729, -5.000000000000000000 ) ) ;
#43476 = CARTESIAN_POINT ( 'NONE',  ( 5.000000000000000000, -2.291666663935477466, -2.886751345948129988 ) ) ;
#43477 = CARTESIAN_POINT ( 'NONE',  ( 9.457646018065525792E-16, -27.06249999863440081, 5.148502694627439702 ) ) ;
#43478 = CARTESIAN_POINT ( 'NONE',  ( -55.39835681537999790, -144.0000000027312126, 4.984105922594378235 ) ) ;
#43479 = FACE_OUTER_BOUND ( 'NONE', #37436, .T. ) ;
#43480 = CARTESIAN_POINT ( 'NONE',  ( 1.339745962155612702, 5.705341801261479162, -5.000000000000000000 ) ) ;
#43481 = CARTESIAN_POINT ( 'NONE',  ( -5.000000000000000000, -44.08333333333334281, -2.886751345948128211 ) ) ;
#43483 = CARTESIAN_POINT ( 'NONE',  ( -3.152548672688508926E-16, -26.81249999863440436, -5.148502694627439702 ) ) ;
#43482 = CARTESIAN_POINT ( 'NONE',  ( 2.499999999999998668, 6.791666669397851130, -4.330127018922193649 ) ) ;
#43484 = DIRECTION ( 'NONE',  ( -0.000000000000000000, 1.000000000000000000, -0.000000000000000000 ) ) ;
#43485 = CARTESIAN_POINT ( 'NONE',  ( -4.458734124999998549, -71.22916666530106511, 2.574251347313722516 ) ) ;
#43486 = CARTESIAN_POINT ( 'NONE',  ( -1.846868145590734756, -145.3750000013656347, -4.458734125000000326 ) ) ;
#43487 = CARTESIAN_POINT ( 'NONE',  ( 2.229367062500001939, -74.97916666530106511, 3.861377020970579999 ) ) ;
#43488 = CARTESIAN_POINT ( 'NONE',  ( -50.40829686548195099, -141.2500000013656347, -1.485763867205728284 ) ) ;
#43489 = CARTESIAN_POINT ( 'NONE',  ( -3.152548672688508926E-16, -24.81249999863440436, -5.148502694627439702 ) ) ;
#43490 = CARTESIAN_POINT ( 'NONE',  ( 5.000000000000000888, -66.45833333060214443, 2.886751345948126879 ) ) ;
#43491 = ORIENTED_EDGE ( 'NONE', *, *, #6627, .T. ) ;
#43492 = CARTESIAN_POINT ( 'NONE',  ( 5.000000000000000000, -93.29166666393547303, -2.886751345948130876 ) ) ;
#43493 = VERTEX_POINT ( 'NONE', #17482 ) ;
#43494 = CARTESIAN_POINT ( 'NONE',  ( -2.229367062500000163, -69.72916666530107932, -3.861377020970580443 ) ) ;
#43495 = CARTESIAN_POINT ( 'NONE',  ( 2.071067811865518582, -166.1875000000000000, 4.999999999999957367 ) ) ;
#43496 = VERTEX_POINT ( 'NONE', #2068 ) ;
#43497 = PLANE ( 'NONE',  #13517 ) ;
#43498 = CARTESIAN_POINT ( 'NONE',  ( -4.999999999999998224, -82.91666666666667140, 2.886751345948131764 ) ) ;
#43499 = CARTESIAN_POINT ( 'NONE',  ( -3.152548672688508926E-16, -60.81249999863440081, -5.148502694627439702 ) ) ;
#43500 = CARTESIAN_POINT ( 'NONE',  ( 4.458734125000001214, 3.854166668032260823, 2.574251347313718519 ) ) ;
#43501 = ORIENTED_EDGE ( 'NONE', *, *, #3851, .F. ) ;
#43502 = CARTESIAN_POINT ( 'NONE',  ( 5.000000000000000888, -141.9375000000000284, -2.071067811865475505 ) ) ;
#43503 = CARTESIAN_POINT ( 'NONE',  ( -4.458734124999999437, 16.60416666803225993, -2.574251347313719407 ) ) ;
#43504 = CARTESIAN_POINT ( 'NONE',  ( -54.64476657466781973, -144.8125000013656063, -4.444560631937228834 ) ) ;
#43505 = CARTESIAN_POINT ( 'NONE',  ( -6.972266317189433020E-16, -92.12499999726878741, -5.000000000000000000 ) ) ;
#43506 = CARTESIAN_POINT ( 'NONE',  ( 4.458734124999997661, -164.5000000013655779, 1.846868145590737864 ) ) ;
#43507 = ORIENTED_EDGE ( 'NONE', *, *, #32707, .T. ) ;
#43508 = CARTESIAN_POINT ( 'NONE',  ( 4.458734124999998549, -76.72916666530106511, -2.574251347313721627 ) ) ;
#43509 = CARTESIAN_POINT ( 'NONE',  ( 5.000000000000000000, -39.49999999999999289, -6.123233995736766282E-16 ) ) ;
#43510 = CARTESIAN_POINT ( 'NONE',  ( -2.229367062499996610, 2.854166668032259935, 3.861377020970582219 ) ) ;
#43511 = AXIS2_PLACEMENT_3D ( 'NONE', #3205, #55966, #41785 ) ;
#43512 = CARTESIAN_POINT ( 'NONE',  ( 4.458734124999998549, -62.97916666530107221, -2.574251347313721627 ) ) ;
#43513 = CARTESIAN_POINT ( 'NONE',  ( 5.000000000000000000, -18.29166666393548013, -2.886751345948129988 ) ) ;
#43514 = CARTESIAN_POINT ( 'NONE',  ( 1.975475456537005874E-15, 20.24999999999999645, 5.000000000000000000 ) ) ;
#43515 = DIRECTION ( 'NONE',  ( -0.000000000000000000, 1.000000000000000000, -0.000000000000000000 ) ) ;
#43516 = CARTESIAN_POINT ( 'NONE',  ( -5.000000000000000000, -59.00000000000000000, 0.000000000000000000 ) ) ;
#43517 = CARTESIAN_POINT ( 'NONE',  ( -48.00000000000002132, -135.0000000000000284, 4.041451884327384114 ) ) ;
#43518 = CARTESIAN_POINT ( 'NONE',  ( 5.000000000000000000, -43.29166666393548013, -2.886751345948130876 ) ) ;
#43519 = CARTESIAN_POINT ( 'NONE',  ( 9.457646018065525792E-16, -41.06249999863440792, 5.148502694627439702 ) ) ;
#43520 = PRODUCT_DEFINITION_SHAPE ( 'NONE', 'NONE',  #24902 ) ;
#43521 = CARTESIAN_POINT ( 'NONE',  ( 2.229367062499998831, -26.89583333196774007, -3.861377020970580887 ) ) ;
#43522 = CARTESIAN_POINT ( 'NONE',  ( -4.458734124999997661, 9.520833334698927786, 2.574251347313722516 ) ) ;
#43523 = CARTESIAN_POINT ( 'NONE',  ( 1.975475456537005874E-15, 11.24999999999999822, 5.000000000000000000 ) ) ;
#43524 = CARTESIAN_POINT ( 'NONE',  ( -2.500000000000000444, 27.83333333333333215, -4.330127018922193649 ) ) ;
#43525 = CARTESIAN_POINT ( 'NONE',  ( -3.535533905932737309, -149.7500000027312126, -3.535533905932738197 ) ) ;
#43526 = CARTESIAN_POINT ( 'NONE',  ( 4.458734125000001214, -108.1458333319677365, 2.574251347313718519 ) ) ;
#43527 = CARTESIAN_POINT ( 'NONE',  ( 4.458734124999998549, -35.72916666530107221, -2.574251347313721627 ) ) ;
#43528 = CARTESIAN_POINT ( 'NONE',  ( -2.499999999999996447, -69.70833333060214443, 4.330127018922195425 ) ) ;
#43529 = CARTESIAN_POINT ( 'NONE',  ( -59.44456063193725015, -146.8125000013656063, -0.3552334253322034230 ) ) ;
#43530 =( BOUNDED_CURVE ( )  B_SPLINE_CURVE ( 2, ( #10799, #54222, #25598, #21093, #41018, #26229, #5661, #30738, #10473 ),
 .UNSPECIFIED., .F., .F. ) 
 B_SPLINE_CURVE_WITH_KNOTS ( ( 3, 2, 2, 2, 3 ),
 ( 0.8770833333333333259, 0.8777777777777777679, 0.8791666666666666519, 0.8805555555555555358, 0.8812499999999999778 ),
 .UNSPECIFIED. ) 
 CURVE ( )  GEOMETRIC_REPRESENTATION_ITEM ( )  RATIONAL_B_SPLINE_CURVE ( ( 0.9330127018922194093, 0.9330127018922194093, 1.000000000000000000, 0.8660254037844387076, 1.000000000000000000, 0.8660254037844387076, 1.000000000000000000, 0.9330127018922194093, 0.9330127018922194093 ) ) 
 REPRESENTATION_ITEM ( '' )  );
#43531 = CARTESIAN_POINT ( 'NONE',  ( -2.071067811865478170, -144.3125000000000284, 5.000000000000000000 ) ) ;
#43532 = CARTESIAN_POINT ( 'NONE',  ( -4.458734124999999437, -73.56249999863439371, 0.000000000000000000 ) ) ;
#43533 = CARTESIAN_POINT ( 'NONE',  ( -55.39835681537999790, -136.8750000000000284, 4.984105922594378235 ) ) ;
#43534 = CARTESIAN_POINT ( 'NONE',  ( 2.229367062499998831, -30.64583333196773651, -3.861377020970580887 ) ) ;
#43535 = DIRECTION ( 'NONE',  ( -0.000000000000000000, 1.000000000000000000, -0.000000000000000000 ) ) ;
#43536 = CARTESIAN_POINT ( 'NONE',  ( 1.975475456537005874E-15, -107.6249999972687874, 5.000000000000000000 ) ) ;
#43537 = CARTESIAN_POINT ( 'NONE',  ( 5.000000000000000000, -21.50000000000000000, -6.123233995736766282E-16 ) ) ;
#43538 = CARTESIAN_POINT ( 'NONE',  ( 3.152801135295367541, -143.3125000013655779, -3.152801135295367541 ) ) ;
#43539 = ORIENTED_EDGE ( 'NONE', *, *, #28390, .T. ) ;
#43540 = CARTESIAN_POINT ( 'NONE',  ( 2.229367062499998831, 28.10416666803225993, -3.861377020970580887 ) ) ;
#43541 = CARTESIAN_POINT ( 'NONE',  ( -1.339745962155610925, -78.66965819600731891, 5.000000000000000000 ) ) ;
#43542 = CARTESIAN_POINT ( 'NONE',  ( 2.229367062499998831, -55.89583333196773651, -3.861377020970580887 ) ) ;
#43543 = CARTESIAN_POINT ( 'NONE',  ( -2.500000000000000444, 28.95833333606451987, -4.330127018922193649 ) ) ;
#43544 = CARTESIAN_POINT ( 'NONE',  ( 2.499999999999998668, 13.79166666939785202, -4.330127018922193649 ) ) ;
#43545 = CARTESIAN_POINT ( 'NONE',  ( 2.500000000000002220, 17.33333333333333215, 4.330127018922192761 ) ) ;
#43546 = EDGE_CURVE ( 'NONE', #27379, #942, #40904, .T. ) ;
#43547 = CARTESIAN_POINT ( 'NONE',  ( -1.339745962155610925, -36.66965819600732601, 5.000000000000000000 ) ) ;
#43548 = CARTESIAN_POINT ( 'NONE',  ( 2.229367062499998831, -7.645833331967735624, -3.861377020970580887 ) ) ;
#43549 = CARTESIAN_POINT ( 'NONE',  ( -5.000000000000000000, -23.00000000000000000, 0.000000000000000000 ) ) ;
#43550 = CARTESIAN_POINT ( 'NONE',  ( -50.01589407740564042, -145.7500000027312126, 0.3983568153799778022 ) ) ;
#43551 = CARTESIAN_POINT ( 'NONE',  ( 3.061616997868383141E-16, -157.8750000027311842, -5.000000000000000000 ) ) ;
#43552 = CARTESIAN_POINT ( 'NONE',  ( 4.458734124999998549, -19.72916666530107221, -2.574251347313721627 ) ) ;
#43553 = CARTESIAN_POINT ( 'NONE',  ( -51.75738570946856498, -135.8750000027312410, 3.805975901505576964 ) ) ;
#43554 = CARTESIAN_POINT ( 'NONE',  ( -2.229367062499996610, -53.14583333196773651, 3.861377020970582219 ) ) ;
#43555 = CARTESIAN_POINT ( 'NONE',  ( 1.846868145590735200, -159.5000000013655779, -4.458734125000000326 ) ) ;
#43556 = ADVANCED_FACE ( 'NONE', ( #47061 ), #51265, .T. ) ;
#43557 = CARTESIAN_POINT ( 'NONE',  ( -5.000000000000000000, -52.87499999726881583, 0.000000000000000000 ) ) ;
#43558 = ORIENTED_EDGE ( 'NONE', *, *, #5165, .F. ) ;
#43560 = ADVANCED_FACE ( 'NONE', ( #7198 ), #37103, .T. ) ;
#43559 = CARTESIAN_POINT ( 'NONE',  ( 4.458734124999999437, 6.937500001365594748, -5.460374474430324690E-16 ) ) ;
#43561 = VERTEX_POINT ( 'NONE', #7512 ) ;
#43562 = CARTESIAN_POINT ( 'NONE',  ( -9.184850993605147944E-16, -143.3750000027312126, 5.000000000000000000 ) ) ;
#43563 = CARTESIAN_POINT ( 'NONE',  ( 3.152801135295366208, -158.5625000013656063, 3.152801135295367985 ) ) ;
#43564 = ORIENTED_EDGE ( 'NONE', *, *, #37702, .F. ) ;
#43565 = CARTESIAN_POINT ( 'NONE',  ( 5.000000000000000888, -23.45833333060214443, 2.886751345948126879 ) ) ;
#43566 = CARTESIAN_POINT ( 'NONE',  ( -51.75738570946856498, -131.7500000000000284, 3.805975901505576964 ) ) ;
#43567 = CARTESIAN_POINT ( 'NONE',  ( 5.000000000000000000, -53.37499999726881583, -6.123233995736766282E-16 ) ) ;
#43568 = CARTESIAN_POINT ( 'NONE',  ( -3.152548672688508926E-16, -40.81249999863440081, -5.148502694627439702 ) ) ;
#43569 = VERTEX_POINT ( 'NONE', #61869 ) ;
#43570 = EDGE_CURVE ( 'NONE', #31695, #6727, #27380, .T. ) ;
#43571 = CARTESIAN_POINT ( 'NONE',  ( 2.071067811865392461, -143.3125000027312410, 5.000000000000084377 ) ) ;
#43572 = CARTESIAN_POINT ( 'NONE',  ( 4.458734124999999437, 20.18750000136559208, -5.460374474430324690E-16 ) ) ;
#43573 = CARTESIAN_POINT ( 'NONE',  ( 0.000000000000000000, -170.0000000000000000, 5.000000000000000000 ) ) ;
#43574 =( BOUNDED_CURVE ( )  B_SPLINE_CURVE ( 2, ( #54433, #40895, #40269, #45735, #59583, #40580, #15185, #10675, #15517 ),
 .UNSPECIFIED., .F., .F. ) 
 B_SPLINE_CURVE_WITH_KNOTS ( ( 3, 2, 2, 2, 3 ),
 ( 0.4270833333333333148, 0.4277777777777777568, 0.4291666666666666408, 0.4305555555555555802, 0.4312500000000000222 ),
 .UNSPECIFIED. ) 
 CURVE ( )  GEOMETRIC_REPRESENTATION_ITEM ( )  RATIONAL_B_SPLINE_CURVE ( ( 0.9330127018922194093, 0.9330127018922194093, 1.000000000000000000, 0.8660254037844387076, 1.000000000000000000, 0.8660254037844387076, 1.000000000000000000, 0.9330127018922194093, 0.9330127018922194093 ) ) 
 REPRESENTATION_ITEM ( '' )  );
#43575 = VERTEX_POINT ( 'NONE', #61195 ) ;
#43576 = CARTESIAN_POINT ( 'NONE',  ( -4.458734124999998549, -87.47916666530107932, 2.574251347313722516 ) ) ;
#43577 = CARTESIAN_POINT ( 'NONE',  ( -51.75738570946856498, -126.8750000027312126, 3.805975901505576964 ) ) ;
#43578 = CARTESIAN_POINT ( 'NONE',  ( 1.339745962155612702, -4.169658196007335782, -5.000000000000000000 ) ) ;
#43579 = DIRECTION ( 'NONE',  ( 7.709882115452476194E-16, 0.000000000000000000, -1.000000000000000000 ) ) ;
#43580 =( BOUNDED_CURVE ( )  B_SPLINE_CURVE ( 2, ( #37884, #47222, #3165, #57515, #33058, #28216, #22146, #47830, #22784 ),
 .UNSPECIFIED., .F., .F. ) 
 B_SPLINE_CURVE_WITH_KNOTS ( ( 3, 2, 2, 2, 3 ),
 ( 0.5017857142857142794, 0.5023809523809523725, 0.5035714285714285587, 0.5047619047619047450, 0.5053571428571428381 ),
 .UNSPECIFIED. ) 
 CURVE ( )  GEOMETRIC_REPRESENTATION_ITEM ( )  RATIONAL_B_SPLINE_CURVE ( ( 0.9330127018922194093, 0.9330127018922194093, 1.000000000000000000, 0.8660254037844387076, 1.000000000000000000, 0.8660254037844387076, 1.000000000000000000, 0.9330127018922194093, 0.9330127018922194093 ) ) 
 REPRESENTATION_ITEM ( '' )  );
#43581 = CARTESIAN_POINT ( 'NONE',  ( -1.339745962155613812, -103.2053418012614969, -5.000000000000000000 ) ) ;
#43582 = CARTESIAN_POINT ( 'NONE',  ( -4.458734124999999437, -58.39583333196773651, -2.574251347313719407 ) ) ;
#43583 = DIRECTION ( 'NONE',  ( -0.000000000000000000, 1.000000000000000000, -0.000000000000000000 ) ) ;
#43584 = CARTESIAN_POINT ( 'NONE',  ( -4.458734124999999437, 21.68750000136559208, 0.000000000000000000 ) ) ;
#43585 = CARTESIAN_POINT ( 'NONE',  ( -9.184850993605147944E-16, -149.2500000000000284, 5.000000000000000000 ) ) ;
#43586 = CARTESIAN_POINT ( 'NONE',  ( 6.123233995736766282E-16, -170.0000000000000000, -5.000000000000000000 ) ) ;
#43587 = CARTESIAN_POINT ( 'NONE',  ( -2.229367062500000163, -46.72916666530106511, -3.861377020970580443 ) ) ;
#43588 = EDGE_CURVE ( 'NONE', #9066, #17838, #17117, .T. ) ;
#43589 = CARTESIAN_POINT ( 'NONE',  ( 5.000000000000000888, -3.458333330602147093, 2.886751345948126879 ) ) ;
#43590 = CARTESIAN_POINT ( 'NONE',  ( -51.75738570946856498, -153.7500000000000284, 3.805975901505576964 ) ) ;
#43591 = LINE ( 'NONE', #63233, #36851 ) ;
#43592 = CARTESIAN_POINT ( 'NONE',  ( 9.457646018065525792E-16, -84.31249999863437949, 5.148502694627439702 ) ) ;
#43593 = CARTESIAN_POINT ( 'NONE',  ( -4.458734124999999437, -11.64583333196774184, -2.574251347313719407 ) ) ;
#43594 = ORIENTED_EDGE ( 'NONE', *, *, #4348, .T. ) ;
#43595 = CARTESIAN_POINT ( 'NONE',  ( -5.000000000000000000, 18.12500000273118417, 0.000000000000000000 ) ) ;
#43596 = CARTESIAN_POINT ( 'NONE',  ( 2.229367062500001939, -96.97916666530105090, 3.861377020970579999 ) ) ;
#43597 = CARTESIAN_POINT ( 'NONE',  ( -5.000000000000000888, -160.5625000027312126, 2.071067811865474617 ) ) ;
#43598 = CARTESIAN_POINT ( 'NONE',  ( -2.229367062500000163, -92.72916666530106511, -3.861377020970580443 ) ) ;
#43599 = CARTESIAN_POINT ( 'NONE',  ( 5.000000000000000000, -54.29166666393549434, -2.886751345948129988 ) ) ;
#43600 = DIRECTION ( 'NONE',  ( 0.000000000000000000, 0.000000000000000000, 1.000000000000000000 ) ) ;
#43601 = CARTESIAN_POINT ( 'NONE',  ( -55.35523342533222291, -129.3125000013656063, 4.444560631937231499 ) ) ;
#43602 = CARTESIAN_POINT ( 'NONE',  ( -57.19623071787016499, -145.3750000013656063, 4.297418129356382899 ) ) ;
#43603 = CARTESIAN_POINT ( 'NONE',  ( 2.229367062500001939, -16.97916666530106866, 3.861377020970579999 ) ) ;
#43604 = CARTESIAN_POINT ( 'NONE',  ( 2.229367062500001939, 8.770833334698927786, 3.861377020970579999 ) ) ;
#43605 =( BOUNDED_CURVE ( )  B_SPLINE_CURVE ( 2, ( #8529, #47447, #57119, #42301, #38417, #57741, #17558, #42618, #32654 ),
 .UNSPECIFIED., .F., .F. ) 
 B_SPLINE_CURVE_WITH_KNOTS ( ( 3, 2, 2, 2, 3 ),
 ( 0.3395833333333333481, 0.3402777777777777901, 0.3416666666666666741, 0.3430555555555555580, 0.3437500000000000000 ),
 .UNSPECIFIED. ) 
 CURVE ( )  GEOMETRIC_REPRESENTATION_ITEM ( )  RATIONAL_B_SPLINE_CURVE ( ( 0.9330127018922194093, 0.9330127018922194093, 1.000000000000000000, 0.8660254037844387076, 1.000000000000000000, 0.8660254037844387076, 1.000000000000000000, 0.9330127018922194093, 0.9330127018922194093 ) ) 
 REPRESENTATION_ITEM ( '' )  );
#43606 = CARTESIAN_POINT ( 'NONE',  ( 4.458734124999999437, -57.06249999863440081, -5.460374474430324690E-16 ) ) ;
#43607 = DIRECTION ( 'NONE',  ( -0.000000000000000000, 1.000000000000000000, -0.000000000000000000 ) ) ;
#43608 = CARTESIAN_POINT ( 'NONE',  ( 2.229367062499998831, -15.64583333196773651, -3.861377020970580887 ) ) ;
#43609 = CARTESIAN_POINT ( 'NONE',  ( 1.975475456537005874E-15, -8.624999997268812280, 5.000000000000000000 ) ) ;
#43610 = CARTESIAN_POINT ( 'NONE',  ( 3.535533905932736864, -155.1250000000000000, 3.535533905932738641 ) ) ;
#43611 = ORIENTED_EDGE ( 'NONE', *, *, #62887, .T. ) ;
#43612 = CARTESIAN_POINT ( 'NONE',  ( -4.458734124999997661, -40.47916666530107221, 2.574251347313722516 ) ) ;
#43613 = CARTESIAN_POINT ( 'NONE',  ( 1.339745962155612702, -83.16965819600733312, -5.000000000000000000 ) ) ;
#43614 = CARTESIAN_POINT ( 'NONE',  ( 1.062108568985190270E-13, -12.25000000000000000, -4.999999999999999112 ) ) ;
#43615 = CARTESIAN_POINT ( 'NONE',  ( -1.339745962155613812, -25.20534180126147561, -5.000000000000000000 ) ) ;
#43616 = CARTESIAN_POINT ( 'NONE',  ( 4.458734124999998549, -83.72916666530107932, -2.574251347313721627 ) ) ;
#43617 = CARTESIAN_POINT ( 'NONE',  ( 9.457646018065525792E-16, 16.68750000136559564, 5.148502694627439702 ) ) ;
#43618 = EDGE_CURVE ( 'NONE', #31318, #22078, #19477, .T. ) ;
#43619 = CARTESIAN_POINT ( 'NONE',  ( -4.458734124999999437, 11.68750000136559564, 0.000000000000000000 ) ) ;
#43620 = EDGE_CURVE ( 'NONE', #10332, #27379, #47480, .T. ) ;
#43621 = EDGE_CURVE ( 'NONE', #1553, #30363, #31911, .T. ) ;
#43622 = DIRECTION ( 'NONE',  ( -0.000000000000000000, 1.000000000000000000, -0.000000000000000000 ) ) ;
#43623 = CARTESIAN_POINT ( 'NONE',  ( -3.152548672688508926E-16, -87.81249999863437949, -5.148502694627439702 ) ) ;
#43624 = CARTESIAN_POINT ( 'NONE',  ( -3.535250795749689387E-16, -68.25000000000000000, -5.773502691896257311 ) ) ;
#43625 = CARTESIAN_POINT ( 'NONE',  ( -5.000000000000000000, 15.12500000273118417, 0.000000000000000000 ) ) ;
#43626 = VERTEX_POINT ( 'NONE', #23206 ) ;
#43627 = CARTESIAN_POINT ( 'NONE',  ( 2.500000000000002220, -102.6666666666666572, 4.330127018922192761 ) ) ;
#43628 = EDGE_LOOP ( 'NONE', ( #34466, #43254, #16068, #26768 ) ) ;
#43629 = CARTESIAN_POINT ( 'NONE',  ( -49.85088928181150436, -144.6875000027312410, -1.666127454062680480 ) ) ;
#43630 =( BOUNDED_CURVE ( )  B_SPLINE_CURVE ( 2, ( #41881, #47353, #22924, #37081, #23543, #61846, #47660, #17458, #3613 ),
 .UNSPECIFIED., .F., .F. ) 
 B_SPLINE_CURVE_WITH_KNOTS ( ( 3, 2, 2, 2, 3 ),
 ( 0.6812500000000000222, 0.6819444444444444642, 0.6833333333333333481, 0.6847222222222222321, 0.6854166666666666741 ),
 .UNSPECIFIED. ) 
 CURVE ( )  GEOMETRIC_REPRESENTATION_ITEM ( )  RATIONAL_B_SPLINE_CURVE ( ( 0.9330127018922194093, 0.9330127018922194093, 1.000000000000000000, 0.8660254037844387076, 1.000000000000000000, 0.8660254037844387076, 1.000000000000000000, 0.9330127018922194093, 0.9330127018922194093 ) ) 
 REPRESENTATION_ITEM ( '' )  );
#43632 = CARTESIAN_POINT ( 'NONE',  ( -5.000000000000000000, -36.08333333333332860, -2.886751345948128211 ) ) ;
#43631 = CARTESIAN_POINT ( 'NONE',  ( -6.972266317189433020E-16, 4.875000002731184168, -5.000000000000000000 ) ) ;
#43633 = CARTESIAN_POINT ( 'NONE',  ( 2.229367062499998831, -38.64583333196773651, -3.861377020970580887 ) ) ;
#43634 = CARTESIAN_POINT ( 'NONE',  ( 1.060575238724906964E-15, -34.62499999726880873, 5.773502691896257311 ) ) ;
#43636 = EDGE_LOOP ( 'NONE', ( #12280, #477, #10259, #10998 ) ) ;
#43635 = CARTESIAN_POINT ( 'NONE',  ( 4.458734125000001214, -65.89583333196772230, 2.574251347313718519 ) ) ;
#43637 = CARTESIAN_POINT ( 'NONE',  ( -57.89159099828107458, -151.9375000013656063, -3.393966926194107447 ) ) ;
#43639 = EDGE_CURVE ( 'NONE', #20419, #54097, #18380, .T. ) ;
#43638 = CARTESIAN_POINT ( 'NONE',  ( 4.458734124999998549, -13.72916666530107399, -2.574251347313721627 ) ) ;
#43641 = ORIENTED_EDGE ( 'NONE', *, *, #50029, .F. ) ;
#43640 = CARTESIAN_POINT ( 'NONE',  ( -4.458734124999998549, -15.47916666530107399, 2.574251347313722516 ) ) ;
#43642 = CARTESIAN_POINT ( 'NONE',  ( -5.000000000000000000, -75.00000000000000000, 0.000000000000000000 ) ) ;
#43643 = CARTESIAN_POINT ( 'NONE',  ( -53.51423613279429503, -135.2500000013656347, 4.591703134518083651 ) ) ;
#43644 = CARTESIAN_POINT ( 'NONE',  ( -4.458734124999999437, -59.56249999863440081, 0.000000000000000000 ) ) ;
#43645 = CARTESIAN_POINT ( 'NONE',  ( 5.000000000000000000, -84.37499999726880162, -6.123233995736766282E-16 ) ) ;
#43647 = ORIENTED_EDGE ( 'NONE', *, *, #58246, .F. ) ;
#43646 = DIRECTION ( 'NONE',  ( 1.000000000000000000, 0.000000000000000000, 0.000000000000000000 ) ) ;
#43648 = CARTESIAN_POINT ( 'NONE',  ( -58.24261429053147765, -146.2500000000000284, -3.805975901505573855 ) ) ;
#43649 = CARTESIAN_POINT ( 'NONE',  ( 2.229367062499998831, -22.89583333196773651, -3.861377020970580887 ) ) ;
#43650 = ORIENTED_EDGE ( 'NONE', *, *, #50396, .T. ) ;
#43651 = CARTESIAN_POINT ( 'NONE',  ( 1.846868145590735200, -168.5000000013656063, -4.458734125000000326 ) ) ;
#43652 = CARTESIAN_POINT ( 'NONE',  ( 4.458734124999998549, -105.9791666653010651, -2.574251347313721627 ) ) ;
#43653 = CARTESIAN_POINT ( 'NONE',  ( 2.500000000000002220, -8.541666663935483683, 4.330127018922192761 ) ) ;
#43654 = ORIENTED_EDGE ( 'NONE', *, *, #11348, .F. ) ;
#43655 = CARTESIAN_POINT ( 'NONE',  ( -53.51423613279429503, -149.5000000013656063, 4.591703134518083651 ) ) ;
#43656 = CARTESIAN_POINT ( 'NONE',  ( -59.98410592259440222, -138.2500000027312126, -0.3983568153799752487 ) ) ;
#43657 = CARTESIAN_POINT ( 'NONE',  ( 2.229367062500001939, -38.97916666530107221, 3.861377020970579999 ) ) ;
#43658 = CARTESIAN_POINT ( 'NONE',  ( 1.975475456537005874E-15, -83.74999999999998579, 5.000000000000000000 ) ) ;
#43659 = CARTESIAN_POINT ( 'NONE',  ( 0.000000000000000000, -120.0000000000000000, 0.000000000000000000 ) ) ;
#43660 = CARTESIAN_POINT ( 'NONE',  ( 4.458734125000001214, -13.89583333196774007, 2.574251347313718519 ) ) ;
#43661 = CARTESIAN_POINT ( 'NONE',  ( -4.458734124999999437, -102.6458333319677365, -2.574251347313719407 ) ) ;
#43662 = ORIENTED_EDGE ( 'NONE', *, *, #2413, .F. ) ;
#43663 = CARTESIAN_POINT ( 'NONE',  ( -4.458734124999999437, -144.1875000013656063, -5.460374474430324690E-16 ) ) ;
#43664 = CARTESIAN_POINT ( 'NONE',  ( -2.229367062499996610, -30.39583333196773651, 3.861377020970582219 ) ) ;
#43665 = CARTESIAN_POINT ( 'NONE',  ( 5.000000000000000888, -70.58333333333332860, 2.886751345948126879 ) ) ;
#43666 = CARTESIAN_POINT ( 'NONE',  ( -50.70258187064364108, -133.1250000013656063, 2.196230717870141014 ) ) ;
#43667 = CARTESIAN_POINT ( 'NONE',  ( 9.457646018065525792E-16, -68.31249999863442213, 5.148502694627439702 ) ) ;
#43668 = CARTESIAN_POINT ( 'NONE',  ( -6.972266317189433020E-16, -47.12499999726880873, -5.000000000000000000 ) ) ;
#43669 = CARTESIAN_POINT ( 'NONE',  ( -5.000000000000000000, -0.9583333306021485365, -2.886751345948128211 ) ) ;
#43670 = CARTESIAN_POINT ( 'NONE',  ( 1.846868145590735200, -140.2500000013656063, -4.458734124999999437 ) ) ;
#43671 = CARTESIAN_POINT ( 'NONE',  ( 2.229367062500001939, 2.770833334698928674, 3.861377020970579999 ) ) ;
#43672 = ORIENTED_EDGE ( 'NONE', *, *, #49435, .F. ) ;
#43673 = CARTESIAN_POINT ( 'NONE',  ( -6.972266317189433020E-16, -50.12499999726881583, -5.000000000000000000 ) ) ;
#43674 = CARTESIAN_POINT ( 'NONE',  ( 6.158835246850667461E-14, 9.749999999999996447, -4.999999999999999112 ) ) ;
#43676 = CARTESIAN_POINT ( 'NONE',  ( 2.229367062499998831, -29.64583333196773296, -3.861377020970580887 ) ) ;
#43675 = CARTESIAN_POINT ( 'NONE',  ( 2.499999999999998668, -94.33333333333332860, -4.330127018922193649 ) ) ;
#43677 = CARTESIAN_POINT ( 'NONE',  ( 2.500000000000002220, -73.66666666666665719, 4.330127018922192761 ) ) ;
#43678 = CARTESIAN_POINT ( 'NONE',  ( 4.458734124999999437, -76.06249999863440792, -5.460374474430324690E-16 ) ) ;
#43679 = CARTESIAN_POINT ( 'NONE',  ( -4.458734124999999437, 20.43750000136559208, 0.000000000000000000 ) ) ;
#43680 = DIRECTION ( 'NONE',  ( -0.000000000000000000, 1.000000000000000000, -0.000000000000000000 ) ) ;
#43681 = CARTESIAN_POINT ( 'NONE',  ( -52.80376928212989185, -140.8750000013656063, -4.297418129356379346 ) ) ;
#43682 = CARTESIAN_POINT ( 'NONE',  ( -4.458734124999999437, -2.312499998634407028, 0.000000000000000000 ) ) ;
#43683 = CARTESIAN_POINT ( 'NONE',  ( 2.229367062499998831, 29.10416666803225993, -3.861377020970580887 ) ) ;
#43684 = CARTESIAN_POINT ( 'NONE',  ( -4.458734124999999437, -44.56249999863440081, 0.000000000000000000 ) ) ;
#43685 = LINE ( 'NONE', #53668, #30486 ) ;
#43686 = CARTESIAN_POINT ( 'NONE',  ( 9.457646018065525792E-16, 2.937500001365594304, 5.148502694627439702 ) ) ;
#43687 = ORIENTED_EDGE ( 'NONE', *, *, #58688, .T. ) ;
#43688 = CARTESIAN_POINT ( 'NONE',  ( -4.458734124999997661, -27.47916666530107221, 2.574251347313722516 ) ) ;
#43689 = CARTESIAN_POINT ( 'NONE',  ( -1.846868145590737420, -156.7500000013656063, 4.458734124999999437 ) ) ;
#43690 = CARTESIAN_POINT ( 'NONE',  ( -2.229367062500000163, -71.47916666530107932, -3.861377020970580443 ) ) ;
#43691 = CARTESIAN_POINT ( 'NONE',  ( 5.000000000000000000, -103.2916666639354730, -2.886751345948129988 ) ) ;
#43692 = CARTESIAN_POINT ( 'NONE',  ( 4.458734124999998549, 23.27083333469892423, -2.574251347313721627 ) ) ;
#43693 = ADVANCED_FACE ( 'NONE', ( #22907 ), #62139, .T. ) ;
#43694 = CARTESIAN_POINT ( 'NONE',  ( -6.972266317189433020E-16, -84.24999999999998579, -5.000000000000000000 ) ) ;
#43695 = CARTESIAN_POINT ( 'NONE',  ( -2.229367062499996610, -110.3958333319677507, 3.861377020970582219 ) ) ;
#43696 = CARTESIAN_POINT ( 'NONE',  ( -2.229367062499996610, -72.39583333196773651, 3.861377020970582219 ) ) ;
#43697 = CARTESIAN_POINT ( 'NONE',  ( -2.499999999999996447, -53.83333333333332860, 4.330127018922195425 ) ) ;
#43698 = EDGE_CURVE ( 'NONE', #17322, #16392, #40527, .T. ) ;
#43699 = CARTESIAN_POINT ( 'NONE',  ( 5.000000000000000000, 28.62500000273118417, -6.123233995736766282E-16 ) ) ;
#43700 = EDGE_LOOP ( 'NONE', ( #31389, #58486, #10899, #45397 ) ) ;
#43701 = DIRECTION ( 'NONE',  ( 0.000000000000000000, -1.000000000000000000, 0.000000000000000000 ) ) ;
#43702 = EDGE_CURVE ( 'NONE', #26835, #22293, #52491, .T. ) ;
#43703 = CARTESIAN_POINT ( 'NONE',  ( -5.000000000000000000, 12.04166666939785202, -2.886751345948128211 ) ) ;
#43704 = CARTESIAN_POINT ( 'NONE',  ( 5.000000000000000888, -15.58333333333333215, 2.886751345948126879 ) ) ;
#43705 = CARTESIAN_POINT ( 'NONE',  ( -2.229367062500000163, -17.47916666530106866, -3.861377020970580443 ) ) ;
#43706 = ADVANCED_FACE ( 'NONE', ( #21945 ), #57001, .T. ) ;
#43707 = CARTESIAN_POINT ( 'NONE',  ( -4.458734124999999437, -84.31249999863439371, 0.000000000000000000 ) ) ;
#43708 = EDGE_CURVE ( 'NONE', #39400, #52308, #28026, .T. ) ;
#43709 =( BOUNDED_CURVE ( )  B_SPLINE_CURVE ( 2, ( #5293, #59323, #22001, #55782, #51593, #17168, #36794, #7529, #27141 ),
 .UNSPECIFIED., .F., .F. ) 
 B_SPLINE_CURVE_WITH_KNOTS ( ( 3, 2, 2, 2, 3 ),
 ( 0.6562500000000000000, 0.6569444444444444420, 0.6583333333333333259, 0.6597222222222222099, 0.6604166666666666519 ),
 .UNSPECIFIED. ) 
 CURVE ( )  GEOMETRIC_REPRESENTATION_ITEM ( )  RATIONAL_B_SPLINE_CURVE ( ( 0.9330127018922194093, 0.9330127018922194093, 1.000000000000000000, 0.8660254037844387076, 1.000000000000000000, 0.8660254037844387076, 1.000000000000000000, 0.9330127018922194093, 0.9330127018922194093 ) ) 
 REPRESENTATION_ITEM ( '' )  );
#43710 = CARTESIAN_POINT ( 'NONE',  ( 4.458734125000000326, -167.6250000013655779, -1.846868145590734978 ) ) ;
#43711 = CARTESIAN_POINT ( 'NONE',  ( 5.000000000000000000, -17.29166666393548368, -2.886751345948129988 ) ) ;
#43713 = ORIENTED_EDGE ( 'NONE', *, *, #24049, .F. ) ;
#43712 = CARTESIAN_POINT ( 'NONE',  ( -3.152548672688508926E-16, -50.56249999863440792, -5.148502694627439702 ) ) ;
#43714 = CARTESIAN_POINT ( 'NONE',  ( 6.123233995736766282E-16, -170.0000000000000000, -5.000000000000000000 ) ) ;
#43716 = VERTEX_POINT ( 'NONE', #12606 ) ;
#43715 = CARTESIAN_POINT ( 'NONE',  ( -2.229367062500000163, 4.270833334698926897, -3.861377020970580443 ) ) ;
#43717 = CARTESIAN_POINT ( 'NONE',  ( -2.499999999999996447, -86.70833333060214443, 4.330127018922195425 ) ) ;
#43718 = CARTESIAN_POINT ( 'NONE',  ( 5.000000000000000000, -60.41666666666666430, -2.886751345948129988 ) ) ;
#43719 = EDGE_CURVE ( 'NONE', #42072, #61537, #18058, .T. ) ;
#43720 = CARTESIAN_POINT ( 'NONE',  ( -1.846868145590734756, -156.3750000013655779, -4.458734125000000326 ) ) ;
#43721 = CARTESIAN_POINT ( 'NONE',  ( 2.229367062499998831, -38.89583333196773651, -3.861377020970580887 ) ) ;
#43722 = CARTESIAN_POINT ( 'NONE',  ( -1.339745962155613812, -56.20534180126148271, -5.000000000000000000 ) ) ;
#43723 = CARTESIAN_POINT ( 'NONE',  ( -9.184850993605147944E-16, -162.2500000000000000, 5.000000000000000000 ) ) ;
#43724 = ADVANCED_FACE ( 'NONE', ( #32537 ), #57322, .T. ) ;
#43725 = CARTESIAN_POINT ( 'NONE',  ( -2.499999999999996447, -29.83333333333332860, 4.330127018922195425 ) ) ;
#43726 = CARTESIAN_POINT ( 'NONE',  ( -52.10840900171896806, -127.4375000013656063, 3.393966926194110556 ) ) ;
#43727 = CARTESIAN_POINT ( 'NONE',  ( -4.458734124999998549, -5.479166665301072214, 2.574251347313722516 ) ) ;
#43728 = CARTESIAN_POINT ( 'NONE',  ( -4.458734124999999437, -44.56249999863440081, 0.000000000000000000 ) ) ;
#43729 =( BOUNDED_CURVE ( )  B_SPLINE_CURVE ( 2, ( #27742, #8140, #47371, #3319, #13268, #46422, #2371, #4552, #63116 ),
 .UNSPECIFIED., .F., .F. ) 
 B_SPLINE_CURVE_WITH_KNOTS ( ( 3, 2, 2, 2, 3 ),
 ( 0.5196428571428571841, 0.5202380952380952772, 0.5214285714285714635, 0.5226190476190476497, 0.5232142857142857428 ),
 .UNSPECIFIED. ) 
 CURVE ( )  GEOMETRIC_REPRESENTATION_ITEM ( )  RATIONAL_B_SPLINE_CURVE ( ( 0.9330127018922194093, 0.9330127018922194093, 1.000000000000000000, 0.8660254037844387076, 1.000000000000000000, 0.8660254037844387076, 1.000000000000000000, 0.9330127018922194093, 0.9330127018922194093 ) ) 
 REPRESENTATION_ITEM ( '' )  );
#43730 = ADVANCED_FACE ( 'NONE', ( #2975 ), #17753, .T. ) ;
#43731 = CARTESIAN_POINT ( 'NONE',  ( 1.975475456537005874E-15, -67.62499999726881583, 5.000000000000000000 ) ) ;
#43732 = CARTESIAN_POINT ( 'NONE',  ( 4.458734125000000326, -150.3750000013655779, -1.846868145590734978 ) ) ;
#43733 = CARTESIAN_POINT ( 'NONE',  ( 9.457646018065525792E-16, -88.31249999863439371, 5.148502694627439702 ) ) ;
#43734 = FACE_OUTER_BOUND ( 'NONE', #21457, .T. ) ;
#43735 = ORIENTED_EDGE ( 'NONE', *, *, #38543, .F. ) ;
#43736 = CARTESIAN_POINT ( 'NONE',  ( -51.75738570946856498, -155.0000000000000284, 3.805975901505577408 ) ) ;
#43737 = CARTESIAN_POINT ( 'NONE',  ( -2.229367062500000163, 29.27083333469892779, -3.861377020970580443 ) ) ;
#43738 = CARTESIAN_POINT ( 'NONE',  ( -56.66612745406270335, -150.4375000027312126, -5.149110718188516067 ) ) ;
#43739 = CARTESIAN_POINT ( 'NONE',  ( 2.499999999999998668, -43.33333333333333570, -4.330127018922193649 ) ) ;
#43740 = EDGE_LOOP ( 'NONE', ( #34368, #22805, #26507, #34859 ) ) ;
#43741 = DIRECTION ( 'NONE',  ( 0.000000000000000000, 0.000000000000000000, 1.000000000000000000 ) ) ;
#43742 = CARTESIAN_POINT ( 'NONE',  ( -3.152548672688508926E-16, -10.81249999863440792, -5.148502694627439702 ) ) ;
#43743 = FACE_OUTER_BOUND ( 'NONE', #4727, .T. ) ;
#43744 = CARTESIAN_POINT ( 'NONE',  ( -2.229367062499996610, -3.145833331967738733, 3.861377020970582219 ) ) ;
#43745 = CARTESIAN_POINT ( 'NONE',  ( 2.500000000000002220, -55.54166666393548013, 4.330127018922192761 ) ) ;
#43746 = CARTESIAN_POINT ( 'NONE',  ( 1.846868145590735200, -152.2500000013656063, -4.458734124999999437 ) ) ;
#43747 = CARTESIAN_POINT ( 'NONE',  ( 2.229367062500001939, 20.77083333469892779, 3.861377020970579999 ) ) ;
#43748 = VERTEX_POINT ( 'NONE', #14801 ) ;
#43749 = CARTESIAN_POINT ( 'NONE',  ( -4.458734124999999437, -94.31249999863440792, 0.000000000000000000 ) ) ;
#43750 = CARTESIAN_POINT ( 'NONE',  ( -2.071067811865306307, -148.6875000000000000, -5.000000000000171418 ) ) ;
#43751 = CARTESIAN_POINT ( 'NONE',  ( -7.640563834021360018E-16, -9.147862274876560562, -8.047472243342937759 ) ) ;
#43752 = CARTESIAN_POINT ( 'NONE',  ( -4.458734124999999437, -11.39583333196774007, -2.574251347313719407 ) ) ;
#43753 = DIRECTION ( 'NONE',  ( -0.000000000000000000, 1.000000000000000000, -0.000000000000000000 ) ) ;
#43754 = DIRECTION ( 'NONE',  ( 0.000000000000000000, 0.000000000000000000, 1.000000000000000000 ) ) ;
#43755 = CARTESIAN_POINT ( 'NONE',  ( -1.339745962155613812, -88.20534180126146850, -5.000000000000000000 ) ) ;
#43756 = CARTESIAN_POINT ( 'NONE',  ( -2.500000000000000444, -42.04166666393548013, -4.330127018922193649 ) ) ;
#43757 = CARTESIAN_POINT ( 'NONE',  ( 1.975475456537005874E-15, -29.74999999999999645, 5.000000000000000000 ) ) ;
#43758 = CARTESIAN_POINT ( 'NONE',  ( 4.458734124999998549, 20.27083333469892779, -2.574251347313721627 ) ) ;
#43759 = CARTESIAN_POINT ( 'NONE',  ( 4.999999999999999112, -5.773502691896267081, -7.063244554130005071 ) ) ;
#43760 = ORIENTED_EDGE ( 'NONE', *, *, #4629, .T. ) ;
#43761 = CARTESIAN_POINT ( 'NONE',  ( -2.229367062500000163, 19.52083333469893134, -3.861377020970580443 ) ) ;
#43762 = CARTESIAN_POINT ( 'NONE',  ( -4.458734124999998549, -62.22916666530106511, 2.574251347313722516 ) ) ;
#43763 = CARTESIAN_POINT ( 'NONE',  ( 4.458734124999999437, -10.06249999863440614, -5.460374474430324690E-16 ) ) ;
#43764 = CARTESIAN_POINT ( 'NONE',  ( -2.499999999999996447, -30.83333333333333215, 4.330127018922195425 ) ) ;
#43765 = CARTESIAN_POINT ( 'NONE',  ( -5.000000000000000000, 8.916666666666666075, -2.886751345948128211 ) ) ;
#43766 = CARTESIAN_POINT ( 'NONE',  ( -4.458734124999999437, -165.9375000013655779, -5.460374474430324690E-16 ) ) ;
#43767 = CARTESIAN_POINT ( 'NONE',  ( -2.500000000000000444, -60.04166666393547303, -4.330127018922193649 ) ) ;
#43768 = CARTESIAN_POINT ( 'NONE',  ( 4.458734125000001214, -51.89583333196773651, 2.574251347313718519 ) ) ;
#43769 = CARTESIAN_POINT ( 'NONE',  ( -5.000000000000000000, -87.87499999726880162, 0.000000000000000000 ) ) ;
#43770 = CARTESIAN_POINT ( 'NONE',  ( -59.59170313451811296, -132.7500000013656063, 1.485763867205729394 ) ) ;
#43771 = CARTESIAN_POINT ( 'NONE',  ( 5.000000000000000000, -14.29166666393548013, -2.886751345948130876 ) ) ;
#43772 = CARTESIAN_POINT ( 'NONE',  ( -49.85088928181150436, -145.5625000000000568, -1.666127454062680480 ) ) ;
#43773 = CARTESIAN_POINT ( 'NONE',  ( 4.458734124999998549, -90.97916666530106511, -2.574251347313721627 ) ) ;
#43774 = CARTESIAN_POINT ( 'NONE',  ( -4.458734125000000326, -155.1250000013656063, 1.846868145590734089 ) ) ;
#43775 = CARTESIAN_POINT ( 'NONE',  ( -2.499999999999996447, -36.83333333333332860, 4.330127018922195425 ) ) ;
#43776 = CARTESIAN_POINT ( 'NONE',  ( 0.000000000000000000, -170.0000000000000000, 0.000000000000000000 ) ) ;
#43777 = CARTESIAN_POINT ( 'NONE',  ( -6.972266317189433020E-16, -96.12499999726880162, -5.000000000000000000 ) ) ;
#43778 = ORIENTED_EDGE ( 'NONE', *, *, #42120, .T. ) ;
#43779 = CARTESIAN_POINT ( 'NONE',  ( 9.457646018065525792E-16, -104.0624999986344221, 5.148502694627439702 ) ) ;
#43780 = CARTESIAN_POINT ( 'NONE',  ( -2.229367062499996610, 9.604166668032261711, 3.861377020970582219 ) ) ;
#43781 =( BOUNDED_CURVE ( )  B_SPLINE_CURVE ( 2, ( #40776, #31437, #55594, #51398, #22446, #22126, #26626, #2207, #27566 ),
 .UNSPECIFIED., .F., .F. ) 
 B_SPLINE_CURVE_WITH_KNOTS ( ( 3, 2, 2, 2, 3 ),
 ( 0.3729166666666666741, 0.3736111111111111160, 0.3750000000000000000, 0.3763888888888888840, 0.3770833333333333259 ),
 .UNSPECIFIED. ) 
 CURVE ( )  GEOMETRIC_REPRESENTATION_ITEM ( )  RATIONAL_B_SPLINE_CURVE ( ( 0.9330127018922194093, 0.9330127018922194093, 1.000000000000000000, 0.8660254037844387076, 1.000000000000000000, 0.8660254037844387076, 1.000000000000000000, 0.9330127018922194093, 0.9330127018922194093 ) ) 
 REPRESENTATION_ITEM ( '' )  );
#43782 = DIRECTION ( 'NONE',  ( 0.000000000000000000, 1.000000000000000000, 0.000000000000000000 ) ) ;
#43783 = CARTESIAN_POINT ( 'NONE',  ( -2.500000000000000444, 0.8333333333333317050, -4.330127018922193649 ) ) ;
#43784 = VECTOR ( 'NONE', #31202, 1000.000000000000000 ) ;
#43785 = CARTESIAN_POINT ( 'NONE',  ( 4.458734124999998549, -62.72916666530106511, -2.574251347313721627 ) ) ;
#43786 = CARTESIAN_POINT ( 'NONE',  ( -5.000000000000000000, -30.95833333060214443, -2.886751345948128211 ) ) ;
#43787 = CARTESIAN_POINT ( 'NONE',  ( 2.499999999999998668, -2.208333330602146205, -4.330127018922193649 ) ) ;
#43789 = VERTEX_POINT ( 'NONE', #4525 ) ;
#43788 = CARTESIAN_POINT ( 'NONE',  ( 2.229367062499998831, -26.64583333196774007, -3.861377020970580887 ) ) ;
#43790 = CARTESIAN_POINT ( 'NONE',  ( 2.500000000000002220, 17.45833333606451987, 4.330127018922192761 ) ) ;
#43791 = CARTESIAN_POINT ( 'NONE',  ( 5.000000000000000000, -157.0625000000000284, 2.071067811865478614 ) ) ;
#43792 = CARTESIAN_POINT ( 'NONE',  ( -1.339745962155618253, 25.20534180126147916, 4.999999999999996447 ) ) ;
#43793 = CARTESIAN_POINT ( 'NONE',  ( -2.500000000000000444, -45.16666666666665719, -4.330127018922193649 ) ) ;
#43795 = CARTESIAN_POINT ( 'NONE',  ( 4.458734124999998549, -24.97916666530106511, -2.574251347313721627 ) ) ;
#43794 = CARTESIAN_POINT ( 'NONE',  ( -2.499999999999996447, 24.29166666939785202, 4.330127018922195425 ) ) ;
#43796 = CARTESIAN_POINT ( 'NONE',  ( 5.000000000000000888, -4.458333330602147981, 2.886751345948126879 ) ) ;
#43797 = CARTESIAN_POINT ( 'NONE',  ( -2.229367062499996610, -71.14583333196773651, 3.861377020970582219 ) ) ;
#43798 = CARTESIAN_POINT ( 'NONE',  ( -1.846868145590734756, -144.3750000013656063, -4.458734125000000326 ) ) ;
#43799 = CARTESIAN_POINT ( 'NONE',  ( 9.457646018065525792E-16, -79.06249999863440792, 5.148502694627439702 ) ) ;
#43800 = CARTESIAN_POINT ( 'NONE',  ( -51.60603307380591787, -139.1875000013656347, -2.891590998281053704 ) ) ;
#43801 = CARTESIAN_POINT ( 'NONE',  ( -4.458734124999998549, -28.47916666530107221, 2.574251347313722516 ) ) ;
#43802 = CARTESIAN_POINT ( 'NONE',  ( -3.535250795749689387E-16, -67.12499999726881583, -5.773502691896257311 ) ) ;
#43803 = EDGE_CURVE ( 'NONE', #52130, #10973, #24150, .T. ) ;
#43804 = EDGE_LOOP ( 'NONE', ( #11837, #14377, #18375, #11356 ) ) ;
#43805 = CARTESIAN_POINT ( 'NONE',  ( -9.184850993605147944E-16, -152.3750000027311842, 5.000000000000000000 ) ) ;
#43806 = VERTEX_POINT ( 'NONE', #57943 ) ;
#43807 = CARTESIAN_POINT ( 'NONE',  ( 4.458734124999999437, -75.06249999863440792, -5.460374474430324690E-16 ) ) ;
#43808 =( NAMED_UNIT ( * ) PLANE_ANGLE_UNIT ( ) SI_UNIT ( $, .RADIAN. ) );
#43809 = ORIENTED_EDGE ( 'NONE', *, *, #33015, .F. ) ;
#43810 = CARTESIAN_POINT ( 'NONE',  ( 5.000000000000000000, 27.58333333333333215, -2.886751345948130876 ) ) ;
#43811 =( BOUNDED_SURFACE ( )  B_SPLINE_SURFACE ( 1, 2, ( 
 ( #12754, #36255, #41066, #40748, #31743, #6670, #32053, #6995, #21467, #51689, #2802, #50416, #46221, #2486, #26277, #16953, #16634, #55883, #51375, #25965, #45900, #11794, #26605, #22422, #42020, #45582, #61028, #2184, #17595, #60396, #16321, #21788, #22099, #31412, #37211, #35942, #31105, #1861, #36566, #61661, #56197, #12118, #7316, #26927, #46544, #23048, #28489, #8561, #32376, #23368, #48107, #52323, #27545, #19141, #18829, #13698, #27860, #37517, #52938, #42966, #23678, #62609, #58075, #8875, #57777, #47176, #38153, #3746, #38448, #13389, #9189, #53253, #32691, #18532, #33634, #28173, #8257, #47478, #4060, #43277, #62916, #33319, #14007, #28802, #3433, #42652, #48418, #47788, #4361, #57158, #23980, #62293, #3119, #13072, #33011, #37838, #43584, #18215, #63226, #38758, #57470, #52628, #58396, #7941, #52000, #22739, #42337, #61975, #17895, #35223, #40355, #14324, #39708, #39391, #498, #25247, #30062, #49372, #30384, #54843, #43894, #5317, #24934, #20102, #50007, #25569, #53877, #5636, #44862, #5958, #10448, #45184, #39079, #59023, #34565, #53567, #44542, #59348, #33945, #15280, #34903, #825, #10134, #1150, #63543, #20431, #49045, #40031, #54525, #48727, #49690, #20750, #24292, #9491, #184, #4991, #4668, #59674, #34248, #15605, #54195, #24613, #10774, #29102, #19464, #29740, #58708, #14634, #9803, #44219, #19784, #29412, #14954, #55490, #6590, #1788, #6281, #56118, #55168, #12042, #7550, #30709, #36816, #40673, #50974, #26853, #7239, #46465, #26205, #16873, #17190, #45824, #35865, #56447, #36491, #6916, #60638, #50334, #50652, #51617, #22023, #11405, #1466, #12368, #31337, #51304, #40994, #11087, #2408, #21068, #59996, #21388, #25887, #31667, #55803, #41616, #61267, #46778, #31983, #27162, #2724, #60318, #45503, #22346, #2111, #16245, #15919, #35541, #31025, #16558, #36182, #11720, #26528, #46147, #21712, #41304, #60954, #3984, #7865, #22977, #42889, #38077, #18134, #58008, #8801, #42263, #62842, #28414, #32936, #33248, #48345, #48033, #42578, #23603, #3360, #32615, #43201, #37760, #52868, #56761, #18757, #3047, #12683, #38382, #61904, #62533, #52241, #13934, #33559, #8492, #57078, #53181, #52559, #32297, #37447, #22665, #4291, #18455, #9114, #57393, #28722, #51924, #41943, #17823, #27470, #61586, #12992, #57704, #8182, #17520, #37140, #28100, #27785, #47098, #47718, #47410, #62217, #13314, #3674, #13630, #23287, #59601, #33872, #30308, #9734, #14558, #58323, #5240, #43826, #49621, #44142, #58639, #10379, #20355, #23909, #19708, #39632, #24219, #54118, #53800, #29338, #24863, #43510, #19390, #34177, #48968, #53490, #20027, #19066, #59271, #35154, #14249, #744, #4596, #14875, #54451, #34828, #29988, #4920, #44464, #44783, #24539, #63471, #39953, #423, #34484, #114, #9419, #39317, #15534, #5557, #39008, #29030, #54769, #58945, #15203, #10056, #38684, #25169, #48654, #63156, #29668, #49300, #10700, #49928, #2029, #41226, #56371, #41542, #46391, #2338, #6202, #1076, #7162, #11643, #25817, #60873, #45111, #12293, #20682, #11328, #45753, #40915, #16162, #31263, #56047, #11963, #31591, #35469, #50578, #6841, #21634, #1707, #21944, #36417, #45430, #26770, #51225, #60560, #16799, #31910, #61194, #6521, #17116, #30952, #60245, #16482, #36103, #55728, #20995, #35789, #36740, #21312, #5882, #11010, #25489, #55411, #40288, #30632, #26133, #50898, #59926, #40600, #26449, #46070, #15848, #55087, #50254, #1395, #52164, #32860, #3599, #12914, #37061, #8727, #13860, #51538, #13237, #32536, #37678, #62459, #23204, #22905, #3908, #28339, #17443, #42501, #62137, #57320, #23527, #62768, #27392, #42817, #18379, #43128, #47644, #18688, #12604, #8108, #27712, #27085, #18057, #52489, #7474, #8422, #28025, #38000, #47339, #38314, #56688, #57632, #22591, #13561, #33179, #22267, #3289, #52794, #57942, #46700, #47955, #2648, #41867, #61514, #32217, #51846, #7789, #61828, #47025, #2974, #42188, #17752, #37368, #57000, #43752, #33484, #44387, #54042, #4224, #24149, #29592, #9660, #53105, #24462, #49223, #53415, #28651, #20278, #19948, #14800, #28960, #38610, #9980, #44067, #24782, #33, #59201, #5163, #58869, #48266, #39243, #4842, #39559, #14483, #10302, #54377, #33797, #19632, #34750, #29268, #9345, #48583, #347, #15129, #29913, #63396, #25096, #49540, #4524, #58243, #5481, #34413, #44704, #34104, #23838, #669, #14171, #9040, #58563, #43441, #39879, #48898, #59524, #63085, #18995, #19314, #38929, #53729, #15772, #10616, #16728, #21234, #35389, #50824, #54694, #2272, #30228, #20920, #55340, #50508, #25743, #40840, #1958, #21559, #41155, #45035, #60167, #16411, #11575, #11256, #31505, #45992, #55008, #36344, #60801, #6451, #6761, #21876, #55975, #16088, #11887, #40523, #6129, #51150, #30881, #26374, #49852, #7084, #40211, #5799, #26698, #10934, #36029, #45357, #46315, #41471, #45675, #30551, #15458, #26060, #25417, #50177, #59847, #35075, #55661, #31195, #1003, #20607, #1323, #35712, #1633, #60484, #42423, #17363, #23132, #17681, #32142, #47571, #57561, #61122, #56925, #13163, #61437, #27639, #27324, #2901, #62066, #17046, #56613, #7721, #22514, #7404, #57247, #56290, #32786, #8651, #31835, #37928, #41793, #52095, #27948, #8350, #3522, #46954, #17979, #18304, #42109, #36985, #13486, #37604, #8034, #61754, #51466, #12530, #22192, #23455, #52417, #42738, #33103, #27011, #3837, #37296, #51776, #46631, #62382, #12844, #52717, #32463, #47268, #28264, #47877, #36663, #3213, #12218, #22833, #2576, #9276, #48513, #24390, #62698, #38538, #53342, #4452, #53027, #39172, #38246, #58797, #54293, #13788, #19876, #23770, #34037, #9903, #53975, #29513, #28892, #63639, #278, #24081, #18923, #39490, #19560, #53658, #43676, #33411, #33724, #34674, #5089, #58167, #48198, #59126, #14414, #34347, #63318, #57867, #49144, #4152, #43060, #19238, #8967, #14728, #38854, #24710, #44314, #29837, #15059, #10232, #49470, #43370, #28578, #5409, #48825, #63016, #18623, #14098, #58490, #9592, #29200, #4763, #43992, #35317, #30805, #12377, #31990, #51624, #54618, #6060, #25983, #21159, #1246, #41950, #56455, #25343, #46786, #7558, #16012, #17197, #32304, #27170, #25670, #2733, #50103, #15697, #22353, #20846, #36824, #39807, #61595, #49783, #59449, #17529, #44966, #45598, #54937, #37147, #56771, #55265, #40130, #12691, #35637, #15379, #35003, #50436, #60090, #51933, #45280, #25025, #44636, #928, #11183, #596, #40449, #20532, #59771, #40765, #60412, #20203, #6377, #1557, #10543, #10863, #30479, #30154, #5729, #43211, #13004, #53190, #18144, #3055, #32624, #52568, #13324, #3991, #22986, #23298, #62546, #37772, #57403, #57713, #47106, #8501, #52877, #23615, #32944, #57085, #28731, #33880, #7874, #33258, #28111, #13638, #18765, #62852, #42898, #23918, #48357, #37454, #18466, #38087, #8812, #43519, #19075, #47418, #38391, #58016, #63164, #13944, #38695, #52251, #47727, #3684, #22673, #28427, #48041, #27478, #33571, #9123, #4301, #58332, #14258, #8191, #42272, #42588, #61912, #17832, #27793, #3370, #62226, #45119, #59935, #44473, #29678, #20692, #43833, #9430, #54127, #5566, #123, #40297, #63479, #29040, #53810, #10065, #10710, #19717, #53500, #758, #10388, #24227, #44152, #49630, #49308, #48663, #432, #25180, #9741, #4604, #15857, #39964, #34837, #48980, #58646, #29998, #20038, #44794, #39642, #15543, #20366, #15212, #19398, #59611, #14566, #39017, #14885, #34188, #35163, #5249, #54779, #30317, #29346, #25500, #49938, #5893, #4929, #24547, #1084, #59281, #39326, #58958, #34492, #24872, #54462, #40923, #11651, #6847, #45760, #41234, #21954, #41550, #61201, #1403, #16491, #36426, #31600, #31271, #51545, #2346, #35798, #56379, #17123, #26461, #26779, #41876, #36749, #36112, #12303, #60566, #26141, #31918, #50905, #46397, #50264, #7481, #60254, #6212, #27094, #55421, #56054, #1714, #46711, #2656, #2036, #50587, #22275, #46078, #25825, #30962, #16173, #61523, #11970, #51234, #35479, #45440, #55095, #21322, #55735, #21004, #16806, #11339, #11021, #21641, #6527, #30642, #40610, #60881, #7170, #33188, #17760, #47654, #47348, #22918, #62470, #37075, #12925, #27721, #42510, #27402, #13570, #12613, #52803, #28660, #51857, #57951, #61840, #8432, #47964, #28347, #3919, #3297, #38009, #38322, #62148, #57010, #13872, #57642, #28036, #18066, #7800, #8117, #9050, #43137, #32547, #22600, #33497, #52498, #8740, #37688, #53114, #48276, #4232, #37377, #32226, #18697, #23215, #52173, #23538, #56697, #23847, #47033, #57330, #13246, #3607, #32869, #42825, #62777, #43450, #17453, #2983, #18390, #42197, #59210, #39253, #15468, #29925, #63407, #20288, #49550, #54053, #54387, #5810, #5492, #43, #25106, #24473, #53737, #679, #58879, #10312, #14181, #44716, #24159, #33808, #39889, #19325, #19959, #9670, #35086, #59535, #29603, #14494, #54706, #9990, #53424, #58575, #43762, #25427, #39570, #15139, #10626, #9358, #63095, #48908, #29278, #28970, #44398, #38939, #30239, #19643, #34116, #49862, #19007, #38620, #14810, #34761, #4853, #49233, #44080, #34424, #357, #58257, #5175, #24792, #48593, #4534, #41165, #40223, #60812, #56303, #15783, #21886, #25753, #36040, #11899, #55985, #31519, #11266, #1968, #2282, #30890, #20931, #41482, #21569, #55671, #45688, #35399, #35722, #36673, #7095, #40536, #50187, #61133, #16422, #36355, #26070, #59858, #51162, #6139, #45046, #6461, #55021, #16738, #40851, #26709, #46324, #31845, #17056, #50835, #45367, #12231, #20616, #51477, #10943, #50521, #21244, #11586, #55352, #6775, #7414, #1013, #30562, #1334, #1645, #46003, #60177, #60494, #16099, #31205, #26386, #18315, #47583, #47277, #8359, #28276, #3534, #12856, #23143, #37306, #22526, #62394, #52104, #27960, #22206, #42751, #12539, #41805, #37940, #7730, #37616, #42122, #13498, #57572, #22844, #46966, #33114, #3226, #61449, #27335, #32152, #47890, #13174, #32798, #52731, #17378, #27024, #17691, #61764, #36999, #57257, #2911, #8663, #32475, #56935, #46642, #2587, #56625, #52427, #51788, #8045, #27650, #42434, #62076, #17990, #40418, #16308, #31091, #26264, #30777, #16939, #15982, #36553, #32040, #55233, #61331, #1526, #11781, #51361, #6657, #50713, #7302, #55868, #36877, #17255, #50398, #31399, #51037, #26591, #56507, #51677, #60382, #12104, #31731, #12429, #56184, #7617, #45569, #1848, #41054, #60058, #6980, #46208, #20818, #2170, #21776, #26914, #16620, #27222, #6347, #46531, #55557, #2472, #41368, #11155, #60700, #61014, #35607, #22085, #41683, #46842, #36241, #25953, #21130, #40735, #11471, #35929, #45886, #21454, #42638, #13687, #58064, #9178, #57456, #62281, #33624, #56823, #22408, #3420, #18519, #13059, #53242, #12742, #42007, #3108, #23036, #23666, #32678, #2788, #33306, #23355, #37198, #57144, #62597, #18202, #61647, #13376, #38139, #22725, #17581, #28790, #52926, #47777, #61963, #7929, #42954, #32998, #57765, #52614, #28478, #8863, #28162, #32362, #8549, #37823, #48093, #47466, #43263, #62902, #42323, #3734, #4048, #18817, #17884, #37505, #38437, #13996, #51986, #27531, #47164, #52309, #8245, #27845, #41081, #54617, #40129, #1878, #11810, #15378, #11182, #31120, #15696, #45597, #45279, #20845, #60411, #35002, #10862, #25669, #40448, #25342, #11504, #10542, #50742, #26618, #49782, #55897, #59770, #6376, #45916, #1245, #6686, #35959, #60727, #36273, #60089, #54936, #31427, #55584, #25982, #16011, #5728, #6059, #7009, #16649, #30478, #20531, #51065, #50435, #26292, #35636, #30153, #21483, #55264, #21158, #46235, #2198, #21802, #44965, #30804, #16337, #41397, #1556, #927, #35316, #50102, #40764, #27872, #52014, #52335, #3758, #47492, #61674, #3445, #22437, #51703, #62304, #56849, #8269, #12134, #23060, #22116, #31756, #37853, #17280, #17908, #7643, #33024, #57485, #27557, #12455, #42665, #7956, #51389, #56534, #41709, #23381, #37529, #13086, #52640, #7331, #61047, #46873, #27247, #26942, #42350, #2816, #18226, #36580, #61358, #13403, #8574, #16969, #12766, #32706, #36904, #47190, #42032, #17607, #61988, #56212, #32066, #37223, #32389, #46558, #57170, #2499, #28185, #47801, #3132, #22752, #23692, #33958, #9814, #53266, #58719, #63557, #5005, #196, #9201, #18842, #39402, #19475, #53579, #43596, #33332, #33647, #34576, #24625, #38460, #48120, #59038, #14337, #34262, #23992, #57790, #49057, #4072, #42980, #4375, #13709, #14645, #38771, #39089, #53890, #29752, #14968, #19794, #54208, #43291, #38167, #44231, #48737, #62927, #29425, #18545, #49385, #52951, #48433, #19153, #9507, #10145, #29116, #5330, #62623, #8888, #63239, #28501, #58409, #28813, #58088, #4681, #14019, #24303, #43908, #49702, #39721, #1799, #44878, #45516, #15618, #60648, #21402, #55179, #40043, #55505, #15932, #59358, #20444, #5646, #50989, #1477, #40685, #16571, #34915, #31346, #10787, #35235, #15293, #6294, #54854, #50663, #509, #25259, #11419, #41006, #24947, #20762, #60330, #841, #11100, #30397, #50020, #25899, #44553, #59685, #5974, #25583, #54537, #21080, #20119, #16257, #36193, #10458, #55814, #45196, #35555, #31038, #1163, #35876, #6603, #26217, #45837, #40368, #60009, #11730, #30072, #30724, #50347, #60966, #61280, #62229, #32628, #2423, #12054, #22991, #41955, #61916, #51628, #21723, #13008, #31678, #6928, #31994, #41318, #42276, #2737, #3059, #17836, #57407, #42592, #47422, #3374, #7252, #2122, #8195, #12695, #26864, #37459, #46160, #13327, #16886, #12381, #46791, #61598, #17201, #32308, #57089, #52256, #27797, #36502, #7562, #7879, #22677, #22357 ),
 ( #36829, #18147, #56131, #51314, #37775, #32948, #26538, #17533, #46477, #22035, #37151, #56459, #27174, #51937, #41626, #56776, #27482, #47111, #62550, #48668, #47731, #4608, #127, #23301, #29350, #33262, #43524, #19405, #62855, #24231, #9434, #14570, #9745, #18768, #28431, #48984, #29043, #63168, #53194, #42901, #43215, #44157, #34192, #48044, #57716, #4933, #23923, #43837, #33573, #3687, #58649, #13641, #52571, #13947, #18470, #63483, #48360, #39021, #53815, #39330, #24553, #19721, #58963, #52880, #38090, #14890, #58336, #8815, #8504, #28114, #3996, #23618, #58019, #28734, #19079, #38395, #14264, #9127, #4304, #38699, #33884, #53504, #35483, #30647, #10714, #50591, #30966, #11025, #25504, #35168, #24876, #25184, #26145, #60259, #30002, #39647, #6531, #5898, #25828, #15547, #49312, #40614, #59285, #34497, #59615, #5254, #6216, #30321, #50269, #45444, #21326, #45764, #11343, #1719, #34843, #29683, #35802, #40301, #54466, #1408, #10069, #40926, #44477, #39970, #49943, #45123, #44799, #59939, #21008, #16177, #55426, #436, #54783, #55100, #60572, #1088, #54131, #20042, #10393, #15216, #49633, #20696, #5570, #762, #20370, #15861, #47037, #41554, #7174, #17763, #12308, #7803, #31275, #42200, #41238, #50909, #57013, #36430, #37078, #22279, #60885, #16809, #61525, #31604, #2986, #7485, #6851, #11975, #56059, #42514, #56700, #32229, #52176, #26465, #22921, #2350, #26782, #46082, #17456, #46401, #61843, #55739, #51238, #22603, #12928, #16494, #31922, #51860, #21958, #46714, #61205, #17129, #12617, #36116, #36753, #56383, #51550, #2041, #27405, #11655, #37380, #27724, #21646, #32551, #27098, #2659, #8121, #41879, #47351, #3300, #24162, #19328, #28350, #38013, #9361, #53741, #4857, #53118, #38325, #29281, #52501, #18069, #62781, #14184, #8742, #48911, #8435, #37691, #62473, #18700, #38942, #47967, #62151, #28974, #19010, #32872, #52806, #58261, #57954, #57333, #9053, #33811, #18393, #13249, #24477, #48596, #43453, #57645, #3611, #38623, #28663, #53428, #48279, #43765, #4536, #23850, #3922, #63411, #28039, #58578, #43140, #14497, #34118, #13573, #4235, #9673, #13875, #33191, #23541, #47657, #23218, #42829, #33501, #63098, #10629, #59213, #47, #19646, #19964, #34428, #49237, #25757, #54390, #39257, #5179, #25109, #49553, #40227, #15143, #59538, #35090, #10317, #29928, #30242, #58883, #44720, #25431, #59862, #5495, #29607, #1336, #6464, #44082, #5813, #54056, #682, #20291, #30566, #15473, #60179, #20934, #9994, #54709, #49865, #45049, #16101, #55354, #39574, #35402, #55024, #35725, #15786, #11268, #24797, #39892, #1016, #14814, #20620, #10947, #44402, #50190, #6142, #45370, #40538, #30893, #361, #50523, #34764, #37001, #31847, #60496, #2285, #52106, #2589, #41807, #61766, #36043, #32477, #11902, #16740, #16424, #7417, #36357, #51790, #1647, #50837, #12541, #22528, #26072, #21888, #61452, #26388, #56307, #55987, #31522, #27026, #45690, #21571, #51164, #7097, #55673, #22209, #21246, #17382, #37308, #11588, #2915, #6778, #17058, #56628, #26712, #32154, #46644, #7732, #46968, #46326, #1971, #42124, #27337, #36675, #41484, #31208, #61136, #17694, #56937, #41168, #46006, #12858, #12233, #40853, #51479, #60815, #14984, #13178, #8048, #33116, #22846, #44247, #4696, #5021, #211, #59375, #44568, #49401, #5345, #8361, #3228, #10162, #14660, #27962, #19809, #47279, #15309, #42436, #13500, #48754, #43925, #18317, #34279, #59056, #34593, #54224, #37618, #52733, #9830, #24640, #24318, #24963, #39418, #47585, #29767, #526, #63572, #20135, #34931, #39735, #9524, #27652, #29131, #62396, #62079, #19491, #17992, #57259, #32800, #52429, #3536, #23145, #42753, #29441, #53904, #37942, #57575, #49073, #39106, #58734, #45531, #25276, #50037, #15634, #25913, #45851, #35570, #5663, #60663, #59702, #54552, #15948, #44897, #26231, #50361, #50676, #1813, #41333, #26554, #31362, #51003, #54870, #49718, #55829, #60344, #10801, #21417, #30088, #60980, #857, #60025, #30740, #1492, #1179, #16272, #41020, #16587, #36207, #20460, #55194, #55521, #6618, #6309, #6943, #11744, #30413, #46174, #2135, #21095, #21738, #16901, #10475, #11114, #40059, #40699, #45213, #35250, #35891, #5995, #25600, #20779, #40384, #11435, #31053, #56473, #57107, #42290, #61294, #17216, #17850, #51643, #3389, #27497, #7266, #32009, #36843, #62565, #13024, #52272, #8518, #46492, #42918, #22371, #27189, #26878, #37472, #46805, #62245, #12068, #12394, #23006, #32962, #36517, #32324, #8209, #7577, #3074, #2752, #41971, #32641, #56147, #61613, #17547, #37167, #2440, #27812, #31693, #47437, #47746, #22049, #13342, #56790, #47126, #42607, #12708, #18164, #37791, #57421, #52586, #51954, #7892, #28128, #3702, #22691, #61931, #41642, #23317, #51328, #44172, #13960, #23633, #34513, #58030, #8831, #43228, #139, #28749, #13656, #62869, #63181, #23936, #14584, #33587, #33896, #9447, #48374, #4316, #4620, #57730, #19092, #63495, #34204, #43537, #4012, #39347, #44490, #18484, #43849, #28444, #38710, #58349, #4944, #53519, #54144, #58977, #48059, #29056, #48680, #24245, #10083, #29694, #53206, #9757, #29364, #49325, #53828, #5268, #18781, #14277, #19420, #33276, #39034, #58661, #38106, #48997, #24567, #19733, #14904, #24889, #38408, #52895, #9140, #11354, #6229, #34857, #40314, #30977, #55750, #6863, #55113, #59952, #31286, #54478, #20056, #1100, #16188, #10726, #50921, #10405, #39660, #775, #20709, #21337, #30333, #452, #50601, #21020, #30017, #54798, #60270, #15875, #59297, #11038, #35815, #20382, #15229, #26478, #6542, #45456, #59627, #5582, #40627, #30661, #55439, #50282, #26156, #45775, #25839, #5911, #1734, #49645, #40937, #45136, #60587, #16507, #39982, #1421, #36128, #35495, #15560, #35180, #11667, #25199, #44813, #49959, #25518, #12627, #61216, #2052, #21660, #42209, #18082, #7186, #27111, #2669, #41251, #32243, #51873, #46092, #17468, #47047, #32564, #41890, #57343, #31615, #52186, #17141, #57026, #7814, #16821, #22291, #12941, #37705, #52511, #37090, #61536, #13259, #36440, #60898, #46724, #61855, #56394, #32883, #56070, #11989, #46414, #56708, #3310, #12321, #51251, #8131, #2997, #26794, #36765, #17772, #27416, #2363, #22614, #37391, #21972, #41565, #8446, #27734, #47363, #31932, #51560, #22931, #42525, #62162, #7499, #53750, #4546, #53440, #33513, #48607, #38024, #29291, #9063, #4869, #48920, #28359, #14195, #24488, #4245, #47980, #3934, #43775, #63421, #38951, #63109, #58276, #33821, #43151, #47669, #3621, #23553, #18403, #33201, #9683, #38336, #23228, #52816, #28673, #53131, #24171, #62791, #43463, #19020, #57964, #13885, #9373, #42843, #48293, #28984, #19339, #23860, #13582, #44094, #54067, #28049, #58589, #57656, #38633, #14507, #34129, #58, #19655, #39267, #8754, #58895, #14824, #34438, #62485, #18710, #49565, #1346, #20948, #1657, #19977, #11278, #54721, #50531, #30904, #10328, #59875, #6474, #49877, #29939, #5503, #25769, #45381, #40550, #45061, #40238, #15797, #25119, #29618, #49248, #44731, #372, #15154, #55364, #20304, #5191, #34775, #10641, #15484, #6153, #691, #25441, #1027, #39904, #59549, #35414, #24808, #30254, #55035, #60191, #35103, #59222, #26082, #36054, #10006, #10959, #39585, #5826, #20632, #16111, #30581, #45702, #21256, #54399, #50203, #35737, #40863, #60507, #16434, #44411, #46976, #2924, #47289, #51799, #27661, #16749, #36687, #12243, #31217, #22218, #61462, #55682, #27036, #56638, #42135, #51489, #3239, #41179, #61776, #26721, #22539, #17394, #26397, #31856, #17703, #22855, #62088, #46653, #7427, #42446, #46017, #11596, #56320, #7741, #2294, #18005, #1979, #50847, #55997, #2598, #12868, #21896, #6788, #37317, #12552, #21581, #46337, #27345, #41815, #60824, #37009, #56947, #11912, #36366, #31534, #32486, #32165, #51174, #7107, #52115, #8059, #41493, #61146, #17068, #14119, #63035, #43080, #58190, #28600, #4474, #47900, #53362, #33745, #63345, #58510, #3856, #13512, #34057, #9296, #48218, #38265, #27974, #28288, #29219, #19259, #33128, #42764, #53679, #8988, #28912, #18643, #52439, #43697, #62406, #37628, #62718, #8373, #48535, #33432, #24101, #38876, #24413, #9612, #14434, #48845, #37952, #32810, #4786, #43390, #57585, #44014, #13187, #63662, #47595, #57887, #13813, #4173, #23477, #18943, #57269, #3547, #23155, #18328, #53051, #38561, #52745, #23788, #8674, #50125, #19895, #40473, #6082, #10564, #10887, #26008, #25692, #20227, #45302, #44656, #10256, #20871, #15403, #30503, #34365, #1269, #44332, #53995, #60113, #39510, #40154, #25367, #298, #59147, #953, #34692, #16034, #30174, #9922, #15079, #54317, #45626, #59798, #35338, #55288, #29534, #19579, #5428, #29857, #49171, #20553, #49490, #35663, #58818, #25045, #11208, #30831, #39193, #35028, #54957, #617, #49804, #39827, #59470, #15719, #14748, #54640, #5749, #44987, #5111, #50460, #24730, #6400, #12792, #35981, #42059, #45938, #60435, #2842, #7354, #1901, #36932, #40788, #52044, #16360, #7031, #41422, #36608, #11833, #26964, #51728, #7668, #27275, #31142, #46261, #2525, #61385, #61071, #17630, #32092, #21508, #22462, #46901, #56240, #56558, #7983, #61701, #2220, #37247, #26642, #55919, #56874, #16992, #12479, #55610, #32413, #26319, #11526, #27581, #41105, #22140, #46583, #60750, #16675, #41735, #36296, #1581, #12161, #50768, #31453, #51094, #21181, #17305, #6711, #21823, #31780, #51411, #33053, #37879, #17930, #28529, #57511, #9226, #22778, #8296, #33671, #43624, #47216, #43006, #62953, #47520, #13739, #13427, #52667, #48147, #3159, #42687, #8601, #28211, #57194, #43318, #42373, #18871, #58435, #37554, #24020, #27899, #38192, #14047, #47825, #38488, #4099, #28839, #4400, #3784, #23084, #63266, #23722, #57817, #23407, #13114, #62652, #38797, #48463, #62331, #52358, #19184, #18571, #58115, #33360, #62012, #53290, #3471, #32731, #52975, #18252, #14363, #8916, #33987, #53607, #9541, #1193, #6010, #25612, #29458, #44260, #44583, #20151, #39431, #59072, #15323, #4712, #29781, #10488, #44913, #54237, #14674, #50052, #55210, #29145, #54566, #19506, #14997, #34610, #15646, #540, #45226, #20793, #58746, #39748, #59390, #34947, #40395, #60036, #5035, #20472, #40074, #15961, #25288, #35583, #53917, #10178, #49413, #24337, #30101, #49732, #48767, #5677, #869, #35262, #24976, #43938, #34295, #54883, #224, #59717, #10813, #63585, #5357, #30425, #39119, #9843, #49089, #24654, #19822, #45545, #30754, #61549, #17784, #27123, #57354, #1505, #50374, #16284, #17480, #47375, #46737, #11127, #8146, #37403, #21106, #2683, #12953, #32255, #6321, #47060, #32577, #6633, #40711, #25926, #37719, #52199, #37102, #22303, #27746, #57039, #42537, #3324, #13273, #22943, #62173, #51885, #18095, #31066, #32897, #27428, #60360, #35902, #56721, #55537, #11447, #50690, #3010, #22626, #41902, #12638, #7826, #42223, #61868, #36028, #20029, #24540, #44144, #44466, #58949, #10057, #51149, #15204, #115, #29669, #49622, #10380, #1957, #55974, #11886, #31504, #34485, #5559, #6760, #21558, #44786, #21875, #36343, #5241, #26697, #7083, #59604, #60800, #12217, #46314, #25171, #2271, #29989, #59273, #41470, #747, #16727, #19709, #61121, #49301, #39318, #17045, #24864, #26373, #11574, #424, #39633, #50823, #34829, #36662, #15536, #14876, #54454, #20358, #31834, #45991, #41154, #56289, #54119, #4921, #39956, #55660, #31194, #32785, #61753, #13485, #27010, #12529, #37927, #47876, #51465, #47267, #3521, #51775, #17978, #17680, #56924, #52416, #7403, #46953, #37295, #12843, #61436, #47570, #46630, #23131, #62697, #22191, #28263, #32141, #42422, #18303, #32462, #42737, #8349, #33102, #8650, #52094, #27323, #3836, #27947, #62065, #8033, #41792, #42108, #43059, #52716, #2900, #56612, #23454, #22832, #62381, #27638, #2575, #57560, #7720, #17362, #3212, #36984, #18622, #37603, #38245, #57866, #13787, #22513, #57246, #13162, #33723, #28577, #34673, #39171, #53341, #5088, #8966, #20202, #48197, #38853, #9591, #4762, #43675, #58796, #5408, #44635, #9275, #24709, #44313, #25024, #29512, #595, #58166, #14413, #53657, #4151, #63638, #14727, #33410, #24389, #34346, #19875, #29199, #39806, #18922, #39489, #4451, #277, #53974, #23769, #48824, #59125, #59448, #53026, #43991, #19559, #43369, #63015, #38537, #34036, #49143, #63317, #14097, #28891, #48512, #24080, #9902, #54292, #19237, #58489, #15058, #10231, #29836, #49469, #16324, #60399, #26279, #45901, #50420, #20516, #6364, #44951, #10525, #21145, #15682, #11169, #34657, #45584, #44620, #54277, #35944, #39790, #40434, #25653, #580, #20189, #1233, #34988, #25968, #10848, #10216, #15365, #59436, #19860, #60073, #35622, #55573, #29820, #39473, #5714, #30139, #49452, #20832, #49768, #1541, #59110, #54603, #40750, #11490, #15039, #35300, #55250, #25328, #50091, #911, #40115, #15998, #5394, #59756, #54921, #30463, #25011, #30792, #6045, #31107, #50728, #45266, #6671, #46222, #56522, #32377, #12121, #17596, #22424, #27546, #22741, #31745, #41383, #61976, #42022, #12442, #7317, #11796, #61663, #60713, #37212, #13073, #36258, #42338, #2185, #32054, #52002, #51376, #56838, #12755, #47177, #17896, #26928, #61032, #37518, #7943, #51690, #2487, #55884, #56198, #57159, #3120, #16954, #6996, #32694, #36893, #52324, #46545, #16635, #8258, #26606, #1864, #22102, #31413, #27861, #61344, #21468, #41067, #51052, #21789, #36567, #41697, #17268, #7631, #27235, #46859, #2803, #19143, #23049, #35150, #42653, #52939, #23679, #18830, #57778, #53255 ) ),
 .UNSPECIFIED., .F., .F., .F. ) 
 B_SPLINE_SURFACE_WITH_KNOTS ( ( 2, 2 ),
 ( 3, 2, 2, 2, 2, 2, 2, 2, 2, 2, 2, 2, 2, 2, 2, 2, 2, 2, 2, 2, 2, 2, 2, 2, 2, 2, 2, 2, 2, 2, 2, 2, 2, 2, 2, 2, 2, 2, 2, 2, 2, 2, 2, 2, 2, 2, 2, 2, 2, 2, 2, 2, 2, 2, 2, 2, 2, 2, 2, 2, 2, 2, 2, 2, 2, 2, 2, 2, 2, 2, 2, 2, 2, 2, 2, 2, 2, 2, 2, 2, 2, 2, 2, 2, 2, 2, 2, 2, 2, 2, 2, 2, 2, 2, 2, 2, 2, 2, 2, 2, 2, 2, 2, 2, 2, 2, 2, 2, 2, 2, 2, 2, 2, 2, 2, 2, 2, 2, 2, 2, 2, 2, 2, 2, 2, 2, 2, 2, 2, 2, 2, 2, 2, 2, 2, 2, 2, 2, 2, 2, 2, 2, 2, 2, 2, 2, 2, 2, 2, 2, 2, 2, 2, 2, 2, 2, 2, 2, 2, 2, 2, 2, 2, 2, 2, 2, 2, 2, 2, 2, 2, 2, 2, 2, 2, 2, 2, 2, 2, 2, 2, 2, 2, 2, 2, 2, 2, 2, 2, 2, 2, 2, 2, 2, 2, 2, 2, 2, 2, 2, 2, 2, 2, 2, 2, 2, 2, 2, 2, 2, 2, 2, 2, 2, 2, 2, 2, 2, 2, 2, 2, 2, 2, 2, 2, 2, 2, 2, 2, 2, 2, 2, 2, 2, 2, 2, 2, 2, 2, 2, 2, 2, 2, 2, 2, 2, 2, 2, 2, 2, 2, 2, 2, 2, 2, 2, 2, 2, 2, 2, 2, 2, 2, 2, 2, 2, 2, 2, 2, 2, 2, 2, 2, 2, 2, 2, 2, 2, 2, 2, 2, 2, 2, 2, 2, 2, 2, 2, 2, 2, 2, 2, 2, 2, 2, 2, 2, 2, 2, 2, 2, 2, 2, 2, 2, 2, 2, 2, 2, 2, 2, 2, 2, 2, 2, 2, 2, 2, 2, 2, 2, 2, 2, 2, 2, 2, 2, 2, 2, 2, 2, 2, 2, 2, 2, 2, 2, 2, 2, 2, 2, 2, 2, 2, 2, 2, 2, 2, 2, 2, 2, 2, 2, 2, 2, 2, 2, 2, 2, 2, 2, 2, 2, 2, 2, 2, 2, 2, 2, 2, 2, 2, 2, 2, 2, 2, 2, 2, 2, 2, 2, 2, 2, 2, 2, 2, 2, 2, 2, 2, 2, 2, 2, 2, 2, 2, 2, 2, 2, 2, 2, 2, 2, 2, 2, 2, 2, 2, 2, 2, 2, 2, 2, 2, 2, 2, 2, 2, 2, 2, 2, 2, 2, 2, 2, 2, 2, 2, 2, 2, 2, 2, 2, 2, 2, 2, 2, 2, 2, 2, 2, 2, 2, 2, 2, 2, 2, 2, 2, 2, 2, 2, 2, 2, 2, 2, 2, 2, 2, 2, 2, 2, 2, 2, 2, 2, 2, 2, 2, 2, 2, 2, 2, 2, 2, 2, 2, 2, 2, 2, 2, 2, 2, 2, 2, 2, 2, 2, 2, 2, 2, 2, 2, 2, 2, 2, 2, 2, 2, 2, 2, 2, 2, 2, 2, 2, 2, 2, 2, 2, 2, 2, 2, 2, 2, 2, 2, 2, 2, 2, 2, 2, 2, 2, 2, 2, 2, 2, 2, 2, 2, 2, 2, 2, 2, 2, 2, 2, 2, 2, 2, 2, 2, 2, 2, 2, 2, 2, 2, 2, 2, 2, 2, 2, 2, 2, 2, 2, 2, 2, 2, 2, 2, 2, 2, 2, 2, 2, 2, 2, 2, 2, 2, 2, 2, 2, 2, 2, 2, 2, 2, 2, 2, 2, 2, 2, 2, 2, 2, 2, 2, 2, 2, 2, 2, 2, 2, 2, 2, 2, 2, 2, 2, 2, 2, 2, 2, 2, 2, 2, 2, 2, 2, 2, 2, 2, 2, 2, 2, 2, 2, 2, 2, 2, 2, 2, 2, 2, 2, 2, 2, 2, 2, 2, 2, 2, 2, 2, 2, 2, 2, 2, 2, 2, 2, 2, 2, 2, 2, 2, 2, 2, 2, 2, 2, 2, 2, 2, 2, 2, 2, 2, 2, 2, 2, 2, 2, 2, 2, 2, 2, 2, 2, 2, 2, 2, 2, 2, 2, 2, 2, 2, 2, 2, 2, 2, 2, 2, 2, 2, 2, 2, 2, 2, 2, 2, 2, 2, 2, 2, 2, 2, 2, 2, 2, 2, 2, 2, 2, 2, 2, 2, 2, 2, 2, 2, 2, 2, 2, 2, 2, 2, 2, 2, 2, 2, 2, 2, 2, 2, 2, 2, 2, 2, 2, 2, 2, 2, 2, 2, 2, 2, 2, 2, 2, 2, 2, 2, 2, 2, 2, 2, 2, 2, 2, 2, 2, 2, 2, 2, 2, 2, 2, 2, 2, 2, 2, 2, 2, 2, 2, 2, 2, 2, 2, 2, 2, 2, 2, 2, 2, 2, 2, 2, 2, 2, 2, 2, 2, 2, 2, 2, 2, 2, 2, 2, 2, 2, 2, 2, 2, 2, 2, 2, 2, 2, 2, 2, 2, 2, 2, 2, 2, 2, 2, 2, 2, 2, 2, 2, 2, 2, 2, 2, 2, 2, 2, 2, 2, 2, 2, 2, 2, 2, 2, 2, 2, 2, 2, 2, 3 ),
 ( 0.000000000000000000, 1.000000000000000000 ),
 ( 0.000000000000000000, 0.001190476190476190584, 0.002380952380952381167, 0.003571428571428571317, 0.004761904761904762334, 0.005952380952380952051, 0.007142857142857142634, 0.008333333333333333218, 0.009523809523809524669, 0.01071428571428571438, 0.01190476190476190410, 0.01309523809523809555, 0.01428571428571428527, 0.01547619047619047672, 0.01666666666666666644, 0.01785714285714285615, 0.01904761904761904934, 0.02023809523809523905, 0.02142857142857142877, 0.02261904761904761849, 0.02380952380952380820, 0.02500000000000000139, 0.02619047619047619110, 0.02738095238095238082, 0.02857142857142857054, 0.02976190476190476025, 0.03095238095238095344, 0.03214285714285713969, 0.03333333333333333287, 0.03452380952380952606, 0.03571428571428571230, 0.03690476190476190549, 0.03809523809523809867, 0.03928571428571428492, 0.04047619047619047811, 0.04166666666666666435, 0.04285714285714285754, 0.04404761904761905073, 0.04523809523809523697, 0.04642857142857143016, 0.04761904761904761640, 0.04880952380952380959, 0.05000000000000000278, 0.05119047619047618902, 0.05238095238095238221, 0.05357142857142856845, 0.05476190476190476164, 0.05595238095238095483, 0.05714285714285714107, 0.05833333333333333426, 0.05952380952380952051, 0.06071428571428571369, 0.06190476190476190688, 0.06309523809523809312, 0.06428571428571427937, 0.06547619047619047949, 0.06666666666666666574, 0.06785714285714285199, 0.06904761904761905211, 0.07023809523809523836, 0.07142857142857142461, 0.07261904761904762473, 0.07380952380952381098, 0.07499999999999999722, 0.07619047619047619735, 0.07738095238095238360, 0.07857142857142856984, 0.07976190476190475609, 0.08095238095238095621, 0.08214285714285714246, 0.08333333333333332871, 0.08452380952380952883, 0.08571428571428571508, 0.08690476190476190133, 0.08809523809523810145, 0.08928571428571428770, 0.09047619047619047394, 0.09166666666666666019, 0.09285714285714286031, 0.09404761904761904656, 0.09523809523809523281, 0.09642857142857143293, 0.09761904761904761918, 0.09880952380952380543, 0.1000000000000000056, 0.1011904761904761918, 0.1023809523809523780, 0.1035714285714285782, 0.1047619047619047644, 0.1059523809523809507, 0.1071428571428571369, 0.1083333333333333370, 0.1095238095238095233, 0.1107142857142857095, 0.1119047619047619097, 0.1130952380952380959, 0.1142857142857142821, 0.1154761904761904823, 0.1166666666666666685, 0.1178571428571428548, 0.1190476190476190410, 0.1202380952380952411, 0.1214285714285714274, 0.1226190476190476136, 0.1238095238095238138, 0.1250000000000000000, 0.1261904761904761862, 0.1273809523809523725, 0.1285714285714285587, 0.1297619047619047727, 0.1309523809523809590, 0.1321428571428571452, 0.1333333333333333315, 0.1345238095238095177, 0.1357142857142857040, 0.1369047619047619180, 0.1380952380952381042, 0.1392857142857142905, 0.1404761904761904767, 0.1416666666666666630, 0.1428571428571428492, 0.1440476190476190355, 0.1452380952380952495, 0.1464285714285714357, 0.1476190476190476220, 0.1488095238095238082, 0.1499999999999999944, 0.1511904761904761807, 0.1523809523809523947, 0.1535714285714285809, 0.1547619047619047672, 0.1559523809523809534, 0.1571428571428571397, 0.1583333333333333259, 0.1595238095238095122, 0.1607142857142857262, 0.1619047619047619124, 0.1630952380952380987, 0.1642857142857142849, 0.1654761904761904712, 0.1666666666666666574, 0.1678571428571428437, 0.1690476190476190577, 0.1702380952380952439, 0.1714285714285714302, 0.1726190476190476164, 0.1738095238095238027, 0.1749999999999999889, 0.1761904761904762029, 0.1773809523809523891, 0.1785714285714285754, 0.1797619047619047616, 0.1809523809523809479, 0.1821428571428571341, 0.1833333333333333204, 0.1845238095238095344, 0.1857142857142857206, 0.1869047619047619069, 0.1880952380952380931, 0.1892857142857142794, 0.1904761904761904656, 0.1916666666666666796, 0.1928571428571428659, 0.1940476190476190521, 0.1952380952380952384, 0.1964285714285714246, 0.1976190476190476109, 0.1988095238095237971, 0.2000000000000000111, 0.2011904761904761973, 0.2023809523809523836, 0.2035714285714285698, 0.2047619047619047561, 0.2059523809523809423, 0.2071428571428571563, 0.2083333333333333426, 0.2095238095238095288, 0.2107142857142857151, 0.2119047619047619013, 0.2130952380952380876, 0.2142857142857142738, 0.2154761904761904878, 0.2166666666666666741, 0.2178571428571428603, 0.2190476190476190466, 0.2202380952380952328, 0.2214285714285714191, 0.2226190476190476053, 0.2238095238095238193, 0.2250000000000000056, 0.2261904761904761918, 0.2273809523809523780, 0.2285714285714285643, 0.2297619047619047505, 0.2309523809523809645, 0.2321428571428571508, 0.2333333333333333370, 0.2345238095238095233, 0.2357142857142857095, 0.2369047619047618958, 0.2380952380952380820, 0.2392857142857142960, 0.2404761904761904823, 0.2416666666666666685, 0.2428571428571428548, 0.2440476190476190410, 0.2452380952380952273, 0.2464285714285714413, 0.2476190476190476275, 0.2488095238095238138, 0.2500000000000000000, 0.2511904761904761862, 0.2523809523809523725, 0.2535714285714285587, 0.2547619047619047450, 0.2559523809523809312, 0.2571428571428571175, 0.2583333333333333592, 0.2595238095238095455, 0.2607142857142857317, 0.2619047619047619180, 0.2630952380952381042, 0.2642857142857142905, 0.2654761904761904767, 0.2666666666666666630, 0.2678571428571428492, 0.2690476190476190355, 0.2702380952380952217, 0.2714285714285714080, 0.2726190476190475942, 0.2738095238095238360, 0.2750000000000000222, 0.2761904761904762085, 0.2773809523809523947, 0.2785714285714285809, 0.2797619047619047672, 0.2809523809523809534, 0.2821428571428571397, 0.2833333333333333259, 0.2845238095238095122, 0.2857142857142856984, 0.2869047619047618847, 0.2880952380952380709, 0.2892857142857143127, 0.2904761904761904989, 0.2916666666666666852, 0.2928571428571428714, 0.2940476190476190577, 0.2952380952380952439, 0.2964285714285714302, 0.2976190476190476164, 0.2988095238095238027, 0.2999999999999999889, 0.3011904761904761751, 0.3023809523809523614, 0.3035714285714285476, 0.3047619047619047894, 0.3059523809523809756, 0.3071428571428571619, 0.3083333333333333481, 0.3095238095238095344, 0.3107142857142857206, 0.3119047619047619069, 0.3130952380952380931, 0.3142857142857142794, 0.3154761904761904656, 0.3166666666666666519, 0.3178571428571428381, 0.3190476190476190244, 0.3202380952380952106, 0.3214285714285714524, 0.3226190476190476386, 0.3238095238095238249, 0.3250000000000000111, 0.3261904761904761973, 0.3273809523809523836, 0.3285714285714285698, 0.3297619047619047561, 0.3309523809523809423, 0.3321428571428571286, 0.3333333333333333148, 0.3345238095238095011, 0.3357142857142856873, 0.3369047619047619291, 0.3380952380952381153, 0.3392857142857143016, 0.3404761904761904878, 0.3416666666666666741, 0.3428571428571428603, 0.3440476190476190466, 0.3452380952380952328, 0.3464285714285714191, 0.3476190476190476053, 0.3488095238095237915, 0.3499999999999999778, 0.3511904761904761640, 0.3523809523809524058, 0.3535714285714285920, 0.3547619047619047783, 0.3559523809523809645, 0.3571428571428571508, 0.3583333333333333370, 0.3595238095238095233, 0.3607142857142857095, 0.3619047619047618958, 0.3630952380952380820, 0.3642857142857142683, 0.3654761904761904545, 0.3666666666666666408, 0.3678571428571428825, 0.3690476190476190688, 0.3702380952380952550, 0.3714285714285714413, 0.3726190476190476275, 0.3738095238095238138, 0.3750000000000000000, 0.3761904761904761862, 0.3773809523809523725, 0.3785714285714285587, 0.3797619047619047450, 0.3809523809523809312, 0.3821428571428571175, 0.3833333333333333592, 0.3845238095238095455, 0.3857142857142857317, 0.3869047619047619180, 0.3880952380952381042, 0.3892857142857142905, 0.3904761904761904767, 0.3916666666666666630, 0.3928571428571428492, 0.3940476190476190355, 0.3952380952380952217, 0.3964285714285714080, 0.3976190476190475942, 0.3988095238095238360, 0.4000000000000000222, 0.4011904761904762085, 0.4023809523809523947, 0.4035714285714285809, 0.4047619047619047672, 0.4059523809523809534, 0.4071428571428571397, 0.4083333333333333259, 0.4095238095238095122, 0.4107142857142856984, 0.4119047619047618847, 0.4130952380952380709, 0.4142857142857143127, 0.4154761904761904989, 0.4166666666666666852, 0.4178571428571428714, 0.4190476190476190577, 0.4202380952380952439, 0.4214285714285714302, 0.4226190476190476164, 0.4238095238095238027, 0.4249999999999999889, 0.4261904761904761751, 0.4273809523809523614, 0.4285714285714285476, 0.4297619047619047894, 0.4309523809523809756, 0.4321428571428571619, 0.4333333333333333481, 0.4345238095238095344, 0.4357142857142857206, 0.4369047619047619069, 0.4380952380952380931, 0.4392857142857142794, 0.4404761904761904656, 0.4416666666666666519, 0.4428571428571428381, 0.4440476190476190244, 0.4452380952380952106, 0.4464285714285714524, 0.4476190476190476386, 0.4488095238095238249, 0.4500000000000000111, 0.4511904761904761973, 0.4523809523809523836, 0.4535714285714285698, 0.4547619047619047561, 0.4559523809523809423, 0.4571428571428571286, 0.4583333333333333148, 0.4595238095238095011, 0.4607142857142856873, 0.4619047619047619291, 0.4630952380952381153, 0.4642857142857143016, 0.4654761904761904878, 0.4666666666666666741, 0.4678571428571428603, 0.4690476190476190466, 0.4702380952380952328, 0.4714285714285714191, 0.4726190476190476053, 0.4738095238095237915, 0.4749999999999999778, 0.4761904761904761640, 0.4773809523809524058, 0.4785714285714285920, 0.4797619047619047783, 0.4809523809523809645, 0.4821428571428571508, 0.4833333333333333370, 0.4845238095238095233, 0.4857142857142857095, 0.4869047619047618958, 0.4880952380952380820, 0.4892857142857142683, 0.4904761904761904545, 0.4916666666666666408, 0.4928571428571428825, 0.4940476190476190688, 0.4952380952380952550, 0.4964285714285714413, 0.4976190476190476275, 0.4988095238095238138, 0.5000000000000000000, 0.5011904761904761862, 0.5023809523809523725, 0.5035714285714285587, 0.5047619047619047450, 0.5059523809523809312, 0.5071428571428571175, 0.5083333333333333037, 0.5095238095238094900, 0.5107142857142856762, 0.5119047619047618625, 0.5130952380952380487, 0.5142857142857142350, 0.5154761904761904212, 0.5166666666666667185, 0.5178571428571429047, 0.5190476190476190910, 0.5202380952380952772, 0.5214285714285714635, 0.5226190476190476497, 0.5238095238095238360, 0.5250000000000000222, 0.5261904761904762085, 0.5273809523809523947, 0.5285714285714285809, 0.5297619047619047672, 0.5309523809523809534, 0.5321428571428571397, 0.5333333333333333259, 0.5345238095238095122, 0.5357142857142856984, 0.5369047619047618847, 0.5380952380952380709, 0.5392857142857142572, 0.5404761904761904434, 0.5416666666666666297, 0.5428571428571428159, 0.5440476190476190022, 0.5452380952380951884, 0.5464285714285713746, 0.5476190476190476719, 0.5488095238095238582, 0.5500000000000000444, 0.5511904761904762307, 0.5523809523809524169, 0.5535714285714286031, 0.5547619047619047894, 0.5559523809523809756, 0.5571428571428571619, 0.5583333333333333481, 0.5595238095238095344, 0.5607142857142857206, 0.5619047619047619069, 0.5630952380952380931, 0.5642857142857142794, 0.5654761904761904656, 0.5666666666666666519, 0.5678571428571428381, 0.5690476190476190244, 0.5702380952380952106, 0.5714285714285713969, 0.5726190476190475831, 0.5738095238095237693, 0.5749999999999999556, 0.5761904761904761418, 0.5773809523809523281, 0.5785714285714286254, 0.5797619047619048116, 0.5809523809523809978, 0.5821428571428571841, 0.5833333333333333703, 0.5845238095238095566, 0.5857142857142857428, 0.5869047619047619291, 0.5880952380952381153, 0.5892857142857143016, 0.5904761904761904878, 0.5916666666666666741, 0.5928571428571428603, 0.5940476190476190466, 0.5952380952380952328, 0.5964285714285714191, 0.5976190476190476053, 0.5988095238095237915, 0.5999999999999999778, 0.6011904761904761640, 0.6023809523809523503, 0.6035714285714285365, 0.6047619047619047228, 0.6059523809523809090, 0.6071428571428570953, 0.6083333333333332815, 0.6095238095238095788, 0.6107142857142857650, 0.6119047619047619513, 0.6130952380952381375, 0.6142857142857143238, 0.6154761904761905100, 0.6166666666666666963, 0.6178571428571428825, 0.6190476190476190688, 0.6202380952380952550, 0.6214285714285714413, 0.6226190476190476275, 0.6238095238095238138, 0.6250000000000000000, 0.6261904761904761862, 0.6273809523809523725, 0.6285714285714285587, 0.6297619047619047450, 0.6309523809523809312, 0.6321428571428571175, 0.6333333333333333037, 0.6345238095238094900, 0.6357142857142856762, 0.6369047619047618625, 0.6380952380952380487, 0.6392857142857142350, 0.6404761904761904212, 0.6416666666666667185, 0.6428571428571429047, 0.6440476190476190910, 0.6452380952380952772, 0.6464285714285714635, 0.6476190476190476497, 0.6488095238095238360, 0.6500000000000000222, 0.6511904761904762085, 0.6523809523809523947, 0.6535714285714285809, 0.6547619047619047672, 0.6559523809523809534, 0.6571428571428571397, 0.6583333333333333259, 0.6595238095238095122, 0.6607142857142856984, 0.6619047619047618847, 0.6630952380952380709, 0.6642857142857142572, 0.6654761904761904434, 0.6666666666666666297, 0.6678571428571428159, 0.6690476190476190022, 0.6702380952380951884, 0.6714285714285713746, 0.6726190476190476719, 0.6738095238095238582, 0.6750000000000000444, 0.6761904761904762307, 0.6773809523809524169, 0.6785714285714286031, 0.6797619047619047894, 0.6809523809523809756, 0.6821428571428571619, 0.6833333333333333481, 0.6845238095238095344, 0.6857142857142857206, 0.6869047619047619069, 0.6880952380952380931, 0.6892857142857142794, 0.6904761904761904656, 0.6916666666666666519, 0.6928571428571428381, 0.6940476190476190244, 0.6952380952380952106, 0.6964285714285713969, 0.6976190476190475831, 0.6988095238095237693, 0.6999999999999999556, 0.7011904761904761418, 0.7023809523809523281, 0.7035714285714286254, 0.7047619047619048116, 0.7059523809523809978, 0.7071428571428571841, 0.7083333333333333703, 0.7095238095238095566, 0.7107142857142857428, 0.7119047619047619291, 0.7130952380952381153, 0.7142857142857143016, 0.7154761904761904878, 0.7166666666666666741, 0.7178571428571428603, 0.7190476190476190466, 0.7202380952380952328, 0.7214285714285714191, 0.7226190476190476053, 0.7238095238095237915, 0.7249999999999999778, 0.7261904761904761640, 0.7273809523809523503, 0.7285714285714285365, 0.7297619047619047228, 0.7309523809523809090, 0.7321428571428570953, 0.7333333333333332815, 0.7345238095238095788, 0.7357142857142857650, 0.7369047619047619513, 0.7380952380952381375, 0.7392857142857143238, 0.7404761904761905100, 0.7416666666666666963, 0.7428571428571428825, 0.7440476190476190688, 0.7452380952380952550, 0.7464285714285714413, 0.7476190476190476275, 0.7488095238095238138, 0.7500000000000000000, 0.7511904761904761862, 0.7523809523809523725, 0.7535714285714285587, 0.7547619047619047450, 0.7559523809523809312, 0.7571428571428571175, 0.7583333333333333037, 0.7595238095238094900, 0.7607142857142856762, 0.7619047619047618625, 0.7630952380952380487, 0.7642857142857142350, 0.7654761904761904212, 0.7666666666666667185, 0.7678571428571429047, 0.7690476190476190910, 0.7702380952380952772, 0.7714285714285714635, 0.7726190476190476497, 0.7738095238095238360, 0.7750000000000000222, 0.7761904761904762085, 0.7773809523809523947, 0.7785714285714285809, 0.7797619047619047672, 0.7809523809523809534, 0.7821428571428571397, 0.7833333333333333259, 0.7845238095238095122, 0.7857142857142856984, 0.7869047619047618847, 0.7880952380952380709, 0.7892857142857142572, 0.7904761904761904434, 0.7916666666666666297, 0.7928571428571428159, 0.7940476190476190022, 0.7952380952380951884, 0.7964285714285713746, 0.7976190476190476719, 0.7988095238095238582, 0.8000000000000000444, 0.8011904761904762307, 0.8023809523809524169, 0.8035714285714286031, 0.8047619047619047894, 0.8059523809523809756, 0.8071428571428571619, 0.8083333333333333481, 0.8095238095238095344, 0.8107142857142857206, 0.8119047619047619069, 0.8130952380952380931, 0.8142857142857142794, 0.8154761904761904656, 0.8166666666666666519, 0.8178571428571428381, 0.8190476190476190244, 0.8202380952380952106, 0.8214285714285713969, 0.8226190476190475831, 0.8238095238095237693, 0.8249999999999999556, 0.8261904761904761418, 0.8273809523809523281, 0.8285714285714286254, 0.8297619047619048116, 0.8309523809523809978, 0.8321428571428571841, 0.8333333333333333703, 0.8345238095238095566, 0.8357142857142857428, 0.8369047619047619291, 0.8380952380952381153, 0.8392857142857143016, 0.8404761904761904878, 0.8416666666666666741, 0.8428571428571428603, 0.8440476190476190466, 0.8452380952380952328, 0.8464285714285714191, 0.8476190476190476053, 0.8488095238095237915, 0.8499999999999999778, 0.8511904761904761640, 0.8523809523809523503, 0.8535714285714285365, 0.8547619047619047228, 0.8559523809523809090, 0.8571428571428570953, 0.8583333333333332815, 0.8595238095238095788, 0.8607142857142857650, 0.8619047619047619513, 0.8630952380952381375, 0.8642857142857143238, 0.8654761904761905100, 0.8666666666666666963, 0.8678571428571428825, 0.8690476190476190688, 0.8702380952380952550, 0.8714285714285714413, 0.8726190476190476275, 0.8738095238095238138, 0.8750000000000000000, 0.8761904761904761862, 0.8773809523809523725, 0.8785714285714285587, 0.8797619047619047450, 0.8809523809523809312, 0.8821428571428571175, 0.8833333333333333037, 0.8845238095238094900, 0.8857142857142856762, 0.8869047619047618625, 0.8880952380952380487, 0.8892857142857142350, 0.8904761904761904212, 0.8916666666666667185, 0.8928571428571429047, 0.8940476190476190910, 0.8952380952380952772, 0.8964285714285714635, 0.8976190476190476497, 0.8988095238095238360, 0.9000000000000000222, 0.9011904761904762085, 0.9023809523809523947, 0.9035714285714285809, 0.9047619047619047672, 0.9059523809523809534, 0.9071428571428571397, 0.9083333333333333259, 0.9095238095238095122, 0.9107142857142856984, 0.9119047619047618847, 0.9130952380952380709, 0.9142857142857142572, 0.9154761904761904434, 0.9166666666666666297, 0.9178571428571428159, 0.9190476190476190022, 0.9202380952380951884, 0.9214285714285713746, 0.9226190476190476719, 0.9238095238095238582, 0.9250000000000000444, 0.9261904761904762307, 0.9273809523809524169, 0.9285714285714286031, 0.9297619047619047894, 0.9309523809523809756, 0.9321428571428571619, 0.9333333333333333481, 0.9345238095238095344, 0.9357142857142857206, 0.9369047619047619069, 0.9380952380952380931, 0.9392857142857142794, 0.9404761904761904656, 0.9416666666666666519, 0.9428571428571428381, 0.9440476190476190244, 0.9452380952380952106, 0.9464285714285713969, 0.9476190476190475831, 0.9488095238095237693, 0.9499999999999999556, 0.9511904761904761418, 0.9523809523809523281, 0.9535714285714286254, 0.9547619047619048116, 0.9559523809523809978, 0.9571428571428571841, 0.9583333333333333703, 0.9595238095238095566, 0.9607142857142857428, 0.9619047619047619291, 0.9630952380952381153, 0.9642857142857143016, 0.9654761904761904878, 0.9666666666666666741, 0.9678571428571428603, 0.9690476190476190466, 0.9702380952380952328, 0.9714285714285714191, 0.9726190476190476053, 0.9738095238095237915, 0.9749999999999999778, 0.9761904761904761640, 0.9773809523809523503, 0.9785714285714285365, 0.9797619047619047228, 0.9809523809523809090, 0.9821428571428570953, 0.9833333333333332815, 0.9845238095238095788, 0.9857142857142857650, 0.9869047619047619513, 0.9880952380952381375, 0.9892857142857143238, 0.9904761904761905100, 0.9916666666666666963, 0.9928571428571428825, 0.9940476190476190688, 0.9952380952380952550, 0.9964285714285714413, 0.9976190476190476275, 0.9988095238095238138, 1.000000000000000000 ),
 .UNSPECIFIED. ) 
 GEOMETRIC_REPRESENTATION_ITEM ( )  RATIONAL_B_SPLINE_SURFACE ( (
 ( 1.000000000000000000, 0.8660254037844387076, 1.000000000000000000, 0.8660254037844387076, 1.000000000000000000, 0.8660254037844387076, 1.000000000000000000, 0.8660254037844387076, 1.000000000000000000, 0.8660254037844387076, 1.000000000000000000, 0.8660254037844387076, 1.000000000000000000, 0.8660254037844387076, 1.000000000000000000, 0.8660254037844387076, 1.000000000000000000, 0.8660254037844387076, 1.000000000000000000, 0.8660254037844387076, 1.000000000000000000, 0.8660254037844387076, 1.000000000000000000, 0.8660254037844387076, 1.000000000000000000, 0.8660254037844387076, 1.000000000000000000, 0.8660254037844387076, 1.000000000000000000, 0.8660254037844387076, 1.000000000000000000, 0.8660254037844387076, 1.000000000000000000, 0.8660254037844387076, 1.000000000000000000, 0.8660254037844387076, 1.000000000000000000, 0.8660254037844387076, 1.000000000000000000, 0.8660254037844387076, 1.000000000000000000, 0.8660254037844387076, 1.000000000000000000, 0.8660254037844387076, 1.000000000000000000, 0.8660254037844387076, 1.000000000000000000, 0.8660254037844387076, 1.000000000000000000, 0.8660254037844387076, 1.000000000000000000, 0.8660254037844387076, 1.000000000000000000, 0.8660254037844387076, 1.000000000000000000, 0.8660254037844387076, 1.000000000000000000, 0.8660254037844387076, 1.000000000000000000, 0.8660254037844387076, 1.000000000000000000, 0.8660254037844387076, 1.000000000000000000, 0.8660254037844387076, 1.000000000000000000, 0.8660254037844387076, 1.000000000000000000, 0.8660254037844387076, 1.000000000000000000, 0.8660254037844387076, 1.000000000000000000, 0.8660254037844387076, 1.000000000000000000, 0.8660254037844387076, 1.000000000000000000, 0.8660254037844387076, 1.000000000000000000, 0.8660254037844387076, 1.000000000000000000, 0.8660254037844387076, 1.000000000000000000, 0.8660254037844387076, 1.000000000000000000, 0.8660254037844387076, 1.000000000000000000, 0.8660254037844387076, 1.000000000000000000, 0.8660254037844387076, 1.000000000000000000, 0.8660254037844387076, 1.000000000000000000, 0.8660254037844387076, 1.000000000000000000, 0.8660254037844387076, 1.000000000000000000, 0.8660254037844387076, 1.000000000000000000, 0.8660254037844387076, 1.000000000000000000, 0.8660254037844387076, 1.000000000000000000, 0.8660254037844387076, 1.000000000000000000, 0.8660254037844387076, 1.000000000000000000, 0.8660254037844387076, 1.000000000000000000, 0.8660254037844387076, 1.000000000000000000, 0.8660254037844387076, 1.000000000000000000, 0.8660254037844387076, 1.000000000000000000, 0.8660254037844387076, 1.000000000000000000, 0.8660254037844387076, 1.000000000000000000, 0.8660254037844387076, 1.000000000000000000, 0.8660254037844387076, 1.000000000000000000, 0.8660254037844387076, 1.000000000000000000, 0.8660254037844387076, 1.000000000000000000, 0.8660254037844387076, 1.000000000000000000, 0.8660254037844387076, 1.000000000000000000, 0.8660254037844387076, 1.000000000000000000, 0.8660254037844387076, 1.000000000000000000, 0.8660254037844387076, 1.000000000000000000, 0.8660254037844387076, 1.000000000000000000, 0.8660254037844387076, 1.000000000000000000, 0.8660254037844387076, 1.000000000000000000, 0.8660254037844387076, 1.000000000000000000, 0.8660254037844387076, 1.000000000000000000, 0.8660254037844387076, 1.000000000000000000, 0.8660254037844387076, 1.000000000000000000, 0.8660254037844387076, 1.000000000000000000, 0.8660254037844387076, 1.000000000000000000, 0.8660254037844387076, 1.000000000000000000, 0.8660254037844387076, 1.000000000000000000, 0.8660254037844387076, 1.000000000000000000, 0.8660254037844387076, 1.000000000000000000, 0.8660254037844387076, 1.000000000000000000, 0.8660254037844387076, 1.000000000000000000, 0.8660254037844387076, 1.000000000000000000, 0.8660254037844387076, 1.000000000000000000, 0.8660254037844387076, 1.000000000000000000, 0.8660254037844387076, 1.000000000000000000, 0.8660254037844387076, 1.000000000000000000, 0.8660254037844387076, 1.000000000000000000, 0.8660254037844387076, 1.000000000000000000, 0.8660254037844387076, 1.000000000000000000, 0.8660254037844387076, 1.000000000000000000, 0.8660254037844387076, 1.000000000000000000, 0.8660254037844387076, 1.000000000000000000, 0.8660254037844387076, 1.000000000000000000, 0.8660254037844387076, 1.000000000000000000, 0.8660254037844387076, 1.000000000000000000, 0.8660254037844387076, 1.000000000000000000, 0.8660254037844387076, 1.000000000000000000, 0.8660254037844387076, 1.000000000000000000, 0.8660254037844387076, 1.000000000000000000, 0.8660254037844387076, 1.000000000000000000, 0.8660254037844387076, 1.000000000000000000, 0.8660254037844387076, 1.000000000000000000, 0.8660254037844387076, 1.000000000000000000, 0.8660254037844387076, 1.000000000000000000, 0.8660254037844387076, 1.000000000000000000, 0.8660254037844387076, 1.000000000000000000, 0.8660254037844387076, 1.000000000000000000, 0.8660254037844387076, 1.000000000000000000, 0.8660254037844387076, 1.000000000000000000, 0.8660254037844387076, 1.000000000000000000, 0.8660254037844387076, 1.000000000000000000, 0.8660254037844387076, 1.000000000000000000, 0.8660254037844387076, 1.000000000000000000, 0.8660254037844387076, 1.000000000000000000, 0.8660254037844387076, 1.000000000000000000, 0.8660254037844387076, 1.000000000000000000, 0.8660254037844387076, 1.000000000000000000, 0.8660254037844387076, 1.000000000000000000, 0.8660254037844387076, 1.000000000000000000, 0.8660254037844387076, 1.000000000000000000, 0.8660254037844387076, 1.000000000000000000, 0.8660254037844387076, 1.000000000000000000, 0.8660254037844387076, 1.000000000000000000, 0.8660254037844387076, 1.000000000000000000, 0.8660254037844387076, 1.000000000000000000, 0.8660254037844387076, 1.000000000000000000, 0.8660254037844387076, 1.000000000000000000, 0.8660254037844387076, 1.000000000000000000, 0.8660254037844387076, 1.000000000000000000, 0.8660254037844387076, 1.000000000000000000, 0.8660254037844387076, 1.000000000000000000, 0.8660254037844387076, 1.000000000000000000, 0.8660254037844387076, 1.000000000000000000, 0.8660254037844387076, 1.000000000000000000, 0.8660254037844387076, 1.000000000000000000, 0.8660254037844387076, 1.000000000000000000, 0.8660254037844387076, 1.000000000000000000, 0.8660254037844387076, 1.000000000000000000, 0.8660254037844387076, 1.000000000000000000, 0.8660254037844387076, 1.000000000000000000, 0.8660254037844387076, 1.000000000000000000, 0.8660254037844387076, 1.000000000000000000, 0.8660254037844387076, 1.000000000000000000, 0.8660254037844387076, 1.000000000000000000, 0.8660254037844387076, 1.000000000000000000, 0.8660254037844387076, 1.000000000000000000, 0.8660254037844387076, 1.000000000000000000, 0.8660254037844387076, 1.000000000000000000, 0.8660254037844387076, 1.000000000000000000, 0.8660254037844387076, 1.000000000000000000, 0.8660254037844387076, 1.000000000000000000, 0.8660254037844387076, 1.000000000000000000, 0.8660254037844387076, 1.000000000000000000, 0.8660254037844387076, 1.000000000000000000, 0.8660254037844387076, 1.000000000000000000, 0.8660254037844387076, 1.000000000000000000, 0.8660254037844387076, 1.000000000000000000, 0.8660254037844387076, 1.000000000000000000, 0.8660254037844387076, 1.000000000000000000, 0.8660254037844387076, 1.000000000000000000, 0.8660254037844387076, 1.000000000000000000, 0.8660254037844387076, 1.000000000000000000, 0.8660254037844387076, 1.000000000000000000, 0.8660254037844387076, 1.000000000000000000, 0.8660254037844387076, 1.000000000000000000, 0.8660254037844387076, 1.000000000000000000, 0.8660254037844387076, 1.000000000000000000, 0.8660254037844387076, 1.000000000000000000, 0.8660254037844387076, 1.000000000000000000, 0.8660254037844387076, 1.000000000000000000, 0.8660254037844387076, 1.000000000000000000, 0.8660254037844387076, 1.000000000000000000, 0.8660254037844387076, 1.000000000000000000, 0.8660254037844387076, 1.000000000000000000, 0.8660254037844387076, 1.000000000000000000, 0.8660254037844387076, 1.000000000000000000, 0.8660254037844387076, 1.000000000000000000, 0.8660254037844387076, 1.000000000000000000, 0.8660254037844387076, 1.000000000000000000, 0.8660254037844387076, 1.000000000000000000, 0.8660254037844387076, 1.000000000000000000, 0.8660254037844387076, 1.000000000000000000, 0.8660254037844387076, 1.000000000000000000, 0.8660254037844387076, 1.000000000000000000, 0.8660254037844387076, 1.000000000000000000, 0.8660254037844387076, 1.000000000000000000, 0.8660254037844387076, 1.000000000000000000, 0.8660254037844387076, 1.000000000000000000, 0.8660254037844387076, 1.000000000000000000, 0.8660254037844387076, 1.000000000000000000, 0.8660254037844387076, 1.000000000000000000, 0.8660254037844387076, 1.000000000000000000, 0.8660254037844387076, 1.000000000000000000, 0.8660254037844387076, 1.000000000000000000, 0.8660254037844387076, 1.000000000000000000, 0.8660254037844387076, 1.000000000000000000, 0.8660254037844387076, 1.000000000000000000, 0.8660254037844387076, 1.000000000000000000, 0.8660254037844387076, 1.000000000000000000, 0.8660254037844387076, 1.000000000000000000, 0.8660254037844387076, 1.000000000000000000, 0.8660254037844387076, 1.000000000000000000, 0.8660254037844387076, 1.000000000000000000, 0.8660254037844387076, 1.000000000000000000, 0.8660254037844387076, 1.000000000000000000, 0.8660254037844387076, 1.000000000000000000, 0.8660254037844387076, 1.000000000000000000, 0.8660254037844387076, 1.000000000000000000, 0.8660254037844387076, 1.000000000000000000, 0.8660254037844387076, 1.000000000000000000, 0.8660254037844387076, 1.000000000000000000, 0.8660254037844387076, 1.000000000000000000, 0.8660254037844387076, 1.000000000000000000, 0.8660254037844387076, 1.000000000000000000, 0.8660254037844387076, 1.000000000000000000, 0.8660254037844387076, 1.000000000000000000, 0.8660254037844387076, 1.000000000000000000, 0.8660254037844387076, 1.000000000000000000, 0.8660254037844387076, 1.000000000000000000, 0.8660254037844387076, 1.000000000000000000, 0.8660254037844387076, 1.000000000000000000, 0.8660254037844387076, 1.000000000000000000, 0.8660254037844387076, 1.000000000000000000, 0.8660254037844387076, 1.000000000000000000, 0.8660254037844387076, 1.000000000000000000, 0.8660254037844387076, 1.000000000000000000, 0.8660254037844387076, 1.000000000000000000, 0.8660254037844387076, 1.000000000000000000, 0.8660254037844387076, 1.000000000000000000, 0.8660254037844387076, 1.000000000000000000, 0.8660254037844387076, 1.000000000000000000, 0.8660254037844387076, 1.000000000000000000, 0.8660254037844387076, 1.000000000000000000, 0.8660254037844387076, 1.000000000000000000, 0.8660254037844387076, 1.000000000000000000, 0.8660254037844387076, 1.000000000000000000, 0.8660254037844387076, 1.000000000000000000, 0.8660254037844387076, 1.000000000000000000, 0.8660254037844387076, 1.000000000000000000, 0.8660254037844387076, 1.000000000000000000, 0.8660254037844387076, 1.000000000000000000, 0.8660254037844387076, 1.000000000000000000, 0.8660254037844387076, 1.000000000000000000, 0.8660254037844387076, 1.000000000000000000, 0.8660254037844387076, 1.000000000000000000, 0.8660254037844387076, 1.000000000000000000, 0.8660254037844387076, 1.000000000000000000, 0.8660254037844387076, 1.000000000000000000, 0.8660254037844387076, 1.000000000000000000, 0.8660254037844387076, 1.000000000000000000, 0.8660254037844387076, 1.000000000000000000, 0.8660254037844387076, 1.000000000000000000, 0.8660254037844387076, 1.000000000000000000, 0.8660254037844387076, 1.000000000000000000, 0.8660254037844387076, 1.000000000000000000, 0.8660254037844387076, 1.000000000000000000, 0.8660254037844387076, 1.000000000000000000, 0.8660254037844387076, 1.000000000000000000, 0.8660254037844387076, 1.000000000000000000, 0.8660254037844387076, 1.000000000000000000, 0.8660254037844387076, 1.000000000000000000, 0.8660254037844387076, 1.000000000000000000, 0.8660254037844387076, 1.000000000000000000, 0.8660254037844387076, 1.000000000000000000, 0.8660254037844387076, 1.000000000000000000, 0.8660254037844387076, 1.000000000000000000, 0.8660254037844387076, 1.000000000000000000, 0.8660254037844387076, 1.000000000000000000, 0.8660254037844387076, 1.000000000000000000, 0.8660254037844387076, 1.000000000000000000, 0.8660254037844387076, 1.000000000000000000, 0.8660254037844387076, 1.000000000000000000, 0.8660254037844387076, 1.000000000000000000, 0.8660254037844387076, 1.000000000000000000, 0.8660254037844387076, 1.000000000000000000, 0.8660254037844387076, 1.000000000000000000, 0.8660254037844387076, 1.000000000000000000, 0.8660254037844387076, 1.000000000000000000, 0.8660254037844387076, 1.000000000000000000, 0.8660254037844387076, 1.000000000000000000, 0.8660254037844387076, 1.000000000000000000, 0.8660254037844387076, 1.000000000000000000, 0.8660254037844387076, 1.000000000000000000, 0.8660254037844387076, 1.000000000000000000, 0.8660254037844387076, 1.000000000000000000, 0.8660254037844387076, 1.000000000000000000, 0.8660254037844387076, 1.000000000000000000, 0.8660254037844387076, 1.000000000000000000, 0.8660254037844387076, 1.000000000000000000, 0.8660254037844387076, 1.000000000000000000, 0.8660254037844387076, 1.000000000000000000, 0.8660254037844387076, 1.000000000000000000, 0.8660254037844387076, 1.000000000000000000, 0.8660254037844387076, 1.000000000000000000, 0.8660254037844387076, 1.000000000000000000, 0.8660254037844387076, 1.000000000000000000, 0.8660254037844387076, 1.000000000000000000, 0.8660254037844387076, 1.000000000000000000, 0.8660254037844387076, 1.000000000000000000, 0.8660254037844387076, 1.000000000000000000, 0.8660254037844387076, 1.000000000000000000, 0.8660254037844387076, 1.000000000000000000, 0.8660254037844387076, 1.000000000000000000, 0.8660254037844387076, 1.000000000000000000, 0.8660254037844387076, 1.000000000000000000, 0.8660254037844387076, 1.000000000000000000, 0.8660254037844387076, 1.000000000000000000, 0.8660254037844387076, 1.000000000000000000, 0.8660254037844387076, 1.000000000000000000, 0.8660254037844387076, 1.000000000000000000, 0.8660254037844387076, 1.000000000000000000, 0.8660254037844387076, 1.000000000000000000, 0.8660254037844387076, 1.000000000000000000, 0.8660254037844387076, 1.000000000000000000, 0.8660254037844387076, 1.000000000000000000, 0.8660254037844387076, 1.000000000000000000, 0.8660254037844387076, 1.000000000000000000, 0.8660254037844387076, 1.000000000000000000, 0.8660254037844387076, 1.000000000000000000, 0.8660254037844387076, 1.000000000000000000, 0.8660254037844387076, 1.000000000000000000, 0.8660254037844387076, 1.000000000000000000, 0.8660254037844387076, 1.000000000000000000, 0.8660254037844387076, 1.000000000000000000, 0.8660254037844387076, 1.000000000000000000, 0.8660254037844387076, 1.000000000000000000, 0.8660254037844387076, 1.000000000000000000, 0.8660254037844387076, 1.000000000000000000, 0.8660254037844387076, 1.000000000000000000, 0.8660254037844387076, 1.000000000000000000, 0.8660254037844387076, 1.000000000000000000, 0.8660254037844387076, 1.000000000000000000, 0.8660254037844387076, 1.000000000000000000, 0.8660254037844387076, 1.000000000000000000, 0.8660254037844387076, 1.000000000000000000, 0.8660254037844387076, 1.000000000000000000, 0.8660254037844387076, 1.000000000000000000, 0.8660254037844387076, 1.000000000000000000, 0.8660254037844387076, 1.000000000000000000, 0.8660254037844387076, 1.000000000000000000, 0.8660254037844387076, 1.000000000000000000, 0.8660254037844387076, 1.000000000000000000, 0.8660254037844387076, 1.000000000000000000, 0.8660254037844387076, 1.000000000000000000, 0.8660254037844387076, 1.000000000000000000, 0.8660254037844387076, 1.000000000000000000, 0.8660254037844387076, 1.000000000000000000, 0.8660254037844387076, 1.000000000000000000, 0.8660254037844387076, 1.000000000000000000, 0.8660254037844387076, 1.000000000000000000, 0.8660254037844387076, 1.000000000000000000, 0.8660254037844387076, 1.000000000000000000, 0.8660254037844387076, 1.000000000000000000, 0.8660254037844387076, 1.000000000000000000, 0.8660254037844387076, 1.000000000000000000, 0.8660254037844387076, 1.000000000000000000, 0.8660254037844387076, 1.000000000000000000, 0.8660254037844387076, 1.000000000000000000, 0.8660254037844387076, 1.000000000000000000, 0.8660254037844387076, 1.000000000000000000, 0.8660254037844387076, 1.000000000000000000, 0.8660254037844387076, 1.000000000000000000, 0.8660254037844387076, 1.000000000000000000, 0.8660254037844387076, 1.000000000000000000, 0.8660254037844387076, 1.000000000000000000, 0.8660254037844387076, 1.000000000000000000, 0.8660254037844387076, 1.000000000000000000, 0.8660254037844387076, 1.000000000000000000, 0.8660254037844387076, 1.000000000000000000, 0.8660254037844387076, 1.000000000000000000, 0.8660254037844387076, 1.000000000000000000, 0.8660254037844387076, 1.000000000000000000, 0.8660254037844387076, 1.000000000000000000, 0.8660254037844387076, 1.000000000000000000, 0.8660254037844387076, 1.000000000000000000, 0.8660254037844387076, 1.000000000000000000, 0.8660254037844387076, 1.000000000000000000, 0.8660254037844387076, 1.000000000000000000, 0.8660254037844387076, 1.000000000000000000, 0.8660254037844387076, 1.000000000000000000, 0.8660254037844387076, 1.000000000000000000, 0.8660254037844387076, 1.000000000000000000, 0.8660254037844387076, 1.000000000000000000, 0.8660254037844387076, 1.000000000000000000, 0.8660254037844387076, 1.000000000000000000, 0.8660254037844387076, 1.000000000000000000, 0.8660254037844387076, 1.000000000000000000, 0.8660254037844387076, 1.000000000000000000, 0.8660254037844387076, 1.000000000000000000, 0.8660254037844387076, 1.000000000000000000, 0.8660254037844387076, 1.000000000000000000, 0.8660254037844387076, 1.000000000000000000, 0.8660254037844387076, 1.000000000000000000, 0.8660254037844387076, 1.000000000000000000, 0.8660254037844387076, 1.000000000000000000, 0.8660254037844387076, 1.000000000000000000, 0.8660254037844387076, 1.000000000000000000, 0.8660254037844387076, 1.000000000000000000, 0.8660254037844387076, 1.000000000000000000, 0.8660254037844387076, 1.000000000000000000, 0.8660254037844387076, 1.000000000000000000, 0.8660254037844387076, 1.000000000000000000, 0.8660254037844387076, 1.000000000000000000, 0.8660254037844387076, 1.000000000000000000, 0.8660254037844387076, 1.000000000000000000, 0.8660254037844387076, 1.000000000000000000, 0.8660254037844387076, 1.000000000000000000, 0.8660254037844387076, 1.000000000000000000, 0.8660254037844387076, 1.000000000000000000, 0.8660254037844387076, 1.000000000000000000, 0.8660254037844387076, 1.000000000000000000, 0.8660254037844387076, 1.000000000000000000, 0.8660254037844387076, 1.000000000000000000, 0.8660254037844387076, 1.000000000000000000, 0.8660254037844387076, 1.000000000000000000, 0.8660254037844387076, 1.000000000000000000, 0.8660254037844387076, 1.000000000000000000, 0.8660254037844387076, 1.000000000000000000, 0.8660254037844387076, 1.000000000000000000, 0.8660254037844387076, 1.000000000000000000, 0.8660254037844387076, 1.000000000000000000, 0.8660254037844387076, 1.000000000000000000, 0.8660254037844387076, 1.000000000000000000, 0.8660254037844387076, 1.000000000000000000, 0.8660254037844387076, 1.000000000000000000, 0.8660254037844387076, 1.000000000000000000, 0.8660254037844387076, 1.000000000000000000, 0.8660254037844387076, 1.000000000000000000, 0.8660254037844387076, 1.000000000000000000, 0.8660254037844387076, 1.000000000000000000, 0.8660254037844387076, 1.000000000000000000, 0.8660254037844387076, 1.000000000000000000, 0.8660254037844387076, 1.000000000000000000, 0.8660254037844387076, 1.000000000000000000, 0.8660254037844387076, 1.000000000000000000, 0.8660254037844387076, 1.000000000000000000, 0.8660254037844387076, 1.000000000000000000, 0.8660254037844387076, 1.000000000000000000, 0.8660254037844387076, 1.000000000000000000, 0.8660254037844387076, 1.000000000000000000, 0.8660254037844387076, 1.000000000000000000, 0.8660254037844387076, 1.000000000000000000, 0.8660254037844387076, 1.000000000000000000, 0.8660254037844387076, 1.000000000000000000, 0.8660254037844387076, 1.000000000000000000, 0.8660254037844387076, 1.000000000000000000, 0.8660254037844387076, 1.000000000000000000, 0.8660254037844387076, 1.000000000000000000, 0.8660254037844387076, 1.000000000000000000, 0.8660254037844387076, 1.000000000000000000, 0.8660254037844387076, 1.000000000000000000, 0.8660254037844387076, 1.000000000000000000, 0.8660254037844387076, 1.000000000000000000, 0.8660254037844387076, 1.000000000000000000, 0.8660254037844387076, 1.000000000000000000, 0.8660254037844387076, 1.000000000000000000, 0.8660254037844387076, 1.000000000000000000, 0.8660254037844387076, 1.000000000000000000, 0.8660254037844387076, 1.000000000000000000, 0.8660254037844387076, 1.000000000000000000, 0.8660254037844387076, 1.000000000000000000, 0.8660254037844387076, 1.000000000000000000, 0.8660254037844387076, 1.000000000000000000, 0.8660254037844387076, 1.000000000000000000, 0.8660254037844387076, 1.000000000000000000, 0.8660254037844387076, 1.000000000000000000, 0.8660254037844387076, 1.000000000000000000, 0.8660254037844387076, 1.000000000000000000, 0.8660254037844387076, 1.000000000000000000, 0.8660254037844387076, 1.000000000000000000, 0.8660254037844387076, 1.000000000000000000, 0.8660254037844387076, 1.000000000000000000, 0.8660254037844387076, 1.000000000000000000, 0.8660254037844387076, 1.000000000000000000, 0.8660254037844387076, 1.000000000000000000, 0.8660254037844387076, 1.000000000000000000, 0.8660254037844387076, 1.000000000000000000, 0.8660254037844387076, 1.000000000000000000, 0.8660254037844387076, 1.000000000000000000, 0.8660254037844387076, 1.000000000000000000, 0.8660254037844387076, 1.000000000000000000, 0.8660254037844387076, 1.000000000000000000, 0.8660254037844387076, 1.000000000000000000, 0.8660254037844387076, 1.000000000000000000, 0.8660254037844387076, 1.000000000000000000, 0.8660254037844387076, 1.000000000000000000, 0.8660254037844387076, 1.000000000000000000, 0.8660254037844387076, 1.000000000000000000, 0.8660254037844387076, 1.000000000000000000, 0.8660254037844387076, 1.000000000000000000, 0.8660254037844387076, 1.000000000000000000, 0.8660254037844387076, 1.000000000000000000, 0.8660254037844387076, 1.000000000000000000, 0.8660254037844387076, 1.000000000000000000, 0.8660254037844387076, 1.000000000000000000, 0.8660254037844387076, 1.000000000000000000, 0.8660254037844387076, 1.000000000000000000, 0.8660254037844387076, 1.000000000000000000, 0.8660254037844387076, 1.000000000000000000, 0.8660254037844387076, 1.000000000000000000, 0.8660254037844387076, 1.000000000000000000, 0.8660254037844387076, 1.000000000000000000, 0.8660254037844387076, 1.000000000000000000, 0.8660254037844387076, 1.000000000000000000, 0.8660254037844387076, 1.000000000000000000, 0.8660254037844387076, 1.000000000000000000, 0.8660254037844387076, 1.000000000000000000, 0.8660254037844387076, 1.000000000000000000, 0.8660254037844387076, 1.000000000000000000, 0.8660254037844387076, 1.000000000000000000, 0.8660254037844387076, 1.000000000000000000, 0.8660254037844387076, 1.000000000000000000, 0.8660254037844387076, 1.000000000000000000, 0.8660254037844387076, 1.000000000000000000, 0.8660254037844387076, 1.000000000000000000, 0.8660254037844387076, 1.000000000000000000, 0.8660254037844387076, 1.000000000000000000, 0.8660254037844387076, 1.000000000000000000, 0.8660254037844387076, 1.000000000000000000, 0.8660254037844387076, 1.000000000000000000, 0.8660254037844387076, 1.000000000000000000, 0.8660254037844387076, 1.000000000000000000, 0.8660254037844387076, 1.000000000000000000, 0.8660254037844387076, 1.000000000000000000, 0.8660254037844387076, 1.000000000000000000, 0.8660254037844387076, 1.000000000000000000, 0.8660254037844387076, 1.000000000000000000, 0.8660254037844387076, 1.000000000000000000, 0.8660254037844387076, 1.000000000000000000, 0.8660254037844387076, 1.000000000000000000, 0.8660254037844387076, 1.000000000000000000, 0.8660254037844387076, 1.000000000000000000, 0.8660254037844387076, 1.000000000000000000, 0.8660254037844387076, 1.000000000000000000, 0.8660254037844387076, 1.000000000000000000, 0.8660254037844387076, 1.000000000000000000, 0.8660254037844387076, 1.000000000000000000, 0.8660254037844387076, 1.000000000000000000, 0.8660254037844387076, 1.000000000000000000, 0.8660254037844387076, 1.000000000000000000, 0.8660254037844387076, 1.000000000000000000, 0.8660254037844387076, 1.000000000000000000, 0.8660254037844387076, 1.000000000000000000, 0.8660254037844387076, 1.000000000000000000, 0.8660254037844387076, 1.000000000000000000, 0.8660254037844387076, 1.000000000000000000, 0.8660254037844387076, 1.000000000000000000, 0.8660254037844387076, 1.000000000000000000, 0.8660254037844387076, 1.000000000000000000, 0.8660254037844387076, 1.000000000000000000, 0.8660254037844387076, 1.000000000000000000, 0.8660254037844387076, 1.000000000000000000, 0.8660254037844387076, 1.000000000000000000, 0.8660254037844387076, 1.000000000000000000, 0.8660254037844387076, 1.000000000000000000, 0.8660254037844387076, 1.000000000000000000, 0.8660254037844387076, 1.000000000000000000, 0.8660254037844387076, 1.000000000000000000, 0.8660254037844387076, 1.000000000000000000, 0.8660254037844387076, 1.000000000000000000, 0.8660254037844387076, 1.000000000000000000, 0.8660254037844387076, 1.000000000000000000, 0.8660254037844387076, 1.000000000000000000, 0.8660254037844387076, 1.000000000000000000, 0.8660254037844387076, 1.000000000000000000, 0.8660254037844387076, 1.000000000000000000, 0.8660254037844387076, 1.000000000000000000, 0.8660254037844387076, 1.000000000000000000, 0.8660254037844387076, 1.000000000000000000, 0.8660254037844387076, 1.000000000000000000, 0.8660254037844387076, 1.000000000000000000, 0.8660254037844387076, 1.000000000000000000, 0.8660254037844387076, 1.000000000000000000, 0.8660254037844387076, 1.000000000000000000, 0.8660254037844387076, 1.000000000000000000, 0.8660254037844387076, 1.000000000000000000, 0.8660254037844387076, 1.000000000000000000, 0.8660254037844387076, 1.000000000000000000, 0.8660254037844387076, 1.000000000000000000, 0.8660254037844387076, 1.000000000000000000, 0.8660254037844387076, 1.000000000000000000, 0.8660254037844387076, 1.000000000000000000, 0.8660254037844387076, 1.000000000000000000, 0.8660254037844387076, 1.000000000000000000, 0.8660254037844387076, 1.000000000000000000, 0.8660254037844387076, 1.000000000000000000, 0.8660254037844387076, 1.000000000000000000, 0.8660254037844387076, 1.000000000000000000, 0.8660254037844387076, 1.000000000000000000, 0.8660254037844387076, 1.000000000000000000, 0.8660254037844387076, 1.000000000000000000, 0.8660254037844387076, 1.000000000000000000, 0.8660254037844387076, 1.000000000000000000, 0.8660254037844387076, 1.000000000000000000, 0.8660254037844387076, 1.000000000000000000, 0.8660254037844387076, 1.000000000000000000, 0.8660254037844387076, 1.000000000000000000, 0.8660254037844387076, 1.000000000000000000, 0.8660254037844387076, 1.000000000000000000, 0.8660254037844387076, 1.000000000000000000, 0.8660254037844387076, 1.000000000000000000, 0.8660254037844387076, 1.000000000000000000, 0.8660254037844387076, 1.000000000000000000, 0.8660254037844387076, 1.000000000000000000, 0.8660254037844387076, 1.000000000000000000, 0.8660254037844387076, 1.000000000000000000, 0.8660254037844387076, 1.000000000000000000, 0.8660254037844387076, 1.000000000000000000, 0.8660254037844387076, 1.000000000000000000, 0.8660254037844387076, 1.000000000000000000, 0.8660254037844387076, 1.000000000000000000, 0.8660254037844387076, 1.000000000000000000, 0.8660254037844387076, 1.000000000000000000, 0.8660254037844387076, 1.000000000000000000, 0.8660254037844387076, 1.000000000000000000, 0.8660254037844387076, 1.000000000000000000, 0.8660254037844387076, 1.000000000000000000, 0.8660254037844387076, 1.000000000000000000, 0.8660254037844387076, 1.000000000000000000, 0.8660254037844387076, 1.000000000000000000, 0.8660254037844387076, 1.000000000000000000, 0.8660254037844387076, 1.000000000000000000, 0.8660254037844387076, 1.000000000000000000, 0.8660254037844387076, 1.000000000000000000, 0.8660254037844387076, 1.000000000000000000, 0.8660254037844387076, 1.000000000000000000, 0.8660254037844387076, 1.000000000000000000, 0.8660254037844387076, 1.000000000000000000, 0.8660254037844387076, 1.000000000000000000, 0.8660254037844387076, 1.000000000000000000, 0.8660254037844387076, 1.000000000000000000, 0.8660254037844387076, 1.000000000000000000, 0.8660254037844387076, 1.000000000000000000, 0.8660254037844387076, 1.000000000000000000, 0.8660254037844387076, 1.000000000000000000, 0.8660254037844387076, 1.000000000000000000, 0.8660254037844387076, 1.000000000000000000, 0.8660254037844387076, 1.000000000000000000, 0.8660254037844387076, 1.000000000000000000, 0.8660254037844387076, 1.000000000000000000, 0.8660254037844387076, 1.000000000000000000, 0.8660254037844387076, 1.000000000000000000, 0.8660254037844387076, 1.000000000000000000, 0.8660254037844387076, 1.000000000000000000, 0.8660254037844387076, 1.000000000000000000, 0.8660254037844387076, 1.000000000000000000, 0.8660254037844387076, 1.000000000000000000, 0.8660254037844387076, 1.000000000000000000, 0.8660254037844387076, 1.000000000000000000, 0.8660254037844387076, 1.000000000000000000, 0.8660254037844387076, 1.000000000000000000, 0.8660254037844387076, 1.000000000000000000, 0.8660254037844387076, 1.000000000000000000, 0.8660254037844387076, 1.000000000000000000, 0.8660254037844387076, 1.000000000000000000, 0.8660254037844387076, 1.000000000000000000, 0.8660254037844387076, 1.000000000000000000, 0.8660254037844387076, 1.000000000000000000, 0.8660254037844387076, 1.000000000000000000, 0.8660254037844387076, 1.000000000000000000, 0.8660254037844387076, 1.000000000000000000, 0.8660254037844387076, 1.000000000000000000, 0.8660254037844387076, 1.000000000000000000, 0.8660254037844387076, 1.000000000000000000, 0.8660254037844387076, 1.000000000000000000, 0.8660254037844387076, 1.000000000000000000, 0.8660254037844387076, 1.000000000000000000, 0.8660254037844387076, 1.000000000000000000, 0.8660254037844387076, 1.000000000000000000, 0.8660254037844387076, 1.000000000000000000, 0.8660254037844387076, 1.000000000000000000, 0.8660254037844387076, 1.000000000000000000, 0.8660254037844387076, 1.000000000000000000, 0.8660254037844387076, 1.000000000000000000, 0.8660254037844387076, 1.000000000000000000, 0.8660254037844387076, 1.000000000000000000, 0.8660254037844387076, 1.000000000000000000, 0.8660254037844387076, 1.000000000000000000, 0.8660254037844387076, 1.000000000000000000, 0.8660254037844387076, 1.000000000000000000, 0.8660254037844387076, 1.000000000000000000, 0.8660254037844387076, 1.000000000000000000, 0.8660254037844387076, 1.000000000000000000, 0.8660254037844387076, 1.000000000000000000, 0.8660254037844387076, 1.000000000000000000, 0.8660254037844387076, 1.000000000000000000, 0.8660254037844387076, 1.000000000000000000, 0.8660254037844387076, 1.000000000000000000, 0.8660254037844387076, 1.000000000000000000, 0.8660254037844387076, 1.000000000000000000, 0.8660254037844387076, 1.000000000000000000, 0.8660254037844387076, 1.000000000000000000, 0.8660254037844387076, 1.000000000000000000, 0.8660254037844387076, 1.000000000000000000, 0.8660254037844387076, 1.000000000000000000, 0.8660254037844387076, 1.000000000000000000, 0.8660254037844387076, 1.000000000000000000, 0.8660254037844387076, 1.000000000000000000, 0.8660254037844387076, 1.000000000000000000, 0.8660254037844387076, 1.000000000000000000, 0.8660254037844387076, 1.000000000000000000, 0.8660254037844387076, 1.000000000000000000, 0.8660254037844387076, 1.000000000000000000, 0.8660254037844387076, 1.000000000000000000, 0.8660254037844387076, 1.000000000000000000, 0.8660254037844387076, 1.000000000000000000, 0.8660254037844387076, 1.000000000000000000, 0.8660254037844387076, 1.000000000000000000, 0.8660254037844387076, 1.000000000000000000, 0.8660254037844387076, 1.000000000000000000, 0.8660254037844387076, 1.000000000000000000, 0.8660254037844387076, 1.000000000000000000, 0.8660254037844387076, 1.000000000000000000, 0.8660254037844387076, 1.000000000000000000, 0.8660254037844387076, 1.000000000000000000, 0.8660254037844387076, 1.000000000000000000, 0.8660254037844387076, 1.000000000000000000, 0.8660254037844387076, 1.000000000000000000, 0.8660254037844387076, 1.000000000000000000, 0.8660254037844387076, 1.000000000000000000, 0.8660254037844387076, 1.000000000000000000, 0.8660254037844387076, 1.000000000000000000, 0.8660254037844387076, 1.000000000000000000, 0.8660254037844387076, 1.000000000000000000, 0.8660254037844387076, 1.000000000000000000, 0.8660254037844387076, 1.000000000000000000, 0.8660254037844387076, 1.000000000000000000, 0.8660254037844387076, 1.000000000000000000, 0.8660254037844387076, 1.000000000000000000, 0.8660254037844387076, 1.000000000000000000, 0.8660254037844387076, 1.000000000000000000, 0.8660254037844387076, 1.000000000000000000, 0.8660254037844387076, 1.000000000000000000, 0.8660254037844387076, 1.000000000000000000, 0.8660254037844387076, 1.000000000000000000, 0.8660254037844387076, 1.000000000000000000, 0.8660254037844387076, 1.000000000000000000, 0.8660254037844387076, 1.000000000000000000, 0.8660254037844387076, 1.000000000000000000, 0.8660254037844387076, 1.000000000000000000, 0.8660254037844387076, 1.000000000000000000, 0.8660254037844387076, 1.000000000000000000, 0.8660254037844387076, 1.000000000000000000, 0.8660254037844387076, 1.000000000000000000, 0.8660254037844387076, 1.000000000000000000, 0.8660254037844387076, 1.000000000000000000, 0.8660254037844387076, 1.000000000000000000, 0.8660254037844387076, 1.000000000000000000, 0.8660254037844387076, 1.000000000000000000, 0.8660254037844387076, 1.000000000000000000, 0.8660254037844387076, 1.000000000000000000, 0.8660254037844387076, 1.000000000000000000, 0.8660254037844387076, 1.000000000000000000, 0.8660254037844387076, 1.000000000000000000, 0.8660254037844387076, 1.000000000000000000, 0.8660254037844387076, 1.000000000000000000, 0.8660254037844387076, 1.000000000000000000, 0.8660254037844387076, 1.000000000000000000, 0.8660254037844387076, 1.000000000000000000, 0.8660254037844387076, 1.000000000000000000, 0.8660254037844387076, 1.000000000000000000, 0.8660254037844387076, 1.000000000000000000, 0.8660254037844387076, 1.000000000000000000, 0.8660254037844387076, 1.000000000000000000, 0.8660254037844387076, 1.000000000000000000, 0.8660254037844387076, 1.000000000000000000, 0.8660254037844387076, 1.000000000000000000, 0.8660254037844387076, 1.000000000000000000, 0.8660254037844387076, 1.000000000000000000, 0.8660254037844387076, 1.000000000000000000, 0.8660254037844387076, 1.000000000000000000, 0.8660254037844387076, 1.000000000000000000, 0.8660254037844387076, 1.000000000000000000, 0.8660254037844387076, 1.000000000000000000, 0.8660254037844387076, 1.000000000000000000, 0.8660254037844387076, 1.000000000000000000, 0.8660254037844387076, 1.000000000000000000, 0.8660254037844387076, 1.000000000000000000, 0.8660254037844387076, 1.000000000000000000, 0.8660254037844387076, 1.000000000000000000, 0.8660254037844387076, 1.000000000000000000, 0.8660254037844387076, 1.000000000000000000, 0.8660254037844387076, 1.000000000000000000, 0.8660254037844387076, 1.000000000000000000, 0.8660254037844387076, 1.000000000000000000, 0.8660254037844387076, 1.000000000000000000, 0.8660254037844387076, 1.000000000000000000, 0.8660254037844387076, 1.000000000000000000, 0.8660254037844387076, 1.000000000000000000, 0.8660254037844387076, 1.000000000000000000, 0.8660254037844387076, 1.000000000000000000, 0.8660254037844387076, 1.000000000000000000, 0.8660254037844387076, 1.000000000000000000, 0.8660254037844387076, 1.000000000000000000, 0.8660254037844387076, 1.000000000000000000, 0.8660254037844387076, 1.000000000000000000, 0.8660254037844387076, 1.000000000000000000, 0.8660254037844387076, 1.000000000000000000, 0.8660254037844387076, 1.000000000000000000, 0.8660254037844387076, 1.000000000000000000, 0.8660254037844387076, 1.000000000000000000, 0.8660254037844387076, 1.000000000000000000, 0.8660254037844387076, 1.000000000000000000, 0.8660254037844387076, 1.000000000000000000, 0.8660254037844387076, 1.000000000000000000, 0.8660254037844387076, 1.000000000000000000, 0.8660254037844387076, 1.000000000000000000, 0.8660254037844387076, 1.000000000000000000, 0.8660254037844387076, 1.000000000000000000, 0.8660254037844387076, 1.000000000000000000, 0.8660254037844387076, 1.000000000000000000, 0.8660254037844387076, 1.000000000000000000, 0.8660254037844387076, 1.000000000000000000, 0.8660254037844387076, 1.000000000000000000, 0.8660254037844387076, 1.000000000000000000, 0.8660254037844387076, 1.000000000000000000, 0.8660254037844387076, 1.000000000000000000, 0.8660254037844387076, 1.000000000000000000, 0.8660254037844387076, 1.000000000000000000, 0.8660254037844387076, 1.000000000000000000, 0.8660254037844387076, 1.000000000000000000, 0.8660254037844387076, 1.000000000000000000, 0.8660254037844387076, 1.000000000000000000, 0.8660254037844387076, 1.000000000000000000, 0.8660254037844387076, 1.000000000000000000, 0.8660254037844387076, 1.000000000000000000, 0.8660254037844387076, 1.000000000000000000, 0.8660254037844387076, 1.000000000000000000, 0.8660254037844387076, 1.000000000000000000, 0.8660254037844387076, 1.000000000000000000, 0.8660254037844387076, 1.000000000000000000, 0.8660254037844387076, 1.000000000000000000, 0.8660254037844387076, 1.000000000000000000, 0.8660254037844387076, 1.000000000000000000, 0.8660254037844387076, 1.000000000000000000, 0.8660254037844387076, 1.000000000000000000, 0.8660254037844387076, 1.000000000000000000, 0.8660254037844387076, 1.000000000000000000, 0.8660254037844387076, 1.000000000000000000),
 ( 1.000000000000000000, 0.8660254037844387076, 1.000000000000000000, 0.8660254037844387076, 1.000000000000000000, 0.8660254037844387076, 1.000000000000000000, 0.8660254037844387076, 1.000000000000000000, 0.8660254037844387076, 1.000000000000000000, 0.8660254037844387076, 1.000000000000000000, 0.8660254037844387076, 1.000000000000000000, 0.8660254037844387076, 1.000000000000000000, 0.8660254037844387076, 1.000000000000000000, 0.8660254037844387076, 1.000000000000000000, 0.8660254037844387076, 1.000000000000000000, 0.8660254037844387076, 1.000000000000000000, 0.8660254037844387076, 1.000000000000000000, 0.8660254037844387076, 1.000000000000000000, 0.8660254037844387076, 1.000000000000000000, 0.8660254037844387076, 1.000000000000000000, 0.8660254037844387076, 1.000000000000000000, 0.8660254037844387076, 1.000000000000000000, 0.8660254037844387076, 1.000000000000000000, 0.8660254037844387076, 1.000000000000000000, 0.8660254037844387076, 1.000000000000000000, 0.8660254037844387076, 1.000000000000000000, 0.8660254037844387076, 1.000000000000000000, 0.8660254037844387076, 1.000000000000000000, 0.8660254037844387076, 1.000000000000000000, 0.8660254037844387076, 1.000000000000000000, 0.8660254037844387076, 1.000000000000000000, 0.8660254037844387076, 1.000000000000000000, 0.8660254037844387076, 1.000000000000000000, 0.8660254037844387076, 1.000000000000000000, 0.8660254037844387076, 1.000000000000000000, 0.8660254037844387076, 1.000000000000000000, 0.8660254037844387076, 1.000000000000000000, 0.8660254037844387076, 1.000000000000000000, 0.8660254037844387076, 1.000000000000000000, 0.8660254037844387076, 1.000000000000000000, 0.8660254037844387076, 1.000000000000000000, 0.8660254037844387076, 1.000000000000000000, 0.8660254037844387076, 1.000000000000000000, 0.8660254037844387076, 1.000000000000000000, 0.8660254037844387076, 1.000000000000000000, 0.8660254037844387076, 1.000000000000000000, 0.8660254037844387076, 1.000000000000000000, 0.8660254037844387076, 1.000000000000000000, 0.8660254037844387076, 1.000000000000000000, 0.8660254037844387076, 1.000000000000000000, 0.8660254037844387076, 1.000000000000000000, 0.8660254037844387076, 1.000000000000000000, 0.8660254037844387076, 1.000000000000000000, 0.8660254037844387076, 1.000000000000000000, 0.8660254037844387076, 1.000000000000000000, 0.8660254037844387076, 1.000000000000000000, 0.8660254037844387076, 1.000000000000000000, 0.8660254037844387076, 1.000000000000000000, 0.8660254037844387076, 1.000000000000000000, 0.8660254037844387076, 1.000000000000000000, 0.8660254037844387076, 1.000000000000000000, 0.8660254037844387076, 1.000000000000000000, 0.8660254037844387076, 1.000000000000000000, 0.8660254037844387076, 1.000000000000000000, 0.8660254037844387076, 1.000000000000000000, 0.8660254037844387076, 1.000000000000000000, 0.8660254037844387076, 1.000000000000000000, 0.8660254037844387076, 1.000000000000000000, 0.8660254037844387076, 1.000000000000000000, 0.8660254037844387076, 1.000000000000000000, 0.8660254037844387076, 1.000000000000000000, 0.8660254037844387076, 1.000000000000000000, 0.8660254037844387076, 1.000000000000000000, 0.8660254037844387076, 1.000000000000000000, 0.8660254037844387076, 1.000000000000000000, 0.8660254037844387076, 1.000000000000000000, 0.8660254037844387076, 1.000000000000000000, 0.8660254037844387076, 1.000000000000000000, 0.8660254037844387076, 1.000000000000000000, 0.8660254037844387076, 1.000000000000000000, 0.8660254037844387076, 1.000000000000000000, 0.8660254037844387076, 1.000000000000000000, 0.8660254037844387076, 1.000000000000000000, 0.8660254037844387076, 1.000000000000000000, 0.8660254037844387076, 1.000000000000000000, 0.8660254037844387076, 1.000000000000000000, 0.8660254037844387076, 1.000000000000000000, 0.8660254037844387076, 1.000000000000000000, 0.8660254037844387076, 1.000000000000000000, 0.8660254037844387076, 1.000000000000000000, 0.8660254037844387076, 1.000000000000000000, 0.8660254037844387076, 1.000000000000000000, 0.8660254037844387076, 1.000000000000000000, 0.8660254037844387076, 1.000000000000000000, 0.8660254037844387076, 1.000000000000000000, 0.8660254037844387076, 1.000000000000000000, 0.8660254037844387076, 1.000000000000000000, 0.8660254037844387076, 1.000000000000000000, 0.8660254037844387076, 1.000000000000000000, 0.8660254037844387076, 1.000000000000000000, 0.8660254037844387076, 1.000000000000000000, 0.8660254037844387076, 1.000000000000000000, 0.8660254037844387076, 1.000000000000000000, 0.8660254037844387076, 1.000000000000000000, 0.8660254037844387076, 1.000000000000000000, 0.8660254037844387076, 1.000000000000000000, 0.8660254037844387076, 1.000000000000000000, 0.8660254037844387076, 1.000000000000000000, 0.8660254037844387076, 1.000000000000000000, 0.8660254037844387076, 1.000000000000000000, 0.8660254037844387076, 1.000000000000000000, 0.8660254037844387076, 1.000000000000000000, 0.8660254037844387076, 1.000000000000000000, 0.8660254037844387076, 1.000000000000000000, 0.8660254037844387076, 1.000000000000000000, 0.8660254037844387076, 1.000000000000000000, 0.8660254037844387076, 1.000000000000000000, 0.8660254037844387076, 1.000000000000000000, 0.8660254037844387076, 1.000000000000000000, 0.8660254037844387076, 1.000000000000000000, 0.8660254037844387076, 1.000000000000000000, 0.8660254037844387076, 1.000000000000000000, 0.8660254037844387076, 1.000000000000000000, 0.8660254037844387076, 1.000000000000000000, 0.8660254037844387076, 1.000000000000000000, 0.8660254037844387076, 1.000000000000000000, 0.8660254037844387076, 1.000000000000000000, 0.8660254037844387076, 1.000000000000000000, 0.8660254037844387076, 1.000000000000000000, 0.8660254037844387076, 1.000000000000000000, 0.8660254037844387076, 1.000000000000000000, 0.8660254037844387076, 1.000000000000000000, 0.8660254037844387076, 1.000000000000000000, 0.8660254037844387076, 1.000000000000000000, 0.8660254037844387076, 1.000000000000000000, 0.8660254037844387076, 1.000000000000000000, 0.8660254037844387076, 1.000000000000000000, 0.8660254037844387076, 1.000000000000000000, 0.8660254037844387076, 1.000000000000000000, 0.8660254037844387076, 1.000000000000000000, 0.8660254037844387076, 1.000000000000000000, 0.8660254037844387076, 1.000000000000000000, 0.8660254037844387076, 1.000000000000000000, 0.8660254037844387076, 1.000000000000000000, 0.8660254037844387076, 1.000000000000000000, 0.8660254037844387076, 1.000000000000000000, 0.8660254037844387076, 1.000000000000000000, 0.8660254037844387076, 1.000000000000000000, 0.8660254037844387076, 1.000000000000000000, 0.8660254037844387076, 1.000000000000000000, 0.8660254037844387076, 1.000000000000000000, 0.8660254037844387076, 1.000000000000000000, 0.8660254037844387076, 1.000000000000000000, 0.8660254037844387076, 1.000000000000000000, 0.8660254037844387076, 1.000000000000000000, 0.8660254037844387076, 1.000000000000000000, 0.8660254037844387076, 1.000000000000000000, 0.8660254037844387076, 1.000000000000000000, 0.8660254037844387076, 1.000000000000000000, 0.8660254037844387076, 1.000000000000000000, 0.8660254037844387076, 1.000000000000000000, 0.8660254037844387076, 1.000000000000000000, 0.8660254037844387076, 1.000000000000000000, 0.8660254037844387076, 1.000000000000000000, 0.8660254037844387076, 1.000000000000000000, 0.8660254037844387076, 1.000000000000000000, 0.8660254037844387076, 1.000000000000000000, 0.8660254037844387076, 1.000000000000000000, 0.8660254037844387076, 1.000000000000000000, 0.8660254037844387076, 1.000000000000000000, 0.8660254037844387076, 1.000000000000000000, 0.8660254037844387076, 1.000000000000000000, 0.8660254037844387076, 1.000000000000000000, 0.8660254037844387076, 1.000000000000000000, 0.8660254037844387076, 1.000000000000000000, 0.8660254037844387076, 1.000000000000000000, 0.8660254037844387076, 1.000000000000000000, 0.8660254037844387076, 1.000000000000000000, 0.8660254037844387076, 1.000000000000000000, 0.8660254037844387076, 1.000000000000000000, 0.8660254037844387076, 1.000000000000000000, 0.8660254037844387076, 1.000000000000000000, 0.8660254037844387076, 1.000000000000000000, 0.8660254037844387076, 1.000000000000000000, 0.8660254037844387076, 1.000000000000000000, 0.8660254037844387076, 1.000000000000000000, 0.8660254037844387076, 1.000000000000000000, 0.8660254037844387076, 1.000000000000000000, 0.8660254037844387076, 1.000000000000000000, 0.8660254037844387076, 1.000000000000000000, 0.8660254037844387076, 1.000000000000000000, 0.8660254037844387076, 1.000000000000000000, 0.8660254037844387076, 1.000000000000000000, 0.8660254037844387076, 1.000000000000000000, 0.8660254037844387076, 1.000000000000000000, 0.8660254037844387076, 1.000000000000000000, 0.8660254037844387076, 1.000000000000000000, 0.8660254037844387076, 1.000000000000000000, 0.8660254037844387076, 1.000000000000000000, 0.8660254037844387076, 1.000000000000000000, 0.8660254037844387076, 1.000000000000000000, 0.8660254037844387076, 1.000000000000000000, 0.8660254037844387076, 1.000000000000000000, 0.8660254037844387076, 1.000000000000000000, 0.8660254037844387076, 1.000000000000000000, 0.8660254037844387076, 1.000000000000000000, 0.8660254037844387076, 1.000000000000000000, 0.8660254037844387076, 1.000000000000000000, 0.8660254037844387076, 1.000000000000000000, 0.8660254037844387076, 1.000000000000000000, 0.8660254037844387076, 1.000000000000000000, 0.8660254037844387076, 1.000000000000000000, 0.8660254037844387076, 1.000000000000000000, 0.8660254037844387076, 1.000000000000000000, 0.8660254037844387076, 1.000000000000000000, 0.8660254037844387076, 1.000000000000000000, 0.8660254037844387076, 1.000000000000000000, 0.8660254037844387076, 1.000000000000000000, 0.8660254037844387076, 1.000000000000000000, 0.8660254037844387076, 1.000000000000000000, 0.8660254037844387076, 1.000000000000000000, 0.8660254037844387076, 1.000000000000000000, 0.8660254037844387076, 1.000000000000000000, 0.8660254037844387076, 1.000000000000000000, 0.8660254037844387076, 1.000000000000000000, 0.8660254037844387076, 1.000000000000000000, 0.8660254037844387076, 1.000000000000000000, 0.8660254037844387076, 1.000000000000000000, 0.8660254037844387076, 1.000000000000000000, 0.8660254037844387076, 1.000000000000000000, 0.8660254037844387076, 1.000000000000000000, 0.8660254037844387076, 1.000000000000000000, 0.8660254037844387076, 1.000000000000000000, 0.8660254037844387076, 1.000000000000000000, 0.8660254037844387076, 1.000000000000000000, 0.8660254037844387076, 1.000000000000000000, 0.8660254037844387076, 1.000000000000000000, 0.8660254037844387076, 1.000000000000000000, 0.8660254037844387076, 1.000000000000000000, 0.8660254037844387076, 1.000000000000000000, 0.8660254037844387076, 1.000000000000000000, 0.8660254037844387076, 1.000000000000000000, 0.8660254037844387076, 1.000000000000000000, 0.8660254037844387076, 1.000000000000000000, 0.8660254037844387076, 1.000000000000000000, 0.8660254037844387076, 1.000000000000000000, 0.8660254037844387076, 1.000000000000000000, 0.8660254037844387076, 1.000000000000000000, 0.8660254037844387076, 1.000000000000000000, 0.8660254037844387076, 1.000000000000000000, 0.8660254037844387076, 1.000000000000000000, 0.8660254037844387076, 1.000000000000000000, 0.8660254037844387076, 1.000000000000000000, 0.8660254037844387076, 1.000000000000000000, 0.8660254037844387076, 1.000000000000000000, 0.8660254037844387076, 1.000000000000000000, 0.8660254037844387076, 1.000000000000000000, 0.8660254037844387076, 1.000000000000000000, 0.8660254037844387076, 1.000000000000000000, 0.8660254037844387076, 1.000000000000000000, 0.8660254037844387076, 1.000000000000000000, 0.8660254037844387076, 1.000000000000000000, 0.8660254037844387076, 1.000000000000000000, 0.8660254037844387076, 1.000000000000000000, 0.8660254037844387076, 1.000000000000000000, 0.8660254037844387076, 1.000000000000000000, 0.8660254037844387076, 1.000000000000000000, 0.8660254037844387076, 1.000000000000000000, 0.8660254037844387076, 1.000000000000000000, 0.8660254037844387076, 1.000000000000000000, 0.8660254037844387076, 1.000000000000000000, 0.8660254037844387076, 1.000000000000000000, 0.8660254037844387076, 1.000000000000000000, 0.8660254037844387076, 1.000000000000000000, 0.8660254037844387076, 1.000000000000000000, 0.8660254037844387076, 1.000000000000000000, 0.8660254037844387076, 1.000000000000000000, 0.8660254037844387076, 1.000000000000000000, 0.8660254037844387076, 1.000000000000000000, 0.8660254037844387076, 1.000000000000000000, 0.8660254037844387076, 1.000000000000000000, 0.8660254037844387076, 1.000000000000000000, 0.8660254037844387076, 1.000000000000000000, 0.8660254037844387076, 1.000000000000000000, 0.8660254037844387076, 1.000000000000000000, 0.8660254037844387076, 1.000000000000000000, 0.8660254037844387076, 1.000000000000000000, 0.8660254037844387076, 1.000000000000000000, 0.8660254037844387076, 1.000000000000000000, 0.8660254037844387076, 1.000000000000000000, 0.8660254037844387076, 1.000000000000000000, 0.8660254037844387076, 1.000000000000000000, 0.8660254037844387076, 1.000000000000000000, 0.8660254037844387076, 1.000000000000000000, 0.8660254037844387076, 1.000000000000000000, 0.8660254037844387076, 1.000000000000000000, 0.8660254037844387076, 1.000000000000000000, 0.8660254037844387076, 1.000000000000000000, 0.8660254037844387076, 1.000000000000000000, 0.8660254037844387076, 1.000000000000000000, 0.8660254037844387076, 1.000000000000000000, 0.8660254037844387076, 1.000000000000000000, 0.8660254037844387076, 1.000000000000000000, 0.8660254037844387076, 1.000000000000000000, 0.8660254037844387076, 1.000000000000000000, 0.8660254037844387076, 1.000000000000000000, 0.8660254037844387076, 1.000000000000000000, 0.8660254037844387076, 1.000000000000000000, 0.8660254037844387076, 1.000000000000000000, 0.8660254037844387076, 1.000000000000000000, 0.8660254037844387076, 1.000000000000000000, 0.8660254037844387076, 1.000000000000000000, 0.8660254037844387076, 1.000000000000000000, 0.8660254037844387076, 1.000000000000000000, 0.8660254037844387076, 1.000000000000000000, 0.8660254037844387076, 1.000000000000000000, 0.8660254037844387076, 1.000000000000000000, 0.8660254037844387076, 1.000000000000000000, 0.8660254037844387076, 1.000000000000000000, 0.8660254037844387076, 1.000000000000000000, 0.8660254037844387076, 1.000000000000000000, 0.8660254037844387076, 1.000000000000000000, 0.8660254037844387076, 1.000000000000000000, 0.8660254037844387076, 1.000000000000000000, 0.8660254037844387076, 1.000000000000000000, 0.8660254037844387076, 1.000000000000000000, 0.8660254037844387076, 1.000000000000000000, 0.8660254037844387076, 1.000000000000000000, 0.8660254037844387076, 1.000000000000000000, 0.8660254037844387076, 1.000000000000000000, 0.8660254037844387076, 1.000000000000000000, 0.8660254037844387076, 1.000000000000000000, 0.8660254037844387076, 1.000000000000000000, 0.8660254037844387076, 1.000000000000000000, 0.8660254037844387076, 1.000000000000000000, 0.8660254037844387076, 1.000000000000000000, 0.8660254037844387076, 1.000000000000000000, 0.8660254037844387076, 1.000000000000000000, 0.8660254037844387076, 1.000000000000000000, 0.8660254037844387076, 1.000000000000000000, 0.8660254037844387076, 1.000000000000000000, 0.8660254037844387076, 1.000000000000000000, 0.8660254037844387076, 1.000000000000000000, 0.8660254037844387076, 1.000000000000000000, 0.8660254037844387076, 1.000000000000000000, 0.8660254037844387076, 1.000000000000000000, 0.8660254037844387076, 1.000000000000000000, 0.8660254037844387076, 1.000000000000000000, 0.8660254037844387076, 1.000000000000000000, 0.8660254037844387076, 1.000000000000000000, 0.8660254037844387076, 1.000000000000000000, 0.8660254037844387076, 1.000000000000000000, 0.8660254037844387076, 1.000000000000000000, 0.8660254037844387076, 1.000000000000000000, 0.8660254037844387076, 1.000000000000000000, 0.8660254037844387076, 1.000000000000000000, 0.8660254037844387076, 1.000000000000000000, 0.8660254037844387076, 1.000000000000000000, 0.8660254037844387076, 1.000000000000000000, 0.8660254037844387076, 1.000000000000000000, 0.8660254037844387076, 1.000000000000000000, 0.8660254037844387076, 1.000000000000000000, 0.8660254037844387076, 1.000000000000000000, 0.8660254037844387076, 1.000000000000000000, 0.8660254037844387076, 1.000000000000000000, 0.8660254037844387076, 1.000000000000000000, 0.8660254037844387076, 1.000000000000000000, 0.8660254037844387076, 1.000000000000000000, 0.8660254037844387076, 1.000000000000000000, 0.8660254037844387076, 1.000000000000000000, 0.8660254037844387076, 1.000000000000000000, 0.8660254037844387076, 1.000000000000000000, 0.8660254037844387076, 1.000000000000000000, 0.8660254037844387076, 1.000000000000000000, 0.8660254037844387076, 1.000000000000000000, 0.8660254037844387076, 1.000000000000000000, 0.8660254037844387076, 1.000000000000000000, 0.8660254037844387076, 1.000000000000000000, 0.8660254037844387076, 1.000000000000000000, 0.8660254037844387076, 1.000000000000000000, 0.8660254037844387076, 1.000000000000000000, 0.8660254037844387076, 1.000000000000000000, 0.8660254037844387076, 1.000000000000000000, 0.8660254037844387076, 1.000000000000000000, 0.8660254037844387076, 1.000000000000000000, 0.8660254037844387076, 1.000000000000000000, 0.8660254037844387076, 1.000000000000000000, 0.8660254037844387076, 1.000000000000000000, 0.8660254037844387076, 1.000000000000000000, 0.8660254037844387076, 1.000000000000000000, 0.8660254037844387076, 1.000000000000000000, 0.8660254037844387076, 1.000000000000000000, 0.8660254037844387076, 1.000000000000000000, 0.8660254037844387076, 1.000000000000000000, 0.8660254037844387076, 1.000000000000000000, 0.8660254037844387076, 1.000000000000000000, 0.8660254037844387076, 1.000000000000000000, 0.8660254037844387076, 1.000000000000000000, 0.8660254037844387076, 1.000000000000000000, 0.8660254037844387076, 1.000000000000000000, 0.8660254037844387076, 1.000000000000000000, 0.8660254037844387076, 1.000000000000000000, 0.8660254037844387076, 1.000000000000000000, 0.8660254037844387076, 1.000000000000000000, 0.8660254037844387076, 1.000000000000000000, 0.8660254037844387076, 1.000000000000000000, 0.8660254037844387076, 1.000000000000000000, 0.8660254037844387076, 1.000000000000000000, 0.8660254037844387076, 1.000000000000000000, 0.8660254037844387076, 1.000000000000000000, 0.8660254037844387076, 1.000000000000000000, 0.8660254037844387076, 1.000000000000000000, 0.8660254037844387076, 1.000000000000000000, 0.8660254037844387076, 1.000000000000000000, 0.8660254037844387076, 1.000000000000000000, 0.8660254037844387076, 1.000000000000000000, 0.8660254037844387076, 1.000000000000000000, 0.8660254037844387076, 1.000000000000000000, 0.8660254037844387076, 1.000000000000000000, 0.8660254037844387076, 1.000000000000000000, 0.8660254037844387076, 1.000000000000000000, 0.8660254037844387076, 1.000000000000000000, 0.8660254037844387076, 1.000000000000000000, 0.8660254037844387076, 1.000000000000000000, 0.8660254037844387076, 1.000000000000000000, 0.8660254037844387076, 1.000000000000000000, 0.8660254037844387076, 1.000000000000000000, 0.8660254037844387076, 1.000000000000000000, 0.8660254037844387076, 1.000000000000000000, 0.8660254037844387076, 1.000000000000000000, 0.8660254037844387076, 1.000000000000000000, 0.8660254037844387076, 1.000000000000000000, 0.8660254037844387076, 1.000000000000000000, 0.8660254037844387076, 1.000000000000000000, 0.8660254037844387076, 1.000000000000000000, 0.8660254037844387076, 1.000000000000000000, 0.8660254037844387076, 1.000000000000000000, 0.8660254037844387076, 1.000000000000000000, 0.8660254037844387076, 1.000000000000000000, 0.8660254037844387076, 1.000000000000000000, 0.8660254037844387076, 1.000000000000000000, 0.8660254037844387076, 1.000000000000000000, 0.8660254037844387076, 1.000000000000000000, 0.8660254037844387076, 1.000000000000000000, 0.8660254037844387076, 1.000000000000000000, 0.8660254037844387076, 1.000000000000000000, 0.8660254037844387076, 1.000000000000000000, 0.8660254037844387076, 1.000000000000000000, 0.8660254037844387076, 1.000000000000000000, 0.8660254037844387076, 1.000000000000000000, 0.8660254037844387076, 1.000000000000000000, 0.8660254037844387076, 1.000000000000000000, 0.8660254037844387076, 1.000000000000000000, 0.8660254037844387076, 1.000000000000000000, 0.8660254037844387076, 1.000000000000000000, 0.8660254037844387076, 1.000000000000000000, 0.8660254037844387076, 1.000000000000000000, 0.8660254037844387076, 1.000000000000000000, 0.8660254037844387076, 1.000000000000000000, 0.8660254037844387076, 1.000000000000000000, 0.8660254037844387076, 1.000000000000000000, 0.8660254037844387076, 1.000000000000000000, 0.8660254037844387076, 1.000000000000000000, 0.8660254037844387076, 1.000000000000000000, 0.8660254037844387076, 1.000000000000000000, 0.8660254037844387076, 1.000000000000000000, 0.8660254037844387076, 1.000000000000000000, 0.8660254037844387076, 1.000000000000000000, 0.8660254037844387076, 1.000000000000000000, 0.8660254037844387076, 1.000000000000000000, 0.8660254037844387076, 1.000000000000000000, 0.8660254037844387076, 1.000000000000000000, 0.8660254037844387076, 1.000000000000000000, 0.8660254037844387076, 1.000000000000000000, 0.8660254037844387076, 1.000000000000000000, 0.8660254037844387076, 1.000000000000000000, 0.8660254037844387076, 1.000000000000000000, 0.8660254037844387076, 1.000000000000000000, 0.8660254037844387076, 1.000000000000000000, 0.8660254037844387076, 1.000000000000000000, 0.8660254037844387076, 1.000000000000000000, 0.8660254037844387076, 1.000000000000000000, 0.8660254037844387076, 1.000000000000000000, 0.8660254037844387076, 1.000000000000000000, 0.8660254037844387076, 1.000000000000000000, 0.8660254037844387076, 1.000000000000000000, 0.8660254037844387076, 1.000000000000000000, 0.8660254037844387076, 1.000000000000000000, 0.8660254037844387076, 1.000000000000000000, 0.8660254037844387076, 1.000000000000000000, 0.8660254037844387076, 1.000000000000000000, 0.8660254037844387076, 1.000000000000000000, 0.8660254037844387076, 1.000000000000000000, 0.8660254037844387076, 1.000000000000000000, 0.8660254037844387076, 1.000000000000000000, 0.8660254037844387076, 1.000000000000000000, 0.8660254037844387076, 1.000000000000000000, 0.8660254037844387076, 1.000000000000000000, 0.8660254037844387076, 1.000000000000000000, 0.8660254037844387076, 1.000000000000000000, 0.8660254037844387076, 1.000000000000000000, 0.8660254037844387076, 1.000000000000000000, 0.8660254037844387076, 1.000000000000000000, 0.8660254037844387076, 1.000000000000000000, 0.8660254037844387076, 1.000000000000000000, 0.8660254037844387076, 1.000000000000000000, 0.8660254037844387076, 1.000000000000000000, 0.8660254037844387076, 1.000000000000000000, 0.8660254037844387076, 1.000000000000000000, 0.8660254037844387076, 1.000000000000000000, 0.8660254037844387076, 1.000000000000000000, 0.8660254037844387076, 1.000000000000000000, 0.8660254037844387076, 1.000000000000000000, 0.8660254037844387076, 1.000000000000000000, 0.8660254037844387076, 1.000000000000000000, 0.8660254037844387076, 1.000000000000000000, 0.8660254037844387076, 1.000000000000000000, 0.8660254037844387076, 1.000000000000000000, 0.8660254037844387076, 1.000000000000000000, 0.8660254037844387076, 1.000000000000000000, 0.8660254037844387076, 1.000000000000000000, 0.8660254037844387076, 1.000000000000000000, 0.8660254037844387076, 1.000000000000000000, 0.8660254037844387076, 1.000000000000000000, 0.8660254037844387076, 1.000000000000000000, 0.8660254037844387076, 1.000000000000000000, 0.8660254037844387076, 1.000000000000000000, 0.8660254037844387076, 1.000000000000000000, 0.8660254037844387076, 1.000000000000000000, 0.8660254037844387076, 1.000000000000000000, 0.8660254037844387076, 1.000000000000000000, 0.8660254037844387076, 1.000000000000000000, 0.8660254037844387076, 1.000000000000000000, 0.8660254037844387076, 1.000000000000000000, 0.8660254037844387076, 1.000000000000000000, 0.8660254037844387076, 1.000000000000000000, 0.8660254037844387076, 1.000000000000000000, 0.8660254037844387076, 1.000000000000000000, 0.8660254037844387076, 1.000000000000000000, 0.8660254037844387076, 1.000000000000000000, 0.8660254037844387076, 1.000000000000000000, 0.8660254037844387076, 1.000000000000000000, 0.8660254037844387076, 1.000000000000000000, 0.8660254037844387076, 1.000000000000000000, 0.8660254037844387076, 1.000000000000000000, 0.8660254037844387076, 1.000000000000000000, 0.8660254037844387076, 1.000000000000000000, 0.8660254037844387076, 1.000000000000000000, 0.8660254037844387076, 1.000000000000000000, 0.8660254037844387076, 1.000000000000000000, 0.8660254037844387076, 1.000000000000000000, 0.8660254037844387076, 1.000000000000000000, 0.8660254037844387076, 1.000000000000000000, 0.8660254037844387076, 1.000000000000000000, 0.8660254037844387076, 1.000000000000000000, 0.8660254037844387076, 1.000000000000000000, 0.8660254037844387076, 1.000000000000000000, 0.8660254037844387076, 1.000000000000000000, 0.8660254037844387076, 1.000000000000000000, 0.8660254037844387076, 1.000000000000000000, 0.8660254037844387076, 1.000000000000000000, 0.8660254037844387076, 1.000000000000000000, 0.8660254037844387076, 1.000000000000000000, 0.8660254037844387076, 1.000000000000000000, 0.8660254037844387076, 1.000000000000000000, 0.8660254037844387076, 1.000000000000000000, 0.8660254037844387076, 1.000000000000000000, 0.8660254037844387076, 1.000000000000000000, 0.8660254037844387076, 1.000000000000000000, 0.8660254037844387076, 1.000000000000000000, 0.8660254037844387076, 1.000000000000000000, 0.8660254037844387076, 1.000000000000000000, 0.8660254037844387076, 1.000000000000000000, 0.8660254037844387076, 1.000000000000000000, 0.8660254037844387076, 1.000000000000000000, 0.8660254037844387076, 1.000000000000000000, 0.8660254037844387076, 1.000000000000000000, 0.8660254037844387076, 1.000000000000000000, 0.8660254037844387076, 1.000000000000000000, 0.8660254037844387076, 1.000000000000000000, 0.8660254037844387076, 1.000000000000000000, 0.8660254037844387076, 1.000000000000000000, 0.8660254037844387076, 1.000000000000000000, 0.8660254037844387076, 1.000000000000000000, 0.8660254037844387076, 1.000000000000000000, 0.8660254037844387076, 1.000000000000000000, 0.8660254037844387076, 1.000000000000000000, 0.8660254037844387076, 1.000000000000000000, 0.8660254037844387076, 1.000000000000000000, 0.8660254037844387076, 1.000000000000000000, 0.8660254037844387076, 1.000000000000000000, 0.8660254037844387076, 1.000000000000000000, 0.8660254037844387076, 1.000000000000000000, 0.8660254037844387076, 1.000000000000000000, 0.8660254037844387076, 1.000000000000000000, 0.8660254037844387076, 1.000000000000000000, 0.8660254037844387076, 1.000000000000000000, 0.8660254037844387076, 1.000000000000000000, 0.8660254037844387076, 1.000000000000000000, 0.8660254037844387076, 1.000000000000000000, 0.8660254037844387076, 1.000000000000000000, 0.8660254037844387076, 1.000000000000000000, 0.8660254037844387076, 1.000000000000000000, 0.8660254037844387076, 1.000000000000000000, 0.8660254037844387076, 1.000000000000000000, 0.8660254037844387076, 1.000000000000000000, 0.8660254037844387076, 1.000000000000000000, 0.8660254037844387076, 1.000000000000000000, 0.8660254037844387076, 1.000000000000000000, 0.8660254037844387076, 1.000000000000000000, 0.8660254037844387076, 1.000000000000000000, 0.8660254037844387076, 1.000000000000000000, 0.8660254037844387076, 1.000000000000000000, 0.8660254037844387076, 1.000000000000000000, 0.8660254037844387076, 1.000000000000000000, 0.8660254037844387076, 1.000000000000000000, 0.8660254037844387076, 1.000000000000000000, 0.8660254037844387076, 1.000000000000000000, 0.8660254037844387076, 1.000000000000000000, 0.8660254037844387076, 1.000000000000000000, 0.8660254037844387076, 1.000000000000000000, 0.8660254037844387076, 1.000000000000000000, 0.8660254037844387076, 1.000000000000000000, 0.8660254037844387076, 1.000000000000000000, 0.8660254037844387076, 1.000000000000000000, 0.8660254037844387076, 1.000000000000000000, 0.8660254037844387076, 1.000000000000000000, 0.8660254037844387076, 1.000000000000000000, 0.8660254037844387076, 1.000000000000000000, 0.8660254037844387076, 1.000000000000000000, 0.8660254037844387076, 1.000000000000000000, 0.8660254037844387076, 1.000000000000000000, 0.8660254037844387076, 1.000000000000000000, 0.8660254037844387076, 1.000000000000000000, 0.8660254037844387076, 1.000000000000000000, 0.8660254037844387076, 1.000000000000000000, 0.8660254037844387076, 1.000000000000000000, 0.8660254037844387076, 1.000000000000000000, 0.8660254037844387076, 1.000000000000000000, 0.8660254037844387076, 1.000000000000000000, 0.8660254037844387076, 1.000000000000000000, 0.8660254037844387076, 1.000000000000000000, 0.8660254037844387076, 1.000000000000000000, 0.8660254037844387076, 1.000000000000000000, 0.8660254037844387076, 1.000000000000000000, 0.8660254037844387076, 1.000000000000000000, 0.8660254037844387076, 1.000000000000000000, 0.8660254037844387076, 1.000000000000000000, 0.8660254037844387076, 1.000000000000000000, 0.8660254037844387076, 1.000000000000000000, 0.8660254037844387076, 1.000000000000000000, 0.8660254037844387076, 1.000000000000000000, 0.8660254037844387076, 1.000000000000000000, 0.8660254037844387076, 1.000000000000000000, 0.8660254037844387076, 1.000000000000000000, 0.8660254037844387076, 1.000000000000000000, 0.8660254037844387076, 1.000000000000000000, 0.8660254037844387076, 1.000000000000000000, 0.8660254037844387076, 1.000000000000000000, 0.8660254037844387076, 1.000000000000000000, 0.8660254037844387076, 1.000000000000000000, 0.8660254037844387076, 1.000000000000000000, 0.8660254037844387076, 1.000000000000000000, 0.8660254037844387076, 1.000000000000000000, 0.8660254037844387076, 1.000000000000000000, 0.8660254037844387076, 1.000000000000000000, 0.8660254037844387076, 1.000000000000000000, 0.8660254037844387076, 1.000000000000000000, 0.8660254037844387076, 1.000000000000000000, 0.8660254037844387076, 1.000000000000000000, 0.8660254037844387076, 1.000000000000000000, 0.8660254037844387076, 1.000000000000000000, 0.8660254037844387076, 1.000000000000000000, 0.8660254037844387076, 1.000000000000000000, 0.8660254037844387076, 1.000000000000000000, 0.8660254037844387076, 1.000000000000000000, 0.8660254037844387076, 1.000000000000000000, 0.8660254037844387076, 1.000000000000000000, 0.8660254037844387076, 1.000000000000000000, 0.8660254037844387076, 1.000000000000000000, 0.8660254037844387076, 1.000000000000000000, 0.8660254037844387076, 1.000000000000000000, 0.8660254037844387076, 1.000000000000000000, 0.8660254037844387076, 1.000000000000000000, 0.8660254037844387076, 1.000000000000000000, 0.8660254037844387076, 1.000000000000000000, 0.8660254037844387076, 1.000000000000000000, 0.8660254037844387076, 1.000000000000000000, 0.8660254037844387076, 1.000000000000000000, 0.8660254037844387076, 1.000000000000000000, 0.8660254037844387076, 1.000000000000000000, 0.8660254037844387076, 1.000000000000000000, 0.8660254037844387076, 1.000000000000000000, 0.8660254037844387076, 1.000000000000000000, 0.8660254037844387076, 1.000000000000000000, 0.8660254037844387076, 1.000000000000000000, 0.8660254037844387076, 1.000000000000000000, 0.8660254037844387076, 1.000000000000000000, 0.8660254037844387076, 1.000000000000000000, 0.8660254037844387076, 1.000000000000000000, 0.8660254037844387076, 1.000000000000000000, 0.8660254037844387076, 1.000000000000000000, 0.8660254037844387076, 1.000000000000000000, 0.8660254037844387076, 1.000000000000000000, 0.8660254037844387076, 1.000000000000000000, 0.8660254037844387076, 1.000000000000000000, 0.8660254037844387076, 1.000000000000000000, 0.8660254037844387076, 1.000000000000000000, 0.8660254037844387076, 1.000000000000000000, 0.8660254037844387076, 1.000000000000000000, 0.8660254037844387076, 1.000000000000000000, 0.8660254037844387076, 1.000000000000000000, 0.8660254037844387076, 1.000000000000000000, 0.8660254037844387076, 1.000000000000000000, 0.8660254037844387076, 1.000000000000000000, 0.8660254037844387076, 1.000000000000000000, 0.8660254037844387076, 1.000000000000000000, 0.8660254037844387076, 1.000000000000000000, 0.8660254037844387076, 1.000000000000000000, 0.8660254037844387076, 1.000000000000000000, 0.8660254037844387076, 1.000000000000000000, 0.8660254037844387076, 1.000000000000000000, 0.8660254037844387076, 1.000000000000000000, 0.8660254037844387076, 1.000000000000000000, 0.8660254037844387076, 1.000000000000000000, 0.8660254037844387076, 1.000000000000000000, 0.8660254037844387076, 1.000000000000000000, 0.8660254037844387076, 1.000000000000000000, 0.8660254037844387076, 1.000000000000000000, 0.8660254037844387076, 1.000000000000000000, 0.8660254037844387076, 1.000000000000000000, 0.8660254037844387076, 1.000000000000000000, 0.8660254037844387076, 1.000000000000000000, 0.8660254037844387076, 1.000000000000000000, 0.8660254037844387076, 1.000000000000000000, 0.8660254037844387076, 1.000000000000000000, 0.8660254037844387076, 1.000000000000000000, 0.8660254037844387076, 1.000000000000000000, 0.8660254037844387076, 1.000000000000000000, 0.8660254037844387076, 1.000000000000000000, 0.8660254037844387076, 1.000000000000000000, 0.8660254037844387076, 1.000000000000000000, 0.8660254037844387076, 1.000000000000000000, 0.8660254037844387076, 1.000000000000000000, 0.8660254037844387076, 1.000000000000000000, 0.8660254037844387076, 1.000000000000000000, 0.8660254037844387076, 1.000000000000000000, 0.8660254037844387076, 1.000000000000000000, 0.8660254037844387076, 1.000000000000000000, 0.8660254037844387076, 1.000000000000000000, 0.8660254037844387076, 1.000000000000000000, 0.8660254037844387076, 1.000000000000000000, 0.8660254037844387076, 1.000000000000000000, 0.8660254037844387076, 1.000000000000000000, 0.8660254037844387076, 1.000000000000000000, 0.8660254037844387076, 1.000000000000000000, 0.8660254037844387076, 1.000000000000000000, 0.8660254037844387076, 1.000000000000000000, 0.8660254037844387076, 1.000000000000000000, 0.8660254037844387076, 1.000000000000000000, 0.8660254037844387076, 1.000000000000000000, 0.8660254037844387076, 1.000000000000000000, 0.8660254037844387076, 1.000000000000000000, 0.8660254037844387076, 1.000000000000000000, 0.8660254037844387076, 1.000000000000000000, 0.8660254037844387076, 1.000000000000000000, 0.8660254037844387076, 1.000000000000000000, 0.8660254037844387076, 1.000000000000000000, 0.8660254037844387076, 1.000000000000000000, 0.8660254037844387076, 1.000000000000000000, 0.8660254037844387076, 1.000000000000000000, 0.8660254037844387076, 1.000000000000000000, 0.8660254037844387076, 1.000000000000000000, 0.8660254037844387076, 1.000000000000000000, 0.8660254037844387076, 1.000000000000000000, 0.8660254037844387076, 1.000000000000000000, 0.8660254037844387076, 1.000000000000000000, 0.8660254037844387076, 1.000000000000000000, 0.8660254037844387076, 1.000000000000000000, 0.8660254037844387076, 1.000000000000000000, 0.8660254037844387076, 1.000000000000000000, 0.8660254037844387076, 1.000000000000000000, 0.8660254037844387076, 1.000000000000000000, 0.8660254037844387076, 1.000000000000000000, 0.8660254037844387076, 1.000000000000000000, 0.8660254037844387076, 1.000000000000000000, 0.8660254037844387076, 1.000000000000000000, 0.8660254037844387076, 1.000000000000000000, 0.8660254037844387076, 1.000000000000000000, 0.8660254037844387076, 1.000000000000000000, 0.8660254037844387076, 1.000000000000000000, 0.8660254037844387076, 1.000000000000000000, 0.8660254037844387076, 1.000000000000000000, 0.8660254037844387076, 1.000000000000000000, 0.8660254037844387076, 1.000000000000000000, 0.8660254037844387076, 1.000000000000000000, 0.8660254037844387076, 1.000000000000000000, 0.8660254037844387076, 1.000000000000000000, 0.8660254037844387076, 1.000000000000000000, 0.8660254037844387076, 1.000000000000000000, 0.8660254037844387076, 1.000000000000000000, 0.8660254037844387076, 1.000000000000000000, 0.8660254037844387076, 1.000000000000000000, 0.8660254037844387076, 1.000000000000000000, 0.8660254037844387076, 1.000000000000000000, 0.8660254037844387076, 1.000000000000000000, 0.8660254037844387076, 1.000000000000000000, 0.8660254037844387076, 1.000000000000000000, 0.8660254037844387076, 1.000000000000000000, 0.8660254037844387076, 1.000000000000000000, 0.8660254037844387076, 1.000000000000000000, 0.8660254037844387076, 1.000000000000000000, 0.8660254037844387076, 1.000000000000000000, 0.8660254037844387076, 1.000000000000000000, 0.8660254037844387076, 1.000000000000000000, 0.8660254037844387076, 1.000000000000000000, 0.8660254037844387076, 1.000000000000000000, 0.8660254037844387076, 1.000000000000000000, 0.8660254037844387076, 1.000000000000000000, 0.8660254037844387076, 1.000000000000000000, 0.8660254037844387076, 1.000000000000000000, 0.8660254037844387076, 1.000000000000000000, 0.8660254037844387076, 1.000000000000000000, 0.8660254037844387076, 1.000000000000000000, 0.8660254037844387076, 1.000000000000000000, 0.8660254037844387076, 1.000000000000000000, 0.8660254037844387076, 1.000000000000000000, 0.8660254037844387076, 1.000000000000000000, 0.8660254037844387076, 1.000000000000000000, 0.8660254037844387076, 1.000000000000000000, 0.8660254037844387076, 1.000000000000000000, 0.8660254037844387076, 1.000000000000000000, 0.8660254037844387076, 1.000000000000000000, 0.8660254037844387076, 1.000000000000000000, 0.8660254037844387076, 1.000000000000000000, 0.8660254037844387076, 1.000000000000000000, 0.8660254037844387076, 1.000000000000000000, 0.8660254037844387076, 1.000000000000000000, 0.8660254037844387076, 1.000000000000000000, 0.8660254037844387076, 1.000000000000000000, 0.8660254037844387076, 1.000000000000000000, 0.8660254037844387076, 1.000000000000000000, 0.8660254037844387076, 1.000000000000000000, 0.8660254037844387076, 1.000000000000000000) ) ) 
 REPRESENTATION_ITEM ( '' )  SURFACE ( )  );
#43812 = CARTESIAN_POINT ( 'NONE',  ( -58.24261429053147765, -155.0000000000000284, -3.805975901505573411 ) ) ;
#43813 = CARTESIAN_POINT ( 'NONE',  ( -4.458734124999998549, -61.47916666530107221, 2.574251347313722516 ) ) ;
#43814 = CARTESIAN_POINT ( 'NONE',  ( 4.458734125000001214, 0.8541666680322613781, 2.574251347313718519 ) ) ;
#43815 = VERTEX_POINT ( 'NONE', #13861 ) ;
#43816 = FACE_OUTER_BOUND ( 'NONE', #29368, .T. ) ;
#43817 = CARTESIAN_POINT ( 'NONE',  ( -2.500000000000000444, 28.95833333606451987, -4.330127018922193649 ) ) ;
#43818 = CARTESIAN_POINT ( 'NONE',  ( -4.458734124999999437, 10.60416666803225993, -2.574251347313719407 ) ) ;
#43819 = CARTESIAN_POINT ( 'NONE',  ( -57.89159099828107458, -146.6875000013656063, -3.393966926194107447 ) ) ;
#43820 = CARTESIAN_POINT ( 'NONE',  ( -2.499999999999996447, 6.291666669397851130, 4.330127018922195425 ) ) ;
#43821 = CARTESIAN_POINT ( 'NONE',  ( 4.458734124999997661, -165.5000000013655779, 1.846868145590737864 ) ) ;
#43822 = CONICAL_SURFACE ( 'NONE', #31541, 7.500000000000001776, 0.8594454914424796144 ) ;
#43823 = VERTEX_POINT ( 'NONE', #34414 ) ;
#43824 = CARTESIAN_POINT ( 'NONE',  ( 4.458734125000000326, -74.89583333196773651, 2.574251347313718519 ) ) ;
#43825 = CARTESIAN_POINT ( 'NONE',  ( 1.339745962155612702, -0.1696581960073343942, -5.000000000000000000 ) ) ;
#43826 = CARTESIAN_POINT ( 'NONE',  ( 2.229367062500001939, 4.020833334698926009, 3.861377020970579999 ) ) ;
#43827 = CARTESIAN_POINT ( 'NONE',  ( 3.061616997868383141E-16, -162.8750000027311842, -5.000000000000000000 ) ) ;
#43828 = CARTESIAN_POINT ( 'NONE',  ( -4.458734124999999437, -65.64583333196773651, -2.574251347313719407 ) ) ;
#43829 = CARTESIAN_POINT ( 'NONE',  ( -5.000000000000000000, -26.95833333060214798, -2.886751345948128211 ) ) ;
#43830 = CARTESIAN_POINT ( 'NONE',  ( 1.975475456537005874E-15, -20.74999999999999645, 5.000000000000000000 ) ) ;
#43831 = DIRECTION ( 'NONE',  ( -0.000000000000000000, 1.000000000000000000, -0.000000000000000000 ) ) ;
#43832 = CARTESIAN_POINT ( 'NONE',  ( 5.000000000000000000, -58.41666666666665719, -2.886751345948130876 ) ) ;
#43833 = CARTESIAN_POINT ( 'NONE',  ( 4.458734124999999437, -43.81249999863440081, -5.460374474430324690E-16 ) ) ;
#43834 = CARTESIAN_POINT ( 'NONE',  ( -4.458734124999999437, -26.56249999863440792, 0.000000000000000000 ) ) ;
#43835 = CARTESIAN_POINT ( 'NONE',  ( -4.458734124999999437, 7.437500001365594748, 0.000000000000000000 ) ) ;
#43836 = CARTESIAN_POINT ( 'NONE',  ( -53.33387254593719717, -143.8125000000000284, 5.149110718188530278 ) ) ;
#43837 = CARTESIAN_POINT ( 'NONE',  ( -4.999999999999999112, 26.08333333333333215, 2.886751345948131764 ) ) ;
#43838 = CARTESIAN_POINT ( 'NONE',  ( 5.000000000000000000, -151.1250000027312126, 0.000000000000000000 ) ) ;
#43839 = CARTESIAN_POINT ( 'NONE',  ( 5.000000000000000000, -54.37499999726880162, -6.123233995736766282E-16 ) ) ;
#43840 = CARTESIAN_POINT ( 'NONE',  ( 2.229367062500001939, -38.97916666530107221, 3.861377020970579999 ) ) ;
#43841 = CARTESIAN_POINT ( 'NONE',  ( -5.000000000000000000, -70.95833333060214443, -2.886751345948128211 ) ) ;
#43842 = CARTESIAN_POINT ( 'NONE',  ( -57.89159099828107458, -147.9375000013656063, -3.393966926194107447 ) ) ;
#43843 = CARTESIAN_POINT ( 'NONE',  ( 5.000000000000000000, -144.0000000000000284, 0.000000000000000000 ) ) ;
#43844 = CARTESIAN_POINT ( 'NONE',  ( -4.458734124999997661, -73.47916666530106511, 2.574251347313722516 ) ) ;
#43845 = CARTESIAN_POINT ( 'NONE',  ( 4.458734124999999437, -166.6250000013656063, -1.846868145590734978 ) ) ;
#43846 = CARTESIAN_POINT ( 'NONE',  ( 2.229367062500001939, -30.97916666530107221, 3.861377020970579999 ) ) ;
#43847 = CARTESIAN_POINT ( 'NONE',  ( -58.24261429053147765, -148.2500000000000284, -3.805975901505573855 ) ) ;
#43848 = FACE_OUTER_BOUND ( 'NONE', #58067, .T. ) ;
#43849 = CARTESIAN_POINT ( 'NONE',  ( -4.999999999999999112, -21.91666666666666785, 2.886751345948131764 ) ) ;
#43850 = CARTESIAN_POINT ( 'NONE',  ( -1.846868145590734756, -144.1250000013655779, -4.458734125000000326 ) ) ;
#43851 = ORIENTED_EDGE ( 'NONE', *, *, #6070, .T. ) ;
#43852 = CARTESIAN_POINT ( 'NONE',  ( 4.458734124999999437, 25.93750000136559564, -5.460374474430324690E-16 ) ) ;
#43853 = CARTESIAN_POINT ( 'NONE',  ( 5.000000000000000000, -16.29166666393548368, -2.886751345948130876 ) ) ;
#43854 = CARTESIAN_POINT ( 'NONE',  ( -4.458734124999999437, -57.64583333196773651, -2.574251347313719407 ) ) ;
#43855 = CARTESIAN_POINT ( 'NONE',  ( 5.000000000000000888, 28.54166666939785202, 2.886751345948126879 ) ) ;
#43856 = LINE ( 'NONE', #39039, #24738 ) ;
#43857 = CARTESIAN_POINT ( 'NONE',  ( 5.000000000000000000, 18.58333333333333215, -2.886751345948129988 ) ) ;
#43858 = CARTESIAN_POINT ( 'NONE',  ( -2.500000000000000444, 7.958333336064518093, -4.330127018922193649 ) ) ;
#43859 = CARTESIAN_POINT ( 'NONE',  ( -2.229367062500000163, -6.479166665301072214, -3.861377020970580443 ) ) ;
#43860 = CARTESIAN_POINT ( 'NONE',  ( -6.031010364368858512E-14, 4.249999999999995559, 5.000000000000000000 ) ) ;
#43861 = CYLINDRICAL_SURFACE ( 'NONE', #61542, 5.000000000000000000 ) ;
#43862 = CARTESIAN_POINT ( 'NONE',  ( 5.000000000000000888, -89.45833333060215864, 2.886751345948126879 ) ) ;
#43863 = CARTESIAN_POINT ( 'NONE',  ( 1.339745962155615144, -12.70534180126147739, 4.999999999999999112 ) ) ;
#43864 = CARTESIAN_POINT ( 'NONE',  ( -4.458734124999999437, -21.31249999863440436, 0.000000000000000000 ) ) ;
#43865 = CARTESIAN_POINT ( 'NONE',  ( 1.975475456537005874E-15, 10.37500000273118417, 5.000000000000000000 ) ) ;
#43866 = CARTESIAN_POINT ( 'NONE',  ( 2.229367062499998831, -51.64583333196773651, -3.861377020970580887 ) ) ;
#43867 = CARTESIAN_POINT ( 'NONE',  ( 2.730187237215162345E-16, -157.4375000013655779, -4.458734124999999437 ) ) ;
#43868 = VECTOR ( 'NONE', #35104, 1000.000000000000000 ) ;
#43869 = CARTESIAN_POINT ( 'NONE',  ( -3.535250795749689387E-16, -51.12499999726880873, -5.773502691896257311 ) ) ;
#43870 = VERTEX_POINT ( 'NONE', #29593 ) ;
#43871 = VECTOR ( 'NONE', #25662, 1000.000000000000114 ) ;
#43872 = CARTESIAN_POINT ( 'NONE',  ( -4.458734124999999437, 5.437500001365592972, 0.000000000000000000 ) ) ;
#43873 = ORIENTED_EDGE ( 'NONE', *, *, #16216, .F. ) ;
#43875 = CARTESIAN_POINT ( 'NONE',  ( -1.339745962155610925, -2.794658198738521726, 5.000000000000000000 ) ) ;
#43874 = CARTESIAN_POINT ( 'NONE',  ( 5.000000000000000000, -87.41666666666667140, -2.886751345948130876 ) ) ;
#43876 = CARTESIAN_POINT ( 'NONE',  ( -1.846868145590737420, -158.7500000013656063, 4.458734124999999437 ) ) ;
#43877 = ORIENTED_EDGE ( 'NONE', *, *, #14917, .F. ) ;
#43878 = LINE ( 'NONE', #9475, #9766 ) ;
#43879 = CARTESIAN_POINT ( 'NONE',  ( -53.33387254593733928, -134.8125000000000568, 5.149110718188519620 ) ) ;
#43880 = DIRECTION ( 'NONE',  ( 0.000000000000000000, 0.000000000000000000, 1.000000000000000000 ) ) ;
#43881 = CARTESIAN_POINT ( 'NONE',  ( 4.458734124999998549, -40.97916666530107932, -2.574251347313721627 ) ) ;
#43882 = ORIENTED_EDGE ( 'NONE', *, *, #42575, .T. ) ;
#43883 = CARTESIAN_POINT ( 'NONE',  ( -4.999999999999998224, -45.91666666666665719, 2.886751345948131764 ) ) ;
#43884 = CARTESIAN_POINT ( 'NONE',  ( 4.458734124999998549, 21.27083333469892779, -2.574251347313721627 ) ) ;
#43885 = CARTESIAN_POINT ( 'NONE',  ( 0.000000000000000000, -120.0000000000000000, 0.000000000000000000 ) ) ;
#43886 = ORIENTED_EDGE ( 'NONE', *, *, #7213, .T. ) ;
#43887 = CARTESIAN_POINT ( 'NONE',  ( 4.458734124999998549, 29.27083333469892423, -2.574251347313721627 ) ) ;
#43888 = CARTESIAN_POINT ( 'NONE',  ( -50.01589407740564042, -126.7500000027312126, 0.3983568153799778022 ) ) ;
#43889 = CARTESIAN_POINT ( 'NONE',  ( 5.000000000000000888, -88.58333333333332860, 2.886751345948126879 ) ) ;
#43890 = CARTESIAN_POINT ( 'NONE',  ( -50.44383482147011222, -135.0000000000000000, 0.1418284928502891451 ) ) ;
#43891 = CARTESIAN_POINT ( 'NONE',  ( 5.000000000000000888, -168.9375000000000284, -2.071067811865475505 ) ) ;
#43892 = CARTESIAN_POINT ( 'NONE',  ( 2.229367062499998831, -59.64583333196774362, -3.861377020970580887 ) ) ;
#43893 = CARTESIAN_POINT ( 'NONE',  ( 7.847095227763521308, 4.129731495738485414, -7.493596212620238894 ) ) ;
#43894 = CARTESIAN_POINT ( 'NONE',  ( -4.458734124999999437, 19.68750000136559208, 0.000000000000000000 ) ) ;
#43895 = ADVANCED_FACE ( 'NONE', ( #58245 ), #54043, .T. ) ;
#43896 =( BOUNDED_CURVE ( )  B_SPLINE_CURVE ( 2, ( #20362, #25497, #11017, #39639, #11335, #39960, #35475, #59931, #21000 ),
 .UNSPECIFIED., .F., .F. ) 
 B_SPLINE_CURVE_WITH_KNOTS ( ( 3, 2, 2, 2, 3 ),
 ( 0.3196428571428571175, 0.3202380952380952106, 0.3214285714285714524, 0.3226190476190476386, 0.3232142857142857317 ),
 .UNSPECIFIED. ) 
 CURVE ( )  GEOMETRIC_REPRESENTATION_ITEM ( )  RATIONAL_B_SPLINE_CURVE ( ( 0.9330127018922194093, 0.9330127018922194093, 1.000000000000000000, 0.8660254037844387076, 1.000000000000000000, 0.8660254037844387076, 1.000000000000000000, 0.9330127018922194093, 0.9330127018922194093 ) ) 
 REPRESENTATION_ITEM ( '' )  );
#43897 = CARTESIAN_POINT ( 'NONE',  ( -7.500000000000000000, -4.330127018922198090, -7.422398894150034288 ) ) ;
#43898 = CARTESIAN_POINT ( 'NONE',  ( 4.458734124999999437, -51.06249999863440792, -5.460374474430324690E-16 ) ) ;
#43899 = CARTESIAN_POINT ( 'NONE',  ( 5.000000000000000000, -9.374999997268814056, -6.123233995736766282E-16 ) ) ;
#43900 = CARTESIAN_POINT ( 'NONE',  ( -6.972266317189433020E-16, -31.24999999999999645, -5.000000000000000000 ) ) ;
#43901 = CARTESIAN_POINT ( 'NONE',  ( -2.499999999999996447, -66.70833333060214443, 4.330127018922195425 ) ) ;
#43902 = CARTESIAN_POINT ( 'NONE',  ( 2.229367062499998831, -88.89583333196773651, -3.861377020970580887 ) ) ;
#43903 = CARTESIAN_POINT ( 'NONE',  ( -2.229367062499996610, -107.1458333319677365, 3.861377020970582219 ) ) ;
#43904 = CARTESIAN_POINT ( 'NONE',  ( -2.229367062499996610, -9.395833331967736513, 3.861377020970582219 ) ) ;
#43905 = ORIENTED_EDGE ( 'NONE', *, *, #53448, .T. ) ;
#43906 = VECTOR ( 'NONE', #15928, 1000.000000000000000 ) ;
#43907 = CARTESIAN_POINT ( 'NONE',  ( -2.500000000000000444, 17.95833333606451632, -4.330127018922193649 ) ) ;
#43908 = CARTESIAN_POINT ( 'NONE',  ( -2.229367062499996610, -101.1458333319677365, 3.861377020970582219 ) ) ;
#43909 = CARTESIAN_POINT ( 'NONE',  ( -9.184850993605147944E-16, -160.3750000027311842, 5.000000000000000000 ) ) ;
#43910 = CARTESIAN_POINT ( 'NONE',  ( -4.458734124999999437, -97.56249999863440792, 0.000000000000000000 ) ) ;
#43911 = AXIS2_PLACEMENT_3D ( 'NONE', #33250, #52870, #13631 ) ;
#43912 = CARTESIAN_POINT ( 'NONE',  ( -5.000000000000000000, 22.00000000000000000, 0.000000000000000000 ) ) ;
#43913 = CARTESIAN_POINT ( 'NONE',  ( 2.499999999999998668, -51.20833333060213732, -4.330127018922193649 ) ) ;
#43914 = CARTESIAN_POINT ( 'NONE',  ( 3.061616997868383141E-16, -152.7500000000000000, -5.000000000000000000 ) ) ;
#43915 = CARTESIAN_POINT ( 'NONE',  ( -52.80376928212989185, -130.8750000013656063, -4.297418129356379346 ) ) ;
#43916 = EDGE_CURVE ( 'NONE', #14179, #50022, #50933, .T. ) ;
#43917 = CARTESIAN_POINT ( 'NONE',  ( -50.55543936806279248, -146.0625000013656063, 0.3552334253322060320 ) ) ;
#43918 = CARTESIAN_POINT ( 'NONE',  ( -3.152548672688508926E-16, -18.56249999863440792, -5.148502694627439702 ) ) ;
#43919 = CARTESIAN_POINT ( 'NONE',  ( -2.229367062499996610, 9.604166668032261711, 3.861377020970582219 ) ) ;
#43920 = CARTESIAN_POINT ( 'NONE',  ( -2.229367062500000163, -57.72916666530107932, -3.861377020970580443 ) ) ;
#43921 = CARTESIAN_POINT ( 'NONE',  ( -5.000000000000000000, -54.08333333333332860, -2.886751345948128211 ) ) ;
#43922 = CARTESIAN_POINT ( 'NONE',  ( -4.458734124999999437, -16.39583333196773651, -2.574251347313719407 ) ) ;
#43923 = DIRECTION ( 'NONE',  ( -0.000000000000000000, 1.000000000000000000, -0.000000000000000000 ) ) ;
#43924 = CARTESIAN_POINT ( 'NONE',  ( -5.000000000000000888, -153.4375000000000000, 2.071067811865474617 ) ) ;
#43925 = CARTESIAN_POINT ( 'NONE',  ( 5.000000000000000000, -5.499999999999998224, -6.123233995736766282E-16 ) ) ;
#43926 = EDGE_LOOP ( 'NONE', ( #58475, #59197, #10833, #17800 ) ) ;
#43927 = CARTESIAN_POINT ( 'NONE',  ( 4.458734124999998549, -40.97916666530106511, -2.574251347313721627 ) ) ;
#43928 = CARTESIAN_POINT ( 'NONE',  ( -57.89159099828107458, -125.9375000013656063, -3.393966926194107447 ) ) ;
#43929 = CARTESIAN_POINT ( 'NONE',  ( 0.000000000000000000, -120.0000000000000000, 0.000000000000000000 ) ) ;
#43930 = CARTESIAN_POINT ( 'NONE',  ( 4.458734124999998549, -85.72916666530106511, -2.574251347313721627 ) ) ;
#43931 = CARTESIAN_POINT ( 'NONE',  ( -4.458734124999999437, 21.35416666803225993, -2.574251347313719407 ) ) ;
#43932 = VECTOR ( 'NONE', #26430, 1000.000000000000000 ) ;
#43933 = CARTESIAN_POINT ( 'NONE',  ( -2.229367062500000163, 8.520833334698926009, -3.861377020970580443 ) ) ;
#43934 = CARTESIAN_POINT ( 'NONE',  ( 1.975475456537005874E-15, -82.74999999999998579, 5.000000000000000000 ) ) ;
#43935 = CARTESIAN_POINT ( 'NONE',  ( -6.972266317189433020E-16, -69.24999999999998579, -5.000000000000000000 ) ) ;
#43936 = CARTESIAN_POINT ( 'NONE',  ( -4.458734124999999437, -86.56249999863439371, 0.000000000000000000 ) ) ;
#43937 = CARTESIAN_POINT ( 'NONE',  ( -4.458734124999999437, 20.43750000136559208, 0.000000000000000000 ) ) ;
#43938 = CARTESIAN_POINT ( 'NONE',  ( -5.000000000000000000, -77.00000000000000000, 0.000000000000000000 ) ) ;
#43939 = CARTESIAN_POINT ( 'NONE',  ( -5.000000000000000000, 13.12500000273118417, 0.000000000000000000 ) ) ;
#43940 = ORIENTED_EDGE ( 'NONE', *, *, #32893, .T. ) ;
#43941 = DIRECTION ( 'NONE',  ( -0.000000000000000000, 1.000000000000000000, -0.000000000000000000 ) ) ;
#43942 = ORIENTED_EDGE ( 'NONE', *, *, #41414, .T. ) ;
#43944 = CARTESIAN_POINT ( 'NONE',  ( 5.000000000000000000, -33.41666666666666430, -2.886751345948129988 ) ) ;
#43943 = DIRECTION ( 'NONE',  ( 0.000000000000000000, 0.000000000000000000, 1.000000000000000000 ) ) ;
#43945 = CARTESIAN_POINT ( 'NONE',  ( 2.229367062499998831, -36.64583333196773651, -3.861377020970580887 ) ) ;
#43946 = CARTESIAN_POINT ( 'NONE',  ( 2.500000000000002220, -32.54166666393547303, 4.330127018922192761 ) ) ;
#43948 = VERTEX_POINT ( 'NONE', #5164 ) ;
#43947 = CARTESIAN_POINT ( 'NONE',  ( -3.152548672688508926E-16, -65.56249999863440792, -5.148502694627439702 ) ) ;
#43949 = CARTESIAN_POINT ( 'NONE',  ( -59.59170313451811296, -150.7500000013655495, 1.485763867205729394 ) ) ;
#43950 = CARTESIAN_POINT ( 'NONE',  ( 2.229367062500001939, -14.97916666530107399, 3.861377020970579999 ) ) ;
#43952 = ORIENTED_EDGE ( 'NONE', *, *, #54346, .F. ) ;
#43951 = CARTESIAN_POINT ( 'NONE',  ( -2.229367062500000163, -14.72916666530107221, -3.861377020970580443 ) ) ;
#43953 = CARTESIAN_POINT ( 'NONE',  ( 1.060575238724906964E-15, -79.74999999999998579, 5.773502691896257311 ) ) ;
#43954 = CARTESIAN_POINT ( 'NONE',  ( -59.29741812935640155, -136.6250000013656063, -2.196230717870135685 ) ) ;
#43955 = CARTESIAN_POINT ( 'NONE',  ( 4.458734125000001214, -55.14583333196772941, 2.574251347313718519 ) ) ;
#43956 =( BOUNDED_CURVE ( )  B_SPLINE_CURVE ( 2, ( #23473, #8055, #3234, #61772, #14114, #22851, #38556, #33741, #18938 ),
 .UNSPECIFIED., .F., .F. ) 
 B_SPLINE_CURVE_WITH_KNOTS ( ( 3, 2, 2, 2, 3 ),
 ( 0.1916666666666668462, 0.1958333333333334980, 0.2000000000000001776, 0.2041666666666668295, 0.2083333333333335091 ),
 .UNSPECIFIED. ) 
 CURVE ( )  GEOMETRIC_REPRESENTATION_ITEM ( )  RATIONAL_B_SPLINE_CURVE ( ( 0.9999999999999970024, 0.9238795325112897361, 1.000000000000000000, 0.9238795325112867385, 1.000000000000000000, 0.9238795325112867385, 1.000000000000000000, 0.9238795325112837409, 1.000000000000003109 ) ) 
 REPRESENTATION_ITEM ( '' )  );
#43957 = CARTESIAN_POINT ( 'NONE',  ( -4.999999999999999112, -84.79166666393547303, 2.886751345948131764 ) ) ;
#43959 = VERTEX_POINT ( 'NONE', #19315 ) ;
#43958 = DIRECTION ( 'NONE',  ( -0.000000000000000000, 1.000000000000000000, -0.000000000000000000 ) ) ;
#43960 = CARTESIAN_POINT ( 'NONE',  ( -50.01589407740564042, -146.6250000000000284, 0.3983568153799778022 ) ) ;
#43961 = AXIS2_PLACEMENT_3D ( 'NONE', #13985, #57446, #33615 ) ;
#43962 = CARTESIAN_POINT ( 'NONE',  ( -3.152548672688508926E-16, -28.81249999863440436, -5.148502694627439702 ) ) ;
#43963 = ORIENTED_EDGE ( 'NONE', *, *, #57908, .F. ) ;
#43964 =( NAMED_UNIT ( * ) PLANE_ANGLE_UNIT ( ) SI_UNIT ( $, .RADIAN. ) );
#43965 = CARTESIAN_POINT ( 'NONE',  ( -4.458734125000000326, -165.2500000013655779, -1.846868145590735644 ) ) ;
#43966 = CARTESIAN_POINT ( 'NONE',  ( -4.458734124999999437, -105.6458333319677507, -2.574251347313719407 ) ) ;
#43967 = CARTESIAN_POINT ( 'NONE',  ( 1.975475456537005874E-15, -68.62499999726881583, 5.000000000000000000 ) ) ;
#43968 = VERTEX_POINT ( 'NONE', #28652 ) ;
#43969 = CARTESIAN_POINT ( 'NONE',  ( -56.48576386720575471, -147.0000000013656063, -4.591703134518078322 ) ) ;
#43970 = CARTESIAN_POINT ( 'NONE',  ( -56.66612745406270335, -138.4375000027312126, -5.149110718188516067 ) ) ;
#43971 = CARTESIAN_POINT ( 'NONE',  ( 4.458734124999998549, -36.72916666530107221, -2.574251347313721627 ) ) ;
#43972 = CARTESIAN_POINT ( 'NONE',  ( -4.458734124999999437, -146.1875000013656063, -5.460374474430324690E-16 ) ) ;
#43973 = CARTESIAN_POINT ( 'NONE',  ( -1.339745962155613812, 22.79465819873851729, -5.000000000000000000 ) ) ;
#43974 = CARTESIAN_POINT ( 'NONE',  ( -59.81910112700024484, -135.1875000000000284, -2.462841084822808835 ) ) ;
#43975 = EDGE_CURVE ( 'NONE', #47768, #37487, #3169, .T. ) ;
#43976 = CARTESIAN_POINT ( 'NONE',  ( -3.152548672688508926E-16, -13.56249999863440259, -5.148502694627439702 ) ) ;
#43977 = CARTESIAN_POINT ( 'NONE',  ( -4.458734124999999437, -102.5624999986344079, 0.000000000000000000 ) ) ;
#43978 = VERTEX_POINT ( 'NONE', #19633 ) ;
#43979 = CARTESIAN_POINT ( 'NONE',  ( 4.458734125000000326, -145.6250000013655779, -1.846868145590734978 ) ) ;
#43980 = CARTESIAN_POINT ( 'NONE',  ( 2.229367062500001939, -31.22916666530107221, 3.861377020970579999 ) ) ;
#43981 = CARTESIAN_POINT ( 'NONE',  ( 0.000000000000000000, -120.0000000000000000, 0.000000000000000000 ) ) ;
#43982 = CARTESIAN_POINT ( 'NONE',  ( -58.39396692619412477, -133.4375000013656063, 2.891590998281057701 ) ) ;
#43983 = CARTESIAN_POINT ( 'NONE',  ( 4.458734125000001214, -67.14583333196773651, 2.574251347313718519 ) ) ;
#43984 = CARTESIAN_POINT ( 'NONE',  ( -60.14911071818854538, -146.1875000027312126, 1.666127454062681146 ) ) ;
#43985 = CARTESIAN_POINT ( 'NONE',  ( 0.000000000000000000, -170.0000000000000000, 0.000000000000000000 ) ) ;
#43986 = CARTESIAN_POINT ( 'NONE',  ( 1.846868145590736310, -139.6250000013656347, 4.458734124999997661 ) ) ;
#43987 = CARTESIAN_POINT ( 'NONE',  ( 4.458734125000000326, 4.854166668032262599, 2.574251347313718519 ) ) ;
#43988 = ORIENTED_EDGE ( 'NONE', *, *, #14786, .T. ) ;
#43989 = CARTESIAN_POINT ( 'NONE',  ( -6.972266317189433020E-16, 1.750000000000000444, -5.000000000000000000 ) ) ;
#43990 = CARTESIAN_POINT ( 'NONE',  ( 3.535533905932738197, -159.8750000000000284, -3.535533905932738197 ) ) ;
#43992 = CARTESIAN_POINT ( 'NONE',  ( 2.229367062499998831, -32.64583333196773651, -3.861377020970580887 ) ) ;
#43991 = CARTESIAN_POINT ( 'NONE',  ( -5.000000000000000000, -97.00000000000000000, 0.000000000000000000 ) ) ;
#43993 = EDGE_CURVE ( 'NONE', #34951, #51281, #718, .T. ) ;
#43994 = CARTESIAN_POINT ( 'NONE',  ( -58.24261429053147765, -143.3750000027312126, -3.805975901505573855 ) ) ;
#43995 = CARTESIAN_POINT ( 'NONE',  ( 9.457646018065525792E-16, -78.31249999863442213, 5.148502694627439702 ) ) ;
#43996 = CARTESIAN_POINT ( 'NONE',  ( 2.229367062500001939, 23.77083333469892779, 3.861377020970579999 ) ) ;
#43997 = CARTESIAN_POINT ( 'NONE',  ( -2.500000000000000444, 26.83333333333333570, -4.330127018922193649 ) ) ;
#43998 = CARTESIAN_POINT ( 'NONE',  ( -59.59170313451811296, -143.5000000013656347, 1.485763867205729394 ) ) ;
#43999 = CARTESIAN_POINT ( 'NONE',  ( 4.458734124999998549, -0.7291666653010709931, -2.574251347313721627 ) ) ;
#44000 = CARTESIAN_POINT ( 'NONE',  ( -2.229367062499996610, 28.60416666803226349, 3.861377020970582219 ) ) ;
#44001 = EDGE_CURVE ( 'NONE', #11807, #7607, #9709, .T. ) ;
#44002 = CARTESIAN_POINT ( 'NONE',  ( 4.458734124999998549, -44.97916666530107221, -2.574251347313721627 ) ) ;
#44003 = CARTESIAN_POINT ( 'NONE',  ( 1.339745962155615144, -43.58034179853029144, 4.999999999999999112 ) ) ;
#44004 = CARTESIAN_POINT ( 'NONE',  ( 4.458734124999998549, 4.270833334698926897, -2.574251347313721627 ) ) ;
#44005 = VERTEX_POINT ( 'NONE', #8729 ) ;
#44006 = CARTESIAN_POINT ( 'NONE',  ( -3.152548672688508926E-16, -22.81249999863440436, -5.148502694627439702 ) ) ;
#44007 =( BOUNDED_CURVE ( )  B_SPLINE_CURVE ( 2, ( #30549, #61751, #7082, #56922, #52092, #31502, #36660, #13160, #41790 ),
 .UNSPECIFIED., .F., .F. ) 
 B_SPLINE_CURVE_WITH_KNOTS ( ( 3, 2, 2, 2, 3 ),
 ( 0.1416666666666667740, 0.1458333333333334814, 0.1500000000000001332, 0.1541666666666668406, 0.1583333333333334925 ),
 .UNSPECIFIED. ) 
 CURVE ( )  GEOMETRIC_REPRESENTATION_ITEM ( )  RATIONAL_B_SPLINE_CURVE ( ( 0.9999999999999980016, 0.9238795325112887369, 1.000000000000000000, 0.9238795325112867385, 1.000000000000000000, 0.9238795325112867385, 1.000000000000000000, 0.9238795325112837409, 1.000000000000003109 ) ) 
 REPRESENTATION_ITEM ( '' )  );
#44008 = CARTESIAN_POINT ( 'NONE',  ( -2.229367062500000163, -68.47916666530107932, -3.861377020970580443 ) ) ;
#44009 = CARTESIAN_POINT ( 'NONE',  ( -2.499999999999996447, -104.7083333306021444, 4.330127018922195425 ) ) ;
#44010 = CARTESIAN_POINT ( 'NONE',  ( -4.458734124999999437, 27.60416666803226349, -2.574251347313719407 ) ) ;
#44011 = CARTESIAN_POINT ( 'NONE',  ( 2.499999999999998668, -58.20833333060214443, -4.330127018922193649 ) ) ;
#44012 = CARTESIAN_POINT ( 'NONE',  ( -3.152548672688508926E-16, -109.8124999986343795, -5.148502694627439702 ) ) ;
#44013 = CARTESIAN_POINT ( 'NONE',  ( -2.229367062500000163, -74.72916666530106511, -3.861377020970580443 ) ) ;
#44014 = CARTESIAN_POINT ( 'NONE',  ( 2.499999999999998668, -55.33333333333332860, -4.330127018922193649 ) ) ;
#44015 = FACE_OUTER_BOUND ( 'NONE', #53307, .T. ) ;
#44016 = DIRECTION ( 'NONE',  ( -0.000000000000000000, 1.000000000000000000, -0.000000000000000000 ) ) ;
#44017 = ORIENTED_EDGE ( 'NONE', *, *, #1576, .T. ) ;
#44018 = CARTESIAN_POINT ( 'NONE',  ( 1.975475456537005874E-15, -99.74999999999998579, 5.000000000000000000 ) ) ;
#44019 = CARTESIAN_POINT ( 'NONE',  ( 1.339745962155615144, -6.580341798530292330, 4.999999999999999112 ) ) ;
#44020 = CARTESIAN_POINT ( 'NONE',  ( -3.535250795749689387E-16, -19.24999999999999645, -5.773502691896257311 ) ) ;
#44021 = CARTESIAN_POINT ( 'NONE',  ( -4.458734124999998549, -22.22916666530107221, 2.574251347313722516 ) ) ;
#44022 = ADVANCED_FACE ( 'NONE', ( #34106 ), #28340, .T. ) ;
#44023 = CARTESIAN_POINT ( 'NONE',  ( 2.229367062500001939, -80.97916666530106511, 3.861377020970579999 ) ) ;
#44024 = CARTESIAN_POINT ( 'NONE',  ( 4.458734124999999437, -166.6875000013655779, 0.000000000000000000 ) ) ;
#44025 = CARTESIAN_POINT ( 'NONE',  ( -3.535250795749689387E-16, -17.12499999726881583, -5.773502691896257311 ) ) ;
#44027 = VERTEX_POINT ( 'NONE', #58871 ) ;
#44026 = CARTESIAN_POINT ( 'NONE',  ( 4.458734124999998549, -48.72916666530107221, -2.574251347313721627 ) ) ;
#44028 = CARTESIAN_POINT ( 'NONE',  ( 1.339745962155612702, 5.705341801261479162, -5.000000000000000000 ) ) ;
#44029 = CARTESIAN_POINT ( 'NONE',  ( 5.000000000000000000, -45.37499999726880873, -6.123233995736766282E-16 ) ) ;
#44031 = ORIENTED_EDGE ( 'NONE', *, *, #14941, .F. ) ;
#44030 = CARTESIAN_POINT ( 'NONE',  ( -2.229367062500000163, -0.7291666653010709931, -3.861377020970580443 ) ) ;
#44032 = CARTESIAN_POINT ( 'NONE',  ( -50.40829686548195099, -152.0000000013656063, -1.485763867205728284 ) ) ;
#44033 = CARTESIAN_POINT ( 'NONE',  ( 5.000000000000000888, -66.58333333333332860, 2.886751345948126879 ) ) ;
#44034 = CARTESIAN_POINT ( 'NONE',  ( 3.152801135295366208, -156.8125000013656063, 3.152801135295367985 ) ) ;
#44035 = CARTESIAN_POINT ( 'NONE',  ( 4.458734125000001214, -41.14583333196774362, 2.574251347313718519 ) ) ;
#44036 = CARTESIAN_POINT ( 'NONE',  ( -51.19402409849444524, -149.6250000027312126, -3.242614290531456334 ) ) ;
#44037 = CARTESIAN_POINT ( 'NONE',  ( -5.000000000000000000, -160.5000000000000000, -6.123233995736766282E-16 ) ) ;
#44038 = CARTESIAN_POINT ( 'NONE',  ( -6.972266317189433020E-16, -57.12499999726879452, -5.000000000000000000 ) ) ;
#44039 = CARTESIAN_POINT ( 'NONE',  ( -55.35523342533222291, -126.5625000013655921, 4.444560631937231499 ) ) ;
#44040 = CARTESIAN_POINT ( 'NONE',  ( 9.457646018065525792E-16, -10.31249999863440614, 5.148502694627439702 ) ) ;
#44041 = CARTESIAN_POINT ( 'NONE',  ( 4.458734124999999437, -46.06249999863440081, -5.460374474430324690E-16 ) ) ;
#44042 = CARTESIAN_POINT ( 'NONE',  ( -49.85088928181150436, -136.6875000027312126, -1.666127454062680480 ) ) ;
#44043 = CARTESIAN_POINT ( 'NONE',  ( -3.152801135295367985, -148.8125000013655779, 3.152801135295367096 ) ) ;
#44044 = CARTESIAN_POINT ( 'NONE',  ( 2.229367062500001939, -91.22916666530106511, 3.861377020970579999 ) ) ;
#44045 = CARTESIAN_POINT ( 'NONE',  ( 5.000000000000000888, -167.0625000027312126, -2.071067811865475505 ) ) ;
#44046 = EDGE_LOOP ( 'NONE', ( #39756, #10438, #11925, #56862 ) ) ;
#44047 = CARTESIAN_POINT ( 'NONE',  ( 2.499999999999998668, -19.20833333060214798, -4.330127018922193649 ) ) ;
#44048 = FACE_OUTER_BOUND ( 'NONE', #5299, .T. ) ;
#44049 = CARTESIAN_POINT ( 'NONE',  ( -50.18089887299979068, -151.8125000027312126, 2.462841084822635640 ) ) ;
#44050 = CARTESIAN_POINT ( 'NONE',  ( -6.972266317189433020E-16, -29.12499999726880873, -5.000000000000000000 ) ) ;
#44051 = VECTOR ( 'NONE', #24604, 1000.000000000000000 ) ;
#44052 = ORIENTED_EDGE ( 'NONE', *, *, #25126, .T. ) ;
#44053 = CARTESIAN_POINT ( 'NONE',  ( 9.457646018065525792E-16, 0.9375000013655959696, 5.148502694627439702 ) ) ;
#44054 = EDGE_CURVE ( 'NONE', #29478, #7305, #44068, .T. ) ;
#44055 = EDGE_CURVE ( 'NONE', #63519, #28539, #15130, .T. ) ;
#44056 = DIRECTION ( 'NONE',  ( 0.8660254037844385966, 0.000000000000000000, 0.4999999999999999445 ) ) ;
#44057 = CARTESIAN_POINT ( 'NONE',  ( 2.229367062499998831, -12.89583333196774007, -3.861377020970580887 ) ) ;
#44058 = ADVANCED_FACE ( 'NONE', ( #55343 ), #30229, .T. ) ;
#44059 = CARTESIAN_POINT ( 'NONE',  ( -5.000000000000000000, -51.08333333333332860, -2.886751345948128211 ) ) ;
#44060 = CARTESIAN_POINT ( 'NONE',  ( -4.458734124999998549, -2.229166665301068662, 2.574251347313722516 ) ) ;
#44061 = CARTESIAN_POINT ( 'NONE',  ( -3.152801135295367096, -152.0625000013655779, -3.152801135295367541 ) ) ;
#44062 = CARTESIAN_POINT ( 'NONE',  ( 9.457646018065525792E-16, 21.68750000136559208, 5.148502694627439702 ) ) ;
#44063 = ORIENTED_EDGE ( 'NONE', *, *, #43620, .F. ) ;
#44064 = CARTESIAN_POINT ( 'NONE',  ( 9.457646018065525792E-16, -99.06249999863440792, 5.148502694627439702 ) ) ;
#44065 = CYLINDRICAL_SURFACE ( 'NONE', #51071, 5.000000000000000000 ) ;
#44066 = DIRECTION ( 'NONE',  ( 0.000000000000000000, 0.000000000000000000, 1.000000000000000000 ) ) ;
#44067 = CARTESIAN_POINT ( 'NONE',  ( 2.229367062500001939, -12.97916666530107221, 3.861377020970579999 ) ) ;
#44069 = EDGE_CURVE ( 'NONE', #30129, #29621, #51634, .T. ) ;
#44068 = LINE ( 'NONE', #23529, #16030 ) ;
#44070 = CARTESIAN_POINT ( 'NONE',  ( 3.061616997868383141E-16, -156.7500000000000000, -5.000000000000000000 ) ) ;
#44071 = FACE_OUTER_BOUND ( 'NONE', #53545, .T. ) ;
#44072 = CARTESIAN_POINT ( 'NONE',  ( 2.500000000000002220, -40.54166666393548013, 4.330127018922192761 ) ) ;
#44073 = DIRECTION ( 'NONE',  ( -0.000000000000000000, 1.000000000000000000, -0.000000000000000000 ) ) ;
#44074 = CARTESIAN_POINT ( 'NONE',  ( -4.458734124999997661, 12.77083333469892779, 2.574251347313722516 ) ) ;
#44075 = CARTESIAN_POINT ( 'NONE',  ( 1.339745962155612702, -46.16965819600732601, -5.000000000000000000 ) ) ;
#44076 = EDGE_CURVE ( 'NONE', #26245, #18754, #45038, .T. ) ;
#44077 = ORIENTED_EDGE ( 'NONE', *, *, #48740, .F. ) ;
#44078 = CARTESIAN_POINT ( 'NONE',  ( -4.458734124999999437, 18.60416666803225993, -2.574251347313719407 ) ) ;
#44079 = ADVANCED_FACE ( 'NONE', ( #55663 ), #670, .T. ) ;
#44080 = CARTESIAN_POINT ( 'NONE',  ( 9.457646018065525792E-16, -64.06249999863440792, 5.148502694627439702 ) ) ;
#44081 = CARTESIAN_POINT ( 'NONE',  ( -3.152548672688508926E-16, -9.812499998634406140, -5.148502694627439702 ) ) ;
#44082 = CARTESIAN_POINT ( 'NONE',  ( -2.500000000000000444, 4.833333333333332149, -4.330127018922193649 ) ) ;
#44083 = CARTESIAN_POINT ( 'NONE',  ( 3.152801135295367541, -169.3125000013656063, -3.152801135295367541 ) ) ;
#44085 = EDGE_CURVE ( 'NONE', #13643, #41864, #31196, .T. ) ;
#44084 = CARTESIAN_POINT ( 'NONE',  ( -51.19402409849444524, -142.5000000000000284, -3.242614290531456334 ) ) ;
#44086 = CARTESIAN_POINT ( 'NONE',  ( -2.229367062500000163, -52.47916666530107221, -3.861377020970580443 ) ) ;
#44087 = CARTESIAN_POINT ( 'NONE',  ( -2.499999999999996447, -87.70833333060214443, 4.330127018922195425 ) ) ;
#44088 = CARTESIAN_POINT ( 'NONE',  ( -4.458734124999999437, -26.39583333196774007, -2.574251347313719407 ) ) ;
#44089 =( BOUNDED_CURVE ( )  B_SPLINE_CURVE ( 2, ( #42649, #4057, #28799, #58072, #18212, #37208, #37835, #33631, #53250 ),
 .UNSPECIFIED., .F., .F. ) 
 B_SPLINE_CURVE_WITH_KNOTS ( ( 3, 2, 2, 2, 3 ),
 ( 0.6145833333333333703, 0.6152777777777778123, 0.6166666666666666963, 0.6180555555555555802, 0.6187500000000000222 ),
 .UNSPECIFIED. ) 
 CURVE ( )  GEOMETRIC_REPRESENTATION_ITEM ( )  RATIONAL_B_SPLINE_CURVE ( ( 0.9330127018922194093, 0.9330127018922194093, 1.000000000000000000, 0.8660254037844387076, 1.000000000000000000, 0.8660254037844387076, 1.000000000000000000, 0.9330127018922194093, 0.9330127018922194093 ) ) 
 REPRESENTATION_ITEM ( '' )  );
#44090 = CARTESIAN_POINT ( 'NONE',  ( 1.975475456537005874E-15, -16.74999999999999645, 5.000000000000000000 ) ) ;
#44091 = CARTESIAN_POINT ( 'NONE',  ( 1.975475456537005874E-15, -28.62499999726881583, 5.000000000000000000 ) ) ;
#44092 = CARTESIAN_POINT ( 'NONE',  ( -50.18089887299979068, -151.8125000027312126, 2.462841084822605442 ) ) ;
#44093 = CARTESIAN_POINT ( 'NONE',  ( 3.152801135295367541, -152.5625000013655779, -3.152801135295367541 ) ) ;
#44094 = CARTESIAN_POINT ( 'NONE',  ( 5.000000000000000000, -39.41666666666666430, -2.886751345948129988 ) ) ;
#44095 = DIRECTION ( 'NONE',  ( -0.000000000000000000, 0.000000000000000000, -1.000000000000000000 ) ) ;
#44096 = LINE ( 'NONE', #38953, #62318 ) ;
#44097 = ORIENTED_EDGE ( 'NONE', *, *, #2353, .T. ) ;
#44098 = CARTESIAN_POINT ( 'NONE',  ( 4.458734124999998549, -102.7291666653010509, -2.574251347313721627 ) ) ;
#44099 = CARTESIAN_POINT ( 'NONE',  ( -4.458734124999998549, 4.520833334698926009, 2.574251347313722516 ) ) ;
#44100 = CARTESIAN_POINT ( 'NONE',  ( -5.000000000000000000, -87.87499999726880162, 0.000000000000000000 ) ) ;
#44101 = CARTESIAN_POINT ( 'NONE',  ( -5.000000000000000000, -1.083333333333331927, -2.886751345948128211 ) ) ;
#44102 = CARTESIAN_POINT ( 'NONE',  ( 4.458734125000000326, -65.89583333196773651, 2.574251347313718519 ) ) ;
#44103 = DIRECTION ( 'NONE',  ( 0.000000000000000000, 0.000000000000000000, -1.000000000000000000 ) ) ;
#44104 = CARTESIAN_POINT ( 'NONE',  ( -4.999999999999999112, -3.791666663935478798, 2.886751345948131764 ) ) ;
#44106 = EDGE_LOOP ( 'NONE', ( #62664, #8631, #14811, #14854 ) ) ;
#44105 = CARTESIAN_POINT ( 'NONE',  ( -2.229367062500000163, -35.47916666530107221, -3.861377020970580443 ) ) ;
#44107 = CYLINDRICAL_SURFACE ( 'NONE', #13219, 5.000000000000000000 ) ;
#44108 = CARTESIAN_POINT ( 'NONE',  ( 2.071067811865603403, -157.1875000000000284, 4.999999999999872990 ) ) ;
#44109 = CARTESIAN_POINT ( 'NONE',  ( -6.972266317189433020E-16, -20.24999999999999289, -5.000000000000000000 ) ) ;
#44110 = CARTESIAN_POINT ( 'NONE',  ( -3.535250795749689387E-16, -44.25000000000000000, -5.773502691896257311 ) ) ;
#44112 = CARTESIAN_POINT ( 'NONE',  ( -3.152548672688508926E-16, -23.81249999863440792, -5.148502694627439702 ) ) ;
#44111 = CARTESIAN_POINT ( 'NONE',  ( -75.00000000000000000, 15.00000000000000000, 8.999999999999998224 ) ) ;
#44113 = CARTESIAN_POINT ( 'NONE',  ( -2.500000000000000444, 21.95833333606451987, -4.330127018922193649 ) ) ;
#44114 = CARTESIAN_POINT ( 'NONE',  ( 2.229367062499998831, -68.64583333196773651, -3.861377020970580887 ) ) ;
#44115 = CARTESIAN_POINT ( 'NONE',  ( 4.458734124999999437, -145.6875000013656063, 0.000000000000000000 ) ) ;
#44116 = CARTESIAN_POINT ( 'NONE',  ( -2.229367062499996610, -82.14583333196773651, 3.861377020970582219 ) ) ;
#44117 = CARTESIAN_POINT ( 'NONE',  ( -58.39396692619412477, -139.6875000013656347, 2.891590998281057701 ) ) ;
#44118 = CARTESIAN_POINT ( 'NONE',  ( 2.229367062500001939, -28.22916666530107221, 3.861377020970579999 ) ) ;
#44119 = CARTESIAN_POINT ( 'NONE',  ( -3.535250795749689387E-16, -71.12499999726880162, -5.773502691896257311 ) ) ;
#44120 = EDGE_LOOP ( 'NONE', ( #42529, #19005, #4896, #60448 ) ) ;
#44121 = CYLINDRICAL_SURFACE ( 'NONE', #14543, 5.000000000000000000 ) ;
#44122 = ORIENTED_EDGE ( 'NONE', *, *, #48885, .F. ) ;
#44123 = CARTESIAN_POINT ( 'NONE',  ( 9.457646018065525792E-16, -74.31249999863440792, 5.148502694627439702 ) ) ;
#44124 = CARTESIAN_POINT ( 'NONE',  ( -6.972266317189433020E-16, -103.2500000000000000, -5.000000000000000000 ) ) ;
#44125 = PRODUCT_RELATED_PRODUCT_CATEGORY ( 'part', '', ( #21005 ) ) ;
#44126 = SURFACE_STYLE_FILL_AREA ( #24524 ) ;
#44127 = VERTEX_POINT ( 'NONE', #50825 ) ;
#44128 = FACE_OUTER_BOUND ( 'NONE', #59655, .T. ) ;
#44129 = CARTESIAN_POINT ( 'NONE',  ( 1.975475456537005874E-15, -82.74999999999998579, 5.000000000000000000 ) ) ;
#44130 = CARTESIAN_POINT ( 'NONE',  ( 9.457646018065525792E-16, -59.31249999863440081, 5.148502694627439702 ) ) ;
#44131 = CARTESIAN_POINT ( 'NONE',  ( 2.229367062500001939, -0.2291666653010705768, 3.861377020970579999 ) ) ;
#44132 = ORIENTED_EDGE ( 'NONE', *, *, #12938, .T. ) ;
#44133 = DIRECTION ( 'NONE',  ( -0.000000000000000000, 1.000000000000000000, -0.000000000000000000 ) ) ;
#44134 = CARTESIAN_POINT ( 'NONE',  ( -1.339745962155610925, -22.66965819600732956, 5.000000000000000000 ) ) ;
#44135 = CARTESIAN_POINT ( 'NONE',  ( -3.152548672688508926E-16, 13.43750000136559386, -5.148502694627439702 ) ) ;
#44136 = CARTESIAN_POINT ( 'NONE',  ( -59.59170313451811296, -139.5000000013656063, 1.485763867205729394 ) ) ;
#44137 = CARTESIAN_POINT ( 'NONE',  ( 2.499999999999998668, -27.20833333060214798, -4.330127018922193649 ) ) ;
#44138 = CARTESIAN_POINT ( 'NONE',  ( -1.846868145590734756, -164.1250000013656063, -4.458734124999999437 ) ) ;
#44139 = VERTEX_POINT ( 'NONE', #6762 ) ;
#44140 = CARTESIAN_POINT ( 'NONE',  ( -4.458734124999999437, -80.39583333196773651, -2.574251347313719407 ) ) ;
#44141 = DIRECTION ( 'NONE',  ( 0.000000000000000000, 0.000000000000000000, 1.000000000000000000 ) ) ;
#44142 = CARTESIAN_POINT ( 'NONE',  ( -2.229367062499996610, 3.854166668032260823, 3.861377020970582219 ) ) ;
#44143 = AXIS2_PLACEMENT_3D ( 'NONE', #1355, #15493, #21592 ) ;
#44144 = CARTESIAN_POINT ( 'NONE',  ( -4.999999999999999112, -82.91666666666667140, 2.886751345948131764 ) ) ;
#44145 = CARTESIAN_POINT ( 'NONE',  ( -2.229367062500000163, -65.72916666530106511, -3.861377020970580443 ) ) ;
#44146 = CARTESIAN_POINT ( 'NONE',  ( -5.000000000000000000, -24.87499999726881583, 0.000000000000000000 ) ) ;
#44147 = DIRECTION ( 'NONE',  ( 0.000000000000000000, 0.000000000000000000, 1.000000000000000000 ) ) ;
#44148 = CARTESIAN_POINT ( 'NONE',  ( -1.339745962155613812, -1.080341798530293218, -5.000000000000000000 ) ) ;
#44149 = CARTESIAN_POINT ( 'NONE',  ( -6.972266317189433020E-16, -49.24999999999999289, -5.000000000000000000 ) ) ;
#44150 = DIRECTION ( 'NONE',  ( 0.5000000000000009992, 0.000000000000000000, 0.8660254037844380415 ) ) ;
#44151 = EDGE_CURVE ( 'NONE', #40464, #22078, #50443, .T. ) ;
#44152 = CARTESIAN_POINT ( 'NONE',  ( -2.229367062499996610, -45.14583333196774362, 3.861377020970582219 ) ) ;
#44153 = CARTESIAN_POINT ( 'NONE',  ( 4.458734125000000326, -31.14583333196773651, 2.574251347313718519 ) ) ;
#44154 = CARTESIAN_POINT ( 'NONE',  ( 2.229367062500001939, 7.770833334698926009, 3.861377020970579999 ) ) ;
#44155 =( BOUNDED_CURVE ( )  B_SPLINE_CURVE ( 2, ( #11431, #56469, #2436, #51324, #16897 ),
 .UNSPECIFIED., .F., .F. ) 
 B_SPLINE_CURVE_WITH_KNOTS ( ( 3, 2, 3 ),
 ( 0.9979166666666666741, 0.9986111111111111160, 1.000000000000000000 ),
 .UNSPECIFIED. ) 
 CURVE ( )  GEOMETRIC_REPRESENTATION_ITEM ( )  RATIONAL_B_SPLINE_CURVE ( ( 0.9330127018922194093, 0.9330127018922194093, 1.000000000000000000, 0.8660254037844387076, 1.000000000000000000 ) ) 
 REPRESENTATION_ITEM ( '' )  );
#44156 = CYLINDRICAL_SURFACE ( 'NONE', #12397, 5.000000000000000000 ) ;
#44157 = CARTESIAN_POINT ( 'NONE',  ( 5.000000000000000000, 26.58333333333333570, -2.886751345948129988 ) ) ;
#44158 = EDGE_CURVE ( 'NONE', #27913, #7221, #7301, .T. ) ;
#44159 = CARTESIAN_POINT ( 'NONE',  ( -5.000000000000000888, -149.6875000027312126, -2.071067811865475949 ) ) ;
#44160 = CARTESIAN_POINT ( 'NONE',  ( -58.24261429053147765, -154.2500000000000284, -3.805975901505573855 ) ) ;
#44161 = CARTESIAN_POINT ( 'NONE',  ( 4.458734124999999437, -36.81249999863440792, -5.460374474430324690E-16 ) ) ;
#44162 = CARTESIAN_POINT ( 'NONE',  ( -5.000000000000000000, -70.87499999726880162, 0.000000000000000000 ) ) ;
#44163 = AXIS2_PLACEMENT_3D ( 'NONE', #44375, #28639, #19302 ) ;
#44164 = CARTESIAN_POINT ( 'NONE',  ( -52.80376928212989185, -142.1250000013656063, -4.297418129356379346 ) ) ;
#44165 = CARTESIAN_POINT ( 'NONE',  ( 3.061616997868383141E-16, -144.7500000000000284, -5.000000000000000000 ) ) ;
#44166 = EDGE_CURVE ( 'NONE', #51005, #44449, #20608, .T. ) ;
#44167 = CARTESIAN_POINT ( 'NONE',  ( 4.458734124999998549, -72.97916666530107932, -2.574251347313721627 ) ) ;
#44168 = CARTESIAN_POINT ( 'NONE',  ( 4.458734124999997661, -166.7500000013655779, 1.846868145590737864 ) ) ;
#44169 = CARTESIAN_POINT ( 'NONE',  ( 9.457646018065525792E-16, -34.06249999863440792, 5.148502694627439702 ) ) ;
#44170 = CARTESIAN_POINT ( 'NONE',  ( 2.500000000000002220, 18.45833333606451632, 4.330127018922192761 ) ) ;
#44171 = CARTESIAN_POINT ( 'NONE',  ( 0.000000000000000000, -170.0000000000000000, 0.000000000000000000 ) ) ;
#44172 = CARTESIAN_POINT ( 'NONE',  ( 5.000000000000000000, -19.49999999999999645, -6.123233995736766282E-16 ) ) ;
#44173 = CARTESIAN_POINT ( 'NONE',  ( -4.458734125000000326, -143.0000000013655779, -1.846868145590735644 ) ) ;
#44174 = VERTEX_POINT ( 'NONE', #30553 ) ;
#44175 = CARTESIAN_POINT ( 'NONE',  ( -5.000000000000000000, -90.87499999726880162, 0.000000000000000000 ) ) ;
#44176 = VERTEX_POINT ( 'NONE', #50179 ) ;
#44177 = CARTESIAN_POINT ( 'NONE',  ( -4.458734124999999437, -60.64583333196774362, -2.574251347313719407 ) ) ;
#44178 = CARTESIAN_POINT ( 'NONE',  ( -2.500000000000000444, 22.95833333606451632, -4.330127018922193649 ) ) ;
#44179 = CARTESIAN_POINT ( 'NONE',  ( 2.500000000000002220, 13.45833333606451987, 4.330127018922192761 ) ) ;
#44180 = CARTESIAN_POINT ( 'NONE',  ( -2.499999999999996447, 17.16666666666666430, 4.330127018922195425 ) ) ;
#44181 = APPLICATION_CONTEXT ( 'automotive_design' ) ;
#44182 = CARTESIAN_POINT ( 'NONE',  ( 9.457646018065525792E-16, -50.06249999863440792, 5.148502694627439702 ) ) ;
#44183 = CARTESIAN_POINT ( 'NONE',  ( 4.458734124999999437, -8.812499998634406140, -5.460374474430324690E-16 ) ) ;
#44184 = CARTESIAN_POINT ( 'NONE',  ( -2.071067811865491493, -168.6875000000000853, -4.999999999999985789 ) ) ;
#44185 = CARTESIAN_POINT ( 'NONE',  ( -1.339745962155497683, -77.20534180126146850, -5.000000000000066613 ) ) ;
#44186 = CARTESIAN_POINT ( 'NONE',  ( 1.975475456537005874E-15, -41.74999999999999289, 5.000000000000000000 ) ) ;
#44187 = VECTOR ( 'NONE', #53414, 1000.000000000000000 ) ;
#44188 =( BOUNDED_CURVE ( )  B_SPLINE_CURVE ( 2, ( #3747, #33635, #48109, #4061, #48419, #37840, #62610, #43279, #62917 ),
 .UNSPECIFIED., .F., .F. ) 
 B_SPLINE_CURVE_WITH_KNOTS ( ( 3, 2, 2, 2, 3 ),
 ( 0.5160714285714286254, 0.5166666666666667185, 0.5178571428571429047, 0.5190476190476190910, 0.5196428571428571841 ),
 .UNSPECIFIED. ) 
 CURVE ( )  GEOMETRIC_REPRESENTATION_ITEM ( )  RATIONAL_B_SPLINE_CURVE ( ( 0.9330127018922194093, 0.9330127018922256266, 1.000000000000000000, 0.8660254037844387076, 1.000000000000000000, 0.8660254037844387076, 1.000000000000000000, 0.9330127018922194093, 0.9330127018922194093 ) ) 
 REPRESENTATION_ITEM ( '' )  );
#44190 = CARTESIAN_POINT ( 'NONE',  ( 4.458734125000001214, -22.89583333196773651, 2.574251347313718519 ) ) ;
#44189 = CARTESIAN_POINT ( 'NONE',  ( 2.500000000000002220, 18.33333333333333215, 4.330127018922192761 ) ) ;
#44191 = CARTESIAN_POINT ( 'NONE',  ( -4.458734124999999437, 29.56250000136559208, 0.000000000000000000 ) ) ;
#44192 = CARTESIAN_POINT ( 'NONE',  ( -2.229367062500000163, -56.47916666530107221, -3.861377020970580443 ) ) ;
#44193 = CARTESIAN_POINT ( 'NONE',  ( -4.458734125000001214, -157.1250000013656063, 1.846868145590734089 ) ) ;
#44194 = CARTESIAN_POINT ( 'NONE',  ( 2.500000000000002220, -54.54166666393548013, 4.330127018922192761 ) ) ;
#44195 = ORIENTED_EDGE ( 'NONE', *, *, #62146, .T. ) ;
#44196 = CARTESIAN_POINT ( 'NONE',  ( -6.972266317189433020E-16, 24.87500000273118417, -5.000000000000000000 ) ) ;
#44197 = CARTESIAN_POINT ( 'NONE',  ( 9.457646018065525792E-16, 5.687500001365592972, 5.148502694627439702 ) ) ;
#44198 = ORIENTED_EDGE ( 'NONE', *, *, #46840, .T. ) ;
#44200 = CARTESIAN_POINT ( 'NONE',  ( -5.000000000000000000, -29.08333333333332860, -2.886751345948128211 ) ) ;
#44199 = DIRECTION ( 'NONE',  ( -0.000000000000000000, 1.000000000000000000, -0.000000000000000000 ) ) ;
#44201 = CARTESIAN_POINT ( 'NONE',  ( -4.458734125000001214, -156.8750000013655779, 1.846868145590734089 ) ) ;
#44202 = EDGE_LOOP ( 'NONE', ( #49907, #10426, #30726, #32361 ) ) ;
#44203 = CARTESIAN_POINT ( 'NONE',  ( -5.000000000000000000, 10.91666666666666607, -2.886751345948128211 ) ) ;
#44204 = CARTESIAN_POINT ( 'NONE',  ( -59.98410592259440222, -134.1250000000000284, -0.3983568153799752487 ) ) ;
#44205 = CARTESIAN_POINT ( 'NONE',  ( 1.975475456537005874E-15, -53.62499999726880162, 5.000000000000000000 ) ) ;
#44206 = CARTESIAN_POINT ( 'NONE',  ( 4.458734124999999437, -45.06249999863440081, -5.460374474430324690E-16 ) ) ;
#44207 = VERTEX_POINT ( 'NONE', #20921 ) ;
#44208 = LINE ( 'NONE', #53556, #44992 ) ;
#44209 = CARTESIAN_POINT ( 'NONE',  ( 2.229367062500001939, 20.02083333469892779, 3.861377020970579999 ) ) ;
#44210 = CARTESIAN_POINT ( 'NONE',  ( -50.01589407740564042, -149.6250000000000284, 0.3983568153799778022 ) ) ;
#44211 = ORIENTED_EDGE ( 'NONE', *, *, #43008, .T. ) ;
#44212 = CARTESIAN_POINT ( 'NONE',  ( 4.458734124999999437, -89.06249999863439371, -5.460374474430324690E-16 ) ) ;
#44213 = CARTESIAN_POINT ( 'NONE',  ( -54.60164318462004474, -125.5000000027311984, -4.984105922594373794 ) ) ;
#44214 = CARTESIAN_POINT ( 'NONE',  ( 1.339745962155600711, 12.41965820146970501, 5.000000000000007994 ) ) ;
#44215 = CARTESIAN_POINT ( 'NONE',  ( -54.61975348727955293, -134.9999999999999716, 4.958636921927378260 ) ) ;
#44216 = CARTESIAN_POINT ( 'NONE',  ( -48.00000000000002132, -135.0000000000000284, 4.041451884327384114 ) ) ;
#44217 = CARTESIAN_POINT ( 'NONE',  ( 4.458734124999999437, -59.81249999863440081, -5.460374474430324690E-16 ) ) ;
#44218 = CARTESIAN_POINT ( 'NONE',  ( 7.968863443239234456, 4.547634245050474533, -8.057411785091787237 ) ) ;
#44219 = CARTESIAN_POINT ( 'NONE',  ( -4.458734124999999437, 15.60416666803225993, -2.574251347313719407 ) ) ;
#44220 = CARTESIAN_POINT ( 'NONE',  ( 0.000000000000000000, -170.0000000000000000, 0.000000000000000000 ) ) ;
#44221 = CARTESIAN_POINT ( 'NONE',  ( 2.229367062499998831, -51.89583333196773651, -3.861377020970580887 ) ) ;
#44222 = CARTESIAN_POINT ( 'NONE',  ( -2.499999999999996447, -9.708333330602146205, 4.330127018922195425 ) ) ;
#44223 = DIRECTION ( 'NONE',  ( -0.000000000000000000, 1.000000000000000000, -0.000000000000000000 ) ) ;
#44224 = CARTESIAN_POINT ( 'NONE',  ( -4.999999999999998224, -66.79166666393547303, 2.886751345948131764 ) ) ;
#44225 = CARTESIAN_POINT ( 'NONE',  ( -4.999999999999998224, -73.91666666666667140, 2.886751345948131764 ) ) ;
#44226 = CARTESIAN_POINT ( 'NONE',  ( 9.457646018065525792E-16, -109.0624999986344221, 5.148502694627439702 ) ) ;
#44227 = COLOUR_RGB ( '',0.8941176470588234615, 0.8941176470588234615, 0.8941176470588234615 ) ;
#44228 = CARTESIAN_POINT ( 'NONE',  ( -4.458734124999999437, -12.64583333196774007, -2.574251347313719407 ) ) ;
#44229 = EDGE_LOOP ( 'NONE', ( #36442, #27146, #53000, #25865 ) ) ;
#44230 = CARTESIAN_POINT ( 'NONE',  ( -5.000000000000000000, -169.5000000000000000, -6.123233995736766282E-16 ) ) ;
#44231 = CARTESIAN_POINT ( 'NONE',  ( -4.458734124999998549, -99.22916666530105090, 2.574251347313722516 ) ) ;
#44232 = CARTESIAN_POINT ( 'NONE',  ( -3.535533905932738641, -159.5000000027312126, 3.535533905932737309 ) ) ;
#44233 = CARTESIAN_POINT ( 'NONE',  ( 4.458734124999999437, -97.06249999863440792, -5.460374474430324690E-16 ) ) ;
#44234 = VECTOR ( 'NONE', #35986, 1000.000000000000227 ) ;
#44235 = CARTESIAN_POINT ( 'NONE',  ( 0.000000000000000000, -170.0000000000000000, 5.000000000000000000 ) ) ;
#44236 = CARTESIAN_POINT ( 'NONE',  ( 5.000000000000000000, -58.37499999726880873, -6.123233995736766282E-16 ) ) ;
#44237 = CARTESIAN_POINT ( 'NONE',  ( -7.894787914004607998, -0.7661396099416333261, -7.591390474663429089 ) ) ;
#44238 = CARTESIAN_POINT ( 'NONE',  ( -50.55543936806279248, -127.0625000013655921, 0.3552334253322060320 ) ) ;
#44239 = CARTESIAN_POINT ( 'NONE',  ( -53.51423613279429503, -145.2500000013656347, 4.591703134518083651 ) ) ;
#44240 = CARTESIAN_POINT ( 'NONE',  ( -4.458734124999997661, -16.22916666530107577, 2.574251347313722516 ) ) ;
#44241 = CARTESIAN_POINT ( 'NONE',  ( -2.229367062500000163, 4.270833334698926897, -3.861377020970580443 ) ) ;
#44242 = CARTESIAN_POINT ( 'NONE',  ( 4.458734124999998549, -58.97916666530106511, -2.574251347313721627 ) ) ;
#44243 = DIRECTION ( 'NONE',  ( -0.000000000000000000, 1.000000000000000000, -0.000000000000000000 ) ) ;
#44244 = CARTESIAN_POINT ( 'NONE',  ( -2.229367062500000163, -13.47916666530107221, -3.861377020970580443 ) ) ;
#44245 = DIRECTION ( 'NONE',  ( -0.000000000000000000, 1.000000000000000000, -0.000000000000000000 ) ) ;
#44246 = CARTESIAN_POINT ( 'NONE',  ( -9.184850993605147944E-16, -154.2500000000000000, 5.000000000000000000 ) ) ;
#44247 = CARTESIAN_POINT ( 'NONE',  ( -4.999999999999999112, -3.916666666666665630, 2.886751345948131764 ) ) ;
#44248 = VERTEX_POINT ( 'NONE', #27643 ) ;
#44249 = CARTESIAN_POINT ( 'NONE',  ( -4.458734124999997661, -38.47916666530107221, 2.574251347313722516 ) ) ;
#44250 = CARTESIAN_POINT ( 'NONE',  ( -50.40829686548195099, -125.2500000013656347, -1.485763867205728284 ) ) ;
#44251 = CARTESIAN_POINT ( 'NONE',  ( -5.088535779737005882, 5.722386535631696525, -7.491772860716161553 ) ) ;
#44252 = CARTESIAN_POINT ( 'NONE',  ( -1.127183054612291972E-14, 24.37500000273118417, 4.999999999999999112 ) ) ;
#44253 = CARTESIAN_POINT ( 'NONE',  ( -3.152548672688508926E-16, -84.56249999863439371, -5.148502694627439702 ) ) ;
#44254 = CARTESIAN_POINT ( 'NONE',  ( -4.458734124999999437, 16.43750000136559564, 0.000000000000000000 ) ) ;
#44255 = CARTESIAN_POINT ( 'NONE',  ( -4.458734124999999437, 7.604166668032259935, -2.574251347313719407 ) ) ;
#44256 = CARTESIAN_POINT ( 'NONE',  ( -2.499999999999996447, -88.70833333060214443, 4.330127018922195425 ) ) ;
#44257 = CARTESIAN_POINT ( 'NONE',  ( -1.339745962155589165, 11.79465819873852084, -5.000000000000014211 ) ) ;
#44258 = CARTESIAN_POINT ( 'NONE',  ( 5.000000000000000000, 20.70833333606451987, -2.886751345948130876 ) ) ;
#44259 = CARTESIAN_POINT ( 'NONE',  ( -2.229367062499996610, 22.60416666803225993, 3.861377020970582219 ) ) ;
#44260 = CARTESIAN_POINT ( 'NONE',  ( -2.500000000000000444, -73.16666666666665719, -4.330127018922193649 ) ) ;
#44261 = CARTESIAN_POINT ( 'NONE',  ( 2.500000000000002220, 7.458333336064517205, 4.330127018922192761 ) ) ;
#44262 = ORIENTED_EDGE ( 'NONE', *, *, #49227, .T. ) ;
#44263 = DIRECTION ( 'NONE',  ( -0.000000000000000000, 1.000000000000000000, -0.000000000000000000 ) ) ;
#44264 = ORIENTED_EDGE ( 'NONE', *, *, #51925, .F. ) ;
#44266 = CARTESIAN_POINT ( 'NONE',  ( 2.500000000000002220, -36.66666666666666430, 4.330127018922192761 ) ) ;
#44265 = LINE ( 'NONE', #48469, #51169 ) ;
#44267 = CARTESIAN_POINT ( 'NONE',  ( 2.229367062499998831, -39.64583333196773651, -3.861377020970580887 ) ) ;
#44268 = ADVANCED_FACE ( 'NONE', ( #61440 ), #12220, .T. ) ;
#44269 =( BOUNDED_CURVE ( )  B_SPLINE_CURVE ( 2, ( #21793, #47182, #2492, #41388, #22745, #42342, #61981, #55888, #46226 ),
 .UNSPECIFIED., .F., .F. ) 
 B_SPLINE_CURVE_WITH_KNOTS ( ( 3, 2, 2, 2, 3 ),
 ( 0.5083333333333337478, 0.5125000000000003997, 0.5166666666666671626, 0.5208333333333338144, 0.5250000000000004663 ),
 .UNSPECIFIED. ) 
 CURVE ( )  GEOMETRIC_REPRESENTATION_ITEM ( )  RATIONAL_B_SPLINE_CURVE ( ( 0.9999999999999918954, 0.9238795325112948431, 1.000000000000000000, 0.9238795325112867385, 1.000000000000000000, 0.9238795325112867385, 1.000000000000000000, 0.9238795325112786339, 1.000000000000008216 ) ) 
 REPRESENTATION_ITEM ( '' )  );
#44270 = CARTESIAN_POINT ( 'NONE',  ( -4.999999999999999112, -34.79166666393547303, 2.886751345948131764 ) ) ;
#44272 = ORIENTED_EDGE ( 'NONE', *, *, #6708, .T. ) ;
#44271 = CARTESIAN_POINT ( 'NONE',  ( 9.457646018065525792E-16, -68.06249999863440792, 5.148502694627439702 ) ) ;
#44273 = CARTESIAN_POINT ( 'NONE',  ( -51.60603307380591787, -152.1875000013656063, -2.891590998281053704 ) ) ;
#44274 = CARTESIAN_POINT ( 'NONE',  ( 2.229367062500001939, -13.97916666530107221, 3.861377020970579999 ) ) ;
#44276 = VERTEX_POINT ( 'NONE', #22195 ) ;
#44275 = CARTESIAN_POINT ( 'NONE',  ( 4.458734124999998549, -15.97916666530107221, -2.574251347313721627 ) ) ;
#44277 = CARTESIAN_POINT ( 'NONE',  ( -5.000000000000000000, -82.99999999999998579, 0.000000000000000000 ) ) ;
#44278 = CARTESIAN_POINT ( 'NONE',  ( -1.846868145590734756, -167.1250000013656063, -4.458734125000000326 ) ) ;
#44279 = CARTESIAN_POINT ( 'NONE',  ( -2.229367062500000163, -55.72916666530107221, -3.861377020970580443 ) ) ;
#44280 = CARTESIAN_POINT ( 'NONE',  ( 2.499999999999998668, -83.20833333060214443, -4.330127018922193649 ) ) ;
#44282 = ORIENTED_EDGE ( 'NONE', *, *, #44891, .F. ) ;
#44281 = CARTESIAN_POINT ( 'NONE',  ( 0.000000000000000000, -120.0000000000000000, 0.000000000000000000 ) ) ;
#44283 = VECTOR ( 'NONE', #39285, 1000.000000000000000 ) ;
#44284 = CARTESIAN_POINT ( 'NONE',  ( -58.24261429053147765, -147.2500000000000284, -3.805975901505573855 ) ) ;
#44285 = CARTESIAN_POINT ( 'NONE',  ( -2.229367062499996610, -29.39583333196774007, 3.861377020970582219 ) ) ;
#44286 = ORIENTED_EDGE ( 'NONE', *, *, #45236, .F. ) ;
#44287 =( BOUNDED_CURVE ( )  B_SPLINE_CURVE ( 2, ( #44863, #4995, #1151, #44543, #20104, #50008, #40357, #29742, #20434 ),
 .UNSPECIFIED., .F., .F. ) 
 B_SPLINE_CURVE_WITH_KNOTS ( ( 3, 2, 2, 2, 3 ),
 ( 0.08392857142857143571, 0.08452380952380952883, 0.08571428571428571508, 0.08690476190476190133, 0.08750000000000000833 ),
 .UNSPECIFIED. ) 
 CURVE ( )  GEOMETRIC_REPRESENTATION_ITEM ( )  RATIONAL_B_SPLINE_CURVE ( ( 0.9330127018922192983, 0.9330127018922200755, 1.000000000000000000, 0.8660254037844387076, 1.000000000000000000, 0.8660254037844387076, 1.000000000000000000, 0.9330127018922185211, 0.9330127018922192983 ) ) 
 REPRESENTATION_ITEM ( '' )  );
#44288 = CARTESIAN_POINT ( 'NONE',  ( 1.846868145590735200, -166.5000000013655779, -4.458734125000000326 ) ) ;
#44289 = CARTESIAN_POINT ( 'NONE',  ( -4.458734124999999437, -106.6458333319677365, -2.574251347313719407 ) ) ;
#44290 = CARTESIAN_POINT ( 'NONE',  ( -4.999999999999998224, -38.79166666393548013, 2.886751345948131764 ) ) ;
#44291 = ORIENTED_EDGE ( 'NONE', *, *, #15606, .F. ) ;
#44292 = CARTESIAN_POINT ( 'NONE',  ( -52.80376928212989185, -145.1250000013656063, -4.297418129356378458 ) ) ;
#44293 = CARTESIAN_POINT ( 'NONE',  ( -59.98410592259440222, -137.2500000027312126, -0.3983568153799752487 ) ) ;
#44294 = CARTESIAN_POINT ( 'NONE',  ( 2.229367062499998831, -36.64583333196773651, -3.861377020970580887 ) ) ;
#44295 = CARTESIAN_POINT ( 'NONE',  ( 1.846868145590736310, -147.8750000013655779, 4.458734124999997661 ) ) ;
#44296 = LINE ( 'NONE', #259, #13775 ) ;
#44297 = CARTESIAN_POINT ( 'NONE',  ( -2.229367062500000163, -11.47916666530107044, -3.861377020970580443 ) ) ;
#44298 = CARTESIAN_POINT ( 'NONE',  ( 2.229367062500001939, -103.2291666653010651, 3.861377020970579999 ) ) ;
#44299 = ORIENTED_EDGE ( 'NONE', *, *, #30353, .F. ) ;
#44300 = CARTESIAN_POINT ( 'NONE',  ( -3.152801135295367096, -141.3125000013655779, -3.152801135295367541 ) ) ;
#44301 = CARTESIAN_POINT ( 'NONE',  ( 4.458734124999998549, -34.97916666530107221, -2.574251347313721627 ) ) ;
#44302 = CARTESIAN_POINT ( 'NONE',  ( -2.500000000000000444, 4.958333336064518981, -4.330127018922193649 ) ) ;
#44303 = CARTESIAN_POINT ( 'NONE',  ( -51.75738570946856498, -153.7500000000000284, 3.805975901505576964 ) ) ;
#44304 = CARTESIAN_POINT ( 'NONE',  ( -50.40829686548195099, -132.0000000013656063, -1.485763867205728284 ) ) ;
#44305 = CARTESIAN_POINT ( 'NONE',  ( 2.229367062499998831, -74.89583333196773651, -3.861377020970580887 ) ) ;
#44306 = CARTESIAN_POINT ( 'NONE',  ( -58.24261429053147765, -146.3750000027312126, -3.805975901505573855 ) ) ;
#44307 = CARTESIAN_POINT ( 'NONE',  ( -5.000000000000000000, 29.12500000273118417, 0.000000000000000000 ) ) ;
#44308 = CARTESIAN_POINT ( 'NONE',  ( 4.729367062499999719, -139.8437500006828031, 0.000000000000000000 ) ) ;
#44309 = CARTESIAN_POINT ( 'NONE',  ( 2.229367062500001939, 6.770833334698928674, 3.861377020970579999 ) ) ;
#44310 = ORIENTED_EDGE ( 'NONE', *, *, #44508, .F. ) ;
#44311 = FILL_AREA_STYLE ('',( #43057 ) ) ;
#44312 = CARTESIAN_POINT ( 'NONE',  ( -2.499999999999996447, 16.29166666939785202, 4.330127018922195425 ) ) ;
#44314 = CARTESIAN_POINT ( 'NONE',  ( -4.458734124999999437, -31.31249999863440436, 0.000000000000000000 ) ) ;
#44313 = CARTESIAN_POINT ( 'NONE',  ( -2.499999999999996447, -94.83333333333332860, 4.330127018922195425 ) ) ;
#44315 = CARTESIAN_POINT ( 'NONE',  ( 1.339745962155615144, -95.70534180126146850, 4.999999999999999112 ) ) ;
#44316 = CARTESIAN_POINT ( 'NONE',  ( 4.458734124999999437, -83.06249999863440792, -5.460374474430324690E-16 ) ) ;
#44317 = CARTESIAN_POINT ( 'NONE',  ( -2.229367062499996610, 16.60416666803225638, 3.861377020970582219 ) ) ;
#44318 = CARTESIAN_POINT ( 'NONE',  ( -5.000000000000000000, -101.8749999972688158, 0.000000000000000000 ) ) ;
#44319 = CARTESIAN_POINT ( 'NONE',  ( -57.89159099828107458, -136.6875000013656063, -3.393966926194107447 ) ) ;
#44320 = CARTESIAN_POINT ( 'NONE',  ( 2.229367062500001939, -2.979166665301069550, 3.861377020970579999 ) ) ;
#44321 = CARTESIAN_POINT ( 'NONE',  ( -3.152548672688508926E-16, 21.18750000136559208, -5.148502694627439702 ) ) ;
#44322 = CARTESIAN_POINT ( 'NONE',  ( 9.457646018065525792E-16, -41.31249999863440792, 5.148502694627439702 ) ) ;
#44323 = CARTESIAN_POINT ( 'NONE',  ( 1.975475456537005874E-15, -80.74999999999998579, 5.000000000000000000 ) ) ;
#44324 = CARTESIAN_POINT ( 'NONE',  ( 9.457646018065525792E-16, 3.937500001365595192, 5.148502694627439702 ) ) ;
#44325 = VERTEX_POINT ( 'NONE', #7406 ) ;
#44326 = CARTESIAN_POINT ( 'NONE',  ( 4.458734125000000326, -26.14583333196773651, 2.574251347313718519 ) ) ;
#44327 = CARTESIAN_POINT ( 'NONE',  ( 2.229367062499998831, -71.64583333196773651, -3.861377020970580887 ) ) ;
#44328 = CARTESIAN_POINT ( 'NONE',  ( 2.500000000000002220, -105.5416666639354730, 4.330127018922192761 ) ) ;
#44329 = CARTESIAN_POINT ( 'NONE',  ( -2.229367062500000163, 27.52083333469892779, -3.861377020970580443 ) ) ;
#44330 = CARTESIAN_POINT ( 'NONE',  ( -4.458734124999997661, -109.4791666653010651, 2.574251347313722516 ) ) ;
#44331 = CARTESIAN_POINT ( 'NONE',  ( -4.458734124999999437, -73.64583333196773651, -2.574251347313719407 ) ) ;
#44332 = CARTESIAN_POINT ( 'NONE',  ( -3.535250795749689387E-16, -58.24999999999999289, -5.773502691896257311 ) ) ;
#44333 = PLANE ( 'NONE',  #6904 ) ;
#44334 = CARTESIAN_POINT ( 'NONE',  ( -2.500000000000000444, 27.95833333606451987, -4.330127018922193649 ) ) ;
#44335 = VERTEX_POINT ( 'NONE', #17047 ) ;
#44336 = CARTESIAN_POINT ( 'NONE',  ( 0.000000000000000000, -170.0000000000000000, 0.000000000000000000 ) ) ;
#44337 =( BOUNDED_CURVE ( )  B_SPLINE_CURVE ( 2, ( #14196, #29940, #15155, #38952, #19021, #58590, #24809, #34439, #54068 ),
 .UNSPECIFIED., .F., .F. ) 
 B_SPLINE_CURVE_WITH_KNOTS ( ( 3, 2, 2, 2, 3 ),
 ( 0.9089285714285714191, 0.9095238095238095122, 0.9107142857142856984, 0.9119047619047618847, 0.9124999999999999778 ),
 .UNSPECIFIED. ) 
 CURVE ( )  GEOMETRIC_REPRESENTATION_ITEM ( )  RATIONAL_B_SPLINE_CURVE ( ( 0.9330127018922194093, 0.9330127018922194093, 1.000000000000000000, 0.8660254037844387076, 1.000000000000000000, 0.8660254037844387076, 1.000000000000000000, 0.9330127018922194093, 0.9330127018922194093 ) ) 
 REPRESENTATION_ITEM ( '' )  );
#44338 = CARTESIAN_POINT ( 'NONE',  ( -4.999999999999998224, -56.79166666393547303, 2.886751345948131764 ) ) ;
#44339 = CARTESIAN_POINT ( 'NONE',  ( 2.499999999999998668, -18.33333333333333215, -4.330127018922193649 ) ) ;
#44340 = CARTESIAN_POINT ( 'NONE',  ( 2.229367062500001939, -19.97916666530107221, 3.861377020970579999 ) ) ;
#44341 = EDGE_CURVE ( 'NONE', #37188, #2754, #16729, .T. ) ;
#44342 = CARTESIAN_POINT ( 'NONE',  ( 4.458734124999998549, -83.72916666530106511, -2.574251347313721627 ) ) ;
#44343 = CARTESIAN_POINT ( 'NONE',  ( 4.458734124999999437, -167.7500000013655779, 1.846868145590737864 ) ) ;
#44344 = CARTESIAN_POINT ( 'NONE',  ( -5.000000000000000000, -19.95833333060214798, -2.886751345948128211 ) ) ;
#44346 = ORIENTED_EDGE ( 'NONE', *, *, #55157, .F. ) ;
#44345 = CARTESIAN_POINT ( 'NONE',  ( 4.458734125000001214, -47.89583333196775072, 2.574251347313718519 ) ) ;
#44347 = DIRECTION ( 'NONE',  ( 1.224646799147353207E-16, 1.000000000000000000, 0.000000000000000000 ) ) ;
#44348 = CARTESIAN_POINT ( 'NONE',  ( -6.972266317189433020E-16, -98.24999999999998579, -5.000000000000000000 ) ) ;
#44350 = VERTEX_POINT ( 'NONE', #42426 ) ;
#44349 = CARTESIAN_POINT ( 'NONE',  ( -3.152548672688508926E-16, 4.187500001365595637, -5.148502694627439702 ) ) ;
#44351 = CARTESIAN_POINT ( 'NONE',  ( -2.500000000000000444, -87.04166666393547303, -4.330127018922193649 ) ) ;
#44352 = CARTESIAN_POINT ( 'NONE',  ( -5.000000000000000000, -64.08333333333332860, -2.886751345948128211 ) ) ;
#44353 = CARTESIAN_POINT ( 'NONE',  ( 4.458734124999999437, -157.6875000013655779, 0.000000000000000000 ) ) ;
#44354 = CARTESIAN_POINT ( 'NONE',  ( -2.229367062500000163, -38.72916666530107221, -3.861377020970580443 ) ) ;
#44355 = CARTESIAN_POINT ( 'NONE',  ( -1.339745962155613812, -77.08034179853029855, -5.000000000000000000 ) ) ;
#44356 = CARTESIAN_POINT ( 'NONE',  ( 5.000000000000000000, -162.0000000000000000, 0.000000000000000000 ) ) ;
#44357 = DIRECTION ( 'NONE',  ( 0.000000000000000000, 0.000000000000000000, 1.000000000000000000 ) ) ;
#44358 = CARTESIAN_POINT ( 'NONE',  ( -58.39396692619412477, -127.6875000013656063, 2.891590998281057701 ) ) ;
#44359 = CARTESIAN_POINT ( 'NONE',  ( -4.458734124999998549, -9.479166665301070438, 2.574251347313722516 ) ) ;
#44360 = CARTESIAN_POINT ( 'NONE',  ( -2.229367062499996610, -44.39583333196774362, 3.861377020970582219 ) ) ;
#44361 = ADVANCED_FACE ( 'NONE', ( #17982 ), #3216, .T. ) ;
#44362 = CARTESIAN_POINT ( 'NONE',  ( -5.000000000000000000, -7.874999997268813168, 0.000000000000000000 ) ) ;
#44363 = CARTESIAN_POINT ( 'NONE',  ( -3.152801135295367096, -150.0625000013655779, -3.152801135295367541 ) ) ;
#44364 = EDGE_CURVE ( 'NONE', #15422, #21297, #20433, .T. ) ;
#44365 = CARTESIAN_POINT ( 'NONE',  ( 2.229367062499998831, -87.89583333196773651, -3.861377020970580887 ) ) ;
#44366 = CARTESIAN_POINT ( 'NONE',  ( -58.24261429053147765, -150.2500000000000284, -3.805975901505573855 ) ) ;
#44367 = VERTEX_POINT ( 'NONE', #14046 ) ;
#44368 = DIRECTION ( 'NONE',  ( -1.000000000000000000, 0.000000000000000000, 3.305092117221761110E-15 ) ) ;
#44369 = CARTESIAN_POINT ( 'NONE',  ( -1.339745962155613812, -69.08034179853028434, -5.000000000000000000 ) ) ;
#44370 = CARTESIAN_POINT ( 'NONE',  ( -58.80597590150559739, -150.1250000027312126, 3.242614290531460330 ) ) ;
#44371 = CARTESIAN_POINT ( 'NONE',  ( -2.500000000000000444, -62.16666666666666430, -4.330127018922193649 ) ) ;
#44372 = ORIENTED_EDGE ( 'NONE', *, *, #21656, .F. ) ;
#44373 = ADVANCED_FACE ( 'NONE', ( #33670 ), #28838, .F. ) ;
#44374 = CARTESIAN_POINT ( 'NONE',  ( 4.458734125000001214, 2.104166668032262599, 2.574251347313718519 ) ) ;
#44375 = CARTESIAN_POINT ( 'NONE',  ( 0.000000000000000000, -170.0000000000000000, 0.000000000000000000 ) ) ;
#44376 = CARTESIAN_POINT ( 'NONE',  ( 2.229367062499998831, -16.89583333196773651, -3.861377020970580887 ) ) ;
#44377 = CARTESIAN_POINT ( 'NONE',  ( -2.499999999999996447, -100.7083333306021444, 4.330127018922195425 ) ) ;
#44378 = CARTESIAN_POINT ( 'NONE',  ( -2.229367062499996610, -4.145833331967739177, 3.861377020970582219 ) ) ;
#44379 = CARTESIAN_POINT ( 'NONE',  ( 5.000000000000000888, -55.45833333060214443, 2.886751345948126879 ) ) ;
#44380 = CARTESIAN_POINT ( 'NONE',  ( -4.458734124999999437, -148.9375000013656063, -5.460374474430324690E-16 ) ) ;
#44381 =( BOUNDED_CURVE ( )  B_SPLINE_CURVE ( 2, ( #46112, #12007, #31634, #51271, #21991, #7204, #23251, #62810, #23575 ),
 .UNSPECIFIED., .F., .F. ) 
 B_SPLINE_CURVE_WITH_KNOTS ( ( 3, 2, 2, 2, 3 ),
 ( 0.6229166666666666741, 0.6236111111111111160, 0.6250000000000000000, 0.6263888888888888840, 0.6270833333333333259 ),
 .UNSPECIFIED. ) 
 CURVE ( )  GEOMETRIC_REPRESENTATION_ITEM ( )  RATIONAL_B_SPLINE_CURVE ( ( 0.9330127018922194093, 0.9330127018922194093, 1.000000000000000000, 0.8660254037844387076, 1.000000000000000000, 0.8660254037844387076, 1.000000000000000000, 0.9330127018922194093, 0.9330127018922194093 ) ) 
 REPRESENTATION_ITEM ( '' )  );
#44382 = CARTESIAN_POINT ( 'NONE',  ( 2.229367062499998831, 22.10416666803225993, -3.861377020970580887 ) ) ;
#44383 = ORIENTED_EDGE ( 'NONE', *, *, #43292, .F. ) ;
#44384 = CARTESIAN_POINT ( 'NONE',  ( -3.152548672688508926E-16, -99.56249999863440792, -5.148502694627439702 ) ) ;
#44385 = DIRECTION ( 'NONE',  ( 0.9396926207859143121, 1.150791560227857665E-16, -0.3420201433256525592 ) ) ;
#44386 = CARTESIAN_POINT ( 'NONE',  ( 0.000000000000000000, -170.0000000000000000, 0.000000000000000000 ) ) ;
#44387 = CARTESIAN_POINT ( 'NONE',  ( -3.152548672688508926E-16, -11.56249999863440792, -5.148502694627439702 ) ) ;
#44388 = CARTESIAN_POINT ( 'NONE',  ( 1.339745962155615144, -39.58034179853028434, 4.999999999999999112 ) ) ;
#44389 = CARTESIAN_POINT ( 'NONE',  ( -6.972266317189433020E-16, -97.24999999999998579, -5.000000000000000000 ) ) ;
#44390 = CARTESIAN_POINT ( 'NONE',  ( -6.972266317189433020E-16, -67.25000000000000000, -5.000000000000000000 ) ) ;
#44391 = EDGE_CURVE ( 'NONE', #57684, #248, #25315, .T. ) ;
#44392 = CARTESIAN_POINT ( 'NONE',  ( 2.500000000000002220, -39.54166666393548013, 4.330127018922192761 ) ) ;
#44393 = CARTESIAN_POINT ( 'NONE',  ( -1.339745962155613812, 20.91965820146970501, -5.000000000000000000 ) ) ;
#44394 = CARTESIAN_POINT ( 'NONE',  ( -4.458734124999999437, 11.60416666803225993, -2.574251347313719407 ) ) ;
#44395 = CARTESIAN_POINT ( 'NONE',  ( 2.499999999999999112, -7.216878364870334295, -7.063244554130005959 ) ) ;
#44396 = CARTESIAN_POINT ( 'NONE',  ( 0.000000000000000000, -170.0000000000000000, 5.000000000000000000 ) ) ;
#44397 = CARTESIAN_POINT ( 'NONE',  ( -4.458734124999999437, 17.68750000136559208, 0.000000000000000000 ) ) ;
#44398 = CARTESIAN_POINT ( 'NONE',  ( 9.457646018065525792E-16, -63.06249999863440081, 5.148502694627439702 ) ) ;
#44399 = ORIENTED_EDGE ( 'NONE', *, *, #20929, .F. ) ;
#44400 = CARTESIAN_POINT ( 'NONE',  ( -4.458734124999999437, -7.645833331967734736, -2.574251347313719407 ) ) ;
#44401 = CARTESIAN_POINT ( 'NONE',  ( -1.339745962155613812, -31.20534180126147916, -5.000000000000000000 ) ) ;
#44402 = CARTESIAN_POINT ( 'NONE',  ( 5.000000000000000000, 2.583333333333333481, -2.886751345948129988 ) ) ;
#44403 = CARTESIAN_POINT ( 'NONE',  ( -2.071067811865478170, -139.4375000027312410, 5.000000000000000000 ) ) ;
#44404 = CARTESIAN_POINT ( 'NONE',  ( 1.975475456537005874E-15, -59.62499999726880873, 5.000000000000000000 ) ) ;
#44405 = CARTESIAN_POINT ( 'NONE',  ( 2.229367062500001939, -52.97916666530107221, 3.861377020970579999 ) ) ;
#44406 = CARTESIAN_POINT ( 'NONE',  ( 5.000000000000000888, -89.45833333060215864, 2.886751345948126879 ) ) ;
#44407 = CARTESIAN_POINT ( 'NONE',  ( -4.458734124999999437, -35.31249999863440792, 0.000000000000000000 ) ) ;
#44408 = CARTESIAN_POINT ( 'NONE',  ( -1.339745962155610925, 20.33034180399266688, 5.000000000000000000 ) ) ;
#44409 = DIRECTION ( 'NONE',  ( -0.000000000000000000, 1.000000000000000000, -0.000000000000000000 ) ) ;
#44410 = CARTESIAN_POINT ( 'NONE',  ( -3.152801135295367985, -154.0625000013656063, 3.152801135295367096 ) ) ;
#44411 = CARTESIAN_POINT ( 'NONE',  ( -5.000000000000000000, -46.08333333333333570, -2.886751345948128211 ) ) ;
#44412 = FACE_OUTER_BOUND ( 'NONE', #58320, .T. ) ;
#44413 = CARTESIAN_POINT ( 'NONE',  ( -59.82678653332929741, -135.0000000000000284, 0.3596868101039389365 ) ) ;
#44414 = VERTEX_POINT ( 'NONE', #25924 ) ;
#44415 = CARTESIAN_POINT ( 'NONE',  ( -4.458734124999998549, -102.2291666653010651, 2.574251347313722516 ) ) ;
#44416 = CARTESIAN_POINT ( 'NONE',  ( -2.229367062500000163, 3.270833334698929118, -3.861377020970580443 ) ) ;
#44417 = CARTESIAN_POINT ( 'NONE',  ( 1.975475456537005874E-15, -8.624999997268812280, 5.000000000000000000 ) ) ;
#44418 = CARTESIAN_POINT ( 'NONE',  ( 2.499999999999998668, -2.333333333333333037, -4.330127018922193649 ) ) ;
#44419 = EDGE_CURVE ( 'NONE', #50232, #50678, #27016, .T. ) ;
#44420 = CARTESIAN_POINT ( 'NONE',  ( -4.458734124999999437, -69.31249999863439371, 0.000000000000000000 ) ) ;
#44421 = DIRECTION ( 'NONE',  ( -0.000000000000000000, 1.000000000000000000, -0.000000000000000000 ) ) ;
#44422 = ADVANCED_FACE ( 'NONE', ( #1826 ), #31064, .F. ) ;
#44423 = ADVANCED_FACE ( 'NONE', ( #40709 ), #34945, .T. ) ;
#44424 = CARTESIAN_POINT ( 'NONE',  ( 2.499999999999998668, -1.208333330602148870, -4.330127018922193649 ) ) ;
#44426 = ORIENTED_EDGE ( 'NONE', *, *, #41684, .F. ) ;
#44425 = CARTESIAN_POINT ( 'NONE',  ( 9.457646018065525792E-16, -35.06249999863440792, 5.148502694627439702 ) ) ;
#44427 = CARTESIAN_POINT ( 'NONE',  ( -2.499999999999996447, -10.83333333333333393, 4.330127018922195425 ) ) ;
#44428 = CARTESIAN_POINT ( 'NONE',  ( 0.000000000000000000, -120.0000000000000000, 0.000000000000000000 ) ) ;
#44429 = ORIENTED_EDGE ( 'NONE', *, *, #56317, .F. ) ;
#44430 = CARTESIAN_POINT ( 'NONE',  ( 2.499999999999998668, -20.33333333333333570, -4.330127018922193649 ) ) ;
#44431 = CARTESIAN_POINT ( 'NONE',  ( 5.000000000000000000, -48.41666666666665719, -2.886751345948129988 ) ) ;
#44433 = CARTESIAN_POINT ( 'NONE',  ( 2.229367062499998831, -22.89583333196773651, -3.861377020970580887 ) ) ;
#44432 = CARTESIAN_POINT ( 'NONE',  ( 0.000000000000000000, -170.0000000000000000, 0.000000000000000000 ) ) ;
#44434 = CARTESIAN_POINT ( 'NONE',  ( 1.975475456537005874E-15, -3.750000000000001776, 5.000000000000000000 ) ) ;
#44435 = CARTESIAN_POINT ( 'NONE',  ( -3.152548672688508926E-16, -72.56249999863439371, -5.148502694627439702 ) ) ;
#44436 = CARTESIAN_POINT ( 'NONE',  ( -1.846868145590737420, -146.0000000013655779, 4.458734124999999437 ) ) ;
#44437 = CARTESIAN_POINT ( 'NONE',  ( -4.458734124999999437, -80.39583333196772230, -2.574251347313719407 ) ) ;
#44438 = CARTESIAN_POINT ( 'NONE',  ( -57.89159099828107458, -139.9375000013656063, -3.393966926194107447 ) ) ;
#44439 = EDGE_CURVE ( 'NONE', #54748, #41738, #26240, .T. ) ;
#44440 = CARTESIAN_POINT ( 'NONE',  ( 4.458734125000001214, -31.14583333196773651, 2.574251347313718519 ) ) ;
#44441 = CARTESIAN_POINT ( 'NONE',  ( 2.499999999999998668, -70.20833333060214443, -4.330127018922193649 ) ) ;
#44442 = VERTEX_POINT ( 'NONE', #49730 ) ;
#44443 = CARTESIAN_POINT ( 'NONE',  ( -6.972266317189433020E-16, -41.24999999999999289, -5.000000000000000000 ) ) ;
#44445 = ORIENTED_EDGE ( 'NONE', *, *, #33124, .F. ) ;
#44444 = EDGE_CURVE ( 'NONE', #50022, #15732, #52703, .T. ) ;
#44446 = CARTESIAN_POINT ( 'NONE',  ( -4.458734124999999437, -73.56249999863439371, 0.000000000000000000 ) ) ;
#44447 = CARTESIAN_POINT ( 'NONE',  ( 5.000000000000000000, 28.58333333333333215, -2.886751345948130876 ) ) ;
#44448 =( NAMED_UNIT ( * ) PLANE_ANGLE_UNIT ( ) SI_UNIT ( $, .RADIAN. ) );
#44449 = VERTEX_POINT ( 'NONE', #50050 ) ;
#44450 = CARTESIAN_POINT ( 'NONE',  ( 2.499999999999998668, 12.66666666666666607, -4.330127018922193649 ) ) ;
#44451 = CARTESIAN_POINT ( 'NONE',  ( 1.339745962155612702, -31.16965819600732956, -5.000000000000000000 ) ) ;
#44452 = CARTESIAN_POINT ( 'NONE',  ( -4.458734124999998549, -57.47916666530108643, 2.574251347313722516 ) ) ;
#44453 = CARTESIAN_POINT ( 'NONE',  ( 9.457646018065525792E-16, -4.312499998634408804, 5.148502694627439702 ) ) ;
#44454 = EDGE_LOOP ( 'NONE', ( #20476, #11640, #31080, #13586 ) ) ;
#44455 = CARTESIAN_POINT ( 'NONE',  ( -2.071067811865391128, -146.6875000000000568, -5.000000000000086153 ) ) ;
#44456 = LINE ( 'NONE', #30944, #35633 ) ;
#44457 = CARTESIAN_POINT ( 'NONE',  ( -2.229367062499996610, 11.85416666803225993, 3.861377020970582219 ) ) ;
#44458 = CARTESIAN_POINT ( 'NONE',  ( -53.51423613279429503, -139.2500000013656063, 4.591703134518082763 ) ) ;
#44459 = CARTESIAN_POINT ( 'NONE',  ( 1.975475456537005874E-15, -0.7499999999999996669, 5.000000000000000000 ) ) ;
#44460 = CARTESIAN_POINT ( 'NONE',  ( -3.152801135295367096, -162.0625000013656063, -3.152801135295367541 ) ) ;
#44461 = ORIENTED_EDGE ( 'NONE', *, *, #15856, .T. ) ;
#44462 = CARTESIAN_POINT ( 'NONE',  ( -2.229367062500000163, -83.47916666530106511, -3.861377020970580443 ) ) ;
#44463 = CARTESIAN_POINT ( 'NONE',  ( -4.999999999999998224, -69.79166666393547303, 2.886751345948131764 ) ) ;
#44464 = CARTESIAN_POINT ( 'NONE',  ( -3.152548672688508926E-16, 1.437500001365596525, -5.148502694627439702 ) ) ;
#44465 =( BOUNDED_CURVE ( )  B_SPLINE_CURVE ( 2, ( #44050, #44691, #24447, #20906, #39230, #332, #59509, #10599, #29895 ),
 .UNSPECIFIED., .F., .F. ) 
 B_SPLINE_CURVE_WITH_KNOTS ( ( 3, 2, 2, 2, 3 ),
 ( 0.4854166666666666630, 0.4861111111111111049, 0.4874999999999999889, 0.4888888888888888729, 0.4895833333333333148 ),
 .UNSPECIFIED. ) 
 CURVE ( )  GEOMETRIC_REPRESENTATION_ITEM ( )  RATIONAL_B_SPLINE_CURVE ( ( 0.9330127018922194093, 0.9330127018922194093, 1.000000000000000000, 0.8660254037844387076, 1.000000000000000000, 0.8660254037844387076, 1.000000000000000000, 0.9330127018922194093, 0.9330127018922194093 ) ) 
 REPRESENTATION_ITEM ( '' )  );
#44466 = CARTESIAN_POINT ( 'NONE',  ( -5.000000000000000000, -82.99999999999998579, 0.000000000000000000 ) ) ;
#44467 = CARTESIAN_POINT ( 'NONE',  ( -6.972266317189433020E-16, 1.750000000000000444, -5.000000000000000000 ) ) ;
#44468 = CARTESIAN_POINT ( 'NONE',  ( 4.458734124999999437, -64.06249999863440792, -5.460374474430324690E-16 ) ) ;
#44469 = CARTESIAN_POINT ( 'NONE',  ( -5.000000000000000000, -24.95833333060214798, -2.886751345948128211 ) ) ;
#44470 = DIRECTION ( 'NONE',  ( 0.000000000000000000, 0.000000000000000000, 1.000000000000000000 ) ) ;
#44471 = CARTESIAN_POINT ( 'NONE',  ( 1.339745962155612702, -78.16965819600731891, -5.000000000000000000 ) ) ;
#44472 = DIRECTION ( 'NONE',  ( -0.000000000000000000, 1.000000000000000000, -0.000000000000000000 ) ) ;
#44473 = CARTESIAN_POINT ( 'NONE',  ( -3.152548672688508926E-16, -43.56249999863440081, -5.148502694627439702 ) ) ;
#44474 = CARTESIAN_POINT ( 'NONE',  ( -3.152548672688508926E-16, -29.81249999863440436, -5.148502694627439702 ) ) ;
#44475 = CARTESIAN_POINT ( 'NONE',  ( 4.458734124999998549, 9.020833334698927786, -2.574251347313721627 ) ) ;
#44476 = CARTESIAN_POINT ( 'NONE',  ( 2.071067811865644703, -150.8125000000000284, -4.999999999999831246 ) ) ;
#44477 = CARTESIAN_POINT ( 'NONE',  ( -2.500000000000000444, 19.83333333333333570, -4.330127018922193649 ) ) ;
#44478 = CARTESIAN_POINT ( 'NONE',  ( 3.535533905932738197, -148.0000000027311842, -3.535533905932738197 ) ) ;
#44479 = CARTESIAN_POINT ( 'NONE',  ( -4.729367062499999719, -110.7187499979515906, 0.000000000000000000 ) ) ;
#44480 = CARTESIAN_POINT ( 'NONE',  ( -4.458734124999998549, -35.22916666530107221, 2.574251347313722516 ) ) ;
#44481 = CARTESIAN_POINT ( 'NONE',  ( -2.499999999999996447, -71.70833333060214443, 4.330127018922195425 ) ) ;
#44482 = CARTESIAN_POINT ( 'NONE',  ( -54.64476657466781973, -144.0625000013656063, -4.444560631937228834 ) ) ;
#44483 = CARTESIAN_POINT ( 'NONE',  ( 1.975475456537005874E-15, -24.62499999726881583, 5.000000000000000000 ) ) ;
#44484 = CARTESIAN_POINT ( 'NONE',  ( -6.875000000000001776, -4.690970937165714894, -7.298562697733108173 ) ) ;
#44485 = CARTESIAN_POINT ( 'NONE',  ( -4.458734124999999437, -78.56249999863440792, 0.000000000000000000 ) ) ;
#44486 = CARTESIAN_POINT ( 'NONE',  ( -4.458734124999999437, -167.2500000013655779, -1.846868145590735644 ) ) ;
#44487 = CARTESIAN_POINT ( 'NONE',  ( -2.229367062500000163, -35.47916666530107221, -3.861377020970580443 ) ) ;
#44488 = CARTESIAN_POINT ( 'NONE',  ( -5.000000000000000000, -33.08333333333332860, -2.886751345948128211 ) ) ;
#44489 = CARTESIAN_POINT ( 'NONE',  ( 5.000000000000000888, -45.45833333060214443, 2.886751345948126879 ) ) ;
#44490 = CARTESIAN_POINT ( 'NONE',  ( 1.060575238724906964E-15, -21.75000000000000000, 5.773502691896257311 ) ) ;
#44491 = CARTESIAN_POINT ( 'NONE',  ( -4.458734125000001214, -141.8750000013656063, 1.846868145590734089 ) ) ;
#44492 = ORIENTED_EDGE ( 'NONE', *, *, #29931, .T. ) ;
#44493 = CARTESIAN_POINT ( 'NONE',  ( -2.499999999999996447, -89.70833333060214443, 4.330127018922195425 ) ) ;
#44494 = VERTEX_POINT ( 'NONE', #59715 ) ;
#44495 = CARTESIAN_POINT ( 'NONE',  ( 9.457646018065525792E-16, -61.31249999863440792, 5.148502694627439702 ) ) ;
#44496 = CARTESIAN_POINT ( 'NONE',  ( -5.000000000000000000, 23.12500000273118417, 0.000000000000000000 ) ) ;
#44497 = CARTESIAN_POINT ( 'NONE',  ( -9.184850993605147944E-16, -162.2500000000000000, 5.000000000000000000 ) ) ;
#44498 = CARTESIAN_POINT ( 'NONE',  ( 5.000000000000000000, 13.58333333333333215, -2.886751345948129988 ) ) ;
#44499 = CARTESIAN_POINT ( 'NONE',  ( 2.229367062499998831, -49.64583333196772941, -3.861377020970580887 ) ) ;
#44500 = CARTESIAN_POINT ( 'NONE',  ( -3.152548672688508926E-16, -7.562499998634404363, -5.148502694627439702 ) ) ;
#44501 = CARTESIAN_POINT ( 'NONE',  ( -1.339745962155613812, 3.919658201469705894, -5.000000000000000000 ) ) ;
#44502 = EDGE_CURVE ( 'NONE', #12181, #27389, #33578, .T. ) ;
#44503 = CARTESIAN_POINT ( 'NONE',  ( 5.000000000000000888, -165.0625000027312126, -2.071067811865475505 ) ) ;
#44504 = CARTESIAN_POINT ( 'NONE',  ( 5.000000000000000888, -158.0625000027312126, -2.071067811865475505 ) ) ;
#44505 = DIRECTION ( 'NONE',  ( -0.000000000000000000, 1.000000000000000000, -0.000000000000000000 ) ) ;
#44507 = CARTESIAN_POINT ( 'NONE',  ( 2.229367062500001939, -18.97916666530106866, 3.861377020970579999 ) ) ;
#44506 = CARTESIAN_POINT ( 'NONE',  ( 1.339745962155602488, 21.41965820146970145, 5.000000000000007105 ) ) ;
#44508 = EDGE_CURVE ( 'NONE', #62283, #20660, #1191, .T. ) ;
#44509 = CARTESIAN_POINT ( 'NONE',  ( -1.049326080737009628E-13, -3.624999997268818053, 5.000000000000000000 ) ) ;
#44510 = CARTESIAN_POINT ( 'NONE',  ( -2.229367062500000163, -53.47916666530107221, -3.861377020970580443 ) ) ;
#44511 = CARTESIAN_POINT ( 'NONE',  ( 1.846868145590736310, -154.8750000013655779, 4.458734124999999437 ) ) ;
#44512 = EDGE_CURVE ( 'NONE', #14934, #45853, #31897, .T. ) ;
#44513 = CARTESIAN_POINT ( 'NONE',  ( 2.500000000000002220, -53.54166666393548013, 4.330127018922192761 ) ) ;
#44514 = ORIENTED_EDGE ( 'NONE', *, *, #31853, .F. ) ;
#44515 = CARTESIAN_POINT ( 'NONE',  ( 1.339745962155612702, -26.29465819873852084, -5.000000000000000000 ) ) ;
#44516 = CARTESIAN_POINT ( 'NONE',  ( 2.229367062499998831, 3.104166668032259935, -3.861377020970580887 ) ) ;
#44517 = VERTEX_POINT ( 'NONE', #39746 ) ;
#44518 =( BOUNDED_CURVE ( )  B_SPLINE_CURVE ( 2, ( #19850, #39464, #34643, #54267, #60060, #10207, #29809, #49442, #6350 ),
 .UNSPECIFIED., .F., .F. ) 
 B_SPLINE_CURVE_WITH_KNOTS ( ( 3, 2, 2, 2, 3 ),
 ( 0.7249999999999996447, 0.7291666666666662966, 0.7333333333333329485, 0.7374999999999998224, 0.7416666666666664742 ),
 .UNSPECIFIED. ) 
 CURVE ( )  GEOMETRIC_REPRESENTATION_ITEM ( )  RATIONAL_B_SPLINE_CURVE ( ( 1.000000000000005995, 0.9238795325112806323, 1.000000000000000000, 0.9238795325112867385, 1.000000000000000000, 0.9238795325112867385, 1.000000000000000000, 0.9238795325112908463, 0.9999999999999958922 ) ) 
 REPRESENTATION_ITEM ( '' )  );
#44519 = CARTESIAN_POINT ( 'NONE',  ( 2.499999999999998668, 11.79166666939785202, -4.330127018922193649 ) ) ;
#44520 = CARTESIAN_POINT ( 'NONE',  ( 4.458734125000000326, -156.3750000013655779, -1.846868145590734978 ) ) ;
#44521 = EDGE_CURVE ( 'NONE', #56591, #39148, #46734, .T. ) ;
#44522 = EDGE_LOOP ( 'NONE', ( #46311, #61704, #37250, #24997 ) ) ;
#44523 = ADVANCED_FACE ( 'NONE', ( #36529 ), #56161, .T. ) ;
#44524 = DIRECTION ( 'NONE',  ( -0.000000000000000000, -0.000000000000000000, 1.000000000000000000 ) ) ;
#44525 = CARTESIAN_POINT ( 'NONE',  ( -56.66612745406270335, -130.3125000000000284, -5.149110718188516067 ) ) ;
#44526 = CARTESIAN_POINT ( 'NONE',  ( 1.339745962155612702, -86.29465819873851729, -5.000000000000000000 ) ) ;
#44527 = CARTESIAN_POINT ( 'NONE',  ( -2.229367062499996610, -42.39583333196773651, 3.861377020970582219 ) ) ;
#44528 = ORIENTED_EDGE ( 'NONE', *, *, #10172, .T. ) ;
#44529 = AXIS2_PLACEMENT_3D ( 'NONE', #20982, #50563, #54755 ) ;
#44530 = EDGE_CURVE ( 'NONE', #44325, #1513, #54045, .T. ) ;
#44531 = CARTESIAN_POINT ( 'NONE',  ( 2.500000000000002220, 9.458333336064519870, 4.330127018922192761 ) ) ;
#44532 = CARTESIAN_POINT ( 'NONE',  ( 4.458734125000001214, 16.10416666803225993, 2.574251347313718519 ) ) ;
#44533 = LINE ( 'NONE', #29403, #44051 ) ;
#44534 = ORIENTED_EDGE ( 'NONE', *, *, #30204, .T. ) ;
#44535 = CARTESIAN_POINT ( 'NONE',  ( -4.458734124999999437, 28.60416666803226349, -2.574251347313719407 ) ) ;
#44536 = CARTESIAN_POINT ( 'NONE',  ( -56.48576386720575471, -152.7500000013655779, -4.591703134518078322 ) ) ;
#44537 = CARTESIAN_POINT ( 'NONE',  ( 0.000000000000000000, -120.0000000000000000, 0.000000000000000000 ) ) ;
#44538 = CARTESIAN_POINT ( 'NONE',  ( 1.339745962155612702, -39.29465819873851729, -5.000000000000000000 ) ) ;
#44539 = LINE ( 'NONE', #10771, #52812 ) ;
#44540 = CARTESIAN_POINT ( 'NONE',  ( 4.458734124999998549, -66.72916666530106511, -2.574251347313721627 ) ) ;
#44541 = CARTESIAN_POINT ( 'NONE',  ( -2.499999999999996447, 10.29166666939785024, 4.330127018922195425 ) ) ;
#44542 = CARTESIAN_POINT ( 'NONE',  ( 2.229367062499998831, 18.35416666803225993, -3.861377020970580887 ) ) ;
#44543 = CARTESIAN_POINT ( 'NONE',  ( -4.999999999999998224, 18.08333333333333215, 2.886751345948131764 ) ) ;
#44544 = CARTESIAN_POINT ( 'NONE',  ( 9.457646018065525792E-16, -50.31249999863440792, 5.148502694627439702 ) ) ;
#44545 = CARTESIAN_POINT ( 'NONE',  ( -5.000000000000000000, -11.87499999726881761, 0.000000000000000000 ) ) ;
#44546 = CARTESIAN_POINT ( 'NONE',  ( 0.000000000000000000, -170.0000000000000000, 0.000000000000000000 ) ) ;
#44547 = CARTESIAN_POINT ( 'NONE',  ( -6.972266317189433020E-16, 18.87500000273118772, -5.000000000000000000 ) ) ;
#44548 = DIRECTION ( 'NONE',  ( -0.000000000000000000, 1.000000000000000000, -0.000000000000000000 ) ) ;
#44549 = CARTESIAN_POINT ( 'NONE',  ( 4.458734124999999437, -109.8124999986343937, -5.460374474430324690E-16 ) ) ;
#44550 = CARTESIAN_POINT ( 'NONE',  ( 4.458734124999999437, -14.06249999863440436, -5.460374474430324690E-16 ) ) ;
#44551 = ORIENTED_EDGE ( 'NONE', *, *, #22300, .F. ) ;
#44552 = CARTESIAN_POINT ( 'NONE',  ( -4.999999999999998224, -46.79166666393547303, 2.886751345948131764 ) ) ;
#44553 = CARTESIAN_POINT ( 'NONE',  ( -2.229367062500000163, -104.4791666653010651, -3.861377020970580443 ) ) ;
#44554 = CARTESIAN_POINT ( 'NONE',  ( -3.535533905932737309, -162.7500000027312126, -3.535533905932738197 ) ) ;
#44555 = CARTESIAN_POINT ( 'NONE',  ( -2.229367062499996610, -98.39583333196773651, 3.861377020970582219 ) ) ;
#44556 = DIRECTION ( 'NONE',  ( 0.000000000000000000, 0.000000000000000000, 1.000000000000000000 ) ) ;
#44557 = CARTESIAN_POINT ( 'NONE',  ( 2.499999999999998668, -55.20833333060214443, -4.330127018922193649 ) ) ;
#44558 = CARTESIAN_POINT ( 'NONE',  ( -5.000000000000000000, 19.04166666939784847, -2.886751345948128211 ) ) ;
#44559 = CARTESIAN_POINT ( 'NONE',  ( -58.39396692619412477, -125.4375000013656063, 2.891590998281057701 ) ) ;
#44560 = CARTESIAN_POINT ( 'NONE',  ( -59.44456063193725015, -146.5625000013656063, -0.3552334253322034230 ) ) ;
#44561 = CARTESIAN_POINT ( 'NONE',  ( 9.457646018065525792E-16, -18.06249999863440792, 5.148502694627439702 ) ) ;
#44562 = CARTESIAN_POINT ( 'NONE',  ( -4.458734124999999437, 5.354166668032262599, -2.574251347313719407 ) ) ;
#44563 = CARTESIAN_POINT ( 'NONE',  ( 2.229367062500001939, -64.22916666530106511, 3.861377020970579999 ) ) ;
#44564 = CARTESIAN_POINT ( 'NONE',  ( -2.071067811865432873, -141.8125000027311842, -5.000000000000041744 ) ) ;
#44565 = CARTESIAN_POINT ( 'NONE',  ( -2.229367062500000163, -20.47916666530107221, -3.861377020970580443 ) ) ;
#44566 = CARTESIAN_POINT ( 'NONE',  ( -5.000000000000000000, -79.87499999726881583, 0.000000000000000000 ) ) ;
#44567 = CARTESIAN_POINT ( 'NONE',  ( 2.071067811865475505, -156.8125000000000284, -5.000000000000000888 ) ) ;
#44568 = CARTESIAN_POINT ( 'NONE',  ( 2.499999999999998668, -4.333333333333334814, -4.330127018922193649 ) ) ;
#44569 = VERTEX_POINT ( 'NONE', #7905 ) ;
#44570 = CARTESIAN_POINT ( 'NONE',  ( 2.229367062500001939, -44.22916666530106511, 3.861377020970579999 ) ) ;
#44571 =( BOUNDED_CURVE ( )  B_SPLINE_CURVE ( 2, ( #55002, #58556, #24142, #24454, #24776, #997, #14794, #4516, #15452 ),
 .UNSPECIFIED., .F., .F. ) 
 B_SPLINE_CURVE_WITH_KNOTS ( ( 3, 2, 2, 2, 3 ),
 ( 0.1767857142857142960, 0.1773809523809523891, 0.1785714285714285754, 0.1797619047619047616, 0.1803571428571428548 ),
 .UNSPECIFIED. ) 
 CURVE ( )  GEOMETRIC_REPRESENTATION_ITEM ( )  RATIONAL_B_SPLINE_CURVE ( ( 0.9330127018922194093, 0.9330127018922194093, 1.000000000000000000, 0.8660254037844387076, 1.000000000000000000, 0.8660254037844387076, 1.000000000000000000, 0.9330127018922194093, 0.9330127018922194093 ) ) 
 REPRESENTATION_ITEM ( '' )  );
#44572 = DIRECTION ( 'NONE',  ( -0.000000000000000000, 1.000000000000000000, -0.000000000000000000 ) ) ;
#44573 = DIRECTION ( 'NONE',  ( -0.000000000000000000, 1.000000000000000000, -0.000000000000000000 ) ) ;
#44574 = CARTESIAN_POINT ( 'NONE',  ( 5.000000000000000000, 28.58333333333333215, -2.886751345948129988 ) ) ;
#44575 = CARTESIAN_POINT ( 'NONE',  ( 9.457646018065525792E-16, -93.06249999863440792, 5.148502694627439702 ) ) ;
#44576 = CARTESIAN_POINT ( 'NONE',  ( -2.229367062499996610, 21.60416666803226349, 3.861377020970582219 ) ) ;
#44577 = VECTOR ( 'NONE', #17108, 1000.000000000000000 ) ;
#44578 = CARTESIAN_POINT ( 'NONE',  ( 2.229367062499998831, 7.354166668032259935, -3.861377020970580887 ) ) ;
#44579 = CARTESIAN_POINT ( 'NONE',  ( 2.499999999999998668, -82.33333333333332860, -4.330127018922193649 ) ) ;
#44580 = CARTESIAN_POINT ( 'NONE',  ( 3.061616997868383141E-16, -165.8750000027312126, -5.000000000000000000 ) ) ;
#44581 = CARTESIAN_POINT ( 'NONE',  ( 5.000000000000000000, -82.50000000000000000, -6.123233995736766282E-16 ) ) ;
#44582 = CARTESIAN_POINT ( 'NONE',  ( -3.152548672688508926E-16, 21.18750000136559208, -5.148502694627439702 ) ) ;
#44583 = CARTESIAN_POINT ( 'NONE',  ( -3.535250795749689387E-16, -73.25000000000000000, -5.773502691896257311 ) ) ;
#44584 = CARTESIAN_POINT ( 'NONE',  ( 5.000000000000000000, 6.708333336064521646, -2.886751345948129988 ) ) ;
#44585 = EDGE_LOOP ( 'NONE', ( #48465, #29176, #47012 ) ) ;
#44586 = CARTESIAN_POINT ( 'NONE',  ( 1.339745962155612702, -80.16965819600733312, -5.000000000000000000 ) ) ;
#44587 = ORIENTED_EDGE ( 'NONE', *, *, #21251, .F. ) ;
#44588 = CARTESIAN_POINT ( 'NONE',  ( 6.123233995736766282E-16, -170.0000000000000000, -5.000000000000000000 ) ) ;
#44589 = CARTESIAN_POINT ( 'NONE',  ( -4.458734124999998549, -36.22916666530106511, 2.574251347313722516 ) ) ;
#44590 = CARTESIAN_POINT ( 'NONE',  ( -2.500000000000000444, -37.04166666393548013, -4.330127018922193649 ) ) ;
#44591 = ORIENTED_EDGE ( 'NONE', *, *, #95, .F. ) ;
#44592 = CARTESIAN_POINT ( 'NONE',  ( -59.59170313451811296, -146.7500000013655495, 1.485763867205729394 ) ) ;
#44593 = CARTESIAN_POINT ( 'NONE',  ( -4.458734124999999437, -10.31249999863440792, 0.000000000000000000 ) ) ;
#44595 = ORIENTED_EDGE ( 'NONE', *, *, #36609, .T. ) ;
#44594 = CARTESIAN_POINT ( 'NONE',  ( 4.458734124999998549, -12.97916666530107044, -2.574251347313721627 ) ) ;
#44596 = CARTESIAN_POINT ( 'NONE',  ( -5.000000000000000000, -81.08333333333332860, -2.886751345948128211 ) ) ;
#44597 = CARTESIAN_POINT ( 'NONE',  ( -3.152801135295367985, -167.8125000013656063, 3.152801135295367096 ) ) ;
#44598 = CARTESIAN_POINT ( 'NONE',  ( -3.152548672688508926E-16, -63.81249999863440792, -5.148502694627439702 ) ) ;
#44599 = CARTESIAN_POINT ( 'NONE',  ( 1.060575238724906964E-15, -79.62499999726881583, 5.773502691896257311 ) ) ;
#44601 = ORIENTED_EDGE ( 'NONE', *, *, #32342, .F. ) ;
#44600 = CARTESIAN_POINT ( 'NONE',  ( -2.499999999999996447, -17.83333333333333215, 4.330127018922195425 ) ) ;
#44602 = CARTESIAN_POINT ( 'NONE',  ( -50.01589407740564042, -143.6250000000000284, 0.3983568153799778022 ) ) ;
#44603 = CARTESIAN_POINT ( 'NONE',  ( 4.458734124999998549, -26.97916666530107221, -2.574251347313721627 ) ) ;
#44604 = CARTESIAN_POINT ( 'NONE',  ( 5.000000000000000888, -29.58333333333332860, 2.886751345948126879 ) ) ;
#44605 = ORIENTED_EDGE ( 'NONE', *, *, #6773, .T. ) ;
#44606 = APPLICATION_PROTOCOL_DEFINITION ( 'draft international standard', 'automotive_design', 1998, #38816 ) ;
#44607 = CARTESIAN_POINT ( 'NONE',  ( 2.730187237215162345E-16, -163.4375000013655779, -4.458734124999999437 ) ) ;
#44608 = CARTESIAN_POINT ( 'NONE',  ( 2.229367062500001939, -105.2291666653010651, 3.861377020970579999 ) ) ;
#44609 = CARTESIAN_POINT ( 'NONE',  ( 5.000000000000000000, -23.50000000000000000, -6.123233995736766282E-16 ) ) ;
#44610 = EDGE_LOOP ( 'NONE', ( #13357, #31456, #38310, #4430 ) ) ;
#44611 = CARTESIAN_POINT ( 'NONE',  ( -52.10840900171896806, -145.4375000013656063, 3.393966926194110556 ) ) ;
#44612 = CARTESIAN_POINT ( 'NONE',  ( 4.458734124999998549, -74.97916666530106511, -2.574251347313721627 ) ) ;
#44613 = CARTESIAN_POINT ( 'NONE',  ( -59.81910112700025905, -135.3125000027312126, -2.462841084822630311 ) ) ;
#44614 = CARTESIAN_POINT ( 'NONE',  ( -4.458734124999999437, -46.31249999863440792, 0.000000000000000000 ) ) ;
#44615 = CARTESIAN_POINT ( 'NONE',  ( 4.458734124999999437, -146.6875000013656063, 0.000000000000000000 ) ) ;
#44616 = CARTESIAN_POINT ( 'NONE',  ( -7.499999999999650058, -0.7583608255766450812, -7.446489218764574147 ) ) ;
#44617 = CARTESIAN_POINT ( 'NONE',  ( -2.229367062499996610, -49.14583333196772941, 3.861377020970582219 ) ) ;
#44618 = CARTESIAN_POINT ( 'NONE',  ( -58.24261429053147765, -135.2500000000000284, -3.805975901505573855 ) ) ;
#44619 = CARTESIAN_POINT ( 'NONE',  ( 2.229367062500001939, -11.97916666530107044, 3.861377020970579999 ) ) ;
#44620 = CARTESIAN_POINT ( 'NONE',  ( -2.499999999999996447, -99.83333333333332860, 4.330127018922195425 ) ) ;
#44621 = VECTOR ( 'NONE', #38278, 1000.000000000000000 ) ;
#44622 = CARTESIAN_POINT ( 'NONE',  ( 1.846868145590736310, -141.8750000013656063, 4.458734124999999437 ) ) ;
#44623 = CARTESIAN_POINT ( 'NONE',  ( -3.152548672688508926E-16, -31.81249999863440792, -5.148502694627439702 ) ) ;
#44624 = CARTESIAN_POINT ( 'NONE',  ( 5.000000000000000888, 4.541666669397852019, 2.886751345948126879 ) ) ;
#44625 = CARTESIAN_POINT ( 'NONE',  ( 2.500000000000002220, -50.66666666666666430, 4.330127018922192761 ) ) ;
#44626 = CARTESIAN_POINT ( 'NONE',  ( -53.51423613279429503, -133.2500000013656347, 4.591703134518082763 ) ) ;
#44627 = CARTESIAN_POINT ( 'NONE',  ( -4.458734124999999437, -73.56249999863439371, 0.000000000000000000 ) ) ;
#44628 = CARTESIAN_POINT ( 'NONE',  ( -9.184850993605147944E-16, -144.3750000027312126, 5.000000000000000000 ) ) ;
#44629 = CARTESIAN_POINT ( 'NONE',  ( -6.972266317189433020E-16, -54.12499999726880162, -5.000000000000000000 ) ) ;
#44630 = LINE ( 'NONE', #15374, #55207 ) ;
#44631 = CARTESIAN_POINT ( 'NONE',  ( 2.229367062499998831, 0.1041666680322607397, -3.861377020970580887 ) ) ;
#44632 = EDGE_LOOP ( 'NONE', ( #41748, #23557, #34972, #59786 ) ) ;
#44633 = CARTESIAN_POINT ( 'NONE',  ( 5.000000000000000888, 16.54166666939785202, 2.886751345948126879 ) ) ;
#44634 = CARTESIAN_POINT ( 'NONE',  ( 1.975475456537005874E-15, -57.74999999999999289, 5.000000000000000000 ) ) ;
#44636 = CARTESIAN_POINT ( 'NONE',  ( 2.229367062499998831, -36.64583333196773651, -3.861377020970580887 ) ) ;
#44635 = CARTESIAN_POINT ( 'NONE',  ( 5.000000000000000888, -94.58333333333332860, 2.886751345948126879 ) ) ;
#44637 = CARTESIAN_POINT ( 'NONE',  ( -6.972266317189433020E-16, -71.25000000000000000, -5.000000000000000000 ) ) ;
#44638 = CARTESIAN_POINT ( 'NONE',  ( -4.458734124999998549, -83.47916666530107932, 2.574251347313722516 ) ) ;
#44639 = CARTESIAN_POINT ( 'NONE',  ( -2.229367062499996610, 19.60416666803225993, 3.861377020970582219 ) ) ;
#44640 = DIRECTION ( 'NONE',  ( -0.000000000000000000, 1.000000000000000000, -0.000000000000000000 ) ) ;
#44641 = CARTESIAN_POINT ( 'NONE',  ( -53.51423613279429503, -139.2500000013656063, 4.591703134518082763 ) ) ;
#44642 = CARTESIAN_POINT ( 'NONE',  ( 2.229367062500001939, -3.979166665301070438, 3.861377020970579999 ) ) ;
#44643 = CARTESIAN_POINT ( 'NONE',  ( -3.152548672688508926E-16, 22.18750000136559564, -5.148502694627439702 ) ) ;
#44644 = CARTESIAN_POINT ( 'NONE',  ( 4.458734124999999437, -41.06249999863440081, -5.460374474430324690E-16 ) ) ;
#44645 = CYLINDRICAL_SURFACE ( 'NONE', #34606, 5.000000000000000000 ) ;
#44646 = CARTESIAN_POINT ( 'NONE',  ( -4.458734124999999437, -4.312499998634401699, 0.000000000000000000 ) ) ;
#44647 = VERTEX_POINT ( 'NONE', #13037 ) ;
#44648 = CARTESIAN_POINT ( 'NONE',  ( -2.229367062499996610, -29.39583333196774007, 3.861377020970582219 ) ) ;
#44649 = CARTESIAN_POINT ( 'NONE',  ( 9.457646018065525792E-16, -73.06249999863440792, 5.148502694627439702 ) ) ;
#44650 = CARTESIAN_POINT ( 'NONE',  ( 5.000000000000000888, -107.4583333306021302, 2.886751345948126879 ) ) ;
#44651 =( BOUNDED_CURVE ( )  B_SPLINE_CURVE ( 2, ( #58546, #47085, #43423, #17175, #36800, #22328, #41929, #6112, #24764 ),
 .UNSPECIFIED., .F., .F. ) 
 B_SPLINE_CURVE_WITH_KNOTS ( ( 3, 2, 2, 2, 3 ),
 ( 0.01250000000000000069, 0.01309523809523809555, 0.01428571428571428527, 0.01547619047619047672, 0.01607142857142857331 ),
 .UNSPECIFIED. ) 
 CURVE ( )  GEOMETRIC_REPRESENTATION_ITEM ( )  RATIONAL_B_SPLINE_CURVE ( ( 0.9330127018922192983, 0.9330127018922194093, 1.000000000000000000, 0.8660254037844387076, 1.000000000000000000, 0.8660254037844387076, 1.000000000000000000, 0.9330127018922191873, 0.9330127018922194093 ) ) 
 REPRESENTATION_ITEM ( '' )  );
#44652 = CARTESIAN_POINT ( 'NONE',  ( -4.458734124999998549, 23.77083333469892423, 2.574251347313722516 ) ) ;
#44653 = CARTESIAN_POINT ( 'NONE',  ( 1.339745962155612702, 26.83034180399266333, -5.000000000000000000 ) ) ;
#44654 = DIRECTION ( 'NONE',  ( -0.000000000000000000, 1.000000000000000000, -0.000000000000000000 ) ) ;
#44655 = CARTESIAN_POINT ( 'NONE',  ( -4.458734124999999437, -72.64583333196773651, -2.574251347313719407 ) ) ;
#44656 = CARTESIAN_POINT ( 'NONE',  ( 2.500000000000002220, -57.66666666666667140, 4.330127018922192761 ) ) ;
#44657 = CARTESIAN_POINT ( 'NONE',  ( 2.499999999999998668, 25.79166666939785202, -4.330127018922193649 ) ) ;
#44658 = ORIENTED_EDGE ( 'NONE', *, *, #33062, .T. ) ;
#44659 = LINE ( 'NONE', #621, #1681 ) ;
#44660 = ADVANCED_FACE ( 'NONE', ( #27510 ), #31375, .T. ) ;
#44661 = CARTESIAN_POINT ( 'NONE',  ( 0.000000000000000000, -170.0000000000000000, 0.000000000000000000 ) ) ;
#44662 = CARTESIAN_POINT ( 'NONE',  ( 1.060575238724906964E-15, -16.75000000000000355, 5.773502691896257311 ) ) ;
#44663 = CARTESIAN_POINT ( 'NONE',  ( 2.229367062499998831, -22.64583333196773651, -3.861377020970580887 ) ) ;
#44664 = CARTESIAN_POINT ( 'NONE',  ( 4.458734124999999437, -82.81249999863440792, -5.460374474430324690E-16 ) ) ;
#44665 =( BOUNDED_CURVE ( )  B_SPLINE_CURVE ( 2, ( #18841, #38459, #44877, #59037, #45515, #50019, #50346, #15292, #25582 ),
 .UNSPECIFIED., .F., .F. ) 
 B_SPLINE_CURVE_WITH_KNOTS ( ( 3, 2, 2, 2, 3 ),
 ( 0.1750000000000001554, 0.1791666666666668351, 0.1833333333333334869, 0.1875000000000001665, 0.1916666666666668462 ),
 .UNSPECIFIED. ) 
 CURVE ( )  GEOMETRIC_REPRESENTATION_ITEM ( )  RATIONAL_B_SPLINE_CURVE ( ( 0.9999999999999970024, 0.9238795325112897361, 1.000000000000000000, 0.9238795325112867385, 1.000000000000000000, 0.9238795325112867385, 1.000000000000000000, 0.9238795325112837409, 1.000000000000003109 ) ) 
 REPRESENTATION_ITEM ( '' )  );
#44666 = CARTESIAN_POINT ( 'NONE',  ( 5.000000000000000000, -21.29166666393548013, -2.886751345948129988 ) ) ;
#44668 = ORIENTED_EDGE ( 'NONE', *, *, #8230, .T. ) ;
#44667 = CARTESIAN_POINT ( 'NONE',  ( -3.152548672688508926E-16, -51.56249999863441502, -5.148502694627439702 ) ) ;
#44669 = CARTESIAN_POINT ( 'NONE',  ( 5.000000000000000888, -70.45833333060214443, 2.886751345948126879 ) ) ;
#44670 = FACE_OUTER_BOUND ( 'NONE', #52190, .T. ) ;
#44672 = ORIENTED_EDGE ( 'NONE', *, *, #7213, .F. ) ;
#44671 = CARTESIAN_POINT ( 'NONE',  ( -2.229367062499996610, -0.3958333319677397322, 3.861377020970582219 ) ) ;
#44673 = CARTESIAN_POINT ( 'NONE',  ( -57.19623071787016499, -151.3750000013656063, 4.297418129356382899 ) ) ;
#44674 = CARTESIAN_POINT ( 'NONE',  ( 5.000000000000000000, -68.41666666666667140, -2.886751345948129988 ) ) ;
#44675 = CARTESIAN_POINT ( 'NONE',  ( -3.152801135295367985, -154.0625000013656063, 3.152801135295367096 ) ) ;
#44676 = CARTESIAN_POINT ( 'NONE',  ( 4.458734124999998549, -45.97916666530106511, -2.574251347313721627 ) ) ;
#44677 = CARTESIAN_POINT ( 'NONE',  ( -5.000000000000000000, -80.95833333060214443, -2.886751345948128211 ) ) ;
#44678 = CARTESIAN_POINT ( 'NONE',  ( 3.535533905932738197, -162.8750000000000284, -3.535533905932738197 ) ) ;
#44679 = LINE ( 'NONE', #50148, #7695 ) ;
#44680 = CARTESIAN_POINT ( 'NONE',  ( -54.64476657466781973, -126.0625000013655921, -4.444560631937228834 ) ) ;
#44681 = CARTESIAN_POINT ( 'NONE',  ( 2.229367062500001939, -12.22916666530107044, 3.861377020970579999 ) ) ;
#44682 = CARTESIAN_POINT ( 'NONE',  ( -3.152548672688508926E-16, -46.81249999863440081, -5.148502694627439702 ) ) ;
#44683 = CARTESIAN_POINT ( 'NONE',  ( 1.975475456537005874E-15, -110.6249999972688158, 5.000000000000000000 ) ) ;
#44684 = CARTESIAN_POINT ( 'NONE',  ( -8.190561711645485556E-16, -144.6875000013656063, 4.458734124999999437 ) ) ;
#44685 = CARTESIAN_POINT ( 'NONE',  ( -4.458734124999999437, -89.64583333196773651, -2.574251347313719407 ) ) ;
#44686 = CARTESIAN_POINT ( 'NONE',  ( -58.80597590150559739, -150.0000000000000284, 3.242614290531460330 ) ) ;
#44687 = VERTEX_POINT ( 'NONE', #60992 ) ;
#44688 = CARTESIAN_POINT ( 'NONE',  ( 1.975475456537005874E-15, -19.62499999726881228, 5.000000000000000000 ) ) ;
#44689 = DIRECTION ( 'NONE',  ( -0.000000000000000000, 1.000000000000000000, -0.000000000000000000 ) ) ;
#44690 = CARTESIAN_POINT ( 'NONE',  ( -50.18089887299979068, -150.8125000027311842, 2.462841084822635640 ) ) ;
#44691 = CARTESIAN_POINT ( 'NONE',  ( 1.339745962155612702, -29.16965819600733312, -5.000000000000000000 ) ) ;
#44692 = ORIENTED_EDGE ( 'NONE', *, *, #15698, .T. ) ;
#44693 = CARTESIAN_POINT ( 'NONE',  ( -4.458734124999999437, 4.687500001365595637, 0.000000000000000000 ) ) ;
#44694 = CARTESIAN_POINT ( 'NONE',  ( 5.000000000000000888, -19.58333333333333215, 2.886751345948126879 ) ) ;
#44695 = CARTESIAN_POINT ( 'NONE',  ( -3.152548672688508926E-16, -19.81249999863440436, -5.148502694627439702 ) ) ;
#44696 = CARTESIAN_POINT ( 'NONE',  ( -4.999999999999998224, -100.7916666639354588, 2.886751345948131764 ) ) ;
#44697 = CARTESIAN_POINT ( 'NONE',  ( -4.458734124999998549, -5.229166665301072214, 2.574251347313722516 ) ) ;
#44698 = CARTESIAN_POINT ( 'NONE',  ( 4.458734124999997661, -150.5000000013656347, 1.846868145590737864 ) ) ;
#44699 = CARTESIAN_POINT ( 'NONE',  ( 4.458734124999998549, 22.02083333469892779, -2.574251347313721627 ) ) ;
#44700 = EDGE_LOOP ( 'NONE', ( #14548, #47550, #57109, #50877 ) ) ;
#44701 = CARTESIAN_POINT ( 'NONE',  ( -2.229367062500000163, -95.47916666530107932, -3.861377020970580443 ) ) ;
#44702 = CARTESIAN_POINT ( 'NONE',  ( -4.999999999999998224, -18.79166666393547658, 2.886751345948131764 ) ) ;
#44703 = CARTESIAN_POINT ( 'NONE',  ( 7.500000000000000000, 4.330127018922190096, -7.422398894150032511 ) ) ;
#44704 = CARTESIAN_POINT ( 'NONE',  ( -4.458734124999999437, -15.39583333196773474, -2.574251347313719407 ) ) ;
#44705 = EDGE_CURVE ( 'NONE', #58314, #62422, #41346, .T. ) ;
#44706 = CARTESIAN_POINT ( 'NONE',  ( 1.975475456537005874E-15, -85.62499999726880162, 5.000000000000000000 ) ) ;
#44707 = CARTESIAN_POINT ( 'NONE',  ( 1.975475456537005874E-15, -58.75000000000000000, 5.000000000000000000 ) ) ;
#44708 = AXIS2_PLACEMENT_3D ( 'NONE', #27840, #37819, #7922 ) ;
#44709 = CARTESIAN_POINT ( 'NONE',  ( -50.55543936806279248, -149.0625000013656063, 0.3552334253322060320 ) ) ;
#44710 = CARTESIAN_POINT ( 'NONE',  ( -4.999999999999999112, -38.79166666393548013, 2.886751345948131764 ) ) ;
#44711 = CARTESIAN_POINT ( 'NONE',  ( -50.18089887299978358, -148.6875000000000000, 2.462841084822545934 ) ) ;
#44712 = CARTESIAN_POINT ( 'NONE',  ( 4.458734124999999437, 11.18750000136559386, -5.460374474430324690E-16 ) ) ;
#44713 = CARTESIAN_POINT ( 'NONE',  ( 0.000000000000000000, -170.0000000000000000, 0.000000000000000000 ) ) ;
#44714 = CARTESIAN_POINT ( 'NONE',  ( -4.999999999999998224, -47.79166666393547303, 2.886751345948131764 ) ) ;
#44715 = CARTESIAN_POINT ( 'NONE',  ( 2.229367062499998831, 15.35416666803225993, -3.861377020970580887 ) ) ;
#44716 = CARTESIAN_POINT ( 'NONE',  ( 2.229367062500001939, -60.97916666530106511, 3.861377020970579999 ) ) ;
#44717 = EDGE_LOOP ( 'NONE', ( #57135, #13006, #37924, #48168 ) ) ;
#44718 = CARTESIAN_POINT ( 'NONE',  ( -2.229367062500000163, -14.72916666530107221, -3.861377020970580443 ) ) ;
#44719 =( BOUNDED_CURVE ( )  B_SPLINE_CURVE ( 2, ( #48608, #4547, #60825, #16750, #6154, #10642, #26398, #2295, #26722 ),
 .UNSPECIFIED., .F., .F. ) 
 B_SPLINE_CURVE_WITH_KNOTS ( ( 3, 2, 2, 2, 3 ),
 ( 0.07678571428571429047, 0.07738095238095238360, 0.07857142857142856984, 0.07976190476190475609, 0.08035714285714286309 ),
 .UNSPECIFIED. ) 
 CURVE ( )  GEOMETRIC_REPRESENTATION_ITEM ( )  RATIONAL_B_SPLINE_CURVE ( ( 0.9330127018922194093, 0.9330127018922194093, 1.000000000000000000, 0.8660254037844387076, 1.000000000000000000, 0.8660254037844387076, 1.000000000000000000, 0.9330127018922185211, 0.9330127018922192983 ) ) 
 REPRESENTATION_ITEM ( '' )  );
#44720 = CARTESIAN_POINT ( 'NONE',  ( 5.000000000000000888, 5.416666666666666963, 2.886751345948126879 ) ) ;
#44721 = CARTESIAN_POINT ( 'NONE',  ( 4.458734124999999437, -164.4375000013655779, 0.000000000000000000 ) ) ;
#44722 = CARTESIAN_POINT ( 'NONE',  ( -52.53715891517739323, -142.4375000000000000, -4.819101127000233298 ) ) ;
#44723 = CARTESIAN_POINT ( 'NONE',  ( -2.229367062499996610, -55.14583333196773651, 3.861377020970582219 ) ) ;
#44724 = CARTESIAN_POINT ( 'NONE',  ( 2.499999999999998668, -88.20833333060214443, -4.330127018922193649 ) ) ;
#44725 = CARTESIAN_POINT ( 'NONE',  ( 9.457646018065525792E-16, -35.06249999863440792, 5.148502694627439702 ) ) ;
#44726 = EDGE_CURVE ( 'NONE', #25339, #47748, #16912, .T. ) ;
#44727 = CARTESIAN_POINT ( 'NONE',  ( -9.184850993605147944E-16, -142.3750000027312126, 5.000000000000000000 ) ) ;
#44728 = CARTESIAN_POINT ( 'NONE',  ( -2.499999999999996447, -88.70833333060214443, 4.330127018922195425 ) ) ;
#44729 = EDGE_CURVE ( 'NONE', #59250, #16461, #38449, .T. ) ;
#44730 = CARTESIAN_POINT ( 'NONE',  ( 4.458734124999999437, -152.6875000013656063, 0.000000000000000000 ) ) ;
#44731 = CARTESIAN_POINT ( 'NONE',  ( -2.499999999999996447, -42.83333333333333570, 4.330127018922195425 ) ) ;
#44732 = FACE_OUTER_BOUND ( 'NONE', #21911, .T. ) ;
#44733 = CARTESIAN_POINT ( 'NONE',  ( 1.339745962155612702, -6.169658196007334894, -5.000000000000000000 ) ) ;
#44734 = ORIENTED_EDGE ( 'NONE', *, *, #38220, .T. ) ;
#44735 = CARTESIAN_POINT ( 'NONE',  ( -2.229367062499996610, -102.1458333319677365, 3.861377020970582219 ) ) ;
#44736 = CARTESIAN_POINT ( 'NONE',  ( -4.458734124999998549, 5.520833334698927786, 2.574251347313722516 ) ) ;
#44737 = CARTESIAN_POINT ( 'NONE',  ( 5.000000000000000888, -59.58333333333335702, 2.886751345948126879 ) ) ;
#44738 = CARTESIAN_POINT ( 'NONE',  ( 5.000000000000000000, -2.416666666666664298, -2.886751345948129988 ) ) ;
#44739 = ADVANCED_FACE ( 'NONE', ( #17231 ), #56485, .F. ) ;
#44740 = CARTESIAN_POINT ( 'NONE',  ( 4.458734124999999437, -67.81249999863440792, -5.460374474430324690E-16 ) ) ;
#44741 = CARTESIAN_POINT ( 'NONE',  ( 1.975475456537005874E-15, -67.74999999999998579, 5.000000000000000000 ) ) ;
#44742 = CARTESIAN_POINT ( 'NONE',  ( 5.000000000000000000, -4.291666663935479242, -2.886751345948129988 ) ) ;
#44744 = VERTEX_POINT ( 'NONE', #27201 ) ;
#44743 = CARTESIAN_POINT ( 'NONE',  ( -3.152548672688508926E-16, -33.56249999863440792, -5.148502694627439702 ) ) ;
#44745 = DIRECTION ( 'NONE',  ( -0.000000000000000000, 1.000000000000000000, -0.000000000000000000 ) ) ;
#44746 = CARTESIAN_POINT ( 'NONE',  ( -6.972266317189433020E-16, -74.12499999726878741, -5.000000000000000000 ) ) ;
#44747 = ORIENTED_EDGE ( 'NONE', *, *, #18953, .F. ) ;
#44748 = CARTESIAN_POINT ( 'NONE',  ( -6.972266317189433020E-16, -101.1249999972688158, -5.000000000000000000 ) ) ;
#44749 = CARTESIAN_POINT ( 'NONE',  ( 2.499999999999998668, -49.33333333333332860, -4.330127018922193649 ) ) ;
#44751 = CARTESIAN_POINT ( 'NONE',  ( 2.229367062500001939, -26.22916666530106866, 3.861377020970579999 ) ) ;
#44750 = CYLINDRICAL_SURFACE ( 'NONE', #45967, 5.000000000000000000 ) ;
#44752 = CARTESIAN_POINT ( 'NONE',  ( -1.339745962155610925, -3.794658198738523058, 5.000000000000000000 ) ) ;
#44753 = CARTESIAN_POINT ( 'NONE',  ( 4.458734124999998549, -75.72916666530106511, -2.574251347313721627 ) ) ;
#44754 = CARTESIAN_POINT ( 'NONE',  ( -3.152801135295367096, -142.3125000013655779, -3.152801135295367541 ) ) ;
#44755 = CARTESIAN_POINT ( 'NONE',  ( 4.458734124999999437, -79.81249999863440792, -5.460374474430324690E-16 ) ) ;
#44756 = CARTESIAN_POINT ( 'NONE',  ( -50.40829686548195099, -139.2500000013656063, -1.485763867205728284 ) ) ;
#44757 = CARTESIAN_POINT ( 'NONE',  ( 2.229367062500001939, -30.22916666530107221, 3.861377020970579999 ) ) ;
#44758 = CARTESIAN_POINT ( 'NONE',  ( -5.000000000000000000, -69.87499999726880162, 0.000000000000000000 ) ) ;
#44759 = ORIENTED_EDGE ( 'NONE', *, *, #18620, .T. ) ;
#44760 = EDGE_CURVE ( 'NONE', #44442, #11139, #46819, .T. ) ;
#44761 = CARTESIAN_POINT ( 'NONE',  ( 5.000000000000000000, -51.50000000000000711, -6.123233995736766282E-16 ) ) ;
#44762 = VERTEX_POINT ( 'NONE', #46071 ) ;
#44763 = CARTESIAN_POINT ( 'NONE',  ( 4.458734125000001214, -74.14583333196773651, 2.574251347313718519 ) ) ;
#44764 = CARTESIAN_POINT ( 'NONE',  ( -54.35296922496373639, -135.0000000000000000, -4.421185004030076193 ) ) ;
#44765 = SHAPE_REPRESENTATION_RELATIONSHIP ( 'NONE' , 'NONE' ,  #3639, #23309 ) ;
#44766 = ORIENTED_EDGE ( 'NONE', *, *, #27955, .T. ) ;
#44767 = CARTESIAN_POINT ( 'NONE',  ( -51.75738570946856498, -140.7500000000000000, 3.805975901505576964 ) ) ;
#44768 =( BOUNDED_CURVE ( )  B_SPLINE_CURVE ( 2, ( #38858, #48829, #15064, #4768, #10237, #24394, #43997, #29842, #19564 ),
 .UNSPECIFIED., .F., .F. ) 
 B_SPLINE_CURVE_WITH_KNOTS ( ( 3, 2, 2, 2, 3 ),
 ( 0.02291666666666666852, 0.02361111111111111049, 0.02500000000000000139, 0.02638888888888888881, 0.02708333333333333426 ),
 .UNSPECIFIED. ) 
 CURVE ( )  GEOMETRIC_REPRESENTATION_ITEM ( )  RATIONAL_B_SPLINE_CURVE ( ( 0.9330127018922194093, 0.9330127018922195203, 1.000000000000000000, 0.8660254037844387076, 1.000000000000000000, 0.8660254037844387076, 1.000000000000000000, 0.9330127018922191873, 0.9330127018922194093 ) ) 
 REPRESENTATION_ITEM ( '' )  );
#44769 = CARTESIAN_POINT ( 'NONE',  ( -6.972266317189433020E-16, 13.74999999999999822, -5.000000000000000000 ) ) ;
#44770 = CARTESIAN_POINT ( 'NONE',  ( -4.458734124999999437, -59.64583333196773651, -2.574251347313719407 ) ) ;
#44771 = CARTESIAN_POINT ( 'NONE',  ( 2.229367062500001939, -6.229166665301072214, 3.861377020970579999 ) ) ;
#44772 = ORIENTED_EDGE ( 'NONE', *, *, #19304, .F. ) ;
#44773 = FACE_OUTER_BOUND ( 'NONE', #50739, .T. ) ;
#44774 = DIRECTION ( 'NONE',  ( 1.000000000000000000, 0.000000000000000000, 0.000000000000000000 ) ) ;
#44775 = CARTESIAN_POINT ( 'NONE',  ( 4.458734124999999437, 11.18750000136559386, -5.460374474430324690E-16 ) ) ;
#44776 = CARTESIAN_POINT ( 'NONE',  ( -53.51423613279429503, -141.2500000013656347, 4.591703134518082763 ) ) ;
#44777 = CARTESIAN_POINT ( 'NONE',  ( -2.500000000000000444, -1.166666666666666519, -4.330127018922193649 ) ) ;
#44778 = CARTESIAN_POINT ( 'NONE',  ( -3.152801135295367985, -161.8125000013656063, 3.152801135295367096 ) ) ;
#44779 = LINE ( 'NONE', #741, #884 ) ;
#44780 = ORIENTED_EDGE ( 'NONE', *, *, #58233, .T. ) ;
#44781 = CARTESIAN_POINT ( 'NONE',  ( 4.458734124999999437, -83.81249999863439371, -5.460374474430324690E-16 ) ) ;
#44782 = CARTESIAN_POINT ( 'NONE',  ( -1.339745962155610925, -51.66965819600733312, 5.000000000000000000 ) ) ;
#44783 = CARTESIAN_POINT ( 'NONE',  ( 2.229367062499998831, 1.354166668032261933, -3.861377020970580887 ) ) ;
#44784 = EDGE_CURVE ( 'NONE', #11542, #55337, #21635, .T. ) ;
#44785 = CARTESIAN_POINT ( 'NONE',  ( 5.000000000000000000, -71.29166666393547303, -2.886751345948130876 ) ) ;
#44786 = CARTESIAN_POINT ( 'NONE',  ( 5.000000000000000000, -84.41666666666667140, -2.886751345948129988 ) ) ;
#44787 = CARTESIAN_POINT ( 'NONE',  ( -7.500000000000000000, -3.469446951953614189E-15, -6.991905250253751980 ) ) ;
#44788 = CARTESIAN_POINT ( 'NONE',  ( 2.229367062500001939, -67.22916666530106511, 3.861377020970579999 ) ) ;
#44789 = CARTESIAN_POINT ( 'NONE',  ( -5.000000000000000000, -25.87499999726881583, 0.000000000000000000 ) ) ;
#44790 = LINE ( 'NONE', #1081, #32711 ) ;
#44791 = LINE ( 'NONE', #60251, #18271 ) ;
#44792 = CARTESIAN_POINT ( 'NONE',  ( -4.999999999999998224, 23.08333333333333215, 2.886751345948131764 ) ) ;
#44793 = DIRECTION ( 'NONE',  ( -0.8660254037844380415, 0.000000000000000000, 0.5000000000000009992 ) ) ;
#44794 = CARTESIAN_POINT ( 'NONE',  ( -4.458734124999999437, -46.39583333196774362, -2.574251347313719407 ) ) ;
#44795 = CARTESIAN_POINT ( 'NONE',  ( -4.458734124999999437, -34.64583333196772941, -2.574251347313719407 ) ) ;
#44796 = CARTESIAN_POINT ( 'NONE',  ( 4.458734125000000326, 6.854166668032259935, 2.574251347313718519 ) ) ;
#44797 = VECTOR ( 'NONE', #34218, 1000.000000000000000 ) ;
#44798 = DIRECTION ( 'NONE',  ( -0.000000000000000000, 1.000000000000000000, -0.000000000000000000 ) ) ;
#44799 = CARTESIAN_POINT ( 'NONE',  ( 5.000000000000000000, 19.50000000000000000, -6.123233995736766282E-16 ) ) ;
#44800 = CARTESIAN_POINT ( 'NONE',  ( -2.071067811865478170, -151.4375000027312410, 5.000000000000000000 ) ) ;
#44801 = FACE_OUTER_BOUND ( 'NONE', #34746, .T. ) ;
#44802 = CARTESIAN_POINT ( 'NONE',  ( 4.458734125000001214, -34.89583333196772941, 2.574251347313718519 ) ) ;
#44803 = CARTESIAN_POINT ( 'NONE',  ( 5.000000000000000000, -71.29166666393547303, -2.886751345948129988 ) ) ;
#44804 = AXIS2_PLACEMENT_3D ( 'NONE', #32146, #52721, #17048 ) ;
#44805 = CARTESIAN_POINT ( 'NONE',  ( -55.35523342533222291, -144.5625000013656063, 4.444560631937231499 ) ) ;
#44806 = CARTESIAN_POINT ( 'NONE',  ( 3.061616997868383141E-16, -140.7500000000000000, -5.000000000000000000 ) ) ;
#44807 = CARTESIAN_POINT ( 'NONE',  ( -1.994931997373328159E-14, -8.660254037844390851, -1.000000000000000888 ) ) ;
#44808 = EDGE_CURVE ( 'NONE', #1423, #59424, #14594, .T. ) ;
#44809 = CARTESIAN_POINT ( 'NONE',  ( 4.458734124999999437, -80.06249999863440792, -5.460374474430324690E-16 ) ) ;
#44810 = CARTESIAN_POINT ( 'NONE',  ( 1.846868145590735200, -167.5000000013655779, -4.458734124999999437 ) ) ;
#44811 = CARTESIAN_POINT ( 'NONE',  ( -6.972266317189433020E-16, -25.12499999726881228, -5.000000000000000000 ) ) ;
#44812 = CARTESIAN_POINT ( 'NONE',  ( 6.123233995736766282E-16, -170.0000000000000000, -5.000000000000000000 ) ) ;
#44813 = CARTESIAN_POINT ( 'NONE',  ( -4.999999999999999112, -29.91666666666667140, 2.886751345948131764 ) ) ;
#44814 = CARTESIAN_POINT ( 'NONE',  ( -4.458734125000000326, -145.0000000013656063, -1.846868145590735644 ) ) ;
#44815 = ORIENTED_EDGE ( 'NONE', *, *, #13302, .T. ) ;
#44816 = CARTESIAN_POINT ( 'NONE',  ( -2.229367062500000163, 27.27083333469892779, -3.861377020970580443 ) ) ;
#44817 = VERTEX_POINT ( 'NONE', #55088 ) ;
#44818 = CARTESIAN_POINT ( 'NONE',  ( -3.152548672688508926E-16, -63.81249999863440792, -5.148502694627439702 ) ) ;
#44819 = CARTESIAN_POINT ( 'NONE',  ( -5.000000000000000000, 20.04166666939785202, -2.886751345948128211 ) ) ;
#44820 = CARTESIAN_POINT ( 'NONE',  ( 0.000000000000000000, -120.0000000000000000, 5.000000000000000000 ) ) ;
#44821 = CARTESIAN_POINT ( 'NONE',  ( 5.000000000000000888, 11.41666666666666607, 2.886751345948126879 ) ) ;
#44822 = CARTESIAN_POINT ( 'NONE',  ( 2.229367062499998831, -51.64583333196773651, -3.861377020970580887 ) ) ;
#44823 = CARTESIAN_POINT ( 'NONE',  ( 2.229367062499998831, -10.64583333196773829, -3.861377020970580887 ) ) ;
#44824 = CARTESIAN_POINT ( 'NONE',  ( -6.972266317189433020E-16, -67.12499999726881583, -5.000000000000000000 ) ) ;
#44825 = FACE_OUTER_BOUND ( 'NONE', #55219, .T. ) ;
#44826 = CARTESIAN_POINT ( 'NONE',  ( 3.750000000000004441, -6.495190528383289141, 0.000000000000000000 ) ) ;
#44827 = DIRECTION ( 'NONE',  ( -0.000000000000000000, 1.000000000000000000, -0.000000000000000000 ) ) ;
#44828 = CARTESIAN_POINT ( 'NONE',  ( 5.000000000000000000, -66.29166666393547303, -2.886751345948130876 ) ) ;
#44830 = CARTESIAN_POINT ( 'NONE',  ( -4.458734124999998549, -21.22916666530107221, 2.574251347313722516 ) ) ;
#44829 = CARTESIAN_POINT ( 'NONE',  ( 1.975475456537005874E-15, -78.74999999999998579, 5.000000000000000000 ) ) ;
#44831 = CARTESIAN_POINT ( 'NONE',  ( -5.000000000000000888, -140.5625000027312410, 2.071067811865474617 ) ) ;
#44832 = CARTESIAN_POINT ( 'NONE',  ( 2.229367062499998831, -55.64583333196773651, -3.861377020970580887 ) ) ;
#44833 = CARTESIAN_POINT ( 'NONE',  ( -3.152801135295367985, -154.0625000013656063, 3.152801135295367096 ) ) ;
#44834 = ADVANCED_FACE ( 'NONE', ( #40916 ), #60874, .T. ) ;
#44835 = CARTESIAN_POINT ( 'NONE',  ( -5.000000000000000000, -55.87499999726880162, 0.000000000000000000 ) ) ;
#44836 = VERTEX_POINT ( 'NONE', #11329 ) ;
#44837 = CARTESIAN_POINT ( 'NONE',  ( 0.000000000000000000, -170.0000000000000000, 0.000000000000000000 ) ) ;
#44838 = CARTESIAN_POINT ( 'NONE',  ( -2.229367062500000163, 2.270833334698928230, -3.861377020970580443 ) ) ;
#44839 = EDGE_LOOP ( 'NONE', ( #2735, #29211, #9356, #9648 ) ) ;
#44841 = CYLINDRICAL_SURFACE ( 'NONE', #58359, 5.000000000000000000 ) ;
#44840 = CARTESIAN_POINT ( 'NONE',  ( -52.53715891517739323, -141.4375000000000284, -4.819101127000233298 ) ) ;
#44842 = CARTESIAN_POINT ( 'NONE',  ( -8.190561711645485556E-16, -156.6875000013655779, 4.458734124999999437 ) ) ;
#44843 = ORIENTED_EDGE ( 'NONE', *, *, #60578, .T. ) ;
#44844 = AXIS2_PLACEMENT_3D ( 'NONE', #41870, #17447, #37067 ) ;
#44845 = CARTESIAN_POINT ( 'NONE',  ( 5.000000000000000000, -83.49999999999998579, -6.123233995736766282E-16 ) ) ;
#44846 = CARTESIAN_POINT ( 'NONE',  ( -49.85088928181150436, -131.5625000000000284, -1.666127454062680702 ) ) ;
#44847 = CARTESIAN_POINT ( 'NONE',  ( 5.000000000000000000, 15.58333333333332860, -2.886751345948130876 ) ) ;
#44848 = CARTESIAN_POINT ( 'NONE',  ( -4.458734124999999437, -44.64583333196773651, -2.574251347313719407 ) ) ;
#44849 = AXIS2_PLACEMENT_3D ( 'NONE', #3016, #56727, #12647 ) ;
#44850 = ORIENTED_EDGE ( 'NONE', *, *, #19251, .F. ) ;
#44851 = AXIS2_PLACEMENT_3D ( 'NONE', #45920, #31124, #30483 ) ;
#44852 =( BOUNDED_CURVE ( )  B_SPLINE_CURVE ( 2, ( #41161, #55980, #11893, #31513, #51156, #34636, #40733, #34971, #44934 ),
 .UNSPECIFIED., .F., .F. ) 
 B_SPLINE_CURVE_WITH_KNOTS ( ( 3, 2, 2, 2, 3 ),
 ( 0.5017857142857142794, 0.5023809523809523725, 0.5035714285714285587, 0.5047619047619047450, 0.5053571428571428381 ),
 .UNSPECIFIED. ) 
 CURVE ( )  GEOMETRIC_REPRESENTATION_ITEM ( )  RATIONAL_B_SPLINE_CURVE ( ( 0.9330127018922194093, 0.9330127018922194093, 1.000000000000000000, 0.8660254037844387076, 1.000000000000000000, 0.8660254037844387076, 1.000000000000000000, 0.9330127018922194093, 0.9330127018922194093 ) ) 
 REPRESENTATION_ITEM ( '' )  );
#44853 = DIRECTION ( 'NONE',  ( -0.4999999999999948375, 0.000000000000000000, 0.8660254037844415942 ) ) ;
#44854 = CARTESIAN_POINT ( 'NONE',  ( -4.458734124999999437, 12.68750000136559564, 0.000000000000000000 ) ) ;
#44855 = CARTESIAN_POINT ( 'NONE',  ( -4.458734124999999437, -88.64583333196773651, -2.574251347313719407 ) ) ;
#44856 = CARTESIAN_POINT ( 'NONE',  ( -50.40829686548195099, -153.0000000013656063, -1.485763867205728284 ) ) ;
#44857 = CARTESIAN_POINT ( 'NONE',  ( -5.000000000000000000, -165.5000000000000000, -6.123233995736766282E-16 ) ) ;
#44858 = DIRECTION ( 'NONE',  ( 0.000000000000000000, -1.000000000000000000, 0.000000000000000000 ) ) ;
#44859 = CARTESIAN_POINT ( 'NONE',  ( -62.00000000000001421, -135.0000000000000284, -4.041451884327373456 ) ) ;
#44860 = CARTESIAN_POINT ( 'NONE',  ( -2.229367062500000163, -65.47916666530106511, -3.861377020970580443 ) ) ;
#44861 = CARTESIAN_POINT ( 'NONE',  ( 7.777900015783946408, 4.169681370001526055, -7.928862157988300297 ) ) ;
#44862 = CARTESIAN_POINT ( 'NONE',  ( 2.229367062500001939, 19.02083333469892779, 3.861377020970579999 ) ) ;
#44863 = CARTESIAN_POINT ( 'NONE',  ( -2.916731409357579869E-14, 18.24999999999999645, 5.000000000000000888 ) ) ;
#44864 = ADVANCED_FACE ( 'NONE', ( #55729 ), #35790, .T. ) ;
#44865 = CARTESIAN_POINT ( 'NONE',  ( 2.071067811865603403, -157.3125000027311842, 4.999999999999872990 ) ) ;
#44866 = ADVANCED_FACE ( 'NONE', ( #2030 ), #16485, .T. ) ;
#44867 = CARTESIAN_POINT ( 'NONE',  ( -2.229367062499996610, -50.39583333196772941, 3.861377020970582219 ) ) ;
#44868 = CARTESIAN_POINT ( 'NONE',  ( -5.000000000000000000, -8.958333330602146205, -2.886751345948128211 ) ) ;
#44869 = CARTESIAN_POINT ( 'NONE',  ( -59.81910112700026616, -145.1874999999999716, -2.462841084822481541 ) ) ;
#44870 = LINE ( 'NONE', #833, #47089 ) ;
#44871 = CARTESIAN_POINT ( 'NONE',  ( 9.457646018065525792E-16, -88.31249999863439371, 5.148502694627439702 ) ) ;
#44872 = EDGE_CURVE ( 'NONE', #2557, #28361, #60654, .T. ) ;
#44873 = FACE_OUTER_BOUND ( 'NONE', #1362, .T. ) ;
#44874 = CARTESIAN_POINT ( 'NONE',  ( -4.458734124999999437, -14.56249999863440436, 0.000000000000000000 ) ) ;
#44876 = VERTEX_POINT ( 'NONE', #20356 ) ;
#44875 = EDGE_CURVE ( 'NONE', #6056, #24978, #22890, .T. ) ;
#44877 = CARTESIAN_POINT ( 'NONE',  ( -3.535533905932737309, -163.7500000027312126, -3.535533905932738197 ) ) ;
#44878 = CARTESIAN_POINT ( 'NONE',  ( -2.229367062500000163, -101.4791666653010651, -3.861377020970580443 ) ) ;
#44879 = CARTESIAN_POINT ( 'NONE',  ( -2.071067811865478170, -162.4375000027311842, 5.000000000000000000 ) ) ;
#44880 = ORIENTED_EDGE ( 'NONE', *, *, #44760, .T. ) ;
#44881 = CARTESIAN_POINT ( 'NONE',  ( 9.457646018065525792E-16, -95.31249999863440792, 5.148502694627439702 ) ) ;
#44882 = CARTESIAN_POINT ( 'NONE',  ( 2.071067811865412445, -162.9375000027312126, -5.000000000000063949 ) ) ;
#44884 = EDGE_CURVE ( 'NONE', #21524, #18684, #36418, .T. ) ;
#44883 = CARTESIAN_POINT ( 'NONE',  ( 5.000000000000000000, -55.37499999726880162, -6.123233995736766282E-16 ) ) ;
#44885 = CARTESIAN_POINT ( 'NONE',  ( -5.000000000000000000, 19.12500000273118772, 0.000000000000000000 ) ) ;
#44886 = ADVANCED_FACE ( 'NONE', ( #11964 ), #5558, .T. ) ;
#44887 = CARTESIAN_POINT ( 'NONE',  ( -59.44456063193725015, -127.5625000013655921, -0.3552334253322034230 ) ) ;
#44888 = CARTESIAN_POINT ( 'NONE',  ( -59.44456063193725015, -142.5625000013656063, -0.3552334253322034230 ) ) ;
#44889 = CARTESIAN_POINT ( 'NONE',  ( 9.457646018065525792E-16, -16.06249999863440436, 5.148502694627439702 ) ) ;
#44890 = CARTESIAN_POINT ( 'NONE',  ( 2.229367062500001939, 7.770833334698926009, 3.861377020970579999 ) ) ;
#44891 = EDGE_CURVE ( 'NONE', #18516, #24077, #30309, .T. ) ;
#44892 = CARTESIAN_POINT ( 'NONE',  ( -4.458734124999997661, -64.47916666530106511, 2.574251347313722516 ) ) ;
#44893 = CARTESIAN_POINT ( 'NONE',  ( -2.071067811865562991, -141.4375000027311842, 4.999999999999913847 ) ) ;
#44894 = CARTESIAN_POINT ( 'NONE',  ( 2.229367062500001939, -21.97916666530107221, 3.861377020970579999 ) ) ;
#44895 = CYLINDRICAL_SURFACE ( 'NONE', #10152, 5.000000000000000000 ) ;
#44896 = CARTESIAN_POINT ( 'NONE',  ( -2.071067811865478170, -154.3125000000000284, 5.000000000000000000 ) ) ;
#44897 = CARTESIAN_POINT ( 'NONE',  ( -2.499999999999996447, -9.833333333333332149, 4.330127018922195425 ) ) ;
#44898 = EDGE_CURVE ( 'NONE', #14179, #60221, #24331, .T. ) ;
#44899 = CARTESIAN_POINT ( 'NONE',  ( -4.458734124999999437, -154.9375000013655779, -5.460374474430324690E-16 ) ) ;
#44900 = VERTEX_POINT ( 'NONE', #3202 ) ;
#44901 = CARTESIAN_POINT ( 'NONE',  ( 2.229367062500001939, -48.22916666530106511, 3.861377020970579999 ) ) ;
#44902 = ADVANCED_FACE ( 'NONE', ( #8022 ), #7710, .T. ) ;
#44903 = CARTESIAN_POINT ( 'NONE',  ( 5.000000000000000000, -92.50000000000000000, -6.123233995736766282E-16 ) ) ;
#44904 = EDGE_CURVE ( 'NONE', #27512, #38937, #29413, .T. ) ;
#44905 = CARTESIAN_POINT ( 'NONE',  ( -5.000000000000000000, 28.99999999999999645, 0.000000000000000000 ) ) ;
#44906 = VECTOR ( 'NONE', #28265, 1000.000000000000000 ) ;
#44907 = AXIS2_PLACEMENT_3D ( 'NONE', #36270, #33257, #13323 ) ;
#44908 = CARTESIAN_POINT ( 'NONE',  ( 2.229367062500001939, 12.02083333469892601, 3.861377020970579999 ) ) ;
#44909 = CARTESIAN_POINT ( 'NONE',  ( -2.500000000000000444, -89.04166666393547303, -4.330127018922193649 ) ) ;
#44910 = VECTOR ( 'NONE', #5659, 1000.000000000000000 ) ;
#44911 = CARTESIAN_POINT ( 'NONE',  ( 0.000000000000000000, -170.0000000000000000, 0.000000000000000000 ) ) ;
#44912 = CARTESIAN_POINT ( 'NONE',  ( -2.229367062499996610, 19.60416666803225993, 3.861377020970582219 ) ) ;
#44913 = CARTESIAN_POINT ( 'NONE',  ( -4.999999999999999112, -73.91666666666664298, 2.886751345948131764 ) ) ;
#44914 =( BOUNDED_CURVE ( )  B_SPLINE_CURVE ( 2, ( #9537, #29141, #34291, #10809, #29777, #4708, #14994, #6006, #24332 ),
 .UNSPECIFIED., .F., .F. ) 
 B_SPLINE_CURVE_WITH_KNOTS ( ( 3, 2, 2, 2, 3 ),
 ( 0.6145833333333333703, 0.6152777777777778123, 0.6166666666666666963, 0.6180555555555555802, 0.6187500000000000222 ),
 .UNSPECIFIED. ) 
 CURVE ( )  GEOMETRIC_REPRESENTATION_ITEM ( )  RATIONAL_B_SPLINE_CURVE ( ( 0.9330127018922194093, 0.9330127018922194093, 1.000000000000000000, 0.8660254037844387076, 1.000000000000000000, 0.8660254037844387076, 1.000000000000000000, 0.9330127018922194093, 0.9330127018922194093 ) ) 
 REPRESENTATION_ITEM ( '' )  );
#44915 = CARTESIAN_POINT ( 'NONE',  ( 5.000000000000000888, 9.541666669397852019, 2.886751345948126879 ) ) ;
#44916 = EDGE_LOOP ( 'NONE', ( #3653, #11562, #37349, #54070 ) ) ;
#44917 = CARTESIAN_POINT ( 'NONE',  ( 3.535533905932738197, -162.0000000027312126, -3.535533905932738197 ) ) ;
#44918 = ORIENTED_EDGE ( 'NONE', *, *, #19755, .T. ) ;
#44919 = CYLINDRICAL_SURFACE ( 'NONE', #19364, 5.000000000000000000 ) ;
#44920 = CARTESIAN_POINT ( 'NONE',  ( -2.229367062500000163, -40.47916666530107221, -3.861377020970580443 ) ) ;
#44921 = CARTESIAN_POINT ( 'NONE',  ( -5.000000000000000000, -38.87499999726880162, 0.000000000000000000 ) ) ;
#44922 = VERTEX_POINT ( 'NONE', #22179 ) ;
#44923 = CARTESIAN_POINT ( 'NONE',  ( 2.229367062499998831, -12.64583333196774007, -3.861377020970580887 ) ) ;
#44925 = VERTEX_POINT ( 'NONE', #57547 ) ;
#44924 = CARTESIAN_POINT ( 'NONE',  ( 4.458734125000001214, -19.14583333196774007, 2.574251347313718519 ) ) ;
#44926 = CARTESIAN_POINT ( 'NONE',  ( -2.500000000000000444, -82.16666666666667140, -4.330127018922193649 ) ) ;
#44927 = FACE_OUTER_BOUND ( 'NONE', #58140, .T. ) ;
#44928 = CARTESIAN_POINT ( 'NONE',  ( -4.458734124999999437, -62.64583333196774362, -2.574251347313719407 ) ) ;
#44929 = CARTESIAN_POINT ( 'NONE',  ( -5.000000000000000000, -88.87499999726880162, 0.000000000000000000 ) ) ;
#44931 = ORIENTED_EDGE ( 'NONE', *, *, #20497, .T. ) ;
#44930 = CARTESIAN_POINT ( 'NONE',  ( 0.000000000000000000, -120.0000000000000000, 0.000000000000000000 ) ) ;
#44932 = CARTESIAN_POINT ( 'NONE',  ( -58.80597590150559739, -142.0000000000000284, 3.242614290531460330 ) ) ;
#44933 = CARTESIAN_POINT ( 'NONE',  ( 4.458734124999998549, -24.97916666530106511, -2.574251347313721627 ) ) ;
#44934 = CARTESIAN_POINT ( 'NONE',  ( 1.975475456537005874E-15, -41.62499999726880162, 5.000000000000000000 ) ) ;
#44935 = ORIENTED_EDGE ( 'NONE', *, *, #40951, .F. ) ;
#44936 = CARTESIAN_POINT ( 'NONE',  ( 3.152801135295367541, -163.5625000013656063, -3.152801135295367541 ) ) ;
#44937 = CARTESIAN_POINT ( 'NONE',  ( -2.229367062499996610, -108.3958333319677365, 3.861377020970582219 ) ) ;
#44938 = CARTESIAN_POINT ( 'NONE',  ( 3.535533905932736864, -156.1250000000000000, 3.535533905932738641 ) ) ;
#44939 = ORIENTED_EDGE ( 'NONE', *, *, #40615, .F. ) ;
#44940 = CARTESIAN_POINT ( 'NONE',  ( -57.89159099828107458, -145.9375000013656063, -3.393966926194107447 ) ) ;
#44941 = CARTESIAN_POINT ( 'NONE',  ( 4.458734124999998549, -76.97916666530106511, -2.574251347313721627 ) ) ;
#44942 = CARTESIAN_POINT ( 'NONE',  ( -59.81910112700025905, -134.3125000027312126, -2.462841084822630311 ) ) ;
#44943 = CARTESIAN_POINT ( 'NONE',  ( -4.458734124999999437, -45.39583333196773651, -2.574251347313719407 ) ) ;
#44944 = CARTESIAN_POINT ( 'NONE',  ( -1.846868145590737420, -141.0000000013655779, 4.458734124999997661 ) ) ;
#44945 = AXIS2_PLACEMENT_3D ( 'NONE', #3115, #61971, #51045 ) ;
#44946 = DIRECTION ( 'NONE',  ( -0.8660254037844410391, -0.4999999999999958367, -0.000000000000000000 ) ) ;
#44947 = CARTESIAN_POINT ( 'NONE',  ( 4.458734124999999437, -48.81249999863440792, -5.460374474430324690E-16 ) ) ;
#44948 = CARTESIAN_POINT ( 'NONE',  ( -1.339745962155610925, 0.2053418012614791066, 5.000000000000000000 ) ) ;
#44949 = CARTESIAN_POINT ( 'NONE',  ( 4.458734125000001214, -16.89583333196773651, 2.574251347313718519 ) ) ;
#44950 = VECTOR ( 'NONE', #39677, 1000.000000000000000 ) ;
#44951 = CARTESIAN_POINT ( 'NONE',  ( -3.535250795749689387E-16, -99.25000000000000000, -5.773502691896257311 ) ) ;
#44952 = CARTESIAN_POINT ( 'NONE',  ( 1.846868145590736310, -139.8750000013656063, 4.458734124999999437 ) ) ;
#44953 = CARTESIAN_POINT ( 'NONE',  ( 4.458734124999998549, -31.97916666530107577, -2.574251347313721627 ) ) ;
#44954 = CARTESIAN_POINT ( 'NONE',  ( -3.535250795749689387E-16, 8.875000002731184168, -5.773502691896257311 ) ) ;
#44955 = CARTESIAN_POINT ( 'NONE',  ( 2.499999999999998668, -50.33333333333332860, -4.330127018922193649 ) ) ;
#44956 = CARTESIAN_POINT ( 'NONE',  ( -56.48576386720575471, -127.7500000013655921, -4.591703134518078322 ) ) ;
#44957 = CARTESIAN_POINT ( 'NONE',  ( 4.458734124999998549, -71.97916666530107932, -2.574251347313721627 ) ) ;
#44958 = CARTESIAN_POINT ( 'NONE',  ( -3.535533905932737309, -166.6250000000000284, -3.535533905932738197 ) ) ;
#44959 = CARTESIAN_POINT ( 'NONE',  ( 1.975475456537005874E-15, -0.6249999972688137229, 5.000000000000000000 ) ) ;
#44960 = CARTESIAN_POINT ( 'NONE',  ( -5.274401269815139237, -6.074457022762090652, -7.633824513837113912 ) ) ;
#44961 =( BOUNDED_CURVE ( )  B_SPLINE_CURVE ( 2, ( #22341, #46140, #46461, #41611, #41299, #60948, #17185, #6585, #31662 ),
 .UNSPECIFIED., .F., .F. ) 
 B_SPLINE_CURVE_WITH_KNOTS ( ( 3, 2, 2, 2, 3 ),
 ( 0.3767857142857142794, 0.3773809523809523725, 0.3785714285714285587, 0.3797619047619047450, 0.3803571428571428381 ),
 .UNSPECIFIED. ) 
 CURVE ( )  GEOMETRIC_REPRESENTATION_ITEM ( )  RATIONAL_B_SPLINE_CURVE ( ( 0.9330127018922194093, 0.9330127018922194093, 1.000000000000000000, 0.8660254037844387076, 1.000000000000000000, 0.8660254037844387076, 1.000000000000000000, 0.9330127018922194093, 0.9330127018922194093 ) ) 
 REPRESENTATION_ITEM ( '' )  );
#44962 = CARTESIAN_POINT ( 'NONE',  ( 9.457646018065525792E-16, -1.312499998634406140, 5.148502694627439702 ) ) ;
#44963 = VERTEX_POINT ( 'NONE', #32130 ) ;
#44964 = CARTESIAN_POINT ( 'NONE',  ( -4.999999999999998224, -14.79166666393548546, 2.886751345948131764 ) ) ;
#44966 = CARTESIAN_POINT ( 'NONE',  ( -4.458734124999999437, -35.31249999863440792, 0.000000000000000000 ) ) ;
#44965 = CARTESIAN_POINT ( 'NONE',  ( 4.458734124999999437, -89.81249999863440792, -5.460374474430324690E-16 ) ) ;
#44967 = CARTESIAN_POINT ( 'NONE',  ( 4.458734124999998549, -80.97916666530106511, -2.574251347313721627 ) ) ;
#44968 = CARTESIAN_POINT ( 'NONE',  ( -4.458734124999999437, 18.43750000136559564, 0.000000000000000000 ) ) ;
#44969 = CARTESIAN_POINT ( 'NONE',  ( 2.626220312808019583E-14, 21.75000000000000000, -5.000000000000000000 ) ) ;
#44970 = CARTESIAN_POINT ( 'NONE',  ( -52.10840900171896806, -138.1875000013656347, 3.393966926194110556 ) ) ;
#44971 = CARTESIAN_POINT ( 'NONE',  ( 4.458734125000000326, -0.8958333319677401763, 2.574251347313718519 ) ) ;
#44972 = CARTESIAN_POINT ( 'NONE',  ( -4.458734124999998549, 19.52083333469893134, 2.574251347313722516 ) ) ;
#44973 = CARTESIAN_POINT ( 'NONE',  ( -2.229367062499996610, -49.39583333196772941, 3.861377020970582219 ) ) ;
#44974 = CARTESIAN_POINT ( 'NONE',  ( -6.972266317189433020E-16, -11.25000000000000178, -5.000000000000000000 ) ) ;
#44975 = CARTESIAN_POINT ( 'NONE',  ( 9.457646018065525792E-16, -2.062499998634406584, 5.148502694627439702 ) ) ;
#44976 = EDGE_CURVE ( 'NONE', #62207, #53065, #58186, .T. ) ;
#44977 = VERTEX_POINT ( 'NONE', #52407 ) ;
#44978 = CARTESIAN_POINT ( 'NONE',  ( -4.458734124999999437, -29.64583333196773651, -2.574251347313719407 ) ) ;
#44979 = CARTESIAN_POINT ( 'NONE',  ( -50.40829686548195099, -130.2500000013656063, -1.485763867205728284 ) ) ;
#44980 = CARTESIAN_POINT ( 'NONE',  ( 2.229367062500001939, -73.97916666530106511, 3.861377020970579999 ) ) ;
#44981 = CARTESIAN_POINT ( 'NONE',  ( 2.499999999999998668, -110.2083333306021444, -4.330127018922193649 ) ) ;
#44982 = CARTESIAN_POINT ( 'NONE',  ( 2.229367062499998831, 28.35416666803225993, -3.861377020970580887 ) ) ;
#44983 = ADVANCED_FACE ( 'NONE', ( #61110 ), #17035, .T. ) ;
#44984 = CARTESIAN_POINT ( 'NONE',  ( -58.24261429053147765, -155.0000000000000284, -3.805975901505573411 ) ) ;
#44985 = CARTESIAN_POINT ( 'NONE',  ( 4.458734124999999437, -109.0624999986343937, -5.460374474430324690E-16 ) ) ;
#44986 = CARTESIAN_POINT ( 'NONE',  ( -2.229367062500000163, -80.72916666530106511, -3.861377020970580443 ) ) ;
#44987 = CARTESIAN_POINT ( 'NONE',  ( 1.060575238724906964E-15, -61.75000000000000000, 5.773502691896257311 ) ) ;
#44988 = CARTESIAN_POINT ( 'NONE',  ( -49.85088928181150436, -151.5625000000000284, -1.666127454062680480 ) ) ;
#44989 = CARTESIAN_POINT ( 'NONE',  ( -2.500000000000000444, 21.95833333606451987, -4.330127018922193649 ) ) ;
#44990 = ORIENTED_EDGE ( 'NONE', *, *, #59869, .F. ) ;
#44991 = DIRECTION ( 'NONE',  ( 0.000000000000000000, 0.000000000000000000, 1.000000000000000000 ) ) ;
#44992 = VECTOR ( 'NONE', #38747, 1000.000000000000000 ) ;
#44993 = CARTESIAN_POINT ( 'NONE',  ( -7.640563834021360018E-16, -9.147862274876560562, -8.047472243342937759 ) ) ;
#44994 = CARTESIAN_POINT ( 'NONE',  ( 1.060575238724906964E-15, -20.74999999999999645, 5.773502691896257311 ) ) ;
#44995 = CARTESIAN_POINT ( 'NONE',  ( -2.229367062499996610, -20.14583333196774007, 3.861377020970582219 ) ) ;
#44996 = VECTOR ( 'NONE', #51735, 1000.000000000000000 ) ;
#44997 = CARTESIAN_POINT ( 'NONE',  ( -4.458734124999999437, -80.39583333196773651, -2.574251347313719407 ) ) ;
#44998 = CARTESIAN_POINT ( 'NONE',  ( -4.999999999999999112, -22.79166666393548013, 2.886751345948131764 ) ) ;
#45000 = VERTEX_POINT ( 'NONE', #46942 ) ;
#44999 = CARTESIAN_POINT ( 'NONE',  ( 2.229367062500001939, -51.97916666530107221, 3.861377020970579999 ) ) ;
#45001 = CARTESIAN_POINT ( 'NONE',  ( -6.972266317189433020E-16, -74.12499999726878741, -5.000000000000000000 ) ) ;
#45003 = VERTEX_POINT ( 'NONE', #47257 ) ;
#45002 = CARTESIAN_POINT ( 'NONE',  ( 4.458734124999998549, -4.979166665301072214, -2.574251347313721627 ) ) ;
#45004 = CARTESIAN_POINT ( 'NONE',  ( -55.35523342533222291, -150.3125000013656063, 4.444560631937231499 ) ) ;
#45005 = CARTESIAN_POINT ( 'NONE',  ( -4.999999999999999112, -64.91666666666667140, 2.886751345948131764 ) ) ;
#45006 = CARTESIAN_POINT ( 'NONE',  ( 4.458734124999999437, -150.7500000013655779, 1.846868145590737864 ) ) ;
#45007 = CARTESIAN_POINT ( 'NONE',  ( 4.458734124999998549, -48.97916666530107221, -2.574251347313721627 ) ) ;
#45008 = LINE ( 'NONE', #50481, #26587 ) ;
#45009 = CARTESIAN_POINT ( 'NONE',  ( 3.535533905932738197, -157.8750000000000284, -3.535533905932738197 ) ) ;
#45010 = CARTESIAN_POINT ( 'NONE',  ( -5.000000000000000000, 7.041666669397852019, -2.886751345948128211 ) ) ;
#45011 = CARTESIAN_POINT ( 'NONE',  ( -49.85088928181150436, -153.5625000000000284, -1.666127454062680702 ) ) ;
#45012 = CARTESIAN_POINT ( 'NONE',  ( -2.229367062500000163, -9.729166665301068662, -3.861377020970580443 ) ) ;
#45013 = CARTESIAN_POINT ( 'NONE',  ( -3.152548672688508926E-16, -44.81249999863440792, -5.148502694627439702 ) ) ;
#45014 = CARTESIAN_POINT ( 'NONE',  ( -54.60164318462004474, -136.5000000027312126, -4.984105922594373794 ) ) ;
#45015 = CARTESIAN_POINT ( 'NONE',  ( 4.458734124999999437, -144.4375000013656063, 0.000000000000000000 ) ) ;
#45016 = CARTESIAN_POINT ( 'NONE',  ( -2.229367062499996610, -92.39583333196773651, 3.861377020970582219 ) ) ;
#45017 = LINE ( 'NONE', #30534, #31727 ) ;
#45018 = ORIENTED_EDGE ( 'NONE', *, *, #50916, .T. ) ;
#45019 = DIRECTION ( 'NONE',  ( 0.000000000000000000, 0.000000000000000000, 1.000000000000000000 ) ) ;
#45020 = CARTESIAN_POINT ( 'NONE',  ( -3.152548672688508926E-16, 28.18750000136559564, -5.148502694627439702 ) ) ;
#45021 = CARTESIAN_POINT ( 'NONE',  ( -53.33387254593733928, -145.9375000027312126, 5.149110718188519620 ) ) ;
#45022 = CARTESIAN_POINT ( 'NONE',  ( 5.000000000000000888, -82.45833333060214443, 2.886751345948126879 ) ) ;
#45023 = VERTEX_POINT ( 'NONE', #57236 ) ;
#45024 = CARTESIAN_POINT ( 'NONE',  ( -4.458734124999999437, 5.604166668032262599, -2.574251347313719407 ) ) ;
#45025 = EDGE_CURVE ( 'NONE', #20174, #59584, #26688, .T. ) ;
#45026 = CARTESIAN_POINT ( 'NONE',  ( -6.972266317189433020E-16, -31.12499999726880873, -5.000000000000000000 ) ) ;
#45027 = CARTESIAN_POINT ( 'NONE',  ( -4.458734124999998549, -19.47916666530107221, 2.574251347313722516 ) ) ;
#45028 = CARTESIAN_POINT ( 'NONE',  ( -5.000000000000000000, -101.0833333333333286, -2.886751345948128211 ) ) ;
#45029 = CARTESIAN_POINT ( 'NONE',  ( -2.229367062500000163, -7.479166665301073991, -3.861377020970580443 ) ) ;
#45030 = CARTESIAN_POINT ( 'NONE',  ( 1.846868145590735200, -147.2500000013656063, -4.458734124999999437 ) ) ;
#45031 = CARTESIAN_POINT ( 'NONE',  ( 9.457646018065525792E-16, 16.68750000136559564, 5.148502694627439702 ) ) ;
#45032 = EDGE_LOOP ( 'NONE', ( #19598, #53922, #33779, #8782 ) ) ;
#45033 = CYLINDRICAL_SURFACE ( 'NONE', #12030, 5.000000000000000000 ) ;
#45034 = CARTESIAN_POINT ( 'NONE',  ( 1.975475456537005874E-15, -71.62499999726878741, 5.000000000000000000 ) ) ;
#45035 = CARTESIAN_POINT ( 'NONE',  ( -2.229367062499996610, -18.14583333196773651, 3.861377020970582219 ) ) ;
#45036 = CARTESIAN_POINT ( 'NONE',  ( -58.24261429053147765, -143.2500000000000284, -3.805975901505573855 ) ) ;
#45037 = DIRECTION ( 'NONE',  ( -0.000000000000000000, 1.000000000000000000, -0.000000000000000000 ) ) ;
#45038 =( BOUNDED_CURVE ( )  B_SPLINE_CURVE ( 2, ( #40841, #11576, #1634, #16413, #10617, #60168, #21235, #5482, #44706 ),
 .UNSPECIFIED., .F., .F. ) 
 B_SPLINE_CURVE_WITH_KNOTS ( ( 3, 2, 2, 2, 3 ),
 ( 0.9520833333333332815, 0.9527777777777777235, 0.9541666666666667185, 0.9555555555555556024, 0.9562500000000000444 ),
 .UNSPECIFIED. ) 
 CURVE ( )  GEOMETRIC_REPRESENTATION_ITEM ( )  RATIONAL_B_SPLINE_CURVE ( ( 0.9330127018922194093, 0.9330127018922194093, 1.000000000000000000, 0.8660254037844387076, 1.000000000000000000, 0.8660254037844387076, 1.000000000000000000, 0.9330127018922194093, 0.9330127018922194093 ) ) 
 REPRESENTATION_ITEM ( '' )  );
#45039 = CARTESIAN_POINT ( 'NONE',  ( -50.70258187064364108, -151.1250000013655779, 2.196230717870141014 ) ) ;
#45040 = CARTESIAN_POINT ( 'NONE',  ( 2.500000000000002220, -46.54166666393547303, 4.330127018922192761 ) ) ;
#45041 = CARTESIAN_POINT ( 'NONE',  ( 5.000000000000000888, -67.45833333060214443, 2.886751345948126879 ) ) ;
#45042 = CARTESIAN_POINT ( 'NONE',  ( -2.229367062499996610, 13.85416666803226171, 3.861377020970582219 ) ) ;
#45043 = DIRECTION ( 'NONE',  ( -0.000000000000000000, 1.000000000000000000, -0.000000000000000000 ) ) ;
#45044 = CYLINDRICAL_SURFACE ( 'NONE', #14044, 5.000000000000000000 ) ;
#45045 = CARTESIAN_POINT ( 'NONE',  ( -2.229367062499996610, 10.85416666803225993, 3.861377020970582219 ) ) ;
#45046 = CARTESIAN_POINT ( 'NONE',  ( -2.229367062500000163, -67.47916666530106511, -3.861377020970580443 ) ) ;
#45047 = ORIENTED_EDGE ( 'NONE', *, *, #6119, .F. ) ;
#45048 = CARTESIAN_POINT ( 'NONE',  ( 9.457646018065525792E-16, -13.31249999863440259, 5.148502694627439702 ) ) ;
#45049 = CARTESIAN_POINT ( 'NONE',  ( -2.500000000000000444, 3.833333333333334370, -4.330127018922193649 ) ) ;
#45050 = CARTESIAN_POINT ( 'NONE',  ( -4.458734125000001214, -164.8750000013655779, 1.846868145590734089 ) ) ;
#45051 = CARTESIAN_POINT ( 'NONE',  ( -1.339745962155613812, -99.08034179853029855, -5.000000000000000000 ) ) ;
#45052 = CARTESIAN_POINT ( 'NONE',  ( -4.458734124999998549, -59.22916666530106511, 2.574251347313722516 ) ) ;
#45053 = CARTESIAN_POINT ( 'NONE',  ( 2.499999999999998668, -90.20833333060214443, -4.330127018922193649 ) ) ;
#45054 = CARTESIAN_POINT ( 'NONE',  ( -2.229367062500000163, -34.47916666530107221, -3.861377020970580443 ) ) ;
#45055 = CARTESIAN_POINT ( 'NONE',  ( 1.975475456537005874E-15, -41.62499999726880162, 5.000000000000000000 ) ) ;
#45056 =( BOUNDED_CURVE ( )  B_SPLINE_CURVE ( 2, ( #43127, #19313, #346, #13859, #9979, #32, #33483, #34749, #9344 ),
 .UNSPECIFIED., .F., .F. ) 
 B_SPLINE_CURVE_WITH_KNOTS ( ( 3, 2, 2, 2, 3 ),
 ( 0.9482142857142856762, 0.9488095238095237693, 0.9499999999999999556, 0.9511904761904761418, 0.9517857142857142350 ),
 .UNSPECIFIED. ) 
 CURVE ( )  GEOMETRIC_REPRESENTATION_ITEM ( )  RATIONAL_B_SPLINE_CURVE ( ( 0.9330127018922194093, 0.9330127018922194093, 1.000000000000000000, 0.8660254037844387076, 1.000000000000000000, 0.8660254037844387076, 1.000000000000000000, 0.9330127018922194093, 0.9330127018922194093 ) ) 
 REPRESENTATION_ITEM ( '' )  );
#45057 = CARTESIAN_POINT ( 'NONE',  ( 2.071067811865517694, -141.9375000027312126, -4.999999999999958256 ) ) ;
#45058 = CARTESIAN_POINT ( 'NONE',  ( 2.500000000000002220, -69.66666666666667140, 4.330127018922192761 ) ) ;
#45059 = CARTESIAN_POINT ( 'NONE',  ( -4.999999999999998224, -78.79166666393547303, 2.886751345948131764 ) ) ;
#45060 = CARTESIAN_POINT ( 'NONE',  ( -4.458734125000000326, -149.1250000013656063, 1.846868145590734089 ) ) ;
#45061 = CARTESIAN_POINT ( 'NONE',  ( 2.499999999999998668, -42.33333333333333570, -4.330127018922193649 ) ) ;
#45062 = CARTESIAN_POINT ( 'NONE',  ( -5.000000000000000000, -14.08333333333333037, -2.886751345948128211 ) ) ;
#45063 = CARTESIAN_POINT ( 'NONE',  ( 1.339745962155612702, -68.16965819600733312, -5.000000000000000000 ) ) ;
#45064 = ORIENTED_EDGE ( 'NONE', *, *, #95, .T. ) ;
#45065 = CARTESIAN_POINT ( 'NONE',  ( -2.229367062499996610, -105.1458333319677365, 3.861377020970582219 ) ) ;
#45066 = CARTESIAN_POINT ( 'NONE',  ( -4.458734124999999437, 2.437500001365593860, 0.000000000000000000 ) ) ;
#45067 = CYLINDRICAL_SURFACE ( 'NONE', #37062, 5.000000000000000000 ) ;
#45068 = CARTESIAN_POINT ( 'NONE',  ( 2.499999999999998668, -1.333333333333332149, -4.330127018922193649 ) ) ;
#45069 = CARTESIAN_POINT ( 'NONE',  ( 4.458734124999999437, -64.81249999863440792, -5.460374474430324690E-16 ) ) ;
#45070 = CARTESIAN_POINT ( 'NONE',  ( 6.123233995736766282E-16, -120.0000000000000000, -5.000000000000000000 ) ) ;
#45071 = CARTESIAN_POINT ( 'NONE',  ( 1.060575238724906964E-15, -9.624999997268814056, 5.773502691896257311 ) ) ;
#45073 = ORIENTED_EDGE ( 'NONE', *, *, #38544, .T. ) ;
#45072 = CARTESIAN_POINT ( 'NONE',  ( 9.457646018065525792E-16, -34.06249999863440792, 5.148502694627439702 ) ) ;
#45074 = CARTESIAN_POINT ( 'NONE',  ( -6.972266317189433020E-16, -78.24999999999998579, -5.000000000000000000 ) ) ;
#45075 = CARTESIAN_POINT ( 'NONE',  ( 1.975475456537005874E-15, -16.62499999726881583, 5.000000000000000000 ) ) ;
#45076 = ORIENTED_EDGE ( 'NONE', *, *, #47630, .F. ) ;
#45077 = CARTESIAN_POINT ( 'NONE',  ( 1.975475456537005874E-15, -55.62499999726880873, 5.000000000000000000 ) ) ;
#45078 = CARTESIAN_POINT ( 'NONE',  ( -2.500000000000000444, -48.16666666666666430, -4.330127018922193649 ) ) ;
#45080 = CARTESIAN_POINT ( 'NONE',  ( 9.457646018065525792E-16, -30.31249999863440436, 5.148502694627439702 ) ) ;
#45079 = CARTESIAN_POINT ( 'NONE',  ( 5.000000000000000000, -46.37499999726880873, -6.123233995736766282E-16 ) ) ;
#45081 = AXIS2_PLACEMENT_3D ( 'NONE', #40563, #1041, #15811 ) ;
#45082 = CYLINDRICAL_SURFACE ( 'NONE', #32740, 5.000000000000000000 ) ;
#45083 = CARTESIAN_POINT ( 'NONE',  ( 2.229367062500001939, -75.97916666530106511, 3.861377020970579999 ) ) ;
#45084 = CARTESIAN_POINT ( 'NONE',  ( -3.535533905932737309, -168.6250000000000284, -3.535533905932738197 ) ) ;
#45086 = EDGE_CURVE ( 'NONE', #176, #7443, #61427, .T. ) ;
#45085 = CARTESIAN_POINT ( 'NONE',  ( -4.458734124999999437, -79.39583333196773651, -2.574251347313719407 ) ) ;
#45087 = CARTESIAN_POINT ( 'NONE',  ( -59.29741812935640155, -140.8750000013656063, -2.196230717870135685 ) ) ;
#45088 = CARTESIAN_POINT ( 'NONE',  ( -2.229367062499996610, -31.39583333196773651, 3.861377020970582219 ) ) ;
#45089 = ORIENTED_EDGE ( 'NONE', *, *, #3576, .T. ) ;
#45090 = LINE ( 'NONE', #50233, #5325 ) ;
#45091 = VERTEX_POINT ( 'NONE', #23122 ) ;
#45092 = CARTESIAN_POINT ( 'NONE',  ( -4.458734124999998549, -71.47916666530107932, 2.574251347313722516 ) ) ;
#45093 = CARTESIAN_POINT ( 'NONE',  ( -4.999999999999998224, 22.20833333606451987, 2.886751345948131764 ) ) ;
#45094 = ORIENTED_EDGE ( 'NONE', *, *, #38212, .T. ) ;
#45095 = DIRECTION ( 'NONE',  ( -0.000000000000000000, 1.000000000000000000, -0.000000000000000000 ) ) ;
#45096 = CARTESIAN_POINT ( 'NONE',  ( -1.339745962155610925, -75.66965819600731891, 5.000000000000000000 ) ) ;
#45097 = CARTESIAN_POINT ( 'NONE',  ( -4.458734124999998549, -64.47916666530106511, 2.574251347313722516 ) ) ;
#45098 = CARTESIAN_POINT ( 'NONE',  ( 4.458734125000001214, -2.145833331967737845, 2.574251347313718519 ) ) ;
#45099 = VERTEX_POINT ( 'NONE', #42726 ) ;
#45100 = CARTESIAN_POINT ( 'NONE',  ( 2.499999999999998668, -62.33333333333333570, -4.330127018922193649 ) ) ;
#45101 = CYLINDRICAL_SURFACE ( 'NONE', #13042, 5.000000000000000000 ) ;
#45102 = CARTESIAN_POINT ( 'NONE',  ( 2.229367062499998831, 15.35416666803225993, -3.861377020970580887 ) ) ;
#45103 = CARTESIAN_POINT ( 'NONE',  ( -59.29741812935640155, -140.6250000013656063, -2.196230717870135685 ) ) ;
#45104 = CARTESIAN_POINT ( 'NONE',  ( 2.499999999999998668, -47.20833333060214443, -4.330127018922193649 ) ) ;
#45105 = CARTESIAN_POINT ( 'NONE',  ( 2.730187237215162345E-16, -162.1875000013655779, -4.458734124999999437 ) ) ;
#45106 =( BOUNDED_CURVE ( )  B_SPLINE_CURVE ( 2, ( #54050, #63404, #3917, #28345, #47962, #13870, #9987, #38617, #29275 ),
 .UNSPECIFIED., .F., .F. ) 
 B_SPLINE_CURVE_WITH_KNOTS ( ( 3, 2, 2, 2, 3 ),
 ( 0.8479166666666666519, 0.8486111111111110938, 0.8499999999999999778, 0.8513888888888888618, 0.8520833333333333037 ),
 .UNSPECIFIED. ) 
 CURVE ( )  GEOMETRIC_REPRESENTATION_ITEM ( )  RATIONAL_B_SPLINE_CURVE ( ( 0.9330127018922194093, 0.9330127018922194093, 1.000000000000000000, 0.8660254037844387076, 1.000000000000000000, 0.8660254037844387076, 1.000000000000000000, 0.9330127018922194093, 0.9330127018922194093 ) ) 
 REPRESENTATION_ITEM ( '' )  );
#45107 = CARTESIAN_POINT ( 'NONE',  ( -1.339745962155610925, 19.33034180399266688, 5.000000000000000000 ) ) ;
#45108 = ORIENTED_EDGE ( 'NONE', *, *, #32681, .T. ) ;
#45109 = CARTESIAN_POINT ( 'NONE',  ( -4.458734124999999437, -80.31249999863440792, 0.000000000000000000 ) ) ;
#45110 = CARTESIAN_POINT ( 'NONE',  ( -6.972266317189433020E-16, -75.25000000000000000, -5.000000000000000000 ) ) ;
#45111 = CARTESIAN_POINT ( 'NONE',  ( 4.458734124999998549, -1.729166665301068440, -2.574251347313721627 ) ) ;
#45112 = CARTESIAN_POINT ( 'NONE',  ( 1.339745962155612258, 25.41965820146970501, 5.000000000000000888 ) ) ;
#45113 = CARTESIAN_POINT ( 'NONE',  ( 5.000000000000000888, -36.58333333333332149, 2.886751345948126879 ) ) ;
#45114 = CARTESIAN_POINT ( 'NONE',  ( 2.229367062499998831, -71.89583333196773651, -3.861377020970580887 ) ) ;
#45115 = CARTESIAN_POINT ( 'NONE',  ( -5.000000000000000000, -27.87499999726880873, 0.000000000000000000 ) ) ;
#45116 = CARTESIAN_POINT ( 'NONE',  ( 1.975475456537005874E-15, -72.62499999726878741, 5.000000000000000000 ) ) ;
#45117 = CARTESIAN_POINT ( 'NONE',  ( -5.000000000000000000, -82.87499999726881583, 0.000000000000000000 ) ) ;
#45118 = CARTESIAN_POINT ( 'NONE',  ( 5.000000000000000888, -58.58333333333333570, 2.886751345948126879 ) ) ;
#45119 = CARTESIAN_POINT ( 'NONE',  ( -4.458734124999999437, -43.39583333196774362, -2.574251347313719407 ) ) ;
#45120 = CARTESIAN_POINT ( 'NONE',  ( -3.152548672688508926E-16, -34.81249999863440792, -5.148502694627439702 ) ) ;
#45121 = CARTESIAN_POINT ( 'NONE',  ( -3.152548672688508926E-16, 4.187500001365595637, -5.148502694627439702 ) ) ;
#45122 = FACE_OUTER_BOUND ( 'NONE', #8935, .T. ) ;
#45123 = CARTESIAN_POINT ( 'NONE',  ( 5.000000000000000000, 19.58333333333333215, -2.886751345948129988 ) ) ;
#45124 = CARTESIAN_POINT ( 'NONE',  ( -2.071067811865475061, -143.8125000027312126, -5.000000000000000888 ) ) ;
#45125 = LINE ( 'NONE', #39649, #24321 ) ;
#45126 = VECTOR ( 'NONE', #32089, 1000.000000000000000 ) ;
#45127 = CARTESIAN_POINT ( 'NONE',  ( 4.458734125000001214, -43.89583333196775072, 2.574251347313718519 ) ) ;
#45128 = CARTESIAN_POINT ( 'NONE',  ( 1.060575238724906964E-15, -71.62499999726880162, 5.773502691896257311 ) ) ;
#45129 = CARTESIAN_POINT ( 'NONE',  ( -50.55543936806279248, -144.3125000013656063, 0.3552334253322060320 ) ) ;
#45130 = CARTESIAN_POINT ( 'NONE',  ( 5.000000000000000000, -24.37499999726881228, -6.123233995736766282E-16 ) ) ;
#45131 = CARTESIAN_POINT ( 'NONE',  ( 1.975475456537005874E-15, -15.62499999726881406, 5.000000000000000000 ) ) ;
#45132 = CARTESIAN_POINT ( 'NONE',  ( 4.458734125000000326, -81.14583333196773651, 2.574251347313718519 ) ) ;
#45133 = CARTESIAN_POINT ( 'NONE',  ( 1.846868145590736310, -166.8750000013656063, 4.458734124999997661 ) ) ;
#45134 = CARTESIAN_POINT ( 'NONE',  ( 6.123233995736766282E-16, -120.0000000000000000, -5.000000000000000000 ) ) ;
#45135 = CARTESIAN_POINT ( 'NONE',  ( -7.777900015783941967, -4.169681370001537601, -7.928862157988302073 ) ) ;
#45136 = CARTESIAN_POINT ( 'NONE',  ( -5.000000000000000000, -28.99999999999999645, 0.000000000000000000 ) ) ;
#45137 = CARTESIAN_POINT ( 'NONE',  ( 4.458734124999999437, -140.4375000013656063, 0.000000000000000000 ) ) ;
#45138 = ORIENTED_EDGE ( 'NONE', *, *, #5090, .F. ) ;
#45139 = CARTESIAN_POINT ( 'NONE',  ( 9.457646018065525792E-16, 20.68750000136559564, 5.148502694627439702 ) ) ;
#45140 = ORIENTED_EDGE ( 'NONE', *, *, #12294, .T. ) ;
#45141 = CARTESIAN_POINT ( 'NONE',  ( 2.229367062500001939, -62.22916666530106511, 3.861377020970579999 ) ) ;
#45142 = VECTOR ( 'NONE', #25395, 1000.000000000000000 ) ;
#45143 = CARTESIAN_POINT ( 'NONE',  ( 1.060575238724906964E-15, 24.37500000273118417, 5.773502691896257311 ) ) ;
#45144 = DIRECTION ( 'NONE',  ( -0.000000000000000000, 1.000000000000000000, -0.000000000000000000 ) ) ;
#45145 = CARTESIAN_POINT ( 'NONE',  ( -2.499999999999996447, 14.16666666666666785, 4.330127018922195425 ) ) ;
#45146 = CARTESIAN_POINT ( 'NONE',  ( 9.457646018065525792E-16, -52.06249999863440792, 5.148502694627439702 ) ) ;
#45147 = CARTESIAN_POINT ( 'NONE',  ( 2.229367062499998831, -9.645833331967738289, -3.861377020970580887 ) ) ;
#45148 = CARTESIAN_POINT ( 'NONE',  ( 2.071067811865443975, -165.9375000027311557, -5.000000000000031974 ) ) ;
#45149 = CARTESIAN_POINT ( 'NONE',  ( -4.999999999999998224, -63.79166666393547303, 2.886751345948131764 ) ) ;
#45150 = CARTESIAN_POINT ( 'NONE',  ( 1.975475456537005874E-15, -89.62499999726880162, 5.000000000000000000 ) ) ;
#45151 = CARTESIAN_POINT ( 'NONE',  ( -6.972266317189433020E-16, -75.12499999726880162, -5.000000000000000000 ) ) ;
#45152 = CARTESIAN_POINT ( 'NONE',  ( 5.000000000000000888, -56.45833333060214443, 2.886751345948126879 ) ) ;
#45154 = CARTESIAN_POINT ( 'NONE',  ( 4.458734125000001214, -15.14583333196773651, 2.574251347313718519 ) ) ;
#45153 = CARTESIAN_POINT ( 'NONE',  ( -5.000000000000000000, -79.00000000000000000, 0.000000000000000000 ) ) ;
#45155 = CARTESIAN_POINT ( 'NONE',  ( -3.535533905932738641, -140.5000000027311842, 3.535533905932737309 ) ) ;
#45156 = CARTESIAN_POINT ( 'NONE',  ( 9.457646018065525792E-16, -60.06249999863440792, 5.148502694627439702 ) ) ;
#45157 = CARTESIAN_POINT ( 'NONE',  ( -4.458734125000000326, -156.2500000013656063, -1.846868145590735644 ) ) ;
#45158 = ADVANCED_FACE ( 'NONE', ( #51766 ), #62371, .T. ) ;
#45159 = CARTESIAN_POINT ( 'NONE',  ( 5.000000000000000888, -56.45833333060213732, 2.886751345948126879 ) ) ;
#45160 = VERTEX_POINT ( 'NONE', #17671 ) ;
#45161 = CARTESIAN_POINT ( 'NONE',  ( 0.000000000000000000, 30.00000000000000000, 5.000000000000000000 ) ) ;
#45162 = CARTESIAN_POINT ( 'NONE',  ( -4.458734124999999437, 1.437500001365592972, 0.000000000000000000 ) ) ;
#45163 = ORIENTED_EDGE ( 'NONE', *, *, #9167, .F. ) ;
#45165 = CARTESIAN_POINT ( 'NONE',  ( 5.000000000000000000, 11.62500000273118594, -6.123233995736766282E-16 ) ) ;
#45164 = CYLINDRICAL_SURFACE ( 'NONE', #9130, 5.000000000000000000 ) ;
#45166 = CARTESIAN_POINT ( 'NONE',  ( 2.730187237215162345E-16, -157.1875000013655779, -4.458734124999999437 ) ) ;
#45167 = ORIENTED_EDGE ( 'NONE', *, *, #48287, .F. ) ;
#45168 = CARTESIAN_POINT ( 'NONE',  ( 5.000000000000000888, 5.416666666666666963, 2.886751345948126879 ) ) ;
#45169 = ADVANCED_FACE ( 'NONE', ( #37285 ), #12832, .T. ) ;
#45170 = CARTESIAN_POINT ( 'NONE',  ( 5.000000000000000000, -99.41666666666665719, -2.886751345948130876 ) ) ;
#45171 = CARTESIAN_POINT ( 'NONE',  ( -58.24261429053147765, -130.2500000000000284, -3.805975901505573855 ) ) ;
#45172 = CYLINDRICAL_SURFACE ( 'NONE', #4149, 5.000000000000000000 ) ;
#45173 = CARTESIAN_POINT ( 'NONE',  ( 4.458734125000001214, -49.14583333196772941, 2.574251347313718519 ) ) ;
#45174 = VERTEX_POINT ( 'NONE', #48502 ) ;
#45175 = CARTESIAN_POINT ( 'NONE',  ( 1.975475456537005874E-15, 10.37500000273118417, 5.000000000000000000 ) ) ;
#45176 = EDGE_CURVE ( 'NONE', #26085, #11102, #34337, .T. ) ;
#45177 = CARTESIAN_POINT ( 'NONE',  ( -2.229367062499996610, 12.85416666803226171, 3.861377020970582219 ) ) ;
#45178 = CARTESIAN_POINT ( 'NONE',  ( 4.458734124999999437, 29.18750000136559208, -5.460374474430324690E-16 ) ) ;
#45179 = CARTESIAN_POINT ( 'NONE',  ( -52.10840900171896806, -152.1875000013656063, 3.393966926194110556 ) ) ;
#45180 = CARTESIAN_POINT ( 'NONE',  ( 5.000000000000000888, -25.58333333333333215, 2.886751345948126879 ) ) ;
#45181 = CARTESIAN_POINT ( 'NONE',  ( -59.98410592259440222, -147.2500000027312126, -0.3983568153799752487 ) ) ;
#45182 = CARTESIAN_POINT ( 'NONE',  ( -2.229367062500000163, -64.47916666530106511, -3.861377020970580443 ) ) ;
#45183 = CARTESIAN_POINT ( 'NONE',  ( -4.999999999999998224, -49.79166666393547303, 2.886751345948131764 ) ) ;
#45184 = CARTESIAN_POINT ( 'NONE',  ( -4.458734124999998549, 18.77083333469893134, 2.574251347313722516 ) ) ;
#45185 = CARTESIAN_POINT ( 'NONE',  ( 1.975475456537005874E-15, -78.62499999726881583, 5.000000000000000000 ) ) ;
#45186 = CARTESIAN_POINT ( 'NONE',  ( -2.499999999999996447, -26.83333333333333570, 4.330127018922195425 ) ) ;
#45187 = CARTESIAN_POINT ( 'NONE',  ( 2.229367062499998831, -47.89583333196774362, -3.861377020970580887 ) ) ;
#45188 = CARTESIAN_POINT ( 'NONE',  ( -2.500000000000000444, -11.04166666393547835, -4.330127018922193649 ) ) ;
#45189 = CARTESIAN_POINT ( 'NONE',  ( 1.339745962155612702, -42.16965819600732601, -5.000000000000000000 ) ) ;
#45190 = DIRECTION ( 'NONE',  ( 0.000000000000000000, 0.000000000000000000, 1.000000000000000000 ) ) ;
#45191 = CARTESIAN_POINT ( 'NONE',  ( 4.458734125000001214, -89.14583333196775072, 2.574251347313718519 ) ) ;
#45192 = DIRECTION ( 'NONE',  ( -0.000000000000000000, 1.000000000000000000, -0.000000000000000000 ) ) ;
#45193 = CARTESIAN_POINT ( 'NONE',  ( 2.229367062499998831, -17.89583333196773651, -3.861377020970580887 ) ) ;
#45194 = VERTEX_POINT ( 'NONE', #4439 ) ;
#45195 = CARTESIAN_POINT ( 'NONE',  ( -5.000000000000000000, -46.87499999726880873, 0.000000000000000000 ) ) ;
#45196 = CARTESIAN_POINT ( 'NONE',  ( -4.458734124999999437, -105.3958333319677365, -2.574251347313719407 ) ) ;
#45197 = CARTESIAN_POINT ( 'NONE',  ( 5.000000000000000000, -159.1875000027312410, 2.071067811865478614 ) ) ;
#45198 = ORIENTED_EDGE ( 'NONE', *, *, #38048, .T. ) ;
#45199 = CARTESIAN_POINT ( 'NONE',  ( -4.458734124999999437, -99.56249999863440792, 0.000000000000000000 ) ) ;
#45200 = CARTESIAN_POINT ( 'NONE',  ( 3.061616997868383141E-16, -162.8750000027311842, -5.000000000000000000 ) ) ;
#45201 = CARTESIAN_POINT ( 'NONE',  ( -5.000000000000000000, -54.95833333060213732, -2.886751345948128211 ) ) ;
#45202 = CARTESIAN_POINT ( 'NONE',  ( 2.499999999999998668, -62.20833333060214443, -4.330127018922193649 ) ) ;
#45203 = CARTESIAN_POINT ( 'NONE',  ( -52.10840900171896806, -127.1875000013656063, 3.393966926194110556 ) ) ;
#45204 = CARTESIAN_POINT ( 'NONE',  ( -57.19623071787016499, -141.3750000013656063, 4.297418129356382899 ) ) ;
#45205 = EDGE_CURVE ( 'NONE', #44248, #13925, #18609, .T. ) ;
#45206 = CARTESIAN_POINT ( 'NONE',  ( 4.458734124999998549, -24.72916666530106866, -2.574251347313721627 ) ) ;
#45207 = CARTESIAN_POINT ( 'NONE',  ( 2.229367062499998831, 8.104166668032261711, -3.861377020970580887 ) ) ;
#45208 = CARTESIAN_POINT ( 'NONE',  ( 4.458734124999998549, -66.97916666530106511, -2.574251347313721627 ) ) ;
#45209 = CYLINDRICAL_SURFACE ( 'NONE', #34661, 5.000000000000000000 ) ;
#45210 = CARTESIAN_POINT ( 'NONE',  ( 2.229367062499998831, -17.64583333196773651, -3.861377020970580887 ) ) ;
#45211 = CARTESIAN_POINT ( 'NONE',  ( -6.972266317189433020E-16, 3.875000002731185500, -5.000000000000000000 ) ) ;
#45212 = CARTESIAN_POINT ( 'NONE',  ( 3.061616997868383141E-16, -149.7500000000000284, -5.000000000000000000 ) ) ;
#45213 = CARTESIAN_POINT ( 'NONE',  ( 5.000000000000000000, -13.41666666666666607, -2.886751345948129988 ) ) ;
#45214 = CARTESIAN_POINT ( 'NONE',  ( 4.458734125000000326, -156.3750000013655779, -1.846868145590734978 ) ) ;
#45215 = ORIENTED_EDGE ( 'NONE', *, *, #20076, .T. ) ;
#45216 = VECTOR ( 'NONE', #58242, 1000.000000000000000 ) ;
#45217 = CARTESIAN_POINT ( 'NONE',  ( -4.458734124999997661, -44.47916666530106511, 2.574251347313722516 ) ) ;
#45218 = LINE ( 'NONE', #1184, #19122 ) ;
#45219 = CARTESIAN_POINT ( 'NONE',  ( 2.500000000000002220, -92.66666666666665719, 4.330127018922192761 ) ) ;
#45220 = CARTESIAN_POINT ( 'NONE',  ( -5.000000000000000000, 27.99999999999999645, 0.000000000000000000 ) ) ;
#45221 = AXIS2_PLACEMENT_3D ( 'NONE', #32723, #28521, #8905 ) ;
#45222 = CARTESIAN_POINT ( 'NONE',  ( 4.458734124999999437, 2.187500001365593416, -5.460374474430324690E-16 ) ) ;
#45223 = CARTESIAN_POINT ( 'NONE',  ( 5.000000000000000888, -93.58333333333332860, 2.886751345948126879 ) ) ;
#45224 = CARTESIAN_POINT ( 'NONE',  ( 5.000000000000000888, -82.58333333333334281, 2.886751345948126879 ) ) ;
#45225 = CARTESIAN_POINT ( 'NONE',  ( 2.229367062500001939, 19.77083333469892779, 3.861377020970579999 ) ) ;
#45226 = CARTESIAN_POINT ( 'NONE',  ( -4.999999999999999112, -74.91666666666665719, 2.886751345948131764 ) ) ;
#45227 = CARTESIAN_POINT ( 'NONE',  ( -2.499999999999996447, 8.291666669397852019, 4.330127018922195425 ) ) ;
#45228 = ORIENTED_EDGE ( 'NONE', *, *, #31385, .F. ) ;
#45229 = CARTESIAN_POINT ( 'NONE',  ( 1.975475456537005874E-15, -30.74999999999999645, 5.000000000000000000 ) ) ;
#45230 = ORIENTED_EDGE ( 'NONE', *, *, #57397, .F. ) ;
#45231 = CARTESIAN_POINT ( 'NONE',  ( 5.000000000000000888, -85.58333333333332860, 2.886751345948126879 ) ) ;
#45232 = CARTESIAN_POINT ( 'NONE',  ( 2.229367062499998831, -42.64583333196773651, -3.861377020970580887 ) ) ;
#45233 =( BOUNDED_CURVE ( )  B_SPLINE_CURVE ( 2, ( #8428, #14176, #9047, #18386, #37684, #33184, #4529, #13242, #53110 ),
 .UNSPECIFIED., .F., .F. ) 
 B_SPLINE_CURVE_WITH_KNOTS ( ( 3, 2, 2, 2, 3 ),
 ( 0.5589285714285714413, 0.5595238095238095344, 0.5607142857142857206, 0.5619047619047619069, 0.5625000000000000000 ),
 .UNSPECIFIED. ) 
 CURVE ( )  GEOMETRIC_REPRESENTATION_ITEM ( )  RATIONAL_B_SPLINE_CURVE ( ( 0.9330127018922194093, 0.9330127018922194093, 1.000000000000000000, 0.8660254037844387076, 1.000000000000000000, 0.8660254037844387076, 1.000000000000000000, 0.9330127018922194093, 0.9330127018922194093 ) ) 
 REPRESENTATION_ITEM ( '' )  );
#45234 = EDGE_CURVE ( 'NONE', #27373, #24115, #42598, .T. ) ;
#45235 = CARTESIAN_POINT ( 'NONE',  ( -3.535250795749689387E-16, -41.12499999726880162, -5.773502691896257311 ) ) ;
#45236 = EDGE_CURVE ( 'NONE', #4902, #52130, #62340, .T. ) ;
#45237 = ORIENTED_EDGE ( 'NONE', *, *, #59431, .F. ) ;
#45238 = CARTESIAN_POINT ( 'NONE',  ( 4.458734125000001214, -17.89583333196774007, 2.574251347313718519 ) ) ;
#45239 = ORIENTED_EDGE ( 'NONE', *, *, #51539, .F. ) ;
#45240 = CARTESIAN_POINT ( 'NONE',  ( -3.535250795749689387E-16, -81.25000000000001421, -5.773502691896257311 ) ) ;
#45241 = CARTESIAN_POINT ( 'NONE',  ( 1.846868145590735200, -168.2500000013656063, -4.458734125000000326 ) ) ;
#45242 = CARTESIAN_POINT ( 'NONE',  ( 5.000000000000000888, -86.45833333060213022, 2.886751345948126879 ) ) ;
#45244 = VERTEX_POINT ( 'NONE', #53961 ) ;
#45243 = CARTESIAN_POINT ( 'NONE',  ( 2.499999999999998668, -55.33333333333332860, -4.330127018922193649 ) ) ;
#45245 = CARTESIAN_POINT ( 'NONE',  ( -59.81910112700025905, -142.1875000000000284, -2.462841084822630311 ) ) ;
#45246 = CARTESIAN_POINT ( 'NONE',  ( -2.229367062500000163, -27.72916666530107221, -3.861377020970580443 ) ) ;
#45247 = CARTESIAN_POINT ( 'NONE',  ( -6.972266317189433020E-16, -50.24999999999999289, -5.000000000000000000 ) ) ;
#45248 = EDGE_CURVE ( 'NONE', #20419, #23270, #1110, .T. ) ;
#45249 = ORIENTED_EDGE ( 'NONE', *, *, #38099, .T. ) ;
#45250 = APPLICATION_PROTOCOL_DEFINITION ( 'draft international standard', 'automotive_design', 1998, #16684 ) ;
#45251 = CARTESIAN_POINT ( 'NONE',  ( -4.458734125000001214, -164.1250000013656063, 1.846868145590734089 ) ) ;
#45252 = EDGE_CURVE ( 'NONE', #42565, #44963, #3541, .T. ) ;
#45253 = CARTESIAN_POINT ( 'NONE',  ( 2.229367062499998831, 27.35416666803225993, -3.861377020970580887 ) ) ;
#45254 = DIRECTION ( 'NONE',  ( 0.000000000000000000, 0.000000000000000000, 1.000000000000000000 ) ) ;
#45255 = ORIENTED_EDGE ( 'NONE', *, *, #15869, .T. ) ;
#45256 = CARTESIAN_POINT ( 'NONE',  ( -4.999999999999998224, -25.91666666666666430, 2.886751345948131764 ) ) ;
#45257 = CARTESIAN_POINT ( 'NONE',  ( -53.51423613279429503, -146.5000000013656347, 4.591703134518083651 ) ) ;
#45258 = CARTESIAN_POINT ( 'NONE',  ( -3.152548672688508926E-16, -73.81249999863440792, -5.148502694627439702 ) ) ;
#45259 = CARTESIAN_POINT ( 'NONE',  ( -58.80597590150559739, -134.1250000027312126, 3.242614290531460330 ) ) ;
#45260 = CARTESIAN_POINT ( 'NONE',  ( -4.458734124999999437, -42.31249999863440081, 0.000000000000000000 ) ) ;
#45261 = CARTESIAN_POINT ( 'NONE',  ( -8.190561711645485556E-16, -141.9375000013656063, 4.458734124999999437 ) ) ;
#45262 = CARTESIAN_POINT ( 'NONE',  ( 4.458734125000000326, -46.89583333196773651, 2.574251347313718519 ) ) ;
#45263 = AXIS2_PLACEMENT_3D ( 'NONE', #54405, #1352, #25447 ) ;
#45264 = CARTESIAN_POINT ( 'NONE',  ( 5.000000000000000888, 29.41666666666666785, 2.886751345948126879 ) ) ;
#45265 = CARTESIAN_POINT ( 'NONE',  ( -2.229367062499996610, -18.14583333196773651, 3.861377020970582219 ) ) ;
#45266 = CARTESIAN_POINT ( 'NONE',  ( -2.499999999999996447, -103.8333333333333286, 4.330127018922195425 ) ) ;
#45267 = CARTESIAN_POINT ( 'NONE',  ( -1.846868145590737420, -142.0000000013655495, 4.458734124999999437 ) ) ;
#45268 = CARTESIAN_POINT ( 'NONE',  ( -4.458734124999999437, -35.56249999863440792, 0.000000000000000000 ) ) ;
#45269 = CARTESIAN_POINT ( 'NONE',  ( -3.535250795749689387E-16, 5.875000002731185056, -5.773502691896257311 ) ) ;
#45270 = CARTESIAN_POINT ( 'NONE',  ( 0.000000000000000000, -170.0000000000000000, 0.000000000000000000 ) ) ;
#45271 = CARTESIAN_POINT ( 'NONE',  ( -50.70258187064364108, -129.1250000013655779, 2.196230717870141014 ) ) ;
#45272 = CARTESIAN_POINT ( 'NONE',  ( 4.458734124999999437, -75.06249999863440792, -5.460374474430324690E-16 ) ) ;
#45273 = CARTESIAN_POINT ( 'NONE',  ( 6.123233995736766282E-16, -170.0000000000000000, -5.000000000000000000 ) ) ;
#45274 = DIRECTION ( 'NONE',  ( -0.000000000000000000, 1.000000000000000000, -0.000000000000000000 ) ) ;
#45275 = CARTESIAN_POINT ( 'NONE',  ( 4.458734125000000326, -2.145833331967737845, 2.574251347313718519 ) ) ;
#45276 = VERTEX_POINT ( 'NONE', #43048 ) ;
#45277 = DIRECTION ( 'NONE',  ( -0.000000000000000000, 1.000000000000000000, -0.000000000000000000 ) ) ;
#45278 = CARTESIAN_POINT ( 'NONE',  ( -5.000000000000000000, -60.08333333333333570, -2.886751345948128211 ) ) ;
#45280 = CARTESIAN_POINT ( 'NONE',  ( -2.229367062500000163, -36.47916666530107221, -3.861377020970580443 ) ) ;
#45279 = CARTESIAN_POINT ( 'NONE',  ( 9.457646018065525792E-16, -86.06249999863439371, 5.148502694627439702 ) ) ;
#45281 = CARTESIAN_POINT ( 'NONE',  ( 5.000000000000000000, -95.41666666666667140, -2.886751345948130876 ) ) ;
#45282 = CARTESIAN_POINT ( 'NONE',  ( 4.458734124999999437, -84.06249999863439371, -5.460374474430324690E-16 ) ) ;
#45283 = CARTESIAN_POINT ( 'NONE',  ( 4.458734124999999437, 16.93750000136559564, -5.460374474430324690E-16 ) ) ;
#45284 = CARTESIAN_POINT ( 'NONE',  ( 1.975475456537005874E-15, -42.62499999726880873, 5.000000000000000000 ) ) ;
#45285 = CARTESIAN_POINT ( 'NONE',  ( -59.29741812935640155, -137.6250000013655779, -2.196230717870135685 ) ) ;
#45286 = CARTESIAN_POINT ( 'NONE',  ( 9.457646018065525792E-16, -8.062499998634404363, 5.148502694627439702 ) ) ;
#45287 = CARTESIAN_POINT ( 'NONE',  ( -2.229367062499996610, 22.60416666803225993, 3.861377020970582219 ) ) ;
#45288 = CARTESIAN_POINT ( 'NONE',  ( -2.229367062500000163, -48.72916666530106511, -3.861377020970580443 ) ) ;
#45289 =( BOUNDED_CURVE ( )  B_SPLINE_CURVE ( 2, ( #47309, #17415, #3262, #11616, #27362, #7448, #2000, #62108, #46996 ),
 .UNSPECIFIED., .F., .F. ) 
 B_SPLINE_CURVE_WITH_KNOTS ( ( 3, 2, 2, 2, 3 ),
 ( 0.8249999999999997335, 0.8291666666666664964, 0.8333333333333331483, 0.8374999999999998002, 0.8416666666666664520 ),
 .UNSPECIFIED. ) 
 CURVE ( )  GEOMETRIC_REPRESENTATION_ITEM ( )  RATIONAL_B_SPLINE_CURVE ( ( 1.000000000000003997, 0.9238795325112826307, 1.000000000000000000, 0.9238795325112867385, 1.000000000000000000, 0.9238795325112867385, 1.000000000000000000, 0.9238795325112908463, 0.9999999999999958922 ) ) 
 REPRESENTATION_ITEM ( '' )  );
#45290 = CARTESIAN_POINT ( 'NONE',  ( 1.339745962155615144, -15.70534180126148271, 4.999999999999999112 ) ) ;
#45291 = CARTESIAN_POINT ( 'NONE',  ( 4.458734124999999437, -84.81249999863439371, -5.460374474430324690E-16 ) ) ;
#45292 = CARTESIAN_POINT ( 'NONE',  ( 4.458734124999999437, -5.812499998634403475, -5.460374474430324690E-16 ) ) ;
#45293 = VERTEX_POINT ( 'NONE', #49134 ) ;
#45294 = CARTESIAN_POINT ( 'NONE',  ( 4.458734124999998549, -27.97916666530107221, -2.574251347313721627 ) ) ;
#45295 = CARTESIAN_POINT ( 'NONE',  ( -55.35523342533222291, -130.5625000013656063, 4.444560631937231499 ) ) ;
#45296 = CARTESIAN_POINT ( 'NONE',  ( -4.458734124999998549, -77.22916666530106511, 2.574251347313722516 ) ) ;
#45297 = CARTESIAN_POINT ( 'NONE',  ( 2.500000000000002220, -108.5416666639354730, 4.330127018922192761 ) ) ;
#45298 = CARTESIAN_POINT ( 'NONE',  ( -3.152548672688508926E-16, 19.43750000136559208, -5.148502694627439702 ) ) ;
#45299 = CARTESIAN_POINT ( 'NONE',  ( -2.500000000000000444, -65.16666666666667140, -4.330127018922193649 ) ) ;
#45300 = DIRECTION ( 'NONE',  ( 0.000000000000000000, 0.000000000000000000, 1.000000000000000000 ) ) ;
#45301 = CARTESIAN_POINT ( 'NONE',  ( -4.458734124999999437, -79.64583333196773651, -2.574251347313719407 ) ) ;
#45302 = CARTESIAN_POINT ( 'NONE',  ( 5.000000000000000888, -57.58333333333334281, 2.886751345948126879 ) ) ;
#45303 = CARTESIAN_POINT ( 'NONE',  ( 5.000000000000000000, -36.29166666393547303, -2.886751345948130876 ) ) ;
#45304 = CARTESIAN_POINT ( 'NONE',  ( 5.000000000000000000, 26.70833333606451632, -2.886751345948129988 ) ) ;
#45305 = VERTEX_POINT ( 'NONE', #5077 ) ;
#45306 = DIRECTION ( 'NONE',  ( -0.000000000000000000, 1.000000000000000000, -0.000000000000000000 ) ) ;
#45307 = CARTESIAN_POINT ( 'NONE',  ( 2.499999999999998668, -52.20833333060213732, -4.330127018922193649 ) ) ;
#45309 = CARTESIAN_POINT ( 'NONE',  ( 5.000000000000000888, -18.58333333333333215, 2.886751345948126879 ) ) ;
#45308 = LINE ( 'NONE', #21187, #29726 ) ;
#45310 = CARTESIAN_POINT ( 'NONE',  ( -4.458734124999999437, -20.31249999863440081, 0.000000000000000000 ) ) ;
#45311 = VECTOR ( 'NONE', #62918, 1000.000000000000000 ) ;
#45312 = CARTESIAN_POINT ( 'NONE',  ( -2.229367062499996610, -88.14583333196773651, 3.861377020970582219 ) ) ;
#45313 = ADVANCED_FACE ( 'NONE', ( #14088 ), #19865, .T. ) ;
#45314 = CARTESIAN_POINT ( 'NONE',  ( -2.500000000000000444, -25.04166666393547658, -4.330127018922193649 ) ) ;
#45316 = ORIENTED_EDGE ( 'NONE', *, *, #51601, .T. ) ;
#45315 = CARTESIAN_POINT ( 'NONE',  ( 2.229367062500001939, -54.97916666530107221, 3.861377020970579999 ) ) ;
#45317 = CARTESIAN_POINT ( 'NONE',  ( 1.975475456537005874E-15, -35.62499999726880162, 5.000000000000000000 ) ) ;
#45318 = DIRECTION ( 'NONE',  ( 0.000000000000000000, 0.000000000000000000, 1.000000000000000000 ) ) ;
#45320 = ORIENTED_EDGE ( 'NONE', *, *, #45234, .T. ) ;
#45319 = CARTESIAN_POINT ( 'NONE',  ( -4.458734124999999437, -3.562499998634407916, 0.000000000000000000 ) ) ;
#45321 =( BOUNDED_CURVE ( )  B_SPLINE_CURVE ( 2, ( #44090, #4864, #33509, #42837, #38629, #62479, #43147, #32879, #18706 ),
 .UNSPECIFIED., .F., .F. ) 
 B_SPLINE_CURVE_WITH_KNOTS ( ( 3, 2, 2, 2, 3 ),
 ( 0.3339285714285714080, 0.3345238095238095011, 0.3357142857142856873, 0.3369047619047619291, 0.3375000000000000222 ),
 .UNSPECIFIED. ) 
 CURVE ( )  GEOMETRIC_REPRESENTATION_ITEM ( )  RATIONAL_B_SPLINE_CURVE ( ( 0.9330127018922194093, 0.9330127018922194093, 1.000000000000000000, 0.8660254037844387076, 1.000000000000000000, 0.8660254037844387076, 1.000000000000000000, 0.9330127018922194093, 0.9330127018922194093 ) ) 
 REPRESENTATION_ITEM ( '' )  );
#45322 = CARTESIAN_POINT ( 'NONE',  ( -50.70258187064364108, -150.1250000013656063, 2.196230717870141014 ) ) ;
#45323 = CARTESIAN_POINT ( 'NONE',  ( 2.499999999999998668, -65.33333333333332860, -4.330127018922193649 ) ) ;
#45324 = CARTESIAN_POINT ( 'NONE',  ( -4.458734125000001214, -152.1250000013655779, 1.846868145590734089 ) ) ;
#45325 = CARTESIAN_POINT ( 'NONE',  ( -4.458734124999999437, -47.64583333196775072, -2.574251347313719407 ) ) ;
#45326 = CARTESIAN_POINT ( 'NONE',  ( 5.000000000000000000, -68.37499999726881583, -6.123233995736766282E-16 ) ) ;
#45327 = CARTESIAN_POINT ( 'NONE',  ( -2.071067811865475061, -157.6875000000000000, -5.000000000000000888 ) ) ;
#45328 = CARTESIAN_POINT ( 'NONE',  ( -2.499999999999996447, -56.70833333060214443, 4.330127018922195425 ) ) ;
#45329 = CARTESIAN_POINT ( 'NONE',  ( -53.33387254593733928, -154.8125000000000000, 5.149110718188519620 ) ) ;
#45330 = CARTESIAN_POINT ( 'NONE',  ( 2.229367062499998831, -11.89583333196774007, -3.861377020970580887 ) ) ;
#45331 = CARTESIAN_POINT ( 'NONE',  ( -4.458734124999998549, -51.47916666530106511, 2.574251347313722516 ) ) ;
#45332 = CARTESIAN_POINT ( 'NONE',  ( 7.500000000000000000, 4.330127018922190096, -10.00000000000000000 ) ) ;
#45333 = CARTESIAN_POINT ( 'NONE',  ( -3.152801135295367096, -144.0625000013655779, -3.152801135295367541 ) ) ;
#45334 = CARTESIAN_POINT ( 'NONE',  ( 9.457646018065525792E-16, -96.31249999863439371, 5.148502694627439702 ) ) ;
#45335 = LINE ( 'NONE', #35367, #20432 ) ;
#45336 = VERTEX_POINT ( 'NONE', #47866 ) ;
#45337 = EDGE_CURVE ( 'NONE', #50505, #18747, #3825, .T. ) ;
#45338 = DIRECTION ( 'NONE',  ( -0.000000000000000000, 1.000000000000000000, -0.000000000000000000 ) ) ;
#45339 = CARTESIAN_POINT ( 'NONE',  ( 4.458734125000001214, 25.85416666803225638, 2.574251347313718519 ) ) ;
#45340 = CARTESIAN_POINT ( 'NONE',  ( -59.98410592259440222, -146.2500000027312126, -0.3983568153799752487 ) ) ;
#45341 =( BOUNDED_CURVE ( )  B_SPLINE_CURVE ( 2, ( #28985, #19341, #43465, #38338, #19022, #34131, #24810, #29293, #62794 ),
 .UNSPECIFIED., .F., .F. ) 
 B_SPLINE_CURVE_WITH_KNOTS ( ( 3, 2, 2, 2, 3 ),
 ( 0.2250000000000001998, 0.2291666666666668517, 0.2333333333333335313, 0.2375000000000001832, 0.2416666666666668628 ),
 .UNSPECIFIED. ) 
 CURVE ( )  GEOMETRIC_REPRESENTATION_ITEM ( )  RATIONAL_B_SPLINE_CURVE ( ( 0.9999999999999964473, 0.9238795325112902912, 1.000000000000000000, 0.9238795325112867385, 1.000000000000000000, 0.9238795325112867385, 1.000000000000000000, 0.9238795325112831858, 1.000000000000003553 ) ) 
 REPRESENTATION_ITEM ( '' )  );
#45342 = EDGE_CURVE ( 'NONE', #45000, #6575, #10094, .T. ) ;
#45343 = CARTESIAN_POINT ( 'NONE',  ( -5.000000000000000000, -62.00000000000000000, 0.000000000000000000 ) ) ;
#45344 = EDGE_LOOP ( 'NONE', ( #24519, #11197, #55560, #44692 ) ) ;
#45345 = CARTESIAN_POINT ( 'NONE',  ( -4.458734124999999437, -4.312499998634401699, 0.000000000000000000 ) ) ;
#45346 = ADVANCED_FACE ( 'NONE', ( #39794 ), #29826, .T. ) ;
#45347 = CARTESIAN_POINT ( 'NONE',  ( 5.000000000000000000, -50.29166666393548013, -2.886751345948130876 ) ) ;
#45348 = CARTESIAN_POINT ( 'NONE',  ( 4.458734124999998549, -16.97916666530107221, -2.574251347313721627 ) ) ;
#45349 = DIRECTION ( 'NONE',  ( 0.000000000000000000, 0.000000000000000000, 1.000000000000000000 ) ) ;
#45350 = CARTESIAN_POINT ( 'NONE',  ( -4.458734124999998549, -7.229166665301073103, 2.574251347313722516 ) ) ;
#45351 = CARTESIAN_POINT ( 'NONE',  ( 2.499999999999998668, 6.791666669397851130, -4.330127018922193649 ) ) ;
#45352 = CARTESIAN_POINT ( 'NONE',  ( -1.846868145590737420, -150.7500000013656347, 4.458734124999997661 ) ) ;
#45353 = CARTESIAN_POINT ( 'NONE',  ( -3.152548672688508926E-16, 17.18750000136559564, -5.148502694627439702 ) ) ;
#45354 = ORIENTED_EDGE ( 'NONE', *, *, #43803, .F. ) ;
#45355 = CARTESIAN_POINT ( 'NONE',  ( -5.000000000000000888, -148.4375000000000000, 2.071067811865474617 ) ) ;
#45356 = CARTESIAN_POINT ( 'NONE',  ( -5.000000000000000000, -13.08333333333333570, -2.886751345948128211 ) ) ;
#45357 = CARTESIAN_POINT ( 'NONE',  ( -2.229367062500000163, -20.47916666530107221, -3.861377020970580443 ) ) ;
#45358 = AXIS2_PLACEMENT_3D ( 'NONE', #42655, #3748, #48421 ) ;
#45359 = CARTESIAN_POINT ( 'NONE',  ( 7.500000000000000888, 1.489914625144004523, -0.1187923833806749097 ) ) ;
#45360 = CARTESIAN_POINT ( 'NONE',  ( -56.48576386720575471, -148.7500000013655779, -4.591703134518078322 ) ) ;
#45361 = CARTESIAN_POINT ( 'NONE',  ( -2.500000000000000444, -45.04166666393547303, -4.330127018922193649 ) ) ;
#45362 = CARTESIAN_POINT ( 'NONE',  ( -1.336351044127974539E-14, 21.37500000273118417, 5.000000000000000000 ) ) ;
#45363 = CARTESIAN_POINT ( 'NONE',  ( -4.458734124999999437, 13.68750000136559386, 0.000000000000000000 ) ) ;
#45364 = CARTESIAN_POINT ( 'NONE',  ( -5.000000000000000000, -8.958333330602144429, -2.886751345948128211 ) ) ;
#45365 = FACE_OUTER_BOUND ( 'NONE', #42664, .T. ) ;
#45366 = CARTESIAN_POINT ( 'NONE',  ( 9.457646018065525792E-16, 9.937500001365593860, 5.148502694627439702 ) ) ;
#45367 = CARTESIAN_POINT ( 'NONE',  ( -4.458734124999999437, -68.31249999863439371, 0.000000000000000000 ) ) ;
#45368 = ORIENTED_EDGE ( 'NONE', *, *, #61823, .T. ) ;
#45369 = CARTESIAN_POINT ( 'NONE',  ( 4.458734124999998549, -11.97916666530107044, -2.574251347313721627 ) ) ;
#45370 = CARTESIAN_POINT ( 'NONE',  ( 2.500000000000002220, 2.333333333333333037, 4.330127018922192761 ) ) ;
#45371 = CARTESIAN_POINT ( 'NONE',  ( 3.152801135295366208, -165.5625000013656063, 3.152801135295367985 ) ) ;
#45372 = CARTESIAN_POINT ( 'NONE',  ( -1.339745962155610925, -40.66965819600732601, 5.000000000000000000 ) ) ;
#45373 = CARTESIAN_POINT ( 'NONE',  ( -4.458734124999999437, -60.31249999863440081, 0.000000000000000000 ) ) ;
#45374 = CARTESIAN_POINT ( 'NONE',  ( 5.000000000000000000, -93.37499999726881583, -6.123233995736766282E-16 ) ) ;
#45375 = CARTESIAN_POINT ( 'NONE',  ( 4.458734125000000326, -35.89583333196773651, 2.574251347313718519 ) ) ;
#45376 = CARTESIAN_POINT ( 'NONE',  ( -1.339745962155613812, -42.08034179853029144, -5.000000000000000000 ) ) ;
#45377 = CYLINDRICAL_SURFACE ( 'NONE', #54261, 5.000000000000000000 ) ;
#45378 = CARTESIAN_POINT ( 'NONE',  ( 1.975475456537005874E-15, -107.6249999972687874, 5.000000000000000000 ) ) ;
#45379 = DIRECTION ( 'NONE',  ( 0.000000000000000000, 0.000000000000000000, 1.000000000000000000 ) ) ;
#45380 = CARTESIAN_POINT ( 'NONE',  ( -4.458734124999999437, -149.2500000013656063, -1.846868145590735644 ) ) ;
#45381 = CARTESIAN_POINT ( 'NONE',  ( -2.500000000000000444, -42.16666666666667140, -4.330127018922193649 ) ) ;
#45382 = CARTESIAN_POINT ( 'NONE',  ( -5.000000000000000000, -57.95833333060216574, -2.886751345948128211 ) ) ;
#45383 = ORIENTED_EDGE ( 'NONE', *, *, #24061, .F. ) ;
#45384 = CARTESIAN_POINT ( 'NONE',  ( 9.457646018065525792E-16, -106.0624999986343795, 5.148502694627439702 ) ) ;
#45385 = CARTESIAN_POINT ( 'NONE',  ( 2.229367062499998831, 0.1041666680322607397, -3.861377020970580887 ) ) ;
#45386 = CARTESIAN_POINT ( 'NONE',  ( -2.499999999999996447, -8.708333330602144429, 4.330127018922195425 ) ) ;
#45387 = CARTESIAN_POINT ( 'NONE',  ( -5.000000000000000000, -3.999999999999996447, 0.000000000000000000 ) ) ;
#45388 = CARTESIAN_POINT ( 'NONE',  ( -4.458734124999997661, -64.22916666530106511, 2.574251347313722516 ) ) ;
#45389 = EDGE_CURVE ( 'NONE', #7044, #61101, #7678, .T. ) ;
#45390 = CARTESIAN_POINT ( 'NONE',  ( -4.999999999999998224, -16.91666666666666430, 2.886751345948131764 ) ) ;
#45391 = CARTESIAN_POINT ( 'NONE',  ( 2.500000000000002220, -6.541666663935481019, 4.330127018922192761 ) ) ;
#45393 = ORIENTED_EDGE ( 'NONE', *, *, #53074, .T. ) ;
#45392 = CARTESIAN_POINT ( 'NONE',  ( 9.457646018065525792E-16, -36.06249999863441502, 5.148502694627439702 ) ) ;
#45394 = CARTESIAN_POINT ( 'NONE',  ( 1.339745962155612702, -33.29465819873851729, -5.000000000000000000 ) ) ;
#45395 = FACE_OUTER_BOUND ( 'NONE', #1529, .T. ) ;
#45397 = ORIENTED_EDGE ( 'NONE', *, *, #35407, .F. ) ;
#45396 = CARTESIAN_POINT ( 'NONE',  ( 9.457646018065525792E-16, 10.68750000136559386, 5.148502694627439702 ) ) ;
#45398 = CARTESIAN_POINT ( 'NONE',  ( 5.000000000000000000, -101.2916666639354730, -2.886751345948130876 ) ) ;
#45399 = CARTESIAN_POINT ( 'NONE',  ( -2.499999999999996447, -52.83333333333332860, 4.330127018922195425 ) ) ;
#45400 = CARTESIAN_POINT ( 'NONE',  ( -3.152548672688508926E-16, -32.81249999863440792, -5.148502694627439702 ) ) ;
#45401 = LINE ( 'NONE', #50224, #55342 ) ;
#45402 = CARTESIAN_POINT ( 'NONE',  ( -2.229367062500000163, -76.47916666530106511, -3.861377020970580443 ) ) ;
#45403 = CARTESIAN_POINT ( 'NONE',  ( -4.458734125000001214, -140.1250000013655779, 1.846868145590734089 ) ) ;
#45404 = CARTESIAN_POINT ( 'NONE',  ( 2.229367062499998831, -79.64583333196773651, -3.861377020970580887 ) ) ;
#45405 = CARTESIAN_POINT ( 'NONE',  ( -58.39396692619412477, -133.6875000013656063, 2.891590998281057701 ) ) ;
#45406 = CARTESIAN_POINT ( 'NONE',  ( -2.229367062500000163, -35.72916666530107221, -3.861377020970580443 ) ) ;
#45407 = ORIENTED_EDGE ( 'NONE', *, *, #25848, .F. ) ;
#45408 = CARTESIAN_POINT ( 'NONE',  ( -5.000000000000000000, 29.56250000136559208, 0.000000000000000000 ) ) ;
#45409 = ORIENTED_EDGE ( 'NONE', *, *, #34284, .T. ) ;
#45410 = CARTESIAN_POINT ( 'NONE',  ( 2.229367062500001939, -77.22916666530106511, 3.861377020970579999 ) ) ;
#45411 = CARTESIAN_POINT ( 'NONE',  ( -5.000000000000000000, 13.04166666939785379, -2.886751345948128211 ) ) ;
#45412 = EDGE_LOOP ( 'NONE', ( #1785, #33850, #40713 ) ) ;
#45413 = CARTESIAN_POINT ( 'NONE',  ( 5.000000000000000000, -16.41666666666667140, -2.886751345948130876 ) ) ;
#45414 =( REPRESENTATION_RELATIONSHIP ('NONE','NONE', #27855, #14320 ) REPRESENTATION_RELATIONSHIP_WITH_TRANSFORMATION ( #34639 )SHAPE_REPRESENTATION_RELATIONSHIP( ) );
#45415 = CARTESIAN_POINT ( 'NONE',  ( -5.000000000000000000, 7.916666666666665186, -2.886751345948128211 ) ) ;
#45416 = CARTESIAN_POINT ( 'NONE',  ( 4.458734124999999437, -64.06249999863440792, -5.460374474430324690E-16 ) ) ;
#45417 = CARTESIAN_POINT ( 'NONE',  ( 2.229367062500001939, -4.229166665301070438, 3.861377020970579999 ) ) ;
#45418 = EDGE_LOOP ( 'NONE', ( #33462, #18008, #15496, #32950 ) ) ;
#45419 =( BOUNDED_CURVE ( )  B_SPLINE_CURVE ( 2, ( #38583, #23500, #63056, #52768, #8697, #52462, #48557, #9320, #28309 ),
 .UNSPECIFIED., .F., .F. ) 
 B_SPLINE_CURVE_WITH_KNOTS ( ( 3, 2, 2, 2, 3 ),
 ( 0.05833333333333338283, 0.06250000000000005551, 0.06666666666666672125, 0.07083333333333338699, 0.07500000000000005274 ),
 .UNSPECIFIED. ) 
 CURVE ( )  GEOMETRIC_REPRESENTATION_ITEM ( )  RATIONAL_B_SPLINE_CURVE ( ( 0.9999999999999991118, 0.9238795325112876267, 1.000000000000000000, 0.9238795325112867385, 1.000000000000000000, 0.9238795325112867385, 1.000000000000000000, 0.9238795325112857393, 1.000000000000001110 ) ) 
 REPRESENTATION_ITEM ( '' )  );
#45420 = CARTESIAN_POINT ( 'NONE',  ( -2.499999999999996447, 5.291666669397853795, 4.330127018922195425 ) ) ;
#45421 = FACE_OUTER_BOUND ( 'NONE', #1995, .T. ) ;
#45422 = CARTESIAN_POINT ( 'NONE',  ( -2.229367062500000163, 5.520833334698927786, -3.861377020970580443 ) ) ;
#45423 = CARTESIAN_POINT ( 'NONE',  ( -59.44456063193725015, -139.5625000013656063, -0.3552334253322034230 ) ) ;
#45424 = DIRECTION ( 'NONE',  ( 0.000000000000000000, 0.000000000000000000, 1.000000000000000000 ) ) ;
#45425 = CARTESIAN_POINT ( 'NONE',  ( 4.458734124999997661, -161.5000000013656063, 1.846868145590737864 ) ) ;
#45426 = CARTESIAN_POINT ( 'NONE',  ( 1.975475456537005874E-15, -75.62499999726880162, 5.000000000000000000 ) ) ;
#45427 = VERTEX_POINT ( 'NONE', #49459 ) ;
#45428 = CARTESIAN_POINT ( 'NONE',  ( -2.229367062500000163, -81.47916666530106511, -3.861377020970580443 ) ) ;
#45429 = CARTESIAN_POINT ( 'NONE',  ( 5.000000000000000888, -164.0625000027312410, -2.071067811865475505 ) ) ;
#45430 = CARTESIAN_POINT ( 'NONE',  ( -4.458734124999998549, -3.229166665301069994, 2.574251347313722516 ) ) ;
#45431 = DIRECTION ( 'NONE',  ( -0.000000000000000000, 1.000000000000000000, -0.000000000000000000 ) ) ;
#45432 =( BOUNDED_CURVE ( )  B_SPLINE_CURVE ( 2, ( #26727, #32491, #27042, #12557, #1985, #46659, #2604, #22543, #13192 ),
 .UNSPECIFIED., .F., .F. ) 
 B_SPLINE_CURVE_WITH_KNOTS ( ( 3, 2, 2, 2, 3 ),
 ( 0.8062500000000000222, 0.8069444444444444642, 0.8083333333333333481, 0.8097222222222222321, 0.8104166666666666741 ),
 .UNSPECIFIED. ) 
 CURVE ( )  GEOMETRIC_REPRESENTATION_ITEM ( )  RATIONAL_B_SPLINE_CURVE ( ( 0.9330127018922194093, 0.9330127018922194093, 1.000000000000000000, 0.8660254037844387076, 1.000000000000000000, 0.8660254037844387076, 1.000000000000000000, 0.9330127018922194093, 0.9330127018922194093 ) ) 
 REPRESENTATION_ITEM ( '' )  );
#45433 = CARTESIAN_POINT ( 'NONE',  ( 1.975475456537005874E-15, 4.375000002731185056, 5.000000000000000000 ) ) ;
#45434 = CARTESIAN_POINT ( 'NONE',  ( -4.458734124999998549, -72.47916666530107932, 2.574251347313722516 ) ) ;
#45435 = CARTESIAN_POINT ( 'NONE',  ( -2.499999999999996447, -29.70833333060215153, 4.330127018922195425 ) ) ;
#45436 = CARTESIAN_POINT ( 'NONE',  ( 6.123233995736766282E-16, -170.0000000000000000, -5.000000000000000000 ) ) ;
#45437 = CARTESIAN_POINT ( 'NONE',  ( -1.339745962155613812, -41.20534180126147561, -5.000000000000000000 ) ) ;
#45438 = CARTESIAN_POINT ( 'NONE',  ( -1.339745962155618253, 23.20534180126147916, 4.999999999999996447 ) ) ;
#45439 = CARTESIAN_POINT ( 'NONE',  ( 4.458734125000000326, 28.10416666803225993, 2.574251347313718519 ) ) ;
#45440 = CARTESIAN_POINT ( 'NONE',  ( 4.458734125000001214, -52.89583333196772941, 2.574251347313718519 ) ) ;
#45441 = CARTESIAN_POINT ( 'NONE',  ( -3.152548672688508926E-16, -31.81249999863440436, -5.148502694627439702 ) ) ;
#45442 = CARTESIAN_POINT ( 'NONE',  ( -4.458734124999999437, 1.354166668032261933, -2.574251347313719407 ) ) ;
#45443 = LINE ( 'NONE', #35482, #38109 ) ;
#45444 = CARTESIAN_POINT ( 'NONE',  ( -5.000000000000000000, 20.91666666666666785, -2.886751345948128211 ) ) ;
#45445 = CARTESIAN_POINT ( 'NONE',  ( 3.535533905932736864, -144.2500000027311842, 3.535533905932738641 ) ) ;
#45446 = DIRECTION ( 'NONE',  ( -0.000000000000000000, 1.000000000000000000, -0.000000000000000000 ) ) ;
#45447 = CARTESIAN_POINT ( 'NONE',  ( 4.458734124999998549, -42.72916666530107221, -2.574251347313721627 ) ) ;
#45448 = CARTESIAN_POINT ( 'NONE',  ( 2.500000000000002220, -78.54166666393547303, 4.330127018922192761 ) ) ;
#45449 = CARTESIAN_POINT ( 'NONE',  ( -52.10840900171896806, -138.4375000013656063, 3.393966926194110556 ) ) ;
#45450 = CYLINDRICAL_SURFACE ( 'NONE', #51435, 5.000000000000000000 ) ;
#45451 = CARTESIAN_POINT ( 'NONE',  ( -58.24261429053147765, -155.0000000000000284, -3.805975901505573411 ) ) ;
#45452 = CARTESIAN_POINT ( 'NONE',  ( -4.458734124999997661, -79.47916666530106511, 2.574251347313722516 ) ) ;
#45453 = CARTESIAN_POINT ( 'NONE',  ( -1.846868145590737420, -162.0000000013656063, 4.458734124999997661 ) ) ;
#45454 = CARTESIAN_POINT ( 'NONE',  ( -2.499999999999996447, -32.83333333333332860, 4.330127018922195425 ) ) ;
#45455 = CARTESIAN_POINT ( 'NONE',  ( 5.000000000000000000, 7.500000000000000000, -6.123233995736766282E-16 ) ) ;
#45456 = CARTESIAN_POINT ( 'NONE',  ( -2.499999999999996447, -27.83333333333333570, 4.330127018922195425 ) ) ;
#45457 = CARTESIAN_POINT ( 'NONE',  ( 4.458734125000000326, -141.3750000013656063, -1.846868145590734978 ) ) ;
#45458 = ORIENTED_EDGE ( 'NONE', *, *, #61814, .T. ) ;
#45459 = CARTESIAN_POINT ( 'NONE',  ( 4.458734124999998549, 22.02083333469892779, -2.574251347313721627 ) ) ;
#45460 = ORIENTED_EDGE ( 'NONE', *, *, #24133, .T. ) ;
#45461 = CARTESIAN_POINT ( 'NONE',  ( -2.229367062500000163, -60.72916666530106511, -3.861377020970580443 ) ) ;
#45462 = CARTESIAN_POINT ( 'NONE',  ( 5.000000000000000000, 20.70833333606451632, -2.886751345948129988 ) ) ;
#45463 = CARTESIAN_POINT ( 'NONE',  ( -6.972266317189433020E-16, 2.750000000000000000, -5.000000000000000000 ) ) ;
#45464 = CARTESIAN_POINT ( 'NONE',  ( 5.000000000000000000, 13.49999999999999822, -6.123233995736766282E-16 ) ) ;
#45465 = CARTESIAN_POINT ( 'NONE',  ( 2.229367062499998831, -52.64583333196773651, -3.861377020970580887 ) ) ;
#45466 = CARTESIAN_POINT ( 'NONE',  ( 4.458734124999998549, -9.729166665301068662, -2.574251347313721627 ) ) ;
#45467 = DIRECTION ( 'NONE',  ( -0.000000000000000000, 1.000000000000000000, -0.000000000000000000 ) ) ;
#45468 = CARTESIAN_POINT ( 'NONE',  ( -2.499999999999996447, -109.8333333333333428, 4.330127018922195425 ) ) ;
#45469 = CARTESIAN_POINT ( 'NONE',  ( -4.999999999999998224, -63.91666666666666430, 2.886751345948131764 ) ) ;
#45470 = CARTESIAN_POINT ( 'NONE',  ( 5.000000000000000000, -11.29166666393547835, -2.886751345948130876 ) ) ;
#45471 = CARTESIAN_POINT ( 'NONE',  ( 1.060575238724906964E-15, -31.75000000000000000, 5.773502691896257311 ) ) ;
#45472 = DIRECTION ( 'NONE',  ( -0.000000000000000000, -0.000000000000000000, 1.000000000000000000 ) ) ;
#45474 = CARTESIAN_POINT ( 'NONE',  ( -4.458734124999998549, -13.47916666530107221, 2.574251347313722516 ) ) ;
#45473 = CARTESIAN_POINT ( 'NONE',  ( -6.972266317189433020E-16, -34.25000000000000000, -5.000000000000000000 ) ) ;
#45475 = CARTESIAN_POINT ( 'NONE',  ( -56.66612745406251861, -135.4375000027312126, -5.149110718188501856 ) ) ;
#45476 = CARTESIAN_POINT ( 'NONE',  ( -4.458734124999999437, -58.39583333196774362, -2.574251347313719407 ) ) ;
#45477 = CARTESIAN_POINT ( 'NONE',  ( -3.152801135295367985, -151.0625000013655779, 3.152801135295367096 ) ) ;
#45478 = CARTESIAN_POINT ( 'NONE',  ( -4.458734124999999437, -63.39583333196772941, -2.574251347313719407 ) ) ;
#45479 = CARTESIAN_POINT ( 'NONE',  ( 5.000000000000000000, -53.37499999726881583, -6.123233995736766282E-16 ) ) ;
#45480 = EDGE_LOOP ( 'NONE', ( #5522, #30506, #46055, #3895 ) ) ;
#45481 = CARTESIAN_POINT ( 'NONE',  ( -2.499999999999996447, 25.29166666939785202, 4.330127018922195425 ) ) ;
#45482 = CARTESIAN_POINT ( 'NONE',  ( -2.229367062499996610, -2.395833331967737845, 3.861377020970582219 ) ) ;
#45483 = ORIENTED_EDGE ( 'NONE', *, *, #59774, .F. ) ;
#45485 = CARTESIAN_POINT ( 'NONE',  ( 1.339745962155612702, -58.29465819873852439, -5.000000000000000000 ) ) ;
#45484 = CARTESIAN_POINT ( 'NONE',  ( -49.85088928181150436, -141.5625000000000568, -1.666127454062680480 ) ) ;
#45486 = CARTESIAN_POINT ( 'NONE',  ( -3.152801135295367096, -158.0625000013656063, -3.152801135295367541 ) ) ;
#45487 = ORIENTED_EDGE ( 'NONE', *, *, #47998, .F. ) ;
#45488 =( BOUNDED_CURVE ( )  B_SPLINE_CURVE ( 2, ( #55624, #1284, #60449, #6093, #11220, #16374, #51107, #60765, #30844 ),
 .UNSPECIFIED., .F., .F. ) 
 B_SPLINE_CURVE_WITH_KNOTS ( ( 3, 2, 2, 2, 3 ),
 ( 0.6604166666666666519, 0.6611111111111110938, 0.6624999999999999778, 0.6638888888888888618, 0.6645833333333333037 ),
 .UNSPECIFIED. ) 
 CURVE ( )  GEOMETRIC_REPRESENTATION_ITEM ( )  RATIONAL_B_SPLINE_CURVE ( ( 0.9330127018922194093, 0.9330127018922194093, 1.000000000000000000, 0.8660254037844387076, 1.000000000000000000, 0.8660254037844387076, 1.000000000000000000, 0.9330127018922194093, 0.9330127018922194093 ) ) 
 REPRESENTATION_ITEM ( '' )  );
#45489 = CARTESIAN_POINT ( 'NONE',  ( -5.000000000000000000, -7.958333330602144429, -2.886751345948128211 ) ) ;
#45490 = CARTESIAN_POINT ( 'NONE',  ( -56.66612745406270335, -131.3125000000000284, -5.149110718188516067 ) ) ;
#45491 = CARTESIAN_POINT ( 'NONE',  ( 0.000000000000000000, -120.0000000000000000, 5.000000000000000000 ) ) ;
#45492 = CARTESIAN_POINT ( 'NONE',  ( -4.458734124999999437, -46.64583333196774362, -2.574251347313719407 ) ) ;
#45493 = ORIENTED_EDGE ( 'NONE', *, *, #8402, .F. ) ;
#45494 = CARTESIAN_POINT ( 'NONE',  ( -9.184850993605147944E-16, -145.2500000000000284, 5.000000000000000000 ) ) ;
#45495 = CARTESIAN_POINT ( 'NONE',  ( 2.229367062500001939, 15.02083333469892779, 3.861377020970579999 ) ) ;
#45496 = CARTESIAN_POINT ( 'NONE',  ( -4.458734124999998549, 24.77083333469893134, 2.574251347313722516 ) ) ;
#45497 = CARTESIAN_POINT ( 'NONE',  ( -50.70258187064364108, -151.1250000013655779, 2.196230717870141014 ) ) ;
#45498 = CARTESIAN_POINT ( 'NONE',  ( 3.061616997868383141E-16, -165.7500000000000000, -5.000000000000000000 ) ) ;
#45499 = CARTESIAN_POINT ( 'NONE',  ( 7.499999999999999112, -1.443375672974070323, -7.063244554130001518 ) ) ;
#45500 = ORIENTED_EDGE ( 'NONE', *, *, #46782, .F. ) ;
#45501 = CARTESIAN_POINT ( 'NONE',  ( -3.152548672688508926E-16, -64.56249999863440792, -5.148502694627439702 ) ) ;
#45502 = CYLINDRICAL_SURFACE ( 'NONE', #42794, 5.000000000000000000 ) ;
#45503 = CARTESIAN_POINT ( 'NONE',  ( 4.458734124999999437, 11.18750000136559386, -5.460374474430324690E-16 ) ) ;
#45504 = CARTESIAN_POINT ( 'NONE',  ( -5.000000000000000000, 6.916666666666664298, -2.886751345948128211 ) ) ;
#45505 = CARTESIAN_POINT ( 'NONE',  ( -6.972266317189433020E-16, -99.24999999999998579, -5.000000000000000000 ) ) ;
#45506 = CARTESIAN_POINT ( 'NONE',  ( -3.152548672688508926E-16, -53.81249999863439371, -5.148502694627439702 ) ) ;
#45507 = CARTESIAN_POINT ( 'NONE',  ( -5.000000000000000000, -14.95833333060214265, -2.886751345948128211 ) ) ;
#45508 = CARTESIAN_POINT ( 'NONE',  ( -1.339745962155613812, -109.2053418012614543, -5.000000000000000000 ) ) ;
#45509 = CARTESIAN_POINT ( 'NONE',  ( 7.499999999999999112, -4.330127018922205195, -1.000000000000000888 ) ) ;
#45510 = CARTESIAN_POINT ( 'NONE',  ( -56.66612745406293783, -138.3125000000000000, -5.149110718188535607 ) ) ;
#45511 = CARTESIAN_POINT ( 'NONE',  ( -6.324555320336760822, 15.00000000000000000, 8.999999999999998224 ) ) ;
#45512 =( BOUNDED_CURVE ( )  B_SPLINE_CURVE ( 2, ( #56793, #12398, #32327, #32966, #22374, #12071, #23009, #32644, #2443 ),
 .UNSPECIFIED., .F., .F. ) 
 B_SPLINE_CURVE_WITH_KNOTS ( ( 3, 2, 2, 2, 3 ),
 ( 0.6583333333333329929, 0.6624999999999996447, 0.6666666666666662966, 0.6708333333333328374, 0.6749999999999996003 ),
 .UNSPECIFIED. ) 
 CURVE ( )  GEOMETRIC_REPRESENTATION_ITEM ( )  RATIONAL_B_SPLINE_CURVE ( ( 1.000000000000005995, 0.9238795325112806323, 1.000000000000000000, 0.9238795325112867385, 1.000000000000000000, 0.9238795325112867385, 1.000000000000000000, 0.9238795325112948431, 0.9999999999999918954 ) ) 
 REPRESENTATION_ITEM ( '' )  );
#45513 = CARTESIAN_POINT ( 'NONE',  ( -2.229367062500000163, -14.72916666530107221, -3.861377020970580443 ) ) ;
#45514 = ORIENTED_EDGE ( 'NONE', *, *, #62482, .T. ) ;
#45515 = CARTESIAN_POINT ( 'NONE',  ( -5.000000000000000000, -163.6250000027311842, -6.123233995736766282E-16 ) ) ;
#45516 = CARTESIAN_POINT ( 'NONE',  ( -3.152548672688508926E-16, -101.5624999986344221, -5.148502694627439702 ) ) ;
#45517 = CARTESIAN_POINT ( 'NONE',  ( 5.000000000000000000, -158.1875000027312126, 2.071067811865478614 ) ) ;
#45518 = VERTEX_POINT ( 'NONE', #15686 ) ;
#45519 = CARTESIAN_POINT ( 'NONE',  ( -2.229367062499996610, -102.3958333319677365, 3.861377020970582219 ) ) ;
#45520 = EDGE_CURVE ( 'NONE', #33038, #25022, #62453, .T. ) ;
#45521 = CARTESIAN_POINT ( 'NONE',  ( -2.229367062500000163, -25.47916666530106866, -3.861377020970580443 ) ) ;
#45522 = CARTESIAN_POINT ( 'NONE',  ( -3.535250795749689387E-16, -57.12499999726880873, -5.773502691896257311 ) ) ;
#45523 = CARTESIAN_POINT ( 'NONE',  ( -50.55543936806279248, -125.0625000013655921, 0.3552334253322060320 ) ) ;
#45524 = CARTESIAN_POINT ( 'NONE',  ( -50.70258187064364108, -141.1250000013656063, 2.196230717870141014 ) ) ;
#45525 = CARTESIAN_POINT ( 'NONE',  ( -4.458734124999997661, -22.22916666530107221, 2.574251347313722516 ) ) ;
#45526 = CARTESIAN_POINT ( 'NONE',  ( 4.458734124999999437, -65.06249999863440792, -5.460374474430324690E-16 ) ) ;
#45527 = CARTESIAN_POINT ( 'NONE',  ( 2.500000000000002220, 8.333333333333332149, 4.330127018922192761 ) ) ;
#45528 = CARTESIAN_POINT ( 'NONE',  ( -3.152548672688508926E-16, -17.56249999863440792, -5.148502694627439702 ) ) ;
#45529 = CARTESIAN_POINT ( 'NONE',  ( -1.339745962155610925, -79.66965819600731891, 5.000000000000000000 ) ) ;
#45530 = CARTESIAN_POINT ( 'NONE',  ( 5.000000000000000888, -150.9375000000000284, -2.071067811865475505 ) ) ;
#45531 = CARTESIAN_POINT ( 'NONE',  ( -2.499999999999996447, -8.833333333333332149, 4.330127018922195425 ) ) ;
#45532 = CARTESIAN_POINT ( 'NONE',  ( -4.458734124999999437, -152.9375000013655779, -5.460374474430324690E-16 ) ) ;
#45533 = ORIENTED_EDGE ( 'NONE', *, *, #32238, .F. ) ;
#45534 = CARTESIAN_POINT ( 'NONE',  ( -3.152548672688508926E-16, -45.81249999863440081, -5.148502694627439702 ) ) ;
#45535 = DIRECTION ( 'NONE',  ( 0.000000000000000000, 0.000000000000000000, 1.000000000000000000 ) ) ;
#45536 = CARTESIAN_POINT ( 'NONE',  ( -7.779103221381273414, 4.168986698926021361, -7.929128246061903695 ) ) ;
#45537 = CARTESIAN_POINT ( 'NONE',  ( 5.000000000000000000, 27.50000000000000000, -6.123233995736766282E-16 ) ) ;
#45538 = CARTESIAN_POINT ( 'NONE',  ( 9.457646018065525792E-16, 1.937500001365593416, 5.148502694627439702 ) ) ;
#45539 = ADVANCED_FACE ( 'NONE', ( #50424 ), #10852, .T. ) ;
#45540 = CARTESIAN_POINT ( 'NONE',  ( -1.339745962155610925, -73.66965819600733312, 5.000000000000000000 ) ) ;
#45541 = EDGE_CURVE ( 'NONE', #17564, #14134, #6676, .T. ) ;
#45542 = CARTESIAN_POINT ( 'NONE',  ( 2.500000000000002220, -11.54166666393547835, 4.330127018922192761 ) ) ;
#45543 = CARTESIAN_POINT ( 'NONE',  ( -5.000000000000000000, 26.00000000000000000, 0.000000000000000000 ) ) ;
#45544 = CARTESIAN_POINT ( 'NONE',  ( 2.229367062499998831, 15.10416666803225993, -3.861377020970580887 ) ) ;
#45545 = CARTESIAN_POINT ( 'NONE',  ( -2.500000000000000444, -78.16666666666665719, -4.330127018922193649 ) ) ;
#45546 = CARTESIAN_POINT ( 'NONE',  ( -4.999999999999999112, 10.20833333606451987, 2.886751345948131764 ) ) ;
#45547 = ORIENTED_EDGE ( 'NONE', *, *, #17654, .T. ) ;
#45548 = CARTESIAN_POINT ( 'NONE',  ( -2.500000000000000444, 7.833333333333334814, -4.330127018922193649 ) ) ;
#45549 = VERTEX_POINT ( 'NONE', #1868 ) ;
#45550 = CARTESIAN_POINT ( 'NONE',  ( -5.000000000000000000, -51.08333333333332860, -2.886751345948128211 ) ) ;
#45551 = CARTESIAN_POINT ( 'NONE',  ( -4.458734124999999437, -44.39583333196773651, -2.574251347313719407 ) ) ;
#45552 = CARTESIAN_POINT ( 'NONE',  ( -8.190561711645485556E-16, -164.9375000013655779, 4.458734124999999437 ) ) ;
#45553 = EDGE_CURVE ( 'NONE', #3800, #11847, #53409, .T. ) ;
#45554 = CARTESIAN_POINT ( 'NONE',  ( 5.000000000000000000, -39.37499999726880162, -6.123233995736766282E-16 ) ) ;
#45555 = ORIENTED_EDGE ( 'NONE', *, *, #23271, .T. ) ;
#45556 = CARTESIAN_POINT ( 'NONE',  ( -2.229367062500000163, -17.47916666530106866, -3.861377020970580443 ) ) ;
#45557 = VERTEX_POINT ( 'NONE', #15044 ) ;
#45558 = CARTESIAN_POINT ( 'NONE',  ( -2.500000000000000444, -86.16666666666667140, -4.330127018922193649 ) ) ;
#45559 = CARTESIAN_POINT ( 'NONE',  ( -2.500000000000000444, 0.9583333360645186483, -4.330127018922193649 ) ) ;
#45560 = CARTESIAN_POINT ( 'NONE',  ( -2.500000000000000444, -87.04166666393547303, -4.330127018922193649 ) ) ;
#45562 = ORIENTED_EDGE ( 'NONE', *, *, #46706, .F. ) ;
#45561 = CARTESIAN_POINT ( 'NONE',  ( -1.339745962155613812, -35.08034179853028434, -5.000000000000000000 ) ) ;
#45563 = CARTESIAN_POINT ( 'NONE',  ( -51.75738570946856498, -142.7500000000000284, 3.805975901505576964 ) ) ;
#45564 = CARTESIAN_POINT ( 'NONE',  ( -3.152548672688508926E-16, -34.81249999863440792, -5.148502694627439702 ) ) ;
#45565 = CARTESIAN_POINT ( 'NONE',  ( -6.972266317189433020E-16, -5.124999997268812280, -5.000000000000000000 ) ) ;
#45566 = ORIENTED_EDGE ( 'NONE', *, *, #22028, .F. ) ;
#45567 = APPLICATION_PROTOCOL_DEFINITION ( 'draft international standard', 'automotive_design', 1998, #12544 ) ;
#45568 = ADVANCED_FACE ( 'NONE', ( #10220 ), #54282, .F. ) ;
#45569 = CARTESIAN_POINT ( 'NONE',  ( -4.458734124999998549, -77.22916666530106511, 2.574251347313722516 ) ) ;
#45570 = CARTESIAN_POINT ( 'NONE',  ( 2.229367062500001939, -109.2291666653010651, 3.861377020970579999 ) ) ;
#45571 = CARTESIAN_POINT ( 'NONE',  ( 1.975475456537005874E-15, -38.62499999726880873, 5.000000000000000000 ) ) ;
#45572 = VERTEX_POINT ( 'NONE', #54926 ) ;
#45573 = CARTESIAN_POINT ( 'NONE',  ( -2.071067811865559882, -161.6874999999999716, -4.999999999999914735 ) ) ;
#45574 = CARTESIAN_POINT ( 'NONE',  ( -51.60603307380591787, -141.1875000013656063, -2.891590998281053704 ) ) ;
#45575 = CARTESIAN_POINT ( 'NONE',  ( 9.457646018065525792E-16, -81.31249999863440792, 5.148502694627439702 ) ) ;
#45576 = CARTESIAN_POINT ( 'NONE',  ( -57.46284108482265651, -135.0625000027312410, 4.819101127000239515 ) ) ;
#45577 = CARTESIAN_POINT ( 'NONE',  ( 4.458734124999998549, -42.72916666530107932, -2.574251347313721627 ) ) ;
#45578 = CARTESIAN_POINT ( 'NONE',  ( -1.846868145590734756, -140.3750000013656063, -4.458734124999999437 ) ) ;
#45579 = CARTESIAN_POINT ( 'NONE',  ( -4.999999999999998224, -57.91666666666665719, 2.886751345948131764 ) ) ;
#45580 = CARTESIAN_POINT ( 'NONE',  ( 4.458734125000000326, -49.89583333196772941, 2.574251347313718519 ) ) ;
#45581 = CARTESIAN_POINT ( 'NONE',  ( -4.458734124999997661, -43.22916666530106511, 2.574251347313722516 ) ) ;
#45582 = CARTESIAN_POINT ( 'NONE',  ( -4.458734124999999437, 27.60416666803226349, -2.574251347313719407 ) ) ;
#45583 = CARTESIAN_POINT ( 'NONE',  ( 4.458734124999999437, -17.81249999863440792, -5.460374474430324690E-16 ) ) ;
#45584 = CARTESIAN_POINT ( 'NONE',  ( 1.060575238724906964E-15, -99.75000000000001421, 5.773502691896257311 ) ) ;
#45585 = CARTESIAN_POINT ( 'NONE',  ( 3.152801135295367541, -140.5625000013655779, -3.152801135295367541 ) ) ;
#45586 = CARTESIAN_POINT ( 'NONE',  ( -3.152548672688508926E-16, -39.81249999863440081, -5.148502694627439702 ) ) ;
#45587 = CARTESIAN_POINT ( 'NONE',  ( -5.000000000000000000, 6.125000002731185056, 0.000000000000000000 ) ) ;
#45588 = CARTESIAN_POINT ( 'NONE',  ( -6.972266317189433020E-16, -7.124999997268814056, -5.000000000000000000 ) ) ;
#45589 = CARTESIAN_POINT ( 'NONE',  ( -51.60603307380591787, -128.9375000013656063, -2.891590998281053704 ) ) ;
#45590 = CARTESIAN_POINT ( 'NONE',  ( 4.458734125000001214, -73.14583333196773651, 2.574251347313718519 ) ) ;
#45591 = CARTESIAN_POINT ( 'NONE',  ( -60.14911071818854538, -142.1875000027312126, 1.666127454062681146 ) ) ;
#45592 = DIRECTION ( 'NONE',  ( -0.000000000000000000, 1.000000000000000000, -0.000000000000000000 ) ) ;
#45593 = CARTESIAN_POINT ( 'NONE',  ( -2.229367062500000163, -2.729166665301069550, -3.861377020970580443 ) ) ;
#45594 = ORIENTED_EDGE ( 'NONE', *, *, #49892, .F. ) ;
#45595 = CARTESIAN_POINT ( 'NONE',  ( -1.336351044127974539E-14, 24.37500000273118417, 5.000000000000000000 ) ) ;
#45596 = CARTESIAN_POINT ( 'NONE',  ( 2.500000000000002220, 23.45833333606451632, 4.330127018922192761 ) ) ;
#45598 = CARTESIAN_POINT ( 'NONE',  ( -4.458734124999999437, -35.39583333196773651, -2.574251347313719407 ) ) ;
#45597 = CARTESIAN_POINT ( 'NONE',  ( 2.229367062500001939, -85.97916666530107932, 3.861377020970579999 ) ) ;
#45599 = CARTESIAN_POINT ( 'NONE',  ( -2.500000000000000444, -5.166666666666666963, -4.330127018922193649 ) ) ;
#45600 = CARTESIAN_POINT ( 'NONE',  ( -4.458734124999998549, -82.47916666530106511, 2.574251347313722516 ) ) ;
#45601 = EDGE_CURVE ( 'NONE', #1992, #25522, #9334, .T. ) ;
#45602 = CARTESIAN_POINT ( 'NONE',  ( -4.458734124999999437, 15.35416666803225993, -2.574251347313719407 ) ) ;
#45603 = CARTESIAN_POINT ( 'NONE',  ( 0.000000000000000000, -170.0000000000000000, 0.000000000000000000 ) ) ;
#45604 = AXIS2_PLACEMENT_3D ( 'NONE', #58779, #904, #40109 ) ;
#45605 = CARTESIAN_POINT ( 'NONE',  ( -50.70258187064364108, -136.1250000013656063, 2.196230717870141014 ) ) ;
#45606 = EDGE_CURVE ( 'NONE', #48949, #33686, #11802, .T. ) ;
#45607 = EDGE_CURVE ( 'NONE', #47078, #63425, #31417, .T. ) ;
#45608 = CARTESIAN_POINT ( 'NONE',  ( -2.229367062499996610, -10.14583333196773829, 3.861377020970582219 ) ) ;
#45609 = CARTESIAN_POINT ( 'NONE',  ( -4.458734124999999437, 24.35416666803225993, -2.574251347313719407 ) ) ;
#45610 = CARTESIAN_POINT ( 'NONE',  ( -4.458734124999999437, -47.64583333196775072, -2.574251347313719407 ) ) ;
#45611 = FACE_OUTER_BOUND ( 'NONE', #56573, .T. ) ;
#45612 = CARTESIAN_POINT ( 'NONE',  ( -2.229367062499996610, -86.14583333196773651, 3.861377020970582219 ) ) ;
#45613 = CARTESIAN_POINT ( 'NONE',  ( 2.229367062500001939, -1.979166665301068662, 3.861377020970579999 ) ) ;
#45614 = DIRECTION ( 'NONE',  ( 0.000000000000000000, 0.000000000000000000, 1.000000000000000000 ) ) ;
#45615 = ORIENTED_EDGE ( 'NONE', *, *, #3249, .F. ) ;
#45616 = CARTESIAN_POINT ( 'NONE',  ( -3.152548672688508926E-16, -28.81249999863440792, -5.148502694627439702 ) ) ;
#45617 = CARTESIAN_POINT ( 'NONE',  ( -59.29741812935640155, -133.8750000013656063, -2.196230717870135685 ) ) ;
#45618 = CARTESIAN_POINT ( 'NONE',  ( 4.458734125000001214, -76.89583333196775072, 2.574251347313718519 ) ) ;
#45619 = CARTESIAN_POINT ( 'NONE',  ( 2.499999999999998668, -108.2083333306021444, -4.330127018922193649 ) ) ;
#45620 =( BOUNDED_CURVE ( )  B_SPLINE_CURVE ( 2, ( #11391, #16545, #11076, #44847, #49993, #810, #31011, #5946, #20417 ),
 .UNSPECIFIED., .F., .F. ) 
 B_SPLINE_CURVE_WITH_KNOTS ( ( 3, 2, 2, 2, 3 ),
 ( 0.1017857142857142849, 0.1023809523809523780, 0.1035714285714285782, 0.1047619047619047644, 0.1053571428571428575 ),
 .UNSPECIFIED. ) 
 CURVE ( )  GEOMETRIC_REPRESENTATION_ITEM ( )  RATIONAL_B_SPLINE_CURVE ( ( 0.9330127018922194093, 0.9330127018922194093, 1.000000000000000000, 0.8660254037844387076, 1.000000000000000000, 0.8660254037844387076, 1.000000000000000000, 0.9330127018922194093, 0.9330127018922194093 ) ) 
 REPRESENTATION_ITEM ( '' )  );
#45621 = CARTESIAN_POINT ( 'NONE',  ( -4.458734124999999437, 22.60416666803225993, -2.574251347313719407 ) ) ;
#45622 = CARTESIAN_POINT ( 'NONE',  ( -5.000000000000000000, -57.87499999726880873, 0.000000000000000000 ) ) ;
#45623 = EDGE_CURVE ( 'NONE', #51351, #2611, #2787, .T. ) ;
#45624 = CARTESIAN_POINT ( 'NONE',  ( 2.499999999999998668, -66.33333333333332860, -4.330127018922193649 ) ) ;
#45625 = CARTESIAN_POINT ( 'NONE',  ( 9.457646018065525792E-16, -78.31249999863440792, 5.148502694627439702 ) ) ;
#45626 = CARTESIAN_POINT ( 'NONE',  ( 5.000000000000000000, -59.50000000000000000, -6.123233995736766282E-16 ) ) ;
#45627 = CARTESIAN_POINT ( 'NONE',  ( 2.500000000000002220, -90.54166666393547303, 4.330127018922192761 ) ) ;
#45628 = CARTESIAN_POINT ( 'NONE',  ( -3.535250795749689387E-16, 22.87500000273118772, -5.773502691896257311 ) ) ;
#45629 = VERTEX_POINT ( 'NONE', #26609 ) ;
#45630 = CARTESIAN_POINT ( 'NONE',  ( -4.999999999999998224, -56.91666666666667140, 2.886751345948131764 ) ) ;
#45631 = FACE_OUTER_BOUND ( 'NONE', #40415, .T. ) ;
#45633 = CARTESIAN_POINT ( 'NONE',  ( 5.000000000000000000, -23.41666666666667140, -2.886751345948129988 ) ) ;
#45632 = DIRECTION ( 'NONE',  ( 0.000000000000000000, 0.000000000000000000, 1.000000000000000000 ) ) ;
#45634 = CARTESIAN_POINT ( 'NONE',  ( 9.457646018065525792E-16, -26.06249999863440792, 5.148502694627439702 ) ) ;
#45635 = CARTESIAN_POINT ( 'NONE',  ( -2.229367062499996610, -86.14583333196773651, 3.861377020970582219 ) ) ;
#45636 = CARTESIAN_POINT ( 'NONE',  ( 1.060575238724906964E-15, -23.62499999726881228, 5.773502691896257311 ) ) ;
#45638 = ORIENTED_EDGE ( 'NONE', *, *, #55043, .F. ) ;
#45637 = CARTESIAN_POINT ( 'NONE',  ( 2.229367062500001939, -52.97916666530107221, 3.861377020970579999 ) ) ;
#45639 = LINE ( 'NONE', #41117, #42791 ) ;
#45640 = CARTESIAN_POINT ( 'NONE',  ( 1.339745962155612702, -74.16965819600731891, -5.000000000000000000 ) ) ;
#45642 = VERTEX_POINT ( 'NONE', #56526 ) ;
#45641 = CARTESIAN_POINT ( 'NONE',  ( -4.458734124999999437, -4.562499998634401699, 0.000000000000000000 ) ) ;
#45643 = CARTESIAN_POINT ( 'NONE',  ( 5.000000000000000000, -69.49999999999998579, -6.123233995736766282E-16 ) ) ;
#45644 = CARTESIAN_POINT ( 'NONE',  ( 3.152801135295366208, -152.8125000013656063, 3.152801135295367985 ) ) ;
#45645 = CARTESIAN_POINT ( 'NONE',  ( -2.229367062499996610, -44.39583333196774362, 3.861377020970582219 ) ) ;
#45646 = CARTESIAN_POINT ( 'NONE',  ( 2.500000000000002220, -68.54166666393547303, 4.330127018922192761 ) ) ;
#45647 = CARTESIAN_POINT ( 'NONE',  ( 5.000000000000000000, -158.0625000000000284, 2.071067811865478614 ) ) ;
#45648 = CARTESIAN_POINT ( 'NONE',  ( -1.127183054612291972E-14, 22.37500000273118417, 4.999999999999999112 ) ) ;
#45649 = CARTESIAN_POINT ( 'NONE',  ( -50.18089887299979068, -154.6875000000000568, 2.462841084822635640 ) ) ;
#45650 = CARTESIAN_POINT ( 'NONE',  ( 4.458734125000001214, -19.14583333196774007, 2.574251347313718519 ) ) ;
#45651 = CARTESIAN_POINT ( 'NONE',  ( 9.457646018065525792E-16, -53.31249999863441502, 5.148502694627439702 ) ) ;
#45652 = AXIS2_PLACEMENT_3D ( 'NONE', #8688, #28301, #3871 ) ;
#45653 = CARTESIAN_POINT ( 'NONE',  ( -2.499999999999996447, 1.166666666666666519, 4.330127018922195425 ) ) ;
#45654 = CARTESIAN_POINT ( 'NONE',  ( 4.458734124999999437, -145.5000000013655779, 1.846868145590737864 ) ) ;
#45655 = CARTESIAN_POINT ( 'NONE',  ( 4.458734124999999437, -95.06249999863440792, -5.460374474430324690E-16 ) ) ;
#45656 = CARTESIAN_POINT ( 'NONE',  ( -2.452879891156814818, -7.244083172395189507, -0.1007566405101857632 ) ) ;
#45657 = ORIENTED_EDGE ( 'NONE', *, *, #18963, .F. ) ;
#45658 = CARTESIAN_POINT ( 'NONE',  ( 3.061616997868383141E-16, -155.7500000000000000, -5.000000000000000000 ) ) ;
#45659 = CARTESIAN_POINT ( 'NONE',  ( -4.458734124999999437, 25.43750000136559208, 0.000000000000000000 ) ) ;
#45660 = CARTESIAN_POINT ( 'NONE',  ( -51.75738570946856498, -146.8750000027312126, 3.805975901505576964 ) ) ;
#45661 = CARTESIAN_POINT ( 'NONE',  ( 1.975475456537005874E-15, -50.75000000000000000, 5.000000000000000000 ) ) ;
#45662 = VERTEX_POINT ( 'NONE', #51694 ) ;
#45663 = CARTESIAN_POINT ( 'NONE',  ( 9.457646018065525792E-16, -4.062499998634408804, 5.148502694627439702 ) ) ;
#45664 = CARTESIAN_POINT ( 'NONE',  ( 2.229367062499998831, -22.89583333196773651, -3.861377020970580887 ) ) ;
#45665 =( BOUNDED_CURVE ( )  B_SPLINE_CURVE ( 2, ( #8773, #9084, #58296, #19677, #9703, #28694, #48313, #34457, #29001 ),
 .UNSPECIFIED., .F., .F. ) 
 B_SPLINE_CURVE_WITH_KNOTS ( ( 3, 2, 2, 2, 3 ),
 ( 0.7854166666666666519, 0.7861111111111110938, 0.7874999999999999778, 0.7888888888888888618, 0.7895833333333333037 ),
 .UNSPECIFIED. ) 
 CURVE ( )  GEOMETRIC_REPRESENTATION_ITEM ( )  RATIONAL_B_SPLINE_CURVE ( ( 0.9330127018922194093, 0.9330127018922194093, 1.000000000000000000, 0.8660254037844387076, 1.000000000000000000, 0.8660254037844387076, 1.000000000000000000, 0.9330127018922194093, 0.9330127018922194093 ) ) 
 REPRESENTATION_ITEM ( '' )  );
#45666 = CARTESIAN_POINT ( 'NONE',  ( 5.000000000000000000, 11.62500000273118594, -6.123233995736766282E-16 ) ) ;
#45667 = CARTESIAN_POINT ( 'NONE',  ( -2.229367062499996610, -7.145833331967735624, 3.861377020970582219 ) ) ;
#45668 = CARTESIAN_POINT ( 'NONE',  ( 7.298354728637812983, -4.926141412639873707, -7.913704048099693189 ) ) ;
#45669 = CARTESIAN_POINT ( 'NONE',  ( 3.152801135295366208, -148.5625000013655779, 3.152801135295367985 ) ) ;
#45670 =( BOUNDED_CURVE ( )  B_SPLINE_CURVE ( 2, ( #35175, #59292, #1095, #49953, #59623, #35490, #14898, #60266, #16184 ),
 .UNSPECIFIED., .F., .F. ) 
 B_SPLINE_CURVE_WITH_KNOTS ( ( 3, 2, 2, 2, 3 ),
 ( 0.9249999999999998224, 0.9291666666666664742, 0.9333333333333331261, 0.9374999999999998890, 0.9416666666666665408 ),
 .UNSPECIFIED. ) 
 CURVE ( )  GEOMETRIC_REPRESENTATION_ITEM ( )  RATIONAL_B_SPLINE_CURVE ( ( 1.000000000000003997, 0.9238795325112826307, 1.000000000000000000, 0.9238795325112867385, 1.000000000000000000, 0.9238795325112867385, 1.000000000000000000, 0.9238795325112887369, 0.9999999999999980016 ) ) 
 REPRESENTATION_ITEM ( '' )  );
#45671 = CARTESIAN_POINT ( 'NONE',  ( 4.458734124999999437, 17.93750000136559208, -5.460374474430324690E-16 ) ) ;
#45672 = EDGE_LOOP ( 'NONE', ( #44429, #23516, #32734, #31934 ) ) ;
#45673 = CARTESIAN_POINT ( 'NONE',  ( -6.972266317189433020E-16, -37.25000000000000000, -5.000000000000000000 ) ) ;
#45674 = CARTESIAN_POINT ( 'NONE',  ( 1.339745962155612702, -71.16965819600731891, -5.000000000000000000 ) ) ;
#45675 = CARTESIAN_POINT ( 'NONE',  ( 4.458734124999998549, -20.72916666530106866, -2.574251347313721627 ) ) ;
#45676 = CARTESIAN_POINT ( 'NONE',  ( 1.975475456537005874E-15, -25.62499999726881228, 5.000000000000000000 ) ) ;
#45677 = CARTESIAN_POINT ( 'NONE',  ( -6.972266317189433020E-16, -37.12499999726880873, -5.000000000000000000 ) ) ;
#45678 = CARTESIAN_POINT ( 'NONE',  ( -57.19623071787017210, -150.3750000013656063, 4.297418129356382899 ) ) ;
#45679 = ADVANCED_FACE ( 'NONE', ( #46863 ), #52007, .T. ) ;
#45680 = EDGE_CURVE ( 'NONE', #32980, #62343, #7947, .T. ) ;
#45681 = CARTESIAN_POINT ( 'NONE',  ( -3.535250795749689387E-16, -47.12499999726880873, -5.773502691896257311 ) ) ;
#45682 = CARTESIAN_POINT ( 'NONE',  ( -52.53715891517739323, -148.4375000000000000, -4.819101127000233298 ) ) ;
#45683 = CARTESIAN_POINT ( 'NONE',  ( 2.229367062500001939, 8.020833334698926009, 3.861377020970579999 ) ) ;
#45684 = CARTESIAN_POINT ( 'NONE',  ( 0.000000000000000000, -170.0000000000000000, 0.000000000000000000 ) ) ;
#45686 = EDGE_CURVE ( 'NONE', #39380, #36403, #44269, .T. ) ;
#45685 = CYLINDRICAL_SURFACE ( 'NONE', #41781, 5.000000000000000000 ) ;
#45687 = CARTESIAN_POINT ( 'NONE',  ( 2.229367062499998831, 12.35416666803226171, -3.861377020970580887 ) ) ;
#45688 = CARTESIAN_POINT ( 'NONE',  ( -4.458734124999999437, -66.31249999863440792, 0.000000000000000000 ) ) ;
#45689 = CARTESIAN_POINT ( 'NONE',  ( -2.229367062500000163, -16.72916666530107577, -3.861377020970580443 ) ) ;
#45690 = CARTESIAN_POINT ( 'NONE',  ( 5.000000000000000000, -0.5000000000000004441, -6.123233995736766282E-16 ) ) ;
#45691 = CARTESIAN_POINT ( 'NONE',  ( 4.458734124999999437, -163.4375000013655779, 0.000000000000000000 ) ) ;
#45692 = CARTESIAN_POINT ( 'NONE',  ( -1.339745962155613812, 21.79465819873852084, -5.000000000000000000 ) ) ;
#45693 = CARTESIAN_POINT ( 'NONE',  ( -4.458734124999998549, -61.22916666530106511, 2.574251347313722516 ) ) ;
#45694 = CARTESIAN_POINT ( 'NONE',  ( 5.000000000000000888, -96.45833333060213022, 2.886751345948126879 ) ) ;
#45695 = ADVANCED_FACE ( 'NONE', ( #22429 ), #22107, .F. ) ;
#45696 = ADVANCED_FACE ( 'NONE', ( #61349 ), #13078, .T. ) ;
#45697 = CARTESIAN_POINT ( 'NONE',  ( -1.339745962155610925, -27.79465819873851729, 5.000000000000000000 ) ) ;
#45698 = CARTESIAN_POINT ( 'NONE',  ( -2.499999999999996447, -35.83333333333332860, 4.330127018922195425 ) ) ;
#45699 = CARTESIAN_POINT ( 'NONE',  ( -4.458734124999997661, -37.22916666530107221, 2.574251347313722516 ) ) ;
#45700 = CARTESIAN_POINT ( 'NONE',  ( -4.330127018922101279, 45.00000000000000000, 7.500000000000002665 ) ) ;
#45701 =( BOUNDED_SURFACE ( )  B_SPLINE_SURFACE ( 3, 2, ( 
 ( #55449, #56407, #21983 ),
 ( #21673, #41263, #12332 ),
 ( #26804, #60911, #41577 ),
 ( #25851, #11364, #40325 ),
 ( #16833, #61230, #56080 ),
 ( #50614, #5923, #12000 ),
 ( #25531, #30675, #51264 ),
 ( #59963, #1747, #15886 ) ),
 .UNSPECIFIED., .F., .F., .F. ) 
 B_SPLINE_SURFACE_WITH_KNOTS ( ( 4, 2, 2, 4 ),
 ( 3, 3 ),
 ( 0.03850042371095789562, 0.04313406099830585649, 0.04545087964197984387, 0.04776769828565382431 ),
 ( 0.000000000000000000, 1.000000000000000000 ),
 .UNSPECIFIED. ) 
 GEOMETRIC_REPRESENTATION_ITEM ( )  RATIONAL_B_SPLINE_SURFACE ( (
 ( 1.000000000000000000, 0.8047781847388135734, 1.000000000000000000),
 ( 1.000000000000000000, 0.8123760230793541925, 1.000000000000000000),
 ( 1.000000000000000000, 0.8190653851695529619, 1.000000000000000000),
 ( 1.000000000000000000, 0.8191940386278896424, 1.000000000000000000),
 ( 1.000000000000000000, 0.8176096570055705337, 1.000000000000000000),
 ( 1.000000000000000000, 0.8122964723277524834, 1.000000000000000000),
 ( 1.000000000000000000, 0.8086312464132844324, 1.000000000000000000),
 ( 1.000000000000000000, 0.8047712192439641088, 1.000000000000000000) ) ) 
 REPRESENTATION_ITEM ( '' )  SURFACE ( )  );
#45702 = CARTESIAN_POINT ( 'NONE',  ( 5.000000000000000000, -45.41666666666666430, -2.886751345948129988 ) ) ;
#45703 = CARTESIAN_POINT ( 'NONE',  ( 5.000000000000000888, -13.58333333333333570, 2.886751345948126879 ) ) ;
#45704 = EDGE_CURVE ( 'NONE', #38280, #42565, #42706, .T. ) ;
#45705 = CARTESIAN_POINT ( 'NONE',  ( 1.975475456537005874E-15, -86.62499999726880162, 5.000000000000000000 ) ) ;
#45706 = ORIENTED_EDGE ( 'NONE', *, *, #39080, .F. ) ;
#45707 = CARTESIAN_POINT ( 'NONE',  ( 4.458734124999998549, -107.7291666653010509, -2.574251347313721627 ) ) ;
#45708 = CARTESIAN_POINT ( 'NONE',  ( 2.229367062500001939, -2.229166665301068662, 3.861377020970579999 ) ) ;
#45709 = CARTESIAN_POINT ( 'NONE',  ( 3.044556291839386294E-14, 17.87500000273118417, -5.000000000000000000 ) ) ;
#45710 = ADVANCED_FACE ( 'NONE', ( #18538 ), #29418, .T. ) ;
#45711 = CARTESIAN_POINT ( 'NONE',  ( -5.000000000000000000, -5.999999999999998224, 0.000000000000000000 ) ) ;
#45712 = CARTESIAN_POINT ( 'NONE',  ( 9.457646018065525792E-16, -73.06249999863439371, 5.148502694627439702 ) ) ;
#45713 = DIRECTION ( 'NONE',  ( -0.000000000000000000, 1.000000000000000000, -0.000000000000000000 ) ) ;
#45714 = EDGE_CURVE ( 'NONE', #23096, #44027, #4674, .T. ) ;
#45715 = CARTESIAN_POINT ( 'NONE',  ( -5.000000000000000000, -5.958333330602148870, -2.886751345948128211 ) ) ;
#45717 = ORIENTED_EDGE ( 'NONE', *, *, #30216, .F. ) ;
#45716 = CARTESIAN_POINT ( 'NONE',  ( 4.458734124999998549, -37.72916666530107221, -2.574251347313721627 ) ) ;
#45718 = CARTESIAN_POINT ( 'NONE',  ( -5.000000000000000000, -16.87499999726881583, 0.000000000000000000 ) ) ;
#45720 = EDGE_LOOP ( 'NONE', ( #48811, #55071, #42953, #20331 ) ) ;
#45719 = CARTESIAN_POINT ( 'NONE',  ( 4.458734125000001214, 10.85416666803225993, 2.574251347313718519 ) ) ;
#45721 = CARTESIAN_POINT ( 'NONE',  ( 0.000000000000000000, -120.0000000000000000, 5.000000000000000000 ) ) ;
#45722 = CARTESIAN_POINT ( 'NONE',  ( 5.000000000000000000, -49.50000000000000000, -6.123233995736766282E-16 ) ) ;
#45723 = CARTESIAN_POINT ( 'NONE',  ( 2.229367062499998831, -28.89583333196774007, -3.861377020970580887 ) ) ;
#45724 = CARTESIAN_POINT ( 'NONE',  ( -5.000000000000000000, 14.04166666939785202, -2.886751345948128211 ) ) ;
#45725 = CARTESIAN_POINT ( 'NONE',  ( 2.229367062500001939, -72.97916666530107932, 3.861377020970579999 ) ) ;
#45726 =( BOUNDED_CURVE ( )  B_SPLINE_CURVE ( 2, ( #10643, #45063, #1029, #46339, #31858, #32488, #42448, #62090, #61464 ),
 .UNSPECIFIED., .F., .F. ) 
 B_SPLINE_CURVE_WITH_KNOTS ( ( 3, 2, 2, 2, 3 ),
 ( 0.8104166666666666741, 0.8111111111111111160, 0.8125000000000000000, 0.8138888888888888840, 0.8145833333333333259 ),
 .UNSPECIFIED. ) 
 CURVE ( )  GEOMETRIC_REPRESENTATION_ITEM ( )  RATIONAL_B_SPLINE_CURVE ( ( 0.9330127018922194093, 0.9330127018922194093, 1.000000000000000000, 0.8660254037844387076, 1.000000000000000000, 0.8660254037844387076, 1.000000000000000000, 0.9330127018922194093, 0.9330127018922194093 ) ) 
 REPRESENTATION_ITEM ( '' )  );
#45727 = CARTESIAN_POINT ( 'NONE',  ( -9.184850993605147944E-16, -169.2500000000000000, 5.000000000000000000 ) ) ;
#45728 = CARTESIAN_POINT ( 'NONE',  ( -4.458734124999999437, -85.39583333196773651, -2.574251347313719407 ) ) ;
#45729 = CARTESIAN_POINT ( 'NONE',  ( -50.55543936806279248, -135.3125000013656063, 0.3552334253322060320 ) ) ;
#45730 = CARTESIAN_POINT ( 'NONE',  ( -4.458734124999999437, -35.64583333196772941, -2.574251347313719407 ) ) ;
#45731 = VERTEX_POINT ( 'NONE', #63232 ) ;
#45732 = CARTESIAN_POINT ( 'NONE',  ( -2.499999999999996447, -93.70833333060214443, 4.330127018922195425 ) ) ;
#45733 = ORIENTED_EDGE ( 'NONE', *, *, #38126, .F. ) ;
#45734 = CARTESIAN_POINT ( 'NONE',  ( -4.458734124999998549, -80.47916666530106511, 2.574251347313722516 ) ) ;
#45735 = CARTESIAN_POINT ( 'NONE',  ( 5.000000000000000000, -21.41666666666666430, -2.886751345948130876 ) ) ;
#45736 = ORIENTED_EDGE ( 'NONE', *, *, #31180, .F. ) ;
#45737 = CARTESIAN_POINT ( 'NONE',  ( 1.062108568985190270E-13, -12.25000000000000000, -4.999999999999999112 ) ) ;
#45738 = CARTESIAN_POINT ( 'NONE',  ( -6.972266317189433020E-16, -1.124999997268814278, -5.000000000000000000 ) ) ;
#45739 = CARTESIAN_POINT ( 'NONE',  ( -4.458734124999999437, -64.64583333196772230, -2.574251347313719407 ) ) ;
#45740 = CARTESIAN_POINT ( 'NONE',  ( -3.152548672688508926E-16, -3.812499998634408360, -5.148502694627439702 ) ) ;
#45741 = VERTEX_POINT ( 'NONE', #38158 ) ;
#45742 = AXIS2_PLACEMENT_3D ( 'NONE', #9961, #15753, #1307 ) ;
#45743 = CARTESIAN_POINT ( 'NONE',  ( -1.339745962155640457, 3.330341803992664218, 4.999999999999984901 ) ) ;
#45744 = VERTEX_POINT ( 'NONE', #58082 ) ;
#45745 = CARTESIAN_POINT ( 'NONE',  ( -6.972266317189433020E-16, -53.12499999726880162, -5.000000000000000000 ) ) ;
#45746 = CARTESIAN_POINT ( 'NONE',  ( -4.458734124999999437, 6.687500001365593860, 0.000000000000000000 ) ) ;
#45747 = CARTESIAN_POINT ( 'NONE',  ( 1.975475456537005874E-15, -11.62499999726881406, 5.000000000000000000 ) ) ;
#45748 = CARTESIAN_POINT ( 'NONE',  ( -1.846868145590734756, -161.1250000013656063, -4.458734124999999437 ) ) ;
#45749 = CARTESIAN_POINT ( 'NONE',  ( -4.999999999999998224, 19.20833333606451632, 2.886751345948131764 ) ) ;
#45750 = ORIENTED_EDGE ( 'NONE', *, *, #47442, .T. ) ;
#45751 = CARTESIAN_POINT ( 'NONE',  ( 9.457646018065525792E-16, -89.06249999863439371, 5.148502694627439702 ) ) ;
#45752 = DIRECTION ( 'NONE',  ( -0.000000000000000000, 1.000000000000000000, -0.000000000000000000 ) ) ;
#45753 = CARTESIAN_POINT ( 'NONE',  ( 9.457646018065525792E-16, -2.062499998634407028, 5.148502694627439702 ) ) ;
#45754 = CARTESIAN_POINT ( 'NONE',  ( 1.339745962155612702, -71.16965819600731891, -5.000000000000000000 ) ) ;
#45755 = FACE_OUTER_BOUND ( 'NONE', #35517, .T. ) ;
#45756 = CARTESIAN_POINT ( 'NONE',  ( 5.000000000000000000, -30.29166666393548013, -2.886751345948129988 ) ) ;
#45757 = CARTESIAN_POINT ( 'NONE',  ( 1.339745962155612702, 12.83034180399266511, -5.000000000000000000 ) ) ;
#45758 = CARTESIAN_POINT ( 'NONE',  ( 4.458734124999998549, 22.27083333469892779, -2.574251347313721627 ) ) ;
#45759 = CARTESIAN_POINT ( 'NONE',  ( -5.000000000000000000, -37.95833333060213022, -2.886751345948128211 ) ) ;
#45760 = CARTESIAN_POINT ( 'NONE',  ( 2.229367062500001939, -48.97916666530107221, 3.861377020970579999 ) ) ;
#45761 = CARTESIAN_POINT ( 'NONE',  ( -2.229367062500000163, -36.72916666530107221, -3.861377020970580443 ) ) ;
#45762 = CARTESIAN_POINT ( 'NONE',  ( 2.229367062499998831, 2.104166668032262599, -3.861377020970580887 ) ) ;
#45763 = CARTESIAN_POINT ( 'NONE',  ( -1.339745962155610925, 9.330341803992663330, 5.000000000000000000 ) ) ;
#45764 = CARTESIAN_POINT ( 'NONE',  ( -3.535250795749689387E-16, 20.74999999999999645, -5.773502691896257311 ) ) ;
#45765 = CARTESIAN_POINT ( 'NONE',  ( 5.000000000000000000, -146.1250000027312126, 0.000000000000000000 ) ) ;
#45766 = CARTESIAN_POINT ( 'NONE',  ( -9.184850993605147944E-16, -159.2500000000000000, 5.000000000000000000 ) ) ;
#45767 = CARTESIAN_POINT ( 'NONE',  ( -4.458734124999999437, -42.39583333196773651, -2.574251347313719407 ) ) ;
#45768 = CARTESIAN_POINT ( 'NONE',  ( -5.000000000000000000, -79.95833333060213022, -2.886751345948128211 ) ) ;
#45769 = CARTESIAN_POINT ( 'NONE',  ( -57.89159099828107458, -141.9375000013656063, -3.393966926194107447 ) ) ;
#45770 = CARTESIAN_POINT ( 'NONE',  ( 3.535533905932736864, -140.1250000000000000, 3.535533905932738641 ) ) ;
#45771 = CARTESIAN_POINT ( 'NONE',  ( 1.975475456537005874E-15, -31.75000000000000000, 5.000000000000000000 ) ) ;
#45772 = CARTESIAN_POINT ( 'NONE',  ( 4.458734124999998549, -81.97916666530106511, -2.574251347313721627 ) ) ;
#45773 = CARTESIAN_POINT ( 'NONE',  ( 4.458734124999997661, -160.7500000013655779, 1.846868145590737864 ) ) ;
#45774 = CARTESIAN_POINT ( 'NONE',  ( -5.174575781537456010, -5.672711317431625488, -7.030005583190790830 ) ) ;
#45775 = CARTESIAN_POINT ( 'NONE',  ( 5.000000000000000000, -28.49999999999999645, -6.123233995736766282E-16 ) ) ;
#45776 = CARTESIAN_POINT ( 'NONE',  ( 1.846868145590736310, -139.6250000013656347, 4.458734124999999437 ) ) ;
#45777 = VERTEX_POINT ( 'NONE', #48731 ) ;
#45778 = CARTESIAN_POINT ( 'NONE',  ( 4.458734125000001214, 24.85416666803225993, 2.574251347313718519 ) ) ;
#45779 = ORIENTED_EDGE ( 'NONE', *, *, #16203, .T. ) ;
#45780 = CARTESIAN_POINT ( 'NONE',  ( 4.458734125000001214, -88.89583333196773651, 2.574251347313718519 ) ) ;
#45781 = CARTESIAN_POINT ( 'NONE',  ( 2.229367062500001939, 12.77083333469892779, 3.861377020970579999 ) ) ;
#45782 = CARTESIAN_POINT ( 'NONE',  ( -2.499999999999996447, 16.29166666939785202, 4.330127018922195425 ) ) ;
#45783 = DIRECTION ( 'NONE',  ( -0.000000000000000000, 1.000000000000000000, -0.000000000000000000 ) ) ;
#45784 = CARTESIAN_POINT ( 'NONE',  ( -5.000000000000000000, 15.00000000000000000, 0.000000000000000000 ) ) ;
#45785 = CARTESIAN_POINT ( 'NONE',  ( -2.229367062499996610, -57.14583333196773651, 3.861377020970582219 ) ) ;
#45786 = AXIS2_PLACEMENT_3D ( 'NONE', #51456, #22822, #7074 ) ;
#45787 = CARTESIAN_POINT ( 'NONE',  ( -4.458734124999998549, -10.22916666530106866, 2.574251347313722516 ) ) ;
#45788 = ADVANCED_FACE ( 'NONE', ( #49049 ), #24296, .T. ) ;
#45789 = CARTESIAN_POINT ( 'NONE',  ( -55.35523342533222291, -135.5625000013656063, 4.444560631937231499 ) ) ;
#45790 = CARTESIAN_POINT ( 'NONE',  ( 2.500000000000002220, -99.54166666393545881, 4.330127018922192761 ) ) ;
#45791 = CARTESIAN_POINT ( 'NONE',  ( -5.000000000000000000, 0.04166666939785235169, -2.886751345948128211 ) ) ;
#45792 = CARTESIAN_POINT ( 'NONE',  ( -2.499999999999996447, -36.83333333333332860, 4.330127018922195425 ) ) ;
#45793 = CARTESIAN_POINT ( 'NONE',  ( -1.339745962155564296, -10.20534180126148271, -5.000000000000028422 ) ) ;
#45795 = CARTESIAN_POINT ( 'NONE',  ( 4.458734125000001214, -16.14583333196773651, 2.574251347313718519 ) ) ;
#45794 = DIRECTION ( 'NONE',  ( -0.000000000000000000, 1.000000000000000000, -0.000000000000000000 ) ) ;
#45796 = CARTESIAN_POINT ( 'NONE',  ( -50.01589407740564042, -135.7500000027312126, 0.3983568153799778022 ) ) ;
#45797 = CARTESIAN_POINT ( 'NONE',  ( -3.152548672688508926E-16, -60.56249999863440792, -5.148502694627439702 ) ) ;
#45798 = CARTESIAN_POINT ( 'NONE',  ( 4.458734125000000326, -151.6250000013656063, -1.846868145590734978 ) ) ;
#45799 = CARTESIAN_POINT ( 'NONE',  ( 4.458734124999999437, -65.81249999863440792, -5.460374474430324690E-16 ) ) ;
#45800 = CARTESIAN_POINT ( 'NONE',  ( -50.55543936806279248, -147.3125000013656063, 0.3552334253322060320 ) ) ;
#45801 =( BOUNDED_CURVE ( )  B_SPLINE_CURVE ( 2, ( #51810, #17715, #46667, #36702, #52759, #56961, #2612, #32499, #22230 ),
 .UNSPECIFIED., .F., .F. ) 
 B_SPLINE_CURVE_WITH_KNOTS ( ( 3, 2, 2, 2, 3 ),
 ( 0.9232142857142857650, 0.9238095238095238582, 0.9250000000000000444, 0.9261904761904762307, 0.9267857142857143238 ),
 .UNSPECIFIED. ) 
 CURVE ( )  GEOMETRIC_REPRESENTATION_ITEM ( )  RATIONAL_B_SPLINE_CURVE ( ( 0.9330127018922194093, 0.9330127018922194093, 1.000000000000000000, 0.8660254037844387076, 1.000000000000000000, 0.8660254037844387076, 1.000000000000000000, 0.9330127018922194093, 0.9330127018922194093 ) ) 
 REPRESENTATION_ITEM ( '' )  );
#45802 = CARTESIAN_POINT ( 'NONE',  ( -5.000000000000000000, -58.87499999726880873, 0.000000000000000000 ) ) ;
#45803 = ORIENTED_EDGE ( 'NONE', *, *, #50325, .F. ) ;
#45804 = CARTESIAN_POINT ( 'NONE',  ( 0.000000000000000000, -170.0000000000000000, 5.000000000000000000 ) ) ;
#45805 = ORIENTED_EDGE ( 'NONE', *, *, #112, .T. ) ;
#45807 = CARTESIAN_POINT ( 'NONE',  ( -1.339745962155610925, -85.79465819873851729, 5.000000000000000000 ) ) ;
#45806 = CARTESIAN_POINT ( 'NONE',  ( -3.535533905932738641, -157.5000000027312126, 3.535533905932737309 ) ) ;
#45808 = CARTESIAN_POINT ( 'NONE',  ( 1.846868145590735200, -151.2500000013656063, -4.458734125000000326 ) ) ;
#45809 = ORIENTED_EDGE ( 'NONE', *, *, #8391, .F. ) ;
#45810 = CARTESIAN_POINT ( 'NONE',  ( -2.499999999999996447, -9.833333333333332149, 4.330127018922195425 ) ) ;
#45811 = CARTESIAN_POINT ( 'NONE',  ( -57.46284108482265651, -127.9375000000000568, 4.819101127000239515 ) ) ;
#45812 = FACE_OUTER_BOUND ( 'NONE', #23451, .T. ) ;
#45813 = CARTESIAN_POINT ( 'NONE',  ( 4.458734124999998549, -49.97916666530106511, -2.574251347313721627 ) ) ;
#45814 = ORIENTED_EDGE ( 'NONE', *, *, #18833, .T. ) ;
#45815 =( BOUNDED_CURVE ( )  B_SPLINE_CURVE ( 2, ( #34311, #27915, #3487, #29795, #30767, #35275, #45559, #39452, #49428 ),
 .UNSPECIFIED., .F., .F. ) 
 B_SPLINE_CURVE_WITH_KNOTS ( ( 3, 2, 2, 2, 3 ),
 ( 0.2312500000000000111, 0.2319444444444444531, 0.2333333333333333370, 0.2347222222222222210, 0.2354166666666666630 ),
 .UNSPECIFIED. ) 
 CURVE ( )  GEOMETRIC_REPRESENTATION_ITEM ( )  RATIONAL_B_SPLINE_CURVE ( ( 0.9330127018922194093, 0.9330127018922194093, 1.000000000000000000, 0.8660254037844387076, 1.000000000000000000, 0.8660254037844387076, 1.000000000000000000, 0.9330127018922194093, 0.9330127018922194093 ) ) 
 REPRESENTATION_ITEM ( '' )  );
#45816 = CARTESIAN_POINT ( 'NONE',  ( 1.975475456537005874E-15, -25.62499999726881228, 5.000000000000000000 ) ) ;
#45817 = CARTESIAN_POINT ( 'NONE',  ( -2.229367062500000163, 11.52083333469892601, -3.861377020970580443 ) ) ;
#45818 = CARTESIAN_POINT ( 'NONE',  ( -4.458734124999999437, 25.68750000136559208, 0.000000000000000000 ) ) ;
#45819 = CARTESIAN_POINT ( 'NONE',  ( -58.39396692619412477, -152.4375000013656063, 2.891590998281057701 ) ) ;
#45820 = LINE ( 'NONE', #11084, #37751 ) ;
#45821 = EDGE_LOOP ( 'NONE', ( #56461, #38591, #34614, #44211 ) ) ;
#45822 = CARTESIAN_POINT ( 'NONE',  ( 9.457646018065525792E-16, -67.06249999863440792, 5.148502694627439702 ) ) ;
#45823 = LINE ( 'NONE', #26527, #17135 ) ;
#45824 = CARTESIAN_POINT ( 'NONE',  ( -4.458734124999998549, 13.77083333469892779, 2.574251347313722516 ) ) ;
#45825 = VECTOR ( 'NONE', #22840, 1000.000000000000000 ) ;
#45826 = VECTOR ( 'NONE', #62770, 1000.000000000000000 ) ;
#45827 = CARTESIAN_POINT ( 'NONE',  ( 1.339745962155641346, 7.830341803992665994, -4.999999999999983125 ) ) ;
#45828 = CARTESIAN_POINT ( 'NONE',  ( -50.01589407740564042, -152.7500000027312410, 0.3983568153799778022 ) ) ;
#45829 = CARTESIAN_POINT ( 'NONE',  ( 4.458734124999999437, -55.06249999863440081, -5.460374474430324690E-16 ) ) ;
#45830 = CARTESIAN_POINT ( 'NONE',  ( -3.535250795749689387E-16, -13.12499999726881050, -5.773502691896257311 ) ) ;
#45831 = CARTESIAN_POINT ( 'NONE',  ( 0.000000000000000000, -120.0000000000000000, 5.000000000000000000 ) ) ;
#45832 = CARTESIAN_POINT ( 'NONE',  ( 0.000000000000000000, -170.0000000000000000, 0.000000000000000000 ) ) ;
#45833 = CARTESIAN_POINT ( 'NONE',  ( 2.500000000000002220, -64.54166666393547303, 4.330127018922192761 ) ) ;
#45834 = CARTESIAN_POINT ( 'NONE',  ( 4.458734124999999437, -17.06249999863440792, -5.460374474430324690E-16 ) ) ;
#45835 = ORIENTED_EDGE ( 'NONE', *, *, #5364, .F. ) ;
#45836 = CARTESIAN_POINT ( 'NONE',  ( -48.00000000000002132, -135.0000000000000284, 4.041451884327384114 ) ) ;
#45837 = CARTESIAN_POINT ( 'NONE',  ( 2.229367062500001939, -105.9791666653010651, 3.861377020970579999 ) ) ;
#45838 = CARTESIAN_POINT ( 'NONE',  ( -3.535533905932738641, -155.5000000027312126, 3.535533905932737309 ) ) ;
#45839 = ORIENTED_EDGE ( 'NONE', *, *, #24466, .F. ) ;
#45840 = CARTESIAN_POINT ( 'NONE',  ( -2.229367062499996610, -104.3958333319677365, 3.861377020970582219 ) ) ;
#45841 = CARTESIAN_POINT ( 'NONE',  ( 9.457646018065525792E-16, -29.06249999863440081, 5.148502694627439702 ) ) ;
#45842 = CARTESIAN_POINT ( 'NONE',  ( -4.999999999999999112, -63.79166666393547303, 2.886751345948131764 ) ) ;
#45843 = CARTESIAN_POINT ( 'NONE',  ( -52.80376928212989185, -153.1250000013656063, -4.297418129356379346 ) ) ;
#45844 = CARTESIAN_POINT ( 'NONE',  ( -57.89159099828107458, -144.6875000013656063, -3.393966926194107447 ) ) ;
#45845 = CARTESIAN_POINT ( 'NONE',  ( 2.229367062499998831, -24.64583333196773651, -3.861377020970580887 ) ) ;
#45846 = CARTESIAN_POINT ( 'NONE',  ( -4.458734124999999437, -65.56249999863440792, 0.000000000000000000 ) ) ;
#45847 = CARTESIAN_POINT ( 'NONE',  ( -59.98410592259440222, -137.1250000000000284, -0.3983568153799752487 ) ) ;
#45848 = CARTESIAN_POINT ( 'NONE',  ( -4.458734124999999437, -17.39583333196773651, -2.574251347313719407 ) ) ;
#45849 = DIRECTION ( 'NONE',  ( 0.000000000000000000, 0.000000000000000000, 1.000000000000000000 ) ) ;
#45850 = CARTESIAN_POINT ( 'NONE',  ( -9.184850993605147944E-16, -149.2500000000000284, 5.000000000000000000 ) ) ;
#45851 = CARTESIAN_POINT ( 'NONE',  ( -3.535250795749689387E-16, -9.250000000000001776, -5.773502691896257311 ) ) ;
#45852 = CARTESIAN_POINT ( 'NONE',  ( 4.458734124999999437, -150.5000000013656347, 1.846868145590737864 ) ) ;
#45853 = VERTEX_POINT ( 'NONE', #19146 ) ;
#45854 = CARTESIAN_POINT ( 'NONE',  ( 2.229367062500001939, -54.22916666530107221, 3.861377020970579999 ) ) ;
#45855 = CARTESIAN_POINT ( 'NONE',  ( -4.764381983412779477E-15, 26.25000000000000000, 5.000000000000000000 ) ) ;
#45856 = CARTESIAN_POINT ( 'NONE',  ( -4.458734124999998549, -88.22916666530107932, 2.574251347313722516 ) ) ;
#45857 = CARTESIAN_POINT ( 'NONE',  ( -4.458734124999999437, 3.687500001365594748, 0.000000000000000000 ) ) ;
#45858 = DIRECTION ( 'NONE',  ( -0.000000000000000000, 1.000000000000000000, -0.000000000000000000 ) ) ;
#45859 = CARTESIAN_POINT ( 'NONE',  ( -6.972266317189433020E-16, 6.750000000000000000, -5.000000000000000000 ) ) ;
#45860 = CARTESIAN_POINT ( 'NONE',  ( 2.500000000000002220, 20.45833333606451987, 4.330127018922192761 ) ) ;
#45861 = CARTESIAN_POINT ( 'NONE',  ( 2.229367062499998831, 13.10416666803226171, -3.861377020970580887 ) ) ;
#45862 = CARTESIAN_POINT ( 'NONE',  ( -2.500000000000000444, 3.958333336064518093, -4.330127018922193649 ) ) ;
#45863 = ORIENTED_EDGE ( 'NONE', *, *, #24032, .F. ) ;
#45864 = LINE ( 'NONE', #55213, #9950 ) ;
#45865 = EDGE_LOOP ( 'NONE', ( #5376, #34425, #47707, #1273 ) ) ;
#45866 =( BOUNDED_CURVE ( )  B_SPLINE_CURVE ( 2, ( #18762, #58015, #33567, #38692, #43516, #19072, #14255, #33878, #9427 ),
 .UNSPECIFIED., .F., .F. ) 
 B_SPLINE_CURVE_WITH_KNOTS ( ( 3, 2, 2, 2, 3 ),
 ( 0.6339285714285713969, 0.6345238095238094900, 0.6357142857142856762, 0.6369047619047618625, 0.6374999999999999556 ),
 .UNSPECIFIED. ) 
 CURVE ( )  GEOMETRIC_REPRESENTATION_ITEM ( )  RATIONAL_B_SPLINE_CURVE ( ( 0.9330127018922194093, 0.9330127018922194093, 1.000000000000000000, 0.8660254037844387076, 1.000000000000000000, 0.8660254037844387076, 1.000000000000000000, 0.9330127018922194093, 0.9330127018922194093 ) ) 
 REPRESENTATION_ITEM ( '' )  );
#45867 = AXIS2_PLACEMENT_3D ( 'NONE', #13970, #53217, #9149 ) ;
#45868 = CARTESIAN_POINT ( 'NONE',  ( 0.000000000000000000, -170.0000000000000000, 0.000000000000000000 ) ) ;
#45869 = CARTESIAN_POINT ( 'NONE',  ( 2.229367062500001939, -43.97916666530106511, 3.861377020970579999 ) ) ;
#45870 = CARTESIAN_POINT ( 'NONE',  ( -3.152801135295367985, -163.0625000013656063, 3.152801135295367096 ) ) ;
#45871 = VECTOR ( 'NONE', #56446, 1000.000000000000000 ) ;
#45872 = CARTESIAN_POINT ( 'NONE',  ( -5.000000000000000000, -37.95833333060214443, -2.886751345948128211 ) ) ;
#45873 = ORIENTED_EDGE ( 'NONE', *, *, #50629, .F. ) ;
#45874 = CARTESIAN_POINT ( 'NONE',  ( -3.152548672688508926E-16, -17.56249999863440792, -5.148502694627439702 ) ) ;
#45875 = EDGE_LOOP ( 'NONE', ( #4679, #4125, #253, #38637 ) ) ;
#45876 = CARTESIAN_POINT ( 'NONE',  ( -2.499999999999996447, -89.83333333333332860, 4.330127018922195425 ) ) ;
#45877 = CARTESIAN_POINT ( 'NONE',  ( -3.152801135295367985, -164.8125000013656063, 3.152801135295367096 ) ) ;
#45878 = CARTESIAN_POINT ( 'NONE',  ( 5.000000000000000000, -88.29166666393547303, -2.886751345948129988 ) ) ;
#45880 = ORIENTED_EDGE ( 'NONE', *, *, #15336, .F. ) ;
#45879 = CARTESIAN_POINT ( 'NONE',  ( 1.975475456537005874E-15, -34.62499999726880873, 5.000000000000000000 ) ) ;
#45881 = CARTESIAN_POINT ( 'NONE',  ( -60.14911071818854538, -142.0625000000000000, 1.666127454062681368 ) ) ;
#45882 = ADVANCED_FACE ( 'NONE', ( #38453 ), #23053, .T. ) ;
#45883 = CARTESIAN_POINT ( 'NONE',  ( 2.229367062500001939, -31.22916666530107221, 3.861377020970579999 ) ) ;
#45884 = CYLINDRICAL_SURFACE ( 'NONE', #52884, 5.000000000000000000 ) ;
#45885 = ORIENTED_EDGE ( 'NONE', *, *, #29867, .F. ) ;
#45886 = CARTESIAN_POINT ( 'NONE',  ( 4.458734124999998549, -79.72916666530107932, -2.574251347313721627 ) ) ;
#45887 = CARTESIAN_POINT ( 'NONE',  ( -4.458734124999999437, 28.68750000136559208, 0.000000000000000000 ) ) ;
#45888 = CARTESIAN_POINT ( 'NONE',  ( -6.972266317189433020E-16, -29.12499999726880873, -5.000000000000000000 ) ) ;
#45889 = VERTEX_POINT ( 'NONE', #57783 ) ;
#45890 = CARTESIAN_POINT ( 'NONE',  ( 0.000000000000000000, 15.00000000000000000, 0.000000000000000000 ) ) ;
#45891 = CARTESIAN_POINT ( 'NONE',  ( -59.59170313451810586, -141.7500000013656063, 1.485763867205729394 ) ) ;
#45892 = CARTESIAN_POINT ( 'NONE',  ( -2.229367062500000163, -80.72916666530106511, -3.861377020970580443 ) ) ;
#45893 = CARTESIAN_POINT ( 'NONE',  ( -58.80597590150559739, -136.1250000027312410, 3.242614290531460330 ) ) ;
#45894 = CARTESIAN_POINT ( 'NONE',  ( 4.458734124999999437, -45.81249999863440081, -5.460374474430324690E-16 ) ) ;
#45895 = CARTESIAN_POINT ( 'NONE',  ( 4.458734124999999437, -141.6250000013656347, -1.846868145590734978 ) ) ;
#45896 =( BOUNDED_CURVE ( )  B_SPLINE_CURVE ( 2, ( #37750, #3975, #23595, #51914, #3663, #38066, #43192, #8482, #18749 ),
 .UNSPECIFIED., .F., .F. ) 
 B_SPLINE_CURVE_WITH_KNOTS ( ( 3, 2, 2, 2, 3 ),
 ( 0.6053571428571428159, 0.6059523809523809090, 0.6071428571428570953, 0.6083333333333332815, 0.6089285714285714857 ),
 .UNSPECIFIED. ) 
 CURVE ( )  GEOMETRIC_REPRESENTATION_ITEM ( )  RATIONAL_B_SPLINE_CURVE ( ( 0.9330127018922194093, 0.9330127018922194093, 1.000000000000000000, 0.8660254037844387076, 1.000000000000000000, 0.8660254037844387076, 1.000000000000000000, 0.9330127018922130810, 0.9330127018922194093 ) ) 
 REPRESENTATION_ITEM ( '' )  );
#45897 = LINE ( 'NONE', #50723, #30202 ) ;
#45898 = CARTESIAN_POINT ( 'NONE',  ( 4.458734124999999437, -47.81249999863440792, -5.460374474430324690E-16 ) ) ;
#45899 = CARTESIAN_POINT ( 'NONE',  ( 9.457646018065525792E-16, -46.06249999863440081, 5.148502694627439702 ) ) ;
#45900 = CARTESIAN_POINT ( 'NONE',  ( 2.229367062500001939, 28.02083333469892779, 3.861377020970579999 ) ) ;
#45901 = CARTESIAN_POINT ( 'NONE',  ( -4.999999999999999112, -98.91666666666665719, 2.886751345948131764 ) ) ;
#45902 = EDGE_CURVE ( 'NONE', #1132, #1992, #9498, .T. ) ;
#45903 = DIRECTION ( 'NONE',  ( -0.000000000000000000, 1.000000000000000000, -0.000000000000000000 ) ) ;
#45904 = CARTESIAN_POINT ( 'NONE',  ( 4.458734125000001214, -41.14583333196774362, 2.574251347313718519 ) ) ;
#45905 = CARTESIAN_POINT ( 'NONE',  ( 5.000000000000000888, -0.4583333306021480369, 2.886751345948126879 ) ) ;
#45906 = CARTESIAN_POINT ( 'NONE',  ( -2.500000000000000444, -40.04166666393548013, -4.330127018922193649 ) ) ;
#45907 = CARTESIAN_POINT ( 'NONE',  ( -54.64476657466781973, -129.8125000013656063, -4.444560631937228834 ) ) ;
#45908 = CARTESIAN_POINT ( 'NONE',  ( -2.229367062500000163, -80.72916666530106511, -3.861377020970580443 ) ) ;
#45909 = CARTESIAN_POINT ( 'NONE',  ( -3.152548672688508926E-16, -98.56249999863439371, -5.148502694627439702 ) ) ;
#45910 = CYLINDRICAL_SURFACE ( 'NONE', #32606, 5.000000000000000000 ) ;
#45911 = CARTESIAN_POINT ( 'NONE',  ( -4.458734124999999437, -0.5624999986344053626, 0.000000000000000000 ) ) ;
#45912 = VERTEX_POINT ( 'NONE', #53259 ) ;
#45913 = VECTOR ( 'NONE', #8363, 1000.000000000000000 ) ;
#45914 = FACE_OUTER_BOUND ( 'NONE', #25614, .T. ) ;
#45915 = CARTESIAN_POINT ( 'NONE',  ( -2.499999999999996447, -75.83333333333334281, 4.330127018922195425 ) ) ;
#45916 = CARTESIAN_POINT ( 'NONE',  ( -4.458734124999999437, -87.39583333196773651, -2.574251347313719407 ) ) ;
#45917 = CARTESIAN_POINT ( 'NONE',  ( 5.000000000000000000, -168.1250000027312126, 0.000000000000000000 ) ) ;
#45918 = CARTESIAN_POINT ( 'NONE',  ( -4.458734124999999437, -85.64583333196773651, -2.574251347313719407 ) ) ;
#45919 = CARTESIAN_POINT ( 'NONE',  ( 9.457646018065525792E-16, 10.68750000136559386, 5.148502694627439702 ) ) ;
#45920 = CARTESIAN_POINT ( 'NONE',  ( 0.000000000000000000, -170.0000000000000000, 0.000000000000000000 ) ) ;
#45921 = CARTESIAN_POINT ( 'NONE',  ( -59.44456063193725015, -135.5625000013656063, -0.3552334253322034230 ) ) ;
#45922 = VECTOR ( 'NONE', #36353, 1000.000000000000000 ) ;
#45923 = CARTESIAN_POINT ( 'NONE',  ( -4.458734124999999437, -7.395833331967734736, -2.574251347313719407 ) ) ;
#45924 = CARTESIAN_POINT ( 'NONE',  ( 2.229367062499998831, 17.10416666803225993, -3.861377020970580887 ) ) ;
#45925 = CARTESIAN_POINT ( 'NONE',  ( 4.458734124999999437, -47.06249999863440792, -5.460374474430324690E-16 ) ) ;
#45926 = CARTESIAN_POINT ( 'NONE',  ( -2.500000000000000444, -14.04166666393548013, -4.330127018922193649 ) ) ;
#45927 = CARTESIAN_POINT ( 'NONE',  ( 4.458734125000001214, -87.89583333196773651, 2.574251347313718519 ) ) ;
#45928 = CARTESIAN_POINT ( 'NONE',  ( -4.458734124999999437, -5.312499998634402587, 0.000000000000000000 ) ) ;
#45929 = ORIENTED_EDGE ( 'NONE', *, *, #60583, .F. ) ;
#45930 = CARTESIAN_POINT ( 'NONE',  ( 2.229367062500001939, -30.22916666530107221, 3.861377020970579999 ) ) ;
#45931 = CARTESIAN_POINT ( 'NONE',  ( -59.59170313451811296, -130.7500000013656063, 1.485763867205729394 ) ) ;
#45932 = CARTESIAN_POINT ( 'NONE',  ( 4.458734124999999437, -73.81249999863440792, -5.460374474430324690E-16 ) ) ;
#45933 = CARTESIAN_POINT ( 'NONE',  ( 1.060575238724906964E-15, -108.6249999972688016, 5.773502691896257311 ) ) ;
#45934 = CARTESIAN_POINT ( 'NONE',  ( -4.458734124999999437, 18.60416666803225993, -2.574251347313719407 ) ) ;
#45935 = CARTESIAN_POINT ( 'NONE',  ( -5.000000000000000000, -43.87499999726880873, 0.000000000000000000 ) ) ;
#45936 = DIRECTION ( 'NONE',  ( 0.000000000000000000, 0.000000000000000000, 1.000000000000000000 ) ) ;
#45937 = CARTESIAN_POINT ( 'NONE',  ( 4.458734124999999437, -76.06249999863440792, -5.460374474430324690E-16 ) ) ;
#45938 = CARTESIAN_POINT ( 'NONE',  ( 5.000000000000000000, -62.41666666666666430, -2.886751345948129988 ) ) ;
#45939 = CARTESIAN_POINT ( 'NONE',  ( -6.972266317189433020E-16, -36.12499999726880162, -5.000000000000000000 ) ) ;
#45940 = CARTESIAN_POINT ( 'NONE',  ( 5.000000000000000000, 24.70833333606451987, -2.886751345948129988 ) ) ;
#45941 = ORIENTED_EDGE ( 'NONE', *, *, #17400, .F. ) ;
#45942 = CARTESIAN_POINT ( 'NONE',  ( 0.000000000000000000, -120.0000000000000000, 0.000000000000000000 ) ) ;
#45943 = CARTESIAN_POINT ( 'NONE',  ( -2.071067811865477726, -168.8125000027312410, -4.999999999999996447 ) ) ;
#45945 = CARTESIAN_POINT ( 'NONE',  ( -5.000000000000000000, -26.00000000000000355, 0.000000000000000000 ) ) ;
#45944 = CARTESIAN_POINT ( 'NONE',  ( 1.975475456537005874E-15, -0.7499999999999996669, 5.000000000000000000 ) ) ;
#45946 = CARTESIAN_POINT ( 'NONE',  ( 9.457646018065525792E-16, -29.06249999863440081, 5.148502694627439702 ) ) ;
#45947 = CARTESIAN_POINT ( 'NONE',  ( 4.458734124999999437, -85.81249999863439371, -5.460374474430324690E-16 ) ) ;
#45948 = CARTESIAN_POINT ( 'NONE',  ( -3.535250795749689387E-16, -23.12499999726881228, -5.773502691896257311 ) ) ;
#45950 = ORIENTED_EDGE ( 'NONE', *, *, #49954, .T. ) ;
#45949 = CARTESIAN_POINT ( 'NONE',  ( -4.458734124999999437, -54.39583333196773651, -2.574251347313719407 ) ) ;
#45951 = CARTESIAN_POINT ( 'NONE',  ( 5.000000000000000888, -27.58333333333333570, 2.886751345948126879 ) ) ;
#45952 = CARTESIAN_POINT ( 'NONE',  ( 1.339745962155614700, 27.83034180399266688, -4.999999999999999112 ) ) ;
#45954 = ORIENTED_EDGE ( 'NONE', *, *, #10696, .F. ) ;
#45953 = CARTESIAN_POINT ( 'NONE',  ( 9.457646018065525792E-16, -4.312499998634408804, 5.148502694627439702 ) ) ;
#45955 = CARTESIAN_POINT ( 'NONE',  ( 2.499999999999998668, -73.33333333333332860, -4.330127018922193649 ) ) ;
#45956 = CARTESIAN_POINT ( 'NONE',  ( -50.40829686548195099, -139.0000000013655779, -1.485763867205728284 ) ) ;
#45957 = CARTESIAN_POINT ( 'NONE',  ( 9.457646018065525792E-16, -44.31249999863440081, 5.148502694627439702 ) ) ;
#45958 = CARTESIAN_POINT ( 'NONE',  ( 1.339745962155612702, -34.29465819873851729, -5.000000000000000000 ) ) ;
#45959 = AXIS2_PLACEMENT_3D ( 'NONE', #29506, #25336, #5722 ) ;
#45960 = CARTESIAN_POINT ( 'NONE',  ( -3.535533905932737309, -158.6250000000000284, -3.535533905932738197 ) ) ;
#45961 = CARTESIAN_POINT ( 'NONE',  ( 2.500000000000002220, -71.54166666393547303, 4.330127018922192761 ) ) ;
#45962 = FACE_OUTER_BOUND ( 'NONE', #33234, .T. ) ;
#45963 = CARTESIAN_POINT ( 'NONE',  ( -59.98410592259440222, -154.1250000000000284, -0.3983568153799752487 ) ) ;
#45964 = EDGE_CURVE ( 'NONE', #41952, #53169, #57477, .T. ) ;
#45965 = AXIS2_PLACEMENT_3D ( 'NONE', #22515, #61755, #35156 ) ;
#45966 = CARTESIAN_POINT ( 'NONE',  ( 4.458734124999999437, -15.06249999863440436, -5.460374474430324690E-16 ) ) ;
#45967 = AXIS2_PLACEMENT_3D ( 'NONE', #44432, #5849, #49896 ) ;
#45968 = CARTESIAN_POINT ( 'NONE',  ( 4.458734124999998549, -53.97916666530107221, -2.574251347313721627 ) ) ;
#45969 = DIRECTION ( 'NONE',  ( 0.000000000000000000, 0.000000000000000000, 1.000000000000000000 ) ) ;
#45970 = CARTESIAN_POINT ( 'NONE',  ( 1.846868145590736310, -142.6250000013655779, 4.458734124999999437 ) ) ;
#45971 = CARTESIAN_POINT ( 'NONE',  ( 9.457646018065525792E-16, -94.31249999863440792, 5.148502694627439702 ) ) ;
#45972 = CARTESIAN_POINT ( 'NONE',  ( 2.071067811865348940, -157.8125000000000284, -5.000000000000127898 ) ) ;
#45973 = ORIENTED_EDGE ( 'NONE', *, *, #31984, .T. ) ;
#45974 = CARTESIAN_POINT ( 'NONE',  ( -2.071067811865308972, -155.3125000000000000, 5.000000000000169642 ) ) ;
#45975 = CARTESIAN_POINT ( 'NONE',  ( 4.458734124999999437, 24.93750000136559208, -5.460374474430324690E-16 ) ) ;
#45976 = CARTESIAN_POINT ( 'NONE',  ( -56.66612745406270335, -146.4375000027312126, -5.149110718188516067 ) ) ;
#45977 = EDGE_CURVE ( 'NONE', #55791, #27450, #42658, .T. ) ;
#45978 = CARTESIAN_POINT ( 'NONE',  ( 1.339745962155612702, -60.29465819873851729, -5.000000000000000000 ) ) ;
#45979 = CARTESIAN_POINT ( 'NONE',  ( 9.457646018065525792E-16, -3.062499998634407472, 5.148502694627439702 ) ) ;
#45980 = CARTESIAN_POINT ( 'NONE',  ( -4.458734124999999437, -147.1875000013656063, -5.460374474430324690E-16 ) ) ;
#45981 = CARTESIAN_POINT ( 'NONE',  ( -2.229367062500000163, -21.72916666530107221, -3.861377020970580443 ) ) ;
#45982 = ADVANCED_FACE ( 'NONE', ( #34254 ), #29107, .T. ) ;
#45983 = CARTESIAN_POINT ( 'NONE',  ( -2.229367062500000163, -63.72916666530106511, -3.861377020970580443 ) ) ;
#45984 = CARTESIAN_POINT ( 'NONE',  ( 2.499999999999998668, -70.33333333333332860, -4.330127018922193649 ) ) ;
#45985 = CARTESIAN_POINT ( 'NONE',  ( -3.152548672688508926E-16, -6.562499998634404363, -5.148502694627439702 ) ) ;
#45986 = CARTESIAN_POINT ( 'NONE',  ( -4.458734124999999437, -146.0000000013655779, -1.846868145590735644 ) ) ;
#45987 = CARTESIAN_POINT ( 'NONE',  ( -4.458734124999999437, 15.35416666803225993, -2.574251347313719407 ) ) ;
#45988 = ORIENTED_EDGE ( 'NONE', *, *, #59043, .F. ) ;
#45989 = CYLINDRICAL_SURFACE ( 'NONE', #7962, 5.000000000000000000 ) ;
#45990 = CARTESIAN_POINT ( 'NONE',  ( 4.999999999999999112, 5.773502691896256422, -7.063244554129997965 ) ) ;
#45992 = CARTESIAN_POINT ( 'NONE',  ( 2.229367062499998831, -18.64583333196774007, -3.861377020970580887 ) ) ;
#45991 = CARTESIAN_POINT ( 'NONE',  ( 2.499999999999998668, -87.33333333333332860, -4.330127018922193649 ) ) ;
#45993 = CARTESIAN_POINT ( 'NONE',  ( 7.500000000000000888, 2.932633423934449812, -0.4709827563909316783 ) ) ;
#45994 = DIRECTION ( 'NONE',  ( -0.000000000000000000, 1.000000000000000000, -0.000000000000000000 ) ) ;
#45995 =( BOUNDED_CURVE ( )  B_SPLINE_CURVE ( 2, ( #51523, #47007, #27068, #41848, #51829, #23510, #43112, #13543, #22885 ),
 .UNSPECIFIED., .F., .F. ) 
 B_SPLINE_CURVE_WITH_KNOTS ( ( 3, 2, 2, 2, 3 ),
 ( 0.9416666666666665408, 0.9458333333333331927, 0.9499999999999997335, 0.9541666666666664964, 0.9583333333333331483 ),
 .UNSPECIFIED. ) 
 CURVE ( )  GEOMETRIC_REPRESENTATION_ITEM ( )  RATIONAL_B_SPLINE_CURVE ( ( 1.000000000000001998, 0.9238795325112847401, 1.000000000000000000, 0.9238795325112867385, 1.000000000000000000, 0.9238795325112867385, 1.000000000000000000, 0.9238795325112908463, 0.9999999999999958922 ) ) 
 REPRESENTATION_ITEM ( '' )  );
#45996 = CARTESIAN_POINT ( 'NONE',  ( -53.51423613279429503, -151.2500000013656063, 4.591703134518082763 ) ) ;
#45997 = CARTESIAN_POINT ( 'NONE',  ( 5.000000000000000888, -47.45833333060214443, 2.886751345948126879 ) ) ;
#45998 = DIRECTION ( 'NONE',  ( 0.000000000000000000, 0.000000000000000000, 1.000000000000000000 ) ) ;
#45999 = CARTESIAN_POINT ( 'NONE',  ( 9.457646018065525792E-16, 9.937500001365593860, 5.148502694627439702 ) ) ;
#46000 = CARTESIAN_POINT ( 'NONE',  ( 5.275681513340003914E-14, 11.74999999999999645, -5.000000000000000000 ) ) ;
#46001 = CARTESIAN_POINT ( 'NONE',  ( -1.339745962155613812, -15.20534180126147916, -5.000000000000000000 ) ) ;
#46002 = CARTESIAN_POINT ( 'NONE',  ( 2.229367062500001939, 13.02083333469892779, 3.861377020970579999 ) ) ;
#46003 = CARTESIAN_POINT ( 'NONE',  ( -3.152548672688508926E-16, -69.56249999863439371, -5.148502694627439702 ) ) ;
#46004 = CARTESIAN_POINT ( 'NONE',  ( -4.458734124999999437, -14.64583333196773474, -2.574251347313719407 ) ) ;
#46005 = AXIS2_PLACEMENT_3D ( 'NONE', #57709, #58014, #53186 ) ;
#46006 = CARTESIAN_POINT ( 'NONE',  ( -5.000000000000000000, -3.000000000000002665, 0.000000000000000000 ) ) ;
#46007 = CARTESIAN_POINT ( 'NONE',  ( -3.152801135295367096, -162.0625000013656063, -3.152801135295367541 ) ) ;
#46008 = CARTESIAN_POINT ( 'NONE',  ( -5.000000000000000000, -40.95833333060215153, -2.886751345948128211 ) ) ;
#46009 = CARTESIAN_POINT ( 'NONE',  ( -2.229367062499996610, -59.14583333196773651, 3.861377020970582219 ) ) ;
#46010 = CARTESIAN_POINT ( 'NONE',  ( -5.000000000000000000, -95.95833333060214443, -2.886751345948128211 ) ) ;
#46011 = EDGE_CURVE ( 'NONE', #54753, #9578, #51371, .T. ) ;
#46012 = VECTOR ( 'NONE', #58587, 1000.000000000000000 ) ;
#46013 = CARTESIAN_POINT ( 'NONE',  ( -2.499999999999996447, -27.83333333333333570, 4.330127018922195425 ) ) ;
#46014 = CARTESIAN_POINT ( 'NONE',  ( -9.184850993605147944E-16, -139.3750000027312126, 5.000000000000000000 ) ) ;
#46015 = CARTESIAN_POINT ( 'NONE',  ( 4.458734125000000326, -33.89583333196772941, 2.574251347313718519 ) ) ;
#46016 = CARTESIAN_POINT ( 'NONE',  ( 1.339745962155612702, -60.29465819873851729, -5.000000000000000000 ) ) ;
#46017 = CARTESIAN_POINT ( 'NONE',  ( 2.500000000000002220, -48.66666666666666430, 4.330127018922192761 ) ) ;
#46018 = CARTESIAN_POINT ( 'NONE',  ( 1.339745962155615144, -13.70534180126148094, 4.999999999999999112 ) ) ;
#46019 = CARTESIAN_POINT ( 'NONE',  ( 1.975475456537005874E-15, -50.75000000000000000, 5.000000000000000000 ) ) ;
#46020 = ORIENTED_EDGE ( 'NONE', *, *, #46137, .F. ) ;
#46021 = CARTESIAN_POINT ( 'NONE',  ( -2.229367062500000163, -106.4791666653010651, -3.861377020970580443 ) ) ;
#46022 = CARTESIAN_POINT ( 'NONE',  ( -3.152548672688508926E-16, -3.812499998634408360, -5.148502694627439702 ) ) ;
#46023 = DIRECTION ( 'NONE',  ( 0.000000000000000000, 0.000000000000000000, 1.000000000000000000 ) ) ;
#46024 = CARTESIAN_POINT ( 'NONE',  ( 5.000000000000000000, -6.416666666666666963, -2.886751345948129988 ) ) ;
#46025 = CARTESIAN_POINT ( 'NONE',  ( -4.458734124999997661, -73.22916666530106511, 2.574251347313722516 ) ) ;
#46026 = CYLINDRICAL_SURFACE ( 'NONE', #18505, 5.000000000000000000 ) ;
#46027 = CARTESIAN_POINT ( 'NONE',  ( 2.499999999999998668, -8.208333330602144429, -4.330127018922193649 ) ) ;
#46029 = EDGE_LOOP ( 'NONE', ( #23319, #18584, #18658, #31734 ) ) ;
#46028 = CARTESIAN_POINT ( 'NONE',  ( 2.229367062500001939, -39.97916666530107221, 3.861377020970579999 ) ) ;
#46030 = LINE ( 'NONE', #61159, #33337 ) ;
#46032 = ORIENTED_EDGE ( 'NONE', *, *, #23995, .F. ) ;
#46031 = CARTESIAN_POINT ( 'NONE',  ( -2.229367062500000163, 13.27083333469892779, -3.861377020970580443 ) ) ;
#46033 = CARTESIAN_POINT ( 'NONE',  ( 1.339745962155615144, -101.5803417985302985, 4.999999999999999112 ) ) ;
#46034 = CARTESIAN_POINT ( 'NONE',  ( -5.000000000000000000, -53.99999999999999289, 0.000000000000000000 ) ) ;
#46035 = CARTESIAN_POINT ( 'NONE',  ( 4.458734124999999437, -28.06249999863440081, -5.460374474430324690E-16 ) ) ;
#46036 = CARTESIAN_POINT ( 'NONE',  ( -1.339745962155610925, -10.66965819600733312, 5.000000000000000000 ) ) ;
#46037 = CARTESIAN_POINT ( 'NONE',  ( -4.458734124999999437, -75.31249999863440792, 0.000000000000000000 ) ) ;
#46038 = CARTESIAN_POINT ( 'NONE',  ( 2.730187237215162345E-16, -140.4375000013656063, -4.458734124999999437 ) ) ;
#46039 = CARTESIAN_POINT ( 'NONE',  ( -4.458734124999999437, -86.39583333196772230, -2.574251347313719407 ) ) ;
#46040 = CARTESIAN_POINT ( 'NONE',  ( -52.80376928212989185, -137.1250000013655779, -4.297418129356379346 ) ) ;
#46041 = CARTESIAN_POINT ( 'NONE',  ( 2.229367062500001939, -35.22916666530107221, 3.861377020970579999 ) ) ;
#46042 = EDGE_CURVE ( 'NONE', #62035, #20917, #53301, .T. ) ;
#46043 = EDGE_CURVE ( 'NONE', #46757, #30862, #15920, .T. ) ;
#46044 = ORIENTED_EDGE ( 'NONE', *, *, #6331, .F. ) ;
#46045 = CARTESIAN_POINT ( 'NONE',  ( 4.458734124999998549, -80.97916666530106511, -2.574251347313721627 ) ) ;
#46046 = CARTESIAN_POINT ( 'NONE',  ( -2.500000000000000444, 12.95833333606451809, -4.330127018922193649 ) ) ;
#46047 =( BOUNDED_CURVE ( )  B_SPLINE_CURVE ( 2, ( #9945, #30196, #25067, #29561, #49194, #44677, #49825, #50146, #10908 ),
 .UNSPECIFIED., .F., .F. ) 
 B_SPLINE_CURVE_WITH_KNOTS ( ( 3, 2, 2, 2, 3 ),
 ( 0.9145833333333333037, 0.9152777777777777457, 0.9166666666666666297, 0.9180555555555555136, 0.9187499999999999556 ),
 .UNSPECIFIED. ) 
 CURVE ( )  GEOMETRIC_REPRESENTATION_ITEM ( )  RATIONAL_B_SPLINE_CURVE ( ( 0.9330127018922194093, 0.9330127018922194093, 1.000000000000000000, 0.8660254037844387076, 1.000000000000000000, 0.8660254037844387076, 1.000000000000000000, 0.9330127018922194093, 0.9330127018922194093 ) ) 
 REPRESENTATION_ITEM ( '' )  );
#46048 = EDGE_CURVE ( 'NONE', #24763, #54724, #42220, .T. ) ;
#46049 = ORIENTED_EDGE ( 'NONE', *, *, #5248, .T. ) ;
#46050 = CARTESIAN_POINT ( 'NONE',  ( -6.972266317189433020E-16, -16.25000000000000000, -5.000000000000000000 ) ) ;
#46051 =( BOUNDED_CURVE ( )  B_SPLINE_CURVE ( 2, ( #23714, #62946, #58108, #33664, #53283, #9219, #48759, #43615, #33978 ),
 .UNSPECIFIED., .F., .F. ) 
 B_SPLINE_CURVE_WITH_KNOTS ( ( 3, 2, 2, 2, 3 ),
 ( 0.3910714285714285698, 0.3916666666666666630, 0.3928571428571428492, 0.3940476190476190355, 0.3946428571428571286 ),
 .UNSPECIFIED. ) 
 CURVE ( )  GEOMETRIC_REPRESENTATION_ITEM ( )  RATIONAL_B_SPLINE_CURVE ( ( 0.9330127018922194093, 0.9330127018922194093, 1.000000000000000000, 0.8660254037844387076, 1.000000000000000000, 0.8660254037844387076, 1.000000000000000000, 0.9330127018922194093, 0.9330127018922194093 ) ) 
 REPRESENTATION_ITEM ( '' )  );
#46052 = CARTESIAN_POINT ( 'NONE',  ( 0.000000000000000000, -120.0000000000000000, 0.000000000000000000 ) ) ;
#46053 = CARTESIAN_POINT ( 'NONE',  ( -4.458734124999999437, -65.64583333196773651, -2.574251347313719407 ) ) ;
#46054 = CARTESIAN_POINT ( 'NONE',  ( -4.458734124999998549, -11.47916666530107044, 2.574251347313722516 ) ) ;
#46055 = ORIENTED_EDGE ( 'NONE', *, *, #45252, .T. ) ;
#46056 = EDGE_CURVE ( 'NONE', #56335, #47300, #13491, .T. ) ;
#46057 = CARTESIAN_POINT ( 'NONE',  ( -1.339745962155613812, -10.08034179853029144, -5.000000000000000000 ) ) ;
#46058 = CARTESIAN_POINT ( 'NONE',  ( 1.975475456537005874E-15, -62.74999999999998579, 5.000000000000000000 ) ) ;
#46059 = ORIENTED_EDGE ( 'NONE', *, *, #50433, .T. ) ;
#46060 = CARTESIAN_POINT ( 'NONE',  ( -3.152548672688508926E-16, -7.812499998634405252, -5.148502694627439702 ) ) ;
#46061 = EDGE_CURVE ( 'NONE', #2195, #59356, #2409, .T. ) ;
#46062 = CARTESIAN_POINT ( 'NONE',  ( 4.458734124999999437, 5.187500001365596525, -5.460374474430324690E-16 ) ) ;
#46063 = CARTESIAN_POINT ( 'NONE',  ( 1.339745962155615144, -64.70534180126146850, 4.999999999999999112 ) ) ;
#46064 = CARTESIAN_POINT ( 'NONE',  ( -1.846868145590734756, -158.1250000013656063, -4.458734124999999437 ) ) ;
#46065 = CARTESIAN_POINT ( 'NONE',  ( 1.339745962155615144, -75.58034179853029855, 4.999999999999999112 ) ) ;
#46066 = VERTEX_POINT ( 'NONE', #4998 ) ;
#46067 = CARTESIAN_POINT ( 'NONE',  ( 9.457646018065525792E-16, -88.06249999863439371, 5.148502694627439702 ) ) ;
#46068 = ADVANCED_FACE ( 'NONE', ( #11411 ), #25892, .T. ) ;
#46069 = DIRECTION ( 'NONE',  ( -0.000000000000000000, 1.000000000000000000, -0.000000000000000000 ) ) ;
#46070 = CARTESIAN_POINT ( 'NONE',  ( 2.229367062499998831, -5.645833331967740953, -3.861377020970580887 ) ) ;
#46071 = CARTESIAN_POINT ( 'NONE',  ( -6.972266317189433020E-16, -88.12499999726880162, -5.000000000000000000 ) ) ;
#46072 = VECTOR ( 'NONE', #23986, 1000.000000000000000 ) ;
#46073 = CARTESIAN_POINT ( 'NONE',  ( -5.000000000000000000, -30.87499999726881228, 0.000000000000000000 ) ) ;
#46074 = PLANE ( 'NONE',  #42985 ) ;
#46075 = CARTESIAN_POINT ( 'NONE',  ( -4.458734124999999437, 23.60416666803225993, -2.574251347313719407 ) ) ;
#46076 = CARTESIAN_POINT ( 'NONE',  ( 1.339745962155612702, -110.1696581960073189, -5.000000000000000000 ) ) ;
#46077 = CARTESIAN_POINT ( 'NONE',  ( -4.458734124999999437, 29.60416666803225993, -2.574251347313719407 ) ) ;
#46078 = CARTESIAN_POINT ( 'NONE',  ( -4.458734124999998549, -52.22916666530106511, 2.574251347313722516 ) ) ;
#46079 = CARTESIAN_POINT ( 'NONE',  ( 4.458734124999999437, -37.06249999863440792, -5.460374474430324690E-16 ) ) ;
#46080 = CARTESIAN_POINT ( 'NONE',  ( 2.229367062500001939, 2.770833334698928674, 3.861377020970579999 ) ) ;
#46081 = CARTESIAN_POINT ( 'NONE',  ( 3.535533905932736864, -160.2500000027312126, 3.535533905932738641 ) ) ;
#46082 = CARTESIAN_POINT ( 'NONE',  ( 1.060575238724906964E-15, 15.25000000000000000, 5.773502691896257311 ) ) ;
#46083 = CARTESIAN_POINT ( 'NONE',  ( 5.000000000000000000, -146.1875000027311842, 2.071067811865478614 ) ) ;
#46084 = CARTESIAN_POINT ( 'NONE',  ( 2.229367062500001939, -44.97916666530106511, 3.861377020970579999 ) ) ;
#46085 = CARTESIAN_POINT ( 'NONE',  ( 2.499999999999998668, -76.20833333060214443, -4.330127018922193649 ) ) ;
#46086 = CARTESIAN_POINT ( 'NONE',  ( -59.29741812935640155, -140.8750000013656063, -2.196230717870135685 ) ) ;
#46087 = FACE_OUTER_BOUND ( 'NONE', #15446, .T. ) ;
#46088 = CARTESIAN_POINT ( 'NONE',  ( -4.999999999999998224, -63.79166666393547303, 2.886751345948131764 ) ) ;
#46089 = CARTESIAN_POINT ( 'NONE',  ( -3.152548672688508926E-16, -84.81249999863439371, -5.148502694627439702 ) ) ;
#46090 = CARTESIAN_POINT ( 'NONE',  ( -4.458734124999999437, -160.2500000013656063, -1.846868145590735644 ) ) ;
#46091 = CARTESIAN_POINT ( 'NONE',  ( -0.3875187462251565851, -8.436519985395204202, -7.781689322724289148 ) ) ;
#46092 = CARTESIAN_POINT ( 'NONE',  ( -2.500000000000000444, -31.16666666666666785, -4.330127018922193649 ) ) ;
#46093 = CARTESIAN_POINT ( 'NONE',  ( 1.846868145590736310, -141.6250000013656631, 4.458734124999999437 ) ) ;
#46094 = ORIENTED_EDGE ( 'NONE', *, *, #45680, .F. ) ;
#46095 = CARTESIAN_POINT ( 'NONE',  ( 2.229367062500001939, 22.77083333469892423, 3.861377020970579999 ) ) ;
#46096 = ORIENTED_EDGE ( 'NONE', *, *, #9968, .T. ) ;
#46097 = CARTESIAN_POINT ( 'NONE',  ( 4.458734125000001214, -89.89583333196775072, 2.574251347313718519 ) ) ;
#46098 = CARTESIAN_POINT ( 'NONE',  ( 4.458734124999999437, 11.93750000136559564, -5.460374474430324690E-16 ) ) ;
#46099 = CARTESIAN_POINT ( 'NONE',  ( -3.535250795749689387E-16, 14.87500000273118594, -5.773502691896257311 ) ) ;
#46100 =( BOUNDED_CURVE ( )  B_SPLINE_CURVE ( 2, ( #28575, #28889, #4448, #23767, #23452, #5086, #48510, #39487, #18619 ),
 .UNSPECIFIED., .F., .F. ) 
 B_SPLINE_CURVE_WITH_KNOTS ( ( 3, 2, 2, 2, 3 ),
 ( 0.8312500000000000444, 0.8319444444444444864, 0.8333333333333333703, 0.8347222222222222543, 0.8354166666666666963 ),
 .UNSPECIFIED. ) 
 CURVE ( )  GEOMETRIC_REPRESENTATION_ITEM ( )  RATIONAL_B_SPLINE_CURVE ( ( 0.9330127018922194093, 0.9330127018922194093, 1.000000000000000000, 0.8660254037844387076, 1.000000000000000000, 0.8660254037844387076, 1.000000000000000000, 0.9330127018922194093, 0.9330127018922194093 ) ) 
 REPRESENTATION_ITEM ( '' )  );
#46101 = CARTESIAN_POINT ( 'NONE',  ( 2.499999999999998668, 2.666666666666667851, -4.330127018922193649 ) ) ;
#46102 = CARTESIAN_POINT ( 'NONE',  ( 1.060575238724906964E-15, 9.250000000000001776, 5.773502691896257311 ) ) ;
#46103 = VECTOR ( 'NONE', #56969, 1000.000000000000000 ) ;
#46104 = CARTESIAN_POINT ( 'NONE',  ( -3.152548672688508926E-16, -55.56249999863440081, -5.148502694627439702 ) ) ;
#46105 = CARTESIAN_POINT ( 'NONE',  ( -4.458734124999998549, -14.22916666530107221, 2.574251347313722516 ) ) ;
#46106 = CARTESIAN_POINT ( 'NONE',  ( 5.000000000000000888, -6.583333333333329485, 2.886751345948126879 ) ) ;
#46107 = CARTESIAN_POINT ( 'NONE',  ( -51.60603307380591787, -135.1875000013656063, -2.891590998281053704 ) ) ;
#46108 = CARTESIAN_POINT ( 'NONE',  ( 1.975475456537005874E-15, 0.3750000027311862216, 5.000000000000000000 ) ) ;
#46109 = CARTESIAN_POINT ( 'NONE',  ( -2.500000000000000444, -75.04166666393547303, -4.330127018922193649 ) ) ;
#46110 = CARTESIAN_POINT ( 'NONE',  ( -2.500000000000000444, -40.16666666666667140, -4.330127018922193649 ) ) ;
#46111 = DIRECTION ( 'NONE',  ( 0.000000000000000000, 0.000000000000000000, 1.000000000000000000 ) ) ;
#46113 = CARTESIAN_POINT ( 'NONE',  ( -2.229367062500000163, -16.72916666530107577, -3.861377020970580443 ) ) ;
#46112 = CARTESIAN_POINT ( 'NONE',  ( 1.975475456537005874E-15, -44.74999999999999289, 5.000000000000000000 ) ) ;
#46114 = CARTESIAN_POINT ( 'NONE',  ( -2.916731409357579869E-14, 17.37500000273118417, 5.000000000000000888 ) ) ;
#46115 = CARTESIAN_POINT ( 'NONE',  ( -3.152548672688508926E-16, -59.56249999863440081, -5.148502694627439702 ) ) ;
#46116 = CARTESIAN_POINT ( 'NONE',  ( -4.458734125000001214, -153.1250000013656063, 1.846868145590734089 ) ) ;
#46117 = CARTESIAN_POINT ( 'NONE',  ( 9.457646018065525792E-16, -71.06249999863440792, 5.148502694627439702 ) ) ;
#46118 = CARTESIAN_POINT ( 'NONE',  ( -54.64476657466781973, -149.0625000013656063, -4.444560631937228834 ) ) ;
#46119 = CARTESIAN_POINT ( 'NONE',  ( -4.458734124999999437, -20.64583333196774007, -2.574251347313719407 ) ) ;
#46120 = CARTESIAN_POINT ( 'NONE',  ( -4.999999999999999112, -58.79166666393546592, 2.886751345948131764 ) ) ;
#46122 = ORIENTED_EDGE ( 'NONE', *, *, #24835, .F. ) ;
#46121 = ADVANCED_FACE ( 'NONE', ( #1471 ), #30066, .T. ) ;
#46123 = CARTESIAN_POINT ( 'NONE',  ( 1.339745962155612702, -31.16965819600732956, -5.000000000000000000 ) ) ;
#46124 = VERTEX_POINT ( 'NONE', #40678 ) ;
#46125 = CARTESIAN_POINT ( 'NONE',  ( 4.458734124999998549, -59.97916666530107221, -2.574251347313721627 ) ) ;
#46127 = CARTESIAN_POINT ( 'NONE',  ( 1.339745962155612702, -103.2946581987385173, -5.000000000000000000 ) ) ;
#46126 = DIRECTION ( 'NONE',  ( 0.000000000000000000, 0.000000000000000000, 1.000000000000000000 ) ) ;
#46128 = CARTESIAN_POINT ( 'NONE',  ( 4.458734124999999437, -154.4375000013655779, 0.000000000000000000 ) ) ;
#46129 = ORIENTED_EDGE ( 'NONE', *, *, #45541, .F. ) ;
#46130 = CARTESIAN_POINT ( 'NONE',  ( -60.14911071818854538, -127.0625000000000142, 1.666127454062681368 ) ) ;
#46131 = CARTESIAN_POINT ( 'NONE',  ( 1.975475456537005874E-15, -77.62499999726881583, 5.000000000000000000 ) ) ;
#46132 = CARTESIAN_POINT ( 'NONE',  ( -2.229367062500000163, -47.72916666530106511, -3.861377020970580443 ) ) ;
#46133 = ORIENTED_EDGE ( 'NONE', *, *, #55046, .T. ) ;
#46134 = CARTESIAN_POINT ( 'NONE',  ( -2.499999999999996447, -109.7083333306021444, 4.330127018922195425 ) ) ;
#46135 = CARTESIAN_POINT ( 'NONE',  ( -2.229367062500000163, 10.52083333469892779, -3.861377020970580443 ) ) ;
#46136 = EDGE_CURVE ( 'NONE', #62531, #2792, #33210, .T. ) ;
#46137 = EDGE_CURVE ( 'NONE', #44176, #41301, #22134, .T. ) ;
#46138 = CARTESIAN_POINT ( 'NONE',  ( -3.152548672688508926E-16, 26.43750000136559208, -5.148502694627439702 ) ) ;
#46139 = CARTESIAN_POINT ( 'NONE',  ( -51.60603307380591787, -148.9375000013656063, -2.891590998281053704 ) ) ;
#46140 = CARTESIAN_POINT ( 'NONE',  ( -1.339745962155610925, -23.66965819600732956, 5.000000000000000000 ) ) ;
#46141 = CARTESIAN_POINT ( 'NONE',  ( -1.339745962155610925, -35.66965819600732601, 5.000000000000000000 ) ) ;
#46142 = VECTOR ( 'NONE', #47440, 1000.000000000000000 ) ;
#46144 = EDGE_CURVE ( 'NONE', #50284, #35341, #35658, .T. ) ;
#46143 = ORIENTED_EDGE ( 'NONE', *, *, #112, .F. ) ;
#46145 = CARTESIAN_POINT ( 'NONE',  ( -3.152548672688508926E-16, -72.56249999863439371, -5.148502694627439702 ) ) ;
#46146 = DIRECTION ( 'NONE',  ( -0.000000000000000000, 1.000000000000000000, -0.000000000000000000 ) ) ;
#46147 = CARTESIAN_POINT ( 'NONE',  ( 4.458734124999998549, 10.27083333469892779, -2.574251347313721627 ) ) ;
#46148 = VECTOR ( 'NONE', #62439, 1000.000000000000000 ) ;
#46149 = CARTESIAN_POINT ( 'NONE',  ( -6.972266317189433020E-16, -63.25000000000000000, -5.000000000000000000 ) ) ;
#46150 = ADVANCED_FACE ( 'NONE', ( #57002 ), #27394, .F. ) ;
#46151 = CARTESIAN_POINT ( 'NONE',  ( 55.00000000000002132, 15.00000000000000000, -5.000000000000000000 ) ) ;
#46152 = CARTESIAN_POINT ( 'NONE',  ( -3.152548672688508926E-16, -52.81249999863440792, -5.148502694627439702 ) ) ;
#46153 = CARTESIAN_POINT ( 'NONE',  ( 2.499999999999998668, -13.20833333060214976, -4.330127018922193649 ) ) ;
#46154 = FACE_OUTER_BOUND ( 'NONE', #43926, .T. ) ;
#46155 = CARTESIAN_POINT ( 'NONE',  ( 0.000000000000000000, -120.0000000000000000, 5.000000000000000000 ) ) ;
#46156 = CARTESIAN_POINT ( 'NONE',  ( -6.972266317189433020E-16, -80.12499999726881583, -5.000000000000000000 ) ) ;
#46157 = CARTESIAN_POINT ( 'NONE',  ( 2.229367062500001939, -20.22916666530107221, 3.861377020970579999 ) ) ;
#46158 = ORIENTED_EDGE ( 'NONE', *, *, #35105, .T. ) ;
#46159 = CARTESIAN_POINT ( 'NONE',  ( -51.75738570946856498, -143.7500000000000284, 3.805975901505576964 ) ) ;
#46160 = CARTESIAN_POINT ( 'NONE',  ( 9.457646018065525792E-16, -109.0624999986344221, 5.148502694627439702 ) ) ;
#46161 = CARTESIAN_POINT ( 'NONE',  ( -2.071067811865478170, -157.4375000027312410, 5.000000000000000000 ) ) ;
#46162 = ORIENTED_EDGE ( 'NONE', *, *, #32793, .F. ) ;
#46163 = CARTESIAN_POINT ( 'NONE',  ( 4.458734125000001214, -105.1458333319677365, 2.574251347313718519 ) ) ;
#46164 = CARTESIAN_POINT ( 'NONE',  ( -4.458734124999999437, -28.39583333196774007, -2.574251347313719407 ) ) ;
#46165 = CARTESIAN_POINT ( 'NONE',  ( -5.000000000000000000, -64.95833333060214443, -2.886751345948128211 ) ) ;
#46166 = CARTESIAN_POINT ( 'NONE',  ( -59.44456063193725015, -151.8125000013656063, -0.3552334253322034230 ) ) ;
#46167 = CARTESIAN_POINT ( 'NONE',  ( -59.29741812935640155, -142.6250000013656063, -2.196230717870135685 ) ) ;
#46168 = CARTESIAN_POINT ( 'NONE',  ( -2.229367062500000163, -23.47916666530107221, -3.861377020970580443 ) ) ;
#46169 = CARTESIAN_POINT ( 'NONE',  ( 9.457646018065525792E-16, -67.31249999863440792, 5.148502694627439702 ) ) ;
#46170 = CARTESIAN_POINT ( 'NONE',  ( -5.000000000000000000, -39.87499999726880162, 0.000000000000000000 ) ) ;
#46171 = CARTESIAN_POINT ( 'NONE',  ( -4.458734124999999437, -27.39583333196774007, -2.574251347313719407 ) ) ;
#46172 = CARTESIAN_POINT ( 'NONE',  ( -6.972266317189433020E-16, -32.24999999999999289, -5.000000000000000000 ) ) ;
#46173 = CARTESIAN_POINT ( 'NONE',  ( 3.535533905932736864, -150.1250000000000000, 3.535533905932738641 ) ) ;
#46174 = CARTESIAN_POINT ( 'NONE',  ( 2.500000000000002220, -12.66666666666666607, 4.330127018922192761 ) ) ;
#46175 = CARTESIAN_POINT ( 'NONE',  ( -3.152801135295367985, -151.8125000013655779, 3.152801135295367096 ) ) ;
#46176 = ORIENTED_EDGE ( 'NONE', *, *, #62993, .T. ) ;
#46177 = CARTESIAN_POINT ( 'NONE',  ( 4.458734124999999437, -49.06249999863440792, -5.460374474430324690E-16 ) ) ;
#46178 = CARTESIAN_POINT ( 'NONE',  ( 6.158835246850667461E-14, -3.124999997268814944, -4.999999999999999112 ) ) ;
#46179 = CARTESIAN_POINT ( 'NONE',  ( 1.339745962155615144, -38.58034179853029144, 4.999999999999999112 ) ) ;
#46180 = CARTESIAN_POINT ( 'NONE',  ( -5.000000000000000000, 24.00000000000000000, 0.000000000000000000 ) ) ;
#46181 =( BOUNDED_CURVE ( )  B_SPLINE_CURVE ( 2, ( #17323, #42700, #46276, #7995, #56887, #22793, #13127, #8310, #37568 ),
 .UNSPECIFIED., .F., .F. ) 
 B_SPLINE_CURVE_WITH_KNOTS ( ( 3, 2, 2, 2, 3 ),
 ( 0.7604166666666666297, 0.7611111111111110716, 0.7624999999999999556, 0.7638888888888888395, 0.7645833333333332815 ),
 .UNSPECIFIED. ) 
 CURVE ( )  GEOMETRIC_REPRESENTATION_ITEM ( )  RATIONAL_B_SPLINE_CURVE ( ( 0.9330127018922194093, 0.9330127018922194093, 1.000000000000000000, 0.8660254037844387076, 1.000000000000000000, 0.8660254037844387076, 1.000000000000000000, 0.9330127018922194093, 0.9330127018922194093 ) ) 
 REPRESENTATION_ITEM ( '' )  );
#46182 = CARTESIAN_POINT ( 'NONE',  ( 5.000000000000000000, 25.50000000000000000, -6.123233995736766282E-16 ) ) ;
#46183 = CARTESIAN_POINT ( 'NONE',  ( 9.457646018065525792E-16, 3.937500001365595192, 5.148502694627439702 ) ) ;
#46184 = CARTESIAN_POINT ( 'NONE',  ( -3.535533905932738641, -160.5000000027312126, 3.535533905932737309 ) ) ;
#46185 = DIRECTION ( 'NONE',  ( 0.000000000000000000, -1.000000000000000000, 0.000000000000000000 ) ) ;
#46186 = CARTESIAN_POINT ( 'NONE',  ( 1.975475456537005874E-15, -7.750000000000000000, 5.000000000000000000 ) ) ;
#46187 = CARTESIAN_POINT ( 'NONE',  ( 2.229367062500001939, 14.77083333469892779, 3.861377020970579999 ) ) ;
#46188 = CARTESIAN_POINT ( 'NONE',  ( 5.000000000000000000, 4.625000002731187720, -6.123233995736766282E-16 ) ) ;
#46189 = ORIENTED_EDGE ( 'NONE', *, *, #29867, .T. ) ;
#46190 = LINE ( 'NONE', #13356, #59229 ) ;
#46191 = ORIENTED_EDGE ( 'NONE', *, *, #22058, .T. ) ;
#46192 = CARTESIAN_POINT ( 'NONE',  ( 2.500000000000002220, 26.33333333333333215, 4.330127018922192761 ) ) ;
#46193 = CARTESIAN_POINT ( 'NONE',  ( 4.458734125000001214, -42.89583333196773651, 2.574251347313718519 ) ) ;
#46194 = CARTESIAN_POINT ( 'NONE',  ( -4.458734125000000326, -164.2500000013656063, -1.846868145590735644 ) ) ;
#46195 = ADVANCED_FACE ( 'NONE', ( #18382 ), #37370, .T. ) ;
#46196 = CARTESIAN_POINT ( 'NONE',  ( -5.000000000000000000, -43.95833333060214443, -2.886751345948128211 ) ) ;
#46197 = ORIENTED_EDGE ( 'NONE', *, *, #3851, .T. ) ;
#46198 = CARTESIAN_POINT ( 'NONE',  ( -2.229367062499996610, -19.14583333196774007, 3.861377020970582219 ) ) ;
#46199 = VERTEX_POINT ( 'NONE', #12917 ) ;
#46200 = CARTESIAN_POINT ( 'NONE',  ( -4.999999999999999112, -85.91666666666667140, 2.886751345948131764 ) ) ;
#46201 = CARTESIAN_POINT ( 'NONE',  ( 1.846868145590736310, -165.6250000013656063, 4.458734124999999437 ) ) ;
#46203 = ORIENTED_EDGE ( 'NONE', *, *, #20853, .F. ) ;
#46202 = CARTESIAN_POINT ( 'NONE',  ( -6.972266317189433020E-16, -19.25000000000000000, -5.000000000000000000 ) ) ;
#46204 = CARTESIAN_POINT ( 'NONE',  ( -60.14911071818854538, -141.0625000000000284, 1.666127454062681368 ) ) ;
#46205 = CARTESIAN_POINT ( 'NONE',  ( 4.458734124999998549, -31.97916666530107577, -2.574251347313721627 ) ) ;
#46206 = PLANE ( 'NONE',  #24794 ) ;
#46207 = EDGE_LOOP ( 'NONE', ( #50716, #8169, #28638, #20498 ) ) ;
#46208 = CARTESIAN_POINT ( 'NONE',  ( 2.229367062499998831, -77.64583333196773651, -3.861377020970580887 ) ) ;
#46209 = CARTESIAN_POINT ( 'NONE',  ( 9.457646018065525792E-16, -110.3124999986343937, 5.148502694627439702 ) ) ;
#46210 = CARTESIAN_POINT ( 'NONE',  ( 2.499999999999998668, -18.33333333333333215, -4.330127018922193649 ) ) ;
#46211 = ORIENTED_EDGE ( 'NONE', *, *, #40175, .T. ) ;
#46212 = CARTESIAN_POINT ( 'NONE',  ( 0.000000000000000000, -120.0000000000000000, 0.000000000000000000 ) ) ;
#46213 = CARTESIAN_POINT ( 'NONE',  ( -52.80376928212989185, -143.1250000013656063, -4.297418129356378458 ) ) ;
#46214 = CARTESIAN_POINT ( 'NONE',  ( -3.152548672688508926E-16, -82.81249999863442213, -5.148502694627439702 ) ) ;
#46215 = CARTESIAN_POINT ( 'NONE',  ( -59.98410592259440222, -131.2500000027312126, -0.3983568153799752487 ) ) ;
#46216 = DIRECTION ( 'NONE',  ( 0.000000000000000000, 0.000000000000000000, 1.000000000000000000 ) ) ;
#46217 = CARTESIAN_POINT ( 'NONE',  ( -3.152801135295367985, -144.0625000013655779, 3.152801135295367096 ) ) ;
#46218 = CARTESIAN_POINT ( 'NONE',  ( -6.972266317189433020E-16, 20.74999999999999645, -5.000000000000000000 ) ) ;
#46219 = CARTESIAN_POINT ( 'NONE',  ( 4.458734124999998549, -56.72916666530107932, -2.574251347313721627 ) ) ;
#46220 = CARTESIAN_POINT ( 'NONE',  ( -4.458734124999999437, -46.31249999863440792, 0.000000000000000000 ) ) ;
#46221 = CARTESIAN_POINT ( 'NONE',  ( -4.458734124999999437, 28.68750000136559208, 0.000000000000000000 ) ) ;
#46222 = CARTESIAN_POINT ( 'NONE',  ( -5.000000000000000000, -104.0000000000000142, 0.000000000000000000 ) ) ;
#46223 = CARTESIAN_POINT ( 'NONE',  ( 5.000000000000000000, -3.500000000000003109, -6.123233995736766282E-16 ) ) ;
#46224 = CARTESIAN_POINT ( 'NONE',  ( -2.229367062499996610, -36.39583333196773651, 3.861377020970582219 ) ) ;
#46225 = CARTESIAN_POINT ( 'NONE',  ( -5.000000000000000000, 3.125000002731185944, 0.000000000000000000 ) ) ;
#46226 = CARTESIAN_POINT ( 'NONE',  ( -9.184850993605147944E-16, -153.3750000027311842, 5.000000000000000000 ) ) ;
#46227 = CARTESIAN_POINT ( 'NONE',  ( -59.44456063193725015, -128.5625000013656063, -0.3552334253322034230 ) ) ;
#46228 = CARTESIAN_POINT ( 'NONE',  ( -4.458734124999999437, -77.64583333196773651, -2.574251347313719407 ) ) ;
#46229 = CARTESIAN_POINT ( 'NONE',  ( 5.000000000000000888, -34.58333333333332860, 2.886751345948126879 ) ) ;
#46230 = CARTESIAN_POINT ( 'NONE',  ( 2.229367062499998831, -96.64583333196773651, -3.861377020970580887 ) ) ;
#46231 = CARTESIAN_POINT ( 'NONE',  ( -4.458734124999999437, -7.645833331967734736, -2.574251347313719407 ) ) ;
#46232 = VERTEX_POINT ( 'NONE', #22593 ) ;
#46233 = CARTESIAN_POINT ( 'NONE',  ( -54.60164318462004474, -139.3750000000000284, -4.984105922594373794 ) ) ;
#46234 = CARTESIAN_POINT ( 'NONE',  ( 1.339745962155612702, -47.29465819873852439, -5.000000000000000000 ) ) ;
#46235 = CARTESIAN_POINT ( 'NONE',  ( -3.152548672688508926E-16, -89.56249999863439371, -5.148502694627439702 ) ) ;
#46236 = CARTESIAN_POINT ( 'NONE',  ( 3.535533905932738197, -169.0000000027312126, -3.535533905932738197 ) ) ;
#46237 = CARTESIAN_POINT ( 'NONE',  ( 4.458734124999998549, -87.97916666530107932, -2.574251347313721627 ) ) ;
#46238 = VECTOR ( 'NONE', #12562, 1000.000000000000114 ) ;
#46239 = CARTESIAN_POINT ( 'NONE',  ( -4.458734124999999437, 11.35416666803225993, -2.574251347313719407 ) ) ;
#46240 = CARTESIAN_POINT ( 'NONE',  ( 0.000000000000000000, -120.0000000000000000, 5.000000000000000000 ) ) ;
#46241 = CARTESIAN_POINT ( 'NONE',  ( -58.39396692619412477, -134.4375000013656063, 2.891590998281057701 ) ) ;
#46242 = AXIS2_PLACEMENT_3D ( 'NONE', #32865, #24154, #29273 ) ;
#46243 = CARTESIAN_POINT ( 'NONE',  ( 4.458734124999998549, -8.729166665301073991, -2.574251347313721627 ) ) ;
#46244 = CARTESIAN_POINT ( 'NONE',  ( 4.458734124999999437, 16.93750000136559564, -5.460374474430324690E-16 ) ) ;
#46245 = CARTESIAN_POINT ( 'NONE',  ( -2.229367062500000163, -50.72916666530107221, -3.861377020970580443 ) ) ;
#46246 = CYLINDRICAL_SURFACE ( 'NONE', #42839, 5.000000000000000000 ) ;
#46247 = CARTESIAN_POINT ( 'NONE',  ( 4.458734124999998549, -86.72916666530107932, -2.574251347313721627 ) ) ;
#46248 = CARTESIAN_POINT ( 'NONE',  ( -4.458734124999997661, -8.229166665301073991, 2.574251347313722516 ) ) ;
#46249 = SURFACE_STYLE_USAGE ( .BOTH. , #57181 ) ;
#46250 = VERTEX_POINT ( 'NONE', #18059 ) ;
#46251 = CARTESIAN_POINT ( 'NONE',  ( 4.458734124999999437, -38.06249999863440792, -5.460374474430324690E-16 ) ) ;
#46252 =( BOUNDED_CURVE ( )  B_SPLINE_CURVE ( 2, ( #44149, #9120, #28728, #49307, #54125, #13941, #430, #10063, #53497 ),
 .UNSPECIFIED., .F., .F. ) 
 B_SPLINE_CURVE_WITH_KNOTS ( ( 3, 2, 2, 2, 3 ),
 ( 0.5660714285714285587, 0.5666666666666666519, 0.5678571428571428381, 0.5690476190476190244, 0.5696428571428571175 ),
 .UNSPECIFIED. ) 
 CURVE ( )  GEOMETRIC_REPRESENTATION_ITEM ( )  RATIONAL_B_SPLINE_CURVE ( ( 0.9330127018922194093, 0.9330127018922194093, 1.000000000000000000, 0.8660254037844387076, 1.000000000000000000, 0.8660254037844387076, 1.000000000000000000, 0.9330127018922194093, 0.9330127018922194093 ) ) 
 REPRESENTATION_ITEM ( '' )  );
#46253 = CARTESIAN_POINT ( 'NONE',  ( -50.55543936806279248, -129.3125000013656063, 0.3552334253322060320 ) ) ;
#46254 = CARTESIAN_POINT ( 'NONE',  ( -4.458734124999999437, -78.39583333196772230, -2.574251347313719407 ) ) ;
#46255 = CARTESIAN_POINT ( 'NONE',  ( 4.458734125000001214, 27.85416666803225993, 2.574251347313718519 ) ) ;
#46256 = EDGE_CURVE ( 'NONE', #30690, #41008, #27714, .T. ) ;
#46257 = CARTESIAN_POINT ( 'NONE',  ( 4.458734124999999437, 20.18750000136559208, -5.460374474430324690E-16 ) ) ;
#46258 = CARTESIAN_POINT ( 'NONE',  ( -2.500000000000000444, -94.16666666666665719, -4.330127018922193649 ) ) ;
#46259 = CARTESIAN_POINT ( 'NONE',  ( 2.499999999999998668, 1.666666666666666963, -4.330127018922193649 ) ) ;
#46260 = CARTESIAN_POINT ( 'NONE',  ( -3.152548672688508926E-16, -77.81249999863440792, -5.148502694627439702 ) ) ;
#46261 = CARTESIAN_POINT ( 'NONE',  ( -4.999999999999999112, -63.91666666666666430, 2.886751345948131764 ) ) ;
#46262 = CARTESIAN_POINT ( 'NONE',  ( 5.000000000000000000, -72.29166666393548724, -2.886751345948130876 ) ) ;
#46263 = CARTESIAN_POINT ( 'NONE',  ( 5.000000000000000000, 20.70833333606451632, -2.886751345948129988 ) ) ;
#46264 = VERTEX_POINT ( 'NONE', #1793 ) ;
#46265 = CARTESIAN_POINT ( 'NONE',  ( -2.499999999999996447, -65.83333333333332860, 4.330127018922195425 ) ) ;
#46266 = B_SPLINE_CURVE_WITH_KNOTS ( 'NONE', 3,
 ( #19106, #38723, #5598, #25214, #53533, #44826 ),
 .UNSPECIFIED., .F., .F.,
 ( 4, 2, 4 ),
 ( 2.475503369227215526E-07, 0.002222330217055624568, 0.004444412883774326306 ),
 .UNSPECIFIED. ) ;
#46267 = CARTESIAN_POINT ( 'NONE',  ( -5.000000000000000000, 8.916666666666666075, -2.886751345948128211 ) ) ;
#46269 = CARTESIAN_POINT ( 'NONE',  ( -4.999999999999999112, -23.91666666666667140, 2.886751345948131764 ) ) ;
#46268 = CARTESIAN_POINT ( 'NONE',  ( -6.972266317189433020E-16, -14.12499999726881228, -5.000000000000000000 ) ) ;
#46270 = CARTESIAN_POINT ( 'NONE',  ( -4.458734124999998549, -28.22916666530106866, 2.574251347313722516 ) ) ;
#46271 = CARTESIAN_POINT ( 'NONE',  ( -4.458734124999997661, -86.22916666530107932, 2.574251347313722516 ) ) ;
#46272 = CARTESIAN_POINT ( 'NONE',  ( 1.060575238724906964E-15, -27.62499999726881228, 5.773502691896257311 ) ) ;
#46274 = ORIENTED_EDGE ( 'NONE', *, *, #21206, .T. ) ;
#46273 = CARTESIAN_POINT ( 'NONE',  ( 4.458734124999998549, -56.72916666530107932, -2.574251347313721627 ) ) ;
#46275 = CARTESIAN_POINT ( 'NONE',  ( 6.123233995736766282E-16, -170.0000000000000000, -5.000000000000000000 ) ) ;
#46276 = CARTESIAN_POINT ( 'NONE',  ( 2.499999999999998668, -62.20833333060214443, -4.330127018922193649 ) ) ;
#46278 = ORIENTED_EDGE ( 'NONE', *, *, #19163, .F. ) ;
#46277 = CARTESIAN_POINT ( 'NONE',  ( 4.458734124999998549, -5.979166665301073103, -2.574251347313721627 ) ) ;
#46279 = CARTESIAN_POINT ( 'NONE',  ( -2.500000000000000444, -72.16666666666667140, -4.330127018922193649 ) ) ;
#46280 = CARTESIAN_POINT ( 'NONE',  ( -54.64476657466781973, -136.8125000013656063, -4.444560631937228834 ) ) ;
#46281 = AXIS2_PLACEMENT_3D ( 'NONE', #360, #24161, #6700 ) ;
#46282 = CARTESIAN_POINT ( 'NONE',  ( 4.458734124999999437, -53.06249999863440792, -5.460374474430324690E-16 ) ) ;
#46283 =( BOUNDED_CURVE ( )  B_SPLINE_CURVE ( 2, ( #21001, #44471, #10707, #25823, #755, #429, #20035, #40294, #59932 ),
 .UNSPECIFIED., .F., .F. ) 
 B_SPLINE_CURVE_WITH_KNOTS ( ( 3, 2, 2, 2, 3 ),
 ( 0.8937500000000000444, 0.8944444444444444864, 0.8958333333333333703, 0.8972222222222222543, 0.8979166666666666963 ),
 .UNSPECIFIED. ) 
 CURVE ( )  GEOMETRIC_REPRESENTATION_ITEM ( )  RATIONAL_B_SPLINE_CURVE ( ( 0.9330127018922194093, 0.9330127018922194093, 1.000000000000000000, 0.8660254037844387076, 1.000000000000000000, 0.8660254037844387076, 1.000000000000000000, 0.9330127018922194093, 0.9330127018922194093 ) ) 
 REPRESENTATION_ITEM ( '' )  );
#46284 = CARTESIAN_POINT ( 'NONE',  ( 5.000000000000000000, -69.37499999726880162, -6.123233995736766282E-16 ) ) ;
#46285 = CARTESIAN_POINT ( 'NONE',  ( 1.975475456537005874E-15, -35.75000000000000711, 5.000000000000000000 ) ) ;
#46286 = AXIS2_PLACEMENT_3D ( 'NONE', #51499, #37960, #17711 ) ;
#46287 = CARTESIAN_POINT ( 'NONE',  ( -51.19402409849444524, -152.5000000000000284, -3.242614290531456334 ) ) ;
#46288 = CARTESIAN_POINT ( 'NONE',  ( -4.458734124999999437, -15.56249999863440436, 0.000000000000000000 ) ) ;
#46289 = CARTESIAN_POINT ( 'NONE',  ( -3.152548672688508926E-16, -53.81249999863439371, -5.148502694627439702 ) ) ;
#46290 = CARTESIAN_POINT ( 'NONE',  ( -6.972266317189433020E-16, 0.7499999999999996669, -5.000000000000000000 ) ) ;
#46291 = FILL_AREA_STYLE_COLOUR ( '', #59555 ) ;
#46292 = CARTESIAN_POINT ( 'NONE',  ( 4.458734124999999437, -140.5000000013656347, 1.846868145590737864 ) ) ;
#46293 = CARTESIAN_POINT ( 'NONE',  ( 2.229367062500001939, -96.22916666530105090, 3.861377020970579999 ) ) ;
#46294 = FACE_OUTER_BOUND ( 'NONE', #21339, .T. ) ;
#46295 = ORIENTED_EDGE ( 'NONE', *, *, #25268, .F. ) ;
#46296 = CARTESIAN_POINT ( 'NONE',  ( -2.071067811865644259, -155.6875000000000000, -4.999999999999831246 ) ) ;
#46297 = CARTESIAN_POINT ( 'NONE',  ( 9.457646018065525792E-16, 23.68750000136559564, 5.148502694627439702 ) ) ;
#46298 = CARTESIAN_POINT ( 'NONE',  ( -49.85088928181150436, -146.6875000027312126, -1.666127454062680702 ) ) ;
#46299 = DIRECTION ( 'NONE',  ( 0.000000000000000000, 0.000000000000000000, 1.000000000000000000 ) ) ;
#46300 = CARTESIAN_POINT ( 'NONE',  ( 4.458734125000001214, -2.895833331967738289, 2.574251347313718519 ) ) ;
#46301 = CARTESIAN_POINT ( 'NONE',  ( -4.458734124999999437, -97.56249999863440792, 0.000000000000000000 ) ) ;
#46302 = CARTESIAN_POINT ( 'NONE',  ( 1.846868145590735200, -148.5000000013656347, -4.458734125000000326 ) ) ;
#46303 = B_SPLINE_CURVE_WITH_KNOTS ( 'NONE', 3,
 ( #15916, #10444, #35537, #45499, #15601, #60313, #10769, #26201, #21708 ),
 .UNSPECIFIED., .F., .F.,
 ( 4, 2, 1, 2, 4 ),
 ( 0.000000000000000000, 0.002165063509461097498, 0.004330127018922194995, 0.006495190528383292493, 0.008660254037844389990 ),
 .UNSPECIFIED. ) ;
#46304 = CARTESIAN_POINT ( 'NONE',  ( 9.457646018065525792E-16, -22.31249999863440792, 5.148502694627439702 ) ) ;
#46305 = DIRECTION ( 'NONE',  ( 0.000000000000000000, 0.000000000000000000, 1.000000000000000000 ) ) ;
#46306 = CARTESIAN_POINT ( 'NONE',  ( 2.229367062500001939, -65.22916666530106511, 3.861377020970579999 ) ) ;
#46307 = CARTESIAN_POINT ( 'NONE',  ( 7.500000000000001776, 4.330127018922190985, -7.564338275809324941 ) ) ;
#46308 = CARTESIAN_POINT ( 'NONE',  ( 2.499999999999998668, 23.79166666939785202, -4.330127018922193649 ) ) ;
#46309 = CARTESIAN_POINT ( 'NONE',  ( -1.846868145590737420, -145.7500000013656063, 4.458734124999997661 ) ) ;
#46310 = CARTESIAN_POINT ( 'NONE',  ( 9.457646018065525792E-16, 15.68750000136559564, 5.148502694627439702 ) ) ;
#46311 = ORIENTED_EDGE ( 'NONE', *, *, #22893, .F. ) ;
#46312 = CARTESIAN_POINT ( 'NONE',  ( 1.975475456537005874E-15, -48.74999999999999289, 5.000000000000000000 ) ) ;
#46313 = CARTESIAN_POINT ( 'NONE',  ( 1.339745962155612702, 16.70534180126147916, -5.000000000000000000 ) ) ;
#46315 = CARTESIAN_POINT ( 'NONE',  ( -3.152548672688508926E-16, -20.56249999863440081, -5.148502694627439702 ) ) ;
#46314 = CARTESIAN_POINT ( 'NONE',  ( -2.500000000000000444, -85.16666666666667140, -4.330127018922193649 ) ) ;
#46316 = CARTESIAN_POINT ( 'NONE',  ( 4.458734124999999437, 26.93750000136559564, -5.460374474430324690E-16 ) ) ;
#46317 = CARTESIAN_POINT ( 'NONE',  ( 1.975475456537005874E-15, 1.375000002731185500, 5.000000000000000000 ) ) ;
#46318 = CARTESIAN_POINT ( 'NONE',  ( -53.51423613279429503, -144.2500000013656063, 4.591703134518082763 ) ) ;
#46319 = CARTESIAN_POINT ( 'NONE',  ( 5.000000000000000000, -48.29166666393547303, -2.886751345948129988 ) ) ;
#46320 = CARTESIAN_POINT ( 'NONE',  ( 2.229367062500001939, 10.02083333469892779, 3.861377020970579999 ) ) ;
#46321 = DIRECTION ( 'NONE',  ( -0.000000000000000000, 1.000000000000000000, -0.000000000000000000 ) ) ;
#46322 = CARTESIAN_POINT ( 'NONE',  ( 1.339745962155624914, 21.70534180126147561, -4.999999999999991118 ) ) ;
#46323 = CARTESIAN_POINT ( 'NONE',  ( -4.458734124999999437, 10.60416666803225993, -2.574251347313719407 ) ) ;
#46324 = CARTESIAN_POINT ( 'NONE',  ( 2.229367062500001939, -67.97916666530106511, 3.861377020970579999 ) ) ;
#46325 = CARTESIAN_POINT ( 'NONE',  ( -4.458734124999997661, -19.47916666530107221, 2.574251347313722516 ) ) ;
#46326 = CARTESIAN_POINT ( 'NONE',  ( -5.000000000000000000, -2.083333333333333037, -2.886751345948128211 ) ) ;
#46327 = CARTESIAN_POINT ( 'NONE',  ( -3.152801135295367985, -161.8125000013656063, 3.152801135295367096 ) ) ;
#46328 = CARTESIAN_POINT ( 'NONE',  ( -6.972266317189433020E-16, -58.24999999999999289, -5.000000000000000000 ) ) ;
#46329 = VECTOR ( 'NONE', #10412, 1000.000000000000000 ) ;
#46330 = CARTESIAN_POINT ( 'NONE',  ( 2.229367062500001939, -57.97916666530107932, 3.861377020970579999 ) ) ;
#46331 = CARTESIAN_POINT ( 'NONE',  ( 1.060575238724906964E-15, -93.62499999726880162, 5.773502691896257311 ) ) ;
#46332 = EDGE_CURVE ( 'NONE', #29366, #60851, #57944, .T. ) ;
#46333 = CARTESIAN_POINT ( 'NONE',  ( 6.123233995736766282E-16, -170.0000000000000000, -5.000000000000000000 ) ) ;
#46334 = CARTESIAN_POINT ( 'NONE',  ( -6.972266317189433020E-16, 4.875000002731184168, -5.000000000000000000 ) ) ;
#46335 = CARTESIAN_POINT ( 'NONE',  ( 2.229367062499998831, -33.64583333196772941, -3.861377020970580887 ) ) ;
#46336 = CARTESIAN_POINT ( 'NONE',  ( 4.330127018922258486, 45.00000000000000000, 7.499999999999910294 ) ) ;
#46337 = CARTESIAN_POINT ( 'NONE',  ( -5.000000000000000000, -50.00000000000000000, 0.000000000000000000 ) ) ;
#46338 = CARTESIAN_POINT ( 'NONE',  ( -1.339745962155610925, -13.79465819873852261, 5.000000000000000000 ) ) ;
#46339 = CARTESIAN_POINT ( 'NONE',  ( 5.000000000000000000, -68.29166666393547303, -2.886751345948130876 ) ) ;
#46340 = ORIENTED_EDGE ( 'NONE', *, *, #32613, .F. ) ;
#46341 = CARTESIAN_POINT ( 'NONE',  ( -4.458734124999999437, -109.3958333319677507, -2.574251347313719407 ) ) ;
#46342 = CARTESIAN_POINT ( 'NONE',  ( 4.458734124999999437, -1.062499998634405696, -5.460374474430324690E-16 ) ) ;
#46343 = CARTESIAN_POINT ( 'NONE',  ( -5.000000000000000000, -99.87499999726881583, 0.000000000000000000 ) ) ;
#46344 = CARTESIAN_POINT ( 'NONE',  ( -5.000000000000000000, -9.083333333333333925, -2.886751345948128211 ) ) ;
#46345 = CARTESIAN_POINT ( 'NONE',  ( 4.458734125000000326, -72.89583333196775072, 2.574251347313718519 ) ) ;
#46346 = CARTESIAN_POINT ( 'NONE',  ( -1.339745962155613812, -26.20534180126147916, -5.000000000000000000 ) ) ;
#46347 = EDGE_CURVE ( 'NONE', #22715, #1445, #8424, .T. ) ;
#46348 = CARTESIAN_POINT ( 'NONE',  ( -3.535250795749689387E-16, -7.124999997268813168, -5.773502691896257311 ) ) ;
#46350 = ORIENTED_EDGE ( 'NONE', *, *, #54650, .T. ) ;
#46349 = CARTESIAN_POINT ( 'NONE',  ( -4.458734124999998549, -37.22916666530107221, 2.574251347313722516 ) ) ;
#46351 = DIRECTION ( 'NONE',  ( 0.000000000000000000, -1.000000000000000000, 0.000000000000000000 ) ) ;
#46352 = ADVANCED_FACE ( 'NONE', ( #32862 ), #47648, .T. ) ;
#46354 = VERTEX_POINT ( 'NONE', #28027 ) ;
#46353 = CARTESIAN_POINT ( 'NONE',  ( -4.458734124999999437, 14.43750000136559386, 0.000000000000000000 ) ) ;
#46355 = DIRECTION ( 'NONE',  ( -0.000000000000000000, 1.000000000000000000, -0.000000000000000000 ) ) ;
#46356 = CARTESIAN_POINT ( 'NONE',  ( -5.000000000000000000, -56.99999999999999289, 0.000000000000000000 ) ) ;
#46357 = CARTESIAN_POINT ( 'NONE',  ( 3.152801135295367541, -161.5625000013656063, -3.152801135295367541 ) ) ;
#46358 = CARTESIAN_POINT ( 'NONE',  ( 4.458734125000001214, -32.14583333196773651, 2.574251347313718519 ) ) ;
#46359 = LINE ( 'NONE', #2619, #50178 ) ;
#46360 = CARTESIAN_POINT ( 'NONE',  ( -4.458734124999999437, -80.31249999863440792, 0.000000000000000000 ) ) ;
#46361 = CARTESIAN_POINT ( 'NONE',  ( -4.458734125000001214, -141.1250000013655779, 1.846868145590734089 ) ) ;
#46362 = CARTESIAN_POINT ( 'NONE',  ( -2.229367062500000163, -85.47916666530107932, -3.861377020970580443 ) ) ;
#46363 = CARTESIAN_POINT ( 'NONE',  ( -53.51423613279429503, -135.5000000013656063, 4.591703134518082763 ) ) ;
#46365 = ADVANCED_FACE ( 'NONE', ( #37066 ), #13862, .T. ) ;
#46364 =( BOUNDED_CURVE ( )  B_SPLINE_CURVE ( 2, ( #40672, #50651, #41615, #1465, #25886, #16872, #21067, #16557, #35864 ),
 .UNSPECIFIED., .F., .F. ) 
 B_SPLINE_CURVE_WITH_KNOTS ( ( 3, 2, 2, 2, 3 ),
 ( 0.4770833333333333592, 0.4777777777777778012, 0.4791666666666666852, 0.4805555555555555691, 0.4812500000000000111 ),
 .UNSPECIFIED. ) 
 CURVE ( )  GEOMETRIC_REPRESENTATION_ITEM ( )  RATIONAL_B_SPLINE_CURVE ( ( 0.9330127018922194093, 0.9330127018922220739, 1.000000000000000000, 0.8660254037844387076, 1.000000000000000000, 0.8660254037844387076, 1.000000000000000000, 0.9330127018922194093, 0.9330127018922194093 ) ) 
 REPRESENTATION_ITEM ( '' )  );
#46366 = CARTESIAN_POINT ( 'NONE',  ( 9.457646018065525792E-16, -33.31249999863440792, 5.148502694627439702 ) ) ;
#46367 = CARTESIAN_POINT ( 'NONE',  ( -5.000000000000000000, 24.12500000273118417, 0.000000000000000000 ) ) ;
#46368 = EDGE_LOOP ( 'NONE', ( #55507, #28968, #10362, #38420 ) ) ;
#46369 = CARTESIAN_POINT ( 'NONE',  ( -2.229367062499996610, -77.39583333196773651, 3.861377020970582219 ) ) ;
#46370 = CARTESIAN_POINT ( 'NONE',  ( -1.339745962155613812, 15.91965820146970501, -5.000000000000000000 ) ) ;
#46371 = ORIENTED_EDGE ( 'NONE', *, *, #16560, .T. ) ;
#46372 = CARTESIAN_POINT ( 'NONE',  ( -4.999999999999998224, -3.791666663935478798, 2.886751345948131764 ) ) ;
#46374 = AXIS2_PLACEMENT_3D ( 'NONE', #18831, #4062, #33636 ) ;
#46373 = LINE ( 'NONE', #42171, #6537 ) ;
#46375 = CARTESIAN_POINT ( 'NONE',  ( -2.229367062499996610, -64.39583333196773651, 3.861377020970582219 ) ) ;
#46376 = CARTESIAN_POINT ( 'NONE',  ( -2.229367062499996610, -8.395833331967736513, 3.861377020970582219 ) ) ;
#46377 = ORIENTED_EDGE ( 'NONE', *, *, #31726, .F. ) ;
#46378 = CARTESIAN_POINT ( 'NONE',  ( 0.000000000000000000, -170.0000000000000000, 0.000000000000000000 ) ) ;
#46379 =( BOUNDED_CURVE ( )  B_SPLINE_CURVE ( 2, ( #12066, #41969, #37471, #46803, #27495, #31691, #61292, #52270, #17214 ),
 .UNSPECIFIED., .F., .F. ) 
 B_SPLINE_CURVE_WITH_KNOTS ( ( 3, 2, 2, 2, 3 ),
 ( 0.1270833333333333259, 0.1277777777777777679, 0.1291666666666666796, 0.1305555555555555636, 0.1312500000000000056 ),
 .UNSPECIFIED. ) 
 CURVE ( )  GEOMETRIC_REPRESENTATION_ITEM ( )  RATIONAL_B_SPLINE_CURVE ( ( 0.9330127018922194093, 0.9330127018922194093, 1.000000000000000000, 0.8660254037844387076, 1.000000000000000000, 0.8660254037844387076, 1.000000000000000000, 0.9330127018922194093, 0.9330127018922194093 ) ) 
 REPRESENTATION_ITEM ( '' )  );
#46380 = CARTESIAN_POINT ( 'NONE',  ( -2.500000000000000444, 2.958333336064520314, -4.330127018922193649 ) ) ;
#46381 = EDGE_CURVE ( 'NONE', #51908, #18523, #47342, .T. ) ;
#46382 = CARTESIAN_POINT ( 'NONE',  ( -2.229367062499996610, -8.395833331967736513, 3.861377020970582219 ) ) ;
#46383 = DIRECTION ( 'NONE',  ( -0.000000000000000000, 1.000000000000000000, -0.000000000000000000 ) ) ;
#46384 = CARTESIAN_POINT ( 'NONE',  ( -3.152548672688508926E-16, 10.43750000136559386, -5.148502694627439702 ) ) ;
#46385 = CARTESIAN_POINT ( 'NONE',  ( -1.339745962155610925, -32.66965819600733312, 5.000000000000000000 ) ) ;
#46386 = CARTESIAN_POINT ( 'NONE',  ( -3.152801135295367985, -156.8125000013656063, 3.152801135295367096 ) ) ;
#46387 = CARTESIAN_POINT ( 'NONE',  ( 3.061616997868383141E-16, -145.7500000000000284, -5.000000000000000000 ) ) ;
#46388 = ORIENTED_EDGE ( 'NONE', *, *, #53014, .T. ) ;
#46389 = CARTESIAN_POINT ( 'NONE',  ( 4.458734124999998549, -86.72916666530107932, -2.574251347313721627 ) ) ;
#46390 = LINE ( 'NONE', #39952, #49019 ) ;
#46391 = CARTESIAN_POINT ( 'NONE',  ( 9.457646018065525792E-16, -1.062499998634405696, 5.148502694627439702 ) ) ;
#46392 = DIRECTION ( 'NONE',  ( -0.000000000000000000, 1.000000000000000000, -0.000000000000000000 ) ) ;
#46393 = CARTESIAN_POINT ( 'NONE',  ( 5.000000000000000000, -31.37499999726880873, -6.123233995736766282E-16 ) ) ;
#46394 = CARTESIAN_POINT ( 'NONE',  ( 2.500000000000002220, -78.66666666666665719, 4.330127018922192761 ) ) ;
#46395 = CARTESIAN_POINT ( 'NONE',  ( 9.457646018065525792E-16, 22.93750000136559919, 5.148502694627439702 ) ) ;
#46396 = CARTESIAN_POINT ( 'NONE',  ( -4.458734124999999437, 28.60416666803226349, -2.574251347313719407 ) ) ;
#46397 = CARTESIAN_POINT ( 'NONE',  ( 9.457646018065525792E-16, -51.06249999863440792, 5.148502694627439702 ) ) ;
#46398 = CARTESIAN_POINT ( 'NONE',  ( -2.229367062499996610, -39.39583333196773651, 3.861377020970582219 ) ) ;
#46399 = CARTESIAN_POINT ( 'NONE',  ( 9.457646018065525792E-16, -0.3124999986344051961, 5.148502694627439702 ) ) ;
#46400 = CARTESIAN_POINT ( 'NONE',  ( 0.000000000000000000, 0.000000000000000000, -25.03750572909317285 ) ) ;
#46401 = CARTESIAN_POINT ( 'NONE',  ( -4.999999999999999112, 15.08333333333333215, 2.886751345948131764 ) ) ;
#46402 = CARTESIAN_POINT ( 'NONE',  ( -5.000000000000000888, -144.6875000027311842, -2.071067811865475949 ) ) ;
#46403 = FACE_OUTER_BOUND ( 'NONE', #60051, .T. ) ;
#46404 = CARTESIAN_POINT ( 'NONE',  ( -4.458734124999999437, -45.39583333196773651, -2.574251347313719407 ) ) ;
#46405 = CARTESIAN_POINT ( 'NONE',  ( 1.060575238724906964E-15, -80.62499999726881583, 5.773502691896257311 ) ) ;
#46406 = EDGE_CURVE ( 'NONE', #39890, #1596, #13967, .T. ) ;
#46407 = CARTESIAN_POINT ( 'NONE',  ( -57.89159099828107458, -139.9375000013656063, -3.393966926194107447 ) ) ;
#46408 = CARTESIAN_POINT ( 'NONE',  ( 5.000000000000000000, -65.37499999726881583, -6.123233995736766282E-16 ) ) ;
#46409 = EDGE_CURVE ( 'NONE', #30399, #58407, #20047, .T. ) ;
#46410 = EDGE_CURVE ( 'NONE', #12181, #18978, #24464, .T. ) ;
#46411 = CARTESIAN_POINT ( 'NONE',  ( 9.457646018065525792E-16, -83.31249999863440792, 5.148502694627439702 ) ) ;
#46412 = CARTESIAN_POINT ( 'NONE',  ( 4.458734124999997661, -161.7500000013655779, 1.846868145590737864 ) ) ;
#46413 = CARTESIAN_POINT ( 'NONE',  ( 1.339745962155615144, 13.41965820146970501, 4.999999999999999112 ) ) ;
#46414 = CARTESIAN_POINT ( 'NONE',  ( 5.000000000000000000, -33.41666666666666430, -2.886751345948129988 ) ) ;
#46415 = DIRECTION ( 'NONE',  ( 0.000000000000000000, 1.000000000000000000, 0.000000000000000000 ) ) ;
#46416 = VERTEX_POINT ( 'NONE', #44707 ) ;
#46417 = CARTESIAN_POINT ( 'NONE',  ( 2.229367062499998831, 21.10416666803226349, -3.861377020970580887 ) ) ;
#46418 = ORIENTED_EDGE ( 'NONE', *, *, #33149, .F. ) ;
#46419 = CARTESIAN_POINT ( 'NONE',  ( 4.458734124999998549, -90.72916666530106511, -2.574251347313721627 ) ) ;
#46420 = CARTESIAN_POINT ( 'NONE',  ( -2.229367062500000163, 11.27083333469892601, -3.861377020970580443 ) ) ;
#46421 = CARTESIAN_POINT ( 'NONE',  ( -2.499999999999996447, 14.29166666939785202, 4.330127018922195425 ) ) ;
#46422 = CARTESIAN_POINT ( 'NONE',  ( -5.000000000000000000, -43.95833333060214443, -2.886751345948128211 ) ) ;
#46423 = CARTESIAN_POINT ( 'NONE',  ( 2.499999999999998668, 6.666666666666667851, -4.330127018922193649 ) ) ;
#46424 = EDGE_CURVE ( 'NONE', #42274, #28232, #4829, .T. ) ;
#46425 = CARTESIAN_POINT ( 'NONE',  ( 4.458734124999998549, -55.72916666530107221, -2.574251347313721627 ) ) ;
#46426 = CARTESIAN_POINT ( 'NONE',  ( 5.000000000000000000, -6.416666666666667851, -2.886751345948130876 ) ) ;
#46427 = CARTESIAN_POINT ( 'NONE',  ( -50.40829686548195099, -135.2500000013656347, -1.485763867205728284 ) ) ;
#46428 = CARTESIAN_POINT ( 'NONE',  ( 0.000000000000000000, -120.0000000000000000, 0.000000000000000000 ) ) ;
#46429 = CARTESIAN_POINT ( 'NONE',  ( 2.500000000000002220, -33.54166666393547303, 4.330127018922192761 ) ) ;
#46430 = ADVANCED_FACE ( 'NONE', ( #9043 ), #23840, .T. ) ;
#46431 = LINE ( 'NONE', #17787, #14484 ) ;
#46432 = CARTESIAN_POINT ( 'NONE',  ( 2.499999999999998668, -42.33333333333333570, -4.330127018922193649 ) ) ;
#46433 = CARTESIAN_POINT ( 'NONE',  ( 1.975475456537005874E-15, -50.62499999726881583, 5.000000000000000000 ) ) ;
#46436 = CARTESIAN_POINT ( 'NONE',  ( -4.458734124999999437, -14.64583333196773474, -2.574251347313719407 ) ) ;
#46435 =( BOUNDED_CURVE ( )  B_SPLINE_CURVE ( 2, ( #57888, #19260, #15080, #62719, #58191, #43391, #10257, #29858, #4174 ),
 .UNSPECIFIED., .F., .F. ) 
 B_SPLINE_CURVE_WITH_KNOTS ( ( 3, 2, 2, 2, 3 ),
 ( 0.7895833333333333037, 0.7902777777777777457, 0.7916666666666666297, 0.7930555555555555136, 0.7937499999999999556 ),
 .UNSPECIFIED. ) 
 CURVE ( )  GEOMETRIC_REPRESENTATION_ITEM ( )  RATIONAL_B_SPLINE_CURVE ( ( 0.9330127018922194093, 0.9330127018922194093, 1.000000000000000000, 0.8660254037844387076, 1.000000000000000000, 0.8660254037844387076, 1.000000000000000000, 0.9330127018922194093, 0.9330127018922194093 ) ) 
 REPRESENTATION_ITEM ( '' )  );
#46434 = CARTESIAN_POINT ( 'NONE',  ( -58.24261429053147765, -139.2500000000000000, -3.805975901505573855 ) ) ;
#46437 = CARTESIAN_POINT ( 'NONE',  ( -8.285706625453232893E-17, -8.895730773063887042, -7.917997657324732153 ) ) ;
#46438 = CARTESIAN_POINT ( 'NONE',  ( -4.458734124999999437, -57.31249999863440081, 0.000000000000000000 ) ) ;
#46439 = CARTESIAN_POINT ( 'NONE',  ( -8.190561711645485556E-16, -153.9375000013655779, 4.458734124999999437 ) ) ;
#46440 = CARTESIAN_POINT ( 'NONE',  ( 9.457646018065525792E-16, -73.06249999863440792, 5.148502694627439702 ) ) ;
#46441 = CARTESIAN_POINT ( 'NONE',  ( -50.55543936806279248, -145.3125000013656063, 0.3552334253322060320 ) ) ;
#46442 = CARTESIAN_POINT ( 'NONE',  ( 4.458734125000001214, -21.14583333196774362, 2.574251347313718519 ) ) ;
#46443 = CARTESIAN_POINT ( 'NONE',  ( 5.000000000000000000, -58.37499999726880873, -6.123233995736766282E-16 ) ) ;
#46444 = ORIENTED_EDGE ( 'NONE', *, *, #19304, .T. ) ;
#46445 = LINE ( 'NONE', #56097, #57999 ) ;
#46446 = ORIENTED_EDGE ( 'NONE', *, *, #518, .F. ) ;
#46447 = CARTESIAN_POINT ( 'NONE',  ( -2.229367062500000163, -63.72916666530106511, -3.861377020970580443 ) ) ;
#46449 = CARTESIAN_POINT ( 'NONE',  ( 5.000000000000000888, 11.54166666939785202, 2.886751345948126879 ) ) ;
#46448 = CARTESIAN_POINT ( 'NONE',  ( -55.00000000000002132, -155.0000000000000284, 1.734723475976807094E-15 ) ) ;
#46450 = CARTESIAN_POINT ( 'NONE',  ( 3.152801135295367541, -152.3125000013655779, -3.152801135295367541 ) ) ;
#46451 = VERTEX_POINT ( 'NONE', #44070 ) ;
#46452 = CARTESIAN_POINT ( 'NONE',  ( 6.123233995736766282E-16, -170.0000000000000000, -5.000000000000000000 ) ) ;
#46453 = CARTESIAN_POINT ( 'NONE',  ( -58.80597590150559739, -126.0000000000000284, 3.242614290531460330 ) ) ;
#46454 = CARTESIAN_POINT ( 'NONE',  ( 1.975475456537005874E-15, -77.62499999726881583, 5.000000000000000000 ) ) ;
#46455 = CARTESIAN_POINT ( 'NONE',  ( -2.229367062499996610, -47.39583333196774362, 3.861377020970582219 ) ) ;
#46456 = VERTEX_POINT ( 'NONE', #44389 ) ;
#46457 = CARTESIAN_POINT ( 'NONE',  ( 5.000000000000000888, 11.41666666666666607, 2.886751345948126879 ) ) ;
#46458 = CARTESIAN_POINT ( 'NONE',  ( 2.229367062500001939, 6.020833334698927786, 3.861377020970579999 ) ) ;
#46459 = CARTESIAN_POINT ( 'NONE',  ( 4.458734124999998549, 26.27083333469893134, -2.574251347313721627 ) ) ;
#46460 = CARTESIAN_POINT ( 'NONE',  ( -57.19623071787017210, -150.3750000013656063, 4.297418129356382899 ) ) ;
#46461 = CARTESIAN_POINT ( 'NONE',  ( -2.499999999999996447, -23.70833333060214443, 4.330127018922195425 ) ) ;
#46462 = CARTESIAN_POINT ( 'NONE',  ( 2.730187237215162345E-16, -167.1875000013655779, -4.458734124999999437 ) ) ;
#46463 = ORIENTED_EDGE ( 'NONE', *, *, #35884, .F. ) ;
#46464 = CARTESIAN_POINT ( 'NONE',  ( -4.458734124999997661, -70.22916666530107932, 2.574251347313722516 ) ) ;
#46465 = CARTESIAN_POINT ( 'NONE',  ( 4.458734125000001214, 14.10416666803225993, 2.574251347313718519 ) ) ;
#46466 = CARTESIAN_POINT ( 'NONE',  ( 2.500000000000002220, -60.54166666393547303, 4.330127018922192761 ) ) ;
#46467 = CARTESIAN_POINT ( 'NONE',  ( -5.000000000000000000, -89.00000000000000000, 0.000000000000000000 ) ) ;
#46468 = CARTESIAN_POINT ( 'NONE',  ( 2.229367062499998831, -55.89583333196773651, -3.861377020970580887 ) ) ;
#46469 = CARTESIAN_POINT ( 'NONE',  ( -2.500000000000000444, -14.04166666393548013, -4.330127018922193649 ) ) ;
#46470 = DIRECTION ( 'NONE',  ( -0.000000000000000000, 1.000000000000000000, -0.000000000000000000 ) ) ;
#46471 = CARTESIAN_POINT ( 'NONE',  ( 3.061616997868383141E-16, -160.7500000000000000, -5.000000000000000000 ) ) ;
#46472 = CARTESIAN_POINT ( 'NONE',  ( 5.000000000000000000, -65.41666666666667140, -2.886751345948130876 ) ) ;
#46473 = CARTESIAN_POINT ( 'NONE',  ( -4.458734124999999437, -20.56249999863440081, 0.000000000000000000 ) ) ;
#46474 = ORIENTED_EDGE ( 'NONE', *, *, #10250, .F. ) ;
#46475 =( BOUNDED_CURVE ( )  B_SPLINE_CURVE ( 2, ( #57430, #58669, #47754, #32973, #29374, #49006, #52903, #33596, #33284 ),
 .UNSPECIFIED., .F., .F. ) 
 B_SPLINE_CURVE_WITH_KNOTS ( ( 3, 2, 2, 2, 3 ),
 ( 0.9895833333333333703, 0.9902777777777778123, 0.9916666666666666963, 0.9930555555555555802, 0.9937500000000000222 ),
 .UNSPECIFIED. ) 
 CURVE ( )  GEOMETRIC_REPRESENTATION_ITEM ( )  RATIONAL_B_SPLINE_CURVE ( ( 0.9330127018922194093, 0.9330127018922194093, 1.000000000000000000, 0.8660254037844387076, 1.000000000000000000, 0.8660254037844387076, 1.000000000000000000, 0.9330127018922194093, 0.9330127018922194093 ) ) 
 REPRESENTATION_ITEM ( '' )  );
#46476 = CARTESIAN_POINT ( 'NONE',  ( -2.499999999999996447, -60.83333333333333570, 4.330127018922195425 ) ) ;
#46477 = CARTESIAN_POINT ( 'NONE',  ( 2.500000000000002220, 29.33333333333333215, 4.330127018922192761 ) ) ;
#46478 = CARTESIAN_POINT ( 'NONE',  ( 2.071067811865475505, -157.9375000027312410, -5.000000000000000888 ) ) ;
#46479 = ORIENTED_EDGE ( 'NONE', *, *, #49152, .T. ) ;
#46480 = CARTESIAN_POINT ( 'NONE',  ( 4.458734125000001214, -101.1458333319677365, 2.574251347313718519 ) ) ;
#46481 = CARTESIAN_POINT ( 'NONE',  ( 2.229367062500001939, -24.97916666530106866, 3.861377020970579999 ) ) ;
#46482 = CARTESIAN_POINT ( 'NONE',  ( -3.535250795749689387E-16, -62.12499999726880873, -5.773502691896257311 ) ) ;
#46483 = CARTESIAN_POINT ( 'NONE',  ( -59.44456063193725015, -150.8125000013656063, -0.3552334253322034230 ) ) ;
#46484 = CARTESIAN_POINT ( 'NONE',  ( -9.184850993605147944E-16, -147.2500000000000284, 5.000000000000000000 ) ) ;
#46485 = EDGE_CURVE ( 'NONE', #24595, #12526, #4226, .T. ) ;
#46486 = CARTESIAN_POINT ( 'NONE',  ( 2.229367062500001939, -23.97916666530107577, 3.861377020970579999 ) ) ;
#46487 = CARTESIAN_POINT ( 'NONE',  ( -2.229367062499996610, -67.39583333196773651, 3.861377020970582219 ) ) ;
#46488 = DIRECTION ( 'NONE',  ( 3.305092117221761110E-15, -0.000000000000000000, 1.000000000000000000 ) ) ;
#46489 = CARTESIAN_POINT ( 'NONE',  ( 4.458734124999998549, -22.72916666530107221, -2.574251347313721627 ) ) ;
#46490 = CARTESIAN_POINT ( 'NONE',  ( -6.972266317189433020E-16, -49.12499999726880162, -5.000000000000000000 ) ) ;
#46491 = CARTESIAN_POINT ( 'NONE',  ( -3.535533905932738641, -152.3750000000000000, 3.535533905932737309 ) ) ;
#46492 = CARTESIAN_POINT ( 'NONE',  ( 5.000000000000000000, -15.50000000000000000, -6.123233995736766282E-16 ) ) ;
#46493 = CARTESIAN_POINT ( 'NONE',  ( -8.190561711645485556E-16, -151.6875000013656063, 4.458734124999999437 ) ) ;
#46494 = EDGE_LOOP ( 'NONE', ( #53162, #20813, #18509, #35313 ) ) ;
#46495 = DIRECTION ( 'NONE',  ( -0.000000000000000000, 1.000000000000000000, -0.000000000000000000 ) ) ;
#46496 = CARTESIAN_POINT ( 'NONE',  ( -4.458734124999999437, -49.56249999863440792, 0.000000000000000000 ) ) ;
#46497 = EDGE_CURVE ( 'NONE', #63218, #43948, #39561, .T. ) ;
#46498 = CARTESIAN_POINT ( 'NONE',  ( -1.339745962155613812, -87.08034179853028434, -5.000000000000000000 ) ) ;
#46499 = CARTESIAN_POINT ( 'NONE',  ( -4.999999999999998224, -110.7916666639354730, 2.886751345948131764 ) ) ;
#46500 = CARTESIAN_POINT ( 'NONE',  ( -3.535250795749689387E-16, 23.75000000000000000, -5.773502691896257311 ) ) ;
#46501 = ADVANCED_FACE ( 'NONE', ( #58565 ), #10304, .T. ) ;
#46502 = EDGE_CURVE ( 'NONE', #46066, #60305, #38213, .T. ) ;
#46503 = CARTESIAN_POINT ( 'NONE',  ( -58.24261429053147765, -152.2500000000000284, -3.805975901505573855 ) ) ;
#46504 = CARTESIAN_POINT ( 'NONE',  ( -2.229367062499996610, 6.854166668032259935, 3.861377020970582219 ) ) ;
#46505 = CARTESIAN_POINT ( 'NONE',  ( -2.071067811865562991, -142.3125000000000000, 4.999999999999913847 ) ) ;
#46506 = CARTESIAN_POINT ( 'NONE',  ( 0.000000000000000000, 0.000000000000000000, -25.03750572909317285 ) ) ;
#46507 = CARTESIAN_POINT ( 'NONE',  ( -2.500000000000000444, -74.16666666666665719, -4.330127018922193649 ) ) ;
#46508 = CARTESIAN_POINT ( 'NONE',  ( 4.458734124999998549, 18.02083333469892779, -2.574251347313721627 ) ) ;
#46509 = CARTESIAN_POINT ( 'NONE',  ( -2.499999999999996447, 5.291666669397853795, 4.330127018922195425 ) ) ;
#46511 = VERTEX_POINT ( 'NONE', #63398 ) ;
#46510 = ADVANCED_FACE ( 'NONE', ( #14486 ), #38611, .T. ) ;
#46512 = CARTESIAN_POINT ( 'NONE',  ( -4.764381983412779477E-15, 26.25000000000000000, 5.000000000000000000 ) ) ;
#46513 = EDGE_LOOP ( 'NONE', ( #61570, #44372, #9717, #5420 ) ) ;
#46514 = CARTESIAN_POINT ( 'NONE',  ( -1.339745962155613812, -71.20534180126148271, -5.000000000000000000 ) ) ;
#46515 = CARTESIAN_POINT ( 'NONE',  ( -4.458734124999999437, -45.31249999863440081, 0.000000000000000000 ) ) ;
#46516 = EDGE_CURVE ( 'NONE', #53481, #40578, #31639, .T. ) ;
#46517 = CARTESIAN_POINT ( 'NONE',  ( 4.458734125000000326, -165.6250000013656063, -1.846868145590734978 ) ) ;
#46518 = EDGE_CURVE ( 'NONE', #44762, #45336, #57936, .T. ) ;
#46519 = CARTESIAN_POINT ( 'NONE',  ( -2.499999999999996447, -43.70833333060214443, 4.330127018922195425 ) ) ;
#46520 = VERTEX_POINT ( 'NONE', #55664 ) ;
#46521 = CARTESIAN_POINT ( 'NONE',  ( -2.229367062499996610, -17.14583333196773651, 3.861377020970582219 ) ) ;
#46522 = ORIENTED_EDGE ( 'NONE', *, *, #26024, .T. ) ;
#46523 = CARTESIAN_POINT ( 'NONE',  ( 5.000000000000000000, -85.49999999999998579, -6.123233995736766282E-16 ) ) ;
#46524 = CARTESIAN_POINT ( 'NONE',  ( 1.846868145590735200, -165.2500000013655779, -4.458734125000000326 ) ) ;
#46526 = ORIENTED_EDGE ( 'NONE', *, *, #45389, .T. ) ;
#46525 = CARTESIAN_POINT ( 'NONE',  ( 5.000000000000000888, -20.45833333060214798, 2.886751345948126879 ) ) ;
#46527 = CARTESIAN_POINT ( 'NONE',  ( -50.18089887299979068, -135.6875000000000000, 2.462841084822635640 ) ) ;
#46528 = CARTESIAN_POINT ( 'NONE',  ( 4.458734125000001214, -32.14583333196773651, 2.574251347313718519 ) ) ;
#46529 = DIRECTION ( 'NONE',  ( 0.000000000000000000, 0.000000000000000000, 1.000000000000000000 ) ) ;
#46530 = ORIENTED_EDGE ( 'NONE', *, *, #11135, .F. ) ;
#46531 = CARTESIAN_POINT ( 'NONE',  ( -4.458734124999999437, -78.31249999863440792, 0.000000000000000000 ) ) ;
#46532 = CARTESIAN_POINT ( 'NONE',  ( 4.458734124999999437, 26.18750000136559564, -5.460374474430324690E-16 ) ) ;
#46533 = CARTESIAN_POINT ( 'NONE',  ( 5.000000000000000000, 24.70833333606452342, -2.886751345948130876 ) ) ;
#46534 = ORIENTED_EDGE ( 'NONE', *, *, #5983, .T. ) ;
#46535 = FACE_OUTER_BOUND ( 'NONE', #6723, .T. ) ;
#46536 = CARTESIAN_POINT ( 'NONE',  ( -51.60603307380591787, -143.1875000013656063, -2.891590998281053704 ) ) ;
#46537 = CARTESIAN_POINT ( 'NONE',  ( -4.458734124999999437, -82.64583333196772230, -2.574251347313719407 ) ) ;
#46538 = CARTESIAN_POINT ( 'NONE',  ( -59.81910112700025905, -132.3125000027312126, -2.462841084822630311 ) ) ;
#46539 = CARTESIAN_POINT ( 'NONE',  ( 5.000000000000000000, 22.58333333333333215, -2.886751345948130876 ) ) ;
#46540 = CARTESIAN_POINT ( 'NONE',  ( -2.499999999999996447, -82.83333333333332860, 4.330127018922195425 ) ) ;
#46541 = CARTESIAN_POINT ( 'NONE',  ( 1.975475456537005874E-15, -84.62499999726880162, 5.000000000000000000 ) ) ;
#46542 = CARTESIAN_POINT ( 'NONE',  ( 2.229367062499998831, -52.64583333196773651, -3.861377020970580887 ) ) ;
#46543 = CARTESIAN_POINT ( 'NONE',  ( -2.229367062500000163, -47.47916666530106511, -3.861377020970580443 ) ) ;
#46544 = CARTESIAN_POINT ( 'NONE',  ( 2.229367062500001939, 26.02083333469892779, 3.861377020970579999 ) ) ;
#46545 = CARTESIAN_POINT ( 'NONE',  ( 2.500000000000002220, -107.6666666666666572, 4.330127018922192761 ) ) ;
#46546 = CARTESIAN_POINT ( 'NONE',  ( 0.000000000000000000, -170.0000000000000000, 0.000000000000000000 ) ) ;
#46547 = CARTESIAN_POINT ( 'NONE',  ( -4.458734124999999437, -36.64583333196773651, -2.574251347313719407 ) ) ;
#46548 = CARTESIAN_POINT ( 'NONE',  ( 5.000000000000000000, -0.3749999972688135008, -6.123233995736766282E-16 ) ) ;
#46549 = CARTESIAN_POINT ( 'NONE',  ( -57.46284108482265651, -153.9375000000000284, 4.819101127000238627 ) ) ;
#46550 = CARTESIAN_POINT ( 'NONE',  ( -59.29741812935640155, -125.6250000013656205, -2.196230717870135685 ) ) ;
#46551 = CARTESIAN_POINT ( 'NONE',  ( -2.229367062500000163, -77.72916666530106511, -3.861377020970580443 ) ) ;
#46552 = CARTESIAN_POINT ( 'NONE',  ( -6.972266317189433020E-16, 5.749999999999999112, -5.000000000000000000 ) ) ;
#46553 = CARTESIAN_POINT ( 'NONE',  ( -2.229367062499996610, -101.1458333319677365, 3.861377020970582219 ) ) ;
#46554 = CARTESIAN_POINT ( 'NONE',  ( 2.229367062499998831, -7.895833331967735624, -3.861377020970580887 ) ) ;
#46555 = ORIENTED_EDGE ( 'NONE', *, *, #26597, .F. ) ;
#46556 = DIRECTION ( 'NONE',  ( 0.000000000000000000, -1.000000000000000000, 0.000000000000000000 ) ) ;
#46557 = CARTESIAN_POINT ( 'NONE',  ( -5.000000000000000000, -35.87499999726881583, 0.000000000000000000 ) ) ;
#46558 = CARTESIAN_POINT ( 'NONE',  ( -4.458734124999999437, -95.31249999863440792, 0.000000000000000000 ) ) ;
#46559 = CARTESIAN_POINT ( 'NONE',  ( -3.535533905932738641, -167.5000000027312126, 3.535533905932737309 ) ) ;
#46560 = CARTESIAN_POINT ( 'NONE',  ( -2.229367062499996610, -89.39583333196773651, 3.861377020970582219 ) ) ;
#46561 = CARTESIAN_POINT ( 'NONE',  ( 2.229367062500001939, 11.77083333469892601, 3.861377020970579999 ) ) ;
#46562 = CARTESIAN_POINT ( 'NONE',  ( 1.975475456537005874E-15, -2.624999997268813168, 5.000000000000000000 ) ) ;
#46563 =( BOUNDED_CURVE ( )  B_SPLINE_CURVE ( 2, ( #21464, #32688, #47476, #18529, #33316, #38445, #22735, #2799, #12751 ),
 .UNSPECIFIED., .F., .F. ) 
 B_SPLINE_CURVE_WITH_KNOTS ( ( 3, 2, 2, 2, 3 ),
 ( 0.7916666666666664076, 0.7958333333333330595, 0.7999999999999998224, 0.8041666666666664742, 0.8083333333333331261 ),
 .UNSPECIFIED. ) 
 CURVE ( )  GEOMETRIC_REPRESENTATION_ITEM ( )  RATIONAL_B_SPLINE_CURVE ( ( 1.000000000000003997, 0.9238795325112826307, 1.000000000000000000, 0.9238795325112867385, 1.000000000000000000, 0.9238795325112867385, 1.000000000000000000, 0.9238795325112908463, 0.9999999999999958922 ) ) 
 REPRESENTATION_ITEM ( '' )  );
#46564 = CARTESIAN_POINT ( 'NONE',  ( -55.35523342533222291, -132.3125000013656063, 4.444560631937231499 ) ) ;
#46565 = CARTESIAN_POINT ( 'NONE',  ( -4.458734124999997661, -6.229166665301072214, 2.574251347313722516 ) ) ;
#46566 = CARTESIAN_POINT ( 'NONE',  ( 2.229367062499998831, 14.10416666803226171, -3.861377020970580887 ) ) ;
#46567 = CARTESIAN_POINT ( 'NONE',  ( 2.229367062499998831, -52.89583333196773651, -3.861377020970580887 ) ) ;
#46568 = CARTESIAN_POINT ( 'NONE',  ( -5.000000000000000000, -13.95833333060214976, -2.886751345948128211 ) ) ;
#46569 = CARTESIAN_POINT ( 'NONE',  ( 5.000000000000000000, 17.50000000000000000, -6.123233995736766282E-16 ) ) ;
#46570 = CARTESIAN_POINT ( 'NONE',  ( -3.152548672688508926E-16, -8.562499998634406140, -5.148502694627439702 ) ) ;
#46571 = DIRECTION ( 'NONE',  ( -0.000000000000000000, 1.000000000000000000, -0.000000000000000000 ) ) ;
#46572 = ORIENTED_EDGE ( 'NONE', *, *, #22458, .T. ) ;
#46573 = CARTESIAN_POINT ( 'NONE',  ( -2.229367062500000163, -34.72916666530107221, -3.861377020970580443 ) ) ;
#46574 = CARTESIAN_POINT ( 'NONE',  ( -50.70258187064364108, -129.3750000013656347, 2.196230717870141014 ) ) ;
#46575 = CARTESIAN_POINT ( 'NONE',  ( -4.458734124999999437, -82.31249999863440792, 0.000000000000000000 ) ) ;
#46576 = CARTESIAN_POINT ( 'NONE',  ( 9.457646018065525792E-16, 24.68750000136559208, 5.148502694627439702 ) ) ;
#46577 = CARTESIAN_POINT ( 'NONE',  ( 2.730187237215162345E-16, -148.4375000013656063, -4.458734124999999437 ) ) ;
#46578 = VECTOR ( 'NONE', #51524, 1000.000000000000000 ) ;
#46579 = CARTESIAN_POINT ( 'NONE',  ( 2.229367062500001939, 23.02083333469892423, 3.861377020970579999 ) ) ;
#46580 = CARTESIAN_POINT ( 'NONE',  ( -1.339745962155613812, -44.08034179853027723, -5.000000000000000000 ) ) ;
#46581 = DIRECTION ( 'NONE',  ( -0.000000000000000000, 1.000000000000000000, -0.000000000000000000 ) ) ;
#46582 = CARTESIAN_POINT ( 'NONE',  ( -2.229367062500000163, -84.72916666530107932, -3.861377020970580443 ) ) ;
#46583 = CARTESIAN_POINT ( 'NONE',  ( -2.500000000000000444, -66.16666666666667140, -4.330127018922193649 ) ) ;
#46584 = CARTESIAN_POINT ( 'NONE',  ( -5.000000000000000000, 21.04166666939785202, -2.886751345948128211 ) ) ;
#46585 = ORIENTED_EDGE ( 'NONE', *, *, #44001, .F. ) ;
#46586 = CARTESIAN_POINT ( 'NONE',  ( 2.500000000000002220, -25.66666666666666430, 4.330127018922192761 ) ) ;
#46587 = CARTESIAN_POINT ( 'NONE',  ( -5.000000000000000000, 27.91666666666666430, -2.886751345948128211 ) ) ;
#46589 = CARTESIAN_POINT ( 'NONE',  ( 5.000000000000000000, -23.50000000000000000, -6.123233995736766282E-16 ) ) ;
#46588 = CYLINDRICAL_SURFACE ( 'NONE', #42927, 5.000000000000000000 ) ;
#46590 = CARTESIAN_POINT ( 'NONE',  ( -2.229367062499996610, -25.14583333196773651, 3.861377020970582219 ) ) ;
#46591 = CARTESIAN_POINT ( 'NONE',  ( -4.458734124999999437, -89.39583333196773651, -2.574251347313719407 ) ) ;
#46592 = CARTESIAN_POINT ( 'NONE',  ( -3.535250795749689387E-16, -31.12499999726881228, -5.773502691896257311 ) ) ;
#46594 = ORIENTED_EDGE ( 'NONE', *, *, #42428, .T. ) ;
#46593 = CARTESIAN_POINT ( 'NONE',  ( 9.457646018065525792E-16, -54.06249999863440081, 5.148502694627439702 ) ) ;
#46595 = CARTESIAN_POINT ( 'NONE',  ( -50.40829686548195099, -153.2500000013655779, -1.485763867205728284 ) ) ;
#46597 = ORIENTED_EDGE ( 'NONE', *, *, #61399, .T. ) ;
#46596 = CARTESIAN_POINT ( 'NONE',  ( -2.229367062500000163, -9.729166665301068662, -3.861377020970580443 ) ) ;
#46598 = CARTESIAN_POINT ( 'NONE',  ( -2.499999999999996447, -71.83333333333332860, 4.330127018922195425 ) ) ;
#46599 = CARTESIAN_POINT ( 'NONE',  ( -57.19623071787016499, -140.3750000013656063, 4.297418129356382899 ) ) ;
#46600 = CARTESIAN_POINT ( 'NONE',  ( 4.458734124999998549, -51.97916666530107221, -2.574251347313721627 ) ) ;
#46601 = DIRECTION ( 'NONE',  ( 0.000000000000000000, 0.000000000000000000, -1.000000000000000000 ) ) ;
#46602 = CARTESIAN_POINT ( 'NONE',  ( 2.500000000000002220, -75.54166666393547303, 4.330127018922192761 ) ) ;
#46603 = CARTESIAN_POINT ( 'NONE',  ( -2.499999999999996447, -53.70833333060213732, 4.330127018922195425 ) ) ;
#46604 = CARTESIAN_POINT ( 'NONE',  ( -60.14911071818854538, -149.0625000000000000, 1.666127454062681368 ) ) ;
#46605 = CARTESIAN_POINT ( 'NONE',  ( 2.229367062500001939, -15.22916666530107399, 3.861377020970579999 ) ) ;
#46606 = CARTESIAN_POINT ( 'NONE',  ( 2.229367062499998831, -50.89583333196772941, -3.861377020970580887 ) ) ;
#46607 = CARTESIAN_POINT ( 'NONE',  ( -2.499999999999996447, -29.70833333060215153, 4.330127018922195425 ) ) ;
#46608 = CARTESIAN_POINT ( 'NONE',  ( -3.152801135295367096, -140.0625000013655779, -3.152801135295367541 ) ) ;
#46609 = CARTESIAN_POINT ( 'NONE',  ( 4.458734124999998549, -100.9791666653010509, -2.574251347313721627 ) ) ;
#46610 = CARTESIAN_POINT ( 'NONE',  ( 1.464175926609780648E-14, 23.87500000273118417, -5.000000000000000000 ) ) ;
#46611 = ORIENTED_EDGE ( 'NONE', *, *, #31176, .F. ) ;
#46612 = CARTESIAN_POINT ( 'NONE',  ( 6.123233995736766282E-16, -120.0000000000000000, -5.000000000000000000 ) ) ;
#46613 = CARTESIAN_POINT ( 'NONE',  ( -53.33387254593733928, -143.9375000027311842, 5.149110718188519620 ) ) ;
#46614 = CARTESIAN_POINT ( 'NONE',  ( 2.499999999999998668, 18.66666666666666430, -4.330127018922193649 ) ) ;
#46615 = CARTESIAN_POINT ( 'NONE',  ( -4.458734124999998549, -0.2291666653010705768, 2.574251347313722516 ) ) ;
#46616 = CARTESIAN_POINT ( 'NONE',  ( -2.229367062499996610, -94.39583333196773651, 3.861377020970582219 ) ) ;
#46617 = VECTOR ( 'NONE', #31574, 1000.000000000000000 ) ;
#46618 = CARTESIAN_POINT ( 'NONE',  ( 4.458734124999999437, -146.7500000013656063, 1.846868145590737864 ) ) ;
#46619 = CARTESIAN_POINT ( 'NONE',  ( 9.457646018065525792E-16, -20.31249999863440081, 5.148502694627439702 ) ) ;
#46620 = CARTESIAN_POINT ( 'NONE',  ( -58.39396692619412477, -136.4375000013655779, 2.891590998281057701 ) ) ;
#46621 = CARTESIAN_POINT ( 'NONE',  ( 2.229367062500001939, -61.22916666530106511, 3.861377020970579999 ) ) ;
#46622 = CARTESIAN_POINT ( 'NONE',  ( -9.184850993605147944E-16, -154.3750000027311842, 5.000000000000000000 ) ) ;
#46623 = CARTESIAN_POINT ( 'NONE',  ( 1.249327701954825010, -8.410337540182549532, -7.776713651265369620 ) ) ;
#46624 = CARTESIAN_POINT ( 'NONE',  ( 4.458734124999997661, -145.5000000013656063, 1.846868145590737864 ) ) ;
#46625 = CARTESIAN_POINT ( 'NONE',  ( -4.458734124999999437, 12.43750000136559564, 0.000000000000000000 ) ) ;
#46626 =( BOUNDED_CURVE ( )  B_SPLINE_CURVE ( 2, ( #44974, #939, #35325, #20858, #40461, #41090, #31766, #16978, #21811 ),
 .UNSPECIFIED., .F., .F. ) 
 B_SPLINE_CURVE_WITH_KNOTS ( ( 3, 2, 2, 2, 3 ),
 ( 0.2946428571428571508, 0.2952380952380952439, 0.2964285714285714302, 0.2976190476190476164, 0.2982142857142857095 ),
 .UNSPECIFIED. ) 
 CURVE ( )  GEOMETRIC_REPRESENTATION_ITEM ( )  RATIONAL_B_SPLINE_CURVE ( ( 0.9330127018922194093, 0.9330127018922194093, 1.000000000000000000, 0.8660254037844387076, 1.000000000000000000, 0.8660254037844387076, 1.000000000000000000, 0.9330127018922194093, 0.9330127018922194093 ) ) 
 REPRESENTATION_ITEM ( '' )  );
#46627 = ORIENTED_EDGE ( 'NONE', *, *, #56157, .F. ) ;
#46628 = CARTESIAN_POINT ( 'NONE',  ( -5.000000000000000000, -52.87499999726881583, 0.000000000000000000 ) ) ;
#46629 = CARTESIAN_POINT ( 'NONE',  ( 5.000000000000000000, 16.58333333333333215, -2.886751345948130876 ) ) ;
#46631 = CARTESIAN_POINT ( 'NONE',  ( -4.458734124999999437, -26.31249999863440792, 0.000000000000000000 ) ) ;
#46630 = CARTESIAN_POINT ( 'NONE',  ( 1.060575238724906964E-15, -89.74999999999998579, 5.773502691896257311 ) ) ;
#46632 = CARTESIAN_POINT ( 'NONE',  ( -2.229367062499996610, -68.39583333196773651, 3.861377020970582219 ) ) ;
#46633 = CARTESIAN_POINT ( 'NONE',  ( -2.229367062500000163, 28.27083333469892779, -3.861377020970580443 ) ) ;
#46634 = CARTESIAN_POINT ( 'NONE',  ( -2.500000000000000444, -18.04166666393547658, -4.330127018922193649 ) ) ;
#46635 = CARTESIAN_POINT ( 'NONE',  ( -50.70258187064364108, -147.1250000013656063, 2.196230717870141014 ) ) ;
#46636 = CARTESIAN_POINT ( 'NONE',  ( -2.499999999999996447, -50.70833333060213732, 4.330127018922195425 ) ) ;
#46637 = CARTESIAN_POINT ( 'NONE',  ( -6.972266317189433020E-16, -24.24999999999999645, -5.000000000000000000 ) ) ;
#46638 = CARTESIAN_POINT ( 'NONE',  ( 2.229367062500001939, 7.020833334698928674, 3.861377020970579999 ) ) ;
#46639 = CARTESIAN_POINT ( 'NONE',  ( 1.975475456537005874E-15, -40.62499999726879452, 5.000000000000000000 ) ) ;
#46640 = CARTESIAN_POINT ( 'NONE',  ( -52.53715891517739323, -141.5625000027312126, -4.819101127000233298 ) ) ;
#46641 = CARTESIAN_POINT ( 'NONE',  ( 4.458734124999998549, 8.270833334698926009, -2.574251347313721627 ) ) ;
#46642 = CARTESIAN_POINT ( 'NONE',  ( 4.458734124999998549, -73.72916666530106511, -2.574251347313721627 ) ) ;
#46643 = CARTESIAN_POINT ( 'NONE',  ( 9.457646018065525792E-16, -18.31249999863440792, 5.148502694627439702 ) ) ;
#46644 = CARTESIAN_POINT ( 'NONE',  ( -2.499999999999996447, -1.833333333333332593, 4.330127018922195425 ) ) ;
#46645 = CARTESIAN_POINT ( 'NONE',  ( 3.152801135295366208, -161.5625000013656063, 3.152801135295367985 ) ) ;
#46646 = CARTESIAN_POINT ( 'NONE',  ( 5.000000000000000000, 15.62500000273118417, -6.123233995736766282E-16 ) ) ;
#46647 = CARTESIAN_POINT ( 'NONE',  ( 2.229367062500001939, -64.97916666530106511, 3.861377020970579999 ) ) ;
#46648 = CARTESIAN_POINT ( 'NONE',  ( -3.535250795749689387E-16, -93.12499999726881583, -5.773502691896257311 ) ) ;
#46649 = CARTESIAN_POINT ( 'NONE',  ( -2.500000000000000444, -89.04166666393547303, -4.330127018922193649 ) ) ;
#46650 = CARTESIAN_POINT ( 'NONE',  ( 4.458734124999999437, -41.81249999863440081, -5.460374474430324690E-16 ) ) ;
#46651 = CARTESIAN_POINT ( 'NONE',  ( 5.000000000000000888, 19.54166666939785202, 2.886751345948126879 ) ) ;
#46652 = CARTESIAN_POINT ( 'NONE',  ( 4.458734125000000326, -66.14583333196773651, 2.574251347313718519 ) ) ;
#46653 = CARTESIAN_POINT ( 'NONE',  ( 5.000000000000000000, -48.41666666666665719, -2.886751345948129988 ) ) ;
#46654 = CARTESIAN_POINT ( 'NONE',  ( -1.339745962155613812, 15.79465819873852261, -5.000000000000000000 ) ) ;
#46655 = ORIENTED_EDGE ( 'NONE', *, *, #3660, .T. ) ;
#46656 = CARTESIAN_POINT ( 'NONE',  ( -5.000000000000000000, -84.99999999999998579, 0.000000000000000000 ) ) ;
#46657 = CARTESIAN_POINT ( 'NONE',  ( 4.458734125000001214, -3.145833331967738733, 2.574251347313718519 ) ) ;
#46658 =( BOUNDED_CURVE ( )  B_SPLINE_CURVE ( 2, ( #21301, #39944, #54761, #54108, #10048, #29661, #10687, #416, #59592 ),
 .UNSPECIFIED., .F., .F. ) 
 B_SPLINE_CURVE_WITH_KNOTS ( ( 3, 2, 2, 2, 3 ),
 ( 0.5339285714285714191, 0.5345238095238095122, 0.5357142857142856984, 0.5369047619047618847, 0.5374999999999999778 ),
 .UNSPECIFIED. ) 
 CURVE ( )  GEOMETRIC_REPRESENTATION_ITEM ( )  RATIONAL_B_SPLINE_CURVE ( ( 0.9330127018922194093, 0.9330127018922194093, 1.000000000000000000, 0.8660254037844387076, 1.000000000000000000, 0.8660254037844387076, 1.000000000000000000, 0.9330127018922194093, 0.9330127018922194093 ) ) 
 REPRESENTATION_ITEM ( '' )  );
#46659 = CARTESIAN_POINT ( 'NONE',  ( -5.000000000000000000, -67.95833333060214443, -2.886751345948128211 ) ) ;
#46660 = CARTESIAN_POINT ( 'NONE',  ( 2.499999999999998668, -7.333333333333330373, -4.330127018922193649 ) ) ;
#46661 = CARTESIAN_POINT ( 'NONE',  ( -4.458734124999999437, -71.31249999863439371, 0.000000000000000000 ) ) ;
#46662 = AXIS2_PLACEMENT_3D ( 'NONE', #28331, #37991, #33474 ) ;
#46663 = CARTESIAN_POINT ( 'NONE',  ( -2.500000000000000444, -5.041666663935480130, -4.330127018922193649 ) ) ;
#46664 = CARTESIAN_POINT ( 'NONE',  ( -4.999999999999999112, -14.79166666393548368, 2.886751345948131764 ) ) ;
#46666 = ORIENTED_EDGE ( 'NONE', *, *, #2429, .F. ) ;
#46665 = CARTESIAN_POINT ( 'NONE',  ( -2.229367062499996610, -40.14583333196773651, 3.861377020970582219 ) ) ;
#46667 = CARTESIAN_POINT ( 'NONE',  ( 2.499999999999998668, -100.2083333306021444, -4.330127018922193649 ) ) ;
#46669 = ORIENTED_EDGE ( 'NONE', *, *, #37851, .T. ) ;
#46668 = CARTESIAN_POINT ( 'NONE',  ( 4.458734124999998549, 10.02083333469892779, -2.574251347313721627 ) ) ;
#46670 = CARTESIAN_POINT ( 'NONE',  ( 5.000000000000000000, -81.37499999726881583, -6.123233995736766282E-16 ) ) ;
#46671 = CARTESIAN_POINT ( 'NONE',  ( -4.999999999999999112, -56.91666666666667140, 2.886751345948131764 ) ) ;
#46672 = CARTESIAN_POINT ( 'NONE',  ( 4.458734125000000326, -160.6250000013655779, -1.846868145590734978 ) ) ;
#46673 = CARTESIAN_POINT ( 'NONE',  ( 4.458734125000001214, -35.14583333196772941, 2.574251347313718519 ) ) ;
#46674 = CARTESIAN_POINT ( 'NONE',  ( 1.975475456537005874E-15, -10.62499999726881228, 5.000000000000000000 ) ) ;
#46675 = CARTESIAN_POINT ( 'NONE',  ( 2.229367062500001939, -79.97916666530106511, 3.861377020970579999 ) ) ;
#46676 = CARTESIAN_POINT ( 'NONE',  ( 5.000000000000000000, -168.0625000000000000, 2.071067811865478614 ) ) ;
#46677 = CARTESIAN_POINT ( 'NONE',  ( 4.458734124999999437, -87.81249999863439371, -5.460374474430324690E-16 ) ) ;
#46678 = CARTESIAN_POINT ( 'NONE',  ( -52.10840900171896806, -132.4375000013656063, 3.393966926194110556 ) ) ;
#46679 = CARTESIAN_POINT ( 'NONE',  ( 4.458734124999999437, -1.062499998634405696, -5.460374474430324690E-16 ) ) ;
#46680 = CARTESIAN_POINT ( 'NONE',  ( -2.229367062499996610, -36.39583333196773651, 3.861377020970582219 ) ) ;
#46681 = CARTESIAN_POINT ( 'NONE',  ( 2.229367062500001939, -83.22916666530106511, 3.861377020970579999 ) ) ;
#46682 = CYLINDRICAL_SURFACE ( 'NONE', #37931, 5.000000000000000000 ) ;
#46683 = ORIENTED_EDGE ( 'NONE', *, *, #33680, .T. ) ;
#46684 = CARTESIAN_POINT ( 'NONE',  ( -9.184850993605147944E-16, -148.3750000027312126, 5.000000000000000000 ) ) ;
#46685 = LINE ( 'NONE', #51830, #55851 ) ;
#46687 = EDGE_CURVE ( 'NONE', #54753, #8786, #35391, .T. ) ;
#46686 = CARTESIAN_POINT ( 'NONE',  ( 2.229367062500001939, -70.22916666530107932, 3.861377020970579999 ) ) ;
#46688 = CARTESIAN_POINT ( 'NONE',  ( 4.458734125000001214, -8.145833331967736513, 2.574251347313718519 ) ) ;
#46689 = VERTEX_POINT ( 'NONE', #45677 ) ;
#46690 = FACE_OUTER_BOUND ( 'NONE', #22188, .T. ) ;
#46691 = CARTESIAN_POINT ( 'NONE',  ( 2.500000000000002220, -3.541666663935478354, 4.330127018922192761 ) ) ;
#46692 = CARTESIAN_POINT ( 'NONE',  ( 4.458734125000001214, -9.145833331967736513, 2.574251347313718519 ) ) ;
#46693 = CARTESIAN_POINT ( 'NONE',  ( -56.66612745406278151, -148.4375000027311842, -5.149110718188523173 ) ) ;
#46694 = CARTESIAN_POINT ( 'NONE',  ( 2.229367062500001939, 0.02083333469892964529, 3.861377020970579999 ) ) ;
#46695 = CARTESIAN_POINT ( 'NONE',  ( 4.458734124999999437, -155.4375000013655779, 0.000000000000000000 ) ) ;
#46696 = CARTESIAN_POINT ( 'NONE',  ( 4.458734125000000326, 27.85416666803225993, 2.574251347313718519 ) ) ;
#46697 = ORIENTED_EDGE ( 'NONE', *, *, #20051, .F. ) ;
#46698 = CARTESIAN_POINT ( 'NONE',  ( 2.229367062499998831, -88.64583333196773651, -3.861377020970580887 ) ) ;
#46699 = CARTESIAN_POINT ( 'NONE',  ( 1.975475456537005874E-15, -67.74999999999998579, 5.000000000000000000 ) ) ;
#46700 = CARTESIAN_POINT ( 'NONE',  ( -2.229367062499996610, -10.14583333196773829, 3.861377020970582219 ) ) ;
#46701 = CARTESIAN_POINT ( 'NONE',  ( 5.000000000000000000, -51.41666666666666430, -2.886751345948130876 ) ) ;
#46702 = AXIS2_PLACEMENT_3D ( 'NONE', #9698, #29305, #48935 ) ;
#46703 = EDGE_CURVE ( 'NONE', #15515, #26615, #50873, .T. ) ;
#46704 = CARTESIAN_POINT ( 'NONE',  ( 3.061616997868383141E-16, -160.7500000000000000, -5.000000000000000000 ) ) ;
#46705 = CARTESIAN_POINT ( 'NONE',  ( -2.500000000000000444, -33.04166666393547303, -4.330127018922193649 ) ) ;
#46706 = EDGE_CURVE ( 'NONE', #45160, #31680, #37715, .T. ) ;
#46707 = FACE_OUTER_BOUND ( 'NONE', #6905, .T. ) ;
#46708 = CARTESIAN_POINT ( 'NONE',  ( -3.152548672688508926E-16, 25.43750000136559208, -5.148502694627439702 ) ) ;
#46709 = CARTESIAN_POINT ( 'NONE',  ( -2.480964764533239819E-13, -94.75000000000000000, 5.000000000000000000 ) ) ;
#46710 = CARTESIAN_POINT ( 'NONE',  ( -4.458734124999999437, 25.60416666803225638, -2.574251347313719407 ) ) ;
#46711 = CARTESIAN_POINT ( 'NONE',  ( 4.458734124999999437, -51.81249999863440792, -5.460374474430324690E-16 ) ) ;
#46712 = CARTESIAN_POINT ( 'NONE',  ( -3.152548672688508926E-16, -4.812499998634402587, -5.148502694627439702 ) ) ;
#46713 = CARTESIAN_POINT ( 'NONE',  ( 5.000000000000000888, -0.4583333306021481479, 2.886751345948126879 ) ) ;
#46714 = CARTESIAN_POINT ( 'NONE',  ( 1.060575238724906964E-15, 14.25000000000000178, 5.773502691896257311 ) ) ;
#46715 = CARTESIAN_POINT ( 'NONE',  ( -5.000000000000000000, -142.6250000027312126, -6.123233995736766282E-16 ) ) ;
#46716 = CYLINDRICAL_SURFACE ( 'NONE', #42827, 5.000000000000000000 ) ;
#46717 = CARTESIAN_POINT ( 'NONE',  ( -3.152548672688508926E-16, -48.56249999863440792, -5.148502694627439702 ) ) ;
#46718 = CARTESIAN_POINT ( 'NONE',  ( -5.000000000000000000, -80.95833333060214443, -2.886751345948128211 ) ) ;
#46719 = CARTESIAN_POINT ( 'NONE',  ( -58.39396692619412477, -139.6875000013656347, 2.891590998281057701 ) ) ;
#46720 = CARTESIAN_POINT ( 'NONE',  ( -2.499999999999996447, -86.83333333333332860, 4.330127018922195425 ) ) ;
#46721 = CARTESIAN_POINT ( 'NONE',  ( 7.908030677224553884, -3.059924800338349904, -7.792662696733364314 ) ) ;
#46722 = CARTESIAN_POINT ( 'NONE',  ( 2.229367062499998831, -85.89583333196773651, -3.861377020970580887 ) ) ;
#46723 = CARTESIAN_POINT ( 'NONE',  ( 3.152801135295367541, -163.5625000013656063, -3.152801135295367541 ) ) ;
#46724 = CARTESIAN_POINT ( 'NONE',  ( -4.999999999999999112, -32.91666666666666430, 2.886751345948131764 ) ) ;
#46725 = CARTESIAN_POINT ( 'NONE',  ( -5.000000000000000000, 24.00000000000000000, 0.000000000000000000 ) ) ;
#46726 = EDGE_LOOP ( 'NONE', ( #43083, #41214, #41531, #1136 ) ) ;
#46727 = CARTESIAN_POINT ( 'NONE',  ( 2.229367062499998831, 16.10416666803225993, -3.861377020970580887 ) ) ;
#46728 = ORIENTED_EDGE ( 'NONE', *, *, #49600, .T. ) ;
#46729 = CARTESIAN_POINT ( 'NONE',  ( -2.229367062499996610, -88.14583333196773651, 3.861377020970582219 ) ) ;
#46730 = CARTESIAN_POINT ( 'NONE',  ( 4.458734125000001214, 15.85416666803226171, 2.574251347313718519 ) ) ;
#46731 = CARTESIAN_POINT ( 'NONE',  ( 1.060575238724906964E-15, 16.37500000273118417, 5.773502691896257311 ) ) ;
#46732 = CARTESIAN_POINT ( 'NONE',  ( -5.000000000000000000, -60.08333333333333570, -2.886751345948128211 ) ) ;
#46733 = CARTESIAN_POINT ( 'NONE',  ( 5.000000000000000000, 7.583333333333333925, -2.886751345948129988 ) ) ;
#46734 =( BOUNDED_CURVE ( )  B_SPLINE_CURVE ( 2, ( #20470, #40072, #12720, #32340, #47140, #22385, #46507, #17862, #3087 ),
 .UNSPECIFIED., .F., .F. ) 
 B_SPLINE_CURVE_WITH_KNOTS ( ( 3, 2, 2, 2, 3 ),
 ( 0.8645833333333333703, 0.8652777777777778123, 0.8666666666666666963, 0.8680555555555555802, 0.8687500000000000222 ),
 .UNSPECIFIED. ) 
 CURVE ( )  GEOMETRIC_REPRESENTATION_ITEM ( )  RATIONAL_B_SPLINE_CURVE ( ( 0.9330127018922194093, 0.9330127018922194093, 1.000000000000000000, 0.8660254037844387076, 1.000000000000000000, 0.8660254037844387076, 1.000000000000000000, 0.9330127018922194093, 0.9330127018922194093 ) ) 
 REPRESENTATION_ITEM ( '' )  );
#46735 = CARTESIAN_POINT ( 'NONE',  ( -4.458734124999999437, -55.39583333196773651, -2.574251347313719407 ) ) ;
#46736 = CARTESIAN_POINT ( 'NONE',  ( -2.500000000000000444, 14.95833333606451809, -4.330127018922193649 ) ) ;
#46737 = CARTESIAN_POINT ( 'NONE',  ( -5.000000000000000000, -79.08333333333331439, -2.886751345948128211 ) ) ;
#46738 = EDGE_CURVE ( 'NONE', #58682, #26042, #29542, .T. ) ;
#46739 = CARTESIAN_POINT ( 'NONE',  ( -4.999999999999998224, 20.08333333333333925, 2.886751345948131764 ) ) ;
#46740 = CYLINDRICAL_SURFACE ( 'NONE', #32736, 5.000000000000000000 ) ;
#46741 = CARTESIAN_POINT ( 'NONE',  ( 5.000000000000000000, -63.41666666666666430, -2.886751345948130876 ) ) ;
#46742 = CARTESIAN_POINT ( 'NONE',  ( -6.972266317189433020E-16, -25.12499999726881228, -5.000000000000000000 ) ) ;
#46743 = CARTESIAN_POINT ( 'NONE',  ( -5.000000000000000000, -40.99999999999999289, 0.000000000000000000 ) ) ;
#46744 = CYLINDRICAL_SURFACE ( 'NONE', #8909, 5.000000000000000000 ) ;
#46746 = CARTESIAN_POINT ( 'NONE',  ( -3.152548672688508926E-16, -18.81249999863440792, -5.148502694627439702 ) ) ;
#46745 = CARTESIAN_POINT ( 'NONE',  ( -2.499999999999996447, -47.83333333333332149, 4.330127018922195425 ) ) ;
#46747 = CARTESIAN_POINT ( 'NONE',  ( -1.339745962155613812, 12.79465819873851906, -5.000000000000000000 ) ) ;
#46748 = CARTESIAN_POINT ( 'NONE',  ( 4.458734124999998549, -63.72916666530107221, -2.574251347313721627 ) ) ;
#46749 = CARTESIAN_POINT ( 'NONE',  ( -1.846868145590734756, -151.3750000013656063, -4.458734125000000326 ) ) ;
#46750 = CARTESIAN_POINT ( 'NONE',  ( 4.458734124999999437, -71.81249999863439371, -5.460374474430324690E-16 ) ) ;
#46751 = CARTESIAN_POINT ( 'NONE',  ( -50.70258187064364108, -147.3750000013656063, 2.196230717870141014 ) ) ;
#46752 = CARTESIAN_POINT ( 'NONE',  ( 2.229367062500001939, -20.22916666530107221, 3.861377020970579999 ) ) ;
#46753 =( BOUNDED_CURVE ( )  B_SPLINE_CURVE ( 2, ( #32228, #45763, #36429, #50590, #51859, #41553, #41878, #6850, #17128 ),
 .UNSPECIFIED., .F., .F. ) 
 B_SPLINE_CURVE_WITH_KNOTS ( ( 3, 2, 2, 2, 3 ),
 ( 0.1410714285714285698, 0.1416666666666666630, 0.1428571428571428492, 0.1440476190476190355, 0.1446428571428571563 ),
 .UNSPECIFIED. ) 
 CURVE ( )  GEOMETRIC_REPRESENTATION_ITEM ( )  RATIONAL_B_SPLINE_CURVE ( ( 0.9330127018922194093, 0.9330127018922194093, 1.000000000000000000, 0.8660254037844387076, 1.000000000000000000, 0.8660254037844387076, 1.000000000000000000, 0.9330127018922178550, 0.9330127018922194093 ) ) 
 REPRESENTATION_ITEM ( '' )  );
#46754 = CARTESIAN_POINT ( 'NONE',  ( 2.499999999999998668, -59.20833333060214443, -4.330127018922193649 ) ) ;
#46755 = EDGE_LOOP ( 'NONE', ( #25726, #7854, #43594, #32856 ) ) ;
#46756 = CARTESIAN_POINT ( 'NONE',  ( 5.000000000000000000, -31.37499999726880873, -6.123233995736766282E-16 ) ) ;
#46757 = VERTEX_POINT ( 'NONE', #1636 ) ;
#46758 = CARTESIAN_POINT ( 'NONE',  ( -4.458734124999998549, -60.47916666530105800, 2.574251347313722516 ) ) ;
#46759 = CARTESIAN_POINT ( 'NONE',  ( -6.972266317189433020E-16, -25.24999999999999645, -5.000000000000000000 ) ) ;
#46760 = FILL_AREA_STYLE_COLOUR ( '', #23560 ) ;
#46761 = CARTESIAN_POINT ( 'NONE',  ( 1.846868145590736310, -151.6250000013656063, 4.458734124999999437 ) ) ;
#46762 = ORIENTED_EDGE ( 'NONE', *, *, #60157, .T. ) ;
#46763 = CARTESIAN_POINT ( 'NONE',  ( 3.535533905932738197, -155.0000000027312126, -3.535533905932738197 ) ) ;
#46764 = CARTESIAN_POINT ( 'NONE',  ( -51.19402409849444524, -127.5000000000000284, -3.242614290531456334 ) ) ;
#46765 = CARTESIAN_POINT ( 'NONE',  ( 1.339745962155615144, -8.705341801261482715, 4.999999999999999112 ) ) ;
#46767 = EDGE_CURVE ( 'NONE', #44335, #45731, #8972, .T. ) ;
#46766 = CARTESIAN_POINT ( 'NONE',  ( 2.229367062499998831, -51.89583333196773651, -3.861377020970580887 ) ) ;
#46768 = ORIENTED_EDGE ( 'NONE', *, *, #50698, .F. ) ;
#46769 = CARTESIAN_POINT ( 'NONE',  ( 0.000000000000000000, -170.0000000000000000, 0.000000000000000000 ) ) ;
#46770 = CARTESIAN_POINT ( 'NONE',  ( -4.458734124999999437, 6.604166668032259047, -2.574251347313719407 ) ) ;
#46771 = CARTESIAN_POINT ( 'NONE',  ( 4.458734125000001214, 25.10416666803225638, 2.574251347313718519 ) ) ;
#46772 = CARTESIAN_POINT ( 'NONE',  ( -55.35523342533222291, -149.3125000013656063, 4.444560631937231499 ) ) ;
#46773 = CARTESIAN_POINT ( 'NONE',  ( 5.000000000000000000, -13.29166666393548191, -2.886751345948130876 ) ) ;
#46774 = CARTESIAN_POINT ( 'NONE',  ( -9.184850993605147944E-16, -165.2500000000000000, 5.000000000000000000 ) ) ;
#46775 = ORIENTED_EDGE ( 'NONE', *, *, #5800, .F. ) ;
#46776 = CARTESIAN_POINT ( 'NONE',  ( -4.458734124999999437, -68.39583333196773651, -2.574251347313719407 ) ) ;
#46777 = CARTESIAN_POINT ( 'NONE',  ( 1.339745962155612702, -10.16965819600733312, -5.000000000000000000 ) ) ;
#46778 = CARTESIAN_POINT ( 'NONE',  ( -4.458734124999999437, 11.60416666803225993, -2.574251347313719407 ) ) ;
#46779 = CARTESIAN_POINT ( 'NONE',  ( -1.339745962155610925, -41.79465819873852439, 5.000000000000000000 ) ) ;
#46780 = CARTESIAN_POINT ( 'NONE',  ( 4.458734125000001214, -60.14583333196774362, 2.574251347313718519 ) ) ;
#46781 = CARTESIAN_POINT ( 'NONE',  ( 1.060575238724906964E-15, -16.62499999726881583, 5.773502691896257311 ) ) ;
#46782 = EDGE_CURVE ( 'NONE', #19199, #56488, #36031, .T. ) ;
#46783 = CARTESIAN_POINT ( 'NONE',  ( 0.000000000000000000, -120.0000000000000000, 5.000000000000000000 ) ) ;
#46784 = CARTESIAN_POINT ( 'NONE',  ( 0.000000000000000000, -120.0000000000000000, 0.000000000000000000 ) ) ;
#46785 = DIRECTION ( 'NONE',  ( -0.000000000000000000, 1.000000000000000000, -0.000000000000000000 ) ) ;
#46786 = CARTESIAN_POINT ( 'NONE',  ( 4.458734124999999437, -33.81249999863440792, -5.460374474430324690E-16 ) ) ;
#46787 = ADVANCED_FACE ( 'NONE', ( #40842 ), #59849, .T. ) ;
#46788 = CARTESIAN_POINT ( 'NONE',  ( -2.229367062500000163, -23.72916666530107577, -3.861377020970580443 ) ) ;
#46789 = ORIENTED_EDGE ( 'NONE', *, *, #58568, .T. ) ;
#46790 = CARTESIAN_POINT ( 'NONE',  ( -6.972266317189433020E-16, -102.2499999999999858, -5.000000000000000000 ) ) ;
#46791 = CARTESIAN_POINT ( 'NONE',  ( -4.458734124999999437, -109.3958333319677507, -2.574251347313719407 ) ) ;
#46792 = CARTESIAN_POINT ( 'NONE',  ( 2.071067811865475505, -153.9375000027312126, -5.000000000000000888 ) ) ;
#46793 = ORIENTED_EDGE ( 'NONE', *, *, #23973, .T. ) ;
#46794 = CARTESIAN_POINT ( 'NONE',  ( -4.458734124999999437, -103.6458333319677223, -2.574251347313719407 ) ) ;
#46795 = CARTESIAN_POINT ( 'NONE',  ( 4.458734125000001214, -24.89583333196773651, 2.574251347313718519 ) ) ;
#46796 = CARTESIAN_POINT ( 'NONE',  ( -2.500000000000000444, -64.04166666393547303, -4.330127018922193649 ) ) ;
#46797 = CARTESIAN_POINT ( 'NONE',  ( -53.51423613279429503, -152.5000000013655779, 4.591703134518082763 ) ) ;
#46798 = CARTESIAN_POINT ( 'NONE',  ( 5.000000000000000000, -147.0000000000000284, 0.000000000000000000 ) ) ;
#46799 = CARTESIAN_POINT ( 'NONE',  ( 9.457646018065525792E-16, -31.06249999863440436, 5.148502694627439702 ) ) ;
#46800 = CARTESIAN_POINT ( 'NONE',  ( 4.458734124999999437, -72.06249999863439371, -5.460374474430324690E-16 ) ) ;
#46801 = CARTESIAN_POINT ( 'NONE',  ( 1.975475456537005874E-15, -39.62499999726880162, 5.000000000000000000 ) ) ;
#46802 = CARTESIAN_POINT ( 'NONE',  ( -4.458734124999999437, -23.39583333196773651, -2.574251347313719407 ) ) ;
#46803 = CARTESIAN_POINT ( 'NONE',  ( 5.000000000000000000, 14.58333333333333215, -2.886751345948130876 ) ) ;
#46804 = CARTESIAN_POINT ( 'NONE',  ( -1.339745962155613812, 8.919658201469705006, -5.000000000000000000 ) ) ;
#46805 = CARTESIAN_POINT ( 'NONE',  ( -5.000000000000000000, -16.00000000000000000, 0.000000000000000000 ) ) ;
#46806 = CARTESIAN_POINT ( 'NONE',  ( -1.846868145590734756, -152.1250000013655779, -4.458734125000000326 ) ) ;
#46807 = ORIENTED_EDGE ( 'NONE', *, *, #52658, .F. ) ;
#46808 = DIRECTION ( 'NONE',  ( 0.000000000000000000, 0.000000000000000000, 1.000000000000000000 ) ) ;
#46809 = CARTESIAN_POINT ( 'NONE',  ( -2.229367062500000163, -53.72916666530107221, -3.861377020970580443 ) ) ;
#46810 =( BOUNDED_CURVE ( )  B_SPLINE_CURVE ( 2, ( #21897, #46338, #15485, #1658, #31218, #45062, #25770, #40551, #1028 ),
 .UNSPECIFIED., .F., .F. ) 
 B_SPLINE_CURVE_WITH_KNOTS ( ( 3, 2, 2, 2, 3 ),
 ( 0.3645833333333333148, 0.3652777777777777568, 0.3666666666666666408, 0.3680555555555555802, 0.3687500000000000222 ),
 .UNSPECIFIED. ) 
 CURVE ( )  GEOMETRIC_REPRESENTATION_ITEM ( )  RATIONAL_B_SPLINE_CURVE ( ( 0.9330127018922194093, 0.9330127018922194093, 1.000000000000000000, 0.8660254037844387076, 1.000000000000000000, 0.8660254037844387076, 1.000000000000000000, 0.9330127018922194093, 0.9330127018922194093 ) ) 
 REPRESENTATION_ITEM ( '' )  );
#46811 = CARTESIAN_POINT ( 'NONE',  ( -4.999999999999998224, -2.791666663935478354, 2.886751345948131764 ) ) ;
#46812 = CARTESIAN_POINT ( 'NONE',  ( -51.75738570946856498, -135.7500000000000284, 3.805975901505576964 ) ) ;
#46813 = CARTESIAN_POINT ( 'NONE',  ( 5.000000000000000000, 25.58333333333333215, -2.886751345948129988 ) ) ;
#46814 = EDGE_CURVE ( 'NONE', #56685, #59581, #23460, .T. ) ;
#46815 = DIRECTION ( 'NONE',  ( -0.000000000000000000, 1.000000000000000000, -0.000000000000000000 ) ) ;
#46816 = CARTESIAN_POINT ( 'NONE',  ( -3.152548672688508926E-16, 0.4375000013655955255, -5.148502694627439702 ) ) ;
#46817 = CARTESIAN_POINT ( 'NONE',  ( -2.500000000000000444, -74.04166666393547303, -4.330127018922193649 ) ) ;
#46818 = CARTESIAN_POINT ( 'NONE',  ( -5.000000000000000000, -80.87499999726881583, 0.000000000000000000 ) ) ;
#46819 = LINE ( 'NONE', #2763, #46839 ) ;
#46820 = CARTESIAN_POINT ( 'NONE',  ( -4.458734124999999437, 16.35416666803225993, -2.574251347313719407 ) ) ;
#46821 = CARTESIAN_POINT ( 'NONE',  ( -2.499999999999996447, 4.291666669397852907, 4.330127018922195425 ) ) ;
#46822 = VERTEX_POINT ( 'NONE', #42743 ) ;
#46823 = CARTESIAN_POINT ( 'NONE',  ( -5.000000000000000000, -29.87499999726881228, 0.000000000000000000 ) ) ;
#46824 = ORIENTED_EDGE ( 'NONE', *, *, #11313, .T. ) ;
#46825 = CARTESIAN_POINT ( 'NONE',  ( 1.975475456537005874E-15, -7.624999997268812280, 5.000000000000000000 ) ) ;
#46826 = CARTESIAN_POINT ( 'NONE',  ( -2.229367062499996610, -48.14583333196772941, 3.861377020970582219 ) ) ;
#46827 = CARTESIAN_POINT ( 'NONE',  ( -3.152801135295367096, -163.3125000013656063, -3.152801135295367541 ) ) ;
#46828 = CARTESIAN_POINT ( 'NONE',  ( -5.000000000000000000, -45.87499999726880873, 0.000000000000000000 ) ) ;
#46829 = ORIENTED_EDGE ( 'NONE', *, *, #43719, .T. ) ;
#46830 = CARTESIAN_POINT ( 'NONE',  ( 9.457646018065525792E-16, -25.06249999863440792, 5.148502694627439702 ) ) ;
#46831 = ORIENTED_EDGE ( 'NONE', *, *, #20941, .T. ) ;
#46832 = CARTESIAN_POINT ( 'NONE',  ( -4.999999999999999112, -87.91666666666667140, 2.886751345948131764 ) ) ;
#46833 = CARTESIAN_POINT ( 'NONE',  ( 2.730187237215162345E-16, -163.1875000013655779, -4.458734124999999437 ) ) ;
#46834 = CARTESIAN_POINT ( 'NONE',  ( -2.499999999999996447, -50.70833333060213732, 4.330127018922195425 ) ) ;
#46835 = CARTESIAN_POINT ( 'NONE',  ( -59.98410592259440222, -138.1250000000000284, -0.3983568153799752487 ) ) ;
#46836 = CARTESIAN_POINT ( 'NONE',  ( -4.458734124999999437, -34.56249999863440792, 0.000000000000000000 ) ) ;
#46837 = CARTESIAN_POINT ( 'NONE',  ( -4.999999999999998224, 21.08333333333333215, 2.886751345948131764 ) ) ;
#46838 = ORIENTED_EDGE ( 'NONE', *, *, #60078, .T. ) ;
#46839 = VECTOR ( 'NONE', #26452, 1000.000000000000000 ) ;
#46840 = EDGE_CURVE ( 'NONE', #6403, #24352, #11939, .T. ) ;
#46841 = ADVANCED_FACE ( 'NONE', ( #41797 ), #52098, .T. ) ;
#46842 = CARTESIAN_POINT ( 'NONE',  ( -2.229367062499996610, -79.14583333196773651, 3.861377020970582219 ) ) ;
#46843 = CARTESIAN_POINT ( 'NONE',  ( 2.229367062500001939, 22.02083333469892779, 3.861377020970579999 ) ) ;
#46844 = EDGE_CURVE ( 'NONE', #42676, #25930, #61962, .T. ) ;
#46845 = VERTEX_POINT ( 'NONE', #27328 ) ;
#46846 = CARTESIAN_POINT ( 'NONE',  ( 5.000000000000000000, 14.49999999999999822, -6.123233995736766282E-16 ) ) ;
#46847 = CARTESIAN_POINT ( 'NONE',  ( -55.35523342533222291, -140.5625000013656063, 4.444560631937231499 ) ) ;
#46848 = CARTESIAN_POINT ( 'NONE',  ( 2.229367062500001939, -79.22916666530106511, 3.861377020970579999 ) ) ;
#46849 = CARTESIAN_POINT ( 'NONE',  ( -55.39835681537999790, -130.0000000027312126, 4.984105922594378235 ) ) ;
#46850 = CARTESIAN_POINT ( 'NONE',  ( 5.000000000000000000, -74.29166666393547303, -2.886751345948130876 ) ) ;
#46851 = CARTESIAN_POINT ( 'NONE',  ( 1.975475456537005874E-15, -23.62499999726880873, 5.000000000000000000 ) ) ;
#46852 =( BOUNDED_CURVE ( )  B_SPLINE_CURVE ( 2, ( #63155, #34176, #5239, #58007, #48967, #4919, #24538, #38683, #19389 ),
 .UNSPECIFIED., .F., .F. ) 
 B_SPLINE_CURVE_WITH_KNOTS ( ( 3, 2, 2, 2, 3 ),
 ( 0.5416666666666671848, 0.5458333333333338366, 0.5500000000000004885, 0.5541666666666671404, 0.5583333333333337922 ),
 .UNSPECIFIED. ) 
 CURVE ( )  GEOMETRIC_REPRESENTATION_ITEM ( )  RATIONAL_B_SPLINE_CURVE ( ( 0.9999999999999898970, 0.9238795325112968415, 1.000000000000000000, 0.9238795325112867385, 1.000000000000000000, 0.9238795325112867385, 1.000000000000000000, 0.9238795325112786339, 1.000000000000008216 ) ) 
 REPRESENTATION_ITEM ( '' )  );
#46853 = CARTESIAN_POINT ( 'NONE',  ( -51.75738570946856498, -155.0000000000000284, 3.805975901505576520 ) ) ;
#46854 = CARTESIAN_POINT ( 'NONE',  ( -2.229367062500000163, -52.47916666530107221, -3.861377020970580443 ) ) ;
#46855 = CARTESIAN_POINT ( 'NONE',  ( 4.458734124999999437, -44.81249999863440081, -5.460374474430324690E-16 ) ) ;
#46856 = FACE_OUTER_BOUND ( 'NONE', #42637, .T. ) ;
#46857 = EDGE_CURVE ( 'NONE', #14691, #2195, #22519, .T. ) ;
#46858 = EDGE_CURVE ( 'NONE', #20760, #44027, #48775, .T. ) ;
#46859 = CARTESIAN_POINT ( 'NONE',  ( -2.500000000000000444, -109.1666666666666572, -4.330127018922193649 ) ) ;
#46860 = LINE ( 'NONE', #2805, #45311 ) ;
#46861 = CARTESIAN_POINT ( 'NONE',  ( -2.229367062499996610, -38.39583333196773651, 3.861377020970582219 ) ) ;
#46862 = CARTESIAN_POINT ( 'NONE',  ( -5.000000000000000000, 2.125000002731185056, 0.000000000000000000 ) ) ;
#46863 = FACE_OUTER_BOUND ( 'NONE', #61003, .T. ) ;
#46864 = ADVANCED_FACE ( 'NONE', ( #47575 ), #27644, .T. ) ;
#46865 = CARTESIAN_POINT ( 'NONE',  ( -59.59170313451811296, -125.5000000013656205, 1.485763867205729394 ) ) ;
#46866 = CARTESIAN_POINT ( 'NONE',  ( 4.458734125000001214, -80.14583333196773651, 2.574251347313718519 ) ) ;
#46867 = EDGE_CURVE ( 'NONE', #5308, #32177, #61124, .T. ) ;
#46868 = CARTESIAN_POINT ( 'NONE',  ( 9.457646018065525792E-16, -102.0624999986344079, 5.148502694627439702 ) ) ;
#46869 = CARTESIAN_POINT ( 'NONE',  ( 4.458734124999999437, -4.062499998634408804, -5.460374474430324690E-16 ) ) ;
#46870 = ORIENTED_EDGE ( 'NONE', *, *, #24061, .T. ) ;
#46871 = ADVANCED_FACE ( 'NONE', ( #42113 ), #18308, .F. ) ;
#46872 = LINE ( 'NONE', #41080, #30849 ) ;
#46873 = CARTESIAN_POINT ( 'NONE',  ( -2.229367062500000163, -93.47916666530106511, -3.861377020970580443 ) ) ;
#46874 = EDGE_CURVE ( 'NONE', #55713, #39107, #55386, .T. ) ;
#46875 = CARTESIAN_POINT ( 'NONE',  ( 2.071067811865476394, -164.3125000027312410, 5.000000000000000000 ) ) ;
#46876 = CARTESIAN_POINT ( 'NONE',  ( 2.229367062499998831, -86.89583333196773651, -3.861377020970580887 ) ) ;
#46877 = CARTESIAN_POINT ( 'NONE',  ( 4.458734124999999437, 12.93750000136559208, -5.460374474430324690E-16 ) ) ;
#46878 = CARTESIAN_POINT ( 'NONE',  ( -1.339745962155613812, -16.20534180126148271, -5.000000000000000000 ) ) ;
#46879 = CARTESIAN_POINT ( 'NONE',  ( -54.64476657466781973, -133.8125000013656063, -4.444560631937228834 ) ) ;
#46880 = CARTESIAN_POINT ( 'NONE',  ( 2.229367062499998831, -11.64583333196774007, -3.861377020970580887 ) ) ;
#46881 = CARTESIAN_POINT ( 'NONE',  ( 2.229367062500001939, 18.77083333469892779, 3.861377020970579999 ) ) ;
#46882 = CARTESIAN_POINT ( 'NONE',  ( 9.457646018065525792E-16, -52.31249999863440792, 5.148502694627439702 ) ) ;
#46883 = CARTESIAN_POINT ( 'NONE',  ( -6.972266317189433020E-16, -14.12499999726881228, -5.000000000000000000 ) ) ;
#46884 = CARTESIAN_POINT ( 'NONE',  ( -2.071067811865308972, -152.3125000000000000, 5.000000000000169642 ) ) ;
#46885 = CARTESIAN_POINT ( 'NONE',  ( 4.458734124999999437, -7.812499998634405252, -5.460374474430324690E-16 ) ) ;
#46886 = CARTESIAN_POINT ( 'NONE',  ( 2.499999999999998668, -106.2083333306021444, -4.330127018922193649 ) ) ;
#46887 = VERTEX_POINT ( 'NONE', #27015 ) ;
#46888 = CARTESIAN_POINT ( 'NONE',  ( 9.457646018065525792E-16, -34.31249999863440792, 5.148502694627439702 ) ) ;
#46889 = AXIS2_PLACEMENT_3D ( 'NONE', #10805, #25917, #45535 ) ;
#46890 = CARTESIAN_POINT ( 'NONE',  ( -52.10840900171896806, -129.4375000013656063, 3.393966926194110556 ) ) ;
#46891 = CARTESIAN_POINT ( 'NONE',  ( 1.339745962155616255, 26.83034180399266333, -4.999999999999997335 ) ) ;
#46892 = CARTESIAN_POINT ( 'NONE',  ( 4.458734124999999437, -79.81249999863440792, -5.460374474430324690E-16 ) ) ;
#46893 = CARTESIAN_POINT ( 'NONE',  ( -4.458734124999999437, 22.35416666803225638, -2.574251347313719407 ) ) ;
#46894 = CIRCLE ( 'NONE', #38644, 5.000000000000000000 ) ;
#46895 = VECTOR ( 'NONE', #33951, 1000.000000000000000 ) ;
#46896 = CARTESIAN_POINT ( 'NONE',  ( -4.458734124999999437, -151.1875000013656063, -5.460374474430324690E-16 ) ) ;
#46897 = CARTESIAN_POINT ( 'NONE',  ( -4.458734124999999437, 13.60416666803226349, -2.574251347313719407 ) ) ;
#46898 = CARTESIAN_POINT ( 'NONE',  ( 2.499999999999998668, -53.33333333333332860, -4.330127018922193649 ) ) ;
#46899 = LINE ( 'NONE', #7981, #57405 ) ;
#46900 = CARTESIAN_POINT ( 'NONE',  ( -2.229367062500000163, -85.72916666530107932, -3.861377020970580443 ) ) ;
#46901 = CARTESIAN_POINT ( 'NONE',  ( 5.000000000000000888, -64.58333333333332860, 2.886751345948126879 ) ) ;
#46902 = CARTESIAN_POINT ( 'NONE',  ( -6.972266317189433020E-16, -63.12499999726880162, -5.000000000000000000 ) ) ;
#46903 = CARTESIAN_POINT ( 'NONE',  ( -3.535250795749689387E-16, 16.87500000273118417, -5.773502691896257311 ) ) ;
#46904 = EDGE_LOOP ( 'NONE', ( #28613, #51097, #26862, #32345 ) ) ;
#46905 = CARTESIAN_POINT ( 'NONE',  ( 3.535533905932736864, -147.2500000027311842, 3.535533905932738641 ) ) ;
#46906 = CARTESIAN_POINT ( 'NONE',  ( -4.999999999999998224, 28.08333333333332860, 2.886751345948131764 ) ) ;
#46908 = CARTESIAN_POINT ( 'NONE',  ( -5.000000000000000000, -22.00000000000000000, 0.000000000000000000 ) ) ;
#46907 = CYLINDRICAL_SURFACE ( 'NONE', #34751, 5.000000000000000000 ) ;
#46909 = CARTESIAN_POINT ( 'NONE',  ( 4.458734124999998549, -25.72916666530107221, -2.574251347313721627 ) ) ;
#46910 = DIRECTION ( 'NONE',  ( -0.000000000000000000, 1.000000000000000000, -0.000000000000000000 ) ) ;
#46911 = CARTESIAN_POINT ( 'NONE',  ( 2.499999999999998668, -27.20833333060214798, -4.330127018922193649 ) ) ;
#46913 = ORIENTED_EDGE ( 'NONE', *, *, #19975, .T. ) ;
#46912 = CARTESIAN_POINT ( 'NONE',  ( -4.458734124999999437, -60.31249999863440081, 0.000000000000000000 ) ) ;
#46914 = LINE ( 'NONE', #32745, #47755 ) ;
#46916 = VERTEX_POINT ( 'NONE', #13490 ) ;
#46915 = CARTESIAN_POINT ( 'NONE',  ( -2.229367062500000163, -10.72916666530106866, -3.861377020970580443 ) ) ;
#46917 = CARTESIAN_POINT ( 'NONE',  ( 2.499999999999998668, -74.33333333333332860, -4.330127018922193649 ) ) ;
#46918 = CARTESIAN_POINT ( 'NONE',  ( -59.44456063193725015, -138.5625000013656063, -0.3552334253322034230 ) ) ;
#46919 = CARTESIAN_POINT ( 'NONE',  ( 9.457646018065525792E-16, -53.31249999863441502, 5.148502694627439702 ) ) ;
#46920 = CARTESIAN_POINT ( 'NONE',  ( 5.000000000000000000, -77.37499999726881583, -6.123233995736766282E-16 ) ) ;
#46922 = ORIENTED_EDGE ( 'NONE', *, *, #12734, .F. ) ;
#46921 = CYLINDRICAL_SURFACE ( 'NONE', #22103, 5.000000000000000000 ) ;
#46923 = CARTESIAN_POINT ( 'NONE',  ( -59.81910112700025905, -149.1875000000000000, -2.462841084822630311 ) ) ;
#46924 = CARTESIAN_POINT ( 'NONE',  ( 4.458734125000001214, -17.14583333196773651, 2.574251347313718519 ) ) ;
#46925 = CARTESIAN_POINT ( 'NONE',  ( 4.458734125000001214, -58.14583333196773651, 2.574251347313718519 ) ) ;
#46926 = CARTESIAN_POINT ( 'NONE',  ( 0.000000000000000000, -170.0000000000000000, 5.000000000000000000 ) ) ;
#46927 = CARTESIAN_POINT ( 'NONE',  ( 3.152801135295367541, -140.3125000013655779, -3.152801135295367541 ) ) ;
#46928 = CARTESIAN_POINT ( 'NONE',  ( 4.458734125000001214, -99.14583333196773651, 2.574251347313718519 ) ) ;
#46929 = CARTESIAN_POINT ( 'NONE',  ( 1.975475456537005874E-15, -2.750000000000000888, 5.000000000000000000 ) ) ;
#46930 = ORIENTED_EDGE ( 'NONE', *, *, #28742, .T. ) ;
#46931 = CARTESIAN_POINT ( 'NONE',  ( -51.60603307380591787, -153.1875000013656063, -2.891590998281053704 ) ) ;
#46932 = CARTESIAN_POINT ( 'NONE',  ( -53.33387254593733928, -141.9375000027312126, 5.149110718188519620 ) ) ;
#46933 = AXIS2_PLACEMENT_3D ( 'NONE', #59617, #45446, #55102 ) ;
#46934 = VECTOR ( 'NONE', #469, 1000.000000000000000 ) ;
#46935 = CARTESIAN_POINT ( 'NONE',  ( 4.458734124999999437, -8.812499998634406140, -5.460374474430324690E-16 ) ) ;
#46936 = AXIS2_PLACEMENT_3D ( 'NONE', #45603, #6691, #36278 ) ;
#46937 =( BOUNDED_CURVE ( )  B_SPLINE_CURVE ( 2, ( #2264, #11566, #16402, #22184, #36654, #55652, #56283, #31186, #32455 ),
 .UNSPECIFIED., .F., .F. ) 
 B_SPLINE_CURVE_WITH_KNOTS ( ( 3, 2, 2, 2, 3 ),
 ( 0.7303571428571428159, 0.7309523809523809090, 0.7321428571428570953, 0.7333333333333332815, 0.7339285714285714857 ),
 .UNSPECIFIED. ) 
 CURVE ( )  GEOMETRIC_REPRESENTATION_ITEM ( )  RATIONAL_B_SPLINE_CURVE ( ( 0.9330127018922194093, 0.9330127018922194093, 1.000000000000000000, 0.8660254037844387076, 1.000000000000000000, 0.8660254037844387076, 1.000000000000000000, 0.9330127018922130810, 0.9330127018922194093 ) ) 
 REPRESENTATION_ITEM ( '' )  );
#46938 = CARTESIAN_POINT ( 'NONE',  ( -3.152548672688508926E-16, -93.81249999863440792, -5.148502694627439702 ) ) ;
#46939 = CARTESIAN_POINT ( 'NONE',  ( 4.458734125000000326, -146.6250000013655779, -1.846868145590734978 ) ) ;
#46940 = CARTESIAN_POINT ( 'NONE',  ( 2.229367062500001939, -20.22916666530107221, 3.861377020970579999 ) ) ;
#46941 = AXIS2_PLACEMENT_3D ( 'NONE', #35015, #39817, #287 ) ;
#46942 = CARTESIAN_POINT ( 'NONE',  ( 1.975475456537005874E-15, -6.624999997268813168, 5.000000000000000000 ) ) ;
#46943 = CARTESIAN_POINT ( 'NONE',  ( -50.70258187064364108, -138.1250000013656063, 2.196230717870141014 ) ) ;
#46944 = CARTESIAN_POINT ( 'NONE',  ( -4.458734124999999437, -63.56249999863440792, 0.000000000000000000 ) ) ;
#46945 = EDGE_CURVE ( 'NONE', #40725, #2367, #11901, .T. ) ;
#46946 = CARTESIAN_POINT ( 'NONE',  ( 2.500000000000002220, -70.66666666666667140, 4.330127018922192761 ) ) ;
#46947 = CARTESIAN_POINT ( 'NONE',  ( -2.499999999999996447, -33.83333333333332860, 4.330127018922195425 ) ) ;
#46948 = CARTESIAN_POINT ( 'NONE',  ( -8.190561711645485556E-16, -145.6875000013656063, 4.458734124999999437 ) ) ;
#46949 = CARTESIAN_POINT ( 'NONE',  ( 4.458734124999999437, 12.93750000136559208, -5.460374474430324690E-16 ) ) ;
#46950 = ORIENTED_EDGE ( 'NONE', *, *, #32424, .T. ) ;
#46951 = CARTESIAN_POINT ( 'NONE',  ( -1.339745962155613812, -5.205341801261476498, -5.000000000000000000 ) ) ;
#46952 = CARTESIAN_POINT ( 'NONE',  ( -3.535533905932737309, -144.6250000000000000, -3.535533905932738197 ) ) ;
#46954 = CARTESIAN_POINT ( 'NONE',  ( 2.229367062499998831, -24.64583333196773651, -3.861377020970580887 ) ) ;
#46953 = CARTESIAN_POINT ( 'NONE',  ( 2.499999999999998668, -89.33333333333332860, -4.330127018922193649 ) ) ;
#46955 = CARTESIAN_POINT ( 'NONE',  ( 5.000000000000000000, -36.41666666666666430, -2.886751345948130876 ) ) ;
#46956 = CARTESIAN_POINT ( 'NONE',  ( -2.229367062499996610, -72.39583333196773651, 3.861377020970582219 ) ) ;
#46957 = DIRECTION ( 'NONE',  ( 0.000000000000000000, 0.000000000000000000, 1.000000000000000000 ) ) ;
#46958 = CARTESIAN_POINT ( 'NONE',  ( 6.123233995736766282E-16, -120.0000000000000000, -5.000000000000000000 ) ) ;
#46959 = CARTESIAN_POINT ( 'NONE',  ( -52.80376928212989185, -145.8750000013655779, -4.297418129356379346 ) ) ;
#46960 = EDGE_CURVE ( 'NONE', #7305, #60372, #60007, .T. ) ;
#46961 = CARTESIAN_POINT ( 'NONE',  ( 2.071067811865349828, -150.3125000027311842, 5.000000000000126121 ) ) ;
#46962 = CARTESIAN_POINT ( 'NONE',  ( 4.458734124999999437, 6.187500001365593860, -5.460374474430324690E-16 ) ) ;
#46963 = DIRECTION ( 'NONE',  ( -0.000000000000000000, 1.000000000000000000, -0.000000000000000000 ) ) ;
#46964 = CARTESIAN_POINT ( 'NONE',  ( 1.975475456537005874E-15, -62.74999999999998579, 5.000000000000000000 ) ) ;
#46965 = CARTESIAN_POINT ( 'NONE',  ( 4.458734125000000326, 7.104166668032259935, 2.574251347313718519 ) ) ;
#46966 = CARTESIAN_POINT ( 'NONE',  ( 9.457646018065525792E-16, -72.06249999863439371, 5.148502694627439702 ) ) ;
#46967 = CARTESIAN_POINT ( 'NONE',  ( -4.458734124999999437, -17.64583333196773651, -2.574251347313719407 ) ) ;
#46968 = CARTESIAN_POINT ( 'NONE',  ( -5.000000000000000000, -2.000000000000001776, 0.000000000000000000 ) ) ;
#46969 = CARTESIAN_POINT ( 'NONE',  ( -8.190561711645485556E-16, -158.6875000013655779, 4.458734124999999437 ) ) ;
#46970 = CARTESIAN_POINT ( 'NONE',  ( -3.152548672688508926E-16, -64.56249999863440792, -5.148502694627439702 ) ) ;
#46971 = CARTESIAN_POINT ( 'NONE',  ( 2.500000000000002220, -102.5416666639354588, 4.330127018922192761 ) ) ;
#46972 = FACE_OUTER_BOUND ( 'NONE', #29715, .T. ) ;
#46973 = CARTESIAN_POINT ( 'NONE',  ( 4.458734124999999437, -40.81249999863440081, -5.460374474430324690E-16 ) ) ;
#46974 = DIRECTION ( 'NONE',  ( -0.000000000000000000, -1.000000000000000000, -0.000000000000000000 ) ) ;
#46975 = CARTESIAN_POINT ( 'NONE',  ( -4.458734124999997661, -65.47916666530106511, 2.574251347313722516 ) ) ;
#46976 = CARTESIAN_POINT ( 'NONE',  ( -2.500000000000000444, -46.16666666666666430, -4.330127018922193649 ) ) ;
#46977 = CARTESIAN_POINT ( 'NONE',  ( -2.500000000000000444, 26.83333333333333570, -4.330127018922193649 ) ) ;
#46978 = CARTESIAN_POINT ( 'NONE',  ( 1.975475456537005874E-15, 16.24999999999999645, 5.000000000000000000 ) ) ;
#46979 = VERTEX_POINT ( 'NONE', #43374 ) ;
#46980 = CARTESIAN_POINT ( 'NONE',  ( 1.339745962155499015, -94.70534180126146850, 5.000000000000065725 ) ) ;
#46981 = AXIS2_PLACEMENT_3D ( 'NONE', #27706, #47333, #37671 ) ;
#46982 = CARTESIAN_POINT ( 'NONE',  ( -6.972266317189433020E-16, -89.12499999726880162, -5.000000000000000000 ) ) ;
#46983 = CARTESIAN_POINT ( 'NONE',  ( 5.000000000000000000, -9.500000000000001776, -6.123233995736766282E-16 ) ) ;
#46984 = CARTESIAN_POINT ( 'NONE',  ( -2.229367062499996610, -70.14583333196773651, 3.861377020970582219 ) ) ;
#46985 = CARTESIAN_POINT ( 'NONE',  ( 1.060575238724906964E-15, -14.62499999726881228, 5.773502691896257311 ) ) ;
#46987 = EDGE_LOOP ( 'NONE', ( #6655, #55971, #39777, #15877 ) ) ;
#46986 = CARTESIAN_POINT ( 'NONE',  ( -4.458734124999998549, -46.22916666530106511, 2.574251347313722516 ) ) ;
#46988 = CARTESIAN_POINT ( 'NONE',  ( 0.000000000000000000, -170.0000000000000000, 0.000000000000000000 ) ) ;
#46990 = ORIENTED_EDGE ( 'NONE', *, *, #30719, .F. ) ;
#46989 = CARTESIAN_POINT ( 'NONE',  ( 4.458734125000001214, 8.854166668032261711, 2.574251347313718519 ) ) ;
#46991 =( BOUNDED_CURVE ( )  B_SPLINE_CURVE ( 2, ( #47779, #13998, #19132, #52312, #58388, #13689, #37507, #23971, #23357 ),
 .UNSPECIFIED., .F., .F. ) 
 B_SPLINE_CURVE_WITH_KNOTS ( ( 3, 2, 2, 2, 3 ),
 ( 0.4437499999999999778, 0.4444444444444444198, 0.4458333333333333592, 0.4472222222222222432, 0.4479166666666666852 ),
 .UNSPECIFIED. ) 
 CURVE ( )  GEOMETRIC_REPRESENTATION_ITEM ( )  RATIONAL_B_SPLINE_CURVE ( ( 0.9330127018922194093, 0.9330127018922194093, 1.000000000000000000, 0.8660254037844387076, 1.000000000000000000, 0.8660254037844387076, 1.000000000000000000, 0.9330127018922194093, 0.9330127018922194093 ) ) 
 REPRESENTATION_ITEM ( '' )  );
#46992 = CARTESIAN_POINT ( 'NONE',  ( -3.535533905932738641, -151.3750000000000000, 3.535533905932737309 ) ) ;
#46993 = CARTESIAN_POINT ( 'NONE',  ( -5.000000000000000000, -53.08333333333332860, -2.886751345948128211 ) ) ;
#46994 = CARTESIAN_POINT ( 'NONE',  ( -3.152801135295367985, -159.0625000013656063, 3.152801135295367096 ) ) ;
#46995 = CARTESIAN_POINT ( 'NONE',  ( -2.229367062500000163, -34.72916666530107221, -3.861377020970580443 ) ) ;
#46996 = CARTESIAN_POINT ( 'NONE',  ( 3.061616997868383141E-16, -144.7500000000000284, -5.000000000000000000 ) ) ;
#46997 = CARTESIAN_POINT ( 'NONE',  ( -4.458734124999998549, -82.22916666530107932, 2.574251347313722516 ) ) ;
#46998 = CARTESIAN_POINT ( 'NONE',  ( -5.000000000000000888, -167.5625000000000568, -2.071067811865475949 ) ) ;
#46999 = CARTESIAN_POINT ( 'NONE',  ( -3.152548672688508926E-16, -89.56249999863439371, -5.148502694627439702 ) ) ;
#47000 = CARTESIAN_POINT ( 'NONE',  ( -54.64476657466781973, -133.0625000013656063, -4.444560631937228834 ) ) ;
#47001 = CARTESIAN_POINT ( 'NONE',  ( -3.152548672688508926E-16, 1.187500001365596081, -5.148502694627439702 ) ) ;
#47002 = CARTESIAN_POINT ( 'NONE',  ( -3.152548672688508926E-16, -41.81249999863440081, -5.148502694627439702 ) ) ;
#47003 = CARTESIAN_POINT ( 'NONE',  ( 2.499999999999998668, -72.33333333333332860, -4.330127018922193649 ) ) ;
#47004 = CARTESIAN_POINT ( 'NONE',  ( -4.458734124999999437, -83.64583333196773651, -2.574251347313719407 ) ) ;
#47005 = CARTESIAN_POINT ( 'NONE',  ( 5.000000000000000000, -86.50000000000000000, -6.123233995736766282E-16 ) ) ;
#47006 = VERTEX_POINT ( 'NONE', #5412 ) ;
#47007 = CARTESIAN_POINT ( 'NONE',  ( -2.071067811865432873, -141.6875000000000284, -5.000000000000041744 ) ) ;
#47008 = FACE_OUTER_BOUND ( 'NONE', #59590, .T. ) ;
#47009 = CARTESIAN_POINT ( 'NONE',  ( 2.229367062500001939, -72.22916666530107932, 3.861377020970579999 ) ) ;
#47010 = CARTESIAN_POINT ( 'NONE',  ( -4.458734124999997661, -38.22916666530107932, 2.574251347313722516 ) ) ;
#47011 = CARTESIAN_POINT ( 'NONE',  ( -2.229367062500000163, -9.729166665301068662, -3.861377020970580443 ) ) ;
#47012 = ORIENTED_EDGE ( 'NONE', *, *, #3527, .F. ) ;
#47013 = CARTESIAN_POINT ( 'NONE',  ( 6.123233995736766282E-16, -170.0000000000000000, -5.000000000000000000 ) ) ;
#47014 = LINE ( 'NONE', #27702, #26536 ) ;
#47015 = CARTESIAN_POINT ( 'NONE',  ( 4.458734124999999437, -9.062499998634406140, -5.460374474430324690E-16 ) ) ;
#47016 = CARTESIAN_POINT ( 'NONE',  ( -51.75738570946856498, -148.8750000027312126, 3.805975901505576964 ) ) ;
#47017 = CARTESIAN_POINT ( 'NONE',  ( -4.458734124999999437, 1.687500001365593194, 0.000000000000000000 ) ) ;
#47018 = CARTESIAN_POINT ( 'NONE',  ( 0.000000000000000000, -170.0000000000000000, 5.000000000000000000 ) ) ;
#47019 = CARTESIAN_POINT ( 'NONE',  ( -4.458734125000000326, -155.8750000013655779, 1.846868145590734089 ) ) ;
#47020 = AXIS2_PLACEMENT_3D ( 'NONE', #58159, #33404, #28257 ) ;
#47021 = CARTESIAN_POINT ( 'NONE',  ( -4.458734124999999437, 27.35416666803225993, -2.574251347313719407 ) ) ;
#47022 = ORIENTED_EDGE ( 'NONE', *, *, #23348, .F. ) ;
#47023 = CARTESIAN_POINT ( 'NONE',  ( 4.458734125000000326, -86.89583333196773651, 2.574251347313718519 ) ) ;
#47024 = CARTESIAN_POINT ( 'NONE',  ( -1.339745962155610925, -46.79465819873852439, 5.000000000000000000 ) ) ;
#47025 = CARTESIAN_POINT ( 'NONE',  ( 4.458734125000001214, -10.89583333196773651, 2.574251347313718519 ) ) ;
#47026 = CARTESIAN_POINT ( 'NONE',  ( 6.123233995736766282E-16, -170.0000000000000000, -5.000000000000000000 ) ) ;
#47027 = CARTESIAN_POINT ( 'NONE',  ( 0.000000000000000000, -120.0000000000000000, 0.000000000000000000 ) ) ;
#47028 = CARTESIAN_POINT ( 'NONE',  ( -3.535250795749689387E-16, -34.12499999726881583, -5.773502691896257311 ) ) ;
#47029 = CARTESIAN_POINT ( 'NONE',  ( -6.972266317189433020E-16, -78.24999999999998579, -5.000000000000000000 ) ) ;
#47030 = CARTESIAN_POINT ( 'NONE',  ( -2.229367062499996610, 24.85416666803225993, 3.861377020970582219 ) ) ;
#47031 = CARTESIAN_POINT ( 'NONE',  ( -4.999999999999998224, -97.79166666393545881, 2.886751345948131764 ) ) ;
#47032 = CARTESIAN_POINT ( 'NONE',  ( 2.229367062499998831, 25.35416666803225993, -3.861377020970580887 ) ) ;
#47033 = CARTESIAN_POINT ( 'NONE',  ( -4.458734124999999437, -58.39583333196774362, -2.574251347313719407 ) ) ;
#47034 = CARTESIAN_POINT ( 'NONE',  ( -4.458734124999999437, -5.645833331967740953, -2.574251347313719407 ) ) ;
#47035 =( BOUNDED_CURVE ( )  B_SPLINE_CURVE ( 2, ( #27157, #42258, #22017, #46773, #50968, #26200, #21382, #7859, #16553 ),
 .UNSPECIFIED., .F., .F. ) 
 B_SPLINE_CURVE_WITH_KNOTS ( ( 3, 2, 2, 2, 3 ),
 ( 0.3520833333333333592, 0.3527777777777778012, 0.3541666666666666852, 0.3555555555555555691, 0.3562500000000000111 ),
 .UNSPECIFIED. ) 
 CURVE ( )  GEOMETRIC_REPRESENTATION_ITEM ( )  RATIONAL_B_SPLINE_CURVE ( ( 0.9330127018922194093, 0.9330127018922220739, 1.000000000000000000, 0.8660254037844387076, 1.000000000000000000, 0.8660254037844387076, 1.000000000000000000, 0.9330127018922194093, 0.9330127018922194093 ) ) 
 REPRESENTATION_ITEM ( '' )  );
#47036 = CARTESIAN_POINT ( 'NONE',  ( -1.339745962155613812, -18.20534180126147916, -5.000000000000000000 ) ) ;
#47037 = CARTESIAN_POINT ( 'NONE',  ( -2.500000000000000444, 17.83333333333333215, -4.330127018922193649 ) ) ;
#47038 = CARTESIAN_POINT ( 'NONE',  ( 2.071067811865476394, -140.3125000027312126, 5.000000000000000000 ) ) ;
#47039 = CARTESIAN_POINT ( 'NONE',  ( 5.000000000000000000, -69.49999999999998579, -6.123233995736766282E-16 ) ) ;
#47040 = CARTESIAN_POINT ( 'NONE',  ( 4.458734125000001214, -48.89583333196772941, 2.574251347313718519 ) ) ;
#47041 = CARTESIAN_POINT ( 'NONE',  ( 5.000000000000000888, -84.45833333060214443, 2.886751345948126879 ) ) ;
#47042 = CARTESIAN_POINT ( 'NONE',  ( -52.80376928212989185, -136.1250000013656063, -4.297418129356379346 ) ) ;
#47043 = CARTESIAN_POINT ( 'NONE',  ( 5.000000000000000000, -37.29166666393548724, -2.886751345948130876 ) ) ;
#47044 = CARTESIAN_POINT ( 'NONE',  ( 5.000000000000000000, -36.41666666666666430, -2.886751345948130876 ) ) ;
#47045 = CARTESIAN_POINT ( 'NONE',  ( -3.152548672688508926E-16, -85.81249999863440792, -5.148502694627439702 ) ) ;
#47046 = CARTESIAN_POINT ( 'NONE',  ( -8.190561711645485556E-16, -155.9375000013655779, 4.458734124999999437 ) ) ;
#47047 = CARTESIAN_POINT ( 'NONE',  ( 2.499999999999998668, -31.33333333333333215, -4.330127018922193649 ) ) ;
#47048 = FILL_AREA_STYLE_COLOUR ( '', #49018 ) ;
#47049 = ORIENTED_EDGE ( 'NONE', *, *, #6767, .F. ) ;
#47050 = CARTESIAN_POINT ( 'NONE',  ( -4.458734124999999437, 15.43750000136559386, 0.000000000000000000 ) ) ;
#47051 = ORIENTED_EDGE ( 'NONE', *, *, #40483, .T. ) ;
#47052 = CARTESIAN_POINT ( 'NONE',  ( -3.152548672688508926E-16, -93.56249999863439371, -5.148502694627439702 ) ) ;
#47053 = CARTESIAN_POINT ( 'NONE',  ( -4.458734124999998549, 13.52083333469892779, 2.574251347313722516 ) ) ;
#47054 = CARTESIAN_POINT ( 'NONE',  ( -2.500000000000000444, 18.95833333606451632, -4.330127018922193649 ) ) ;
#47055 = CARTESIAN_POINT ( 'NONE',  ( -4.999999999999998224, -59.91666666666665719, 2.886751345948131764 ) ) ;
#47056 = CARTESIAN_POINT ( 'NONE',  ( -2.500000000000000444, 5.833333333333333037, -4.330127018922193649 ) ) ;
#47057 = ADVANCED_FACE ( 'NONE', ( #48203 ), #14418, .T. ) ;
#47058 = CARTESIAN_POINT ( 'NONE',  ( 4.458734125000000326, -57.89583333196773651, 2.574251347313718519 ) ) ;
#47059 = CARTESIAN_POINT ( 'NONE',  ( -5.000000000000000000, 15.04166666939785202, -2.886751345948128211 ) ) ;
#47060 = CARTESIAN_POINT ( 'NONE',  ( -2.499999999999996447, -79.83333333333332860, 4.330127018922195425 ) ) ;
#47061 = FACE_OUTER_BOUND ( 'NONE', #8939, .T. ) ;
#47062 = CARTESIAN_POINT ( 'NONE',  ( 1.975475456537005874E-15, -37.62499999726880873, 5.000000000000000000 ) ) ;
#47063 = CARTESIAN_POINT ( 'NONE',  ( -4.999999999999998224, -12.79166666393547835, 2.886751345948131764 ) ) ;
#47064 = CARTESIAN_POINT ( 'NONE',  ( 3.044556291839386294E-14, 17.87500000273118417, -5.000000000000000000 ) ) ;
#47065 = CARTESIAN_POINT ( 'NONE',  ( 5.000000000000000888, -41.58333333333332860, 2.886751345948126879 ) ) ;
#47066 = CARTESIAN_POINT ( 'NONE',  ( -9.184850993605147944E-16, -149.2500000000000284, 5.000000000000000000 ) ) ;
#47068 = CARTESIAN_POINT ( 'NONE',  ( 2.229367062500001939, -21.22916666530107221, 3.861377020970579999 ) ) ;
#47067 = CARTESIAN_POINT ( 'NONE',  ( -2.500000000000000444, 13.83333333333333215, -4.330127018922193649 ) ) ;
#47069 = AXIS2_PLACEMENT_3D ( 'NONE', #3351, #22968, #18124 ) ;
#47070 = CARTESIAN_POINT ( 'NONE',  ( 5.000000000000000888, -107.4583333306021586, 2.886751345948126879 ) ) ;
#47071 = CARTESIAN_POINT ( 'NONE',  ( 2.229367062499998831, -66.64583333196773651, -3.861377020970580887 ) ) ;
#47072 = CARTESIAN_POINT ( 'NONE',  ( -4.458734125000001214, -147.1250000013656063, 1.846868145590734089 ) ) ;
#47073 = CARTESIAN_POINT ( 'NONE',  ( 2.229367062500001939, -70.97916666530107932, 3.861377020970579999 ) ) ;
#47074 = AXIS2_PLACEMENT_3D ( 'NONE', #57822, #57201, #33365 ) ;
#47075 = CARTESIAN_POINT ( 'NONE',  ( -57.89159099828107458, -142.9375000013656063, -3.393966926194107447 ) ) ;
#47076 = CARTESIAN_POINT ( 'NONE',  ( -4.458734124999999437, -20.56249999863440081, 0.000000000000000000 ) ) ;
#47077 = CARTESIAN_POINT ( 'NONE',  ( 2.500000000000002220, -59.54166666393546592, 4.330127018922192761 ) ) ;
#47078 = VERTEX_POINT ( 'NONE', #34041 ) ;
#47079 = CARTESIAN_POINT ( 'NONE',  ( 5.000000000000000000, -85.37499999726880162, -6.123233995736766282E-16 ) ) ;
#47080 = ORIENTED_EDGE ( 'NONE', *, *, #57391, .F. ) ;
#47081 = CARTESIAN_POINT ( 'NONE',  ( 4.458734124999999437, -68.06249999863440792, -5.460374474430324690E-16 ) ) ;
#47082 = CARTESIAN_POINT ( 'NONE',  ( -6.972266317189433020E-16, -81.12499999726881583, -5.000000000000000000 ) ) ;
#47083 = CARTESIAN_POINT ( 'NONE',  ( 0.000000000000000000, -170.0000000000000000, 0.000000000000000000 ) ) ;
#47084 = EDGE_LOOP ( 'NONE', ( #27457, #41707, #17873, #61465 ) ) ;
#47085 = CARTESIAN_POINT ( 'NONE',  ( -1.339745962155613146, 27.33034180399266333, 5.000000000000000000 ) ) ;
#47086 = CARTESIAN_POINT ( 'NONE',  ( -58.24261429053147765, -126.2500000000000284, -3.805975901505573855 ) ) ;
#47087 = CARTESIAN_POINT ( 'NONE',  ( -2.229367062499996610, -53.39583333196773651, 3.861377020970582219 ) ) ;
#47088 = VERTEX_POINT ( 'NONE', #58495 ) ;
#47089 = VECTOR ( 'NONE', #21717, 1000.000000000000000 ) ;
#47090 = CARTESIAN_POINT ( 'NONE',  ( -2.498395430326213474E-14, 14.37500000273118417, 5.000000000000000000 ) ) ;
#47091 = CARTESIAN_POINT ( 'NONE',  ( -4.458734124999998549, 8.770833334698927786, 2.574251347313722516 ) ) ;
#47092 = CARTESIAN_POINT ( 'NONE',  ( -4.458734124999999437, 17.60416666803225993, -2.574251347313719407 ) ) ;
#47093 = CARTESIAN_POINT ( 'NONE',  ( -59.44456063193725015, -150.5625000013656063, -0.3552334253322034230 ) ) ;
#47094 = CARTESIAN_POINT ( 'NONE',  ( 1.339745962155612702, -108.1696581960073189, -5.000000000000000000 ) ) ;
#47095 = CARTESIAN_POINT ( 'NONE',  ( 0.000000000000000000, -120.0000000000000000, 0.000000000000000000 ) ) ;
#47096 = ORIENTED_EDGE ( 'NONE', *, *, #50433, .F. ) ;
#47097 = CARTESIAN_POINT ( 'NONE',  ( -3.152548672688508926E-16, -68.56249999863439371, -5.148502694627439702 ) ) ;
#47098 = CARTESIAN_POINT ( 'NONE',  ( 4.458734124999998549, 5.270833334698926897, -2.574251347313721627 ) ) ;
#47099 = CARTESIAN_POINT ( 'NONE',  ( -5.000000000000000000, -89.08333333333332860, -2.886751345948128211 ) ) ;
#47100 = CARTESIAN_POINT ( 'NONE',  ( 4.458734124999998549, -58.97916666530105800, -2.574251347313721627 ) ) ;
#47101 = CARTESIAN_POINT ( 'NONE',  ( 5.000000000000000888, -19.45833333060214798, 2.886751345948126879 ) ) ;
#47102 = CARTESIAN_POINT ( 'NONE',  ( -4.999999999999998224, -32.79166666393547303, 2.886751345948131764 ) ) ;
#47103 = CARTESIAN_POINT ( 'NONE',  ( -5.000000000000000000, -44.95833333060214443, -2.886751345948128211 ) ) ;
#47104 = CARTESIAN_POINT ( 'NONE',  ( 0.000000000000000000, -114.9999999999999858, 5.000000000000000000 ) ) ;
#47105 = CARTESIAN_POINT ( 'NONE',  ( -1.339745962155610925, 19.20534180126147916, 5.000000000000000000 ) ) ;
#47106 = CARTESIAN_POINT ( 'NONE',  ( -4.458734124999999437, -39.31249999863440081, 0.000000000000000000 ) ) ;
#47107 = CARTESIAN_POINT ( 'NONE',  ( -2.229367062499996610, -22.39583333196773651, 3.861377020970582219 ) ) ;
#47108 = EDGE_LOOP ( 'NONE', ( #59746, #6569, #2054, #28707 ) ) ;
#47109 = AXIS2_PLACEMENT_3D ( 'NONE', #61190, #17112, #20991 ) ;
#47110 = DIRECTION ( 'NONE',  ( -0.000000000000000000, 1.000000000000000000, -0.000000000000000000 ) ) ;
#47111 = CARTESIAN_POINT ( 'NONE',  ( 5.000000000000000000, 28.58333333333333215, -2.886751345948129988 ) ) ;
#47112 = CARTESIAN_POINT ( 'NONE',  ( 3.535533905932736864, -153.2500000027312126, 3.535533905932738641 ) ) ;
#47113 = ORIENTED_EDGE ( 'NONE', *, *, #18185, .F. ) ;
#47114 = CARTESIAN_POINT ( 'NONE',  ( -3.152548672688508926E-16, -108.8124999986343937, -5.148502694627439702 ) ) ;
#47115 = CARTESIAN_POINT ( 'NONE',  ( -2.229367062499996610, -34.14583333196772941, 3.861377020970582219 ) ) ;
#47116 = CARTESIAN_POINT ( 'NONE',  ( 1.060575238724906964E-15, -63.62499999726881583, 5.773502691896257311 ) ) ;
#47117 =( BOUNDED_CURVE ( )  B_SPLINE_CURVE ( 2, ( #36479, #40340, #56104, #12025, #15592, #2397, #22007, #59660, #54827 ),
 .UNSPECIFIED., .F., .F. ) 
 B_SPLINE_CURVE_WITH_KNOTS ( ( 3, 2, 2, 2, 3 ),
 ( 0.03541666666666666574, 0.03611111111111110772, 0.03749999999999999861, 0.03888888888888888951, 0.03958333333333333842 ),
 .UNSPECIFIED. ) 
 CURVE ( )  GEOMETRIC_REPRESENTATION_ITEM ( )  RATIONAL_B_SPLINE_CURVE ( ( 0.9330127018922194093, 0.9330127018922194093, 1.000000000000000000, 0.8660254037844387076, 1.000000000000000000, 0.8660254037844387076, 1.000000000000000000, 0.9330127018922189652, 0.9330127018922192983 ) ) 
 REPRESENTATION_ITEM ( '' )  );
#47118 = CARTESIAN_POINT ( 'NONE',  ( -50.55543936806279248, -150.3125000013656063, 0.3552334253322060320 ) ) ;
#47119 = CARTESIAN_POINT ( 'NONE',  ( -3.535533905932737309, -147.6250000000000000, -3.535533905932738197 ) ) ;
#47120 = CARTESIAN_POINT ( 'NONE',  ( -2.229367062500000163, -30.47916666530107221, -3.861377020970580443 ) ) ;
#47121 = CARTESIAN_POINT ( 'NONE',  ( 4.458734125000000326, -71.14583333196773651, 2.574251347313718519 ) ) ;
#47122 = CARTESIAN_POINT ( 'NONE',  ( 5.000000000000000000, 22.70833333606451632, -2.886751345948130876 ) ) ;
#47123 = CARTESIAN_POINT ( 'NONE',  ( 2.229367062500001939, -23.97916666530107577, 3.861377020970579999 ) ) ;
#47124 = CARTESIAN_POINT ( 'NONE',  ( 1.975475456537005874E-15, -45.74999999999999289, 5.000000000000000000 ) ) ;
#47125 = CARTESIAN_POINT ( 'NONE',  ( 1.339745962155615144, 18.41965820146970856, 4.999999999999999112 ) ) ;
#47126 = CARTESIAN_POINT ( 'NONE',  ( -2.500000000000000444, -18.16666666666666430, -4.330127018922193649 ) ) ;
#47127 = CARTESIAN_POINT ( 'NONE',  ( 3.152801135295366208, -147.5625000013655779, 3.152801135295367985 ) ) ;
#47128 = ORIENTED_EDGE ( 'NONE', *, *, #29898, .T. ) ;
#47129 = CARTESIAN_POINT ( 'NONE',  ( -58.80597590150559739, -153.0000000000000284, 3.242614290531460330 ) ) ;
#47130 = CARTESIAN_POINT ( 'NONE',  ( 2.229367062499998831, -49.89583333196772941, -3.861377020970580887 ) ) ;
#47131 = CARTESIAN_POINT ( 'NONE',  ( -1.339745962155610925, -86.66965819600733312, 5.000000000000000000 ) ) ;
#47132 = CYLINDRICAL_SURFACE ( 'NONE', #14442, 5.000000000000000000 ) ;
#47133 = CARTESIAN_POINT ( 'NONE',  ( 1.060575238724906964E-15, 23.25000000000000000, 5.773502691896257311 ) ) ;
#47134 = EDGE_CURVE ( 'NONE', #1494, #25237, #5095, .T. ) ;
#47135 = AXIS2_PLACEMENT_3D ( 'NONE', #28442, #48057, #450 ) ;
#47136 = CARTESIAN_POINT ( 'NONE',  ( -50.18089887299979068, -152.6875000000000000, 2.462841084822605442 ) ) ;
#47137 = CARTESIAN_POINT ( 'NONE',  ( -2.229367062499996610, -0.1458333319677394824, 3.861377020970582219 ) ) ;
#47138 =( BOUNDED_CURVE ( )  B_SPLINE_CURVE ( 2, ( #59846, #16726, #55007, #40522, #5480, #26059, #30227, #36342, #16410 ),
 .UNSPECIFIED., .F., .F. ) 
 B_SPLINE_CURVE_WITH_KNOTS ( ( 3, 2, 2, 2, 3 ),
 ( 0.3624999999999999889, 0.3630952380952380820, 0.3642857142857142683, 0.3654761904761904545, 0.3660714285714285476 ),
 .UNSPECIFIED. ) 
 CURVE ( )  GEOMETRIC_REPRESENTATION_ITEM ( )  RATIONAL_B_SPLINE_CURVE ( ( 0.9330127018922194093, 0.9330127018922194093, 1.000000000000000000, 0.8660254037844387076, 1.000000000000000000, 0.8660254037844387076, 1.000000000000000000, 0.9330127018922194093, 0.9330127018922194093 ) ) 
 REPRESENTATION_ITEM ( '' )  );
#47139 = DIRECTION ( 'NONE',  ( -0.000000000000000000, 1.000000000000000000, -0.000000000000000000 ) ) ;
#47140 = CARTESIAN_POINT ( 'NONE',  ( -5.000000000000000000, -74.00000000000000000, 0.000000000000000000 ) ) ;
#47141 = CARTESIAN_POINT ( 'NONE',  ( -4.458734124999998549, 11.52083333469892779, 2.574251347313722516 ) ) ;
#47142 = ORIENTED_EDGE ( 'NONE', *, *, #56322, .F. ) ;
#47143 = DIRECTION ( 'NONE',  ( 0.000000000000000000, 0.000000000000000000, -1.000000000000000000 ) ) ;
#47144 = ORIENTED_EDGE ( 'NONE', *, *, #20940, .F. ) ;
#47145 = DIRECTION ( 'NONE',  ( 0.000000000000000000, 0.000000000000000000, 1.000000000000000000 ) ) ;
#47146 = CARTESIAN_POINT ( 'NONE',  ( -2.229367062499996610, -50.14583333196772941, 3.861377020970582219 ) ) ;
#47147 = CARTESIAN_POINT ( 'NONE',  ( 4.458734124999999437, -159.6875000013655779, 0.000000000000000000 ) ) ;
#47148 = ADVANCED_FACE ( 'NONE', ( #38541 ), #24713, .T. ) ;
#47149 = CARTESIAN_POINT ( 'NONE',  ( -5.000000000000000000, -42.87499999726880873, 0.000000000000000000 ) ) ;
#47150 = ORIENTED_EDGE ( 'NONE', *, *, #18533, .F. ) ;
#47152 = EDGE_CURVE ( 'NONE', #22810, #35769, #31137, .T. ) ;
#47151 = CARTESIAN_POINT ( 'NONE',  ( -4.458734124999998549, -21.22916666530107221, 2.574251347313722516 ) ) ;
#47153 = ORIENTED_EDGE ( 'NONE', *, *, #24714, .T. ) ;
#47154 = CARTESIAN_POINT ( 'NONE',  ( -2.499999999999996447, -11.83333333333333393, 4.330127018922195425 ) ) ;
#47155 = CARTESIAN_POINT ( 'NONE',  ( 2.730187237215162345E-16, -166.1875000013655779, -4.458734124999999437 ) ) ;
#47156 = VECTOR ( 'NONE', #33287, 1000.000000000000000 ) ;
#47157 = CARTESIAN_POINT ( 'NONE',  ( 1.339745962155615144, -39.58034179853028434, 4.999999999999999112 ) ) ;
#47158 = CARTESIAN_POINT ( 'NONE',  ( -54.60164318462004474, -137.3750000000000284, -4.984105922594373794 ) ) ;
#47159 = VECTOR ( 'NONE', #14626, 1000.000000000000000 ) ;
#47160 = CARTESIAN_POINT ( 'NONE',  ( 4.458734124999998549, -39.97916666530107221, -2.574251347313721627 ) ) ;
#47161 = CARTESIAN_POINT ( 'NONE',  ( 1.975475456537005874E-15, -38.75000000000000000, 5.000000000000000000 ) ) ;
#47162 = ORIENTED_EDGE ( 'NONE', *, *, #22427, .F. ) ;
#47163 = ADVANCED_FACE ( 'NONE', ( #58172 ), #33728, .T. ) ;
#47164 = CARTESIAN_POINT ( 'NONE',  ( 4.458734125000001214, -84.89583333196773651, 2.574251347313718519 ) ) ;
#47165 = CARTESIAN_POINT ( 'NONE',  ( 2.229367062500001939, 24.02083333469892779, 3.861377020970579999 ) ) ;
#47166 = CARTESIAN_POINT ( 'NONE',  ( 1.975475456537005874E-15, -28.62499999726881583, 5.000000000000000000 ) ) ;
#47167 = ORIENTED_EDGE ( 'NONE', *, *, #58893, .T. ) ;
#47168 = CARTESIAN_POINT ( 'NONE',  ( 1.975475456537005874E-15, -69.62499999726880162, 5.000000000000000000 ) ) ;
#47169 = CARTESIAN_POINT ( 'NONE',  ( -54.64476657466781973, -137.0625000013656063, -4.444560631937228834 ) ) ;
#47170 = CARTESIAN_POINT ( 'NONE',  ( 9.457646018065525792E-16, -83.31249999863440792, 5.148502694627439702 ) ) ;
#47171 = CARTESIAN_POINT ( 'NONE',  ( -59.81910112700025905, -129.3125000027312694, -2.462841084822630311 ) ) ;
#47172 = CARTESIAN_POINT ( 'NONE',  ( 0.000000000000000000, 0.000000000000000000, -9.226681596905677907 ) ) ;
#47173 = CARTESIAN_POINT ( 'NONE',  ( 0.000000000000000000, -170.0000000000000000, 5.000000000000000000 ) ) ;
#47174 = CARTESIAN_POINT ( 'NONE',  ( 2.229367062500001939, -55.97916666530107221, 3.861377020970579999 ) ) ;
#47175 = CARTESIAN_POINT ( 'NONE',  ( 2.499999999999998668, 21.66666666666666785, -4.330127018922193649 ) ) ;
#47176 = CARTESIAN_POINT ( 'NONE',  ( 4.458734124999998549, 24.27083333469892779, -2.574251347313721627 ) ) ;
#47177 = CARTESIAN_POINT ( 'NONE',  ( -3.535250795749689387E-16, -106.2499999999999858, -5.773502691896257311 ) ) ;
#47178 = CARTESIAN_POINT ( 'NONE',  ( 5.000000000000000888, -159.0625000027312126, -2.071067811865475505 ) ) ;
#47179 = CARTESIAN_POINT ( 'NONE',  ( 4.458734124999998549, -45.97916666530106511, -2.574251347313721627 ) ) ;
#47180 = EDGE_CURVE ( 'NONE', #48706, #28142, #63644, .T. ) ;
#47181 = CARTESIAN_POINT ( 'NONE',  ( -2.500000000000000444, 0.9583333360645186483, -4.330127018922193649 ) ) ;
#47182 = CARTESIAN_POINT ( 'NONE',  ( -2.071067811865644259, -153.8125000027311273, -4.999999999999831246 ) ) ;
#47183 = CARTESIAN_POINT ( 'NONE',  ( -50.55543936806279248, -125.0625000013655921, 0.3552334253322060320 ) ) ;
#47184 = CARTESIAN_POINT ( 'NONE',  ( -4.458734124999999437, -81.56249999863440792, 0.000000000000000000 ) ) ;
#47185 = CARTESIAN_POINT ( 'NONE',  ( 4.458734124999998549, -102.7291666653010651, -2.574251347313721627 ) ) ;
#47186 = CARTESIAN_POINT ( 'NONE',  ( 2.229367062499998831, -3.895833331967739177, -3.861377020970580887 ) ) ;
#47187 =( BOUNDED_CURVE ( )  B_SPLINE_CURVE ( 2, ( #61269, #46779, #17191, #22666, #57705, #2412, #17522, #37141, #26855 ),
 .UNSPECIFIED., .F., .F. ) 
 B_SPLINE_CURVE_WITH_KNOTS ( ( 3, 2, 2, 2, 3 ),
 ( 0.5124999999999999556, 0.5130952380952380487, 0.5142857142857142350, 0.5154761904761904212, 0.5160714285714286254 ),
 .UNSPECIFIED. ) 
 CURVE ( )  GEOMETRIC_REPRESENTATION_ITEM ( )  RATIONAL_B_SPLINE_CURVE ( ( 0.9330127018922194093, 0.9330127018922194093, 1.000000000000000000, 0.8660254037844387076, 1.000000000000000000, 0.8660254037844387076, 1.000000000000000000, 0.9330127018922130810, 0.9330127018922194093 ) ) 
 REPRESENTATION_ITEM ( '' )  );
#47188 = ORIENTED_EDGE ( 'NONE', *, *, #16664, .F. ) ;
#47189 = CARTESIAN_POINT ( 'NONE',  ( -6.972266317189433020E-16, -86.12499999726880162, -5.000000000000000000 ) ) ;
#47190 = CARTESIAN_POINT ( 'NONE',  ( 2.229367062499998831, -94.64583333196773651, -3.861377020970580887 ) ) ;
#47191 = CARTESIAN_POINT ( 'NONE',  ( -2.071067811865478170, -167.4375000027311842, 5.000000000000000000 ) ) ;
#47192 = CARTESIAN_POINT ( 'NONE',  ( -2.229367062500000163, -85.72916666530107932, -3.861377020970580443 ) ) ;
#47193 = CARTESIAN_POINT ( 'NONE',  ( 9.457646018065525792E-16, 14.68750000136559564, 5.148502694627439702 ) ) ;
#47194 = LINE ( 'NONE', #7013, #14040 ) ;
#47195 = CARTESIAN_POINT ( 'NONE',  ( -53.51423613279429503, -133.2500000013656347, 4.591703134518082763 ) ) ;
#47196 = CARTESIAN_POINT ( 'NONE',  ( 4.458734125000000326, -12.89583333196774362, 2.574251347313718519 ) ) ;
#47197 = CARTESIAN_POINT ( 'NONE',  ( -2.229367062499996610, 14.60416666803226171, 3.861377020970582219 ) ) ;
#47198 = CARTESIAN_POINT ( 'NONE',  ( -2.229367062499996610, -52.39583333196773651, 3.861377020970582219 ) ) ;
#47199 = CARTESIAN_POINT ( 'NONE',  ( -2.499999999999996447, 17.29166666939785557, 4.330127018922195425 ) ) ;
#47200 = CARTESIAN_POINT ( 'NONE',  ( -2.071067811865686448, -152.6875000000000284, -4.999999999999789502 ) ) ;
#47201 = CARTESIAN_POINT ( 'NONE',  ( -4.458734124999999437, -9.395833331967736513, -2.574251347313719407 ) ) ;
#47202 = CARTESIAN_POINT ( 'NONE',  ( -1.339745962155613812, -39.20534180126147561, -5.000000000000000000 ) ) ;
#47203 = ORIENTED_EDGE ( 'NONE', *, *, #18045, .T. ) ;
#47204 = CARTESIAN_POINT ( 'NONE',  ( -4.458734124999997661, -33.47916666530107221, 2.574251347313722516 ) ) ;
#47205 = AXIS2_PLACEMENT_3D ( 'NONE', #7425, #31533, #11277 ) ;
#47206 = CARTESIAN_POINT ( 'NONE',  ( -58.39396692619412477, -128.6875000013656063, 2.891590998281057701 ) ) ;
#47207 = CARTESIAN_POINT ( 'NONE',  ( 5.000000000000000000, -68.49999999999998579, -6.123233995736766282E-16 ) ) ;
#47208 = CARTESIAN_POINT ( 'NONE',  ( 9.457646018065525792E-16, -78.06249999863440792, 5.148502694627439702 ) ) ;
#47209 = CARTESIAN_POINT ( 'NONE',  ( -4.458734124999998549, 25.52083333469893134, 2.574251347313722516 ) ) ;
#47210 = CARTESIAN_POINT ( 'NONE',  ( 4.458734125000001214, 14.10416666803225993, 2.574251347313718519 ) ) ;
#47211 = EDGE_CURVE ( 'NONE', #18516, #10357, #44768, .T. ) ;
#47212 = ADVANCED_FACE ( 'NONE', ( #50107 ), #20537, .T. ) ;
#47213 = DIRECTION ( 'NONE',  ( 0.000000000000000000, 0.000000000000000000, 1.000000000000000000 ) ) ;
#47214 = DIRECTION ( 'NONE',  ( -0.000000000000000000, 1.000000000000000000, -0.000000000000000000 ) ) ;
#47215 = CARTESIAN_POINT ( 'NONE',  ( 2.229367062500001939, -86.22916666530107932, 3.861377020970579999 ) ) ;
#47216 = CARTESIAN_POINT ( 'NONE',  ( 2.499999999999998668, -68.33333333333332860, -4.330127018922193649 ) ) ;
#47217 = LINE ( 'NONE', #51095, #54211 ) ;
#47218 = CARTESIAN_POINT ( 'NONE',  ( -5.000000000000000000, 20.04166666939785202, -2.886751345948128211 ) ) ;
#47219 = VERTEX_POINT ( 'NONE', #25675 ) ;
#47220 = CARTESIAN_POINT ( 'NONE',  ( -1.339745962155613812, -62.08034179853028434, -5.000000000000000000 ) ) ;
#47221 = CARTESIAN_POINT ( 'NONE',  ( 6.158835246850667461E-14, 8.749999999999998224, -4.999999999999999112 ) ) ;
#47223 = CARTESIAN_POINT ( 'NONE',  ( 1.060575238724906964E-15, -26.74999999999999645, 5.773502691896257311 ) ) ;
#47222 = CARTESIAN_POINT ( 'NONE',  ( 1.339745962155612702, -40.29465819873851729, -5.000000000000000000 ) ) ;
#47224 = CARTESIAN_POINT ( 'NONE',  ( 2.229367062499998831, -32.64583333196773651, -3.861377020970580887 ) ) ;
#47225 = CARTESIAN_POINT ( 'NONE',  ( 5.000000000000000888, -62.58333333333333570, 2.886751345948126879 ) ) ;
#47226 = EDGE_CURVE ( 'NONE', #42641, #26676, #55588, .T. ) ;
#47227 = CARTESIAN_POINT ( 'NONE',  ( 5.000000000000000888, -29.45833333060214798, 2.886751345948126879 ) ) ;
#47229 = ORIENTED_EDGE ( 'NONE', *, *, #17017, .F. ) ;
#47228 = CARTESIAN_POINT ( 'NONE',  ( -2.229367062499996610, -60.14583333196774362, 3.861377020970582219 ) ) ;
#47230 = CARTESIAN_POINT ( 'NONE',  ( -50.70258187064364108, -154.3750000013656063, 2.196230717870141014 ) ) ;
#47231 = ADVANCED_FACE ( 'NONE', ( #30810 ), #60416, .T. ) ;
#47233 = ORIENTED_EDGE ( 'NONE', *, *, #10339, .T. ) ;
#47232 = CARTESIAN_POINT ( 'NONE',  ( -2.229367062499996610, -8.395833331967736513, 3.861377020970582219 ) ) ;
#47234 = CARTESIAN_POINT ( 'NONE',  ( -2.499999999999996447, -77.83333333333334281, 4.330127018922195425 ) ) ;
#47235 = CARTESIAN_POINT ( 'NONE',  ( -56.48576386720575471, -137.7500000013656063, -4.591703134518078322 ) ) ;
#47236 = CARTESIAN_POINT ( 'NONE',  ( 2.229367062499998831, -50.89583333196772941, -3.861377020970580887 ) ) ;
#47237 = CARTESIAN_POINT ( 'NONE',  ( -3.535250795749689387E-16, -79.12499999726881583, -5.773502691896257311 ) ) ;
#47239 = ORIENTED_EDGE ( 'NONE', *, *, #57391, .T. ) ;
#47238 = CARTESIAN_POINT ( 'NONE',  ( 1.339745962155615144, -65.58034179853029855, 4.999999999999999112 ) ) ;
#47240 = CARTESIAN_POINT ( 'NONE',  ( -56.66612745406270335, -151.3125000000000284, -5.149110718188516067 ) ) ;
#47241 = CARTESIAN_POINT ( 'NONE',  ( -3.152548672688508926E-16, -19.81249999863440436, -5.148502694627439702 ) ) ;
#47242 = CARTESIAN_POINT ( 'NONE',  ( -4.458734124999998549, -54.47916666530107932, 2.574251347313722516 ) ) ;
#47243 = CARTESIAN_POINT ( 'NONE',  ( -2.500000000000000444, -30.04166666393548013, -4.330127018922193649 ) ) ;
#47244 = SURFACE_SIDE_STYLE ('',( #51441 ) ) ;
#47245 = CARTESIAN_POINT ( 'NONE',  ( -4.458734125000001214, -141.8750000013656063, 1.846868145590734089 ) ) ;
#47246 = CARTESIAN_POINT ( 'NONE',  ( 4.458734124999998549, -97.97916666530105090, -2.574251347313721627 ) ) ;
#47247 = DIRECTION ( 'NONE',  ( -0.000000000000000000, 1.000000000000000000, -0.000000000000000000 ) ) ;
#47248 = ORIENTED_EDGE ( 'NONE', *, *, #49885, .F. ) ;
#47249 = CARTESIAN_POINT ( 'NONE',  ( -51.60603307380591787, -149.1875000013656063, -2.891590998281053704 ) ) ;
#47250 = CARTESIAN_POINT ( 'NONE',  ( -52.53715891517739323, -144.5625000027311842, -4.819101127000233298 ) ) ;
#47251 = AXIS2_PLACEMENT_3D ( 'NONE', #3810, #47546, #9565 ) ;
#47252 = CYLINDRICAL_SURFACE ( 'NONE', #35269, 5.000000000000000000 ) ;
#47253 = CARTESIAN_POINT ( 'NONE',  ( -4.458734124999998549, -9.229166665301068662, 2.574251347313722516 ) ) ;
#47254 = CARTESIAN_POINT ( 'NONE',  ( -4.458734124999999437, -96.56249999863440792, 0.000000000000000000 ) ) ;
#47255 = CARTESIAN_POINT ( 'NONE',  ( 3.152801135295366208, -149.8125000013655779, 3.152801135295367985 ) ) ;
#47256 = CARTESIAN_POINT ( 'NONE',  ( 9.457646018065525792E-16, -26.31249999863440792, 5.148502694627439702 ) ) ;
#47257 = CARTESIAN_POINT ( 'NONE',  ( 1.975475456537005874E-15, -92.62499999726881583, 5.000000000000000000 ) ) ;
#47258 = CARTESIAN_POINT ( 'NONE',  ( -51.60603307380591787, -135.9375000013656063, -2.891590998281053704 ) ) ;
#47259 = CARTESIAN_POINT ( 'NONE',  ( 9.457646018065525792E-16, -65.31249999863440792, 5.148502694627439702 ) ) ;
#47260 = PLANE ( 'NONE',  #16861 ) ;
#47261 = CARTESIAN_POINT ( 'NONE',  ( -5.000000000000000000, -42.87499999726880873, 0.000000000000000000 ) ) ;
#47262 = CARTESIAN_POINT ( 'NONE',  ( -4.458734124999999437, -145.9375000013656063, -5.460374474430324690E-16 ) ) ;
#47263 = CARTESIAN_POINT ( 'NONE',  ( -4.458734124999999437, 8.437500001365595637, 0.000000000000000000 ) ) ;
#47264 = VERTEX_POINT ( 'NONE', #6381 ) ;
#47265 = CARTESIAN_POINT ( 'NONE',  ( -2.499999999999996447, -52.70833333060213732, 4.330127018922195425 ) ) ;
#47266 = CARTESIAN_POINT ( 'NONE',  ( 1.975475456537005874E-15, -66.62499999726881583, 5.000000000000000000 ) ) ;
#47268 = CARTESIAN_POINT ( 'NONE',  ( 4.458734124999998549, -26.72916666530106866, -2.574251347313721627 ) ) ;
#47267 = CARTESIAN_POINT ( 'NONE',  ( 2.500000000000002220, -88.66666666666665719, 4.330127018922192761 ) ) ;
#47269 = CARTESIAN_POINT ( 'NONE',  ( -2.229367062500000163, -69.72916666530107932, -3.861377020970580443 ) ) ;
#47270 = CARTESIAN_POINT ( 'NONE',  ( 4.458734125000000326, 27.85416666803225993, 2.574251347313718519 ) ) ;
#47271 = CARTESIAN_POINT ( 'NONE',  ( -6.972266317189433020E-16, -18.12499999726881228, -5.000000000000000000 ) ) ;
#47272 = CARTESIAN_POINT ( 'NONE',  ( -53.51423613279429503, -145.2500000013656347, 4.591703134518082763 ) ) ;
#47273 = CARTESIAN_POINT ( 'NONE',  ( 4.458734125000000326, 1.104166668032261711, 2.574251347313718519 ) ) ;
#47274 = DIRECTION ( 'NONE',  ( -0.000000000000000000, 1.000000000000000000, -0.000000000000000000 ) ) ;
#47275 = CARTESIAN_POINT ( 'NONE',  ( 5.000000000000000000, 21.50000000000000000, -6.123233995736766282E-16 ) ) ;
#47276 = CARTESIAN_POINT ( 'NONE',  ( -3.152548672688508926E-16, 7.437500001365594748, -5.148502694627439702 ) ) ;
#47277 = CARTESIAN_POINT ( 'NONE',  ( -4.458734124999998549, -70.22916666530107932, 2.574251347313722516 ) ) ;
#47278 = CARTESIAN_POINT ( 'NONE',  ( -4.458734124999999437, -18.56249999863440792, 0.000000000000000000 ) ) ;
#47279 = CARTESIAN_POINT ( 'NONE',  ( -5.000000000000000000, -5.083333333333334814, -2.886751345948128211 ) ) ;
#47280 = CARTESIAN_POINT ( 'NONE',  ( 4.458734124999999437, -160.4375000013655779, 0.000000000000000000 ) ) ;
#47281 = CYLINDRICAL_SURFACE ( 'NONE', #12024, 5.000000000000000000 ) ;
#47282 = CARTESIAN_POINT ( 'NONE',  ( 4.458734125000001214, -63.89583333196772941, 2.574251347313718519 ) ) ;
#47283 = CARTESIAN_POINT ( 'NONE',  ( -5.000000000000000000, -99.87499999726881583, 0.000000000000000000 ) ) ;
#47284 = CARTESIAN_POINT ( 'NONE',  ( 0.000000000000000000, -170.0000000000000000, 5.000000000000000000 ) ) ;
#47285 = CARTESIAN_POINT ( 'NONE',  ( 4.458734124999999437, -38.81249999863440081, -5.460374474430324690E-16 ) ) ;
#47286 = ADVANCED_FACE ( 'NONE', ( #50746 ), #25029, .T. ) ;
#47287 = CARTESIAN_POINT ( 'NONE',  ( -4.458734124999999437, -103.5624999986344079, 0.000000000000000000 ) ) ;
#47288 = CARTESIAN_POINT ( 'NONE',  ( 4.458734124999999437, -65.06249999863440792, -5.460374474430324690E-16 ) ) ;
#47289 = CARTESIAN_POINT ( 'NONE',  ( 2.499999999999998668, -46.33333333333333570, -4.330127018922193649 ) ) ;
#47290 = LINE ( 'NONE', #27037, #24372 ) ;
#47291 = CARTESIAN_POINT ( 'NONE',  ( -9.184850993605147944E-16, -152.3750000027311842, 5.000000000000000000 ) ) ;
#47292 = ORIENTED_EDGE ( 'NONE', *, *, #6777, .T. ) ;
#47293 = CARTESIAN_POINT ( 'NONE',  ( -4.999999999999998224, -84.91666666666667140, 2.886751345948131764 ) ) ;
#47294 = CARTESIAN_POINT ( 'NONE',  ( 0.000000000000000000, -170.0000000000000000, 0.000000000000000000 ) ) ;
#47295 = CARTESIAN_POINT ( 'NONE',  ( 2.499999999999998668, -12.33333333333333570, -4.330127018922193649 ) ) ;
#47296 = CARTESIAN_POINT ( 'NONE',  ( -2.229367062500000163, -18.47916666530106866, -3.861377020970580443 ) ) ;
#47297 = CARTESIAN_POINT ( 'NONE',  ( -4.458734124999997661, -76.22916666530107932, 2.574251347313722516 ) ) ;
#47298 = CARTESIAN_POINT ( 'NONE',  ( 5.000000000000000000, -12.29166666393547835, -2.886751345948129988 ) ) ;
#47300 = VERTEX_POINT ( 'NONE', #45284 ) ;
#47299 = CARTESIAN_POINT ( 'NONE',  ( -4.458734124999999437, -43.39583333196774362, -2.574251347313719407 ) ) ;
#47301 = CARTESIAN_POINT ( 'NONE',  ( 1.339745962155612702, -41.29465819873852439, -5.000000000000000000 ) ) ;
#47303 = EDGE_LOOP ( 'NONE', ( #55236, #55037, #23766, #163 ) ) ;
#47302 = CARTESIAN_POINT ( 'NONE',  ( 2.229367062500001939, 5.770833334698927786, 3.861377020970579999 ) ) ;
#47304 = DIRECTION ( 'NONE',  ( 0.000000000000000000, -1.000000000000000000, 0.000000000000000000 ) ) ;
#47305 = CARTESIAN_POINT ( 'NONE',  ( 2.499999999999998668, -55.33333333333332860, -4.330127018922193649 ) ) ;
#47306 = ADVANCED_FACE ( 'NONE', ( #26296 ), #25348, .T. ) ;
#47307 = CARTESIAN_POINT ( 'NONE',  ( -1.846868145590734756, -158.3750000013655779, -4.458734125000000326 ) ) ;
#47308 = CARTESIAN_POINT ( 'NONE',  ( -4.458734124999999437, -33.56249999863440792, 0.000000000000000000 ) ) ;
#47309 = CARTESIAN_POINT ( 'NONE',  ( -9.184850993605147944E-16, -145.2500000000000284, 5.000000000000000000 ) ) ;
#47310 = CARTESIAN_POINT ( 'NONE',  ( 2.229367062499998831, -81.64583333196773651, -3.861377020970580887 ) ) ;
#47311 = CARTESIAN_POINT ( 'NONE',  ( -3.535533905932737309, -165.6250000000000284, -3.535533905932738197 ) ) ;
#47312 = EDGE_CURVE ( 'NONE', #57843, #50566, #11406, .T. ) ;
#47313 = CYLINDRICAL_SURFACE ( 'NONE', #53895, 5.000000000000000000 ) ;
#47314 = CARTESIAN_POINT ( 'NONE',  ( -57.19623071787017210, -130.6250000013656347, 4.297418129356382899 ) ) ;
#47315 = CARTESIAN_POINT ( 'NONE',  ( 2.229367062500001939, 0.7708333346989268975, 3.861377020970579999 ) ) ;
#47316 = CARTESIAN_POINT ( 'NONE',  ( 4.458734125000001214, -41.14583333196774362, 2.574251347313718519 ) ) ;
#47317 =( BOUNDED_CURVE ( )  B_SPLINE_CURVE ( 2, ( #58540, #24439, #34084, #59174, #39536, #40190, #15108, #6107, #10591 ),
 .UNSPECIFIED., .F., .F. ) 
 B_SPLINE_CURVE_WITH_KNOTS ( ( 3, 2, 2, 2, 3 ),
 ( 0.8517857142857142572, 0.8523809523809523503, 0.8535714285714285365, 0.8547619047619047228, 0.8553571428571428159 ),
 .UNSPECIFIED. ) 
 CURVE ( )  GEOMETRIC_REPRESENTATION_ITEM ( )  RATIONAL_B_SPLINE_CURVE ( ( 0.9330127018922194093, 0.9330127018922194093, 1.000000000000000000, 0.8660254037844387076, 1.000000000000000000, 0.8660254037844387076, 1.000000000000000000, 0.9330127018922194093, 0.9330127018922194093 ) ) 
 REPRESENTATION_ITEM ( '' )  );
#47318 = EDGE_CURVE ( 'NONE', #33853, #15348, #11813, .T. ) ;
#47319 = CARTESIAN_POINT ( 'NONE',  ( 2.500000000000002220, -54.66666666666667140, 4.330127018922192761 ) ) ;
#47320 = CARTESIAN_POINT ( 'NONE',  ( 4.458734124999999437, -83.06249999863440792, -5.460374474430324690E-16 ) ) ;
#47321 = CARTESIAN_POINT ( 'NONE',  ( 1.339745962155615144, -86.70534180126148271, 4.999999999999999112 ) ) ;
#47322 = ORIENTED_EDGE ( 'NONE', *, *, #16497, .F. ) ;
#47323 = CARTESIAN_POINT ( 'NONE',  ( -2.071067811865306307, -148.8125000027312126, -5.000000000000171418 ) ) ;
#47324 = CYLINDRICAL_SURFACE ( 'NONE', #382, 5.000000000000000000 ) ;
#47325 = CARTESIAN_POINT ( 'NONE',  ( -4.458734124999999437, -70.56249999863439371, 0.000000000000000000 ) ) ;
#47326 = CARTESIAN_POINT ( 'NONE',  ( -4.458734124999999437, -6.562499998634403475, 0.000000000000000000 ) ) ;
#47327 = ORIENTED_EDGE ( 'NONE', *, *, #815, .F. ) ;
#47328 = DIRECTION ( 'NONE',  ( -0.000000000000000000, 1.000000000000000000, -0.000000000000000000 ) ) ;
#47329 = CARTESIAN_POINT ( 'NONE',  ( -6.972266317189433020E-16, -64.24999999999998579, -5.000000000000000000 ) ) ;
#47330 = CARTESIAN_POINT ( 'NONE',  ( -3.152548672688508926E-16, -6.812499998634404363, -5.148502694627439702 ) ) ;
#47331 = DIRECTION ( 'NONE',  ( -0.000000000000000000, 1.000000000000000000, -0.000000000000000000 ) ) ;
#47332 = CARTESIAN_POINT ( 'NONE',  ( 2.229367062499998831, 3.354166668032259935, -3.861377020970580887 ) ) ;
#47333 = DIRECTION ( 'NONE',  ( -0.000000000000000000, 1.000000000000000000, -0.000000000000000000 ) ) ;
#47334 = CARTESIAN_POINT ( 'NONE',  ( -1.846868145590737420, -157.7500000013656063, 4.458734124999997661 ) ) ;
#47335 = CARTESIAN_POINT ( 'NONE',  ( -4.458734124999999437, 25.43750000136559208, 0.000000000000000000 ) ) ;
#47336 = ORIENTED_EDGE ( 'NONE', *, *, #42129, .F. ) ;
#47337 = CARTESIAN_POINT ( 'NONE',  ( -2.229367062500000163, -89.47916666530106511, -3.861377020970580443 ) ) ;
#47338 = CARTESIAN_POINT ( 'NONE',  ( -2.499999999999996447, -77.83333333333334281, 4.330127018922195425 ) ) ;
#47339 = CARTESIAN_POINT ( 'NONE',  ( -4.458734124999998549, -9.229166665301068662, 2.574251347313722516 ) ) ;
#47340 = AXIS2_PLACEMENT_3D ( 'NONE', #60441, #15724, #54645 ) ;
#47341 = DIRECTION ( 'NONE',  ( -0.000000000000000000, 1.000000000000000000, -0.000000000000000000 ) ) ;
#47342 = LINE ( 'NONE', #43130, #10925 ) ;
#47343 = CARTESIAN_POINT ( 'NONE',  ( -1.339745962155610925, 15.20534180126147916, 5.000000000000000000 ) ) ;
#47344 = CARTESIAN_POINT ( 'NONE',  ( 1.060575238724906964E-15, -38.62499999726881583, 5.773502691896257311 ) ) ;
#47345 = CARTESIAN_POINT ( 'NONE',  ( 2.229367062499998831, 19.35416666803225993, -3.861377020970580887 ) ) ;
#47346 = CARTESIAN_POINT ( 'NONE',  ( 1.975475456537005874E-15, -97.62499999726880162, 5.000000000000000000 ) ) ;
#47347 = CARTESIAN_POINT ( 'NONE',  ( -4.458734124999999437, 20.68750000136559208, 0.000000000000000000 ) ) ;
#47348 = CARTESIAN_POINT ( 'NONE',  ( -4.458734124999999437, -54.31249999863440081, 0.000000000000000000 ) ) ;
#47349 = CARTESIAN_POINT ( 'NONE',  ( -4.458734124999999437, -3.645833331967739177, -2.574251347313719407 ) ) ;
#47350 = CYLINDRICAL_SURFACE ( 'NONE', #21679, 5.000000000000000000 ) ;
#47351 = CARTESIAN_POINT ( 'NONE',  ( 2.499999999999998668, 12.66666666666666607, -4.330127018922193649 ) ) ;
#47352 = CARTESIAN_POINT ( 'NONE',  ( 2.071067811865475505, -141.9375000027312126, -5.000000000000000888 ) ) ;
#47353 = CARTESIAN_POINT ( 'NONE',  ( -1.339745962155610925, -51.79465819873851729, 5.000000000000000000 ) ) ;
#47354 = CARTESIAN_POINT ( 'NONE',  ( -4.458734124999999437, -50.39583333196773651, -2.574251347313719407 ) ) ;
#47355 = CARTESIAN_POINT ( 'NONE',  ( 5.000000000000000000, -85.37499999726880162, -6.123233995736766282E-16 ) ) ;
#47356 = CARTESIAN_POINT ( 'NONE',  ( -50.70258187064364108, -137.3750000013656063, 2.196230717870141014 ) ) ;
#47357 = FACE_OUTER_BOUND ( 'NONE', #44202, .T. ) ;
#47358 = EDGE_CURVE ( 'NONE', #62035, #45003, #31432, .T. ) ;
#47359 = CARTESIAN_POINT ( 'NONE',  ( -52.53715891517739323, -145.4375000000000284, -4.819101127000233298 ) ) ;
#47360 = CARTESIAN_POINT ( 'NONE',  ( 2.229367062499998831, -86.89583333196773651, -3.861377020970580887 ) ) ;
#47361 = CARTESIAN_POINT ( 'NONE',  ( 3.152801135295367541, -158.5625000013656063, -3.152801135295367541 ) ) ;
#47362 =( BOUNDED_CURVE ( )  B_SPLINE_CURVE ( 2, ( #49958, #10725, #6862, #60269, #50920, #16187, #54797, #50600, #30332 ),
 .UNSPECIFIED., .F., .F. ) 
 B_SPLINE_CURVE_WITH_KNOTS ( ( 3, 2, 2, 2, 3 ),
 ( 0.3083333333333336257, 0.3125000000000002776, 0.3166666666666669294, 0.3208333333333336368, 0.3250000000000002887 ),
 .UNSPECIFIED. ) 
 CURVE ( )  GEOMETRIC_REPRESENTATION_ITEM ( )  RATIONAL_B_SPLINE_CURVE ( ( 0.9999999999999948930, 0.9238795325112918455, 1.000000000000000000, 0.9238795325112867385, 1.000000000000000000, 0.9238795325112867385, 1.000000000000000000, 0.9238795325112816315, 1.000000000000005107 ) ) 
 REPRESENTATION_ITEM ( '' )  );
#47363 = CARTESIAN_POINT ( 'NONE',  ( -4.999999999999999112, -34.91666666666666430, 2.886751345948131764 ) ) ;
#47364 = CARTESIAN_POINT ( 'NONE',  ( -2.071067811865391128, -147.6875000000000568, -5.000000000000086153 ) ) ;
#47365 = ORIENTED_EDGE ( 'NONE', *, *, #29384, .F. ) ;
#47366 = CARTESIAN_POINT ( 'NONE',  ( 2.229367062499998831, 15.10416666803225993, -3.861377020970580887 ) ) ;
#47367 = EDGE_LOOP ( 'NONE', ( #20842, #1875, #47776, #5648 ) ) ;
#47368 = CARTESIAN_POINT ( 'NONE',  ( -4.458734124999999437, -98.39583333196773651, -2.574251347313719407 ) ) ;
#47369 = CARTESIAN_POINT ( 'NONE',  ( -2.229367062499996610, 10.60416666803225993, 3.861377020970582219 ) ) ;
#47370 = CARTESIAN_POINT ( 'NONE',  ( 2.500000000000002220, 12.45833333606451809, 4.330127018922192761 ) ) ;
#47371 = CARTESIAN_POINT ( 'NONE',  ( -2.499999999999996447, -43.70833333060214443, 4.330127018922195425 ) ) ;
#47372 = CARTESIAN_POINT ( 'NONE',  ( 2.499999999999998668, 8.666666666666666075, -4.330127018922193649 ) ) ;
#47373 = CARTESIAN_POINT ( 'NONE',  ( 4.458734125000000326, -58.89583333196773651, 2.574251347313718519 ) ) ;
#47374 = CARTESIAN_POINT ( 'NONE',  ( 0.000000000000000000, -170.0000000000000000, 0.000000000000000000 ) ) ;
#47375 = CARTESIAN_POINT ( 'NONE',  ( -5.000000000000000000, -79.00000000000000000, 0.000000000000000000 ) ) ;
#47376 = CARTESIAN_POINT ( 'NONE',  ( -2.229367062499996610, -31.14583333196773651, 3.861377020970582219 ) ) ;
#47377 = CARTESIAN_POINT ( 'NONE',  ( -6.972266317189433020E-16, -13.12499999726881050, -5.000000000000000000 ) ) ;
#47378 = CYLINDRICAL_SURFACE ( 'NONE', #60760, 5.000000000000000000 ) ;
#47379 = CARTESIAN_POINT ( 'NONE',  ( -2.500000000000000444, -42.16666666666667140, -4.330127018922193649 ) ) ;
#47380 = CARTESIAN_POINT ( 'NONE',  ( -4.999999999999998224, 13.20833333606451987, 2.886751345948131764 ) ) ;
#47382 = CARTESIAN_POINT ( 'NONE',  ( 9.457646018065525792E-16, -21.31249999863440081, 5.148502694627439702 ) ) ;
#47381 = CARTESIAN_POINT ( 'NONE',  ( -1.339745962155613812, -48.20534180126148271, -5.000000000000000000 ) ) ;
#47383 = CARTESIAN_POINT ( 'NONE',  ( -14.99999999999998934, -1.734723475976807094E-15, 0.000000000000000000 ) ) ;
#47384 = CARTESIAN_POINT ( 'NONE',  ( -4.458734124999999437, -62.39583333196774362, -2.574251347313719407 ) ) ;
#47385 = CARTESIAN_POINT ( 'NONE',  ( 4.458734124999999437, -147.6875000013656063, 0.000000000000000000 ) ) ;
#47386 = CARTESIAN_POINT ( 'NONE',  ( 4.458734124999999437, -68.81249999863439371, -5.460374474430324690E-16 ) ) ;
#47387 = CARTESIAN_POINT ( 'NONE',  ( -57.89159099828107458, -141.9375000013656063, -3.393966926194107447 ) ) ;
#47388 = CARTESIAN_POINT ( 'NONE',  ( 4.458734124999999437, -26.06249999863440792, -5.460374474430324690E-16 ) ) ;
#47389 = CARTESIAN_POINT ( 'NONE',  ( -5.000000000000000000, -63.87499999726880873, 0.000000000000000000 ) ) ;
#47390 = ORIENTED_EDGE ( 'NONE', *, *, #14895, .F. ) ;
#47391 = CARTESIAN_POINT ( 'NONE',  ( 5.000000000000000888, -1.583333333333332371, 2.886751345948126879 ) ) ;
#47392 = ORIENTED_EDGE ( 'NONE', *, *, #39262, .F. ) ;
#47393 = CARTESIAN_POINT ( 'NONE',  ( 9.457646018065525792E-16, -68.31249999863442213, 5.148502694627439702 ) ) ;
#47394 = CARTESIAN_POINT ( 'NONE',  ( -58.24261429053147765, -155.0000000000000284, -3.805975901505573411 ) ) ;
#47395 = ORIENTED_EDGE ( 'NONE', *, *, #43342, .T. ) ;
#47396 = CARTESIAN_POINT ( 'NONE',  ( 0.6508621380849231031, 8.763657152406445050, -7.907633014911220393 ) ) ;
#47397 = CARTESIAN_POINT ( 'NONE',  ( 1.975475456537005874E-15, -74.62499999726880162, 5.000000000000000000 ) ) ;
#47398 = CARTESIAN_POINT ( 'NONE',  ( 2.229367062500001939, -54.22916666530107221, 3.861377020970579999 ) ) ;
#47399 = ORIENTED_EDGE ( 'NONE', *, *, #893, .F. ) ;
#47400 = DIRECTION ( 'NONE',  ( 0.000000000000000000, 0.000000000000000000, 1.000000000000000000 ) ) ;
#47401 = CARTESIAN_POINT ( 'NONE',  ( -2.229367062500000163, 7.520833334698929562, -3.861377020970580443 ) ) ;
#47402 = CARTESIAN_POINT ( 'NONE',  ( -4.458734124999999437, 19.68750000136559208, 0.000000000000000000 ) ) ;
#47403 = CARTESIAN_POINT ( 'NONE',  ( -50.55543936806279248, -149.0625000013656063, 0.3552334253322060320 ) ) ;
#47404 = CARTESIAN_POINT ( 'NONE',  ( -4.999999999999998224, 6.208333336064520758, 2.886751345948131764 ) ) ;
#47405 = CARTESIAN_POINT ( 'NONE',  ( 1.846868145590735200, -168.2500000013656063, -4.458734124999999437 ) ) ;
#47406 =( BOUNDED_CURVE ( )  B_SPLINE_CURVE ( 2, ( #38093, #57719, #58338, #54133, #10395, #58651, #24878, #24555, #129 ),
 .UNSPECIFIED., .F., .F. ) 
 B_SPLINE_CURVE_WITH_KNOTS ( ( 3, 2, 2, 2, 3 ),
 ( 0.5696428571428571175, 0.5702380952380952106, 0.5714285714285713969, 0.5726190476190475831, 0.5732142857142856762 ),
 .UNSPECIFIED. ) 
 CURVE ( )  GEOMETRIC_REPRESENTATION_ITEM ( )  RATIONAL_B_SPLINE_CURVE ( ( 0.9330127018922194093, 0.9330127018922194093, 1.000000000000000000, 0.8660254037844387076, 1.000000000000000000, 0.8660254037844387076, 1.000000000000000000, 0.9330127018922194093, 0.9330127018922194093 ) ) 
 REPRESENTATION_ITEM ( '' )  );
#47407 = EDGE_LOOP ( 'NONE', ( #62793, #7501, #6323, #49526 ) ) ;
#47408 = CARTESIAN_POINT ( 'NONE',  ( -4.458734124999999437, -72.31249999863439371, 0.000000000000000000 ) ) ;
#47409 = DIRECTION ( 'NONE',  ( -0.000000000000000000, 1.000000000000000000, -0.000000000000000000 ) ) ;
#47410 = CARTESIAN_POINT ( 'NONE',  ( 4.458734125000001214, 5.104166668032261711, 2.574251347313718519 ) ) ;
#47411 = CARTESIAN_POINT ( 'NONE',  ( 3.535533905932738197, -140.0000000027311842, -3.535533905932738197 ) ) ;
#47412 = CARTESIAN_POINT ( 'NONE',  ( -4.458734124999999437, -59.56249999863440081, 0.000000000000000000 ) ) ;
#47413 = CARTESIAN_POINT ( 'NONE',  ( 5.000000000000000000, -22.29166666393548368, -2.886751345948129988 ) ) ;
#47414 = CARTESIAN_POINT ( 'NONE',  ( -5.000000000000000000, -32.95833333060215153, -2.886751345948128211 ) ) ;
#47415 = CARTESIAN_POINT ( 'NONE',  ( -5.000000000000000000, -44.87499999726880873, 0.000000000000000000 ) ) ;
#47416 = CARTESIAN_POINT ( 'NONE',  ( -54.60164318462004474, -140.5000000027312126, -4.984105922594373794 ) ) ;
#47417 = CARTESIAN_POINT ( 'NONE',  ( 1.339745962155612702, -65.29465819873851729, -5.000000000000000000 ) ) ;
#47418 = CARTESIAN_POINT ( 'NONE',  ( -4.458734124999998549, -41.22916666530107221, 2.574251347313722516 ) ) ;
#47419 = CARTESIAN_POINT ( 'NONE',  ( 2.229367062499998831, -22.89583333196773651, -3.861377020970580887 ) ) ;
#47420 = ORIENTED_EDGE ( 'NONE', *, *, #33908, .F. ) ;
#47421 = CARTESIAN_POINT ( 'NONE',  ( 5.000000000000000000, 11.50000000000000000, -6.123233995736766282E-16 ) ) ;
#47422 = CARTESIAN_POINT ( 'NONE',  ( -4.458734124999999437, -108.3958333319677365, -2.574251347313719407 ) ) ;
#47423 = CARTESIAN_POINT ( 'NONE',  ( -2.071067811865478170, -153.4375000027312410, 5.000000000000000000 ) ) ;
#47424 = ORIENTED_EDGE ( 'NONE', *, *, #40976, .F. ) ;
#47425 = CARTESIAN_POINT ( 'NONE',  ( -2.229367062500000163, -109.7291666653010651, -3.861377020970580443 ) ) ;
#47426 = VECTOR ( 'NONE', #33646, 1000.000000000000000 ) ;
#47427 = CARTESIAN_POINT ( 'NONE',  ( -2.229367062500000163, -31.47916666530107577, -3.861377020970580443 ) ) ;
#47428 = CARTESIAN_POINT ( 'NONE',  ( -2.500000000000000444, -69.04166666393547303, -4.330127018922193649 ) ) ;
#47429 = CARTESIAN_POINT ( 'NONE',  ( -58.39396692619412477, -147.6875000013656063, 2.891590998281057701 ) ) ;
#47430 = CARTESIAN_POINT ( 'NONE',  ( 5.000000000000000888, -145.9375000000000000, -2.071067811865475505 ) ) ;
#47431 = CARTESIAN_POINT ( 'NONE',  ( 4.458734124999998549, -28.72916666530107221, -2.574251347313721627 ) ) ;
#47432 = CARTESIAN_POINT ( 'NONE',  ( 2.229367062500001939, -69.22916666530107932, 3.861377020970579999 ) ) ;
#47433 = CARTESIAN_POINT ( 'NONE',  ( 3.152801135295367541, -168.5625000013656063, -3.152801135295367541 ) ) ;
#47434 = CARTESIAN_POINT ( 'NONE',  ( 4.458734125000000326, -25.89583333196773651, 2.574251347313718519 ) ) ;
#47435 = CARTESIAN_POINT ( 'NONE',  ( 3.061616997868383141E-16, -146.7500000000000284, -5.000000000000000000 ) ) ;
#47436 = CYLINDRICAL_SURFACE ( 'NONE', #18456, 11.00000000000000000 ) ;
#47437 = CARTESIAN_POINT ( 'NONE',  ( 1.060575238724906964E-15, -17.75000000000000355, 5.773502691896257311 ) ) ;
#47438 = CARTESIAN_POINT ( 'NONE',  ( 3.152801135295366208, -146.5625000013655779, 3.152801135295367985 ) ) ;
#47439 = ORIENTED_EDGE ( 'NONE', *, *, #40976, .T. ) ;
#47440 = DIRECTION ( 'NONE',  ( -0.000000000000000000, 1.000000000000000000, -0.000000000000000000 ) ) ;
#47441 = CARTESIAN_POINT ( 'NONE',  ( 4.458734124999999437, -57.06249999863440081, -5.460374474430324690E-16 ) ) ;
#47442 = EDGE_CURVE ( 'NONE', #11069, #14391, #52925, .T. ) ;
#47443 = CARTESIAN_POINT ( 'NONE',  ( 5.000000000000000888, 26.54166666939785202, 2.886751345948126879 ) ) ;
#47444 = FACE_OUTER_BOUND ( 'NONE', #37641, .T. ) ;
#47445 = CARTESIAN_POINT ( 'NONE',  ( -2.500000000000000444, 21.83333333333333215, -4.330127018922193649 ) ) ;
#47446 = CARTESIAN_POINT ( 'NONE',  ( -3.152548672688508926E-16, -3.562499998634408360, -5.148502694627439702 ) ) ;
#47447 = CARTESIAN_POINT ( 'NONE',  ( -1.339745962155610925, -10.79465819873852261, 5.000000000000000000 ) ) ;
#47448 = CARTESIAN_POINT ( 'NONE',  ( -3.535533905932737309, -164.6250000000000284, -3.535533905932738197 ) ) ;
#47449 = CARTESIAN_POINT ( 'NONE',  ( 2.229367062500001939, 11.77083333469892601, 3.861377020970579999 ) ) ;
#47450 = ORIENTED_EDGE ( 'NONE', *, *, #61024, .F. ) ;
#47451 = CARTESIAN_POINT ( 'NONE',  ( -1.339745962155610925, -29.66965819600733312, 5.000000000000000000 ) ) ;
#47452 = VERTEX_POINT ( 'NONE', #60731 ) ;
#47453 = CARTESIAN_POINT ( 'NONE',  ( -1.339745962155613812, -24.08034179853029499, -5.000000000000000000 ) ) ;
#47454 = CARTESIAN_POINT ( 'NONE',  ( 2.229367062499998831, -50.64583333196772941, -3.861377020970580887 ) ) ;
#47455 = CARTESIAN_POINT ( 'NONE',  ( 3.152801135295366208, -160.8125000013656063, 3.152801135295367985 ) ) ;
#47456 = CARTESIAN_POINT ( 'NONE',  ( 1.060575238724906964E-15, -45.62499999726880873, 5.773502691896257311 ) ) ;
#47457 = ORIENTED_EDGE ( 'NONE', *, *, #42050, .T. ) ;
#47458 = CARTESIAN_POINT ( 'NONE',  ( 4.458734124999998549, -25.72916666530107221, -2.574251347313721627 ) ) ;
#47459 = ORIENTED_EDGE ( 'NONE', *, *, #29535, .T. ) ;
#47460 = CARTESIAN_POINT ( 'NONE',  ( 1.339745962155615144, -53.70534180126147561, 4.999999999999999112 ) ) ;
#47461 = CARTESIAN_POINT ( 'NONE',  ( -4.458734124999999437, -161.9375000013655779, -5.460374474430324690E-16 ) ) ;
#47462 = CARTESIAN_POINT ( 'NONE',  ( -2.499999999999996447, -38.70833333060213732, 4.330127018922195425 ) ) ;
#47463 = CARTESIAN_POINT ( 'NONE',  ( -51.75738570946856498, -136.7500000000000284, 3.805975901505576964 ) ) ;
#47464 = CARTESIAN_POINT ( 'NONE',  ( -2.229367062499996610, -40.39583333196773651, 3.861377020970582219 ) ) ;
#47465 = VERTEX_POINT ( 'NONE', #16653 ) ;
#47466 = CARTESIAN_POINT ( 'NONE',  ( 4.458734124999999437, -83.81249999863439371, -5.460374474430324690E-16 ) ) ;
#47467 = CARTESIAN_POINT ( 'NONE',  ( -3.152548672688508926E-16, 23.43750000136559564, -5.148502694627439702 ) ) ;
#47468 = DIRECTION ( 'NONE',  ( -0.000000000000000000, 1.000000000000000000, -0.000000000000000000 ) ) ;
#47469 = VERTEX_POINT ( 'NONE', #599 ) ;
#47470 = DIRECTION ( 'NONE',  ( -0.6485228581062915110, 0.000000000000000000, -0.7611951803011149931 ) ) ;
#47471 = CARTESIAN_POINT ( 'NONE',  ( -57.89159099828107458, -139.9375000013656063, -3.393966926194107447 ) ) ;
#47472 = CARTESIAN_POINT ( 'NONE',  ( -4.458734124999999437, -84.56249999863439371, 0.000000000000000000 ) ) ;
#47473 = CARTESIAN_POINT ( 'NONE',  ( -56.66612745406270335, -132.4375000027312410, -5.149110718188516067 ) ) ;
#47474 = LINE ( 'NONE', #17589, #3818 ) ;
#47475 = CARTESIAN_POINT ( 'NONE',  ( -3.152801135295367985, -140.0625000013655779, 3.152801135295367096 ) ) ;
#47476 = CARTESIAN_POINT ( 'NONE',  ( 3.535533905932736864, -145.2500000027311842, 3.535533905932738641 ) ) ;
#47477 = CARTESIAN_POINT ( 'NONE',  ( 9.457646018065525792E-16, -52.06249999863440792, 5.148502694627439702 ) ) ;
#47478 = CARTESIAN_POINT ( 'NONE',  ( 4.458734124999998549, 23.27083333469892423, -2.574251347313721627 ) ) ;
#47479 = ADVANCED_FACE ( 'NONE', ( #59453 ), #15384, .T. ) ;
#47480 =( BOUNDED_CURVE ( )  B_SPLINE_CURVE ( 2, ( #27393, #7790, #37680, #46701, #42818, #7163, #26773, #32861, #3600 ),
 .UNSPECIFIED., .F., .F. ) 
 B_SPLINE_CURVE_WITH_KNOTS ( ( 3, 2, 2, 2, 3 ),
 ( 0.5803571428571429047, 0.5809523809523809978, 0.5821428571428571841, 0.5833333333333333703, 0.5839285714285714635 ),
 .UNSPECIFIED. ) 
 CURVE ( )  GEOMETRIC_REPRESENTATION_ITEM ( )  RATIONAL_B_SPLINE_CURVE ( ( 0.9330127018922194093, 0.9330127018922194093, 1.000000000000000000, 0.8660254037844387076, 1.000000000000000000, 0.8660254037844387076, 1.000000000000000000, 0.9330127018922194093, 0.9330127018922194093 ) ) 
 REPRESENTATION_ITEM ( '' )  );
#47481 = CYLINDRICAL_SURFACE ( 'NONE', #55335, 5.000000000000000000 ) ;
#47482 = CARTESIAN_POINT ( 'NONE',  ( -7.549004593702450805, -4.358419834287835748, -7.700121441565821456 ) ) ;
#47483 = CARTESIAN_POINT ( 'NONE',  ( 4.458734125000001214, -42.14583333196773651, 2.574251347313718519 ) ) ;
#47484 = CARTESIAN_POINT ( 'NONE',  ( -3.535250795749689387E-16, -6.124999997268812280, -5.773502691896257311 ) ) ;
#47485 = CARTESIAN_POINT ( 'NONE',  ( -5.000000000000000000, -73.08333333333332860, -2.886751345948128211 ) ) ;
#47486 = CARTESIAN_POINT ( 'NONE',  ( 0.000000000000000000, -120.0000000000000000, 0.000000000000000000 ) ) ;
#47487 = CARTESIAN_POINT ( 'NONE',  ( -4.458734124999999437, -86.64583333196773651, -2.574251347313719407 ) ) ;
#47488 = CARTESIAN_POINT ( 'NONE',  ( 4.458734125000000326, -103.8958333319677365, 2.574251347313718519 ) ) ;
#47489 = CARTESIAN_POINT ( 'NONE',  ( -2.229367062500000163, -4.729166665301071326, -3.861377020970580443 ) ) ;
#47490 = VERTEX_POINT ( 'NONE', #44969 ) ;
#47491 = CARTESIAN_POINT ( 'NONE',  ( 5.000000000000000888, -47.58333333333333570, 2.886751345948126879 ) ) ;
#47492 = CARTESIAN_POINT ( 'NONE',  ( 4.458734125000001214, -90.89583333196772230, 2.574251347313718519 ) ) ;
#47493 = CARTESIAN_POINT ( 'NONE',  ( -2.071067811865478170, -164.4375000027311842, 5.000000000000000000 ) ) ;
#47494 = CARTESIAN_POINT ( 'NONE',  ( 4.458734124999998549, -93.97916666530106511, -2.574251347313721627 ) ) ;
#47495 = CARTESIAN_POINT ( 'NONE',  ( -2.229367062500000163, 9.270833334698927786, -3.861377020970580443 ) ) ;
#47496 = DIRECTION ( 'NONE',  ( -0.000000000000000000, 1.000000000000000000, -0.000000000000000000 ) ) ;
#47497 = CARTESIAN_POINT ( 'NONE',  ( -52.10840900171896806, -130.1875000013656063, 3.393966926194110556 ) ) ;
#47498 =( BOUNDED_CURVE ( )  B_SPLINE_CURVE ( 2, ( #58595, #28367, #47988, #48613, #14514, #3942, #62799, #35420, #31222 ),
 .UNSPECIFIED., .F., .F. ) 
 B_SPLINE_CURVE_WITH_KNOTS ( ( 3, 2, 2, 2, 3 ),
 ( 0.1437499999999999889, 0.1444444444444444309, 0.1458333333333333426, 0.1472222222222222265, 0.1479166666666666685 ),
 .UNSPECIFIED. ) 
 CURVE ( )  GEOMETRIC_REPRESENTATION_ITEM ( )  RATIONAL_B_SPLINE_CURVE ( ( 0.9330127018922194093, 0.9330127018922194093, 1.000000000000000000, 0.8660254037844387076, 1.000000000000000000, 0.8660254037844387076, 1.000000000000000000, 0.9330127018922194093, 0.9330127018922194093 ) ) 
 REPRESENTATION_ITEM ( '' )  );
#47499 = ADVANCED_FACE ( 'NONE', ( #932 ), #54941, .T. ) ;
#47500 = CARTESIAN_POINT ( 'NONE',  ( -3.152548672688508926E-16, -11.56249999863440792, -5.148502694627439702 ) ) ;
#47501 = CARTESIAN_POINT ( 'NONE',  ( 4.458734125000001214, 12.85416666803226171, 2.574251347313718519 ) ) ;
#47502 = EDGE_CURVE ( 'NONE', #35740, #43806, #839, .T. ) ;
#47503 = CARTESIAN_POINT ( 'NONE',  ( -2.229367062499996610, -51.39583333196773651, 3.861377020970582219 ) ) ;
#47504 = FACE_OUTER_BOUND ( 'NONE', #16334, .T. ) ;
#47505 = CARTESIAN_POINT ( 'NONE',  ( -5.000000000000000000, -37.00000000000000711, 0.000000000000000000 ) ) ;
#47506 = CARTESIAN_POINT ( 'NONE',  ( -4.458734124999997661, -10.22916666530106866, 2.574251347313722516 ) ) ;
#47507 = CARTESIAN_POINT ( 'NONE',  ( 7.500000000000000000, -4.330127018922199866, -10.00000000000000000 ) ) ;
#47508 = ORIENTED_EDGE ( 'NONE', *, *, #5090, .T. ) ;
#47509 = CARTESIAN_POINT ( 'NONE',  ( -4.458734124999999437, -37.56249999863440792, 0.000000000000000000 ) ) ;
#47510 = CARTESIAN_POINT ( 'NONE',  ( -50.55543936806279248, -127.3125000013655921, 0.3552334253322060320 ) ) ;
#47511 = CARTESIAN_POINT ( 'NONE',  ( 5.000000000000000000, -68.41666666666667140, -2.886751345948130876 ) ) ;
#47512 = CARTESIAN_POINT ( 'NONE',  ( -5.000000000000000000, -28.08333333333333925, -2.886751345948128211 ) ) ;
#47513 = CARTESIAN_POINT ( 'NONE',  ( -4.458734124999999437, -81.31249999863440792, 0.000000000000000000 ) ) ;
#47514 = CARTESIAN_POINT ( 'NONE',  ( 2.229367062500001939, 24.77083333469892779, 3.861377020970579999 ) ) ;
#47515 = EDGE_CURVE ( 'NONE', #62207, #45023, #61678, .T. ) ;
#47516 = CARTESIAN_POINT ( 'NONE',  ( -2.229367062499996610, 15.85416666803226171, 3.861377020970582219 ) ) ;
#47517 = DIRECTION ( 'NONE',  ( 0.000000000000000000, 0.000000000000000000, 1.000000000000000000 ) ) ;
#47518 = CARTESIAN_POINT ( 'NONE',  ( 0.000000000000000000, -120.0000000000000000, 0.000000000000000000 ) ) ;
#47519 = CARTESIAN_POINT ( 'NONE',  ( 4.458734124999999437, -84.06249999863439371, -5.460374474430324690E-16 ) ) ;
#47520 = CARTESIAN_POINT ( 'NONE',  ( 5.000000000000000888, -68.58333333333334281, 2.886751345948126879 ) ) ;
#47521 = CARTESIAN_POINT ( 'NONE',  ( -5.000000000000000000, 18.12500000273118417, 0.000000000000000000 ) ) ;
#47522 = VERTEX_POINT ( 'NONE', #36584 ) ;
#47523 = DIRECTION ( 'NONE',  ( -0.000000000000000000, 1.000000000000000000, -0.000000000000000000 ) ) ;
#47524 = CYLINDRICAL_SURFACE ( 'NONE', #28862, 5.000000000000000000 ) ;
#47526 = CARTESIAN_POINT ( 'NONE',  ( -3.535250795749689387E-16, -31.25000000000000000, -5.773502691896257311 ) ) ;
#47525 = CARTESIAN_POINT ( 'NONE',  ( 5.000000000000000000, -52.41666666666666430, -2.886751345948130876 ) ) ;
#47527 = CARTESIAN_POINT ( 'NONE',  ( -2.229367062500000163, -35.47916666530107221, -3.861377020970580443 ) ) ;
#47528 = CARTESIAN_POINT ( 'NONE',  ( 1.339745962155615144, -62.70534180126146850, 4.999999999999999112 ) ) ;
#47529 = CARTESIAN_POINT ( 'NONE',  ( 1.060575238724906964E-15, -30.62499999726881228, 5.773502691896257311 ) ) ;
#47530 = EDGE_CURVE ( 'NONE', #50712, #28828, #62307, .T. ) ;
#47532 = EDGE_LOOP ( 'NONE', ( #46122, #47545, #36477, #16085 ) ) ;
#47531 = CARTESIAN_POINT ( 'NONE',  ( -2.229367062500000163, -58.47916666530106511, -3.861377020970580443 ) ) ;
#47533 = DIRECTION ( 'NONE',  ( -0.000000000000000000, 1.000000000000000000, -0.000000000000000000 ) ) ;
#47535 = ORIENTED_EDGE ( 'NONE', *, *, #15415, .T. ) ;
#47534 = CARTESIAN_POINT ( 'NONE',  ( -4.458734124999998549, -7.479166665301073991, 2.574251347313722516 ) ) ;
#47536 = CARTESIAN_POINT ( 'NONE',  ( -5.000000000000000000, -78.08333333333332860, -2.886751345948128211 ) ) ;
#47537 = CARTESIAN_POINT ( 'NONE',  ( -50.55543936806279248, -136.0625000013656063, 0.3552334253322060320 ) ) ;
#47538 = CARTESIAN_POINT ( 'NONE',  ( -4.458734124999999437, -49.56249999863440792, 0.000000000000000000 ) ) ;
#47539 = CARTESIAN_POINT ( 'NONE',  ( -5.000000000000000000, -77.87499999726881583, 0.000000000000000000 ) ) ;
#47541 = VERTEX_POINT ( 'NONE', #56218 ) ;
#47540 = CARTESIAN_POINT ( 'NONE',  ( -5.000000000000000000, -54.87499999726880162, 0.000000000000000000 ) ) ;
#47542 = CARTESIAN_POINT ( 'NONE',  ( -59.81910112700025905, -151.1875000000000000, -2.462841084822630311 ) ) ;
#47543 = CARTESIAN_POINT ( 'NONE',  ( -4.458734124999998549, -20.47916666530107577, 2.574251347313722516 ) ) ;
#47545 = ORIENTED_EDGE ( 'NONE', *, *, #60184, .T. ) ;
#47544 = CARTESIAN_POINT ( 'NONE',  ( 2.229367062500001939, -57.22916666530107932, 3.861377020970579999 ) ) ;
#47546 = DIRECTION ( 'NONE',  ( -0.6485228581062917330, 0.000000000000000000, -0.7611951803011149931 ) ) ;
#47547 = CARTESIAN_POINT ( 'NONE',  ( 4.458734125000000326, -140.3750000013656063, -1.846868145590734978 ) ) ;
#47548 = CARTESIAN_POINT ( 'NONE',  ( -2.229367062500000163, -97.72916666530105090, -3.861377020970580443 ) ) ;
#47549 = CARTESIAN_POINT ( 'NONE',  ( -5.000000000000000000, 18.00000000000000000, 0.000000000000000000 ) ) ;
#47550 = ORIENTED_EDGE ( 'NONE', *, *, #63552, .T. ) ;
#47551 = CARTESIAN_POINT ( 'NONE',  ( -51.60603307380591787, -151.1875000013656063, -2.891590998281053704 ) ) ;
#47552 = CARTESIAN_POINT ( 'NONE',  ( -59.81910112700025905, -144.3125000027312126, -2.462841084822630311 ) ) ;
#47553 =( BOUNDED_CURVE ( )  B_SPLINE_CURVE ( 2, ( #28916, #19583, #48539, #58194, #58822, #49494, #29538, #19263, #63039 ),
 .UNSPECIFIED., .F., .F. ) 
 B_SPLINE_CURVE_WITH_KNOTS ( ( 3, 2, 2, 2, 3 ),
 ( 0.9749999999999998668, 0.9791666666666665186, 0.9833333333333331705, 0.9874999999999999334, 0.9916666666666665853 ),
 .UNSPECIFIED. ) 
 CURVE ( )  GEOMETRIC_REPRESENTATION_ITEM ( )  RATIONAL_B_SPLINE_CURVE ( ( 1.000000000000001998, 0.9238795325112847401, 1.000000000000000000, 0.9238795325112867385, 1.000000000000000000, 0.9238795325112867385, 1.000000000000000000, 0.9238795325112887369, 0.9999999999999980016 ) ) 
 REPRESENTATION_ITEM ( '' )  );
#47554 = CARTESIAN_POINT ( 'NONE',  ( 1.339745962155615144, -83.70534180126149693, 4.999999999999999112 ) ) ;
#47555 = ADVANCED_FACE ( 'NONE', ( #37533 ), #27561, .T. ) ;
#47556 = CARTESIAN_POINT ( 'NONE',  ( 4.458734124999998549, -5.729166665301072214, -2.574251347313721627 ) ) ;
#47557 = CARTESIAN_POINT ( 'NONE',  ( -4.458734124999999437, -93.64583333196772230, -2.574251347313719407 ) ) ;
#47558 = ADVANCED_FACE ( 'NONE', ( #2202 ), #27877, .T. ) ;
#47559 = CARTESIAN_POINT ( 'NONE',  ( -4.458734125000001214, -144.1250000013655779, 1.846868145590734089 ) ) ;
#47560 = CARTESIAN_POINT ( 'NONE',  ( 4.458734125000001214, -30.14583333196773296, 2.574251347313718519 ) ) ;
#47561 = DIRECTION ( 'NONE',  ( -0.000000000000000000, 1.000000000000000000, -0.000000000000000000 ) ) ;
#47562 = CARTESIAN_POINT ( 'NONE',  ( -57.19623071787017210, -135.3750000013656063, 4.297418129356382899 ) ) ;
#47563 = CARTESIAN_POINT ( 'NONE',  ( -3.152548672688508926E-16, -66.81249999863442213, -5.148502694627439702 ) ) ;
#47564 = CARTESIAN_POINT ( 'NONE',  ( 5.000000000000000000, -17.41666666666666430, -2.886751345948130876 ) ) ;
#47565 = CARTESIAN_POINT ( 'NONE',  ( -1.846868145590737420, -139.7500000013655779, 4.458734124999997661 ) ) ;
#47566 = CARTESIAN_POINT ( 'NONE',  ( -2.229367062499996610, 12.60416666803226171, 3.861377020970582219 ) ) ;
#47567 = ORIENTED_EDGE ( 'NONE', *, *, #6078, .T. ) ;
#47568 = CARTESIAN_POINT ( 'NONE',  ( -4.999999999999998224, -49.79166666393547303, 2.886751345948131764 ) ) ;
#47569 = DIRECTION ( 'NONE',  ( -0.000000000000000000, 1.000000000000000000, -0.000000000000000000 ) ) ;
#47571 = CARTESIAN_POINT ( 'NONE',  ( -2.229367062500000163, -22.47916666530107221, -3.861377020970580443 ) ) ;
#47570 = CARTESIAN_POINT ( 'NONE',  ( 2.500000000000002220, -89.66666666666665719, 4.330127018922192761 ) ) ;
#47572 = CARTESIAN_POINT ( 'NONE',  ( 6.324555320336760822, 0.000000000000000000, 8.999999999999998224 ) ) ;
#47573 = CARTESIAN_POINT ( 'NONE',  ( -4.458734124999999437, -78.64583333196773651, -2.574251347313719407 ) ) ;
#47574 = CARTESIAN_POINT ( 'NONE',  ( -4.458734124999997661, 26.52083333469892779, 2.574251347313722516 ) ) ;
#47575 = FACE_OUTER_BOUND ( 'NONE', #18595, .T. ) ;
#47576 = CARTESIAN_POINT ( 'NONE',  ( -50.70258187064364108, -144.1250000013656063, 2.196230717870141014 ) ) ;
#47577 = CARTESIAN_POINT ( 'NONE',  ( -2.229367062499996610, 0.8541666680322613781, 3.861377020970582219 ) ) ;
#47578 = CARTESIAN_POINT ( 'NONE',  ( -3.152548672688508926E-16, 28.18750000136559564, -5.148502694627439702 ) ) ;
#47579 = EDGE_CURVE ( 'NONE', #53022, #13464, #7335, .T. ) ;
#47580 = CARTESIAN_POINT ( 'NONE',  ( -2.229367062500000163, -37.72916666530107221, -3.861377020970580443 ) ) ;
#47581 = CARTESIAN_POINT ( 'NONE',  ( 2.500000000000002220, -43.54166666393548013, 4.330127018922192761 ) ) ;
#47582 = CARTESIAN_POINT ( 'NONE',  ( 9.457646018065525792E-16, 7.937500001365596525, 5.148502694627439702 ) ) ;
#47583 = CARTESIAN_POINT ( 'NONE',  ( -2.229367062499996610, -70.14583333196773651, 3.861377020970582219 ) ) ;
#47584 = CARTESIAN_POINT ( 'NONE',  ( -3.152548672688508926E-16, -20.81249999863440081, -5.148502694627439702 ) ) ;
#47585 = CARTESIAN_POINT ( 'NONE',  ( 5.000000000000000888, -6.583333333333329485, 2.886751345948126879 ) ) ;
#47586 = CARTESIAN_POINT ( 'NONE',  ( -4.458734125000001214, -157.8750000013656063, 1.846868145590734089 ) ) ;
#47587 = CARTESIAN_POINT ( 'NONE',  ( -5.000000000000000888, -158.4375000000000568, 2.071067811865474617 ) ) ;
#47588 = CARTESIAN_POINT ( 'NONE',  ( 4.458734124999999437, -64.81249999863440792, -5.460374474430324690E-16 ) ) ;
#47589 = CARTESIAN_POINT ( 'NONE',  ( -2.500000000000000444, -100.0416666639354588, -4.330127018922193649 ) ) ;
#47590 = CARTESIAN_POINT ( 'NONE',  ( 5.000000000000000000, 15.50000000000000000, -6.123233995736766282E-16 ) ) ;
#47591 = CARTESIAN_POINT ( 'NONE',  ( -3.152548672688508926E-16, -39.56249999863440081, -5.148502694627439702 ) ) ;
#47592 = CARTESIAN_POINT ( 'NONE',  ( -2.500000000000000444, -84.16666666666667140, -4.330127018922193649 ) ) ;
#47593 = CARTESIAN_POINT ( 'NONE',  ( -2.229367062500000163, -108.7291666653010651, -3.861377020970580443 ) ) ;
#47594 = CARTESIAN_POINT ( 'NONE',  ( 4.458734124999999437, -66.06249999863440792, -5.460374474430324690E-16 ) ) ;
#47595 = CARTESIAN_POINT ( 'NONE',  ( 5.000000000000000888, -55.58333333333333570, 2.886751345948126879 ) ) ;
#47596 = DIRECTION ( 'NONE',  ( 0.000000000000000000, 1.000000000000000000, 0.000000000000000000 ) ) ;
#47597 = EDGE_LOOP ( 'NONE', ( #49880, #26893, #57521, #22679 ) ) ;
#47598 = CARTESIAN_POINT ( 'NONE',  ( -5.000000000000000000, 15.04166666939785202, -2.886751345948128211 ) ) ;
#47599 = CARTESIAN_POINT ( 'NONE',  ( 1.975475456537005874E-15, 12.37500000273118417, 5.000000000000000000 ) ) ;
#47600 = CARTESIAN_POINT ( 'NONE',  ( -4.999999999999999112, -12.91666666666666785, 2.886751345948131764 ) ) ;
#47601 = CARTESIAN_POINT ( 'NONE',  ( 4.458734125000001214, -16.89583333196773651, 2.574251347313718519 ) ) ;
#47602 = CARTESIAN_POINT ( 'NONE',  ( 4.458734124999998549, -76.72916666530106511, -2.574251347313721627 ) ) ;
#47603 = CARTESIAN_POINT ( 'NONE',  ( -5.000000000000000000, -5.999999999999998224, 0.000000000000000000 ) ) ;
#47604 = CARTESIAN_POINT ( 'NONE',  ( -2.500000000000000444, -11.04166666393547835, -4.330127018922193649 ) ) ;
#47606 = ORIENTED_EDGE ( 'NONE', *, *, #44521, .F. ) ;
#47605 = CARTESIAN_POINT ( 'NONE',  ( 4.458734124999999437, -44.81249999863440081, -5.460374474430324690E-16 ) ) ;
#47607 = CARTESIAN_POINT ( 'NONE',  ( 5.000000000000000000, -41.41666666666667140, -2.886751345948130876 ) ) ;
#47609 = ORIENTED_EDGE ( 'NONE', *, *, #53448, .F. ) ;
#47608 = CARTESIAN_POINT ( 'NONE',  ( 2.229367062499998831, 5.104166668032261711, -3.861377020970580887 ) ) ;
#47610 = CARTESIAN_POINT ( 'NONE',  ( 1.975475456537005874E-15, -81.62499999726881583, 5.000000000000000000 ) ) ;
#47611 = CARTESIAN_POINT ( 'NONE',  ( 2.500000000000002220, -59.66666666666665719, 4.330127018922192761 ) ) ;
#47612 = CARTESIAN_POINT ( 'NONE',  ( 2.730187237215162345E-16, -161.4375000013655779, -4.458734124999999437 ) ) ;
#47613 = B_SPLINE_CURVE_WITH_KNOTS ( 'NONE', 3,
 ( #13845, #63383, #9025, #22886, #3892, #57617 ),
 .UNSPECIFIED., .F., .F.,
 ( 4, 2, 4 ),
 ( 0.004615310220740751271, 0.006918661718823357169, 0.009222013216905963068 ),
 .UNSPECIFIED. ) ;
#47614 = CARTESIAN_POINT ( 'NONE',  ( 4.458734124999999437, -34.06249999863440792, -5.460374474430324690E-16 ) ) ;
#47615 = CARTESIAN_POINT ( 'NONE',  ( 5.000000000000000888, -14.58333333333333215, 2.886751345948126879 ) ) ;
#47616 = CARTESIAN_POINT ( 'NONE',  ( 2.071067811865475505, -167.8125000000000284, -5.000000000000000888 ) ) ;
#47617 = CARTESIAN_POINT ( 'NONE',  ( -6.972266317189433020E-16, -11.25000000000000178, -5.000000000000000000 ) ) ;
#47618 = CARTESIAN_POINT ( 'NONE',  ( -50.40829686548195099, -129.2500000013656347, -1.485763867205728284 ) ) ;
#47619 = CARTESIAN_POINT ( 'NONE',  ( -2.229367062499996610, -6.395833331967741842, 3.861377020970582219 ) ) ;
#47620 = CARTESIAN_POINT ( 'NONE',  ( 4.458734124999998549, -40.97916666530107932, -2.574251347313721627 ) ) ;
#47621 = CARTESIAN_POINT ( 'NONE',  ( 5.000000000000000000, -54.41666666666667140, -2.886751345948130876 ) ) ;
#47622 = CARTESIAN_POINT ( 'NONE',  ( 4.458734124999999437, -84.06249999863439371, -5.460374474430324690E-16 ) ) ;
#47623 = CARTESIAN_POINT ( 'NONE',  ( -6.972266317189433020E-16, -84.24999999999998579, -5.000000000000000000 ) ) ;
#47624 = ORIENTED_EDGE ( 'NONE', *, *, #42564, .F. ) ;
#47625 = CARTESIAN_POINT ( 'NONE',  ( -53.33387254593733928, -152.9375000027312126, 5.149110718188519620 ) ) ;
#47626 = CARTESIAN_POINT ( 'NONE',  ( -5.000000000000000000, -105.0000000000000142, 0.000000000000000000 ) ) ;
#47627 = CARTESIAN_POINT ( 'NONE',  ( 9.457646018065525792E-16, -67.31249999863440792, 5.148502694627439702 ) ) ;
#47628 = CARTESIAN_POINT ( 'NONE',  ( -1.846868145590737420, -147.0000000013656063, 4.458734124999997661 ) ) ;
#47629 = EDGE_LOOP ( 'NONE', ( #55502, #54758, #42813, #6546 ) ) ;
#47630 = EDGE_CURVE ( 'NONE', #1769, #21623, #37227, .T. ) ;
#47631 = ADVANCED_FACE ( 'NONE', ( #22756 ), #21806, .F. ) ;
#47632 = CARTESIAN_POINT ( 'NONE',  ( 5.000000000000000000, -3.291666663935478354, -2.886751345948130876 ) ) ;
#47633 = CARTESIAN_POINT ( 'NONE',  ( -2.229367062500000163, -14.72916666530107221, -3.861377020970580443 ) ) ;
#47634 = ADVANCED_FACE ( 'NONE', ( #32393 ), #27251, .T. ) ;
#47635 = CARTESIAN_POINT ( 'NONE',  ( -5.000000000000000000, -35.08333333333332860, -2.886751345948128211 ) ) ;
#47636 = CARTESIAN_POINT ( 'NONE',  ( -4.458734124999998549, 2.770833334698928674, 2.574251347313722516 ) ) ;
#47637 = CARTESIAN_POINT ( 'NONE',  ( -6.972266317189433020E-16, -96.12499999726880162, -5.000000000000000000 ) ) ;
#47638 = CARTESIAN_POINT ( 'NONE',  ( 1.846868145590736310, -154.6250000013655779, 4.458734124999997661 ) ) ;
#47639 = CARTESIAN_POINT ( 'NONE',  ( 2.229367062499998831, 25.10416666803225993, -3.861377020970580887 ) ) ;
#47640 = VERTEX_POINT ( 'NONE', #17285 ) ;
#47641 = CARTESIAN_POINT ( 'NONE',  ( 4.458734124999999437, -90.81249999863440792, -5.460374474430324690E-16 ) ) ;
#47642 = CARTESIAN_POINT ( 'NONE',  ( -2.499999999999996447, -30.83333333333333215, 4.330127018922195425 ) ) ;
#47643 = CARTESIAN_POINT ( 'NONE',  ( 1.339745962155615144, 7.419658201469705894, 4.999999999999999112 ) ) ;
#47644 = CARTESIAN_POINT ( 'NONE',  ( -4.458734124999998549, -8.229166665301073991, 2.574251347313722516 ) ) ;
#47645 = EDGE_CURVE ( 'NONE', #43789, #4593, #47194, .T. ) ;
#47647 = EDGE_CURVE ( 'NONE', #56674, #5292, #7416, .T. ) ;
#47646 = CARTESIAN_POINT ( 'NONE',  ( 3.750000000000005329, 6.495190528383288253, 0.000000000000000000 ) ) ;
#47648 = CYLINDRICAL_SURFACE ( 'NONE', #54031, 5.000000000000000000 ) ;
#47649 = CARTESIAN_POINT ( 'NONE',  ( 5.000000000000000000, -36.37499999726881583, -6.123233995736766282E-16 ) ) ;
#47650 = CARTESIAN_POINT ( 'NONE',  ( 4.458734125000000326, 20.10416666803225638, 2.574251347313718519 ) ) ;
#47651 = CARTESIAN_POINT ( 'NONE',  ( -5.000000000000000000, -4.083333333333334814, -2.886751345948128211 ) ) ;
#47652 = CARTESIAN_POINT ( 'NONE',  ( -3.152548672688508926E-16, 24.43750000136559564, -5.148502694627439702 ) ) ;
#47653 = EDGE_CURVE ( 'NONE', #36379, #11571, #20559, .T. ) ;
#47654 = CARTESIAN_POINT ( 'NONE',  ( -4.458734124999998549, -54.22916666530107221, 2.574251347313722516 ) ) ;
#47655 = CARTESIAN_POINT ( 'NONE',  ( 4.458734124999999437, -4.062499998634408804, -5.460374474430324690E-16 ) ) ;
#47656 = CARTESIAN_POINT ( 'NONE',  ( 1.975475456537005874E-15, -63.74999999999998579, 5.000000000000000000 ) ) ;
#47657 = CARTESIAN_POINT ( 'NONE',  ( 5.000000000000000000, 7.583333333333333925, -2.886751345948129988 ) ) ;
#47658 = EDGE_CURVE ( 'NONE', #60221, #4973, #9691, .T. ) ;
#47659 = CARTESIAN_POINT ( 'NONE',  ( -2.071067811865475061, -139.8125000027312126, -5.000000000000000888 ) ) ;
#47661 = EDGE_CURVE ( 'NONE', #29252, #60646, #22520, .T. ) ;
#47660 = CARTESIAN_POINT ( 'NONE',  ( -2.500000000000000444, -52.16666666666666430, -4.330127018922193649 ) ) ;
#47662 = CARTESIAN_POINT ( 'NONE',  ( 4.458734125000001214, -45.89583333196774362, 2.574251347313718519 ) ) ;
#47663 = CARTESIAN_POINT ( 'NONE',  ( -2.500000000000000444, -86.04166666393547303, -4.330127018922193649 ) ) ;
#47664 = CARTESIAN_POINT ( 'NONE',  ( -59.29741812935640155, -137.8750000013655779, -2.196230717870135685 ) ) ;
#47665 = CARTESIAN_POINT ( 'NONE',  ( 0.000000000000000000, 0.000000000000000000, 0.000000000000000000 ) ) ;
#47666 = CARTESIAN_POINT ( 'NONE',  ( -2.499999999999996447, -104.7083333306021444, 4.330127018922195425 ) ) ;
#47667 = CARTESIAN_POINT ( 'NONE',  ( 9.457646018065525792E-16, -92.31249999863440792, 5.148502694627439702 ) ) ;
#47668 = CARTESIAN_POINT ( 'NONE',  ( 4.458734124999997661, -156.7500000013656063, 1.846868145590737864 ) ) ;
#47669 = CARTESIAN_POINT ( 'NONE',  ( 5.000000000000000000, -37.41666666666666430, -2.886751345948129988 ) ) ;
#47670 = CARTESIAN_POINT ( 'NONE',  ( 1.339745962155641346, 8.830341803992666883, -4.999999999999983125 ) ) ;
#47671 = EDGE_LOOP ( 'NONE', ( #59096, #12942, #39158, #32887 ) ) ;
#47672 = CARTESIAN_POINT ( 'NONE',  ( 4.458734124999999437, 15.93750000136559564, -5.460374474430324690E-16 ) ) ;
#47673 = ORIENTED_EDGE ( 'NONE', *, *, #30204, .F. ) ;
#47674 = CARTESIAN_POINT ( 'NONE',  ( 9.457646018065525792E-16, -96.06249999863440792, 5.148502694627439702 ) ) ;
#47675 = CARTESIAN_POINT ( 'NONE',  ( -2.229367062499996610, 6.604166668032259935, 3.861377020970582219 ) ) ;
#47676 = CARTESIAN_POINT ( 'NONE',  ( 2.499999999999998668, 9.791666669397850242, -4.330127018922193649 ) ) ;
#47677 = DIRECTION ( 'NONE',  ( -0.000000000000000000, 1.000000000000000000, -0.000000000000000000 ) ) ;
#47678 = CARTESIAN_POINT ( 'NONE',  ( 5.000000000000000888, 1.416666666666666741, 2.886751345948126879 ) ) ;
#47679 = CARTESIAN_POINT ( 'NONE',  ( -4.458734124999999437, -63.39583333196772941, -2.574251347313719407 ) ) ;
#47680 =( BOUNDED_CURVE ( )  B_SPLINE_CURVE ( 2, ( #45362, #29920, #30557, #54048, #1327, #20926, #25101, #44393, #6134 ),
 .UNSPECIFIED., .F., .F. ) 
 B_SPLINE_CURVE_WITH_KNOTS ( ( 3, 2, 2, 2, 3 ),
 ( 0.05535714285714286170, 0.05595238095238095483, 0.05714285714285714107, 0.05833333333333333426, 0.05892857142857142738 ),
 .UNSPECIFIED. ) 
 CURVE ( )  GEOMETRIC_REPRESENTATION_ITEM ( )  RATIONAL_B_SPLINE_CURVE ( ( 0.9330127018922194093, 0.9330127018922197424, 1.000000000000000000, 0.8660254037844387076, 1.000000000000000000, 0.8660254037844387076, 1.000000000000000000, 0.9330127018922194093, 0.9330127018922194093 ) ) 
 REPRESENTATION_ITEM ( '' )  );
#47681 = CARTESIAN_POINT ( 'NONE',  ( -4.769696007084728073, -120.0000000000000000, 1.499999999999999556 ) ) ;
#47682 = CARTESIAN_POINT ( 'NONE',  ( -2.229367062499996610, -29.14583333196774007, 3.861377020970582219 ) ) ;
#47683 = DIRECTION ( 'NONE',  ( -0.000000000000000000, 1.000000000000000000, -0.000000000000000000 ) ) ;
#47684 = FACE_OUTER_BOUND ( 'NONE', #51036, .T. ) ;
#47685 = CARTESIAN_POINT ( 'NONE',  ( 1.975475456537005874E-15, -5.624999997268812280, 5.000000000000000000 ) ) ;
#47686 = CARTESIAN_POINT ( 'NONE',  ( 5.000000000000000000, -47.41666666666666430, -2.886751345948129988 ) ) ;
#47687 = LINE ( 'NONE', #32904, #24328 ) ;
#47689 = CARTESIAN_POINT ( 'NONE',  ( -4.458734124999999437, -19.64583333196774362, -2.574251347313719407 ) ) ;
#47688 = CARTESIAN_POINT ( 'NONE',  ( 5.000000000000000000, -26.29166666393547658, -2.886751345948130876 ) ) ;
#47690 = CARTESIAN_POINT ( 'NONE',  ( -1.339745962155613812, -58.20534180126147561, -5.000000000000000000 ) ) ;
#47691 = CARTESIAN_POINT ( 'NONE',  ( 2.229367062499998831, -63.64583333196772941, -3.861377020970580887 ) ) ;
#47692 = CARTESIAN_POINT ( 'NONE',  ( 1.846868145590735200, -148.5000000013656347, -4.458734125000000326 ) ) ;
#47693 = CARTESIAN_POINT ( 'NONE',  ( 4.458734124999998549, -74.72916666530106511, -2.574251347313721627 ) ) ;
#47694 = CARTESIAN_POINT ( 'NONE',  ( -50.40829686548195099, -144.2500000013656063, -1.485763867205728284 ) ) ;
#47695 = CARTESIAN_POINT ( 'NONE',  ( 4.458734124999999437, -27.06249999863440081, -5.460374474430324690E-16 ) ) ;
#47696 = CARTESIAN_POINT ( 'NONE',  ( -5.000000000000000000, -68.87499999726880162, 0.000000000000000000 ) ) ;
#47697 = ORIENTED_EDGE ( 'NONE', *, *, #18939, .F. ) ;
#47698 = CARTESIAN_POINT ( 'NONE',  ( 2.499999999999998668, -1.333333333333332149, -4.330127018922193649 ) ) ;
#47699 = EDGE_LOOP ( 'NONE', ( #11728, #13682, #6974, #23898 ) ) ;
#47700 = CARTESIAN_POINT ( 'NONE',  ( 4.458734125000001214, -69.14583333196773651, 2.574251347313718519 ) ) ;
#47701 = CARTESIAN_POINT ( 'NONE',  ( 1.339745962155615144, -21.58034179853029855, 4.999999999999999112 ) ) ;
#47702 = DIRECTION ( 'NONE',  ( -0.000000000000000000, -0.000000000000000000, 1.000000000000000000 ) ) ;
#47703 = VERTEX_POINT ( 'NONE', #14023 ) ;
#47704 = CARTESIAN_POINT ( 'NONE',  ( 0.000000000000000000, -170.0000000000000000, 0.000000000000000000 ) ) ;
#47705 = CARTESIAN_POINT ( 'NONE',  ( -4.458734124999999437, -55.56249999863440081, 0.000000000000000000 ) ) ;
#47706 = CARTESIAN_POINT ( 'NONE',  ( -4.458734124999999437, 3.354166668032260823, -2.574251347313719407 ) ) ;
#47707 = ORIENTED_EDGE ( 'NONE', *, *, #42491, .T. ) ;
#47708 = VECTOR ( 'NONE', #52202, 1000.000000000000000 ) ;
#47709 = CARTESIAN_POINT ( 'NONE',  ( 0.000000000000000000, -120.0000000000000000, 0.000000000000000000 ) ) ;
#47710 = CARTESIAN_POINT ( 'NONE',  ( 4.458734124999999437, 2.187500001365593416, -5.460374474430324690E-16 ) ) ;
#47711 = CARTESIAN_POINT ( 'NONE',  ( -4.458734124999998549, 20.77083333469892779, 2.574251347313722516 ) ) ;
#47712 = CARTESIAN_POINT ( 'NONE',  ( -58.39396692619412477, -143.4375000013656063, 2.891590998281057701 ) ) ;
#47713 = CARTESIAN_POINT ( 'NONE',  ( 1.339745962155624914, 20.83034180399265978, -4.999999999999991118 ) ) ;
#47714 = CARTESIAN_POINT ( 'NONE',  ( -3.152801135295367096, -168.0625000013656063, -3.152801135295367541 ) ) ;
#47715 = VERTEX_POINT ( 'NONE', #62932 ) ;
#47716 = CARTESIAN_POINT ( 'NONE',  ( 4.458734124999998549, -77.72916666530106511, -2.574251347313721627 ) ) ;
#47717 = CARTESIAN_POINT ( 'NONE',  ( 5.000000000000000888, -10.45833333060214443, 2.886751345948126879 ) ) ;
#47718 = CARTESIAN_POINT ( 'NONE',  ( 4.458734124999999437, 5.187500001365596525, -5.460374474430324690E-16 ) ) ;
#47719 = CARTESIAN_POINT ( 'NONE',  ( -4.458734124999999437, -57.56249999863440081, 0.000000000000000000 ) ) ;
#47720 = CARTESIAN_POINT ( 'NONE',  ( -2.500000000000000444, -22.04166666393548013, -4.330127018922193649 ) ) ;
#47721 = CARTESIAN_POINT ( 'NONE',  ( -58.24261429053147765, -142.2500000000000284, -3.805975901505573855 ) ) ;
#47722 = CARTESIAN_POINT ( 'NONE',  ( 2.499999999999998668, -42.20833333060214443, -4.330127018922193649 ) ) ;
#47723 = CARTESIAN_POINT ( 'NONE',  ( -52.53715891517739323, -140.5625000027311842, -4.819101127000233298 ) ) ;
#47724 =( BOUNDED_CURVE ( )  B_SPLINE_CURVE ( 2, ( #42799, #4823, #38590, #33162, #29572, #24442, #49203, #43421, #28631 ),
 .UNSPECIFIED., .F., .F. ) 
 B_SPLINE_CURVE_WITH_KNOTS ( ( 3, 2, 2, 2, 3 ),
 ( 0.9875000000000000444, 0.9880952380952381375, 0.9892857142857143238, 0.9904761904761905100, 0.9910714285714286031 ),
 .UNSPECIFIED. ) 
 CURVE ( )  GEOMETRIC_REPRESENTATION_ITEM ( )  RATIONAL_B_SPLINE_CURVE ( ( 0.9330127018922194093, 0.9330127018922194093, 1.000000000000000000, 0.8660254037844387076, 1.000000000000000000, 0.8660254037844387076, 1.000000000000000000, 0.9330127018922194093, 0.9330127018922194093 ) ) 
 REPRESENTATION_ITEM ( '' )  );
#47725 = CARTESIAN_POINT ( 'NONE',  ( -5.000000000000000888, -156.5625000000000284, -2.071067811865475949 ) ) ;
#47726 = CARTESIAN_POINT ( 'NONE',  ( -51.19402409849444524, -139.5000000000000284, -3.242614290531456334 ) ) ;
#47727 = CARTESIAN_POINT ( 'NONE',  ( 4.458734124999999437, -41.81249999863440081, -5.460374474430324690E-16 ) ) ;
#47728 = CARTESIAN_POINT ( 'NONE',  ( 9.457646018065525792E-16, -28.31249999863440081, 5.148502694627439702 ) ) ;
#47729 =( BOUNDED_CURVE ( )  B_SPLINE_CURVE ( 2, ( #34435, #6149, #25116, #38948, #5188, #34125, #54064, #58586, #53747 ),
 .UNSPECIFIED., .F., .F. ) 
 B_SPLINE_CURVE_WITH_KNOTS ( ( 3, 2, 2, 2, 3 ),
 ( 0.02321428571428571508, 0.02380952380952380820, 0.02500000000000000139, 0.02619047619047619110, 0.02678571428571428770 ),
 .UNSPECIFIED. ) 
 CURVE ( )  GEOMETRIC_REPRESENTATION_ITEM ( )  RATIONAL_B_SPLINE_CURVE ( ( 0.9330127018922194093, 0.9330127018922195203, 1.000000000000000000, 0.8660254037844387076, 1.000000000000000000, 0.8660254037844387076, 1.000000000000000000, 0.9330127018922191873, 0.9330127018922194093 ) ) 
 REPRESENTATION_ITEM ( '' )  );
#47730 = CARTESIAN_POINT ( 'NONE',  ( 6.123233995736766282E-16, -120.0000000000000000, -5.000000000000000000 ) ) ;
#47731 = CARTESIAN_POINT ( 'NONE',  ( 2.500000000000002220, 28.33333333333333215, 4.330127018922192761 ) ) ;
#47732 = CARTESIAN_POINT ( 'NONE',  ( -2.071067811865478170, -155.4375000027312694, 5.000000000000000000 ) ) ;
#47733 = ORIENTED_EDGE ( 'NONE', *, *, #40512, .F. ) ;
#47734 = CARTESIAN_POINT ( 'NONE',  ( -4.458734124999998549, -110.4791666653010793, 2.574251347313722516 ) ) ;
#47735 = CARTESIAN_POINT ( 'NONE',  ( 4.458734124999999437, -32.81249999863440792, -5.460374474430324690E-16 ) ) ;
#47736 = CARTESIAN_POINT ( 'NONE',  ( 2.500000000000002220, -70.54166666393547303, 4.330127018922192761 ) ) ;
#47737 = CARTESIAN_POINT ( 'NONE',  ( -59.29741812935640155, -147.8750000013656063, -2.196230717870135685 ) ) ;
#47738 = CARTESIAN_POINT ( 'NONE',  ( 3.535533905932738197, -147.8750000000000000, -3.535533905932738197 ) ) ;
#47739 = ADVANCED_FACE ( 'NONE', ( #14342 ), #39407, .T. ) ;
#47740 = CARTESIAN_POINT ( 'NONE',  ( -4.458734124999999437, -27.31249999863440081, 0.000000000000000000 ) ) ;
#47741 = CARTESIAN_POINT ( 'NONE',  ( 4.458734124999999437, -77.06249999863440792, -5.460374474430324690E-16 ) ) ;
#47742 = CARTESIAN_POINT ( 'NONE',  ( 4.458734124999997661, -167.7500000013655779, 1.846868145590737864 ) ) ;
#47743 = CARTESIAN_POINT ( 'NONE',  ( 4.458734124999999437, -27.81249999863440081, -5.460374474430324690E-16 ) ) ;
#47744 = CARTESIAN_POINT ( 'NONE',  ( -60.14911071818854538, -148.0625000000000000, 1.666127454062681146 ) ) ;
#47745 = LINE ( 'NONE', #62564, #38960 ) ;
#47746 = CARTESIAN_POINT ( 'NONE',  ( -2.499999999999996447, -17.83333333333333215, 4.330127018922195425 ) ) ;
#47747 = CARTESIAN_POINT ( 'NONE',  ( 3.152801135295367541, -149.3125000013655779, -3.152801135295367541 ) ) ;
#47748 = VERTEX_POINT ( 'NONE', #43914 ) ;
#47749 = CARTESIAN_POINT ( 'NONE',  ( -6.972266317189433020E-16, -28.25000000000000000, -5.000000000000000000 ) ) ;
#47750 = CARTESIAN_POINT ( 'NONE',  ( 4.458734124999998549, -58.97916666530106511, -2.574251347313721627 ) ) ;
#47751 = CARTESIAN_POINT ( 'NONE',  ( -3.535250795749689387E-16, 26.87500000273118772, -5.773502691896257311 ) ) ;
#47752 = FACE_OUTER_BOUND ( 'NONE', #39859, .T. ) ;
#47753 = CARTESIAN_POINT ( 'NONE',  ( -5.000000000000000000, 18.91666666666666430, -2.886751345948128211 ) ) ;
#47754 = CARTESIAN_POINT ( 'NONE',  ( -2.499999999999996447, -88.83333333333332860, 4.330127018922195425 ) ) ;
#47755 = VECTOR ( 'NONE', #57208, 1000.000000000000000 ) ;
#47756 = CARTESIAN_POINT ( 'NONE',  ( -4.458734124999999437, -0.3958333319677397322, -2.574251347313719407 ) ) ;
#47757 = DIRECTION ( 'NONE',  ( 0.000000000000000000, 0.000000000000000000, 1.000000000000000000 ) ) ;
#47758 = CARTESIAN_POINT ( 'NONE',  ( -4.458734124999999437, 9.437500001365593860, 0.000000000000000000 ) ) ;
#47759 =( BOUNDED_CURVE ( )  B_SPLINE_CURVE ( 2, ( #8220, #13035, #56800, #4024, #37804, #28454, #27824, #23327, #7903 ),
 .UNSPECIFIED., .F., .F. ) 
 B_SPLINE_CURVE_WITH_KNOTS ( ( 3, 2, 2, 2, 3 ),
 ( 0.5767857142857142350, 0.5773809523809523281, 0.5785714285714286254, 0.5797619047619048116, 0.5803571428571429047 ),
 .UNSPECIFIED. ) 
 CURVE ( )  GEOMETRIC_REPRESENTATION_ITEM ( )  RATIONAL_B_SPLINE_CURVE ( ( 0.9330127018922194093, 0.9330127018922194093, 1.000000000000000000, 0.8660254037844387076, 1.000000000000000000, 0.8660254037844387076, 1.000000000000000000, 0.9330127018922194093, 0.9330127018922194093 ) ) 
 REPRESENTATION_ITEM ( '' )  );
#47760 = CARTESIAN_POINT ( 'NONE',  ( 1.975475456537005874E-15, -87.62499999726880162, 5.000000000000000000 ) ) ;
#47761 = ORIENTED_EDGE ( 'NONE', *, *, #8728, .T. ) ;
#47762 = CARTESIAN_POINT ( 'NONE',  ( 3.061616997868383141E-16, -167.8750000027312126, -5.000000000000000000 ) ) ;
#47763 = CARTESIAN_POINT ( 'NONE',  ( -4.458734124999999437, -50.31249999863440792, 0.000000000000000000 ) ) ;
#47764 = CARTESIAN_POINT ( 'NONE',  ( 1.846868145590735200, -158.5000000013656631, -4.458734125000000326 ) ) ;
#47765 = CARTESIAN_POINT ( 'NONE',  ( -2.499999999999996447, -51.70833333060213732, 4.330127018922195425 ) ) ;
#47766 = ORIENTED_EDGE ( 'NONE', *, *, #54232, .T. ) ;
#47767 = CARTESIAN_POINT ( 'NONE',  ( -3.152548672688508926E-16, -22.56249999863440081, -5.148502694627439702 ) ) ;
#47768 = VERTEX_POINT ( 'NONE', #39095 ) ;
#47770 = CARTESIAN_POINT ( 'NONE',  ( 5.000000000000000000, -53.49999999999999289, -6.123233995736766282E-16 ) ) ;
#47769 = CARTESIAN_POINT ( 'NONE',  ( -4.999999999999998224, -95.91666666666665719, 2.886751345948131764 ) ) ;
#47771 = CARTESIAN_POINT ( 'NONE',  ( -4.458734125000000326, -161.0000000013656063, -1.846868145590735644 ) ) ;
#47772 =( BOUNDED_CURVE ( )  B_SPLINE_CURVE ( 2, ( #41024, #27194, #26883, #51648, #7897, #56795, #12400, #32014, #51333 ),
 .UNSPECIFIED., .F., .F. ) 
 B_SPLINE_CURVE_WITH_KNOTS ( ( 3, 2, 2, 2, 3 ),
 ( 0.7270833333333333037, 0.7277777777777777457, 0.7291666666666666297, 0.7305555555555555136, 0.7312499999999999556 ),
 .UNSPECIFIED. ) 
 CURVE ( )  GEOMETRIC_REPRESENTATION_ITEM ( )  RATIONAL_B_SPLINE_CURVE ( ( 0.9330127018922194093, 0.9330127018922194093, 1.000000000000000000, 0.8660254037844387076, 1.000000000000000000, 0.8660254037844387076, 1.000000000000000000, 0.9330127018922194093, 0.9330127018922194093 ) ) 
 REPRESENTATION_ITEM ( '' )  );
#47773 = FACE_OUTER_BOUND ( 'NONE', #18, .T. ) ;
#47774 = CARTESIAN_POINT ( 'NONE',  ( -49.85088928181150436, -132.5625000000000568, -1.666127454062680702 ) ) ;
#47775 = CARTESIAN_POINT ( 'NONE',  ( 2.229367062499998831, -38.89583333196773651, -3.861377020970580887 ) ) ;
#47776 = ORIENTED_EDGE ( 'NONE', *, *, #25634, .T. ) ;
#47777 = CARTESIAN_POINT ( 'NONE',  ( 2.229367062499998831, -82.64583333196773651, -3.861377020970580887 ) ) ;
#47778 = CARTESIAN_POINT ( 'NONE',  ( -2.229367062500000163, 17.52083333469892779, -3.861377020970580443 ) ) ;
#47779 = CARTESIAN_POINT ( 'NONE',  ( -6.972266317189433020E-16, -24.12499999726881228, -5.000000000000000000 ) ) ;
#47780 = VERTEX_POINT ( 'NONE', #53584 ) ;
#47781 = CARTESIAN_POINT ( 'NONE',  ( -51.60603307380591787, -138.1875000013656347, -2.891590998281053704 ) ) ;
#47782 = CARTESIAN_POINT ( 'NONE',  ( -3.152548672688508926E-16, -84.81249999863439371, -5.148502694627439702 ) ) ;
#47783 = CARTESIAN_POINT ( 'NONE',  ( -51.19402409849444524, -127.6250000027312268, -3.242614290531456334 ) ) ;
#47784 = CARTESIAN_POINT ( 'NONE',  ( 0.000000000000000000, 0.000000000000000000, -9.974600000000000577 ) ) ;
#47785 = CARTESIAN_POINT ( 'NONE',  ( 3.061616997868383141E-16, -158.8750000027311842, -5.000000000000000000 ) ) ;
#47786 = CARTESIAN_POINT ( 'NONE',  ( 4.458734125000000326, -57.89583333196773651, 2.574251347313718519 ) ) ;
#47787 = CARTESIAN_POINT ( 'NONE',  ( 5.000000000000000000, -37.50000000000000711, -6.123233995736766282E-16 ) ) ;
#47788 = CARTESIAN_POINT ( 'NONE',  ( -3.152548672688508926E-16, 22.43750000136559208, -5.148502694627439702 ) ) ;
#47789 = CARTESIAN_POINT ( 'NONE',  ( -6.972266317189433020E-16, -97.24999999999998579, -5.000000000000000000 ) ) ;
#47790 = VECTOR ( 'NONE', #20737, 1000.000000000000000 ) ;
#47791 = CYLINDRICAL_SURFACE ( 'NONE', #45358, 5.000000000000000000 ) ;
#47792 = CARTESIAN_POINT ( 'NONE',  ( -3.152548672688508926E-16, -42.81249999863440081, -5.148502694627439702 ) ) ;
#47793 = CARTESIAN_POINT ( 'NONE',  ( 2.499999999999998668, -2.208333330602146205, -4.330127018922193649 ) ) ;
#47794 = CARTESIAN_POINT ( 'NONE',  ( 2.500000000000002220, -31.66666666666666075, 4.330127018922192761 ) ) ;
#47795 = CARTESIAN_POINT ( 'NONE',  ( -57.89159099828107458, -124.6875000013656063, -3.393966926194107447 ) ) ;
#47796 = CARTESIAN_POINT ( 'NONE',  ( 2.229367062500001939, -87.22916666530107932, 3.861377020970579999 ) ) ;
#47797 = CARTESIAN_POINT ( 'NONE',  ( 4.458734124999998549, -104.7291666653010509, -2.574251347313721627 ) ) ;
#47798 = CARTESIAN_POINT ( 'NONE',  ( 9.457646018065525792E-16, -10.31249999863440969, 5.148502694627439702 ) ) ;
#47799 = VERTEX_POINT ( 'NONE', #28189 ) ;
#47800 = CARTESIAN_POINT ( 'NONE',  ( 2.499999999999998668, -52.33333333333332860, -4.330127018922193649 ) ) ;
#47801 = CARTESIAN_POINT ( 'NONE',  ( 2.229367062499998831, -95.64583333196773651, -3.861377020970580887 ) ) ;
#47802 = CARTESIAN_POINT ( 'NONE',  ( 3.535533905932736864, -165.2500000027312126, 3.535533905932738641 ) ) ;
#47803 = CARTESIAN_POINT ( 'NONE',  ( -4.458734124999999437, -90.56249999863440792, 0.000000000000000000 ) ) ;
#47804 = CARTESIAN_POINT ( 'NONE',  ( -3.535250795749689387E-16, -53.12499999726881583, -5.773502691896257311 ) ) ;
#47805 = CARTESIAN_POINT ( 'NONE',  ( -6.972266317189433020E-16, -42.12499999726880873, -5.000000000000000000 ) ) ;
#47806 = CARTESIAN_POINT ( 'NONE',  ( -58.39396692619412477, -128.4375000013656063, 2.891590998281057701 ) ) ;
#47807 = CARTESIAN_POINT ( 'NONE',  ( 2.229367062500001939, -12.97916666530107221, 3.861377020970579999 ) ) ;
#47808 = CARTESIAN_POINT ( 'NONE',  ( -2.229367062500000163, 9.270833334698927786, -3.861377020970580443 ) ) ;
#47809 = CARTESIAN_POINT ( 'NONE',  ( 2.229367062499998831, -55.89583333196773651, -3.861377020970580887 ) ) ;
#47810 = DIRECTION ( 'NONE',  ( -0.000000000000000000, 1.000000000000000000, -0.000000000000000000 ) ) ;
#47811 = CARTESIAN_POINT ( 'NONE',  ( -5.000000000000000000, -106.0833333333333286, -2.886751345948128211 ) ) ;
#47812 = CARTESIAN_POINT ( 'NONE',  ( -4.458734124999999437, -13.39583333196774007, -2.574251347313719407 ) ) ;
#47813 = CARTESIAN_POINT ( 'NONE',  ( 1.339745962155615144, -8.580341798530293218, 4.999999999999999112 ) ) ;
#47814 = VERTEX_POINT ( 'NONE', #58724 ) ;
#47815 = CARTESIAN_POINT ( 'NONE',  ( -3.152548672688508926E-16, -39.81249999863440081, -5.148502694627439702 ) ) ;
#47816 = CARTESIAN_POINT ( 'NONE',  ( -50.55543936806279248, -125.3125000013655921, 0.3552334253322060320 ) ) ;
#47817 = DIRECTION ( 'NONE',  ( 1.000000000000000000, 0.000000000000000000, -1.061635649774262664E-14 ) ) ;
#47818 = CARTESIAN_POINT ( 'NONE',  ( 0.000000000000000000, -120.0000000000000000, 0.000000000000000000 ) ) ;
#47819 = CARTESIAN_POINT ( 'NONE',  ( -4.458734124999998549, -84.22916666530107932, 2.574251347313722516 ) ) ;
#47820 = CARTESIAN_POINT ( 'NONE',  ( -4.458734124999999437, 23.43750000136559564, 0.000000000000000000 ) ) ;
#47821 = CARTESIAN_POINT ( 'NONE',  ( 2.229367062500001939, 17.02083333469892779, 3.861377020970579999 ) ) ;
#47822 = LINE ( 'NONE', #3781, #23651 ) ;
#47823 = CARTESIAN_POINT ( 'NONE',  ( 1.975475456537005874E-15, -55.74999999999999289, 5.000000000000000000 ) ) ;
#47824 = CARTESIAN_POINT ( 'NONE',  ( 2.229367062499998831, -86.89583333196773651, -3.861377020970580887 ) ) ;
#47825 = CARTESIAN_POINT ( 'NONE',  ( -2.500000000000000444, -70.16666666666667140, -4.330127018922193649 ) ) ;
#47826 = CARTESIAN_POINT ( 'NONE',  ( -2.499999999999996447, 12.29166666939785202, 4.330127018922195425 ) ) ;
#47827 = ORIENTED_EDGE ( 'NONE', *, *, #52922, .T. ) ;
#47828 = CARTESIAN_POINT ( 'NONE',  ( -51.75738570946856498, -135.7500000000000284, 3.805975901505576964 ) ) ;
#47829 = CARTESIAN_POINT ( 'NONE',  ( -1.339745962155623360, 16.20534180126147916, 4.999999999999991118 ) ) ;
#47831 = CARTESIAN_POINT ( 'NONE',  ( -2.500000000000000444, -29.16666666666666785, -4.330127018922193649 ) ) ;
#47830 = CARTESIAN_POINT ( 'NONE',  ( 1.339745962155615144, -40.70534180126147561, 4.999999999999999112 ) ) ;
#47832 = CARTESIAN_POINT ( 'NONE',  ( -3.152548672688508926E-16, -35.56249999863440792, -5.148502694627439702 ) ) ;
#47833 = EDGE_CURVE ( 'NONE', #62764, #19054, #17984, .T. ) ;
#47834 = CARTESIAN_POINT ( 'NONE',  ( -5.000000000000000000, 5.000000000000000888, 0.000000000000000000 ) ) ;
#47835 = AXIS2_PLACEMENT_3D ( 'NONE', #14485, #34, #33486 ) ;
#47836 = CARTESIAN_POINT ( 'NONE',  ( -2.499999999999996447, -34.70833333060213732, 4.330127018922195425 ) ) ;
#47838 = ORIENTED_EDGE ( 'NONE', *, *, #54323, .F. ) ;
#47837 = CARTESIAN_POINT ( 'NONE',  ( 2.229367062500001939, -61.97916666530106511, 3.861377020970579999 ) ) ;
#47839 = CARTESIAN_POINT ( 'NONE',  ( -52.80376928212989185, -153.1250000013656063, -4.297418129356379346 ) ) ;
#47841 = ORIENTED_EDGE ( 'NONE', *, *, #15023, .T. ) ;
#47840 = CARTESIAN_POINT ( 'NONE',  ( 2.229367062499998831, -8.895833331967736513, -3.861377020970580887 ) ) ;
#47842 = CARTESIAN_POINT ( 'NONE',  ( 5.000000000000000000, -77.50000000000000000, -6.123233995736766282E-16 ) ) ;
#47843 = CARTESIAN_POINT ( 'NONE',  ( -53.51423613279429503, -136.2500000013656063, 4.591703134518083651 ) ) ;
#47844 = CARTESIAN_POINT ( 'NONE',  ( 2.229367062500001939, -56.22916666530107221, 3.861377020970579999 ) ) ;
#47845 = CARTESIAN_POINT ( 'NONE',  ( -5.000000000000000000, -75.87499999726880162, 0.000000000000000000 ) ) ;
#47847 = ORIENTED_EDGE ( 'NONE', *, *, #27823, .T. ) ;
#47846 = CARTESIAN_POINT ( 'NONE',  ( 5.000000000000000000, -13.41666666666666785, -2.886751345948130876 ) ) ;
#47848 = CARTESIAN_POINT ( 'NONE',  ( -50.01589407740564042, -148.6250000000000284, 0.3983568153799778022 ) ) ;
#47849 = CARTESIAN_POINT ( 'NONE',  ( 2.229367062499998831, -19.89583333196774007, -3.861377020970580887 ) ) ;
#47851 = ORIENTED_EDGE ( 'NONE', *, *, #50698, .T. ) ;
#47850 = CARTESIAN_POINT ( 'NONE',  ( 4.458734125000001214, -55.14583333196772941, 2.574251347313718519 ) ) ;
#47852 =( BOUNDED_CURVE ( )  B_SPLINE_CURVE ( 2, ( #33229, #18739, #18114, #23890, #4272, #3342, #62516, #3652, #42869 ),
 .UNSPECIFIED., .F., .F. ) 
 B_SPLINE_CURVE_WITH_KNOTS ( ( 3, 2, 2, 2, 3 ),
 ( 0.4312500000000000222, 0.4319444444444444642, 0.4333333333333333481, 0.4347222222222222321, 0.4354166666666666741 ),
 .UNSPECIFIED. ) 
 CURVE ( )  GEOMETRIC_REPRESENTATION_ITEM ( )  RATIONAL_B_SPLINE_CURVE ( ( 0.9330127018922194093, 0.9330127018922194093, 1.000000000000000000, 0.8660254037844387076, 1.000000000000000000, 0.8660254037844387076, 1.000000000000000000, 0.9330127018922194093, 0.9330127018922194093 ) ) 
 REPRESENTATION_ITEM ( '' )  );
#47853 = DIRECTION ( 'NONE',  ( 0.000000000000000000, 0.000000000000000000, 1.000000000000000000 ) ) ;
#47854 = CARTESIAN_POINT ( 'NONE',  ( -3.152801135295367985, -166.0625000013656063, 3.152801135295367096 ) ) ;
#47855 = CARTESIAN_POINT ( 'NONE',  ( -2.229367062499996610, -100.3958333319677365, 3.861377020970582219 ) ) ;
#47856 = CARTESIAN_POINT ( 'NONE',  ( -6.972266317189433020E-16, -27.12499999726881228, -5.000000000000000000 ) ) ;
#47857 = ORIENTED_EDGE ( 'NONE', *, *, #48885, .T. ) ;
#47858 = CARTESIAN_POINT ( 'NONE',  ( -50.70258187064364108, -149.3750000013656063, 2.196230717870141014 ) ) ;
#47859 = CARTESIAN_POINT ( 'NONE',  ( -49.85088928181150436, -142.6875000027312126, -1.666127454062680702 ) ) ;
#47860 = CARTESIAN_POINT ( 'NONE',  ( -2.352990130084580066E-16, 8.660254037844390851, -10.00000000000000000 ) ) ;
#47861 = CARTESIAN_POINT ( 'NONE',  ( 4.458734125000001214, -9.895833331967736513, 2.574251347313718519 ) ) ;
#47862 = CARTESIAN_POINT ( 'NONE',  ( 4.458734125000000326, -103.1458333319677507, 2.574251347313718519 ) ) ;
#47863 =( BOUNDED_CURVE ( )  B_SPLINE_CURVE ( 2, ( #30910, #21264, #36060, #60513, #55689, #32170, #56003, #36693, #26404 ),
 .UNSPECIFIED., .F., .F. ) 
 B_SPLINE_CURVE_WITH_KNOTS ( ( 3, 2, 2, 2, 3 ),
 ( 0.7303571428571428159, 0.7309523809523809090, 0.7321428571428570953, 0.7333333333333332815, 0.7339285714285714857 ),
 .UNSPECIFIED. ) 
 CURVE ( )  GEOMETRIC_REPRESENTATION_ITEM ( )  RATIONAL_B_SPLINE_CURVE ( ( 0.9330127018922194093, 0.9330127018922194093, 1.000000000000000000, 0.8660254037844387076, 1.000000000000000000, 0.8660254037844387076, 1.000000000000000000, 0.9330127018922130810, 0.9330127018922194093 ) ) 
 REPRESENTATION_ITEM ( '' )  );
#47864 = CARTESIAN_POINT ( 'NONE',  ( -1.846868145590737420, -145.0000000013656063, 4.458734124999999437 ) ) ;
#47865 = CARTESIAN_POINT ( 'NONE',  ( -3.152548672688508926E-16, -28.81249999863440436, -5.148502694627439702 ) ) ;
#47866 = CARTESIAN_POINT ( 'NONE',  ( 1.975475456537005874E-15, -88.62499999726880162, 5.000000000000000000 ) ) ;
#47867 = CARTESIAN_POINT ( 'NONE',  ( -57.89159099828107458, -135.6875000013656063, -3.393966926194107447 ) ) ;
#47868 = CARTESIAN_POINT ( 'NONE',  ( 4.458734124999998549, -70.97916666530107932, -2.574251347313721627 ) ) ;
#47869 = CARTESIAN_POINT ( 'NONE',  ( -5.000000000000000000, 16.91666666666666785, -2.886751345948128211 ) ) ;
#47870 = CARTESIAN_POINT ( 'NONE',  ( -3.152801135295367985, -142.8125000013655779, 3.152801135295367096 ) ) ;
#47871 = CARTESIAN_POINT ( 'NONE',  ( -4.458734124999997661, 9.520833334698927786, 2.574251347313722516 ) ) ;
#47872 = ORIENTED_EDGE ( 'NONE', *, *, #2726, .F. ) ;
#47873 = VECTOR ( 'NONE', #48662, 1000.000000000000000 ) ;
#47874 = DIRECTION ( 'NONE',  ( 0.000000000000000000, 0.000000000000000000, 1.000000000000000000 ) ) ;
#47875 = CARTESIAN_POINT ( 'NONE',  ( -4.999999999999998224, 16.20833333606451987, 2.886751345948131764 ) ) ;
#47877 = CARTESIAN_POINT ( 'NONE',  ( 4.458734125000001214, -26.89583333196774007, 2.574251347313718519 ) ) ;
#47876 = CARTESIAN_POINT ( 'NONE',  ( 5.000000000000000000, -88.50000000000000000, -6.123233995736766282E-16 ) ) ;
#47878 = DIRECTION ( 'NONE',  ( -0.000000000000000000, 1.000000000000000000, -0.000000000000000000 ) ) ;
#47879 = CARTESIAN_POINT ( 'NONE',  ( 4.458734124999998549, -74.97916666530106511, -2.574251347313721627 ) ) ;
#47880 = AXIS2_PLACEMENT_3D ( 'NONE', #43394, #39197, #49175 ) ;
#47881 = CARTESIAN_POINT ( 'NONE',  ( 4.458734124999998549, 22.02083333469892779, -2.574251347313721627 ) ) ;
#47882 = DIRECTION ( 'NONE',  ( -0.000000000000000000, 1.000000000000000000, -0.000000000000000000 ) ) ;
#47883 = VECTOR ( 'NONE', #47882, 1000.000000000000000 ) ;
#47884 = CARTESIAN_POINT ( 'NONE',  ( -59.29741812935640155, -140.6250000013656063, -2.196230717870135685 ) ) ;
#47885 = CARTESIAN_POINT ( 'NONE',  ( 4.458734124999998549, 1.270833334698927342, -2.574251347313721627 ) ) ;
#47886 = CARTESIAN_POINT ( 'NONE',  ( 4.458734124999999437, 27.93750000136559208, -5.460374474430324690E-16 ) ) ;
#47887 = CARTESIAN_POINT ( 'NONE',  ( -3.152548672688508926E-16, -39.81249999863440081, -5.148502694627439702 ) ) ;
#47888 = CARTESIAN_POINT ( 'NONE',  ( -58.24261429053147765, -144.2500000000000284, -3.805975901505573855 ) ) ;
#47889 = CARTESIAN_POINT ( 'NONE',  ( 2.229367062499998831, 4.354166668032260823, -3.861377020970580887 ) ) ;
#47890 = CARTESIAN_POINT ( 'NONE',  ( -3.152548672688508926E-16, -72.56249999863439371, -5.148502694627439702 ) ) ;
#47891 = CARTESIAN_POINT ( 'NONE',  ( 2.229367062499998831, -23.89583333196773651, -3.861377020970580887 ) ) ;
#47892 = CARTESIAN_POINT ( 'NONE',  ( 4.458734124999999437, -156.4375000013655779, 0.000000000000000000 ) ) ;
#47893 = CARTESIAN_POINT ( 'NONE',  ( 9.457646018065525792E-16, -64.06249999863440792, 5.148502694627439702 ) ) ;
#47894 = CARTESIAN_POINT ( 'NONE',  ( -2.499999999999996447, -97.70833333060213022, 4.330127018922195425 ) ) ;
#47895 = CARTESIAN_POINT ( 'NONE',  ( 2.626220312808019583E-14, 15.74999999999999645, -5.000000000000000000 ) ) ;
#47896 = CARTESIAN_POINT ( 'NONE',  ( 9.457646018065525792E-16, -42.06249999863440081, 5.148502694627439702 ) ) ;
#47897 = CARTESIAN_POINT ( 'NONE',  ( -5.000000000000000000, -84.08333333333332860, -2.886751345948128211 ) ) ;
#47898 = CARTESIAN_POINT ( 'NONE',  ( 4.458734125000000326, -104.1458333319677365, 2.574251347313718519 ) ) ;
#47899 = CARTESIAN_POINT ( 'NONE',  ( -4.458734124999999437, -67.56249999863440792, 0.000000000000000000 ) ) ;
#47900 = CARTESIAN_POINT ( 'NONE',  ( -5.000000000000000000, -52.00000000000000711, 0.000000000000000000 ) ) ;
#47901 = CARTESIAN_POINT ( 'NONE',  ( 2.499999999999998668, -72.20833333060214443, -4.330127018922193649 ) ) ;
#47902 = CARTESIAN_POINT ( 'NONE',  ( 5.000000000000000000, 28.70833333606451987, -2.886751345948129988 ) ) ;
#47903 = ORIENTED_EDGE ( 'NONE', *, *, #55953, .F. ) ;
#47904 = DIRECTION ( 'NONE',  ( -0.000000000000000000, 1.000000000000000000, -0.000000000000000000 ) ) ;
#47905 = CARTESIAN_POINT ( 'NONE',  ( 2.499999999999998668, 2.791666669397851130, -4.330127018922193649 ) ) ;
#47906 = CARTESIAN_POINT ( 'NONE',  ( -5.000000000000000000, -11.00000000000000355, 0.000000000000000000 ) ) ;
#47907 = CARTESIAN_POINT ( 'NONE',  ( -2.229367062499996610, -19.14583333196774007, 3.861377020970582219 ) ) ;
#47908 = ADVANCED_FACE ( 'NONE', ( #49064 ), #53270, .T. ) ;
#47909 = CARTESIAN_POINT ( 'NONE',  ( -4.458734124999999437, -76.39583333196773651, -2.574251347313719407 ) ) ;
#47910 = CARTESIAN_POINT ( 'NONE',  ( 5.000000000000000888, -59.45833333060214443, 2.886751345948126879 ) ) ;
#47911 = CARTESIAN_POINT ( 'NONE',  ( 5.000000000000000000, -15.29166666393548368, -2.886751345948129988 ) ) ;
#47913 = ORIENTED_EDGE ( 'NONE', *, *, #41458, .T. ) ;
#47912 = CARTESIAN_POINT ( 'NONE',  ( -4.458734124999998549, -44.22916666530106511, 2.574251347313722516 ) ) ;
#47914 = CARTESIAN_POINT ( 'NONE',  ( 6.972266317189433020E-16, 29.74999999999999645, -5.000000000000000000 ) ) ;
#47916 = ORIENTED_EDGE ( 'NONE', *, *, #58903, .F. ) ;
#47915 = CARTESIAN_POINT ( 'NONE',  ( 4.458734124999999437, 8.937500001365592084, -5.460374474430324690E-16 ) ) ;
#47917 = CARTESIAN_POINT ( 'NONE',  ( -1.339745962155613812, -87.08034179853028434, -5.000000000000000000 ) ) ;
#47918 = CARTESIAN_POINT ( 'NONE',  ( -5.000000000000000000, -60.00000000000000000, 0.000000000000000000 ) ) ;
#47919 = CARTESIAN_POINT ( 'NONE',  ( 4.458734124999999437, -155.6875000013655779, 0.000000000000000000 ) ) ;
#47920 = CARTESIAN_POINT ( 'NONE',  ( -4.458734124999999437, -35.56249999863440792, 0.000000000000000000 ) ) ;
#47921 = CARTESIAN_POINT ( 'NONE',  ( -2.500000000000000444, -56.16666666666667140, -4.330127018922193649 ) ) ;
#47922 =( BOUNDED_CURVE ( )  B_SPLINE_CURVE ( 2, ( #52048, #56878, #32417, #63588, #13742, #38800, #38195, #9544, #18574 ),
 .UNSPECIFIED., .F., .F. ) 
 B_SPLINE_CURVE_WITH_KNOTS ( ( 3, 2, 2, 2, 3 ),
 ( 0.9104166666666666519, 0.9111111111111110938, 0.9124999999999999778, 0.9138888888888888618, 0.9145833333333333037 ),
 .UNSPECIFIED. ) 
 CURVE ( )  GEOMETRIC_REPRESENTATION_ITEM ( )  RATIONAL_B_SPLINE_CURVE ( ( 0.9330127018922194093, 0.9330127018922194093, 1.000000000000000000, 0.8660254037844387076, 1.000000000000000000, 0.8660254037844387076, 1.000000000000000000, 0.9330127018922194093, 0.9330127018922194093 ) ) 
 REPRESENTATION_ITEM ( '' )  );
#47923 = AXIS2_PLACEMENT_3D ( 'NONE', #22857, #37630, #17070 ) ;
#47924 = CARTESIAN_POINT ( 'NONE',  ( 2.071067811865476394, -166.1875000000000000, 5.000000000000000000 ) ) ;
#47925 = EDGE_CURVE ( 'NONE', #50923, #63287, #51122, .T. ) ;
#47926 = CARTESIAN_POINT ( 'NONE',  ( 2.499999999999998668, -11.33333333333333393, -4.330127018922193649 ) ) ;
#47927 = CARTESIAN_POINT ( 'NONE',  ( -50.55543936806279248, -130.3125000013656063, 0.3552334253322060320 ) ) ;
#47928 = CARTESIAN_POINT ( 'NONE',  ( -3.152548672688508926E-16, -6.812499998634404363, -5.148502694627439702 ) ) ;
#47929 = AXIS2_PLACEMENT_3D ( 'NONE', #53346, #43680, #39494 ) ;
#47930 = CARTESIAN_POINT ( 'NONE',  ( 4.458734124999998549, -39.97916666530107221, -2.574251347313721627 ) ) ;
#47931 = CARTESIAN_POINT ( 'NONE',  ( -6.972266317189433020E-16, -54.24999999999999289, -5.000000000000000000 ) ) ;
#47932 = CARTESIAN_POINT ( 'NONE',  ( -1.846868145590737420, -147.7500000013655779, 4.458734124999999437 ) ) ;
#47933 = AXIS2_PLACEMENT_3D ( 'NONE', #36284, #2827, #37232 ) ;
#47934 = EDGE_CURVE ( 'NONE', #40505, #42214, #59044, .T. ) ;
#47935 = CARTESIAN_POINT ( 'NONE',  ( -4.458734124999998549, -83.47916666530107932, 2.574251347313722516 ) ) ;
#47936 = CARTESIAN_POINT ( 'NONE',  ( 3.535533905932738197, -167.0000000027312126, -3.535533905932738197 ) ) ;
#47937 = VERTEX_POINT ( 'NONE', #47805 ) ;
#47938 = LINE ( 'NONE', #22250, #56331 ) ;
#47939 = CARTESIAN_POINT ( 'NONE',  ( 6.158835246850666199E-14, -2.124999997268816276, -4.999999999999999112 ) ) ;
#47940 = CARTESIAN_POINT ( 'NONE',  ( 4.458734124999998549, -68.97916666530106511, -2.574251347313721627 ) ) ;
#47941 = CARTESIAN_POINT ( 'NONE',  ( 1.846868145590736310, -144.8750000013656063, 4.458734124999997661 ) ) ;
#47942 = ORIENTED_EDGE ( 'NONE', *, *, #17820, .T. ) ;
#47943 = CARTESIAN_POINT ( 'NONE',  ( -2.499999999999996447, -13.83333333333333570, 4.330127018922195425 ) ) ;
#47944 = CARTESIAN_POINT ( 'NONE',  ( 4.458734124999999437, -12.06249999863440081, -5.460374474430324690E-16 ) ) ;
#47945 = CARTESIAN_POINT ( 'NONE',  ( 1.339745962155612702, -79.16965819600730470, -5.000000000000000000 ) ) ;
#47946 = CARTESIAN_POINT ( 'NONE',  ( 9.457646018065525792E-16, 2.937500001365594304, 5.148502694627439702 ) ) ;
#47947 = CARTESIAN_POINT ( 'NONE',  ( -6.972266317189433020E-16, -43.25000000000000000, -5.000000000000000000 ) ) ;
#47948 = CARTESIAN_POINT ( 'NONE',  ( -1.846868145590737420, -153.7500000013656063, 4.458734124999997661 ) ) ;
#47949 =( BOUNDED_CURVE ( )  B_SPLINE_CURVE ( 2, ( #8914, #52042, #8599, #38190, #28209, #43004, #57815, #13737, #52973 ),
 .UNSPECIFIED., .F., .F. ) 
 B_SPLINE_CURVE_WITH_KNOTS ( ( 3, 2, 2, 2, 3 ),
 ( 0.7812500000000000000, 0.7819444444444444420, 0.7833333333333333259, 0.7847222222222222099, 0.7854166666666666519 ),
 .UNSPECIFIED. ) 
 CURVE ( )  GEOMETRIC_REPRESENTATION_ITEM ( )  RATIONAL_B_SPLINE_CURVE ( ( 0.9330127018922194093, 0.9330127018922194093, 1.000000000000000000, 0.8660254037844387076, 1.000000000000000000, 0.8660254037844387076, 1.000000000000000000, 0.9330127018922194093, 0.9330127018922194093 ) ) 
 REPRESENTATION_ITEM ( '' )  );
#47950 = CARTESIAN_POINT ( 'NONE',  ( 2.229367062499998831, 24.10416666803225993, -3.861377020970580887 ) ) ;
#47951 = ORIENTED_EDGE ( 'NONE', *, *, #46406, .T. ) ;
#47952 = CARTESIAN_POINT ( 'NONE',  ( 2.229367062500001939, -91.97916666530106511, 3.861377020970579999 ) ) ;
#47953 = CARTESIAN_POINT ( 'NONE',  ( -75.00000000000000000, 0.000000000000000000, 8.999999999999998224 ) ) ;
#47954 = LINE ( 'NONE', #62767, #44187 ) ;
#47955 = CARTESIAN_POINT ( 'NONE',  ( -4.458734124999998549, -10.22916666530106866, 2.574251347313722516 ) ) ;
#47956 = DIRECTION ( 'NONE',  ( 0.000000000000000000, 0.000000000000000000, 1.000000000000000000 ) ) ;
#47957 = CARTESIAN_POINT ( 'NONE',  ( 0.000000000000000000, -120.0000000000000000, 5.000000000000000000 ) ) ;
#47958 = CARTESIAN_POINT ( 'NONE',  ( -50.70258187064364108, -153.1250000013656063, 2.196230717870141014 ) ) ;
#47959 = CARTESIAN_POINT ( 'NONE',  ( 5.000000000000000888, -38.45833333060213732, 2.886751345948126879 ) ) ;
#47960 = CARTESIAN_POINT ( 'NONE',  ( -6.972266317189433020E-16, -48.12499999726880873, -5.000000000000000000 ) ) ;
#47961 = CARTESIAN_POINT ( 'NONE',  ( 2.229367062500001939, 19.02083333469892779, 3.861377020970579999 ) ) ;
#47962 = CARTESIAN_POINT ( 'NONE',  ( -5.000000000000000000, -72.00000000000000000, 0.000000000000000000 ) ) ;
#47963 = CARTESIAN_POINT ( 'NONE',  ( -4.458734124999997661, 24.77083333469893134, 2.574251347313722516 ) ) ;
#47964 = CARTESIAN_POINT ( 'NONE',  ( 2.229367062499998831, -55.64583333196773651, -3.861377020970580887 ) ) ;
#47965 = CARTESIAN_POINT ( 'NONE',  ( 9.457646018065525792E-16, -1.312499998634406140, 5.148502694627439702 ) ) ;
#47966 = CARTESIAN_POINT ( 'NONE',  ( -6.972266317189433020E-16, -63.25000000000000000, -5.000000000000000000 ) ) ;
#47967 = CARTESIAN_POINT ( 'NONE',  ( -3.535250795749689387E-16, 10.74999999999999822, -5.773502691896257311 ) ) ;
#47968 = CARTESIAN_POINT ( 'NONE',  ( -1.846868145590734756, -168.1250000013656063, -4.458734125000000326 ) ) ;
#47969 = CARTESIAN_POINT ( 'NONE',  ( -2.499999999999996447, -45.83333333333333570, 4.330127018922195425 ) ) ;
#47970 = CARTESIAN_POINT ( 'NONE',  ( -4.458734124999999437, -46.31249999863440792, 0.000000000000000000 ) ) ;
#47971 = CARTESIAN_POINT ( 'NONE',  ( -4.999999999999999112, -81.79166666393547303, 2.886751345948131764 ) ) ;
#47972 = AXIS2_PLACEMENT_3D ( 'NONE', #12531, #51777, #17980 ) ;
#47973 = VECTOR ( 'NONE', #57864, 1000.000000000000000 ) ;
#47974 = CARTESIAN_POINT ( 'NONE',  ( -50.55543936806279248, -137.3125000013656063, 0.3552334253322060320 ) ) ;
#47975 = CYLINDRICAL_SURFACE ( 'NONE', #48282, 5.000000000000000000 ) ;
#47976 = CARTESIAN_POINT ( 'NONE',  ( 1.975475456537005874E-15, -91.74999999999998579, 5.000000000000000000 ) ) ;
#47977 = AXIS2_PLACEMENT_3D ( 'NONE', #31203, #8043, #51160 ) ;
#47978 = CARTESIAN_POINT ( 'NONE',  ( -3.152548672688508926E-16, -89.81249999863440792, -5.148502694627439702 ) ) ;
#47979 = CARTESIAN_POINT ( 'NONE',  ( 4.458734124999999437, -158.6250000013655779, -1.846868145590734978 ) ) ;
#47980 = CARTESIAN_POINT ( 'NONE',  ( 2.500000000000002220, -36.66666666666666430, 4.330127018922192761 ) ) ;
#47981 = CYLINDRICAL_SURFACE ( 'NONE', #19221, 5.000000000000000000 ) ;
#47982 = EDGE_LOOP ( 'NONE', ( #6792, #55710, #59178, #22068 ) ) ;
#47983 = CARTESIAN_POINT ( 'NONE',  ( -3.152548672688508926E-16, 19.18750000136559208, -5.148502694627439702 ) ) ;
#47984 = VERTEX_POINT ( 'NONE', #3762 ) ;
#47985 = CARTESIAN_POINT ( 'NONE',  ( -2.229367062500000163, -93.47916666530106511, -3.861377020970580443 ) ) ;
#47986 = CARTESIAN_POINT ( 'NONE',  ( 4.458734124999998549, 8.020833334698926009, -2.574251347313721627 ) ) ;
#47987 = CARTESIAN_POINT ( 'NONE',  ( 1.060575238724906964E-15, 11.37500000273118594, 5.773502691896257311 ) ) ;
#47988 = CARTESIAN_POINT ( 'NONE',  ( 2.499999999999998668, 12.66666666666666607, -4.330127018922193649 ) ) ;
#47989 = CARTESIAN_POINT ( 'NONE',  ( -5.000000000000000000, 2.999999999999999112, 0.000000000000000000 ) ) ;
#47990 = CARTESIAN_POINT ( 'NONE',  ( 4.458734124999998549, -61.72916666530106511, -2.574251347313721627 ) ) ;
#47991 = LINE ( 'NONE', #47681, #36966 ) ;
#47992 = EDGE_CURVE ( 'NONE', #16995, #31397, #39754, .T. ) ;
#47993 = ADVANCED_FACE ( 'NONE', ( #30077 ), #39726, .T. ) ;
#47994 = CARTESIAN_POINT ( 'NONE',  ( 2.500000000000002220, 5.458333336064518981, 4.330127018922192761 ) ) ;
#47995 = CARTESIAN_POINT ( 'NONE',  ( 4.458734125000001214, -27.89583333196774007, 2.574251347313718519 ) ) ;
#47996 = CARTESIAN_POINT ( 'NONE',  ( 3.535533905932738197, -153.0000000027312126, -3.535533905932738197 ) ) ;
#47997 = CARTESIAN_POINT ( 'NONE',  ( -5.000000000000000000, 26.04166666939784847, -2.886751345948128211 ) ) ;
#47998 = EDGE_CURVE ( 'NONE', #53339, #21155, #36153, .T. ) ;
#47999 = CYLINDRICAL_SURFACE ( 'NONE', #49433, 5.000000000000000000 ) ;
#48000 = CARTESIAN_POINT ( 'NONE',  ( -2.500000000000000444, -44.16666666666665719, -4.330127018922193649 ) ) ;
#48001 = CARTESIAN_POINT ( 'NONE',  ( -2.229367062499996610, -19.39583333196774007, 3.861377020970582219 ) ) ;
#48002 = CARTESIAN_POINT ( 'NONE',  ( 0.000000000000000000, -120.0000000000000000, 5.000000000000000000 ) ) ;
#48003 = CARTESIAN_POINT ( 'NONE',  ( 2.229367062500001939, -66.97916666530106511, 3.861377020970579999 ) ) ;
#48004 = CARTESIAN_POINT ( 'NONE',  ( -3.152801135295367096, -147.3125000013655779, -3.152801135295367541 ) ) ;
#48005 = CARTESIAN_POINT ( 'NONE',  ( -2.229367062499996610, -76.14583333196773651, 3.861377020970582219 ) ) ;
#48006 = CARTESIAN_POINT ( 'NONE',  ( -58.39396692619412477, -143.6875000013656063, 2.891590998281057701 ) ) ;
#48007 = ADVANCED_FACE ( 'NONE', ( #847 ), #49708, .T. ) ;
#48008 = CARTESIAN_POINT ( 'NONE',  ( -2.229367062499996610, -27.39583333196774007, 3.861377020970582219 ) ) ;
#48009 = CARTESIAN_POINT ( 'NONE',  ( 1.060575238724906964E-15, -63.62499999726881583, 5.773502691896257311 ) ) ;
#48010 = VERTEX_POINT ( 'NONE', #10151 ) ;
#48012 = ORIENTED_EDGE ( 'NONE', *, *, #51599, .F. ) ;
#48011 = EDGE_CURVE ( 'NONE', #42214, #44744, #29048, .T. ) ;
#48013 = CARTESIAN_POINT ( 'NONE',  ( 2.229367062500001939, -70.22916666530107932, 3.861377020970579999 ) ) ;
#48014 = CARTESIAN_POINT ( 'NONE',  ( 2.500000000000002220, 28.33333333333333215, 4.330127018922192761 ) ) ;
#48015 = CARTESIAN_POINT ( 'NONE',  ( -6.972266317189433020E-16, -56.12499999726880162, -5.000000000000000000 ) ) ;
#48016 = VECTOR ( 'NONE', #9789, 1000.000000000000000 ) ;
#48017 = ORIENTED_EDGE ( 'NONE', *, *, #58198, .T. ) ;
#48018 = AXIS2_PLACEMENT_3D ( 'NONE', #53872, #3428, #9799 ) ;
#48019 = EDGE_CURVE ( 'NONE', #24978, #45572, #27133, .T. ) ;
#48020 = CARTESIAN_POINT ( 'NONE',  ( -5.000000000000000000, -82.99999999999998579, 0.000000000000000000 ) ) ;
#48021 = CARTESIAN_POINT ( 'NONE',  ( -4.458734124999999437, -54.56249999863440081, 0.000000000000000000 ) ) ;
#48022 = CARTESIAN_POINT ( 'NONE',  ( -2.229367062499996610, 0.6041666680322611560, 3.861377020970582219 ) ) ;
#48023 = ORIENTED_EDGE ( 'NONE', *, *, #909, .T. ) ;
#48024 = VECTOR ( 'NONE', #4325, 1000.000000000000114 ) ;
#48025 = CARTESIAN_POINT ( 'NONE',  ( 6.123233995736766282E-16, -170.0000000000000000, -5.000000000000000000 ) ) ;
#48026 = CARTESIAN_POINT ( 'NONE',  ( 4.458734125000001214, 16.10416666803225993, 2.574251347313718519 ) ) ;
#48027 = CARTESIAN_POINT ( 'NONE',  ( -59.44456063193725015, -146.5625000013656063, -0.3552334253322034230 ) ) ;
#48028 = CARTESIAN_POINT ( 'NONE',  ( -4.999999999999998224, -1.916666666666663854, 2.886751345948131764 ) ) ;
#48029 = CARTESIAN_POINT ( 'NONE',  ( -4.458734124999999437, -163.9375000013655779, -5.460374474430324690E-16 ) ) ;
#48030 = ORIENTED_EDGE ( 'NONE', *, *, #23605, .T. ) ;
#48031 = CARTESIAN_POINT ( 'NONE',  ( -4.458734124999999437, -78.39583333196772230, -2.574251347313719407 ) ) ;
#48032 = DIRECTION ( 'NONE',  ( 0.000000000000000000, 0.000000000000000000, 1.000000000000000000 ) ) ;
#48033 = CARTESIAN_POINT ( 'NONE',  ( -4.458734124999998549, 8.770833334698927786, 2.574251347313722516 ) ) ;
#48034 = CARTESIAN_POINT ( 'NONE',  ( 1.975475456537005874E-15, -15.62499999726881406, 5.000000000000000000 ) ) ;
#48035 = CARTESIAN_POINT ( 'NONE',  ( -4.458734124999998549, -59.47916666530106511, 2.574251347313722516 ) ) ;
#48036 = CARTESIAN_POINT ( 'NONE',  ( 1.060575238724906964E-15, -20.62499999726880873, 5.773502691896257311 ) ) ;
#48037 = CARTESIAN_POINT ( 'NONE',  ( -58.80597590150559739, -142.0000000000000284, 3.242614290531460330 ) ) ;
#48038 = CARTESIAN_POINT ( 'NONE',  ( 0.000000000000000000, -170.0000000000000000, 0.000000000000000000 ) ) ;
#48039 = CARTESIAN_POINT ( 'NONE',  ( -1.339745962155613812, -106.0803417985302843, -5.000000000000000000 ) ) ;
#48040 = CARTESIAN_POINT ( 'NONE',  ( 0.000000000000000000, -170.0000000000000000, 0.000000000000000000 ) ) ;
#48041 = CARTESIAN_POINT ( 'NONE',  ( -2.229367062499996610, -42.14583333196773651, 3.861377020970582219 ) ) ;
#48042 = CARTESIAN_POINT ( 'NONE',  ( -2.229367062500000163, -27.72916666530107221, -3.861377020970580443 ) ) ;
#48043 = FACE_OUTER_BOUND ( 'NONE', #7081, .T. ) ;
#48044 = CARTESIAN_POINT ( 'NONE',  ( 5.000000000000000888, 26.41666666666666430, 2.886751345948126879 ) ) ;
#48045 = CARTESIAN_POINT ( 'NONE',  ( -5.000000000000000000, -151.6250000027312126, -6.123233995736766282E-16 ) ) ;
#48046 = VERTEX_POINT ( 'NONE', #9188 ) ;
#48047 = CARTESIAN_POINT ( 'NONE',  ( -3.152548672688508926E-16, -106.8124999986343795, -5.148502694627439702 ) ) ;
#48048 = CARTESIAN_POINT ( 'NONE',  ( -4.458734124999999437, -33.31249999863440792, 0.000000000000000000 ) ) ;
#48049 = CARTESIAN_POINT ( 'NONE',  ( 2.500000000000002220, -69.54166666393547303, 4.330127018922192761 ) ) ;
#48050 = CARTESIAN_POINT ( 'NONE',  ( -58.39396692619412477, -148.6875000013656063, 2.891590998281057701 ) ) ;
#48051 =( BOUNDED_CURVE ( )  B_SPLINE_CURVE ( 2, ( #20034, #45757, #54123, #20687, #16169, #29993, #30313, #50261, #60250 ),
 .UNSPECIFIED., .F., .F. ) 
 B_SPLINE_CURVE_WITH_KNOTS ( ( 3, 2, 2, 2, 3 ),
 ( 0.1354166666666666574, 0.1361111111111110994, 0.1375000000000000111, 0.1388888888888888951, 0.1395833333333333370 ),
 .UNSPECIFIED. ) 
 CURVE ( )  GEOMETRIC_REPRESENTATION_ITEM ( )  RATIONAL_B_SPLINE_CURVE ( ( 0.9330127018922194093, 0.9330127018922194093, 1.000000000000000000, 0.8660254037844387076, 1.000000000000000000, 0.8660254037844387076, 1.000000000000000000, 0.9330127018922194093, 0.9330127018922194093 ) ) 
 REPRESENTATION_ITEM ( '' )  );
#48052 = CARTESIAN_POINT ( 'NONE',  ( -3.535533905932737309, -142.6250000000000000, -3.535533905932738197 ) ) ;
#48053 = CARTESIAN_POINT ( 'NONE',  ( -3.152548672688508926E-16, -29.56249999863440436, -5.148502694627439702 ) ) ;
#48054 = CARTESIAN_POINT ( 'NONE',  ( 4.458734125000000326, -73.14583333196772230, 2.574251347313718519 ) ) ;
#48055 = CARTESIAN_POINT ( 'NONE',  ( 4.458734124999999437, -169.6875000013656063, 0.000000000000000000 ) ) ;
#48056 = CARTESIAN_POINT ( 'NONE',  ( -3.152548672688508926E-16, -32.56249999863440792, -5.148502694627439702 ) ) ;
#48057 = DIRECTION ( 'NONE',  ( -0.000000000000000000, 1.000000000000000000, -0.000000000000000000 ) ) ;
#48058 = CARTESIAN_POINT ( 'NONE',  ( -55.39835681537999790, -138.0000000027312126, 4.984105922594378235 ) ) ;
#48059 = CARTESIAN_POINT ( 'NONE',  ( 5.000000000000000888, -22.58333333333333215, 2.886751345948126879 ) ) ;
#48060 = CARTESIAN_POINT ( 'NONE',  ( 4.458734125000000326, -149.3750000013656347, -1.846868145590734978 ) ) ;
#48061 = ORIENTED_EDGE ( 'NONE', *, *, #44085, .T. ) ;
#48062 = CARTESIAN_POINT ( 'NONE',  ( 1.975475456537005874E-15, -78.62499999726881583, 5.000000000000000000 ) ) ;
#48063 = CARTESIAN_POINT ( 'NONE',  ( 9.457646018065525792E-16, -55.31249999863439371, 5.148502694627439702 ) ) ;
#48064 = CARTESIAN_POINT ( 'NONE',  ( 1.975475456537005874E-15, -90.62499999726880162, 5.000000000000000000 ) ) ;
#48065 = DIRECTION ( 'NONE',  ( -0.000000000000000000, 1.000000000000000000, -0.000000000000000000 ) ) ;
#48066 = CARTESIAN_POINT ( 'NONE',  ( 2.500000000000002220, 18.33333333333333215, 4.330127018922192761 ) ) ;
#48067 = LINE ( 'NONE', #28137, #6952 ) ;
#48068 = CARTESIAN_POINT ( 'NONE',  ( -4.458734124999998549, 0.7708333346989267865, 2.574251347313722516 ) ) ;
#48069 = CARTESIAN_POINT ( 'NONE',  ( -5.000000000000000888, -154.4375000000000000, 2.071067811865474617 ) ) ;
#48070 = EDGE_CURVE ( 'NONE', #53780, #26245, #57453, .T. ) ;
#48071 = CARTESIAN_POINT ( 'NONE',  ( -9.184850993605147944E-16, -164.3750000027311842, 5.000000000000000000 ) ) ;
#48072 = CARTESIAN_POINT ( 'NONE',  ( -4.458734124999999437, 10.35416666803225816, -2.574251347313719407 ) ) ;
#48073 = CARTESIAN_POINT ( 'NONE',  ( -6.972266317189433020E-16, -53.12499999726880162, -5.000000000000000000 ) ) ;
#48074 = ORIENTED_EDGE ( 'NONE', *, *, #51594, .F. ) ;
#48075 = CARTESIAN_POINT ( 'NONE',  ( -50.18089887299981200, -135.6875000000000000, 2.462841084822874116 ) ) ;
#48076 = CARTESIAN_POINT ( 'NONE',  ( -3.152548672688508926E-16, -48.56249999863440792, -5.148502694627439702 ) ) ;
#48077 = CARTESIAN_POINT ( 'NONE',  ( -3.152801135295367096, -161.3125000013656063, -3.152801135295367541 ) ) ;
#48078 = AXIS2_PLACEMENT_3D ( 'NONE', #30615, #59911, #35447 ) ;
#48079 = CARTESIAN_POINT ( 'NONE',  ( 5.000000000000000000, -52.37499999726881583, -6.123233995736766282E-16 ) ) ;
#48080 = ORIENTED_EDGE ( 'NONE', *, *, #26824, .F. ) ;
#48081 = CARTESIAN_POINT ( 'NONE',  ( -4.458734124999998549, -23.22916666530107221, 2.574251347313722516 ) ) ;
#48082 = ORIENTED_EDGE ( 'NONE', *, *, #411, .T. ) ;
#48083 = CARTESIAN_POINT ( 'NONE',  ( 5.000000000000000000, -53.41666666666667140, -2.886751345948130876 ) ) ;
#48084 = CARTESIAN_POINT ( 'NONE',  ( 3.152801135295367541, -159.3125000013656063, -3.152801135295367541 ) ) ;
#48085 = EDGE_CURVE ( 'NONE', #11953, #14479, #57776, .T. ) ;
#48086 = ORIENTED_EDGE ( 'NONE', *, *, #6693, .F. ) ;
#48087 = EDGE_CURVE ( 'NONE', #58058, #12673, #42019, .T. ) ;
#48088 = DIRECTION ( 'NONE',  ( -1.000000000000000000, 0.000000000000000000, 0.000000000000000000 ) ) ;
#48089 = CARTESIAN_POINT ( 'NONE',  ( -59.81910112700025905, -133.1875000000000284, -2.462841084822630311 ) ) ;
#48090 = CARTESIAN_POINT ( 'NONE',  ( -4.458734124999999437, -37.64583333196773651, -2.574251347313719407 ) ) ;
#48091 = EDGE_LOOP ( 'NONE', ( #34240, #3036, #31364, #36795 ) ) ;
#48092 = EDGE_CURVE ( 'NONE', #19422, #6296, #24559, .T. ) ;
#48093 = CARTESIAN_POINT ( 'NONE',  ( 4.458734124999998549, -83.72916666530107932, -2.574251347313721627 ) ) ;
#48094 = CARTESIAN_POINT ( 'NONE',  ( 9.457646018065525792E-16, 19.93750000136559208, 5.148502694627439702 ) ) ;
#48095 = CARTESIAN_POINT ( 'NONE',  ( -1.339745962155613812, -18.08034179853029499, -5.000000000000000000 ) ) ;
#48096 =( BOUNDED_CURVE ( )  B_SPLINE_CURVE ( 2, ( #55702, #20323, #24828, #25141, #10662, #34798, #40258, #29639, #40885 ),
 .UNSPECIFIED., .F., .F. ) 
 B_SPLINE_CURVE_WITH_KNOTS ( ( 3, 2, 2, 2, 3 ),
 ( 0.5104166666666666297, 0.5111111111111110716, 0.5124999999999999556, 0.5138888888888888395, 0.5145833333333332815 ),
 .UNSPECIFIED. ) 
 CURVE ( )  GEOMETRIC_REPRESENTATION_ITEM ( )  RATIONAL_B_SPLINE_CURVE ( ( 0.9330127018922194093, 0.9330127018922194093, 1.000000000000000000, 0.8660254037844387076, 1.000000000000000000, 0.8660254037844387076, 1.000000000000000000, 0.9330127018922194093, 0.9330127018922194093 ) ) 
 REPRESENTATION_ITEM ( '' )  );
#48097 = ORIENTED_EDGE ( 'NONE', *, *, #12660, .F. ) ;
#48098 = CARTESIAN_POINT ( 'NONE',  ( -50.55543936806279248, -138.3125000013656063, 0.3552334253322060320 ) ) ;
#48099 = CARTESIAN_POINT ( 'NONE',  ( 4.458734125000001214, -85.14583333196773651, 2.574251347313718519 ) ) ;
#48100 = CARTESIAN_POINT ( 'NONE',  ( -50.01589407740564042, -127.7500000027312126, 0.3983568153799778022 ) ) ;
#48101 = CARTESIAN_POINT ( 'NONE',  ( 2.500000000000002220, -35.54166666393547303, 4.330127018922192761 ) ) ;
#48102 = CARTESIAN_POINT ( 'NONE',  ( 1.975475456537005874E-15, 0.3750000027311862216, 5.000000000000000000 ) ) ;
#48103 =( BOUNDED_CURVE ( )  B_SPLINE_CURVE ( 2, ( #16289, #1832, #21433, #5682, #35909, #874, #46192, #55541, #6964 ),
 .UNSPECIFIED., .F., .F. ) 
 B_SPLINE_CURVE_WITH_KNOTS ( ( 3, 2, 2, 2, 3 ),
 ( 0.02321428571428571508, 0.02380952380952380820, 0.02500000000000000139, 0.02619047619047619110, 0.02678571428571428770 ),
 .UNSPECIFIED. ) 
 CURVE ( )  GEOMETRIC_REPRESENTATION_ITEM ( )  RATIONAL_B_SPLINE_CURVE ( ( 0.9330127018922194093, 0.9330127018922195203, 1.000000000000000000, 0.8660254037844387076, 1.000000000000000000, 0.8660254037844387076, 1.000000000000000000, 0.9330127018922191873, 0.9330127018922194093 ) ) 
 REPRESENTATION_ITEM ( '' )  );
#48104 = AXIS2_PLACEMENT_3D ( 'NONE', #20869, #51409, #36930 ) ;
#48105 = CARTESIAN_POINT ( 'NONE',  ( -2.229367062500000163, -57.47916666530107932, -3.861377020970580443 ) ) ;
#48106 = CARTESIAN_POINT ( 'NONE',  ( 1.975475456537005874E-15, -84.62499999726880162, 5.000000000000000000 ) ) ;
#48107 = CARTESIAN_POINT ( 'NONE',  ( -2.229367062500000163, 25.52083333469892779, -3.861377020970580443 ) ) ;
#48108 = VECTOR ( 'NONE', #58609, 1000.000000000000000 ) ;
#48109 = CARTESIAN_POINT ( 'NONE',  ( 2.499999999999998668, -42.33333333333333570, -4.330127018922193649 ) ) ;
#48110 = CARTESIAN_POINT ( 'NONE',  ( -58.24261429053147765, -155.0000000000000284, -3.805975901505573411 ) ) ;
#48111 = CARTESIAN_POINT ( 'NONE',  ( 4.458734125000001214, -44.14583333196773651, 2.574251347313718519 ) ) ;
#48112 = CARTESIAN_POINT ( 'NONE',  ( 5.000000000000000000, -5.291666663935480130, -2.886751345948129988 ) ) ;
#48113 = CARTESIAN_POINT ( 'NONE',  ( -1.339745962155613812, -93.20534180126148271, -5.000000000000000000 ) ) ;
#48114 = CARTESIAN_POINT ( 'NONE',  ( -6.972266317189433020E-16, -46.12499999726880873, -5.000000000000000000 ) ) ;
#48115 = CARTESIAN_POINT ( 'NONE',  ( 4.458734125000001214, -82.14583333196772230, 2.574251347313718519 ) ) ;
#48116 = CARTESIAN_POINT ( 'NONE',  ( -3.152548672688508926E-16, -106.5624999986343937, -5.148502694627439702 ) ) ;
#48117 = CARTESIAN_POINT ( 'NONE',  ( 4.458734125000000326, -12.14583333196774007, 2.574251347313718519 ) ) ;
#48118 = ORIENTED_EDGE ( 'NONE', *, *, #9960, .F. ) ;
#48119 = CARTESIAN_POINT ( 'NONE',  ( 1.975475456537005874E-15, -9.624999997268814056, 5.000000000000000000 ) ) ;
#48120 = CARTESIAN_POINT ( 'NONE',  ( -2.229367062500000163, -97.47916666530105090, -3.861377020970580443 ) ) ;
#48121 = CARTESIAN_POINT ( 'NONE',  ( -3.535533905932738641, -166.5000000027312126, 3.535533905932737309 ) ) ;
#48122 = CARTESIAN_POINT ( 'NONE',  ( -3.152548672688508926E-16, -94.81249999863442213, -5.148502694627439702 ) ) ;
#48123 = CARTESIAN_POINT ( 'NONE',  ( 5.000000000000000000, -53.29166666393547303, -2.886751345948129988 ) ) ;
#48124 = CARTESIAN_POINT ( 'NONE',  ( -1.339745962155613812, -30.20534180126148271, -5.000000000000000000 ) ) ;
#48125 = AXIS2_PLACEMENT_3D ( 'NONE', #36821, #32940, #61591 ) ;
#48126 = CARTESIAN_POINT ( 'NONE',  ( -59.59170313451811296, -130.5000000013656063, 1.485763867205729394 ) ) ;
#48127 = CARTESIAN_POINT ( 'NONE',  ( -50.40829686548195099, -148.0000000013656063, -1.485763867205728284 ) ) ;
#48128 = CARTESIAN_POINT ( 'NONE',  ( 4.458734124999999437, -12.81249999863440259, -5.460374474430324690E-16 ) ) ;
#48129 = CARTESIAN_POINT ( 'NONE',  ( -4.458734124999998549, 13.52083333469892779, 2.574251347313722516 ) ) ;
#48130 = CARTESIAN_POINT ( 'NONE',  ( -4.458734124999997661, -57.47916666530108643, 2.574251347313722516 ) ) ;
#48131 = DIRECTION ( 'NONE',  ( -0.000000000000000000, 1.000000000000000000, -0.000000000000000000 ) ) ;
#48132 = CARTESIAN_POINT ( 'NONE',  ( -6.972266317189433020E-16, 6.875000002731185944, -5.000000000000000000 ) ) ;
#48133 = CARTESIAN_POINT ( 'NONE',  ( 4.458734124999998549, -11.72916666530107044, -2.574251347313721627 ) ) ;
#48134 = CARTESIAN_POINT ( 'NONE',  ( 1.339745962155615144, -106.5803417985302843, 4.999999999999999112 ) ) ;
#48135 = ORIENTED_EDGE ( 'NONE', *, *, #54784, .T. ) ;
#48136 = CARTESIAN_POINT ( 'NONE',  ( -2.229367062500000163, -38.72916666530107221, -3.861377020970580443 ) ) ;
#48137 = DIRECTION ( 'NONE',  ( -0.000000000000000000, 1.000000000000000000, -0.000000000000000000 ) ) ;
#48138 = LINE ( 'NONE', #13419, #53431 ) ;
#48139 = CARTESIAN_POINT ( 'NONE',  ( -5.000000000000000000, 27.12500000273118772, 0.000000000000000000 ) ) ;
#48140 = CARTESIAN_POINT ( 'NONE',  ( -4.458734124999999437, -87.31249999863439371, 0.000000000000000000 ) ) ;
#48141 = CARTESIAN_POINT ( 'NONE',  ( -4.458734124999998549, 19.52083333469893134, 2.574251347313722516 ) ) ;
#48143 = EDGE_CURVE ( 'NONE', #15979, #45293, #15552, .T. ) ;
#48142 = CARTESIAN_POINT ( 'NONE',  ( 4.458734125000001214, 13.10416666803226171, 2.574251347313718519 ) ) ;
#48144 = CARTESIAN_POINT ( 'NONE',  ( -5.000000000000000000, -48.00000000000000000, 0.000000000000000000 ) ) ;
#48145 = CARTESIAN_POINT ( 'NONE',  ( -50.01589407740564042, -137.7500000027312126, 0.3983568153799778022 ) ) ;
#48146 = CARTESIAN_POINT ( 'NONE',  ( -2.229367062499996610, -86.39583333196773651, 3.861377020970582219 ) ) ;
#48147 = CARTESIAN_POINT ( 'NONE',  ( -4.999999999999999112, -68.91666666666667140, 2.886751345948131764 ) ) ;
#48148 = CARTESIAN_POINT ( 'NONE',  ( 1.060575238724906964E-15, 14.37500000273118594, 5.773502691896257311 ) ) ;
#48149 = ORIENTED_EDGE ( 'NONE', *, *, #17654, .F. ) ;
#48150 = CARTESIAN_POINT ( 'NONE',  ( 5.000000000000000000, -79.41666666666665719, -2.886751345948130876 ) ) ;
#48151 = VECTOR ( 'NONE', #54156, 1000.000000000000000 ) ;
#48152 = CARTESIAN_POINT ( 'NONE',  ( 3.535533905932736864, -167.1250000000000284, 3.535533905932738641 ) ) ;
#48153 =( BOUNDED_CURVE ( )  B_SPLINE_CURVE ( 2, ( #154, #52053, #49012, #27907, #39361, #58992, #4961, #7677, #27591 ),
 .UNSPECIFIED., .F., .F. ) 
 B_SPLINE_CURVE_WITH_KNOTS ( ( 3, 2, 2, 2, 3 ),
 ( 0.2437499999999999944, 0.2444444444444444364, 0.2458333333333333204, 0.2472222222222222321, 0.2479166666666666741 ),
 .UNSPECIFIED. ) 
 CURVE ( )  GEOMETRIC_REPRESENTATION_ITEM ( )  RATIONAL_B_SPLINE_CURVE ( ( 0.9330127018922194093, 0.9330127018922194093, 1.000000000000000000, 0.8660254037844387076, 1.000000000000000000, 0.8660254037844387076, 1.000000000000000000, 0.9330127018922194093, 0.9330127018922194093 ) ) 
 REPRESENTATION_ITEM ( '' )  );
#48155 = CARTESIAN_POINT ( 'NONE',  ( -4.999999999999999112, -28.91666666666666430, 2.886751345948131764 ) ) ;
#48154 = CARTESIAN_POINT ( 'NONE',  ( 1.975475456537005874E-15, 2.249999999999999556, 5.000000000000000000 ) ) ;
#48156 = CARTESIAN_POINT ( 'NONE',  ( -4.458734124999998549, -32.22916666530106511, 2.574251347313722516 ) ) ;
#48157 = CARTESIAN_POINT ( 'NONE',  ( -2.500000000000000444, -36.04166666393547303, -4.330127018922193649 ) ) ;
#48159 = ORIENTED_EDGE ( 'NONE', *, *, #45623, .T. ) ;
#48158 = CARTESIAN_POINT ( 'NONE',  ( 2.229367062500001939, -62.97916666530106511, 3.861377020970579999 ) ) ;
#48160 = CARTESIAN_POINT ( 'NONE',  ( -50.40829686548195099, -149.2500000013655779, -1.485763867205728284 ) ) ;
#48162 = ORIENTED_EDGE ( 'NONE', *, *, #45342, .F. ) ;
#48161 = CARTESIAN_POINT ( 'NONE',  ( 4.458734125000001214, -12.14583333196774007, 2.574251347313718519 ) ) ;
#48163 = CARTESIAN_POINT ( 'NONE',  ( -2.499999999999996447, -78.83333333333332860, 4.330127018922195425 ) ) ;
#48164 = CARTESIAN_POINT ( 'NONE',  ( -50.40829686548195099, -136.0000000013656063, -1.485763867205728284 ) ) ;
#48165 = CARTESIAN_POINT ( 'NONE',  ( 2.229367062499998831, -57.89583333196773651, -3.861377020970580887 ) ) ;
#48166 = CARTESIAN_POINT ( 'NONE',  ( -2.500000000000000444, -81.04166666393547303, -4.330127018922193649 ) ) ;
#48168 = ORIENTED_EDGE ( 'NONE', *, *, #9514, .T. ) ;
#48167 = DIRECTION ( 'NONE',  ( -0.000000000000000000, 1.000000000000000000, -0.000000000000000000 ) ) ;
#48169 = CARTESIAN_POINT ( 'NONE',  ( -53.33387254593733928, -144.8125000000000284, 5.149110718188519620 ) ) ;
#48170 = CARTESIAN_POINT ( 'NONE',  ( -2.229367062500000163, -21.72916666530107221, -3.861377020970580443 ) ) ;
#48171 = AXIS2_PLACEMENT_3D ( 'NONE', #9755, #29362, #53517 ) ;
#48173 = ORIENTED_EDGE ( 'NONE', *, *, #23271, .F. ) ;
#48172 = CARTESIAN_POINT ( 'NONE',  ( -4.458734124999999437, -57.56249999863440081, 0.000000000000000000 ) ) ;
#48174 = CARTESIAN_POINT ( 'NONE',  ( 0.000000000000000000, 0.000000000000000000, 0.000000000000000000 ) ) ;
#48175 = CARTESIAN_POINT ( 'NONE',  ( 2.730187237215162345E-16, -167.4375000013655779, -4.458734124999999437 ) ) ;
#48176 = CARTESIAN_POINT ( 'NONE',  ( 4.458734124999998549, -102.9791666653010651, -2.574251347313721627 ) ) ;
#48177 = CARTESIAN_POINT ( 'NONE',  ( 3.061616997868383141E-16, -167.8750000027312126, -5.000000000000000000 ) ) ;
#48178 = ORIENTED_EDGE ( 'NONE', *, *, #44512, .T. ) ;
#48179 = CARTESIAN_POINT ( 'NONE',  ( -59.59170313451810586, -149.7500000013656063, 1.485763867205729394 ) ) ;
#48180 = CARTESIAN_POINT ( 'NONE',  ( -54.60164318462004474, -140.5000000027312126, -4.984105922594373794 ) ) ;
#48181 = CARTESIAN_POINT ( 'NONE',  ( 2.229367062499998831, -37.64583333196773651, -3.861377020970580887 ) ) ;
#48182 = FACE_OUTER_BOUND ( 'NONE', #27221, .T. ) ;
#48183 = CARTESIAN_POINT ( 'NONE',  ( 9.457646018065525792E-16, -8.062499998634404363, 5.148502694627439702 ) ) ;
#48184 = CARTESIAN_POINT ( 'NONE',  ( -4.458734124999999437, -98.64583333196773651, -2.574251347313719407 ) ) ;
#48185 = CARTESIAN_POINT ( 'NONE',  ( -3.152801135295367985, -143.0625000013655779, 3.152801135295367096 ) ) ;
#48186 = CARTESIAN_POINT ( 'NONE',  ( -2.229367062500000163, -27.72916666530107221, -3.861377020970580443 ) ) ;
#48187 = CARTESIAN_POINT ( 'NONE',  ( 5.000000000000000000, -70.41666666666667140, -2.886751345948130876 ) ) ;
#48188 = CARTESIAN_POINT ( 'NONE',  ( -59.59170313451811296, -133.5000000013656347, 1.485763867205729394 ) ) ;
#48189 = CARTESIAN_POINT ( 'NONE',  ( -4.458734124999998549, -69.47916666530107932, 2.574251347313722516 ) ) ;
#48190 = CARTESIAN_POINT ( 'NONE',  ( -1.339745962155613812, -16.20534180126148271, -5.000000000000000000 ) ) ;
#48191 = CARTESIAN_POINT ( 'NONE',  ( -2.499999999999996447, -42.70833333060214443, 4.330127018922195425 ) ) ;
#48192 = CARTESIAN_POINT ( 'NONE',  ( 1.846868145590736310, -141.6250000013656347, 4.458734124999997661 ) ) ;
#48193 = CARTESIAN_POINT ( 'NONE',  ( 9.457646018065525792E-16, 6.687500001365594748, 5.148502694627439702 ) ) ;
#48194 = ORIENTED_EDGE ( 'NONE', *, *, #53528, .T. ) ;
#48195 = CARTESIAN_POINT ( 'NONE',  ( -5.000000000000000000, 1.999999999999998224, 0.000000000000000000 ) ) ;
#48196 = DIRECTION ( 'NONE',  ( -0.000000000000000000, 1.000000000000000000, -0.000000000000000000 ) ) ;
#48198 = CARTESIAN_POINT ( 'NONE',  ( -2.229367062499996610, -30.14583333196773651, 3.861377020970582219 ) ) ;
#48197 = CARTESIAN_POINT ( 'NONE',  ( -5.000000000000000000, -94.00000000000000000, 0.000000000000000000 ) ) ;
#48199 = CARTESIAN_POINT ( 'NONE',  ( -6.972266317189433020E-16, -14.12499999726881228, -5.000000000000000000 ) ) ;
#48200 = CARTESIAN_POINT ( 'NONE',  ( 2.229367062500001939, -75.22916666530106511, 3.861377020970579999 ) ) ;
#48201 = EDGE_CURVE ( 'NONE', #20975, #14229, #334, .T. ) ;
#48202 = CARTESIAN_POINT ( 'NONE',  ( 4.458734125000000326, 20.85416666803226349, 2.574251347313718519 ) ) ;
#48203 = FACE_OUTER_BOUND ( 'NONE', #63282, .T. ) ;
#48204 = CARTESIAN_POINT ( 'NONE',  ( -51.60603307380591787, -140.9375000013656063, -2.891590998281053704 ) ) ;
#48205 = CARTESIAN_POINT ( 'NONE',  ( 2.229367062500001939, 3.020833334698928674, 3.861377020970579999 ) ) ;
#48206 = CARTESIAN_POINT ( 'NONE',  ( 2.229367062499998831, 27.10416666803225993, -3.861377020970580887 ) ) ;
#48207 = CARTESIAN_POINT ( 'NONE',  ( -4.458734124999999437, -43.64583333196773651, -2.574251347313719407 ) ) ;
#48208 = CARTESIAN_POINT ( 'NONE',  ( 5.000000000000000000, -60.29166666393547303, -2.886751345948130876 ) ) ;
#48209 = CARTESIAN_POINT ( 'NONE',  ( -4.458734124999999437, 3.604166668032260379, -2.574251347313719407 ) ) ;
#48210 = CARTESIAN_POINT ( 'NONE',  ( 9.457646018065525792E-16, -25.31249999863440792, 5.148502694627439702 ) ) ;
#48211 = CARTESIAN_POINT ( 'NONE',  ( -3.152801135295367096, -154.0625000013656063, -3.152801135295367541 ) ) ;
#48212 = CARTESIAN_POINT ( 'NONE',  ( -2.229367062499996610, -71.14583333196773651, 3.861377020970582219 ) ) ;
#48213 = CARTESIAN_POINT ( 'NONE',  ( 5.000000000000000000, -102.2916666639354588, -2.886751345948129988 ) ) ;
#48214 = CARTESIAN_POINT ( 'NONE',  ( 1.975475456537005874E-15, -41.74999999999999289, 5.000000000000000000 ) ) ;
#48215 = CARTESIAN_POINT ( 'NONE',  ( 0.3483149870578491347, -8.861353789385031376, -7.493854785173814648 ) ) ;
#48216 = CARTESIAN_POINT ( 'NONE',  ( 4.458734124999998549, -106.9791666653010509, -2.574251347313721627 ) ) ;
#48217 = CARTESIAN_POINT ( 'NONE',  ( -2.229367062500000163, -70.72916666530107932, -3.861377020970580443 ) ) ;
#48218 = CARTESIAN_POINT ( 'NONE',  ( 1.060575238724906964E-15, -52.75000000000000000, 5.773502691896257311 ) ) ;
#48219 = DIRECTION ( 'NONE',  ( -0.000000000000000000, 1.000000000000000000, -0.000000000000000000 ) ) ;
#48220 = CARTESIAN_POINT ( 'NONE',  ( 5.000000000000000888, 28.54166666939785202, 2.886751345948126879 ) ) ;
#48221 = ORIENTED_EDGE ( 'NONE', *, *, #815, .T. ) ;
#48222 = CARTESIAN_POINT ( 'NONE',  ( -2.500000000000000444, -14.16666666666666785, -4.330127018922193649 ) ) ;
#48223 = CARTESIAN_POINT ( 'NONE',  ( -4.458734124999999437, -14.39583333196773474, -2.574251347313719407 ) ) ;
#48224 = CARTESIAN_POINT ( 'NONE',  ( -3.152548672688508926E-16, -76.56249999863440792, -5.148502694627439702 ) ) ;
#48225 =( BOUNDED_CURVE ( )  B_SPLINE_CURVE ( 2, ( #61407, #60458, #17015, #56263, #26343, #27296, #26984, #16384, #2866 ),
 .UNSPECIFIED., .F., .F. ) 
 B_SPLINE_CURVE_WITH_KNOTS ( ( 3, 2, 2, 2, 3 ),
 ( 0.9645833333333333481, 0.9652777777777777901, 0.9666666666666666741, 0.9680555555555555580, 0.9687500000000000000 ),
 .UNSPECIFIED. ) 
 CURVE ( )  GEOMETRIC_REPRESENTATION_ITEM ( )  RATIONAL_B_SPLINE_CURVE ( ( 0.9330127018922194093, 0.9330127018922194093, 1.000000000000000000, 0.8660254037844387076, 1.000000000000000000, 0.8660254037844387076, 1.000000000000000000, 0.9330127018922194093, 0.9330127018922194093 ) ) 
 REPRESENTATION_ITEM ( '' )  );
#48226 = CARTESIAN_POINT ( 'NONE',  ( -8.190561711645485556E-16, -166.9375000013655779, 4.458734124999999437 ) ) ;
#48227 = CARTESIAN_POINT ( 'NONE',  ( -2.499999999999996447, -20.70833333060214798, 4.330127018922195425 ) ) ;
#48229 = EDGE_LOOP ( 'NONE', ( #57768, #31013, #47239, #45163 ) ) ;
#48228 = CARTESIAN_POINT ( 'NONE',  ( -2.229367062499996610, -42.14583333196773651, 3.861377020970582219 ) ) ;
#48230 = CARTESIAN_POINT ( 'NONE',  ( 5.000000000000000888, -45.45833333060214443, 2.886751345948126879 ) ) ;
#48232 = ORIENTED_EDGE ( 'NONE', *, *, #18815, .F. ) ;
#48231 = CARTESIAN_POINT ( 'NONE',  ( -2.229367062499996610, 8.604166668032261711, 3.861377020970582219 ) ) ;
#48233 = CYLINDRICAL_SURFACE ( 'NONE', #59736, 5.000000000000000000 ) ;
#48234 = CARTESIAN_POINT ( 'NONE',  ( -3.535250795749689387E-16, -61.25000000000000000, -5.773502691896257311 ) ) ;
#48235 = CARTESIAN_POINT ( 'NONE',  ( 3.152801135295367541, -155.5625000013656063, -3.152801135295367541 ) ) ;
#48236 = CARTESIAN_POINT ( 'NONE',  ( 2.229367062500001939, -40.22916666530107221, 3.861377020970579999 ) ) ;
#48237 = PRODUCT_DEFINITION_FORMATION_WITH_SPECIFIED_SOURCE ( 'ANY', '', #19930, .NOT_KNOWN. ) ;
#48238 = CARTESIAN_POINT ( 'NONE',  ( 6.123233995736766282E-16, -120.0000000000000000, -5.000000000000000000 ) ) ;
#48239 = CARTESIAN_POINT ( 'NONE',  ( -3.535533905932738641, -161.3750000000000284, 3.535533905932737309 ) ) ;
#48240 = CARTESIAN_POINT ( 'NONE',  ( 2.500000000000002220, 5.458333336064518981, 4.330127018922192761 ) ) ;
#48241 = AXIS2_PLACEMENT_3D ( 'NONE', #14043, #53287, #37876 ) ;
#48242 = CARTESIAN_POINT ( 'NONE',  ( -56.48576386720575471, -127.0000000013656063, -4.591703134518078322 ) ) ;
#48243 = CARTESIAN_POINT ( 'NONE',  ( 4.458734125000001214, -8.145833331967736513, 2.574251347313718519 ) ) ;
#48244 = CARTESIAN_POINT ( 'NONE',  ( 9.457646018065525792E-16, -41.31249999863440081, 5.148502694627439702 ) ) ;
#48245 =( BOUNDED_CURVE ( )  B_SPLINE_CURVE ( 2, ( #50367, #35576, #30418, #41025, #31059, #16905, #26560, #6314, #40704 ),
 .UNSPECIFIED., .F., .F. ) 
 B_SPLINE_CURVE_WITH_KNOTS ( ( 3, 2, 2, 2, 3 ),
 ( 0.8589285714285714857, 0.8595238095238095788, 0.8607142857142857650, 0.8619047619047619513, 0.8625000000000000444 ),
 .UNSPECIFIED. ) 
 CURVE ( )  GEOMETRIC_REPRESENTATION_ITEM ( )  RATIONAL_B_SPLINE_CURVE ( ( 0.9330127018922194093, 0.9330127018922256266, 1.000000000000000000, 0.8660254037844387076, 1.000000000000000000, 0.8660254037844387076, 1.000000000000000000, 0.9330127018922194093, 0.9330127018922194093 ) ) 
 REPRESENTATION_ITEM ( '' )  );
#48246 = CARTESIAN_POINT ( 'NONE',  ( 4.458734125000000326, -149.3750000013656347, -1.846868145590734978 ) ) ;
#48247 = CARTESIAN_POINT ( 'NONE',  ( -4.458734124999999437, -89.56249999863440792, 0.000000000000000000 ) ) ;
#48248 = CARTESIAN_POINT ( 'NONE',  ( 5.000000000000000000, -167.1875000027312126, 2.071067811865478614 ) ) ;
#48249 = ORIENTED_EDGE ( 'NONE', *, *, #15362, .F. ) ;
#48250 = CARTESIAN_POINT ( 'NONE',  ( -4.999999999999998224, 3.208333336064520758, 2.886751345948131764 ) ) ;
#48251 = CARTESIAN_POINT ( 'NONE',  ( -52.53715891517739323, -150.5625000027311842, -4.819101127000233298 ) ) ;
#48252 = CARTESIAN_POINT ( 'NONE',  ( 5.000000000000000888, -43.58333333333333570, 2.886751345948126879 ) ) ;
#48253 = CARTESIAN_POINT ( 'NONE',  ( -4.458734124999999437, -77.64583333196773651, -2.574251347313719407 ) ) ;
#48254 = ORIENTED_EDGE ( 'NONE', *, *, #61347, .T. ) ;
#48255 = CARTESIAN_POINT ( 'NONE',  ( -62.00000000000001421, -155.0000000000000284, -4.041451884327373456 ) ) ;
#48256 = CARTESIAN_POINT ( 'NONE',  ( -2.229367062500000163, -9.729166665301068662, -3.861377020970580443 ) ) ;
#48257 = CARTESIAN_POINT ( 'NONE',  ( -5.000000000000000888, 6.123233995736767268E-16, 0.000000000000000000 ) ) ;
#48258 = CARTESIAN_POINT ( 'NONE',  ( 4.458734125000001214, -1.895833331967737623, 2.574251347313718519 ) ) ;
#48259 = CARTESIAN_POINT ( 'NONE',  ( -2.499999999999996447, -42.83333333333333570, 4.330127018922195425 ) ) ;
#48260 = CARTESIAN_POINT ( 'NONE',  ( -8.190561711645485556E-16, -154.6875000013655779, 4.458734124999999437 ) ) ;
#48261 = CARTESIAN_POINT ( 'NONE',  ( 4.458734124999999437, 18.93750000136559564, -5.460374474430324690E-16 ) ) ;
#48262 = ORIENTED_EDGE ( 'NONE', *, *, #61683, .T. ) ;
#48263 = CARTESIAN_POINT ( 'NONE',  ( 2.229367062500001939, -90.97916666530106511, 3.861377020970579999 ) ) ;
#48264 = CARTESIAN_POINT ( 'NONE',  ( -5.000000000000000000, -33.87499999726880873, 0.000000000000000000 ) ) ;
#48265 = CARTESIAN_POINT ( 'NONE',  ( -58.80597590150559739, -154.1250000027312126, 3.242614290531460330 ) ) ;
#48266 = CARTESIAN_POINT ( 'NONE',  ( -2.229367062500000163, -13.47916666530107221, -3.861377020970580443 ) ) ;
#48267 = EDGE_CURVE ( 'NONE', #22693, #44005, #49286, .T. ) ;
#48268 = CARTESIAN_POINT ( 'NONE',  ( 0.000000000000000000, -120.0000000000000000, 0.000000000000000000 ) ) ;
#48269 = DIRECTION ( 'NONE',  ( -0.000000000000000000, 1.000000000000000000, -0.000000000000000000 ) ) ;
#48270 = LINE ( 'NONE', #48586, #697 ) ;
#48271 = CARTESIAN_POINT ( 'NONE',  ( -2.499999999999996447, -35.70833333060213732, 4.330127018922195425 ) ) ;
#48272 = FACE_OUTER_BOUND ( 'NONE', #30210, .T. ) ;
#48273 = CARTESIAN_POINT ( 'NONE',  ( -2.229367062500000163, 17.52083333469892779, -3.861377020970580443 ) ) ;
#48274 = CARTESIAN_POINT ( 'NONE',  ( 5.000000000000000000, -46.29166666393545881, -2.886751345948130876 ) ) ;
#48275 = CARTESIAN_POINT ( 'NONE',  ( 9.457646018065525792E-16, 17.93750000136559208, 5.148502694627439702 ) ) ;
#48276 = CARTESIAN_POINT ( 'NONE',  ( -3.152548672688508926E-16, -57.56249999863439371, -5.148502694627439702 ) ) ;
#48277 = CARTESIAN_POINT ( 'NONE',  ( 4.458734124999998549, -10.97916666530107044, -2.574251347313721627 ) ) ;
#48278 = CARTESIAN_POINT ( 'NONE',  ( 6.123233995736766282E-16, -170.0000000000000000, -5.000000000000000000 ) ) ;
#48279 = CARTESIAN_POINT ( 'NONE',  ( -5.000000000000000000, 9.000000000000001776, 0.000000000000000000 ) ) ;
#48280 = CARTESIAN_POINT ( 'NONE',  ( 1.846868145590736310, -167.6250000013655779, 4.458734124999999437 ) ) ;
#48281 = CARTESIAN_POINT ( 'NONE',  ( 5.000000000000000888, -69.58333333333332860, 2.886751345948126879 ) ) ;
#48282 = AXIS2_PLACEMENT_3D ( 'NONE', #53746, #63418, #8750 ) ;
#48283 = CARTESIAN_POINT ( 'NONE',  ( 2.229367062500001939, -53.97916666530107221, 3.861377020970579999 ) ) ;
#48284 = CARTESIAN_POINT ( 'NONE',  ( -2.499999999999996447, -83.70833333060214443, 4.330127018922195425 ) ) ;
#48285 = CARTESIAN_POINT ( 'NONE',  ( -51.60603307380591787, -134.1875000013656063, -2.891590998281053704 ) ) ;
#48286 = CARTESIAN_POINT ( 'NONE',  ( 2.500000000000002220, -14.54166666393548191, 4.330127018922192761 ) ) ;
#48287 = EDGE_CURVE ( 'NONE', #54583, #43806, #18828, .T. ) ;
#48288 = CARTESIAN_POINT ( 'NONE',  ( 0.000000000000000000, -170.0000000000000000, 0.000000000000000000 ) ) ;
#48289 = VECTOR ( 'NONE', #28343, 1000.000000000000000 ) ;
#48290 = ADVANCED_FACE ( 'NONE', ( #34564 ), #10447, .T. ) ;
#48291 = CARTESIAN_POINT ( 'NONE',  ( 2.229367062500001939, -92.22916666530106511, 3.861377020970579999 ) ) ;
#48292 = CARTESIAN_POINT ( 'NONE',  ( -1.846868145590734756, -159.3750000013656063, -4.458734124999999437 ) ) ;
#48293 = CARTESIAN_POINT ( 'NONE',  ( -5.000000000000000000, -38.99999999999999289, 0.000000000000000000 ) ) ;
#48294 = DIRECTION ( 'NONE',  ( -0.000000000000000000, 1.000000000000000000, -0.000000000000000000 ) ) ;
#48295 = VERTEX_POINT ( 'NONE', #23979 ) ;
#48296 = CARTESIAN_POINT ( 'NONE',  ( 2.229367062500001939, -97.97916666530105090, 3.861377020970579999 ) ) ;
#48297 = CARTESIAN_POINT ( 'NONE',  ( 2.229367062499998831, 10.10416666803225993, -3.861377020970580887 ) ) ;
#48298 = CARTESIAN_POINT ( 'NONE',  ( -2.499999999999996447, 9.291666669397853795, 4.330127018922195425 ) ) ;
#48299 =( BOUNDED_CURVE ( )  B_SPLINE_CURVE ( 2, ( #50331, #25564, #6912, #6277, #59670, #45180, #16241, #50648, #1783 ),
 .UNSPECIFIED., .F., .F. ) 
 B_SPLINE_CURVE_WITH_KNOTS ( ( 3, 2, 2, 2, 3 ),
 ( 0.3946428571428571286, 0.3952380952380952217, 0.3964285714285714080, 0.3976190476190475942, 0.3982142857142857428 ),
 .UNSPECIFIED. ) 
 CURVE ( )  GEOMETRIC_REPRESENTATION_ITEM ( )  RATIONAL_B_SPLINE_CURVE ( ( 0.9330127018922194093, 0.9330127018922194093, 1.000000000000000000, 0.8660254037844387076, 1.000000000000000000, 0.8660254037844387076, 1.000000000000000000, 0.9330127018922163007, 0.9330127018922194093 ) ) 
 REPRESENTATION_ITEM ( '' )  );
#48300 = CARTESIAN_POINT ( 'NONE',  ( -9.184850993605147944E-16, -158.2500000000000000, 5.000000000000000000 ) ) ;
#48301 = CARTESIAN_POINT ( 'NONE',  ( -5.000000000000000000, 1.000000000000000888, 0.000000000000000000 ) ) ;
#48302 = EDGE_CURVE ( 'NONE', #5147, #59356, #54842, .T. ) ;
#48303 = CARTESIAN_POINT ( 'NONE',  ( 2.229367062500001939, -59.97916666530106511, 3.861377020970579999 ) ) ;
#48304 = CARTESIAN_POINT ( 'NONE',  ( -9.184850993605147944E-16, -162.2500000000000000, 5.000000000000000000 ) ) ;
#48305 = CARTESIAN_POINT ( 'NONE',  ( -2.500000000000000444, -0.04166666393548221214, -4.330127018922193649 ) ) ;
#48306 = CARTESIAN_POINT ( 'NONE',  ( 4.458734125000001214, -28.89583333196774007, 2.574251347313718519 ) ) ;
#48307 = CARTESIAN_POINT ( 'NONE',  ( -6.972266317189433020E-16, -11.25000000000000178, -5.000000000000000000 ) ) ;
#48308 = CARTESIAN_POINT ( 'NONE',  ( -4.458734124999999437, 29.43750000136559208, 0.000000000000000000 ) ) ;
#48309 = CARTESIAN_POINT ( 'NONE',  ( -1.336351044127974539E-14, 25.24999999999999645, 5.000000000000000000 ) ) ;
#48310 = CARTESIAN_POINT ( 'NONE',  ( 5.000000000000000000, -42.41666666666667140, -2.886751345948129988 ) ) ;
#48312 = CARTESIAN_POINT ( 'NONE',  ( -2.229367062499996610, -27.39583333196774007, 3.861377020970582219 ) ) ;
#48311 = CARTESIAN_POINT ( 'NONE',  ( -2.500000000000000444, -90.04166666393547303, -4.330127018922193649 ) ) ;
#48313 = CARTESIAN_POINT ( 'NONE',  ( 2.500000000000002220, -64.66666666666665719, 4.330127018922192761 ) ) ;
#48314 = CARTESIAN_POINT ( 'NONE',  ( 9.457646018065525792E-16, -70.06249999863439371, 5.148502694627439702 ) ) ;
#48315 = CARTESIAN_POINT ( 'NONE',  ( -1.846868145590734756, -146.3750000013655779, -4.458734125000000326 ) ) ;
#48316 =( REPRESENTATION_RELATIONSHIP ('NONE','NONE', #27855, #49651 ) REPRESENTATION_RELATIONSHIP_WITH_TRANSFORMATION ( #41682 )SHAPE_REPRESENTATION_RELATIONSHIP( ) );
#48317 = CARTESIAN_POINT ( 'NONE',  ( -4.458734124999999437, -78.31249999863440792, 0.000000000000000000 ) ) ;
#48318 = CARTESIAN_POINT ( 'NONE',  ( -59.29741812935640155, -143.8750000013655779, -2.196230717870135685 ) ) ;
#48319 = CARTESIAN_POINT ( 'NONE',  ( -4.458734124999998549, -22.47916666530107577, 2.574251347313722516 ) ) ;
#48320 = CARTESIAN_POINT ( 'NONE',  ( -2.499999999999996447, -66.70833333060214443, 4.330127018922195425 ) ) ;
#48321 = ORIENTED_EDGE ( 'NONE', *, *, #24179, .F. ) ;
#48322 = EDGE_CURVE ( 'NONE', #40253, #7528, #19783, .T. ) ;
#48323 = CARTESIAN_POINT ( 'NONE',  ( -5.000000000000000888, -152.5625000027311842, 2.071067811865474617 ) ) ;
#48324 = ORIENTED_EDGE ( 'NONE', *, *, #30823, .T. ) ;
#48325 = CARTESIAN_POINT ( 'NONE',  ( 4.458734124999998549, -67.97916666530107932, -2.574251347313721627 ) ) ;
#48326 = CARTESIAN_POINT ( 'NONE',  ( -1.510657702057710340E-15, 28.25000000000000000, 5.000000000000000000 ) ) ;
#48327 = FILL_AREA_STYLE ('',( #46760 ) ) ;
#48328 = ORIENTED_EDGE ( 'NONE', *, *, #20950, .T. ) ;
#48329 = VECTOR ( 'NONE', #42513, 1000.000000000000000 ) ;
#48330 =( BOUNDED_CURVE ( )  B_SPLINE_CURVE ( 2, ( #15853, #54775, #6209, #1082, #49935, #58955, #5890, #35160, #55418, #20363, #11336, #30959, #59278, #25498, #24545, #39961, #15209, #120, #35476, #5245, #19714, #55093, #11018, #34490, #54124, #10062, #29674, #49306, #54459, #10385, #49627, #22597, #37070, #6844, #27399, #56694, #61198, #61520, #12922, #12610, #7166, #57007, #32223, #51542, #2033, #11647, #27091, #17120, #17450, #36746, #51854, #46708, #31915, #21319, #12299, #41547, #7797, #51230, #47030, #2980, #26457, #21638, #31268, #32543, #2653, #22272, #42194, #16488, #6525, #56051, #60879, #40920, #7478, #46075, #61836, #26776, #41231, #17758, #37374, #26138, #2343, #46395, #11967, #41873, #16803, #21951, #56376, #36423, #31597, #45758, #1710, #60563, #36109, #55732, #50902, #37685, #9354, #14490, #52170, #13869, #13567, #63092, #18387, #9048, #28966, #38006, #28032, #48589, #28657, #43134, #52801, #42507, #42822, #43758, #14177, #47650, #8736, #63403, #8114, #3604, #33185, #27718, #18694, #57948, #47345, #23534, #53111, #38616, #47961, #19319, #57328, #3295, #18063, #23211, #38320, #22914, #28344, #19002, #38935, #58571, #62774, #62467, #43447, #58251, #57639, #33492, #48273, #3916, #4229, #23844, #62144, #33804, #53420, #13243, #4530, #24155, #32866, #52496, #8429, #19639, #34111, #59854, #58875, #15778, #29274, #35395, #39886, #34420, #5806, #9666, #20927, #48904, #6135, #30235, #55017, #49858, #59531, #20613, #40218, #10939, #39, #35082, #25423, #10309, #50183, #1009, #54049, #30558, #25749, #25102, #45042, #40531, #45363, #34757, #1328, #59206, #24788, #60173, #29921, #53733, #4849, #24469, #675, #44074, #10622, #15464, #39249, #54701, #5488, #14806, #15135, #9986, #29598, #49230, #20284, #5170, #49546, #44394, #353, #19955, #39566, #54383, #44712, #6770, #50517, #61129, #36036, #41801, #36351, #50830, #2584, #12537, #16095, #11894, #31841, #16418, #46320, #45999, #21565, #17053, #35718, #1964, #2278, #55348, #16734, #36669, #51473, #41162, #1640, #36994, #42117, #11262, #41478, #60807, #21882, #27020, #7410, #51157, #32148, #56621, #45683, #56298, #7091, #55981, #6457, #26381, #12226, #30886, #11582, #31514, #26705, #26066, #46638, #21240, #22202, #27331, #40847, #51784, #60490, #61445, #17373, #7726, #46962, #2907, #22522, #55668, #31201, #27646, #33109, #52725, #3843, #33730, #9283, #37612, #53036, #8974, #57253, #8657, #43066, #13169, #42746, #12852, #4158, #3221, #61759, #23138, #32471, #33417, #57568, #57873, #28584, #48519, #18929, #23775, #22839, #43377, #56931, #63022, #23463, #62072, #48205, #37935, #28899, #28270, #42430, #38545, #24087, #8355, #4460, #52100, #17687, #17986, #18310, #58175, #27957, #37302, #14105, #18630, #8041, #52423, #13797, #47885, #53348, #47273, #32794, #62389, #47577, #13493, #3529, #62704, #38252, #35012, #58497, #5735, #4771, #14421, #20539, #63647, #602, #34352, #15704, #49789, #24716, #40136, #936, #43999, #29844, #44971, #19883, #19566, #39178, #59455, #15387, #54625, #15068, #10241, #49477, #58803, #53982, #59780, #39496, #14735, #30160, #35322, #43682, #59132, #10550, #9911, #5415, #29519, #49153, #25353, #44320, #54943, #10870, #5097, #25032, #30487, #34680, #284, #54299, #50109, #53665, #6064, #44642, #20212, #34043, #39814, #63328, #19245, #38861, #9598, #29206, #48831, #24398, #21489, #41403, #25989, #55904, #55591, #31126, #16655, #35965, #11510, #11815, #1252, #26299, #7015, #61055, #50749, #11190, #46565, #51709, #25678, #51076, #6694, #31434, #36586, #16975, #60734, #41715, #1563, #22123, #2204, #36280, #45923, #16018, #16343, #17287, #51395, #21165, #1886, #36911, #45286, #40772, #41087, #40457, #31762, #30812, #20855, #26623, #46243, #12142, #21808, #56542, #50444, #60097, #55271, #60418, #56222, #35645, #7337, #26948, #12461, #32072, #2505, #61366, #6384, #45608, #52021, #52957, #17915, #58096, #61681, #27253, #7965, #27879, #28510, #37536, #7650, #18552, #28192, #42040, #61995, #3764, #47500, #46880, #62309, #23388, #27563, #2824, #32713, #57176, #8895, #3451, #62630, #22443, #33341, #32395, #17613, #48128, #47196, #47807, #13094, #43299, #42670, #23702, #4079, #37229, #18233, #37858, #8275, #56855, #52341, #62935, #18849, #3140, #23065, #38470, #12773, #22759, #57491, #42356, #13717, #13410, #33031, #52647, #8581, #42988, #38174, #57796, #14026, #33655, #19161, #29124, #39411, #24001, #29434, #519, #44889, #59696, #44240, #49067, #20454, #204, #33967, #34924, #15627, #63565, #40052, #43603, #15302, #38779, #34272, #54217, #49394, #5014, #5656, #20129, #53587, #10468, #39729, #19802, #44561, #53273, #59368, #53898, #54545, #14653, #43918, #30080, #58418, #10155, #59049, #49711, #14977, #25269, #29760, #34585, #4382, #5338, #24633, #850, #9823, #9208, #28821, #9517, #24956, #48442, #63247, #48747, #14345, #4689, #24311, #19485, #39098, #58727, #5987, #16581, #55188, #60974, #55514, #6303, #21732, #31687, #35244, #31047, #50997, #35564, #1807, #1486, #50671, #26225, #45525, #21089, #21411, #10794, #35885, #36201, #6937, #60338, #20772, #56142, #61288, #54863, #60658, #16266, #41014, #46168, #26548, #11109, #16895, #30733, #11429, #46486, #30406, #50355, #6612, #50030, #41327, #40377, #25592, #45845, #45206, #2130, #55823, #31356, #36511, #22043, #12062, #51322, #11738, #1172, #7260, #26873, #2433, #41636, #60018, #15942, #25907, #40693, #61607, #62558, #44088, #27491, #4862, #7571, #36837, #17541, #37467, #38100, #13336, #57100, #33270, #47740, #37161, #57724, #3696, #8203, #8512, #24482, #23310, #17844, #42911, #42285, #7887, #18478, #13017, #28122, #32003, #13650, #47431, #52889, #57415, #42601, #51637, #23000, #52266, #8825, #61925, #28439, #48053, #56784, #3383, #17210, #32636, #12703, #32317, #32956, #52581, #56467, #3068, #47120, #27183, #62238, #51947, #12389, #27806, #22685, #46799, #2746, #22365, #18157, #41965, #37784, #39897, #34769, #54395, #54715, #19651, #367, #59543, #39263, #29934, #10635, #5818, #10322, #10000, #35408, #20939, #53, #30247, #5500, #49871, #59867, #1021, #15478, #25763, #50195, #5186, #35094, #25436, #25114, #29612, #49559, #49242, #20297, #15791, #1340, #58888, #45054, #20626, #14819, #40232, #39579, #6147, #34433, #44725, #54061, #59217, #44407, #55029, #24802, #10953, #19969, #15149, #687, #45375, #30572, #53639, #33706, #56672, #48496, #9572, #13770, #51832, #44294, #43971, #38833, #53007, #61810, #7774, #19538, #17736, #27377, #34326, #33392, #14395, #48181, #29488, #53951, #24060, #8946, #24369, #4433, #47010, #28560, #37354, #19854, #34017, #29179, #48805, #4744, #28874, #43657, #63298, #4133, #23755, #9882, #53326, #63617, #56984, #39152, #43350, #2959, #62996, #38520, #18906, #58777, #58148, #9259, #12590, #14077, #19216, #58470, #22576, #14707, #42173, #49124, #5066, #24686, #256, #32203, #30457, #6356, #50408, #25960, #5708, #60066, #60390, #25323, #5389, #10841, #50082, #45260, #11480, #50721, #15357, #30785, #45577, #34982, #6039, #20825, #54597, #20508, #59750, #15032, #25644, #1226, #39468, #40426, #11163, #35294, #35615, #1533, #26272, #16316, #21138, #574, #34648, #40107, #15990, #55241, #901, #25004, #35937, #1856, #59105, #40743, #15675, #55565, #44943, #31100, #6665, #54914, #10519, #45894, #54272, #10212, #29815, #49447, #30133, #44614, #20183, #49762, #39781, #59428, #49765, #6042, #45262, #577, #30136, #25008, #50086, #39785, #60394, #20828, #21141, #16319, #11792, #45898, #50724, #5711, #6668, #20186, #26275, #30788, #25326, #35940, #59433, #31410, #15994, #44947, #1859, #51048, #35297, #44617, #15360, #34985, #905, #1229, #21465, #54918, #54600, #55568, #45580, #10522, #15678, #40746, #40429, #20513, #40110, #11484, #25648, #31103, #60069, #10844, #41064, #35618, #60711, #59753, #16632, #30460, #55245, #36253, #11165, #1536, #50413, #55881, #6359, #25963, #47477, #27857, #7313, #56835, #8256, #46854, #26925, #46542, #22736, #42335, #17894, #42018, #37209, #12752, #22097, #61342, #23046, #2800, #61974, #12116, #3431, #6993, #22420, #37515, #2484, #32374, #36889, #12439, #51997, #26603, #41694, #17264, #32051, #42650, #7939, #56518, #57156, #61659, #41380, #51687, #17592, #7628, #27232, #13070, #32689, #52321, #27543, #47174, #3117, #62291, #18213, #37836, #57468, #13387, #31741, #33008, #46219, #2182, #51373, #21786, #61026, #16951, #36564, #56195, #8559, #48105, #62914, #58073, #62607, #48726, #47786, #4666, #182, #23366, #29410, #33317, #43582, #19462, #63541, #39077, #24290, #23978, #4989, #49043, #18530, #63224, #19139, #58394, #24611, #19782, #28488, #43892, #58705, #44217, #14632, #39390, #13696, #33632, #9187, #28171, #14322, #52626, #38756, #53564, #34246, #48415, #59021, #38150, #3744, #57775, #4058, #33943, #42964, #28800, #53875, #14952, #52936, #9489, #4359, #8873, #23676, #9802, #43274, #18827, #29100, #38446, #14005, #53251, #496, #15603, #35539, #30707, #10772, #50650, #1464, #34901, #55488, #21066, #25567, #25885, #50332, #54523, #29738, #21386, #40671, #15917, #30061, #39706, #55166, #45182, #45501, #1148, #60316, #11085, #59994, #49370, #40353, #10132, #6588, #6279, #60636, #44860, #40992, #24932, #54193, #10446, #54841, #11404, #823, #34563, #16243, #35863, #5315, #25245, #31023, #30382, #44540, #20748, #26203, #49688, #45822, #59672, #20429, #1786, #50005, #20100, #59346, #15278, #5634, #40029, #35221, #5956, #37138, #7237, #52239, #57076, #46776, #31665, #47097, #7548, #2722, #17821, #56445, #16871, #36489, #32295, #51922, #27468, #51615, #22344, #41942, #51302, #26851, #32612, #12366, #7862, #21710, #61902, #46464, #11718, #3045, #56116, #61584, #2407, #22021, #17519, #36180, #12040, #41614, #61265, #26526, #12681, #31335, #22663, #27783, #50972, #12990, #60952, #27160, #42261, #56759, #37445, #8180, #47408, #3358, #22975, #46145, #42576, #16556, #55801, #6914, #2109, #17188, #41302, #36814, #31981, #58321, #34175, #23285, #43198, #13312, #4594, #3672, #62215, #23601, #32934, #33870, #58006, #14247, #53488, #48966, #19388, #24217, #42887, #43824, #57390, #63469, #4289, #62532, #9417, #38380, #29336, #39006, #24537, #18132, #23907, #62840, #48343, #29027, #48652, #33557, #14556, #58637, #28098, #53179, #9112, #43508, #53798, #9732, #38074, #4918, #57702, #18452, #37758, #28720, #52557, #18755, #8490, #47716, #13628, #33246, #13932, #52866, #8799, #63154, #28412, #48031, #3982, #19064, #38682, #30306, #14873, #20353, #55086, #35787, #50576, #35152, #39951, #11326, #54767, #24860, #25815, #54449, #49926, #30630, #50252, #6200, #10054, #25167, #45109, #44140, #11008, #1074, #34482, #34826, #40286, #59599, #111, #10697, #59924, #421, #39315, #30950, #45428, #25487, #39631, #49298, #20680, #5880, #35466, #58943, #20993, #20025, #15847, #10377, #16160, #40598, #1393, #59270, #60242, #55409, #54116, #15201, #5238, #6519, #19706, #29667, #44462, #29986, #49618, #5555, #44781, #743, #15532, #42186, #21942, #61512, #31262, #7787, #36415, #21309, #50896, #7159, #31589, #22265, #41224, #41540, #17114, #56045, #11961, #1705, #26769, #7473, #41865, #51223, #11641, #36738, #17441, #56369, #51844, #2646, #51536, #40913, #31907, #61192, #32215, #46389, #2972, #47023, #26447, #21632, #6839, #52163, #37059, #56686, #61826, #36101, #32534, #2336, #16797, #60558, #27083, #46067, #27390, #12292, #60871, #12602, #22589, #26131, #46698, #17750, #37367, #56998, #12912, #45751, #16480, #55726, #2027, #57939, #47337, #8724, #53102, #23835, #33176, #57317, #28957, #34101, #8106, #33481, #52791, #18992, #37997, #28648, #48580, #57629, #47641, #4521, #48263, #62765, #28337, #62135, #62456, #63393, #33795, #3596, #13234, #24146, #43125, #63082, #47952, #3287, #38311, #13857, #27710, #18685, #9037, #58240, #3905, #19311, #32857, #22903, #37675, #23201, #4221, #42498, #23524, #38607, #38926, #14480, #43438, #58560, #18054, #13558, #14168, #53412, #18376, #9343, #43749, #52486, #8419, #28022, #42814, #54691, #50736, #29910, #7004, #21477, #54039, #11805, #41075, #53726, #44701, #6680, #9977, #48895, #41392, #60721, #35073, #49220, #58866, #10613, #39876, #24459, #49537, #1872, #46230, #61041, #666, #5478, #21797, #59198, #25093, #20275, #344, #59521, #16644, #36267, #55892, #19630, #34747, #31114, #26287, #15456, #26613, #31421, #29589, #51060, #2193, #45909, #16964, #9657, #5160, #4839, #29266, #44064, #30, #24780, #14798, #39240, #34410, #44384, #19944, #39556, #15126, #54374, #10301, #42346, #7952, #42661, #17603, #3441, #27553, #7326, #32062, #61353, #62618, #13081, #52331, #8570, #46553, #42976, #22432, #27243, #26936, #17903, #56530, #62300, #56845, #7639, #23056, #46868, #31751, #41705, #37219, #42029, #32702, #51698, #52010, #47185, #2811, #61670, #22748, #12129, #12762, #37525, #8266, #32385, #22112, #57481, #36575, #3127, #18222, #47488, #37848, #61984, #57166, #13397, #27868, #12451, #33020, #52636, #28181, #47797, #2496, #3754, #23376, #56205, #51384, #17276, #36900, #43287, #63235, #38766, #57786, #48734, #24299, #18542, #53575, #19471, #5001, #14333, #29748, #4068, #38161, #48116, #58084, #39398, #48428, #14015, #14964, #9502, #43903, #54203, #49379, #33642, #9811, #29421, #10141, #14641, #5324, #62923, #19149, #58405, #13706, #4677, #63551, #33328, #29111, #39085, #24620, #34258, #53886, #24943, #59033, #44226, #18838, #192, #52947, #19791, #58715, #38456, #49052, #8883, #44549, #28497, #23988, #33954, #34572, #28809, #23687 ),
 .UNSPECIFIED., .F., .F. ) 
 B_SPLINE_CURVE_WITH_KNOTS ( ( 3, 2, 2, 2, 2, 2, 2, 2, 2, 2, 2, 2, 2, 2, 2, 2, 2, 2, 2, 2, 2, 2, 2, 2, 2, 2, 2, 2, 2, 2, 2, 2, 2, 2, 2, 2, 2, 2, 2, 2, 2, 2, 2, 2, 2, 2, 2, 2, 2, 2, 2, 2, 2, 2, 2, 2, 2, 2, 2, 2, 2, 2, 2, 2, 2, 2, 2, 2, 2, 2, 2, 2, 2, 2, 2, 2, 2, 2, 2, 2, 2, 2, 2, 2, 2, 2, 2, 2, 2, 2, 2, 2, 2, 2, 2, 2, 2, 2, 2, 2, 2, 2, 2, 2, 2, 2, 2, 2, 2, 2, 2, 2, 2, 2, 2, 2, 2, 2, 2, 2, 2, 2, 2, 2, 2, 2, 2, 2, 2, 2, 2, 2, 2, 2, 2, 2, 2, 2, 2, 2, 2, 2, 2, 2, 2, 2, 2, 2, 2, 2, 2, 2, 2, 2, 2, 2, 2, 2, 2, 2, 2, 2, 2, 2, 2, 2, 2, 2, 2, 2, 2, 2, 2, 2, 2, 2, 2, 2, 2, 2, 2, 2, 2, 2, 2, 2, 2, 2, 2, 2, 2, 2, 2, 2, 2, 2, 2, 2, 2, 2, 2, 2, 2, 2, 2, 2, 2, 2, 2, 2, 2, 2, 2, 2, 2, 2, 2, 2, 2, 2, 2, 2, 2, 2, 2, 2, 2, 2, 2, 2, 2, 2, 2, 2, 2, 2, 2, 2, 2, 2, 2, 2, 2, 2, 2, 2, 2, 2, 2, 2, 2, 2, 2, 2, 2, 2, 2, 2, 2, 2, 2, 2, 2, 2, 2, 2, 2, 2, 2, 2, 2, 2, 2, 2, 2, 2, 2, 2, 2, 2, 2, 2, 2, 2, 2, 2, 2, 2, 2, 2, 2, 2, 2, 2, 2, 2, 2, 2, 2, 2, 2, 2, 2, 2, 2, 2, 2, 2, 2, 2, 2, 2, 2, 2, 2, 2, 2, 2, 2, 2, 2, 2, 2, 2, 2, 2, 2, 2, 2, 2, 2, 2, 2, 2, 2, 2, 2, 2, 2, 2, 2, 2, 2, 2, 2, 2, 2, 2, 2, 2, 2, 2, 2, 2, 2, 2, 2, 2, 2, 2, 2, 2, 2, 2, 2, 2, 2, 2, 2, 2, 2, 2, 2, 2, 2, 2, 2, 2, 2, 2, 2, 2, 2, 2, 2, 2, 2, 2, 2, 2, 2, 2, 2, 2, 2, 2, 2, 2, 2, 2, 2, 2, 2, 2, 2, 2, 2, 2, 2, 2, 2, 2, 2, 2, 2, 2, 2, 2, 2, 2, 2, 2, 2, 2, 2, 2, 2, 2, 2, 2, 2, 2, 2, 2, 2, 2, 2, 2, 2, 2, 2, 2, 2, 2, 2, 2, 2, 2, 2, 2, 2, 2, 2, 2, 2, 2, 2, 2, 2, 2, 2, 2, 2, 2, 2, 2, 2, 2, 2, 2, 2, 2, 2, 2, 2, 2, 2, 2, 2, 2, 2, 2, 2, 2, 2, 2, 2, 2, 2, 2, 2, 2, 2, 2, 2, 2, 2, 2, 2, 2, 2, 2, 2, 2, 2, 2, 2, 2, 2, 2, 2, 2, 2, 2, 2, 2, 2, 2, 2, 2, 2, 2, 2, 2, 2, 2, 2, 2, 2, 2, 2, 2, 2, 2, 2, 2, 2, 2, 2, 2, 2, 2, 2, 2, 2, 2, 2, 2, 2, 2, 2, 2, 2, 2, 2, 2, 2, 2, 2, 2, 2, 2, 2, 2, 2, 2, 2, 2, 2, 2, 2, 2, 2, 2, 2, 2, 2, 2, 2, 2, 2, 2, 2, 2, 2, 2, 2, 2, 2, 2, 2, 2, 2, 2, 2, 2, 2, 2, 2, 2, 2, 2, 2, 2, 2, 2, 2, 2, 2, 2, 2, 2, 2, 2, 2, 2, 2, 2, 2, 2, 2, 2, 2, 2, 2, 2, 2, 2, 2, 2, 2, 2, 2, 2, 2, 2, 2, 2, 2, 2, 2, 2, 2, 2, 2, 2, 2, 2, 2, 2, 2, 2, 2, 2, 2, 2, 2, 2, 2, 2, 2, 2, 2, 2, 2, 2, 2, 2, 2, 2, 2, 2, 2, 2, 2, 2, 2, 2, 2, 2, 2, 2, 2, 2, 2, 2, 2, 2, 2, 2, 2, 2, 2, 2, 2, 2, 2, 2, 2, 2, 2, 2, 2, 2, 2, 2, 2, 2, 2, 2, 2, 2, 2, 2, 2, 2, 2, 2, 2, 2, 2, 2, 2, 2, 2, 2, 2, 2, 2, 2, 2, 2, 2, 2, 2, 2, 2, 2, 2, 2, 2, 2, 2, 2, 2, 2, 2, 2, 2, 2, 2, 2, 2, 2, 2, 2, 2, 2, 2, 2, 2, 2, 2, 2, 2, 2, 2, 2, 2, 2, 2, 2, 2, 2, 2, 2, 2, 2, 2, 2, 2, 2, 2, 2, 2, 2, 2, 2, 2, 2, 2, 2, 2, 2, 2, 2, 2, 2, 2, 2, 2, 2, 2, 2, 2, 2, 2, 2, 2, 2, 2, 2, 2, 2, 2, 2, 2, 2, 2, 2, 2, 2, 2, 2, 2, 2, 2, 2, 2, 2, 2, 2, 2, 2, 2, 2, 2, 2, 2, 2, 3 ),
 ( 0.000000000000000000, 0.001190476190476190584, 0.002380952380952381167, 0.003571428571428571317, 0.004761904761904762334, 0.005952380952380952051, 0.007142857142857142634, 0.008333333333333333218, 0.009523809523809524669, 0.01071428571428571438, 0.01190476190476190410, 0.01309523809523809555, 0.01428571428571428527, 0.01547619047619047672, 0.01666666666666666644, 0.01785714285714285615, 0.01904761904761904934, 0.02023809523809523905, 0.02142857142857142877, 0.02261904761904761849, 0.02380952380952380820, 0.02500000000000000139, 0.02619047619047619110, 0.02738095238095238082, 0.02857142857142857054, 0.02976190476190476025, 0.03095238095238095344, 0.03214285714285713969, 0.03333333333333333287, 0.03452380952380952606, 0.03571428571428571230, 0.03690476190476190549, 0.03809523809523809867, 0.03928571428571428492, 0.04047619047619047811, 0.04166666666666666435, 0.04285714285714285754, 0.04404761904761905073, 0.04523809523809523697, 0.04642857142857143016, 0.04761904761904761640, 0.04880952380952380959, 0.05000000000000000278, 0.05119047619047618902, 0.05238095238095238221, 0.05357142857142856845, 0.05476190476190476164, 0.05595238095238095483, 0.05714285714285714107, 0.05833333333333333426, 0.05952380952380952051, 0.06071428571428571369, 0.06190476190476190688, 0.06309523809523809312, 0.06428571428571427937, 0.06547619047619047949, 0.06666666666666666574, 0.06785714285714285199, 0.06904761904761905211, 0.07023809523809523836, 0.07142857142857142461, 0.07261904761904762473, 0.07380952380952381098, 0.07499999999999999722, 0.07619047619047619735, 0.07738095238095238360, 0.07857142857142856984, 0.07976190476190475609, 0.08095238095238095621, 0.08214285714285714246, 0.08333333333333332871, 0.08452380952380952883, 0.08571428571428571508, 0.08690476190476190133, 0.08809523809523810145, 0.08928571428571428770, 0.09047619047619047394, 0.09166666666666666019, 0.09285714285714286031, 0.09404761904761904656, 0.09523809523809523281, 0.09642857142857143293, 0.09761904761904761918, 0.09880952380952380543, 0.1000000000000000056, 0.1011904761904761918, 0.1023809523809523780, 0.1035714285714285782, 0.1047619047619047644, 0.1059523809523809507, 0.1071428571428571369, 0.1083333333333333370, 0.1095238095238095233, 0.1107142857142857095, 0.1119047619047619097, 0.1130952380952380959, 0.1142857142857142821, 0.1154761904761904823, 0.1166666666666666685, 0.1178571428571428548, 0.1190476190476190410, 0.1202380952380952411, 0.1214285714285714274, 0.1226190476190476136, 0.1238095238095238138, 0.1250000000000000000, 0.1261904761904761862, 0.1273809523809523725, 0.1285714285714285587, 0.1297619047619047727, 0.1309523809523809590, 0.1321428571428571452, 0.1333333333333333315, 0.1345238095238095177, 0.1357142857142857040, 0.1369047619047619180, 0.1380952380952381042, 0.1392857142857142905, 0.1404761904761904767, 0.1416666666666666630, 0.1428571428571428492, 0.1440476190476190355, 0.1452380952380952495, 0.1464285714285714357, 0.1476190476190476220, 0.1488095238095238082, 0.1499999999999999944, 0.1511904761904761807, 0.1523809523809523947, 0.1535714285714285809, 0.1547619047619047672, 0.1559523809523809534, 0.1571428571428571397, 0.1583333333333333259, 0.1595238095238095122, 0.1607142857142857262, 0.1619047619047619124, 0.1630952380952380987, 0.1642857142857142849, 0.1654761904761904712, 0.1666666666666666574, 0.1678571428571428437, 0.1690476190476190577, 0.1702380952380952439, 0.1714285714285714302, 0.1726190476190476164, 0.1738095238095238027, 0.1749999999999999889, 0.1761904761904762029, 0.1773809523809523891, 0.1785714285714285754, 0.1797619047619047616, 0.1809523809523809479, 0.1821428571428571341, 0.1833333333333333204, 0.1845238095238095344, 0.1857142857142857206, 0.1869047619047619069, 0.1880952380952380931, 0.1892857142857142794, 0.1904761904761904656, 0.1916666666666666796, 0.1928571428571428659, 0.1940476190476190521, 0.1952380952380952384, 0.1964285714285714246, 0.1976190476190476109, 0.1988095238095237971, 0.2000000000000000111, 0.2011904761904761973, 0.2023809523809523836, 0.2035714285714285698, 0.2047619047619047561, 0.2059523809523809423, 0.2071428571428571563, 0.2083333333333333426, 0.2095238095238095288, 0.2107142857142857151, 0.2119047619047619013, 0.2130952380952380876, 0.2142857142857142738, 0.2154761904761904878, 0.2166666666666666741, 0.2178571428571428603, 0.2190476190476190466, 0.2202380952380952328, 0.2214285714285714191, 0.2226190476190476053, 0.2238095238095238193, 0.2250000000000000056, 0.2261904761904761918, 0.2273809523809523780, 0.2285714285714285643, 0.2297619047619047505, 0.2309523809523809645, 0.2321428571428571508, 0.2333333333333333370, 0.2345238095238095233, 0.2357142857142857095, 0.2369047619047618958, 0.2380952380952380820, 0.2392857142857142960, 0.2404761904761904823, 0.2416666666666666685, 0.2428571428571428548, 0.2440476190476190410, 0.2452380952380952273, 0.2464285714285714413, 0.2476190476190476275, 0.2488095238095238138, 0.2500000000000000000, 0.2511904761904761862, 0.2523809523809523725, 0.2535714285714285587, 0.2547619047619047450, 0.2559523809523809312, 0.2571428571428571175, 0.2583333333333333592, 0.2595238095238095455, 0.2607142857142857317, 0.2619047619047619180, 0.2630952380952381042, 0.2642857142857142905, 0.2654761904761904767, 0.2666666666666666630, 0.2678571428571428492, 0.2690476190476190355, 0.2702380952380952217, 0.2714285714285714080, 0.2726190476190475942, 0.2738095238095238360, 0.2750000000000000222, 0.2761904761904762085, 0.2773809523809523947, 0.2785714285714285809, 0.2797619047619047672, 0.2809523809523809534, 0.2821428571428571397, 0.2833333333333333259, 0.2845238095238095122, 0.2857142857142856984, 0.2869047619047618847, 0.2880952380952380709, 0.2892857142857143127, 0.2904761904761904989, 0.2916666666666666852, 0.2928571428571428714, 0.2940476190476190577, 0.2952380952380952439, 0.2964285714285714302, 0.2976190476190476164, 0.2988095238095238027, 0.2999999999999999889, 0.3011904761904761751, 0.3023809523809523614, 0.3035714285714285476, 0.3047619047619047894, 0.3059523809523809756, 0.3071428571428571619, 0.3083333333333333481, 0.3095238095238095344, 0.3107142857142857206, 0.3119047619047619069, 0.3130952380952380931, 0.3142857142857142794, 0.3154761904761904656, 0.3166666666666666519, 0.3178571428571428381, 0.3190476190476190244, 0.3202380952380952106, 0.3214285714285714524, 0.3226190476190476386, 0.3238095238095238249, 0.3250000000000000111, 0.3261904761904761973, 0.3273809523809523836, 0.3285714285714285698, 0.3297619047619047561, 0.3309523809523809423, 0.3321428571428571286, 0.3333333333333333148, 0.3345238095238095011, 0.3357142857142856873, 0.3369047619047619291, 0.3380952380952381153, 0.3392857142857143016, 0.3404761904761904878, 0.3416666666666666741, 0.3428571428571428603, 0.3440476190476190466, 0.3452380952380952328, 0.3464285714285714191, 0.3476190476190476053, 0.3488095238095237915, 0.3499999999999999778, 0.3511904761904761640, 0.3523809523809524058, 0.3535714285714285920, 0.3547619047619047783, 0.3559523809523809645, 0.3571428571428571508, 0.3583333333333333370, 0.3595238095238095233, 0.3607142857142857095, 0.3619047619047618958, 0.3630952380952380820, 0.3642857142857142683, 0.3654761904761904545, 0.3666666666666666408, 0.3678571428571428825, 0.3690476190476190688, 0.3702380952380952550, 0.3714285714285714413, 0.3726190476190476275, 0.3738095238095238138, 0.3750000000000000000, 0.3761904761904761862, 0.3773809523809523725, 0.3785714285714285587, 0.3797619047619047450, 0.3809523809523809312, 0.3821428571428571175, 0.3833333333333333592, 0.3845238095238095455, 0.3857142857142857317, 0.3869047619047619180, 0.3880952380952381042, 0.3892857142857142905, 0.3904761904761904767, 0.3916666666666666630, 0.3928571428571428492, 0.3940476190476190355, 0.3952380952380952217, 0.3964285714285714080, 0.3976190476190475942, 0.3988095238095238360, 0.4000000000000000222, 0.4011904761904762085, 0.4023809523809523947, 0.4035714285714285809, 0.4047619047619047672, 0.4059523809523809534, 0.4071428571428571397, 0.4083333333333333259, 0.4095238095238095122, 0.4107142857142856984, 0.4119047619047618847, 0.4130952380952380709, 0.4142857142857143127, 0.4154761904761904989, 0.4166666666666666852, 0.4178571428571428714, 0.4190476190476190577, 0.4202380952380952439, 0.4214285714285714302, 0.4226190476190476164, 0.4238095238095238027, 0.4249999999999999889, 0.4261904761904761751, 0.4273809523809523614, 0.4285714285714285476, 0.4297619047619047894, 0.4309523809523809756, 0.4321428571428571619, 0.4333333333333333481, 0.4345238095238095344, 0.4357142857142857206, 0.4369047619047619069, 0.4380952380952380931, 0.4392857142857142794, 0.4404761904761904656, 0.4416666666666666519, 0.4428571428571428381, 0.4440476190476190244, 0.4452380952380952106, 0.4464285714285714524, 0.4476190476190476386, 0.4488095238095238249, 0.4500000000000000111, 0.4511904761904761973, 0.4523809523809523836, 0.4535714285714285698, 0.4547619047619047561, 0.4559523809523809423, 0.4571428571428571286, 0.4583333333333333148, 0.4595238095238095011, 0.4607142857142856873, 0.4619047619047619291, 0.4630952380952381153, 0.4642857142857143016, 0.4654761904761904878, 0.4666666666666666741, 0.4678571428571428603, 0.4690476190476190466, 0.4702380952380952328, 0.4714285714285714191, 0.4726190476190476053, 0.4738095238095237915, 0.4749999999999999778, 0.4761904761904761640, 0.4773809523809524058, 0.4785714285714285920, 0.4797619047619047783, 0.4809523809523809645, 0.4821428571428571508, 0.4833333333333333370, 0.4845238095238095233, 0.4857142857142857095, 0.4869047619047618958, 0.4880952380952380820, 0.4892857142857142683, 0.4904761904761904545, 0.4916666666666666408, 0.4928571428571428825, 0.4940476190476190688, 0.4952380952380952550, 0.4964285714285714413, 0.4976190476190476275, 0.4988095238095238138, 0.5000000000000000000, 0.5011904761904761862, 0.5023809523809523725, 0.5035714285714285587, 0.5047619047619047450, 0.5059523809523809312, 0.5071428571428571175, 0.5083333333333333037, 0.5095238095238094900, 0.5107142857142856762, 0.5119047619047618625, 0.5130952380952380487, 0.5142857142857142350, 0.5154761904761904212, 0.5166666666666667185, 0.5178571428571429047, 0.5190476190476190910, 0.5202380952380952772, 0.5214285714285714635, 0.5226190476190476497, 0.5238095238095238360, 0.5250000000000000222, 0.5261904761904762085, 0.5273809523809523947, 0.5285714285714285809, 0.5297619047619047672, 0.5309523809523809534, 0.5321428571428571397, 0.5333333333333333259, 0.5345238095238095122, 0.5357142857142856984, 0.5369047619047618847, 0.5380952380952380709, 0.5392857142857142572, 0.5404761904761904434, 0.5416666666666666297, 0.5428571428571428159, 0.5440476190476190022, 0.5452380952380951884, 0.5464285714285713746, 0.5476190476190476719, 0.5488095238095238582, 0.5500000000000000444, 0.5511904761904762307, 0.5523809523809524169, 0.5535714285714286031, 0.5547619047619047894, 0.5559523809523809756, 0.5571428571428571619, 0.5583333333333333481, 0.5595238095238095344, 0.5607142857142857206, 0.5619047619047619069, 0.5630952380952380931, 0.5642857142857142794, 0.5654761904761904656, 0.5666666666666666519, 0.5678571428571428381, 0.5690476190476190244, 0.5702380952380952106, 0.5714285714285713969, 0.5726190476190475831, 0.5738095238095237693, 0.5749999999999999556, 0.5761904761904761418, 0.5773809523809523281, 0.5785714285714286254, 0.5797619047619048116, 0.5809523809523809978, 0.5821428571428571841, 0.5833333333333333703, 0.5845238095238095566, 0.5857142857142857428, 0.5869047619047619291, 0.5880952380952381153, 0.5892857142857143016, 0.5904761904761904878, 0.5916666666666666741, 0.5928571428571428603, 0.5940476190476190466, 0.5952380952380952328, 0.5964285714285714191, 0.5976190476190476053, 0.5988095238095237915, 0.5999999999999999778, 0.6011904761904761640, 0.6023809523809523503, 0.6035714285714285365, 0.6047619047619047228, 0.6059523809523809090, 0.6071428571428570953, 0.6083333333333332815, 0.6095238095238095788, 0.6107142857142857650, 0.6119047619047619513, 0.6130952380952381375, 0.6142857142857143238, 0.6154761904761905100, 0.6166666666666666963, 0.6178571428571428825, 0.6190476190476190688, 0.6202380952380952550, 0.6214285714285714413, 0.6226190476190476275, 0.6238095238095238138, 0.6250000000000000000, 0.6261904761904761862, 0.6273809523809523725, 0.6285714285714285587, 0.6297619047619047450, 0.6309523809523809312, 0.6321428571428571175, 0.6333333333333333037, 0.6345238095238094900, 0.6357142857142856762, 0.6369047619047618625, 0.6380952380952380487, 0.6392857142857142350, 0.6404761904761904212, 0.6416666666666667185, 0.6428571428571429047, 0.6440476190476190910, 0.6452380952380952772, 0.6464285714285714635, 0.6476190476190476497, 0.6488095238095238360, 0.6500000000000000222, 0.6511904761904762085, 0.6523809523809523947, 0.6535714285714285809, 0.6547619047619047672, 0.6559523809523809534, 0.6571428571428571397, 0.6583333333333333259, 0.6595238095238095122, 0.6607142857142856984, 0.6619047619047618847, 0.6630952380952380709, 0.6642857142857142572, 0.6654761904761904434, 0.6666666666666666297, 0.6678571428571428159, 0.6690476190476190022, 0.6702380952380951884, 0.6714285714285713746, 0.6726190476190476719, 0.6738095238095238582, 0.6750000000000000444, 0.6761904761904762307, 0.6773809523809524169, 0.6785714285714286031, 0.6797619047619047894, 0.6809523809523809756, 0.6821428571428571619, 0.6833333333333333481, 0.6845238095238095344, 0.6857142857142857206, 0.6869047619047619069, 0.6880952380952380931, 0.6892857142857142794, 0.6904761904761904656, 0.6916666666666666519, 0.6928571428571428381, 0.6940476190476190244, 0.6952380952380952106, 0.6964285714285713969, 0.6976190476190475831, 0.6988095238095237693, 0.6999999999999999556, 0.7011904761904761418, 0.7023809523809523281, 0.7035714285714286254, 0.7047619047619048116, 0.7059523809523809978, 0.7071428571428571841, 0.7083333333333333703, 0.7095238095238095566, 0.7107142857142857428, 0.7119047619047619291, 0.7130952380952381153, 0.7142857142857143016, 0.7154761904761904878, 0.7166666666666666741, 0.7178571428571428603, 0.7190476190476190466, 0.7202380952380952328, 0.7214285714285714191, 0.7226190476190476053, 0.7238095238095237915, 0.7249999999999999778, 0.7261904761904761640, 0.7273809523809523503, 0.7285714285714285365, 0.7297619047619047228, 0.7309523809523809090, 0.7321428571428570953, 0.7333333333333332815, 0.7345238095238095788, 0.7357142857142857650, 0.7369047619047619513, 0.7380952380952381375, 0.7392857142857143238, 0.7404761904761905100, 0.7416666666666666963, 0.7428571428571428825, 0.7440476190476190688, 0.7452380952380952550, 0.7464285714285714413, 0.7476190476190476275, 0.7488095238095238138, 0.7500000000000000000, 0.7511904761904761862, 0.7523809523809523725, 0.7535714285714285587, 0.7547619047619047450, 0.7559523809523809312, 0.7571428571428571175, 0.7583333333333333037, 0.7595238095238094900, 0.7607142857142856762, 0.7619047619047618625, 0.7630952380952380487, 0.7642857142857142350, 0.7654761904761904212, 0.7666666666666667185, 0.7678571428571429047, 0.7690476190476190910, 0.7702380952380952772, 0.7714285714285714635, 0.7726190476190476497, 0.7738095238095238360, 0.7750000000000000222, 0.7761904761904762085, 0.7773809523809523947, 0.7785714285714285809, 0.7797619047619047672, 0.7809523809523809534, 0.7821428571428571397, 0.7833333333333333259, 0.7845238095238095122, 0.7857142857142856984, 0.7869047619047618847, 0.7880952380952380709, 0.7892857142857142572, 0.7904761904761904434, 0.7916666666666666297, 0.7928571428571428159, 0.7940476190476190022, 0.7952380952380951884, 0.7964285714285713746, 0.7976190476190476719, 0.7988095238095238582, 0.8000000000000000444, 0.8011904761904762307, 0.8023809523809524169, 0.8035714285714286031, 0.8047619047619047894, 0.8059523809523809756, 0.8071428571428571619, 0.8083333333333333481, 0.8095238095238095344, 0.8107142857142857206, 0.8119047619047619069, 0.8130952380952380931, 0.8142857142857142794, 0.8154761904761904656, 0.8166666666666666519, 0.8178571428571428381, 0.8190476190476190244, 0.8202380952380952106, 0.8214285714285713969, 0.8226190476190475831, 0.8238095238095237693, 0.8249999999999999556, 0.8261904761904761418, 0.8273809523809523281, 0.8285714285714286254, 0.8297619047619048116, 0.8309523809523809978, 0.8321428571428571841, 0.8333333333333333703, 0.8345238095238095566, 0.8357142857142857428, 0.8369047619047619291, 0.8380952380952381153, 0.8392857142857143016, 0.8404761904761904878, 0.8416666666666666741, 0.8428571428571428603, 0.8440476190476190466, 0.8452380952380952328, 0.8464285714285714191, 0.8476190476190476053, 0.8488095238095237915, 0.8499999999999999778, 0.8511904761904761640, 0.8523809523809523503, 0.8535714285714285365, 0.8547619047619047228, 0.8559523809523809090, 0.8571428571428570953, 0.8583333333333332815, 0.8595238095238095788, 0.8607142857142857650, 0.8619047619047619513, 0.8630952380952381375, 0.8642857142857143238, 0.8654761904761905100, 0.8666666666666666963, 0.8678571428571428825, 0.8690476190476190688, 0.8702380952380952550, 0.8714285714285714413, 0.8726190476190476275, 0.8738095238095238138, 0.8750000000000000000, 0.8761904761904761862, 0.8773809523809523725, 0.8785714285714285587, 0.8797619047619047450, 0.8809523809523809312, 0.8821428571428571175, 0.8833333333333333037, 0.8845238095238094900, 0.8857142857142856762, 0.8869047619047618625, 0.8880952380952380487, 0.8892857142857142350, 0.8904761904761904212, 0.8916666666666667185, 0.8928571428571429047, 0.8940476190476190910, 0.8952380952380952772, 0.8964285714285714635, 0.8976190476190476497, 0.8988095238095238360, 0.9000000000000000222, 0.9011904761904762085, 0.9023809523809523947, 0.9035714285714285809, 0.9047619047619047672, 0.9059523809523809534, 0.9071428571428571397, 0.9083333333333333259, 0.9095238095238095122, 0.9107142857142856984, 0.9119047619047618847, 0.9130952380952380709, 0.9142857142857142572, 0.9154761904761904434, 0.9166666666666666297, 0.9178571428571428159, 0.9190476190476190022, 0.9202380952380951884, 0.9214285714285713746, 0.9226190476190476719, 0.9238095238095238582, 0.9250000000000000444, 0.9261904761904762307, 0.9273809523809524169, 0.9285714285714286031, 0.9297619047619047894, 0.9309523809523809756, 0.9321428571428571619, 0.9333333333333333481, 0.9345238095238095344, 0.9357142857142857206, 0.9369047619047619069, 0.9380952380952380931, 0.9392857142857142794, 0.9404761904761904656, 0.9416666666666666519, 0.9428571428571428381, 0.9440476190476190244, 0.9452380952380952106, 0.9464285714285713969, 0.9476190476190475831, 0.9488095238095237693, 0.9499999999999999556, 0.9511904761904761418, 0.9523809523809523281, 0.9535714285714286254, 0.9547619047619048116, 0.9559523809523809978, 0.9571428571428571841, 0.9583333333333333703, 0.9595238095238095566, 0.9607142857142857428, 0.9619047619047619291, 0.9630952380952381153, 0.9642857142857143016, 0.9654761904761904878, 0.9666666666666666741, 0.9678571428571428603, 0.9690476190476190466, 0.9702380952380952328, 0.9714285714285714191, 0.9726190476190476053, 0.9738095238095237915, 0.9749999999999999778, 0.9761904761904761640, 0.9773809523809523503, 0.9785714285714285365, 0.9797619047619047228, 0.9809523809523809090, 0.9821428571428570953, 0.9833333333333332815, 0.9845238095238095788, 0.9857142857142857650, 0.9869047619047619513, 0.9880952380952381375, 0.9892857142857143238, 0.9904761904761905100, 0.9916666666666666963, 0.9928571428571428825, 0.9940476190476190688, 0.9952380952380952550, 0.9964285714285714413, 0.9976190476190476275, 0.9988095238095238138, 1.000000000000000000 ),
 .UNSPECIFIED. ) 
 CURVE ( )  GEOMETRIC_REPRESENTATION_ITEM ( )  RATIONAL_B_SPLINE_CURVE ( ( 1.000000000000000000, 0.8660254037844387076, 1.000000000000000000, 0.8660254037844387076, 1.000000000000000000, 0.8660254037844387076, 1.000000000000000000, 0.8660254037844387076, 1.000000000000000000, 0.8660254037844387076, 1.000000000000000000, 0.8660254037844387076, 1.000000000000000000, 0.8660254037844387076, 1.000000000000000000, 0.8660254037844387076, 1.000000000000000000, 0.8660254037844387076, 1.000000000000000000, 0.8660254037844387076, 1.000000000000000000, 0.8660254037844387076, 1.000000000000000000, 0.8660254037844387076, 1.000000000000000000, 0.8660254037844387076, 1.000000000000000000, 0.8660254037844387076, 1.000000000000000000, 0.8660254037844387076, 1.000000000000000000, 0.8660254037844387076, 1.000000000000000000, 0.8660254037844387076, 1.000000000000000000, 0.8660254037844387076, 1.000000000000000000, 0.8660254037844387076, 1.000000000000000000, 0.8660254037844387076, 1.000000000000000000, 0.8660254037844387076, 1.000000000000000000, 0.8660254037844387076, 1.000000000000000000, 0.8660254037844387076, 1.000000000000000000, 0.8660254037844387076, 1.000000000000000000, 0.8660254037844387076, 1.000000000000000000, 0.8660254037844387076, 1.000000000000000000, 0.8660254037844387076, 1.000000000000000000, 0.8660254037844387076, 1.000000000000000000, 0.8660254037844387076, 1.000000000000000000, 0.8660254037844387076, 1.000000000000000000, 0.8660254037844387076, 1.000000000000000000, 0.8660254037844387076, 1.000000000000000000, 0.8660254037844387076, 1.000000000000000000, 0.8660254037844387076, 1.000000000000000000, 0.8660254037844387076, 1.000000000000000000, 0.8660254037844387076, 1.000000000000000000, 0.8660254037844387076, 1.000000000000000000, 0.8660254037844387076, 1.000000000000000000, 0.8660254037844387076, 1.000000000000000000, 0.8660254037844387076, 1.000000000000000000, 0.8660254037844387076, 1.000000000000000000, 0.8660254037844387076, 1.000000000000000000, 0.8660254037844387076, 1.000000000000000000, 0.8660254037844387076, 1.000000000000000000, 0.8660254037844387076, 1.000000000000000000, 0.8660254037844387076, 1.000000000000000000, 0.8660254037844387076, 1.000000000000000000, 0.8660254037844387076, 1.000000000000000000, 0.8660254037844387076, 1.000000000000000000, 0.8660254037844387076, 1.000000000000000000, 0.8660254037844387076, 1.000000000000000000, 0.8660254037844387076, 1.000000000000000000, 0.8660254037844387076, 1.000000000000000000, 0.8660254037844387076, 1.000000000000000000, 0.8660254037844387076, 1.000000000000000000, 0.8660254037844387076, 1.000000000000000000, 0.8660254037844387076, 1.000000000000000000, 0.8660254037844387076, 1.000000000000000000, 0.8660254037844387076, 1.000000000000000000, 0.8660254037844387076, 1.000000000000000000, 0.8660254037844387076, 1.000000000000000000, 0.8660254037844387076, 1.000000000000000000, 0.8660254037844387076, 1.000000000000000000, 0.8660254037844387076, 1.000000000000000000, 0.8660254037844387076, 1.000000000000000000, 0.8660254037844387076, 1.000000000000000000, 0.8660254037844387076, 1.000000000000000000, 0.8660254037844387076, 1.000000000000000000, 0.8660254037844387076, 1.000000000000000000, 0.8660254037844387076, 1.000000000000000000, 0.8660254037844387076, 1.000000000000000000, 0.8660254037844387076, 1.000000000000000000, 0.8660254037844387076, 1.000000000000000000, 0.8660254037844387076, 1.000000000000000000, 0.8660254037844387076, 1.000000000000000000, 0.8660254037844387076, 1.000000000000000000, 0.8660254037844387076, 1.000000000000000000, 0.8660254037844387076, 1.000000000000000000, 0.8660254037844387076, 1.000000000000000000, 0.8660254037844387076, 1.000000000000000000, 0.8660254037844387076, 1.000000000000000000, 0.8660254037844387076, 1.000000000000000000, 0.8660254037844387076, 1.000000000000000000, 0.8660254037844387076, 1.000000000000000000, 0.8660254037844387076, 1.000000000000000000, 0.8660254037844387076, 1.000000000000000000, 0.8660254037844387076, 1.000000000000000000, 0.8660254037844387076, 1.000000000000000000, 0.8660254037844387076, 1.000000000000000000, 0.8660254037844387076, 1.000000000000000000, 0.8660254037844387076, 1.000000000000000000, 0.8660254037844387076, 1.000000000000000000, 0.8660254037844387076, 1.000000000000000000, 0.8660254037844387076, 1.000000000000000000, 0.8660254037844387076, 1.000000000000000000, 0.8660254037844387076, 1.000000000000000000, 0.8660254037844387076, 1.000000000000000000, 0.8660254037844387076, 1.000000000000000000, 0.8660254037844387076, 1.000000000000000000, 0.8660254037844387076, 1.000000000000000000, 0.8660254037844387076, 1.000000000000000000, 0.8660254037844387076, 1.000000000000000000, 0.8660254037844387076, 1.000000000000000000, 0.8660254037844387076, 1.000000000000000000, 0.8660254037844387076, 1.000000000000000000, 0.8660254037844387076, 1.000000000000000000, 0.8660254037844387076, 1.000000000000000000, 0.8660254037844387076, 1.000000000000000000, 0.8660254037844387076, 1.000000000000000000, 0.8660254037844387076, 1.000000000000000000, 0.8660254037844387076, 1.000000000000000000, 0.8660254037844387076, 1.000000000000000000, 0.8660254037844387076, 1.000000000000000000, 0.8660254037844387076, 1.000000000000000000, 0.8660254037844387076, 1.000000000000000000, 0.8660254037844387076, 1.000000000000000000, 0.8660254037844387076, 1.000000000000000000, 0.8660254037844387076, 1.000000000000000000, 0.8660254037844387076, 1.000000000000000000, 0.8660254037844387076, 1.000000000000000000, 0.8660254037844387076, 1.000000000000000000, 0.8660254037844387076, 1.000000000000000000, 0.8660254037844387076, 1.000000000000000000, 0.8660254037844387076, 1.000000000000000000, 0.8660254037844387076, 1.000000000000000000, 0.8660254037844387076, 1.000000000000000000, 0.8660254037844387076, 1.000000000000000000, 0.8660254037844387076, 1.000000000000000000, 0.8660254037844387076, 1.000000000000000000, 0.8660254037844387076, 1.000000000000000000, 0.8660254037844387076, 1.000000000000000000, 0.8660254037844387076, 1.000000000000000000, 0.8660254037844387076, 1.000000000000000000, 0.8660254037844387076, 1.000000000000000000, 0.8660254037844387076, 1.000000000000000000, 0.8660254037844387076, 1.000000000000000000, 0.8660254037844387076, 1.000000000000000000, 0.8660254037844387076, 1.000000000000000000, 0.8660254037844387076, 1.000000000000000000, 0.8660254037844387076, 1.000000000000000000, 0.8660254037844387076, 1.000000000000000000, 0.8660254037844387076, 1.000000000000000000, 0.8660254037844387076, 1.000000000000000000, 0.8660254037844387076, 1.000000000000000000, 0.8660254037844387076, 1.000000000000000000, 0.8660254037844387076, 1.000000000000000000, 0.8660254037844387076, 1.000000000000000000, 0.8660254037844387076, 1.000000000000000000, 0.8660254037844387076, 1.000000000000000000, 0.8660254037844387076, 1.000000000000000000, 0.8660254037844387076, 1.000000000000000000, 0.8660254037844387076, 1.000000000000000000, 0.8660254037844387076, 1.000000000000000000, 0.8660254037844387076, 1.000000000000000000, 0.8660254037844387076, 1.000000000000000000, 0.8660254037844387076, 1.000000000000000000, 0.8660254037844387076, 1.000000000000000000, 0.8660254037844387076, 1.000000000000000000, 0.8660254037844387076, 1.000000000000000000, 0.8660254037844387076, 1.000000000000000000, 0.8660254037844387076, 1.000000000000000000, 0.8660254037844387076, 1.000000000000000000, 0.8660254037844387076, 1.000000000000000000, 0.8660254037844387076, 1.000000000000000000, 0.8660254037844387076, 1.000000000000000000, 0.8660254037844387076, 1.000000000000000000, 0.8660254037844387076, 1.000000000000000000, 0.8660254037844387076, 1.000000000000000000, 0.8660254037844387076, 1.000000000000000000, 0.8660254037844387076, 1.000000000000000000, 0.8660254037844387076, 1.000000000000000000, 0.8660254037844387076, 1.000000000000000000, 0.8660254037844387076, 1.000000000000000000, 0.8660254037844387076, 1.000000000000000000, 0.8660254037844387076, 1.000000000000000000, 0.8660254037844387076, 1.000000000000000000, 0.8660254037844387076, 1.000000000000000000, 0.8660254037844387076, 1.000000000000000000, 0.8660254037844387076, 1.000000000000000000, 0.8660254037844387076, 1.000000000000000000, 0.8660254037844387076, 1.000000000000000000, 0.8660254037844387076, 1.000000000000000000, 0.8660254037844387076, 1.000000000000000000, 0.8660254037844387076, 1.000000000000000000, 0.8660254037844387076, 1.000000000000000000, 0.8660254037844387076, 1.000000000000000000, 0.8660254037844387076, 1.000000000000000000, 0.8660254037844387076, 1.000000000000000000, 0.8660254037844387076, 1.000000000000000000, 0.8660254037844387076, 1.000000000000000000, 0.8660254037844387076, 1.000000000000000000, 0.8660254037844387076, 1.000000000000000000, 0.8660254037844387076, 1.000000000000000000, 0.8660254037844387076, 1.000000000000000000, 0.8660254037844387076, 1.000000000000000000, 0.8660254037844387076, 1.000000000000000000, 0.8660254037844387076, 1.000000000000000000, 0.8660254037844387076, 1.000000000000000000, 0.8660254037844387076, 1.000000000000000000, 0.8660254037844387076, 1.000000000000000000, 0.8660254037844387076, 1.000000000000000000, 0.8660254037844387076, 1.000000000000000000, 0.8660254037844387076, 1.000000000000000000, 0.8660254037844387076, 1.000000000000000000, 0.8660254037844387076, 1.000000000000000000, 0.8660254037844387076, 1.000000000000000000, 0.8660254037844387076, 1.000000000000000000, 0.8660254037844387076, 1.000000000000000000, 0.8660254037844387076, 1.000000000000000000, 0.8660254037844387076, 1.000000000000000000, 0.8660254037844387076, 1.000000000000000000, 0.8660254037844387076, 1.000000000000000000, 0.8660254037844387076, 1.000000000000000000, 0.8660254037844387076, 1.000000000000000000, 0.8660254037844387076, 1.000000000000000000, 0.8660254037844387076, 1.000000000000000000, 0.8660254037844387076, 1.000000000000000000, 0.8660254037844387076, 1.000000000000000000, 0.8660254037844387076, 1.000000000000000000, 0.8660254037844387076, 1.000000000000000000, 0.8660254037844387076, 1.000000000000000000, 0.8660254037844387076, 1.000000000000000000, 0.8660254037844387076, 1.000000000000000000, 0.8660254037844387076, 1.000000000000000000, 0.8660254037844387076, 1.000000000000000000, 0.8660254037844387076, 1.000000000000000000, 0.8660254037844387076, 1.000000000000000000, 0.8660254037844387076, 1.000000000000000000, 0.8660254037844387076, 1.000000000000000000, 0.8660254037844387076, 1.000000000000000000, 0.8660254037844387076, 1.000000000000000000, 0.8660254037844387076, 1.000000000000000000, 0.8660254037844387076, 1.000000000000000000, 0.8660254037844387076, 1.000000000000000000, 0.8660254037844387076, 1.000000000000000000, 0.8660254037844387076, 1.000000000000000000, 0.8660254037844387076, 1.000000000000000000, 0.8660254037844387076, 1.000000000000000000, 0.8660254037844387076, 1.000000000000000000, 0.8660254037844387076, 1.000000000000000000, 0.8660254037844387076, 1.000000000000000000, 0.8660254037844387076, 1.000000000000000000, 0.8660254037844387076, 1.000000000000000000, 0.8660254037844387076, 1.000000000000000000, 0.8660254037844387076, 1.000000000000000000, 0.8660254037844387076, 1.000000000000000000, 0.8660254037844387076, 1.000000000000000000, 0.8660254037844387076, 1.000000000000000000, 0.8660254037844387076, 1.000000000000000000, 0.8660254037844387076, 1.000000000000000000, 0.8660254037844387076, 1.000000000000000000, 0.8660254037844387076, 1.000000000000000000, 0.8660254037844387076, 1.000000000000000000, 0.8660254037844387076, 1.000000000000000000, 0.8660254037844387076, 1.000000000000000000, 0.8660254037844387076, 1.000000000000000000, 0.8660254037844387076, 1.000000000000000000, 0.8660254037844387076, 1.000000000000000000, 0.8660254037844387076, 1.000000000000000000, 0.8660254037844387076, 1.000000000000000000, 0.8660254037844387076, 1.000000000000000000, 0.8660254037844387076, 1.000000000000000000, 0.8660254037844387076, 1.000000000000000000, 0.8660254037844387076, 1.000000000000000000, 0.8660254037844387076, 1.000000000000000000, 0.8660254037844387076, 1.000000000000000000, 0.8660254037844387076, 1.000000000000000000, 0.8660254037844387076, 1.000000000000000000, 0.8660254037844387076, 1.000000000000000000, 0.8660254037844387076, 1.000000000000000000, 0.8660254037844387076, 1.000000000000000000, 0.8660254037844387076, 1.000000000000000000, 0.8660254037844387076, 1.000000000000000000, 0.8660254037844387076, 1.000000000000000000, 0.8660254037844387076, 1.000000000000000000, 0.8660254037844387076, 1.000000000000000000, 0.8660254037844387076, 1.000000000000000000, 0.8660254037844387076, 1.000000000000000000, 0.8660254037844387076, 1.000000000000000000, 0.8660254037844387076, 1.000000000000000000, 0.8660254037844387076, 1.000000000000000000, 0.8660254037844387076, 1.000000000000000000, 0.8660254037844387076, 1.000000000000000000, 0.8660254037844387076, 1.000000000000000000, 0.8660254037844387076, 1.000000000000000000, 0.8660254037844387076, 1.000000000000000000, 0.8660254037844387076, 1.000000000000000000, 0.8660254037844387076, 1.000000000000000000, 0.8660254037844387076, 1.000000000000000000, 0.8660254037844387076, 1.000000000000000000, 0.8660254037844387076, 1.000000000000000000, 0.8660254037844387076, 1.000000000000000000, 0.8660254037844387076, 1.000000000000000000, 0.8660254037844387076, 1.000000000000000000, 0.8660254037844387076, 1.000000000000000000, 0.8660254037844387076, 1.000000000000000000, 0.8660254037844387076, 1.000000000000000000, 0.8660254037844387076, 1.000000000000000000, 0.8660254037844387076, 1.000000000000000000, 0.8660254037844387076, 1.000000000000000000, 0.8660254037844387076, 1.000000000000000000, 0.8660254037844387076, 1.000000000000000000, 0.8660254037844387076, 1.000000000000000000, 0.8660254037844387076, 1.000000000000000000, 0.8660254037844387076, 1.000000000000000000, 0.8660254037844387076, 1.000000000000000000, 0.8660254037844387076, 1.000000000000000000, 0.8660254037844387076, 1.000000000000000000, 0.8660254037844387076, 1.000000000000000000, 0.8660254037844387076, 1.000000000000000000, 0.8660254037844387076, 1.000000000000000000, 0.8660254037844387076, 1.000000000000000000, 0.8660254037844387076, 1.000000000000000000, 0.8660254037844387076, 1.000000000000000000, 0.8660254037844387076, 1.000000000000000000, 0.8660254037844387076, 1.000000000000000000, 0.8660254037844387076, 1.000000000000000000, 0.8660254037844387076, 1.000000000000000000, 0.8660254037844387076, 1.000000000000000000, 0.8660254037844387076, 1.000000000000000000, 0.8660254037844387076, 1.000000000000000000, 0.8660254037844387076, 1.000000000000000000, 0.8660254037844387076, 1.000000000000000000, 0.8660254037844387076, 1.000000000000000000, 0.8660254037844387076, 1.000000000000000000, 0.8660254037844387076, 1.000000000000000000, 0.8660254037844387076, 1.000000000000000000, 0.8660254037844387076, 1.000000000000000000, 0.8660254037844387076, 1.000000000000000000, 0.8660254037844387076, 1.000000000000000000, 0.8660254037844387076, 1.000000000000000000, 0.8660254037844387076, 1.000000000000000000, 0.8660254037844387076, 1.000000000000000000, 0.8660254037844387076, 1.000000000000000000, 0.8660254037844387076, 1.000000000000000000, 0.8660254037844387076, 1.000000000000000000, 0.8660254037844387076, 1.000000000000000000, 0.8660254037844387076, 1.000000000000000000, 0.8660254037844387076, 1.000000000000000000, 0.8660254037844387076, 1.000000000000000000, 0.8660254037844387076, 1.000000000000000000, 0.8660254037844387076, 1.000000000000000000, 0.8660254037844387076, 1.000000000000000000, 0.8660254037844387076, 1.000000000000000000, 0.8660254037844387076, 1.000000000000000000, 0.8660254037844387076, 1.000000000000000000, 0.8660254037844387076, 1.000000000000000000, 0.8660254037844387076, 1.000000000000000000, 0.8660254037844387076, 1.000000000000000000, 0.8660254037844387076, 1.000000000000000000, 0.8660254037844387076, 1.000000000000000000, 0.8660254037844387076, 1.000000000000000000, 0.8660254037844387076, 1.000000000000000000, 0.8660254037844387076, 1.000000000000000000, 0.8660254037844387076, 1.000000000000000000, 0.8660254037844387076, 1.000000000000000000, 0.8660254037844387076, 1.000000000000000000, 0.8660254037844387076, 1.000000000000000000, 0.8660254037844387076, 1.000000000000000000, 0.8660254037844387076, 1.000000000000000000, 0.8660254037844387076, 1.000000000000000000, 0.8660254037844387076, 1.000000000000000000, 0.8660254037844387076, 1.000000000000000000, 0.8660254037844387076, 1.000000000000000000, 0.8660254037844387076, 1.000000000000000000, 0.8660254037844387076, 1.000000000000000000, 0.8660254037844387076, 1.000000000000000000, 0.8660254037844387076, 1.000000000000000000, 0.8660254037844387076, 1.000000000000000000, 0.8660254037844387076, 1.000000000000000000, 0.8660254037844387076, 1.000000000000000000, 0.8660254037844387076, 1.000000000000000000, 0.8660254037844387076, 1.000000000000000000, 0.8660254037844387076, 1.000000000000000000, 0.8660254037844387076, 1.000000000000000000, 0.8660254037844387076, 1.000000000000000000, 0.8660254037844387076, 1.000000000000000000, 0.8660254037844387076, 1.000000000000000000, 0.8660254037844387076, 1.000000000000000000, 0.8660254037844387076, 1.000000000000000000, 0.8660254037844387076, 1.000000000000000000, 0.8660254037844387076, 1.000000000000000000, 0.8660254037844387076, 1.000000000000000000, 0.8660254037844387076, 1.000000000000000000, 0.8660254037844387076, 1.000000000000000000, 0.8660254037844387076, 1.000000000000000000, 0.8660254037844387076, 1.000000000000000000, 0.8660254037844387076, 1.000000000000000000, 0.8660254037844387076, 1.000000000000000000, 0.8660254037844387076, 1.000000000000000000, 0.8660254037844387076, 1.000000000000000000, 0.8660254037844387076, 1.000000000000000000, 0.8660254037844387076, 1.000000000000000000, 0.8660254037844387076, 1.000000000000000000, 0.8660254037844387076, 1.000000000000000000, 0.8660254037844387076, 1.000000000000000000, 0.8660254037844387076, 1.000000000000000000, 0.8660254037844387076, 1.000000000000000000, 0.8660254037844387076, 1.000000000000000000, 0.8660254037844387076, 1.000000000000000000, 0.8660254037844387076, 1.000000000000000000, 0.8660254037844387076, 1.000000000000000000, 0.8660254037844387076, 1.000000000000000000, 0.8660254037844387076, 1.000000000000000000, 0.8660254037844387076, 1.000000000000000000, 0.8660254037844387076, 1.000000000000000000, 0.8660254037844387076, 1.000000000000000000, 0.8660254037844387076, 1.000000000000000000, 0.8660254037844387076, 1.000000000000000000, 0.8660254037844387076, 1.000000000000000000, 0.8660254037844387076, 1.000000000000000000, 0.8660254037844387076, 1.000000000000000000, 0.8660254037844387076, 1.000000000000000000, 0.8660254037844387076, 1.000000000000000000, 0.8660254037844387076, 1.000000000000000000, 0.8660254037844387076, 1.000000000000000000, 0.8660254037844387076, 1.000000000000000000, 0.8660254037844387076, 1.000000000000000000, 0.8660254037844387076, 1.000000000000000000, 0.8660254037844387076, 1.000000000000000000, 0.8660254037844387076, 1.000000000000000000, 0.8660254037844387076, 1.000000000000000000, 0.8660254037844387076, 1.000000000000000000, 0.8660254037844387076, 1.000000000000000000, 0.8660254037844387076, 1.000000000000000000, 0.8660254037844387076, 1.000000000000000000, 0.8660254037844387076, 1.000000000000000000, 0.8660254037844387076, 1.000000000000000000, 0.8660254037844387076, 1.000000000000000000, 0.8660254037844387076, 1.000000000000000000, 0.8660254037844387076, 1.000000000000000000, 0.8660254037844387076, 1.000000000000000000, 0.8660254037844387076, 1.000000000000000000, 0.8660254037844387076, 1.000000000000000000, 0.8660254037844387076, 1.000000000000000000, 0.8660254037844387076, 1.000000000000000000, 0.8660254037844387076, 1.000000000000000000, 0.8660254037844387076, 1.000000000000000000, 0.8660254037844387076, 1.000000000000000000, 0.8660254037844387076, 1.000000000000000000, 0.8660254037844387076, 1.000000000000000000, 0.8660254037844387076, 1.000000000000000000, 0.8660254037844387076, 1.000000000000000000, 0.8660254037844387076, 1.000000000000000000, 0.8660254037844387076, 1.000000000000000000, 0.8660254037844387076, 1.000000000000000000, 0.8660254037844387076, 1.000000000000000000, 0.8660254037844387076, 1.000000000000000000, 0.8660254037844387076, 1.000000000000000000, 0.8660254037844387076, 1.000000000000000000, 0.8660254037844387076, 1.000000000000000000, 0.8660254037844387076, 1.000000000000000000, 0.8660254037844387076, 1.000000000000000000, 0.8660254037844387076, 1.000000000000000000, 0.8660254037844387076, 1.000000000000000000, 0.8660254037844387076, 1.000000000000000000, 0.8660254037844387076, 1.000000000000000000, 0.8660254037844387076, 1.000000000000000000, 0.8660254037844387076, 1.000000000000000000, 0.8660254037844387076, 1.000000000000000000, 0.8660254037844387076, 1.000000000000000000, 0.8660254037844387076, 1.000000000000000000, 0.8660254037844387076, 1.000000000000000000, 0.8660254037844387076, 1.000000000000000000, 0.8660254037844387076, 1.000000000000000000, 0.8660254037844387076, 1.000000000000000000, 0.8660254037844387076, 1.000000000000000000, 0.8660254037844387076, 1.000000000000000000, 0.8660254037844387076, 1.000000000000000000, 0.8660254037844387076, 1.000000000000000000, 0.8660254037844387076, 1.000000000000000000, 0.8660254037844387076, 1.000000000000000000, 0.8660254037844387076, 1.000000000000000000, 0.8660254037844387076, 1.000000000000000000, 0.8660254037844387076, 1.000000000000000000, 0.8660254037844387076, 1.000000000000000000, 0.8660254037844387076, 1.000000000000000000, 0.8660254037844387076, 1.000000000000000000, 0.8660254037844387076, 1.000000000000000000, 0.8660254037844387076, 1.000000000000000000, 0.8660254037844387076, 1.000000000000000000, 0.8660254037844387076, 1.000000000000000000, 0.8660254037844387076, 1.000000000000000000, 0.8660254037844387076, 1.000000000000000000, 0.8660254037844387076, 1.000000000000000000, 0.8660254037844387076, 1.000000000000000000, 0.8660254037844387076, 1.000000000000000000, 0.8660254037844387076, 1.000000000000000000, 0.8660254037844387076, 1.000000000000000000, 0.8660254037844387076, 1.000000000000000000, 0.8660254037844387076, 1.000000000000000000, 0.8660254037844387076, 1.000000000000000000, 0.8660254037844387076, 1.000000000000000000, 0.8660254037844387076, 1.000000000000000000, 0.8660254037844387076, 1.000000000000000000, 0.8660254037844387076, 1.000000000000000000, 0.8660254037844387076, 1.000000000000000000, 0.8660254037844387076, 1.000000000000000000, 0.8660254037844387076, 1.000000000000000000, 0.8660254037844387076, 1.000000000000000000, 0.8660254037844387076, 1.000000000000000000, 0.8660254037844387076, 1.000000000000000000, 0.8660254037844387076, 1.000000000000000000, 0.8660254037844387076, 1.000000000000000000, 0.8660254037844387076, 1.000000000000000000, 0.8660254037844387076, 1.000000000000000000, 0.8660254037844387076, 1.000000000000000000, 0.8660254037844387076, 1.000000000000000000, 0.8660254037844387076, 1.000000000000000000, 0.8660254037844387076, 1.000000000000000000, 0.8660254037844387076, 1.000000000000000000, 0.8660254037844387076, 1.000000000000000000, 0.8660254037844387076, 1.000000000000000000, 0.8660254037844387076, 1.000000000000000000, 0.8660254037844387076, 1.000000000000000000, 0.8660254037844387076, 1.000000000000000000, 0.8660254037844387076, 1.000000000000000000, 0.8660254037844387076, 1.000000000000000000, 0.8660254037844387076, 1.000000000000000000, 0.8660254037844387076, 1.000000000000000000, 0.8660254037844387076, 1.000000000000000000, 0.8660254037844387076, 1.000000000000000000, 0.8660254037844387076, 1.000000000000000000, 0.8660254037844387076, 1.000000000000000000, 0.8660254037844387076, 1.000000000000000000, 0.8660254037844387076, 1.000000000000000000, 0.8660254037844387076, 1.000000000000000000, 0.8660254037844387076, 1.000000000000000000, 0.8660254037844387076, 1.000000000000000000, 0.8660254037844387076, 1.000000000000000000, 0.8660254037844387076, 1.000000000000000000, 0.8660254037844387076, 1.000000000000000000, 0.8660254037844387076, 1.000000000000000000, 0.8660254037844387076, 1.000000000000000000, 0.8660254037844387076, 1.000000000000000000, 0.8660254037844387076, 1.000000000000000000, 0.8660254037844387076, 1.000000000000000000, 0.8660254037844387076, 1.000000000000000000, 0.8660254037844387076, 1.000000000000000000, 0.8660254037844387076, 1.000000000000000000, 0.8660254037844387076, 1.000000000000000000, 0.8660254037844387076, 1.000000000000000000, 0.8660254037844387076, 1.000000000000000000, 0.8660254037844387076, 1.000000000000000000, 0.8660254037844387076, 1.000000000000000000, 0.8660254037844387076, 1.000000000000000000, 0.8660254037844387076, 1.000000000000000000, 0.8660254037844387076, 1.000000000000000000, 0.8660254037844387076, 1.000000000000000000, 0.8660254037844387076, 1.000000000000000000, 0.8660254037844387076, 1.000000000000000000, 0.8660254037844387076, 1.000000000000000000, 0.8660254037844387076, 1.000000000000000000, 0.8660254037844387076, 1.000000000000000000, 0.8660254037844387076, 1.000000000000000000, 0.8660254037844387076, 1.000000000000000000, 0.8660254037844387076, 1.000000000000000000, 0.8660254037844387076, 1.000000000000000000, 0.8660254037844387076, 1.000000000000000000, 0.8660254037844387076, 1.000000000000000000, 0.8660254037844387076, 1.000000000000000000, 0.8660254037844387076, 1.000000000000000000, 0.8660254037844387076, 1.000000000000000000, 0.8660254037844387076, 1.000000000000000000, 0.8660254037844387076, 1.000000000000000000, 0.8660254037844387076, 1.000000000000000000, 0.8660254037844387076, 1.000000000000000000, 0.8660254037844387076, 1.000000000000000000, 0.8660254037844387076, 1.000000000000000000, 0.8660254037844387076, 1.000000000000000000, 0.8660254037844387076, 1.000000000000000000, 0.8660254037844387076, 1.000000000000000000, 0.8660254037844387076, 1.000000000000000000, 0.8660254037844387076, 1.000000000000000000, 0.8660254037844387076, 1.000000000000000000, 0.8660254037844387076, 1.000000000000000000, 0.8660254037844387076, 1.000000000000000000, 0.8660254037844387076, 1.000000000000000000, 0.8660254037844387076, 1.000000000000000000, 0.8660254037844387076, 1.000000000000000000, 0.8660254037844387076, 1.000000000000000000, 0.8660254037844387076, 1.000000000000000000, 0.8660254037844387076, 1.000000000000000000, 0.8660254037844387076, 1.000000000000000000, 0.8660254037844387076, 1.000000000000000000, 0.8660254037844387076, 1.000000000000000000, 0.8660254037844387076, 1.000000000000000000, 0.8660254037844387076, 1.000000000000000000, 0.8660254037844387076, 1.000000000000000000, 0.8660254037844387076, 1.000000000000000000, 0.8660254037844387076, 1.000000000000000000, 0.8660254037844387076, 1.000000000000000000, 0.8660254037844387076, 1.000000000000000000, 0.8660254037844387076, 1.000000000000000000, 0.8660254037844387076, 1.000000000000000000, 0.8660254037844387076, 1.000000000000000000, 0.8660254037844387076, 1.000000000000000000, 0.8660254037844387076, 1.000000000000000000, 0.8660254037844387076, 1.000000000000000000, 0.8660254037844387076, 1.000000000000000000, 0.8660254037844387076, 1.000000000000000000, 0.8660254037844387076, 1.000000000000000000, 0.8660254037844387076, 1.000000000000000000, 0.8660254037844387076, 1.000000000000000000, 0.8660254037844387076, 1.000000000000000000, 0.8660254037844387076, 1.000000000000000000, 0.8660254037844387076, 1.000000000000000000, 0.8660254037844387076, 1.000000000000000000, 0.8660254037844387076, 1.000000000000000000, 0.8660254037844387076, 1.000000000000000000, 0.8660254037844387076, 1.000000000000000000, 0.8660254037844387076, 1.000000000000000000, 0.8660254037844387076, 1.000000000000000000, 0.8660254037844387076, 1.000000000000000000, 0.8660254037844387076, 1.000000000000000000, 0.8660254037844387076, 1.000000000000000000, 0.8660254037844387076, 1.000000000000000000, 0.8660254037844387076, 1.000000000000000000, 0.8660254037844387076, 1.000000000000000000, 0.8660254037844387076, 1.000000000000000000, 0.8660254037844387076, 1.000000000000000000, 0.8660254037844387076, 1.000000000000000000, 0.8660254037844387076, 1.000000000000000000, 0.8660254037844387076, 1.000000000000000000, 0.8660254037844387076, 1.000000000000000000, 0.8660254037844387076, 1.000000000000000000, 0.8660254037844387076, 1.000000000000000000, 0.8660254037844387076, 1.000000000000000000, 0.8660254037844387076, 1.000000000000000000, 0.8660254037844387076, 1.000000000000000000, 0.8660254037844387076, 1.000000000000000000, 0.8660254037844387076, 1.000000000000000000, 0.8660254037844387076, 1.000000000000000000, 0.8660254037844387076, 1.000000000000000000, 0.8660254037844387076, 1.000000000000000000, 0.8660254037844387076, 1.000000000000000000, 0.8660254037844387076, 1.000000000000000000, 0.8660254037844387076, 1.000000000000000000, 0.8660254037844387076, 1.000000000000000000, 0.8660254037844387076, 1.000000000000000000, 0.8660254037844387076, 1.000000000000000000, 0.8660254037844387076, 1.000000000000000000, 0.8660254037844387076, 1.000000000000000000, 0.8660254037844387076, 1.000000000000000000, 0.8660254037844387076, 1.000000000000000000, 0.8660254037844387076, 1.000000000000000000, 0.8660254037844387076, 1.000000000000000000, 0.8660254037844387076, 1.000000000000000000, 0.8660254037844387076, 1.000000000000000000, 0.8660254037844387076, 1.000000000000000000, 0.8660254037844387076, 1.000000000000000000, 0.8660254037844387076, 1.000000000000000000, 0.8660254037844387076, 1.000000000000000000, 0.8660254037844387076, 1.000000000000000000, 0.8660254037844387076, 1.000000000000000000, 0.8660254037844387076, 1.000000000000000000, 0.8660254037844387076, 1.000000000000000000, 0.8660254037844387076, 1.000000000000000000, 0.8660254037844387076, 1.000000000000000000, 0.8660254037844387076, 1.000000000000000000, 0.8660254037844387076, 1.000000000000000000, 0.8660254037844387076, 1.000000000000000000, 0.8660254037844387076, 1.000000000000000000, 0.8660254037844387076, 1.000000000000000000, 0.8660254037844387076, 1.000000000000000000, 0.8660254037844387076, 1.000000000000000000, 0.8660254037844387076, 1.000000000000000000, 0.8660254037844387076, 1.000000000000000000, 0.8660254037844387076, 1.000000000000000000, 0.8660254037844387076, 1.000000000000000000, 0.8660254037844387076, 1.000000000000000000, 0.8660254037844387076, 1.000000000000000000, 0.8660254037844387076, 1.000000000000000000, 0.8660254037844387076, 1.000000000000000000, 0.8660254037844387076, 1.000000000000000000, 0.8660254037844387076, 1.000000000000000000, 0.8660254037844387076, 1.000000000000000000, 0.8660254037844387076, 1.000000000000000000, 0.8660254037844387076, 1.000000000000000000, 0.8660254037844387076, 1.000000000000000000, 0.8660254037844387076, 1.000000000000000000, 0.8660254037844387076, 1.000000000000000000, 0.8660254037844387076, 1.000000000000000000, 0.8660254037844387076, 1.000000000000000000, 0.8660254037844387076, 1.000000000000000000, 0.8660254037844387076, 1.000000000000000000, 0.8660254037844387076, 1.000000000000000000, 0.8660254037844387076, 1.000000000000000000, 0.8660254037844387076, 1.000000000000000000, 0.8660254037844387076, 1.000000000000000000, 0.8660254037844387076, 1.000000000000000000, 0.8660254037844387076, 1.000000000000000000, 0.8660254037844387076, 1.000000000000000000, 0.8660254037844387076, 1.000000000000000000, 0.8660254037844387076, 1.000000000000000000, 0.8660254037844387076, 1.000000000000000000, 0.8660254037844387076, 1.000000000000000000, 0.8660254037844387076, 1.000000000000000000, 0.8660254037844387076, 1.000000000000000000, 0.8660254037844387076, 1.000000000000000000, 0.8660254037844387076, 1.000000000000000000, 0.8660254037844387076, 1.000000000000000000, 0.8660254037844387076, 1.000000000000000000, 0.8660254037844387076, 1.000000000000000000, 0.8660254037844387076, 1.000000000000000000, 0.8660254037844387076, 1.000000000000000000, 0.8660254037844387076, 1.000000000000000000, 0.8660254037844387076, 1.000000000000000000, 0.8660254037844387076, 1.000000000000000000, 0.8660254037844387076, 1.000000000000000000, 0.8660254037844387076, 1.000000000000000000, 0.8660254037844387076, 1.000000000000000000, 0.8660254037844387076, 1.000000000000000000, 0.8660254037844387076, 1.000000000000000000, 0.8660254037844387076, 1.000000000000000000, 0.8660254037844387076, 1.000000000000000000, 0.8660254037844387076, 1.000000000000000000, 0.8660254037844387076, 1.000000000000000000, 0.8660254037844387076, 1.000000000000000000, 0.8660254037844387076, 1.000000000000000000, 0.8660254037844387076, 1.000000000000000000, 0.8660254037844387076, 1.000000000000000000, 0.8660254037844387076, 1.000000000000000000, 0.8660254037844387076, 1.000000000000000000, 0.8660254037844387076, 1.000000000000000000, 0.8660254037844387076, 1.000000000000000000, 0.8660254037844387076, 1.000000000000000000, 0.8660254037844387076, 1.000000000000000000, 0.8660254037844387076, 1.000000000000000000, 0.8660254037844387076, 1.000000000000000000, 0.8660254037844387076, 1.000000000000000000, 0.8660254037844387076, 1.000000000000000000, 0.8660254037844387076, 1.000000000000000000, 0.8660254037844387076, 1.000000000000000000, 0.8660254037844387076, 1.000000000000000000, 0.8660254037844387076, 1.000000000000000000, 0.8660254037844387076, 1.000000000000000000, 0.8660254037844387076, 1.000000000000000000, 0.8660254037844387076, 1.000000000000000000, 0.8660254037844387076, 1.000000000000000000, 0.8660254037844387076, 1.000000000000000000, 0.8660254037844387076, 1.000000000000000000, 0.8660254037844387076, 1.000000000000000000, 0.8660254037844387076, 1.000000000000000000, 0.8660254037844387076, 1.000000000000000000, 0.8660254037844387076, 1.000000000000000000, 0.8660254037844387076, 1.000000000000000000, 0.8660254037844387076, 1.000000000000000000, 0.8660254037844387076, 1.000000000000000000, 0.8660254037844387076, 1.000000000000000000, 0.8660254037844387076, 1.000000000000000000, 0.8660254037844387076, 1.000000000000000000, 0.8660254037844387076, 1.000000000000000000, 0.8660254037844387076, 1.000000000000000000, 0.8660254037844387076, 1.000000000000000000, 0.8660254037844387076, 1.000000000000000000, 0.8660254037844387076, 1.000000000000000000, 0.8660254037844387076, 1.000000000000000000, 0.8660254037844387076, 1.000000000000000000, 0.8660254037844387076, 1.000000000000000000, 0.8660254037844387076, 1.000000000000000000, 0.8660254037844387076, 1.000000000000000000, 0.8660254037844387076, 1.000000000000000000, 0.8660254037844387076, 1.000000000000000000, 0.8660254037844387076, 1.000000000000000000, 0.8660254037844387076, 1.000000000000000000, 0.8660254037844387076, 1.000000000000000000, 0.8660254037844387076, 1.000000000000000000, 0.8660254037844387076, 1.000000000000000000, 0.8660254037844387076, 1.000000000000000000, 0.8660254037844387076, 1.000000000000000000, 0.8660254037844387076, 1.000000000000000000, 0.8660254037844387076, 1.000000000000000000, 0.8660254037844387076, 1.000000000000000000, 0.8660254037844387076, 1.000000000000000000, 0.8660254037844387076, 1.000000000000000000, 0.8660254037844387076, 1.000000000000000000, 0.8660254037844387076, 1.000000000000000000, 0.8660254037844387076, 1.000000000000000000, 0.8660254037844387076, 1.000000000000000000, 0.8660254037844387076, 1.000000000000000000, 0.8660254037844387076, 1.000000000000000000, 0.8660254037844387076, 1.000000000000000000, 0.8660254037844387076, 1.000000000000000000, 0.8660254037844387076, 1.000000000000000000, 0.8660254037844387076, 1.000000000000000000, 0.8660254037844387076, 1.000000000000000000, 0.8660254037844387076, 1.000000000000000000, 0.8660254037844387076, 1.000000000000000000, 0.8660254037844387076, 1.000000000000000000, 0.8660254037844387076, 1.000000000000000000, 0.8660254037844387076, 1.000000000000000000, 0.8660254037844387076, 1.000000000000000000, 0.8660254037844387076, 1.000000000000000000, 0.8660254037844387076, 1.000000000000000000, 0.8660254037844387076, 1.000000000000000000, 0.8660254037844387076, 1.000000000000000000, 0.8660254037844387076, 1.000000000000000000, 0.8660254037844387076, 1.000000000000000000, 0.8660254037844387076, 1.000000000000000000, 0.8660254037844387076, 1.000000000000000000, 0.8660254037844387076, 1.000000000000000000, 0.8660254037844387076, 1.000000000000000000, 0.8660254037844387076, 1.000000000000000000, 0.8660254037844387076, 1.000000000000000000, 0.8660254037844387076, 1.000000000000000000, 0.8660254037844387076, 1.000000000000000000, 0.8660254037844387076, 1.000000000000000000, 0.8660254037844387076, 1.000000000000000000, 0.8660254037844387076, 1.000000000000000000, 0.8660254037844387076, 1.000000000000000000, 0.8660254037844387076, 1.000000000000000000, 0.8660254037844387076, 1.000000000000000000, 0.8660254037844387076, 1.000000000000000000, 0.8660254037844387076, 1.000000000000000000, 0.8660254037844387076, 1.000000000000000000, 0.8660254037844387076, 1.000000000000000000, 0.8660254037844387076, 1.000000000000000000, 0.8660254037844387076, 1.000000000000000000, 0.8660254037844387076, 1.000000000000000000, 0.8660254037844387076, 1.000000000000000000, 0.8660254037844387076, 1.000000000000000000, 0.8660254037844387076, 1.000000000000000000, 0.8660254037844387076, 1.000000000000000000, 0.8660254037844387076, 1.000000000000000000, 0.8660254037844387076, 1.000000000000000000, 0.8660254037844387076, 1.000000000000000000, 0.8660254037844387076, 1.000000000000000000, 0.8660254037844387076, 1.000000000000000000, 0.8660254037844387076, 1.000000000000000000, 0.8660254037844387076, 1.000000000000000000, 0.8660254037844387076, 1.000000000000000000, 0.8660254037844387076, 1.000000000000000000, 0.8660254037844387076, 1.000000000000000000, 0.8660254037844387076, 1.000000000000000000, 0.8660254037844387076, 1.000000000000000000, 0.8660254037844387076, 1.000000000000000000, 0.8660254037844387076, 1.000000000000000000, 0.8660254037844387076, 1.000000000000000000, 0.8660254037844387076, 1.000000000000000000 ) ) 
 REPRESENTATION_ITEM ( '' )  );
#48332 = VECTOR ( 'NONE', #7821, 1000.000000000000000 ) ;
#48331 = CARTESIAN_POINT ( 'NONE',  ( -1.339745962155660663, -2.794658198738523058, 4.999999999999972466 ) ) ;
#48333 = CARTESIAN_POINT ( 'NONE',  ( -4.458734124999999437, -60.56249999863440081, 0.000000000000000000 ) ) ;
#48334 = CARTESIAN_POINT ( 'NONE',  ( 4.458734125000001214, 2.854166668032259491, 2.574251347313718519 ) ) ;
#48335 = ORIENTED_EDGE ( 'NONE', *, *, #33933, .F. ) ;
#48336 = DIRECTION ( 'NONE',  ( 0.000000000000000000, 0.000000000000000000, 1.000000000000000000 ) ) ;
#48337 = CARTESIAN_POINT ( 'NONE',  ( -4.458734124999998549, 16.77083333469892779, 2.574251347313722516 ) ) ;
#48338 = CARTESIAN_POINT ( 'NONE',  ( -53.51423613279429503, -145.2500000013656347, 4.591703134518082763 ) ) ;
#48339 = CARTESIAN_POINT ( 'NONE',  ( 2.499999999999998668, 16.66666666666666785, -4.330127018922193649 ) ) ;
#48340 = AXIS2_PLACEMENT_3D ( 'NONE', #49200, #24759, #39222 ) ;
#48341 = CARTESIAN_POINT ( 'NONE',  ( 1.846868145590735200, -166.2500000013656063, -4.458734124999999437 ) ) ;
#48342 = ORIENTED_EDGE ( 'NONE', *, *, #41668, .F. ) ;
#48343 = CARTESIAN_POINT ( 'NONE',  ( 2.229367062500001939, -75.97916666530106511, 3.861377020970579999 ) ) ;
#48344 = LINE ( 'NONE', #25168, #31548 ) ;
#48345 = CARTESIAN_POINT ( 'NONE',  ( -2.229367062499996610, 8.854166668032261711, 3.861377020970582219 ) ) ;
#48346 = EDGE_CURVE ( 'NONE', #41941, #62409, #55879, .T. ) ;
#48347 = EDGE_CURVE ( 'NONE', #44647, #42718, #33691, .T. ) ;
#48348 = CARTESIAN_POINT ( 'NONE',  ( -5.000000000000000888, -162.6875000027311842, -2.071067811865475949 ) ) ;
#48349 = EDGE_CURVE ( 'NONE', #27617, #4086, #2914, .T. ) ;
#48350 = CARTESIAN_POINT ( 'NONE',  ( -3.152548672688508926E-16, -66.81249999863442213, -5.148502694627439702 ) ) ;
#48351 = CARTESIAN_POINT ( 'NONE',  ( -5.000000000000000000, -17.95833333060214798, -2.886751345948128211 ) ) ;
#48352 = CARTESIAN_POINT ( 'NONE',  ( 6.123233995736766282E-16, -170.0000000000000000, -5.000000000000000000 ) ) ;
#48353 = CARTESIAN_POINT ( 'NONE',  ( 5.000000000000000888, -44.45833333060214443, 2.886751345948126879 ) ) ;
#48354 = CARTESIAN_POINT ( 'NONE',  ( -4.458734124999999437, -110.4374999986343937, 0.000000000000000000 ) ) ;
#48355 = CARTESIAN_POINT ( 'NONE',  ( 1.339745962155612702, -18.16965819600733312, -5.000000000000000000 ) ) ;
#48356 = CYLINDRICAL_SURFACE ( 'NONE', #23236, 5.000000000000000000 ) ;
#48357 = CARTESIAN_POINT ( 'NONE',  ( 2.229367062499998831, -40.64583333196773651, -3.861377020970580887 ) ) ;
#48358 = CARTESIAN_POINT ( 'NONE',  ( -2.229367062500000163, -28.72916666530107221, -3.861377020970580443 ) ) ;
#48359 = CARTESIAN_POINT ( 'NONE',  ( -59.81910112700027327, -140.3125000027311842, -2.462841084822392279 ) ) ;
#48360 = CARTESIAN_POINT ( 'NONE',  ( 2.500000000000002220, 25.33333333333333215, 4.330127018922192761 ) ) ;
#48361 = CARTESIAN_POINT ( 'NONE',  ( 5.000000000000000000, -151.1875000027312126, 2.071067811865478614 ) ) ;
#48362 = CARTESIAN_POINT ( 'NONE',  ( -4.458734124999998549, -107.4791666653010651, 2.574251347313722516 ) ) ;
#48363 = CARTESIAN_POINT ( 'NONE',  ( -4.458734124999998549, -32.22916666530106511, 2.574251347313722516 ) ) ;
#48364 = CARTESIAN_POINT ( 'NONE',  ( 2.500000000000002220, -66.54166666393547303, 4.330127018922192761 ) ) ;
#48365 = ADVANCED_FACE ( 'NONE', ( #15604 ), #15279, .T. ) ;
#48366 = CARTESIAN_POINT ( 'NONE',  ( -50.55543936806279248, -147.3125000013656063, 0.3552334253322060320 ) ) ;
#48367 = CARTESIAN_POINT ( 'NONE',  ( 3.535533905932736864, -142.1250000000000000, 3.535533905932738641 ) ) ;
#48368 = ADVANCED_FACE ( 'NONE', ( #54524 ), #6917, .F. ) ;
#48369 = CARTESIAN_POINT ( 'NONE',  ( 2.229367062500001939, -74.22916666530106511, 3.861377020970579999 ) ) ;
#48370 = CARTESIAN_POINT ( 'NONE',  ( 3.152801135295366208, -167.8125000013656063, 3.152801135295367985 ) ) ;
#48371 = CARTESIAN_POINT ( 'NONE',  ( 2.229367062500001939, -27.97916666530107221, 3.861377020970579999 ) ) ;
#48372 = CARTESIAN_POINT ( 'NONE',  ( -1.339745962155610925, -27.66965819600733667, 5.000000000000000000 ) ) ;
#48373 = CYLINDRICAL_SURFACE ( 'NONE', #61588, 5.000000000000000000 ) ;
#48374 = CARTESIAN_POINT ( 'NONE',  ( -4.999999999999999112, -20.91666666666666785, 2.886751345948131764 ) ) ;
#48375 = CARTESIAN_POINT ( 'NONE',  ( -3.152801135295367096, -148.0625000013655779, -3.152801135295367541 ) ) ;
#48376 = ORIENTED_EDGE ( 'NONE', *, *, #13729, .T. ) ;
#48377 = CARTESIAN_POINT ( 'NONE',  ( -3.152548672688508926E-16, 29.18750000136559208, -5.148502694627439702 ) ) ;
#48378 = CARTESIAN_POINT ( 'NONE',  ( 2.499999999999998668, 1.666666666666666963, -4.330127018922193649 ) ) ;
#48379 = CARTESIAN_POINT ( 'NONE',  ( -2.229367062500000163, -56.72916666530107221, -3.861377020970580443 ) ) ;
#48380 = CARTESIAN_POINT ( 'NONE',  ( 2.500000000000002220, 24.45833333606451987, 4.330127018922192761 ) ) ;
#48381 = CARTESIAN_POINT ( 'NONE',  ( -5.000000000000000888, -162.4375000000000568, 2.071067811865474617 ) ) ;
#48382 = CARTESIAN_POINT ( 'NONE',  ( 5.000000000000000888, 18.41666666666666430, 2.886751345948126879 ) ) ;
#48383 = AXIS2_PLACEMENT_3D ( 'NONE', #42925, #7898, #36849 ) ;
#48384 = CARTESIAN_POINT ( 'NONE',  ( 0.000000000000000000, -120.0000000000000000, 5.000000000000000000 ) ) ;
#48385 = CARTESIAN_POINT ( 'NONE',  ( 4.458734125000001214, -4.895833331967740065, 2.574251347313718519 ) ) ;
#48386 = CARTESIAN_POINT ( 'NONE',  ( -2.916731409357579869E-14, 13.25000000000000178, 5.000000000000000888 ) ) ;
#48387 = CARTESIAN_POINT ( 'NONE',  ( 1.975475456537005874E-15, -8.750000000000000000, 5.000000000000000000 ) ) ;
#48388 = CARTESIAN_POINT ( 'NONE',  ( 4.458734124999998549, 8.020833334698926009, -2.574251347313721627 ) ) ;
#48389 = CARTESIAN_POINT ( 'NONE',  ( 1.339745962155729053, -56.16965819600732601, -4.999999999999933387 ) ) ;
#48390 = CARTESIAN_POINT ( 'NONE',  ( 1.339745962155612702, 0.7053418012614794952, -5.000000000000000000 ) ) ;
#48391 = CARTESIAN_POINT ( 'NONE',  ( 2.229367062500001939, -51.97916666530107221, 3.861377020970579999 ) ) ;
#48392 = CARTESIAN_POINT ( 'NONE',  ( 2.730187237215162345E-16, -160.4375000013655779, -4.458734124999999437 ) ) ;
#48393 = CARTESIAN_POINT ( 'NONE',  ( 5.000000000000000000, -52.29166666393548013, -2.886751345948129988 ) ) ;
#48394 = ORIENTED_EDGE ( 'NONE', *, *, #46857, .T. ) ;
#48395 = CARTESIAN_POINT ( 'NONE',  ( -2.229367062499996610, 3.604166668032260379, 3.861377020970582219 ) ) ;
#48396 = VERTEX_POINT ( 'NONE', #6589 ) ;
#48398 = CARTESIAN_POINT ( 'NONE',  ( -5.000000000000000888, -142.6875000027312126, -2.071067811865475949 ) ) ;
#48397 = FACE_OUTER_BOUND ( 'NONE', #5176, .T. ) ;
#48399 = CARTESIAN_POINT ( 'NONE',  ( 1.846868145590736310, -158.6250000013655779, 4.458734124999999437 ) ) ;
#48400 = ORIENTED_EDGE ( 'NONE', *, *, #39621, .F. ) ;
#48401 = CARTESIAN_POINT ( 'NONE',  ( -6.972266317189433020E-16, -62.12499999726880162, -5.000000000000000000 ) ) ;
#48402 = CARTESIAN_POINT ( 'NONE',  ( -55.39835681537999790, -131.8750000000000284, 4.984105922594378235 ) ) ;
#48403 = CARTESIAN_POINT ( 'NONE',  ( 2.500000000000002220, -47.54166666393547303, 4.330127018922192761 ) ) ;
#48404 = CARTESIAN_POINT ( 'NONE',  ( -4.458734124999998549, -38.47916666530107221, 2.574251347313722516 ) ) ;
#48405 = ORIENTED_EDGE ( 'NONE', *, *, #26298, .F. ) ;
#48406 = LINE ( 'NONE', #9792, #13133 ) ;
#48407 = CARTESIAN_POINT ( 'NONE',  ( -2.229367062500000163, 16.52083333469892779, -3.861377020970580443 ) ) ;
#48408 = CARTESIAN_POINT ( 'NONE',  ( 1.339745962155612702, -12.16965819600733667, -5.000000000000000000 ) ) ;
#48409 = ORIENTED_EDGE ( 'NONE', *, *, #24727, .T. ) ;
#48410 = CARTESIAN_POINT ( 'NONE',  ( 4.458734124999998549, -85.97916666530107932, -2.574251347313721627 ) ) ;
#48411 = CARTESIAN_POINT ( 'NONE',  ( -58.80597590150559739, -128.1250000027312126, 3.242614290531460330 ) ) ;
#48412 = CARTESIAN_POINT ( 'NONE',  ( -6.972266317189433020E-16, 24.87500000273118417, -5.000000000000000000 ) ) ;
#48413 = CARTESIAN_POINT ( 'NONE',  ( -52.47078701390809385, -134.9999999999999716, 4.127771267674353872 ) ) ;
#48414 = CARTESIAN_POINT ( 'NONE',  ( 3.535533905932736864, -169.1250000000000284, 3.535533905932738641 ) ) ;
#48415 = CARTESIAN_POINT ( 'NONE',  ( 4.458734124999999437, -60.81249999863440081, -5.460374474430324690E-16 ) ) ;
#48416 = CARTESIAN_POINT ( 'NONE',  ( -57.46284108482265651, -145.9375000000000284, 4.819101127000238627 ) ) ;
#48417 = VECTOR ( 'NONE', #55574, 1000.000000000000000 ) ;
#48418 = CARTESIAN_POINT ( 'NONE',  ( -2.229367062500000163, 22.52083333469892423, -3.861377020970580443 ) ) ;
#48419 = CARTESIAN_POINT ( 'NONE',  ( 5.000000000000000000, -42.49999999999999289, -6.123233995736766282E-16 ) ) ;
#48420 =( BOUNDED_CURVE ( )  B_SPLINE_CURVE ( 2, ( #26552, #2133, #51641, #8207, #60661, #22689, #12706, #21736, #47435 ),
 .UNSPECIFIED., .F., .F. ) 
 B_SPLINE_CURVE_WITH_KNOTS ( ( 3, 2, 2, 2, 3 ),
 ( 0.7583333333333330817, 0.7624999999999997335, 0.7666666666666664964, 0.7708333333333331483, 0.7749999999999998002 ),
 .UNSPECIFIED. ) 
 CURVE ( )  GEOMETRIC_REPRESENTATION_ITEM ( )  RATIONAL_B_SPLINE_CURVE ( ( 1.000000000000003997, 0.9238795325112826307, 1.000000000000000000, 0.9238795325112867385, 1.000000000000000000, 0.9238795325112867385, 1.000000000000000000, 0.9238795325112908463, 0.9999999999999958922 ) ) 
 REPRESENTATION_ITEM ( '' )  );
#48421 = DIRECTION ( 'NONE',  ( -0.6485228581062915110, 0.000000000000000000, -0.7611951803011149931 ) ) ;
#48422 = EDGE_CURVE ( 'NONE', #42211, #48477, #46364, .T. ) ;
#48423 = CARTESIAN_POINT ( 'NONE',  ( -2.229367062499996610, -46.39583333196774362, 3.861377020970582219 ) ) ;
#48424 = CARTESIAN_POINT ( 'NONE',  ( -4.999999999999999112, -3.791666663935478798, 2.886751345948131764 ) ) ;
#48425 = CARTESIAN_POINT ( 'NONE',  ( 0.000000000000000000, -170.0000000000000000, 0.000000000000000000 ) ) ;
#48426 = CARTESIAN_POINT ( 'NONE',  ( -5.000000000000000000, -66.87499999726881583, 0.000000000000000000 ) ) ;
#48427 = CARTESIAN_POINT ( 'NONE',  ( -4.458734124999999437, -85.56249999863439371, 0.000000000000000000 ) ) ;
#48428 = CARTESIAN_POINT ( 'NONE',  ( 4.458734124999999437, -106.8124999986343937, -5.460374474430324690E-16 ) ) ;
#48429 = CARTESIAN_POINT ( 'NONE',  ( 4.458734124999999437, -12.06249999863440081, -5.460374474430324690E-16 ) ) ;
#48431 = ORIENTED_EDGE ( 'NONE', *, *, #15284, .F. ) ;
#48430 = EDGE_CURVE ( 'NONE', #36504, #44414, #25568, .T. ) ;
#48432 = CARTESIAN_POINT ( 'NONE',  ( 5.000000000000000888, -52.58333333333332860, 2.886751345948126879 ) ) ;
#48433 = CARTESIAN_POINT ( 'NONE',  ( 4.458734124999999437, -99.81249999863440792, -5.460374474430324690E-16 ) ) ;
#48434 = CARTESIAN_POINT ( 'NONE',  ( -2.071067811865478170, -163.4375000027311842, 5.000000000000000000 ) ) ;
#48435 = CARTESIAN_POINT ( 'NONE',  ( -3.152548672688508926E-16, -91.81249999863442213, -5.148502694627439702 ) ) ;
#48437 = EDGE_CURVE ( 'NONE', #50402, #11950, #6915, .T. ) ;
#48436 = CARTESIAN_POINT ( 'NONE',  ( -2.500000000000000444, -52.04166666393547303, -4.330127018922193649 ) ) ;
#48438 = DIRECTION ( 'NONE',  ( -0.000000000000000000, 1.000000000000000000, -0.000000000000000000 ) ) ;
#48439 = EDGE_CURVE ( 'NONE', #33230, #55713, #7238, .T. ) ;
#48440 = CARTESIAN_POINT ( 'NONE',  ( -59.29741812935640155, -129.6250000013655779, -2.196230717870135685 ) ) ;
#48441 = CARTESIAN_POINT ( 'NONE',  ( -59.44456063193725015, -147.5625000013656063, -0.3552334253322034230 ) ) ;
#48442 = CARTESIAN_POINT ( 'NONE',  ( -2.229367062499996610, -20.14583333196774007, 3.861377020970582219 ) ) ;
#48443 = CARTESIAN_POINT ( 'NONE',  ( -4.458734124999998549, 12.52083333469892779, 2.574251347313722516 ) ) ;
#48444 = CARTESIAN_POINT ( 'NONE',  ( -4.458734124999999437, -61.64583333196774362, -2.574251347313719407 ) ) ;
#48445 = DIRECTION ( 'NONE',  ( 0.000000000000000000, 0.000000000000000000, 1.000000000000000000 ) ) ;
#48446 = CARTESIAN_POINT ( 'NONE',  ( 4.458734124999998549, -13.72916666530107399, -2.574251347313721627 ) ) ;
#48447 = CARTESIAN_POINT ( 'NONE',  ( 1.975475456537005874E-15, -34.62499999726880873, 5.000000000000000000 ) ) ;
#48448 = CARTESIAN_POINT ( 'NONE',  ( -5.000000000000000888, -154.5625000000000000, -2.071067811865475949 ) ) ;
#48449 = EDGE_CURVE ( 'NONE', #46456, #23583, #36490, .T. ) ;
#48450 = ORIENTED_EDGE ( 'NONE', *, *, #58125, .F. ) ;
#48451 = CARTESIAN_POINT ( 'NONE',  ( -3.152548672688508926E-16, -41.81249999863440081, -5.148502694627439702 ) ) ;
#48452 = DIRECTION ( 'NONE',  ( -0.000000000000000000, 1.000000000000000000, -0.000000000000000000 ) ) ;
#48453 = EDGE_CURVE ( 'NONE', #57839, #34229, #26637, .T. ) ;
#48454 = CARTESIAN_POINT ( 'NONE',  ( 1.975475456537005874E-15, -64.62499999726880162, 5.000000000000000000 ) ) ;
#48455 = DIRECTION ( 'NONE',  ( 0.000000000000000000, 0.000000000000000000, 1.000000000000000000 ) ) ;
#48456 = CARTESIAN_POINT ( 'NONE',  ( 9.457646018065525792E-16, -86.06249999863439371, 5.148502694627439702 ) ) ;
#48457 = CARTESIAN_POINT ( 'NONE',  ( -3.152548672688508926E-16, 20.18750000136559208, -5.148502694627439702 ) ) ;
#48458 = CARTESIAN_POINT ( 'NONE',  ( -4.458734124999999437, 10.68750000136559386, 0.000000000000000000 ) ) ;
#48459 = EDGE_CURVE ( 'NONE', #721, #14946, #45823, .T. ) ;
#48460 = CARTESIAN_POINT ( 'NONE',  ( -2.500000000000000444, -82.04166666393547303, -4.330127018922193649 ) ) ;
#48461 = CARTESIAN_POINT ( 'NONE',  ( -3.535533905932737309, -165.7500000027312126, -3.535533905932738197 ) ) ;
#48462 = CARTESIAN_POINT ( 'NONE',  ( -55.00000000000002132, 15.00000000000000000, 0.000000000000000000 ) ) ;
#48463 = CARTESIAN_POINT ( 'NONE',  ( 2.499999999999998668, -71.33333333333332860, -4.330127018922193649 ) ) ;
#48464 = CARTESIAN_POINT ( 'NONE',  ( 5.000000000000000000, 12.62500000273118417, -6.123233995736766282E-16 ) ) ;
#48465 = ORIENTED_EDGE ( 'NONE', *, *, #55161, .F. ) ;
#48466 = CARTESIAN_POINT ( 'NONE',  ( -2.499999999999996447, -6.708333330602149758, 4.330127018922195425 ) ) ;
#48467 = ORIENTED_EDGE ( 'NONE', *, *, #22818, .T. ) ;
#48468 = CARTESIAN_POINT ( 'NONE',  ( -54.60164318462004474, -144.5000000027312126, -4.984105922594373794 ) ) ;
#48470 = CARTESIAN_POINT ( 'NONE',  ( 5.000000000000000888, -30.58333333333332860, 2.886751345948126879 ) ) ;
#48469 = CARTESIAN_POINT ( 'NONE',  ( -58.24261429053147765, -155.0000000000000284, -3.805975901505573411 ) ) ;
#48471 = CARTESIAN_POINT ( 'NONE',  ( -3.152548672688508926E-16, -33.56249999863440792, -5.148502694627439702 ) ) ;
#48472 = CARTESIAN_POINT ( 'NONE',  ( -5.000000000000000000, -33.87499999726880873, 0.000000000000000000 ) ) ;
#48474 = VERTEX_POINT ( 'NONE', #21711 ) ;
#48473 = CARTESIAN_POINT ( 'NONE',  ( 9.457646018065525792E-16, -67.06249999863440792, 5.148502694627439702 ) ) ;
#48475 = CARTESIAN_POINT ( 'NONE',  ( -57.89159099828107458, -150.9375000013656063, -3.393966926194107447 ) ) ;
#48477 = VERTEX_POINT ( 'NONE', #1787 ) ;
#48476 = CARTESIAN_POINT ( 'NONE',  ( -2.229367062499996610, -15.39583333196773651, 3.861377020970582219 ) ) ;
#48478 = CARTESIAN_POINT ( 'NONE',  ( 5.000000000000000000, -79.41666666666665719, -2.886751345948129988 ) ) ;
#48479 = CARTESIAN_POINT ( 'NONE',  ( 0.000000000000000000, -120.0000000000000000, 0.000000000000000000 ) ) ;
#48480 = CARTESIAN_POINT ( 'NONE',  ( 9.457646018065525792E-16, -59.31249999863440081, 5.148502694627439702 ) ) ;
#48481 =( BOUNDED_CURVE ( )  B_SPLINE_CURVE ( 2, ( #20377, #40623, #4083, #54473, #10400, #28514, #23706, #30012, #45131 ),
 .UNSPECIFIED., .F., .F. ) 
 B_SPLINE_CURVE_WITH_KNOTS ( ( 3, 2, 2, 2, 3 ),
 ( 0.3160714285714285587, 0.3166666666666666519, 0.3178571428571428381, 0.3190476190476190244, 0.3196428571428571175 ),
 .UNSPECIFIED. ) 
 CURVE ( )  GEOMETRIC_REPRESENTATION_ITEM ( )  RATIONAL_B_SPLINE_CURVE ( ( 0.9330127018922194093, 0.9330127018922194093, 1.000000000000000000, 0.8660254037844387076, 1.000000000000000000, 0.8660254037844387076, 1.000000000000000000, 0.9330127018922194093, 0.9330127018922194093 ) ) 
 REPRESENTATION_ITEM ( '' )  );
#48482 = CARTESIAN_POINT ( 'NONE',  ( -2.499999999999996447, -82.70833333060214443, 4.330127018922195425 ) ) ;
#48484 = ORIENTED_EDGE ( 'NONE', *, *, #32676, .T. ) ;
#48483 = CARTESIAN_POINT ( 'NONE',  ( -5.000000000000000000, 10.12500000273118594, 0.000000000000000000 ) ) ;
#48485 = CARTESIAN_POINT ( 'NONE',  ( -49.85088928181150436, -146.5625000000000284, -1.666127454062680702 ) ) ;
#48486 = CARTESIAN_POINT ( 'NONE',  ( 2.229367062500001939, -22.22916666530107221, 3.861377020970579999 ) ) ;
#48488 = ORIENTED_EDGE ( 'NONE', *, *, #16562, .F. ) ;
#48487 = CARTESIAN_POINT ( 'NONE',  ( 9.457646018065525792E-16, -60.31249999863440792, 5.148502694627439702 ) ) ;
#48489 = DIRECTION ( 'NONE',  ( 1.000000000000000000, 0.000000000000000000, 0.000000000000000000 ) ) ;
#48490 = CARTESIAN_POINT ( 'NONE',  ( -4.458734125000000326, -167.2500000013655779, -1.846868145590735644 ) ) ;
#48491 = CARTESIAN_POINT ( 'NONE',  ( 4.458734124999999437, -103.0624999986344079, -5.460374474430324690E-16 ) ) ;
#48492 = CARTESIAN_POINT ( 'NONE',  ( 1.339745962155615144, -8.580341798530293218, 4.999999999999999112 ) ) ;
#48493 = ORIENTED_EDGE ( 'NONE', *, *, #26837, .T. ) ;
#48494 = CARTESIAN_POINT ( 'NONE',  ( -50.40829686548195099, -151.2500000013656063, -1.485763867205728284 ) ) ;
#48495 = CARTESIAN_POINT ( 'NONE',  ( -56.66612745406270335, -139.4375000027312410, -5.149110718188516067 ) ) ;
#48496 = CARTESIAN_POINT ( 'NONE',  ( -4.458734124999999437, -36.31249999863440792, 0.000000000000000000 ) ) ;
#48497 = LINE ( 'NONE', #52078, #5514 ) ;
#48498 = CARTESIAN_POINT ( 'NONE',  ( 4.458734125000001214, -11.89583333196774007, 2.574251347313718519 ) ) ;
#48499 = CARTESIAN_POINT ( 'NONE',  ( -2.229367062500000163, -100.7291666653010651, -3.861377020970580443 ) ) ;
#48500 = CARTESIAN_POINT ( 'NONE',  ( 1.846868145590735200, -145.5000000013655779, -4.458734125000000326 ) ) ;
#48501 = CARTESIAN_POINT ( 'NONE',  ( -4.458734124999999437, -28.56249999863440081, 0.000000000000000000 ) ) ;
#48502 = CARTESIAN_POINT ( 'NONE',  ( -6.972266317189433020E-16, -61.25000000000000000, -5.000000000000000000 ) ) ;
#48503 = CARTESIAN_POINT ( 'NONE',  ( -50.70258187064364108, -131.1250000013655779, 2.196230717870141014 ) ) ;
#48504 = CARTESIAN_POINT ( 'NONE',  ( 2.229367062500001939, -68.22916666530106511, 3.861377020970579999 ) ) ;
#48505 = DIRECTION ( 'NONE',  ( -0.6485228581062915110, 0.000000000000000000, -0.7611951803011149931 ) ) ;
#48506 = CARTESIAN_POINT ( 'NONE',  ( 1.975475456537005874E-15, -54.62499999726880873, 5.000000000000000000 ) ) ;
#48507 = CARTESIAN_POINT ( 'NONE',  ( -3.152801135295367096, -141.0625000013655779, -3.152801135295367541 ) ) ;
#48508 = CARTESIAN_POINT ( 'NONE',  ( 4.458734124999998549, 3.020833334698928674, -2.574251347313721627 ) ) ;
#48509 = ORIENTED_EDGE ( 'NONE', *, *, #27265, .F. ) ;
#48510 = CARTESIAN_POINT ( 'NONE',  ( -2.500000000000000444, -71.04166666393547303, -4.330127018922193649 ) ) ;
#48511 = CARTESIAN_POINT ( 'NONE',  ( 5.000000000000000000, -160.0000000000000000, 0.000000000000000000 ) ) ;
#48513 = CARTESIAN_POINT ( 'NONE',  ( -2.229367062500000163, -27.47916666530107221, -3.861377020970580443 ) ) ;
#48512 = CARTESIAN_POINT ( 'NONE',  ( -2.499999999999996447, -97.83333333333332860, 4.330127018922195425 ) ) ;
#48514 = CARTESIAN_POINT ( 'NONE',  ( 5.000000000000000000, -73.41666666666665719, -2.886751345948130876 ) ) ;
#48515 = CARTESIAN_POINT ( 'NONE',  ( -4.458734124999999437, -74.64583333196773651, -2.574251347313719407 ) ) ;
#48516 = CARTESIAN_POINT ( 'NONE',  ( 9.457646018065525792E-16, 20.68750000136559208, 5.148502694627439702 ) ) ;
#48517 = CARTESIAN_POINT ( 'NONE',  ( -1.339745962155608039, 22.91965820146970856, -5.000000000000004441 ) ) ;
#48518 = CARTESIAN_POINT ( 'NONE',  ( -50.55543936806279248, -141.0625000013656063, 0.3552334253322060320 ) ) ;
#48519 = CARTESIAN_POINT ( 'NONE',  ( -4.458734124999997661, 3.770833334698929562, 2.574251347313722516 ) ) ;
#48520 = CARTESIAN_POINT ( 'NONE',  ( -4.458734124999999437, 25.35416666803225993, -2.574251347313719407 ) ) ;
#48521 = CARTESIAN_POINT ( 'NONE',  ( 4.458734124999999437, -45.06249999863440081, -5.460374474430324690E-16 ) ) ;
#48522 = CARTESIAN_POINT ( 'NONE',  ( 0.000000000000000000, -170.0000000000000000, 5.000000000000000000 ) ) ;
#48523 = CARTESIAN_POINT ( 'NONE',  ( -4.458734124999999437, 0.6041666680322611560, -2.574251347313719407 ) ) ;
#48524 = ORIENTED_EDGE ( 'NONE', *, *, #35811, .F. ) ;
#48525 = CARTESIAN_POINT ( 'NONE',  ( 2.229367062500001939, -27.22916666530106866, 3.861377020970579999 ) ) ;
#48526 =( BOUNDED_CURVE ( )  B_SPLINE_CURVE ( 2, ( #21681, #31306, #22310, #62183, #3017, #22632, #2381, #7833, #42231 ),
 .UNSPECIFIED., .F., .F. ) 
 B_SPLINE_CURVE_WITH_KNOTS ( ( 3, 2, 2, 2, 3 ),
 ( 0.5196428571428571841, 0.5202380952380952772, 0.5214285714285714635, 0.5226190476190476497, 0.5232142857142857428 ),
 .UNSPECIFIED. ) 
 CURVE ( )  GEOMETRIC_REPRESENTATION_ITEM ( )  RATIONAL_B_SPLINE_CURVE ( ( 0.9330127018922194093, 0.9330127018922194093, 1.000000000000000000, 0.8660254037844387076, 1.000000000000000000, 0.8660254037844387076, 1.000000000000000000, 0.9330127018922194093, 0.9330127018922194093 ) ) 
 REPRESENTATION_ITEM ( '' )  );
#48527 = CARTESIAN_POINT ( 'NONE',  ( -3.152801135295367985, -156.8125000013656063, 3.152801135295367096 ) ) ;
#48528 = CARTESIAN_POINT ( 'NONE',  ( -4.458734124999999437, -71.31249999863439371, 0.000000000000000000 ) ) ;
#48529 = CARTESIAN_POINT ( 'NONE',  ( -2.499999999999996447, -107.7083333306021444, 4.330127018922195425 ) ) ;
#48530 = CARTESIAN_POINT ( 'NONE',  ( 4.458734125000001214, 23.10416666803225993, 2.574251347313718519 ) ) ;
#48531 = EDGE_CURVE ( 'NONE', #31783, #47937, #5957, .T. ) ;
#48532 = CYLINDRICAL_SURFACE ( 'NONE', #34891, 5.000000000000000000 ) ;
#48533 = CARTESIAN_POINT ( 'NONE',  ( -2.229367062500000163, -107.7291666653010651, -3.861377020970580443 ) ) ;
#48534 = CARTESIAN_POINT ( 'NONE',  ( -4.458734124999999437, -73.56249999863439371, 0.000000000000000000 ) ) ;
#48535 = CARTESIAN_POINT ( 'NONE',  ( -3.535250795749689387E-16, -54.24999999999999289, -5.773502691896257311 ) ) ;
#48536 = CARTESIAN_POINT ( 'NONE',  ( -2.500000000000000444, -66.16666666666667140, -4.330127018922193649 ) ) ;
#48537 = CARTESIAN_POINT ( 'NONE',  ( -5.000000000000000000, 29.12500000273118417, 0.000000000000000000 ) ) ;
#48538 = ORIENTED_EDGE ( 'NONE', *, *, #45606, .T. ) ;
#48539 = CARTESIAN_POINT ( 'NONE',  ( -3.535533905932737309, -140.6250000000000000, -3.535533905932738197 ) ) ;
#48540 = DIRECTION ( 'NONE',  ( 0.000000000000000000, 1.000000000000000000, 0.000000000000000000 ) ) ;
#48541 = CARTESIAN_POINT ( 'NONE',  ( 5.000000000000000000, -13.49999999999999822, -6.123233995736766282E-16 ) ) ;
#48542 = CARTESIAN_POINT ( 'NONE',  ( -2.229367062500000163, -16.47916666530107577, -3.861377020970580443 ) ) ;
#48543 = CARTESIAN_POINT ( 'NONE',  ( 4.458734124999999437, -78.81249999863440792, -5.460374474430324690E-16 ) ) ;
#48544 = CARTESIAN_POINT ( 'NONE',  ( 1.846868145590735200, -169.5000000013655495, -4.458734125000000326 ) ) ;
#48545 = CARTESIAN_POINT ( 'NONE',  ( -5.000000000000000000, -20.87499999726881228, 0.000000000000000000 ) ) ;
#48547 = ORIENTED_EDGE ( 'NONE', *, *, #38231, .F. ) ;
#48546 = CARTESIAN_POINT ( 'NONE',  ( -3.152548672688508926E-16, -49.56249999863440792, -5.148502694627439702 ) ) ;
#48548 = CARTESIAN_POINT ( 'NONE',  ( 1.339745962155615144, -98.70534180126146850, 4.999999999999999112 ) ) ;
#48550 = ORIENTED_EDGE ( 'NONE', *, *, #33124, .T. ) ;
#48549 = CARTESIAN_POINT ( 'NONE',  ( -4.458734124999999437, 3.354166668032260823, -2.574251347313719407 ) ) ;
#48551 = CARTESIAN_POINT ( 'NONE',  ( -54.64476657466781973, -152.8125000013656063, -4.444560631937228834 ) ) ;
#48552 = CARTESIAN_POINT ( 'NONE',  ( 5.000000000000000000, -61.41666666666665719, -2.886751345948129988 ) ) ;
#48553 = CARTESIAN_POINT ( 'NONE',  ( -1.846868145590737420, -155.0000000013656063, 4.458734124999999437 ) ) ;
#48554 = CARTESIAN_POINT ( 'NONE',  ( 4.458734124999998549, -39.97916666530107221, -2.574251347313721627 ) ) ;
#48555 = CARTESIAN_POINT ( 'NONE',  ( 55.00000000000002132, 15.00000000000000000, 5.000000000000000000 ) ) ;
#48556 = CARTESIAN_POINT ( 'NONE',  ( -2.071067811865478170, -163.3125000000000000, 5.000000000000000000 ) ) ;
#48557 = CARTESIAN_POINT ( 'NONE',  ( 3.535533905932738197, -167.8750000000000284, -3.535533905932738197 ) ) ;
#48558 = CARTESIAN_POINT ( 'NONE',  ( -50.55543936806279248, -125.3125000013655921, 0.3552334253322060320 ) ) ;
#48559 = CARTESIAN_POINT ( 'NONE',  ( -4.458734124999999437, -4.645833331967739177, -2.574251347313719407 ) ) ;
#48560 = CARTESIAN_POINT ( 'NONE',  ( 4.458734125000001214, -48.14583333196773651, 2.574251347313718519 ) ) ;
#48561 = VECTOR ( 'NONE', #11261, 1000.000000000000000 ) ;
#48562 = LINE ( 'NONE', #4502, #4916 ) ;
#48563 = CARTESIAN_POINT ( 'NONE',  ( -3.152801135295367985, -147.8125000013655779, 3.152801135295367096 ) ) ;
#48564 = CARTESIAN_POINT ( 'NONE',  ( -3.152548672688508926E-16, -91.81249999863442213, -5.148502694627439702 ) ) ;
#48565 = LINE ( 'NONE', #13541, #54363 ) ;
#48566 = ORIENTED_EDGE ( 'NONE', *, *, #5618, .T. ) ;
#48567 = CARTESIAN_POINT ( 'NONE',  ( -6.972266317189433020E-16, -47.24999999999999289, -5.000000000000000000 ) ) ;
#48568 = CYLINDRICAL_SURFACE ( 'NONE', #58040, 5.000000000000000000 ) ;
#48569 = CARTESIAN_POINT ( 'NONE',  ( -51.75738570946856498, -151.8750000027312126, 3.805975901505576964 ) ) ;
#48570 = DIRECTION ( 'NONE',  ( -0.000000000000000000, 1.000000000000000000, -0.000000000000000000 ) ) ;
#48571 = ORIENTED_EDGE ( 'NONE', *, *, #37065, .F. ) ;
#48572 = CARTESIAN_POINT ( 'NONE',  ( 2.500000000000002220, -78.66666666666665719, 4.330127018922192761 ) ) ;
#48573 = CARTESIAN_POINT ( 'NONE',  ( -2.229367062500000163, -11.72916666530107044, -3.861377020970580443 ) ) ;
#48574 = CARTESIAN_POINT ( 'NONE',  ( -6.972266317189433020E-16, 22.74999999999999645, -5.000000000000000000 ) ) ;
#48575 = CARTESIAN_POINT ( 'NONE',  ( 9.457646018065525792E-16, -1.062499998634405696, 5.148502694627439702 ) ) ;
#48576 = CARTESIAN_POINT ( 'NONE',  ( 0.000000000000000000, -170.0000000000000000, 0.000000000000000000 ) ) ;
#48577 = CARTESIAN_POINT ( 'NONE',  ( 4.458734124999997661, -152.5000000013656347, 1.846868145590737864 ) ) ;
#48578 = CARTESIAN_POINT ( 'NONE',  ( 2.229367062500001939, 19.77083333469892779, 3.861377020970579999 ) ) ;
#48579 = ORIENTED_EDGE ( 'NONE', *, *, #26460, .T. ) ;
#48580 = CARTESIAN_POINT ( 'NONE',  ( 2.229367062499998831, -90.64583333196773651, -3.861377020970580887 ) ) ;
#48581 = CARTESIAN_POINT ( 'NONE',  ( -2.500000000000000444, -47.16666666666666430, -4.330127018922193649 ) ) ;
#48582 = CARTESIAN_POINT ( 'NONE',  ( 5.000000000000000000, -40.49999999999999289, -6.123233995736766282E-16 ) ) ;
#48583 = CARTESIAN_POINT ( 'NONE',  ( -2.229367062500000163, -14.47916666530107221, -3.861377020970580443 ) ) ;
#48584 = CARTESIAN_POINT ( 'NONE',  ( 2.500000000000002220, -39.54166666393548013, 4.330127018922192761 ) ) ;
#48585 = CARTESIAN_POINT ( 'NONE',  ( -6.972266317189433020E-16, -13.25000000000000000, -5.000000000000000000 ) ) ;
#48586 = CARTESIAN_POINT ( 'NONE',  ( -62.00000000000001421, -135.0000000000000284, -4.041451884327373456 ) ) ;
#48587 = CARTESIAN_POINT ( 'NONE',  ( -5.000000000000000000, -38.95833333060214443, -2.886751345948128211 ) ) ;
#48588 = CARTESIAN_POINT ( 'NONE',  ( -51.75738570946856498, -147.8750000027312126, 3.805975901505576964 ) ) ;
#48589 = CARTESIAN_POINT ( 'NONE',  ( -4.458734124999997661, 20.77083333469892779, 2.574251347313722516 ) ) ;
#48590 = CARTESIAN_POINT ( 'NONE',  ( -6.972266317189433020E-16, -51.12499999726880873, -5.000000000000000000 ) ) ;
#48591 = ORIENTED_EDGE ( 'NONE', *, *, #49593, .T. ) ;
#48592 = CARTESIAN_POINT ( 'NONE',  ( 2.229367062500001939, 19.02083333469892779, 3.861377020970579999 ) ) ;
#48593 = CARTESIAN_POINT ( 'NONE',  ( -3.152548672688508926E-16, -64.56249999863440792, -5.148502694627439702 ) ) ;
#48594 = CARTESIAN_POINT ( 'NONE',  ( 2.229367062500001939, -9.229166665301075767, 3.861377020970579999 ) ) ;
#48595 = CARTESIAN_POINT ( 'NONE',  ( -1.339745962155610925, -33.66965819600732601, 5.000000000000000000 ) ) ;
#48596 = CARTESIAN_POINT ( 'NONE',  ( 5.000000000000000000, 9.583333333333333925, -2.886751345948129988 ) ) ;
#48597 = CARTESIAN_POINT ( 'NONE',  ( 3.152801135295367541, -167.3125000013656063, -3.152801135295367541 ) ) ;
#48598 = CARTESIAN_POINT ( 'NONE',  ( 2.499999999999998668, -88.33333333333332860, -4.330127018922193649 ) ) ;
#48599 = CARTESIAN_POINT ( 'NONE',  ( 2.229367062499998831, -52.64583333196773651, -3.861377020970580887 ) ) ;
#48600 = CARTESIAN_POINT ( 'NONE',  ( 2.499999999999998668, -89.20833333060214443, -4.330127018922193649 ) ) ;
#48601 = CARTESIAN_POINT ( 'NONE',  ( -54.64476657466781973, -132.0625000013656063, -4.444560631937228834 ) ) ;
#48602 =( BOUNDED_CURVE ( )  B_SPLINE_CURVE ( 2, ( #50735, #60720, #40757, #50428, #2192, #31420, #60406, #51059, #11498 ),
 .UNSPECIFIED., .F., .F. ) 
 B_SPLINE_CURVE_WITH_KNOTS ( ( 3, 2, 2, 2, 3 ),
 ( 0.7232142857142856984, 0.7238095238095237915, 0.7249999999999999778, 0.7261904761904761640, 0.7267857142857142572 ),
 .UNSPECIFIED. ) 
 CURVE ( )  GEOMETRIC_REPRESENTATION_ITEM ( )  RATIONAL_B_SPLINE_CURVE ( ( 0.9330127018922194093, 0.9330127018922194093, 1.000000000000000000, 0.8660254037844387076, 1.000000000000000000, 0.8660254037844387076, 1.000000000000000000, 0.9330127018922194093, 0.9330127018922194093 ) ) 
 REPRESENTATION_ITEM ( '' )  );
#48603 = DIRECTION ( 'NONE',  ( 0.000000000000000000, 1.000000000000000000, 0.000000000000000000 ) ) ;
#48604 = CARTESIAN_POINT ( 'NONE',  ( -51.75738570946856498, -152.8750000027312126, 3.805975901505576964 ) ) ;
#48605 = CARTESIAN_POINT ( 'NONE',  ( 4.458734124999998549, -89.97916666530106511, -2.574251347313721627 ) ) ;
#48606 = CARTESIAN_POINT ( 'NONE',  ( -4.458734125000000326, -153.1250000013656063, 1.846868145590734089 ) ) ;
#48607 = CARTESIAN_POINT ( 'NONE',  ( -2.499999999999996447, -35.83333333333332860, 4.330127018922195425 ) ) ;
#48608 = CARTESIAN_POINT ( 'NONE',  ( 1.975475456537005874E-15, 19.25000000000000000, 5.000000000000000000 ) ) ;
#48609 = CARTESIAN_POINT ( 'NONE',  ( 1.339745962155615144, -22.70534180126147916, 4.999999999999999112 ) ) ;
#48610 = ORIENTED_EDGE ( 'NONE', *, *, #9504, .F. ) ;
#48611 = CARTESIAN_POINT ( 'NONE',  ( -2.229367062500000163, -102.4791666653010651, -3.861377020970580443 ) ) ;
#48612 = CARTESIAN_POINT ( 'NONE',  ( 2.229367062499998831, 8.104166668032261711, -3.861377020970580887 ) ) ;
#48613 = CARTESIAN_POINT ( 'NONE',  ( 5.000000000000000000, 12.58333333333333215, -2.886751345948130876 ) ) ;
#48614 = CARTESIAN_POINT ( 'NONE',  ( 5.000000000000000000, 5.583333333333332149, -2.886751345948129988 ) ) ;
#48615 = CARTESIAN_POINT ( 'NONE',  ( -2.229367062500000163, -62.47916666530106511, -3.861377020970580443 ) ) ;
#48616 = CARTESIAN_POINT ( 'NONE',  ( -2.499999999999996447, 20.16666666666666430, 4.330127018922195425 ) ) ;
#48617 = CARTESIAN_POINT ( 'NONE',  ( -2.499999999999996447, -2.708333330602146649, 4.330127018922195425 ) ) ;
#48619 = ORIENTED_EDGE ( 'NONE', *, *, #27461, .F. ) ;
#48618 = CARTESIAN_POINT ( 'NONE',  ( -2.229367062499996610, -28.14583333196774007, 3.861377020970582219 ) ) ;
#48620 = CARTESIAN_POINT ( 'NONE',  ( 2.071067811865264563, -152.9375000027311842, -5.000000000000211386 ) ) ;
#48621 = CARTESIAN_POINT ( 'NONE',  ( 2.500000000000002220, 19.33333333333333570, 4.330127018922192761 ) ) ;
#48622 = CARTESIAN_POINT ( 'NONE',  ( -50.18089887299980489, -136.6875000000000568, 2.462841084822814164 ) ) ;
#48623 = CARTESIAN_POINT ( 'NONE',  ( -2.500000000000000444, -47.16666666666666430, -4.330127018922193649 ) ) ;
#48625 = CARTESIAN_POINT ( 'NONE',  ( -3.152548672688508926E-16, -25.81249999863440792, -5.148502694627439702 ) ) ;
#48624 = LINE ( 'NONE', #24187, #20298 ) ;
#48626 = CARTESIAN_POINT ( 'NONE',  ( -6.972266317189433020E-16, -58.24999999999999289, -5.000000000000000000 ) ) ;
#48627 = CARTESIAN_POINT ( 'NONE',  ( -4.458734124999998549, -72.22916666530107932, 2.574251347313722516 ) ) ;
#48628 = CARTESIAN_POINT ( 'NONE',  ( -4.458734124999999437, -145.1875000013656063, -5.460374474430324690E-16 ) ) ;
#48630 = EDGE_CURVE ( 'NONE', #57060, #46199, #9454, .T. ) ;
#48629 = CARTESIAN_POINT ( 'NONE',  ( 4.458734125000001214, -78.89583333196772230, 2.574251347313718519 ) ) ;
#48631 = CARTESIAN_POINT ( 'NONE',  ( -52.10840900171896806, -139.4375000013656063, 3.393966926194110556 ) ) ;
#48632 = CARTESIAN_POINT ( 'NONE',  ( 2.229367062499998831, -24.89583333196773651, -3.861377020970580887 ) ) ;
#48633 = CARTESIAN_POINT ( 'NONE',  ( 1.060575238724906964E-15, -67.62499999726881583, 5.773502691896257311 ) ) ;
#48634 = ORIENTED_EDGE ( 'NONE', *, *, #10669, .T. ) ;
#48635 = CARTESIAN_POINT ( 'NONE',  ( -5.000000000000000888, -152.6875000027312126, -2.071067811865475949 ) ) ;
#48636 = ORIENTED_EDGE ( 'NONE', *, *, #51902, .T. ) ;
#48637 = CARTESIAN_POINT ( 'NONE',  ( -2.229367062499996610, -73.39583333196773651, 3.861377020970582219 ) ) ;
#48638 = CARTESIAN_POINT ( 'NONE',  ( -6.972266317189433020E-16, 7.875000002731185056, -5.000000000000000000 ) ) ;
#48639 = ORIENTED_EDGE ( 'NONE', *, *, #32028, .F. ) ;
#48640 = CARTESIAN_POINT ( 'NONE',  ( 2.499999999999998668, 27.66666666666666430, -4.330127018922193649 ) ) ;
#48641 = DIRECTION ( 'NONE',  ( 0.000000000000000000, 0.000000000000000000, 1.000000000000000000 ) ) ;
#48642 = CARTESIAN_POINT ( 'NONE',  ( -4.458734124999999437, -57.56249999863440081, 0.000000000000000000 ) ) ;
#48643 = CARTESIAN_POINT ( 'NONE',  ( 9.457646018065525792E-16, 0.6875000013655957476, 5.148502694627439702 ) ) ;
#48644 = ORIENTED_EDGE ( 'NONE', *, *, #31908, .F. ) ;
#48645 = ADVANCED_FACE ( 'NONE', ( #6280 ), #45502, .T. ) ;
#48646 = CARTESIAN_POINT ( 'NONE',  ( -2.500000000000000444, -23.04166666393548013, -4.330127018922193649 ) ) ;
#48647 = CARTESIAN_POINT ( 'NONE',  ( -2.229367062499996610, 10.85416666803225993, 3.861377020970582219 ) ) ;
#48648 = CARTESIAN_POINT ( 'NONE',  ( -54.64476657466781973, -146.8125000013656063, -4.444560631937228834 ) ) ;
#48649 = DIRECTION ( 'NONE',  ( -0.000000000000000000, 1.000000000000000000, -0.000000000000000000 ) ) ;
#48650 = CARTESIAN_POINT ( 'NONE',  ( 1.846868145590736310, -165.6250000013656063, 4.458734124999997661 ) ) ;
#48651 = ORIENTED_EDGE ( 'NONE', *, *, #36943, .T. ) ;
#48652 = CARTESIAN_POINT ( 'NONE',  ( -2.229367062499996610, -76.14583333196773651, 3.861377020970582219 ) ) ;
#48653 = CARTESIAN_POINT ( 'NONE',  ( 1.339745962155615144, -0.5803417985302927740, 4.999999999999999112 ) ) ;
#48654 = CARTESIAN_POINT ( 'NONE',  ( -4.458734124999998549, -0.2291666653010705768, 2.574251347313722516 ) ) ;
#48655 = AXIS2_PLACEMENT_3D ( 'NONE', #17275, #36899, #12450 ) ;
#48656 = CARTESIAN_POINT ( 'NONE',  ( 1.339745962155612702, 4.830341803992664218, -5.000000000000000000 ) ) ;
#48657 = CARTESIAN_POINT ( 'NONE',  ( 4.458734124999998549, -63.97916666530107221, -2.574251347313721627 ) ) ;
#48658 = CARTESIAN_POINT ( 'NONE',  ( -4.999999999999999112, -26.79166666393548013, 2.886751345948131764 ) ) ;
#48659 = CARTESIAN_POINT ( 'NONE',  ( -6.972266317189433020E-16, -20.24999999999999289, -5.000000000000000000 ) ) ;
#48660 = CYLINDRICAL_SURFACE ( 'NONE', #37797, 5.000000000000000000 ) ;
#48661 = CARTESIAN_POINT ( 'NONE',  ( 5.000000000000000888, -18.45833333060214798, 2.886751345948126879 ) ) ;
#48662 = DIRECTION ( 'NONE',  ( -0.000000000000000000, 1.000000000000000000, -0.000000000000000000 ) ) ;
#48663 = CARTESIAN_POINT ( 'NONE',  ( -4.458734124999999437, -45.39583333196773651, -2.574251347313719407 ) ) ;
#48664 = CARTESIAN_POINT ( 'NONE',  ( -4.458734124999999437, -27.64583333196774007, -2.574251347313719407 ) ) ;
#48665 = CARTESIAN_POINT ( 'NONE',  ( -2.229367062500000163, 8.270833334698926009, -3.861377020970580443 ) ) ;
#48666 =( BOUNDED_CURVE ( )  B_SPLINE_CURVE ( 2, ( #59458, #15390, #30163, #5738, #34683, #54303, #10244, #45290, #25356 ),
 .UNSPECIFIED., .F., .F. ) 
 B_SPLINE_CURVE_WITH_KNOTS ( ( 3, 2, 2, 2, 3 ),
 ( 0.3232142857142857317, 0.3238095238095238249, 0.3250000000000000111, 0.3261904761904761973, 0.3267857142857142905 ),
 .UNSPECIFIED. ) 
 CURVE ( )  GEOMETRIC_REPRESENTATION_ITEM ( )  RATIONAL_B_SPLINE_CURVE ( ( 0.9330127018922194093, 0.9330127018922194093, 1.000000000000000000, 0.8660254037844387076, 1.000000000000000000, 0.8660254037844387076, 1.000000000000000000, 0.9330127018922194093, 0.9330127018922194093 ) ) 
 REPRESENTATION_ITEM ( '' )  );
#48667 = CARTESIAN_POINT ( 'NONE',  ( -53.33387254593710480, -139.9375000027311557, 5.149110718188539160 ) ) ;
#48668 = CARTESIAN_POINT ( 'NONE',  ( 5.000000000000000888, 28.41666666666666430, 2.886751345948126879 ) ) ;
#48669 = CARTESIAN_POINT ( 'NONE',  ( -5.000000000000000888, -150.5625000027311842, 2.071067811865474617 ) ) ;
#48670 = CARTESIAN_POINT ( 'NONE',  ( -52.53715891517739323, -154.4375000000000000, -4.819101127000233298 ) ) ;
#48671 = CARTESIAN_POINT ( 'NONE',  ( 2.229367062500001939, -34.97916666530107221, 3.861377020970579999 ) ) ;
#48672 = CARTESIAN_POINT ( 'NONE',  ( 5.000000000000000888, -67.45833333060213022, 2.886751345948126879 ) ) ;
#48673 = CARTESIAN_POINT ( 'NONE',  ( -52.80376928212989185, -147.1250000013656063, -4.297418129356379346 ) ) ;
#48674 = CARTESIAN_POINT ( 'NONE',  ( -9.184850993605147944E-16, -144.2500000000000284, 5.000000000000000000 ) ) ;
#48675 = CARTESIAN_POINT ( 'NONE',  ( -2.229367062499996610, -76.39583333196773651, 3.861377020970582219 ) ) ;
#48676 = CARTESIAN_POINT ( 'NONE',  ( -8.190561711645485556E-16, -164.9375000013655779, 4.458734124999999437 ) ) ;
#48677 = CARTESIAN_POINT ( 'NONE',  ( -4.458734124999997661, -31.22916666530106866, 2.574251347313722516 ) ) ;
#48678 = DIRECTION ( 'NONE',  ( 0.000000000000000000, 0.000000000000000000, 1.000000000000000000 ) ) ;
#48679 = FACE_OUTER_BOUND ( 'NONE', #2124, .T. ) ;
#48680 = CARTESIAN_POINT ( 'NONE',  ( 1.060575238724906964E-15, -22.75000000000000000, 5.773502691896257311 ) ) ;
#48681 = CARTESIAN_POINT ( 'NONE',  ( -3.152801135295367096, -145.0625000013655779, -3.152801135295367541 ) ) ;
#48682 = ORIENTED_EDGE ( 'NONE', *, *, #27618, .F. ) ;
#48683 = CARTESIAN_POINT ( 'NONE',  ( 5.000000000000000000, -90.37499999726880162, -6.123233995736766282E-16 ) ) ;
#48684 = CARTESIAN_POINT ( 'NONE',  ( 1.975475456537005874E-15, 0.2500000000000001665, 5.000000000000000000 ) ) ;
#48685 = CARTESIAN_POINT ( 'NONE',  ( -3.152548672688508926E-16, -56.81249999863440792, -5.148502694627439702 ) ) ;
#48686 = CARTESIAN_POINT ( 'NONE',  ( 5.000000000000000000, 26.70833333606451632, -2.886751345948129988 ) ) ;
#48687 = CARTESIAN_POINT ( 'NONE',  ( 0.000000000000000000, -170.0000000000000000, 5.000000000000000000 ) ) ;
#48688 = CARTESIAN_POINT ( 'NONE',  ( 5.000000000000000888, 21.41666666666666430, 2.886751345948126879 ) ) ;
#48689 = APPLICATION_CONTEXT ( 'automotive_design' ) ;
#48690 = CARTESIAN_POINT ( 'NONE',  ( -2.499999999999996447, 8.291666669397852019, 4.330127018922195425 ) ) ;
#48691 = CARTESIAN_POINT ( 'NONE',  ( -2.229367062500000163, -5.479166665301072214, -3.861377020970580443 ) ) ;
#48692 = LINE ( 'NONE', #15243, #53389 ) ;
#48693 = CARTESIAN_POINT ( 'NONE',  ( 0.000000000000000000, -170.0000000000000000, 0.000000000000000000 ) ) ;
#48694 = CARTESIAN_POINT ( 'NONE',  ( 2.499999999999998668, -89.20833333060214443, -4.330127018922193649 ) ) ;
#48695 = CARTESIAN_POINT ( 'NONE',  ( -6.972266317189433020E-16, -88.12499999726880162, -5.000000000000000000 ) ) ;
#48696 =( BOUNDED_CURVE ( )  B_SPLINE_CURVE ( 2, ( #4591, #24214, #43820, #47404, #3355, #22972, #42572, #28095, #3668 ),
 .UNSPECIFIED., .F., .F. ) 
 B_SPLINE_CURVE_WITH_KNOTS ( ( 3, 2, 2, 2, 3 ),
 ( 0.1625000000000000056, 0.1630952380952380987, 0.1642857142857142849, 0.1654761904761904712, 0.1660714285714285643 ),
 .UNSPECIFIED. ) 
 CURVE ( )  GEOMETRIC_REPRESENTATION_ITEM ( )  RATIONAL_B_SPLINE_CURVE ( ( 0.9330127018922194093, 0.9330127018922194093, 1.000000000000000000, 0.8660254037844387076, 1.000000000000000000, 0.8660254037844387076, 1.000000000000000000, 0.9330127018922194093, 0.9330127018922194093 ) ) 
 REPRESENTATION_ITEM ( '' )  );
#48697 = CARTESIAN_POINT ( 'NONE',  ( 2.229367062499998831, -22.64583333196773651, -3.861377020970580887 ) ) ;
#48698 = CARTESIAN_POINT ( 'NONE',  ( -5.000000000000000000, -71.95833333060214443, -2.886751345948128211 ) ) ;
#48699 = CARTESIAN_POINT ( 'NONE',  ( -4.458734124999999437, -55.39583333196773651, -2.574251347313719407 ) ) ;
#48700 = CARTESIAN_POINT ( 'NONE',  ( 4.458734124999999437, -154.6875000013656063, 0.000000000000000000 ) ) ;
#48701 = ADVANCED_FACE ( 'NONE', ( #28413 ), #27784, .T. ) ;
#48702 = AXIS2_PLACEMENT_3D ( 'NONE', #1993, #20964, #41192 ) ;
#48703 = CARTESIAN_POINT ( 'NONE',  ( -2.499999999999996447, -48.70833333060213732, 4.330127018922195425 ) ) ;
#48704 = ORIENTED_EDGE ( 'NONE', *, *, #28849, .T. ) ;
#48705 = CARTESIAN_POINT ( 'NONE',  ( -3.152548672688508926E-16, 4.187500001365595637, -5.148502694627439702 ) ) ;
#48706 = VERTEX_POINT ( 'NONE', #3359 ) ;
#48708 = CARTESIAN_POINT ( 'NONE',  ( 1.339745962155615144, -9.580341798530296771, 4.999999999999999112 ) ) ;
#48707 = DIRECTION ( 'NONE',  ( 0.000000000000000000, 0.000000000000000000, 1.000000000000000000 ) ) ;
#48709 = CARTESIAN_POINT ( 'NONE',  ( -3.152801135295367985, -161.8125000013656063, 3.152801135295367096 ) ) ;
#48710 = VERTEX_POINT ( 'NONE', #3983 ) ;
#48711 = UNCERTAINTY_MEASURE_WITH_UNIT (LENGTH_MEASURE( 1.000000000000000082E-05 ), #61097, 'distance_accuracy_value', 'NONE');
#48712 = EDGE_CURVE ( 'NONE', #26939, #58774, #59511, .T. ) ;
#48713 = CARTESIAN_POINT ( 'NONE',  ( 0.000000000000000000, -170.0000000000000000, 5.000000000000000000 ) ) ;
#48714 = CARTESIAN_POINT ( 'NONE',  ( -58.80597590150559739, -134.0000000000000284, 3.242614290531460330 ) ) ;
#48715 = CARTESIAN_POINT ( 'NONE',  ( -4.458734124999998549, -45.47916666530105800, 2.574251347313722516 ) ) ;
#48716 = ORIENTED_EDGE ( 'NONE', *, *, #46767, .T. ) ;
#48717 = CARTESIAN_POINT ( 'NONE',  ( -9.184850993605147944E-16, -143.3750000027312126, 5.000000000000000000 ) ) ;
#48718 = EDGE_CURVE ( 'NONE', #18754, #45557, #16040, .T. ) ;
#48719 = CARTESIAN_POINT ( 'NONE',  ( 4.458734125000001214, 20.10416666803225993, 2.574251347313718519 ) ) ;
#48720 = ORIENTED_EDGE ( 'NONE', *, *, #27801, .F. ) ;
#48721 = EDGE_CURVE ( 'NONE', #13464, #25378, #5328, .T. ) ;
#48722 = CARTESIAN_POINT ( 'NONE',  ( -2.229367062500000163, -88.72916666530106511, -3.861377020970580443 ) ) ;
#48723 = CARTESIAN_POINT ( 'NONE',  ( -55.39835681537999790, -126.0000000027311984, 4.984105922594378235 ) ) ;
#48724 = CARTESIAN_POINT ( 'NONE',  ( -53.31921341345466203, -135.0000000000000000, 4.586462452526608224 ) ) ;
#48725 = CARTESIAN_POINT ( 'NONE',  ( -6.972266317189433020E-16, 8.750000000000000000, -5.000000000000000000 ) ) ;
#48726 = CARTESIAN_POINT ( 'NONE',  ( 4.458734124999999437, -57.81249999863440081, -5.460374474430324690E-16 ) ) ;
#48727 = CARTESIAN_POINT ( 'NONE',  ( 4.458734124999998549, 17.27083333469892779, -2.574251347313721627 ) ) ;
#48728 = CARTESIAN_POINT ( 'NONE',  ( 6.123233995736766282E-16, -170.0000000000000000, -5.000000000000000000 ) ) ;
#48729 = CARTESIAN_POINT ( 'NONE',  ( 4.458734124999998549, -49.97916666530106511, -2.574251347313721627 ) ) ;
#48730 = CARTESIAN_POINT ( 'NONE',  ( 5.000000000000000888, -8.458333330602146205, 2.886751345948126879 ) ) ;
#48731 = CARTESIAN_POINT ( 'NONE',  ( 1.975475456537005874E-15, -80.62499999726881583, 5.000000000000000000 ) ) ;
#48732 = CARTESIAN_POINT ( 'NONE',  ( -2.500000000000000444, -46.04166666393547303, -4.330127018922193649 ) ) ;
#48733 = CARTESIAN_POINT ( 'NONE',  ( -4.458734124999998549, -86.47916666530107932, 2.574251347313722516 ) ) ;
#48734 = CARTESIAN_POINT ( 'NONE',  ( 4.458734124999998549, -105.7291666653010651, -2.574251347313721627 ) ) ;
#48735 = CARTESIAN_POINT ( 'NONE',  ( -4.458734124999999437, -13.56249999863440259, 0.000000000000000000 ) ) ;
#48736 = ORIENTED_EDGE ( 'NONE', *, *, #14608, .T. ) ;
#48737 = CARTESIAN_POINT ( 'NONE',  ( -4.458734124999999437, -99.31249999863440792, 0.000000000000000000 ) ) ;
#48738 = CARTESIAN_POINT ( 'NONE',  ( 5.000000000000000888, -162.0625000027312126, -2.071067811865475505 ) ) ;
#48739 = CARTESIAN_POINT ( 'NONE',  ( 4.458734125000001214, -95.14583333196772230, 2.574251347313718519 ) ) ;
#48740 = EDGE_CURVE ( 'NONE', #8603, #15531, #51923, .T. ) ;
#48741 = CARTESIAN_POINT ( 'NONE',  ( -2.500000000000000444, -8.166666666666669627, -4.330127018922193649 ) ) ;
#48742 = CARTESIAN_POINT ( 'NONE',  ( -4.999999999999999112, -50.79166666393547303, 2.886751345948131764 ) ) ;
#48743 = CARTESIAN_POINT ( 'NONE',  ( 1.975475456537005874E-15, -36.62499999726880873, 5.000000000000000000 ) ) ;
#48744 = VECTOR ( 'NONE', #56501, 1000.000000000000000 ) ;
#48745 = CARTESIAN_POINT ( 'NONE',  ( -59.59170313451811296, -128.5000000013656063, 1.485763867205729394 ) ) ;
#48746 = CARTESIAN_POINT ( 'NONE',  ( -54.64476657466781973, -144.8125000013656063, -4.444560631937228834 ) ) ;
#48747 = CARTESIAN_POINT ( 'NONE',  ( -4.458734124999999437, -20.31249999863440081, 0.000000000000000000 ) ) ;
#48748 = CARTESIAN_POINT ( 'NONE',  ( -4.458734124999999437, 13.35416666803225993, -2.574251347313719407 ) ) ;
#48749 = CARTESIAN_POINT ( 'NONE',  ( -3.152548672688508926E-16, -59.81249999863440792, -5.148502694627439702 ) ) ;
#48750 = CARTESIAN_POINT ( 'NONE',  ( 55.00000000000002132, 15.00000000000000000, 5.000000000000000000 ) ) ;
#48751 = CARTESIAN_POINT ( 'NONE',  ( 4.458734124999998549, -14.72916666530107221, -2.574251347313721627 ) ) ;
#48752 = DIRECTION ( 'NONE',  ( -0.000000000000000000, 1.000000000000000000, -0.000000000000000000 ) ) ;
#48753 = CARTESIAN_POINT ( 'NONE',  ( -3.535533905932737309, -155.6250000000000000, -3.535533905932738197 ) ) ;
#48754 = CARTESIAN_POINT ( 'NONE',  ( 5.000000000000000000, -5.416666666666666963, -2.886751345948129988 ) ) ;
#48755 = VERTEX_POINT ( 'NONE', #7864 ) ;
#48756 = CARTESIAN_POINT ( 'NONE',  ( 4.458734125000000326, -40.14583333196773651, 2.574251347313718519 ) ) ;
#48757 = CARTESIAN_POINT ( 'NONE',  ( 5.000000000000000000, -83.37499999726881583, -6.123233995736766282E-16 ) ) ;
#48758 = CARTESIAN_POINT ( 'NONE',  ( -1.339745962155613812, -92.08034179853028434, -5.000000000000000000 ) ) ;
#48759 = CARTESIAN_POINT ( 'NONE',  ( -2.500000000000000444, -25.16666666666666430, -4.330127018922193649 ) ) ;
#48760 = CARTESIAN_POINT ( 'NONE',  ( -4.458734124999999437, -83.31249999863439371, 0.000000000000000000 ) ) ;
#48761 = CARTESIAN_POINT ( 'NONE',  ( -4.458734124999998549, 21.52083333469893134, 2.574251347313722516 ) ) ;
#48762 = CARTESIAN_POINT ( 'NONE',  ( 2.229367062500001939, 9.020833334698927786, 3.861377020970579999 ) ) ;
#48763 = CARTESIAN_POINT ( 'NONE',  ( 2.500000000000002220, -0.6666666666666660745, 4.330127018922192761 ) ) ;
#48764 = CARTESIAN_POINT ( 'NONE',  ( 1.975475456537005874E-15, -68.74999999999998579, 5.000000000000000000 ) ) ;
#48765 = CARTESIAN_POINT ( 'NONE',  ( 1.339745962155612702, 20.83034180399265978, -5.000000000000000000 ) ) ;
#48766 = CARTESIAN_POINT ( 'NONE',  ( 2.229367062500001939, 20.77083333469892779, 3.861377020970579999 ) ) ;
#48767 = CARTESIAN_POINT ( 'NONE',  ( 5.000000000000000888, -76.58333333333332860, 2.886751345948126879 ) ) ;
#48768 = CARTESIAN_POINT ( 'NONE',  ( 5.000000000000000888, 13.54166666939785202, 2.886751345948126879 ) ) ;
#48769 = ORIENTED_EDGE ( 'NONE', *, *, #25215, .F. ) ;
#48770 = DIRECTION ( 'NONE',  ( 0.000000000000000000, 0.000000000000000000, 1.000000000000000000 ) ) ;
#48771 = EDGE_LOOP ( 'NONE', ( #57938, #16623, #12568, #1000 ) ) ;
#48773 = CARTESIAN_POINT ( 'NONE',  ( -2.499999999999996447, -34.83333333333332860, 4.330127018922195425 ) ) ;
#48772 = DIRECTION ( 'NONE',  ( 0.000000000000000000, 0.000000000000000000, 1.000000000000000000 ) ) ;
#48774 = CARTESIAN_POINT ( 'NONE',  ( -2.229367062499996610, -36.14583333196773651, 3.861377020970582219 ) ) ;
#48775 =( BOUNDED_CURVE ( )  B_SPLINE_CURVE ( 2, ( #56617, #62070, #27952, #62387, #7407, #17983, #17685, #17367, #51468 ),
 .UNSPECIFIED., .F., .F. ) 
 B_SPLINE_CURVE_WITH_KNOTS ( ( 3, 2, 2, 2, 3 ),
 ( 0.8770833333333333259, 0.8777777777777777679, 0.8791666666666666519, 0.8805555555555555358, 0.8812499999999999778 ),
 .UNSPECIFIED. ) 
 CURVE ( )  GEOMETRIC_REPRESENTATION_ITEM ( )  RATIONAL_B_SPLINE_CURVE ( ( 0.9330127018922194093, 0.9330127018922194093, 1.000000000000000000, 0.8660254037844387076, 1.000000000000000000, 0.8660254037844387076, 1.000000000000000000, 0.9330127018922194093, 0.9330127018922194093 ) ) 
 REPRESENTATION_ITEM ( '' )  );
#48776 = EDGE_CURVE ( 'NONE', #27142, #29335, #42577, .T. ) ;
#48777 = CARTESIAN_POINT ( 'NONE',  ( -5.000000000000000000, -32.95833333060215153, -2.886751345948128211 ) ) ;
#48778 = EDGE_CURVE ( 'NONE', #24820, #25740, #18490, .T. ) ;
#48780 = ORIENTED_EDGE ( 'NONE', *, *, #56322, .T. ) ;
#48779 = CARTESIAN_POINT ( 'NONE',  ( -2.229367062500000163, -67.47916666530106511, -3.861377020970580443 ) ) ;
#48781 = CARTESIAN_POINT ( 'NONE',  ( -57.19623071787017210, -152.6250000013656063, 4.297418129356382899 ) ) ;
#48782 = CARTESIAN_POINT ( 'NONE',  ( 4.458734125000001214, -14.89583333196773474, 2.574251347313718519 ) ) ;
#48784 = VERTEX_POINT ( 'NONE', #12367 ) ;
#48783 = CARTESIAN_POINT ( 'NONE',  ( 4.458734124999999437, -12.06249999863440081, -5.460374474430324690E-16 ) ) ;
#48785 = EDGE_CURVE ( 'NONE', #18747, #10208, #59272, .T. ) ;
#48786 = CARTESIAN_POINT ( 'NONE',  ( 1.060575238724906964E-15, -83.75000000000000000, 5.773502691896257311 ) ) ;
#48787 = PLANE ( 'NONE',  #2229 ) ;
#48788 = CARTESIAN_POINT ( 'NONE',  ( 2.229367062499998831, -56.89583333196773651, -3.861377020970580887 ) ) ;
#48789 = CARTESIAN_POINT ( 'NONE',  ( 5.000000000000000888, -84.45833333060214443, 2.886751345948126879 ) ) ;
#48791 = EDGE_LOOP ( 'NONE', ( #33541, #19686, #3172, #57030 ) ) ;
#48790 = FACE_OUTER_BOUND ( 'NONE', #2017, .T. ) ;
#48792 = CARTESIAN_POINT ( 'NONE',  ( -60.14911071818854538, -147.0625000000000000, 1.666127454062681368 ) ) ;
#48793 = CARTESIAN_POINT ( 'NONE',  ( -4.458734124999999437, -25.56249999863440792, 0.000000000000000000 ) ) ;
#48794 = ADVANCED_FACE ( 'NONE', ( #28099 ), #3673, .T. ) ;
#48795 = ORIENTED_EDGE ( 'NONE', *, *, #39709, .T. ) ;
#48796 =( BOUNDED_CURVE ( )  B_SPLINE_CURVE ( 2, ( #16087, #11573, #25742, #35711, #50822, #45356, #55339, #11255, #30880 ),
 .UNSPECIFIED., .F., .F. ) 
 B_SPLINE_CURVE_WITH_KNOTS ( ( 3, 2, 2, 2, 3 ),
 ( 0.3053571428571428825, 0.3059523809523809756, 0.3071428571428571619, 0.3083333333333333481, 0.3089285714285714413 ),
 .UNSPECIFIED. ) 
 CURVE ( )  GEOMETRIC_REPRESENTATION_ITEM ( )  RATIONAL_B_SPLINE_CURVE ( ( 0.9330127018922194093, 0.9330127018922194093, 1.000000000000000000, 0.8660254037844387076, 1.000000000000000000, 0.8660254037844387076, 1.000000000000000000, 0.9330127018922194093, 0.9330127018922194093 ) ) 
 REPRESENTATION_ITEM ( '' )  );
#48797 = CARTESIAN_POINT ( 'NONE',  ( 3.152801135295366208, -165.8125000013656063, 3.152801135295367985 ) ) ;
#48798 = EDGE_CURVE ( 'NONE', #39600, #7768, #28721, .T. ) ;
#48799 = CARTESIAN_POINT ( 'NONE',  ( 4.458734124999999437, -104.0624999986344079, -5.460374474430324690E-16 ) ) ;
#48800 = CARTESIAN_POINT ( 'NONE',  ( -58.24261429053147765, -135.3750000027312410, -3.805975901505573855 ) ) ;
#48801 = ORIENTED_EDGE ( 'NONE', *, *, #54198, .F. ) ;
#48802 = EDGE_CURVE ( 'NONE', #38026, #42718, #48344, .T. ) ;
#48803 = CARTESIAN_POINT ( 'NONE',  ( -57.89159099828107458, -146.9375000013656063, -3.393966926194107447 ) ) ;
#48804 = CARTESIAN_POINT ( 'NONE',  ( -58.24261429053147765, -140.3750000027312126, -3.805975901505573855 ) ) ;
#48805 = CARTESIAN_POINT ( 'NONE',  ( 4.458734124999998549, -38.72916666530106511, -2.574251347313721627 ) ) ;
#48806 = EDGE_CURVE ( 'NONE', #41613, #21757, #25051, .T. ) ;
#48807 = CARTESIAN_POINT ( 'NONE',  ( -4.729367062499999719, -90.71874999795159056, 0.000000000000000000 ) ) ;
#48808 = CARTESIAN_POINT ( 'NONE',  ( 6.158835246850667461E-14, -2.250000000000001776, -4.999999999999999112 ) ) ;
#48809 = CARTESIAN_POINT ( 'NONE',  ( 9.457646018065525792E-16, -11.06249999863440969, 5.148502694627439702 ) ) ;
#48810 = CARTESIAN_POINT ( 'NONE',  ( 4.458734124999998549, -100.9791666653010509, -2.574251347313721627 ) ) ;
#48811 = ORIENTED_EDGE ( 'NONE', *, *, #48449, .F. ) ;
#48812 = CARTESIAN_POINT ( 'NONE',  ( 1.846868145590736310, -144.8750000013655779, 4.458734124999999437 ) ) ;
#48813 = CARTESIAN_POINT ( 'NONE',  ( -3.152548672688508926E-16, -34.81249999863440792, -5.148502694627439702 ) ) ;
#48814 = CARTESIAN_POINT ( 'NONE',  ( -50.01589407740564042, -153.6250000000000284, 0.3983568153799778022 ) ) ;
#48815 = CARTESIAN_POINT ( 'NONE',  ( -52.10840900171896806, -133.1875000013656063, 3.393966926194110556 ) ) ;
#48816 = CARTESIAN_POINT ( 'NONE',  ( -2.229367062499996610, -66.39583333196773651, 3.861377020970582219 ) ) ;
#48817 = CARTESIAN_POINT ( 'NONE',  ( 1.339745962155615144, -17.70534180126147916, 4.999999999999999112 ) ) ;
#48818 = FACE_OUTER_BOUND ( 'NONE', #36945, .T. ) ;
#48819 = CARTESIAN_POINT ( 'NONE',  ( 3.152801135295366208, -139.5625000013655779, 3.152801135295367985 ) ) ;
#48820 = CARTESIAN_POINT ( 'NONE',  ( -4.458734124999999437, 3.354166668032260823, -2.574251347313719407 ) ) ;
#48821 = ORIENTED_EDGE ( 'NONE', *, *, #61491, .T. ) ;
#48822 = CARTESIAN_POINT ( 'NONE',  ( 0.000000000000000000, -170.0000000000000000, 5.000000000000000000 ) ) ;
#48823 = CARTESIAN_POINT ( 'NONE',  ( 2.071067811865582087, -160.1874999999999716, 4.999999999999894307 ) ) ;
#48825 = CARTESIAN_POINT ( 'NONE',  ( 2.229367062500001939, -31.97916666530106866, 3.861377020970579999 ) ) ;
#48824 = CARTESIAN_POINT ( 'NONE',  ( 2.500000000000002220, -96.66666666666665719, 4.330127018922192761 ) ) ;
#48826 = CARTESIAN_POINT ( 'NONE',  ( -5.000000000000000000, -22.87499999726881228, 0.000000000000000000 ) ) ;
#48827 = CARTESIAN_POINT ( 'NONE',  ( 4.458734124999999437, -78.06249999863440792, -5.460374474430324690E-16 ) ) ;
#48828 = CARTESIAN_POINT ( 'NONE',  ( 2.229367062500001939, 22.77083333469892423, 3.861377020970579999 ) ) ;
#48829 = CARTESIAN_POINT ( 'NONE',  ( -1.339745962155614034, 27.20534180126147916, 4.999999999999999112 ) ) ;
#48830 = CARTESIAN_POINT ( 'NONE',  ( -54.64476657466781973, -141.8125000013656063, -4.444560631937228834 ) ) ;
#48831 = CARTESIAN_POINT ( 'NONE',  ( 4.458734124999998549, -4.729166665301071326, -2.574251347313721627 ) ) ;
#48832 = CARTESIAN_POINT ( 'NONE',  ( 4.458734124999999437, 24.93750000136559208, -5.460374474430324690E-16 ) ) ;
#48833 = CARTESIAN_POINT ( 'NONE',  ( -2.229367062499996610, -42.39583333196773651, 3.861377020970582219 ) ) ;
#48834 = CARTESIAN_POINT ( 'NONE',  ( 5.000000000000000000, -43.37499999726880873, -6.123233995736766282E-16 ) ) ;
#48835 = CARTESIAN_POINT ( 'NONE',  ( 4.458734125000000326, 2.104166668032262599, 2.574251347313718519 ) ) ;
#48836 = ORIENTED_EDGE ( 'NONE', *, *, #25660, .F. ) ;
#48837 = CARTESIAN_POINT ( 'NONE',  ( -4.458734124999997661, -25.47916666530106866, 2.574251347313722516 ) ) ;
#48838 = CARTESIAN_POINT ( 'NONE',  ( -2.229367062500000163, -67.47916666530106511, -3.861377020970580443 ) ) ;
#48839 = CARTESIAN_POINT ( 'NONE',  ( -2.500000000000000444, -107.0416666639354730, -4.330127018922193649 ) ) ;
#48840 = AXIS2_PLACEMENT_3D ( 'NONE', #62069, #31836, #12533 ) ;
#48841 = CARTESIAN_POINT ( 'NONE',  ( -4.458734124999999437, 25.68750000136559208, 0.000000000000000000 ) ) ;
#48842 = LINE ( 'NONE', #30500, #8183 ) ;
#48843 = CARTESIAN_POINT ( 'NONE',  ( 1.975475456537005874E-15, -33.75000000000000000, 5.000000000000000000 ) ) ;
#48844 = CARTESIAN_POINT ( 'NONE',  ( -3.152548672688508926E-16, -72.81249999863439371, -5.148502694627439702 ) ) ;
#48845 = CARTESIAN_POINT ( 'NONE',  ( -2.499999999999996447, -54.83333333333332860, 4.330127018922195425 ) ) ;
#48846 = DIRECTION ( 'NONE',  ( 0.000000000000000000, 0.000000000000000000, 1.000000000000000000 ) ) ;
#48847 = CARTESIAN_POINT ( 'NONE',  ( 3.535533905932736864, -156.2500000027312126, 3.535533905932738641 ) ) ;
#48848 = ORIENTED_EDGE ( 'NONE', *, *, #13362, .F. ) ;
#48849 = CARTESIAN_POINT ( 'NONE',  ( 6.123233995736766282E-16, -170.0000000000000000, -5.000000000000000000 ) ) ;
#48850 =( BOUNDED_CURVE ( )  B_SPLINE_CURVE ( 2, ( #19896, #34694, #11527, #54641, #36297, #55920, #49805, #35982, #20228 ),
 .UNSPECIFIED., .F., .F. ) 
 B_SPLINE_CURVE_WITH_KNOTS ( ( 3, 2, 2, 2, 3 ),
 ( 0.4339285714285714413, 0.4345238095238095344, 0.4357142857142857206, 0.4369047619047619069, 0.4375000000000000000 ),
 .UNSPECIFIED. ) 
 CURVE ( )  GEOMETRIC_REPRESENTATION_ITEM ( )  RATIONAL_B_SPLINE_CURVE ( ( 0.9330127018922194093, 0.9330127018922194093, 1.000000000000000000, 0.8660254037844387076, 1.000000000000000000, 0.8660254037844387076, 1.000000000000000000, 0.9330127018922194093, 0.9330127018922194093 ) ) 
 REPRESENTATION_ITEM ( '' )  );
#48851 = CARTESIAN_POINT ( 'NONE',  ( -1.339745962155625802, 13.20534180126147916, 4.999999999999991118 ) ) ;
#48852 = CARTESIAN_POINT ( 'NONE',  ( -2.499999999999996447, -19.83333333333333570, 4.330127018922195425 ) ) ;
#48853 = CARTESIAN_POINT ( 'NONE',  ( -4.458734124999998549, -23.22916666530107221, 2.574251347313722516 ) ) ;
#48854 = CARTESIAN_POINT ( 'NONE',  ( 4.458734124999999437, -81.81249999863440792, -5.460374474430324690E-16 ) ) ;
#48855 = CARTESIAN_POINT ( 'NONE',  ( 1.846868145590736310, -167.8750000013656063, 4.458734124999999437 ) ) ;
#48856 = CARTESIAN_POINT ( 'NONE',  ( 5.000000000000000888, -16.45833333060214443, 2.886751345948126879 ) ) ;
#48858 = ORIENTED_EDGE ( 'NONE', *, *, #25496, .F. ) ;
#48857 = CARTESIAN_POINT ( 'NONE',  ( 2.229367062499998831, -48.64583333196772941, -3.861377020970580887 ) ) ;
#48859 = DIRECTION ( 'NONE',  ( -1.000000000000000000, 1.224646799147354686E-16, 0.000000000000000000 ) ) ;
#48861 = ORIENTED_EDGE ( 'NONE', *, *, #33924, .T. ) ;
#48860 = CARTESIAN_POINT ( 'NONE',  ( 4.458734124999998549, 1.020833334698927120, -2.574251347313721627 ) ) ;
#48862 = CARTESIAN_POINT ( 'NONE',  ( -59.29741812935640155, -151.6250000013655779, -2.196230717870135685 ) ) ;
#48863 = CARTESIAN_POINT ( 'NONE',  ( -5.000000000000000000, -59.08333333333334281, -2.886751345948128211 ) ) ;
#48864 = CARTESIAN_POINT ( 'NONE',  ( -1.846868145590734756, -155.3750000013656347, -4.458734125000000326 ) ) ;
#48865 = CARTESIAN_POINT ( 'NONE',  ( -4.458734124999999437, -43.56249999863440081, 0.000000000000000000 ) ) ;
#48866 = CARTESIAN_POINT ( 'NONE',  ( -50.18089887299978358, -149.8125000027312126, 2.462841084822575688 ) ) ;
#48867 = CARTESIAN_POINT ( 'NONE',  ( -3.535533905932738641, -162.3750000000000284, 3.535533905932737309 ) ) ;
#48868 = CARTESIAN_POINT ( 'NONE',  ( -1.339745962155610925, -56.66965819600733312, 5.000000000000000000 ) ) ;
#48869 = CARTESIAN_POINT ( 'NONE',  ( -59.29741812935640155, -126.8750000013656205, -2.196230717870135685 ) ) ;
#48870 = CARTESIAN_POINT ( 'NONE',  ( 4.458734124999999437, -7.062499998634404363, -5.460374474430324690E-16 ) ) ;
#48871 = CARTESIAN_POINT ( 'NONE',  ( -2.229367062500000163, -48.72916666530106511, -3.861377020970580443 ) ) ;
#48872 = CARTESIAN_POINT ( 'NONE',  ( 5.000000000000000000, -151.1250000027312126, 0.000000000000000000 ) ) ;
#48873 = CARTESIAN_POINT ( 'NONE',  ( -3.152801135295367096, -147.0625000013655779, -3.152801135295367541 ) ) ;
#48874 = CARTESIAN_POINT ( 'NONE',  ( -2.229367062500000163, -90.72916666530106511, -3.861377020970580443 ) ) ;
#48875 = CARTESIAN_POINT ( 'NONE',  ( 2.499999999999998668, 8.666666666666666075, -4.330127018922193649 ) ) ;
#48876 = ORIENTED_EDGE ( 'NONE', *, *, #39672, .F. ) ;
#48877 = EDGE_CURVE ( 'NONE', #50850, #54554, #40273, .T. ) ;
#48878 = DIRECTION ( 'NONE',  ( 0.000000000000000000, 1.000000000000000000, 0.000000000000000000 ) ) ;
#48879 = CARTESIAN_POINT ( 'NONE',  ( 1.975475456537005874E-15, 6.375000002731185944, 5.000000000000000000 ) ) ;
#48880 = CARTESIAN_POINT ( 'NONE',  ( -53.33387254593733928, -148.9375000027311842, 5.149110718188519620 ) ) ;
#48881 = EDGE_CURVE ( 'NONE', #24136, #25000, #46852, .T. ) ;
#48882 = CARTESIAN_POINT ( 'NONE',  ( 0.000000000000000000, -170.0000000000000000, 0.000000000000000000 ) ) ;
#48883 = EDGE_LOOP ( 'NONE', ( #28477, #2475, #16074, #27278 ) ) ;
#48884 = CARTESIAN_POINT ( 'NONE',  ( -2.229367062500000163, 3.520833334698929118, -3.861377020970580443 ) ) ;
#48885 = EDGE_CURVE ( 'NONE', #47465, #24820, #22636, .T. ) ;
#48886 = DIRECTION ( 'NONE',  ( -0.000000000000000000, 1.000000000000000000, -0.000000000000000000 ) ) ;
#48887 = CARTESIAN_POINT ( 'NONE',  ( 9.457646018065525792E-16, -14.31249999863440259, 5.148502694627439702 ) ) ;
#48888 = CARTESIAN_POINT ( 'NONE',  ( -6.972266317189433020E-16, -105.1249999972687874, -5.000000000000000000 ) ) ;
#48889 = CARTESIAN_POINT ( 'NONE',  ( 2.229367062500001939, -3.979166665301070438, 3.861377020970579999 ) ) ;
#48890 = DIRECTION ( 'NONE',  ( -0.000000000000000000, 1.000000000000000000, -0.000000000000000000 ) ) ;
#48891 = CARTESIAN_POINT ( 'NONE',  ( -1.846868145590737420, -152.7500000013656063, 4.458734124999997661 ) ) ;
#48892 =( BOUNDED_CURVE ( )  B_SPLINE_CURVE ( 2, ( #60087, #50101, #6057, #18465, #38086, #8500, #42587, #9122, #23614 ),
 .UNSPECIFIED., .F., .F. ) 
 B_SPLINE_CURVE_WITH_KNOTS ( ( 3, 2, 2, 2, 3 ),
 ( 0.3416666666666669516, 0.3458333333333336035, 0.3500000000000002554, 0.3541666666666669627, 0.3583333333333336146 ),
 .UNSPECIFIED. ) 
 CURVE ( )  GEOMETRIC_REPRESENTATION_ITEM ( )  RATIONAL_B_SPLINE_CURVE ( ( 0.9999999999999948930, 0.9238795325112918455, 1.000000000000000000, 0.9238795325112867385, 1.000000000000000000, 0.9238795325112867385, 1.000000000000000000, 0.9238795325112816315, 1.000000000000005107 ) ) 
 REPRESENTATION_ITEM ( '' )  );
#48893 = CARTESIAN_POINT ( 'NONE',  ( 4.458734124999999437, 21.93750000136559208, -5.460374474430324690E-16 ) ) ;
#48894 = ORIENTED_EDGE ( 'NONE', *, *, #19331, .T. ) ;
#48895 = CARTESIAN_POINT ( 'NONE',  ( 4.458734124999998549, -95.72916666530107932, -2.574251347313721627 ) ) ;
#48896 = CARTESIAN_POINT ( 'NONE',  ( -5.000000000000000888, -148.5625000000000000, -2.071067811865475949 ) ) ;
#48897 = CARTESIAN_POINT ( 'NONE',  ( 1.975475456537005874E-15, -40.74999999999999289, 5.000000000000000000 ) ) ;
#48898 = CARTESIAN_POINT ( 'NONE',  ( -2.229367062499996610, -16.14583333196773651, 3.861377020970582219 ) ) ;
#48899 = CARTESIAN_POINT ( 'NONE',  ( -1.339745962155612258, 28.33034180399266333, 5.000000000000000000 ) ) ;
#48900 = CARTESIAN_POINT ( 'NONE',  ( 5.000000000000000000, 8.625000002731184168, -6.123233995736766282E-16 ) ) ;
#48901 = CARTESIAN_POINT ( 'NONE',  ( -5.000000000000000000, -88.00000000000000000, 0.000000000000000000 ) ) ;
#48902 = CARTESIAN_POINT ( 'NONE',  ( 2.500000000000002220, -41.54166666393548013, 4.330127018922192761 ) ) ;
#48903 = CARTESIAN_POINT ( 'NONE',  ( 5.000000000000000000, -29.50000000000000000, -6.123233995736766282E-16 ) ) ;
#48904 = CARTESIAN_POINT ( 'NONE',  ( -3.152548672688508926E-16, 15.43750000136559564, -5.148502694627439702 ) ) ;
#48905 = CARTESIAN_POINT ( 'NONE',  ( 0.000000000000000000, -170.0000000000000000, 5.000000000000000000 ) ) ;
#48906 = ORIENTED_EDGE ( 'NONE', *, *, #46960, .F. ) ;
#48907 = CARTESIAN_POINT ( 'NONE',  ( 9.457646018065525792E-16, 19.93750000136559208, 5.148502694627439702 ) ) ;
#48908 = CARTESIAN_POINT ( 'NONE',  ( 4.458734124999999437, -62.81249999863440792, -5.460374474430324690E-16 ) ) ;
#48909 = CARTESIAN_POINT ( 'NONE',  ( -4.458734124999999437, -8.645833331967736513, -2.574251347313719407 ) ) ;
#48910 = CARTESIAN_POINT ( 'NONE',  ( -5.000000000000000000, -31.00000000000000000, 0.000000000000000000 ) ) ;
#48911 = CARTESIAN_POINT ( 'NONE',  ( 1.060575238724906964E-15, 11.25000000000000000, 5.773502691896257311 ) ) ;
#48912 = CARTESIAN_POINT ( 'NONE',  ( -8.190561711645485556E-16, -168.6875000013656063, 4.458734124999999437 ) ) ;
#48913 = CARTESIAN_POINT ( 'NONE',  ( -5.000000000000000000, -20.87499999726881228, 0.000000000000000000 ) ) ;
#48914 = CARTESIAN_POINT ( 'NONE',  ( 9.457646018065525792E-16, -56.06249999863440792, 5.148502694627439702 ) ) ;
#48915 = CARTESIAN_POINT ( 'NONE',  ( 1.060575238724906964E-15, -90.62499999726880162, 5.773502691896257311 ) ) ;
#48916 = CARTESIAN_POINT ( 'NONE',  ( -9.184850993605147944E-16, -141.3750000027312126, 5.000000000000000000 ) ) ;
#48917 = CARTESIAN_POINT ( 'NONE',  ( 55.00000000000002132, 15.00000000000000000, 0.000000000000000000 ) ) ;
#48918 = DIRECTION ( 'NONE',  ( 1.000000000000000000, 0.000000000000000000, 0.000000000000000000 ) ) ;
#48919 = CARTESIAN_POINT ( 'NONE',  ( 4.458734124999997661, -152.7500000013656063, 1.846868145590737864 ) ) ;
#48920 = CARTESIAN_POINT ( 'NONE',  ( -3.535250795749689387E-16, -36.25000000000000711, -5.773502691896257311 ) ) ;
#48921 = CARTESIAN_POINT ( 'NONE',  ( -1.339745962155555858, -20.08034179853028789, -5.000000000000032863 ) ) ;
#48922 = CYLINDRICAL_SURFACE ( 'NONE', #34542, 5.000000000000000000 ) ;
#48923 = EDGE_LOOP ( 'NONE', ( #20352, #33238, #60618, #51743 ) ) ;
#48924 = CARTESIAN_POINT ( 'NONE',  ( -3.152548672688508926E-16, -102.5624999986344079, -5.148502694627439702 ) ) ;
#48925 = CARTESIAN_POINT ( 'NONE',  ( 2.229367062500001939, 1.770833334698927786, 3.861377020970579999 ) ) ;
#48926 = CARTESIAN_POINT ( 'NONE',  ( 5.000000000000000000, -80.41666666666665719, -2.886751345948130876 ) ) ;
#48927 = CARTESIAN_POINT ( 'NONE',  ( 5.000000000000000000, 2.583333333333333481, -2.886751345948129988 ) ) ;
#48928 = CARTESIAN_POINT ( 'NONE',  ( -3.152548672688508926E-16, -65.56249999863440792, -5.148502694627439702 ) ) ;
#48929 = EDGE_CURVE ( 'NONE', #43815, #20671, #59903, .T. ) ;
#48930 = CARTESIAN_POINT ( 'NONE',  ( -5.000000000000000000, 2.999999999999999112, 0.000000000000000000 ) ) ;
#48931 = CARTESIAN_POINT ( 'NONE',  ( -4.999999999999999112, -2.791666663935477466, 2.886751345948131764 ) ) ;
#48933 = VERTEX_POINT ( 'NONE', #39007 ) ;
#48932 = CARTESIAN_POINT ( 'NONE',  ( -4.458734124999998549, -36.22916666530106511, 2.574251347313722516 ) ) ;
#48934 = CARTESIAN_POINT ( 'NONE',  ( 1.975475456537005874E-15, -41.74999999999999289, 5.000000000000000000 ) ) ;
#48935 = DIRECTION ( 'NONE',  ( 0.000000000000000000, 0.000000000000000000, 1.000000000000000000 ) ) ;
#48936 = CARTESIAN_POINT ( 'NONE',  ( -54.60164318462004474, -136.3750000000000284, -4.984105922594373794 ) ) ;
#48937 = CARTESIAN_POINT ( 'NONE',  ( 5.000000000000000000, -46.50000000000000000, -6.123233995736766282E-16 ) ) ;
#48939 = CARTESIAN_POINT ( 'NONE',  ( -4.458734124999999437, -22.56249999863440436, 0.000000000000000000 ) ) ;
#48938 = CARTESIAN_POINT ( 'NONE',  ( -4.999999999999998224, 24.20833333606451987, 2.886751345948131764 ) ) ;
#48940 = DIRECTION ( 'NONE',  ( -0.000000000000000000, 1.000000000000000000, -0.000000000000000000 ) ) ;
#48941 = CARTESIAN_POINT ( 'NONE',  ( 2.229367062499998831, -67.64583333196773651, -3.861377020970580887 ) ) ;
#48942 = CARTESIAN_POINT ( 'NONE',  ( -1.846868145590737420, -145.0000000013656063, 4.458734124999999437 ) ) ;
#48943 = CARTESIAN_POINT ( 'NONE',  ( -4.458734124999999437, -84.39583333196773651, -2.574251347313719407 ) ) ;
#48944 = CARTESIAN_POINT ( 'NONE',  ( -50.70258187064364108, -140.3750000013656063, 2.196230717870141014 ) ) ;
#48945 = CARTESIAN_POINT ( 'NONE',  ( 2.229367062500001939, -32.22916666530106511, 3.861377020970579999 ) ) ;
#48946 = CARTESIAN_POINT ( 'NONE',  ( -5.000000000000000000, -72.95833333060214443, -2.886751345948128211 ) ) ;
#48947 = ORIENTED_EDGE ( 'NONE', *, *, #46858, .T. ) ;
#48948 = CARTESIAN_POINT ( 'NONE',  ( 5.000000000000000000, -51.41666666666666430, -2.886751345948130876 ) ) ;
#48949 = VERTEX_POINT ( 'NONE', #58638 ) ;
#48950 = CARTESIAN_POINT ( 'NONE',  ( -4.458734124999999437, -75.56249999863440792, 0.000000000000000000 ) ) ;
#48951 = CARTESIAN_POINT ( 'NONE',  ( 2.499999999999998668, 28.66666666666666785, -4.330127018922193649 ) ) ;
#48952 = ORIENTED_EDGE ( 'NONE', *, *, #55511, .F. ) ;
#48953 = CARTESIAN_POINT ( 'NONE',  ( 3.044556291839386294E-14, 12.75000000000000000, -5.000000000000000000 ) ) ;
#48954 = CARTESIAN_POINT ( 'NONE',  ( 6.123233995736766282E-16, -170.0000000000000000, -5.000000000000000000 ) ) ;
#48955 = CARTESIAN_POINT ( 'NONE',  ( -3.152548672688508926E-16, -57.81249999863440081, -5.148502694627439702 ) ) ;
#48956 = CARTESIAN_POINT ( 'NONE',  ( 4.458734124999999437, -0.06249999863440491854, -5.460374474430324690E-16 ) ) ;
#48957 = ORIENTED_EDGE ( 'NONE', *, *, #39366, .F. ) ;
#48958 = CARTESIAN_POINT ( 'NONE',  ( -4.999999999999998224, -19.91666666666666430, 2.886751345948131764 ) ) ;
#48959 = CARTESIAN_POINT ( 'NONE',  ( 1.975475456537005874E-15, -22.62499999726880873, 5.000000000000000000 ) ) ;
#48960 = CARTESIAN_POINT ( 'NONE',  ( -4.458734124999998549, 14.77083333469892779, 2.574251347313722516 ) ) ;
#48961 = CARTESIAN_POINT ( 'NONE',  ( -59.29741812935640155, -143.6250000013655779, -2.196230717870135685 ) ) ;
#48962 = CARTESIAN_POINT ( 'NONE',  ( 5.000000000000000000, -27.29166666393548013, -2.886751345948130876 ) ) ;
#48963 = CARTESIAN_POINT ( 'NONE',  ( -3.152801135295367096, -166.0625000013656063, -3.152801135295367541 ) ) ;
#48964 = AXIS2_PLACEMENT_3D ( 'NONE', #57335, #53120, #32231 ) ;
#48965 = ORIENTED_EDGE ( 'NONE', *, *, #54173, .T. ) ;
#48966 = CARTESIAN_POINT ( 'NONE',  ( -3.152548672688508926E-16, -74.56249999863442213, -5.148502694627439702 ) ) ;
#48967 = CARTESIAN_POINT ( 'NONE',  ( -5.000000000000000000, -153.5000000000000284, -6.123233995736766282E-16 ) ) ;
#48968 = CARTESIAN_POINT ( 'NONE',  ( -4.458734124999999437, 2.604166668032263043, -2.574251347313719407 ) ) ;
#48969 = VECTOR ( 'NONE', #29119, 1000.000000000000000 ) ;
#48970 = AXIS2_PLACEMENT_3D ( 'NONE', #18756, #14248, #44141 ) ;
#48971 =( BOUNDED_CURVE ( )  B_SPLINE_CURVE ( 2, ( #17971, #8643, #3828, #58158, #9269, #34029, #42729, #22825, #32776 ),
 .UNSPECIFIED., .F., .F. ) 
 B_SPLINE_CURVE_WITH_KNOTS ( ( 3, 2, 2, 2, 3 ),
 ( 0.8625000000000000444, 0.8630952380952381375, 0.8642857142857143238, 0.8654761904761905100, 0.8660714285714286031 ),
 .UNSPECIFIED. ) 
 CURVE ( )  GEOMETRIC_REPRESENTATION_ITEM ( )  RATIONAL_B_SPLINE_CURVE ( ( 0.9330127018922194093, 0.9330127018922194093, 1.000000000000000000, 0.8660254037844387076, 1.000000000000000000, 0.8660254037844387076, 1.000000000000000000, 0.9330127018922194093, 0.9330127018922194093 ) ) 
 REPRESENTATION_ITEM ( '' )  );
#48972 = DIRECTION ( 'NONE',  ( 0.000000000000000000, 0.000000000000000000, 1.000000000000000000 ) ) ;
#48973 = CARTESIAN_POINT ( 'NONE',  ( 2.229367062500001939, -66.22916666530106511, 3.861377020970579999 ) ) ;
#48974 = AXIS2_PLACEMENT_3D ( 'NONE', #10310, #5490, #35720 ) ;
#48975 = CARTESIAN_POINT ( 'NONE',  ( 5.000000000000000000, -23.37499999726881228, -6.123233995736766282E-16 ) ) ;
#48976 = CARTESIAN_POINT ( 'NONE',  ( -56.66612745406288099, -142.4375000027312126, -5.149110718188529390 ) ) ;
#48977 = CARTESIAN_POINT ( 'NONE',  ( 2.500000000000002220, -28.54166666393548013, 4.330127018922192761 ) ) ;
#48978 = CARTESIAN_POINT ( 'NONE',  ( -6.972266317189433020E-16, -61.25000000000000000, -5.000000000000000000 ) ) ;
#48979 = DIRECTION ( 'NONE',  ( 0.000000000000000000, 0.000000000000000000, 1.000000000000000000 ) ) ;
#48980 = CARTESIAN_POINT ( 'NONE',  ( 9.457646018065525792E-16, -46.06249999863440081, 5.148502694627439702 ) ) ;
#48981 = CARTESIAN_POINT ( 'NONE',  ( 9.457646018065525792E-16, -27.31249999863440081, 5.148502694627439702 ) ) ;
#48982 = CARTESIAN_POINT ( 'NONE',  ( 4.458734125000000326, 8.854166668032261711, 2.574251347313718519 ) ) ;
#48983 = LINE ( 'NONE', #55099, #41166 ) ;
#48984 = CARTESIAN_POINT ( 'NONE',  ( -4.999999999999999112, 27.08333333333333215, 2.886751345948131764 ) ) ;
#48985 = CARTESIAN_POINT ( 'NONE',  ( 2.071067811865476394, -150.3125000027312410, 5.000000000000000000 ) ) ;
#48986 = DIRECTION ( 'NONE',  ( -0.000000000000000000, 1.000000000000000000, -0.000000000000000000 ) ) ;
#48987 = EDGE_CURVE ( 'NONE', #48784, #47703, #54450, .T. ) ;
#48988 = CARTESIAN_POINT ( 'NONE',  ( -3.152548672688508926E-16, -39.56249999863440081, -5.148502694627439702 ) ) ;
#48989 = CARTESIAN_POINT ( 'NONE',  ( -2.500000000000000444, -71.04166666393547303, -4.330127018922193649 ) ) ;
#48990 = CARTESIAN_POINT ( 'NONE',  ( -51.60603307380591787, -142.1875000013656063, -2.891590998281053704 ) ) ;
#48991 = CARTESIAN_POINT ( 'NONE',  ( 2.071067811865475505, -142.8125000000000000, -5.000000000000000888 ) ) ;
#48992 = CARTESIAN_POINT ( 'NONE',  ( -4.458734124999997661, -72.47916666530107932, 2.574251347313722516 ) ) ;
#48993 = CARTESIAN_POINT ( 'NONE',  ( -8.190561711645485556E-16, -165.9375000013655779, 4.458734124999999437 ) ) ;
#48994 = CARTESIAN_POINT ( 'NONE',  ( 4.458734124999999437, -32.81249999863440792, -5.460374474430324690E-16 ) ) ;
#48995 = CARTESIAN_POINT ( 'NONE',  ( -59.98410592259440222, -148.1250000000000284, -0.3983568153799752487 ) ) ;
#48996 = FACE_OUTER_BOUND ( 'NONE', #45032, .T. ) ;
#48997 = CARTESIAN_POINT ( 'NONE',  ( -2.500000000000000444, -24.16666666666666430, -4.330127018922193649 ) ) ;
#48998 = CARTESIAN_POINT ( 'NONE',  ( -3.152801135295367096, -144.0625000013655779, -3.152801135295367541 ) ) ;
#48999 = VERTEX_POINT ( 'NONE', #49620 ) ;
#49000 = CARTESIAN_POINT ( 'NONE',  ( 2.229367062500001939, 25.77083333469892779, 3.861377020970579999 ) ) ;
#49001 = ORIENTED_EDGE ( 'NONE', *, *, #21146, .F. ) ;
#49002 = CARTESIAN_POINT ( 'NONE',  ( 4.458734125000000326, -63.14583333196774362, 2.574251347313718519 ) ) ;
#49003 = CARTESIAN_POINT ( 'NONE',  ( -4.999999999999999112, 23.20833333606451632, 2.886751345948131764 ) ) ;
#49004 = CARTESIAN_POINT ( 'NONE',  ( 1.339745962155612702, 4.830341803992664218, -5.000000000000000000 ) ) ;
#49005 = CARTESIAN_POINT ( 'NONE',  ( -2.499999999999996447, 19.16666666666666430, 4.330127018922195425 ) ) ;
#49006 = CARTESIAN_POINT ( 'NONE',  ( -5.000000000000000000, -89.08333333333332860, -2.886751345948128211 ) ) ;
#49007 = CARTESIAN_POINT ( 'NONE',  ( 4.458734124999998549, -8.729166665301073991, -2.574251347313721627 ) ) ;
#49008 = CARTESIAN_POINT ( 'NONE',  ( -1.339745962155610925, -22.79465819873851729, 5.000000000000000000 ) ) ;
#49009 = CARTESIAN_POINT ( 'NONE',  ( -54.60164318462004474, -145.5000000027312126, -4.984105922594373794 ) ) ;
#49010 = CARTESIAN_POINT ( 'NONE',  ( 1.975475456537005874E-15, -91.62499999726877320, 5.000000000000000000 ) ) ;
#49011 = CARTESIAN_POINT ( 'NONE',  ( -5.000000000000000000, -87.87499999726880162, 0.000000000000000000 ) ) ;
#49013 = CARTESIAN_POINT ( 'NONE',  ( 9.457646018065525792E-16, -21.06249999863440436, 5.148502694627439702 ) ) ;
#49012 = CARTESIAN_POINT ( 'NONE',  ( 2.499999999999998668, 0.6666666666666660745, -4.330127018922193649 ) ) ;
#49014 = AXIS2_PLACEMENT_3D ( 'NONE', #2179, #36885, #56192 ) ;
#49015 = CARTESIAN_POINT ( 'NONE',  ( 1.339745962155615144, 10.41965820146970501, 4.999999999999999112 ) ) ;
#49016 = CARTESIAN_POINT ( 'NONE',  ( -3.152548672688508926E-16, -53.56249999863439371, -5.148502694627439702 ) ) ;
#49017 = CARTESIAN_POINT ( 'NONE',  ( 3.152801135295367541, -157.5625000013656063, -3.152801135295367541 ) ) ;
#49018 = COLOUR_RGB ( '',0.8941176470588234615, 0.8941176470588234615, 0.8941176470588234615 ) ;
#49019 = VECTOR ( 'NONE', #15533, 1000.000000000000000 ) ;
#49020 = CARTESIAN_POINT ( 'NONE',  ( -4.999999999999999112, -48.79166666393547303, 2.886751345948131764 ) ) ;
#49021 = VERTEX_POINT ( 'NONE', #6840 ) ;
#49022 = AXIS2_PLACEMENT_3D ( 'NONE', #58328, #44472, #14564 ) ;
#49023 = CARTESIAN_POINT ( 'NONE',  ( -4.458734124999998549, 3.520833334698929118, 2.574251347313722516 ) ) ;
#49024 = ORIENTED_EDGE ( 'NONE', *, *, #59868, .T. ) ;
#49025 =( BOUNDED_CURVE ( )  B_SPLINE_CURVE ( 2, ( #14703, #34322, #53947, #5062, #40420, #9877, #29484, #49120, #50400 ),
 .UNSPECIFIED., .F., .F. ) 
 B_SPLINE_CURVE_WITH_KNOTS ( ( 3, 2, 2, 2, 3 ),
 ( 0.7020833333333332815, 0.7027777777777777235, 0.7041666666666667185, 0.7055555555555556024, 0.7062500000000000444 ),
 .UNSPECIFIED. ) 
 CURVE ( )  GEOMETRIC_REPRESENTATION_ITEM ( )  RATIONAL_B_SPLINE_CURVE ( ( 0.9330127018922194093, 0.9330127018922194093, 1.000000000000000000, 0.8660254037844387076, 1.000000000000000000, 0.8660254037844387076, 1.000000000000000000, 0.9330127018922194093, 0.9330127018922194093 ) ) 
 REPRESENTATION_ITEM ( '' )  );
#49027 = CARTESIAN_POINT ( 'NONE',  ( 2.499999999999998668, -9.208333330602146205, -4.330127018922193649 ) ) ;
#49026 = CARTESIAN_POINT ( 'NONE',  ( 1.339745962155615144, -4.705341801261478274, 4.999999999999999112 ) ) ;
#49028 = CARTESIAN_POINT ( 'NONE',  ( 3.152801135295366208, -155.5625000013656063, 3.152801135295367985 ) ) ;
#49029 = VERTEX_POINT ( 'NONE', #54768 ) ;
#49030 = CARTESIAN_POINT ( 'NONE',  ( 1.339745962155615144, -23.58034179853029144, 4.999999999999999112 ) ) ;
#49031 = CARTESIAN_POINT ( 'NONE',  ( -51.19402409849444524, -134.5000000000000284, -3.242614290531456334 ) ) ;
#49032 = CARTESIAN_POINT ( 'NONE',  ( -6.972266317189433020E-16, -30.12499999726880873, -5.000000000000000000 ) ) ;
#49033 = CARTESIAN_POINT ( 'NONE',  ( -2.229367062500000163, -40.72916666530107221, -3.861377020970580443 ) ) ;
#49034 = ORIENTED_EDGE ( 'NONE', *, *, #54997, .F. ) ;
#49035 = CARTESIAN_POINT ( 'NONE',  ( 6.123233995736766282E-16, -120.0000000000000000, -5.000000000000000000 ) ) ;
#49036 = CARTESIAN_POINT ( 'NONE',  ( -2.229367062500000163, 21.52083333469892779, -3.861377020970580443 ) ) ;
#49037 = VERTEX_POINT ( 'NONE', #20994 ) ;
#49038 = CARTESIAN_POINT ( 'NONE',  ( 4.458734124999998549, -88.97916666530107932, -2.574251347313721627 ) ) ;
#49039 = CARTESIAN_POINT ( 'NONE',  ( -51.75738570946856498, -125.8750000027312126, 3.805975901505576964 ) ) ;
#49040 = FACE_OUTER_BOUND ( 'NONE', #35862, .T. ) ;
#49041 = CARTESIAN_POINT ( 'NONE',  ( 5.000000000000000888, -100.5833333333333286, 2.886751345948126879 ) ) ;
#49042 = CARTESIAN_POINT ( 'NONE',  ( 2.500000000000002220, -52.54166666393548013, 4.330127018922192761 ) ) ;
#49043 = CARTESIAN_POINT ( 'NONE',  ( 2.229367062500001939, -58.97916666530106511, 3.861377020970579999 ) ) ;
#49044 = CARTESIAN_POINT ( 'NONE',  ( -2.499999999999996447, -61.70833333060214443, 4.330127018922195425 ) ) ;
#49045 = CARTESIAN_POINT ( 'NONE',  ( -2.229367062500000163, 17.52083333469892779, -3.861377020970580443 ) ) ;
#49046 = DIRECTION ( 'NONE',  ( -0.000000000000000000, 1.000000000000000000, -0.000000000000000000 ) ) ;
#49047 = CARTESIAN_POINT ( 'NONE',  ( -4.458734124999999437, -48.56249999863440792, 0.000000000000000000 ) ) ;
#49048 = CARTESIAN_POINT ( 'NONE',  ( -5.000000000000000000, -7.958333330602145317, -2.886751345948128211 ) ) ;
#49049 = FACE_OUTER_BOUND ( 'NONE', #37022, .T. ) ;
#49050 = DIRECTION ( 'NONE',  ( -0.5000000000000008882, -0.8660254037844382635, 0.000000000000000000 ) ) ;
#49051 = CARTESIAN_POINT ( 'NONE',  ( -5.000000000000000000, -74.00000000000000000, 0.000000000000000000 ) ) ;
#49052 = CARTESIAN_POINT ( 'NONE',  ( 2.229367062499998831, -109.6458333319677365, -3.861377020970580887 ) ) ;
#49053 = CARTESIAN_POINT ( 'NONE',  ( 4.458734124999999437, -11.06249999863440792, -5.460374474430324690E-16 ) ) ;
#49054 = ORIENTED_EDGE ( 'NONE', *, *, #12644, .T. ) ;
#49055 = AXIS2_PLACEMENT_3D ( 'NONE', #29729, #29091, #5305 ) ;
#49056 = CARTESIAN_POINT ( 'NONE',  ( -2.499999999999996447, -46.70833333060214443, 4.330127018922195425 ) ) ;
#49057 = CARTESIAN_POINT ( 'NONE',  ( 2.229367062500001939, -97.97916666530105090, 3.861377020970579999 ) ) ;
#49058 = CARTESIAN_POINT ( 'NONE',  ( -2.071067811865475061, -159.8125000027312126, -5.000000000000000888 ) ) ;
#49059 = CARTESIAN_POINT ( 'NONE',  ( 4.458734124999998549, -96.97916666530106511, -2.574251347313721627 ) ) ;
#49060 = ADVANCED_FACE ( 'NONE', ( #31590 ), #21633, .T. ) ;
#49061 = VECTOR ( 'NONE', #44409, 1000.000000000000000 ) ;
#49062 = CARTESIAN_POINT ( 'NONE',  ( -1.339745962155601378, 21.79465819873851729, -5.000000000000007105 ) ) ;
#49063 = CARTESIAN_POINT ( 'NONE',  ( -2.500000000000000444, -57.04166666393548013, -4.330127018922193649 ) ) ;
#49064 = FACE_OUTER_BOUND ( 'NONE', #22717, .T. ) ;
#49065 = CARTESIAN_POINT ( 'NONE',  ( -57.19623071787017210, -127.3750000013656205, 4.297418129356382899 ) ) ;
#49066 = CARTESIAN_POINT ( 'NONE',  ( -56.48576386720575471, -146.7500000013656063, -4.591703134518078322 ) ) ;
#49067 = CARTESIAN_POINT ( 'NONE',  ( -4.458734124999999437, -16.31249999863440436, 0.000000000000000000 ) ) ;
#49068 = CARTESIAN_POINT ( 'NONE',  ( 2.229367062500001939, 4.770833334698926897, 3.861377020970579999 ) ) ;
#49069 = CARTESIAN_POINT ( 'NONE',  ( -3.152548672688508926E-16, -58.81249999863440081, -5.148502694627439702 ) ) ;
#49070 = CARTESIAN_POINT ( 'NONE',  ( 0.000000000000000000, -170.0000000000000000, 0.000000000000000000 ) ) ;
#49071 = CARTESIAN_POINT ( 'NONE',  ( -3.152548672688508926E-16, -12.56249999863440259, -5.148502694627439702 ) ) ;
#49072 = CARTESIAN_POINT ( 'NONE',  ( 2.071067811865476394, -156.1875000000000000, 5.000000000000000000 ) ) ;
#49073 = CARTESIAN_POINT ( 'NONE',  ( 5.000000000000000888, -8.583333333333330373, 2.886751345948126879 ) ) ;
#49074 = ORIENTED_EDGE ( 'NONE', *, *, #58870, .F. ) ;
#49075 = CARTESIAN_POINT ( 'NONE',  ( -2.229367062499996610, -42.39583333196773651, 3.861377020970582219 ) ) ;
#49076 =( BOUNDED_CURVE ( )  B_SPLINE_CURVE ( 2, ( #51612, #31977, #41939, #61580, #17515, #32292, #7545, #50647, #3042 ),
 .UNSPECIFIED., .F., .F. ) 
 B_SPLINE_CURVE_WITH_KNOTS ( ( 3, 2, 2, 2, 3 ),
 ( 0.7660714285714286254, 0.7666666666666667185, 0.7678571428571429047, 0.7690476190476190910, 0.7696428571428571841 ),
 .UNSPECIFIED. ) 
 CURVE ( )  GEOMETRIC_REPRESENTATION_ITEM ( )  RATIONAL_B_SPLINE_CURVE ( ( 0.9330127018922194093, 0.9330127018922256266, 1.000000000000000000, 0.8660254037844387076, 1.000000000000000000, 0.8660254037844387076, 1.000000000000000000, 0.9330127018922194093, 0.9330127018922194093 ) ) 
 REPRESENTATION_ITEM ( '' )  );
#49077 = CARTESIAN_POINT ( 'NONE',  ( -54.64476657466781973, -125.0625000013655921, -4.444560631937228834 ) ) ;
#49078 = CARTESIAN_POINT ( 'NONE',  ( -5.112021521198522933, 5.708827036477257977, -7.069802615102034338 ) ) ;
#49079 = CARTESIAN_POINT ( 'NONE',  ( 0.000000000000000000, -170.0000000000000000, 0.000000000000000000 ) ) ;
#49080 = CARTESIAN_POINT ( 'NONE',  ( 9.457646018065525792E-16, -87.06249999863440792, 5.148502694627439702 ) ) ;
#49081 = CARTESIAN_POINT ( 'NONE',  ( 4.458734125000001214, 19.85416666803226349, 2.574251347313718519 ) ) ;
#49082 = CARTESIAN_POINT ( 'NONE',  ( -4.458734124999999437, 8.687500001365595637, 0.000000000000000000 ) ) ;
#49083 = EDGE_CURVE ( 'NONE', #61986, #35368, #61324, .T. ) ;
#49084 = CARTESIAN_POINT ( 'NONE',  ( 1.339745962155615144, -0.7053418012614794952, 4.999999999999999112 ) ) ;
#49085 = EDGE_CURVE ( 'NONE', #8062, #42248, #62078, .T. ) ;
#49086 = CARTESIAN_POINT ( 'NONE',  ( -1.339745962155613812, -7.205341801261479162, -5.000000000000000000 ) ) ;
#49087 = DIRECTION ( 'NONE',  ( 0.000000000000000000, -1.000000000000000000, 0.000000000000000000 ) ) ;
#49088 = CARTESIAN_POINT ( 'NONE',  ( -2.229367062500000163, 23.27083333469892779, -3.861377020970580443 ) ) ;
#49089 = CARTESIAN_POINT ( 'NONE',  ( -4.999999999999999112, -77.91666666666665719, 2.886751345948131764 ) ) ;
#49090 = CARTESIAN_POINT ( 'NONE',  ( -5.000000000000000000, 14.12500000273118594, 0.000000000000000000 ) ) ;
#49091 = ORIENTED_EDGE ( 'NONE', *, *, #37086, .F. ) ;
#49092 = FACE_OUTER_BOUND ( 'NONE', #15200, .T. ) ;
#49093 = ORIENTED_EDGE ( 'NONE', *, *, #18972, .T. ) ;
#49095 = CARTESIAN_POINT ( 'NONE',  ( -2.499999999999996447, -35.83333333333332860, 4.330127018922195425 ) ) ;
#49094 = CARTESIAN_POINT ( 'NONE',  ( 0.000000000000000000, -120.0000000000000000, 0.000000000000000000 ) ) ;
#49096 = CARTESIAN_POINT ( 'NONE',  ( 4.458734124999998549, -37.72916666530107221, -2.574251347313721627 ) ) ;
#49097 = EDGE_CURVE ( 'NONE', #37277, #61639, #8707, .T. ) ;
#49098 = CARTESIAN_POINT ( 'NONE',  ( 5.000000000000000000, -34.37499999726881583, -6.123233995736766282E-16 ) ) ;
#49100 = ORIENTED_EDGE ( 'NONE', *, *, #18613, .F. ) ;
#49099 = CARTESIAN_POINT ( 'NONE',  ( -2.229367062500000163, -63.47916666530106511, -3.861377020970580443 ) ) ;
#49101 = CARTESIAN_POINT ( 'NONE',  ( -58.39396692619412477, -150.6875000013656063, 2.891590998281057701 ) ) ;
#49102 = CARTESIAN_POINT ( 'NONE',  ( 9.457646018065525792E-16, -13.06249999863440259, 5.148502694627439702 ) ) ;
#49104 = VERTEX_POINT ( 'NONE', #26132 ) ;
#49103 = CARTESIAN_POINT ( 'NONE',  ( -4.458734124999998549, -13.47916666530107221, 2.574251347313722516 ) ) ;
#49105 = CARTESIAN_POINT ( 'NONE',  ( 2.499999999999998668, -81.33333333333332860, -4.330127018922193649 ) ) ;
#49106 = CARTESIAN_POINT ( 'NONE',  ( 1.846868145590735200, -167.2500000013655779, -4.458734125000000326 ) ) ;
#49107 = CARTESIAN_POINT ( 'NONE',  ( -3.152548672688508926E-16, -59.81249999863440792, -5.148502694627439702 ) ) ;
#49108 = CIRCLE ( 'NONE', #37833, 4.999999999999999112 ) ;
#49109 = CARTESIAN_POINT ( 'NONE',  ( -5.000000000000000000, -82.95833333060213022, -2.886751345948128211 ) ) ;
#49111 = ORIENTED_EDGE ( 'NONE', *, *, #47934, .T. ) ;
#49110 = CARTESIAN_POINT ( 'NONE',  ( -5.000000000000000000, -48.95833333060213732, -2.886751345948128211 ) ) ;
#49112 = CARTESIAN_POINT ( 'NONE',  ( -59.81910112700025905, -144.1875000000000000, -2.462841084822630311 ) ) ;
#49113 = CIRCLE ( 'NONE', #31642, 5.000000000000000000 ) ;
#49114 = CARTESIAN_POINT ( 'NONE',  ( 9.457646018065525792E-16, -26.31249999863440792, 5.148502694627439702 ) ) ;
#49115 = ORIENTED_EDGE ( 'NONE', *, *, #61459, .T. ) ;
#49116 = CONTEXT_DEPENDENT_SHAPE_REPRESENTATION ( #32268, #24024 ) ;
#49117 = CARTESIAN_POINT ( 'NONE',  ( 1.846868145590736310, -165.8750000013656063, 4.458734124999999437 ) ) ;
#49118 = ADVANCED_FACE ( 'NONE', ( #5881 ), #1075, .T. ) ;
#49119 = CARTESIAN_POINT ( 'NONE',  ( 4.458734124999999437, -107.0624999986343937, -5.460374474430324690E-16 ) ) ;
#49120 = CARTESIAN_POINT ( 'NONE',  ( 1.339745962155615144, -55.58034179853028434, 4.999999999999999112 ) ) ;
#49121 = ORIENTED_EDGE ( 'NONE', *, *, #5626, .F. ) ;
#49122 = CARTESIAN_POINT ( 'NONE',  ( -57.19623071787016499, -146.6250000013656063, 4.297418129356382899 ) ) ;
#49123 = CARTESIAN_POINT ( 'NONE',  ( -54.60164318462004474, -138.5000000027312126, -4.984105922594373794 ) ) ;
#49124 = CARTESIAN_POINT ( 'NONE',  ( 2.229367062500001939, -40.97916666530107221, 3.861377020970579999 ) ) ;
#49125 = CARTESIAN_POINT ( 'NONE',  ( 3.152801135295367541, -144.5625000013655779, -3.152801135295367541 ) ) ;
#49126 = CARTESIAN_POINT ( 'NONE',  ( -7.500000000000000000, 4.730921838224027454, -7.493596905200499592 ) ) ;
#49127 = CARTESIAN_POINT ( 'NONE',  ( 2.500000000000002220, 29.33333333333333215, 4.330127018922192761 ) ) ;
#49128 = CARTESIAN_POINT ( 'NONE',  ( 4.458734125000001214, -14.89583333196773474, 2.574251347313718519 ) ) ;
#49129 = CARTESIAN_POINT ( 'NONE',  ( 9.457646018065525792E-16, -102.3124999986343937, 5.148502694627439702 ) ) ;
#49130 = ORIENTED_EDGE ( 'NONE', *, *, #61045, .F. ) ;
#49131 = CARTESIAN_POINT ( 'NONE',  ( 4.458734125000000326, -140.6250000013656063, -1.846868145590734978 ) ) ;
#49132 = CARTESIAN_POINT ( 'NONE',  ( 4.458734124999998549, -33.97916666530107221, -2.574251347313721627 ) ) ;
#49133 = CARTESIAN_POINT ( 'NONE',  ( 5.000000000000000000, 7.708333336064517205, -2.886751345948129988 ) ) ;
#49134 = CARTESIAN_POINT ( 'NONE',  ( 1.975475456537005874E-15, 10.24999999999999822, 5.000000000000000000 ) ) ;
#49135 = CARTESIAN_POINT ( 'NONE',  ( -50.40829686548195099, -133.0000000013656063, -1.485763867205728284 ) ) ;
#49136 = CARTESIAN_POINT ( 'NONE',  ( 2.229367062499998831, -73.89583333196773651, -3.861377020970580887 ) ) ;
#49137 = CARTESIAN_POINT ( 'NONE',  ( -58.80597590150559739, -146.1250000027312126, 3.242614290531460330 ) ) ;
#49138 = CARTESIAN_POINT ( 'NONE',  ( -56.66612745406283125, -146.4375000027312694, -5.149110718188525837 ) ) ;
#49139 = CARTESIAN_POINT ( 'NONE',  ( 1.339745962155624914, 14.83034180399266333, -4.999999999999991118 ) ) ;
#49140 = CARTESIAN_POINT ( 'NONE',  ( -2.229367062500000163, 4.270833334698926897, -3.861377020970580443 ) ) ;
#49141 = VERTEX_POINT ( 'NONE', #40287 ) ;
#49142 = CARTESIAN_POINT ( 'NONE',  ( -3.750000000000007105, -6.495190528383289141, 0.000000000000000000 ) ) ;
#49144 = CARTESIAN_POINT ( 'NONE',  ( 2.229367062499998831, -30.64583333196773651, -3.861377020970580887 ) ) ;
#49143 = CARTESIAN_POINT ( 'NONE',  ( 5.000000000000000000, -97.50000000000000000, -6.123233995736766282E-16 ) ) ;
#49145 = CARTESIAN_POINT ( 'NONE',  ( -1.339745962155610925, -35.79465819873851729, 5.000000000000000000 ) ) ;
#49146 = CARTESIAN_POINT ( 'NONE',  ( -4.458734124999998549, -79.47916666530106511, 2.574251347313722516 ) ) ;
#49147 = ADVANCED_FACE ( 'NONE', ( #56046 ), #1706, .T. ) ;
#49148 = CARTESIAN_POINT ( 'NONE',  ( -2.229367062500000163, 21.27083333469892779, -3.861377020970580443 ) ) ;
#49149 = DIRECTION ( 'NONE',  ( 0.000000000000000000, 0.000000000000000000, 1.000000000000000000 ) ) ;
#49150 = CARTESIAN_POINT ( 'NONE',  ( -50.40829686548195099, -140.0000000013656063, -1.485763867205728284 ) ) ;
#49151 = ADVANCED_FACE ( 'NONE', ( #21311 ), #59600, .T. ) ;
#49152 = EDGE_CURVE ( 'NONE', #11358, #20646, #46390, .T. ) ;
#49153 = CARTESIAN_POINT ( 'NONE',  ( 4.458734124999999437, -2.812499998634407472, -5.460374474430324690E-16 ) ) ;
#49154 = CARTESIAN_POINT ( 'NONE',  ( -4.458734124999998549, 22.52083333469892423, 2.574251347313722516 ) ) ;
#49155 = CARTESIAN_POINT ( 'NONE',  ( -4.458734124999997661, -42.47916666530106511, 2.574251347313722516 ) ) ;
#49156 = CARTESIAN_POINT ( 'NONE',  ( -5.000000000000000000, -50.87499999726881583, 0.000000000000000000 ) ) ;
#49157 = CARTESIAN_POINT ( 'NONE',  ( -4.458734124999999437, 3.687500001365594748, 0.000000000000000000 ) ) ;
#49158 = ORIENTED_EDGE ( 'NONE', *, *, #23584, .T. ) ;
#49159 = CARTESIAN_POINT ( 'NONE',  ( 4.458734125000000326, -24.14583333196774362, 2.574251347313718519 ) ) ;
#49160 = VECTOR ( 'NONE', #9385, 1000.000000000000000 ) ;
#49161 = CARTESIAN_POINT ( 'NONE',  ( 9.457646018065525792E-16, -71.06249999863440792, 5.148502694627439702 ) ) ;
#49162 = CARTESIAN_POINT ( 'NONE',  ( -5.000000000000000000, -102.8749999972688158, 0.000000000000000000 ) ) ;
#49163 = AXIS2_PLACEMENT_3D ( 'NONE', #14368, #28534, #43943 ) ;
#49164 = EDGE_CURVE ( 'NONE', #28144, #46456, #29164, .T. ) ;
#49165 =( BOUNDED_CURVE ( )  B_SPLINE_CURVE ( 2, ( #26513, #6266, #51289, #50959, #11705, #45489, #6900, #26191, #60300 ),
 .UNSPECIFIED., .F., .F. ) 
 B_SPLINE_CURVE_WITH_KNOTS ( ( 3, 2, 2, 2, 3 ),
 ( 0.2625000000000000111, 0.2630952380952381042, 0.2642857142857142905, 0.2654761904761904767, 0.2660714285714285698 ),
 .UNSPECIFIED. ) 
 CURVE ( )  GEOMETRIC_REPRESENTATION_ITEM ( )  RATIONAL_B_SPLINE_CURVE ( ( 0.9330127018922194093, 0.9330127018922194093, 1.000000000000000000, 0.8660254037844387076, 1.000000000000000000, 0.8660254037844387076, 1.000000000000000000, 0.9330127018922194093, 0.9330127018922194093 ) ) 
 REPRESENTATION_ITEM ( '' )  );
#49166 = CARTESIAN_POINT ( 'NONE',  ( 4.458734125000001214, 24.10416666803226349, 2.574251347313718519 ) ) ;
#49167 = DIRECTION ( 'NONE',  ( 0.000000000000000000, 1.000000000000000000, 0.000000000000000000 ) ) ;
#49168 = EDGE_CURVE ( 'NONE', #20011, #14094, #26756, .T. ) ;
#49169 = CARTESIAN_POINT ( 'NONE',  ( 4.458734124999998549, -108.9791666653010651, -2.574251347313721627 ) ) ;
#49170 = CARTESIAN_POINT ( 'NONE',  ( 4.458734125000000326, -72.14583333196773651, 2.574251347313718519 ) ) ;
#49171 = CARTESIAN_POINT ( 'NONE',  ( -2.500000000000000444, -60.16666666666665719, -4.330127018922193649 ) ) ;
#49172 = CYLINDRICAL_SURFACE ( 'NONE', #15148, 5.000000000000000000 ) ;
#49173 = CARTESIAN_POINT ( 'NONE',  ( -2.499999999999996447, -10.70833333060214621, 4.330127018922195425 ) ) ;
#49174 = VERTEX_POINT ( 'NONE', #52487 ) ;
#49175 = DIRECTION ( 'NONE',  ( 1.000000000000000000, 0.000000000000000000, 0.000000000000000000 ) ) ;
#49176 = CARTESIAN_POINT ( 'NONE',  ( 6.123233995736766282E-16, -170.0000000000000000, -5.000000000000000000 ) ) ;
#49177 = CARTESIAN_POINT ( 'NONE',  ( -2.500000000000000444, -17.16666666666666430, -4.330127018922193649 ) ) ;
#49178 = CARTESIAN_POINT ( 'NONE',  ( 4.458734125000001214, -20.89583333196774007, 2.574251347313718519 ) ) ;
#49179 = CARTESIAN_POINT ( 'NONE',  ( -4.458734124999999437, -85.39583333196773651, -2.574251347313719407 ) ) ;
#49180 = VECTOR ( 'NONE', #56788, 1000.000000000000000 ) ;
#49182 = CARTESIAN_POINT ( 'NONE',  ( -4.458734125000000326, -167.2500000013655779, -1.846868145590735644 ) ) ;
#49181 =( BOUNDED_CURVE ( )  B_SPLINE_CURVE ( 2, ( #51464, #27946, #46952, #21874, #32140, #42736, #12216, #37926, #12842 ),
 .UNSPECIFIED., .F., .F. ) 
 B_SPLINE_CURVE_WITH_KNOTS ( ( 3, 2, 2, 2, 3 ),
 ( 0.8416666666666664520, 0.8458333333333331039, 0.8499999999999997558, 0.8541666666666664076, 0.8583333333333330595 ),
 .UNSPECIFIED. ) 
 CURVE ( )  GEOMETRIC_REPRESENTATION_ITEM ( )  RATIONAL_B_SPLINE_CURVE ( ( 1.000000000000003997, 0.9238795325112826307, 1.000000000000000000, 0.9238795325112867385, 1.000000000000000000, 0.9238795325112867385, 1.000000000000000000, 0.9238795325112908463, 0.9999999999999958922 ) ) 
 REPRESENTATION_ITEM ( '' )  );
#49183 = CARTESIAN_POINT ( 'NONE',  ( 2.500000000000002220, -19.54166666393548013, 4.330127018922192761 ) ) ;
#49185 = ORIENTED_EDGE ( 'NONE', *, *, #12508, .F. ) ;
#49184 = CARTESIAN_POINT ( 'NONE',  ( 9.457646018065525792E-16, -51.06249999863440792, 5.148502694627439702 ) ) ;
#49186 = CARTESIAN_POINT ( 'NONE',  ( 2.499999999999998668, 5.666666666666666963, -4.330127018922193649 ) ) ;
#49187 = CARTESIAN_POINT ( 'NONE',  ( 2.500000000000002220, -15.54166666393548191, 4.330127018922192761 ) ) ;
#49189 = ORIENTED_EDGE ( 'NONE', *, *, #6344, .T. ) ;
#49188 = CARTESIAN_POINT ( 'NONE',  ( 4.458734124999998549, -0.9791666653010713262, -2.574251347313721627 ) ) ;
#49190 = CARTESIAN_POINT ( 'NONE',  ( -58.39396692619412477, -153.4375000013656063, 2.891590998281057701 ) ) ;
#49191 = CARTESIAN_POINT ( 'NONE',  ( 2.500000000000002220, -67.66666666666667140, 4.330127018922192761 ) ) ;
#49192 = CARTESIAN_POINT ( 'NONE',  ( -3.152801135295367096, -155.3125000013656063, -3.152801135295367541 ) ) ;
#49193 = CARTESIAN_POINT ( 'NONE',  ( -2.229367062499996610, -43.39583333196773651, 3.861377020970582219 ) ) ;
#49194 = CARTESIAN_POINT ( 'NONE',  ( -5.000000000000000000, -80.87499999726881583, 0.000000000000000000 ) ) ;
#49195 = CARTESIAN_POINT ( 'NONE',  ( 2.071067811865476394, -164.1875000000000000, 5.000000000000000000 ) ) ;
#49196 = CARTESIAN_POINT ( 'NONE',  ( -1.339745962155613812, -57.08034179853028434, -5.000000000000000000 ) ) ;
#49197 = CARTESIAN_POINT ( 'NONE',  ( -53.51423613279429503, -128.5000000013656063, 4.591703134518082763 ) ) ;
#49198 = CARTESIAN_POINT ( 'NONE',  ( -2.229367062500000163, -12.72916666530107044, -3.861377020970580443 ) ) ;
#49199 = CARTESIAN_POINT ( 'NONE',  ( 4.458734125000001214, -45.14583333196774362, 2.574251347313718519 ) ) ;
#49200 = CARTESIAN_POINT ( 'NONE',  ( 0.000000000000000000, -170.0000000000000000, 0.000000000000000000 ) ) ;
#49201 = CARTESIAN_POINT ( 'NONE',  ( 4.458734124999999437, -150.5000000013656347, 1.846868145590737864 ) ) ;
#49202 = CARTESIAN_POINT ( 'NONE',  ( -3.152548672688508926E-16, -86.81249999863439371, -5.148502694627439702 ) ) ;
#49203 = CARTESIAN_POINT ( 'NONE',  ( 2.500000000000002220, -108.6666666666666572, 4.330127018922192761 ) ) ;
#49204 = EDGE_LOOP ( 'NONE', ( #11388, #31724, #18783, #38564 ) ) ;
#49205 = CARTESIAN_POINT ( 'NONE',  ( -2.499999999999996447, 14.29166666939785202, 4.330127018922195425 ) ) ;
#49206 = CARTESIAN_POINT ( 'NONE',  ( -1.049326080737009628E-13, -5.624999997268816720, 5.000000000000000000 ) ) ;
#49207 = CARTESIAN_POINT ( 'NONE',  ( -50.01589407740564042, -148.7500000027312126, 0.3983568153799778022 ) ) ;
#49208 =( GEOMETRIC_REPRESENTATION_CONTEXT ( 3 ) GLOBAL_UNCERTAINTY_ASSIGNED_CONTEXT ( ( #57501 ) ) GLOBAL_UNIT_ASSIGNED_CONTEXT ( ( #53783, #43808, #24203 ) ) REPRESENTATION_CONTEXT ( 'NONE', 'WORKASPACE' ) );
#49209 = CARTESIAN_POINT ( 'NONE',  ( 1.975475456537005874E-15, -82.62499999726878741, 5.000000000000000000 ) ) ;
#49210 = VECTOR ( 'NONE', #29890, 1000.000000000000000 ) ;
#49211 = VERTEX_POINT ( 'NONE', #13235 ) ;
#49212 = CARTESIAN_POINT ( 'NONE',  ( -3.152548672688508926E-16, 1.437500001365596525, -5.148502694627439702 ) ) ;
#49213 = CARTESIAN_POINT ( 'NONE',  ( 1.975475456537005874E-15, -13.75000000000000000, 5.000000000000000000 ) ) ;
#49214 = CARTESIAN_POINT ( 'NONE',  ( 2.229367062500001939, -15.22916666530107399, 3.861377020970579999 ) ) ;
#49215 = CARTESIAN_POINT ( 'NONE',  ( -4.458734124999999437, -1.312499998634406140, 0.000000000000000000 ) ) ;
#49216 = CARTESIAN_POINT ( 'NONE',  ( 0.000000000000000000, -170.0000000000000000, 0.000000000000000000 ) ) ;
#49217 = CARTESIAN_POINT ( 'NONE',  ( -4.458734125000000326, -148.8750000013655779, 1.846868145590734089 ) ) ;
#49218 = CARTESIAN_POINT ( 'NONE',  ( -4.458734124999999437, 23.43750000136559564, 0.000000000000000000 ) ) ;
#49219 = ORIENTED_EDGE ( 'NONE', *, *, #62555, .T. ) ;
#49220 = CARTESIAN_POINT ( 'NONE',  ( 9.457646018065525792E-16, -96.06249999863439371, 5.148502694627439702 ) ) ;
#49221 = CARTESIAN_POINT ( 'NONE',  ( -5.000000000000000000, -33.95833333060213732, -2.886751345948128211 ) ) ;
#49222 = CARTESIAN_POINT ( 'NONE',  ( 5.000000000000000888, -12.45833333060214976, 2.886751345948126879 ) ) ;
#49223 = CARTESIAN_POINT ( 'NONE',  ( -4.458734124999998549, -12.22916666530106866, 2.574251347313722516 ) ) ;
#49224 = CARTESIAN_POINT ( 'NONE',  ( 1.339745962155612702, -39.16965819600733312, -5.000000000000000000 ) ) ;
#49225 = CARTESIAN_POINT ( 'NONE',  ( -58.39396692619412477, -154.5625000013656063, 2.891590998281057701 ) ) ;
#49226 = CARTESIAN_POINT ( 'NONE',  ( -53.51423613279429503, -154.2500000013656063, 4.591703134518082763 ) ) ;
#49227 = EDGE_CURVE ( 'NONE', #3670, #33371, #2531, .T. ) ;
#49228 = CARTESIAN_POINT ( 'NONE',  ( 5.000000000000000000, -40.37499999726880162, -6.123233995736766282E-16 ) ) ;
#49229 = CARTESIAN_POINT ( 'NONE',  ( 2.499999999999998668, -74.33333333333332860, -4.330127018922193649 ) ) ;
#49230 = CARTESIAN_POINT ( 'NONE',  ( 9.457646018065525792E-16, 11.93750000136559564, 5.148502694627439702 ) ) ;
#49231 = CARTESIAN_POINT ( 'NONE',  ( 2.499999999999998668, 9.666666666666667851, -4.330127018922193649 ) ) ;
#49232 = CARTESIAN_POINT ( 'NONE',  ( 4.458734125000000326, 18.10416666803225993, 2.574251347313718519 ) ) ;
#49233 = CARTESIAN_POINT ( 'NONE',  ( 2.229367062500001939, -63.97916666530106511, 3.861377020970579999 ) ) ;
#49234 = ORIENTED_EDGE ( 'NONE', *, *, #35006, .F. ) ;
#49235 = CARTESIAN_POINT ( 'NONE',  ( -2.229367062500000163, -8.729166665301073991, -3.861377020970580443 ) ) ;
#49236 =( BOUNDED_CURVE ( )  B_SPLINE_CURVE ( 2, ( #20533, #40131, #59772, #29514, #34038, #49784, #25671, #50104, #15699 ),
 .UNSPECIFIED., .F., .F. ) 
 B_SPLINE_CURVE_WITH_KNOTS ( ( 3, 2, 2, 2, 3 ),
 ( 0.2803571428571428603, 0.2809523809523809534, 0.2821428571428571397, 0.2833333333333333259, 0.2839285714285714191 ),
 .UNSPECIFIED. ) 
 CURVE ( )  GEOMETRIC_REPRESENTATION_ITEM ( )  RATIONAL_B_SPLINE_CURVE ( ( 0.9330127018922194093, 0.9330127018922194093, 1.000000000000000000, 0.8660254037844387076, 1.000000000000000000, 0.8660254037844387076, 1.000000000000000000, 0.9330127018922194093, 0.9330127018922194093 ) ) 
 REPRESENTATION_ITEM ( '' )  );
#49237 = CARTESIAN_POINT ( 'NONE',  ( 2.499999999999998668, 6.666666666666667851, -4.330127018922193649 ) ) ;
#49238 = CARTESIAN_POINT ( 'NONE',  ( 4.458734124999999437, -167.5000000013655779, 1.846868145590737864 ) ) ;
#49239 = CARTESIAN_POINT ( 'NONE',  ( 1.339745962155615144, -63.58034179853028434, 4.999999999999999112 ) ) ;
#49240 = CARTESIAN_POINT ( 'NONE',  ( 4.458734124999998549, -51.72916666530107221, -2.574251347313721627 ) ) ;
#49241 = CARTESIAN_POINT ( 'NONE',  ( -2.499999999999996447, -90.70833333060214443, 4.330127018922195425 ) ) ;
#49242 = CARTESIAN_POINT ( 'NONE',  ( 9.457646018065525792E-16, -34.06249999863440792, 5.148502694627439702 ) ) ;
#49243 = EDGE_CURVE ( 'NONE', #49211, #19793, #27084, .T. ) ;
#49244 = CARTESIAN_POINT ( 'NONE',  ( 1.975475456537005874E-15, 20.37500000273118417, 5.000000000000000000 ) ) ;
#49245 = CARTESIAN_POINT ( 'NONE',  ( -1.339745962155610925, -54.66965819600732601, 5.000000000000000000 ) ) ;
#49246 = CARTESIAN_POINT ( 'NONE',  ( 0.000000000000000000, -170.0000000000000000, 0.000000000000000000 ) ) ;
#49247 = CARTESIAN_POINT ( 'NONE',  ( -4.458734124999999437, -155.2500000013656063, -1.846868145590735644 ) ) ;
#49248 = CARTESIAN_POINT ( 'NONE',  ( 1.060575238724906964E-15, -42.75000000000000000, 5.773502691896257311 ) ) ;
#49249 = CARTESIAN_POINT ( 'NONE',  ( 0.000000000000000000, -120.0000000000000000, 0.000000000000000000 ) ) ;
#49250 = EDGE_CURVE ( 'NONE', #28956, #54753, #18107, .T. ) ;
#49251 = LINE ( 'NONE', #4548, #49991 ) ;
#49252 = ORIENTED_EDGE ( 'NONE', *, *, #16412, .T. ) ;
#49253 = CARTESIAN_POINT ( 'NONE',  ( 4.458734124999999437, -101.8124999986344079, -5.460374474430324690E-16 ) ) ;
#49254 = CARTESIAN_POINT ( 'NONE',  ( 4.458734124999998549, 2.020833334698927786, -2.574251347313721627 ) ) ;
#49255 = AXIS2_PLACEMENT_3D ( 'NONE', #4426, #19209, #38826 ) ;
#49256 = DIRECTION ( 'NONE',  ( -0.000000000000000000, 1.000000000000000000, -0.000000000000000000 ) ) ;
#49257 = ADVANCED_FACE ( 'NONE', ( #37998 ), #56999, .T. ) ;
#49258 = CARTESIAN_POINT ( 'NONE',  ( -5.000000000000000000, -1.000000000000000888, 0.000000000000000000 ) ) ;
#49259 = VECTOR ( 'NONE', #34856, 1000.000000000000000 ) ;
#49260 = CARTESIAN_POINT ( 'NONE',  ( -2.229367062500000163, -68.47916666530107932, -3.861377020970580443 ) ) ;
#49261 = CARTESIAN_POINT ( 'NONE',  ( -6.972266317189433020E-16, -55.12499999726880873, -5.000000000000000000 ) ) ;
#49262 = EDGE_CURVE ( 'NONE', #59301, #61600, #6648, .T. ) ;
#49263 = CARTESIAN_POINT ( 'NONE',  ( 5.000000000000000888, -0.4583333306021480369, 2.886751345948126879 ) ) ;
#49265 = EDGE_LOOP ( 'NONE', ( #44591, #36624, #16780, #38165 ) ) ;
#49264 = CARTESIAN_POINT ( 'NONE',  ( 4.458734124999998549, -32.72916666530107221, -2.574251347313721627 ) ) ;
#49266 = CARTESIAN_POINT ( 'NONE',  ( 0.000000000000000000, -170.0000000000000000, 0.000000000000000000 ) ) ;
#49267 = DIRECTION ( 'NONE',  ( 0.000000000000000000, 0.000000000000000000, 1.000000000000000000 ) ) ;
#49268 = ORIENTED_EDGE ( 'NONE', *, *, #5537, .F. ) ;
#49269 = CARTESIAN_POINT ( 'NONE',  ( 5.000000000000000888, -20.58333333333333215, 2.886751345948126879 ) ) ;
#49270 = CARTESIAN_POINT ( 'NONE',  ( 5.000000000000000000, -51.50000000000000711, -6.123233995736766282E-16 ) ) ;
#49271 =( BOUNDED_CURVE ( )  B_SPLINE_CURVE ( 2, ( #39282, #4559, #44427, #387, #13901, #53143, #39598, #28995, #48307 ),
 .UNSPECIFIED., .F., .F. ) 
 B_SPLINE_CURVE_WITH_KNOTS ( ( 3, 2, 2, 2, 3 ),
 ( 0.2910714285714285920, 0.2916666666666666852, 0.2928571428571428714, 0.2940476190476190577, 0.2946428571428571508 ),
 .UNSPECIFIED. ) 
 CURVE ( )  GEOMETRIC_REPRESENTATION_ITEM ( )  RATIONAL_B_SPLINE_CURVE ( ( 0.9330127018922194093, 0.9330127018922194093, 1.000000000000000000, 0.8660254037844387076, 1.000000000000000000, 0.8660254037844387076, 1.000000000000000000, 0.9330127018922194093, 0.9330127018922194093 ) ) 
 REPRESENTATION_ITEM ( '' )  );
#49273 = CARTESIAN_POINT ( 'NONE',  ( -2.229367062500000163, -23.72916666530107577, -3.861377020970580443 ) ) ;
#49272 = DIRECTION ( 'NONE',  ( -0.000000000000000000, 1.000000000000000000, -0.000000000000000000 ) ) ;
#49274 = CARTESIAN_POINT ( 'NONE',  ( -3.152548672688508926E-16, -71.56249999863440792, -5.148502694627439702 ) ) ;
#49275 = CARTESIAN_POINT ( 'NONE',  ( 3.152801135295367541, -145.5625000013655779, -3.152801135295367541 ) ) ;
#49276 = CARTESIAN_POINT ( 'NONE',  ( -3.152548672688508926E-16, -81.56249999863440792, -5.148502694627439702 ) ) ;
#49277 = CARTESIAN_POINT ( 'NONE',  ( -52.10840900171896806, -140.4375000013656063, 3.393966926194110556 ) ) ;
#49278 = CARTESIAN_POINT ( 'NONE',  ( 4.458734124999998549, -28.97916666530107577, -2.574251347313721627 ) ) ;
#49279 = CARTESIAN_POINT ( 'NONE',  ( 1.060575238724906964E-15, -71.62499999726880162, 5.773502691896257311 ) ) ;
#49280 = ORIENTED_EDGE ( 'NONE', *, *, #40160, .F. ) ;
#49281 = ORIENTED_EDGE ( 'NONE', *, *, #49683, .F. ) ;
#49282 = CARTESIAN_POINT ( 'NONE',  ( 9.457646018065525792E-16, -72.31249999863440792, 5.148502694627439702 ) ) ;
#49283 = LINE ( 'NONE', #90, #10186 ) ;
#49284 = VERTEX_POINT ( 'NONE', #56687 ) ;
#49285 = DIRECTION ( 'NONE',  ( -1.000000000000000000, 0.000000000000000000, 3.614007241618347908E-17 ) ) ;
#49286 =( BOUNDED_CURVE ( )  B_SPLINE_CURVE ( 2, ( #62292, #52627, #8874, #18214, #47787, #3745, #23367, #42965, #23677 ),
 .UNSPECIFIED., .F., .F. ) 
 B_SPLINE_CURVE_WITH_KNOTS ( ( 3, 2, 2, 2, 3 ),
 ( 0.5604166666666666741, 0.5611111111111111160, 0.5625000000000000000, 0.5638888888888888840, 0.5645833333333333259 ),
 .UNSPECIFIED. ) 
 CURVE ( )  GEOMETRIC_REPRESENTATION_ITEM ( )  RATIONAL_B_SPLINE_CURVE ( ( 0.9330127018922194093, 0.9330127018922194093, 1.000000000000000000, 0.8660254037844387076, 1.000000000000000000, 0.8660254037844387076, 1.000000000000000000, 0.9330127018922194093, 0.9330127018922194093 ) ) 
 REPRESENTATION_ITEM ( '' )  );
#49287 = CARTESIAN_POINT ( 'NONE',  ( 2.500000000000002220, -31.54166666393548724, 4.330127018922192761 ) ) ;
#49288 = CARTESIAN_POINT ( 'NONE',  ( 9.457646018065525792E-16, -57.31249999863440081, 5.148502694627439702 ) ) ;
#49289 = CARTESIAN_POINT ( 'NONE',  ( -3.152548672688508926E-16, -2.812499998634407028, -5.148502694627439702 ) ) ;
#49290 = VERTEX_POINT ( 'NONE', #7788 ) ;
#49291 = CARTESIAN_POINT ( 'NONE',  ( -6.972266317189433020E-16, -20.24999999999999289, -5.000000000000000000 ) ) ;
#49292 = CARTESIAN_POINT ( 'NONE',  ( 3.061616997868383141E-16, -141.7500000000000284, -5.000000000000000000 ) ) ;
#49293 = CARTESIAN_POINT ( 'NONE',  ( -4.458734124999999437, 13.60416666803226349, -2.574251347313719407 ) ) ;
#49294 = CARTESIAN_POINT ( 'NONE',  ( -55.35523342533222291, -139.3125000013656063, 4.444560631937231499 ) ) ;
#49295 = CARTESIAN_POINT ( 'NONE',  ( 1.339745962155615144, -27.58034179853028789, 4.999999999999999112 ) ) ;
#49296 = CARTESIAN_POINT ( 'NONE',  ( -4.458734125000000326, -166.8750000013656063, 1.846868145590734089 ) ) ;
#49297 = ORIENTED_EDGE ( 'NONE', *, *, #10253, .F. ) ;
#49298 = CARTESIAN_POINT ( 'NONE',  ( 4.458734124999998549, -81.72916666530106511, -2.574251347313721627 ) ) ;
#49299 = CARTESIAN_POINT ( 'NONE',  ( 1.975475456537005874E-15, -51.62499999726880873, 5.000000000000000000 ) ) ;
#49300 = CARTESIAN_POINT ( 'NONE',  ( -2.229367062500000163, -0.4791666653010707710, -3.861377020970580443 ) ) ;
#49301 = CARTESIAN_POINT ( 'NONE',  ( -5.000000000000000000, -86.00000000000000000, 0.000000000000000000 ) ) ;
#49302 = CARTESIAN_POINT ( 'NONE',  ( 1.975475456537005874E-15, 2.249999999999999556, 5.000000000000000000 ) ) ;
#49303 = CARTESIAN_POINT ( 'NONE',  ( 2.229367062499998831, -66.89583333196773651, -3.861377020970580887 ) ) ;
#49304 = CARTESIAN_POINT ( 'NONE',  ( 1.060575238724906964E-15, -23.62499999726881228, 5.773502691896257311 ) ) ;
#49305 = CARTESIAN_POINT ( 'NONE',  ( 1.975475456537005874E-15, -20.74999999999999645, 5.000000000000000000 ) ) ;
#49306 = CARTESIAN_POINT ( 'NONE',  ( -3.152548672688508926E-16, 27.43750000136559564, -5.148502694627439702 ) ) ;
#49307 = CARTESIAN_POINT ( 'NONE',  ( 5.000000000000000000, -49.41666666666666430, -2.886751345948130876 ) ) ;
#49308 = CARTESIAN_POINT ( 'NONE',  ( -4.458734124999999437, -45.31249999863440081, 0.000000000000000000 ) ) ;
#49309 = CARTESIAN_POINT ( 'NONE',  ( 2.229367062500001939, -33.22916666530106511, 3.861377020970579999 ) ) ;
#49310 = CARTESIAN_POINT ( 'NONE',  ( -2.229367062500000163, 7.270833334698929562, -3.861377020970580443 ) ) ;
#49311 = DIRECTION ( 'NONE',  ( -0.000000000000000000, 1.000000000000000000, -0.000000000000000000 ) ) ;
#49312 = CARTESIAN_POINT ( 'NONE',  ( 2.499999999999998668, 21.66666666666666785, -4.330127018922193649 ) ) ;
#49313 = CARTESIAN_POINT ( 'NONE',  ( 5.000000000000000000, -148.1250000027312126, 0.000000000000000000 ) ) ;
#49314 = CARTESIAN_POINT ( 'NONE',  ( -6.127431526422343306E-17, 9.147862274876549904, -8.047472243342932430 ) ) ;
#49315 = CARTESIAN_POINT ( 'NONE',  ( -2.229367062499996610, -37.14583333196773651, 3.861377020970582219 ) ) ;
#49316 = CARTESIAN_POINT ( 'NONE',  ( -5.000000000000000000, -75.87499999726880162, 0.000000000000000000 ) ) ;
#49317 = CARTESIAN_POINT ( 'NONE',  ( -57.19623071787017210, -143.6250000013655779, 4.297418129356382899 ) ) ;
#49318 = CARTESIAN_POINT ( 'NONE',  ( -5.000000000000000000, -142.5000000000000284, -6.123233995736766282E-16 ) ) ;
#49319 = CARTESIAN_POINT ( 'NONE',  ( -2.499999999999999556, -7.216878364870334295, -7.063244554130003294 ) ) ;
#49320 = CARTESIAN_POINT ( 'NONE',  ( -2.229367062500000163, -80.72916666530106511, -3.861377020970580443 ) ) ;
#49321 = CARTESIAN_POINT ( 'NONE',  ( -3.152801135295367096, -166.3125000013656063, -3.152801135295367541 ) ) ;
#49322 = CARTESIAN_POINT ( 'NONE',  ( -3.152548672688508926E-16, -36.56249999863441502, -5.148502694627439702 ) ) ;
#49323 = CARTESIAN_POINT ( 'NONE',  ( 2.499999999999998668, 18.79166666939785202, -4.330127018922193649 ) ) ;
#49324 = CYLINDRICAL_SURFACE ( 'NONE', #37976, 5.000000000000000000 ) ;
#49325 = CARTESIAN_POINT ( 'NONE',  ( 2.499999999999998668, -23.33333333333333215, -4.330127018922193649 ) ) ;
#49326 = CARTESIAN_POINT ( 'NONE',  ( -4.458734125000000326, -142.0000000013655495, -1.846868145590735644 ) ) ;
#49327 = ORIENTED_EDGE ( 'NONE', *, *, #7055, .F. ) ;
#49328 = CARTESIAN_POINT ( 'NONE',  ( -4.458734124999999437, 29.35416666803225993, -2.574251347313719407 ) ) ;
#49329 = ORIENTED_EDGE ( 'NONE', *, *, #22300, .T. ) ;
#49330 = CARTESIAN_POINT ( 'NONE',  ( -2.229367062499996610, -64.39583333196773651, 3.861377020970582219 ) ) ;
#49331 = CARTESIAN_POINT ( 'NONE',  ( -2.500000000000000444, 19.95833333606451987, -4.330127018922193649 ) ) ;
#49332 = CARTESIAN_POINT ( 'NONE',  ( 2.500000000000002220, -90.54166666393547303, 4.330127018922192761 ) ) ;
#49333 = CARTESIAN_POINT ( 'NONE',  ( -5.000000000000000000, 12.00000000000000000, 0.000000000000000000 ) ) ;
#49334 = CARTESIAN_POINT ( 'NONE',  ( -4.458734124999999437, -53.31249999863439371, 0.000000000000000000 ) ) ;
#49335 = CARTESIAN_POINT ( 'NONE',  ( 4.458734124999998549, -5.729166665301072214, -2.574251347313721627 ) ) ;
#49336 = CARTESIAN_POINT ( 'NONE',  ( -4.999999999999998224, 4.208333336064518093, 2.886751345948131764 ) ) ;
#49337 = CARTESIAN_POINT ( 'NONE',  ( -5.000000000000000000, -9.000000000000001776, 0.000000000000000000 ) ) ;
#49338 = CARTESIAN_POINT ( 'NONE',  ( -2.499999999999996447, 0.1666666666666656582, 4.330127018922195425 ) ) ;
#49339 = CARTESIAN_POINT ( 'NONE',  ( 1.975475456537005874E-15, -66.62499999726881583, 5.000000000000000000 ) ) ;
#49341 = CARTESIAN_POINT ( 'NONE',  ( 2.229367062499998831, -21.64583333196774007, -3.861377020970580887 ) ) ;
#49340 = CARTESIAN_POINT ( 'NONE',  ( 6.123233995736766282E-16, -120.0000000000000000, -5.000000000000000000 ) ) ;
#49342 = CARTESIAN_POINT ( 'NONE',  ( 1.975475456537005874E-15, -97.62499999726880162, 5.000000000000000000 ) ) ;
#49343 = CARTESIAN_POINT ( 'NONE',  ( 4.458734125000001214, -55.89583333196773651, 2.574251347313718519 ) ) ;
#49344 = CARTESIAN_POINT ( 'NONE',  ( -1.846868145590734756, -155.3750000013656347, -4.458734125000000326 ) ) ;
#49345 = VECTOR ( 'NONE', #59707, 1000.000000000000000 ) ;
#49346 = CARTESIAN_POINT ( 'NONE',  ( 1.060575238724906964E-15, -54.62499999726880873, 5.773502691896257311 ) ) ;
#49347 = ORIENTED_EDGE ( 'NONE', *, *, #37350, .F. ) ;
#49348 = CARTESIAN_POINT ( 'NONE',  ( -1.049326080737009628E-13, -4.750000000000003553, 5.000000000000000000 ) ) ;
#49349 = CARTESIAN_POINT ( 'NONE',  ( -2.229367062499996610, 4.604166668032261711, 3.861377020970582219 ) ) ;
#49350 = ORIENTED_EDGE ( 'NONE', *, *, #7490, .T. ) ;
#49352 = CARTESIAN_POINT ( 'NONE',  ( 0.000000000000000000, -170.0000000000000000, 0.000000000000000000 ) ) ;
#49351 = CARTESIAN_POINT ( 'NONE',  ( 0.000000000000000000, -120.0000000000000000, 0.000000000000000000 ) ) ;
#49353 = CARTESIAN_POINT ( 'NONE',  ( 4.458734124999999437, -156.5000000013656347, 1.846868145590737864 ) ) ;
#49354 = VERTEX_POINT ( 'NONE', #32535 ) ;
#49355 = CARTESIAN_POINT ( 'NONE',  ( -6.972266317189433020E-16, -23.12499999726880873, -5.000000000000000000 ) ) ;
#49356 = CARTESIAN_POINT ( 'NONE',  ( -51.19402409849444524, -130.5000000000000284, -3.242614290531456334 ) ) ;
#49357 = CARTESIAN_POINT ( 'NONE',  ( 1.975475456537005874E-15, -80.62499999726881583, 5.000000000000000000 ) ) ;
#49358 = CARTESIAN_POINT ( 'NONE',  ( -4.458734124999999437, -42.64583333196773651, -2.574251347313719407 ) ) ;
#49359 = VERTEX_POINT ( 'NONE', #17115 ) ;
#49360 =( BOUNDED_CURVE ( )  B_SPLINE_CURVE ( 2, ( #55555, #1523, #30446, #50394, #20173, #11467, #6030, #25313, #15665 ),
 .UNSPECIFIED., .F., .F. ) 
 B_SPLINE_CURVE_WITH_KNOTS ( ( 3, 2, 2, 2, 3 ),
 ( 0.8125000000000000000, 0.8130952380952380931, 0.8142857142857142794, 0.8154761904761904656, 0.8160714285714285587 ),
 .UNSPECIFIED. ) 
 CURVE ( )  GEOMETRIC_REPRESENTATION_ITEM ( )  RATIONAL_B_SPLINE_CURVE ( ( 0.9330127018922194093, 0.9330127018922194093, 1.000000000000000000, 0.8660254037844387076, 1.000000000000000000, 0.8660254037844387076, 1.000000000000000000, 0.9330127018922194093, 0.9330127018922194093 ) ) 
 REPRESENTATION_ITEM ( '' )  );
#49361 = CARTESIAN_POINT ( 'NONE',  ( 5.000000000000000888, 9.541666669397852019, 2.886751345948126879 ) ) ;
#49362 = CARTESIAN_POINT ( 'NONE',  ( 2.229367062500001939, 12.02083333469892601, 3.861377020970579999 ) ) ;
#49363 = CARTESIAN_POINT ( 'NONE',  ( -5.000000000000000000, -9.874999997268815832, 0.000000000000000000 ) ) ;
#49364 = ORIENTED_EDGE ( 'NONE', *, *, #3325, .F. ) ;
#49365 = CARTESIAN_POINT ( 'NONE',  ( -3.152548672688508926E-16, 29.43750000136559564, -5.148502694627439702 ) ) ;
#49366 = CARTESIAN_POINT ( 'NONE',  ( -57.19623071787017210, -152.3750000013656063, 4.297418129356382899 ) ) ;
#49367 = CARTESIAN_POINT ( 'NONE',  ( 1.339745962155612702, -44.29465819873851729, -5.000000000000000000 ) ) ;
#49368 = LINE ( 'NONE', #9487, #29501 ) ;
#49369 = CARTESIAN_POINT ( 'NONE',  ( -5.000000000000000000, 23.91666666666666785, -2.886751345948128211 ) ) ;
#49370 = CARTESIAN_POINT ( 'NONE',  ( 2.229367062500001939, -64.97916666530106511, 3.861377020970579999 ) ) ;
#49371 = CARTESIAN_POINT ( 'NONE',  ( -1.339745962155610925, -61.66965819600733312, 5.000000000000000000 ) ) ;
#49372 = CARTESIAN_POINT ( 'NONE',  ( 9.457646018065525792E-16, 19.93750000136559208, 5.148502694627439702 ) ) ;
#49373 = CARTESIAN_POINT ( 'NONE',  ( -6.972266317189433020E-16, -33.24999999999999289, -5.000000000000000000 ) ) ;
#49374 = CARTESIAN_POINT ( 'NONE',  ( 9.457646018065525792E-16, -49.31249999863441502, 5.148502694627439702 ) ) ;
#49375 = CARTESIAN_POINT ( 'NONE',  ( -4.999999999999999112, -6.791666663935481907, 2.886751345948131764 ) ) ;
#49376 = CARTESIAN_POINT ( 'NONE',  ( -2.499999999999996447, 5.166666666666666963, 4.330127018922195425 ) ) ;
#49377 = DIRECTION ( 'NONE',  ( 0.000000000000000000, -1.000000000000000000, 0.000000000000000000 ) ) ;
#49378 = DIRECTION ( 'NONE',  ( 0.000000000000000000, 0.000000000000000000, 1.000000000000000000 ) ) ;
#49379 = CARTESIAN_POINT ( 'NONE',  ( -4.458734124999999437, -107.3124999986343937, 0.000000000000000000 ) ) ;
#49380 = AXIS2_PLACEMENT_3D ( 'NONE', #57953, #13572, #32550 ) ;
#49381 = EDGE_CURVE ( 'NONE', #21692, #34622, #37457, .T. ) ;
#49382 = CARTESIAN_POINT ( 'NONE',  ( -4.458734124999997661, -14.47916666530107221, 2.574251347313722516 ) ) ;
#49383 = EDGE_LOOP ( 'NONE', ( #40336, #49841, #29578, #50395 ) ) ;
#49384 = CARTESIAN_POINT ( 'NONE',  ( -2.071067811865391128, -143.8125000027312126, -5.000000000000086153 ) ) ;
#49385 = CARTESIAN_POINT ( 'NONE',  ( 2.229367062499998831, -99.64583333196773651, -3.861377020970580887 ) ) ;
#49386 = CARTESIAN_POINT ( 'NONE',  ( -2.071067811865478170, -161.4375000027312410, 5.000000000000000000 ) ) ;
#49387 = CARTESIAN_POINT ( 'NONE',  ( 4.458734124999998549, -94.97916666530106511, -2.574251347313721627 ) ) ;
#49388 = VECTOR ( 'NONE', #39274, 1000.000000000000000 ) ;
#49389 = CARTESIAN_POINT ( 'NONE',  ( 5.000000000000000000, -163.1875000027312126, 2.071067811865478614 ) ) ;
#49390 = CARTESIAN_POINT ( 'NONE',  ( -5.000000000000000000, -59.95833333060215153, -2.886751345948128211 ) ) ;
#49391 = CARTESIAN_POINT ( 'NONE',  ( 0.000000000000000000, -120.0000000000000000, 0.000000000000000000 ) ) ;
#49392 = CARTESIAN_POINT ( 'NONE',  ( -57.19623071787017210, -125.3750000013656205, 4.297418129356382899 ) ) ;
#49393 = CARTESIAN_POINT ( 'NONE',  ( -52.80376928212989185, -147.8750000013655779, -4.297418129356378458 ) ) ;
#49394 = CARTESIAN_POINT ( 'NONE',  ( -4.458734124999999437, -17.39583333196773651, -2.574251347313719407 ) ) ;
#49395 = CARTESIAN_POINT ( 'NONE',  ( -4.458734124999998549, 6.520833334698930450, 2.574251347313722516 ) ) ;
#49396 = CARTESIAN_POINT ( 'NONE',  ( -4.458734124999999437, -56.56249999863440081, 0.000000000000000000 ) ) ;
#49397 = CARTESIAN_POINT ( 'NONE',  ( 0.000000000000000000, -170.0000000000000000, 5.000000000000000000 ) ) ;
#49398 = CARTESIAN_POINT ( 'NONE',  ( 4.458734125000000326, -20.89583333196774007, 2.574251347313718519 ) ) ;
#49399 = CYLINDRICAL_SURFACE ( 'NONE', #16865, 5.000000000000000000 ) ;
#49400 = CARTESIAN_POINT ( 'NONE',  ( 3.535533905932738197, -155.8750000000000000, -3.535533905932738197 ) ) ;
#49401 = CARTESIAN_POINT ( 'NONE',  ( 5.000000000000000000, -4.416666666666666075, -2.886751345948129988 ) ) ;
#49402 = ORIENTED_EDGE ( 'NONE', *, *, #15415, .F. ) ;
#49403 = CARTESIAN_POINT ( 'NONE',  ( -4.458734124999999437, -46.64583333196774362, -2.574251347313719407 ) ) ;
#49404 = CARTESIAN_POINT ( 'NONE',  ( -5.000000000000000000, 25.91666666666666430, -2.886751345948128211 ) ) ;
#49405 = CARTESIAN_POINT ( 'NONE',  ( -2.499999999999996447, -8.833333333333332149, 4.330127018922195425 ) ) ;
#49406 = CARTESIAN_POINT ( 'NONE',  ( 5.000000000000000000, 29.50000000000000000, -6.123233995736766282E-16 ) ) ;
#49407 = CARTESIAN_POINT ( 'NONE',  ( 2.229367062499998831, -91.64583333196773651, -3.861377020970580887 ) ) ;
#49408 = CARTESIAN_POINT ( 'NONE',  ( 4.458734124999998549, 21.02083333469892779, -2.574251347313721627 ) ) ;
#49409 = CARTESIAN_POINT ( 'NONE',  ( 9.457646018065525792E-16, 10.93750000136559208, 5.148502694627439702 ) ) ;
#49410 = CARTESIAN_POINT ( 'NONE',  ( -1.339745962155610925, -6.794658198738519062, 5.000000000000000000 ) ) ;
#49411 = CARTESIAN_POINT ( 'NONE',  ( 2.500000000000002220, -82.66666666666667140, 4.330127018922192761 ) ) ;
#49412 = CARTESIAN_POINT ( 'NONE',  ( 2.229367062499998831, 22.10416666803225993, -3.861377020970580887 ) ) ;
#49413 = CARTESIAN_POINT ( 'NONE',  ( -3.535250795749689387E-16, -76.24999999999998579, -5.773502691896257311 ) ) ;
#49414 =( BOUNDED_CURVE ( )  B_SPLINE_CURVE ( 2, ( #16942, #2791, #46210, #61333, #6659, #2172, #21778, #36555, #26266 ),
 .UNSPECIFIED., .F., .F. ) 
 B_SPLINE_CURVE_WITH_KNOTS ( ( 3, 2, 2, 2, 3 ),
 ( 0.3446428571428571397, 0.3452380952380952328, 0.3464285714285714191, 0.3476190476190476053, 0.3482142857142856984 ),
 .UNSPECIFIED. ) 
 CURVE ( )  GEOMETRIC_REPRESENTATION_ITEM ( )  RATIONAL_B_SPLINE_CURVE ( ( 0.9330127018922194093, 0.9330127018922194093, 1.000000000000000000, 0.8660254037844387076, 1.000000000000000000, 0.8660254037844387076, 1.000000000000000000, 0.9330127018922194093, 0.9330127018922194093 ) ) 
 REPRESENTATION_ITEM ( '' )  );
#49415 = CARTESIAN_POINT ( 'NONE',  ( 2.499999999999998668, 6.791666669397851130, -4.330127018922193649 ) ) ;
#49416 = ORIENTED_EDGE ( 'NONE', *, *, #12508, .T. ) ;
#49417 = FACE_OUTER_BOUND ( 'NONE', #25121, .T. ) ;
#49418 = ORIENTED_EDGE ( 'NONE', *, *, #40828, .F. ) ;
#49419 = CARTESIAN_POINT ( 'NONE',  ( -1.339745962155613812, -104.2053418012614827, -5.000000000000000000 ) ) ;
#49420 = CARTESIAN_POINT ( 'NONE',  ( -4.458734124999999437, -40.39583333196773651, -2.574251347313719407 ) ) ;
#49421 = CARTESIAN_POINT ( 'NONE',  ( 1.060575238724906964E-15, -39.62499999726880873, 5.773502691896257311 ) ) ;
#49422 = VERTEX_POINT ( 'NONE', #28649 ) ;
#49423 = CARTESIAN_POINT ( 'NONE',  ( -50.70258187064364108, -148.3750000013656063, 2.196230717870141014 ) ) ;
#49424 = CARTESIAN_POINT ( 'NONE',  ( -4.458734124999999437, -14.31249999863440436, 0.000000000000000000 ) ) ;
#49426 = ORIENTED_EDGE ( 'NONE', *, *, #2713, .T. ) ;
#49425 = CARTESIAN_POINT ( 'NONE',  ( -4.458734124999999437, -12.64583333196774007, -2.574251347313719407 ) ) ;
#49427 = CARTESIAN_POINT ( 'NONE',  ( 5.000000000000000888, -82.58333333333332860, 2.886751345948126879 ) ) ;
#49428 = CARTESIAN_POINT ( 'NONE',  ( -6.972266317189433020E-16, 0.8750000027311866102, -5.000000000000000000 ) ) ;
#49429 = CARTESIAN_POINT ( 'NONE',  ( 9.457646018065525792E-16, -64.31249999863440792, 5.148502694627439702 ) ) ;
#49430 = CARTESIAN_POINT ( 'NONE',  ( 5.000000000000000888, -82.45833333060214443, 2.886751345948126879 ) ) ;
#49432 = EDGE_LOOP ( 'NONE', ( #6518, #28466, #22792, #51607 ) ) ;
#49431 = FACE_OUTER_BOUND ( 'NONE', #57272, .T. ) ;
#49433 = AXIS2_PLACEMENT_3D ( 'NONE', #4561, #38653, #23876 ) ;
#49434 = CARTESIAN_POINT ( 'NONE',  ( -55.39835681537999790, -143.8750000000000284, 4.984105922594378235 ) ) ;
#49435 = EDGE_CURVE ( 'NONE', #29985, #24352, #39557, .T. ) ;
#49436 = CARTESIAN_POINT ( 'NONE',  ( -4.458734124999999437, -29.56249999863440436, 0.000000000000000000 ) ) ;
#49437 = DIRECTION ( 'NONE',  ( 0.000000000000000000, 0.000000000000000000, 1.000000000000000000 ) ) ;
#49438 = EDGE_LOOP ( 'NONE', ( #8472, #46838, #4532, #3625 ) ) ;
#49439 = CONTEXT_DEPENDENT_SHAPE_REPRESENTATION ( #45414, #57925 ) ;
#49440 = CARTESIAN_POINT ( 'NONE',  ( 4.458734124999999437, -163.6875000013655779, 0.000000000000000000 ) ) ;
#49441 = CARTESIAN_POINT ( 'NONE',  ( -2.229367062500000163, -106.7291666653010651, -3.861377020970580443 ) ) ;
#49442 = CARTESIAN_POINT ( 'NONE',  ( 2.071067811865560326, -147.8125000000000000, -4.999999999999914735 ) ) ;
#49443 = ORIENTED_EDGE ( 'NONE', *, *, #6409, .T. ) ;
#49444 = CARTESIAN_POINT ( 'NONE',  ( -57.89159099828107458, -147.9375000013656063, -3.393966926194107447 ) ) ;
#49445 = CARTESIAN_POINT ( 'NONE',  ( -4.458734124999999437, -73.56249999863439371, 0.000000000000000000 ) ) ;
#49446 = CARTESIAN_POINT ( 'NONE',  ( -60.14911071818854538, -136.1875000027312126, 1.666127454062681368 ) ) ;
#49447 = CARTESIAN_POINT ( 'NONE',  ( -2.229367062499996610, -46.14583333196774362, 3.861377020970582219 ) ) ;
#49448 = CARTESIAN_POINT ( 'NONE',  ( 4.458734124999999437, -145.6250000013655779, -1.846868145590734978 ) ) ;
#49449 = CARTESIAN_POINT ( 'NONE',  ( -7.500000000000667910, 3.157052757790226316, -7.642767288269818771 ) ) ;
#49450 = CARTESIAN_POINT ( 'NONE',  ( -1.339745962155613146, 28.20534180126148271, 5.000000000000000000 ) ) ;
#49451 = CARTESIAN_POINT ( 'NONE',  ( 4.458734124999999437, -14.81249999863440436, -5.460374474430324690E-16 ) ) ;
#49452 = CARTESIAN_POINT ( 'NONE',  ( 1.060575238724906964E-15, -101.7500000000000000, 5.773502691896257311 ) ) ;
#49453 = VERTEX_POINT ( 'NONE', #18993 ) ;
#49454 = EDGE_CURVE ( 'NONE', #4902, #20671, #63394, .T. ) ;
#49455 = CARTESIAN_POINT ( 'NONE',  ( -58.24261429053147765, -143.3750000027312126, -3.805975901505573855 ) ) ;
#49456 = CARTESIAN_POINT ( 'NONE',  ( -4.458734124999998549, -32.47916666530107221, 2.574251347313722516 ) ) ;
#49457 = EDGE_CURVE ( 'NONE', #13616, #43111, #58561, .T. ) ;
#49458 = CARTESIAN_POINT ( 'NONE',  ( -3.535250795749689387E-16, 4.875000002731184168, -5.773502691896257311 ) ) ;
#49459 = CARTESIAN_POINT ( 'NONE',  ( -6.972266317189433020E-16, 25.74999999999999645, -5.000000000000000000 ) ) ;
#49460 = CARTESIAN_POINT ( 'NONE',  ( -54.64476657466781973, -134.8125000013656063, -4.444560631937228834 ) ) ;
#49461 = CARTESIAN_POINT ( 'NONE',  ( -4.458734124999998549, -75.47916666530107932, 2.574251347313722516 ) ) ;
#49462 = CARTESIAN_POINT ( 'NONE',  ( -51.19402409849444524, -146.6250000027312126, -3.242614290531456334 ) ) ;
#49463 = CARTESIAN_POINT ( 'NONE',  ( 1.975475456537005874E-15, -68.74999999999998579, 5.000000000000000000 ) ) ;
#49464 =( BOUNDED_CURVE ( )  B_SPLINE_CURVE ( 2, ( #59918, #15839, #6513, #1066, #34820, #11319, #16473, #736, #40907 ),
 .UNSPECIFIED., .F., .F. ) 
 B_SPLINE_CURVE_WITH_KNOTS ( ( 3, 2, 2, 2, 3 ),
 ( 0.8660714285714286031, 0.8666666666666666963, 0.8678571428571428825, 0.8690476190476190688, 0.8696428571428571619 ),
 .UNSPECIFIED. ) 
 CURVE ( )  GEOMETRIC_REPRESENTATION_ITEM ( )  RATIONAL_B_SPLINE_CURVE ( ( 0.9330127018922194093, 0.9330127018922194093, 1.000000000000000000, 0.8660254037844387076, 1.000000000000000000, 0.8660254037844387076, 1.000000000000000000, 0.9330127018922194093, 0.9330127018922194093 ) ) 
 REPRESENTATION_ITEM ( '' )  );
#49465 = CARTESIAN_POINT ( 'NONE',  ( 4.458734124999999437, 1.937500001365593416, -5.460374474430324690E-16 ) ) ;
#49466 = ORIENTED_EDGE ( 'NONE', *, *, #24133, .F. ) ;
#49467 = CARTESIAN_POINT ( 'NONE',  ( -55.00000000000002132, -155.0000000000000284, 1.734723475976807094E-15 ) ) ;
#49468 = CARTESIAN_POINT ( 'NONE',  ( -4.999999999999998224, -75.91666666666665719, 2.886751345948131764 ) ) ;
#49470 = CARTESIAN_POINT ( 'NONE',  ( 2.229367062499998831, -31.64583333196773651, -3.861377020970580887 ) ) ;
#49469 = CARTESIAN_POINT ( 'NONE',  ( 5.000000000000000888, -98.58333333333332860, 2.886751345948126879 ) ) ;
#49471 = CARTESIAN_POINT ( 'NONE',  ( 1.975475456537005874E-15, -95.75000000000000000, 5.000000000000000000 ) ) ;
#49472 = CARTESIAN_POINT ( 'NONE',  ( -4.458734124999998549, -81.47916666530106511, 2.574251347313722516 ) ) ;
#49473 = CARTESIAN_POINT ( 'NONE',  ( 2.229367062499998831, 17.10416666803225993, -3.861377020970580887 ) ) ;
#49474 = CARTESIAN_POINT ( 'NONE',  ( -5.000000000000000000, 23.12500000273118417, 0.000000000000000000 ) ) ;
#49475 = EDGE_CURVE ( 'NONE', #36935, #59502, #4840, .T. ) ;
#49476 = CARTESIAN_POINT ( 'NONE',  ( -50.40829686548195099, -136.0000000013656063, -1.485763867205728284 ) ) ;
#49477 = CARTESIAN_POINT ( 'NONE',  ( 2.229367062499998831, -1.645833331967737401, -3.861377020970580887 ) ) ;
#49478 = CARTESIAN_POINT ( 'NONE',  ( 2.229367062499998831, 24.10416666803225993, -3.861377020970580887 ) ) ;
#49479 = CARTESIAN_POINT ( 'NONE',  ( -3.152548672688508926E-16, -42.81249999863440081, -5.148502694627439702 ) ) ;
#49480 = CARTESIAN_POINT ( 'NONE',  ( 2.499999999999998668, -105.3333333333333286, -4.330127018922193649 ) ) ;
#49481 = CARTESIAN_POINT ( 'NONE',  ( 2.229367062499998831, 3.354166668032259935, -3.861377020970580887 ) ) ;
#49482 = VERTEX_POINT ( 'NONE', #34411 ) ;
#49483 = CARTESIAN_POINT ( 'NONE',  ( 4.458734124999998549, -28.97916666530108287, -2.574251347313721627 ) ) ;
#49484 = CARTESIAN_POINT ( 'NONE',  ( 4.458734125000001214, -67.89583333196773651, 2.574251347313718519 ) ) ;
#49485 = CARTESIAN_POINT ( 'NONE',  ( -3.535250795749689387E-16, -107.1249999972687874, -5.773502691896257311 ) ) ;
#49486 = CARTESIAN_POINT ( 'NONE',  ( -2.229367062499996610, 23.85416666803225993, 3.861377020970582219 ) ) ;
#49487 = ADVANCED_FACE ( 'NONE', ( #23836 ), #44065, .T. ) ;
#49488 = DIRECTION ( 'NONE',  ( -0.000000000000000000, 1.000000000000000000, -0.000000000000000000 ) ) ;
#49489 = CARTESIAN_POINT ( 'NONE',  ( 4.458734124999999437, -74.06249999863440792, -5.460374474430324690E-16 ) ) ;
#49490 = CARTESIAN_POINT ( 'NONE',  ( 2.499999999999998668, -60.33333333333333570, -4.330127018922193649 ) ) ;
#49491 = CARTESIAN_POINT ( 'NONE',  ( -1.339745962155610925, -65.79465819873851729, 5.000000000000000000 ) ) ;
#49492 = CARTESIAN_POINT ( 'NONE',  ( 5.000000000000000888, 23.54166666939785202, 2.886751345948126879 ) ) ;
#49493 = EDGE_LOOP ( 'NONE', ( #36011, #15338, #48538, #61883 ) ) ;
#49494 = CARTESIAN_POINT ( 'NONE',  ( -5.000000000000000888, -140.4375000000000000, 2.071067811865474617 ) ) ;
#49495 = CARTESIAN_POINT ( 'NONE',  ( 2.500000000000002220, -67.66666666666667140, 4.330127018922192761 ) ) ;
#49496 = CARTESIAN_POINT ( 'NONE',  ( 2.499999999999998668, -20.33333333333333570, -4.330127018922193649 ) ) ;
#49497 = CARTESIAN_POINT ( 'NONE',  ( 2.229367062499998831, -21.64583333196774007, -3.861377020970580887 ) ) ;
#49498 = CARTESIAN_POINT ( 'NONE',  ( 9.457646018065525792E-16, -81.06249999863440792, 5.148502694627439702 ) ) ;
#49499 = CARTESIAN_POINT ( 'NONE',  ( 5.000000000000000888, -20.45833333060214798, 2.886751345948126879 ) ) ;
#49501 = EDGE_LOOP ( 'NONE', ( #11463, #60622, #6192, #29 ) ) ;
#49500 = CARTESIAN_POINT ( 'NONE',  ( -3.152548672688508926E-16, -48.56249999863440792, -5.148502694627439702 ) ) ;
#49502 = CARTESIAN_POINT ( 'NONE',  ( 1.339745962155615144, -70.58034179853028434, 4.999999999999999112 ) ) ;
#49503 = LINE ( 'NONE', #39208, #6625 ) ;
#49505 = ORIENTED_EDGE ( 'NONE', *, *, #52370, .F. ) ;
#49504 = CARTESIAN_POINT ( 'NONE',  ( 2.229367062499998831, 0.1041666680322607397, -3.861377020970580887 ) ) ;
#49506 = CARTESIAN_POINT ( 'NONE',  ( -52.80376928212989185, -148.8750000013656063, -4.297418129356378458 ) ) ;
#49507 = CARTESIAN_POINT ( 'NONE',  ( -5.000000000000000000, -68.08333333333332860, -2.886751345948128211 ) ) ;
#49508 = CARTESIAN_POINT ( 'NONE',  ( -1.846868145590737420, -153.0000000013656063, 4.458734124999999437 ) ) ;
#49509 = CARTESIAN_POINT ( 'NONE',  ( -2.229367062499996610, -41.39583333196773651, 3.861377020970582219 ) ) ;
#49510 = CARTESIAN_POINT ( 'NONE',  ( -6.972266317189433020E-16, -16.12499999726881228, -5.000000000000000000 ) ) ;
#49511 = CARTESIAN_POINT ( 'NONE',  ( 3.535533905932736864, -162.1250000000000284, 3.535533905932738641 ) ) ;
#49512 = DIRECTION ( 'NONE',  ( -0.000000000000000000, 1.000000000000000000, -0.000000000000000000 ) ) ;
#49513 = CARTESIAN_POINT ( 'NONE',  ( -56.48576386720575471, -128.0000000013656063, -4.591703134518078322 ) ) ;
#49514 = EDGE_CURVE ( 'NONE', #21194, #27082, #35772, .T. ) ;
#49515 = CARTESIAN_POINT ( 'NONE',  ( 4.458734125000001214, -10.14583333196773829, 2.574251347313718519 ) ) ;
#49516 = CARTESIAN_POINT ( 'NONE',  ( -2.229367062500000163, -43.72916666530106511, -3.861377020970580443 ) ) ;
#49517 = CARTESIAN_POINT ( 'NONE',  ( 0.000000000000000000, -170.0000000000000000, 0.000000000000000000 ) ) ;
#49518 = CARTESIAN_POINT ( 'NONE',  ( 4.458734125000000326, -146.3750000013655779, -1.846868145590734978 ) ) ;
#49519 = CARTESIAN_POINT ( 'NONE',  ( -4.458734124999998549, -90.47916666530106511, 2.574251347313722516 ) ) ;
#49520 = DIRECTION ( 'NONE',  ( -0.000000000000000000, 1.000000000000000000, -0.000000000000000000 ) ) ;
#49521 = VERTEX_POINT ( 'NONE', #38312 ) ;
#49522 = FACE_OUTER_BOUND ( 'NONE', #42388, .T. ) ;
#49523 = CARTESIAN_POINT ( 'NONE',  ( -3.152548672688508926E-16, 29.18750000136559208, -5.148502694627439702 ) ) ;
#49524 = CARTESIAN_POINT ( 'NONE',  ( -58.80597590150559739, -152.1250000027312126, 3.242614290531460330 ) ) ;
#49525 = CARTESIAN_POINT ( 'NONE',  ( 1.975475456537005874E-15, -38.75000000000000000, 5.000000000000000000 ) ) ;
#49526 = ORIENTED_EDGE ( 'NONE', *, *, #21949, .T. ) ;
#49527 = CARTESIAN_POINT ( 'NONE',  ( 2.229367062499998831, 2.354166668032262599, -3.861377020970580887 ) ) ;
#49528 = DIRECTION ( 'NONE',  ( -0.000000000000000000, 1.000000000000000000, -0.000000000000000000 ) ) ;
#49529 = CARTESIAN_POINT ( 'NONE',  ( -2.229367062500000163, -17.72916666530106866, -3.861377020970580443 ) ) ;
#49530 = EDGE_CURVE ( 'NONE', #1448, #26085, #4951, .T. ) ;
#49531 = CARTESIAN_POINT ( 'NONE',  ( 2.499999999999998668, 11.79166666939785202, -4.330127018922193649 ) ) ;
#49532 = CARTESIAN_POINT ( 'NONE',  ( 9.457646018065525792E-16, -5.062499998634401699, 5.148502694627439702 ) ) ;
#49533 = CARTESIAN_POINT ( 'NONE',  ( 2.499999999999998668, -55.20833333060214443, -4.330127018922193649 ) ) ;
#49534 = CARTESIAN_POINT ( 'NONE',  ( 4.458734124999999437, -148.3750000013655779, -1.846868145590734978 ) ) ;
#49535 = CARTESIAN_POINT ( 'NONE',  ( -2.229367062500000163, 23.27083333469892779, -3.861377020970580443 ) ) ;
#49536 = ORIENTED_EDGE ( 'NONE', *, *, #25677, .T. ) ;
#49537 = CARTESIAN_POINT ( 'NONE',  ( -2.229367062500000163, -96.47916666530105090, -3.861377020970580443 ) ) ;
#49538 = CARTESIAN_POINT ( 'NONE',  ( -5.000000000000000000, -148.5000000000000284, -6.123233995736766282E-16 ) ) ;
#49539 = CARTESIAN_POINT ( 'NONE',  ( 2.499999999999998668, -57.20833333060214443, -4.330127018922193649 ) ) ;
#49540 = CARTESIAN_POINT ( 'NONE',  ( 2.229367062500001939, -14.97916666530107399, 3.861377020970579999 ) ) ;
#49541 = CARTESIAN_POINT ( 'NONE',  ( 0.000000000000000000, -120.0000000000000000, 0.000000000000000000 ) ) ;
#49542 = CARTESIAN_POINT ( 'NONE',  ( 0.000000000000000000, -120.0000000000000000, 0.000000000000000000 ) ) ;
#49543 =( BOUNDED_CURVE ( )  B_SPLINE_CURVE ( 2, ( #54258, #25309, #24357, #58459, #9560, #63605, #20169, #58766, #24044 ),
 .UNSPECIFIED., .F., .F. ) 
 B_SPLINE_CURVE_WITH_KNOTS ( ( 3, 2, 2, 2, 3 ),
 ( 0.1803571428571428548, 0.1809523809523809479, 0.1821428571428571341, 0.1833333333333333204, 0.1839285714285714413 ),
 .UNSPECIFIED. ) 
 CURVE ( )  GEOMETRIC_REPRESENTATION_ITEM ( )  RATIONAL_B_SPLINE_CURVE ( ( 0.9330127018922194093, 0.9330127018922194093, 1.000000000000000000, 0.8660254037844387076, 1.000000000000000000, 0.8660254037844387076, 1.000000000000000000, 0.9330127018922178550, 0.9330127018922194093 ) ) 
 REPRESENTATION_ITEM ( '' )  );
#49544 = CARTESIAN_POINT ( 'NONE',  ( -59.59170313451811296, -151.5000000013655779, 1.485763867205729394 ) ) ;
#49545 = CARTESIAN_POINT ( 'NONE',  ( 5.000000000000000000, -41.37499999726880162, -6.123233995736766282E-16 ) ) ;
#49546 = CARTESIAN_POINT ( 'NONE',  ( -4.458734124999999437, 11.68750000136559564, 0.000000000000000000 ) ) ;
#49547 = CARTESIAN_POINT ( 'NONE',  ( 3.044556291839386294E-14, 11.87500000273118417, -5.000000000000000000 ) ) ;
#49548 = DIRECTION ( 'NONE',  ( -0.6485228581062915110, 0.000000000000000000, -0.7611951803011149931 ) ) ;
#49549 = CARTESIAN_POINT ( 'NONE',  ( -2.229367062499996610, 19.85416666803225993, 3.861377020970582219 ) ) ;
#49550 = CARTESIAN_POINT ( 'NONE',  ( 4.458734125000001214, -59.89583333196774362, 2.574251347313718519 ) ) ;
#49551 = ORIENTED_EDGE ( 'NONE', *, *, #62637, .F. ) ;
#49552 = CARTESIAN_POINT ( 'NONE',  ( -4.458734124999999437, -10.56249999863440792, 0.000000000000000000 ) ) ;
#49553 = CARTESIAN_POINT ( 'NONE',  ( -2.499999999999996447, 6.166666666666667851, 4.330127018922195425 ) ) ;
#49554 = CARTESIAN_POINT ( 'NONE',  ( -1.846868145590737420, -165.7500000013655495, 4.458734124999999437 ) ) ;
#49555 = CARTESIAN_POINT ( 'NONE',  ( -1.339745962155610925, -59.66965819600732601, 5.000000000000000000 ) ) ;
#49556 = CARTESIAN_POINT ( 'NONE',  ( 9.457646018065525792E-16, -55.06249999863439371, 5.148502694627439702 ) ) ;
#49557 = CARTESIAN_POINT ( 'NONE',  ( -2.500000000000000444, -87.04166666393547303, -4.330127018922193649 ) ) ;
#49558 = EDGE_CURVE ( 'NONE', #33932, #4271, #9086, .T. ) ;
#49559 = CARTESIAN_POINT ( 'NONE',  ( 2.229367062500001939, -33.97916666530107221, 3.861377020970579999 ) ) ;
#49560 = CYLINDRICAL_SURFACE ( 'NONE', #12403, 5.000000000000000000 ) ;
#49561 =( BOUNDED_CURVE ( )  B_SPLINE_CURVE ( 2, ( #38493, #5599, #17935, #4104, #24026, #23411, #13743, #30031, #33364 ),
 .UNSPECIFIED., .F., .F. ) 
 B_SPLINE_CURVE_WITH_KNOTS ( ( 3, 2, 2, 2, 3 ),
 ( 0.7767857142857143016, 0.7773809523809523947, 0.7785714285714285809, 0.7797619047619047672, 0.7803571428571428603 ),
 .UNSPECIFIED. ) 
 CURVE ( )  GEOMETRIC_REPRESENTATION_ITEM ( )  RATIONAL_B_SPLINE_CURVE ( ( 0.9330127018922194093, 0.9330127018922194093, 1.000000000000000000, 0.8660254037844387076, 1.000000000000000000, 0.8660254037844387076, 1.000000000000000000, 0.9330127018922194093, 0.9330127018922194093 ) ) 
 REPRESENTATION_ITEM ( '' )  );
#49562 = LINE ( 'NONE', #5821, #62510 ) ;
#49563 = CARTESIAN_POINT ( 'NONE',  ( 1.975475456537005874E-15, -88.62499999726880162, 5.000000000000000000 ) ) ;
#49564 = CARTESIAN_POINT ( 'NONE',  ( -4.458734124999999437, -153.2500000013656063, -1.846868145590735644 ) ) ;
#49565 = CARTESIAN_POINT ( 'NONE',  ( -2.499999999999996447, -40.83333333333333570, 4.330127018922195425 ) ) ;
#49566 = CARTESIAN_POINT ( 'NONE',  ( 2.500000000000002220, -86.54166666393547303, 4.330127018922192761 ) ) ;
#49567 = ORIENTED_EDGE ( 'NONE', *, *, #22999, .F. ) ;
#49568 = CARTESIAN_POINT ( 'NONE',  ( 2.229367062500001939, -100.9791666653010651, 3.861377020970579999 ) ) ;
#49569 = CARTESIAN_POINT ( 'NONE',  ( 4.458734124999999437, 1.937500001365593416, -5.460374474430324690E-16 ) ) ;
#49570 = CARTESIAN_POINT ( 'NONE',  ( 5.000000000000000000, -59.50000000000000000, -6.123233995736766282E-16 ) ) ;
#49571 = CARTESIAN_POINT ( 'NONE',  ( 1.060575238724906964E-15, -1.750000000000001554, 5.773502691896257311 ) ) ;
#49572 = CARTESIAN_POINT ( 'NONE',  ( -2.229367062499996610, -67.14583333196773651, 3.861377020970582219 ) ) ;
#49573 = FACE_OUTER_BOUND ( 'NONE', #27051, .T. ) ;
#49574 = CARTESIAN_POINT ( 'NONE',  ( -5.000000000000000000, -3.958333330602147537, -2.886751345948128211 ) ) ;
#49576 = ORIENTED_EDGE ( 'NONE', *, *, #8291, .T. ) ;
#49575 = CARTESIAN_POINT ( 'NONE',  ( -2.229367062499996610, -33.14583333196772941, 3.861377020970582219 ) ) ;
#49577 = CARTESIAN_POINT ( 'NONE',  ( -2.499999999999996447, -77.83333333333334281, 4.330127018922195425 ) ) ;
#49578 = FACE_OUTER_BOUND ( 'NONE', #14467, .T. ) ;
#49579 = ORIENTED_EDGE ( 'NONE', *, *, #27140, .F. ) ;
#49580 = CARTESIAN_POINT ( 'NONE',  ( 1.464175926609780648E-14, 24.74999999999999645, -5.000000000000000000 ) ) ;
#49581 = CARTESIAN_POINT ( 'NONE',  ( -5.000000000000000000, -48.08333333333332860, -2.886751345948128211 ) ) ;
#49583 = CARTESIAN_POINT ( 'NONE',  ( -4.458734124999999437, -27.56249999863440081, 0.000000000000000000 ) ) ;
#49582 = DIRECTION ( 'NONE',  ( 0.000000000000000000, 0.000000000000000000, 1.000000000000000000 ) ) ;
#49584 = CARTESIAN_POINT ( 'NONE',  ( 5.000000000000000000, -4.416666666666666075, -2.886751345948130876 ) ) ;
#49585 = CARTESIAN_POINT ( 'NONE',  ( -4.458734124999999437, -70.31249999863439371, 0.000000000000000000 ) ) ;
#49586 = CARTESIAN_POINT ( 'NONE',  ( -1.846868145590734756, -142.3750000013656063, -4.458734125000000326 ) ) ;
#49587 = CARTESIAN_POINT ( 'NONE',  ( 4.458734125000001214, -79.89583333196773651, 2.574251347313718519 ) ) ;
#49588 = CARTESIAN_POINT ( 'NONE',  ( -51.60603307380591787, -140.1875000013656063, -2.891590998281053704 ) ) ;
#49589 = CARTESIAN_POINT ( 'NONE',  ( 2.229367062499998831, -31.89583333196773651, -3.861377020970580887 ) ) ;
#49590 = CARTESIAN_POINT ( 'NONE',  ( 5.000000000000000000, -72.37499999726880162, -6.123233995736766282E-16 ) ) ;
#49592 = VERTEX_POINT ( 'NONE', #53413 ) ;
#49591 = EDGE_CURVE ( 'NONE', #44139, #13129, #63083, .T. ) ;
#49593 = EDGE_CURVE ( 'NONE', #47703, #2151, #13604, .T. ) ;
#49594 = CARTESIAN_POINT ( 'NONE',  ( 5.000000000000000000, -20.29166666393548368, -2.886751345948130876 ) ) ;
#49595 = ORIENTED_EDGE ( 'NONE', *, *, #6689, .T. ) ;
#49596 = CARTESIAN_POINT ( 'NONE',  ( 9.457646018065525792E-16, -73.31249999863440792, 5.148502694627439702 ) ) ;
#49597 = CARTESIAN_POINT ( 'NONE',  ( 1.975475456537005874E-15, -14.62499999726881228, 5.000000000000000000 ) ) ;
#49598 = EDGE_CURVE ( 'NONE', #7443, #25868, #13220, .T. ) ;
#49599 = VERTEX_POINT ( 'NONE', #45673 ) ;
#49600 = EDGE_CURVE ( 'NONE', #36859, #969, #35018, .T. ) ;
#49601 = CARTESIAN_POINT ( 'NONE',  ( -4.999999999999998224, -75.79166666393547303, 2.886751345948131764 ) ) ;
#49602 = CARTESIAN_POINT ( 'NONE',  ( 4.458734124999999437, -59.06249999863440081, -5.460374474430324690E-16 ) ) ;
#49603 = EDGE_CURVE ( 'NONE', #45427, #2557, #59522, .T. ) ;
#49604 = CARTESIAN_POINT ( 'NONE',  ( 4.458734124999998549, -5.979166665301073103, -2.574251347313721627 ) ) ;
#49605 = ORIENTED_EDGE ( 'NONE', *, *, #23885, .T. ) ;
#49606 = EDGE_CURVE ( 'NONE', #27699, #39231, #15659, .T. ) ;
#49607 = CARTESIAN_POINT ( 'NONE',  ( 0.000000000000000000, -120.0000000000000000, 0.000000000000000000 ) ) ;
#49608 = DIRECTION ( 'NONE',  ( 0.000000000000000000, 0.000000000000000000, 1.000000000000000000 ) ) ;
#49609 = EDGE_CURVE ( 'NONE', #8886, #43978, #6758, .T. ) ;
#49610 = CARTESIAN_POINT ( 'NONE',  ( -3.152548672688508926E-16, 11.43750000136559386, -5.148502694627439702 ) ) ;
#49611 = CARTESIAN_POINT ( 'NONE',  ( -58.39396692619412477, -142.4375000013656063, 2.891590998281057701 ) ) ;
#49612 = CARTESIAN_POINT ( 'NONE',  ( -2.499999999999996447, -0.8333333333333317050, 4.330127018922195425 ) ) ;
#49613 = CARTESIAN_POINT ( 'NONE',  ( -1.846868145590737420, -160.7500000013655779, 4.458734124999997661 ) ) ;
#49614 =( BOUNDED_CURVE ( )  B_SPLINE_CURVE ( 2, ( #3715, #38725, #23331, #53536, #8533, #23949, #42936, #43863, #29378 ),
 .UNSPECIFIED., .F., .F. ) 
 B_SPLINE_CURVE_WITH_KNOTS ( ( 3, 2, 2, 2, 3 ),
 ( 0.3017857142857142683, 0.3023809523809523614, 0.3035714285714285476, 0.3047619047619047894, 0.3053571428571428825 ),
 .UNSPECIFIED. ) 
 CURVE ( )  GEOMETRIC_REPRESENTATION_ITEM ( )  RATIONAL_B_SPLINE_CURVE ( ( 0.9330127018922194093, 0.9330127018922194093, 1.000000000000000000, 0.8660254037844387076, 1.000000000000000000, 0.8660254037844387076, 1.000000000000000000, 0.9330127018922194093, 0.9330127018922194093 ) ) 
 REPRESENTATION_ITEM ( '' )  );
#49615 = CARTESIAN_POINT ( 'NONE',  ( -55.00000000000002132, -155.0000000000000284, 1.734723475976807094E-15 ) ) ;
#49617 = ADVANCED_FACE ( 'NONE', ( #5479 ), #45989, .T. ) ;
#49616 = ORIENTED_EDGE ( 'NONE', *, *, #63433, .F. ) ;
#49618 = CARTESIAN_POINT ( 'NONE',  ( 2.229367062499998831, -83.64583333196773651, -3.861377020970580887 ) ) ;
#49619 = ADVANCED_FACE ( 'NONE', ( #25415 ), #45033, .T. ) ;
#49620 = CARTESIAN_POINT ( 'NONE',  ( 6.123233995736766282E-16, 30.00000000000000000, -5.000000000000000000 ) ) ;
#49621 = CARTESIAN_POINT ( 'NONE',  ( 9.457646018065525792E-16, 3.937500001365595192, 5.148502694627439702 ) ) ;
#49622 = CARTESIAN_POINT ( 'NONE',  ( 5.000000000000000888, -83.58333333333332860, 2.886751345948126879 ) ) ;
#49623 = CARTESIAN_POINT ( 'NONE',  ( 0.000000000000000000, -170.0000000000000000, 0.000000000000000000 ) ) ;
#49624 = CARTESIAN_POINT ( 'NONE',  ( -4.458734124999999437, -66.56249999863440792, 0.000000000000000000 ) ) ;
#49625 = CARTESIAN_POINT ( 'NONE',  ( 2.499999999999998668, -23.20833333060214443, -4.330127018922193649 ) ) ;
#49626 = CARTESIAN_POINT ( 'NONE',  ( -2.499999999999996447, -20.83333333333333570, 4.330127018922195425 ) ) ;
#49627 = CARTESIAN_POINT ( 'NONE',  ( 4.458734124999999437, 27.18750000136559564, -5.460374474430324690E-16 ) ) ;
#49628 = CARTESIAN_POINT ( 'NONE',  ( 1.975475456537005874E-15, -11.74999999999999645, 5.000000000000000000 ) ) ;
#49629 = LINE ( 'NONE', #30316, #47873 ) ;
#49630 = CARTESIAN_POINT ( 'NONE',  ( -4.458734124999998549, -45.22916666530106511, 2.574251347313722516 ) ) ;
#49631 = CARTESIAN_POINT ( 'NONE',  ( -3.152548672688508926E-16, -30.81249999863440436, -5.148502694627439702 ) ) ;
#49632 = CARTESIAN_POINT ( 'NONE',  ( -4.458734124999997661, 7.520833334698926009, 2.574251347313722516 ) ) ;
#49633 = CARTESIAN_POINT ( 'NONE',  ( 2.500000000000002220, 18.33333333333333215, 4.330127018922192761 ) ) ;
#49634 = CARTESIAN_POINT ( 'NONE',  ( 5.000000000000000888, -150.0625000027312126, -2.071067811865475505 ) ) ;
#49635 = CARTESIAN_POINT ( 'NONE',  ( 1.975475456537005874E-15, -54.62499999726880873, 5.000000000000000000 ) ) ;
#49636 = CARTESIAN_POINT ( 'NONE',  ( -2.229367062499996610, -38.14583333196773651, 3.861377020970582219 ) ) ;
#49637 = CARTESIAN_POINT ( 'NONE',  ( -2.500000000000000444, -75.04166666393547303, -4.330127018922193649 ) ) ;
#49638 = CARTESIAN_POINT ( 'NONE',  ( -50.70258187064364108, -145.3750000013656347, 2.196230717870141014 ) ) ;
#49639 = CARTESIAN_POINT ( 'NONE',  ( 0.000000000000000000, -170.0000000000000000, 0.000000000000000000 ) ) ;
#49640 = LINE ( 'NONE', #5577, #5934 ) ;
#49641 = CARTESIAN_POINT ( 'NONE',  ( 4.458734124999998549, -80.97916666530106511, -2.574251347313721627 ) ) ;
#49642 = CARTESIAN_POINT ( 'NONE',  ( 2.730187237215162345E-16, -166.4375000013655779, -4.458734124999999437 ) ) ;
#49643 = CARTESIAN_POINT ( 'NONE',  ( -3.535533905932738641, -160.3750000000000284, 3.535533905932737309 ) ) ;
#49644 = CARTESIAN_POINT ( 'NONE',  ( 2.499999999999998668, -45.20833333060214443, -4.330127018922193649 ) ) ;
#49645 = CARTESIAN_POINT ( 'NONE',  ( -2.499999999999996447, -28.83333333333333570, 4.330127018922195425 ) ) ;
#49646 = CARTESIAN_POINT ( 'NONE',  ( -4.458734125000001214, -142.8750000013656063, 1.846868145590734089 ) ) ;
#49647 = ORIENTED_EDGE ( 'NONE', *, *, #51601, .F. ) ;
#49648 = CARTESIAN_POINT ( 'NONE',  ( 2.229367062500001939, 27.77083333469892779, 3.861377020970579999 ) ) ;
#49649 = ORIENTED_EDGE ( 'NONE', *, *, #12582, .F. ) ;
#49650 = CARTESIAN_POINT ( 'NONE',  ( -3.152548672688508926E-16, -60.81249999863440081, -5.148502694627439702 ) ) ;
#49651 = SHAPE_REPRESENTATION ( 'coupler', ( #43054 ), #60569 ) ;
#49652 = CARTESIAN_POINT ( 'NONE',  ( 1.060575238724906964E-15, 23.37500000273118062, 5.773502691896257311 ) ) ;
#49653 = CARTESIAN_POINT ( 'NONE',  ( 0.000000000000000000, -170.0000000000000000, 0.000000000000000000 ) ) ;
#49654 = CARTESIAN_POINT ( 'NONE',  ( -2.499999999999996447, 12.16666666666666607, 4.330127018922195425 ) ) ;
#49655 = CARTESIAN_POINT ( 'NONE',  ( -4.458734124999999437, -50.39583333196772941, -2.574251347313719407 ) ) ;
#49656 = CARTESIAN_POINT ( 'NONE',  ( 4.458734124999999437, -13.81249999863440259, -5.460374474430324690E-16 ) ) ;
#49657 = CARTESIAN_POINT ( 'NONE',  ( 5.000000000000000888, -166.0625000027312410, -2.071067811865475505 ) ) ;
#49658 = DIRECTION ( 'NONE',  ( -0.000000000000000000, 1.000000000000000000, -0.000000000000000000 ) ) ;
#49659 = DIRECTION ( 'NONE',  ( 7.709882115452476194E-16, -0.000000000000000000, 1.000000000000000000 ) ) ;
#49660 = CARTESIAN_POINT ( 'NONE',  ( 5.000000000000000000, -167.0624999999999716, 2.071067811865478614 ) ) ;
#49661 = CARTESIAN_POINT ( 'NONE',  ( 2.626220312808019583E-14, 20.87500000273118062, -5.000000000000000000 ) ) ;
#49663 = CARTESIAN_POINT ( 'NONE',  ( -2.229367062500000163, -23.47916666530107221, -3.861377020970580443 ) ) ;
#49662 = CARTESIAN_POINT ( 'NONE',  ( 0.000000000000000000, -170.0000000000000000, 5.000000000000000000 ) ) ;
#49664 = CARTESIAN_POINT ( 'NONE',  ( 3.044556291839386294E-14, 17.87500000273118417, -5.000000000000000000 ) ) ;
#49665 = CARTESIAN_POINT ( 'NONE',  ( -4.458734124999998549, -55.22916666530107932, 2.574251347313722516 ) ) ;
#49666 = CARTESIAN_POINT ( 'NONE',  ( -3.152801135295367985, -156.0625000013656063, 3.152801135295367096 ) ) ;
#49667 = CARTESIAN_POINT ( 'NONE',  ( -3.535250795749689387E-16, -55.12499999726880162, -5.773502691896257311 ) ) ;
#49668 = ORIENTED_EDGE ( 'NONE', *, *, #5962, .F. ) ;
#49669 = DIRECTION ( 'NONE',  ( -0.000000000000000000, 1.000000000000000000, -0.000000000000000000 ) ) ;
#49670 = CARTESIAN_POINT ( 'NONE',  ( 2.229367062500001939, 5.770833334698927786, 3.861377020970579999 ) ) ;
#49671 = ORIENTED_EDGE ( 'NONE', *, *, #51246, .F. ) ;
#49673 = DIRECTION ( 'NONE',  ( -0.000000000000000000, 1.000000000000000000, -0.000000000000000000 ) ) ;
#49672 = CARTESIAN_POINT ( 'NONE',  ( -2.499999999999996447, -27.83333333333333570, 4.330127018922195425 ) ) ;
#49674 = CARTESIAN_POINT ( 'NONE',  ( -3.152801135295367096, -155.0625000013656063, -3.152801135295367541 ) ) ;
#49675 = ORIENTED_EDGE ( 'NONE', *, *, #6440, .T. ) ;
#49676 = CARTESIAN_POINT ( 'NONE',  ( 1.975475456537005874E-15, -87.62499999726880162, 5.000000000000000000 ) ) ;
#49677 = CARTESIAN_POINT ( 'NONE',  ( -59.98410592259440222, -131.1250000000000284, -0.3983568153799752487 ) ) ;
#49678 = CARTESIAN_POINT ( 'NONE',  ( 5.000000000000000000, -86.50000000000000000, -6.123233995736766282E-16 ) ) ;
#49679 = CARTESIAN_POINT ( 'NONE',  ( 4.458734125000001214, -44.14583333196773651, 2.574251347313718519 ) ) ;
#49680 = ORIENTED_EDGE ( 'NONE', *, *, #58177, .F. ) ;
#49681 = CARTESIAN_POINT ( 'NONE',  ( 3.535533905932736864, -143.2500000027311842, 3.535533905932738641 ) ) ;
#49682 = CARTESIAN_POINT ( 'NONE',  ( 2.229367062499998831, 16.35416666803225993, -3.861377020970580887 ) ) ;
#49683 = EDGE_CURVE ( 'NONE', #49750, #48396, #55503, .T. ) ;
#49684 = CARTESIAN_POINT ( 'NONE',  ( -2.229367062499996610, 27.85416666803225993, 3.861377020970582219 ) ) ;
#49685 = CARTESIAN_POINT ( 'NONE',  ( -59.81910112700025905, -124.3125000027312268, -2.462841084822630311 ) ) ;
#49686 = CARTESIAN_POINT ( 'NONE',  ( 1.975475456537005874E-15, -44.74999999999999289, 5.000000000000000000 ) ) ;
#49687 = CARTESIAN_POINT ( 'NONE',  ( 1.255007937094098239E-14, 23.75000000000000000, -4.999999999999999112 ) ) ;
#49688 = CARTESIAN_POINT ( 'NONE',  ( 2.229367062500001939, -66.97916666530106511, 3.861377020970579999 ) ) ;
#49689 = CARTESIAN_POINT ( 'NONE',  ( -59.98410592259440222, -146.1250000000000284, -0.3983568153799752487 ) ) ;
#49690 = CARTESIAN_POINT ( 'NONE',  ( 4.458734124999999437, 17.18750000136559564, -5.460374474430324690E-16 ) ) ;
#49691 = FACE_OUTER_BOUND ( 'NONE', #27570, .T. ) ;
#49692 = EDGE_CURVE ( 'NONE', #40265, #61986, #44007, .T. ) ;
#49693 = CARTESIAN_POINT ( 'NONE',  ( -2.229367062500000163, -48.72916666530106511, -3.861377020970580443 ) ) ;
#49694 = CARTESIAN_POINT ( 'NONE',  ( 2.500000000000002220, -10.54166666393547835, 4.330127018922192761 ) ) ;
#49695 = CARTESIAN_POINT ( 'NONE',  ( -59.98410592259440222, -145.1250000000000284, -0.3983568153799752487 ) ) ;
#49696 = CYLINDRICAL_SURFACE ( 'NONE', #31701, 5.000000000000000000 ) ;
#49697 = CARTESIAN_POINT ( 'NONE',  ( 0.000000000000000000, -120.0000000000000000, 0.000000000000000000 ) ) ;
#49698 = CARTESIAN_POINT ( 'NONE',  ( 5.275681513340003914E-14, 10.87500000273118239, -5.000000000000000000 ) ) ;
#49699 = CARTESIAN_POINT ( 'NONE',  ( -2.229367062499996610, -18.39583333196774007, 3.861377020970582219 ) ) ;
#49700 = VERTEX_POINT ( 'NONE', #17043 ) ;
#49701 = CARTESIAN_POINT ( 'NONE',  ( -2.071067811865477726, -169.6875000000000284, -4.999999999999996447 ) ) ;
#49702 = CARTESIAN_POINT ( 'NONE',  ( -4.458734124999998549, -101.2291666653010651, 2.574251347313722516 ) ) ;
#49703 = CARTESIAN_POINT ( 'NONE',  ( -3.535533905932737309, -159.7500000027312126, -3.535533905932738197 ) ) ;
#49704 = ORIENTED_EDGE ( 'NONE', *, *, #21742, .T. ) ;
#49705 = CARTESIAN_POINT ( 'NONE',  ( 2.229367062499998831, -96.89583333196773651, -3.861377020970580887 ) ) ;
#49706 = CARTESIAN_POINT ( 'NONE',  ( -9.184850993605147944E-16, -163.3750000027311842, 5.000000000000000000 ) ) ;
#49707 = CARTESIAN_POINT ( 'NONE',  ( -2.499999999999996447, -59.70833333060214443, 4.330127018922195425 ) ) ;
#49708 = CYLINDRICAL_SURFACE ( 'NONE', #28416, 5.000000000000000000 ) ;
#49709 = CARTESIAN_POINT ( 'NONE',  ( -59.59170313451811296, -125.5000000013656205, 1.485763867205729394 ) ) ;
#49710 = CARTESIAN_POINT ( 'NONE',  ( -56.48576386720575471, -144.7500000013655779, -4.591703134518078322 ) ) ;
#49711 = CARTESIAN_POINT ( 'NONE',  ( 2.229367062500001939, -18.97916666530106866, 3.861377020970579999 ) ) ;
#49712 = CARTESIAN_POINT ( 'NONE',  ( 4.458734124999998549, 7.020833334698929562, -2.574251347313721627 ) ) ;
#49713 = CARTESIAN_POINT ( 'NONE',  ( 4.458734124999998549, -64.97916666530106511, -2.574251347313721627 ) ) ;
#49714 = CARTESIAN_POINT ( 'NONE',  ( -3.535533905932738641, -141.5000000027311842, 3.535533905932737309 ) ) ;
#49715 = CARTESIAN_POINT ( 'NONE',  ( 4.458734124999999437, -21.81249999863440436, -5.460374474430324690E-16 ) ) ;
#49716 = FACE_OUTER_BOUND ( 'NONE', #60452, .T. ) ;
#49717 = CARTESIAN_POINT ( 'NONE',  ( -3.535533905932738641, -156.3750000000000000, 3.535533905932737309 ) ) ;
#49718 = CARTESIAN_POINT ( 'NONE',  ( 2.500000000000002220, -10.66666666666666430, 4.330127018922192761 ) ) ;
#49719 = CARTESIAN_POINT ( 'NONE',  ( -4.458734125000000326, -156.0000000013656063, -1.846868145590735644 ) ) ;
#49720 = ORIENTED_EDGE ( 'NONE', *, *, #32028, .T. ) ;
#49721 = CARTESIAN_POINT ( 'NONE',  ( 9.457646018065525792E-16, -47.31249999863440792, 5.148502694627439702 ) ) ;
#49722 = CARTESIAN_POINT ( 'NONE',  ( 1.339745962155608039, 21.41965820146970501, 5.000000000000003553 ) ) ;
#49723 = CARTESIAN_POINT ( 'NONE',  ( 0.2779000157839532359, 8.820699686765054892, -7.928862157988302961 ) ) ;
#49724 = CARTESIAN_POINT ( 'NONE',  ( -2.499999999999996447, 28.16666666666666785, 4.330127018922195425 ) ) ;
#49725 = CARTESIAN_POINT ( 'NONE',  ( -2.229367062499996610, -92.14583333196773651, 3.861377020970582219 ) ) ;
#49726 = VECTOR ( 'NONE', #6992, 1000.000000000000000 ) ;
#49727 = CARTESIAN_POINT ( 'NONE',  ( -4.458734124999999437, 9.604166668032259935, -2.574251347313719407 ) ) ;
#49728 = CARTESIAN_POINT ( 'NONE',  ( -6.972266317189433020E-16, -0.2500000000000001665, -5.000000000000000000 ) ) ;
#49729 = CARTESIAN_POINT ( 'NONE',  ( 1.339745962155612702, -37.16965819600733312, -5.000000000000000000 ) ) ;
#49730 = CARTESIAN_POINT ( 'NONE',  ( 1.975475456537005874E-15, -26.74999999999999645, 5.000000000000000000 ) ) ;
#49731 = CARTESIAN_POINT ( 'NONE',  ( 9.457646018065525792E-16, 22.68750000136559564, 5.148502694627439702 ) ) ;
#49732 = CARTESIAN_POINT ( 'NONE',  ( 5.000000000000000000, -76.50000000000000000, -6.123233995736766282E-16 ) ) ;
#49733 = CARTESIAN_POINT ( 'NONE',  ( 2.499999999999998668, 9.791666669397850242, -4.330127018922193649 ) ) ;
#49734 = ORIENTED_EDGE ( 'NONE', *, *, #10698, .F. ) ;
#49735 = CARTESIAN_POINT ( 'NONE',  ( -2.500000000000000444, -98.16666666666665719, -4.330127018922193649 ) ) ;
#49736 = ORIENTED_EDGE ( 'NONE', *, *, #518, .T. ) ;
#49737 = CARTESIAN_POINT ( 'NONE',  ( -2.500000000000000444, -51.16666666666666430, -4.330127018922193649 ) ) ;
#49738 = CARTESIAN_POINT ( 'NONE',  ( -2.229367062500000163, -39.47916666530107221, -3.861377020970580443 ) ) ;
#49739 =( BOUNDED_CURVE ( )  B_SPLINE_CURVE ( 2, ( #36993, #46961, #60489, #36035, #60806, #2277, #41477, #55667, #61128 ),
 .UNSPECIFIED., .F., .F. ) 
 B_SPLINE_CURVE_WITH_KNOTS ( ( 3, 2, 2, 2, 3 ),
 ( 0.6249999999999996669, 0.6291666666666663188, 0.6333333333333328596, 0.6374999999999995115, 0.6416666666666662744 ),
 .UNSPECIFIED. ) 
 CURVE ( )  GEOMETRIC_REPRESENTATION_ITEM ( )  RATIONAL_B_SPLINE_CURVE ( ( 1.000000000000005995, 0.9238795325112806323, 1.000000000000000000, 0.9238795325112867385, 1.000000000000000000, 0.9238795325112867385, 1.000000000000000000, 0.9238795325112948431, 0.9999999999999918954 ) ) 
 REPRESENTATION_ITEM ( '' )  );
#49740 = CARTESIAN_POINT ( 'NONE',  ( 2.499999999999998668, -40.20833333060214443, -4.330127018922193649 ) ) ;
#49741 = ORIENTED_EDGE ( 'NONE', *, *, #62832, .T. ) ;
#49742 = CARTESIAN_POINT ( 'NONE',  ( 2.229367062500001939, -10.97916666530107044, 3.861377020970579999 ) ) ;
#49744 = ORIENTED_EDGE ( 'NONE', *, *, #15425, .T. ) ;
#49743 = CARTESIAN_POINT ( 'NONE',  ( -4.458734124999998549, -18.47916666530106866, 2.574251347313722516 ) ) ;
#49745 = CARTESIAN_POINT ( 'NONE',  ( -2.499999999999996447, -84.83333333333332860, 4.330127018922195425 ) ) ;
#49746 = CARTESIAN_POINT ( 'NONE',  ( 3.152801135295367541, -167.3125000013656063, -3.152801135295367541 ) ) ;
#49747 = CARTESIAN_POINT ( 'NONE',  ( -2.229367062499996610, -60.39583333196774362, 3.861377020970582219 ) ) ;
#49748 = CARTESIAN_POINT ( 'NONE',  ( 1.060575238724906964E-15, -85.62499999726880162, 5.773502691896257311 ) ) ;
#49750 = VERTEX_POINT ( 'NONE', #32139 ) ;
#49749 = CARTESIAN_POINT ( 'NONE',  ( -6.972266317189433020E-16, -28.25000000000000000, -5.000000000000000000 ) ) ;
#49751 = CARTESIAN_POINT ( 'NONE',  ( -58.24261429053147765, -142.2500000000000284, -3.805975901505573855 ) ) ;
#49752 = CARTESIAN_POINT ( 'NONE',  ( -4.458734124999999437, -27.64583333196774007, -2.574251347313719407 ) ) ;
#49753 = CARTESIAN_POINT ( 'NONE',  ( 2.500000000000002220, -5.541666663935480130, 4.330127018922192761 ) ) ;
#49754 = VERTEX_POINT ( 'NONE', #46312 ) ;
#49755 = CARTESIAN_POINT ( 'NONE',  ( 4.458734124999999437, -162.7500000013655779, 1.846868145590737864 ) ) ;
#49756 = CARTESIAN_POINT ( 'NONE',  ( -3.152548672688508926E-16, 29.43750000136559564, -5.148502694627439702 ) ) ;
#49757 = CARTESIAN_POINT ( 'NONE',  ( 2.071067811865645591, -156.1875000000000000, 4.999999999999830358 ) ) ;
#49758 = VERTEX_POINT ( 'NONE', #8030 ) ;
#49759 = CARTESIAN_POINT ( 'NONE',  ( -50.40829686548195099, -145.2500000013656347, -1.485763867205728284 ) ) ;
#49760 = CARTESIAN_POINT ( 'NONE',  ( -2.229367062499996610, -75.39583333196773651, 3.861377020970582219 ) ) ;
#49761 = CARTESIAN_POINT ( 'NONE',  ( -51.19402409849444524, -136.6250000027312410, -3.242614290531456334 ) ) ;
#49762 = CARTESIAN_POINT ( 'NONE',  ( -2.229367062500000163, -46.47916666530106511, -3.861377020970580443 ) ) ;
#49763 = CARTESIAN_POINT ( 'NONE',  ( -3.152801135295367985, -146.0625000013655779, 3.152801135295367096 ) ) ;
#49764 = DIRECTION ( 'NONE',  ( 0.000000000000000000, 1.000000000000000000, 0.000000000000000000 ) ) ;
#49765 = CARTESIAN_POINT ( 'NONE',  ( 4.458734124999998549, -46.72916666530106511, -2.574251347313721627 ) ) ;
#49766 = CARTESIAN_POINT ( 'NONE',  ( -1.339745962155613812, -0.2053418012614791066, -5.000000000000000000 ) ) ;
#49767 = CARTESIAN_POINT ( 'NONE',  ( -3.152548672688508926E-16, -15.56249999863440614, -5.148502694627439702 ) ) ;
#49768 = CARTESIAN_POINT ( 'NONE',  ( -4.999999999999999112, -101.9166666666666572, 2.886751345948131764 ) ) ;
#49769 = CARTESIAN_POINT ( 'NONE',  ( -4.458734124999999437, -141.1875000013656063, -5.460374474430324690E-16 ) ) ;
#49770 = CARTESIAN_POINT ( 'NONE',  ( -4.458734124999998549, -31.47916666530107221, 2.574251347313722516 ) ) ;
#49771 = CARTESIAN_POINT ( 'NONE',  ( -2.499999999999996447, 8.291666669397852019, 4.330127018922195425 ) ) ;
#49772 = CARTESIAN_POINT ( 'NONE',  ( -2.499999999999996447, -52.83333333333332860, 4.330127018922195425 ) ) ;
#49773 = CARTESIAN_POINT ( 'NONE',  ( -57.89159099828107458, -129.6875000013656063, -3.393966926194107447 ) ) ;
#49774 = CARTESIAN_POINT ( 'NONE',  ( 4.458734124999998549, -73.97916666530106511, -2.574251347313721627 ) ) ;
#49775 = CARTESIAN_POINT ( 'NONE',  ( 1.339745962155612702, -34.29465819873851729, -5.000000000000000000 ) ) ;
#49776 = CARTESIAN_POINT ( 'NONE',  ( -5.000000000000000000, -70.08333333333332860, -2.886751345948128211 ) ) ;
#49777 = DIRECTION ( 'NONE',  ( 0.000000000000000000, 0.000000000000000000, 1.000000000000000000 ) ) ;
#49778 = CARTESIAN_POINT ( 'NONE',  ( -2.229367062500000163, 2.270833334698928230, -3.861377020970580443 ) ) ;
#49779 = ORIENTED_EDGE ( 'NONE', *, *, #62174, .T. ) ;
#49780 = CARTESIAN_POINT ( 'NONE',  ( 6.123233995736766282E-16, -170.0000000000000000, -5.000000000000000000 ) ) ;
#49781 = CARTESIAN_POINT ( 'NONE',  ( -58.24261429053147765, -155.0000000000000284, -3.805975901505573411 ) ) ;
#49783 = CARTESIAN_POINT ( 'NONE',  ( 9.457646018065525792E-16, -35.06249999863440792, 5.148502694627439702 ) ) ;
#49782 = CARTESIAN_POINT ( 'NONE',  ( 9.457646018065525792E-16, -87.06249999863440792, 5.148502694627439702 ) ) ;
#49784 = CARTESIAN_POINT ( 'NONE',  ( 5.000000000000000888, -9.583333333333332149, 2.886751345948126879 ) ) ;
#49785 = CARTESIAN_POINT ( 'NONE',  ( -3.152548672688508926E-16, -80.81249999863440792, -5.148502694627439702 ) ) ;
#49786 = CARTESIAN_POINT ( 'NONE',  ( 9.457646018065525792E-16, 17.68750000136559208, 5.148502694627439702 ) ) ;
#49787 = CARTESIAN_POINT ( 'NONE',  ( -2.499999999999996447, -52.83333333333332860, 4.330127018922195425 ) ) ;
#49788 = CARTESIAN_POINT ( 'NONE',  ( -56.48576386720575471, -135.7500000013656063, -4.591703134518078322 ) ) ;
#49789 = CARTESIAN_POINT ( 'NONE',  ( -4.458734124999999437, -0.3958333319677397322, -2.574251347313719407 ) ) ;
#49790 = CARTESIAN_POINT ( 'NONE',  ( 2.229367062500001939, 19.77083333469892779, 3.861377020970579999 ) ) ;
#49791 = CARTESIAN_POINT ( 'NONE',  ( 9.457646018065525792E-16, -46.31249999863440792, 5.148502694627439702 ) ) ;
#49792 =( BOUNDED_CURVE ( )  B_SPLINE_CURVE ( 2, ( #17804, #2704, #41925, #32596, #51907, #62199, #18117, #38056, #37741 ),
 .UNSPECIFIED., .F., .F. ) 
 B_SPLINE_CURVE_WITH_KNOTS ( ( 3, 2, 2, 2, 3 ),
 ( 0.2589285714285714524, 0.2595238095238095455, 0.2607142857142857317, 0.2619047619047619180, 0.2625000000000000111 ),
 .UNSPECIFIED. ) 
 CURVE ( )  GEOMETRIC_REPRESENTATION_ITEM ( )  RATIONAL_B_SPLINE_CURVE ( ( 0.9330127018922194093, 0.9330127018922194093, 1.000000000000000000, 0.8660254037844387076, 1.000000000000000000, 0.8660254037844387076, 1.000000000000000000, 0.9330127018922194093, 0.9330127018922194093 ) ) 
 REPRESENTATION_ITEM ( '' )  );
#49793 = CYLINDRICAL_SURFACE ( 'NONE', #46941, 5.000000000000000000 ) ;
#49794 = CARTESIAN_POINT ( 'NONE',  ( -4.458734124999997661, -6.229166665301072214, 2.574251347313722516 ) ) ;
#49795 = CARTESIAN_POINT ( 'NONE',  ( 2.229367062499998831, -28.89583333196774007, -3.861377020970580887 ) ) ;
#49796 =( BOUNDED_CURVE ( )  B_SPLINE_CURVE ( 2, ( #54814, #1756, #1439, #21041, #20073, #39679, #21358, #11060, #30035 ),
 .UNSPECIFIED., .F., .F. ) 
 B_SPLINE_CURVE_WITH_KNOTS ( ( 3, 2, 2, 2, 3 ),
 ( 0.5062499999999999778, 0.5069444444444444198, 0.5083333333333333037, 0.5097222222222221877, 0.5104166666666666297 ),
 .UNSPECIFIED. ) 
 CURVE ( )  GEOMETRIC_REPRESENTATION_ITEM ( )  RATIONAL_B_SPLINE_CURVE ( ( 0.9330127018922194093, 0.9330127018922194093, 1.000000000000000000, 0.8660254037844387076, 1.000000000000000000, 0.8660254037844387076, 1.000000000000000000, 0.9330127018922194093, 0.9330127018922194093 ) ) 
 REPRESENTATION_ITEM ( '' )  );
#49797 = CARTESIAN_POINT ( 'NONE',  ( -50.55543936806279248, -130.3125000013656063, 0.3552334253322060320 ) ) ;
#49798 = CARTESIAN_POINT ( 'NONE',  ( 4.458734124999999437, -75.81249999863440792, -5.460374474430324690E-16 ) ) ;
#49799 = CARTESIAN_POINT ( 'NONE',  ( 5.000000000000000000, -106.2916666639354730, -2.886751345948129988 ) ) ;
#49800 = ADVANCED_FACE ( 'NONE', ( #41468 ), #61434, .T. ) ;
#49801 = CARTESIAN_POINT ( 'NONE',  ( 4.458734124999998549, 28.27083333469892779, -2.574251347313721627 ) ) ;
#49802 = CARTESIAN_POINT ( 'NONE',  ( 2.500000000000002220, 26.45833333606451632, 4.330127018922192761 ) ) ;
#49803 = CARTESIAN_POINT ( 'NONE',  ( -4.458734124999999437, -80.64583333196773651, -2.574251347313719407 ) ) ;
#49804 = CARTESIAN_POINT ( 'NONE',  ( -2.500000000000000444, -61.16666666666666430, -4.330127018922193649 ) ) ;
#49805 = CARTESIAN_POINT ( 'NONE',  ( -2.500000000000000444, -32.04166666393548724, -4.330127018922193649 ) ) ;
#49806 = CARTESIAN_POINT ( 'NONE',  ( 5.000000000000000000, 23.62500000273118417, -6.123233995736766282E-16 ) ) ;
#49807 = ORIENTED_EDGE ( 'NONE', *, *, #9100, .F. ) ;
#49808 = DIRECTION ( 'NONE',  ( 0.000000000000000000, 0.000000000000000000, 1.000000000000000000 ) ) ;
#49809 = CARTESIAN_POINT ( 'NONE',  ( -5.000000000000000000, -56.87499999726880162, 0.000000000000000000 ) ) ;
#49810 = CARTESIAN_POINT ( 'NONE',  ( -4.999999999999999112, -15.91666666666666963, 2.886751345948131764 ) ) ;
#49811 = CARTESIAN_POINT ( 'NONE',  ( -2.229367062500000163, -22.47916666530107221, -3.861377020970580443 ) ) ;
#49812 = CARTESIAN_POINT ( 'NONE',  ( 2.229367062499998831, -83.64583333196773651, -3.861377020970580887 ) ) ;
#49813 = CARTESIAN_POINT ( 'NONE',  ( -3.535250795749689387E-16, -24.12499999726881583, -5.773502691896257311 ) ) ;
#49815 = EDGE_LOOP ( 'NONE', ( #12592, #26796, #59002, #4549 ) ) ;
#49814 = CARTESIAN_POINT ( 'NONE',  ( -4.458734124999998549, -48.22916666530106511, 2.574251347313722516 ) ) ;
#49816 = CARTESIAN_POINT ( 'NONE',  ( -6.972266317189433020E-16, -76.12499999726880162, -5.000000000000000000 ) ) ;
#49817 = FACE_OUTER_BOUND ( 'NONE', #43700, .T. ) ;
#49819 = VERTEX_POINT ( 'NONE', #42420 ) ;
#49818 = CARTESIAN_POINT ( 'NONE',  ( -2.229367062500000163, 3.270833334698929118, -3.861377020970580443 ) ) ;
#49820 =( BOUNDED_CURVE ( )  B_SPLINE_CURVE ( 2, ( #45463, #60907, #46101, #25526, #50609, #20716, #25846, #11360, #59635 ),
 .UNSPECIFIED., .F., .F. ) 
 B_SPLINE_CURVE_WITH_KNOTS ( ( 3, 2, 2, 2, 3 ),
 ( 0.2270833333333333315, 0.2277777777777777735, 0.2291666666666666574, 0.2305555555555555691, 0.2312500000000000111 ),
 .UNSPECIFIED. ) 
 CURVE ( )  GEOMETRIC_REPRESENTATION_ITEM ( )  RATIONAL_B_SPLINE_CURVE ( ( 0.9330127018922194093, 0.9330127018922194093, 1.000000000000000000, 0.8660254037844387076, 1.000000000000000000, 0.8660254037844387076, 1.000000000000000000, 0.9330127018922194093, 0.9330127018922194093 ) ) 
 REPRESENTATION_ITEM ( '' )  );
#49821 = CARTESIAN_POINT ( 'NONE',  ( -52.10840900171896806, -150.1875000013656063, 3.393966926194110556 ) ) ;
#49822 = CARTESIAN_POINT ( 'NONE',  ( -5.000000000000000000, -65.08333333333332860, -2.886751345948128211 ) ) ;
#49823 = CARTESIAN_POINT ( 'NONE',  ( 1.846868145590736310, -152.8750000013655779, 4.458734124999999437 ) ) ;
#49824 = CARTESIAN_POINT ( 'NONE',  ( -2.229367062500000163, -48.72916666530106511, -3.861377020970580443 ) ) ;
#49825 = CARTESIAN_POINT ( 'NONE',  ( -2.500000000000000444, -81.04166666393547303, -4.330127018922193649 ) ) ;
#49826 = CARTESIAN_POINT ( 'NONE',  ( -2.071067811865478170, -160.3125000000000284, 5.000000000000000000 ) ) ;
#49827 = CARTESIAN_POINT ( 'NONE',  ( 1.975475456537005874E-15, 11.24999999999999822, 5.000000000000000000 ) ) ;
#49828 = CARTESIAN_POINT ( 'NONE',  ( -57.46284108482265651, -154.9375000000000000, 4.819101127000239515 ) ) ;
#49829 = CARTESIAN_POINT ( 'NONE',  ( -3.152548672688508926E-16, -11.81249999863440969, -5.148502694627439702 ) ) ;
#49830 = CARTESIAN_POINT ( 'NONE',  ( -4.458734124999999437, -47.56249999863440792, 0.000000000000000000 ) ) ;
#49831 = CYLINDRICAL_SURFACE ( 'NONE', #50924, 5.000000000000000000 ) ;
#49832 = CARTESIAN_POINT ( 'NONE',  ( -4.458734125000001214, -142.8750000013656063, 1.846868145590734089 ) ) ;
#49833 = CARTESIAN_POINT ( 'NONE',  ( 4.458734124999998549, -92.97916666530106511, -2.574251347313721627 ) ) ;
#49834 = CARTESIAN_POINT ( 'NONE',  ( 0.000000000000000000, -120.0000000000000000, 0.000000000000000000 ) ) ;
#49835 = ORIENTED_EDGE ( 'NONE', *, *, #23163, .T. ) ;
#49836 = CARTESIAN_POINT ( 'NONE',  ( 0.000000000000000000, -170.0000000000000000, 0.000000000000000000 ) ) ;
#49837 = CARTESIAN_POINT ( 'NONE',  ( -5.000000000000000000, -68.87499999726880162, 0.000000000000000000 ) ) ;
#49838 = CARTESIAN_POINT ( 'NONE',  ( -53.33387254593733928, -147.9375000027312126, 5.149110718188519620 ) ) ;
#49839 =( BOUNDED_CURVE ( )  B_SPLINE_CURVE ( 2, ( #46978, #2926, #42138, #12554, #12245, #57271, #7428, #46654, #2600 ),
 .UNSPECIFIED., .F., .F. ) 
 B_SPLINE_CURVE_WITH_KNOTS ( ( 3, 2, 2, 2, 3 ),
 ( 0.09821428571428571230, 0.09880952380952380543, 0.1000000000000000056, 0.1011904761904761918, 0.1017857142857142849 ),
 .UNSPECIFIED. ) 
 CURVE ( )  GEOMETRIC_REPRESENTATION_ITEM ( )  RATIONAL_B_SPLINE_CURVE ( ( 0.9330127018922194093, 0.9330127018922194093, 1.000000000000000000, 0.8660254037844387076, 1.000000000000000000, 0.8660254037844387076, 1.000000000000000000, 0.9330127018922194093, 0.9330127018922194093 ) ) 
 REPRESENTATION_ITEM ( '' )  );
#49840 = CARTESIAN_POINT ( 'NONE',  ( 5.000000000000000888, -30.58333333333333215, 2.886751345948126879 ) ) ;
#49841 = ORIENTED_EDGE ( 'NONE', *, *, #51089, .F. ) ;
#49842 = CARTESIAN_POINT ( 'NONE',  ( 2.229367062499998831, 4.354166668032260823, -3.861377020970580887 ) ) ;
#49843 = CARTESIAN_POINT ( 'NONE',  ( -4.458734124999999437, -16.56249999863440436, 0.000000000000000000 ) ) ;
#49844 = VECTOR ( 'NONE', #25552, 1000.000000000000000 ) ;
#49845 = CARTESIAN_POINT ( 'NONE',  ( -1.339745962155610925, -100.7946581987385315, 5.000000000000000000 ) ) ;
#49846 = CARTESIAN_POINT ( 'NONE',  ( -4.458734124999999437, -6.395833331967740953, -2.574251347313719407 ) ) ;
#49847 = CARTESIAN_POINT ( 'NONE',  ( 5.000000000000000000, -55.29166666393548013, -2.886751345948130876 ) ) ;
#49848 = CARTESIAN_POINT ( 'NONE',  ( -3.152801135295367985, -147.8125000013655779, 3.152801135295367096 ) ) ;
#49849 = CARTESIAN_POINT ( 'NONE',  ( -3.152548672688508926E-16, 14.18750000136559386, -5.148502694627439702 ) ) ;
#49850 = ORIENTED_EDGE ( 'NONE', *, *, #41666, .T. ) ;
#49851 = CARTESIAN_POINT ( 'NONE',  ( -2.071067811865604735, -148.3124999999999716, 4.999999999999872990 ) ) ;
#49852 = CARTESIAN_POINT ( 'NONE',  ( 4.458734125000001214, -19.89583333196773651, 2.574251347313718519 ) ) ;
#49853 = CARTESIAN_POINT ( 'NONE',  ( -5.000000000000000888, 6.123233995736767268E-16, -25.03750572909317285 ) ) ;
#49854 = CARTESIAN_POINT ( 'NONE',  ( 2.499999999999998668, 1.791666669397853795, -4.330127018922193649 ) ) ;
#49855 = CARTESIAN_POINT ( 'NONE',  ( -51.60603307380591787, -147.9375000013656063, -2.891590998281053704 ) ) ;
#49856 = CARTESIAN_POINT ( 'NONE',  ( 5.000000000000000888, -48.45833333060215153, 2.886751345948126879 ) ) ;
#49857 = LINE ( 'NONE', #35717, #48561 ) ;
#49858 = CARTESIAN_POINT ( 'NONE',  ( 4.458734125000000326, 15.10416666803225993, 2.574251347313718519 ) ) ;
#49859 = CARTESIAN_POINT ( 'NONE',  ( -2.500000000000000444, -9.041666663935483683, -4.330127018922193649 ) ) ;
#49860 = FACE_OUTER_BOUND ( 'NONE', #39144, .T. ) ;
#49861 = CARTESIAN_POINT ( 'NONE',  ( -2.229367062500000163, 13.52083333469892779, -3.861377020970580443 ) ) ;
#49862 = CARTESIAN_POINT ( 'NONE',  ( -2.229367062500000163, -63.47916666530106511, -3.861377020970580443 ) ) ;
#49863 = ORIENTED_EDGE ( 'NONE', *, *, #17739, .F. ) ;
#49864 = CARTESIAN_POINT ( 'NONE',  ( -2.229367062500000163, -13.72916666530107221, -3.861377020970580443 ) ) ;
#49865 = CARTESIAN_POINT ( 'NONE',  ( -5.000000000000000000, 3.916666666666665630, -2.886751345948128211 ) ) ;
#49866 = CARTESIAN_POINT ( 'NONE',  ( 1.846868145590736310, -164.6250000013655779, 4.458734124999999437 ) ) ;
#49867 = CARTESIAN_POINT ( 'NONE',  ( -4.999999999999998224, 26.20833333606451632, 2.886751345948131764 ) ) ;
#49868 = CARTESIAN_POINT ( 'NONE',  ( -3.152548672688508926E-16, -59.56249999863440081, -5.148502694627439702 ) ) ;
#49869 = CARTESIAN_POINT ( 'NONE',  ( -5.000000000000000000, -91.95833333060214443, -2.886751345948128211 ) ) ;
#49870 = EDGE_CURVE ( 'NONE', #49141, #56905, #42735, .T. ) ;
#49871 = CARTESIAN_POINT ( 'NONE',  ( 9.457646018065525792E-16, -33.06249999863440792, 5.148502694627439702 ) ) ;
#49872 = CARTESIAN_POINT ( 'NONE',  ( 5.000000000000001776, 6.123233995736768255E-16, -9.974600000000000577 ) ) ;
#49873 = CARTESIAN_POINT ( 'NONE',  ( -4.999999999999998224, -54.79166666393548013, 2.886751345948131764 ) ) ;
#49874 = CARTESIAN_POINT ( 'NONE',  ( -54.60164318462004474, -151.5000000027312410, -4.984105922594373794 ) ) ;
#49875 = CARTESIAN_POINT ( 'NONE',  ( 1.339745962155612702, -16.16965819600733667, -5.000000000000000000 ) ) ;
#49876 = CARTESIAN_POINT ( 'NONE',  ( -3.152801135295367985, -150.0625000013655779, 3.152801135295367096 ) ) ;
#49877 = CARTESIAN_POINT ( 'NONE',  ( -2.499999999999996447, -41.83333333333333570, 4.330127018922195425 ) ) ;
#49878 = DIRECTION ( 'NONE',  ( 0.000000000000000000, 1.000000000000000000, 0.000000000000000000 ) ) ;
#49879 = CARTESIAN_POINT ( 'NONE',  ( -56.37266686252615955, -135.0000000000000284, -4.242180533871957593 ) ) ;
#49880 = ORIENTED_EDGE ( 'NONE', *, *, #28330, .F. ) ;
#49881 = CARTESIAN_POINT ( 'NONE',  ( 4.458734125000001214, -103.8958333319677365, 2.574251347313718519 ) ) ;
#49882 = CARTESIAN_POINT ( 'NONE',  ( -4.458734124999999437, 4.354166668032260823, -2.574251347313719407 ) ) ;
#49883 = DIRECTION ( 'NONE',  ( -0.000000000000000000, 1.000000000000000000, -0.000000000000000000 ) ) ;
#49884 = CARTESIAN_POINT ( 'NONE',  ( -3.535250795749689387E-16, -1.250000000000001110, -5.773502691896257311 ) ) ;
#49885 = EDGE_CURVE ( 'NONE', #32122, #60943, #56288, .T. ) ;
#49886 = CARTESIAN_POINT ( 'NONE',  ( 2.229367062500001939, -65.97916666530106511, 3.861377020970579999 ) ) ;
#49887 = CARTESIAN_POINT ( 'NONE',  ( -2.500000000000000444, -26.16666666666666430, -4.330127018922193649 ) ) ;
#49888 = CARTESIAN_POINT ( 'NONE',  ( -5.000000000000000000, -8.874999997268814056, 0.000000000000000000 ) ) ;
#49890 = ORIENTED_EDGE ( 'NONE', *, *, #57455, .T. ) ;
#49889 = CARTESIAN_POINT ( 'NONE',  ( -4.458734124999999437, -32.31249999863440792, 0.000000000000000000 ) ) ;
#49891 = CARTESIAN_POINT ( 'NONE',  ( -6.972266317189433020E-16, -22.12499999726881228, -5.000000000000000000 ) ) ;
#49892 = EDGE_CURVE ( 'NONE', #32964, #55487, #39503, .T. ) ;
#49893 = VERTEX_POINT ( 'NONE', #62063 ) ;
#49894 = CARTESIAN_POINT ( 'NONE',  ( 1.339745962155612702, -101.1696581960073331, -5.000000000000000000 ) ) ;
#49895 = CARTESIAN_POINT ( 'NONE',  ( -2.499999999999996447, -51.83333333333332860, 4.330127018922195425 ) ) ;
#49897 = CARTESIAN_POINT ( 'NONE',  ( -2.229367062499996610, -29.39583333196774007, 3.861377020970582219 ) ) ;
#49896 = DIRECTION ( 'NONE',  ( 0.000000000000000000, 0.000000000000000000, 1.000000000000000000 ) ) ;
#49898 = CARTESIAN_POINT ( 'NONE',  ( -6.972266317189433020E-16, -42.12499999726880873, -5.000000000000000000 ) ) ;
#49899 = CARTESIAN_POINT ( 'NONE',  ( -4.458734124999998549, -78.22916666530106511, 2.574251347313722516 ) ) ;
#49900 = CARTESIAN_POINT ( 'NONE',  ( -4.458734125000000326, -143.2500000013655779, -1.846868145590735644 ) ) ;
#49901 = CARTESIAN_POINT ( 'NONE',  ( -4.458734124999999437, -82.39583333196773651, -2.574251347313719407 ) ) ;
#49902 = CARTESIAN_POINT ( 'NONE',  ( -52.10840900171896806, -137.4375000013656063, 3.393966926194110556 ) ) ;
#49903 = AXIS2_PLACEMENT_3D ( 'NONE', #11757, #21751, #41986 ) ;
#49904 = CARTESIAN_POINT ( 'NONE',  ( 9.457646018065525792E-16, -30.31249999863440436, 5.148502694627439702 ) ) ;
#49905 = VERTEX_POINT ( 'NONE', #27945 ) ;
#49906 = DIRECTION ( 'NONE',  ( -0.000000000000000000, 1.000000000000000000, -0.000000000000000000 ) ) ;
#49907 = ORIENTED_EDGE ( 'NONE', *, *, #36719, .F. ) ;
#49908 = CARTESIAN_POINT ( 'NONE',  ( 2.229367062499998831, -72.89583333196773651, -3.861377020970580887 ) ) ;
#49909 = DIRECTION ( 'NONE',  ( -0.000000000000000000, 1.000000000000000000, -0.000000000000000000 ) ) ;
#49910 = ORIENTED_EDGE ( 'NONE', *, *, #27271, .T. ) ;
#49911 = CARTESIAN_POINT ( 'NONE',  ( 2.499999999999998668, -16.33333333333333215, -4.330127018922193649 ) ) ;
#49912 = CARTESIAN_POINT ( 'NONE',  ( 2.499999999999998668, -12.33333333333333570, -4.330127018922193649 ) ) ;
#49913 = CARTESIAN_POINT ( 'NONE',  ( -2.229367062499996610, -63.39583333196774362, 3.861377020970582219 ) ) ;
#49914 = CARTESIAN_POINT ( 'NONE',  ( -4.458734124999999437, -1.562499998634406140, 0.000000000000000000 ) ) ;
#49915 = VERTEX_POINT ( 'NONE', #17976 ) ;
#49916 =( BOUNDED_CURVE ( )  B_SPLINE_CURVE ( 2, ( #6257, #5612, #801, #5937, #10751, #35843, #40006, #15585, #49983 ),
 .UNSPECIFIED., .F., .F. ) 
 B_SPLINE_CURVE_WITH_KNOTS ( ( 3, 2, 2, 2, 3 ),
 ( 0.1160714285714285754, 0.1166666666666666685, 0.1178571428571428548, 0.1190476190476190410, 0.1196428571428571480 ),
 .UNSPECIFIED. ) 
 CURVE ( )  GEOMETRIC_REPRESENTATION_ITEM ( )  RATIONAL_B_SPLINE_CURVE ( ( 0.9330127018922194093, 0.9330127018922194093, 1.000000000000000000, 0.8660254037844387076, 1.000000000000000000, 0.8660254037844387076, 1.000000000000000000, 0.9330127018922185211, 0.9330127018922192983 ) ) 
 REPRESENTATION_ITEM ( '' )  );
#49917 = CARTESIAN_POINT ( 'NONE',  ( 1.975475456537005874E-15, 8.375000002731187720, 5.000000000000000000 ) ) ;
#49918 = EDGE_CURVE ( 'NONE', #44207, #13355, #4567, .T. ) ;
#49919 = CARTESIAN_POINT ( 'NONE',  ( 5.000000000000000000, -27.49999999999999645, -6.123233995736766282E-16 ) ) ;
#49920 = CARTESIAN_POINT ( 'NONE',  ( 4.458734124999998549, 11.27083333469892779, -2.574251347313721627 ) ) ;
#49921 = CARTESIAN_POINT ( 'NONE',  ( -58.39396692619412477, -141.4375000013656063, 2.891590998281057701 ) ) ;
#49922 = CARTESIAN_POINT ( 'NONE',  ( -6.972266317189433020E-16, -47.12499999726880873, -5.000000000000000000 ) ) ;
#49923 = CARTESIAN_POINT ( 'NONE',  ( 2.730187237215162345E-16, -160.1875000013655779, -4.458734124999999437 ) ) ;
#49924 = CARTESIAN_POINT ( 'NONE',  ( 0.000000000000000000, -170.0000000000000000, 0.000000000000000000 ) ) ;
#49925 = EDGE_LOOP ( 'NONE', ( #8552, #56164, #53711, #33075 ) ) ;
#49926 = CARTESIAN_POINT ( 'NONE',  ( 4.458734124999999437, -79.81249999863440792, -5.460374474430324690E-16 ) ) ;
#49927 = CARTESIAN_POINT ( 'NONE',  ( 1.339745962155612702, -29.16965819600733312, -5.000000000000000000 ) ) ;
#49928 = CARTESIAN_POINT ( 'NONE',  ( 2.229367062499998831, -0.6458333319677399542, -3.861377020970580887 ) ) ;
#49929 = DIRECTION ( 'NONE',  ( -0.000000000000000000, 1.000000000000000000, -0.000000000000000000 ) ) ;
#49930 =( BOUNDED_CURVE ( )  B_SPLINE_CURVE ( 2, ( #31940, #3005, #41898, #12329, #17149, #18090, #12948, #36448, #37098 ),
 .UNSPECIFIED., .F., .F. ) 
 B_SPLINE_CURVE_WITH_KNOTS ( ( 3, 2, 2, 2, 3 ),
 ( 0.3854166666666666852, 0.3861111111111111271, 0.3875000000000000111, 0.3888888888888888951, 0.3895833333333333370 ),
 .UNSPECIFIED. ) 
 CURVE ( )  GEOMETRIC_REPRESENTATION_ITEM ( )  RATIONAL_B_SPLINE_CURVE ( ( 0.9330127018922194093, 0.9330127018922194093, 1.000000000000000000, 0.8660254037844387076, 1.000000000000000000, 0.8660254037844387076, 1.000000000000000000, 0.9330127018922194093, 0.9330127018922194093 ) ) 
 REPRESENTATION_ITEM ( '' )  );
#49931 = CARTESIAN_POINT ( 'NONE',  ( 1.975475456537005874E-15, -40.62499999726879452, 5.000000000000000000 ) ) ;
#49932 = CARTESIAN_POINT ( 'NONE',  ( -3.152548672688508926E-16, -68.81249999863439371, -5.148502694627439702 ) ) ;
#49933 = CARTESIAN_POINT ( 'NONE',  ( 1.060575238724906964E-15, -27.62499999726881228, 5.773502691896257311 ) ) ;
#49934 = DIRECTION ( 'NONE',  ( -0.000000000000000000, 1.000000000000000000, -0.000000000000000000 ) ) ;
#49935 = CARTESIAN_POINT ( 'NONE',  ( 2.229367062499998831, 29.35416666803225993, -3.861377020970580887 ) ) ;
#49936 = CARTESIAN_POINT ( 'NONE',  ( -5.000000000000000000, -55.99999999999999289, 0.000000000000000000 ) ) ;
#49937 = CARTESIAN_POINT ( 'NONE',  ( 1.339745962155729053, -43.16965819600733312, -4.999999999999933387 ) ) ;
#49938 = CARTESIAN_POINT ( 'NONE',  ( 4.458734124999999437, -47.81249999863440792, -5.460374474430324690E-16 ) ) ;
#49939 = CARTESIAN_POINT ( 'NONE',  ( 4.458734125000000326, -30.14583333196773651, 2.574251347313718519 ) ) ;
#49940 = CARTESIAN_POINT ( 'NONE',  ( 2.229367062499998831, 4.104166668032260823, -3.861377020970580887 ) ) ;
#49941 = VECTOR ( 'NONE', #34212, 1000.000000000000000 ) ;
#49942 = CARTESIAN_POINT ( 'NONE',  ( -3.535533905932738641, -161.5000000027312126, 3.535533905932737309 ) ) ;
#49943 = CARTESIAN_POINT ( 'NONE',  ( 2.499999999999998668, 19.66666666666666430, -4.330127018922193649 ) ) ;
#49944 = CARTESIAN_POINT ( 'NONE',  ( 5.000000000000000888, -146.0625000027312126, -2.071067811865475505 ) ) ;
#49945 = CARTESIAN_POINT ( 'NONE',  ( 1.975475456537005874E-15, -84.62499999726880162, 5.000000000000000000 ) ) ;
#49946 = CARTESIAN_POINT ( 'NONE',  ( 2.229367062500001939, -40.97916666530107221, 3.861377020970579999 ) ) ;
#49947 = CARTESIAN_POINT ( 'NONE',  ( -3.535250795749689387E-16, -75.12499999726880162, -5.773502691896257311 ) ) ;
#49948 = AXIS2_PLACEMENT_3D ( 'NONE', #41548, #31598, #32867 ) ;
#49949 = VECTOR ( 'NONE', #18219, 1000.000000000000000 ) ;
#49950 = CARTESIAN_POINT ( 'NONE',  ( -57.89159099828107458, -143.9375000013656063, -3.393966926194107447 ) ) ;
#49951 = FACE_OUTER_BOUND ( 'NONE', #42733, .T. ) ;
#49952 = EDGE_CURVE ( 'NONE', #12052, #62764, #15276, .T. ) ;
#49953 = CARTESIAN_POINT ( 'NONE',  ( 5.000000000000000000, -141.1875000027312126, 2.071067811865478614 ) ) ;
#49954 = EDGE_CURVE ( 'NONE', #11304, #38064, #78, .T. ) ;
#49955 = CARTESIAN_POINT ( 'NONE',  ( 4.458734124999999437, -81.06249999863440792, -5.460374474430324690E-16 ) ) ;
#49956 = CARTESIAN_POINT ( 'NONE',  ( 3.152801135295366208, -165.8125000013656063, 3.152801135295367985 ) ) ;
#49957 = CARTESIAN_POINT ( 'NONE',  ( 1.975475456537005874E-15, 18.37500000273118062, 5.000000000000000000 ) ) ;
#49958 = CARTESIAN_POINT ( 'NONE',  ( 3.061616997868383141E-16, -159.8750000027311842, -5.000000000000000000 ) ) ;
#49959 = CARTESIAN_POINT ( 'NONE',  ( -5.000000000000000000, -30.00000000000000000, 0.000000000000000000 ) ) ;
#49960 = CYLINDRICAL_SURFACE ( 'NONE', #23338, 5.000000000000000000 ) ;
#49961 = VERTEX_POINT ( 'NONE', #33408 ) ;
#49962 = CARTESIAN_POINT ( 'NONE',  ( -4.458734124999998549, 22.52083333469892423, 2.574251347313722516 ) ) ;
#49963 = ORIENTED_EDGE ( 'NONE', *, *, #9778, .F. ) ;
#49964 = CARTESIAN_POINT ( 'NONE',  ( -4.458734124999999437, -62.64583333196774362, -2.574251347313719407 ) ) ;
#49965 = CARTESIAN_POINT ( 'NONE',  ( -5.000000000000000000, 24.12500000273118417, 0.000000000000000000 ) ) ;
#49966 = CARTESIAN_POINT ( 'NONE',  ( 2.500000000000002220, 12.33333333333333215, 4.330127018922192761 ) ) ;
#49967 = EDGE_CURVE ( 'NONE', #10973, #6056, #46100, .T. ) ;
#49968 = CARTESIAN_POINT ( 'NONE',  ( 4.458734124999998549, -51.72916666530107221, -2.574251347313721627 ) ) ;
#49969 = CARTESIAN_POINT ( 'NONE',  ( -2.229367062500000163, -10.47916666530106866, -3.861377020970580443 ) ) ;
#49970 = CYLINDRICAL_SURFACE ( 'NONE', #26729, 5.000000000000000000 ) ;
#49971 = CYLINDRICAL_SURFACE ( 'NONE', #14261, 5.000000000000000000 ) ;
#49972 = CARTESIAN_POINT ( 'NONE',  ( -6.972266317189433020E-16, -27.12499999726881228, -5.000000000000000000 ) ) ;
#49973 = ADVANCED_FACE ( 'NONE', ( #4148 ), #43366, .T. ) ;
#49974 = CARTESIAN_POINT ( 'NONE',  ( -58.24261429053147765, -139.3750000027312126, -3.805975901505573855 ) ) ;
#49975 = CARTESIAN_POINT ( 'NONE',  ( 5.000000000000000000, -56.29166666393548013, -2.886751345948130876 ) ) ;
#49977 = CARTESIAN_POINT ( 'NONE',  ( -3.152548672688508926E-16, -20.56249999863440081, -5.148502694627439702 ) ) ;
#49976 = CARTESIAN_POINT ( 'NONE',  ( 2.500000000000002220, 21.45833333606451987, 4.330127018922192761 ) ) ;
#49978 = CARTESIAN_POINT ( 'NONE',  ( -2.500000000000000444, -78.04166666393547303, -4.330127018922193649 ) ) ;
#49979 = CARTESIAN_POINT ( 'NONE',  ( 9.457646018065525792E-16, -59.06249999863439371, 5.148502694627439702 ) ) ;
#49980 = CARTESIAN_POINT ( 'NONE',  ( 1.846868145590736310, -156.8750000013655779, 4.458734124999999437 ) ) ;
#49981 = CARTESIAN_POINT ( 'NONE',  ( -2.499999999999996447, -55.70833333060214443, 4.330127018922195425 ) ) ;
#49982 = EDGE_LOOP ( 'NONE', ( #5193, #51026, #29195, #49985 ) ) ;
#49983 = CARTESIAN_POINT ( 'NONE',  ( -2.916731409357579869E-14, 13.25000000000000178, 5.000000000000000888 ) ) ;
#49984 = CARTESIAN_POINT ( 'NONE',  ( -4.458734124999999437, -1.562499998634406140, 0.000000000000000000 ) ) ;
#49985 = ORIENTED_EDGE ( 'NONE', *, *, #31521, .T. ) ;
#49987 = DIRECTION ( 'NONE',  ( 0.000000000000000000, 0.000000000000000000, 1.000000000000000000 ) ) ;
#49986 = CARTESIAN_POINT ( 'NONE',  ( -53.33387254593725402, -148.9375000027311842, 5.149110718188524949 ) ) ;
#49988 = CARTESIAN_POINT ( 'NONE',  ( 1.846868145590736310, -154.6250000013655779, 4.458734124999999437 ) ) ;
#49989 = EDGE_LOOP ( 'NONE', ( #40172, #58454, #3091, #15616 ) ) ;
#49990 =( BOUNDED_CURVE ( )  B_SPLINE_CURVE ( 2, ( #63349, #23792, #63666, #54322, #9927, #58514, #34061, #59474, #19899 ),
 .UNSPECIFIED., .F., .F. ) 
 B_SPLINE_CURVE_WITH_KNOTS ( ( 3, 2, 2, 2, 3 ),
 ( 0.4053571428571428603, 0.4059523809523809534, 0.4071428571428571397, 0.4083333333333333259, 0.4089285714285714191 ),
 .UNSPECIFIED. ) 
 CURVE ( )  GEOMETRIC_REPRESENTATION_ITEM ( )  RATIONAL_B_SPLINE_CURVE ( ( 0.9330127018922194093, 0.9330127018922194093, 1.000000000000000000, 0.8660254037844387076, 1.000000000000000000, 0.8660254037844387076, 1.000000000000000000, 0.9330127018922194093, 0.9330127018922194093 ) ) 
 REPRESENTATION_ITEM ( '' )  );
#49991 = VECTOR ( 'NONE', #4871, 1000.000000000000000 ) ;
#49992 = CARTESIAN_POINT ( 'NONE',  ( -54.60164318462004474, -130.3750000000000284, -4.984105922594373794 ) ) ;
#49993 = CARTESIAN_POINT ( 'NONE',  ( 5.000000000000000000, 15.50000000000000000, -6.123233995736766282E-16 ) ) ;
#49994 = CARTESIAN_POINT ( 'NONE',  ( 4.458734124999998549, -44.97916666530107221, -2.574251347313721627 ) ) ;
#49995 = AXIS2_PLACEMENT_3D ( 'NONE', #8844, #63510, #58991 ) ;
#49996 = ORIENTED_EDGE ( 'NONE', *, *, #27490, .T. ) ;
#49997 = AXIS2_PLACEMENT_3D ( 'NONE', #282, #8971, #4456 ) ;
#49998 = LINE ( 'NONE', #40346, #31636 ) ;
#49999 = CARTESIAN_POINT ( 'NONE',  ( 4.458734124999999437, 15.18750000136559564, -5.460374474430324690E-16 ) ) ;
#50000 = CARTESIAN_POINT ( 'NONE',  ( 4.458734124999999437, 27.18750000136559564, -5.460374474430324690E-16 ) ) ;
#50001 = CARTESIAN_POINT ( 'NONE',  ( -54.64476657466781973, -152.8125000013656063, -4.444560631937228834 ) ) ;
#50002 = DIRECTION ( 'NONE',  ( -0.000000000000000000, 1.000000000000000000, -0.000000000000000000 ) ) ;
#50003 = FACE_OUTER_BOUND ( 'NONE', #32822, .T. ) ;
#50004 = FACE_OUTER_BOUND ( 'NONE', #52224, .T. ) ;
#50005 = CARTESIAN_POINT ( 'NONE',  ( -4.458734124999999437, -67.39583333196773651, -2.574251347313719407 ) ) ;
#50006 = CARTESIAN_POINT ( 'NONE',  ( -2.500000000000000444, -50.04166666393547303, -4.330127018922193649 ) ) ;
#50007 = CARTESIAN_POINT ( 'NONE',  ( 2.229367062499998831, 19.35416666803225993, -3.861377020970580887 ) ) ;
#50008 = CARTESIAN_POINT ( 'NONE',  ( -5.000000000000000000, 17.91666666666666430, -2.886751345948128211 ) ) ;
#50009 = CARTESIAN_POINT ( 'NONE',  ( 5.000000000000000000, -157.1250000027311842, 0.000000000000000000 ) ) ;
#50010 = CARTESIAN_POINT ( 'NONE',  ( 4.458734124999998549, -48.97916666530107221, -2.574251347313721627 ) ) ;
#50011 = CARTESIAN_POINT ( 'NONE',  ( -5.000000000000000000, -10.95833333060214621, -2.886751345948128211 ) ) ;
#50012 = CARTESIAN_POINT ( 'NONE',  ( 5.000000000000000000, -42.29166666393548724, -2.886751345948130876 ) ) ;
#50013 = DIRECTION ( 'NONE',  ( -0.000000000000000000, 1.000000000000000000, -0.000000000000000000 ) ) ;
#50014 = CARTESIAN_POINT ( 'NONE',  ( -2.229367062499996610, -90.39583333196773651, 3.861377020970582219 ) ) ;
#50015 = FACE_OUTER_BOUND ( 'NONE', #30940, .T. ) ;
#50016 =( BOUNDED_CURVE ( )  B_SPLINE_CURVE ( 2, ( #23611, #39323, #30314, #59609, #30639, #5563, #1400, #45437, #24869 ),
 .UNSPECIFIED., .F., .F. ) 
 B_SPLINE_CURVE_WITH_KNOTS ( ( 3, 2, 2, 2, 3 ),
 ( 0.5053571428571428381, 0.5059523809523809312, 0.5071428571428571175, 0.5083333333333333037, 0.5089285714285713969 ),
 .UNSPECIFIED. ) 
 CURVE ( )  GEOMETRIC_REPRESENTATION_ITEM ( )  RATIONAL_B_SPLINE_CURVE ( ( 0.9330127018922194093, 0.9330127018922194093, 1.000000000000000000, 0.8660254037844387076, 1.000000000000000000, 0.8660254037844387076, 1.000000000000000000, 0.9330127018922194093, 0.9330127018922194093 ) ) 
 REPRESENTATION_ITEM ( '' )  );
#50017 = CARTESIAN_POINT ( 'NONE',  ( 4.458734124999998549, -15.97916666530107221, -2.574251347313721627 ) ) ;
#50018 = ORIENTED_EDGE ( 'NONE', *, *, #29545, .T. ) ;
#50019 = CARTESIAN_POINT ( 'NONE',  ( -5.000000000000000888, -163.5625000027312126, 2.071067811865474617 ) ) ;
#50020 = CARTESIAN_POINT ( 'NONE',  ( -4.458734124999999437, -104.3124999986344079, 0.000000000000000000 ) ) ;
#50021 = CARTESIAN_POINT ( 'NONE',  ( 5.000000000000000000, -156.1875000027312126, 2.071067811865478614 ) ) ;
#50022 = VERTEX_POINT ( 'NONE', #49142 ) ;
#50023 = CARTESIAN_POINT ( 'NONE',  ( -2.229367062499996610, -99.39583333196773651, 3.861377020970582219 ) ) ;
#50024 = CARTESIAN_POINT ( 'NONE',  ( 6.123233995736766282E-16, -120.0000000000000000, -5.000000000000000000 ) ) ;
#50025 = CARTESIAN_POINT ( 'NONE',  ( -4.999999999999999112, -59.79166666393547303, 2.886751345948131764 ) ) ;
#50026 = CARTESIAN_POINT ( 'NONE',  ( -1.339745962155613812, 18.91965820146970501, -5.000000000000000000 ) ) ;
#50027 = CARTESIAN_POINT ( 'NONE',  ( -57.89159099828107458, -127.6875000013656063, -3.393966926194107447 ) ) ;
#50028 = CARTESIAN_POINT ( 'NONE',  ( -58.39396692619412477, -142.4375000013656063, 2.891590998281057701 ) ) ;
#50029 = EDGE_CURVE ( 'NONE', #42274, #12871, #63013, .T. ) ;
#50030 = CARTESIAN_POINT ( 'NONE',  ( -4.458734124999999437, -24.31249999863440436, 0.000000000000000000 ) ) ;
#50031 = CARTESIAN_POINT ( 'NONE',  ( 4.458734124999998549, 6.020833334698928674, -2.574251347313721627 ) ) ;
#50032 = CARTESIAN_POINT ( 'NONE',  ( 2.229367062499998831, -66.89583333196773651, -3.861377020970580887 ) ) ;
#50033 = CARTESIAN_POINT ( 'NONE',  ( 1.339745962155615144, -48.58034179853029855, 4.999999999999999112 ) ) ;
#50034 = CARTESIAN_POINT ( 'NONE',  ( -4.458734124999999437, -22.31249999863440436, 0.000000000000000000 ) ) ;
#50035 = CARTESIAN_POINT ( 'NONE',  ( 0.000000000000000000, -120.0000000000000000, 0.000000000000000000 ) ) ;
#50036 = CARTESIAN_POINT ( 'NONE',  ( -5.000000000000000888, -149.5625000000000568, -2.071067811865475949 ) ) ;
#50037 = CARTESIAN_POINT ( 'NONE',  ( -5.000000000000000000, -9.000000000000001776, 0.000000000000000000 ) ) ;
#50038 = CARTESIAN_POINT ( 'NONE',  ( -4.458734124999999437, -153.9375000013655779, -5.460374474430324690E-16 ) ) ;
#50039 = ORIENTED_EDGE ( 'NONE', *, *, #22815, .T. ) ;
#50040 = CARTESIAN_POINT ( 'NONE',  ( -4.458734124999999437, -45.64583333196774362, -2.574251347313719407 ) ) ;
#50041 = VECTOR ( 'NONE', #22211, 1000.000000000000000 ) ;
#50042 = CYLINDRICAL_SURFACE ( 'NONE', #2720, 5.000000000000000000 ) ;
#50043 = CARTESIAN_POINT ( 'NONE',  ( 5.000000000000000888, -92.58333333333334281, 2.886751345948126879 ) ) ;
#50044 = CARTESIAN_POINT ( 'NONE',  ( -3.152548672688508926E-16, -88.56249999863439371, -5.148502694627439702 ) ) ;
#50045 = CIRCLE ( 'NONE', #4861, 5.000000000000000000 ) ;
#50046 = VECTOR ( 'NONE', #54375, 1000.000000000000000 ) ;
#50047 = CARTESIAN_POINT ( 'NONE',  ( -2.229367062499996610, 5.854166668032262599, 3.861377020970582219 ) ) ;
#50048 = AXIS2_PLACEMENT_3D ( 'NONE', #12064, #46488, #36839 ) ;
#50049 = DIRECTION ( 'NONE',  ( -0.000000000000000000, -0.000000000000000000, 1.000000000000000000 ) ) ;
#50050 = CARTESIAN_POINT ( 'NONE',  ( -6.972266317189433020E-16, -5.124999997268812280, -5.000000000000000000 ) ) ;
#50051 = CARTESIAN_POINT ( 'NONE',  ( 4.458734125000001214, 18.85416666803226349, 2.574251347313718519 ) ) ;
#50052 = CARTESIAN_POINT ( 'NONE',  ( -2.500000000000000444, -74.16666666666665719, -4.330127018922193649 ) ) ;
#50053 = CARTESIAN_POINT ( 'NONE',  ( 2.499999999999998668, 5.791666669397853795, -4.330127018922193649 ) ) ;
#50055 = ORIENTED_EDGE ( 'NONE', *, *, #32316, .T. ) ;
#50054 = EDGE_CURVE ( 'NONE', #53062, #53577, #34034, .T. ) ;
#50056 = CARTESIAN_POINT ( 'NONE',  ( -1.339745962155613812, -98.20534180126146850, -5.000000000000000000 ) ) ;
#50057 = EDGE_LOOP ( 'NONE', ( #25471, #8242, #45089, #6512 ) ) ;
#50058 = FACE_OUTER_BOUND ( 'NONE', #2321, .T. ) ;
#50059 = CARTESIAN_POINT ( 'NONE',  ( -2.229367062500000163, -38.47916666530107221, -3.861377020970580443 ) ) ;
#50060 = EDGE_CURVE ( 'NONE', #57220, #6403, #24374, .T. ) ;
#50061 = EDGE_CURVE ( 'NONE', #39400, #57534, #42333, .T. ) ;
#50062 = CARTESIAN_POINT ( 'NONE',  ( 2.500000000000002220, -37.54166666393548013, 4.330127018922192761 ) ) ;
#50063 = ORIENTED_EDGE ( 'NONE', *, *, #34637, .T. ) ;
#50064 = CARTESIAN_POINT ( 'NONE',  ( 4.458734124999999437, -15.81249999863440436, -5.460374474430324690E-16 ) ) ;
#50065 = ORIENTED_EDGE ( 'NONE', *, *, #40068, .F. ) ;
#50066 = CARTESIAN_POINT ( 'NONE',  ( 5.000000000000000000, -83.49999999999998579, -6.123233995736766282E-16 ) ) ;
#50067 = CARTESIAN_POINT ( 'NONE',  ( 4.458734125000000326, -168.3750000013655779, -1.846868145590734978 ) ) ;
#50068 = CARTESIAN_POINT ( 'NONE',  ( 2.499999999999998668, -85.20833333060214443, -4.330127018922193649 ) ) ;
#50070 = VERTEX_POINT ( 'NONE', #3834 ) ;
#50069 = DIRECTION ( 'NONE',  ( -0.000000000000000000, 1.000000000000000000, -0.000000000000000000 ) ) ;
#50071 = CARTESIAN_POINT ( 'NONE',  ( -59.81910112700025905, -143.1875000000000000, -2.462841084822630311 ) ) ;
#50072 = CARTESIAN_POINT ( 'NONE',  ( 4.458734124999998549, -27.97916666530107577, -2.574251347313721627 ) ) ;
#50073 = CARTESIAN_POINT ( 'NONE',  ( -6.972266317189433020E-16, 3.749999999999999556, -5.000000000000000000 ) ) ;
#50074 = ORIENTED_EDGE ( 'NONE', *, *, #26702, .F. ) ;
#50075 = CARTESIAN_POINT ( 'NONE',  ( 3.152801135295367541, -164.5625000013656063, -3.152801135295367541 ) ) ;
#50076 = CARTESIAN_POINT ( 'NONE',  ( 4.458734124999998549, 28.27083333469892779, -2.574251347313721627 ) ) ;
#50077 = CARTESIAN_POINT ( 'NONE',  ( -6.972266317189433020E-16, -39.12499999726880162, -5.000000000000000000 ) ) ;
#50078 = ORIENTED_EDGE ( 'NONE', *, *, #42855, .F. ) ;
#50079 = CARTESIAN_POINT ( 'NONE',  ( -52.10840900171896806, -146.4375000013656063, 3.393966926194110556 ) ) ;
#50080 = CARTESIAN_POINT ( 'NONE',  ( -4.458734124999998549, -75.47916666530107932, 2.574251347313722516 ) ) ;
#50081 = CARTESIAN_POINT ( 'NONE',  ( -57.46284108482265651, -133.0625000027312410, 4.819101127000239515 ) ) ;
#50082 = CARTESIAN_POINT ( 'NONE',  ( -4.458734124999997661, -42.22916666530107932, 2.574251347313722516 ) ) ;
#50083 = CARTESIAN_POINT ( 'NONE',  ( 4.458734124999999437, -141.6875000013656063, 0.000000000000000000 ) ) ;
#50084 = VECTOR ( 'NONE', #50169, 1000.000000000000000 ) ;
#50085 = DIRECTION ( 'NONE',  ( -0.000000000000000000, 1.000000000000000000, -0.000000000000000000 ) ) ;
#50086 = CARTESIAN_POINT ( 'NONE',  ( -4.458734124999997661, -47.22916666530105800, 2.574251347313722516 ) ) ;
#50087 = MANIFOLD_SOLID_BREP ( 'EndChamfer', #57235 ) ;
#50088 = CARTESIAN_POINT ( 'NONE',  ( 6.123233995736766282E-16, -120.0000000000000000, -5.000000000000000000 ) ) ;
#50089 = AXIS2_PLACEMENT_3D ( 'NONE', #15481, #59872, #5822 ) ;
#50090 = CARTESIAN_POINT ( 'NONE',  ( 9.457646018065525792E-16, -18.06249999863440436, 5.148502694627439702 ) ) ;
#50091 = CARTESIAN_POINT ( 'NONE',  ( 1.060575238724906964E-15, -102.7500000000000142, 5.773502691896257311 ) ) ;
#50092 = DIRECTION ( 'NONE',  ( 0.000000000000000000, 1.000000000000000000, 0.000000000000000000 ) ) ;
#50093 = CARTESIAN_POINT ( 'NONE',  ( 2.229367062500001939, -34.22916666530107221, 3.861377020970579999 ) ) ;
#50094 = CARTESIAN_POINT ( 'NONE',  ( -5.000000000000000000, 9.125000002731184168, 0.000000000000000000 ) ) ;
#50095 = CARTESIAN_POINT ( 'NONE',  ( -1.339745962155610925, -6.669658196007334894, 5.000000000000000000 ) ) ;
#50096 = CARTESIAN_POINT ( 'NONE',  ( -50.55543936806279248, -128.0625000013656063, 0.3552334253322060320 ) ) ;
#50097 = CARTESIAN_POINT ( 'NONE',  ( 4.458734124999999437, -74.06249999863440792, -5.460374474430324690E-16 ) ) ;
#50098 = CARTESIAN_POINT ( 'NONE',  ( 2.499999999999998668, -34.33333333333332860, -4.330127018922193649 ) ) ;
#50099 = CARTESIAN_POINT ( 'NONE',  ( 9.457646018065525792E-16, 0.6875000013655957476, 5.148502694627439702 ) ) ;
#50100 = ORIENTED_EDGE ( 'NONE', *, *, #41324, .F. ) ;
#50101 = CARTESIAN_POINT ( 'NONE',  ( -2.071067811865580754, -159.6874999999999716, -4.999999999999894307 ) ) ;
#50103 = CARTESIAN_POINT ( 'NONE',  ( -2.229367062500000163, -34.47916666530107221, -3.861377020970580443 ) ) ;
#50102 = CARTESIAN_POINT ( 'NONE',  ( -4.458734124999999437, -90.39583333196773651, -2.574251347313719407 ) ) ;
#50104 = CARTESIAN_POINT ( 'NONE',  ( 1.339745962155615144, -9.705341801261479162, 4.999999999999999112 ) ) ;
#50105 = CARTESIAN_POINT ( 'NONE',  ( -2.229367062500000163, -80.72916666530106511, -3.861377020970580443 ) ) ;
#50106 = CARTESIAN_POINT ( 'NONE',  ( -2.229367062500000163, 17.27083333469892779, -3.861377020970580443 ) ) ;
#50107 = FACE_OUTER_BOUND ( 'NONE', #36981, .T. ) ;
#50108 = CARTESIAN_POINT ( 'NONE',  ( -59.44456063193725015, -139.5625000013656063, -0.3552334253322034230 ) ) ;
#50109 = CARTESIAN_POINT ( 'NONE',  ( 4.458734124999998549, -3.729166665301070438, -2.574251347313721627 ) ) ;
#50110 = CARTESIAN_POINT ( 'NONE',  ( 9.457646018065525792E-16, 23.68750000136559564, 5.148502694627439702 ) ) ;
#50111 = CARTESIAN_POINT ( 'NONE',  ( 4.458734125000000326, -48.14583333196773651, 2.574251347313718519 ) ) ;
#50112 = CARTESIAN_POINT ( 'NONE',  ( 0.000000000000000000, -170.0000000000000000, 0.000000000000000000 ) ) ;
#50113 = CARTESIAN_POINT ( 'NONE',  ( 4.458734124999999437, -86.81249999863439371, -5.460374474430324690E-16 ) ) ;
#50114 = CARTESIAN_POINT ( 'NONE',  ( -2.229367062499996610, -4.145833331967739177, 3.861377020970582219 ) ) ;
#50115 = VERTEX_POINT ( 'NONE', #275 ) ;
#50116 = CARTESIAN_POINT ( 'NONE',  ( 4.458734125000000326, -30.14583333196773651, 2.574251347313718519 ) ) ;
#50117 = CARTESIAN_POINT ( 'NONE',  ( -59.29741812935640155, -131.8750000013656347, -2.196230717870135685 ) ) ;
#50118 = CARTESIAN_POINT ( 'NONE',  ( -3.152548672688508926E-16, -76.56249999863440792, -5.148502694627439702 ) ) ;
#50119 = CARTESIAN_POINT ( 'NONE',  ( 5.000000000000000888, -109.4583333306021586, 2.886751345948126879 ) ) ;
#50120 =( BOUNDED_CURVE ( )  B_SPLINE_CURVE ( 2, ( #15762, #40201, #25085, #16078, #40514, #11564, #26050, #59837, #54999 ),
 .UNSPECIFIED., .F., .F. ) 
 B_SPLINE_CURVE_WITH_KNOTS ( ( 3, 2, 2, 2, 3 ),
 ( 0.1660714285714285643, 0.1666666666666666574, 0.1678571428571428437, 0.1690476190476190577, 0.1696428571428571508 ),
 .UNSPECIFIED. ) 
 CURVE ( )  GEOMETRIC_REPRESENTATION_ITEM ( )  RATIONAL_B_SPLINE_CURVE ( ( 0.9330127018922194093, 0.9330127018922194093, 1.000000000000000000, 0.8660254037844387076, 1.000000000000000000, 0.8660254037844387076, 1.000000000000000000, 0.9330127018922194093, 0.9330127018922194093 ) ) 
 REPRESENTATION_ITEM ( '' )  );
#50121 = CARTESIAN_POINT ( 'NONE',  ( 2.229367062499998831, 20.35416666803225993, -3.861377020970580887 ) ) ;
#50122 = CARTESIAN_POINT ( 'NONE',  ( 1.975475456537005874E-15, 10.24999999999999822, 5.000000000000000000 ) ) ;
#50123 = CARTESIAN_POINT ( 'NONE',  ( 0.000000000000000000, -120.0000000000000000, 0.000000000000000000 ) ) ;
#50124 = CARTESIAN_POINT ( 'NONE',  ( 4.458734124999999437, -78.06249999863440792, -5.460374474430324690E-16 ) ) ;
#50125 = CARTESIAN_POINT ( 'NONE',  ( -2.499999999999996447, -56.83333333333333570, 4.330127018922195425 ) ) ;
#50126 = CARTESIAN_POINT ( 'NONE',  ( -58.24261429053147765, -151.2500000000000284, -3.805975901505573855 ) ) ;
#50127 = CARTESIAN_POINT ( 'NONE',  ( -4.999999999999999112, 24.20833333606451987, 2.886751345948131764 ) ) ;
#50128 = ORIENTED_EDGE ( 'NONE', *, *, #57123, .F. ) ;
#50129 = CARTESIAN_POINT ( 'NONE',  ( 0.000000000000000000, -120.0000000000000000, 0.000000000000000000 ) ) ;
#50130 = CARTESIAN_POINT ( 'NONE',  ( -6.972266317189433020E-16, -52.12499999726880873, -5.000000000000000000 ) ) ;
#50132 = CARTESIAN_POINT ( 'NONE',  ( 5.000000000000000000, -16.50000000000000000, -6.123233995736766282E-16 ) ) ;
#50131 = CARTESIAN_POINT ( 'NONE',  ( -3.535533905932737309, -149.6250000000000000, -3.535533905932738197 ) ) ;
#50133 = CARTESIAN_POINT ( 'NONE',  ( -4.458734124999999437, -24.39583333196773651, -2.574251347313719407 ) ) ;
#50134 = CARTESIAN_POINT ( 'NONE',  ( -3.152548672688508926E-16, -82.56249999863440792, -5.148502694627439702 ) ) ;
#50135 = CARTESIAN_POINT ( 'NONE',  ( -4.999999999999999112, -25.79166666393547658, 2.886751345948131764 ) ) ;
#50137 = ORIENTED_EDGE ( 'NONE', *, *, #36629, .T. ) ;
#50136 = CARTESIAN_POINT ( 'NONE',  ( 4.458734124999999437, -52.81249999863440792, -5.460374474430324690E-16 ) ) ;
#50138 = CARTESIAN_POINT ( 'NONE',  ( -6.972266317189433020E-16, -90.12499999726880162, -5.000000000000000000 ) ) ;
#50139 = DIRECTION ( 'NONE',  ( -0.000000000000000000, 1.000000000000000000, -0.000000000000000000 ) ) ;
#50141 = ORIENTED_EDGE ( 'NONE', *, *, #45902, .T. ) ;
#50140 = CARTESIAN_POINT ( 'NONE',  ( 4.458734124999999437, -6.062499998634403475, -5.460374474430324690E-16 ) ) ;
#50142 = CARTESIAN_POINT ( 'NONE',  ( -57.19623071787016499, -149.3750000013656063, 4.297418129356382899 ) ) ;
#50143 = CARTESIAN_POINT ( 'NONE',  ( 2.499999999999998668, -66.33333333333332860, -4.330127018922193649 ) ) ;
#50144 = CARTESIAN_POINT ( 'NONE',  ( 2.730187237215162345E-16, -152.4375000013655779, -4.458734124999999437 ) ) ;
#50145 = CARTESIAN_POINT ( 'NONE',  ( -4.458734124999998549, -44.47916666530106511, 2.574251347313722516 ) ) ;
#50146 = CARTESIAN_POINT ( 'NONE',  ( -1.339745962155613812, -81.08034179853028434, -5.000000000000000000 ) ) ;
#50147 = CARTESIAN_POINT ( 'NONE',  ( 5.000000000000000000, -159.0000000000000000, 0.000000000000000000 ) ) ;
#50148 = CARTESIAN_POINT ( 'NONE',  ( 6.123233995736766282E-16, -120.0000000000000000, -5.000000000000000000 ) ) ;
#50149 = CARTESIAN_POINT ( 'NONE',  ( -51.75738570946856498, -153.7500000000000284, 3.805975901505576964 ) ) ;
#50150 = CARTESIAN_POINT ( 'NONE',  ( 4.458734124999998549, -12.97916666530107044, -2.574251347313721627 ) ) ;
#50151 = AXIS2_PLACEMENT_3D ( 'NONE', #51621, #6922, #17525 ) ;
#50152 = CARTESIAN_POINT ( 'NONE',  ( 4.458734124999998549, -49.97916666530106511, -2.574251347313721627 ) ) ;
#50153 = DIRECTION ( 'NONE',  ( 0.000000000000000000, 0.000000000000000000, 1.000000000000000000 ) ) ;
#50154 = CARTESIAN_POINT ( 'NONE',  ( 3.152801135295367541, -146.3125000013655779, -3.152801135295367541 ) ) ;
#50155 = CARTESIAN_POINT ( 'NONE',  ( -4.458734124999999437, -95.56249999863440792, 0.000000000000000000 ) ) ;
#50156 = CARTESIAN_POINT ( 'NONE',  ( 1.062108568985190270E-13, -11.12499999726881761, -4.999999999999999112 ) ) ;
#50157 = ORIENTED_EDGE ( 'NONE', *, *, #15318, .F. ) ;
#50158 = CARTESIAN_POINT ( 'NONE',  ( 4.458734124999999437, 26.93750000136559564, -5.460374474430324690E-16 ) ) ;
#50159 = CARTESIAN_POINT ( 'NONE',  ( -50.01589407740564042, -146.7500000027312126, 0.3983568153799778022 ) ) ;
#50160 = CARTESIAN_POINT ( 'NONE',  ( 5.000000000000000000, -30.41666666666666785, -2.886751345948130876 ) ) ;
#50161 = EDGE_CURVE ( 'NONE', #6339, #6165, #33100, .T. ) ;
#50162 = ORIENTED_EDGE ( 'NONE', *, *, #50060, .T. ) ;
#50163 = CARTESIAN_POINT ( 'NONE',  ( 9.457646018065525792E-16, -2.062499998634407028, 5.148502694627439702 ) ) ;
#50164 = CARTESIAN_POINT ( 'NONE',  ( 1.339745962155615144, -106.7053418012614543, 4.999999999999999112 ) ) ;
#50165 = CARTESIAN_POINT ( 'NONE',  ( 2.229367062500001939, -19.22916666530106866, 3.861377020970579999 ) ) ;
#50166 =( BOUNDED_CURVE ( )  B_SPLINE_CURVE ( 2, ( #55070, #10992, #6822, #30613, #26428, #45411, #46046, #2011, #1379 ),
 .UNSPECIFIED., .F., .F. ) 
 B_SPLINE_CURVE_WITH_KNOTS ( ( 3, 2, 2, 2, 3 ),
 ( 0.1125000000000000028, 0.1130952380952380959, 0.1142857142857142821, 0.1154761904761904823, 0.1160714285714285754 ),
 .UNSPECIFIED. ) 
 CURVE ( )  GEOMETRIC_REPRESENTATION_ITEM ( )  RATIONAL_B_SPLINE_CURVE ( ( 0.9330127018922194093, 0.9330127018922194093, 1.000000000000000000, 0.8660254037844387076, 1.000000000000000000, 0.8660254037844387076, 1.000000000000000000, 0.9330127018922194093, 0.9330127018922194093 ) ) 
 REPRESENTATION_ITEM ( '' )  );
#50167 = CARTESIAN_POINT ( 'NONE',  ( 2.500000000000002220, 11.45833333606451809, 4.330127018922192761 ) ) ;
#50168 = CARTESIAN_POINT ( 'NONE',  ( 4.458734125000001214, -5.895833331967740953, 2.574251347313718519 ) ) ;
#50169 = DIRECTION ( 'NONE',  ( -0.000000000000000000, 1.000000000000000000, -0.000000000000000000 ) ) ;
#50170 = CARTESIAN_POINT ( 'NONE',  ( -3.152801135295367985, -149.8125000013655779, 3.152801135295367096 ) ) ;
#50171 =( BOUNDED_CURVE ( )  B_SPLINE_CURVE ( 2, ( #17389, #12548, #45698, #55679, #7104, #41490, #2595, #30901, #26394 ),
 .UNSPECIFIED., .F., .F. ) 
 B_SPLINE_CURVE_WITH_KNOTS ( ( 3, 2, 2, 2, 3 ),
 ( 0.5479166666666667185, 0.5486111111111111605, 0.5500000000000000444, 0.5513888888888889284, 0.5520833333333333703 ),
 .UNSPECIFIED. ) 
 CURVE ( )  GEOMETRIC_REPRESENTATION_ITEM ( )  RATIONAL_B_SPLINE_CURVE ( ( 0.9330127018922194093, 0.9330127018922194093, 1.000000000000000000, 0.8660254037844387076, 1.000000000000000000, 0.8660254037844387076, 1.000000000000000000, 0.9330127018922194093, 0.9330127018922194093 ) ) 
 REPRESENTATION_ITEM ( '' )  );
#50172 = AXIS2_PLACEMENT_3D ( 'NONE', #20678, #21307, #60869 ) ;
#50173 = CARTESIAN_POINT ( 'NONE',  ( 4.458734124999999437, 16.93750000136559564, -5.460374474430324690E-16 ) ) ;
#50174 = ORIENTED_EDGE ( 'NONE', *, *, #7679, .T. ) ;
#50175 = CARTESIAN_POINT ( 'NONE',  ( -1.339745962155610925, -13.66965819600733489, 5.000000000000000000 ) ) ;
#50176 = CARTESIAN_POINT ( 'NONE',  ( 1.250000000000000222, 7.938566201357357244, -7.198902722707428481 ) ) ;
#50177 = CARTESIAN_POINT ( 'NONE',  ( -2.229367062499996610, -21.14583333196774007, 3.861377020970582219 ) ) ;
#50178 = VECTOR ( 'NONE', #36387, 1000.000000000000000 ) ;
#50179 = CARTESIAN_POINT ( 'NONE',  ( -58.24261429053147765, -145.2500000000000284, -3.805975901505573855 ) ) ;
#50180 = CARTESIAN_POINT ( 'NONE',  ( -55.35523342533222291, -149.3125000013656063, 4.444560631937231499 ) ) ;
#50181 = CARTESIAN_POINT ( 'NONE',  ( -5.000000000000000000, -44.95833333060215153, -2.886751345948128211 ) ) ;
#50182 = CARTESIAN_POINT ( 'NONE',  ( 6.123233995736766282E-16, -170.0000000000000000, -5.000000000000000000 ) ) ;
#50183 = CARTESIAN_POINT ( 'NONE',  ( 2.229367062499998831, 14.35416666803226171, -3.861377020970580887 ) ) ;
#50184 = CARTESIAN_POINT ( 'NONE',  ( 0.000000000000000000, -170.0000000000000000, 0.000000000000000000 ) ) ;
#50185 = CARTESIAN_POINT ( 'NONE',  ( 5.000000000000000000, 9.499999999999998224, -6.123233995736766282E-16 ) ) ;
#50186 = CARTESIAN_POINT ( 'NONE',  ( 4.458734125000000326, 10.10416666803226171, 2.574251347313718519 ) ) ;
#50187 = CARTESIAN_POINT ( 'NONE',  ( 4.458734124999999437, -66.81249999863440792, -5.460374474430324690E-16 ) ) ;
#50188 = VERTEX_POINT ( 'NONE', #14095 ) ;
#50189 = CARTESIAN_POINT ( 'NONE',  ( -2.229367062499996610, -13.39583333196774007, 3.861377020970582219 ) ) ;
#50190 = CARTESIAN_POINT ( 'NONE',  ( 5.000000000000000000, 2.499999999999998668, -6.123233995736766282E-16 ) ) ;
#50191 = CARTESIAN_POINT ( 'NONE',  ( 4.458734124999999437, -163.5000000013655779, 1.846868145590737864 ) ) ;
#50192 = CARTESIAN_POINT ( 'NONE',  ( -2.500000000000000444, -38.16666666666667140, -4.330127018922193649 ) ) ;
#50193 = CARTESIAN_POINT ( 'NONE',  ( -2.229367062499996610, -60.14583333196774362, 3.861377020970582219 ) ) ;
#50194 = CARTESIAN_POINT ( 'NONE',  ( 5.000000000000000000, -95.37499999726881583, -6.123233995736766282E-16 ) ) ;
#50195 = CARTESIAN_POINT ( 'NONE',  ( -2.229367062500000163, -33.47916666530107221, -3.861377020970580443 ) ) ;
#50196 = CIRCLE ( 'NONE', #18381, 5.000000000000000000 ) ;
#50197 = CARTESIAN_POINT ( 'NONE',  ( -2.499999999999996447, -41.70833333060214443, 4.330127018922195425 ) ) ;
#50198 = CARTESIAN_POINT ( 'NONE',  ( -6.972266317189433020E-16, -29.12499999726881228, -5.000000000000000000 ) ) ;
#50199 = CARTESIAN_POINT ( 'NONE',  ( 1.975475456537005874E-15, -63.62499999726880873, 5.000000000000000000 ) ) ;
#50200 = CARTESIAN_POINT ( 'NONE',  ( 5.000000000000000000, 1.583333333333332371, -2.886751345948130876 ) ) ;
#50201 = CARTESIAN_POINT ( 'NONE',  ( -1.846868145590734756, -149.3750000013656063, -4.458734124999999437 ) ) ;
#50202 =( BOUNDED_CURVE ( )  B_SPLINE_CURVE ( 2, ( #28203, #4392, #49405, #4700, #34285, #5669, #9530, #24323, #19813 ),
 .UNSPECIFIED., .F., .F. ) 
 B_SPLINE_CURVE_WITH_KNOTS ( ( 3, 2, 2, 2, 3 ),
 ( 0.2767857142857143016, 0.2773809523809523947, 0.2785714285714285809, 0.2797619047619047672, 0.2803571428571428603 ),
 .UNSPECIFIED. ) 
 CURVE ( )  GEOMETRIC_REPRESENTATION_ITEM ( )  RATIONAL_B_SPLINE_CURVE ( ( 0.9330127018922194093, 0.9330127018922194093, 1.000000000000000000, 0.8660254037844387076, 1.000000000000000000, 0.8660254037844387076, 1.000000000000000000, 0.9330127018922194093, 0.9330127018922194093 ) ) 
 REPRESENTATION_ITEM ( '' )  );
#50203 = CARTESIAN_POINT ( 'NONE',  ( 2.500000000000002220, -45.66666666666666430, 4.330127018922192761 ) ) ;
#50204 = CARTESIAN_POINT ( 'NONE',  ( 7.500000000000000000, -4.330127018922199866, -7.422398894150035176 ) ) ;
#50205 = CARTESIAN_POINT ( 'NONE',  ( 5.000000000000000000, -86.37499999726880162, -6.123233995736766282E-16 ) ) ;
#50206 = ORIENTED_EDGE ( 'NONE', *, *, #40089, .F. ) ;
#50207 = CARTESIAN_POINT ( 'NONE',  ( 4.458734124999998549, -104.7291666653010509, -2.574251347313721627 ) ) ;
#50208 = CARTESIAN_POINT ( 'NONE',  ( -3.152548672688508926E-16, 2.187500001365593416, -5.148502694627439702 ) ) ;
#50209 = CARTESIAN_POINT ( 'NONE',  ( 2.499999999999998668, -59.33333333333333570, -4.330127018922193649 ) ) ;
#50210 = CARTESIAN_POINT ( 'NONE',  ( 1.060575238724906964E-15, -3.750000000000003553, 5.773502691896257311 ) ) ;
#50211 = CARTESIAN_POINT ( 'NONE',  ( -4.458734124999999437, -67.31249999863440792, 0.000000000000000000 ) ) ;
#50212 = CARTESIAN_POINT ( 'NONE',  ( -51.75738570946856498, -147.8750000027312126, 3.805975901505576964 ) ) ;
#50213 = CARTESIAN_POINT ( 'NONE',  ( -5.000000000000000000, -9.958333330602144429, -2.886751345948128211 ) ) ;
#50215 = ORIENTED_EDGE ( 'NONE', *, *, #13455, .F. ) ;
#50214 = CARTESIAN_POINT ( 'NONE',  ( 4.458734125000001214, -35.89583333196773651, 2.574251347313718519 ) ) ;
#50216 = CARTESIAN_POINT ( 'NONE',  ( 3.061616997868383141E-16, -165.7500000000000000, -5.000000000000000000 ) ) ;
#50217 = DIRECTION ( 'NONE',  ( -0.000000000000000000, 1.000000000000000000, -0.000000000000000000 ) ) ;
#50219 = ORIENTED_EDGE ( 'NONE', *, *, #39433, .T. ) ;
#50218 = CARTESIAN_POINT ( 'NONE',  ( -4.458734124999998549, 14.52083333469892779, 2.574251347313722516 ) ) ;
#50220 = CARTESIAN_POINT ( 'NONE',  ( -2.499999999999996447, -48.70833333060213732, 4.330127018922195425 ) ) ;
#50221 = CARTESIAN_POINT ( 'NONE',  ( 5.000000000000000000, -50.50000000000000000, -6.123233995736766282E-16 ) ) ;
#50222 = CARTESIAN_POINT ( 'NONE',  ( -4.458734124999998549, -32.47916666530107221, 2.574251347313722516 ) ) ;
#50223 = VECTOR ( 'NONE', #47683, 1000.000000000000000 ) ;
#50224 = CARTESIAN_POINT ( 'NONE',  ( 0.000000000000000000, -120.0000000000000000, 5.000000000000000000 ) ) ;
#50225 = CARTESIAN_POINT ( 'NONE',  ( -4.458734124999999437, -75.39583333196773651, -2.574251347313719407 ) ) ;
#50226 =( BOUNDED_CURVE ( )  B_SPLINE_CURVE ( 2, ( #35611, #32044, #6984, #7306, #55237, #1852, #1222, #36246, #21134 ),
 .UNSPECIFIED., .F., .F. ) 
 B_SPLINE_CURVE_WITH_KNOTS ( ( 3, 2, 2, 2, 3 ),
 ( 0.07500000000000005274, 0.07916666666666671848, 0.08333333333333339810, 0.08750000000000007772, 0.09166666666666674346 ),
 .UNSPECIFIED. ) 
 CURVE ( )  GEOMETRIC_REPRESENTATION_ITEM ( )  RATIONAL_B_SPLINE_CURVE ( ( 0.9999999999999990008, 0.9238795325112877377, 1.000000000000000000, 0.9238795325112867385, 1.000000000000000000, 0.9238795325112867385, 1.000000000000000000, 0.9238795325112851842, 1.000000000000001554 ) ) 
 REPRESENTATION_ITEM ( '' )  );
#50227 = CARTESIAN_POINT ( 'NONE',  ( -1.846868145590734756, -141.3750000013656063, -4.458734125000000326 ) ) ;
#50228 = CARTESIAN_POINT ( 'NONE',  ( -4.458734124999999437, -80.31249999863440792, 0.000000000000000000 ) ) ;
#50229 = AXIS2_PLACEMENT_3D ( 'NONE', #46448, #2394, #61249 ) ;
#50230 = CARTESIAN_POINT ( 'NONE',  ( -56.48576386720575471, -137.0000000013655779, -4.591703134518078322 ) ) ;
#50231 = CARTESIAN_POINT ( 'NONE',  ( -2.229367062499996610, -32.39583333196773651, 3.861377020970582219 ) ) ;
#50232 = VERTEX_POINT ( 'NONE', #8648 ) ;
#50233 = CARTESIAN_POINT ( 'NONE',  ( 0.000000000000000000, -170.0000000000000000, 5.000000000000000000 ) ) ;
#50234 = EDGE_LOOP ( 'NONE', ( #10728, #55781, #13233 ) ) ;
#50235 = CARTESIAN_POINT ( 'NONE',  ( 4.458734124999998549, -77.97916666530106511, -2.574251347313721627 ) ) ;
#50236 = CARTESIAN_POINT ( 'NONE',  ( -5.000000000000000000, 22.12500000273118417, 0.000000000000000000 ) ) ;
#50237 = ORIENTED_EDGE ( 'NONE', *, *, #24837, .F. ) ;
#50238 = CARTESIAN_POINT ( 'NONE',  ( -2.500000000000000444, -15.04166666393548191, -4.330127018922193649 ) ) ;
#50239 = CARTESIAN_POINT ( 'NONE',  ( -4.999999999999998224, 8.083333333333332149, 2.886751345948131764 ) ) ;
#50241 = ADVANCED_FACE ( 'NONE', ( #45914 ), #25666, .F. ) ;
#50240 = CARTESIAN_POINT ( 'NONE',  ( 2.229367062499998831, -63.89583333196772941, -3.861377020970580887 ) ) ;
#50242 = CARTESIAN_POINT ( 'NONE',  ( 4.458734125000001214, -3.145833331967738733, 2.574251347313718519 ) ) ;
#50243 = ORIENTED_EDGE ( 'NONE', *, *, #4362, .F. ) ;
#50244 = CYLINDRICAL_SURFACE ( 'NONE', #63501, 5.000000000000000000 ) ;
#50245 = FACE_OUTER_BOUND ( 'NONE', #40421, .T. ) ;
#50246 = CARTESIAN_POINT ( 'NONE',  ( -4.458734124999999437, 5.604166668032262599, -2.574251347313719407 ) ) ;
#50247 = CARTESIAN_POINT ( 'NONE',  ( -50.40829686548195099, -140.0000000013656063, -1.485763867205728284 ) ) ;
#50248 = CARTESIAN_POINT ( 'NONE',  ( -55.39835681537999790, -154.8750000000000284, 4.984105922594378235 ) ) ;
#50249 = CARTESIAN_POINT ( 'NONE',  ( -1.846868145590734756, -160.1250000013655779, -4.458734124999999437 ) ) ;
#50250 = CARTESIAN_POINT ( 'NONE',  ( -5.000000000000000000, 19.04166666939784847, -2.886751345948128211 ) ) ;
#50251 = ORIENTED_EDGE ( 'NONE', *, *, #26751, .T. ) ;
#50252 = CARTESIAN_POINT ( 'NONE',  ( 2.229367062500001939, -79.97916666530106511, 3.861377020970579999 ) ) ;
#50253 = CARTESIAN_POINT ( 'NONE',  ( -2.499999999999996447, -96.83333333333332860, 4.330127018922195425 ) ) ;
#50254 = CARTESIAN_POINT ( 'NONE',  ( 4.458734125000001214, -5.895833331967740953, 2.574251347313718519 ) ) ;
#50255 = CARTESIAN_POINT ( 'NONE',  ( 1.339745962155615588, 25.83034180399265622, -4.999999999999997335 ) ) ;
#50256 = EDGE_CURVE ( 'NONE', #11403, #28956, #52672, .T. ) ;
#50257 = CARTESIAN_POINT ( 'NONE',  ( 2.499999999999998668, -36.33333333333332860, -4.330127018922193649 ) ) ;
#50258 = CARTESIAN_POINT ( 'NONE',  ( 9.457646018065525792E-16, -71.31249999863439371, 5.148502694627439702 ) ) ;
#50259 = CARTESIAN_POINT ( 'NONE',  ( 2.499999999999998668, -28.20833333060214798, -4.330127018922193649 ) ) ;
#50260 = EDGE_CURVE ( 'NONE', #21155, #19310, #29834, .T. ) ;
#50261 = CARTESIAN_POINT ( 'NONE',  ( 1.339745962155615144, 12.41965820146970501, 4.999999999999999112 ) ) ;
#50262 = CARTESIAN_POINT ( 'NONE',  ( -1.336351044127974539E-14, 23.24999999999999645, 5.000000000000000000 ) ) ;
#50263 = CARTESIAN_POINT ( 'NONE',  ( 2.229367062500001939, 27.02083333469892423, 3.861377020970579999 ) ) ;
#50264 = CARTESIAN_POINT ( 'NONE',  ( -2.229367062499996610, -51.14583333196772941, 3.861377020970582219 ) ) ;
#50265 = CARTESIAN_POINT ( 'NONE',  ( 4.458734124999998549, -34.97916666530107221, -2.574251347313721627 ) ) ;
#50266 = CARTESIAN_POINT ( 'NONE',  ( 9.457646018065525792E-16, 3.687500001365594748, 5.148502694627439702 ) ) ;
#50267 = AXIS2_PLACEMENT_3D ( 'NONE', #63499, #39902, #45379 ) ;
#50268 = CARTESIAN_POINT ( 'NONE',  ( 2.071067811865392461, -146.3125000027312694, 5.000000000000084377 ) ) ;
#50269 = CARTESIAN_POINT ( 'NONE',  ( -5.000000000000000000, 20.99999999999999645, 0.000000000000000000 ) ) ;
#50270 = CARTESIAN_POINT ( 'NONE',  ( 2.071067811865476394, -147.3125000027311842, 5.000000000000000000 ) ) ;
#50271 = CARTESIAN_POINT ( 'NONE',  ( 1.975475456537005874E-15, -33.62499999726880873, 5.000000000000000000 ) ) ;
#50272 = AXIS2_PLACEMENT_3D ( 'NONE', #21336, #30660, #51250 ) ;
#50273 = CARTESIAN_POINT ( 'NONE',  ( 9.457646018065525792E-16, -41.06249999863440792, 5.148502694627439702 ) ) ;
#50274 = CARTESIAN_POINT ( 'NONE',  ( 1.060575238724906964E-15, -72.62499999726880162, 5.773502691896257311 ) ) ;
#50275 = EDGE_CURVE ( 'NONE', #14167, #12673, #459, .T. ) ;
#50276 = CARTESIAN_POINT ( 'NONE',  ( -50.70258187064364108, -142.3750000013656063, 2.196230717870141014 ) ) ;
#50277 = CARTESIAN_POINT ( 'NONE',  ( -4.458734124999999437, -110.3124999986343937, 0.000000000000000000 ) ) ;
#50278 = CARTESIAN_POINT ( 'NONE',  ( 1.339745962155612702, 3.705341801261478718, -5.000000000000000000 ) ) ;
#50279 = CARTESIAN_POINT ( 'NONE',  ( 9.457646018065525792E-16, -79.31249999863440792, 5.148502694627439702 ) ) ;
#50280 = CARTESIAN_POINT ( 'NONE',  ( 2.730187237215162345E-16, -160.4375000013655779, -4.458734124999999437 ) ) ;
#50281 = CARTESIAN_POINT ( 'NONE',  ( 6.123233995736766282E-16, -120.0000000000000000, -5.000000000000000000 ) ) ;
#50282 = CARTESIAN_POINT ( 'NONE',  ( 2.499999999999998668, -28.33333333333333570, -4.330127018922193649 ) ) ;
#50283 = CARTESIAN_POINT ( 'NONE',  ( 3.152801135295367541, -141.3125000013655779, -3.152801135295367541 ) ) ;
#50284 = VERTEX_POINT ( 'NONE', #21156 ) ;
#50285 = CARTESIAN_POINT ( 'NONE',  ( -2.229367062499996610, 25.60416666803225993, 3.861377020970582219 ) ) ;
#50286 = ORIENTED_EDGE ( 'NONE', *, *, #28401, .F. ) ;
#50287 = CARTESIAN_POINT ( 'NONE',  ( 2.229367062499998831, -63.89583333196772941, -3.861377020970580887 ) ) ;
#50288 = CARTESIAN_POINT ( 'NONE',  ( -2.499999999999996447, 21.29166666939785202, 4.330127018922195425 ) ) ;
#50289 = CARTESIAN_POINT ( 'NONE',  ( -2.500000000000000444, -3.041666663935477910, -4.330127018922193649 ) ) ;
#50290 = CARTESIAN_POINT ( 'NONE',  ( 5.000000000000000000, 14.58333333333333215, -2.886751345948129988 ) ) ;
#50291 = CARTESIAN_POINT ( 'NONE',  ( -4.458734124999997661, -48.22916666530106511, 2.574251347313722516 ) ) ;
#50292 = CARTESIAN_POINT ( 'NONE',  ( 4.458734124999999437, -11.81249999863440081, -5.460374474430324690E-16 ) ) ;
#50293 = CARTESIAN_POINT ( 'NONE',  ( 0.000000000000000000, -170.0000000000000000, 5.000000000000000000 ) ) ;
#50294 = EDGE_CURVE ( 'NONE', #59225, #35059, #40762, .T. ) ;
#50295 = CARTESIAN_POINT ( 'NONE',  ( 1.975475456537005874E-15, 14.25000000000000000, 5.000000000000000000 ) ) ;
#50296 = FACE_OUTER_BOUND ( 'NONE', #19534, .T. ) ;
#50297 = CARTESIAN_POINT ( 'NONE',  ( -5.000000000000000000, -74.95833333060214443, -2.886751345948128211 ) ) ;
#50298 = CARTESIAN_POINT ( 'NONE',  ( 1.060575238724906964E-15, -33.75000000000000000, 5.773502691896257311 ) ) ;
#50299 = CARTESIAN_POINT ( 'NONE',  ( 0.000000000000000000, 0.000000000000000000, -9.449444346342714240 ) ) ;
#50300 = CARTESIAN_POINT ( 'NONE',  ( -2.229367062500000163, -12.72916666530107044, -3.861377020970580443 ) ) ;
#50301 = CARTESIAN_POINT ( 'NONE',  ( -2.499999999999996447, -77.70833333060214443, 4.330127018922195425 ) ) ;
#50302 = CARTESIAN_POINT ( 'NONE',  ( 2.229367062499998831, -60.64583333196774362, -3.861377020970580887 ) ) ;
#50303 = CARTESIAN_POINT ( 'NONE',  ( 2.730187237215162345E-16, -152.4375000013655779, -4.458734124999999437 ) ) ;
#50304 = CARTESIAN_POINT ( 'NONE',  ( -2.229367062500000163, -68.47916666530107932, -3.861377020970580443 ) ) ;
#50305 =( BOUNDED_CURVE ( )  B_SPLINE_CURVE ( 2, ( #25866, #25226, #45481, #6570, #59976, #34535, #15899, #35518, #44196 ),
 .UNSPECIFIED., .F., .F. ) 
 B_SPLINE_CURVE_WITH_KNOTS ( ( 3, 2, 2, 2, 3 ),
 ( 0.02678571428571428770, 0.02738095238095238082, 0.02857142857142857054, 0.02976190476190476025, 0.03035714285714285685 ),
 .UNSPECIFIED. ) 
 CURVE ( )  GEOMETRIC_REPRESENTATION_ITEM ( )  RATIONAL_B_SPLINE_CURVE ( ( 0.9330127018922194093, 0.9330127018922195203, 1.000000000000000000, 0.8660254037844387076, 1.000000000000000000, 0.8660254037844387076, 1.000000000000000000, 0.9330127018922194093, 0.9330127018922194093 ) ) 
 REPRESENTATION_ITEM ( '' )  );
#50306 = CARTESIAN_POINT ( 'NONE',  ( 2.499999999999998668, -56.20833333060214443, -4.330127018922193649 ) ) ;
#50307 = ORIENTED_EDGE ( 'NONE', *, *, #52658, .T. ) ;
#50308 = CARTESIAN_POINT ( 'NONE',  ( -6.972266317189433020E-16, -26.25000000000000000, -5.000000000000000000 ) ) ;
#50309 = CARTESIAN_POINT ( 'NONE',  ( 4.458734125000001214, -0.1458333319677394824, 2.574251347313718519 ) ) ;
#50310 = VERTEX_POINT ( 'NONE', #35957 ) ;
#50312 = CARTESIAN_POINT ( 'NONE',  ( 1.339745962155615144, 11.41965820146970501, 4.999999999999999112 ) ) ;
#50311 = CARTESIAN_POINT ( 'NONE',  ( 1.339745962155615144, -21.70534180126147916, 4.999999999999999112 ) ) ;
#50313 = CARTESIAN_POINT ( 'NONE',  ( 3.152801135295366208, -154.5625000013656063, 3.152801135295367985 ) ) ;
#50314 = ORIENTED_EDGE ( 'NONE', *, *, #11054, .T. ) ;
#50315 = AXIS2_PLACEMENT_3D ( 'NONE', #28239, #19530, #58141 ) ;
#50316 = LINE ( 'NONE', #41289, #47790 ) ;
#50317 = CARTESIAN_POINT ( 'NONE',  ( -57.46284108482265651, -130.9375000000000000, 4.819101127000239515 ) ) ;
#50319 = AXIS2_PLACEMENT_3D ( 'NONE', #33525, #9382, #33832 ) ;
#50318 = CARTESIAN_POINT ( 'NONE',  ( 2.500000000000002220, -86.66666666666667140, 4.330127018922192761 ) ) ;
#50321 = EDGE_CURVE ( 'NONE', #10433, #44276, #59634, .T. ) ;
#50320 = CARTESIAN_POINT ( 'NONE',  ( -4.458734124999998549, -48.47916666530106511, 2.574251347313722516 ) ) ;
#50322 = EDGE_LOOP ( 'NONE', ( #28086, #41566, #26656, #47142 ) ) ;
#50323 =( BOUNDED_CURVE ( )  B_SPLINE_CURVE ( 2, ( #2225, #27587, #12484, #42378, #31146, #22145, #2847, #7036, #16997 ),
 .UNSPECIFIED., .F., .F. ) 
 B_SPLINE_CURVE_WITH_KNOTS ( ( 3, 2, 2, 2, 3 ),
 ( 0.1589285714285714191, 0.1595238095238095122, 0.1607142857142857262, 0.1619047619047619124, 0.1625000000000000056 ),
 .UNSPECIFIED. ) 
 CURVE ( )  GEOMETRIC_REPRESENTATION_ITEM ( )  RATIONAL_B_SPLINE_CURVE ( ( 0.9330127018922194093, 0.9330127018922194093, 1.000000000000000000, 0.8660254037844387076, 1.000000000000000000, 0.8660254037844387076, 1.000000000000000000, 0.9330127018922194093, 0.9330127018922194093 ) ) 
 REPRESENTATION_ITEM ( '' )  );
#50324 = EDGE_CURVE ( 'NONE', #29294, #60836, #22251, .T. ) ;
#50325 = EDGE_CURVE ( 'NONE', #49104, #17322, #1876, .T. ) ;
#50326 = CARTESIAN_POINT ( 'NONE',  ( 5.000000000000000000, 10.62500000273118594, -6.123233995736766282E-16 ) ) ;
#50327 = CARTESIAN_POINT ( 'NONE',  ( -4.458734124999999437, 11.68750000136559564, 0.000000000000000000 ) ) ;
#50328 = CARTESIAN_POINT ( 'NONE',  ( 2.229367062499998831, 26.35416666803225993, -3.861377020970580887 ) ) ;
#50329 = CARTESIAN_POINT ( 'NONE',  ( -53.51423613279429503, -151.2500000013656063, 4.591703134518082763 ) ) ;
#50330 = CARTESIAN_POINT ( 'NONE',  ( 5.000000000000000888, 12.54166666939785557, 2.886751345948126879 ) ) ;
#50331 = CARTESIAN_POINT ( 'NONE',  ( -6.972266317189433020E-16, -25.24999999999999645, -5.000000000000000000 ) ) ;
#50332 = CARTESIAN_POINT ( 'NONE',  ( 4.458734124999998549, -63.72916666530106511, -2.574251347313721627 ) ) ;
#50333 = CARTESIAN_POINT ( 'NONE',  ( 1.975475456537005874E-15, 1.250000000000000000, 5.000000000000000000 ) ) ;
#50334 = CARTESIAN_POINT ( 'NONE',  ( 4.458734124999998549, 13.27083333469892779, -2.574251347313721627 ) ) ;
#50335 = DIRECTION ( 'NONE',  ( -1.000000000000000000, -0.000000000000000000, -3.614007241618347908E-17 ) ) ;
#50336 = CARTESIAN_POINT ( 'NONE',  ( -5.000000000000000888, -157.5625000000000853, -2.071067811865475949 ) ) ;
#50337 = CARTESIAN_POINT ( 'NONE',  ( 4.458734124999999437, -56.06249999863440081, -5.460374474430324690E-16 ) ) ;
#50338 = CARTESIAN_POINT ( 'NONE',  ( 5.000000000000000000, -14.29166666393548191, -2.886751345948129988 ) ) ;
#50339 = CARTESIAN_POINT ( 'NONE',  ( 2.500000000000002220, -25.54166666393547658, 4.330127018922192761 ) ) ;
#50340 = EDGE_CURVE ( 'NONE', #34622, #50557, #30151, .T. ) ;
#50341 = CARTESIAN_POINT ( 'NONE',  ( 1.975475456537005874E-15, -65.62499999726881583, 5.000000000000000000 ) ) ;
#50342 = CARTESIAN_POINT ( 'NONE',  ( 4.458734125000001214, -88.14583333196773651, 2.574251347313718519 ) ) ;
#50343 = CARTESIAN_POINT ( 'NONE',  ( 2.500000000000002220, -104.5416666639354730, 4.330127018922192761 ) ) ;
#50344 = CARTESIAN_POINT ( 'NONE',  ( 4.458734124999999437, -16.06249999863440436, -5.460374474430324690E-16 ) ) ;
#50345 = ORIENTED_EDGE ( 'NONE', *, *, #49683, .T. ) ;
#50346 = CARTESIAN_POINT ( 'NONE',  ( -3.535533905932738641, -163.5000000027312126, 3.535533905932737309 ) ) ;
#50347 = CARTESIAN_POINT ( 'NONE',  ( -2.229367062500000163, -106.4791666653010651, -3.861377020970580443 ) ) ;
#50348 = CARTESIAN_POINT ( 'NONE',  ( 3.535533905932736864, -157.2500000027312126, 3.535533905932738641 ) ) ;
#50349 = EDGE_LOOP ( 'NONE', ( #63614, #22869, #18960, #48509 ) ) ;
#50350 = CARTESIAN_POINT ( 'NONE',  ( 2.229367062499998831, -101.8958333319677365, -3.861377020970580887 ) ) ;
#50351 = CARTESIAN_POINT ( 'NONE',  ( 4.458734124999998549, -27.72916666530107221, -2.574251347313721627 ) ) ;
#50352 = CARTESIAN_POINT ( 'NONE',  ( 2.500000000000002220, -59.54166666393546592, 4.330127018922192761 ) ) ;
#50353 = CARTESIAN_POINT ( 'NONE',  ( -59.29741812935640155, -125.6250000013656205, -2.196230717870135685 ) ) ;
#50354 = CARTESIAN_POINT ( 'NONE',  ( -57.89159099828107458, -141.6875000013656063, -3.393966926194107447 ) ) ;
#50355 = CARTESIAN_POINT ( 'NONE',  ( -2.229367062499996610, -24.14583333196773651, 3.861377020970582219 ) ) ;
#50356 = CARTESIAN_POINT ( 'NONE',  ( 9.457646018065525792E-16, -65.31249999863440792, 5.148502694627439702 ) ) ;
#50357 = CARTESIAN_POINT ( 'NONE',  ( -56.66612745406272467, -153.4375000027312126, -5.149110718188517843 ) ) ;
#50358 = CARTESIAN_POINT ( 'NONE',  ( 4.458734124999999437, -20.81249999863440081, -5.460374474430324690E-16 ) ) ;
#50359 = DIRECTION ( 'NONE',  ( -0.000000000000000000, 1.000000000000000000, -0.000000000000000000 ) ) ;
#50360 = CARTESIAN_POINT ( 'NONE',  ( -3.535533905932737309, -152.6250000000000000, -3.535533905932738197 ) ) ;
#50361 = CARTESIAN_POINT ( 'NONE',  ( -5.000000000000000000, -10.00000000000000178, 0.000000000000000000 ) ) ;
#50362 = CARTESIAN_POINT ( 'NONE',  ( -1.846868145590734756, -150.1250000013655779, -4.458734125000000326 ) ) ;
#50363 = ORIENTED_EDGE ( 'NONE', *, *, #548, .F. ) ;
#50364 = VECTOR ( 'NONE', #26617, 1000.000000000000000 ) ;
#50365 = CARTESIAN_POINT ( 'NONE',  ( -2.229367062499996610, -48.39583333196772941, 3.861377020970582219 ) ) ;
#50366 = LINE ( 'NONE', #19812, #22277 ) ;
#50367 = CARTESIAN_POINT ( 'NONE',  ( 2.493747252781420335E-13, -90.25000000000000000, -5.000000000000000000 ) ) ;
#50368 = CARTESIAN_POINT ( 'NONE',  ( 4.458734125000001214, -89.89583333196775072, 2.574251347313718519 ) ) ;
#50369 = CARTESIAN_POINT ( 'NONE',  ( -4.458734124999999437, 2.687500001365593860, 0.000000000000000000 ) ) ;
#50370 = CARTESIAN_POINT ( 'NONE',  ( -5.000000000000000888, -160.5625000027312126, 2.071067811865474617 ) ) ;
#50371 = CARTESIAN_POINT ( 'NONE',  ( 1.339745962155661996, -11.16965819600733667, -4.999999999999970690 ) ) ;
#50372 = CARTESIAN_POINT ( 'NONE',  ( 6.123233995736766282E-16, -120.0000000000000000, -5.000000000000000000 ) ) ;
#50373 = CARTESIAN_POINT ( 'NONE',  ( -4.458734124999999437, 16.43750000136559564, 0.000000000000000000 ) ) ;
#50374 = CARTESIAN_POINT ( 'NONE',  ( 1.060575238724906964E-15, -78.75000000000001421, 5.773502691896257311 ) ) ;
#50375 = CARTESIAN_POINT ( 'NONE',  ( 5.000000000000000000, 8.625000002731184168, -6.123233995736766282E-16 ) ) ;
#50376 = ORIENTED_EDGE ( 'NONE', *, *, #11766, .T. ) ;
#50377 = CARTESIAN_POINT ( 'NONE',  ( -6.972266317189433020E-16, -70.25000000000000000, -5.000000000000000000 ) ) ;
#50378 = VERTEX_POINT ( 'NONE', #10860 ) ;
#50379 =( BOUNDED_CURVE ( )  B_SPLINE_CURVE ( 2, ( #16804, #6526, #35796, #55419, #16489, #11337, #36424, #30640, #50585 ),
 .UNSPECIFIED., .F., .F. ) 
 B_SPLINE_CURVE_WITH_KNOTS ( ( 3, 2, 2, 2, 3 ),
 ( 0.9589285714285714635, 0.9595238095238095566, 0.9607142857142857428, 0.9619047619047619291, 0.9625000000000000222 ),
 .UNSPECIFIED. ) 
 CURVE ( )  GEOMETRIC_REPRESENTATION_ITEM ( )  RATIONAL_B_SPLINE_CURVE ( ( 0.9330127018922194093, 0.9330127018922194093, 1.000000000000000000, 0.8660254037844387076, 1.000000000000000000, 0.8660254037844387076, 1.000000000000000000, 0.9330127018922194093, 0.9330127018922194093 ) ) 
 REPRESENTATION_ITEM ( '' )  );
#50380 = CARTESIAN_POINT ( 'NONE',  ( 6.123233995736766282E-16, -120.0000000000000000, -5.000000000000000000 ) ) ;
#50381 = CARTESIAN_POINT ( 'NONE',  ( -4.458734124999998549, -43.22916666530105800, 2.574251347313722516 ) ) ;
#50382 = CARTESIAN_POINT ( 'NONE',  ( -4.458734124999999437, -168.1875000013655779, -5.460374474430324690E-16 ) ) ;
#50383 = CARTESIAN_POINT ( 'NONE',  ( 2.499999999999998668, -38.20833333060213732, -4.330127018922193649 ) ) ;
#50384 = ORIENTED_EDGE ( 'NONE', *, *, #1467, .F. ) ;
#50385 = CARTESIAN_POINT ( 'NONE',  ( 2.229367062500001939, -15.97916666530107399, 3.861377020970579999 ) ) ;
#50386 = ORIENTED_EDGE ( 'NONE', *, *, #3971, .T. ) ;
#50387 = CARTESIAN_POINT ( 'NONE',  ( 1.060575238724906964E-15, -88.74999999999998579, 5.773502691896257311 ) ) ;
#50388 = CARTESIAN_POINT ( 'NONE',  ( -4.458734125000001214, -168.8750000013655779, 1.846868145590734089 ) ) ;
#50389 = CARTESIAN_POINT ( 'NONE',  ( -4.999999999999999112, -86.79166666393548724, 2.886751345948131764 ) ) ;
#50391 = ORIENTED_EDGE ( 'NONE', *, *, #63066, .F. ) ;
#50390 = CARTESIAN_POINT ( 'NONE',  ( 1.339745962155612702, -20.16965819600733312, -5.000000000000000000 ) ) ;
#50392 = CARTESIAN_POINT ( 'NONE',  ( -58.24261429053147765, -143.2500000000000284, -3.805975901505573855 ) ) ;
#50393 = CARTESIAN_POINT ( 'NONE',  ( 9.457646018065525792E-16, -34.31249999863440792, 5.148502694627439702 ) ) ;
#50394 = CARTESIAN_POINT ( 'NONE',  ( -4.999999999999998224, -83.91666666666667140, 2.886751345948131764 ) ) ;
#50395 = ORIENTED_EDGE ( 'NONE', *, *, #34543, .T. ) ;
#50396 = EDGE_CURVE ( 'NONE', #29442, #27774, #48892, .T. ) ;
#50397 = EDGE_CURVE ( 'NONE', #7528, #27617, #41953, .T. ) ;
#50398 = CARTESIAN_POINT ( 'NONE',  ( -4.458734124999998549, -76.22916666530107932, 2.574251347313722516 ) ) ;
#50399 = CARTESIAN_POINT ( 'NONE',  ( 4.458734124999999437, -110.0624999986343937, -5.460374474430324690E-16 ) ) ;
#50400 = CARTESIAN_POINT ( 'NONE',  ( 1.975475456537005874E-15, -55.62499999726880873, 5.000000000000000000 ) ) ;
#50401 = ADVANCED_FACE ( 'NONE', ( #41079 ), #22985, .T. ) ;
#50402 = VERTEX_POINT ( 'NONE', #28110 ) ;
#50403 = CARTESIAN_POINT ( 'NONE',  ( -1.339745962155610925, 5.330341803992665994, 5.000000000000000000 ) ) ;
#50404 = CARTESIAN_POINT ( 'NONE',  ( -56.48576386720575471, -142.0000000013656063, -4.591703134518078322 ) ) ;
#50405 = VECTOR ( 'NONE', #4085, 1000.000000000000000 ) ;
#50406 = CARTESIAN_POINT ( 'NONE',  ( 9.457646018065525792E-16, -77.31249999863440792, 5.148502694627439702 ) ) ;
#50407 = CARTESIAN_POINT ( 'NONE',  ( -53.33387254593733928, -133.9375000027312410, 5.149110718188519620 ) ) ;
#50408 = CARTESIAN_POINT ( 'NONE',  ( -3.152548672688508926E-16, -41.56249999863440081, -5.148502694627439702 ) ) ;
#50409 = CARTESIAN_POINT ( 'NONE',  ( 1.846868145590736310, -140.8750000013656063, 4.458734124999997661 ) ) ;
#50410 =( BOUNDED_CURVE ( )  B_SPLINE_CURVE ( 2, ( #59665, #33934, #34894, #19454, #59337, #10122, #19130, #24602, #15270 ),
 .UNSPECIFIED., .F., .F. ) 
 B_SPLINE_CURVE_WITH_KNOTS ( ( 3, 2, 2, 2, 3 ),
 ( 0.9446428571428571175, 0.9452380952380952106, 0.9464285714285713969, 0.9476190476190475831, 0.9482142857142856762 ),
 .UNSPECIFIED. ) 
 CURVE ( )  GEOMETRIC_REPRESENTATION_ITEM ( )  RATIONAL_B_SPLINE_CURVE ( ( 0.9330127018922194093, 0.9330127018922194093, 1.000000000000000000, 0.8660254037844387076, 1.000000000000000000, 0.8660254037844387076, 1.000000000000000000, 0.9330127018922194093, 0.9330127018922194093 ) ) 
 REPRESENTATION_ITEM ( '' )  );
#50411 = EDGE_CURVE ( 'NONE', #17652, #63145, #62851, .T. ) ;
#50412 = CARTESIAN_POINT ( 'NONE',  ( 1.339745962155618697, 24.70534180126148627, -4.999999999999998224 ) ) ;
#50413 = CARTESIAN_POINT ( 'NONE',  ( 4.458734124999998549, -51.72916666530107221, -2.574251347313721627 ) ) ;
#50414 = CARTESIAN_POINT ( 'NONE',  ( 2.229367062499998831, -45.64583333196774362, -3.861377020970580887 ) ) ;
#50415 = VECTOR ( 'NONE', #58357, 1000.000000000000000 ) ;
#50416 = CARTESIAN_POINT ( 'NONE',  ( -4.458734124999998549, 28.77083333469892779, 2.574251347313722516 ) ) ;
#50417 = EDGE_CURVE ( 'NONE', #47264, #57839, #13637, .T. ) ;
#50418 = CARTESIAN_POINT ( 'NONE',  ( 2.229367062499998831, -18.64583333196774007, -3.861377020970580887 ) ) ;
#50419 = EDGE_CURVE ( 'NONE', #58935, #17875, #28798, .T. ) ;
#50420 = CARTESIAN_POINT ( 'NONE',  ( -5.000000000000000000, -99.00000000000000000, 0.000000000000000000 ) ) ;
#50421 = CARTESIAN_POINT ( 'NONE',  ( 1.975475456537005874E-15, -37.62499999726880873, 5.000000000000000000 ) ) ;
#50422 = CARTESIAN_POINT ( 'NONE',  ( -4.458734124999998549, -38.47916666530107221, 2.574251347313722516 ) ) ;
#50423 = CARTESIAN_POINT ( 'NONE',  ( -2.499999999999996447, 7.291666669397852019, 4.330127018922195425 ) ) ;
#50424 = FACE_OUTER_BOUND ( 'NONE', #49265, .T. ) ;
#50425 = CARTESIAN_POINT ( 'NONE',  ( -52.80376928212989185, -130.8750000013656063, -4.297418129356379346 ) ) ;
#50426 = CARTESIAN_POINT ( 'NONE',  ( -3.152548672688508926E-16, -71.81249999863439371, -5.148502694627439702 ) ) ;
#50427 = EDGE_CURVE ( 'NONE', #24352, #57225, #8951, .T. ) ;
#50428 = CARTESIAN_POINT ( 'NONE',  ( 5.000000000000000000, -71.41666666666667140, -2.886751345948130876 ) ) ;
#50429 = CYLINDRICAL_SURFACE ( 'NONE', #11015, 5.000000000000000000 ) ;
#50430 = CARTESIAN_POINT ( 'NONE',  ( -2.229367062499996610, 0.6041666680322611560, 3.861377020970582219 ) ) ;
#50431 = ORIENTED_EDGE ( 'NONE', *, *, #43261, .F. ) ;
#50432 = DIRECTION ( 'NONE',  ( -0.6485228581062915110, 0.000000000000000000, -0.7611951803011149931 ) ) ;
#50433 = EDGE_CURVE ( 'NONE', #45549, #55857, #3683, .T. ) ;
#50434 = CARTESIAN_POINT ( 'NONE',  ( 5.000000000000000000, -15.50000000000000000, -6.123233995736766282E-16 ) ) ;
#50436 = CARTESIAN_POINT ( 'NONE',  ( -4.458734124999998549, -36.22916666530106511, 2.574251347313722516 ) ) ;
#50435 = CARTESIAN_POINT ( 'NONE',  ( 2.229367062500001939, -88.97916666530106511, 3.861377020970579999 ) ) ;
#50437 = CARTESIAN_POINT ( 'NONE',  ( 2.500000000000002220, 27.33333333333333215, 4.330127018922192761 ) ) ;
#50438 = CARTESIAN_POINT ( 'NONE',  ( 2.229367062499998831, -79.89583333196773651, -3.861377020970580887 ) ) ;
#50439 = CARTESIAN_POINT ( 'NONE',  ( 9.457646018065525792E-16, 16.68750000136559564, 5.148502694627439702 ) ) ;
#50440 = CARTESIAN_POINT ( 'NONE',  ( 2.500000000000002220, -77.54166666393547303, 4.330127018922192761 ) ) ;
#50441 = CARTESIAN_POINT ( 'NONE',  ( -55.35523342533222291, -136.3125000013656063, 4.444560631937231499 ) ) ;
#50442 = ADVANCED_FACE ( 'NONE', ( #57402 ), #48356, .T. ) ;
#50443 = B_SPLINE_CURVE_WITH_KNOTS ( 'NONE', 3,
 ( #6130, #26375, #35076, #45359, #26061, #5801, #45993, #1959, #34752, #54378 ),
 .UNSPECIFIED., .F., .F.,
 ( 4, 2, 2, 2, 4 ),
 ( 0.01051144076094935251, 0.01162027323572611265, 0.01272910571050287452, 0.01383793818527963640, 0.01494677066005639827 ),
 .UNSPECIFIED. ) ;
#50444 = CARTESIAN_POINT ( 'NONE',  ( 9.457646018065525792E-16, -9.062499998634407916, 5.148502694627439702 ) ) ;
#50445 = CARTESIAN_POINT ( 'NONE',  ( 4.458734124999998549, 20.02083333469892779, -2.574251347313721627 ) ) ;
#50446 = CARTESIAN_POINT ( 'NONE',  ( -4.458734124999999437, -49.56249999863440792, 0.000000000000000000 ) ) ;
#50447 = CARTESIAN_POINT ( 'NONE',  ( -5.000000000000000000, -45.95833333060214443, -2.886751345948128211 ) ) ;
#50448 = CARTESIAN_POINT ( 'NONE',  ( -3.152548672688508926E-16, -87.56249999863440792, -5.148502694627439702 ) ) ;
#50449 = CARTESIAN_POINT ( 'NONE',  ( -2.229367062499996610, -2.145833331967737845, 3.861377020970582219 ) ) ;
#50450 = CARTESIAN_POINT ( 'NONE',  ( 5.000000000000000000, -169.1250000027312126, 0.000000000000000000 ) ) ;
#50451 = ORIENTED_EDGE ( 'NONE', *, *, #60368, .F. ) ;
#50452 = CARTESIAN_POINT ( 'NONE',  ( -4.458734124999999437, -28.64583333196774007, -2.574251347313719407 ) ) ;
#50453 = CARTESIAN_POINT ( 'NONE',  ( -59.59170313451811296, -133.7500000013656063, 1.485763867205729394 ) ) ;
#50454 = CARTESIAN_POINT ( 'NONE',  ( -4.458734124999999437, -73.31249999863439371, 0.000000000000000000 ) ) ;
#50455 = CARTESIAN_POINT ( 'NONE',  ( 2.229367062500001939, 27.77083333469892779, 3.861377020970579999 ) ) ;
#50456 = CARTESIAN_POINT ( 'NONE',  ( 9.457646018065525792E-16, 18.93750000136559208, 5.148502694627439702 ) ) ;
#50457 = CARTESIAN_POINT ( 'NONE',  ( 4.769696007084727185, -114.9999999999999858, 1.500000000000000000 ) ) ;
#50458 = DIRECTION ( 'NONE',  ( -0.000000000000000000, 1.000000000000000000, -0.000000000000000000 ) ) ;
#50459 = CARTESIAN_POINT ( 'NONE',  ( 4.458734125000000326, -78.14583333196775072, 2.574251347313718519 ) ) ;
#50460 = CARTESIAN_POINT ( 'NONE',  ( -4.999999999999999112, -61.91666666666665719, 2.886751345948131764 ) ) ;
#50461 = CARTESIAN_POINT ( 'NONE',  ( -5.000000000000000000, -75.00000000000000000, 0.000000000000000000 ) ) ;
#50462 = CARTESIAN_POINT ( 'NONE',  ( -3.535250795749689387E-16, 26.87500000273118772, -5.773502691896257311 ) ) ;
#50463 = ORIENTED_EDGE ( 'NONE', *, *, #25966, .T. ) ;
#50464 = CARTESIAN_POINT ( 'NONE',  ( 1.339745962155612702, -1.169658196007335338, -5.000000000000000000 ) ) ;
#50465 = DIRECTION ( 'NONE',  ( 0.000000000000000000, 0.000000000000000000, 1.000000000000000000 ) ) ;
#50467 = CARTESIAN_POINT ( 'NONE',  ( -2.499999999999996447, -25.83333333333333215, 4.330127018922195425 ) ) ;
#50466 = CARTESIAN_POINT ( 'NONE',  ( -58.24261429053147765, -138.3750000027312126, -3.805975901505573855 ) ) ;
#50468 = CARTESIAN_POINT ( 'NONE',  ( -4.458734124999998549, -27.22916666530107221, 2.574251347313722516 ) ) ;
#50469 = VECTOR ( 'NONE', #6490, 1000.000000000000000 ) ;
#50470 = CARTESIAN_POINT ( 'NONE',  ( -3.152548672688508926E-16, -88.56249999863439371, -5.148502694627439702 ) ) ;
#50471 = CARTESIAN_POINT ( 'NONE',  ( -2.499999999999996447, -21.70833333060214798, 4.330127018922195425 ) ) ;
#50473 = ORIENTED_EDGE ( 'NONE', *, *, #61012, .F. ) ;
#50472 = CARTESIAN_POINT ( 'NONE',  ( 2.229367062499998831, -57.64583333196773651, -3.861377020970580887 ) ) ;
#50474 = FACE_OUTER_BOUND ( 'NONE', #51904, .T. ) ;
#50475 = CARTESIAN_POINT ( 'NONE',  ( 1.162044386198238837E-16, 29.25000000000000000, 5.000000000000000000 ) ) ;
#50477 = VERTEX_POINT ( 'NONE', #31425 ) ;
#50476 = CARTESIAN_POINT ( 'NONE',  ( 2.229367062499998831, -3.895833331967739177, -3.861377020970580887 ) ) ;
#50478 = CARTESIAN_POINT ( 'NONE',  ( -2.499999999999996447, -63.83333333333332860, 4.330127018922195425 ) ) ;
#50479 = CARTESIAN_POINT ( 'NONE',  ( 3.152801135295366208, -151.8125000013655779, 3.152801135295367985 ) ) ;
#50480 = CARTESIAN_POINT ( 'NONE',  ( 4.458734124999998549, -47.97916666530107221, -2.574251347313721627 ) ) ;
#50481 = CARTESIAN_POINT ( 'NONE',  ( 0.000000000000000000, -170.0000000000000000, 5.000000000000000000 ) ) ;
#50482 = CARTESIAN_POINT ( 'NONE',  ( 3.535533905932736864, -157.1250000000000284, 3.535533905932738641 ) ) ;
#50483 = CARTESIAN_POINT ( 'NONE',  ( 5.000000000000000000, -10.37499999726881583, -6.123233995736766282E-16 ) ) ;
#50484 = CARTESIAN_POINT ( 'NONE',  ( -55.39835681537999790, -151.8750000000000284, 4.984105922594378235 ) ) ;
#50485 = CARTESIAN_POINT ( 'NONE',  ( 4.458734124999999437, -10.06249999863440614, -5.460374474430324690E-16 ) ) ;
#50486 = CARTESIAN_POINT ( 'NONE',  ( 2.229367062500001939, -53.22916666530107221, 3.861377020970579999 ) ) ;
#50487 = CARTESIAN_POINT ( 'NONE',  ( -1.339745962155610925, 1.205341801261479828, 5.000000000000000000 ) ) ;
#50488 = CARTESIAN_POINT ( 'NONE',  ( -4.458734125000000326, -143.0000000013655779, -1.846868145590735644 ) ) ;
#50489 = CARTESIAN_POINT ( 'NONE',  ( -4.458734124999998549, -95.47916666530106511, 2.574251347313722516 ) ) ;
#50490 = CARTESIAN_POINT ( 'NONE',  ( -0.5984201754795734907, -8.314755988442763979, -0.7022220667781372549 ) ) ;
#50491 = ORIENTED_EDGE ( 'NONE', *, *, #26003, .F. ) ;
#50492 = CYLINDRICAL_SURFACE ( 'NONE', #34416, 5.000000000000000000 ) ;
#50493 = CARTESIAN_POINT ( 'NONE',  ( -3.152548672688508926E-16, 25.18750000136558853, -5.148502694627439702 ) ) ;
#50494 = CARTESIAN_POINT ( 'NONE',  ( -54.60164318462004474, -146.5000000027312126, -4.984105922594373794 ) ) ;
#50495 = CARTESIAN_POINT ( 'NONE',  ( 1.339745962155615144, -60.70534180126147561, 4.999999999999999112 ) ) ;
#50496 = ORIENTED_EDGE ( 'NONE', *, *, #8730, .T. ) ;
#50497 = CARTESIAN_POINT ( 'NONE',  ( 4.458734125000001214, -3.895833331967739621, 2.574251347313718519 ) ) ;
#50498 = CARTESIAN_POINT ( 'NONE',  ( 1.339745962155615144, -50.58034179853029144, 4.999999999999999112 ) ) ;
#50499 = CARTESIAN_POINT ( 'NONE',  ( 2.229367062500001939, -17.22916666530106866, 3.861377020970579999 ) ) ;
#50500 = CARTESIAN_POINT ( 'NONE',  ( 3.061616997868383141E-16, -154.8750000027311842, -5.000000000000000000 ) ) ;
#50501 = CARTESIAN_POINT ( 'NONE',  ( -2.229367062499996610, -6.145833331967740953, 3.861377020970582219 ) ) ;
#50502 = CARTESIAN_POINT ( 'NONE',  ( 2.500000000000002220, 23.45833333606451632, 4.330127018922192761 ) ) ;
#50503 = CARTESIAN_POINT ( 'NONE',  ( -8.190561711645485556E-16, -149.6875000013656063, 4.458734124999999437 ) ) ;
#50504 = CARTESIAN_POINT ( 'NONE',  ( 4.458734124999999437, 15.93750000136559564, -5.460374474430324690E-16 ) ) ;
#50505 = VERTEX_POINT ( 'NONE', #3990 ) ;
#50506 = CARTESIAN_POINT ( 'NONE',  ( -2.499999999999996447, -62.70833333060214443, 4.330127018922195425 ) ) ;
#50507 = CARTESIAN_POINT ( 'NONE',  ( -2.352990130084580066E-16, 8.660254037844390851, -7.422398894150034288 ) ) ;
#50508 = CARTESIAN_POINT ( 'NONE',  ( 2.229367062499998831, -17.64583333196773651, -3.861377020970580887 ) ) ;
#50509 = VECTOR ( 'NONE', #23617, 1000.000000000000000 ) ;
#50510 = CARTESIAN_POINT ( 'NONE',  ( 5.000000000000000000, -25.29166666393547658, -2.886751345948130876 ) ) ;
#50511 = CARTESIAN_POINT ( 'NONE',  ( 1.339745962155615144, -3.705341801261480494, 4.999999999999999112 ) ) ;
#50512 =( BOUNDED_CURVE ( )  B_SPLINE_CURVE ( 2, ( #2511, #56861, #32401, #12467, #41409, #7970, #12779, #47202, #37864 ),
 .UNSPECIFIED., .F., .T. ) 
 B_SPLINE_CURVE_WITH_KNOTS ( ( 3, 2, 2, 2, 3 ),
 ( 0.4910714285714285476, 0.4916666666666666408, 0.4928571428571428825, 0.4940476190476190688, 0.4946428571428571619 ),
 .UNSPECIFIED. ) 
 CURVE ( )  GEOMETRIC_REPRESENTATION_ITEM ( )  RATIONAL_B_SPLINE_CURVE ( ( 0.9330127018922194093, 0.9330127018922194093, 1.000000000000000000, 0.8660254037844387076, 1.000000000000000000, 0.8660254037844387076, 1.000000000000000000, 0.9330127018922194093, 0.9330127018922194093 ) ) 
 REPRESENTATION_ITEM ( '' )  );
#50513 = CARTESIAN_POINT ( 'NONE',  ( -58.39396692619412477, -150.4375000013656063, 2.891590998281057701 ) ) ;
#50514 = ADVANCED_FACE ( 'NONE', ( #38390 ), #2196, .T. ) ;
#50515 = CARTESIAN_POINT ( 'NONE',  ( 5.000000000000000000, -46.37499999726880873, -6.123233995736766282E-16 ) ) ;
#50516 = DIRECTION ( 'NONE',  ( 0.000000000000000000, 1.000000000000000000, 0.000000000000000000 ) ) ;
#50517 = CARTESIAN_POINT ( 'NONE',  ( 2.229367062500001939, 11.02083333469892956, 3.861377020970579999 ) ) ;
#50518 = CARTESIAN_POINT ( 'NONE',  ( 6.158835246850666199E-14, 8.749999999999998224, -4.999999999999999112 ) ) ;
#50519 = CARTESIAN_POINT ( 'NONE',  ( 0.000000000000000000, -120.0000000000000000, 0.000000000000000000 ) ) ;
#50520 = CARTESIAN_POINT ( 'NONE',  ( -3.152548672688508926E-16, 13.43750000136559386, -5.148502694627439702 ) ) ;
#50521 = CARTESIAN_POINT ( 'NONE',  ( 4.458734124999998549, -68.72916666530106511, -2.574251347313721627 ) ) ;
#50522 = CARTESIAN_POINT ( 'NONE',  ( 4.458734124999999437, -14.06249999863440436, -5.460374474430324690E-16 ) ) ;
#50523 = CARTESIAN_POINT ( 'NONE',  ( -5.000000000000000000, 1.999999999999998224, 0.000000000000000000 ) ) ;
#50524 = CARTESIAN_POINT ( 'NONE',  ( -8.190561711645485556E-16, -163.6875000013655779, 4.458734124999999437 ) ) ;
#50525 = CARTESIAN_POINT ( 'NONE',  ( -2.229367062499996610, -61.14583333196774362, 3.861377020970582219 ) ) ;
#50526 = CARTESIAN_POINT ( 'NONE',  ( 5.000000000000000000, -96.37499999726881583, -6.123233995736766282E-16 ) ) ;
#50527 = CARTESIAN_POINT ( 'NONE',  ( -4.999999999999998224, -76.91666666666667140, 2.886751345948131764 ) ) ;
#50528 = CARTESIAN_POINT ( 'NONE',  ( -1.339745962155610925, -79.79465819873850307, 5.000000000000000000 ) ) ;
#50529 = CARTESIAN_POINT ( 'NONE',  ( 4.458734124999998549, -36.72916666530107221, -2.574251347313721627 ) ) ;
#50530 = CARTESIAN_POINT ( 'NONE',  ( 5.000000000000000000, -60.41666666666665719, -2.886751345948130876 ) ) ;
#50531 = CARTESIAN_POINT ( 'NONE',  ( 5.000000000000000000, -41.41666666666667140, -2.886751345948129988 ) ) ;
#50532 = LINE ( 'NONE', #5827, #40812 ) ;
#50533 = CARTESIAN_POINT ( 'NONE',  ( -6.972266317189433020E-16, -6.124999997268813168, -5.000000000000000000 ) ) ;
#50534 = VERTEX_POINT ( 'NONE', #28426 ) ;
#50535 = CARTESIAN_POINT ( 'NONE',  ( 2.229367062499998831, -107.6458333319677365, -3.861377020970580887 ) ) ;
#50536 = CARTESIAN_POINT ( 'NONE',  ( 4.458734125000001214, -2.145833331967737845, 2.574251347313718519 ) ) ;
#50537 = CARTESIAN_POINT ( 'NONE',  ( -5.000000000000000000, -96.95833333060213022, -2.886751345948128211 ) ) ;
#50538 = CARTESIAN_POINT ( 'NONE',  ( -2.500000000000000444, -7.166666666666668739, -4.330127018922193649 ) ) ;
#50539 = CARTESIAN_POINT ( 'NONE',  ( 4.458734125000000326, -70.89583333196773651, 2.574251347313718519 ) ) ;
#50540 = CARTESIAN_POINT ( 'NONE',  ( -2.500000000000000444, -9.041666663935483683, -4.330127018922193649 ) ) ;
#50542 = ORIENTED_EDGE ( 'NONE', *, *, #50769, .T. ) ;
#50541 = CARTESIAN_POINT ( 'NONE',  ( -2.229367062499996610, -38.14583333196773651, 3.861377020970582219 ) ) ;
#50543 = CARTESIAN_POINT ( 'NONE',  ( 5.000000000000000000, -6.499999999999999112, -6.123233995736766282E-16 ) ) ;
#50545 = ORIENTED_EDGE ( 'NONE', *, *, #39344, .F. ) ;
#50544 = CARTESIAN_POINT ( 'NONE',  ( -4.458734124999999437, 12.35416666803225993, -2.574251347313719407 ) ) ;
#50546 = CARTESIAN_POINT ( 'NONE',  ( 2.500000000000002220, -101.6666666666666572, 4.330127018922192761 ) ) ;
#50547 = CARTESIAN_POINT ( 'NONE',  ( -5.000000000000000000, -51.08333333333332860, -2.886751345948128211 ) ) ;
#50548 = CARTESIAN_POINT ( 'NONE',  ( 4.458734125000001214, -28.14583333196774007, 2.574251347313718519 ) ) ;
#50549 = CARTESIAN_POINT ( 'NONE',  ( -2.499999999999996447, -34.83333333333332860, 4.330127018922195425 ) ) ;
#50550 = CARTESIAN_POINT ( 'NONE',  ( 4.458734124999998549, -77.72916666530106511, -2.574251347313721627 ) ) ;
#50551 = CARTESIAN_POINT ( 'NONE',  ( -8.190561711645485556E-16, -140.9375000013656063, 4.458734124999999437 ) ) ;
#50552 = CARTESIAN_POINT ( 'NONE',  ( -2.229367062499996610, -85.14583333196773651, 3.861377020970582219 ) ) ;
#50553 = CARTESIAN_POINT ( 'NONE',  ( -57.89159099828107458, -135.9375000013656063, -3.393966926194107447 ) ) ;
#50554 = CARTESIAN_POINT ( 'NONE',  ( -3.152548672688508926E-16, -35.81249999863440792, -5.148502694627439702 ) ) ;
#50555 = EDGE_LOOP ( 'NONE', ( #48097, #1689, #20594, #3257 ) ) ;
#50556 = CARTESIAN_POINT ( 'NONE',  ( -6.972266317189433020E-16, -38.12499999726880873, -5.000000000000000000 ) ) ;
#50557 = VERTEX_POINT ( 'NONE', #56210 ) ;
#50558 = CARTESIAN_POINT ( 'NONE',  ( -3.152548672688508926E-16, -77.81249999863440792, -5.148502694627439702 ) ) ;
#50559 = CARTESIAN_POINT ( 'NONE',  ( -55.80335512604638382, -135.0000000000000284, -4.395415492492952048 ) ) ;
#50560 = ORIENTED_EDGE ( 'NONE', *, *, #10335, .F. ) ;
#50561 = CARTESIAN_POINT ( 'NONE',  ( -4.999999999999998224, -14.79166666393548546, 2.886751345948131764 ) ) ;
#50562 =( BOUNDED_SURFACE ( )  B_SPLINE_SURFACE ( 1, 2, ( 
 ( #53046, #52434, #8367, #8984, #23150, #42759, #37947, #57580, #33428, #33122, #38261, #52739, #28282, #57882, #28596, #43386, #44982, #49801, #9918, #53675, #29528, #59466, #5424, #25041, #9607, #44010, #44329, #14430, #24725, #24097, #38871, #29215, #15397, #63340, #25363, #34688, #24408, #39506, #4780, #40148, #63657, #10559, #10251, #34053, #19255, #58506, #19575, #949, #48841, #59142, #39823, #34360, #39189, #19891, #58814, #294, #35023, #15075, #14744, #15715, #53991, #54953, #10883, #35333, #4471, #54311, #20222, #49166, #5107, #29853, #49486, #44652, #613, #54636, #30170, #5745, #20550, #43692, #59793, #48530, #46579, #36292, #26960, #2520, #55284, #45621, #41101, #31448, #12157, #40469, #35977, #1577, #22136, #51090, #17300, #30499, #11827, #31138, #56235, #21178, #40784, #26002, #41731, #21505, #36928, #60431, #25689, #16357, #61379, #56555, #36603, #16031, #50121, #55605, #46257, #11522, #60109, #60746, #26315, #50762, #31776, #51407, #6706, #45298, #61067, #6077, #1263, #20866, #30826, #50456, #16670, #35659, #16988, #45934, #1897, #55915, #11204, #6396, #7027, #26638, #2216, #41417, #21819, #7350, #13423, #8290, #2838, #56870, #12787, #22456, #18248, #42369, #47821, #33047, #42683, #18567, #61697, #43314, #62949, #52662, #8597, #62326, #23402, #27894, #13734, #28207, #47516, #42054, #32409, #52039, #17627, #37874, #62009, #3780, #43002, #57507, #38189, #37244, #18865, #38483, #7979, #62647, #27270, #52971, #57811, #27577, #3467, #47210, #4095, #3154, #33356, #8911, #22774, #46897, #17927, #37549, #28525, #57190, #23080, #48142, #13110, #32727, #23717, #52354, #12476, #32088, #51724, #7664, #25283, #9222, #864, #20467, #44908, #14042, #219, #29776, #43619, #4705, #39114, #63261, #58742, #19180, #38793, #19817, #10171, #49409, #33667, #5030, #48458, #10484, #39426, #54561, #30096, #58431, #9535, #24649, #59067, #39743, #4396, #63580, #29140, #49727, #14992, #58111, #53286, #34604, #14669, #20147, #48762, #24330, #53602, #5672, #49082, #28835, #43933, #24016, #19500, #14360, #33981, #535, #34290, #53912, #9838, #5353, #29450, #44255, #54233, #24971, #44578, #59385, #15319, #34940, #54878, #6954, #46504, #7276, #36526, #40390, #60032, #26238, #26887, #26564, #11122, #35897, #1500, #31703, #50047, #12080, #35578, #50685, #41027, #51011, #6004, #21101, #55838, #20786, #16909, #40069, #2450, #36214, #1188, #11754, #59710, #6626, #15641, #15956, #51337, #31370, #55205, #46183, #30749, #40706, #45857, #35257, #2143, #60354, #16279, #11442, #21748, #25607, #41343, #55532, #10808, #30420, #50369, #1822, #60989, #31061, #6316, #56155, #45222, #25921, #21425, #45538, #60673, #16596, #32974, #51652, #23015, #41652, #8528, #7590, #28453, #28138, #13665, #56482, #32337, #48068, #52594, #27198, #18175, #46816, #61303, #57431, #3398, #62254, #18495, #23326, #47137, #2760, #3083, #47756, #42616, #37803, #22382, #17557, #17859, #41981, #61940, #17226, #12405, #8219, #13351, #61622, #3711, #37176, #56799, #36853, #33285, #12717, #57740, #52904, #38116, #32018, #42931, #62575, #51963, #8840, #27822, #57118, #7902, #22703, #37481, #13034, #27507, #22061, #42300, #32653, #52281, #47446, #4956, #58987, #34213, #23946, #34868, #14287, #58670, #43236, #20066, #19103, #4632, #62878, #14915, #54488, #38416, #48385, #34523, #28762, #29066, #14596, #39670, #29704, #48691, #24256, #39042, #49335, #53218, #54155, #63506, #59307, #18790, #38720, #53838, #10096, #43859, #4326, #19744, #39357, #9150, #19430, #464, #29375, #5279, #24899, #33597, #24577, #23642, #44500, #43548, #10416, #15242, #30027, #58041, #33906, #4023, #13971, #63193, #149, #58361, #53530, #9458, #49007, #44183, #9767, #50934, #11049, #54808, #30674, #60599, #6552, #26167, #10737, #45147, #45466, #15571, #25850, #25211, #39993, #35827, #45787, #30344, #1746, #49969, #5922, #44823, #41262, #25530, #21672, #60910, #2063, #20393, #11679, #55762, #1112, #21347, #55448, #21030, #20719, #50292, #1431, #40639, #59638, #36452, #40949, #40324, #5594, #59962, #50613, #16518, #16197, #15885, #16832, #35505, #60279, #785, #56954, #55124, #6240, #35190, #36140, #12875, #11363, #49656, #30987, #31297, #6874, #26489, #46105, #57592, #48223, #13194, #9304, #32493, #38883, #28607, #57276, #4180, #19266, #62726, #52123, #32817, #4481, #23795, #13520, #18012, #33137, #37636, #52445, #38272, #43397, #63042, #8066, #43087, #22862, #48542, #57896, #28919, #24109, #8380, #47601, #18650, #33439, #14126, #42453, #37958, #3554, #43705, #53057, #58517, #27668, #13820, #52751, #58197, #23162, #42771, #27981, #63352, #23484, #47296, #62415, #3248, #18335, #62095, #8681, #38568, #28295, #47907, #3863, #18950, #8995, #33752, #53370, #10263, #24737, #15727, #35346, #44340, #29226, #44995, #20878, #45310, #10895, #14755, #34372, #624, #1278, #961, #49178, #29865, #39516, #6088, #24420, #15412, #35035, #20234, #25374, #49497, #54965, #54647, #5435, #4794, #58825, #54001, #44021, #39835, #304, #49811, #10572, #44663, #20562, #63669, #40480, #14441, #9930, #40164, #48853, #30510, #59477, #29544, #25053, #5118, #25700, #19902, #59806, #30181, #19587, #39199, #59154, #15087, #50133, #34701, #5756, #34064, #54326, #53686, #9619, #26017, #55927, #46590, #11842, #1590, #27283, #11215, #2850, #22471, #46909, #16042, #2228, #31788, #45634, #6718, #12487, #30839, #22148, #2534, #11534, #51419, #21833, #31461, #35988, #21516, #51101, #7040, #50468, #60121, #7362, #55618, #35671, #31149, #61079, #26971, #26650, #16368, #55297, #26328, #46270, #6407, #32100, #50777, #60759, #21189, #41743, #40796, #60444, #51737, #45946, #41430, #17000, #61392, #1910, #41112, #12170, #16683, #36940, #36304, #36615, #56249, #17317, #56566, #7676, #8608, #42068, #22786, #14055, #57824, #42381, #8922, #3167, #3478, #52675, #33679, #4107, #23091, #42695, #13434, #23729, #27589, #33367, #37886, #53299, #17637, #13122, #28218, #48156, #62338, #62020, #13746, #52982, #47224, #18259, #38496, #3793, #43324, #28536, #7990, #43016, #61708, #62963, #17938, #48471, #18880, #9235, #12802, #52366, #4407, #58123, #37562, #38199, #57203, #37253, #28848, #23414, #18578, #56882, #32421, #57517, #32739, #33060, #52052, #62658, #8305, #27906, #47527, #47832, #53615, #231, #63273, #14370, #10185, #20157, #48774, #44589, #29153, #24344, #19192, #15651, #43945, #59723, #35268, #38805, #34953, #54890, #58444, #10819, #19512, #34618, #24982, #54572, #33994, #49096, #39753, #4719, #875, #24029, #30431, #59397, #63592, #15330, #50059, #54244, #43633, #39127, #9548, #10494, #58753, #30108, #14682, #5043, #29787, #34302, #49738, #24661, #44267, #59079, #5683, #53925, #25295, #19829, #9850, #29464, #39440, #49420, #44920, #15005, #5363, #20479, #40080, #547, #31072, #2459, #31383, #51347, #16919, #35590, #6965, #25620, #56168, #55216, #12414, #12091, #61314, #40402, #16290, #32026, #36536, #11134, #2153, #30760, #45232, #41354, #51021, #46193, #22070, #7286, #50696, #50381, #6639, #31713, #26575, #21759, #6327, #1510, #1833, #25932, #45869, #1199, #60042, #55848, #60997, #45551, #26897, #21113, #40718, #20799, #17239, #60366, #41662, #36863, #56493, #15966, #46515, #6016, #35910, #55542, #11764, #41038, #11453, #26247, #21434, #60684, #16606, #36224, #23336, #27516, #7601, #3094, #52602, #42938, #18184, #7911, #18798, #61949, #42625, #27208, #4030, #22711, #52290, #37184, #8227, #56809, #32348, #57439, #3718, #62581, #46826, #62264, #41993, #23649, #13359, #48076, #43245, #12726, #42309, #37811, #8536, #33291, #61633, #57128, #17868, #62885, #28146, #38422, #51662, #32982, #27832, #13672, #37489, #13044, #47146, #58048, #47763, #13978, #32662, #2771, #47454, #22392, #17566, #57748, #51972, #3406, #23022, #18503, #38124, #52910, #8847, #28461, #43866, #34877, #54498, #63514, #48391, #472, #40001, #795, #30036, #33914, #53539, #19753, #20402, #20074, #4639, #29382, #58679, #25221, #43554, #34530, #54163, #39364, #44510, #49016, #10423, #10104, #4964, #23950, #14295, #9465, #63200, #58995, #19438, #5289, #29712, #157, #39680, #19110, #59648, #33606, #29074, #59316, #4333, #49665, #14924, #48699, #24586, #24262, #44832, #39050, #15251, #49343, #38729, #58367, #14606, #34221, #5605, #53847, #44192, #24907, #9776, #53226, #9157, #28770, #11376, #2078, #30997, #20726, #46438, #30355, #21994, #41587, #2384, #35200, #21359, #50945, #1122, #25860, #60288, #35513, #15581, #45476, #6563, #54815, #31638, #30685, #16212, #10746, #26500, #49979, #5931, #51274, #11061, #26178, #16528, #46115, #25539, #40649, #31309, #59972, #56090, #45156, #40330, #11690, #15893, #6886, #55134, #45797, #50302, #6250, #7207, #21684, #1440, #41273, #21042, #35838, #1757, #26818, #60923, #55460, #50624, #40963, #16842, #60611, #36463, #36152, #55773, #12010, #32266, #47384, #3643, #42234, #61557, #13283, #32909, #2693, #22635, #57677, #22951, #42862, #8466, #27132, #62186, #17161, #47691, #46748, #3956, #23254, #52840, #31952, #7836, #23577, #28074, #22313, #57362, #41914, #36785, #52532, #42547, #37729, #13603, #62507, #61877, #17491, #17793, #18424, #18106, #38045, #37112, #56731, #57051, #12651, #37417, #56418, #51584, #3335, #33221, #51895, #8774, #27437, #47071, #12341, #28384, #3020, #48003, #61239, #7522, #12962, #32587, #52210, #8157, #27756, #48941, #14530, #19041, #4566, #58610, #38973, #33535, #29960, #14846, #38658, #62813, #58297, #44114, #34458, #9704, #57982, #13907, #14216, #59242, #9085, #53772, #54089, #29002, #33843, #34150, #28695, #29309, #29640, #4889, #48314, #10351, #53150, #49585, #5527, #43173, #18731, #24512, #10028, #4264, #53462, #24190, #23882, #43797, #43485, #63130, #77, #58917, #49274, #38356, #19678, #9391, #15174, #39290, #39606, #34799, #48627, #63444, #5210, #24829, #44435, #19361, #396, #19998, #54422, #45725, #11932, #25142, #6494, #25791, #50868, #40259, #35433, #20655, #16770, #16136, #31563, #59899, #20324, #15819, #36388, #60844, #31237, #10663, #56019, #55059, #40886, #10983, #54742, #35758, #20970, #30603, #26420, #46037, #50225, #39926, #55703, #51196, #44753, #21605, #25461, #45083, #11298, #714, #11617, #6174, #40571, #45402, #59573, #35127, #26105, #1677, #30923, #36074, #60212, #2001, #21279, #55382, #15506, #5853, #1049, #30279, #50550, #1368, #60531, #16455, #6811, #41199, #49899, #32831, #52459, #12265, #8081, #2313, #62109, #22560, #7449, #27363, #51512, #13209, #27057, #3263, #42160, #17090, #17416, #27683, #17722, #56970, #56344, #46675, #51818, #36711, #32187, #46360, #41514, #2945, #12888, #31878, #37337, #2620, #22238, #21917, #8395, #41838, #57293, #27996, #37650, #61167, #22875, #47310, #61483, #32507, #61796, #7760, #37031, #56657, #46997, #52139, #12574, #7128, #42468, #18028, #26744, #16022, #1889, #55908, #31130, #20859, #31767, #11194, #55595, #40140, #16979, #35649, #1568, #59784, #11819, #51399, #35326, #36590, #60101, #11514, #21493, #31438, #10874, #25993, #16659, #45291, #41407, #940, #7340, #60738, #25682, #36285, #26952, #50753, #20543, #1256, #56226, #51081, #40462, #7019, #55275, #45612, #6698, #12147, #26627, #21168, #40777, #35969, #46247, #50113, #2208, #60422, #15709, #54947, #30816, #26304, #21812, #16347, #50448, #61059, #30491, #6068, #45927, #6388, #41091, #26237, #45856, #59708, #30419, #34937, #50044, #54558, #30094, #55201, #1498, #21100, #5350, #60031, #39740, #1819, #11120, #21423, #41026, #10481, #863, #15954, #50368, #31060, #59381, #6003, #20785, #50682 ),
 ( #15315, #54876, #20466, #60670, #6315, #36212, #49406, #30748, #25606, #11441, #40066, #15640, #44905, #16594, #40389, #55836, #35256, #44574, #10807, #11750, #24968, #55530, #49724, #531, #45220, #40705, #1186, #5670, #35577, #25919, #45537, #6624, #20144, #60352, #25282, #16278, #35896, #62252, #27819, #31700, #51335, #17555, #18171, #61938, #2448, #27196, #56480, #23013, #41341, #32332, #51961, #37174, #42298, #46813, #32649, #7899, #2758, #21745, #12076, #7273, #60986, #56797, #61300, #3081, #27504, #61620, #37478, #16906, #37800, #57428, #26885, #17857, #46180, #8216, #12715, #46500, #22379, #22057, #42614, #41649, #57114, #47133, #36523, #2140, #56153, #17223, #36850, #12402, #22700, #51009, #13032, #32016, #31368, #52279, #6950, #51650, #7585, #26561, #47445, #41978, #3396, #42926, #52592, #48688, #58358, #53527, #9764, #14591, #38414, #18492, #58038, #24254, #33904, #9456, #38114, #8838, #9148, #62572, #53215, #8526, #3709, #63190, #29064, #57737, #4628, #13663, #33283, #28135, #4953, #52902, #49005, #24575, #29372, #47753, #39040, #19428, #28451, #43857, #19100, #48382, #48066, #13969, #28759, #4324, #23324, #147, #63504, #4020, #32970, #23640, #14285, #58668, #43545, #43234, #44180, #62876, #23944, #18787, #19742, #33595, #38718, #34211, #53836, #39354, #13349, #30985, #54486, #5920, #59960, #6238, #5276, #20390, #11046, #39668, #35823, #58985, #1744, #55122, #20063, #30671, #45784, #25527, #14912, #59305, #50610, #50290, #15238, #25847, #34865, #39990, #45145, #6550, #21028, #59636, #15568, #30341, #40636, #44498, #45464, #54806, #26165, #34521, #30025, #1108, #1429, #35188, #10413, #60276, #16195, #461, #10735, #15883, #49966, #20717, #49654, #5590, #49333, #40322, #25207, #55446, #35503, #11361, #21345, #44821, #54152, #10092, #783, #29702, #24897, #17781, #27120, #16830, #31941, #60908, #32574, #36449, #3006, #2679, #6872, #55759, #11676, #56078, #57035, #26487, #51569, #32252, #26802, #11998, #12330, #46102, #36774, #27425, #56405, #2061, #8141, #31295, #47372, #3321, #27743, #56717, #60596, #37400, #12949, #51261, #21981, #21669, #41575, #41260, #31625, #46733, #12635, #51882, #16516, #7508, #50931, #52195, #22299, #40946, #36138, #7195, #46423, #41899, #61545, #22623, #2372, #61226, #17150, #17477, #37099, #7822, #47056, #42219, #61865, #48614, #38033, #33209, #18413, #14515, #13895, #9690, #57665, #18091, #13591, #34136, #58596, #28990, #8455, #53756, #52827, #38643, #8762, #52520, #33521, #18719, #28368, #24177, #22940, #58284, #38344, #13269, #29298, #14203, #62494, #42534, #47989, #23868, #33829, #53138, #42851, #48927, #3943, #9071, #62170, #38959, #23564, #43160, #37714, #53447, #57352, #32892, #28061, #9379, #57971, #47678, #3630, #62800, #28681, #4553, #48301, #23237, #43783, #63430, #4253, #43471, #63117, #19029, #19346, #54075, #34445, #5834, #24497, #55041, #10014, #11285, #10967, #60200, #39275, #15161, #30911, #15804, #29625, #1035, #49258, #44101, #40245, #49884, #45068, #1353, #6160, #29946, #5197, #49571, #35421, #25448, #20639, #24815, #379, #699, #44418, #44738, #65, #58902, #54728, #59884, #19983, #30588, #39592, #59228, #19662, #16117, #34783, #40557, #35744, #20956, #14831, #50210, #25777, #54406, #45387, #10648, #30262, #55370, #4876, #10336, #20311, #5511, #25125, #39911, #59557, #15491, #35112, #51496, #41822, #17075, #6797, #17709, #60831, #41500, #26089, #2930, #1986, #51182, #45711, #61468, #37323, #21265, #22544, #46024, #61153, #7433, #17401, #60514, #11918, #2605, #31223, #27349, #50538, #56953, #46660, #11603, #22224, #12874, #36694, #6481, #50854, #42144, #37016, #26405, #56644, #21588, #31544, #56328, #61781, #12558, #7113, #26728, #21903, #32171, #36061, #46344, #41186, #51804, #1664, #40870, #46983, #16757, #36373, #12250, #16441, #7746, #56004, #2301, #31863, #55690, #27043, #33438, #53056, #18649, #43396, #28294, #33751, #8994, #47906, #22861, #13193, #32816, #42452, #38271, #62414, #4179, #28606, #62725, #38567, #18011, #63351, #19265, #52444, #63041, #47295, #9303, #57895, #8379, #23483, #27980, #24108, #47600, #58196, #13819, #62094, #3247, #37635, #3553, #48541, #57275, #43086, #23794, #18334, #23161, #3862, #42770, #48222, #18949, #14125, #37957, #38882, #57591, #58516, #32492, #52122, #53369, #8065, #28918, #4480, #13519, #33136, #52750, #8680, #43704, #27667, #20233, #30180, #49810, #34063, #25052, #4793, #30509, #39834, #10894, #50132, #39198, #29543, #44662, #15411, #59805, #24419, #19901, #49177, #6087, #35034, #1277, #14440, #59476, #15086, #40163, #5117, #24736, #9929, #25699, #5434, #20877, #44339, #9618, #303, #45309, #40479, #20561, #63668, #53685, #39515, #5755, #59153, #44020, #623, #10262, #34700, #15726, #29225, #34371, #48852, #54325, #54646, #19586, #58824, #29864, #49496, #14754, #25373, #54000, #10571, #44994, #960, #35345, #54964, #7361, #6406, #21515, #12169, #40795, #36939, #60120, #2849, #56248, #21188, #31787, #46908, #26649, #16041, #60443, #32099, #51418, #16367, #26970, #35987, #41111, #7039, #51736, #22147, #60758, #16682, #31460, #41742, #45633, #46589, #55926, #7675, #35670, #31148, #46269, #2533, #36303, #55617, #61391, #17316, #1589, #11841, #16999, #51100, #2227, #11533, #26016, #61078, #55296, #56565, #50776, #22470, #12486, #27282, #30838, #6717, #11214, #50467, #26327, #45945, #1909, #21832, #41429, #36614, #18577, #38495, #43323, #3477, #47223, #23090, #52981, #62657, #38198, #3166, #37561, #37885, #7989, #18258, #17636, #32420, #28217, #57823, #22785, #13745, #42380, #62019, #37252, #33678, #17937, #14054, #53298, #58122, #12801, #4106, #48155, #57202, #33366, #47831, #3792, #9234, #42067, #8921, #57516, #52051, #28847, #28535, #13121, #61707, #32738, #43015, #23728, #8607, #52365, #62962, #48470, #4406, #56881, #8304, #27905, #23413, #27588, #18879, #47526, #13433, #42694, #62337, #33059, #52674, #45471, #10184, #35833, #19828, #26172, #25855, #39439, #14369, #4718, #24343, #33993, #30679, #53924, #60283, #1436, #54243, #30993, #9547, #55768, #11685, #43944, #55454, #38804, #1752, #50298, #63591, #15004, #19511, #16524, #39126, #50619, #6245, #53614, #58443, #29152, #58752, #40958, #48773, #34617, #16205, #9849, #14681, #59078, #34301, #21037, #11370, #40644, #29463, #31303, #49095, #50939, #24028, #43632, #6558, #63272, #21353, #60606, #5042, #24660, #44266, #230, #45792, #36147, #19191, #22630, #42229, #26494, #17486, #60918, #22947, #12646, #3330, #42542, #31633, #21989, #37107, #7831, #52204, #16838, #12337, #41582, #62181, #27432, #57357, #6881, #51890, #7517, #32582, #61234, #17157, #2379, #18101, #61553, #13278, #36780, #2072, #56413, #37724, #32903, #12957, #56085, #46110, #31948, #61873, #51579, #36458, #56726, #2688, #27127, #8151, #21678, #46743, #7202, #32261, #41268, #37411, #22308, #41907, #47065, #12005, #51269, #3015, #17788, #57046, #27751, #47379, #26812, #46432, #48310, #42857, #33218, #52836, #62502, #58292, #18727, #24186, #9388, #19037, #58607, #38041, #19674, #39286, #8770, #19356, #3637, #29307, #38654, #28379, #43481, #48000, #44110, #3952, #14526, #14211, #18420, #23249, #57673, #23574, #4885, #13599, #63126, #43793, #38352, #43169, #23877, #62808, #4260, #38969, #33839, #57978, #58913, #13903, #14841, #52527, #8461, #4562, #28069, #48937, #24507, #33531, #53146, #9081, #28690, #53457, #28998, #48623, #63440, #34146, #47686, #53767, #9700, #73, #40255, #30920, #6491, #59238, #49581, #45078, #35431, #16133, #44431, #39921, #5523, #26101, #55056, #21276, #34454, #15816, #35123, #60209, #25138, #44749, #29956, #45722, #25458, #40883, #710, #29636, #20320, #1674, #60527, #40568, #19994, #54086, #59569, #50221, #15501, #392, #1045, #30275, #54738, #35755, #50547, #10659, #54417, #1365, #10024, #49270, #5206, #34795, #10980, #49895, #24825, #15171, #10346, #39602, #59896, #5848, #6171, #30600, #20651, #55379, #25788, #45399, #20968, #11295, #46993, #31234, #56966, #2616, #56015, #7445, #36384, #8077, #11927, #42156, #41834, #46034, #50864, #6808, #31559, #32503, #1997, #27053, #7756, #2310, #51192, #51508, #21602, #12260, #2941, #31874, #41196, #47305, #26417, #22871, #42464, #3259, #32183, #36071, #12885, #52135, #26740, #61163, #60841, #17086, #16767, #7124, #22234, #51814, #27359, #55700, #46671, #46356, #27678, #61478, #16452, #11614, #21913, #41510, #17412, #37027, #61792, #36706, #56340, #56653, #12570, #22554, #17719, #37333, #43407, #62738, #24119, #13529, #8692, #57602, #53698, #53067, #48863, #33148, #57289, #52763, #9630, #34075, #4491, #47611, #29238, #28304, #14136, #47918, #27992, #9007, #57907, #3876, #43718, #14453, #43097, #18346, #28929, #4807, #24431, #58529, #62428, #37969, #48234, #62105, #48552, #23495, #13831, #18660, #18024, #8390, #63052, #18962, #4192, #9315, #33450, #63364, #37646, #13205, #19279, #3565, #32827, #38282, #33763, #28619, #23172, #23805, #38578, #58209, #38894, #52456, #53382, #42783, #10905, #50478, #11224, #40491, #44352, #315, #30193, #30847, #30520, #15097, #39846, #5446, #35681, #54012, #45005, #971, #49822, #54976, #59489, #45323, #20573, #15424, #34384, #24747, #19913, #9942, #5766, #10273, #15738, #40179, #10581, #50143, #29557, #6418, #44033, #39527, #6098, #58837, #20888, #25384, #59165, #35046, #34714, #55309, #54340, #25711, #59816, #49191, #14766, #5129, #29877, #60132, #49507, #54658, #35355, #25064, #44674, #1290, #634, #16053, #10226, #19600, #20244, #39212, #40805, #32431, #52060, #12810, #41752, #45643, #2859, #22481, #36313, #7048, #11543, #26661, #31160, #6728, #31796, #61402, #17326, #1601, #36625, #16378, #42076, #51428, #61717, #17646, #50789, #41121, #56257, #26979, #7686, #35997, #31470, #60769, #37262, #46598, #26027, #21199, #7371, #46279, #51744, #16694, #55937, #21525, #56890, #17009, #60453, #11852, #55628, #51111, #2238, #26338, #21842, #45955, #1920, #2542, #36948, #56574, #41438, #12182, #61087, #22158, #12496, #32108, #27292, #46917, #23100, #18585, #8930, #53308, #17946, #13445, #42703, #43642, #28543, #58455, #7998, #52989, #8618, #33687, #62347, #18268, #3486, #63283, #62665, #14378, #37895, #3176, #57524, #19200, #38813, #14062, #57211, #34002, #33070, #23736, #52683, #37571, #38209, #3801, #28226, #9242, #24040, #47842, #27914, #38503, #27601, #47234, #4415, #8314, #47536, #57834, #22796, #58131, #23422, #43025, #13753, #42389, #13130, #48163, #4116, #33375, #18889, #43331, #28856, #62973, #48478, #62029, #52377, #32749, #43953, #59407, #19837, #25305, #10500, #20165, #59730, #39135, #20805, #40408, #34310, #20489, #4728, #30438, #39761, #29473, #44596, #9863, #45240, #49105, #15656, #15339, #19521, #24353, #63601, #5051, #6021, #58762, #556, #44926, #39451, #24669, #24989, #14692, #49427, #40087, #5371, #53933, #60047, #44277, #15971, #53625, #9556, #5689, #29161, #50066, #25626, #239, #48786, #881, #34962, #59087, #15013, #35274, #34628, #54253, #10194, #54578, #54896, #30115, #29794, #49745, #10825, #1206, #11142, #51668, #50704, #36231, #30766, #46523, #2780, #6335, #7610, #31081, #46200, #36544, #2465, #45558, #60692, #51354, #16296, #12421, #35598, #41999, #31720, #60373, #7293, #22400, #2160, #55222, #35919, #27215, #26903, #55548, #22076, #11459, #16612, #21767, #46832, #61322, #55858, #11772, #6971, #17245, #21119, #41672, #31390, #61640, #50387, #6646, #41360, #36869, #51029, #26253, #56499, #32033, #40726, #26581, #56176, #61004, #16929, #45876, #1516, #12097 ) ),
 .UNSPECIFIED., .F., .F., .F. ) 
 B_SPLINE_SURFACE_WITH_KNOTS ( ( 2, 2 ),
 ( 3, 2, 2, 2, 2, 2, 2, 2, 2, 2, 2, 2, 2, 2, 2, 2, 2, 2, 2, 2, 2, 2, 2, 2, 2, 2, 2, 2, 2, 2, 2, 2, 2, 2, 2, 2, 2, 2, 2, 2, 2, 2, 2, 2, 2, 2, 2, 2, 2, 2, 2, 2, 2, 2, 2, 2, 2, 2, 2, 2, 2, 2, 2, 2, 2, 2, 2, 2, 2, 2, 2, 2, 2, 2, 2, 2, 2, 2, 2, 2, 2, 2, 2, 2, 2, 2, 2, 2, 2, 2, 2, 2, 2, 2, 2, 2, 2, 2, 2, 2, 2, 2, 2, 2, 2, 2, 2, 2, 2, 2, 2, 2, 2, 2, 2, 2, 2, 2, 2, 2, 2, 2, 2, 2, 2, 2, 2, 2, 2, 2, 2, 2, 2, 2, 2, 2, 2, 2, 2, 2, 2, 2, 2, 2, 2, 2, 2, 2, 2, 2, 2, 2, 2, 2, 2, 2, 2, 2, 2, 2, 2, 2, 2, 2, 2, 2, 2, 2, 2, 2, 2, 2, 2, 2, 2, 2, 2, 2, 2, 2, 2, 2, 2, 2, 2, 2, 2, 2, 2, 2, 2, 2, 2, 2, 2, 2, 2, 2, 2, 2, 2, 2, 2, 2, 2, 2, 2, 2, 2, 2, 2, 2, 2, 2, 2, 2, 2, 2, 2, 2, 2, 2, 2, 2, 2, 2, 2, 2, 2, 2, 2, 2, 2, 2, 2, 2, 2, 2, 2, 2, 2, 2, 2, 2, 2, 2, 2, 2, 2, 2, 2, 2, 2, 2, 2, 2, 2, 2, 2, 2, 2, 2, 2, 2, 2, 2, 2, 2, 2, 2, 2, 2, 2, 2, 2, 2, 2, 2, 2, 2, 2, 2, 2, 2, 2, 2, 2, 2, 2, 2, 2, 2, 2, 2, 2, 2, 2, 2, 2, 2, 2, 2, 2, 2, 2, 2, 2, 2, 2, 2, 2, 2, 2, 2, 2, 2, 2, 2, 2, 2, 2, 2, 2, 2, 2, 2, 2, 2, 2, 2, 2, 2, 2, 2, 2, 2, 2, 2, 2, 2, 2, 2, 2, 2, 2, 2, 2, 2, 2, 2, 2, 2, 2, 2, 2, 2, 2, 2, 2, 2, 2, 2, 2, 2, 2, 2, 2, 2, 2, 2, 2, 2, 2, 2, 2, 2, 2, 2, 2, 2, 2, 2, 2, 2, 2, 2, 2, 2, 2, 2, 2, 2, 2, 2, 2, 2, 2, 2, 2, 2, 2, 2, 2, 2, 2, 2, 2, 2, 2, 2, 2, 2, 2, 2, 2, 2, 2, 2, 2, 2, 2, 2, 2, 2, 2, 2, 2, 2, 2, 2, 2, 2, 2, 2, 2, 2, 2, 2, 2, 2, 2, 2, 2, 2, 2, 2, 2, 2, 2, 2, 2, 2, 2, 2, 2, 2, 2, 2, 2, 2, 2, 2, 2, 2, 2, 2, 2, 2, 2, 2, 2, 2, 2, 2, 2, 2, 2, 2, 2, 2, 2, 2, 2, 2, 2, 2, 2, 2, 2, 2, 2, 2, 2, 2, 2, 2, 2, 2, 2, 2, 2, 2, 2, 2, 2, 2, 2, 2, 2, 2, 2, 2, 2, 2, 2, 2, 2, 2, 2, 2, 2, 2, 2, 2, 2, 2, 2, 2, 2, 2, 2, 2, 2, 2, 2, 2, 2, 2, 2, 2, 2, 2, 2, 2, 2, 2, 2, 2, 2, 2, 2, 2, 2, 2, 2, 2, 2, 2, 2, 2, 2, 2, 2, 2, 2, 2, 2, 2, 2, 2, 2, 2, 2, 2, 2, 2, 2, 2, 2, 2, 2, 2, 2, 2, 2, 2, 2, 2, 2, 2, 2, 2, 2, 2, 2, 2, 2, 2, 2, 2, 2, 2, 2, 2, 2, 2, 2, 2, 2, 2, 2, 2, 2, 2, 2, 2, 2, 2, 2, 2, 2, 2, 2, 2, 2, 2, 2, 2, 2, 2, 2, 2, 2, 2, 2, 2, 2, 2, 2, 2, 2, 2, 2, 2, 2, 2, 2, 2, 2, 2, 2, 2, 2, 2, 2, 2, 2, 2, 2, 2, 2, 2, 2, 2, 2, 2, 2, 2, 2, 2, 2, 2, 2, 2, 2, 2, 2, 2, 2, 2, 2, 2, 2, 2, 2, 2, 2, 2, 2, 2, 2, 2, 2, 2, 2, 2, 2, 2, 2, 2, 2, 2, 2, 2, 2, 2, 2, 2, 2, 2, 2, 2, 2, 2, 2, 2, 2, 2, 2, 2, 3 ),
 ( 0.000000000000000000, 1.000000000000000000 ),
 ( 0.000000000000000000, 0.001388888888888888942, 0.002777777777777777884, 0.004166666666666666609, 0.005555555555555555768, 0.006944444444444444059, 0.008333333333333333218, 0.009722222222222222376, 0.01111111111111111154, 0.01250000000000000069, 0.01388888888888888812, 0.01527777777777777728, 0.01666666666666666644, 0.01805555555555555386, 0.01944444444444444475, 0.02083333333333333218, 0.02222222222222222307, 0.02361111111111111049, 0.02500000000000000139, 0.02638888888888888881, 0.02777777777777777624, 0.02916666666666666713, 0.03055555555555555455, 0.03194444444444444198, 0.03333333333333333287, 0.03472222222222222376, 0.03611111111111110772, 0.03749999999999999861, 0.03888888888888888951, 0.04027777777777778040, 0.04166666666666666435, 0.04305555555555555525, 0.04444444444444444614, 0.04583333333333333010, 0.04722222222222222099, 0.04861111111111111188, 0.05000000000000000278, 0.05138888888888888673, 0.05277777777777777762, 0.05416666666666666852, 0.05555555555555555247, 0.05694444444444444337, 0.05833333333333333426, 0.05972222222222222515, 0.06111111111111110911, 0.06250000000000000000, 0.06388888888888888395, 0.06527777777777778179, 0.06666666666666666574, 0.06805555555555554970, 0.06944444444444444753, 0.07083333333333333148, 0.07222222222222221544, 0.07361111111111111327, 0.07499999999999999722, 0.07638888888888889506, 0.07777777777777777901, 0.07916666666666666297, 0.08055555555555556080, 0.08194444444444444475, 0.08333333333333332871, 0.08472222222222222654, 0.08611111111111111049, 0.08749999999999999445, 0.08888888888888889228, 0.09027777777777777624, 0.09166666666666666019, 0.09305555555555555802, 0.09444444444444444198, 0.09583333333333333981, 0.09722222222222222376, 0.09861111111111110772, 0.1000000000000000056, 0.1013888888888888895, 0.1027777777777777735, 0.1041666666666666713, 0.1055555555555555552, 0.1069444444444444392, 0.1083333333333333370, 0.1097222222222222210, 0.1111111111111111049, 0.1125000000000000028, 0.1138888888888888867, 0.1152777777777777846, 0.1166666666666666685, 0.1180555555555555525, 0.1194444444444444503, 0.1208333333333333343, 0.1222222222222222182, 0.1236111111111111160, 0.1250000000000000000, 0.1263888888888888840, 0.1277777777777777679, 0.1291666666666666796, 0.1305555555555555636, 0.1319444444444444475, 0.1333333333333333315, 0.1347222222222222154, 0.1361111111111110994, 0.1375000000000000111, 0.1388888888888888951, 0.1402777777777777790, 0.1416666666666666630, 0.1430555555555555469, 0.1444444444444444309, 0.1458333333333333426, 0.1472222222222222265, 0.1486111111111111105, 0.1499999999999999944, 0.1513888888888888784, 0.1527777777777777901, 0.1541666666666666741, 0.1555555555555555580, 0.1569444444444444420, 0.1583333333333333259, 0.1597222222222222099, 0.1611111111111111216, 0.1625000000000000056, 0.1638888888888888895, 0.1652777777777777735, 0.1666666666666666574, 0.1680555555555555691, 0.1694444444444444531, 0.1708333333333333370, 0.1722222222222222210, 0.1736111111111111049, 0.1749999999999999889, 0.1763888888888889006, 0.1777777777777777846, 0.1791666666666666685, 0.1805555555555555525, 0.1819444444444444364, 0.1833333333333333204, 0.1847222222222222321, 0.1861111111111111160, 0.1875000000000000000, 0.1888888888888888840, 0.1902777777777777679, 0.1916666666666666796, 0.1930555555555555636, 0.1944444444444444475, 0.1958333333333333315, 0.1972222222222222154, 0.1986111111111110994, 0.2000000000000000111, 0.2013888888888888951, 0.2027777777777777790, 0.2041666666666666630, 0.2055555555555555469, 0.2069444444444444309, 0.2083333333333333426, 0.2097222222222222265, 0.2111111111111111105, 0.2124999999999999944, 0.2138888888888888784, 0.2152777777777777901, 0.2166666666666666741, 0.2180555555555555580, 0.2194444444444444420, 0.2208333333333333259, 0.2222222222222222099, 0.2236111111111111216, 0.2250000000000000056, 0.2263888888888888895, 0.2277777777777777735, 0.2291666666666666574, 0.2305555555555555691, 0.2319444444444444531, 0.2333333333333333370, 0.2347222222222222210, 0.2361111111111111049, 0.2374999999999999889, 0.2388888888888889006, 0.2402777777777777846, 0.2416666666666666685, 0.2430555555555555525, 0.2444444444444444364, 0.2458333333333333204, 0.2472222222222222321, 0.2486111111111111160, 0.2500000000000000000, 0.2513888888888888840, 0.2527777777777777679, 0.2541666666666666519, 0.2555555555555555358, 0.2569444444444444198, 0.2583333333333333592, 0.2597222222222222432, 0.2611111111111111271, 0.2625000000000000111, 0.2638888888888888951, 0.2652777777777777790, 0.2666666666666666630, 0.2680555555555555469, 0.2694444444444444309, 0.2708333333333333148, 0.2722222222222221988, 0.2736111111111111382, 0.2750000000000000222, 0.2763888888888889062, 0.2777777777777777901, 0.2791666666666666741, 0.2805555555555555580, 0.2819444444444444420, 0.2833333333333333259, 0.2847222222222222099, 0.2861111111111110938, 0.2874999999999999778, 0.2888888888888888618, 0.2902777777777778012, 0.2916666666666666852, 0.2930555555555555691, 0.2944444444444444531, 0.2958333333333333370, 0.2972222222222222210, 0.2986111111111111049, 0.2999999999999999889, 0.3013888888888888729, 0.3027777777777777568, 0.3041666666666666408, 0.3055555555555555802, 0.3069444444444444642, 0.3083333333333333481, 0.3097222222222222321, 0.3111111111111111160, 0.3125000000000000000, 0.3138888888888888840, 0.3152777777777777679, 0.3166666666666666519, 0.3180555555555555358, 0.3194444444444444198, 0.3208333333333333592, 0.3222222222222222432, 0.3236111111111111271, 0.3250000000000000111, 0.3263888888888888951, 0.3277777777777777790, 0.3291666666666666630, 0.3305555555555555469, 0.3319444444444444309, 0.3333333333333333148, 0.3347222222222221988, 0.3361111111111111382, 0.3375000000000000222, 0.3388888888888889062, 0.3402777777777777901, 0.3416666666666666741, 0.3430555555555555580, 0.3444444444444444420, 0.3458333333333333259, 0.3472222222222222099, 0.3486111111111110938, 0.3499999999999999778, 0.3513888888888888618, 0.3527777777777778012, 0.3541666666666666852, 0.3555555555555555691, 0.3569444444444444531, 0.3583333333333333370, 0.3597222222222222210, 0.3611111111111111049, 0.3624999999999999889, 0.3638888888888888729, 0.3652777777777777568, 0.3666666666666666408, 0.3680555555555555802, 0.3694444444444444642, 0.3708333333333333481, 0.3722222222222222321, 0.3736111111111111160, 0.3750000000000000000, 0.3763888888888888840, 0.3777777777777777679, 0.3791666666666666519, 0.3805555555555555358, 0.3819444444444444198, 0.3833333333333333592, 0.3847222222222222432, 0.3861111111111111271, 0.3875000000000000111, 0.3888888888888888951, 0.3902777777777777790, 0.3916666666666666630, 0.3930555555555555469, 0.3944444444444444309, 0.3958333333333333148, 0.3972222222222221988, 0.3986111111111111382, 0.4000000000000000222, 0.4013888888888889062, 0.4027777777777777901, 0.4041666666666666741, 0.4055555555555555580, 0.4069444444444444420, 0.4083333333333333259, 0.4097222222222222099, 0.4111111111111110938, 0.4124999999999999778, 0.4138888888888888618, 0.4152777777777778012, 0.4166666666666666852, 0.4180555555555555691, 0.4194444444444444531, 0.4208333333333333370, 0.4222222222222222210, 0.4236111111111111049, 0.4249999999999999889, 0.4263888888888888729, 0.4277777777777777568, 0.4291666666666666408, 0.4305555555555555802, 0.4319444444444444642, 0.4333333333333333481, 0.4347222222222222321, 0.4361111111111111160, 0.4375000000000000000, 0.4388888888888888840, 0.4402777777777777679, 0.4416666666666666519, 0.4430555555555555358, 0.4444444444444444198, 0.4458333333333333592, 0.4472222222222222432, 0.4486111111111111271, 0.4500000000000000111, 0.4513888888888888951, 0.4527777777777777790, 0.4541666666666666630, 0.4555555555555555469, 0.4569444444444444309, 0.4583333333333333148, 0.4597222222222221988, 0.4611111111111111382, 0.4625000000000000222, 0.4638888888888889062, 0.4652777777777777901, 0.4666666666666666741, 0.4680555555555555580, 0.4694444444444444420, 0.4708333333333333259, 0.4722222222222222099, 0.4736111111111110938, 0.4749999999999999778, 0.4763888888888888618, 0.4777777777777778012, 0.4791666666666666852, 0.4805555555555555691, 0.4819444444444444531, 0.4833333333333333370, 0.4847222222222222210, 0.4861111111111111049, 0.4874999999999999889, 0.4888888888888888729, 0.4902777777777777568, 0.4916666666666666408, 0.4930555555555555802, 0.4944444444444444642, 0.4958333333333333481, 0.4972222222222222321, 0.4986111111111111160, 0.5000000000000000000, 0.5013888888888888840, 0.5027777777777777679, 0.5041666666666666519, 0.5055555555555555358, 0.5069444444444444198, 0.5083333333333333037, 0.5097222222222221877, 0.5111111111111110716, 0.5124999999999999556, 0.5138888888888888395, 0.5152777777777777235, 0.5166666666666667185, 0.5180555555555556024, 0.5194444444444444864, 0.5208333333333333703, 0.5222222222222222543, 0.5236111111111111382, 0.5250000000000000222, 0.5263888888888889062, 0.5277777777777777901, 0.5291666666666666741, 0.5305555555555555580, 0.5319444444444444420, 0.5333333333333333259, 0.5347222222222222099, 0.5361111111111110938, 0.5374999999999999778, 0.5388888888888888618, 0.5402777777777777457, 0.5416666666666666297, 0.5430555555555555136, 0.5444444444444443976, 0.5458333333333332815, 0.5472222222222222765, 0.5486111111111111605, 0.5500000000000000444, 0.5513888888888889284, 0.5527777777777778123, 0.5541666666666666963, 0.5555555555555555802, 0.5569444444444444642, 0.5583333333333333481, 0.5597222222222222321, 0.5611111111111111160, 0.5625000000000000000, 0.5638888888888888840, 0.5652777777777777679, 0.5666666666666666519, 0.5680555555555555358, 0.5694444444444444198, 0.5708333333333333037, 0.5722222222222221877, 0.5736111111111110716, 0.5749999999999999556, 0.5763888888888888395, 0.5777777777777777235, 0.5791666666666667185, 0.5805555555555556024, 0.5819444444444444864, 0.5833333333333333703, 0.5847222222222222543, 0.5861111111111111382, 0.5875000000000000222, 0.5888888888888889062, 0.5902777777777777901, 0.5916666666666666741, 0.5930555555555555580, 0.5944444444444444420, 0.5958333333333333259, 0.5972222222222222099, 0.5986111111111110938, 0.5999999999999999778, 0.6013888888888888618, 0.6027777777777777457, 0.6041666666666666297, 0.6055555555555555136, 0.6069444444444443976, 0.6083333333333332815, 0.6097222222222222765, 0.6111111111111111605, 0.6125000000000000444, 0.6138888888888889284, 0.6152777777777778123, 0.6166666666666666963, 0.6180555555555555802, 0.6194444444444444642, 0.6208333333333333481, 0.6222222222222222321, 0.6236111111111111160, 0.6250000000000000000, 0.6263888888888888840, 0.6277777777777777679, 0.6291666666666666519, 0.6305555555555555358, 0.6319444444444444198, 0.6333333333333333037, 0.6347222222222221877, 0.6361111111111110716, 0.6374999999999999556, 0.6388888888888888395, 0.6402777777777777235, 0.6416666666666667185, 0.6430555555555556024, 0.6444444444444444864, 0.6458333333333333703, 0.6472222222222222543, 0.6486111111111111382, 0.6500000000000000222, 0.6513888888888889062, 0.6527777777777777901, 0.6541666666666666741, 0.6555555555555555580, 0.6569444444444444420, 0.6583333333333333259, 0.6597222222222222099, 0.6611111111111110938, 0.6624999999999999778, 0.6638888888888888618, 0.6652777777777777457, 0.6666666666666666297, 0.6680555555555555136, 0.6694444444444443976, 0.6708333333333332815, 0.6722222222222222765, 0.6736111111111111605, 0.6750000000000000444, 0.6763888888888889284, 0.6777777777777778123, 0.6791666666666666963, 0.6805555555555555802, 0.6819444444444444642, 0.6833333333333333481, 0.6847222222222222321, 0.6861111111111111160, 0.6875000000000000000, 0.6888888888888888840, 0.6902777777777777679, 0.6916666666666666519, 0.6930555555555555358, 0.6944444444444444198, 0.6958333333333333037, 0.6972222222222221877, 0.6986111111111110716, 0.6999999999999999556, 0.7013888888888888395, 0.7027777777777777235, 0.7041666666666667185, 0.7055555555555556024, 0.7069444444444444864, 0.7083333333333333703, 0.7097222222222222543, 0.7111111111111111382, 0.7125000000000000222, 0.7138888888888889062, 0.7152777777777777901, 0.7166666666666666741, 0.7180555555555555580, 0.7194444444444444420, 0.7208333333333333259, 0.7222222222222222099, 0.7236111111111110938, 0.7249999999999999778, 0.7263888888888888618, 0.7277777777777777457, 0.7291666666666666297, 0.7305555555555555136, 0.7319444444444443976, 0.7333333333333332815, 0.7347222222222222765, 0.7361111111111111605, 0.7375000000000000444, 0.7388888888888889284, 0.7402777777777778123, 0.7416666666666666963, 0.7430555555555555802, 0.7444444444444444642, 0.7458333333333333481, 0.7472222222222222321, 0.7486111111111111160, 0.7500000000000000000, 0.7513888888888888840, 0.7527777777777777679, 0.7541666666666666519, 0.7555555555555555358, 0.7569444444444444198, 0.7583333333333333037, 0.7597222222222221877, 0.7611111111111110716, 0.7624999999999999556, 0.7638888888888888395, 0.7652777777777777235, 0.7666666666666667185, 0.7680555555555556024, 0.7694444444444444864, 0.7708333333333333703, 0.7722222222222222543, 0.7736111111111111382, 0.7750000000000000222, 0.7763888888888889062, 0.7777777777777777901, 0.7791666666666666741, 0.7805555555555555580, 0.7819444444444444420, 0.7833333333333333259, 0.7847222222222222099, 0.7861111111111110938, 0.7874999999999999778, 0.7888888888888888618, 0.7902777777777777457, 0.7916666666666666297, 0.7930555555555555136, 0.7944444444444443976, 0.7958333333333332815, 0.7972222222222222765, 0.7986111111111111605, 0.8000000000000000444, 0.8013888888888889284, 0.8027777777777778123, 0.8041666666666666963, 0.8055555555555555802, 0.8069444444444444642, 0.8083333333333333481, 0.8097222222222222321, 0.8111111111111111160, 0.8125000000000000000, 0.8138888888888888840, 0.8152777777777777679, 0.8166666666666666519, 0.8180555555555555358, 0.8194444444444444198, 0.8208333333333333037, 0.8222222222222221877, 0.8236111111111110716, 0.8249999999999999556, 0.8263888888888888395, 0.8277777777777777235, 0.8291666666666667185, 0.8305555555555556024, 0.8319444444444444864, 0.8333333333333333703, 0.8347222222222222543, 0.8361111111111111382, 0.8375000000000000222, 0.8388888888888889062, 0.8402777777777777901, 0.8416666666666666741, 0.8430555555555555580, 0.8444444444444444420, 0.8458333333333333259, 0.8472222222222222099, 0.8486111111111110938, 0.8499999999999999778, 0.8513888888888888618, 0.8527777777777777457, 0.8541666666666666297, 0.8555555555555555136, 0.8569444444444443976, 0.8583333333333332815, 0.8597222222222222765, 0.8611111111111111605, 0.8625000000000000444, 0.8638888888888889284, 0.8652777777777778123, 0.8666666666666666963, 0.8680555555555555802, 0.8694444444444444642, 0.8708333333333333481, 0.8722222222222222321, 0.8736111111111111160, 0.8750000000000000000, 0.8763888888888888840, 0.8777777777777777679, 0.8791666666666666519, 0.8805555555555555358, 0.8819444444444444198, 0.8833333333333333037, 0.8847222222222221877, 0.8861111111111110716, 0.8874999999999999556, 0.8888888888888888395, 0.8902777777777777235, 0.8916666666666667185, 0.8930555555555556024, 0.8944444444444444864, 0.8958333333333333703, 0.8972222222222222543, 0.8986111111111111382, 0.9000000000000000222, 0.9013888888888889062, 0.9027777777777777901, 0.9041666666666666741, 0.9055555555555555580, 0.9069444444444444420, 0.9083333333333333259, 0.9097222222222222099, 0.9111111111111110938, 0.9124999999999999778, 0.9138888888888888618, 0.9152777777777777457, 0.9166666666666666297, 0.9180555555555555136, 0.9194444444444443976, 0.9208333333333332815, 0.9222222222222222765, 0.9236111111111111605, 0.9250000000000000444, 0.9263888888888889284, 0.9277777777777778123, 0.9291666666666666963, 0.9305555555555555802, 0.9319444444444444642, 0.9333333333333333481, 0.9347222222222222321, 0.9361111111111111160, 0.9375000000000000000, 0.9388888888888888840, 0.9402777777777777679, 0.9416666666666666519, 0.9430555555555555358, 0.9444444444444444198, 0.9458333333333333037, 0.9472222222222221877, 0.9486111111111110716, 0.9499999999999999556, 0.9513888888888888395, 0.9527777777777777235, 0.9541666666666667185, 0.9555555555555556024, 0.9569444444444444864, 0.9583333333333333703, 0.9597222222222222543, 0.9611111111111111382, 0.9625000000000000222, 0.9638888888888889062, 0.9652777777777777901, 0.9666666666666666741, 0.9680555555555555580, 0.9694444444444444420, 0.9708333333333333259, 0.9722222222222222099, 0.9736111111111110938, 0.9749999999999999778, 0.9763888888888888618, 0.9777777777777777457, 0.9791666666666666297, 0.9805555555555555136, 0.9819444444444443976, 0.9833333333333332815, 0.9847222222222222765, 0.9861111111111111605, 0.9875000000000000444, 0.9888888888888889284, 0.9902777777777778123, 0.9916666666666666963, 0.9930555555555555802, 0.9944444444444444642, 0.9958333333333333481, 0.9972222222222222321, 0.9986111111111111160, 1.000000000000000000 ),
 .UNSPECIFIED. ) 
 GEOMETRIC_REPRESENTATION_ITEM ( )  RATIONAL_B_SPLINE_SURFACE ( (
 ( 1.000000000000000000, 0.8660254037844387076, 1.000000000000000000, 0.8660254037844387076, 1.000000000000000000, 0.8660254037844387076, 1.000000000000000000, 0.8660254037844387076, 1.000000000000000000, 0.8660254037844387076, 1.000000000000000000, 0.8660254037844387076, 1.000000000000000000, 0.8660254037844387076, 1.000000000000000000, 0.8660254037844387076, 1.000000000000000000, 0.8660254037844387076, 1.000000000000000000, 0.8660254037844387076, 1.000000000000000000, 0.8660254037844387076, 1.000000000000000000, 0.8660254037844387076, 1.000000000000000000, 0.8660254037844387076, 1.000000000000000000, 0.8660254037844387076, 1.000000000000000000, 0.8660254037844387076, 1.000000000000000000, 0.8660254037844387076, 1.000000000000000000, 0.8660254037844387076, 1.000000000000000000, 0.8660254037844387076, 1.000000000000000000, 0.8660254037844387076, 1.000000000000000000, 0.8660254037844387076, 1.000000000000000000, 0.8660254037844387076, 1.000000000000000000, 0.8660254037844387076, 1.000000000000000000, 0.8660254037844387076, 1.000000000000000000, 0.8660254037844387076, 1.000000000000000000, 0.8660254037844387076, 1.000000000000000000, 0.8660254037844387076, 1.000000000000000000, 0.8660254037844387076, 1.000000000000000000, 0.8660254037844387076, 1.000000000000000000, 0.8660254037844387076, 1.000000000000000000, 0.8660254037844387076, 1.000000000000000000, 0.8660254037844387076, 1.000000000000000000, 0.8660254037844387076, 1.000000000000000000, 0.8660254037844387076, 1.000000000000000000, 0.8660254037844387076, 1.000000000000000000, 0.8660254037844387076, 1.000000000000000000, 0.8660254037844387076, 1.000000000000000000, 0.8660254037844387076, 1.000000000000000000, 0.8660254037844387076, 1.000000000000000000, 0.8660254037844387076, 1.000000000000000000, 0.8660254037844387076, 1.000000000000000000, 0.8660254037844387076, 1.000000000000000000, 0.8660254037844387076, 1.000000000000000000, 0.8660254037844387076, 1.000000000000000000, 0.8660254037844387076, 1.000000000000000000, 0.8660254037844387076, 1.000000000000000000, 0.8660254037844387076, 1.000000000000000000, 0.8660254037844387076, 1.000000000000000000, 0.8660254037844387076, 1.000000000000000000, 0.8660254037844387076, 1.000000000000000000, 0.8660254037844387076, 1.000000000000000000, 0.8660254037844387076, 1.000000000000000000, 0.8660254037844387076, 1.000000000000000000, 0.8660254037844387076, 1.000000000000000000, 0.8660254037844387076, 1.000000000000000000, 0.8660254037844387076, 1.000000000000000000, 0.8660254037844387076, 1.000000000000000000, 0.8660254037844387076, 1.000000000000000000, 0.8660254037844387076, 1.000000000000000000, 0.8660254037844387076, 1.000000000000000000, 0.8660254037844387076, 1.000000000000000000, 0.8660254037844387076, 1.000000000000000000, 0.8660254037844387076, 1.000000000000000000, 0.8660254037844387076, 1.000000000000000000, 0.8660254037844387076, 1.000000000000000000, 0.8660254037844387076, 1.000000000000000000, 0.8660254037844387076, 1.000000000000000000, 0.8660254037844387076, 1.000000000000000000, 0.8660254037844387076, 1.000000000000000000, 0.8660254037844387076, 1.000000000000000000, 0.8660254037844387076, 1.000000000000000000, 0.8660254037844387076, 1.000000000000000000, 0.8660254037844387076, 1.000000000000000000, 0.8660254037844387076, 1.000000000000000000, 0.8660254037844387076, 1.000000000000000000, 0.8660254037844387076, 1.000000000000000000, 0.8660254037844387076, 1.000000000000000000, 0.8660254037844387076, 1.000000000000000000, 0.8660254037844387076, 1.000000000000000000, 0.8660254037844387076, 1.000000000000000000, 0.8660254037844387076, 1.000000000000000000, 0.8660254037844387076, 1.000000000000000000, 0.8660254037844387076, 1.000000000000000000, 0.8660254037844387076, 1.000000000000000000, 0.8660254037844387076, 1.000000000000000000, 0.8660254037844387076, 1.000000000000000000, 0.8660254037844387076, 1.000000000000000000, 0.8660254037844387076, 1.000000000000000000, 0.8660254037844387076, 1.000000000000000000, 0.8660254037844387076, 1.000000000000000000, 0.8660254037844387076, 1.000000000000000000, 0.8660254037844387076, 1.000000000000000000, 0.8660254037844387076, 1.000000000000000000, 0.8660254037844387076, 1.000000000000000000, 0.8660254037844387076, 1.000000000000000000, 0.8660254037844387076, 1.000000000000000000, 0.8660254037844387076, 1.000000000000000000, 0.8660254037844387076, 1.000000000000000000, 0.8660254037844387076, 1.000000000000000000, 0.8660254037844387076, 1.000000000000000000, 0.8660254037844387076, 1.000000000000000000, 0.8660254037844387076, 1.000000000000000000, 0.8660254037844387076, 1.000000000000000000, 0.8660254037844387076, 1.000000000000000000, 0.8660254037844387076, 1.000000000000000000, 0.8660254037844387076, 1.000000000000000000, 0.8660254037844387076, 1.000000000000000000, 0.8660254037844387076, 1.000000000000000000, 0.8660254037844387076, 1.000000000000000000, 0.8660254037844387076, 1.000000000000000000, 0.8660254037844387076, 1.000000000000000000, 0.8660254037844387076, 1.000000000000000000, 0.8660254037844387076, 1.000000000000000000, 0.8660254037844387076, 1.000000000000000000, 0.8660254037844387076, 1.000000000000000000, 0.8660254037844387076, 1.000000000000000000, 0.8660254037844387076, 1.000000000000000000, 0.8660254037844387076, 1.000000000000000000, 0.8660254037844387076, 1.000000000000000000, 0.8660254037844387076, 1.000000000000000000, 0.8660254037844387076, 1.000000000000000000, 0.8660254037844387076, 1.000000000000000000, 0.8660254037844387076, 1.000000000000000000, 0.8660254037844387076, 1.000000000000000000, 0.8660254037844387076, 1.000000000000000000, 0.8660254037844387076, 1.000000000000000000, 0.8660254037844387076, 1.000000000000000000, 0.8660254037844387076, 1.000000000000000000, 0.8660254037844387076, 1.000000000000000000, 0.8660254037844387076, 1.000000000000000000, 0.8660254037844387076, 1.000000000000000000, 0.8660254037844387076, 1.000000000000000000, 0.8660254037844387076, 1.000000000000000000, 0.8660254037844387076, 1.000000000000000000, 0.8660254037844387076, 1.000000000000000000, 0.8660254037844387076, 1.000000000000000000, 0.8660254037844387076, 1.000000000000000000, 0.8660254037844387076, 1.000000000000000000, 0.8660254037844387076, 1.000000000000000000, 0.8660254037844387076, 1.000000000000000000, 0.8660254037844387076, 1.000000000000000000, 0.8660254037844387076, 1.000000000000000000, 0.8660254037844387076, 1.000000000000000000, 0.8660254037844387076, 1.000000000000000000, 0.8660254037844387076, 1.000000000000000000, 0.8660254037844387076, 1.000000000000000000, 0.8660254037844387076, 1.000000000000000000, 0.8660254037844387076, 1.000000000000000000, 0.8660254037844387076, 1.000000000000000000, 0.8660254037844387076, 1.000000000000000000, 0.8660254037844387076, 1.000000000000000000, 0.8660254037844387076, 1.000000000000000000, 0.8660254037844387076, 1.000000000000000000, 0.8660254037844387076, 1.000000000000000000, 0.8660254037844387076, 1.000000000000000000, 0.8660254037844387076, 1.000000000000000000, 0.8660254037844387076, 1.000000000000000000, 0.8660254037844387076, 1.000000000000000000, 0.8660254037844387076, 1.000000000000000000, 0.8660254037844387076, 1.000000000000000000, 0.8660254037844387076, 1.000000000000000000, 0.8660254037844387076, 1.000000000000000000, 0.8660254037844387076, 1.000000000000000000, 0.8660254037844387076, 1.000000000000000000, 0.8660254037844387076, 1.000000000000000000, 0.8660254037844387076, 1.000000000000000000, 0.8660254037844387076, 1.000000000000000000, 0.8660254037844387076, 1.000000000000000000, 0.8660254037844387076, 1.000000000000000000, 0.8660254037844387076, 1.000000000000000000, 0.8660254037844387076, 1.000000000000000000, 0.8660254037844387076, 1.000000000000000000, 0.8660254037844387076, 1.000000000000000000, 0.8660254037844387076, 1.000000000000000000, 0.8660254037844387076, 1.000000000000000000, 0.8660254037844387076, 1.000000000000000000, 0.8660254037844387076, 1.000000000000000000, 0.8660254037844387076, 1.000000000000000000, 0.8660254037844387076, 1.000000000000000000, 0.8660254037844387076, 1.000000000000000000, 0.8660254037844387076, 1.000000000000000000, 0.8660254037844387076, 1.000000000000000000, 0.8660254037844387076, 1.000000000000000000, 0.8660254037844387076, 1.000000000000000000, 0.8660254037844387076, 1.000000000000000000, 0.8660254037844387076, 1.000000000000000000, 0.8660254037844387076, 1.000000000000000000, 0.8660254037844387076, 1.000000000000000000, 0.8660254037844387076, 1.000000000000000000, 0.8660254037844387076, 1.000000000000000000, 0.8660254037844387076, 1.000000000000000000, 0.8660254037844387076, 1.000000000000000000, 0.8660254037844387076, 1.000000000000000000, 0.8660254037844387076, 1.000000000000000000, 0.8660254037844387076, 1.000000000000000000, 0.8660254037844387076, 1.000000000000000000, 0.8660254037844387076, 1.000000000000000000, 0.8660254037844387076, 1.000000000000000000, 0.8660254037844387076, 1.000000000000000000, 0.8660254037844387076, 1.000000000000000000, 0.8660254037844387076, 1.000000000000000000, 0.8660254037844387076, 1.000000000000000000, 0.8660254037844387076, 1.000000000000000000, 0.8660254037844387076, 1.000000000000000000, 0.8660254037844387076, 1.000000000000000000, 0.8660254037844387076, 1.000000000000000000, 0.8660254037844387076, 1.000000000000000000, 0.8660254037844387076, 1.000000000000000000, 0.8660254037844387076, 1.000000000000000000, 0.8660254037844387076, 1.000000000000000000, 0.8660254037844387076, 1.000000000000000000, 0.8660254037844387076, 1.000000000000000000, 0.8660254037844387076, 1.000000000000000000, 0.8660254037844387076, 1.000000000000000000, 0.8660254037844387076, 1.000000000000000000, 0.8660254037844387076, 1.000000000000000000, 0.8660254037844387076, 1.000000000000000000, 0.8660254037844387076, 1.000000000000000000, 0.8660254037844387076, 1.000000000000000000, 0.8660254037844387076, 1.000000000000000000, 0.8660254037844387076, 1.000000000000000000, 0.8660254037844387076, 1.000000000000000000, 0.8660254037844387076, 1.000000000000000000, 0.8660254037844387076, 1.000000000000000000, 0.8660254037844387076, 1.000000000000000000, 0.8660254037844387076, 1.000000000000000000, 0.8660254037844387076, 1.000000000000000000, 0.8660254037844387076, 1.000000000000000000, 0.8660254037844387076, 1.000000000000000000, 0.8660254037844387076, 1.000000000000000000, 0.8660254037844387076, 1.000000000000000000, 0.8660254037844387076, 1.000000000000000000, 0.8660254037844387076, 1.000000000000000000, 0.8660254037844387076, 1.000000000000000000, 0.8660254037844387076, 1.000000000000000000, 0.8660254037844387076, 1.000000000000000000, 0.8660254037844387076, 1.000000000000000000, 0.8660254037844387076, 1.000000000000000000, 0.8660254037844387076, 1.000000000000000000, 0.8660254037844387076, 1.000000000000000000, 0.8660254037844387076, 1.000000000000000000, 0.8660254037844387076, 1.000000000000000000, 0.8660254037844387076, 1.000000000000000000, 0.8660254037844387076, 1.000000000000000000, 0.8660254037844387076, 1.000000000000000000, 0.8660254037844387076, 1.000000000000000000, 0.8660254037844387076, 1.000000000000000000, 0.8660254037844387076, 1.000000000000000000, 0.8660254037844387076, 1.000000000000000000, 0.8660254037844387076, 1.000000000000000000, 0.8660254037844387076, 1.000000000000000000, 0.8660254037844387076, 1.000000000000000000, 0.8660254037844387076, 1.000000000000000000, 0.8660254037844387076, 1.000000000000000000, 0.8660254037844387076, 1.000000000000000000, 0.8660254037844387076, 1.000000000000000000, 0.8660254037844387076, 1.000000000000000000, 0.8660254037844387076, 1.000000000000000000, 0.8660254037844387076, 1.000000000000000000, 0.8660254037844387076, 1.000000000000000000, 0.8660254037844387076, 1.000000000000000000, 0.8660254037844387076, 1.000000000000000000, 0.8660254037844387076, 1.000000000000000000, 0.8660254037844387076, 1.000000000000000000, 0.8660254037844387076, 1.000000000000000000, 0.8660254037844387076, 1.000000000000000000, 0.8660254037844387076, 1.000000000000000000, 0.8660254037844387076, 1.000000000000000000, 0.8660254037844387076, 1.000000000000000000, 0.8660254037844387076, 1.000000000000000000, 0.8660254037844387076, 1.000000000000000000, 0.8660254037844387076, 1.000000000000000000, 0.8660254037844387076, 1.000000000000000000, 0.8660254037844387076, 1.000000000000000000, 0.8660254037844387076, 1.000000000000000000, 0.8660254037844387076, 1.000000000000000000, 0.8660254037844387076, 1.000000000000000000, 0.8660254037844387076, 1.000000000000000000, 0.8660254037844387076, 1.000000000000000000, 0.8660254037844387076, 1.000000000000000000, 0.8660254037844387076, 1.000000000000000000, 0.8660254037844387076, 1.000000000000000000, 0.8660254037844387076, 1.000000000000000000, 0.8660254037844387076, 1.000000000000000000, 0.8660254037844387076, 1.000000000000000000, 0.8660254037844387076, 1.000000000000000000, 0.8660254037844387076, 1.000000000000000000, 0.8660254037844387076, 1.000000000000000000, 0.8660254037844387076, 1.000000000000000000, 0.8660254037844387076, 1.000000000000000000, 0.8660254037844387076, 1.000000000000000000, 0.8660254037844387076, 1.000000000000000000, 0.8660254037844387076, 1.000000000000000000, 0.8660254037844387076, 1.000000000000000000, 0.8660254037844387076, 1.000000000000000000, 0.8660254037844387076, 1.000000000000000000, 0.8660254037844387076, 1.000000000000000000, 0.8660254037844387076, 1.000000000000000000, 0.8660254037844387076, 1.000000000000000000, 0.8660254037844387076, 1.000000000000000000, 0.8660254037844387076, 1.000000000000000000, 0.8660254037844387076, 1.000000000000000000, 0.8660254037844387076, 1.000000000000000000, 0.8660254037844387076, 1.000000000000000000, 0.8660254037844387076, 1.000000000000000000, 0.8660254037844387076, 1.000000000000000000, 0.8660254037844387076, 1.000000000000000000, 0.8660254037844387076, 1.000000000000000000, 0.8660254037844387076, 1.000000000000000000, 0.8660254037844387076, 1.000000000000000000, 0.8660254037844387076, 1.000000000000000000, 0.8660254037844387076, 1.000000000000000000, 0.8660254037844387076, 1.000000000000000000, 0.8660254037844387076, 1.000000000000000000, 0.8660254037844387076, 1.000000000000000000, 0.8660254037844387076, 1.000000000000000000, 0.8660254037844387076, 1.000000000000000000, 0.8660254037844387076, 1.000000000000000000, 0.8660254037844387076, 1.000000000000000000, 0.8660254037844387076, 1.000000000000000000, 0.8660254037844387076, 1.000000000000000000, 0.8660254037844387076, 1.000000000000000000, 0.8660254037844387076, 1.000000000000000000, 0.8660254037844387076, 1.000000000000000000, 0.8660254037844387076, 1.000000000000000000, 0.8660254037844387076, 1.000000000000000000, 0.8660254037844387076, 1.000000000000000000, 0.8660254037844387076, 1.000000000000000000, 0.8660254037844387076, 1.000000000000000000, 0.8660254037844387076, 1.000000000000000000, 0.8660254037844387076, 1.000000000000000000, 0.8660254037844387076, 1.000000000000000000, 0.8660254037844387076, 1.000000000000000000, 0.8660254037844387076, 1.000000000000000000, 0.8660254037844387076, 1.000000000000000000, 0.8660254037844387076, 1.000000000000000000, 0.8660254037844387076, 1.000000000000000000, 0.8660254037844387076, 1.000000000000000000, 0.8660254037844387076, 1.000000000000000000, 0.8660254037844387076, 1.000000000000000000, 0.8660254037844387076, 1.000000000000000000, 0.8660254037844387076, 1.000000000000000000, 0.8660254037844387076, 1.000000000000000000, 0.8660254037844387076, 1.000000000000000000, 0.8660254037844387076, 1.000000000000000000, 0.8660254037844387076, 1.000000000000000000, 0.8660254037844387076, 1.000000000000000000, 0.8660254037844387076, 1.000000000000000000, 0.8660254037844387076, 1.000000000000000000, 0.8660254037844387076, 1.000000000000000000, 0.8660254037844387076, 1.000000000000000000, 0.8660254037844387076, 1.000000000000000000, 0.8660254037844387076, 1.000000000000000000, 0.8660254037844387076, 1.000000000000000000, 0.8660254037844387076, 1.000000000000000000, 0.8660254037844387076, 1.000000000000000000, 0.8660254037844387076, 1.000000000000000000, 0.8660254037844387076, 1.000000000000000000, 0.8660254037844387076, 1.000000000000000000, 0.8660254037844387076, 1.000000000000000000, 0.8660254037844387076, 1.000000000000000000, 0.8660254037844387076, 1.000000000000000000, 0.8660254037844387076, 1.000000000000000000, 0.8660254037844387076, 1.000000000000000000, 0.8660254037844387076, 1.000000000000000000, 0.8660254037844387076, 1.000000000000000000, 0.8660254037844387076, 1.000000000000000000, 0.8660254037844387076, 1.000000000000000000, 0.8660254037844387076, 1.000000000000000000, 0.8660254037844387076, 1.000000000000000000, 0.8660254037844387076, 1.000000000000000000, 0.8660254037844387076, 1.000000000000000000, 0.8660254037844387076, 1.000000000000000000, 0.8660254037844387076, 1.000000000000000000, 0.8660254037844387076, 1.000000000000000000, 0.8660254037844387076, 1.000000000000000000, 0.8660254037844387076, 1.000000000000000000, 0.8660254037844387076, 1.000000000000000000, 0.8660254037844387076, 1.000000000000000000, 0.8660254037844387076, 1.000000000000000000, 0.8660254037844387076, 1.000000000000000000, 0.8660254037844387076, 1.000000000000000000, 0.8660254037844387076, 1.000000000000000000, 0.8660254037844387076, 1.000000000000000000, 0.8660254037844387076, 1.000000000000000000, 0.8660254037844387076, 1.000000000000000000, 0.8660254037844387076, 1.000000000000000000, 0.8660254037844387076, 1.000000000000000000, 0.8660254037844387076, 1.000000000000000000, 0.8660254037844387076, 1.000000000000000000, 0.8660254037844387076, 1.000000000000000000, 0.8660254037844387076, 1.000000000000000000, 0.8660254037844387076, 1.000000000000000000, 0.8660254037844387076, 1.000000000000000000, 0.8660254037844387076, 1.000000000000000000, 0.8660254037844387076, 1.000000000000000000, 0.8660254037844387076, 1.000000000000000000, 0.8660254037844387076, 1.000000000000000000, 0.8660254037844387076, 1.000000000000000000, 0.8660254037844387076, 1.000000000000000000, 0.8660254037844387076, 1.000000000000000000, 0.8660254037844387076, 1.000000000000000000, 0.8660254037844387076, 1.000000000000000000, 0.8660254037844387076, 1.000000000000000000, 0.8660254037844387076, 1.000000000000000000, 0.8660254037844387076, 1.000000000000000000, 0.8660254037844387076, 1.000000000000000000, 0.8660254037844387076, 1.000000000000000000, 0.8660254037844387076, 1.000000000000000000, 0.8660254037844387076, 1.000000000000000000, 0.8660254037844387076, 1.000000000000000000, 0.8660254037844387076, 1.000000000000000000, 0.8660254037844387076, 1.000000000000000000, 0.8660254037844387076, 1.000000000000000000, 0.8660254037844387076, 1.000000000000000000, 0.8660254037844387076, 1.000000000000000000, 0.8660254037844387076, 1.000000000000000000, 0.8660254037844387076, 1.000000000000000000, 0.8660254037844387076, 1.000000000000000000, 0.8660254037844387076, 1.000000000000000000, 0.8660254037844387076, 1.000000000000000000, 0.8660254037844387076, 1.000000000000000000, 0.8660254037844387076, 1.000000000000000000, 0.8660254037844387076, 1.000000000000000000, 0.8660254037844387076, 1.000000000000000000, 0.8660254037844387076, 1.000000000000000000, 0.8660254037844387076, 1.000000000000000000, 0.8660254037844387076, 1.000000000000000000, 0.8660254037844387076, 1.000000000000000000, 0.8660254037844387076, 1.000000000000000000, 0.8660254037844387076, 1.000000000000000000, 0.8660254037844387076, 1.000000000000000000, 0.8660254037844387076, 1.000000000000000000, 0.8660254037844387076, 1.000000000000000000, 0.8660254037844387076, 1.000000000000000000, 0.8660254037844387076, 1.000000000000000000, 0.8660254037844387076, 1.000000000000000000, 0.8660254037844387076, 1.000000000000000000, 0.8660254037844387076, 1.000000000000000000, 0.8660254037844387076, 1.000000000000000000, 0.8660254037844387076, 1.000000000000000000, 0.8660254037844387076, 1.000000000000000000, 0.8660254037844387076, 1.000000000000000000, 0.8660254037844387076, 1.000000000000000000, 0.8660254037844387076, 1.000000000000000000, 0.8660254037844387076, 1.000000000000000000, 0.8660254037844387076, 1.000000000000000000, 0.8660254037844387076, 1.000000000000000000, 0.8660254037844387076, 1.000000000000000000, 0.8660254037844387076, 1.000000000000000000, 0.8660254037844387076, 1.000000000000000000, 0.8660254037844387076, 1.000000000000000000, 0.8660254037844387076, 1.000000000000000000, 0.8660254037844387076, 1.000000000000000000, 0.8660254037844387076, 1.000000000000000000, 0.8660254037844387076, 1.000000000000000000, 0.8660254037844387076, 1.000000000000000000, 0.8660254037844387076, 1.000000000000000000, 0.8660254037844387076, 1.000000000000000000, 0.8660254037844387076, 1.000000000000000000, 0.8660254037844387076, 1.000000000000000000, 0.8660254037844387076, 1.000000000000000000, 0.8660254037844387076, 1.000000000000000000, 0.8660254037844387076, 1.000000000000000000, 0.8660254037844387076, 1.000000000000000000, 0.8660254037844387076, 1.000000000000000000, 0.8660254037844387076, 1.000000000000000000, 0.8660254037844387076, 1.000000000000000000, 0.8660254037844387076, 1.000000000000000000, 0.8660254037844387076, 1.000000000000000000, 0.8660254037844387076, 1.000000000000000000, 0.8660254037844387076, 1.000000000000000000, 0.8660254037844387076, 1.000000000000000000, 0.8660254037844387076, 1.000000000000000000, 0.8660254037844387076, 1.000000000000000000, 0.8660254037844387076, 1.000000000000000000, 0.8660254037844387076, 1.000000000000000000, 0.8660254037844387076, 1.000000000000000000, 0.8660254037844387076, 1.000000000000000000, 0.8660254037844387076, 1.000000000000000000, 0.8660254037844387076, 1.000000000000000000, 0.8660254037844387076, 1.000000000000000000, 0.8660254037844387076, 1.000000000000000000, 0.8660254037844387076, 1.000000000000000000, 0.8660254037844387076, 1.000000000000000000, 0.8660254037844387076, 1.000000000000000000, 0.8660254037844387076, 1.000000000000000000, 0.8660254037844387076, 1.000000000000000000, 0.8660254037844387076, 1.000000000000000000, 0.8660254037844387076, 1.000000000000000000, 0.8660254037844387076, 1.000000000000000000, 0.8660254037844387076, 1.000000000000000000, 0.8660254037844387076, 1.000000000000000000, 0.8660254037844387076, 1.000000000000000000, 0.8660254037844387076, 1.000000000000000000, 0.8660254037844387076, 1.000000000000000000, 0.8660254037844387076, 1.000000000000000000, 0.8660254037844387076, 1.000000000000000000, 0.8660254037844387076, 1.000000000000000000, 0.8660254037844387076, 1.000000000000000000, 0.8660254037844387076, 1.000000000000000000, 0.8660254037844387076, 1.000000000000000000, 0.8660254037844387076, 1.000000000000000000, 0.8660254037844387076, 1.000000000000000000, 0.8660254037844387076, 1.000000000000000000, 0.8660254037844387076, 1.000000000000000000, 0.8660254037844387076, 1.000000000000000000, 0.8660254037844387076, 1.000000000000000000, 0.8660254037844387076, 1.000000000000000000, 0.8660254037844387076, 1.000000000000000000, 0.8660254037844387076, 1.000000000000000000, 0.8660254037844387076, 1.000000000000000000, 0.8660254037844387076, 1.000000000000000000, 0.8660254037844387076, 1.000000000000000000, 0.8660254037844387076, 1.000000000000000000, 0.8660254037844387076, 1.000000000000000000, 0.8660254037844387076, 1.000000000000000000, 0.8660254037844387076, 1.000000000000000000, 0.8660254037844387076, 1.000000000000000000, 0.8660254037844387076, 1.000000000000000000, 0.8660254037844387076, 1.000000000000000000, 0.8660254037844387076, 1.000000000000000000, 0.8660254037844387076, 1.000000000000000000, 0.8660254037844387076, 1.000000000000000000, 0.8660254037844387076, 1.000000000000000000, 0.8660254037844387076, 1.000000000000000000, 0.8660254037844387076, 1.000000000000000000, 0.8660254037844387076, 1.000000000000000000, 0.8660254037844387076, 1.000000000000000000, 0.8660254037844387076, 1.000000000000000000, 0.8660254037844387076, 1.000000000000000000, 0.8660254037844387076, 1.000000000000000000, 0.8660254037844387076, 1.000000000000000000, 0.8660254037844387076, 1.000000000000000000, 0.8660254037844387076, 1.000000000000000000, 0.8660254037844387076, 1.000000000000000000, 0.8660254037844387076, 1.000000000000000000, 0.8660254037844387076, 1.000000000000000000, 0.8660254037844387076, 1.000000000000000000, 0.8660254037844387076, 1.000000000000000000, 0.8660254037844387076, 1.000000000000000000, 0.8660254037844387076, 1.000000000000000000, 0.8660254037844387076, 1.000000000000000000, 0.8660254037844387076, 1.000000000000000000, 0.8660254037844387076, 1.000000000000000000, 0.8660254037844387076, 1.000000000000000000, 0.8660254037844387076, 1.000000000000000000, 0.8660254037844387076, 1.000000000000000000, 0.8660254037844387076, 1.000000000000000000, 0.8660254037844387076, 1.000000000000000000, 0.8660254037844387076, 1.000000000000000000, 0.8660254037844387076, 1.000000000000000000, 0.8660254037844387076, 1.000000000000000000, 0.8660254037844387076, 1.000000000000000000, 0.8660254037844387076, 1.000000000000000000, 0.8660254037844387076, 1.000000000000000000, 0.8660254037844387076, 1.000000000000000000, 0.8660254037844387076, 1.000000000000000000, 0.8660254037844387076, 1.000000000000000000, 0.8660254037844387076, 1.000000000000000000, 0.8660254037844387076, 1.000000000000000000, 0.8660254037844387076, 1.000000000000000000, 0.8660254037844387076, 1.000000000000000000, 0.8660254037844387076, 1.000000000000000000, 0.8660254037844387076, 1.000000000000000000, 0.8660254037844387076, 1.000000000000000000, 0.8660254037844387076, 1.000000000000000000, 0.8660254037844387076, 1.000000000000000000, 0.8660254037844387076, 1.000000000000000000, 0.8660254037844387076, 1.000000000000000000, 0.8660254037844387076, 1.000000000000000000, 0.8660254037844387076, 1.000000000000000000, 0.8660254037844387076, 1.000000000000000000, 0.8660254037844387076, 1.000000000000000000, 0.8660254037844387076, 1.000000000000000000, 0.8660254037844387076, 1.000000000000000000, 0.8660254037844387076, 1.000000000000000000, 0.8660254037844387076, 1.000000000000000000, 0.8660254037844387076, 1.000000000000000000, 0.8660254037844387076, 1.000000000000000000, 0.8660254037844387076, 1.000000000000000000, 0.8660254037844387076, 1.000000000000000000, 0.8660254037844387076, 1.000000000000000000, 0.8660254037844387076, 1.000000000000000000, 0.8660254037844387076, 1.000000000000000000, 0.8660254037844387076, 1.000000000000000000, 0.8660254037844387076, 1.000000000000000000, 0.8660254037844387076, 1.000000000000000000, 0.8660254037844387076, 1.000000000000000000, 0.8660254037844387076, 1.000000000000000000, 0.8660254037844387076, 1.000000000000000000, 0.8660254037844387076, 1.000000000000000000, 0.8660254037844387076, 1.000000000000000000, 0.8660254037844387076, 1.000000000000000000, 0.8660254037844387076, 1.000000000000000000, 0.8660254037844387076, 1.000000000000000000, 0.8660254037844387076, 1.000000000000000000, 0.8660254037844387076, 1.000000000000000000, 0.8660254037844387076, 1.000000000000000000, 0.8660254037844387076, 1.000000000000000000, 0.8660254037844387076, 1.000000000000000000, 0.8660254037844387076, 1.000000000000000000, 0.8660254037844387076, 1.000000000000000000, 0.8660254037844387076, 1.000000000000000000, 0.8660254037844387076, 1.000000000000000000, 0.8660254037844387076, 1.000000000000000000, 0.8660254037844387076, 1.000000000000000000, 0.8660254037844387076, 1.000000000000000000, 0.8660254037844387076, 1.000000000000000000, 0.8660254037844387076, 1.000000000000000000, 0.8660254037844387076, 1.000000000000000000, 0.8660254037844387076, 1.000000000000000000, 0.8660254037844387076, 1.000000000000000000, 0.8660254037844387076, 1.000000000000000000, 0.8660254037844387076, 1.000000000000000000, 0.8660254037844387076, 1.000000000000000000, 0.8660254037844387076, 1.000000000000000000, 0.8660254037844387076, 1.000000000000000000, 0.8660254037844387076, 1.000000000000000000, 0.8660254037844387076, 1.000000000000000000, 0.8660254037844387076, 1.000000000000000000, 0.8660254037844387076, 1.000000000000000000, 0.8660254037844387076, 1.000000000000000000, 0.8660254037844387076, 1.000000000000000000, 0.8660254037844387076, 1.000000000000000000, 0.8660254037844387076, 1.000000000000000000, 0.8660254037844387076, 1.000000000000000000, 0.8660254037844387076, 1.000000000000000000, 0.8660254037844387076, 1.000000000000000000, 0.8660254037844387076, 1.000000000000000000, 0.8660254037844387076, 1.000000000000000000, 0.8660254037844387076, 1.000000000000000000, 0.8660254037844387076, 1.000000000000000000, 0.8660254037844387076, 1.000000000000000000, 0.8660254037844387076, 1.000000000000000000, 0.8660254037844387076, 1.000000000000000000, 0.8660254037844387076, 1.000000000000000000, 0.8660254037844387076, 1.000000000000000000, 0.8660254037844387076, 1.000000000000000000, 0.8660254037844387076, 1.000000000000000000, 0.8660254037844387076, 1.000000000000000000, 0.8660254037844387076, 1.000000000000000000, 0.8660254037844387076, 1.000000000000000000, 0.8660254037844387076, 1.000000000000000000, 0.8660254037844387076, 1.000000000000000000, 0.8660254037844387076, 1.000000000000000000, 0.8660254037844387076, 1.000000000000000000, 0.8660254037844387076, 1.000000000000000000, 0.8660254037844387076, 1.000000000000000000, 0.8660254037844387076, 1.000000000000000000, 0.8660254037844387076, 1.000000000000000000, 0.8660254037844387076, 1.000000000000000000, 0.8660254037844387076, 1.000000000000000000, 0.8660254037844387076, 1.000000000000000000, 0.8660254037844387076, 1.000000000000000000, 0.8660254037844387076, 1.000000000000000000, 0.8660254037844387076, 1.000000000000000000, 0.8660254037844387076, 1.000000000000000000, 0.8660254037844387076, 1.000000000000000000, 0.8660254037844387076, 1.000000000000000000, 0.8660254037844387076, 1.000000000000000000, 0.8660254037844387076, 1.000000000000000000, 0.8660254037844387076, 1.000000000000000000, 0.8660254037844387076, 1.000000000000000000, 0.8660254037844387076, 1.000000000000000000, 0.8660254037844387076, 1.000000000000000000, 0.8660254037844387076, 1.000000000000000000, 0.8660254037844387076, 1.000000000000000000, 0.8660254037844387076, 1.000000000000000000, 0.8660254037844387076, 1.000000000000000000, 0.8660254037844387076, 1.000000000000000000, 0.8660254037844387076, 1.000000000000000000, 0.8660254037844387076, 1.000000000000000000, 0.8660254037844387076, 1.000000000000000000, 0.8660254037844387076, 1.000000000000000000, 0.8660254037844387076, 1.000000000000000000, 0.8660254037844387076, 1.000000000000000000, 0.8660254037844387076, 1.000000000000000000, 0.8660254037844387076, 1.000000000000000000, 0.8660254037844387076, 1.000000000000000000, 0.8660254037844387076, 1.000000000000000000, 0.8660254037844387076, 1.000000000000000000, 0.8660254037844387076, 1.000000000000000000, 0.8660254037844387076, 1.000000000000000000, 0.8660254037844387076, 1.000000000000000000, 0.8660254037844387076, 1.000000000000000000, 0.8660254037844387076, 1.000000000000000000, 0.8660254037844387076, 1.000000000000000000, 0.8660254037844387076, 1.000000000000000000, 0.8660254037844387076, 1.000000000000000000, 0.8660254037844387076, 1.000000000000000000, 0.8660254037844387076, 1.000000000000000000, 0.8660254037844387076, 1.000000000000000000, 0.8660254037844387076, 1.000000000000000000, 0.8660254037844387076, 1.000000000000000000, 0.8660254037844387076, 1.000000000000000000, 0.8660254037844387076, 1.000000000000000000, 0.8660254037844387076, 1.000000000000000000, 0.8660254037844387076, 1.000000000000000000, 0.8660254037844387076, 1.000000000000000000, 0.8660254037844387076, 1.000000000000000000, 0.8660254037844387076, 1.000000000000000000, 0.8660254037844387076, 1.000000000000000000, 0.8660254037844387076, 1.000000000000000000, 0.8660254037844387076, 1.000000000000000000, 0.8660254037844387076, 1.000000000000000000, 0.8660254037844387076, 1.000000000000000000, 0.8660254037844387076, 1.000000000000000000, 0.8660254037844387076, 1.000000000000000000, 0.8660254037844387076, 1.000000000000000000, 0.8660254037844387076, 1.000000000000000000, 0.8660254037844387076, 1.000000000000000000, 0.8660254037844387076, 1.000000000000000000, 0.8660254037844387076, 1.000000000000000000, 0.8660254037844387076, 1.000000000000000000, 0.8660254037844387076, 1.000000000000000000, 0.8660254037844387076, 1.000000000000000000, 0.8660254037844387076, 1.000000000000000000, 0.8660254037844387076, 1.000000000000000000, 0.8660254037844387076, 1.000000000000000000, 0.8660254037844387076, 1.000000000000000000),
 ( 1.000000000000000000, 0.8660254037844387076, 1.000000000000000000, 0.8660254037844387076, 1.000000000000000000, 0.8660254037844387076, 1.000000000000000000, 0.8660254037844387076, 1.000000000000000000, 0.8660254037844387076, 1.000000000000000000, 0.8660254037844387076, 1.000000000000000000, 0.8660254037844387076, 1.000000000000000000, 0.8660254037844387076, 1.000000000000000000, 0.8660254037844387076, 1.000000000000000000, 0.8660254037844387076, 1.000000000000000000, 0.8660254037844387076, 1.000000000000000000, 0.8660254037844387076, 1.000000000000000000, 0.8660254037844387076, 1.000000000000000000, 0.8660254037844387076, 1.000000000000000000, 0.8660254037844387076, 1.000000000000000000, 0.8660254037844387076, 1.000000000000000000, 0.8660254037844387076, 1.000000000000000000, 0.8660254037844387076, 1.000000000000000000, 0.8660254037844387076, 1.000000000000000000, 0.8660254037844387076, 1.000000000000000000, 0.8660254037844387076, 1.000000000000000000, 0.8660254037844387076, 1.000000000000000000, 0.8660254037844387076, 1.000000000000000000, 0.8660254037844387076, 1.000000000000000000, 0.8660254037844387076, 1.000000000000000000, 0.8660254037844387076, 1.000000000000000000, 0.8660254037844387076, 1.000000000000000000, 0.8660254037844387076, 1.000000000000000000, 0.8660254037844387076, 1.000000000000000000, 0.8660254037844387076, 1.000000000000000000, 0.8660254037844387076, 1.000000000000000000, 0.8660254037844387076, 1.000000000000000000, 0.8660254037844387076, 1.000000000000000000, 0.8660254037844387076, 1.000000000000000000, 0.8660254037844387076, 1.000000000000000000, 0.8660254037844387076, 1.000000000000000000, 0.8660254037844387076, 1.000000000000000000, 0.8660254037844387076, 1.000000000000000000, 0.8660254037844387076, 1.000000000000000000, 0.8660254037844387076, 1.000000000000000000, 0.8660254037844387076, 1.000000000000000000, 0.8660254037844387076, 1.000000000000000000, 0.8660254037844387076, 1.000000000000000000, 0.8660254037844387076, 1.000000000000000000, 0.8660254037844387076, 1.000000000000000000, 0.8660254037844387076, 1.000000000000000000, 0.8660254037844387076, 1.000000000000000000, 0.8660254037844387076, 1.000000000000000000, 0.8660254037844387076, 1.000000000000000000, 0.8660254037844387076, 1.000000000000000000, 0.8660254037844387076, 1.000000000000000000, 0.8660254037844387076, 1.000000000000000000, 0.8660254037844387076, 1.000000000000000000, 0.8660254037844387076, 1.000000000000000000, 0.8660254037844387076, 1.000000000000000000, 0.8660254037844387076, 1.000000000000000000, 0.8660254037844387076, 1.000000000000000000, 0.8660254037844387076, 1.000000000000000000, 0.8660254037844387076, 1.000000000000000000, 0.8660254037844387076, 1.000000000000000000, 0.8660254037844387076, 1.000000000000000000, 0.8660254037844387076, 1.000000000000000000, 0.8660254037844387076, 1.000000000000000000, 0.8660254037844387076, 1.000000000000000000, 0.8660254037844387076, 1.000000000000000000, 0.8660254037844387076, 1.000000000000000000, 0.8660254037844387076, 1.000000000000000000, 0.8660254037844387076, 1.000000000000000000, 0.8660254037844387076, 1.000000000000000000, 0.8660254037844387076, 1.000000000000000000, 0.8660254037844387076, 1.000000000000000000, 0.8660254037844387076, 1.000000000000000000, 0.8660254037844387076, 1.000000000000000000, 0.8660254037844387076, 1.000000000000000000, 0.8660254037844387076, 1.000000000000000000, 0.8660254037844387076, 1.000000000000000000, 0.8660254037844387076, 1.000000000000000000, 0.8660254037844387076, 1.000000000000000000, 0.8660254037844387076, 1.000000000000000000, 0.8660254037844387076, 1.000000000000000000, 0.8660254037844387076, 1.000000000000000000, 0.8660254037844387076, 1.000000000000000000, 0.8660254037844387076, 1.000000000000000000, 0.8660254037844387076, 1.000000000000000000, 0.8660254037844387076, 1.000000000000000000, 0.8660254037844387076, 1.000000000000000000, 0.8660254037844387076, 1.000000000000000000, 0.8660254037844387076, 1.000000000000000000, 0.8660254037844387076, 1.000000000000000000, 0.8660254037844387076, 1.000000000000000000, 0.8660254037844387076, 1.000000000000000000, 0.8660254037844387076, 1.000000000000000000, 0.8660254037844387076, 1.000000000000000000, 0.8660254037844387076, 1.000000000000000000, 0.8660254037844387076, 1.000000000000000000, 0.8660254037844387076, 1.000000000000000000, 0.8660254037844387076, 1.000000000000000000, 0.8660254037844387076, 1.000000000000000000, 0.8660254037844387076, 1.000000000000000000, 0.8660254037844387076, 1.000000000000000000, 0.8660254037844387076, 1.000000000000000000, 0.8660254037844387076, 1.000000000000000000, 0.8660254037844387076, 1.000000000000000000, 0.8660254037844387076, 1.000000000000000000, 0.8660254037844387076, 1.000000000000000000, 0.8660254037844387076, 1.000000000000000000, 0.8660254037844387076, 1.000000000000000000, 0.8660254037844387076, 1.000000000000000000, 0.8660254037844387076, 1.000000000000000000, 0.8660254037844387076, 1.000000000000000000, 0.8660254037844387076, 1.000000000000000000, 0.8660254037844387076, 1.000000000000000000, 0.8660254037844387076, 1.000000000000000000, 0.8660254037844387076, 1.000000000000000000, 0.8660254037844387076, 1.000000000000000000, 0.8660254037844387076, 1.000000000000000000, 0.8660254037844387076, 1.000000000000000000, 0.8660254037844387076, 1.000000000000000000, 0.8660254037844387076, 1.000000000000000000, 0.8660254037844387076, 1.000000000000000000, 0.8660254037844387076, 1.000000000000000000, 0.8660254037844387076, 1.000000000000000000, 0.8660254037844387076, 1.000000000000000000, 0.8660254037844387076, 1.000000000000000000, 0.8660254037844387076, 1.000000000000000000, 0.8660254037844387076, 1.000000000000000000, 0.8660254037844387076, 1.000000000000000000, 0.8660254037844387076, 1.000000000000000000, 0.8660254037844387076, 1.000000000000000000, 0.8660254037844387076, 1.000000000000000000, 0.8660254037844387076, 1.000000000000000000, 0.8660254037844387076, 1.000000000000000000, 0.8660254037844387076, 1.000000000000000000, 0.8660254037844387076, 1.000000000000000000, 0.8660254037844387076, 1.000000000000000000, 0.8660254037844387076, 1.000000000000000000, 0.8660254037844387076, 1.000000000000000000, 0.8660254037844387076, 1.000000000000000000, 0.8660254037844387076, 1.000000000000000000, 0.8660254037844387076, 1.000000000000000000, 0.8660254037844387076, 1.000000000000000000, 0.8660254037844387076, 1.000000000000000000, 0.8660254037844387076, 1.000000000000000000, 0.8660254037844387076, 1.000000000000000000, 0.8660254037844387076, 1.000000000000000000, 0.8660254037844387076, 1.000000000000000000, 0.8660254037844387076, 1.000000000000000000, 0.8660254037844387076, 1.000000000000000000, 0.8660254037844387076, 1.000000000000000000, 0.8660254037844387076, 1.000000000000000000, 0.8660254037844387076, 1.000000000000000000, 0.8660254037844387076, 1.000000000000000000, 0.8660254037844387076, 1.000000000000000000, 0.8660254037844387076, 1.000000000000000000, 0.8660254037844387076, 1.000000000000000000, 0.8660254037844387076, 1.000000000000000000, 0.8660254037844387076, 1.000000000000000000, 0.8660254037844387076, 1.000000000000000000, 0.8660254037844387076, 1.000000000000000000, 0.8660254037844387076, 1.000000000000000000, 0.8660254037844387076, 1.000000000000000000, 0.8660254037844387076, 1.000000000000000000, 0.8660254037844387076, 1.000000000000000000, 0.8660254037844387076, 1.000000000000000000, 0.8660254037844387076, 1.000000000000000000, 0.8660254037844387076, 1.000000000000000000, 0.8660254037844387076, 1.000000000000000000, 0.8660254037844387076, 1.000000000000000000, 0.8660254037844387076, 1.000000000000000000, 0.8660254037844387076, 1.000000000000000000, 0.8660254037844387076, 1.000000000000000000, 0.8660254037844387076, 1.000000000000000000, 0.8660254037844387076, 1.000000000000000000, 0.8660254037844387076, 1.000000000000000000, 0.8660254037844387076, 1.000000000000000000, 0.8660254037844387076, 1.000000000000000000, 0.8660254037844387076, 1.000000000000000000, 0.8660254037844387076, 1.000000000000000000, 0.8660254037844387076, 1.000000000000000000, 0.8660254037844387076, 1.000000000000000000, 0.8660254037844387076, 1.000000000000000000, 0.8660254037844387076, 1.000000000000000000, 0.8660254037844387076, 1.000000000000000000, 0.8660254037844387076, 1.000000000000000000, 0.8660254037844387076, 1.000000000000000000, 0.8660254037844387076, 1.000000000000000000, 0.8660254037844387076, 1.000000000000000000, 0.8660254037844387076, 1.000000000000000000, 0.8660254037844387076, 1.000000000000000000, 0.8660254037844387076, 1.000000000000000000, 0.8660254037844387076, 1.000000000000000000, 0.8660254037844387076, 1.000000000000000000, 0.8660254037844387076, 1.000000000000000000, 0.8660254037844387076, 1.000000000000000000, 0.8660254037844387076, 1.000000000000000000, 0.8660254037844387076, 1.000000000000000000, 0.8660254037844387076, 1.000000000000000000, 0.8660254037844387076, 1.000000000000000000, 0.8660254037844387076, 1.000000000000000000, 0.8660254037844387076, 1.000000000000000000, 0.8660254037844387076, 1.000000000000000000, 0.8660254037844387076, 1.000000000000000000, 0.8660254037844387076, 1.000000000000000000, 0.8660254037844387076, 1.000000000000000000, 0.8660254037844387076, 1.000000000000000000, 0.8660254037844387076, 1.000000000000000000, 0.8660254037844387076, 1.000000000000000000, 0.8660254037844387076, 1.000000000000000000, 0.8660254037844387076, 1.000000000000000000, 0.8660254037844387076, 1.000000000000000000, 0.8660254037844387076, 1.000000000000000000, 0.8660254037844387076, 1.000000000000000000, 0.8660254037844387076, 1.000000000000000000, 0.8660254037844387076, 1.000000000000000000, 0.8660254037844387076, 1.000000000000000000, 0.8660254037844387076, 1.000000000000000000, 0.8660254037844387076, 1.000000000000000000, 0.8660254037844387076, 1.000000000000000000, 0.8660254037844387076, 1.000000000000000000, 0.8660254037844387076, 1.000000000000000000, 0.8660254037844387076, 1.000000000000000000, 0.8660254037844387076, 1.000000000000000000, 0.8660254037844387076, 1.000000000000000000, 0.8660254037844387076, 1.000000000000000000, 0.8660254037844387076, 1.000000000000000000, 0.8660254037844387076, 1.000000000000000000, 0.8660254037844387076, 1.000000000000000000, 0.8660254037844387076, 1.000000000000000000, 0.8660254037844387076, 1.000000000000000000, 0.8660254037844387076, 1.000000000000000000, 0.8660254037844387076, 1.000000000000000000, 0.8660254037844387076, 1.000000000000000000, 0.8660254037844387076, 1.000000000000000000, 0.8660254037844387076, 1.000000000000000000, 0.8660254037844387076, 1.000000000000000000, 0.8660254037844387076, 1.000000000000000000, 0.8660254037844387076, 1.000000000000000000, 0.8660254037844387076, 1.000000000000000000, 0.8660254037844387076, 1.000000000000000000, 0.8660254037844387076, 1.000000000000000000, 0.8660254037844387076, 1.000000000000000000, 0.8660254037844387076, 1.000000000000000000, 0.8660254037844387076, 1.000000000000000000, 0.8660254037844387076, 1.000000000000000000, 0.8660254037844387076, 1.000000000000000000, 0.8660254037844387076, 1.000000000000000000, 0.8660254037844387076, 1.000000000000000000, 0.8660254037844387076, 1.000000000000000000, 0.8660254037844387076, 1.000000000000000000, 0.8660254037844387076, 1.000000000000000000, 0.8660254037844387076, 1.000000000000000000, 0.8660254037844387076, 1.000000000000000000, 0.8660254037844387076, 1.000000000000000000, 0.8660254037844387076, 1.000000000000000000, 0.8660254037844387076, 1.000000000000000000, 0.8660254037844387076, 1.000000000000000000, 0.8660254037844387076, 1.000000000000000000, 0.8660254037844387076, 1.000000000000000000, 0.8660254037844387076, 1.000000000000000000, 0.8660254037844387076, 1.000000000000000000, 0.8660254037844387076, 1.000000000000000000, 0.8660254037844387076, 1.000000000000000000, 0.8660254037844387076, 1.000000000000000000, 0.8660254037844387076, 1.000000000000000000, 0.8660254037844387076, 1.000000000000000000, 0.8660254037844387076, 1.000000000000000000, 0.8660254037844387076, 1.000000000000000000, 0.8660254037844387076, 1.000000000000000000, 0.8660254037844387076, 1.000000000000000000, 0.8660254037844387076, 1.000000000000000000, 0.8660254037844387076, 1.000000000000000000, 0.8660254037844387076, 1.000000000000000000, 0.8660254037844387076, 1.000000000000000000, 0.8660254037844387076, 1.000000000000000000, 0.8660254037844387076, 1.000000000000000000, 0.8660254037844387076, 1.000000000000000000, 0.8660254037844387076, 1.000000000000000000, 0.8660254037844387076, 1.000000000000000000, 0.8660254037844387076, 1.000000000000000000, 0.8660254037844387076, 1.000000000000000000, 0.8660254037844387076, 1.000000000000000000, 0.8660254037844387076, 1.000000000000000000, 0.8660254037844387076, 1.000000000000000000, 0.8660254037844387076, 1.000000000000000000, 0.8660254037844387076, 1.000000000000000000, 0.8660254037844387076, 1.000000000000000000, 0.8660254037844387076, 1.000000000000000000, 0.8660254037844387076, 1.000000000000000000, 0.8660254037844387076, 1.000000000000000000, 0.8660254037844387076, 1.000000000000000000, 0.8660254037844387076, 1.000000000000000000, 0.8660254037844387076, 1.000000000000000000, 0.8660254037844387076, 1.000000000000000000, 0.8660254037844387076, 1.000000000000000000, 0.8660254037844387076, 1.000000000000000000, 0.8660254037844387076, 1.000000000000000000, 0.8660254037844387076, 1.000000000000000000, 0.8660254037844387076, 1.000000000000000000, 0.8660254037844387076, 1.000000000000000000, 0.8660254037844387076, 1.000000000000000000, 0.8660254037844387076, 1.000000000000000000, 0.8660254037844387076, 1.000000000000000000, 0.8660254037844387076, 1.000000000000000000, 0.8660254037844387076, 1.000000000000000000, 0.8660254037844387076, 1.000000000000000000, 0.8660254037844387076, 1.000000000000000000, 0.8660254037844387076, 1.000000000000000000, 0.8660254037844387076, 1.000000000000000000, 0.8660254037844387076, 1.000000000000000000, 0.8660254037844387076, 1.000000000000000000, 0.8660254037844387076, 1.000000000000000000, 0.8660254037844387076, 1.000000000000000000, 0.8660254037844387076, 1.000000000000000000, 0.8660254037844387076, 1.000000000000000000, 0.8660254037844387076, 1.000000000000000000, 0.8660254037844387076, 1.000000000000000000, 0.8660254037844387076, 1.000000000000000000, 0.8660254037844387076, 1.000000000000000000, 0.8660254037844387076, 1.000000000000000000, 0.8660254037844387076, 1.000000000000000000, 0.8660254037844387076, 1.000000000000000000, 0.8660254037844387076, 1.000000000000000000, 0.8660254037844387076, 1.000000000000000000, 0.8660254037844387076, 1.000000000000000000, 0.8660254037844387076, 1.000000000000000000, 0.8660254037844387076, 1.000000000000000000, 0.8660254037844387076, 1.000000000000000000, 0.8660254037844387076, 1.000000000000000000, 0.8660254037844387076, 1.000000000000000000, 0.8660254037844387076, 1.000000000000000000, 0.8660254037844387076, 1.000000000000000000, 0.8660254037844387076, 1.000000000000000000, 0.8660254037844387076, 1.000000000000000000, 0.8660254037844387076, 1.000000000000000000, 0.8660254037844387076, 1.000000000000000000, 0.8660254037844387076, 1.000000000000000000, 0.8660254037844387076, 1.000000000000000000, 0.8660254037844387076, 1.000000000000000000, 0.8660254037844387076, 1.000000000000000000, 0.8660254037844387076, 1.000000000000000000, 0.8660254037844387076, 1.000000000000000000, 0.8660254037844387076, 1.000000000000000000, 0.8660254037844387076, 1.000000000000000000, 0.8660254037844387076, 1.000000000000000000, 0.8660254037844387076, 1.000000000000000000, 0.8660254037844387076, 1.000000000000000000, 0.8660254037844387076, 1.000000000000000000, 0.8660254037844387076, 1.000000000000000000, 0.8660254037844387076, 1.000000000000000000, 0.8660254037844387076, 1.000000000000000000, 0.8660254037844387076, 1.000000000000000000, 0.8660254037844387076, 1.000000000000000000, 0.8660254037844387076, 1.000000000000000000, 0.8660254037844387076, 1.000000000000000000, 0.8660254037844387076, 1.000000000000000000, 0.8660254037844387076, 1.000000000000000000, 0.8660254037844387076, 1.000000000000000000, 0.8660254037844387076, 1.000000000000000000, 0.8660254037844387076, 1.000000000000000000, 0.8660254037844387076, 1.000000000000000000, 0.8660254037844387076, 1.000000000000000000, 0.8660254037844387076, 1.000000000000000000, 0.8660254037844387076, 1.000000000000000000, 0.8660254037844387076, 1.000000000000000000, 0.8660254037844387076, 1.000000000000000000, 0.8660254037844387076, 1.000000000000000000, 0.8660254037844387076, 1.000000000000000000, 0.8660254037844387076, 1.000000000000000000, 0.8660254037844387076, 1.000000000000000000, 0.8660254037844387076, 1.000000000000000000, 0.8660254037844387076, 1.000000000000000000, 0.8660254037844387076, 1.000000000000000000, 0.8660254037844387076, 1.000000000000000000, 0.8660254037844387076, 1.000000000000000000, 0.8660254037844387076, 1.000000000000000000, 0.8660254037844387076, 1.000000000000000000, 0.8660254037844387076, 1.000000000000000000, 0.8660254037844387076, 1.000000000000000000, 0.8660254037844387076, 1.000000000000000000, 0.8660254037844387076, 1.000000000000000000, 0.8660254037844387076, 1.000000000000000000, 0.8660254037844387076, 1.000000000000000000, 0.8660254037844387076, 1.000000000000000000, 0.8660254037844387076, 1.000000000000000000, 0.8660254037844387076, 1.000000000000000000, 0.8660254037844387076, 1.000000000000000000, 0.8660254037844387076, 1.000000000000000000, 0.8660254037844387076, 1.000000000000000000, 0.8660254037844387076, 1.000000000000000000, 0.8660254037844387076, 1.000000000000000000, 0.8660254037844387076, 1.000000000000000000, 0.8660254037844387076, 1.000000000000000000, 0.8660254037844387076, 1.000000000000000000, 0.8660254037844387076, 1.000000000000000000, 0.8660254037844387076, 1.000000000000000000, 0.8660254037844387076, 1.000000000000000000, 0.8660254037844387076, 1.000000000000000000, 0.8660254037844387076, 1.000000000000000000, 0.8660254037844387076, 1.000000000000000000, 0.8660254037844387076, 1.000000000000000000, 0.8660254037844387076, 1.000000000000000000, 0.8660254037844387076, 1.000000000000000000, 0.8660254037844387076, 1.000000000000000000, 0.8660254037844387076, 1.000000000000000000, 0.8660254037844387076, 1.000000000000000000, 0.8660254037844387076, 1.000000000000000000, 0.8660254037844387076, 1.000000000000000000, 0.8660254037844387076, 1.000000000000000000, 0.8660254037844387076, 1.000000000000000000, 0.8660254037844387076, 1.000000000000000000, 0.8660254037844387076, 1.000000000000000000, 0.8660254037844387076, 1.000000000000000000, 0.8660254037844387076, 1.000000000000000000, 0.8660254037844387076, 1.000000000000000000, 0.8660254037844387076, 1.000000000000000000, 0.8660254037844387076, 1.000000000000000000, 0.8660254037844387076, 1.000000000000000000, 0.8660254037844387076, 1.000000000000000000, 0.8660254037844387076, 1.000000000000000000, 0.8660254037844387076, 1.000000000000000000, 0.8660254037844387076, 1.000000000000000000, 0.8660254037844387076, 1.000000000000000000, 0.8660254037844387076, 1.000000000000000000, 0.8660254037844387076, 1.000000000000000000, 0.8660254037844387076, 1.000000000000000000, 0.8660254037844387076, 1.000000000000000000, 0.8660254037844387076, 1.000000000000000000, 0.8660254037844387076, 1.000000000000000000, 0.8660254037844387076, 1.000000000000000000, 0.8660254037844387076, 1.000000000000000000, 0.8660254037844387076, 1.000000000000000000, 0.8660254037844387076, 1.000000000000000000, 0.8660254037844387076, 1.000000000000000000, 0.8660254037844387076, 1.000000000000000000, 0.8660254037844387076, 1.000000000000000000, 0.8660254037844387076, 1.000000000000000000, 0.8660254037844387076, 1.000000000000000000, 0.8660254037844387076, 1.000000000000000000, 0.8660254037844387076, 1.000000000000000000, 0.8660254037844387076, 1.000000000000000000, 0.8660254037844387076, 1.000000000000000000, 0.8660254037844387076, 1.000000000000000000, 0.8660254037844387076, 1.000000000000000000, 0.8660254037844387076, 1.000000000000000000, 0.8660254037844387076, 1.000000000000000000, 0.8660254037844387076, 1.000000000000000000, 0.8660254037844387076, 1.000000000000000000, 0.8660254037844387076, 1.000000000000000000, 0.8660254037844387076, 1.000000000000000000, 0.8660254037844387076, 1.000000000000000000, 0.8660254037844387076, 1.000000000000000000, 0.8660254037844387076, 1.000000000000000000, 0.8660254037844387076, 1.000000000000000000, 0.8660254037844387076, 1.000000000000000000, 0.8660254037844387076, 1.000000000000000000, 0.8660254037844387076, 1.000000000000000000, 0.8660254037844387076, 1.000000000000000000, 0.8660254037844387076, 1.000000000000000000, 0.8660254037844387076, 1.000000000000000000, 0.8660254037844387076, 1.000000000000000000, 0.8660254037844387076, 1.000000000000000000, 0.8660254037844387076, 1.000000000000000000, 0.8660254037844387076, 1.000000000000000000, 0.8660254037844387076, 1.000000000000000000, 0.8660254037844387076, 1.000000000000000000, 0.8660254037844387076, 1.000000000000000000, 0.8660254037844387076, 1.000000000000000000, 0.8660254037844387076, 1.000000000000000000, 0.8660254037844387076, 1.000000000000000000, 0.8660254037844387076, 1.000000000000000000, 0.8660254037844387076, 1.000000000000000000, 0.8660254037844387076, 1.000000000000000000, 0.8660254037844387076, 1.000000000000000000, 0.8660254037844387076, 1.000000000000000000, 0.8660254037844387076, 1.000000000000000000, 0.8660254037844387076, 1.000000000000000000, 0.8660254037844387076, 1.000000000000000000, 0.8660254037844387076, 1.000000000000000000, 0.8660254037844387076, 1.000000000000000000, 0.8660254037844387076, 1.000000000000000000, 0.8660254037844387076, 1.000000000000000000, 0.8660254037844387076, 1.000000000000000000, 0.8660254037844387076, 1.000000000000000000, 0.8660254037844387076, 1.000000000000000000, 0.8660254037844387076, 1.000000000000000000, 0.8660254037844387076, 1.000000000000000000, 0.8660254037844387076, 1.000000000000000000, 0.8660254037844387076, 1.000000000000000000, 0.8660254037844387076, 1.000000000000000000, 0.8660254037844387076, 1.000000000000000000, 0.8660254037844387076, 1.000000000000000000, 0.8660254037844387076, 1.000000000000000000, 0.8660254037844387076, 1.000000000000000000, 0.8660254037844387076, 1.000000000000000000, 0.8660254037844387076, 1.000000000000000000, 0.8660254037844387076, 1.000000000000000000, 0.8660254037844387076, 1.000000000000000000, 0.8660254037844387076, 1.000000000000000000, 0.8660254037844387076, 1.000000000000000000, 0.8660254037844387076, 1.000000000000000000, 0.8660254037844387076, 1.000000000000000000, 0.8660254037844387076, 1.000000000000000000, 0.8660254037844387076, 1.000000000000000000, 0.8660254037844387076, 1.000000000000000000, 0.8660254037844387076, 1.000000000000000000, 0.8660254037844387076, 1.000000000000000000, 0.8660254037844387076, 1.000000000000000000, 0.8660254037844387076, 1.000000000000000000, 0.8660254037844387076, 1.000000000000000000, 0.8660254037844387076, 1.000000000000000000, 0.8660254037844387076, 1.000000000000000000, 0.8660254037844387076, 1.000000000000000000, 0.8660254037844387076, 1.000000000000000000, 0.8660254037844387076, 1.000000000000000000, 0.8660254037844387076, 1.000000000000000000, 0.8660254037844387076, 1.000000000000000000, 0.8660254037844387076, 1.000000000000000000, 0.8660254037844387076, 1.000000000000000000, 0.8660254037844387076, 1.000000000000000000, 0.8660254037844387076, 1.000000000000000000, 0.8660254037844387076, 1.000000000000000000, 0.8660254037844387076, 1.000000000000000000, 0.8660254037844387076, 1.000000000000000000, 0.8660254037844387076, 1.000000000000000000, 0.8660254037844387076, 1.000000000000000000, 0.8660254037844387076, 1.000000000000000000, 0.8660254037844387076, 1.000000000000000000, 0.8660254037844387076, 1.000000000000000000, 0.8660254037844387076, 1.000000000000000000, 0.8660254037844387076, 1.000000000000000000, 0.8660254037844387076, 1.000000000000000000, 0.8660254037844387076, 1.000000000000000000, 0.8660254037844387076, 1.000000000000000000, 0.8660254037844387076, 1.000000000000000000, 0.8660254037844387076, 1.000000000000000000, 0.8660254037844387076, 1.000000000000000000, 0.8660254037844387076, 1.000000000000000000, 0.8660254037844387076, 1.000000000000000000, 0.8660254037844387076, 1.000000000000000000, 0.8660254037844387076, 1.000000000000000000, 0.8660254037844387076, 1.000000000000000000, 0.8660254037844387076, 1.000000000000000000, 0.8660254037844387076, 1.000000000000000000, 0.8660254037844387076, 1.000000000000000000, 0.8660254037844387076, 1.000000000000000000, 0.8660254037844387076, 1.000000000000000000, 0.8660254037844387076, 1.000000000000000000, 0.8660254037844387076, 1.000000000000000000, 0.8660254037844387076, 1.000000000000000000, 0.8660254037844387076, 1.000000000000000000, 0.8660254037844387076, 1.000000000000000000, 0.8660254037844387076, 1.000000000000000000, 0.8660254037844387076, 1.000000000000000000, 0.8660254037844387076, 1.000000000000000000, 0.8660254037844387076, 1.000000000000000000, 0.8660254037844387076, 1.000000000000000000, 0.8660254037844387076, 1.000000000000000000, 0.8660254037844387076, 1.000000000000000000, 0.8660254037844387076, 1.000000000000000000, 0.8660254037844387076, 1.000000000000000000, 0.8660254037844387076, 1.000000000000000000, 0.8660254037844387076, 1.000000000000000000, 0.8660254037844387076, 1.000000000000000000, 0.8660254037844387076, 1.000000000000000000, 0.8660254037844387076, 1.000000000000000000, 0.8660254037844387076, 1.000000000000000000, 0.8660254037844387076, 1.000000000000000000, 0.8660254037844387076, 1.000000000000000000, 0.8660254037844387076, 1.000000000000000000, 0.8660254037844387076, 1.000000000000000000, 0.8660254037844387076, 1.000000000000000000, 0.8660254037844387076, 1.000000000000000000, 0.8660254037844387076, 1.000000000000000000, 0.8660254037844387076, 1.000000000000000000, 0.8660254037844387076, 1.000000000000000000, 0.8660254037844387076, 1.000000000000000000, 0.8660254037844387076, 1.000000000000000000, 0.8660254037844387076, 1.000000000000000000, 0.8660254037844387076, 1.000000000000000000, 0.8660254037844387076, 1.000000000000000000, 0.8660254037844387076, 1.000000000000000000, 0.8660254037844387076, 1.000000000000000000, 0.8660254037844387076, 1.000000000000000000, 0.8660254037844387076, 1.000000000000000000, 0.8660254037844387076, 1.000000000000000000, 0.8660254037844387076, 1.000000000000000000, 0.8660254037844387076, 1.000000000000000000, 0.8660254037844387076, 1.000000000000000000, 0.8660254037844387076, 1.000000000000000000, 0.8660254037844387076, 1.000000000000000000, 0.8660254037844387076, 1.000000000000000000, 0.8660254037844387076, 1.000000000000000000, 0.8660254037844387076, 1.000000000000000000, 0.8660254037844387076, 1.000000000000000000, 0.8660254037844387076, 1.000000000000000000, 0.8660254037844387076, 1.000000000000000000, 0.8660254037844387076, 1.000000000000000000, 0.8660254037844387076, 1.000000000000000000, 0.8660254037844387076, 1.000000000000000000, 0.8660254037844387076, 1.000000000000000000, 0.8660254037844387076, 1.000000000000000000, 0.8660254037844387076, 1.000000000000000000, 0.8660254037844387076, 1.000000000000000000, 0.8660254037844387076, 1.000000000000000000, 0.8660254037844387076, 1.000000000000000000, 0.8660254037844387076, 1.000000000000000000, 0.8660254037844387076, 1.000000000000000000, 0.8660254037844387076, 1.000000000000000000, 0.8660254037844387076, 1.000000000000000000, 0.8660254037844387076, 1.000000000000000000, 0.8660254037844387076, 1.000000000000000000, 0.8660254037844387076, 1.000000000000000000, 0.8660254037844387076, 1.000000000000000000, 0.8660254037844387076, 1.000000000000000000, 0.8660254037844387076, 1.000000000000000000, 0.8660254037844387076, 1.000000000000000000, 0.8660254037844387076, 1.000000000000000000, 0.8660254037844387076, 1.000000000000000000, 0.8660254037844387076, 1.000000000000000000, 0.8660254037844387076, 1.000000000000000000, 0.8660254037844387076, 1.000000000000000000, 0.8660254037844387076, 1.000000000000000000, 0.8660254037844387076, 1.000000000000000000, 0.8660254037844387076, 1.000000000000000000, 0.8660254037844387076, 1.000000000000000000, 0.8660254037844387076, 1.000000000000000000, 0.8660254037844387076, 1.000000000000000000, 0.8660254037844387076, 1.000000000000000000, 0.8660254037844387076, 1.000000000000000000, 0.8660254037844387076, 1.000000000000000000, 0.8660254037844387076, 1.000000000000000000, 0.8660254037844387076, 1.000000000000000000, 0.8660254037844387076, 1.000000000000000000, 0.8660254037844387076, 1.000000000000000000, 0.8660254037844387076, 1.000000000000000000, 0.8660254037844387076, 1.000000000000000000, 0.8660254037844387076, 1.000000000000000000, 0.8660254037844387076, 1.000000000000000000, 0.8660254037844387076, 1.000000000000000000, 0.8660254037844387076, 1.000000000000000000, 0.8660254037844387076, 1.000000000000000000, 0.8660254037844387076, 1.000000000000000000, 0.8660254037844387076, 1.000000000000000000, 0.8660254037844387076, 1.000000000000000000, 0.8660254037844387076, 1.000000000000000000, 0.8660254037844387076, 1.000000000000000000, 0.8660254037844387076, 1.000000000000000000, 0.8660254037844387076, 1.000000000000000000, 0.8660254037844387076, 1.000000000000000000, 0.8660254037844387076, 1.000000000000000000, 0.8660254037844387076, 1.000000000000000000, 0.8660254037844387076, 1.000000000000000000, 0.8660254037844387076, 1.000000000000000000, 0.8660254037844387076, 1.000000000000000000, 0.8660254037844387076, 1.000000000000000000, 0.8660254037844387076, 1.000000000000000000, 0.8660254037844387076, 1.000000000000000000, 0.8660254037844387076, 1.000000000000000000, 0.8660254037844387076, 1.000000000000000000, 0.8660254037844387076, 1.000000000000000000, 0.8660254037844387076, 1.000000000000000000, 0.8660254037844387076, 1.000000000000000000, 0.8660254037844387076, 1.000000000000000000, 0.8660254037844387076, 1.000000000000000000, 0.8660254037844387076, 1.000000000000000000, 0.8660254037844387076, 1.000000000000000000, 0.8660254037844387076, 1.000000000000000000, 0.8660254037844387076, 1.000000000000000000, 0.8660254037844387076, 1.000000000000000000, 0.8660254037844387076, 1.000000000000000000, 0.8660254037844387076, 1.000000000000000000, 0.8660254037844387076, 1.000000000000000000, 0.8660254037844387076, 1.000000000000000000, 0.8660254037844387076, 1.000000000000000000, 0.8660254037844387076, 1.000000000000000000, 0.8660254037844387076, 1.000000000000000000, 0.8660254037844387076, 1.000000000000000000, 0.8660254037844387076, 1.000000000000000000, 0.8660254037844387076, 1.000000000000000000, 0.8660254037844387076, 1.000000000000000000, 0.8660254037844387076, 1.000000000000000000, 0.8660254037844387076, 1.000000000000000000, 0.8660254037844387076, 1.000000000000000000, 0.8660254037844387076, 1.000000000000000000, 0.8660254037844387076, 1.000000000000000000, 0.8660254037844387076, 1.000000000000000000, 0.8660254037844387076, 1.000000000000000000, 0.8660254037844387076, 1.000000000000000000, 0.8660254037844387076, 1.000000000000000000, 0.8660254037844387076, 1.000000000000000000, 0.8660254037844387076, 1.000000000000000000, 0.8660254037844387076, 1.000000000000000000, 0.8660254037844387076, 1.000000000000000000, 0.8660254037844387076, 1.000000000000000000, 0.8660254037844387076, 1.000000000000000000, 0.8660254037844387076, 1.000000000000000000, 0.8660254037844387076, 1.000000000000000000, 0.8660254037844387076, 1.000000000000000000, 0.8660254037844387076, 1.000000000000000000, 0.8660254037844387076, 1.000000000000000000, 0.8660254037844387076, 1.000000000000000000, 0.8660254037844387076, 1.000000000000000000, 0.8660254037844387076, 1.000000000000000000, 0.8660254037844387076, 1.000000000000000000, 0.8660254037844387076, 1.000000000000000000, 0.8660254037844387076, 1.000000000000000000, 0.8660254037844387076, 1.000000000000000000, 0.8660254037844387076, 1.000000000000000000, 0.8660254037844387076, 1.000000000000000000, 0.8660254037844387076, 1.000000000000000000, 0.8660254037844387076, 1.000000000000000000, 0.8660254037844387076, 1.000000000000000000, 0.8660254037844387076, 1.000000000000000000, 0.8660254037844387076, 1.000000000000000000, 0.8660254037844387076, 1.000000000000000000, 0.8660254037844387076, 1.000000000000000000, 0.8660254037844387076, 1.000000000000000000, 0.8660254037844387076, 1.000000000000000000, 0.8660254037844387076, 1.000000000000000000, 0.8660254037844387076, 1.000000000000000000) ) ) 
 REPRESENTATION_ITEM ( '' )  SURFACE ( )  );
#50563 = DIRECTION ( 'NONE',  ( -0.000000000000000000, 1.000000000000000000, -0.000000000000000000 ) ) ;
#50564 = CARTESIAN_POINT ( 'NONE',  ( 2.229367062499998831, -61.89583333196774362, -3.861377020970580887 ) ) ;
#50565 = CARTESIAN_POINT ( 'NONE',  ( 4.458734125000001214, -5.145833331967740065, 2.574251347313718519 ) ) ;
#50566 = VERTEX_POINT ( 'NONE', #12132 ) ;
#50567 = CARTESIAN_POINT ( 'NONE',  ( -6.972266317189433020E-16, -59.12499999726880873, -5.000000000000000000 ) ) ;
#50568 = CARTESIAN_POINT ( 'NONE',  ( -1.339745962155613812, 2.919658201469706782, -5.000000000000000000 ) ) ;
#50569 = ORIENTED_EDGE ( 'NONE', *, *, #60987, .F. ) ;
#50570 = DIRECTION ( 'NONE',  ( 0.8660254037844410391, -0.4999999999999958367, -0.000000000000000000 ) ) ;
#50571 = CARTESIAN_POINT ( 'NONE',  ( -4.458734124999998549, 5.770833334698927786, 2.574251347313722516 ) ) ;
#50572 = CARTESIAN_POINT ( 'NONE',  ( -2.499999999999996447, -75.83333333333334281, 4.330127018922195425 ) ) ;
#50573 = CARTESIAN_POINT ( 'NONE',  ( 1.846868145590735200, -159.2500000013656063, -4.458734124999999437 ) ) ;
#50574 = CARTESIAN_POINT ( 'NONE',  ( 1.975475456537005874E-15, -105.7500000000000000, 5.000000000000000000 ) ) ;
#50575 = VERTEX_POINT ( 'NONE', #23297 ) ;
#50576 = CARTESIAN_POINT ( 'NONE',  ( -2.229367062499996610, -79.14583333196773651, 3.861377020970582219 ) ) ;
#50577 = CARTESIAN_POINT ( 'NONE',  ( 2.500000000000002220, -29.54166666393548013, 4.330127018922192761 ) ) ;
#50578 = CARTESIAN_POINT ( 'NONE',  ( 4.458734124999998549, -2.729166665301069550, -2.574251347313721627 ) ) ;
#50579 = CARTESIAN_POINT ( 'NONE',  ( 2.500000000000002220, 25.45833333606451987, 4.330127018922192761 ) ) ;
#50580 = DIRECTION ( 'NONE',  ( -0.000000000000000000, 1.000000000000000000, -0.000000000000000000 ) ) ;
#50581 = CARTESIAN_POINT ( 'NONE',  ( 4.458734124999998549, -69.97916666530107932, -2.574251347313721627 ) ) ;
#50582 = CARTESIAN_POINT ( 'NONE',  ( -5.000000000000000000, -29.95833333060214088, -2.886751345948128211 ) ) ;
#50583 = CARTESIAN_POINT ( 'NONE',  ( -2.500000000000000444, 5.833333333333333037, -4.330127018922193649 ) ) ;
#50584 = CARTESIAN_POINT ( 'NONE',  ( -5.000000000000000000, -0.8749999972688139449, 0.000000000000000000 ) ) ;
#50585 = CARTESIAN_POINT ( 'NONE',  ( 1.975475456537005874E-15, -104.7500000000000000, 5.000000000000000000 ) ) ;
#50586 = CARTESIAN_POINT ( 'NONE',  ( -6.972266317189433020E-16, -82.12499999726881583, -5.000000000000000000 ) ) ;
#50587 = CARTESIAN_POINT ( 'NONE',  ( 9.457646018065525792E-16, -52.06249999863440792, 5.148502694627439702 ) ) ;
#50588 = CARTESIAN_POINT ( 'NONE',  ( -3.152548672688508926E-16, -35.81249999863440792, -5.148502694627439702 ) ) ;
#50589 = CARTESIAN_POINT ( 'NONE',  ( -4.458734124999997661, 0.5208333346989266754, 2.574251347313722516 ) ) ;
#50590 = CARTESIAN_POINT ( 'NONE',  ( -4.999999999999998224, 9.208333336064519870, 2.886751345948131764 ) ) ;
#50591 = CARTESIAN_POINT ( 'NONE',  ( -5.000000000000000000, 22.91666666666666430, -2.886751345948128211 ) ) ;
#50592 = CARTESIAN_POINT ( 'NONE',  ( 5.000000000000000000, -147.1250000027312126, 0.000000000000000000 ) ) ;
#50593 = CARTESIAN_POINT ( 'NONE',  ( 5.000000000000000000, -26.37499999726881583, -6.123233995736766282E-16 ) ) ;
#50594 = CARTESIAN_POINT ( 'NONE',  ( 2.229367062500001939, -41.97916666530107932, 3.861377020970579999 ) ) ;
#50595 = CARTESIAN_POINT ( 'NONE',  ( -2.499999999999996447, -77.70833333060214443, 4.330127018922195425 ) ) ;
#50596 = CARTESIAN_POINT ( 'NONE',  ( -56.48576386720575471, -139.0000000013655779, -4.591703134518078322 ) ) ;
#50597 = CARTESIAN_POINT ( 'NONE',  ( -3.535533905932738641, -140.3750000000000000, 3.535533905932737309 ) ) ;
#50598 = CARTESIAN_POINT ( 'NONE',  ( -3.152548672688508926E-16, -80.81249999863440792, -5.148502694627439702 ) ) ;
#50599 = CARTESIAN_POINT ( 'NONE',  ( -1.846868145590737420, -161.0000000013656063, 4.458734124999997661 ) ) ;
#50600 = CARTESIAN_POINT ( 'NONE',  ( -2.071067811865372921, -159.4375000027312410, 5.000000000000104805 ) ) ;
#50601 = CARTESIAN_POINT ( 'NONE',  ( 1.060575238724906964E-15, -26.74999999999999645, 5.773502691896257311 ) ) ;
#50602 = CARTESIAN_POINT ( 'NONE',  ( -1.339745962155610925, -90.66965819600733312, 5.000000000000000000 ) ) ;
#50603 = EDGE_LOOP ( 'NONE', ( #58628, #31036, #9976, #43340 ) ) ;
#50604 = CARTESIAN_POINT ( 'NONE',  ( 2.229367062500001939, 23.77083333469892779, 3.861377020970579999 ) ) ;
#50605 = ORIENTED_EDGE ( 'NONE', *, *, #30207, .T. ) ;
#50606 = CARTESIAN_POINT ( 'NONE',  ( 2.229367062499998831, 13.10416666803226171, -3.861377020970580887 ) ) ;
#50607 = CARTESIAN_POINT ( 'NONE',  ( 5.000000000000000000, 17.62500000273118417, -6.123233995736766282E-16 ) ) ;
#50608 =( BOUNDED_CURVE ( )  B_SPLINE_CURVE ( 2, ( #14884, #49937, #29039, #43518, #15542, #10064, #5565, #20365, #14565 ),
 .UNSPECIFIED., .F., .F. ) 
 B_SPLINE_CURVE_WITH_KNOTS ( ( 3, 2, 2, 2, 3 ),
 ( 0.5160714285714286254, 0.5166666666666667185, 0.5178571428571429047, 0.5190476190476190910, 0.5196428571428571841 ),
 .UNSPECIFIED. ) 
 CURVE ( )  GEOMETRIC_REPRESENTATION_ITEM ( )  RATIONAL_B_SPLINE_CURVE ( ( 0.9330127018922194093, 0.9330127018922256266, 1.000000000000000000, 0.8660254037844387076, 1.000000000000000000, 0.8660254037844387076, 1.000000000000000000, 0.9330127018922194093, 0.9330127018922194093 ) ) 
 REPRESENTATION_ITEM ( '' )  );
#50609 = CARTESIAN_POINT ( 'NONE',  ( 5.000000000000000000, 2.499999999999998668, -6.123233995736766282E-16 ) ) ;
#50610 = CARTESIAN_POINT ( 'NONE',  ( 2.499999999999998668, 14.66666666666666607, -4.330127018922193649 ) ) ;
#50611 = ADVANCED_FACE ( 'NONE', ( #42897 ), #31754, .T. ) ;
#50612 = CARTESIAN_POINT ( 'NONE',  ( 4.458734124999999437, -52.81249999863440792, -5.460374474430324690E-16 ) ) ;
#50613 = CARTESIAN_POINT ( 'NONE',  ( -3.152548672688508926E-16, -12.56249999863440081, -5.148502694627439702 ) ) ;
#50614 = CARTESIAN_POINT ( 'NONE',  ( 7.500000000000000000, 3.160172554975063886, -7.231829826456836585 ) ) ;
#50615 = CARTESIAN_POINT ( 'NONE',  ( 1.975475456537005874E-15, -51.75000000000000000, 5.000000000000000000 ) ) ;
#50616 = CARTESIAN_POINT ( 'NONE',  ( 5.000000000000000888, 15.54166666939785202, 2.886751345948126879 ) ) ;
#50617 = CARTESIAN_POINT ( 'NONE',  ( 5.000000000000000000, -1.416666666666663410, -2.886751345948130876 ) ) ;
#50618 = CARTESIAN_POINT ( 'NONE',  ( 0.000000000000000000, -170.0000000000000000, 0.000000000000000000 ) ) ;
#50619 = CARTESIAN_POINT ( 'NONE',  ( -3.535250795749689387E-16, -34.25000000000000711, -5.773502691896257311 ) ) ;
#50620 = CARTESIAN_POINT ( 'NONE',  ( 2.500000000000002220, -74.66666666666665719, 4.330127018922192761 ) ) ;
#50622 = CARTESIAN_POINT ( 'NONE',  ( -3.152548672688508926E-16, -12.81249999863440259, -5.148502694627439702 ) ) ;
#50621 = CARTESIAN_POINT ( 'NONE',  ( -59.81910112700025905, -151.1875000000000000, -2.462841084822570359 ) ) ;
#50623 = CARTESIAN_POINT ( 'NONE',  ( -5.000000000000000000, -140.6250000027312126, -6.123233995736766282E-16 ) ) ;
#50624 = CARTESIAN_POINT ( 'NONE',  ( 2.229367062499998831, -61.64583333196774362, -3.861377020970580887 ) ) ;
#50625 = CARTESIAN_POINT ( 'NONE',  ( 1.846868145590736310, -150.8750000013655779, 4.458734124999999437 ) ) ;
#50626 = MANIFOLD_SOLID_BREP ( 'Cut-Extrude1', #12032 ) ;
#50627 = CARTESIAN_POINT ( 'NONE',  ( -2.229367062499996610, -67.14583333196773651, 3.861377020970582219 ) ) ;
#50628 = CARTESIAN_POINT ( 'NONE',  ( -52.80376928212989185, -147.1250000013656063, -4.297418129356379346 ) ) ;
#50629 = EDGE_CURVE ( 'NONE', #43493, #28751, #50608, .T. ) ;
#50630 = CARTESIAN_POINT ( 'NONE',  ( -4.999999999999999112, -57.79166666393548013, 2.886751345948131764 ) ) ;
#50631 = ORIENTED_EDGE ( 'NONE', *, *, #33776, .F. ) ;
#50632 = CARTESIAN_POINT ( 'NONE',  ( -49.85088928181150436, -137.5625000000000000, -1.666127454062680480 ) ) ;
#50633 = ORIENTED_EDGE ( 'NONE', *, *, #30288, .T. ) ;
#50635 = CARTESIAN_POINT ( 'NONE',  ( 5.000000000000000000, -103.4166666666666430, -2.886751345948130876 ) ) ;
#50634 = CARTESIAN_POINT ( 'NONE',  ( -51.75738570946856498, -141.7500000000000284, 3.805975901505576964 ) ) ;
#50636 = CARTESIAN_POINT ( 'NONE',  ( 1.846868145590735200, -153.2500000013655779, -4.458734125000000326 ) ) ;
#50637 = VERTEX_POINT ( 'NONE', #53809 ) ;
#50638 = CARTESIAN_POINT ( 'NONE',  ( -1.339745962155610925, -9.794658198738520838, 5.000000000000000000 ) ) ;
#50639 = CARTESIAN_POINT ( 'NONE',  ( -59.98410592259440222, -128.1250000000000284, -0.3983568153799752487 ) ) ;
#50640 = FACE_OUTER_BOUND ( 'NONE', #56179, .T. ) ;
#50641 = CARTESIAN_POINT ( 'NONE',  ( 9.457646018065525792E-16, -48.31249999863440081, 5.148502694627439702 ) ) ;
#50642 = ORIENTED_EDGE ( 'NONE', *, *, #60597, .F. ) ;
#50643 = DIRECTION ( 'NONE',  ( -0.000000000000000000, -1.000000000000000000, -0.000000000000000000 ) ) ;
#50644 = CARTESIAN_POINT ( 'NONE',  ( 4.458734124999998549, 15.27083333469893134, -2.574251347313721627 ) ) ;
#50645 = CARTESIAN_POINT ( 'NONE',  ( 4.458734124999999437, 24.18750000136559564, -5.460374474430324690E-16 ) ) ;
#50646 = CARTESIAN_POINT ( 'NONE',  ( -56.48576386720575471, -153.7500000013656063, -4.591703134518078322 ) ) ;
#50647 = CARTESIAN_POINT ( 'NONE',  ( 1.339745962155615144, -77.70534180126146850, 4.999999999999999112 ) ) ;
#50648 = CARTESIAN_POINT ( 'NONE',  ( 1.339745962155557191, -25.70534180126148271, 5.000000000000032863 ) ) ;
#50649 = ORIENTED_EDGE ( 'NONE', *, *, #57478, .F. ) ;
#50650 = CARTESIAN_POINT ( 'NONE',  ( -2.229367062499996610, -63.14583333196774362, 3.861377020970582219 ) ) ;
#50651 = CARTESIAN_POINT ( 'NONE',  ( 1.339745962155661996, -28.16965819600733312, -4.999999999999970690 ) ) ;
#50652 = CARTESIAN_POINT ( 'NONE',  ( 4.458734124999999437, 13.18750000136559208, -5.460374474430324690E-16 ) ) ;
#50653 = CARTESIAN_POINT ( 'NONE',  ( 5.000000000000000000, 7.625000002731186832, -6.123233995736766282E-16 ) ) ;
#50654 = CARTESIAN_POINT ( 'NONE',  ( -5.000000000000000000, -1.874999997268814944, 0.000000000000000000 ) ) ;
#50655 = CARTESIAN_POINT ( 'NONE',  ( 2.229367062500001939, -54.22916666530107221, 3.861377020970579999 ) ) ;
#50656 = CARTESIAN_POINT ( 'NONE',  ( 2.500000000000002220, -15.54166666393548191, 4.330127018922192761 ) ) ;
#50657 = DIRECTION ( 'NONE',  ( -0.000000000000000000, 1.000000000000000000, -0.000000000000000000 ) ) ;
#50658 = CARTESIAN_POINT ( 'NONE',  ( 7.500000000000000000, -1.486698507076798847, -0.09861472150523931113 ) ) ;
#50659 = CARTESIAN_POINT ( 'NONE',  ( -6.972266317189433020E-16, -64.12499999726880162, -5.000000000000000000 ) ) ;
#50660 = CARTESIAN_POINT ( 'NONE',  ( 4.458734125000000326, -17.14583333196773651, 2.574251347313718519 ) ) ;
#50661 = EDGE_LOOP ( 'NONE', ( #63534, #21702, #61723, #27607 ) ) ;
#50662 = DIRECTION ( 'NONE',  ( 0.8660254037844384856, 0.000000000000000000, -0.5000000000000002220 ) ) ;
#50663 = CARTESIAN_POINT ( 'NONE',  ( -4.458734124999999437, -103.3958333319677365, -2.574251347313719407 ) ) ;
#50664 = CARTESIAN_POINT ( 'NONE',  ( -5.000000000000000888, -155.5625000027311842, 2.071067811865474617 ) ) ;
#50665 = ORIENTED_EDGE ( 'NONE', *, *, #6773, .F. ) ;
#50666 = CARTESIAN_POINT ( 'NONE',  ( 2.229367062500001939, -101.2291666653010651, 3.861377020970579999 ) ) ;
#50667 = CARTESIAN_POINT ( 'NONE',  ( -4.458734124999998549, -25.22916666530106866, 2.574251347313722516 ) ) ;
#50668 = CARTESIAN_POINT ( 'NONE',  ( 5.000000000000000888, -60.45833333060213732, 2.886751345948126879 ) ) ;
#50669 = CARTESIAN_POINT ( 'NONE',  ( -52.10840900171896806, -153.4375000013656063, 3.393966926194110556 ) ) ;
#50670 = CARTESIAN_POINT ( 'NONE',  ( -52.80376928212989185, -140.8750000013656063, -4.297418129356378458 ) ) ;
#50671 = CARTESIAN_POINT ( 'NONE',  ( 9.457646018065525792E-16, -22.06249999863440436, 5.148502694627439702 ) ) ;
#50672 = CARTESIAN_POINT ( 'NONE',  ( -2.229367062500000163, -64.72916666530106511, -3.861377020970580443 ) ) ;
#50673 = CARTESIAN_POINT ( 'NONE',  ( 4.458734125000000326, -17.89583333196773651, 2.574251347313718519 ) ) ;
#50674 = DIRECTION ( 'NONE',  ( -0.000000000000000000, 1.000000000000000000, -0.000000000000000000 ) ) ;
#50675 = CARTESIAN_POINT ( 'NONE',  ( 3.535533905932736864, -151.1250000000000000, 3.535533905932738641 ) ) ;
#50676 = CARTESIAN_POINT ( 'NONE',  ( -5.000000000000000000, -10.08333333333333393, -2.886751345948128211 ) ) ;
#50677 = CARTESIAN_POINT ( 'NONE',  ( -8.190561711645485556E-16, -152.6875000013656063, 4.458734124999999437 ) ) ;
#50678 = VERTEX_POINT ( 'NONE', #35162 ) ;
#50679 = CARTESIAN_POINT ( 'NONE',  ( 2.229367062500001939, -46.22916666530106511, 3.861377020970579999 ) ) ;
#50680 = CARTESIAN_POINT ( 'NONE',  ( 5.000000000000000000, 21.70833333606451987, -2.886751345948130876 ) ) ;
#50681 = DIRECTION ( 'NONE',  ( -1.000000000000000000, 0.000000000000000000, -7.709882115452477180E-16 ) ) ;
#50682 = CARTESIAN_POINT ( 'NONE',  ( -4.458734124999999437, -90.31249999863440792, 0.000000000000000000 ) ) ;
#50683 = EDGE_CURVE ( 'NONE', #11557, #3938, #24226, .T. ) ;
#50684 =( BOUNDED_CURVE ( )  B_SPLINE_CURVE ( 2, ( #23977, #59345, #14321, #15277, #34245, #9488, #10131, #43581, #53874 ),
 .UNSPECIFIED., .F., .F. ) 
 B_SPLINE_CURVE_WITH_KNOTS ( ( 3, 2, 2, 2, 3 ),
 ( 0.9482142857142856762, 0.9488095238095237693, 0.9499999999999999556, 0.9511904761904761418, 0.9517857142857142350 ),
 .UNSPECIFIED. ) 
 CURVE ( )  GEOMETRIC_REPRESENTATION_ITEM ( )  RATIONAL_B_SPLINE_CURVE ( ( 0.9330127018922194093, 0.9330127018922194093, 1.000000000000000000, 0.8660254037844387076, 1.000000000000000000, 0.8660254037844387076, 1.000000000000000000, 0.9330127018922194093, 0.9330127018922194093 ) ) 
 REPRESENTATION_ITEM ( '' )  );
#50685 = CARTESIAN_POINT ( 'NONE',  ( -4.458734124999999437, 5.604166668032262599, -2.574251347313719407 ) ) ;
#50686 = CARTESIAN_POINT ( 'NONE',  ( 2.499999999999998668, 1.791666669397853795, -4.330127018922193649 ) ) ;
#50687 = CARTESIAN_POINT ( 'NONE',  ( 1.339745962155615144, 13.29465819873852084, 4.999999999999999112 ) ) ;
#50688 = CARTESIAN_POINT ( 'NONE',  ( 4.330127018922258486, 45.00000000000000000, 7.499999999999910294 ) ) ;
#50689 = CARTESIAN_POINT ( 'NONE',  ( -4.458734124999999437, 14.35416666803226171, -2.574251347313719407 ) ) ;
#50690 = CARTESIAN_POINT ( 'NONE',  ( -5.000000000000000000, -82.00000000000000000, 0.000000000000000000 ) ) ;
#50691 = CARTESIAN_POINT ( 'NONE',  ( 1.060575238724906964E-15, 5.375000002731184168, 5.773502691896257311 ) ) ;
#50692 = ORIENTED_EDGE ( 'NONE', *, *, #31092, .F. ) ;
#50693 = CARTESIAN_POINT ( 'NONE',  ( 3.535533905932736864, -162.2500000027312126, 3.535533905932738641 ) ) ;
#50694 = ORIENTED_EDGE ( 'NONE', *, *, #34461, .T. ) ;
#50695 = CARTESIAN_POINT ( 'NONE',  ( 1.339745962155614256, 27.83034180399267044, -4.999999999999999112 ) ) ;
#50696 = CARTESIAN_POINT ( 'NONE',  ( -2.229367062499996610, -43.14583333196773651, 3.861377020970582219 ) ) ;
#50697 = CARTESIAN_POINT ( 'NONE',  ( 2.730187237215162345E-16, -162.4375000013655779, -4.458734124999999437 ) ) ;
#50698 = EDGE_CURVE ( 'NONE', #62517, #15325, #57200, .T. ) ;
#50699 = CARTESIAN_POINT ( 'NONE',  ( 1.060575238724906964E-15, -37.62499999726881583, 5.773502691896257311 ) ) ;
#50700 = ORIENTED_EDGE ( 'NONE', *, *, #53535, .T. ) ;
#50702 = ADVANCED_FACE ( 'NONE', ( #59280 ), #10709, .F. ) ;
#50701 = CARTESIAN_POINT ( 'NONE',  ( -2.229367062500000163, -18.47916666530106866, -3.861377020970580443 ) ) ;
#50703 = EDGE_LOOP ( 'NONE', ( #25058, #32598, #59261, #13610 ) ) ;
#50704 = CARTESIAN_POINT ( 'NONE',  ( -3.535250795749689387E-16, -85.24999999999998579, -5.773502691896257311 ) ) ;
#50705 = CARTESIAN_POINT ( 'NONE',  ( 3.152801135295366208, -164.5625000013656063, 3.152801135295367985 ) ) ;
#50706 = CARTESIAN_POINT ( 'NONE',  ( -2.499999999999996447, -87.70833333060214443, 4.330127018922195425 ) ) ;
#50708 = ORIENTED_EDGE ( 'NONE', *, *, #1208, .F. ) ;
#50707 = CYLINDRICAL_SURFACE ( 'NONE', #21045, 5.000000000000000000 ) ;
#50709 = CARTESIAN_POINT ( 'NONE',  ( -58.80597590150559739, -143.0000000000000284, 3.242614290531460330 ) ) ;
#50710 = CARTESIAN_POINT ( 'NONE',  ( 9.457646018065525792E-16, -30.31249999863440436, 5.148502694627439702 ) ) ;
#50711 = CARTESIAN_POINT ( 'NONE',  ( -6.972266317189433020E-16, -29.25000000000000000, -5.000000000000000000 ) ) ;
#50712 = VERTEX_POINT ( 'NONE', #29996 ) ;
#50713 = CARTESIAN_POINT ( 'NONE',  ( 4.458734124999999437, -75.81249999863440792, -5.460374474430324690E-16 ) ) ;
#50714 = CARTESIAN_POINT ( 'NONE',  ( -4.458734124999998549, -108.4791666653010793, 2.574251347313722516 ) ) ;
#50715 = CARTESIAN_POINT ( 'NONE',  ( -6.972266317189433020E-16, -15.25000000000000000, -5.000000000000000000 ) ) ;
#50716 = ORIENTED_EDGE ( 'NONE', *, *, #34251, .F. ) ;
#50717 = CARTESIAN_POINT ( 'NONE',  ( -6.972266317189433020E-16, -26.25000000000000000, -5.000000000000000000 ) ) ;
#50718 = CARTESIAN_POINT ( 'NONE',  ( -58.39396692619412477, -143.6875000013656063, 2.891590998281057701 ) ) ;
#50719 = CARTESIAN_POINT ( 'NONE',  ( 2.229367062499998831, -82.89583333196773651, -3.861377020970580887 ) ) ;
#50720 = CARTESIAN_POINT ( 'NONE',  ( -56.66612745406270335, -136.4375000027312126, -5.149110718188516067 ) ) ;
#50721 = CARTESIAN_POINT ( 'NONE',  ( -2.229367062500000163, -42.47916666530107932, -3.861377020970580443 ) ) ;
#50722 = CARTESIAN_POINT ( 'NONE',  ( 4.458734124999997661, -140.7500000013655779, 1.846868145590737864 ) ) ;
#50723 = CARTESIAN_POINT ( 'NONE',  ( 0.000000000000000000, -170.0000000000000000, 5.000000000000000000 ) ) ;
#50724 = CARTESIAN_POINT ( 'NONE',  ( 4.458734125000000326, -47.89583333196774362, 2.574251347313718519 ) ) ;
#50725 = CARTESIAN_POINT ( 'NONE',  ( -2.229367062499996610, -44.14583333196774362, 3.861377020970582219 ) ) ;
#50726 = CARTESIAN_POINT ( 'NONE',  ( -2.498395430326213474E-14, 21.24999999999999289, 5.000000000000000000 ) ) ;
#50727 = EDGE_CURVE ( 'NONE', #54333, #43422, #49629, .T. ) ;
#50728 = CARTESIAN_POINT ( 'NONE',  ( 1.060575238724906964E-15, -103.7500000000000000, 5.773502691896257311 ) ) ;
#50729 = DIRECTION ( 'NONE',  ( -0.000000000000000000, 1.000000000000000000, -0.000000000000000000 ) ) ;
#50730 = CARTESIAN_POINT ( 'NONE',  ( 4.458734124999998549, -36.97916666530107221, -2.574251347313721627 ) ) ;
#50731 = CARTESIAN_POINT ( 'NONE',  ( -4.999999999999999112, 0.2083333360645180099, 2.886751345948131764 ) ) ;
#50732 = CARTESIAN_POINT ( 'NONE',  ( 5.000000000000000000, -50.41666666666666430, -2.886751345948130876 ) ) ;
#50733 = CARTESIAN_POINT ( 'NONE',  ( -53.51423613279429503, -127.2500000013656347, 4.591703134518082763 ) ) ;
#50734 = CARTESIAN_POINT ( 'NONE',  ( 2.229367062499998831, -80.89583333196773651, -3.861377020970580887 ) ) ;
#50735 = CARTESIAN_POINT ( 'NONE',  ( -6.972266317189433020E-16, -71.25000000000000000, -5.000000000000000000 ) ) ;
#50736 = CARTESIAN_POINT ( 'NONE',  ( 4.458734124999999437, -94.81249999863440792, -5.460374474430324690E-16 ) ) ;
#50737 = CARTESIAN_POINT ( 'NONE',  ( 0.000000000000000000, -170.0000000000000000, 0.000000000000000000 ) ) ;
#50738 = CARTESIAN_POINT ( 'NONE',  ( -3.152548672688508926E-16, -1.812499998634406584, -5.148502694627439702 ) ) ;
#50739 = EDGE_LOOP ( 'NONE', ( #29132, #30843, #13758, #20446 ) ) ;
#50740 = CARTESIAN_POINT ( 'NONE',  ( 3.535533905932738197, -145.8750000000000000, -3.535533905932738197 ) ) ;
#50741 = CARTESIAN_POINT ( 'NONE',  ( -6.972266317189433020E-16, -68.24999999999998579, -5.000000000000000000 ) ) ;
#50742 = CARTESIAN_POINT ( 'NONE',  ( 4.458734125000001214, -86.89583333196773651, 2.574251347313718519 ) ) ;
#50743 = CARTESIAN_POINT ( 'NONE',  ( -3.535533905932738641, -168.5000000027312126, 3.535533905932737309 ) ) ;
#50744 = CARTESIAN_POINT ( 'NONE',  ( 4.458734124999999437, -87.06249999863439371, -5.460374474430324690E-16 ) ) ;
#50745 = CARTESIAN_POINT ( 'NONE',  ( 2.229367062500001939, 16.77083333469892779, 3.861377020970579999 ) ) ;
#50746 = FACE_OUTER_BOUND ( 'NONE', #12806, .T. ) ;
#50747 = AXIS2_PLACEMENT_3D ( 'NONE', #11067, #20730, #60294 ) ;
#50748 = CARTESIAN_POINT ( 'NONE',  ( -58.39396692619412477, -136.4375000013655779, 2.891590998281057701 ) ) ;
#50749 = CARTESIAN_POINT ( 'NONE',  ( 9.457646018065525792E-16, -6.062499998634404363, 5.148502694627439702 ) ) ;
#50750 = CARTESIAN_POINT ( 'NONE',  ( 2.229367062499998831, 19.10416666803225993, -3.861377020970580887 ) ) ;
#50751 = CARTESIAN_POINT ( 'NONE',  ( 4.458734124999998549, -49.97916666530106511, -2.574251347313721627 ) ) ;
#50752 = CARTESIAN_POINT ( 'NONE',  ( -2.499999999999996447, -13.70833333060214976, 4.330127018922195425 ) ) ;
#50753 = CARTESIAN_POINT ( 'NONE',  ( -2.229367062500000163, -85.47916666530107932, -3.861377020970580443 ) ) ;
#50754 = CARTESIAN_POINT ( 'NONE',  ( -2.229367062499996610, -5.145833331967740065, 3.861377020970582219 ) ) ;
#50755 = DIRECTION ( 'NONE',  ( -0.4999999999999948375, 0.000000000000000000, 0.8660254037844415942 ) ) ;
#50756 = ORIENTED_EDGE ( 'NONE', *, *, #25650, .T. ) ;
#50757 = CARTESIAN_POINT ( 'NONE',  ( -4.458734124999999437, -32.64583333196773651, -2.574251347313719407 ) ) ;
#50758 =( BOUNDED_CURVE ( )  B_SPLINE_CURVE ( 2, ( #35648, #39499, #30815, #30490, #49156, #1255, #59135, #39181, #14738 ),
 .UNSPECIFIED., .F., .F. ) 
 B_SPLINE_CURVE_WITH_KNOTS ( ( 3, 2, 2, 2, 3 ),
 ( 0.6645833333333333037, 0.6652777777777777457, 0.6666666666666666297, 0.6680555555555555136, 0.6687499999999999556 ),
 .UNSPECIFIED. ) 
 CURVE ( )  GEOMETRIC_REPRESENTATION_ITEM ( )  RATIONAL_B_SPLINE_CURVE ( ( 0.9330127018922194093, 0.9330127018922194093, 1.000000000000000000, 0.8660254037844387076, 1.000000000000000000, 0.8660254037844387076, 1.000000000000000000, 0.9330127018922194093, 0.9330127018922194093 ) ) 
 REPRESENTATION_ITEM ( '' )  );
#50759 = CARTESIAN_POINT ( 'NONE',  ( -52.10840900171896806, -131.4375000013656063, 3.393966926194110556 ) ) ;
#50760 = CARTESIAN_POINT ( 'NONE',  ( 2.229367062499998831, -75.64583333196773651, -3.861377020970580887 ) ) ;
#50761 = CARTESIAN_POINT ( 'NONE',  ( -3.152548672688508926E-16, 27.18750000136559564, -5.148502694627439702 ) ) ;
#50762 = CARTESIAN_POINT ( 'NONE',  ( -4.458734124999998549, 19.77083333469892779, 2.574251347313722516 ) ) ;
#50763 = ADVANCED_FACE ( 'NONE', ( #9429 ), #19074, .T. ) ;
#50764 = EDGE_CURVE ( 'NONE', #54593, #46416, #11531, .T. ) ;
#50765 = LINE ( 'NONE', #51408, #45126 ) ;
#50766 = CARTESIAN_POINT ( 'NONE',  ( 2.500000000000002220, -28.66666666666666785, 4.330127018922192761 ) ) ;
#50767 = CARTESIAN_POINT ( 'NONE',  ( 4.458734124999998549, -79.97916666530106511, -2.574251347313721627 ) ) ;
#50768 = CARTESIAN_POINT ( 'NONE',  ( 1.060575238724906964E-15, -66.75000000000000000, 5.773502691896257311 ) ) ;
#50769 = EDGE_CURVE ( 'NONE', #18978, #30981, #20167, .T. ) ;
#50770 = CARTESIAN_POINT ( 'NONE',  ( -2.499999999999996447, -74.83333333333332860, 4.330127018922195425 ) ) ;
#50771 = CARTESIAN_POINT ( 'NONE',  ( -5.000000000000000000, 25.12500000273118417, 0.000000000000000000 ) ) ;
#50772 = ORIENTED_EDGE ( 'NONE', *, *, #21251, .T. ) ;
#50773 = CARTESIAN_POINT ( 'NONE',  ( 1.975475456537005874E-15, -72.62499999726878741, 5.000000000000000000 ) ) ;
#50774 = CYLINDRICAL_SURFACE ( 'NONE', #9346, 5.000000000000000000 ) ;
#50776 = CARTESIAN_POINT ( 'NONE',  ( -3.535250795749689387E-16, -25.25000000000000355, -5.773502691896257311 ) ) ;
#50775 = CARTESIAN_POINT ( 'NONE',  ( -5.000000000000000000, -106.8749999972687874, 0.000000000000000000 ) ) ;
#50777 = CARTESIAN_POINT ( 'NONE',  ( -2.229367062500000163, -28.47916666530107221, -3.861377020970580443 ) ) ;
#50778 = CARTESIAN_POINT ( 'NONE',  ( 4.458734125000000326, -88.89583333196773651, 2.574251347313718519 ) ) ;
#50779 = EDGE_CURVE ( 'NONE', #50505, #34696, #41573, .T. ) ;
#50780 = AXIS2_PLACEMENT_3D ( 'NONE', #40530, #39565, #59530 ) ;
#50781 = CARTESIAN_POINT ( 'NONE',  ( 2.500000000000002220, -21.54166666393548013, 4.330127018922192761 ) ) ;
#50783 = VERTEX_POINT ( 'NONE', #36616 ) ;
#50782 = CARTESIAN_POINT ( 'NONE',  ( -4.458734124999998549, -56.22916666530107221, 2.574251347313722516 ) ) ;
#50784 = CARTESIAN_POINT ( 'NONE',  ( 0.000000000000000000, -120.0000000000000000, 0.000000000000000000 ) ) ;
#50785 = CARTESIAN_POINT ( 'NONE',  ( 1.339745962155615144, -74.58034179853031276, 4.999999999999999112 ) ) ;
#50786 = EDGE_CURVE ( 'NONE', #40505, #4115, #30876, .T. ) ;
#50788 = ORIENTED_EDGE ( 'NONE', *, *, #36142, .T. ) ;
#50787 = CARTESIAN_POINT ( 'NONE',  ( -4.458734124999998549, -2.479166665301069550, 2.574251347313722516 ) ) ;
#50789 = CARTESIAN_POINT ( 'NONE',  ( -5.000000000000000000, -71.08333333333332860, -2.886751345948128211 ) ) ;
#50790 = EDGE_CURVE ( 'NONE', #26750, #328, #3479, .T. ) ;
#50791 = CARTESIAN_POINT ( 'NONE',  ( -3.152801135295367985, -152.0625000013655779, 3.152801135295367096 ) ) ;
#50792 = CARTESIAN_POINT ( 'NONE',  ( 9.457646018065525792E-16, -47.31249999863440792, 5.148502694627439702 ) ) ;
#50793 = CYLINDRICAL_SURFACE ( 'NONE', #33740, 5.000000000000000000 ) ;
#50794 =( BOUNDED_CURVE ( )  B_SPLINE_CURVE ( 2, ( #37049, #36729, #9574, #47632, #22894, #56677, #46691, #37667, #12904 ),
 .UNSPECIFIED., .F., .F. ) 
 B_SPLINE_CURVE_WITH_KNOTS ( ( 3, 2, 2, 2, 3 ),
 ( 0.2687499999999999889, 0.2694444444444444309, 0.2708333333333333148, 0.2722222222222221988, 0.2729166666666666963 ),
 .UNSPECIFIED. ) 
 CURVE ( )  GEOMETRIC_REPRESENTATION_ITEM ( )  RATIONAL_B_SPLINE_CURVE ( ( 0.9330127018922194093, 0.9330127018922194093, 1.000000000000000000, 0.8660254037844387076, 1.000000000000000000, 0.8660254037844387076, 1.000000000000000000, 0.9330127018922167448, 0.9330127018922194093 ) ) 
 REPRESENTATION_ITEM ( '' )  );
#50795 = CARTESIAN_POINT ( 'NONE',  ( -5.000000000000000000, -159.5000000000000000, -6.123233995736766282E-16 ) ) ;
#50796 = ADVANCED_FACE ( 'NONE', ( #3794 ), #13435, .T. ) ;
#50797 = CARTESIAN_POINT ( 'NONE',  ( 5.000000000000000000, -71.37499999726880162, -6.123233995736766282E-16 ) ) ;
#50798 = CARTESIAN_POINT ( 'NONE',  ( 5.000000000000000888, -10.45833333060214443, 2.886751345948126879 ) ) ;
#50799 = CARTESIAN_POINT ( 'NONE',  ( -54.60164318462004474, -154.3750000000000284, -4.984105922594373794 ) ) ;
#50800 = CARTESIAN_POINT ( 'NONE',  ( 4.458734124999998549, -17.97916666530106866, -2.574251347313721627 ) ) ;
#50801 = CARTESIAN_POINT ( 'NONE',  ( 4.458734124999998549, -51.97916666530107221, -2.574251347313721627 ) ) ;
#50802 = VECTOR ( 'NONE', #34871, 1000.000000000000000 ) ;
#50803 = CARTESIAN_POINT ( 'NONE',  ( -2.500000000000000444, -59.04166666393546592, -4.330127018922193649 ) ) ;
#50804 = CARTESIAN_POINT ( 'NONE',  ( -3.152801135295367096, -145.0625000013655779, -3.152801135295367541 ) ) ;
#50805 = CARTESIAN_POINT ( 'NONE',  ( 2.229367062499998831, -93.89583333196772230, -3.861377020970580887 ) ) ;
#50806 = VERTEX_POINT ( 'NONE', #17939 ) ;
#50807 = CARTESIAN_POINT ( 'NONE',  ( -58.39396692619412477, -152.6875000013656063, 2.891590998281057701 ) ) ;
#50808 = CARTESIAN_POINT ( 'NONE',  ( 2.229367062500001939, 24.77083333469892779, 3.861377020970579999 ) ) ;
#50809 = CARTESIAN_POINT ( 'NONE',  ( -55.39835681537999790, -145.0000000027312126, 4.984105922594378235 ) ) ;
#50810 = CARTESIAN_POINT ( 'NONE',  ( 2.500000000000002220, -50.66666666666666430, 4.330127018922192761 ) ) ;
#50811 = CARTESIAN_POINT ( 'NONE',  ( -3.152548672688508926E-16, -1.562499998634406140, -5.148502694627439702 ) ) ;
#50812 = CARTESIAN_POINT ( 'NONE',  ( 1.339745962155615144, -1.580341798530293662, 4.999999999999999112 ) ) ;
#50813 = CARTESIAN_POINT ( 'NONE',  ( 4.458734124999998549, -23.97916666530107221, -2.574251347313721627 ) ) ;
#50814 = CARTESIAN_POINT ( 'NONE',  ( -2.229367062500000163, -60.72916666530106511, -3.861377020970580443 ) ) ;
#50815 = LINE ( 'NONE', #12835, #33293 ) ;
#50816 = CARTESIAN_POINT ( 'NONE',  ( 2.229367062500001939, -8.979166665301075767, 3.861377020970579999 ) ) ;
#50817 = LINE ( 'NONE', #41464, #50084 ) ;
#50818 = CARTESIAN_POINT ( 'NONE',  ( 1.846868145590736310, -146.6250000013655779, 4.458734124999997661 ) ) ;
#50819 = CARTESIAN_POINT ( 'NONE',  ( 4.458734124999998549, 18.02083333469892779, -2.574251347313721627 ) ) ;
#50820 = ORIENTED_EDGE ( 'NONE', *, *, #49097, .T. ) ;
#50821 = CARTESIAN_POINT ( 'NONE',  ( -6.972266317189433020E-16, -27.12499999726881228, -5.000000000000000000 ) ) ;
#50822 = CARTESIAN_POINT ( 'NONE',  ( -5.000000000000000000, -12.99999999999999822, 0.000000000000000000 ) ) ;
#50824 = CARTESIAN_POINT ( 'NONE',  ( -2.229367062499996610, -17.14583333196773651, 3.861377020970582219 ) ) ;
#50823 = CARTESIAN_POINT ( 'NONE',  ( 2.500000000000002220, -86.66666666666667140, 4.330127018922192761 ) ) ;
#50825 = CARTESIAN_POINT ( 'NONE',  ( -6.972266317189433020E-16, -35.12499999726880873, -5.000000000000000000 ) ) ;
#50826 = CARTESIAN_POINT ( 'NONE',  ( 5.000000000000000888, -3.583333333333333925, 2.886751345948126879 ) ) ;
#50827 = CARTESIAN_POINT ( 'NONE',  ( -50.40829686548195099, -149.0000000013656063, -1.485763867205728284 ) ) ;
#50828 = CARTESIAN_POINT ( 'NONE',  ( -5.000000000000000000, -46.95833333060215153, -2.886751345948128211 ) ) ;
#50829 = CARTESIAN_POINT ( 'NONE',  ( 1.339745962155615144, -24.70534180126147561, 4.999999999999999112 ) ) ;
#50830 = CARTESIAN_POINT ( 'NONE',  ( -4.458734124999999437, 10.60416666803225993, -2.574251347313719407 ) ) ;
#50831 = CARTESIAN_POINT ( 'NONE',  ( -1.339745962155613812, -90.08034179853029855, -5.000000000000000000 ) ) ;
#50832 = PRODUCT_DEFINITION ( 'UNKNOWN', '', #13310, #38600 ) ;
#50833 = CARTESIAN_POINT ( 'NONE',  ( -50.18089887299977647, -141.8125000027311842, 2.462841084822456672 ) ) ;
#50834 = CARTESIAN_POINT ( 'NONE',  ( -4.458734124999997661, 10.77083333469892956, 2.574251347313722516 ) ) ;
#50835 = CARTESIAN_POINT ( 'NONE',  ( -4.458734124999998549, -68.22916666530107932, 2.574251347313722516 ) ) ;
#50836 = CARTESIAN_POINT ( 'NONE',  ( 2.229367062500001939, -13.22916666530107221, 3.861377020970579999 ) ) ;
#50837 = CARTESIAN_POINT ( 'NONE',  ( 5.000000000000000888, 0.4166666666666659080, 2.886751345948126879 ) ) ;
#50838 = CARTESIAN_POINT ( 'NONE',  ( -3.152801135295367985, -163.8125000013656063, 3.152801135295367096 ) ) ;
#50839 = CARTESIAN_POINT ( 'NONE',  ( -5.000000000000000000, 26.04166666939784847, -2.886751345948128211 ) ) ;
#50840 = CARTESIAN_POINT ( 'NONE',  ( -4.458734124999999437, -61.39583333196774362, -2.574251347313719407 ) ) ;
#50841 = CARTESIAN_POINT ( 'NONE',  ( -5.000000000000000000, -96.87499999726881583, 0.000000000000000000 ) ) ;
#50842 = CARTESIAN_POINT ( 'NONE',  ( -2.499999999999996447, 10.16666666666666785, 4.330127018922195425 ) ) ;
#50843 = CARTESIAN_POINT ( 'NONE',  ( 5.000000000000000000, 5.625000002731185056, -6.123233995736766282E-16 ) ) ;
#50844 = CARTESIAN_POINT ( 'NONE',  ( 4.458734124999999437, -37.81249999863440792, -5.460374474430324690E-16 ) ) ;
#50845 = ADVANCED_FACE ( 'NONE', ( #57518 ), #7991, .T. ) ;
#50846 = CARTESIAN_POINT ( 'NONE',  ( -1.339745962155497683, -91.08034179853028434, -5.000000000000066613 ) ) ;
#50847 = CARTESIAN_POINT ( 'NONE',  ( -3.535250795749689387E-16, -49.25000000000000000, -5.773502691896257311 ) ) ;
#50848 = LINE ( 'NONE', #55998, #55202 ) ;
#50849 = CARTESIAN_POINT ( 'NONE',  ( -6.972266317189433020E-16, -108.2499999999999858, -5.000000000000000000 ) ) ;
#50850 = VERTEX_POINT ( 'NONE', #14921 ) ;
#50851 = CARTESIAN_POINT ( 'NONE',  ( 4.458734125000001214, -104.8958333319677365, 2.574251347313718519 ) ) ;
#50852 = CARTESIAN_POINT ( 'NONE',  ( -2.229367062500000163, -2.729166665301069550, -3.861377020970580443 ) ) ;
#50853 = DIRECTION ( 'NONE',  ( 0.000000000000000000, 0.000000000000000000, 1.000000000000000000 ) ) ;
#50854 = CARTESIAN_POINT ( 'NONE',  ( -2.499999999999996447, -7.833333333333331261, 4.330127018922195425 ) ) ;
#50855 = CARTESIAN_POINT ( 'NONE',  ( 4.458734124999999437, -73.81249999863440792, -5.460374474430324690E-16 ) ) ;
#50856 = CARTESIAN_POINT ( 'NONE',  ( -55.00000000000002132, -155.0000000000000284, 1.734723475976807094E-15 ) ) ;
#50857 = CARTESIAN_POINT ( 'NONE',  ( 1.060575238724906964E-15, -8.624999997268814056, 5.773502691896257311 ) ) ;
#50859 = ORIENTED_EDGE ( 'NONE', *, *, #41306, .T. ) ;
#50858 = CARTESIAN_POINT ( 'NONE',  ( -3.152548672688508926E-16, -39.56249999863440081, -5.148502694627439702 ) ) ;
#50860 = CARTESIAN_POINT ( 'NONE',  ( -5.000000000000000000, 28.12500000273118417, 0.000000000000000000 ) ) ;
#50862 = ORIENTED_EDGE ( 'NONE', *, *, #27921, .F. ) ;
#50861 = CARTESIAN_POINT ( 'NONE',  ( 4.458734124999998549, 11.02083333469892779, -2.574251347313721627 ) ) ;
#50863 = CARTESIAN_POINT ( 'NONE',  ( -2.500000000000000444, 24.83333333333333215, -4.330127018922193649 ) ) ;
#50864 = CARTESIAN_POINT ( 'NONE',  ( -5.000000000000000000, -54.08333333333332860, -2.886751345948128211 ) ) ;
#50865 = ADVANCED_FACE ( 'NONE', ( #18260 ), #2851, .T. ) ;
#50866 = EDGE_CURVE ( 'NONE', #4573, #51626, #11145, .T. ) ;
#50867 = CARTESIAN_POINT ( 'NONE',  ( 4.458734125000001214, -30.14583333196773296, 2.574251347313718519 ) ) ;
#50868 = CARTESIAN_POINT ( 'NONE',  ( -4.458734124999999437, -73.39583333196773651, -2.574251347313719407 ) ) ;
#50869 = CARTESIAN_POINT ( 'NONE',  ( 3.535533905932738197, -168.8750000000000284, -3.535533905932738197 ) ) ;
#50870 = EDGE_CURVE ( 'NONE', #2056, #34626, #35384, .T. ) ;
#50871 = CARTESIAN_POINT ( 'NONE',  ( -4.458734124999999437, -86.31249999863439371, 0.000000000000000000 ) ) ;
#50872 = CARTESIAN_POINT ( 'NONE',  ( -59.29741812935640155, -136.8750000013656063, -2.196230717870135685 ) ) ;
#50873 =( BOUNDED_CURVE ( )  B_SPLINE_CURVE ( 2, ( #7086, #35077, #54697, #55344, #55010, #50826, #10618, #50511, #6763 ),
 .UNSPECIFIED., .F., .F. ) 
 B_SPLINE_CURVE_WITH_KNOTS ( ( 3, 2, 2, 2, 3 ),
 ( 0.2374999999999999889, 0.2380952380952380820, 0.2392857142857142960, 0.2404761904761904823, 0.2410714285714285754 ),
 .UNSPECIFIED. ) 
 CURVE ( )  GEOMETRIC_REPRESENTATION_ITEM ( )  RATIONAL_B_SPLINE_CURVE ( ( 0.9330127018922194093, 0.9330127018922194093, 1.000000000000000000, 0.8660254037844387076, 1.000000000000000000, 0.8660254037844387076, 1.000000000000000000, 0.9330127018922194093, 0.9330127018922194093 ) ) 
 REPRESENTATION_ITEM ( '' )  );
#50874 = CARTESIAN_POINT ( 'NONE',  ( -4.458734124999998549, -33.47916666530107221, 2.574251347313722516 ) ) ;
#50875 = EDGE_CURVE ( 'NONE', #53932, #61278, #32422, .T. ) ;
#50876 = CARTESIAN_POINT ( 'NONE',  ( -1.339745962155610925, -93.66965819600733312, 5.000000000000000000 ) ) ;
#50877 = ORIENTED_EDGE ( 'NONE', *, *, #8217, .F. ) ;
#50878 = CARTESIAN_POINT ( 'NONE',  ( -3.152548672688508926E-16, -80.81249999863440792, -5.148502694627439702 ) ) ;
#50879 = CARTESIAN_POINT ( 'NONE',  ( -51.41708869693315620, -135.0000000000000284, -2.669894875933531253 ) ) ;
#50880 = ORIENTED_EDGE ( 'NONE', *, *, #36142, .F. ) ;
#50881 = CYLINDRICAL_SURFACE ( 'NONE', #12139, 5.000000000000000000 ) ;
#50882 = CARTESIAN_POINT ( 'NONE',  ( -2.499999999999996447, -18.70833333060214798, 4.330127018922195425 ) ) ;
#50883 = CARTESIAN_POINT ( 'NONE',  ( 2.229367062499998831, -65.89583333196773651, -3.861377020970580887 ) ) ;
#50884 = CARTESIAN_POINT ( 'NONE',  ( -4.458734124999999437, -10.56249999863440792, 0.000000000000000000 ) ) ;
#50885 = ORIENTED_EDGE ( 'NONE', *, *, #39714, .F. ) ;
#50886 = CARTESIAN_POINT ( 'NONE',  ( -4.999999999999998224, -9.791666663935476578, 2.886751345948131764 ) ) ;
#50887 =( BOUNDED_CURVE ( )  B_SPLINE_CURVE ( 2, ( #52873, #29035, #23913, #28422, #4600, #39014, #50583, #54458, #428 ),
 .UNSPECIFIED., .F., .F. ) 
 B_SPLINE_CURVE_WITH_KNOTS ( ( 3, 2, 2, 2, 3 ),
 ( 0.1979166666666666574, 0.1986111111111110994, 0.2000000000000000111, 0.2013888888888888951, 0.2020833333333333370 ),
 .UNSPECIFIED. ) 
 CURVE ( )  GEOMETRIC_REPRESENTATION_ITEM ( )  RATIONAL_B_SPLINE_CURVE ( ( 0.9330127018922194093, 0.9330127018922194093, 1.000000000000000000, 0.8660254037844387076, 1.000000000000000000, 0.8660254037844387076, 1.000000000000000000, 0.9330127018922194093, 0.9330127018922194093 ) ) 
 REPRESENTATION_ITEM ( '' )  );
#50888 = CARTESIAN_POINT ( 'NONE',  ( -6.031010364368858512E-14, 3.375000002731183280, 5.000000000000000000 ) ) ;
#50889 = VERTEX_POINT ( 'NONE', #53844 ) ;
#50890 = CARTESIAN_POINT ( 'NONE',  ( -2.229367062499996610, -6.395833331967741842, 3.861377020970582219 ) ) ;
#50891 = CARTESIAN_POINT ( 'NONE',  ( 4.458734125000001214, 6.104166668032262599, 2.574251347313718519 ) ) ;
#50892 = CARTESIAN_POINT ( 'NONE',  ( -4.999999999999998224, -11.79166666393547835, 2.886751345948131764 ) ) ;
#50893 = CARTESIAN_POINT ( 'NONE',  ( 3.152801135295366208, -162.5625000013656063, 3.152801135295367985 ) ) ;
#50894 = CYLINDRICAL_SURFACE ( 'NONE', #50172, 5.000000000000000000 ) ;
#50895 = ORIENTED_EDGE ( 'NONE', *, *, #42915, .F. ) ;
#50896 = CARTESIAN_POINT ( 'NONE',  ( 2.229367062499998831, -84.64583333196773651, -3.861377020970580887 ) ) ;
#50897 = CARTESIAN_POINT ( 'NONE',  ( 5.000000000000000000, -75.41666666666667140, -2.886751345948130876 ) ) ;
#50898 = CARTESIAN_POINT ( 'NONE',  ( -4.458734124999999437, -5.312499998634402587, 0.000000000000000000 ) ) ;
#50899 = CARTESIAN_POINT ( 'NONE',  ( -52.53715891517739323, -147.4375000000000284, -4.819101127000233298 ) ) ;
#50900 = CARTESIAN_POINT ( 'NONE',  ( 1.060575238724906964E-15, -30.62499999726881228, 5.773502691896257311 ) ) ;
#50901 = DIRECTION ( 'NONE',  ( -0.000000000000000000, 1.000000000000000000, -0.000000000000000000 ) ) ;
#50902 = CARTESIAN_POINT ( 'NONE',  ( -2.229367062499996610, 21.85416666803226349, 3.861377020970582219 ) ) ;
#50903 = CARTESIAN_POINT ( 'NONE',  ( -2.499999999999996447, -55.83333333333332860, 4.330127018922195425 ) ) ;
#50904 = CARTESIAN_POINT ( 'NONE',  ( -4.458734124999999437, 25.68750000136559208, 0.000000000000000000 ) ) ;
#50905 = CARTESIAN_POINT ( 'NONE',  ( 2.229367062500001939, -50.97916666530107221, 3.861377020970579999 ) ) ;
#50906 = CARTESIAN_POINT ( 'NONE',  ( 2.229367062499998831, -37.89583333196773651, -3.861377020970580887 ) ) ;
#50907 = CARTESIAN_POINT ( 'NONE',  ( 4.458734124999999437, 0.9375000013655959696, -5.460374474430324690E-16 ) ) ;
#50908 = CARTESIAN_POINT ( 'NONE',  ( -2.500000000000000444, -18.16666666666666430, -4.330127018922193649 ) ) ;
#50909 = CARTESIAN_POINT ( 'NONE',  ( -4.999999999999999112, 17.08333333333333215, 2.886751345948131764 ) ) ;
#50910 = CARTESIAN_POINT ( 'NONE',  ( -3.535533905932737309, -146.7500000027311842, -3.535533905932738197 ) ) ;
#50911 = DIRECTION ( 'NONE',  ( -0.000000000000000000, 1.000000000000000000, -0.000000000000000000 ) ) ;
#50912 = CARTESIAN_POINT ( 'NONE',  ( 2.229367062499998831, -44.64583333196774362, -3.861377020970580887 ) ) ;
#50913 = CARTESIAN_POINT ( 'NONE',  ( 2.499999999999998668, -77.20833333060214443, -4.330127018922193649 ) ) ;
#50914 = CARTESIAN_POINT ( 'NONE',  ( -53.51423613279429503, -138.5000000013656347, 4.591703134518082763 ) ) ;
#50915 = DIRECTION ( 'NONE',  ( -0.000000000000000000, 1.000000000000000000, -0.000000000000000000 ) ) ;
#50916 = EDGE_CURVE ( 'NONE', #46199, #63065, #48153, .T. ) ;
#50917 = CARTESIAN_POINT ( 'NONE',  ( -1.339745962155613812, -64.08034179853029855, -5.000000000000000000 ) ) ;
#50918 = CARTESIAN_POINT ( 'NONE',  ( 4.458734124999999437, -87.06249999863439371, -5.460374474430324690E-16 ) ) ;
#50919 = CARTESIAN_POINT ( 'NONE',  ( -8.190561711645485556E-16, -162.9375000013655779, 4.458734124999999437 ) ) ;
#50920 = CARTESIAN_POINT ( 'NONE',  ( -5.000000000000000000, -159.6250000027311842, -6.123233995736766282E-16 ) ) ;
#50921 = CARTESIAN_POINT ( 'NONE',  ( -5.000000000000000000, -26.08333333333333215, -2.886751345948128211 ) ) ;
#50922 = CARTESIAN_POINT ( 'NONE',  ( -1.846868145590737420, -139.7500000013655779, 4.458734124999999437 ) ) ;
#50923 = VERTEX_POINT ( 'NONE', #3168 ) ;
#50924 = AXIS2_PLACEMENT_3D ( 'NONE', #980, #20583, #50153 ) ;
#50925 = CARTESIAN_POINT ( 'NONE',  ( -4.458734124999999437, 24.35416666803225993, -2.574251347313719407 ) ) ;
#50926 = VERTEX_POINT ( 'NONE', #22788 ) ;
#50927 = CARTESIAN_POINT ( 'NONE',  ( 4.458734125000001214, -91.89583333196773651, 2.574251347313718519 ) ) ;
#50928 = CARTESIAN_POINT ( 'NONE',  ( 2.229367062499998831, 12.10416666803226171, -3.861377020970580887 ) ) ;
#50929 = CARTESIAN_POINT ( 'NONE',  ( -4.999999999999999112, 18.20833333606451987, 2.886751345948131764 ) ) ;
#50930 = CARTESIAN_POINT ( 'NONE',  ( -1.339745962155613812, -61.08034179853027723, -5.000000000000000000 ) ) ;
#50931 = CARTESIAN_POINT ( 'NONE',  ( -2.499999999999996447, 7.166666666666665186, 4.330127018922195425 ) ) ;
#50932 = CARTESIAN_POINT ( 'NONE',  ( 4.458734124999999437, -54.81249999863440081, -5.460374474430324690E-16 ) ) ;
#50933 = CIRCLE ( 'NONE', #47835, 7.500000000000001776 ) ;
#50934 = CARTESIAN_POINT ( 'NONE',  ( 2.229367062500001939, -8.979166665301075767, 3.861377020970579999 ) ) ;
#50935 = CARTESIAN_POINT ( 'NONE',  ( 2.500000000000002220, -6.666666666666667851, 4.330127018922192761 ) ) ;
#50936 = CARTESIAN_POINT ( 'NONE',  ( -51.60603307380591787, -136.1875000013656063, -2.891590998281053704 ) ) ;
#50937 = CARTESIAN_POINT ( 'NONE',  ( 0.000000000000000000, -170.0000000000000000, 0.000000000000000000 ) ) ;
#50938 = CYLINDRICAL_SURFACE ( 'NONE', #1499, 5.000000000000000000 ) ;
#50939 = CARTESIAN_POINT ( 'NONE',  ( -4.999999999999999112, -35.91666666666666430, 2.886751345948131764 ) ) ;
#50940 = CARTESIAN_POINT ( 'NONE',  ( 1.255007937094098239E-14, 23.87500000273118062, -4.999999999999999112 ) ) ;
#50943 = CARTESIAN_POINT ( 'NONE',  ( 4.458734124999998549, -16.97916666530107221, -2.574251347313721627 ) ) ;
#50942 =( BOUNDED_CURVE ( )  B_SPLINE_CURVE ( 2, ( #46902, #27582, #61072, #32732, #52359, #56241, #52045, #2221, #42374 ),
 .UNSPECIFIED., .F., .F. ) 
 B_SPLINE_CURVE_WITH_KNOTS ( ( 3, 2, 2, 2, 3 ),
 ( 0.6589285714285714191, 0.6595238095238095122, 0.6607142857142856984, 0.6619047619047618847, 0.6624999999999999778 ),
 .UNSPECIFIED. ) 
 CURVE ( )  GEOMETRIC_REPRESENTATION_ITEM ( )  RATIONAL_B_SPLINE_CURVE ( ( 0.9330127018922194093, 0.9330127018922194093, 1.000000000000000000, 0.8660254037844387076, 1.000000000000000000, 0.8660254037844387076, 1.000000000000000000, 0.9330127018922194093, 0.9330127018922194093 ) ) 
 REPRESENTATION_ITEM ( '' )  );
#50941 = CARTESIAN_POINT ( 'NONE',  ( -5.000000000000000000, 14.91666666666666607, -2.886751345948128211 ) ) ;
#50944 = CARTESIAN_POINT ( 'NONE',  ( 5.000000000000000888, 17.54166666939785557, 2.886751345948126879 ) ) ;
#50945 = CARTESIAN_POINT ( 'NONE',  ( 4.458734125000001214, -57.89583333196773651, 2.574251347313718519 ) ) ;
#50946 = CARTESIAN_POINT ( 'NONE',  ( -1.846868145590734756, -152.3750000013655779, -4.458734125000000326 ) ) ;
#50947 = CARTESIAN_POINT ( 'NONE',  ( 4.458734124999998549, -70.72916666530107932, -2.574251347313721627 ) ) ;
#50948 = CARTESIAN_POINT ( 'NONE',  ( -54.64476657466781973, -147.0625000013656063, -4.444560631937228834 ) ) ;
#50949 = CARTESIAN_POINT ( 'NONE',  ( 4.458734124999999437, -22.06249999863440436, -5.460374474430324690E-16 ) ) ;
#50950 = CARTESIAN_POINT ( 'NONE',  ( -5.000000000000000000, -58.95833333060213732, -2.886751345948128211 ) ) ;
#50951 = ORIENTED_EDGE ( 'NONE', *, *, #13645, .T. ) ;
#50952 = CARTESIAN_POINT ( 'NONE',  ( 0.000000000000000000, -120.0000000000000000, 0.000000000000000000 ) ) ;
#50953 = ORIENTED_EDGE ( 'NONE', *, *, #17739, .T. ) ;
#50954 = CARTESIAN_POINT ( 'NONE',  ( 4.458734125000001214, -63.14583333196774362, 2.574251347313718519 ) ) ;
#50956 = CARTESIAN_POINT ( 'NONE',  ( 5.000000000000000888, -58.58333333333333570, 2.886751345948126879 ) ) ;
#50955 = CARTESIAN_POINT ( 'NONE',  ( -51.75738570946856498, -148.8750000027312126, 3.805975901505576964 ) ) ;
#50957 = CARTESIAN_POINT ( 'NONE',  ( -4.458734125000000326, -151.0000000013656063, -1.846868145590735644 ) ) ;
#50958 = ORIENTED_EDGE ( 'NONE', *, *, #2070, .T. ) ;
#50959 = CARTESIAN_POINT ( 'NONE',  ( -4.999999999999998224, -7.791666663935482795, 2.886751345948131764 ) ) ;
#50960 = FACE_OUTER_BOUND ( 'NONE', #37891, .T. ) ;
#50961 = CARTESIAN_POINT ( 'NONE',  ( 1.975475456537005874E-15, -8.750000000000000000, 5.000000000000000000 ) ) ;
#50962 = CARTESIAN_POINT ( 'NONE',  ( -4.458734124999999437, -48.56249999863440792, 0.000000000000000000 ) ) ;
#50963 = EDGE_LOOP ( 'NONE', ( #14539, #10409, #32430, #40061 ) ) ;
#50964 = CARTESIAN_POINT ( 'NONE',  ( -4.330127018922205195, 45.00000000000000000, -7.499999999999943157 ) ) ;
#50965 = CARTESIAN_POINT ( 'NONE',  ( -4.458734124999999437, 7.687500001365594748, 0.000000000000000000 ) ) ;
#50966 = CARTESIAN_POINT ( 'NONE',  ( -2.229367062499996610, 22.85416666803225993, 3.861377020970582219 ) ) ;
#50967 = CARTESIAN_POINT ( 'NONE',  ( -50.40829686548195099, -148.0000000013655779, -1.485763867205728284 ) ) ;
#50968 = CARTESIAN_POINT ( 'NONE',  ( 5.000000000000000000, -13.37499999726881050, -6.123233995736766282E-16 ) ) ;
#50969 = DIRECTION ( 'NONE',  ( -0.000000000000000000, 1.000000000000000000, -0.000000000000000000 ) ) ;
#50970 = VECTOR ( 'NONE', #19102, 1000.000000000000000 ) ;
#50971 = EDGE_LOOP ( 'NONE', ( #5861, #24200, #26233, #4967 ) ) ;
#50972 = CARTESIAN_POINT ( 'NONE',  ( 2.229367062499998831, -71.64583333196773651, -3.861377020970580887 ) ) ;
#50973 = CARTESIAN_POINT ( 'NONE',  ( 1.975475456537005874E-15, -49.62499999726880873, 5.000000000000000000 ) ) ;
#50974 = CARTESIAN_POINT ( 'NONE',  ( 2.229367062499998831, 14.35416666803226171, -3.861377020970580887 ) ) ;
#50975 = EDGE_CURVE ( 'NONE', #5037, #43626, #54743, .T. ) ;
#50976 = VECTOR ( 'NONE', #43701, 1000.000000000000000 ) ;
#50977 = VECTOR ( 'NONE', #25333, 1000.000000000000000 ) ;
#50978 = CARTESIAN_POINT ( 'NONE',  ( -6.972266317189433020E-16, -70.12499999726880162, -5.000000000000000000 ) ) ;
#50979 = CARTESIAN_POINT ( 'NONE',  ( -2.071067811865351604, -157.3125000000000284, 5.000000000000126121 ) ) ;
#50980 = CARTESIAN_POINT ( 'NONE',  ( -2.229367062499996610, -54.39583333196773651, 3.861377020970582219 ) ) ;
#50981 = CARTESIAN_POINT ( 'NONE',  ( -2.499999999999996447, -13.70833333060214976, 4.330127018922195425 ) ) ;
#50982 = CARTESIAN_POINT ( 'NONE',  ( -53.33387254593723270, -146.8125000000000284, 5.149110718188528502 ) ) ;
#50983 = DIRECTION ( 'NONE',  ( -0.000000000000000000, 1.000000000000000000, -0.000000000000000000 ) ) ;
#50984 = CARTESIAN_POINT ( 'NONE',  ( 0.000000000000000000, -170.0000000000000000, 0.000000000000000000 ) ) ;
#50985 = CARTESIAN_POINT ( 'NONE',  ( -2.229367062499996610, -21.39583333196774007, 3.861377020970582219 ) ) ;
#50986 = ORIENTED_EDGE ( 'NONE', *, *, #35911, .T. ) ;
#50987 =( BOUNDED_CURVE ( )  B_SPLINE_CURVE ( 2, ( #16907, #47136, #3397, #16595, #32017, #12716, #36525, #27197, #46503 ),
 .UNSPECIFIED., .F., .F. ) 
 B_SPLINE_CURVE_WITH_KNOTS ( ( 3, 2, 2, 2, 3 ),
 ( 0.07500000000000005274, 0.07916666666666671848, 0.08333333333333339810, 0.08750000000000007772, 0.09166666666666674346 ),
 .UNSPECIFIED. ) 
 CURVE ( )  GEOMETRIC_REPRESENTATION_ITEM ( )  RATIONAL_B_SPLINE_CURVE ( ( 0.9999999999999990008, 0.9238795325112877377, 1.000000000000000000, 0.9238795325112867385, 1.000000000000000000, 0.9238795325112867385, 1.000000000000000000, 0.9238795325112851842, 1.000000000000001554 ) ) 
 REPRESENTATION_ITEM ( '' )  );
#50988 = CARTESIAN_POINT ( 'NONE',  ( 6.123233995736766282E-16, -170.0000000000000000, -5.000000000000000000 ) ) ;
#50989 = CARTESIAN_POINT ( 'NONE',  ( -2.229367062500000163, -102.4791666653010651, -3.861377020970580443 ) ) ;
#50990 = CARTESIAN_POINT ( 'NONE',  ( 2.071067811865475505, -156.9375000027312126, -5.000000000000000888 ) ) ;
#50991 = VERTEX_POINT ( 'NONE', #60285 ) ;
#50992 = CARTESIAN_POINT ( 'NONE',  ( -4.458734124999998549, -105.4791666653010793, 2.574251347313722516 ) ) ;
#50993 = CARTESIAN_POINT ( 'NONE',  ( 9.457646018065525792E-16, -26.06249999863440792, 5.148502694627439702 ) ) ;
#50994 = CARTESIAN_POINT ( 'NONE',  ( -5.000000000000000000, -61.95833333060215153, -2.886751345948128211 ) ) ;
#50995 = CARTESIAN_POINT ( 'NONE',  ( -52.10840900171896806, -151.4375000013656063, 3.393966926194110556 ) ) ;
#50996 = CARTESIAN_POINT ( 'NONE',  ( -56.48576386720575471, -142.7500000013655779, -4.591703134518078322 ) ) ;
#50997 = CARTESIAN_POINT ( 'NONE',  ( 4.458734124999998549, -21.72916666530107221, -2.574251347313721627 ) ) ;
#50998 = CARTESIAN_POINT ( 'NONE',  ( -4.458734124999997661, -66.47916666530106511, 2.574251347313722516 ) ) ;
#50999 = CARTESIAN_POINT ( 'NONE',  ( -58.80597590150559739, -137.0000000000000284, 3.242614290531460330 ) ) ;
#51000 = CARTESIAN_POINT ( 'NONE',  ( 4.458734124999998549, -24.72916666530106866, -2.574251347313721627 ) ) ;
#51001 = CARTESIAN_POINT ( 'NONE',  ( 0.000000000000000000, -120.0000000000000000, 5.000000000000000000 ) ) ;
#51002 = CARTESIAN_POINT ( 'NONE',  ( -5.000000000000000000, -150.5000000000000284, -6.123233995736766282E-16 ) ) ;
#51003 = CARTESIAN_POINT ( 'NONE',  ( 5.000000000000000000, -10.50000000000000178, -6.123233995736766282E-16 ) ) ;
#51004 = CARTESIAN_POINT ( 'NONE',  ( 3.152801135295366208, -153.5625000013656063, 3.152801135295367985 ) ) ;
#51005 = VERTEX_POINT ( 'NONE', #25536 ) ;
#51006 = CARTESIAN_POINT ( 'NONE',  ( 9.457646018065525792E-16, -52.31249999863440792, 5.148502694627439702 ) ) ;
#51007 = CARTESIAN_POINT ( 'NONE',  ( -2.500000000000000444, -87.04166666393547303, -4.330127018922193649 ) ) ;
#51008 = CARTESIAN_POINT ( 'NONE',  ( -7.848314987057850800, 4.129027267381560229, -7.493854785173809319 ) ) ;
#51009 = CARTESIAN_POINT ( 'NONE',  ( 5.000000000000000000, 22.58333333333333570, -2.886751345948129988 ) ) ;
#51010 = CARTESIAN_POINT ( 'NONE',  ( -6.972266317189433020E-16, 25.74999999999999645, -5.000000000000000000 ) ) ;
#51011 = CARTESIAN_POINT ( 'NONE',  ( -3.152548672688508926E-16, 5.437500001365592084, -5.148502694627439702 ) ) ;
#51012 = CARTESIAN_POINT ( 'NONE',  ( 1.975475456537005874E-15, 13.24999999999999822, 5.000000000000000000 ) ) ;
#51013 = CARTESIAN_POINT ( 'NONE',  ( -6.972266317189433020E-16, -7.249999999999998224, -5.000000000000000000 ) ) ;
#51014 = CARTESIAN_POINT ( 'NONE',  ( 4.458734124999998549, 17.02083333469892423, -2.574251347313721627 ) ) ;
#51015 = CARTESIAN_POINT ( 'NONE',  ( 5.000000000000000000, 5.625000002731185056, -6.123233995736766282E-16 ) ) ;
#51016 = ORIENTED_EDGE ( 'NONE', *, *, #29647, .F. ) ;
#51017 = CARTESIAN_POINT ( 'NONE',  ( -6.972266317189433020E-16, -80.12499999726881583, -5.000000000000000000 ) ) ;
#51018 = ORIENTED_EDGE ( 'NONE', *, *, #8728, .F. ) ;
#51019 = AXIS2_PLACEMENT_3D ( 'NONE', #24942, #14640, #49378 ) ;
#51020 = DIRECTION ( 'NONE',  ( 0.000000000000000000, 0.000000000000000000, 1.000000000000000000 ) ) ;
#51021 = CARTESIAN_POINT ( 'NONE',  ( 4.458734124999999437, -42.81249999863440081, -5.460374474430324690E-16 ) ) ;
#51022 = CARTESIAN_POINT ( 'NONE',  ( -4.458734125000001214, -165.1250000013656063, 1.846868145590734089 ) ) ;
#51023 = AXIS2_PLACEMENT_3D ( 'NONE', #34580, #53582, #44556 ) ;
#51024 = AXIS2_PLACEMENT_3D ( 'NONE', #25246, #35222, #34247 ) ;
#51025 = CARTESIAN_POINT ( 'NONE',  ( 5.000000000000000000, -45.29166666393546592, -2.886751345948129988 ) ) ;
#51026 = ORIENTED_EDGE ( 'NONE', *, *, #29535, .F. ) ;
#51027 = CARTESIAN_POINT ( 'NONE',  ( -4.458734124999999437, -17.39583333196773651, -2.574251347313719407 ) ) ;
#51028 = VERTEX_POINT ( 'NONE', #59969 ) ;
#51029 = CARTESIAN_POINT ( 'NONE',  ( -5.000000000000000000, -89.08333333333334281, -2.886751345948128211 ) ) ;
#51030 = CARTESIAN_POINT ( 'NONE',  ( 3.152801135295366208, -165.5625000013656063, 3.152801135295367985 ) ) ;
#51032 = VERTEX_POINT ( 'NONE', #54812 ) ;
#51031 = CARTESIAN_POINT ( 'NONE',  ( -5.000000000000000000, -34.95833333060213732, -2.886751345948128211 ) ) ;
#51033 = CARTESIAN_POINT ( 'NONE',  ( -52.53715891517739323, -140.4375000000000000, -4.819101127000233298 ) ) ;
#51034 = CARTESIAN_POINT ( 'NONE',  ( 2.229367062499998831, -31.89583333196773651, -3.861377020970580887 ) ) ;
#51035 = CARTESIAN_POINT ( 'NONE',  ( -1.339745962155623360, 20.33034180399266333, 4.999999999999991118 ) ) ;
#51036 = EDGE_LOOP ( 'NONE', ( #777, #41052, #22933 ) ) ;
#51037 = CARTESIAN_POINT ( 'NONE',  ( -4.458734124999999437, -76.39583333196775072, -2.574251347313719407 ) ) ;
#51038 = CARTESIAN_POINT ( 'NONE',  ( 9.457646018065525792E-16, 28.93750000136559564, 5.148502694627439702 ) ) ;
#51039 = CARTESIAN_POINT ( 'NONE',  ( -2.500000000000000444, -54.16666666666667140, -4.330127018922193649 ) ) ;
#51040 = ORIENTED_EDGE ( 'NONE', *, *, #29028, .T. ) ;
#51041 = CARTESIAN_POINT ( 'NONE',  ( -2.499999999999996447, 5.291666669397853795, 4.330127018922195425 ) ) ;
#51042 = CARTESIAN_POINT ( 'NONE',  ( -51.60603307380591787, -144.1875000013656063, -2.891590998281053704 ) ) ;
#51043 = CARTESIAN_POINT ( 'NONE',  ( -4.458734124999999437, -79.64583333196772230, -2.574251347313719407 ) ) ;
#51044 = CARTESIAN_POINT ( 'NONE',  ( -50.01589407740564042, -128.7500000027312126, 0.3983568153799778022 ) ) ;
#51045 = DIRECTION ( 'NONE',  ( 0.000000000000000000, 0.000000000000000000, 1.000000000000000000 ) ) ;
#51046 = CARTESIAN_POINT ( 'NONE',  ( -1.846868145590737420, -143.0000000013655779, 4.458734124999997661 ) ) ;
#51047 = CARTESIAN_POINT ( 'NONE',  ( -4.999999999999998224, 6.208333336064520758, 2.886751345948131764 ) ) ;
#51048 = CARTESIAN_POINT ( 'NONE',  ( 2.229367062500001939, -48.97916666530107221, 3.861377020970579999 ) ) ;
#51049 = CARTESIAN_POINT ( 'NONE',  ( 4.458734124999998549, -46.72916666530106511, -2.574251347313721627 ) ) ;
#51050 = CARTESIAN_POINT ( 'NONE',  ( -1.339745962155613812, 20.79465819873852084, -5.000000000000000000 ) ) ;
#51051 = EDGE_CURVE ( 'NONE', #22073, #33230, #17733, .T. ) ;
#51052 = CARTESIAN_POINT ( 'NONE',  ( 5.000000000000000888, -108.5833333333333428, 2.886751345948126879 ) ) ;
#51053 = CARTESIAN_POINT ( 'NONE',  ( 0.000000000000000000, -170.0000000000000000, 5.000000000000000000 ) ) ;
#51054 = CARTESIAN_POINT ( 'NONE',  ( 4.458734124999999437, -40.06249999863440081, -5.460374474430324690E-16 ) ) ;
#51055 = CARTESIAN_POINT ( 'NONE',  ( 5.000000000000000000, 3.625000002731186388, -6.123233995736766282E-16 ) ) ;
#51056 = CARTESIAN_POINT ( 'NONE',  ( -1.339745962155613812, -73.20534180126146850, -5.000000000000000000 ) ) ;
#51057 = CARTESIAN_POINT ( 'NONE',  ( -51.60603307380591787, -130.9375000013656063, -2.891590998281053704 ) ) ;
#51058 = CARTESIAN_POINT ( 'NONE',  ( 4.458734124999998549, -81.97916666530106511, -2.574251347313721627 ) ) ;
#51059 = CARTESIAN_POINT ( 'NONE',  ( 1.339745962155615144, -71.70534180126148271, 4.999999999999999112 ) ) ;
#51060 = CARTESIAN_POINT ( 'NONE',  ( -4.458734124999999437, -98.39583333196773651, -2.574251347313719407 ) ) ;
#51061 = CARTESIAN_POINT ( 'NONE',  ( -2.229367062500000163, -3.729166665301070438, -3.861377020970580443 ) ) ;
#51062 = ORIENTED_EDGE ( 'NONE', *, *, #32208, .F. ) ;
#51063 = CARTESIAN_POINT ( 'NONE',  ( -52.53715891517739323, -139.4375000000000284, -4.819101127000233298 ) ) ;
#51064 = CARTESIAN_POINT ( 'NONE',  ( -1.339745962155613812, -86.08034179853028434, -5.000000000000000000 ) ) ;
#51065 = CARTESIAN_POINT ( 'NONE',  ( 4.458734125000001214, -88.89583333196773651, 2.574251347313718519 ) ) ;
#51066 = CARTESIAN_POINT ( 'NONE',  ( 7.204675194429079505E-15, 27.74999999999999645, -5.000000000000000000 ) ) ;
#51067 = CARTESIAN_POINT ( 'NONE',  ( -4.458734124999998549, -87.47916666530107932, 2.574251347313722516 ) ) ;
#51068 = AXIS2_PLACEMENT_3D ( 'NONE', #1078, #50580, #15850 ) ;
#51069 = CARTESIAN_POINT ( 'NONE',  ( 4.458734124999999437, 11.93750000136559564, -5.460374474430324690E-16 ) ) ;
#51070 = CARTESIAN_POINT ( 'NONE',  ( 1.339745962155615144, -77.58034179853028434, 4.999999999999999112 ) ) ;
#51071 = AXIS2_PLACEMENT_3D ( 'NONE', #38927, #39241, #29590 ) ;
#51072 =( BOUNDED_CURVE ( )  B_SPLINE_CURVE ( 2, ( #6825, #36725, #50882, #55715, #12588, #52150, #27069, #32201, #26431 ),
 .UNSPECIFIED., .F., .F. ) 
 B_SPLINE_CURVE_WITH_KNOTS ( ( 3, 2, 2, 2, 3 ),
 ( 0.3979166666666666963, 0.3986111111111111382, 0.4000000000000000222, 0.4013888888888889062, 0.4020833333333333481 ),
 .UNSPECIFIED. ) 
 CURVE ( )  GEOMETRIC_REPRESENTATION_ITEM ( )  RATIONAL_B_SPLINE_CURVE ( ( 0.9330127018922194093, 0.9330127018922220739, 1.000000000000000000, 0.8660254037844387076, 1.000000000000000000, 0.8660254037844387076, 1.000000000000000000, 0.9330127018922194093, 0.9330127018922194093 ) ) 
 REPRESENTATION_ITEM ( '' )  );
#51073 = CARTESIAN_POINT ( 'NONE',  ( -58.39396692619412477, -133.4375000013656063, 2.891590998281057701 ) ) ;
#51074 = EDGE_CURVE ( 'NONE', #21872, #25868, #21355, .T. ) ;
#51075 = AXIS2_PLACEMENT_3D ( 'NONE', #33658, #43607, #23391 ) ;
#51076 = CARTESIAN_POINT ( 'NONE',  ( -2.229367062500000163, -6.479166665301072214, -3.861377020970580443 ) ) ;
#51077 = CARTESIAN_POINT ( 'NONE',  ( 2.229367062500001939, 17.77083333469892779, 3.861377020970579999 ) ) ;
#51078 = EDGE_CURVE ( 'NONE', #10933, #35595, #24672, .T. ) ;
#51079 = CARTESIAN_POINT ( 'NONE',  ( 4.458734124999998549, -48.97916666530107221, -2.574251347313721627 ) ) ;
#51080 = CARTESIAN_POINT ( 'NONE',  ( -2.071067811865538566, -163.6875000000000000, -4.999999999999937828 ) ) ;
#51081 = CARTESIAN_POINT ( 'NONE',  ( 4.458734124999999437, -85.81249999863439371, -5.460374474430324690E-16 ) ) ;
#51082 = CARTESIAN_POINT ( 'NONE',  ( 4.458734124999998549, -5.729166665301072214, -2.574251347313721627 ) ) ;
#51083 = PRESENTATION_STYLE_ASSIGNMENT (( #46249 ) ) ;
#51084 = VERTEX_POINT ( 'NONE', #29709 ) ;
#51085 = CARTESIAN_POINT ( 'NONE',  ( -2.229367062499996610, -37.39583333196773651, 3.861377020970582219 ) ) ;
#51086 = CARTESIAN_POINT ( 'NONE',  ( -52.80376928212989185, -127.1250000013656205, -4.297418129356379346 ) ) ;
#51087 = CARTESIAN_POINT ( 'NONE',  ( -2.229367062500000163, -79.47916666530106511, -3.861377020970580443 ) ) ;
#51088 = CARTESIAN_POINT ( 'NONE',  ( -4.458734124999999437, 28.35416666803226349, -2.574251347313719407 ) ) ;
#51089 = EDGE_CURVE ( 'NONE', #46416, #34465, #19781, .T. ) ;
#51090 = CARTESIAN_POINT ( 'NONE',  ( 9.457646018065525792E-16, 21.93750000136559208, 5.148502694627439702 ) ) ;
#51091 = CARTESIAN_POINT ( 'NONE',  ( 5.000000000000000888, -53.58333333333333570, 2.886751345948126879 ) ) ;
#51092 = CARTESIAN_POINT ( 'NONE',  ( -5.000000000000000000, -25.87499999726881583, 0.000000000000000000 ) ) ;
#51093 = CARTESIAN_POINT ( 'NONE',  ( -4.458734124999997661, -80.47916666530105090, 2.574251347313722516 ) ) ;
#51094 = CARTESIAN_POINT ( 'NONE',  ( -4.999999999999999112, -66.91666666666667140, 2.886751345948131764 ) ) ;
#51095 = CARTESIAN_POINT ( 'NONE',  ( -48.00000000000002132, -135.0000000000000284, 4.041451884327384114 ) ) ;
#51096 = CARTESIAN_POINT ( 'NONE',  ( -4.999999999999999112, 18.20833333606451987, 2.886751345948131764 ) ) ;
#51097 = ORIENTED_EDGE ( 'NONE', *, *, #5989, .T. ) ;
#51098 = DIRECTION ( 'NONE',  ( 0.000000000000000000, 1.000000000000000000, 0.000000000000000000 ) ) ;
#51100 = CARTESIAN_POINT ( 'NONE',  ( 2.500000000000002220, -24.66666666666666430, 4.330127018922192761 ) ) ;
#51099 = CARTESIAN_POINT ( 'NONE',  ( -3.535533905932738641, -149.3750000000000000, 3.535533905932737309 ) ) ;
#51101 = CARTESIAN_POINT ( 'NONE',  ( 9.457646018065525792E-16, -27.06249999863440081, 5.148502694627439702 ) ) ;
#51102 = CARTESIAN_POINT ( 'NONE',  ( 2.229367062500001939, -87.97916666530107932, 3.861377020970579999 ) ) ;
#51103 = CARTESIAN_POINT ( 'NONE',  ( -3.535250795749689387E-16, -26.12499999726881583, -5.773502691896257311 ) ) ;
#51104 = EDGE_CURVE ( 'NONE', #15979, #14724, #15891, .T. ) ;
#51106 = ORIENTED_EDGE ( 'NONE', *, *, #35831, .F. ) ;
#51105 = CARTESIAN_POINT ( 'NONE',  ( -2.229367062500000163, -53.47916666530107221, -3.861377020970580443 ) ) ;
#51107 = CARTESIAN_POINT ( 'NONE',  ( 2.500000000000002220, -49.66666666666666430, 4.330127018922192761 ) ) ;
#51108 = CARTESIAN_POINT ( 'NONE',  ( -6.972266317189433020E-16, -18.25000000000000000, -5.000000000000000000 ) ) ;
#51110 = ORIENTED_EDGE ( 'NONE', *, *, #18173, .T. ) ;
#51109 = CARTESIAN_POINT ( 'NONE',  ( -2.229367062499996610, -4.395833331967740065, 3.861377020970582219 ) ) ;
#51111 = CARTESIAN_POINT ( 'NONE',  ( -5.000000000000000000, -73.00000000000000000, 0.000000000000000000 ) ) ;
#51112 = CARTESIAN_POINT ( 'NONE',  ( -57.19623071787016499, -137.3750000013656063, 4.297418129356382899 ) ) ;
#51113 = CARTESIAN_POINT ( 'NONE',  ( -4.458734124999999437, -44.64583333196773651, -2.574251347313719407 ) ) ;
#51114 = DIRECTION ( 'NONE',  ( 0.000000000000000000, 0.000000000000000000, 1.000000000000000000 ) ) ;
#51115 = CARTESIAN_POINT ( 'NONE',  ( -2.499999999999996447, -71.70833333060214443, 4.330127018922195425 ) ) ;
#51116 = CARTESIAN_POINT ( 'NONE',  ( -5.000000000000000000, -21.95833333060214798, -2.886751345948128211 ) ) ;
#51117 = CARTESIAN_POINT ( 'NONE',  ( -51.60603307380591787, -125.1875000013656063, -2.891590998281053704 ) ) ;
#51118 = AXIS2_PLACEMENT_3D ( 'NONE', #60956, #16877, #12045 ) ;
#51119 = CARTESIAN_POINT ( 'NONE',  ( 4.458734125000001214, -18.14583333196773651, 2.574251347313718519 ) ) ;
#51120 = AXIS2_PLACEMENT_3D ( 'NONE', #7329, #26940, #34836 ) ;
#51121 = CARTESIAN_POINT ( 'NONE',  ( 9.457646018065525792E-16, -51.31249999863440792, 5.148502694627439702 ) ) ;
#51122 = B_SPLINE_CURVE_WITH_KNOTS ( 'NONE', 3,
 ( #57794, #5010, #19157, #24630, #44237, #29121 ),
 .UNSPECIFIED., .F., .F.,
 ( 4, 2, 4 ),
 ( 0.000000000000000000, 0.002307655110370376069, 0.004615310220740751271 ),
 .UNSPECIFIED. ) ;
#51123 =( NAMED_UNIT ( * ) PLANE_ANGLE_UNIT ( ) SI_UNIT ( $, .RADIAN. ) );
#51124 = CARTESIAN_POINT ( 'NONE',  ( -4.458734125000000326, -169.2500000013655779, -1.846868145590735644 ) ) ;
#51125 = CARTESIAN_POINT ( 'NONE',  ( -4.458734124999999437, -93.56249999863440792, 0.000000000000000000 ) ) ;
#51126 = CYLINDRICAL_SURFACE ( 'NONE', #53300, 5.000000000000000000 ) ;
#51127 =( BOUNDED_CURVE ( )  B_SPLINE_CURVE ( 2, ( #52271, #23005, #57420, #18483, #13655, #25198, #9446, #33586, #33895 ),
 .UNSPECIFIED., .F., .F. ) 
 B_SPLINE_CURVE_WITH_KNOTS ( ( 3, 2, 2, 2, 3 ),
 ( 0.04464285714285714385, 0.04523809523809523697, 0.04642857142857143016, 0.04761904761904761640, 0.04821428571428571647 ),
 .UNSPECIFIED. ) 
 CURVE ( )  GEOMETRIC_REPRESENTATION_ITEM ( )  RATIONAL_B_SPLINE_CURVE ( ( 0.9330127018922194093, 0.9330127018922194093, 1.000000000000000000, 0.8660254037844387076, 1.000000000000000000, 0.8660254037844387076, 1.000000000000000000, 0.9330127018922189652, 0.9330127018922194093 ) ) 
 REPRESENTATION_ITEM ( '' )  );
#51128 = ORIENTED_EDGE ( 'NONE', *, *, #4296, .T. ) ;
#51129 = LINE ( 'NONE', #60785, #2636 ) ;
#51130 = CARTESIAN_POINT ( 'NONE',  ( 4.458734124999999437, 23.93750000136559564, -5.460374474430324690E-16 ) ) ;
#51131 = CARTESIAN_POINT ( 'NONE',  ( -59.81910112700025905, -146.3125000027312410, -2.462841084822630311 ) ) ;
#51132 = CYLINDRICAL_SURFACE ( 'NONE', #62008, 5.000000000000000000 ) ;
#51133 = EDGE_CURVE ( 'NONE', #31959, #53780, #1754, .T. ) ;
#51134 = CARTESIAN_POINT ( 'NONE',  ( -4.458734124999999437, -0.3124999986344051406, 0.000000000000000000 ) ) ;
#51135 = CARTESIAN_POINT ( 'NONE',  ( 2.229367062499998831, -95.89583333196773651, -3.861377020970580887 ) ) ;
#51136 = EDGE_CURVE ( 'NONE', #24361, #34224, #26368, .T. ) ;
#51137 = EDGE_CURVE ( 'NONE', #44836, #40158, #31247, .T. ) ;
#51138 = CARTESIAN_POINT ( 'NONE',  ( -4.458734124999999437, -150.1875000013656063, -5.460374474430324690E-16 ) ) ;
#51139 = CARTESIAN_POINT ( 'NONE',  ( -3.152548672688508926E-16, -21.81249999863440436, -5.148502694627439702 ) ) ;
#51140 = CARTESIAN_POINT ( 'NONE',  ( 2.499999999999998668, -46.33333333333333570, -4.330127018922193649 ) ) ;
#51141 = CARTESIAN_POINT ( 'NONE',  ( 4.458734125000001214, -62.14583333196774362, 2.574251347313718519 ) ) ;
#51142 = DIRECTION ( 'NONE',  ( -1.000000000000000000, 0.000000000000000000, -0.000000000000000000 ) ) ;
#51143 = CARTESIAN_POINT ( 'NONE',  ( 1.339745962155619807, 23.83034180399266688, -4.999999999999996447 ) ) ;
#51144 = CARTESIAN_POINT ( 'NONE',  ( -3.152801135295367985, -145.8125000013655779, 3.152801135295367096 ) ) ;
#51145 = CARTESIAN_POINT ( 'NONE',  ( 4.458734125000000326, 13.85416666803225993, 2.574251347313718519 ) ) ;
#51146 = VERTEX_POINT ( 'NONE', #41584 ) ;
#51147 = DIRECTION ( 'NONE',  ( -1.000000000000000000, 0.000000000000000000, 3.305092117221761110E-15 ) ) ;
#51148 = CYLINDRICAL_SURFACE ( 'NONE', #19536, 5.000000000000000000 ) ;
#51150 = CARTESIAN_POINT ( 'NONE',  ( 2.229367062499998831, -19.64583333196774007, -3.861377020970580887 ) ) ;
#51149 = CARTESIAN_POINT ( 'NONE',  ( -3.535250795749689387E-16, -83.25000000000000000, -5.773502691896257311 ) ) ;
#51152 = EDGE_CURVE ( 'NONE', #35992, #35135, #37834, .T. ) ;
#51151 = CARTESIAN_POINT ( 'NONE',  ( -2.229367062500000163, 29.27083333469892779, -3.861377020970580443 ) ) ;
#51153 = CARTESIAN_POINT ( 'NONE',  ( -5.000000000000000000, -6.083333333333336590, -2.886751345948128211 ) ) ;
#51154 = CARTESIAN_POINT ( 'NONE',  ( -50.40829686548195099, -145.0000000013656063, -1.485763867205728284 ) ) ;
#51155 = CARTESIAN_POINT ( 'NONE',  ( -4.999999999999999112, -47.79166666393548013, 2.886751345948131764 ) ) ;
#51156 = CARTESIAN_POINT ( 'NONE',  ( 5.000000000000000000, -41.37499999726880162, -6.123233995736766282E-16 ) ) ;
#51157 = CARTESIAN_POINT ( 'NONE',  ( 4.458734124999998549, 8.270833334698926009, -2.574251347313721627 ) ) ;
#51158 = CARTESIAN_POINT ( 'NONE',  ( 1.975475456537005874E-15, -56.62499999726880162, 5.000000000000000000 ) ) ;
#51159 = EDGE_CURVE ( 'NONE', #42322, #14985, #48526, .T. ) ;
#51160 = DIRECTION ( 'NONE',  ( 0.000000000000000000, 0.000000000000000000, 1.000000000000000000 ) ) ;
#51161 = CARTESIAN_POINT ( 'NONE',  ( 2.229367062499998831, 11.35416666803225993, -3.861377020970580887 ) ) ;
#51162 = CARTESIAN_POINT ( 'NONE',  ( -4.458734124999999437, -67.31249999863440792, 0.000000000000000000 ) ) ;
#51163 = CARTESIAN_POINT ( 'NONE',  ( -4.458734124999999437, -13.64583333196774184, -2.574251347313719407 ) ) ;
#51164 = CARTESIAN_POINT ( 'NONE',  ( 2.500000000000002220, -0.6666666666666660745, 4.330127018922192761 ) ) ;
#51165 = CARTESIAN_POINT ( 'NONE',  ( 1.846868145590736310, -161.6250000013656063, 4.458734124999999437 ) ) ;
#51166 = CARTESIAN_POINT ( 'NONE',  ( -6.972266317189433020E-16, -38.25000000000000000, -5.000000000000000000 ) ) ;
#51167 = CARTESIAN_POINT ( 'NONE',  ( 4.458734125000001214, -56.89583333196774362, 2.574251347313718519 ) ) ;
#51168 = CARTESIAN_POINT ( 'NONE',  ( -5.000000000000000000, -92.95833333060215864, -2.886751345948128211 ) ) ;
#51169 = VECTOR ( 'NONE', #59077, 1000.000000000000000 ) ;
#51170 = LINE ( 'NONE', #18245, #21406 ) ;
#51171 = CARTESIAN_POINT ( 'NONE',  ( 1.339745962155615144, -56.70534180126148271, 4.999999999999999112 ) ) ;
#51172 = CARTESIAN_POINT ( 'NONE',  ( -3.152548672688508926E-16, -33.56249999863440792, -5.148502694627439702 ) ) ;
#51173 = CARTESIAN_POINT ( 'NONE',  ( 0.000000000000000000, -170.0000000000000000, 5.000000000000000000 ) ) ;
#51174 = CARTESIAN_POINT ( 'NONE',  ( -4.999999999999999112, -50.91666666666667140, 2.886751345948131764 ) ) ;
#51175 = CARTESIAN_POINT ( 'NONE',  ( 6.123233995736766282E-16, -120.0000000000000000, -5.000000000000000000 ) ) ;
#51176 = CARTESIAN_POINT ( 'NONE',  ( 5.000000000000000000, -89.41666666666665719, -2.886751345948130876 ) ) ;
#51177 = ORIENTED_EDGE ( 'NONE', *, *, #52869, .F. ) ;
#51178 = CARTESIAN_POINT ( 'NONE',  ( 4.458734125000001214, -108.8958333319677365, 2.574251347313718519 ) ) ;
#51179 = CARTESIAN_POINT ( 'NONE',  ( -4.458734124999999437, -1.562499998634406140, 0.000000000000000000 ) ) ;
#51180 =( BOUNDED_CURVE ( )  B_SPLINE_CURVE ( 2, ( #22826, #4144, #48191, #18298, #47261, #63008, #22506, #42101, #3206 ),
 .UNSPECIFIED., .F., .T. ) 
 B_SPLINE_CURVE_WITH_KNOTS ( ( 3, 2, 2, 2, 3 ),
 ( 0.5979166666666666519, 0.5986111111111110938, 0.5999999999999999778, 0.6013888888888888618, 0.6020833333333333037 ),
 .UNSPECIFIED. ) 
 CURVE ( )  GEOMETRIC_REPRESENTATION_ITEM ( )  RATIONAL_B_SPLINE_CURVE ( ( 0.9330127018922194093, 0.9330127018922194093, 1.000000000000000000, 0.8660254037844387076, 1.000000000000000000, 0.8660254037844387076, 1.000000000000000000, 0.9330127018922194093, 0.9330127018922194093 ) ) 
 REPRESENTATION_ITEM ( '' )  );
#51181 = FACE_OUTER_BOUND ( 'NONE', #52485, .T. ) ;
#51182 = CARTESIAN_POINT ( 'NONE',  ( -4.999999999999999112, -5.916666666666666963, 2.886751345948131764 ) ) ;
#51183 = CARTESIAN_POINT ( 'NONE',  ( -2.229367062500000163, -70.47916666530107932, -3.861377020970580443 ) ) ;
#51184 = CARTESIAN_POINT ( 'NONE',  ( -5.000000000000000000, -26.00000000000000355, 0.000000000000000000 ) ) ;
#51185 = CARTESIAN_POINT ( 'NONE',  ( -5.000000000000000000, -4.958333330602147981, -2.886751345948128211 ) ) ;
#51187 = ORIENTED_EDGE ( 'NONE', *, *, #34124, .T. ) ;
#51186 = CARTESIAN_POINT ( 'NONE',  ( -4.458734124999999437, -38.31249999863439371, 0.000000000000000000 ) ) ;
#51188 = CARTESIAN_POINT ( 'NONE',  ( 5.000000000000000000, -22.29166666393548013, -2.886751345948130876 ) ) ;
#51190 = VERTEX_POINT ( 'NONE', #60920 ) ;
#51189 = CARTESIAN_POINT ( 'NONE',  ( 9.457646018065525792E-16, 14.68750000136559208, 5.148502694627439702 ) ) ;
#51191 = CARTESIAN_POINT ( 'NONE',  ( 5.000000000000000888, -81.45833333060213022, 2.886751345948126879 ) ) ;
#51192 = CARTESIAN_POINT ( 'NONE',  ( 1.060575238724906964E-15, -54.75000000000000000, 5.773502691896257311 ) ) ;
#51193 = CARTESIAN_POINT ( 'NONE',  ( 1.846868145590736310, -161.8750000013656063, 4.458734124999999437 ) ) ;
#51194 = CARTESIAN_POINT ( 'NONE',  ( 2.229367062499998831, -31.89583333196773651, -3.861377020970580887 ) ) ;
#51195 = DIRECTION ( 'NONE',  ( -0.000000000000000000, 1.000000000000000000, -0.000000000000000000 ) ) ;
#51196 = CARTESIAN_POINT ( 'NONE',  ( 2.229367062499998831, -75.64583333196773651, -3.861377020970580887 ) ) ;
#51197 = CARTESIAN_POINT ( 'NONE',  ( -5.000000000000000888, -168.4375000000000568, 2.071067811865474617 ) ) ;
#51198 = CARTESIAN_POINT ( 'NONE',  ( 2.229367062499998831, -88.64583333196773651, -3.861377020970580887 ) ) ;
#51199 = CARTESIAN_POINT ( 'NONE',  ( -54.64476657466781973, -136.0625000013656063, -4.444560631937228834 ) ) ;
#51200 = CARTESIAN_POINT ( 'NONE',  ( -4.458734124999999437, -34.64583333196773651, -2.574251347313719407 ) ) ;
#51201 = CARTESIAN_POINT ( 'NONE',  ( 5.000000000000000000, -83.29166666393547303, -2.886751345948130876 ) ) ;
#51202 = ORIENTED_EDGE ( 'NONE', *, *, #28756, .T. ) ;
#51203 = CARTESIAN_POINT ( 'NONE',  ( 2.229367062500001939, -78.22916666530106511, 3.861377020970579999 ) ) ;
#51204 = CARTESIAN_POINT ( 'NONE',  ( 1.339745962155586056, 3.294658198738519506, 5.000000000000015987 ) ) ;
#51205 = EDGE_LOOP ( 'NONE', ( #46059, #39588, #50491, #6635 ) ) ;
#51206 = CYLINDRICAL_SURFACE ( 'NONE', #59384, 5.000000000000000000 ) ;
#51207 = VECTOR ( 'NONE', #57509, 1000.000000000000000 ) ;
#51208 = LINE ( 'NONE', #16466, #42475 ) ;
#51209 = CARTESIAN_POINT ( 'NONE',  ( -4.458734124999998549, -66.47916666530106511, 2.574251347313722516 ) ) ;
#51210 = CARTESIAN_POINT ( 'NONE',  ( -2.229367062499996610, -9.395833331967736513, 3.861377020970582219 ) ) ;
#51211 = ORIENTED_EDGE ( 'NONE', *, *, #26009, .T. ) ;
#51212 = CARTESIAN_POINT ( 'NONE',  ( -58.24261429053147765, -149.2500000000000284, -3.805975901505573855 ) ) ;
#51213 = EDGE_CURVE ( 'NONE', #13355, #2572, #41270, .T. ) ;
#51214 = ORIENTED_EDGE ( 'NONE', *, *, #39188, .F. ) ;
#51215 = CARTESIAN_POINT ( 'NONE',  ( 4.458734125000001214, -8.145833331967736513, 2.574251347313718519 ) ) ;
#51216 = DIRECTION ( 'NONE',  ( 0.000000000000000000, 0.000000000000000000, 1.000000000000000000 ) ) ;
#51217 = CARTESIAN_POINT ( 'NONE',  ( -2.229367062499996610, 9.854166668032261711, 3.861377020970582219 ) ) ;
#51218 = FACE_OUTER_BOUND ( 'NONE', #53670, .T. ) ;
#51219 = CARTESIAN_POINT ( 'NONE',  ( 4.458734124999999437, -158.4375000013655779, 0.000000000000000000 ) ) ;
#51220 = ADVANCED_FACE ( 'NONE', ( #55770 ), #2074, .T. ) ;
#51221 = CARTESIAN_POINT ( 'NONE',  ( 1.339745962155612702, -75.16965819600731891, -5.000000000000000000 ) ) ;
#51222 = ORIENTED_EDGE ( 'NONE', *, *, #23961, .T. ) ;
#51223 = CARTESIAN_POINT ( 'NONE',  ( 4.458734124999998549, -85.72916666530107932, -2.574251347313721627 ) ) ;
#51224 = DIRECTION ( 'NONE',  ( -0.000000000000000000, 1.000000000000000000, -0.000000000000000000 ) ) ;
#51225 = CARTESIAN_POINT ( 'NONE',  ( -4.458734124999999437, -3.395833331967739177, -2.574251347313719407 ) ) ;
#51226 = EDGE_CURVE ( 'NONE', #17875, #51190, #55120, .T. ) ;
#51227 = CARTESIAN_POINT ( 'NONE',  ( -9.184850993605147944E-16, -140.2500000000000000, 5.000000000000000000 ) ) ;
#51228 = CARTESIAN_POINT ( 'NONE',  ( -2.500000000000000444, -29.04166666393548013, -4.330127018922193649 ) ) ;
#51229 = CARTESIAN_POINT ( 'NONE',  ( 6.123233995736766282E-16, -170.0000000000000000, -5.000000000000000000 ) ) ;
#51230 = CARTESIAN_POINT ( 'NONE',  ( 9.457646018065525792E-16, 24.93750000136559208, 5.148502694627439702 ) ) ;
#51231 = DIRECTION ( 'NONE',  ( -0.6485228581062915110, 0.000000000000000000, -0.7611951803011149931 ) ) ;
#51232 = CARTESIAN_POINT ( 'NONE',  ( -4.458734124999999437, 29.68750000136559208, 0.000000000000000000 ) ) ;
#51233 = EDGE_CURVE ( 'NONE', #35553, #27844, #61706, .T. ) ;
#51234 = CARTESIAN_POINT ( 'NONE',  ( 4.458734124999998549, -52.72916666530107221, -2.574251347313721627 ) ) ;
#51235 = CARTESIAN_POINT ( 'NONE',  ( -3.152548672688508926E-16, -38.81249999863440081, -5.148502694627439702 ) ) ;
#51236 = CARTESIAN_POINT ( 'NONE',  ( -2.229367062499996610, -0.3958333319677397322, 3.861377020970582219 ) ) ;
#51237 = CARTESIAN_POINT ( 'NONE',  ( 0.000000000000000000, -170.0000000000000000, 5.000000000000000000 ) ) ;
#51238 = CARTESIAN_POINT ( 'NONE',  ( -2.500000000000000444, 14.83333333333333215, -4.330127018922193649 ) ) ;
#51239 = EDGE_CURVE ( 'NONE', #16219, #59810, #44381, .T. ) ;
#51240 = CARTESIAN_POINT ( 'NONE',  ( 2.071067811865475505, -146.9375000027311842, -5.000000000000000888 ) ) ;
#51241 = CARTESIAN_POINT ( 'NONE',  ( 1.339745962155612702, -33.16965819600733312, -5.000000000000000000 ) ) ;
#51242 = CARTESIAN_POINT ( 'NONE',  ( -4.458734124999998549, -45.22916666530106511, 2.574251347313722516 ) ) ;
#51243 = CARTESIAN_POINT ( 'NONE',  ( 5.000000000000000000, -80.29166666393545881, -2.886751345948129988 ) ) ;
#51244 = CARTESIAN_POINT ( 'NONE',  ( -50.55543936806279248, -140.3125000013656063, 0.3552334253322060320 ) ) ;
#51245 = DIRECTION ( 'NONE',  ( 0.000000000000000000, 0.000000000000000000, 1.000000000000000000 ) ) ;
#51246 = EDGE_CURVE ( 'NONE', #12673, #15879, #32946, .T. ) ;
#51247 = CARTESIAN_POINT ( 'NONE',  ( 2.499999999999998668, -36.33333333333332860, -4.330127018922193649 ) ) ;
#51248 = CARTESIAN_POINT ( 'NONE',  ( 2.229367062499998831, -87.89583333196773651, -3.861377020970580887 ) ) ;
#51249 = CARTESIAN_POINT ( 'NONE',  ( -4.458734124999999437, -163.2500000013656063, -1.846868145590735644 ) ) ;
#51250 = DIRECTION ( 'NONE',  ( 0.000000000000000000, 0.000000000000000000, 1.000000000000000000 ) ) ;
#51251 = CARTESIAN_POINT ( 'NONE',  ( 1.060575238724906964E-15, -33.75000000000000000, 5.773502691896257311 ) ) ;
#51252 = CARTESIAN_POINT ( 'NONE',  ( 2.730187237215162345E-16, -141.1875000013656063, -4.458734124999999437 ) ) ;
#51253 = ORIENTED_EDGE ( 'NONE', *, *, #46011, .T. ) ;
#51254 = CARTESIAN_POINT ( 'NONE',  ( 2.229367062499998831, 22.10416666803225993, -3.861377020970580887 ) ) ;
#51255 = EDGE_LOOP ( 'NONE', ( #54289, #19771, #7743, #56256 ) ) ;
#51256 = CARTESIAN_POINT ( 'NONE',  ( 2.229367062499998831, -89.64583333196773651, -3.861377020970580887 ) ) ;
#51257 = CARTESIAN_POINT ( 'NONE',  ( -4.458734124999998549, 11.52083333469892779, 2.574251347313722516 ) ) ;
#51258 = AXIS2_PLACEMENT_3D ( 'NONE', #36455, #12002, #31630 ) ;
#51259 = CARTESIAN_POINT ( 'NONE',  ( 5.000000000000000000, 15.62500000273118417, -6.123233995736766282E-16 ) ) ;
#51260 = CARTESIAN_POINT ( 'NONE',  ( -5.000000000000000000, -60.00000000000000000, 0.000000000000000000 ) ) ;
#51261 = CARTESIAN_POINT ( 'NONE',  ( -4.999999999999999112, 8.083333333333330373, 2.886751345948131764 ) ) ;
#51262 =( BOUNDED_CURVE ( )  B_SPLINE_CURVE ( 2, ( #6432, #2558, #1939, #36326, #21857, #12196, #55954, #7064, #31812, #51759, #51447, #21214, #22172, #26043, #61419, #7703, #2881, #17343, #40822, #56592, #12512, #32123, #61733, #27306, #46931, #22495, #17662, #37278, #56906, #12825, #32445, #60468, #50807, #16393, #11558, #36012, #55644, #53324, #33084, #33704, #9257, #4131, #62680, #52698, #27930, #18602, #62046, #52396, #13145, #32765, #13466, #8015, #8632, #3195, #27619, #48494, #47551, #8944, #17962, #22811, #38831, #18904, #28872, #3501, #33390, #38518, #42403, #37585, #23115, #4431, #28558, #43040, #42719, #57226, #28244, #24058, #58146, #8331, #57540, #48179, #14075, #43348, #62362, #43655, #63296, #47858, #57850, #14392, #47249, #19214, #58468, #3816, #18285, #52074, #37909, #23439, #38228, #23753, #13768, #53005, #62994, #6036, #35291, #15029, #15672, #54911, #63615, #19852, #49444, #59747, #58775, #19535, #14705, #29811, #60063, #59425, #10838, #34978, #39466, #25641, #30454, #9880, #54594, #43969, #48803, #20822, #34645, #898, #24683, #49122, #34324, #45257, #50079, #59102, #54269, #5386, #10516, #25001, #53949, #34015, #44940, #20505, #29486, #10209, #30130, #40103, #40423, #39149, #44611, #29177, #25320, #49759, #5064, #44292, #24367, #5705, #1223, #254, #53637, #571, #20180, #39778, #9570, #4742, #15354, #17259, #31097, #55874, #51042, #2175, #21781, #6985, #61336, #16313, #26596, #12109, #50718, #27226, #31736, #15987, #22413, #35934, #36882, #11786, #46536, #46213, #16625, #30782, #31404, #11160, #41373, #61019, #16945, #40740, #21459, #36558, #35612, #11477, #55561, #6662, #56189, #55238, #41059, #50404, #26269, #56512, #12433, #45891, #6353, #51366, #1853, #7307, #26919, #60705, #7622, #25957, #45574, #2477, #36247, #22090, #1530, #32045, #60387, #21135, #41689, #51681, #46847, #2794, #42012, #23359, #8250, #22730, #33310, #23041, #18524, #37828, #47471, #56829, #42644, #12747, #62285, #8553, #42328, #17889, #18207, #57462, #13064, #37509, #13381, #13691, #33002, #17586, #27850, #37203, #61968, #52930, #28482, #57149, #32367, #28166, #32684, #38144, #48098, #52619, #47781, #3738, #52315, #3425, #42958, #62601, #57769, #8867, #3112, #51991, #27537, #4052, #23670, #43268, #62907, #18821, #61652, #7935, #47169, #56081, #31299, #21985, #1748, #55764, #16520, #36143, #16834, #11366, #36454, #6554, #30989, #51886, #50936, #12333, #21349, #26168, #42225, #22304, #56722, #6877, #36777, #41903, #45789, #40953, #26491, #7827, #31944, #46427, #46107, #60601, #31629, #27429, #61550 ),
 .UNSPECIFIED., .F., .F. ) 
 B_SPLINE_CURVE_WITH_KNOTS ( ( 3, 2, 2, 2, 2, 2, 2, 2, 2, 2, 2, 2, 2, 2, 2, 2, 2, 2, 2, 2, 2, 2, 2, 2, 2, 2, 2, 2, 2, 2, 2, 2, 2, 2, 2, 2, 2, 2, 2, 2, 2, 2, 2, 2, 2, 2, 2, 2, 2, 2, 2, 2, 2, 2, 2, 2, 2, 2, 2, 2, 2, 2, 2, 2, 2, 2, 2, 2, 2, 2, 2, 2, 2, 2, 2, 2, 2, 2, 2, 2, 2, 2, 2, 2, 2, 2, 2, 2, 2, 2, 2, 2, 2, 2, 2, 2, 2, 2, 2, 2, 2, 2, 2, 2, 2, 2, 2, 2, 2, 2, 2, 2, 2, 2, 2, 2, 2, 2, 2, 2, 2, 2, 2, 2, 2, 2, 2, 2, 2, 2, 2, 2, 2, 2, 2, 2, 2, 2, 2, 2, 2, 2, 2, 2, 2, 2, 2, 2, 2, 2, 2, 2, 2, 2, 2, 2, 2, 2, 3 ),
 ( 0.000000000000000000, 0.004166666666666666609, 0.008333333333333333218, 0.01250000000000000243, 0.01666666666666666644, 0.02083333333333333218, 0.02500000000000000486, 0.02916666666666666713, 0.03333333333333333287, 0.03749999999999999861, 0.04166666666666666435, 0.04583333333333333010, 0.05000000000000000971, 0.05416666666666666852, 0.05833333333333333426, 0.06250000000000000000, 0.06666666666666666574, 0.07083333333333333148, 0.07499999999999999722, 0.07916666666666666297, 0.08333333333333332871, 0.08749999999999999445, 0.09166666666666666019, 0.09583333333333333981, 0.1000000000000000194, 0.1041666666666666713, 0.1083333333333333370, 0.1124999999999999889, 0.1166666666666666685, 0.1208333333333333204, 0.1250000000000000000, 0.1291666666666666796, 0.1333333333333333315, 0.1375000000000000111, 0.1416666666666666630, 0.1458333333333333426, 0.1499999999999999944, 0.1541666666666666741, 0.1583333333333333259, 0.1625000000000000056, 0.1666666666666666574, 0.1708333333333333370, 0.1749999999999999889, 0.1791666666666666685, 0.1833333333333333204, 0.1875000000000000000, 0.1916666666666666796, 0.1958333333333333592, 0.2000000000000000389, 0.2041666666666666630, 0.2083333333333333426, 0.2125000000000000222, 0.2166666666666666741, 0.2208333333333333259, 0.2249999999999999778, 0.2291666666666666574, 0.2333333333333333370, 0.2374999999999999611, 0.2416666666666666408, 0.2458333333333333204, 0.2500000000000000000, 0.2541666666666666519, 0.2583333333333333592, 0.2625000000000000111, 0.2666666666666666630, 0.2708333333333333148, 0.2750000000000000222, 0.2791666666666666741, 0.2833333333333333259, 0.2874999999999999778, 0.2916666666666666852, 0.2958333333333333370, 0.2999999999999999889, 0.3041666666666666408, 0.3083333333333333481, 0.3125000000000000000, 0.3166666666666666519, 0.3208333333333333592, 0.3250000000000000111, 0.3291666666666666630, 0.3333333333333333148, 0.3375000000000000222, 0.3416666666666666741, 0.3458333333333333259, 0.3499999999999999778, 0.3541666666666666852, 0.3583333333333333370, 0.3624999999999999889, 0.3666666666666666408, 0.3708333333333333481, 0.3750000000000000000, 0.3791666666666666519, 0.3833333333333333592, 0.3874999999999999556, 0.3916666666666667185, 0.3958333333333333148, 0.4000000000000000777, 0.4041666666666666741, 0.4083333333333333259, 0.4124999999999999223, 0.4166666666666666852, 0.4208333333333332815, 0.4250000000000000444, 0.4291666666666666408, 0.4333333333333333481, 0.4375000000000000000, 0.4416666666666666519, 0.4458333333333333592, 0.4499999999999999556, 0.4541666666666667185, 0.4583333333333333148, 0.4625000000000000777, 0.4666666666666666741, 0.4708333333333333259, 0.4749999999999999223, 0.4791666666666666852, 0.4833333333333332815, 0.4875000000000000444, 0.4916666666666666408, 0.4958333333333333481, 0.5000000000000000000, 0.5041666666666666519, 0.5083333333333333037, 0.5124999999999999556, 0.5166666666666667185, 0.5208333333333333703, 0.5250000000000000222, 0.5291666666666666741, 0.5333333333333333259, 0.5374999999999999778, 0.5416666666666666297, 0.5458333333333332815, 0.5500000000000000444, 0.5541666666666666963, 0.5583333333333333481, 0.5625000000000000000, 0.5666666666666666519, 0.5708333333333333037, 0.5749999999999999556, 0.5791666666666667185, 0.5833333333333333703, 0.5875000000000000222, 0.5916666666666666741, 0.5958333333333333259, 0.5999999999999999778, 0.6041666666666666297, 0.6083333333333332815, 0.6125000000000000444, 0.6166666666666666963, 0.6208333333333333481, 0.6250000000000000000, 0.6291666666666666519, 0.6333333333333333037, 0.6374999999999999556, 0.6416666666666667185, 0.6458333333333333703, 0.6500000000000000222, 0.6541666666666666741, 0.6562500000437863079 ),
 .UNSPECIFIED. ) 
 CURVE ( )  GEOMETRIC_REPRESENTATION_ITEM ( )  RATIONAL_B_SPLINE_CURVE ( ( 1.000000000000000000, 0.9238795325112867385, 1.000000000000000000, 0.9238795325112867385, 1.000000000000000000, 0.9238795325112867385, 1.000000000000000000, 0.9238795325112867385, 1.000000000000000000, 0.9238795325112867385, 1.000000000000000000, 0.9238795325112867385, 1.000000000000000000, 0.9238795325112867385, 1.000000000000000000, 0.9238795325112867385, 1.000000000000000000, 0.9238795325112867385, 1.000000000000000000, 0.9238795325112867385, 1.000000000000000000, 0.9238795325112867385, 1.000000000000000000, 0.9238795325112867385, 1.000000000000000000, 0.9238795325112867385, 1.000000000000000000, 0.9238795325112867385, 1.000000000000000000, 0.9238795325112867385, 1.000000000000000000, 0.9238795325112867385, 1.000000000000000000, 0.9238795325112867385, 1.000000000000000000, 0.9238795325112867385, 1.000000000000000000, 0.9238795325112867385, 1.000000000000000000, 0.9238795325112867385, 1.000000000000000000, 0.9238795325112867385, 1.000000000000000000, 0.9238795325112867385, 1.000000000000000000, 0.9238795325112867385, 1.000000000000000000, 0.9238795325112867385, 1.000000000000000000, 0.9238795325112867385, 1.000000000000000000, 0.9238795325112867385, 1.000000000000000000, 0.9238795325112867385, 1.000000000000000000, 0.9238795325112867385, 1.000000000000000000, 0.9238795325112867385, 1.000000000000000000, 0.9238795325112867385, 1.000000000000000000, 0.9238795325112867385, 1.000000000000000000, 0.9238795325112867385, 1.000000000000000000, 0.9238795325112867385, 1.000000000000000000, 0.9238795325112867385, 1.000000000000000000, 0.9238795325112867385, 1.000000000000000000, 0.9238795325112867385, 1.000000000000000000, 0.9238795325112867385, 1.000000000000000000, 0.9238795325112867385, 1.000000000000000000, 0.9238795325112867385, 1.000000000000000000, 0.9238795325112867385, 1.000000000000000000, 0.9238795325112867385, 1.000000000000000000, 0.9238795325112867385, 1.000000000000000000, 0.9238795325112867385, 1.000000000000000000, 0.9238795325112867385, 1.000000000000000000, 0.9238795325112867385, 1.000000000000000000, 0.9238795325112867385, 1.000000000000000000, 0.9238795325112867385, 1.000000000000000000, 0.9238795325112867385, 1.000000000000000000, 0.9238795325112867385, 1.000000000000000000, 0.9238795325112867385, 1.000000000000000000, 0.9238795325112867385, 1.000000000000000000, 0.9238795325112867385, 1.000000000000000000, 0.9238795325112867385, 1.000000000000000000, 0.9238795325112867385, 1.000000000000000000, 0.9238795325112867385, 1.000000000000000000, 0.9238795325112867385, 1.000000000000000000, 0.9238795325112867385, 1.000000000000000000, 0.9238795325112867385, 1.000000000000000000, 0.9238795325112867385, 1.000000000000000000, 0.9238795325112867385, 1.000000000000000000, 0.9238795325112867385, 1.000000000000000000, 0.9238795325112867385, 1.000000000000000000, 0.9238795325112867385, 1.000000000000000000, 0.9238795325112867385, 1.000000000000000000, 0.9238795325112867385, 1.000000000000000000, 0.9238795325112867385, 1.000000000000000000, 0.9238795325112867385, 1.000000000000000000, 0.9238795325112867385, 1.000000000000000000, 0.9238795325112867385, 1.000000000000000000, 0.9238795325112867385, 1.000000000000000000, 0.9238795325112867385, 1.000000000000000000, 0.9238795325112867385, 1.000000000000000000, 0.9238795325112867385, 1.000000000000000000, 0.9238795325112867385, 1.000000000000000000, 0.9238795325112867385, 1.000000000000000000, 0.9238795325112867385, 1.000000000000000000, 0.9238795325112867385, 1.000000000000000000, 0.9238795325112867385, 1.000000000000000000, 0.9238795325112867385, 1.000000000000000000, 0.9238795325112867385, 1.000000000000000000, 0.9238795325112867385, 1.000000000000000000, 0.9238795325112867385, 1.000000000000000000, 0.9238795325112867385, 1.000000000000000000, 0.9238795325112867385, 1.000000000000000000, 0.9238795325112867385, 1.000000000000000000, 0.9238795325112867385, 1.000000000000000000, 0.9238795325112867385, 1.000000000000000000, 0.9238795325112867385, 1.000000000000000000, 0.9238795325112867385, 1.000000000000000000, 0.9238795325112867385, 1.000000000000000000, 0.9238795325112867385, 1.000000000000000000, 0.9238795325112867385, 1.000000000000000000, 0.9238795325112867385, 1.000000000000000000, 0.9238795325112867385, 1.000000000000000000, 0.9238795325112867385, 1.000000000000000000, 0.9238795325112867385, 1.000000000000000000, 0.9238795325112867385, 1.000000000000000000, 0.9238795325112867385, 1.000000000000000000, 0.9238795325112867385, 1.000000000000000000, 0.9238795325112867385, 1.000000000000000000, 0.9238795325112867385, 1.000000000000000000, 0.9238795325112867385, 1.000000000000000000, 0.9238795325112867385, 1.000000000000000000, 0.9238795325112867385, 1.000000000000000000, 0.9238795325112867385, 1.000000000000000000, 0.9238795325112867385, 1.000000000000000000, 0.9238795325112867385, 1.000000000000000000, 0.9238795325112867385, 1.000000000000000000, 0.9238795325112867385, 1.000000000000000000, 0.9238795325112867385, 1.000000000000000000, 0.9238795325112867385, 1.000000000000000000, 0.9238795325112867385, 1.000000000000000000, 0.9238795325112867385, 1.000000000000000000, 0.9238795325112867385, 1.000000000000000000, 0.9238795325112867385, 1.000000000000000000, 0.9238795325112867385, 1.000000000000000000, 0.9238795325112867385, 1.000000000000000000, 0.9238795325112867385, 1.000000000000000000, 0.9238795325112867385, 1.000000000000000000, 0.9238795325112867385, 1.000000000000000000, 0.9238795325112867385, 1.000000000000000000, 0.9238795325112867385, 1.000000000000000000, 0.9238795325112867385, 1.000000000000000000, 0.9238795325112867385, 1.000000000000000000, 0.9238795325112867385, 1.000000000000000000, 0.9238795325112867385, 1.000000000000000000, 0.9238795325112867385, 1.000000000000000000, 0.9238795325112867385, 1.000000000000000000, 0.9238795325112867385, 1.000000000000000000, 0.9238795325112867385, 1.000000000000000000, 0.9238795325112867385, 1.000000000000000000, 0.9238795325112867385, 1.000000000000000000, 0.9238795325112867385, 1.000000000000000000, 0.9238795325112867385, 1.000000000000000000, 0.9238795325112867385, 1.000000000000000000, 0.9238795325112867385, 1.000000000000000000, 0.9238795325112867385, 1.000000000000000000, 0.9238795325112867385, 1.000000000000000000, 0.9238795325112867385, 1.000000000000000000, 0.9238795325112867385, 1.000000000000000000, 0.9238795325112867385, 1.000000000000000000, 0.9238795325112867385, 1.000000000000000000, 0.9238795325112867385, 1.000000000000000000, 0.9238795325112867385, 1.000000000000000000, 0.9238795325112867385, 1.000000000000000000, 0.9238795325112867385, 1.000000000000000000, 0.9238795325112867385, 1.000000000000000000, 0.9238795325112867385, 1.000000000000000000, 0.9238795325112867385, 1.000000000000000000, 0.9238795325112867385, 1.000000000000000000, 0.9238795325112867385, 1.000000000000000000, 0.9238795325112867385, 1.000000000000000000, 0.9238795325112867385, 1.000000000000000000, 0.9238795325112867385, 1.000000000000000000, 0.9238795325112867385, 1.000000000000000000, 0.9238795325112867385, 1.000000000000000000, 0.9238795325112867385, 1.000000000000000000, 0.9619397654557151345, 0.9619397662556433692 ) ) 
 REPRESENTATION_ITEM ( '' )  );
#51263 = CARTESIAN_POINT ( 'NONE',  ( -2.229367062499996610, -55.14583333196773651, 3.861377020970582219 ) ) ;
#51264 = CARTESIAN_POINT ( 'NONE',  ( 7.915340744421234476, 3.857466640755322640, -7.913699667209310284 ) ) ;
#51265 = CYLINDRICAL_SURFACE ( 'NONE', #61182, 5.000000000000000000 ) ;
#51266 = CARTESIAN_POINT ( 'NONE',  ( 5.000000000000000000, -40.29166666393548013, -2.886751345948130876 ) ) ;
#51267 = CARTESIAN_POINT ( 'NONE',  ( -4.999999999999998224, 0.2083333360645180099, 2.886751345948131764 ) ) ;
#51268 = CARTESIAN_POINT ( 'NONE',  ( -5.000000000000000000, 18.04166666939785557, -2.886751345948128211 ) ) ;
#51269 = CARTESIAN_POINT ( 'NONE',  ( 1.060575238724906964E-15, -41.74999999999999289, 5.773502691896257311 ) ) ;
#51270 = CARTESIAN_POINT ( 'NONE',  ( -2.499999999999996447, 13.29166666939785379, 4.330127018922195425 ) ) ;
#51272 = CARTESIAN_POINT ( 'NONE',  ( 4.458734124999999437, -13.06249999863440259, -5.460374474430324690E-16 ) ) ;
#51271 = CARTESIAN_POINT ( 'NONE',  ( -4.999999999999998224, -44.91666666666666430, 2.886751345948131764 ) ) ;
#51273 = CARTESIAN_POINT ( 'NONE',  ( -5.007715329123872641E-16, -8.660254037844399733, -7.422398894150038728 ) ) ;
#51274 = CARTESIAN_POINT ( 'NONE',  ( -4.458734124999998549, -59.22916666530106511, 2.574251347313722516 ) ) ;
#51275 = CARTESIAN_POINT ( 'NONE',  ( 1.846868145590736310, -152.8750000013655779, 4.458734124999999437 ) ) ;
#51276 = CARTESIAN_POINT ( 'NONE',  ( -2.229367062500000163, -69.47916666530107932, -3.861377020970580443 ) ) ;
#51277 = CARTESIAN_POINT ( 'NONE',  ( -55.35523342533222291, -145.5625000013656063, 4.444560631937231499 ) ) ;
#51278 = CARTESIAN_POINT ( 'NONE',  ( 2.229367062499998831, -20.89583333196774007, -3.861377020970580887 ) ) ;
#51279 =( BOUNDED_CURVE ( )  B_SPLINE_CURVE ( 2, ( #6293, #20443, #5004, #30723, #5645, #25898, #40684, #195, #508 ),
 .UNSPECIFIED., .F., .F. ) 
 B_SPLINE_CURVE_WITH_KNOTS ( ( 3, 2, 2, 2, 3 ),
 ( 0.04464285714285714385, 0.04523809523809523697, 0.04642857142857143016, 0.04761904761904761640, 0.04821428571428571647 ),
 .UNSPECIFIED. ) 
 CURVE ( )  GEOMETRIC_REPRESENTATION_ITEM ( )  RATIONAL_B_SPLINE_CURVE ( ( 0.9330127018922194093, 0.9330127018922194093, 1.000000000000000000, 0.8660254037844387076, 1.000000000000000000, 0.8660254037844387076, 1.000000000000000000, 0.9330127018922189652, 0.9330127018922194093 ) ) 
 REPRESENTATION_ITEM ( '' )  );
#51280 = CARTESIAN_POINT ( 'NONE',  ( 2.500000000000002220, -63.54166666393547303, 4.330127018922192761 ) ) ;
#51281 = VERTEX_POINT ( 'NONE', #9082 ) ;
#51282 = CARTESIAN_POINT ( 'NONE',  ( 2.500000000000002220, -85.54166666393547303, 4.330127018922192761 ) ) ;
#51283 = ORIENTED_EDGE ( 'NONE', *, *, #57306, .T. ) ;
#51284 = CARTESIAN_POINT ( 'NONE',  ( -4.458734124999999437, -60.64583333196774362, -2.574251347313719407 ) ) ;
#51286 = CARTESIAN_POINT ( 'NONE',  ( 1.975475456537005874E-15, -103.7500000000000000, 5.000000000000000000 ) ) ;
#51285 = PLANE ( 'NONE',  #11203 ) ;
#51287 = CARTESIAN_POINT ( 'NONE',  ( -3.152801135295367096, -151.0625000013655779, -3.152801135295367541 ) ) ;
#51288 = ORIENTED_EDGE ( 'NONE', *, *, #54601, .F. ) ;
#51289 = CARTESIAN_POINT ( 'NONE',  ( -2.499999999999996447, -7.708333330602144429, 4.330127018922195425 ) ) ;
#51290 = CARTESIAN_POINT ( 'NONE',  ( 7.263825692932297962, 4.945657111639574666, -7.907570769506046204 ) ) ;
#51291 = LINE ( 'NONE', #17808, #62743 ) ;
#51292 = CARTESIAN_POINT ( 'NONE',  ( -2.229367062500000163, -49.72916666530107221, -3.861377020970580443 ) ) ;
#51293 = ORIENTED_EDGE ( 'NONE', *, *, #443, .T. ) ;
#51294 = LINE ( 'NONE', #41606, #23425 ) ;
#51295 = CARTESIAN_POINT ( 'NONE',  ( 2.229367062499998831, 7.354166668032259935, -3.861377020970580887 ) ) ;
#51296 = CARTESIAN_POINT ( 'NONE',  ( 4.458734124999999437, 22.18750000136559564, -5.460374474430324690E-16 ) ) ;
#51297 = CARTESIAN_POINT ( 'NONE',  ( -52.10840900171896806, -149.1875000013656063, 3.393966926194110556 ) ) ;
#51298 = CARTESIAN_POINT ( 'NONE',  ( 1.339745962155729053, -78.16965819600734733, -4.999999999999933387 ) ) ;
#51299 = CARTESIAN_POINT ( 'NONE',  ( -4.458734124999999437, -168.0000000013656347, -1.846868145590735644 ) ) ;
#51300 = AXIS2_PLACEMENT_3D ( 'NONE', #18118, #47702, #33233 ) ;
#51301 = ORIENTED_EDGE ( 'NONE', *, *, #54250, .T. ) ;
#51302 = CARTESIAN_POINT ( 'NONE',  ( 2.229367062499998831, -69.64583333196773651, -3.861377020970580887 ) ) ;
#51303 = CARTESIAN_POINT ( 'NONE',  ( 0.3306966981845720355, 8.469326210127405830, -7.349897473153450989 ) ) ;
#51304 = CARTESIAN_POINT ( 'NONE',  ( -4.458734124999999437, 12.60416666803225993, -2.574251347313719407 ) ) ;
#51305 = CARTESIAN_POINT ( 'NONE',  ( 5.000000000000000888, -157.0625000027311842, -2.071067811865475505 ) ) ;
#51306 = CARTESIAN_POINT ( 'NONE',  ( 4.458734124999998549, -53.97916666530107221, -2.574251347313721627 ) ) ;
#51307 = CARTESIAN_POINT ( 'NONE',  ( 5.000000000000000000, -15.29166666393548368, -2.886751345948129988 ) ) ;
#51308 = CARTESIAN_POINT ( 'NONE',  ( -6.972266317189433020E-16, -33.12499999726880873, -5.000000000000000000 ) ) ;
#51309 = DIRECTION ( 'NONE',  ( 0.8660254037844313801, -0.5000000000000125455, 0.000000000000000000 ) ) ;
#51310 = CYLINDRICAL_SURFACE ( 'NONE', #36783, 5.000000000000000000 ) ;
#51311 = CARTESIAN_POINT ( 'NONE',  ( -2.229367062499996610, -20.39583333196774007, 3.861377020970582219 ) ) ;
#51312 = VERTEX_POINT ( 'NONE', #23878 ) ;
#51313 = CARTESIAN_POINT ( 'NONE',  ( -8.660254037844341113, 45.00000000000000000, 6.047423072554883697E-14 ) ) ;
#51314 = CARTESIAN_POINT ( 'NONE',  ( -3.535250795749689387E-16, 29.74999999999999645, -5.773502691896257311 ) ) ;
#51315 = CARTESIAN_POINT ( 'NONE',  ( 2.071067811865475505, -158.9375000027311842, -5.000000000000000888 ) ) ;
#51316 = ORIENTED_EDGE ( 'NONE', *, *, #23681, .F. ) ;
#51317 = CARTESIAN_POINT ( 'NONE',  ( -4.458734124999999437, -100.5624999986344079, 0.000000000000000000 ) ) ;
#51318 = CARTESIAN_POINT ( 'NONE',  ( -4.458734124999999437, -24.39583333196773651, -2.574251347313719407 ) ) ;
#51319 = CARTESIAN_POINT ( 'NONE',  ( 5.000000000000000000, -60.29166666393546592, -2.886751345948129988 ) ) ;
#51320 = CARTESIAN_POINT ( 'NONE',  ( -50.70258187064364108, -151.3750000013656063, 2.196230717870141014 ) ) ;
#51321 = CARTESIAN_POINT ( 'NONE',  ( 3.061616997868383141E-16, -148.7500000000000284, -5.000000000000000000 ) ) ;
#51322 = CARTESIAN_POINT ( 'NONE',  ( -4.458734124999999437, -25.31249999863440792, 0.000000000000000000 ) ) ;
#51323 = CARTESIAN_POINT ( 'NONE',  ( 9.457646018065525792E-16, -69.31249999863439371, 5.148502694627439702 ) ) ;
#51324 = CARTESIAN_POINT ( 'NONE',  ( -4.999999999999998224, -89.91666666666667140, 2.886751345948131764 ) ) ;
#51325 = CARTESIAN_POINT ( 'NONE',  ( -2.229367062499996610, -24.14583333196773651, 3.861377020970582219 ) ) ;
#51326 = LINE ( 'NONE', #31360, #31744 ) ;
#51327 = CARTESIAN_POINT ( 'NONE',  ( 5.000000000000000000, -151.0000000000000284, 0.000000000000000000 ) ) ;
#51328 = CARTESIAN_POINT ( 'NONE',  ( 5.000000000000000000, -19.41666666666666075, -2.886751345948129988 ) ) ;
#51329 = CARTESIAN_POINT ( 'NONE',  ( -1.846868145590734756, -151.1250000013655779, -4.458734125000000326 ) ) ;
#51330 = ORIENTED_EDGE ( 'NONE', *, *, #30288, .F. ) ;
#51331 = CARTESIAN_POINT ( 'NONE',  ( 2.229367062500001939, -52.22916666530107221, 3.861377020970579999 ) ) ;
#51332 =( BOUNDED_CURVE ( )  B_SPLINE_CURVE ( 2, ( #56321, #8374, #47901, #8675, #37953, #41816, #61463, #27662, #28289 ),
 .UNSPECIFIED., .F., .F. ) 
 B_SPLINE_CURVE_WITH_KNOTS ( ( 3, 2, 2, 2, 3 ),
 ( 0.7232142857142856984, 0.7238095238095237915, 0.7249999999999999778, 0.7261904761904761640, 0.7267857142857142572 ),
 .UNSPECIFIED. ) 
 CURVE ( )  GEOMETRIC_REPRESENTATION_ITEM ( )  RATIONAL_B_SPLINE_CURVE ( ( 0.9330127018922194093, 0.9330127018922194093, 1.000000000000000000, 0.8660254037844387076, 1.000000000000000000, 0.8660254037844387076, 1.000000000000000000, 0.9330127018922194093, 0.9330127018922194093 ) ) 
 REPRESENTATION_ITEM ( '' )  );
#51333 = CARTESIAN_POINT ( 'NONE',  ( 1.975475456537005874E-15, -58.62499999726879452, 5.000000000000000000 ) ) ;
#51334 = CARTESIAN_POINT ( 'NONE',  ( 1.339745962155615144, -92.70534180126148271, 4.999999999999999112 ) ) ;
#51335 = CARTESIAN_POINT ( 'NONE',  ( 2.499999999999998668, 26.66666666666666430, -4.330127018922193649 ) ) ;
#51336 = CARTESIAN_POINT ( 'NONE',  ( -6.972266317189433020E-16, -76.12499999726880162, -5.000000000000000000 ) ) ;
#51337 = CARTESIAN_POINT ( 'NONE',  ( 4.458734124999999437, 4.187500001365595637, -5.460374474430324690E-16 ) ) ;
#51338 = CARTESIAN_POINT ( 'NONE',  ( 3.061616997868383141E-16, -142.7500000000000284, -5.000000000000000000 ) ) ;
#51339 = CARTESIAN_POINT ( 'NONE',  ( 2.500000000000002220, -41.54166666393548013, 4.330127018922192761 ) ) ;
#51340 = CARTESIAN_POINT ( 'NONE',  ( 6.123233995736766282E-16, -120.0000000000000000, -5.000000000000000000 ) ) ;
#51341 = CARTESIAN_POINT ( 'NONE',  ( 9.457646018065525792E-16, 14.68750000136559208, 5.148502694627439702 ) ) ;
#51342 = CARTESIAN_POINT ( 'NONE',  ( 5.000000000000000888, 2.541666669397851130, 2.886751345948126879 ) ) ;
#51343 = VERTEX_POINT ( 'NONE', #18728 ) ;
#51344 = DIRECTION ( 'NONE',  ( -0.000000000000000000, 1.000000000000000000, -0.000000000000000000 ) ) ;
#51345 = VERTEX_POINT ( 'NONE', #43170 ) ;
#51346 = CARTESIAN_POINT ( 'NONE',  ( -4.999999999999998224, -70.91666666666667140, 2.886751345948131764 ) ) ;
#51347 = CARTESIAN_POINT ( 'NONE',  ( -4.458734124999998549, -41.22916666530107221, 2.574251347313722516 ) ) ;
#51348 = CARTESIAN_POINT ( 'NONE',  ( 1.846868145590736310, -165.8750000013656063, 4.458734124999999437 ) ) ;
#51349 = CIRCLE ( 'NONE', #23604, 5.000000000000000000 ) ;
#51350 = CARTESIAN_POINT ( 'NONE',  ( 5.000000000000000000, -47.29166666393547303, -2.886751345948129988 ) ) ;
#51351 = VERTEX_POINT ( 'NONE', #38353 ) ;
#51352 = CARTESIAN_POINT ( 'NONE',  ( 9.457646018065525792E-16, -17.06249999863440792, 5.148502694627439702 ) ) ;
#51353 = EDGE_LOOP ( 'NONE', ( #22255, #60753, #33856, #52372 ) ) ;
#51354 = CARTESIAN_POINT ( 'NONE',  ( 2.499999999999998668, -86.33333333333332860, -4.330127018922193649 ) ) ;
#51355 = CARTESIAN_POINT ( 'NONE',  ( -1.846868145590734756, -163.1250000013656063, -4.458734125000000326 ) ) ;
#51356 = VERTEX_POINT ( 'NONE', #57359 ) ;
#51357 = CARTESIAN_POINT ( 'NONE',  ( -59.98410592259440222, -137.1250000000000284, -0.3983568153799752487 ) ) ;
#51358 = CARTESIAN_POINT ( 'NONE',  ( -4.458734124999999437, -32.56249999863440792, 0.000000000000000000 ) ) ;
#51359 = CARTESIAN_POINT ( 'NONE',  ( -5.000000000000000000, 20.91666666666666785, -2.886751345948128211 ) ) ;
#51360 = ORIENTED_EDGE ( 'NONE', *, *, #13457, .T. ) ;
#51361 = CARTESIAN_POINT ( 'NONE',  ( 2.229367062499998831, -75.64583333196773651, -3.861377020970580887 ) ) ;
#51362 = CARTESIAN_POINT ( 'NONE',  ( 9.457646018065525792E-16, 26.93750000136559564, 5.148502694627439702 ) ) ;
#51363 = CARTESIAN_POINT ( 'NONE',  ( -5.000000000000000000, -28.95833333060214443, -2.886751345948128211 ) ) ;
#51364 = VERTEX_POINT ( 'NONE', #24508 ) ;
#51365 = CARTESIAN_POINT ( 'NONE',  ( -5.000000000000000888, -161.4375000000000000, 2.071067811865474617 ) ) ;
#51366 = CARTESIAN_POINT ( 'NONE',  ( -57.19623071787016499, -141.6250000013655495, 4.297418129356382899 ) ) ;
#51367 = CARTESIAN_POINT ( 'NONE',  ( -4.458734124999998549, -80.47916666530106511, 2.574251347313722516 ) ) ;
#51368 = CARTESIAN_POINT ( 'NONE',  ( -49.85088928181150436, -128.6875000027312410, -1.666127454062680702 ) ) ;
#51369 = CARTESIAN_POINT ( 'NONE',  ( -6.972266317189433020E-16, -74.12499999726878741, -5.000000000000000000 ) ) ;
#51370 = CARTESIAN_POINT ( 'NONE',  ( -1.846868145590737420, -144.0000000013655779, 4.458734124999997661 ) ) ;
#51371 =( BOUNDED_CURVE ( )  B_SPLINE_CURVE ( 2, ( #43900, #62297, #14012, #63548, #8567, #28178, #47794, #19468, #23373 ),
 .UNSPECIFIED., .F., .F. ) 
 B_SPLINE_CURVE_WITH_KNOTS ( ( 3, 2, 2, 2, 3 ),
 ( 0.4375000000000000000, 0.4380952380952380931, 0.4392857142857142794, 0.4404761904761904656, 0.4410714285714285587 ),
 .UNSPECIFIED. ) 
 CURVE ( )  GEOMETRIC_REPRESENTATION_ITEM ( )  RATIONAL_B_SPLINE_CURVE ( ( 0.9330127018922194093, 0.9330127018922194093, 1.000000000000000000, 0.8660254037844387076, 1.000000000000000000, 0.8660254037844387076, 1.000000000000000000, 0.9330127018922194093, 0.9330127018922194093 ) ) 
 REPRESENTATION_ITEM ( '' )  );
#51372 = CARTESIAN_POINT ( 'NONE',  ( -5.000000000000000000, 6.041666669397852019, -2.886751345948128211 ) ) ;
#51373 = CARTESIAN_POINT ( 'NONE',  ( 4.458734125000000326, -56.89583333196774362, 2.574251347313718519 ) ) ;
#51374 = CARTESIAN_POINT ( 'NONE',  ( -4.458734124999997661, -44.22916666530106511, 2.574251347313722516 ) ) ;
#51375 = CARTESIAN_POINT ( 'NONE',  ( 4.458734124999999437, 28.18750000136559208, -5.460374474430324690E-16 ) ) ;
#51376 = CARTESIAN_POINT ( 'NONE',  ( -5.000000000000000000, -105.9999999999999858, 0.000000000000000000 ) ) ;
#51377 = CARTESIAN_POINT ( 'NONE',  ( 2.071067811865306751, -153.9375000027312410, -5.000000000000171418 ) ) ;
#51378 = CARTESIAN_POINT ( 'NONE',  ( 9.457646018065525792E-16, -39.31249999863439371, 5.148502694627439702 ) ) ;
#51379 = CARTESIAN_POINT ( 'NONE',  ( 5.000000000000000000, 3.708333336064517205, -2.886751345948129988 ) ) ;
#51380 = CARTESIAN_POINT ( 'NONE',  ( -58.24261429053147765, -154.2500000000000284, -3.805975901505573855 ) ) ;
#51381 = CARTESIAN_POINT ( 'NONE',  ( -53.51423613279429503, -125.2500000013656347, 4.591703134518082763 ) ) ;
#51382 = CARTESIAN_POINT ( 'NONE',  ( -4.458734124999998549, -77.47916666530106511, 2.574251347313722516 ) ) ;
#51383 = CARTESIAN_POINT ( 'NONE',  ( -59.81910112700026616, -142.3125000027311842, -2.462841084822451343 ) ) ;
#51384 = CARTESIAN_POINT ( 'NONE',  ( -2.229367062499996610, -105.1458333319677365, 3.861377020970582219 ) ) ;
#51385 = CARTESIAN_POINT ( 'NONE',  ( 4.458734125000000326, -7.145833331967736513, 2.574251347313718519 ) ) ;
#51386 = VERTEX_POINT ( 'NONE', #42859 ) ;
#51387 = CARTESIAN_POINT ( 'NONE',  ( -56.66612745406283125, -146.3125000000000284, -5.149110718188525837 ) ) ;
#51388 = CARTESIAN_POINT ( 'NONE',  ( 2.499999999999998668, -47.33333333333333570, -4.330127018922193649 ) ) ;
#51389 = CARTESIAN_POINT ( 'NONE',  ( 4.458734124999998549, -92.72916666530107932, -2.574251347313721627 ) ) ;
#51390 = CARTESIAN_POINT ( 'NONE',  ( 5.000000000000000888, -168.0625000027312126, -2.071067811865475505 ) ) ;
#51391 = CARTESIAN_POINT ( 'NONE',  ( 4.458734125000001214, -85.14583333196773651, 2.574251347313718519 ) ) ;
#51392 = CARTESIAN_POINT ( 'NONE',  ( 2.229367062500001939, 9.770833334698927786, 3.861377020970579999 ) ) ;
#51393 = CARTESIAN_POINT ( 'NONE',  ( 0.000000000000000000, -120.0000000000000000, 0.000000000000000000 ) ) ;
#51394 = CARTESIAN_POINT ( 'NONE',  ( -57.89159099828107458, -132.6875000013656063, -3.393966926194107447 ) ) ;
#51395 = CARTESIAN_POINT ( 'NONE',  ( 4.458734124999998549, -7.729166665301073991, -2.574251347313721627 ) ) ;
#51396 = CARTESIAN_POINT ( 'NONE',  ( -2.229367062499996610, 15.60416666803225993, 3.861377020970582219 ) ) ;
#51397 = CARTESIAN_POINT ( 'NONE',  ( 9.457646018065525792E-16, -53.31249999863440792, 5.148502694627439702 ) ) ;
#51398 = CARTESIAN_POINT ( 'NONE',  ( -4.999999999999998224, -15.79166666393548191, 2.886751345948131764 ) ) ;
#51399 = CARTESIAN_POINT ( 'NONE',  ( 2.229367062500001939, -83.97916666530106511, 3.861377020970579999 ) ) ;
#51400 = CARTESIAN_POINT ( 'NONE',  ( 4.458734125000000326, -10.89583333196773651, 2.574251347313718519 ) ) ;
#51401 = ORIENTED_EDGE ( 'NONE', *, *, #32316, .F. ) ;
#51402 = CARTESIAN_POINT ( 'NONE',  ( 4.458734124999998549, -32.97916666530106511, -2.574251347313721627 ) ) ;
#51403 = CARTESIAN_POINT ( 'NONE',  ( -53.51423613279429503, -126.5000000013656063, 4.591703134518082763 ) ) ;
#51404 = CARTESIAN_POINT ( 'NONE',  ( 9.457646018065525792E-16, -81.06249999863440792, 5.148502694627439702 ) ) ;
#51405 = CARTESIAN_POINT ( 'NONE',  ( 2.500000000000002220, -109.5416666639354730, 4.330127018922192761 ) ) ;
#51406 = CARTESIAN_POINT ( 'NONE',  ( 1.846868145590735200, -148.5000000013656347, -4.458734124999999437 ) ) ;
#51407 = CARTESIAN_POINT ( 'NONE',  ( -4.458734124999999437, 19.60416666803225993, -2.574251347313719407 ) ) ;
#51408 = CARTESIAN_POINT ( 'NONE',  ( 0.000000000000000000, -120.0000000000000000, 5.000000000000000000 ) ) ;
#51409 = DIRECTION ( 'NONE',  ( -0.000000000000000000, 1.000000000000000000, -0.000000000000000000 ) ) ;
#51410 = CARTESIAN_POINT ( 'NONE',  ( 4.458734125000000326, -82.14583333196772230, 2.574251347313718519 ) ) ;
#51411 = CARTESIAN_POINT ( 'NONE',  ( 5.000000000000000000, -67.41666666666665719, -2.886751345948129988 ) ) ;
#51412 = CARTESIAN_POINT ( 'NONE',  ( 0.000000000000000000, -120.0000000000000000, 0.000000000000000000 ) ) ;
#51413 = CARTESIAN_POINT ( 'NONE',  ( -2.500000000000000444, 16.95833333606451987, -4.330127018922193649 ) ) ;
#51414 = ORIENTED_EDGE ( 'NONE', *, *, #41313, .F. ) ;
#51415 = CARTESIAN_POINT ( 'NONE',  ( 2.499999999999998668, -25.33333333333333215, -4.330127018922193649 ) ) ;
#51416 = CARTESIAN_POINT ( 'NONE',  ( -5.000000000000000000, 9.000000000000001776, 0.000000000000000000 ) ) ;
#51418 = CARTESIAN_POINT ( 'NONE',  ( 5.000000000000000000, -22.41666666666666785, -2.886751345948129988 ) ) ;
#51417 = DIRECTION ( 'NONE',  ( -0.000000000000000000, 1.000000000000000000, -0.000000000000000000 ) ) ;
#51419 = CARTESIAN_POINT ( 'NONE',  ( 2.229367062499998831, -26.64583333196774007, -3.861377020970580887 ) ) ;
#51420 = EDGE_CURVE ( 'NONE', #18873, #43870, #63441, .T. ) ;
#51421 = CARTESIAN_POINT ( 'NONE',  ( 2.229367062499998831, -86.64583333196773651, -3.861377020970580887 ) ) ;
#51422 = CARTESIAN_POINT ( 'NONE',  ( -2.500000000000000444, -31.04166666393548368, -4.330127018922193649 ) ) ;
#51424 = ORIENTED_EDGE ( 'NONE', *, *, #1109, .T. ) ;
#51423 = CARTESIAN_POINT ( 'NONE',  ( 2.229367062499998831, -55.64583333196773651, -3.861377020970580887 ) ) ;
#51425 = CARTESIAN_POINT ( 'NONE',  ( -50.70258187064364108, -153.3750000013656347, 2.196230717870141014 ) ) ;
#51427 = ORIENTED_EDGE ( 'NONE', *, *, #42910, .F. ) ;
#51426 = CARTESIAN_POINT ( 'NONE',  ( 4.458734124999999437, -9.062499998634406140, -5.460374474430324690E-16 ) ) ;
#51428 = CARTESIAN_POINT ( 'NONE',  ( -2.499999999999996447, -70.83333333333332860, 4.330127018922195425 ) ) ;
#51429 = CARTESIAN_POINT ( 'NONE',  ( -53.51423613279429503, -138.2500000013656063, 4.591703134518083651 ) ) ;
#51430 = VECTOR ( 'NONE', #3146, 1000.000000000000000 ) ;
#51431 = CARTESIAN_POINT ( 'NONE',  ( 2.229367062500001939, -54.22916666530107221, 3.861377020970579999 ) ) ;
#51432 = CARTESIAN_POINT ( 'NONE',  ( -6.972266317189433020E-16, -24.24999999999999645, -5.000000000000000000 ) ) ;
#51433 = CARTESIAN_POINT ( 'NONE',  ( -4.999999999999999112, -77.79166666393547303, 2.886751345948131764 ) ) ;
#51434 = CARTESIAN_POINT ( 'NONE',  ( -1.339745962155613812, -54.08034179853029144, -5.000000000000000000 ) ) ;
#51435 = AXIS2_PLACEMENT_3D ( 'NONE', #49639, #16183, #1415 ) ;
#51436 = CARTESIAN_POINT ( 'NONE',  ( -58.24261429053147765, -151.2500000000000284, -3.805975901505573855 ) ) ;
#51437 = CARTESIAN_POINT ( 'NONE',  ( -2.229367062500000163, -14.72916666530107221, -3.861377020970580443 ) ) ;
#51438 = CARTESIAN_POINT ( 'NONE',  ( -4.458734124999998549, -50.47916666530107221, 2.574251347313722516 ) ) ;
#51439 = ADVANCED_FACE ( 'NONE', ( #33532 ), #53147, .F. ) ;
#51440 = CARTESIAN_POINT ( 'NONE',  ( 5.000000000000000888, 10.41666666666666785, 2.886751345948126879 ) ) ;
#51441 = SURFACE_STYLE_FILL_AREA ( #8010 ) ;
#51442 = CARTESIAN_POINT ( 'NONE',  ( 4.458734125000000326, -141.3750000013656063, -1.846868145590734978 ) ) ;
#51443 = ADVANCED_FACE ( 'NONE', ( #53769 ), #25293, .T. ) ;
#51444 = CARTESIAN_POINT ( 'NONE',  ( -2.229367062500000163, -101.7291666653010651, -3.861377020970580443 ) ) ;
#51445 = CARTESIAN_POINT ( 'NONE',  ( 3.061616997868383141E-16, -147.8750000027312126, -5.000000000000000000 ) ) ;
#51446 = ORIENTED_EDGE ( 'NONE', *, *, #59690, .T. ) ;
#51447 = CARTESIAN_POINT ( 'NONE',  ( -54.64476657466781973, -154.0625000013656347, -4.444560631937228834 ) ) ;
#51448 = CARTESIAN_POINT ( 'NONE',  ( -59.81910112700025905, -141.3125000027312126, -2.462841084822630311 ) ) ;
#51449 = CARTESIAN_POINT ( 'NONE',  ( -2.499999999999996447, -12.70833333060214798, 4.330127018922195425 ) ) ;
#51450 = EDGE_CURVE ( 'NONE', #9796, #49029, #59243, .T. ) ;
#51451 = CARTESIAN_POINT ( 'NONE',  ( -2.229367062499996610, -2.145833331967737845, 3.861377020970582219 ) ) ;
#51452 =( BOUNDED_CURVE ( )  B_SPLINE_CURVE ( 2, ( #2785, #51035, #61960, #42004, #8241, #61645, #17578, #21452, #27843 ),
 .UNSPECIFIED., .F., .F. ) 
 B_SPLINE_CURVE_WITH_KNOTS ( ( 3, 2, 2, 2, 3 ),
 ( 0.07291666666666667129, 0.07361111111111111327, 0.07499999999999999722, 0.07638888888888889506, 0.07708333333333333703 ),
 .UNSPECIFIED. ) 
 CURVE ( )  GEOMETRIC_REPRESENTATION_ITEM ( )  RATIONAL_B_SPLINE_CURVE ( ( 0.9330127018922194093, 0.9330127018922200755, 1.000000000000000000, 0.8660254037844387076, 1.000000000000000000, 0.8660254037844387076, 1.000000000000000000, 0.9330127018922194093, 0.9330127018922194093 ) ) 
 REPRESENTATION_ITEM ( '' )  );
#51453 = CARTESIAN_POINT ( 'NONE',  ( 2.229367062500001939, -96.22916666530105090, 3.861377020970579999 ) ) ;
#51454 = CARTESIAN_POINT ( 'NONE',  ( 3.152801135295366208, -146.8125000013655779, 3.152801135295367985 ) ) ;
#51455 = CARTESIAN_POINT ( 'NONE',  ( -3.152548672688508926E-16, -20.81249999863440081, -5.148502694627439702 ) ) ;
#51456 = CARTESIAN_POINT ( 'NONE',  ( 0.000000000000000000, -170.0000000000000000, 0.000000000000000000 ) ) ;
#51457 = CARTESIAN_POINT ( 'NONE',  ( -59.29741812935640155, -136.6250000013655779, -2.196230717870135685 ) ) ;
#51458 = CARTESIAN_POINT ( 'NONE',  ( -4.458734124999999437, -62.56249999863440792, 0.000000000000000000 ) ) ;
#51459 = CARTESIAN_POINT ( 'NONE',  ( 1.015826369459276846, -8.073766409988136772, -7.642786413614194529 ) ) ;
#51460 = CARTESIAN_POINT ( 'NONE',  ( -3.152801135295367096, -145.0625000013655779, -3.152801135295367541 ) ) ;
#51461 = CARTESIAN_POINT ( 'NONE',  ( 9.457646018065525792E-16, 8.687500001365595637, 5.148502694627439702 ) ) ;
#51462 = ORIENTED_EDGE ( 'NONE', *, *, #47318, .T. ) ;
#51463 = CARTESIAN_POINT ( 'NONE',  ( 6.123233995736766282E-16, -120.0000000000000000, -5.000000000000000000 ) ) ;
#51464 = CARTESIAN_POINT ( 'NONE',  ( 3.061616997868383141E-16, -144.7500000000000284, -5.000000000000000000 ) ) ;
#51466 = CARTESIAN_POINT ( 'NONE',  ( -4.458734124999999437, -25.39583333196773651, -2.574251347313719407 ) ) ;
#51465 = CARTESIAN_POINT ( 'NONE',  ( 5.000000000000000888, -88.58333333333332860, 2.886751345948126879 ) ) ;
#51467 = CARTESIAN_POINT ( 'NONE',  ( 4.458734124999998549, 29.02083333469893134, -2.574251347313721627 ) ) ;
#51468 = CARTESIAN_POINT ( 'NONE',  ( 1.975475456537005874E-15, -76.62499999726880162, 5.000000000000000000 ) ) ;
#51469 = CARTESIAN_POINT ( 'NONE',  ( -52.80376928212989185, -146.8750000013656063, -4.297418129356379346 ) ) ;
#51470 = EDGE_CURVE ( 'NONE', #9470, #40984, #2162, .T. ) ;
#51471 = CARTESIAN_POINT ( 'NONE',  ( 1.060575238724906964E-15, -51.62499999726881583, 5.773502691896257311 ) ) ;
#51472 = FACE_OUTER_BOUND ( 'NONE', #41818, .T. ) ;
#51473 = CARTESIAN_POINT ( 'NONE',  ( 4.458734124999999437, 9.187500001365592084, -5.460374474430324690E-16 ) ) ;
#51474 = CARTESIAN_POINT ( 'NONE',  ( -6.972266317189433020E-16, -56.12499999726880162, -5.000000000000000000 ) ) ;
#51475 = CARTESIAN_POINT ( 'NONE',  ( -51.75738570946856498, -141.8750000027312126, 3.805975901505576964 ) ) ;
#51476 = CARTESIAN_POINT ( 'NONE',  ( -4.458734124999999437, 6.604166668032259935, -2.574251347313719407 ) ) ;
#51477 = CARTESIAN_POINT ( 'NONE',  ( -3.152548672688508926E-16, -68.56249999863439371, -5.148502694627439702 ) ) ;
#51478 = CARTESIAN_POINT ( 'NONE',  ( 2.229367062500001939, -22.22916666530107221, 3.861377020970579999 ) ) ;
#51479 = CARTESIAN_POINT ( 'NONE',  ( 2.499999999999998668, -3.333333333333333925, -4.330127018922193649 ) ) ;
#51480 = CARTESIAN_POINT ( 'NONE',  ( -1.846868145590737420, -160.7500000013655779, 4.458734124999999437 ) ) ;
#51481 = CARTESIAN_POINT ( 'NONE',  ( -6.972266317189433020E-16, 15.87500000273118417, -5.000000000000000000 ) ) ;
#51482 = VECTOR ( 'NONE', #35033, 1000.000000000000000 ) ;
#51483 = CARTESIAN_POINT ( 'NONE',  ( -2.229367062500000163, -63.47916666530106511, -3.861377020970580443 ) ) ;
#51484 = CARTESIAN_POINT ( 'NONE',  ( -2.499999999999996447, -92.70833333060214443, 4.330127018922195425 ) ) ;
#51485 = CARTESIAN_POINT ( 'NONE',  ( 2.500000000000002220, 5.458333336064518981, 4.330127018922192761 ) ) ;
#51486 = CARTESIAN_POINT ( 'NONE',  ( 4.458734124999998549, -37.72916666530107221, -2.574251347313721627 ) ) ;
#51487 = CARTESIAN_POINT ( 'NONE',  ( 5.000000000000000000, 19.70833333606451632, -2.886751345948130876 ) ) ;
#51488 = CARTESIAN_POINT ( 'NONE',  ( 4.458734124999999437, -68.06249999863440792, -5.460374474430324690E-16 ) ) ;
#51489 = CARTESIAN_POINT ( 'NONE',  ( 5.000000000000000000, -47.41666666666666430, -2.886751345948129988 ) ) ;
#51490 = CARTESIAN_POINT ( 'NONE',  ( -5.000000000000000000, 26.91666666666666430, -2.886751345948128211 ) ) ;
#51491 = CARTESIAN_POINT ( 'NONE',  ( 1.339745962155612702, -89.29465819873851729, -5.000000000000000000 ) ) ;
#51492 = ORIENTED_EDGE ( 'NONE', *, *, #14144, .F. ) ;
#51493 = CARTESIAN_POINT ( 'NONE',  ( 4.458734125000001214, -105.8958333319677365, 2.574251347313718519 ) ) ;
#51494 = CARTESIAN_POINT ( 'NONE',  ( 4.458734124999998549, -0.9791666653010713262, -2.574251347313721627 ) ) ;
#51495 = CARTESIAN_POINT ( 'NONE',  ( 0.000000000000000000, -170.0000000000000000, 0.000000000000000000 ) ) ;
#51496 = CARTESIAN_POINT ( 'NONE',  ( -5.000000000000000000, -5.083333333333334814, -2.886751345948128211 ) ) ;
#51497 = EDGE_CURVE ( 'NONE', #44325, #14472, #48624, .T. ) ;
#51498 = CARTESIAN_POINT ( 'NONE',  ( 9.457646018065525792E-16, -71.06249999863439371, 5.148502694627439702 ) ) ;
#51499 = CARTESIAN_POINT ( 'NONE',  ( -55.00000000000002132, -155.0000000000000284, 1.734723475976807094E-15 ) ) ;
#51500 = CARTESIAN_POINT ( 'NONE',  ( -5.000000000000000000, -10.95833333060214621, -2.886751345948128211 ) ) ;
#51502 = ORIENTED_EDGE ( 'NONE', *, *, #51152, .T. ) ;
#51501 = CARTESIAN_POINT ( 'NONE',  ( -4.458734124999998549, -41.22916666530107221, 2.574251347313722516 ) ) ;
#51503 = CARTESIAN_POINT ( 'NONE',  ( 3.535533905932736864, -144.1250000000000000, 3.535533905932738641 ) ) ;
#51505 = EDGE_LOOP ( 'NONE', ( #48639, #1463, #19023, #35927 ) ) ;
#51504 = CARTESIAN_POINT ( 'NONE',  ( -2.229367062500000163, 10.27083333469892779, -3.861377020970580443 ) ) ;
#51506 =( BOUNDED_CURVE ( )  B_SPLINE_CURVE ( 2, ( #53244, #9180, #28792, #11632, #175, #16470, #4981, #26435, #1695 ),
 .UNSPECIFIED., .F., .F. ) 
 B_SPLINE_CURVE_WITH_KNOTS ( ( 3, 2, 2, 2, 3 ),
 ( 0.4083333333333336590, 0.4125000000000003109, 0.4166666666666670182, 0.4208333333333336701, 0.4250000000000003220 ),
 .UNSPECIFIED. ) 
 CURVE ( )  GEOMETRIC_REPRESENTATION_ITEM ( )  RATIONAL_B_SPLINE_CURVE ( ( 0.9999999999999938938, 0.9238795325112928447, 1.000000000000000000, 0.9238795325112867385, 1.000000000000000000, 0.9238795325112867385, 1.000000000000000000, 0.9238795325112806323, 1.000000000000005995 ) ) 
 REPRESENTATION_ITEM ( '' )  );
#51507 = CARTESIAN_POINT ( 'NONE',  ( 5.000000000000000000, -81.29166666393547303, -2.886751345948130876 ) ) ;
#51508 = CARTESIAN_POINT ( 'NONE',  ( -2.499999999999996447, -54.83333333333332860, 4.330127018922195425 ) ) ;
#51509 = CARTESIAN_POINT ( 'NONE',  ( -8.190561711645485556E-16, -161.9375000013655779, 4.458734124999999437 ) ) ;
#51510 = CARTESIAN_POINT ( 'NONE',  ( 4.458734124999998549, -34.97916666530107221, -2.574251347313721627 ) ) ;
#51511 = CARTESIAN_POINT ( 'NONE',  ( -5.000000000000000000, -10.95833333060214621, -2.886751345948128211 ) ) ;
#51512 = CARTESIAN_POINT ( 'NONE',  ( 9.457646018065525792E-16, -79.06249999863440792, 5.148502694627439702 ) ) ;
#51513 = CARTESIAN_POINT ( 'NONE',  ( 3.152801135295366208, -140.8125000013655779, 3.152801135295367985 ) ) ;
#51514 = CARTESIAN_POINT ( 'NONE',  ( -4.458734124999999437, -87.39583333196773651, -2.574251347313719407 ) ) ;
#51515 = CARTESIAN_POINT ( 'NONE',  ( -50.40829686548195099, -134.2500000013656063, -1.485763867205728284 ) ) ;
#51516 = CARTESIAN_POINT ( 'NONE',  ( -2.229367062499996610, 1.604166668032262155, 3.861377020970582219 ) ) ;
#51517 = CARTESIAN_POINT ( 'NONE',  ( -3.152548672688508926E-16, -36.81249999863440792, -5.148502694627439702 ) ) ;
#51518 = CARTESIAN_POINT ( 'NONE',  ( 1.339745962155612702, -72.29465819873850307, -5.000000000000000000 ) ) ;
#51519 = EDGE_CURVE ( 'NONE', #21623, #27699, #24288, .T. ) ;
#51520 = CARTESIAN_POINT ( 'NONE',  ( 4.458734124999999437, -77.06249999863440792, -5.460374474430324690E-16 ) ) ;
#51521 = ORIENTED_EDGE ( 'NONE', *, *, #24466, .T. ) ;
#51522 = ADVANCED_FACE ( 'NONE', ( #30276 ), #44750, .T. ) ;
#51523 = CARTESIAN_POINT ( 'NONE',  ( 3.061616997868383141E-16, -141.7500000000000284, -5.000000000000000000 ) ) ;
#51524 = DIRECTION ( 'NONE',  ( -0.000000000000000000, 1.000000000000000000, -0.000000000000000000 ) ) ;
#51525 = CARTESIAN_POINT ( 'NONE',  ( 2.229367062499998831, -68.89583333196773651, -3.861377020970580887 ) ) ;
#51526 = CARTESIAN_POINT ( 'NONE',  ( -2.229367062500000163, -6.729166665301073103, -3.861377020970580443 ) ) ;
#51527 = ORIENTED_EDGE ( 'NONE', *, *, #53864, .T. ) ;
#51528 = CARTESIAN_POINT ( 'NONE',  ( 5.000000000000000888, -5.583333333333336590, 2.886751345948126879 ) ) ;
#51529 = CARTESIAN_POINT ( 'NONE',  ( 2.229367062499998831, -8.895833331967736513, -3.861377020970580887 ) ) ;
#51530 = FACE_OUTER_BOUND ( 'NONE', #3904, .T. ) ;
#51531 = CARTESIAN_POINT ( 'NONE',  ( 2.229367062500001939, 7.020833334698928674, 3.861377020970579999 ) ) ;
#51532 = CARTESIAN_POINT ( 'NONE',  ( 1.975475456537005874E-15, -78.62499999726881583, 5.000000000000000000 ) ) ;
#51533 = CARTESIAN_POINT ( 'NONE',  ( 4.458734124999997661, -155.5000000013656063, 1.846868145590737864 ) ) ;
#51534 = CARTESIAN_POINT ( 'NONE',  ( 2.229367062500001939, 26.77083333469892423, 3.861377020970579999 ) ) ;
#51535 = VERTEX_POINT ( 'NONE', #20321 ) ;
#51536 = CARTESIAN_POINT ( 'NONE',  ( -4.458734124999999437, -86.31249999863439371, 0.000000000000000000 ) ) ;
#51537 = CARTESIAN_POINT ( 'NONE',  ( -5.000000000000000000, -25.08333333333333215, -2.886751345948128211 ) ) ;
#51538 = CARTESIAN_POINT ( 'NONE',  ( 2.229367062499998831, -6.645833331967741842, -3.861377020970580887 ) ) ;
#51539 = EDGE_CURVE ( 'NONE', #25291, #17887, #21870, .T. ) ;
#51540 = CARTESIAN_POINT ( 'NONE',  ( -2.499999999999996447, -32.70833333060215153, 4.330127018922195425 ) ) ;
#51541 = DIRECTION ( 'NONE',  ( -0.000000000000000000, 1.000000000000000000, -0.000000000000000000 ) ) ;
#51542 = CARTESIAN_POINT ( 'NONE',  ( 4.458734125000000326, 26.10416666803225993, 2.574251347313718519 ) ) ;
#51543 = CARTESIAN_POINT ( 'NONE',  ( 1.339745962155615144, -7.705341801261480938, 4.999999999999999112 ) ) ;
#51544 = CARTESIAN_POINT ( 'NONE',  ( 9.457646018065525792E-16, 23.93750000136559564, 5.148502694627439702 ) ) ;
#51545 = CARTESIAN_POINT ( 'NONE',  ( 4.458734124999999437, -49.81249999863440792, -5.460374474430324690E-16 ) ) ;
#51546 = CARTESIAN_POINT ( 'NONE',  ( 4.458734124999999437, -38.06249999863440792, -5.460374474430324690E-16 ) ) ;
#51547 = CARTESIAN_POINT ( 'NONE',  ( 2.229367062499998831, -2.895833331967738289, -3.861377020970580887 ) ) ;
#51548 =( BOUNDED_SURFACE ( )  B_SPLINE_SURFACE ( 3, 2, ( 
 ( #31828, #36978, #56606 ),
 ( #6754, #51459, #46623 ),
 ( #6445, #12523, #1627 ),
 ( #7077, #35706, #1318 ),
 ( #26054, #26691, #40834 ),
 ( #22185, #16721, #21228 ),
 ( #41148, #60161, #45668 ),
 ( #25737, #61115, #41786 ) ),
 .UNSPECIFIED., .F., .F., .F. ) 
 B_SPLINE_SURFACE_WITH_KNOTS ( ( 4, 2, 2, 4 ),
 ( 3, 3 ),
 ( 0.03861844051980971304, 0.04325213341840643266, 0.04556897986770479247, 0.04788582631700314535 ),
 ( 0.000000000000000000, 1.000000000000000000 ),
 .UNSPECIFIED. ) 
 GEOMETRIC_REPRESENTATION_ITEM ( )  RATIONAL_B_SPLINE_SURFACE ( (
 ( 1.000000000000000000, 0.8047781759831919013, 1.000000000000000000),
 ( 1.000000000000000000, 0.8123762462802479600, 1.000000000000000000),
 ( 1.000000000000000000, 0.8190659850620179983, 1.000000000000000000),
 ( 1.000000000000000000, 0.8191937571011910224, 1.000000000000000000),
 ( 1.000000000000000000, 0.8176092952781196521, 1.000000000000000000),
 ( 1.000000000000000000, 0.8122962088595743202, 1.000000000000000000),
 ( 1.000000000000000000, 0.8086311330828506172, 1.000000000000000000),
 ( 1.000000000000000000, 0.8047712282214323221, 1.000000000000000000) ) ) 
 REPRESENTATION_ITEM ( '' )  SURFACE ( )  );
#51549 = CARTESIAN_POINT ( 'NONE',  ( -2.071067811865306307, -149.8125000027311842, -5.000000000000171418 ) ) ;
#51550 = CARTESIAN_POINT ( 'NONE',  ( 2.499999999999998668, 13.66666666666666785, -4.330127018922193649 ) ) ;
#51551 = CARTESIAN_POINT ( 'NONE',  ( -2.071067811865475061, -142.8125000027312126, -5.000000000000000888 ) ) ;
#51552 = CARTESIAN_POINT ( 'NONE',  ( 5.000000000000000888, -158.9375000000000000, -2.071067811865475505 ) ) ;
#51553 = CARTESIAN_POINT ( 'NONE',  ( 9.457646018065525792E-16, -46.06249999863440081, 5.148502694627439702 ) ) ;
#51554 = CARTESIAN_POINT ( 'NONE',  ( 5.000000000000000888, -77.45833333060213022, 2.886751345948126879 ) ) ;
#51555 = CARTESIAN_POINT ( 'NONE',  ( -59.44456063193725015, -138.8125000013656063, -0.3552334253322034230 ) ) ;
#51556 = CARTESIAN_POINT ( 'NONE',  ( 5.000000000000000888, -65.45833333060213022, 2.886751345948126879 ) ) ;
#51557 = CARTESIAN_POINT ( 'NONE',  ( 1.339745962155615144, -22.70534180126147916, 4.999999999999999112 ) ) ;
#51558 = CARTESIAN_POINT ( 'NONE',  ( -4.458734124999999437, -84.56249999863439371, 0.000000000000000000 ) ) ;
#51559 = CARTESIAN_POINT ( 'NONE',  ( 4.458734124999999437, -159.6875000013655779, 0.000000000000000000 ) ) ;
#51560 = CARTESIAN_POINT ( 'NONE',  ( -5.000000000000000000, -35.08333333333332149, -2.886751345948128211 ) ) ;
#51561 = CARTESIAN_POINT ( 'NONE',  ( -2.071067811865562991, -147.3125000000000000, 4.999999999999913847 ) ) ;
#51562 = EDGE_LOOP ( 'NONE', ( #15376, #14153, #33001, #85 ) ) ;
#51563 = CARTESIAN_POINT ( 'NONE',  ( 4.458734124999999437, 17.93750000136559208, -5.460374474430324690E-16 ) ) ;
#51564 = ORIENTED_EDGE ( 'NONE', *, *, #40815, .F. ) ;
#51565 = CARTESIAN_POINT ( 'NONE',  ( 2.229367062499998831, -90.64583333196773651, -3.861377020970580887 ) ) ;
#51566 = CARTESIAN_POINT ( 'NONE',  ( 4.458734124999999437, 15.93750000136559564, -5.460374474430324690E-16 ) ) ;
#51567 = CARTESIAN_POINT ( 'NONE',  ( -5.000000000000000000, 17.12500000273118417, 0.000000000000000000 ) ) ;
#51568 = CARTESIAN_POINT ( 'NONE',  ( -6.972266317189433020E-16, -37.25000000000000000, -5.000000000000000000 ) ) ;
#51569 = CARTESIAN_POINT ( 'NONE',  ( 2.499999999999998668, 9.666666666666667851, -4.330127018922193649 ) ) ;
#51570 = CARTESIAN_POINT ( 'NONE',  ( -4.458734124999999437, -57.31249999863440081, 0.000000000000000000 ) ) ;
#51571 = CARTESIAN_POINT ( 'NONE',  ( 1.975475456537005874E-15, -61.62499999726880873, 5.000000000000000000 ) ) ;
#51572 = ADVANCED_FACE ( 'NONE', ( #34796 ), #10347, .T. ) ;
#51573 = ADVANCED_FACE ( 'NONE', ( #19675 ), #29637, .T. ) ;
#51574 = DIRECTION ( 'NONE',  ( -0.000000000000000000, 1.000000000000000000, -0.000000000000000000 ) ) ;
#51575 = CARTESIAN_POINT ( 'NONE',  ( -5.000000000000000000, -37.87499999726881583, 0.000000000000000000 ) ) ;
#51576 = CARTESIAN_POINT ( 'NONE',  ( 1.975475456537005874E-15, -33.62499999726880873, 5.000000000000000000 ) ) ;
#51577 = ADVANCED_FACE ( 'NONE', ( #54739 ), #5207, .T. ) ;
#51578 = CARTESIAN_POINT ( 'NONE',  ( -5.000000000000000000, -24.87499999726881583, 0.000000000000000000 ) ) ;
#51579 = CARTESIAN_POINT ( 'NONE',  ( 5.000000000000000000, -40.41666666666667140, -2.886751345948129988 ) ) ;
#51580 = CARTESIAN_POINT ( 'NONE',  ( 1.339745962155612702, -96.29465819873851729, -5.000000000000000000 ) ) ;
#51582 = CARTESIAN_POINT ( 'NONE',  ( 9.457646018065525792E-16, -14.31249999863440259, 5.148502694627439702 ) ) ;
#51581 = CARTESIAN_POINT ( 'NONE',  ( -55.39835681537999790, -138.8750000000000284, 4.984105922594378235 ) ) ;
#51583 = EDGE_CURVE ( 'NONE', #49037, #42676, #28429, .T. ) ;
#51584 = CARTESIAN_POINT ( 'NONE',  ( -2.229367062499996610, -66.14583333196773651, 3.861377020970582219 ) ) ;
#51585 = CARTESIAN_POINT ( 'NONE',  ( -4.458734124999999437, -153.1875000013656063, -5.460374474430324690E-16 ) ) ;
#51586 = CARTESIAN_POINT ( 'NONE',  ( -4.458734124999999437, -69.39583333196773651, -2.574251347313719407 ) ) ;
#51587 = CARTESIAN_POINT ( 'NONE',  ( -55.35523342533222291, -148.5625000013656063, 4.444560631937231499 ) ) ;
#51588 = ADVANCED_FACE ( 'NONE', ( #31702 ), #61939, .T. ) ;
#51589 = ADVANCED_FACE ( 'NONE', ( #11752 ), #17225, .F. ) ;
#51590 = CARTESIAN_POINT ( 'NONE',  ( 4.458734124999998549, -19.97916666530106866, -2.574251347313721627 ) ) ;
#51591 = CARTESIAN_POINT ( 'NONE',  ( -5.000000000000000000, -61.87499999726880873, 0.000000000000000000 ) ) ;
#51592 = VERTEX_POINT ( 'NONE', #2142 ) ;
#51593 = CARTESIAN_POINT ( 'NONE',  ( -5.000000000000000000, -49.00000000000000000, 0.000000000000000000 ) ) ;
#51595 = ORIENTED_EDGE ( 'NONE', *, *, #30003, .F. ) ;
#51594 = EDGE_CURVE ( 'NONE', #38517, #9564, #7037, .T. ) ;
#51596 = CARTESIAN_POINT ( 'NONE',  ( -4.458734124999998549, -61.47916666530107221, 2.574251347313722516 ) ) ;
#51597 = CYLINDRICAL_SURFACE ( 'NONE', #4000, 5.000000000000000000 ) ;
#51598 = CARTESIAN_POINT ( 'NONE',  ( -3.152801135295367985, -150.8125000013655779, 3.152801135295367096 ) ) ;
#51599 = EDGE_CURVE ( 'NONE', #28712, #28080, #50987, .T. ) ;
#51600 = ORIENTED_EDGE ( 'NONE', *, *, #9724, .F. ) ;
#51601 = EDGE_CURVE ( 'NONE', #5304, #34281, #36852, .T. ) ;
#51602 = EDGE_CURVE ( 'NONE', #17309, #43124, #37479, .T. ) ;
#51603 = CARTESIAN_POINT ( 'NONE',  ( 1.975475456537005874E-15, 0.3750000027311862216, 5.000000000000000000 ) ) ;
#51604 = CARTESIAN_POINT ( 'NONE',  ( -58.24261429053147765, -125.2500000000000284, -3.805975901505573855 ) ) ;
#51605 = DIRECTION ( 'NONE',  ( 1.000000000000000000, 0.000000000000000000, -7.709882115452477180E-16 ) ) ;
#51606 = CARTESIAN_POINT ( 'NONE',  ( -2.229367062500000163, -46.72916666530106511, -3.861377020970580443 ) ) ;
#51607 = ORIENTED_EDGE ( 'NONE', *, *, #18972, .F. ) ;
#51608 = CARTESIAN_POINT ( 'NONE',  ( -1.339745962155640457, 2.330341803992662886, 4.999999999999984901 ) ) ;
#51609 = CARTESIAN_POINT ( 'NONE',  ( 4.458734125000001214, 7.104166668032259047, 2.574251347313718519 ) ) ;
#51610 = CARTESIAN_POINT ( 'NONE',  ( -2.229367062500000163, 21.52083333469892779, -3.861377020970580443 ) ) ;
#51611 = CARTESIAN_POINT ( 'NONE',  ( -50.40829686548195099, -150.0000000013655779, -1.485763867205728284 ) ) ;
#51612 = CARTESIAN_POINT ( 'NONE',  ( 2.493747252781420335E-13, -77.25000000000001421, -5.000000000000000000 ) ) ;
#51613 = CARTESIAN_POINT ( 'NONE',  ( 4.458734124999999437, -168.3750000013655779, -1.846868145590734978 ) ) ;
#51614 = ORIENTED_EDGE ( 'NONE', *, *, #380, .F. ) ;
#51615 = CARTESIAN_POINT ( 'NONE',  ( -4.458734124999999437, -69.39583333196773651, -2.574251347313719407 ) ) ;
#51616 = CARTESIAN_POINT ( 'NONE',  ( -2.500000000000000444, -86.04166666393547303, -4.330127018922193649 ) ) ;
#51617 = CARTESIAN_POINT ( 'NONE',  ( 4.458734125000001214, 13.10416666803226171, 2.574251347313718519 ) ) ;
#51618 = CARTESIAN_POINT ( 'NONE',  ( 2.500000000000002220, -69.54166666393547303, 4.330127018922192761 ) ) ;
#51619 = CARTESIAN_POINT ( 'NONE',  ( 4.458734125000001214, -56.14583333196774362, 2.574251347313718519 ) ) ;
#51620 = CARTESIAN_POINT ( 'NONE',  ( -3.535250795749689387E-16, -14.12499999726881050, -5.773502691896257311 ) ) ;
#51621 = CARTESIAN_POINT ( 'NONE',  ( 0.000000000000000000, -120.0000000000000000, 0.000000000000000000 ) ) ;
#51622 = CARTESIAN_POINT ( 'NONE',  ( 1.975475456537005874E-15, -44.62499999726880162, 5.000000000000000000 ) ) ;
#51623 = CARTESIAN_POINT ( 'NONE',  ( 1.975475456537005874E-15, -65.74999999999998579, 5.000000000000000000 ) ) ;
#51624 = CARTESIAN_POINT ( 'NONE',  ( 9.457646018065525792E-16, -33.06249999863440792, 5.148502694627439702 ) ) ;
#51625 = CARTESIAN_POINT ( 'NONE',  ( -4.458734124999997661, -22.47916666530107221, 2.574251347313722516 ) ) ;
#51626 = VERTEX_POINT ( 'NONE', #61621 ) ;
#51627 = CARTESIAN_POINT ( 'NONE',  ( -9.184850993605147944E-16, -159.2500000000000000, 5.000000000000000000 ) ) ;
#51628 = CARTESIAN_POINT ( 'NONE',  ( -4.458734124999999437, -107.3124999986343937, 0.000000000000000000 ) ) ;
#51629 = CARTESIAN_POINT ( 'NONE',  ( -3.535533905932738641, -154.5000000027312126, 3.535533905932737309 ) ) ;
#51630 = ORIENTED_EDGE ( 'NONE', *, *, #59743, .T. ) ;
#51631 = CARTESIAN_POINT ( 'NONE',  ( 2.229367062500001939, -100.2291666653010651, 3.861377020970579999 ) ) ;
#51632 = CARTESIAN_POINT ( 'NONE',  ( 9.457646018065525792E-16, -28.06249999863440081, 5.148502694627439702 ) ) ;
#51633 = CARTESIAN_POINT ( 'NONE',  ( -5.000000000000000000, -62.87499999726880873, 0.000000000000000000 ) ) ;
#51634 =( BOUNDED_CURVE ( )  B_SPLINE_CURVE ( 2, ( #25097, #11257, #59525, #50510, #40213, #15459, #36030, #55009, #45676 ),
 .UNSPECIFIED., .F., .F. ) 
 B_SPLINE_CURVE_WITH_KNOTS ( ( 3, 2, 2, 2, 3 ),
 ( 0.4520833333333333370, 0.4527777777777777790, 0.4541666666666666630, 0.4555555555555555469, 0.4562499999999999889 ),
 .UNSPECIFIED. ) 
 CURVE ( )  GEOMETRIC_REPRESENTATION_ITEM ( )  RATIONAL_B_SPLINE_CURVE ( ( 0.9330127018922194093, 0.9330127018922194093, 1.000000000000000000, 0.8660254037844387076, 1.000000000000000000, 0.8660254037844387076, 1.000000000000000000, 0.9330127018922194093, 0.9330127018922194093 ) ) 
 REPRESENTATION_ITEM ( '' )  );
#51635 = CARTESIAN_POINT ( 'NONE',  ( -57.19623071787017210, -152.6250000013656063, 4.297418129356382899 ) ) ;
#51636 = CARTESIAN_POINT ( 'NONE',  ( -5.000000000000000000, -147.5000000000000284, -6.123233995736766282E-16 ) ) ;
#51637 = CARTESIAN_POINT ( 'NONE',  ( 9.457646018065525792E-16, -29.06249999863440436, 5.148502694627439702 ) ) ;
#51638 = CARTESIAN_POINT ( 'NONE',  ( 4.458734124999998549, -69.97916666530107932, -2.574251347313721627 ) ) ;
#51639 = CARTESIAN_POINT ( 'NONE',  ( 5.000000000000000000, 8.500000000000000000, -6.123233995736766282E-16 ) ) ;
#51640 = CARTESIAN_POINT ( 'NONE',  ( -2.229367062499996610, -23.14583333196773651, 3.861377020970582219 ) ) ;
#51641 = CARTESIAN_POINT ( 'NONE',  ( 3.535533905932736864, -147.1250000000000000, 3.535533905932738641 ) ) ;
#51642 = CARTESIAN_POINT ( 'NONE',  ( -60.14911071818854538, -138.1875000027312126, 1.666127454062681146 ) ) ;
#51643 = CARTESIAN_POINT ( 'NONE',  ( 2.500000000000002220, -14.66666666666666785, 4.330127018922192761 ) ) ;
#51644 = CARTESIAN_POINT ( 'NONE',  ( 4.458734125000000326, -151.3750000013656063, -1.846868145590734978 ) ) ;
#51645 = VERTEX_POINT ( 'NONE', #2759 ) ;
#51646 = DIRECTION ( 'NONE',  ( -0.000000000000000000, 1.000000000000000000, -0.000000000000000000 ) ) ;
#51647 = CARTESIAN_POINT ( 'NONE',  ( -2.229367062500000163, -50.72916666530107221, -3.861377020970580443 ) ) ;
#51648 = CARTESIAN_POINT ( 'NONE',  ( 5.000000000000000000, -58.29166666393548013, -2.886751345948130876 ) ) ;
#51649 = CARTESIAN_POINT ( 'NONE',  ( 1.975475456537005874E-15, -78.74999999999998579, 5.000000000000000000 ) ) ;
#51650 = CARTESIAN_POINT ( 'NONE',  ( -4.999999999999999112, 22.08333333333333215, 2.886751345948131764 ) ) ;
#51651 = FACE_OUTER_BOUND ( 'NONE', #5085, .T. ) ;
#51652 = CARTESIAN_POINT ( 'NONE',  ( -4.458734124999999437, 1.604166668032262155, -2.574251347313719407 ) ) ;
#51653 =( BOUNDED_CURVE ( )  B_SPLINE_CURVE ( 2, ( #13161, #46313, #32784, #46629, #52093, #2270, #41469, #8032, #52415 ),
 .UNSPECIFIED., .F., .F. ) 
 B_SPLINE_CURVE_WITH_KNOTS ( ( 3, 2, 2, 2, 3 ),
 ( 0.1104166666666666630, 0.1111111111111111049, 0.1125000000000000028, 0.1138888888888888867, 0.1145833333333333426 ),
 .UNSPECIFIED. ) 
 CURVE ( )  GEOMETRIC_REPRESENTATION_ITEM ( )  RATIONAL_B_SPLINE_CURVE ( ( 0.9330127018922194093, 0.9330127018922194093, 1.000000000000000000, 0.8660254037844387076, 1.000000000000000000, 0.8660254037844387076, 1.000000000000000000, 0.9330127018922187432, 0.9330127018922194093 ) ) 
 REPRESENTATION_ITEM ( '' )  );
#51654 = CARTESIAN_POINT ( 'NONE',  ( -3.535533905932737309, -160.7500000027312126, -3.535533905932738197 ) ) ;
#51655 = CARTESIAN_POINT ( 'NONE',  ( 6.123233995736765296E-16, 15.00000000000000000, -4.999999999999999112 ) ) ;
#51656 = CARTESIAN_POINT ( 'NONE',  ( 2.500000000000002220, -7.666666666666668739, 4.330127018922192761 ) ) ;
#51657 = CARTESIAN_POINT ( 'NONE',  ( -4.458734124999999437, 17.35416666803225993, -2.574251347313719407 ) ) ;
#51658 = CARTESIAN_POINT ( 'NONE',  ( 5.000000000000000000, 3.625000002731186388, -6.123233995736766282E-16 ) ) ;
#51659 = ORIENTED_EDGE ( 'NONE', *, *, #59964, .F. ) ;
#51660 = CARTESIAN_POINT ( 'NONE',  ( -4.999999999999998224, -29.79166666393548013, 2.886751345948131764 ) ) ;
#51661 = ORIENTED_EDGE ( 'NONE', *, *, #52384, .T. ) ;
#51662 = CARTESIAN_POINT ( 'NONE',  ( 2.229367062499998831, -49.64583333196772941, -3.861377020970580887 ) ) ;
#51663 = CARTESIAN_POINT ( 'NONE',  ( -4.458734125000000326, -163.2500000013655495, -1.846868145590735644 ) ) ;
#51664 = CARTESIAN_POINT ( 'NONE',  ( 5.000000000000000000, -47.37499999726880873, -6.123233995736766282E-16 ) ) ;
#51665 = VERTEX_POINT ( 'NONE', #22059 ) ;
#51666 = CARTESIAN_POINT ( 'NONE',  ( -4.458734124999998549, -24.22916666530107577, 2.574251347313722516 ) ) ;
#51667 = ORIENTED_EDGE ( 'NONE', *, *, #44891, .T. ) ;
#51668 = CARTESIAN_POINT ( 'NONE',  ( -2.500000000000000444, -85.16666666666667140, -4.330127018922193649 ) ) ;
#51669 = CARTESIAN_POINT ( 'NONE',  ( 3.152801135295367541, -164.3125000013656063, -3.152801135295367541 ) ) ;
#51670 = ADVANCED_FACE ( 'NONE', ( #51651 ), #32335, .T. ) ;
#51671 = CARTESIAN_POINT ( 'NONE',  ( -1.339745962155610925, -50.66965819600732601, 5.000000000000000000 ) ) ;
#51672 = CARTESIAN_POINT ( 'NONE',  ( -59.81910112700025905, -138.1875000000000000, -2.462841084822630311 ) ) ;
#51673 = CARTESIAN_POINT ( 'NONE',  ( -2.229367062499996610, -34.39583333196772941, 3.861377020970582219 ) ) ;
#51674 = DIRECTION ( 'NONE',  ( 1.000000000000000000, 0.000000000000000000, -0.000000000000000000 ) ) ;
#51675 = ORIENTED_EDGE ( 'NONE', *, *, #3236, .T. ) ;
#51676 = EDGE_CURVE ( 'NONE', #23803, #50991, #61302, .T. ) ;
#51677 = CARTESIAN_POINT ( 'NONE',  ( 2.229367062499998831, -76.64583333196773651, -3.861377020970580887 ) ) ;
#51678 = CARTESIAN_POINT ( 'NONE',  ( 4.458734124999999437, 22.18750000136559564, -5.460374474430324690E-16 ) ) ;
#51679 = VERTEX_POINT ( 'NONE', #55837 ) ;
#51680 = CARTESIAN_POINT ( 'NONE',  ( -6.972266317189433020E-16, 9.875000002731185944, -5.000000000000000000 ) ) ;
#51681 = CARTESIAN_POINT ( 'NONE',  ( -57.19623071787016499, -140.6250000013656063, 4.297418129356382899 ) ) ;
#51682 = CARTESIAN_POINT ( 'NONE',  ( -2.229367062500000163, -78.72916666530106511, -3.861377020970580443 ) ) ;
#51683 = CARTESIAN_POINT ( 'NONE',  ( -59.81910112700025905, -130.3125000027312410, -2.462841084822630311 ) ) ;
#51684 = CARTESIAN_POINT ( 'NONE',  ( 3.061616997868383141E-16, -142.7500000000000284, -5.000000000000000000 ) ) ;
#51685 = CARTESIAN_POINT ( 'NONE',  ( 5.000000000000000888, -9.583333333333332149, 2.886751345948126879 ) ) ;
#51686 = CARTESIAN_POINT ( 'NONE',  ( 2.499999999999998668, 20.66666666666666785, -4.330127018922193649 ) ) ;
#51687 = CARTESIAN_POINT ( 'NONE',  ( -4.458734124999999437, -55.31249999863440081, 0.000000000000000000 ) ) ;
#51688 = CARTESIAN_POINT ( 'NONE',  ( 2.229367062500001939, -47.97916666530106511, 3.861377020970579999 ) ) ;
#51689 = CARTESIAN_POINT ( 'NONE',  ( 9.457646018065525792E-16, 28.93750000136559564, 5.148502694627439702 ) ) ;
#51690 = CARTESIAN_POINT ( 'NONE',  ( 1.060575238724906964E-15, -106.7499999999999716, 5.773502691896257311 ) ) ;
#51691 = CARTESIAN_POINT ( 'NONE',  ( -9.184850993605147944E-16, -159.3750000027311842, 5.000000000000000000 ) ) ;
#51692 = CARTESIAN_POINT ( 'NONE',  ( 9.457646018065525792E-16, -41.31249999863440081, 5.148502694627439702 ) ) ;
#51693 = CARTESIAN_POINT ( 'NONE',  ( -3.535250795749689387E-16, 2.875000002731185944, -5.773502691896257311 ) ) ;
#51694 = CARTESIAN_POINT ( 'NONE',  ( -1.230605004983934782E-13, -36.75000000000000711, 5.000000000000000000 ) ) ;
#51695 = CARTESIAN_POINT ( 'NONE',  ( -50.55543936806279248, -126.0625000013655921, 0.3552334253322060320 ) ) ;
#51696 = CARTESIAN_POINT ( 'NONE',  ( -4.458734124999999437, -79.64583333196772230, -2.574251347313719407 ) ) ;
#51697 = CARTESIAN_POINT ( 'NONE',  ( 1.975475456537005874E-15, 24.24999999999999645, 5.000000000000000000 ) ) ;
#51698 = CARTESIAN_POINT ( 'NONE',  ( -3.152548672688508926E-16, -102.5624999986344079, -5.148502694627439702 ) ) ;
#51699 = CARTESIAN_POINT ( 'NONE',  ( -4.458734124999997661, -5.479166665301072214, 2.574251347313722516 ) ) ;
#51700 =( BOUNDED_CURVE ( )  B_SPLINE_CURVE ( 2, ( #47760, #19107, #4331, #9462, #49011, #52908, #19434, #29072, #48695 ),
 .UNSPECIFIED., .F., .F. ) 
 B_SPLINE_CURVE_WITH_KNOTS ( ( 3, 2, 2, 2, 3 ),
 ( 0.8339285714285714635, 0.8345238095238095566, 0.8357142857142857428, 0.8369047619047619291, 0.8375000000000000222 ),
 .UNSPECIFIED. ) 
 CURVE ( )  GEOMETRIC_REPRESENTATION_ITEM ( )  RATIONAL_B_SPLINE_CURVE ( ( 0.9330127018922194093, 0.9330127018922194093, 1.000000000000000000, 0.8660254037844387076, 1.000000000000000000, 0.8660254037844387076, 1.000000000000000000, 0.9330127018922194093, 0.9330127018922194093 ) ) 
 REPRESENTATION_ITEM ( '' )  );
#51701 = EDGE_LOOP ( 'NONE', ( #15092, #37966, #43940, #38339 ) ) ;
#51702 = DIRECTION ( 'NONE',  ( -0.000000000000000000, 1.000000000000000000, -0.000000000000000000 ) ) ;
#51703 = CARTESIAN_POINT ( 'NONE',  ( -4.458734124999998549, -91.22916666530106511, 2.574251347313722516 ) ) ;
#51704 = CARTESIAN_POINT ( 'NONE',  ( -5.000000000000000000, -4.999999999999997335, 0.000000000000000000 ) ) ;
#51705 = CARTESIAN_POINT ( 'NONE',  ( 2.229367062500001939, -88.22916666530107932, 3.861377020970579999 ) ) ;
#51706 = CARTESIAN_POINT ( 'NONE',  ( 9.457646018065525792E-16, 11.68750000136559564, 5.148502694627439702 ) ) ;
#51707 = DIRECTION ( 'NONE',  ( -0.000000000000000000, 1.000000000000000000, -0.000000000000000000 ) ) ;
#51708 = CARTESIAN_POINT ( 'NONE',  ( -53.51423613279429503, -135.2500000013656347, 4.591703134518082763 ) ) ;
#51709 = CARTESIAN_POINT ( 'NONE',  ( -4.458734124999999437, -6.312499998634403475, 0.000000000000000000 ) ) ;
#51710 = CARTESIAN_POINT ( 'NONE',  ( 2.229367062500001939, 15.77083333469892601, 3.861377020970579999 ) ) ;
#51711 = CARTESIAN_POINT ( 'NONE',  ( 9.457646018065525792E-16, -54.31249999863440792, 5.148502694627439702 ) ) ;
#51712 = CARTESIAN_POINT ( 'NONE',  ( -3.535533905932737309, -163.6250000000000284, -3.535533905932738197 ) ) ;
#51713 = CARTESIAN_POINT ( 'NONE',  ( -3.535533905932737309, -152.6250000000000000, -3.535533905932738197 ) ) ;
#51714 = CARTESIAN_POINT ( 'NONE',  ( -3.152548672688508926E-16, -6.562499998634404363, -5.148502694627439702 ) ) ;
#51715 = FILL_AREA_STYLE ('',( #22128 ) ) ;
#51716 = ORIENTED_EDGE ( 'NONE', *, *, #48011, .T. ) ;
#51717 = CARTESIAN_POINT ( 'NONE',  ( 4.458734124999999437, -33.06249999863440792, -5.460374474430324690E-16 ) ) ;
#51718 = CARTESIAN_POINT ( 'NONE',  ( -58.39396692619412477, -127.6875000013656063, 2.891590998281057701 ) ) ;
#51719 = CARTESIAN_POINT ( 'NONE',  ( 2.500000000000002220, -68.66666666666667140, 4.330127018922192761 ) ) ;
#51720 = CARTESIAN_POINT ( 'NONE',  ( 4.458734124999998549, -82.72916666530106511, -2.574251347313721627 ) ) ;
#51721 = CARTESIAN_POINT ( 'NONE',  ( -2.229367062499996610, 22.60416666803225993, 3.861377020970582219 ) ) ;
#51722 = CARTESIAN_POINT ( 'NONE',  ( -1.846868145590737420, -151.0000000013656063, 4.458734124999997661 ) ) ;
#51723 = VECTOR ( 'NONE', #33165, 1000.000000000000000 ) ;
#51725 = EDGE_CURVE ( 'NONE', #50678, #22715, #57574, .T. ) ;
#51724 = CARTESIAN_POINT ( 'NONE',  ( -2.229367062500000163, 12.52083333469892601, -3.861377020970580443 ) ) ;
#51726 = DIRECTION ( 'NONE',  ( 0.000000000000000000, 0.000000000000000000, 1.000000000000000000 ) ) ;
#51727 = CARTESIAN_POINT ( 'NONE',  ( -3.152548672688508926E-16, -81.81249999863440792, -5.148502694627439702 ) ) ;
#51728 = CARTESIAN_POINT ( 'NONE',  ( 5.000000000000000888, -63.58333333333332149, 2.886751345948126879 ) ) ;
#51729 = DIRECTION ( 'NONE',  ( -0.000000000000000000, 1.000000000000000000, -0.000000000000000000 ) ) ;
#51730 = CARTESIAN_POINT ( 'NONE',  ( 5.000000000000000000, 17.70833333606451632, -2.886751345948129988 ) ) ;
#51731 = ORIENTED_EDGE ( 'NONE', *, *, #32159, .T. ) ;
#51732 = CARTESIAN_POINT ( 'NONE',  ( 5.000000000000000000, -18.29166666393547658, -2.886751345948130876 ) ) ;
#51733 =( BOUNDED_CURVE ( )  B_SPLINE_CURVE ( 2, ( #48934, #58289, #18725, #54083, #33215, #52833, #58604, #23571, #19034 ),
 .UNSPECIFIED., .F., .F. ) 
 B_SPLINE_CURVE_WITH_KNOTS ( ( 3, 2, 2, 2, 3 ),
 ( 0.5979166666666666519, 0.5986111111111110938, 0.5999999999999999778, 0.6013888888888888618, 0.6020833333333333037 ),
 .UNSPECIFIED. ) 
 CURVE ( )  GEOMETRIC_REPRESENTATION_ITEM ( )  RATIONAL_B_SPLINE_CURVE ( ( 0.9330127018922194093, 0.9330127018922194093, 1.000000000000000000, 0.8660254037844387076, 1.000000000000000000, 0.8660254037844387076, 1.000000000000000000, 0.9330127018922194093, 0.9330127018922194093 ) ) 
 REPRESENTATION_ITEM ( '' )  );
#51734 = CARTESIAN_POINT ( 'NONE',  ( -58.24261429053147765, -139.3750000027312126, -3.805975901505573855 ) ) ;
#51736 = CARTESIAN_POINT ( 'NONE',  ( -4.999999999999999112, -22.91666666666666785, 2.886751345948131764 ) ) ;
#51735 = DIRECTION ( 'NONE',  ( -0.000000000000000000, 1.000000000000000000, -0.000000000000000000 ) ) ;
#51737 = CARTESIAN_POINT ( 'NONE',  ( 2.229367062500001939, -28.97916666530107221, 3.861377020970579999 ) ) ;
#51738 = CARTESIAN_POINT ( 'NONE',  ( 5.000000000000000888, -27.45833333060214798, 2.886751345948126879 ) ) ;
#51740 = ORIENTED_EDGE ( 'NONE', *, *, #57023, .F. ) ;
#51739 = CARTESIAN_POINT ( 'NONE',  ( 4.458734124999999437, -58.81249999863440081, -5.460374474430324690E-16 ) ) ;
#51741 = LINE ( 'NONE', #37259, #14864 ) ;
#51743 = ORIENTED_EDGE ( 'NONE', *, *, #35440, .F. ) ;
#51742 = CARTESIAN_POINT ( 'NONE',  ( -4.458734124999999437, -8.645833331967736513, -2.574251347313719407 ) ) ;
#51744 = CARTESIAN_POINT ( 'NONE',  ( -3.535250795749689387E-16, -72.24999999999998579, -5.773502691896257311 ) ) ;
#51745 = CARTESIAN_POINT ( 'NONE',  ( -53.51423613279429503, -140.2500000013656063, 4.591703134518083651 ) ) ;
#51746 = CARTESIAN_POINT ( 'NONE',  ( -2.229367062499996610, -49.39583333196772941, 3.861377020970582219 ) ) ;
#51747 = CARTESIAN_POINT ( 'NONE',  ( 5.000000000000000000, -77.29166666393545881, -2.886751345948129988 ) ) ;
#51749 = ORIENTED_EDGE ( 'NONE', *, *, #60522, .T. ) ;
#51748 = DIRECTION ( 'NONE',  ( 0.000000000000000000, 0.000000000000000000, 1.000000000000000000 ) ) ;
#51750 = CARTESIAN_POINT ( 'NONE',  ( -56.66612745406270335, -150.3125000000000284, -5.149110718188516067 ) ) ;
#51751 = CARTESIAN_POINT ( 'NONE',  ( 2.229367062500001939, -18.22916666530106866, 3.861377020970579999 ) ) ;
#51752 = CARTESIAN_POINT ( 'NONE',  ( 4.458734124999999437, -56.06249999863440081, -5.460374474430324690E-16 ) ) ;
#51753 = CARTESIAN_POINT ( 'NONE',  ( 1.464175926609780648E-14, 22.74999999999999645, -5.000000000000000000 ) ) ;
#51754 = SURFACE_STYLE_USAGE ( .BOTH. , #2875 ) ;
#51755 = CARTESIAN_POINT ( 'NONE',  ( 1.846868145590735200, -169.5000000013655495, -4.458734125000000326 ) ) ;
#51756 = CARTESIAN_POINT ( 'NONE',  ( 4.458734124999998549, -99.97916666530106511, -2.574251347313721627 ) ) ;
#51757 = DIRECTION ( 'NONE',  ( 0.000000000000000000, 0.000000000000000000, 1.000000000000000000 ) ) ;
#51758 = ORIENTED_EDGE ( 'NONE', *, *, #27890, .T. ) ;
#51759 = CARTESIAN_POINT ( 'NONE',  ( -52.80376928212989185, -154.1250000013656063, -4.297418129356378458 ) ) ;
#51760 = CARTESIAN_POINT ( 'NONE',  ( -51.75738570946856498, -142.8750000027312126, 3.805975901505576964 ) ) ;
#51761 = CARTESIAN_POINT ( 'NONE',  ( 0.000000000000000000, -170.0000000000000000, 0.000000000000000000 ) ) ;
#51762 = CARTESIAN_POINT ( 'NONE',  ( -4.458734124999999437, -5.395833331967740953, -2.574251347313719407 ) ) ;
#51763 = CARTESIAN_POINT ( 'NONE',  ( 2.229367062499998831, -93.89583333196772230, -3.861377020970580887 ) ) ;
#51764 = CARTESIAN_POINT ( 'NONE',  ( 4.458734124999999437, -147.7500000013655779, 1.846868145590737864 ) ) ;
#51765 = CARTESIAN_POINT ( 'NONE',  ( 4.458734124999998549, -20.97916666530107221, -2.574251347313721627 ) ) ;
#51766 = FACE_OUTER_BOUND ( 'NONE', #45821, .T. ) ;
#51767 = CARTESIAN_POINT ( 'NONE',  ( -58.39396692619412477, -138.4375000013656063, 2.891590998281057701 ) ) ;
#51768 = CARTESIAN_POINT ( 'NONE',  ( 2.229367062500001939, -62.22916666530106511, 3.861377020970579999 ) ) ;
#51769 = CARTESIAN_POINT ( 'NONE',  ( -6.972266317189433020E-16, -66.24999999999998579, -5.000000000000000000 ) ) ;
#51770 = FACE_OUTER_BOUND ( 'NONE', #11501, .T. ) ;
#51771 = CARTESIAN_POINT ( 'NONE',  ( 3.152801135295366208, -145.5625000013655779, 3.152801135295367985 ) ) ;
#51772 = CARTESIAN_POINT ( 'NONE',  ( 4.458734125000000326, 11.85416666803225993, 2.574251347313718519 ) ) ;
#51773 = ORIENTED_EDGE ( 'NONE', *, *, #2726, .T. ) ;
#51774 = CARTESIAN_POINT ( 'NONE',  ( 2.500000000000002220, -61.66666666666666430, 4.330127018922192761 ) ) ;
#51776 = CARTESIAN_POINT ( 'NONE',  ( -4.458734124999998549, -26.22916666530106866, 2.574251347313722516 ) ) ;
#51775 = CARTESIAN_POINT ( 'NONE',  ( -2.499999999999996447, -88.83333333333332860, 4.330127018922195425 ) ) ;
#51777 = DIRECTION ( 'NONE',  ( -0.000000000000000000, 1.000000000000000000, -0.000000000000000000 ) ) ;
#51778 = CARTESIAN_POINT ( 'NONE',  ( -3.152548672688508926E-16, -71.81249999863439371, -5.148502694627439702 ) ) ;
#51779 = EDGE_CURVE ( 'NONE', #42402, #45642, #41342, .T. ) ;
#51780 = CARTESIAN_POINT ( 'NONE',  ( -3.152548672688508926E-16, 29.18750000136559208, -5.148502694627439702 ) ) ;
#51781 = DIRECTION ( 'NONE',  ( 0.000000000000000000, 0.000000000000000000, 1.000000000000000000 ) ) ;
#51782 = CARTESIAN_POINT ( 'NONE',  ( -50.55543936806279248, -146.0625000013656063, 0.3552334253322060320 ) ) ;
#51783 = CARTESIAN_POINT ( 'NONE',  ( 4.250000000000000000, 0.000000000000000000, -0.5251556536572846712 ) ) ;
#51784 = CARTESIAN_POINT ( 'NONE',  ( -4.458734124999999437, 6.604166668032259935, -2.574251347313719407 ) ) ;
#51785 = LINE ( 'NONE', #36995, #42741 ) ;
#51786 = CARTESIAN_POINT ( 'NONE',  ( -5.000000000000000000, -15.08333333333333215, -2.886751345948128211 ) ) ;
#51787 = CARTESIAN_POINT ( 'NONE',  ( 4.458734125000000326, 6.104166668032262599, 2.574251347313718519 ) ) ;
#51788 = CARTESIAN_POINT ( 'NONE',  ( 9.457646018065525792E-16, -74.06249999863440792, 5.148502694627439702 ) ) ;
#51789 = CARTESIAN_POINT ( 'NONE',  ( -3.152548672688508926E-16, -18.81249999863440792, -5.148502694627439702 ) ) ;
#51790 = CARTESIAN_POINT ( 'NONE',  ( 5.000000000000000000, 0.5833333333333314830, -2.886751345948129988 ) ) ;
#51791 = CARTESIAN_POINT ( 'NONE',  ( -4.458734125000000326, -159.0000000013656063, -1.846868145590735644 ) ) ;
#51792 = CARTESIAN_POINT ( 'NONE',  ( 2.500000000000002220, 23.33333333333333215, 4.330127018922192761 ) ) ;
#51793 = CARTESIAN_POINT ( 'NONE',  ( -4.458734124999999437, -66.39583333196773651, -2.574251347313719407 ) ) ;
#51794 = CARTESIAN_POINT ( 'NONE',  ( 5.000000000000000888, -101.4583333306021586, 2.886751345948126879 ) ) ;
#51795 = CARTESIAN_POINT ( 'NONE',  ( 1.975475456537005874E-15, 5.375000002731185944, 5.000000000000000000 ) ) ;
#51796 = CARTESIAN_POINT ( 'NONE',  ( -3.152548672688508926E-16, -38.56249999863440081, -5.148502694627439702 ) ) ;
#51797 = LINE ( 'NONE', #45700, #20477 ) ;
#51798 = CARTESIAN_POINT ( 'NONE',  ( 9.457646018065525792E-16, -69.31249999863439371, 5.148502694627439702 ) ) ;
#51799 = CARTESIAN_POINT ( 'NONE',  ( 5.000000000000000000, -46.41666666666666430, -2.886751345948129988 ) ) ;
#51800 = CARTESIAN_POINT ( 'NONE',  ( 5.000000000000000000, -152.1875000027312126, 2.071067811865478614 ) ) ;
#51801 = ORIENTED_EDGE ( 'NONE', *, *, #42411, .F. ) ;
#51802 = CARTESIAN_POINT ( 'NONE',  ( -2.229367062500000163, -109.4791666653010651, -3.861377020970580443 ) ) ;
#51803 = DIRECTION ( 'NONE',  ( 0.000000000000000000, -1.000000000000000000, 0.000000000000000000 ) ) ;
#51804 = CARTESIAN_POINT ( 'NONE',  ( -3.535250795749689387E-16, -9.250000000000001776, -5.773502691896257311 ) ) ;
#51805 = CARTESIAN_POINT ( 'NONE',  ( 4.458734124999998549, -69.72916666530107932, -2.574251347313721627 ) ) ;
#51806 = DIRECTION ( 'NONE',  ( -0.000000000000000000, 1.000000000000000000, -0.000000000000000000 ) ) ;
#51807 = CARTESIAN_POINT ( 'NONE',  ( -3.535250795749689387E-16, -13.12499999726881050, -5.773502691896257311 ) ) ;
#51809 = EDGE_LOOP ( 'NONE', ( #7691, #23590, #6035, #37988 ) ) ;
#51808 = CARTESIAN_POINT ( 'NONE',  ( 4.458734124999999437, -41.81249999863440081, -5.460374474430324690E-16 ) ) ;
#51810 = CARTESIAN_POINT ( 'NONE',  ( -6.972266317189433020E-16, -100.1249999972688016, -5.000000000000000000 ) ) ;
#51812 = ORIENTED_EDGE ( 'NONE', *, *, #9968, .F. ) ;
#51811 = CARTESIAN_POINT ( 'NONE',  ( -4.458734124999999437, 5.354166668032262599, -2.574251347313719407 ) ) ;
#51813 = CARTESIAN_POINT ( 'NONE',  ( 2.499999999999998668, -34.20833333060213732, -4.330127018922193649 ) ) ;
#51814 = CARTESIAN_POINT ( 'NONE',  ( 2.500000000000002220, -56.66666666666667140, 4.330127018922192761 ) ) ;
#51815 = CARTESIAN_POINT ( 'NONE',  ( 4.458734124999999437, -159.6875000013655779, 0.000000000000000000 ) ) ;
#51816 = CARTESIAN_POINT ( 'NONE',  ( -2.229367062499996610, -37.39583333196773651, 3.861377020970582219 ) ) ;
#51817 = CARTESIAN_POINT ( 'NONE',  ( 5.000000000000000888, -10.58333333333333393, 2.886751345948126879 ) ) ;
#51818 = CARTESIAN_POINT ( 'NONE',  ( 9.457646018065525792E-16, -80.06249999863439371, 5.148502694627439702 ) ) ;
#51819 = CARTESIAN_POINT ( 'NONE',  ( 5.000000000000000888, -167.9375000000000000, -2.071067811865475505 ) ) ;
#51820 = CARTESIAN_POINT ( 'NONE',  ( -4.458734124999999437, -88.31249999863439371, 0.000000000000000000 ) ) ;
#51821 = CARTESIAN_POINT ( 'NONE',  ( -59.59170313451811296, -132.7500000013656063, 1.485763867205729394 ) ) ;
#51822 = CARTESIAN_POINT ( 'NONE',  ( -4.458734124999999437, 0.4375000013655955255, 0.000000000000000000 ) ) ;
#51823 = CARTESIAN_POINT ( 'NONE',  ( 9.457646018065525792E-16, -37.31249999863440792, 5.148502694627439702 ) ) ;
#51824 =( BOUNDED_CURVE ( )  B_SPLINE_CURVE ( 2, ( #45565, #54263, #60380, #10509, #891, #11152, #49753, #30123, #35926 ),
 .UNSPECIFIED., .F., .F. ) 
 B_SPLINE_CURVE_WITH_KNOTS ( ( 3, 2, 2, 2, 3 ),
 ( 0.2854166666666666519, 0.2861111111111110938, 0.2874999999999999778, 0.2888888888888888618, 0.2895833333333333592 ),
 .UNSPECIFIED. ) 
 CURVE ( )  GEOMETRIC_REPRESENTATION_ITEM ( )  RATIONAL_B_SPLINE_CURVE ( ( 0.9330127018922194093, 0.9330127018922194093, 1.000000000000000000, 0.8660254037844387076, 1.000000000000000000, 0.8660254037844387076, 1.000000000000000000, 0.9330127018922167448, 0.9330127018922194093 ) ) 
 REPRESENTATION_ITEM ( '' )  );
#51825 = CARTESIAN_POINT ( 'NONE',  ( 5.000000000000000888, -16.45833333060214443, 2.886751345948126879 ) ) ;
#51826 = CARTESIAN_POINT ( 'NONE',  ( 2.229367062499998831, -84.89583333196773651, -3.861377020970580887 ) ) ;
#51827 = CARTESIAN_POINT ( 'NONE',  ( -6.972266317189433020E-16, 15.87500000273118417, -5.000000000000000000 ) ) ;
#51828 = ORIENTED_EDGE ( 'NONE', *, *, #6876, .F. ) ;
#51829 = CARTESIAN_POINT ( 'NONE',  ( -5.000000000000000000, -141.5000000000000284, -6.123233995736766282E-16 ) ) ;
#51830 = CARTESIAN_POINT ( 'NONE',  ( 0.000000000000000000, -120.0000000000000000, 5.000000000000000000 ) ) ;
#51831 = CARTESIAN_POINT ( 'NONE',  ( 4.458734124999998549, -70.97916666530107932, -2.574251347313721627 ) ) ;
#51832 = CARTESIAN_POINT ( 'NONE',  ( -3.152548672688508926E-16, -36.56249999863441502, -5.148502694627439702 ) ) ;
#51833 = CARTESIAN_POINT ( 'NONE',  ( -4.458734124999998549, -10.47916666530107044, 2.574251347313722516 ) ) ;
#51834 = VERTEX_POINT ( 'NONE', #18174 ) ;
#51835 = CARTESIAN_POINT ( 'NONE',  ( -9.184850993605147944E-16, -150.3750000027312126, 5.000000000000000000 ) ) ;
#51836 = CYLINDRICAL_SURFACE ( 'NONE', #11144, 5.000000000000000000 ) ;
#51837 = CARTESIAN_POINT ( 'NONE',  ( 4.458734125000001214, -5.145833331967740065, 2.574251347313718519 ) ) ;
#51838 = CARTESIAN_POINT ( 'NONE',  ( -5.000000000000000000, 2.999999999999999112, 0.000000000000000000 ) ) ;
#51839 = CARTESIAN_POINT ( 'NONE',  ( 2.229367062500001939, 2.020833334698927786, 3.861377020970579999 ) ) ;
#51840 = CARTESIAN_POINT ( 'NONE',  ( -2.500000000000000444, -33.04166666393547303, -4.330127018922193649 ) ) ;
#51841 = CARTESIAN_POINT ( 'NONE',  ( 4.458734124999999437, -155.3750000013656063, -1.846868145590734978 ) ) ;
#51842 = CARTESIAN_POINT ( 'NONE',  ( -2.229367062499996610, 27.60416666803225993, 3.861377020970582219 ) ) ;
#51843 = ORIENTED_EDGE ( 'NONE', *, *, #1594, .T. ) ;
#51844 = CARTESIAN_POINT ( 'NONE',  ( -2.229367062499996610, -86.14583333196773651, 3.861377020970582219 ) ) ;
#51845 = CARTESIAN_POINT ( 'NONE',  ( -1.339745962155610925, -30.79465819873851373, 5.000000000000000000 ) ) ;
#51846 = CARTESIAN_POINT ( 'NONE',  ( 2.229367062499998831, -10.64583333196773829, -3.861377020970580887 ) ) ;
#51847 = EDGE_CURVE ( 'NONE', #11867, #44276, #8839, .T. ) ;
#51848 = DIRECTION ( 'NONE',  ( 0.000000000000000000, 0.000000000000000000, 1.000000000000000000 ) ) ;
#51849 = CARTESIAN_POINT ( 'NONE',  ( -6.972266317189433020E-16, -48.24999999999999289, -5.000000000000000000 ) ) ;
#51850 = VECTOR ( 'NONE', #6725, 1000.000000000000000 ) ;
#51851 = CARTESIAN_POINT ( 'NONE',  ( -51.19402409849444524, -138.5000000000000284, -3.242614290531456334 ) ) ;
#51852 = CARTESIAN_POINT ( 'NONE',  ( -5.000000000000000000, -37.95833333060214443, -2.886751345948128211 ) ) ;
#51853 = DIRECTION ( 'NONE',  ( -0.000000000000000000, 1.000000000000000000, -0.000000000000000000 ) ) ;
#51854 = CARTESIAN_POINT ( 'NONE',  ( -2.229367062500000163, 25.52083333469892779, -3.861377020970580443 ) ) ;
#51855 = CARTESIAN_POINT ( 'NONE',  ( -5.000000000000000000, -3.999999999999996447, 0.000000000000000000 ) ) ;
#51856 = CARTESIAN_POINT ( 'NONE',  ( 9.457646018065525792E-16, 24.93750000136559208, 5.148502694627439702 ) ) ;
#51857 = CARTESIAN_POINT ( 'NONE',  ( -4.458734124999999437, -55.31249999863440081, 0.000000000000000000 ) ) ;
#51858 = CARTESIAN_POINT ( 'NONE',  ( -2.229367062500000163, -3.729166665301070438, -3.861377020970580443 ) ) ;
#51859 = CARTESIAN_POINT ( 'NONE',  ( -5.000000000000000000, 9.125000002731184168, 0.000000000000000000 ) ) ;
#51860 = CARTESIAN_POINT ( 'NONE',  ( 5.000000000000000888, 14.41666666666666785, 2.886751345948126879 ) ) ;
#51861 = CARTESIAN_POINT ( 'NONE',  ( 5.000000000000000000, -143.1250000027312126, 0.000000000000000000 ) ) ;
#51863 = EDGE_CURVE ( 'NONE', #54901, #46689, #33315, .T. ) ;
#51862 = CARTESIAN_POINT ( 'NONE',  ( -2.499999999999996447, -20.70833333060214798, 4.330127018922195425 ) ) ;
#51864 = CARTESIAN_POINT ( 'NONE',  ( 2.229367062500001939, -46.97916666530106511, 3.861377020970579999 ) ) ;
#51865 = CARTESIAN_POINT ( 'NONE',  ( -5.000000000000000000, -83.95833333060214443, -2.886751345948128211 ) ) ;
#51866 = CARTESIAN_POINT ( 'NONE',  ( -52.80376928212989185, -140.1250000013655779, -4.297418129356379346 ) ) ;
#51867 = DIRECTION ( 'NONE',  ( -0.000000000000000000, 1.000000000000000000, -0.000000000000000000 ) ) ;
#51868 = CARTESIAN_POINT ( 'NONE',  ( 5.000000000000000888, -36.58333333333332149, 2.886751345948126879 ) ) ;
#51869 = EDGE_CURVE ( 'NONE', #22249, #61639, #33905, .T. ) ;
#51870 = CARTESIAN_POINT ( 'NONE',  ( -4.458734124999997661, -86.47916666530107932, 2.574251347313722516 ) ) ;
#51871 = CARTESIAN_POINT ( 'NONE',  ( 3.152801135295367541, -156.5625000013656063, -3.152801135295367541 ) ) ;
#51872 =( BOUNDED_CURVE ( )  B_SPLINE_CURVE ( 2, ( #12789, #43003, #37551, #8912, #48144, #43315, #38484, #63581, #5354 ),
 .UNSPECIFIED., .F., .F. ) 
 B_SPLINE_CURVE_WITH_KNOTS ( ( 3, 2, 2, 2, 3 ),
 ( 0.5553571428571428825, 0.5559523809523809756, 0.5571428571428571619, 0.5583333333333333481, 0.5589285714285714413 ),
 .UNSPECIFIED. ) 
 CURVE ( )  GEOMETRIC_REPRESENTATION_ITEM ( )  RATIONAL_B_SPLINE_CURVE ( ( 0.9330127018922194093, 0.9330127018922194093, 1.000000000000000000, 0.8660254037844387076, 1.000000000000000000, 0.8660254037844387076, 1.000000000000000000, 0.9330127018922194093, 0.9330127018922194093 ) ) 
 REPRESENTATION_ITEM ( '' )  );
#51873 = CARTESIAN_POINT ( 'NONE',  ( -5.000000000000000000, -31.08333333333332860, -2.886751345948128211 ) ) ;
#51874 = DIRECTION ( 'NONE',  ( 0.000000000000000000, 0.000000000000000000, 1.000000000000000000 ) ) ;
#51875 = ORIENTED_EDGE ( 'NONE', *, *, #28898, .T. ) ;
#51876 = CARTESIAN_POINT ( 'NONE',  ( -3.152548672688508926E-16, 18.18750000136559564, -5.148502694627439702 ) ) ;
#51877 = ORIENTED_EDGE ( 'NONE', *, *, #49243, .F. ) ;
#51878 = CARTESIAN_POINT ( 'NONE',  ( 2.229367062500001939, -95.97916666530105090, 3.861377020970579999 ) ) ;
#51879 = CARTESIAN_POINT ( 'NONE',  ( -4.458734124999999437, 14.35416666803226171, -2.574251347313719407 ) ) ;
#51880 = CARTESIAN_POINT ( 'NONE',  ( -5.000000000000000000, 19.04166666939785202, -2.886751345948128211 ) ) ;
#51881 = LINE ( 'NONE', #61864, #18591 ) ;
#51882 = CARTESIAN_POINT ( 'NONE',  ( 5.000000000000000888, 7.416666666666665186, 2.886751345948126879 ) ) ;
#51883 = CARTESIAN_POINT ( 'NONE',  ( 4.458734125000000326, -54.89583333196774362, 2.574251347313718519 ) ) ;
#51884 = CARTESIAN_POINT ( 'NONE',  ( -6.972266317189433020E-16, -53.12499999726880162, -5.000000000000000000 ) ) ;
#51885 = CARTESIAN_POINT ( 'NONE',  ( -2.500000000000000444, -81.16666666666667140, -4.330127018922193649 ) ) ;
#51886 = CARTESIAN_POINT ( 'NONE',  ( -50.40829686548195099, -136.2500000013656063, -1.485763867205728284 ) ) ;
#51887 = CARTESIAN_POINT ( 'NONE',  ( 1.339745962155615144, -40.58034179853029144, 4.999999999999999112 ) ) ;
#51888 = CARTESIAN_POINT ( 'NONE',  ( -6.972266317189433020E-16, -63.25000000000000000, -5.000000000000000000 ) ) ;
#51889 = CARTESIAN_POINT ( 'NONE',  ( -5.000000000000000888, -151.6875000027312126, -2.071067811865475949 ) ) ;
#51890 = CARTESIAN_POINT ( 'NONE',  ( -2.499999999999996447, -38.83333333333332860, 4.330127018922195425 ) ) ;
#51891 = CARTESIAN_POINT ( 'NONE',  ( 5.000000000000000000, -107.4166666666666430, -2.886751345948130876 ) ) ;
#51893 = CARTESIAN_POINT ( 'NONE',  ( -4.458734124999998549, -19.47916666530107221, 2.574251347313722516 ) ) ;
#51892 = CARTESIAN_POINT ( 'NONE',  ( -5.000000000000000000, 13.91666666666666785, -2.886751345948128211 ) ) ;
#51894 = CARTESIAN_POINT ( 'NONE',  ( -5.000000000000000000, 12.91666666666666607, -2.886751345948128211 ) ) ;
#51895 = CARTESIAN_POINT ( 'NONE',  ( -4.458734124999999437, -66.39583333196773651, -2.574251347313719407 ) ) ;
#51896 = CARTESIAN_POINT ( 'NONE',  ( -4.458734125000001214, -148.1250000013655779, 1.846868145590734089 ) ) ;
#51897 = CARTESIAN_POINT ( 'NONE',  ( -4.458734124999999437, -72.39583333196775072, -2.574251347313719407 ) ) ;
#51898 = CARTESIAN_POINT ( 'NONE',  ( -50.55543936806279248, -144.3125000013656063, 0.3552334253322060320 ) ) ;
#51899 = CARTESIAN_POINT ( 'NONE',  ( 4.458734125000001214, -20.14583333196774007, 2.574251347313718519 ) ) ;
#51900 = CARTESIAN_POINT ( 'NONE',  ( -5.000000000000000000, -61.95833333060215153, -2.886751345948128211 ) ) ;
#51901 = ORIENTED_EDGE ( 'NONE', *, *, #33394, .T. ) ;
#51902 = EDGE_CURVE ( 'NONE', #33278, #56532, #4630, .T. ) ;
#51903 = DIRECTION ( 'NONE',  ( 0.000000000000000000, 0.000000000000000000, 1.000000000000000000 ) ) ;
#51904 = EDGE_LOOP ( 'NONE', ( #49668, #37736, #33289, #39623 ) ) ;
#51905 =( BOUNDED_CURVE ( )  B_SPLINE_CURVE ( 2, ( #40559, #26093, #21905, #45390, #60202, #36063, #31549, #56006, #55692 ),
 .UNSPECIFIED., .F., .F. ) 
 B_SPLINE_CURVE_WITH_KNOTS ( ( 3, 2, 2, 2, 3 ),
 ( 0.3895833333333333370, 0.3902777777777777790, 0.3916666666666666630, 0.3930555555555555469, 0.3937499999999999889 ),
 .UNSPECIFIED. ) 
 CURVE ( )  GEOMETRIC_REPRESENTATION_ITEM ( )  RATIONAL_B_SPLINE_CURVE ( ( 0.9330127018922194093, 0.9330127018922194093, 1.000000000000000000, 0.8660254037844387076, 1.000000000000000000, 0.8660254037844387076, 1.000000000000000000, 0.9330127018922194093, 0.9330127018922194093 ) ) 
 REPRESENTATION_ITEM ( '' )  );
#51906 = CARTESIAN_POINT ( 'NONE',  ( -2.229367062499996610, -65.39583333196773651, 3.861377020970582219 ) ) ;
#51907 = CARTESIAN_POINT ( 'NONE',  ( 5.000000000000000000, -7.374999997268813168, -6.123233995736766282E-16 ) ) ;
#51908 = VERTEX_POINT ( 'NONE', #38719 ) ;
#51909 = CARTESIAN_POINT ( 'NONE',  ( 1.975475456537005874E-15, -53.62499999726880162, 5.000000000000000000 ) ) ;
#51910 = CARTESIAN_POINT ( 'NONE',  ( -57.46284108482265651, -126.9375000000000284, 4.819101127000239515 ) ) ;
#51911 = CARTESIAN_POINT ( 'NONE',  ( 5.000000000000000000, -8.416666666666669627, -2.886751345948130876 ) ) ;
#51912 = CARTESIAN_POINT ( 'NONE',  ( 2.229367062500001939, -56.22916666530107221, 3.861377020970579999 ) ) ;
#51913 = ORIENTED_EDGE ( 'NONE', *, *, #27971, .F. ) ;
#51914 = CARTESIAN_POINT ( 'NONE',  ( -4.999999999999998224, -54.91666666666667140, 2.886751345948131764 ) ) ;
#51915 = CARTESIAN_POINT ( 'NONE',  ( -2.229367062499996610, 8.854166668032261711, 3.861377020970582219 ) ) ;
#51916 = CARTESIAN_POINT ( 'NONE',  ( 4.458734124999999437, 17.18750000136559564, -5.460374474430324690E-16 ) ) ;
#51917 = CARTESIAN_POINT ( 'NONE',  ( -50.70258187064364108, -147.1250000013656063, 2.196230717870141014 ) ) ;
#51918 = CARTESIAN_POINT ( 'NONE',  ( 5.000000000000000000, -78.37499999726881583, -6.123233995736766282E-16 ) ) ;
#51919 = CARTESIAN_POINT ( 'NONE',  ( 5.000000000000000000, -165.0000000000000000, 0.000000000000000000 ) ) ;
#51920 =( BOUNDED_CURVE ( )  B_SPLINE_CURVE ( 2, ( #47291, #3242, #22541, #51800, #41495, #37011, #27976, #37954, #61148 ),
 .UNSPECIFIED., .F., .F. ) 
 B_SPLINE_CURVE_WITH_KNOTS ( ( 3, 2, 2, 2, 3 ),
 ( 0.5583333333333337922, 0.5625000000000004441, 0.5666666666666670960, 0.5708333333333338588, 0.5750000000000005107 ),
 .UNSPECIFIED. ) 
 CURVE ( )  GEOMETRIC_REPRESENTATION_ITEM ( )  RATIONAL_B_SPLINE_CURVE ( ( 0.9999999999999918954, 0.9238795325112948431, 1.000000000000000000, 0.9238795325112867385, 1.000000000000000000, 0.9238795325112867385, 1.000000000000000000, 0.9238795325112766355, 1.000000000000010214 ) ) 
 REPRESENTATION_ITEM ( '' )  );
#51921 = VERTEX_POINT ( 'NONE', #39041 ) ;
#51922 = CARTESIAN_POINT ( 'NONE',  ( -4.458734124999997661, -69.22916666530107932, 2.574251347313722516 ) ) ;
#51923 = LINE ( 'NONE', #17822, #15065 ) ;
#51924 = CARTESIAN_POINT ( 'NONE',  ( 4.458734124999998549, 6.270833334698928674, -2.574251347313721627 ) ) ;
#51925 = EDGE_CURVE ( 'NONE', #59890, #53853, #39873, .T. ) ;
#51926 = EDGE_CURVE ( 'NONE', #9545, #19516, #46475, .T. ) ;
#51927 = CARTESIAN_POINT ( 'NONE',  ( 9.457646018065525792E-16, -61.31249999863440792, 5.148502694627439702 ) ) ;
#51928 = CARTESIAN_POINT ( 'NONE',  ( -2.500000000000000444, -18.04166666393547658, -4.330127018922193649 ) ) ;
#51929 = LINE ( 'NONE', #27789, #14189 ) ;
#51930 = DIRECTION ( 'NONE',  ( 0.000000000000000000, 0.000000000000000000, 1.000000000000000000 ) ) ;
#51931 = CARTESIAN_POINT ( 'NONE',  ( -50.01589407740564042, -140.7500000027312126, 0.3983568153799778022 ) ) ;
#51932 = CARTESIAN_POINT ( 'NONE',  ( -5.000000000000000000, -83.87499999726880162, 0.000000000000000000 ) ) ;
#51933 = CARTESIAN_POINT ( 'NONE',  ( -4.458734124999999437, -36.39583333196772941, -2.574251347313719407 ) ) ;
#51934 = CARTESIAN_POINT ( 'NONE',  ( -2.229367062499996610, -23.39583333196773651, 3.861377020970582219 ) ) ;
#51935 = ORIENTED_EDGE ( 'NONE', *, *, #2413, .T. ) ;
#51936 = CYLINDRICAL_SURFACE ( 'NONE', #1212, 5.000000000000000000 ) ;
#51937 = CARTESIAN_POINT ( 'NONE',  ( -5.000000000000000000, 28.91666666666666430, -2.886751345948128211 ) ) ;
#51938 = CARTESIAN_POINT ( 'NONE',  ( 3.535533905932738197, -155.0000000027312126, -3.535533905932738197 ) ) ;
#51939 = ORIENTED_EDGE ( 'NONE', *, *, #29898, .F. ) ;
#51940 = CARTESIAN_POINT ( 'NONE',  ( -4.458734124999999437, -108.5624999986343937, 0.000000000000000000 ) ) ;
#51941 = CARTESIAN_POINT ( 'NONE',  ( 9.457646018065525792E-16, -33.06249999863440792, 5.148502694627439702 ) ) ;
#51942 = CARTESIAN_POINT ( 'NONE',  ( -2.499999999999996447, -60.70833333060214443, 4.330127018922195425 ) ) ;
#51943 = EDGE_CURVE ( 'NONE', #4579, #14700, #8527, .T. ) ;
#51944 = AXIS2_PLACEMENT_3D ( 'NONE', #27314, #47561, #37592 ) ;
#51945 = CARTESIAN_POINT ( 'NONE',  ( -58.39396692619412477, -150.6875000013656063, 2.891590998281057701 ) ) ;
#51946 = CARTESIAN_POINT ( 'NONE',  ( 2.071067811865476394, -147.1875000000000284, 5.000000000000000000 ) ) ;
#51947 = CARTESIAN_POINT ( 'NONE',  ( 4.458734124999998549, -30.72916666530107221, -2.574251347313721627 ) ) ;
#51948 = ADVANCED_FACE ( 'NONE', ( #3710 ), #4955, .T. ) ;
#51949 = CARTESIAN_POINT ( 'NONE',  ( 2.229367062499998831, -68.89583333196773651, -3.861377020970580887 ) ) ;
#51950 = CARTESIAN_POINT ( 'NONE',  ( 1.339745962155618697, 22.83034180399266688, -4.999999999999998224 ) ) ;
#51951 = CARTESIAN_POINT ( 'NONE',  ( 9.457646018065525792E-16, -25.06249999863440792, 5.148502694627439702 ) ) ;
#51952 = CARTESIAN_POINT ( 'NONE',  ( 3.061616997868383141E-16, -157.8750000027311842, -5.000000000000000000 ) ) ;
#51953 = CARTESIAN_POINT ( 'NONE',  ( -1.339745962155610925, 9.330341803992663330, 5.000000000000000000 ) ) ;
#51954 = CARTESIAN_POINT ( 'NONE',  ( 1.060575238724906964E-15, -18.75000000000000000, 5.773502691896257311 ) ) ;
#51955 = CARTESIAN_POINT ( 'NONE',  ( 1.846868145590735200, -149.2500000013655779, -4.458734125000000326 ) ) ;
#51956 = ORIENTED_EDGE ( 'NONE', *, *, #53943, .T. ) ;
#51957 = DIRECTION ( 'NONE',  ( 0.000000000000000000, 0.000000000000000000, 1.000000000000000000 ) ) ;
#51958 = CARTESIAN_POINT ( 'NONE',  ( 4.458734125000000326, -53.14583333196773651, 2.574251347313718519 ) ) ;
#51959 = CARTESIAN_POINT ( 'NONE',  ( 2.500000000000002220, -84.54166666393547303, 4.330127018922192761 ) ) ;
#51960 = CARTESIAN_POINT ( 'NONE',  ( -1.339745962155610925, -0.7946581987385198387, 5.000000000000000000 ) ) ;
#51961 = CARTESIAN_POINT ( 'NONE',  ( -2.500000000000000444, 25.83333333333333215, -4.330127018922193649 ) ) ;
#51962 = DIRECTION ( 'NONE',  ( -0.000000000000000000, 1.000000000000000000, -0.000000000000000000 ) ) ;
#51963 = CARTESIAN_POINT ( 'NONE',  ( -2.229367062500000163, -2.479166665301069106, -3.861377020970580443 ) ) ;
#51964 = CARTESIAN_POINT ( 'NONE',  ( 5.000000000000000000, -48.41666666666666430, -2.886751345948130876 ) ) ;
#51965 = CARTESIAN_POINT ( 'NONE',  ( 5.000000000000000888, -140.9375000000000284, -2.071067811865475505 ) ) ;
#51966 = CARTESIAN_POINT ( 'NONE',  ( 1.339745962155615144, -7.705341801261480938, 4.999999999999999112 ) ) ;
#51967 = CARTESIAN_POINT ( 'NONE',  ( 2.229367062499998831, 8.104166668032261711, -3.861377020970580887 ) ) ;
#51968 = ORIENTED_EDGE ( 'NONE', *, *, #29322, .T. ) ;
#51969 = DIRECTION ( 'NONE',  ( 0.000000000000000000, 0.000000000000000000, 1.000000000000000000 ) ) ;
#51970 = ORIENTED_EDGE ( 'NONE', *, *, #41156, .T. ) ;
#51971 = CYLINDRICAL_SURFACE ( 'NONE', #30672, 5.000000000000000000 ) ;
#51972 = CARTESIAN_POINT ( 'NONE',  ( 2.229367062500001939, -50.97916666530107221, 3.861377020970579999 ) ) ;
#51973 = CARTESIAN_POINT ( 'NONE',  ( -1.846868145590734756, -159.3750000013656347, -4.458734125000000326 ) ) ;
#51974 = CARTESIAN_POINT ( 'NONE',  ( -2.500000000000000444, -44.04166666393546592, -4.330127018922193649 ) ) ;
#51975 = ORIENTED_EDGE ( 'NONE', *, *, #4992, .T. ) ;
#51976 = CARTESIAN_POINT ( 'NONE',  ( 2.229367062500001939, -24.97916666530106866, 3.861377020970579999 ) ) ;
#51977 = ORIENTED_EDGE ( 'NONE', *, *, #5820, .F. ) ;
#51978 = CARTESIAN_POINT ( 'NONE',  ( -5.000000000000000000, -142.6250000027312126, -6.123233995736766282E-16 ) ) ;
#51979 = CARTESIAN_POINT ( 'NONE',  ( -8.190561711645485556E-16, -163.6875000013655779, 4.458734124999999437 ) ) ;
#51980 = DIRECTION ( 'NONE',  ( 0.000000000000000000, 0.000000000000000000, -1.000000000000000000 ) ) ;
#51981 = CARTESIAN_POINT ( 'NONE',  ( -52.53715891517739323, -137.4375000000000284, -4.819101127000233298 ) ) ;
#51982 = CARTESIAN_POINT ( 'NONE',  ( -2.229367062500000163, -39.72916666530107221, -3.861377020970580443 ) ) ;
#51983 = DIRECTION ( 'NONE',  ( -0.000000000000000000, 1.000000000000000000, -0.000000000000000000 ) ) ;
#51984 = ORIENTED_EDGE ( 'NONE', *, *, #54679, .F. ) ;
#51985 = VECTOR ( 'NONE', #18913, 1000.000000000000000 ) ;
#51986 = CARTESIAN_POINT ( 'NONE',  ( 4.458734124999998549, -84.72916666530106511, -2.574251347313721627 ) ) ;
#51987 = CARTESIAN_POINT ( 'NONE',  ( 4.458734124999998549, 25.27083333469892779, -2.574251347313721627 ) ) ;
#51988 = DIRECTION ( 'NONE',  ( -0.000000000000000000, 1.000000000000000000, -0.000000000000000000 ) ) ;
#51989 = ORIENTED_EDGE ( 'NONE', *, *, #43588, .T. ) ;
#51990 = CARTESIAN_POINT ( 'NONE',  ( -2.500000000000000444, -60.04166666393547303, -4.330127018922193649 ) ) ;
#51991 = CARTESIAN_POINT ( 'NONE',  ( -57.19623071787016499, -137.6250000013655779, 4.297418129356382899 ) ) ;
#51992 = CARTESIAN_POINT ( 'NONE',  ( -4.458734124999999437, -79.56249999863440792, 0.000000000000000000 ) ) ;
#51993 = CARTESIAN_POINT ( 'NONE',  ( -52.53715891517739323, -129.5625000027312410, -4.819101127000233298 ) ) ;
#51994 = CYLINDRICAL_SURFACE ( 'NONE', #44945, 5.000000000000000000 ) ;
#51995 = FACE_OUTER_BOUND ( 'NONE', #14613, .T. ) ;
#51996 = CARTESIAN_POINT ( 'NONE',  ( -6.031010364368858512E-14, 4.249999999999995559, 5.000000000000000000 ) ) ;
#51997 = CARTESIAN_POINT ( 'NONE',  ( -4.458734124999999437, -54.39583333196773651, -2.574251347313719407 ) ) ;
#51998 = APPLICATION_CONTEXT ( 'automotive_design' ) ;
#51999 = CARTESIAN_POINT ( 'NONE',  ( -57.46284108482265651, -151.0625000027312126, 4.819101127000238627 ) ) ;
#52000 = CARTESIAN_POINT ( 'NONE',  ( 2.229367062500001939, 21.02083333469892779, 3.861377020970579999 ) ) ;
#52001 =( BOUNDED_CURVE ( )  B_SPLINE_CURVE ( 2, ( #57914, #13835, #33455, #53072, #12890, #22877, #48240, #24124, #4197 ),
 .UNSPECIFIED., .F., .F. ) 
 B_SPLINE_CURVE_WITH_KNOTS ( ( 3, 2, 2, 2, 3 ),
 ( 0.1937500000000000056, 0.1944444444444444475, 0.1958333333333333315, 0.1972222222222222154, 0.1979166666666666574 ),
 .UNSPECIFIED. ) 
 CURVE ( )  GEOMETRIC_REPRESENTATION_ITEM ( )  RATIONAL_B_SPLINE_CURVE ( ( 0.9330127018922194093, 0.9330127018922194093, 1.000000000000000000, 0.8660254037844387076, 1.000000000000000000, 0.8660254037844387076, 1.000000000000000000, 0.9330127018922194093, 0.9330127018922194093 ) ) 
 REPRESENTATION_ITEM ( '' )  );
#52002 = CARTESIAN_POINT ( 'NONE',  ( -4.999999999999999112, -105.9166666666666714, 2.886751345948131764 ) ) ;
#52003 = CARTESIAN_POINT ( 'NONE',  ( -9.184850993605147944E-16, -154.3750000027311842, 5.000000000000000000 ) ) ;
#52004 = EDGE_CURVE ( 'NONE', #21047, #23493, #48067, .T. ) ;
#52005 = CARTESIAN_POINT ( 'NONE',  ( 4.458734124999999437, -45.06249999863440081, -5.460374474430324690E-16 ) ) ;
#52006 = CARTESIAN_POINT ( 'NONE',  ( 2.499999999999998668, 0.7916666693978530178, -4.330127018922193649 ) ) ;
#52007 = CYLINDRICAL_SURFACE ( 'NONE', #57143, 5.000000000000000000 ) ;
#52008 = CARTESIAN_POINT ( 'NONE',  ( -57.89159099828107458, -125.6875000013656063, -3.393966926194107447 ) ) ;
#52009 = CARTESIAN_POINT ( 'NONE',  ( 9.457646018065525792E-16, -81.31249999863440792, 5.148502694627439702 ) ) ;
#52010 = CARTESIAN_POINT ( 'NONE',  ( 2.229367062499998831, -102.6458333319677365, -3.861377020970580887 ) ) ;
#52011 = CARTESIAN_POINT ( 'NONE',  ( 4.458734124999998549, -5.979166665301071326, -2.574251347313721627 ) ) ;
#52012 = ORIENTED_EDGE ( 'NONE', *, *, #36761, .T. ) ;
#52013 = LINE ( 'NONE', #61673, #37155 ) ;
#52014 = CARTESIAN_POINT ( 'NONE',  ( 2.229367062499998831, -90.64583333196773651, -3.861377020970580887 ) ) ;
#52015 = CARTESIAN_POINT ( 'NONE',  ( 5.000000000000000888, -164.0625000027312126, -2.071067811865475505 ) ) ;
#52016 = CARTESIAN_POINT ( 'NONE',  ( 4.458734124999998549, -85.97916666530107932, -2.574251347313721627 ) ) ;
#52017 = CARTESIAN_POINT ( 'NONE',  ( -4.458734124999999437, 10.35416666803225993, -2.574251347313719407 ) ) ;
#52018 = CARTESIAN_POINT ( 'NONE',  ( 5.000000000000000888, -2.458333330602146205, 2.886751345948126879 ) ) ;
#52019 = CARTESIAN_POINT ( 'NONE',  ( -57.19623071787017210, -135.3750000013656063, 4.297418129356382899 ) ) ;
#52020 =( BOUNDED_CURVE ( )  B_SPLINE_CURVE ( 2, ( #24814, #58283, #13590, #9378, #57664, #14202, #38958, #33828, #28989 ),
 .UNSPECIFIED., .F., .F. ) 
 B_SPLINE_CURVE_WITH_KNOTS ( ( 3, 2, 2, 2, 3 ),
 ( 0.2583333333333335813, 0.2625000000000002331, 0.2666666666666668850, 0.2708333333333335369, 0.2750000000000002442 ),
 .UNSPECIFIED. ) 
 CURVE ( )  GEOMETRIC_REPRESENTATION_ITEM ( )  RATIONAL_B_SPLINE_CURVE ( ( 0.9999999999999958922, 0.9238795325112908463, 1.000000000000000000, 0.9238795325112867385, 1.000000000000000000, 0.9238795325112867385, 1.000000000000000000, 0.9238795325112826307, 1.000000000000003997 ) ) 
 REPRESENTATION_ITEM ( '' )  );
#52021 = CARTESIAN_POINT ( 'NONE',  ( -4.458734124999997661, -10.22916666530106866, 2.574251347313722516 ) ) ;
#52022 = CARTESIAN_POINT ( 'NONE',  ( 4.458734124999999437, 17.93750000136559208, -5.460374474430324690E-16 ) ) ;
#52023 = CARTESIAN_POINT ( 'NONE',  ( -3.152548672688508926E-16, -54.81249999863440081, -5.148502694627439702 ) ) ;
#52024 = CARTESIAN_POINT ( 'NONE',  ( -2.071067811865404451, -163.3125000000000284, 5.000000000000073719 ) ) ;
#52025 = CARTESIAN_POINT ( 'NONE',  ( -4.999999999999998224, -105.9166666666666572, 2.886751345948131764 ) ) ;
#52026 = CARTESIAN_POINT ( 'NONE',  ( -4.458734124999999437, -10.39583333196773474, -2.574251347313719407 ) ) ;
#52027 = DIRECTION ( 'NONE',  ( 0.000000000000000000, 0.000000000000000000, 1.000000000000000000 ) ) ;
#52028 = ADVANCED_FACE ( 'NONE', ( #43235 ), #23325, .T. ) ;
#52029 = VERTEX_POINT ( 'NONE', #18789 ) ;
#52030 = CARTESIAN_POINT ( 'NONE',  ( -3.152548672688508926E-16, -35.81249999863440792, -5.148502694627439702 ) ) ;
#52031 = CARTESIAN_POINT ( 'NONE',  ( -50.70258187064364108, -128.3750000013656631, 2.196230717870141014 ) ) ;
#52032 = ADVANCED_FACE ( 'NONE', ( #38115 ), #13664, .T. ) ;
#52033 = FACE_OUTER_BOUND ( 'NONE', #56710, .T. ) ;
#52034 = CARTESIAN_POINT ( 'NONE',  ( 4.458734124999998549, -78.72916666530106511, -2.574251347313721627 ) ) ;
#52035 = CARTESIAN_POINT ( 'NONE',  ( -2.229367062499996610, 26.60416666803225993, 3.861377020970582219 ) ) ;
#52036 = AXIS2_PLACEMENT_3D ( 'NONE', #55614, #45306, #44991 ) ;
#52037 = AXIS2_PLACEMENT_3D ( 'NONE', #49542, #5483, #39882 ) ;
#52038 = CARTESIAN_POINT ( 'NONE',  ( -3.152801135295367096, -151.3125000013655779, -3.152801135295367541 ) ) ;
#52039 = CARTESIAN_POINT ( 'NONE',  ( -4.458734124999999437, 15.60416666803225993, -2.574251347313719407 ) ) ;
#52040 = EDGE_CURVE ( 'NONE', #50678, #52441, #19657, .T. ) ;
#52041 = CARTESIAN_POINT ( 'NONE',  ( 1.975475456537005874E-15, -81.62499999726881583, 5.000000000000000000 ) ) ;
#52042 = CARTESIAN_POINT ( 'NONE',  ( -1.339745962155610925, -64.66965819600733312, 5.000000000000000000 ) ) ;
#52043 = CARTESIAN_POINT ( 'NONE',  ( 4.458734124999999437, -86.06249999863439371, -5.460374474430324690E-16 ) ) ;
#52044 = CARTESIAN_POINT ( 'NONE',  ( -5.000000000000000000, -63.00000000000000000, 0.000000000000000000 ) ) ;
#52045 = CARTESIAN_POINT ( 'NONE',  ( 2.500000000000002220, -63.54166666393547303, 4.330127018922192761 ) ) ;
#52046 = CARTESIAN_POINT ( 'NONE',  ( 1.060575238724906964E-15, 18.37500000273118772, 5.773502691896257311 ) ) ;
#52047 = ORIENTED_EDGE ( 'NONE', *, *, #13101, .T. ) ;
#52048 = CARTESIAN_POINT ( 'NONE',  ( -6.972266317189433020E-16, -79.24999999999998579, -5.000000000000000000 ) ) ;
#52049 = DIRECTION ( 'NONE',  ( -0.000000000000000000, 1.000000000000000000, -0.000000000000000000 ) ) ;
#52051 = CARTESIAN_POINT ( 'NONE',  ( 2.500000000000002220, -29.66666666666666785, 4.330127018922192761 ) ) ;
#52050 = CARTESIAN_POINT ( 'NONE',  ( 2.499999999999998668, -52.33333333333332860, -4.330127018922193649 ) ) ;
#52052 = CARTESIAN_POINT ( 'NONE',  ( -2.229367062499996610, -35.14583333196772941, 3.861377020970582219 ) ) ;
#52053 = CARTESIAN_POINT ( 'NONE',  ( 1.339745962155612702, 0.7053418012614794952, -5.000000000000000000 ) ) ;
#52054 = CARTESIAN_POINT ( 'NONE',  ( 5.000000000000000000, -27.29166666393547658, -2.886751345948129988 ) ) ;
#52056 = ORIENTED_EDGE ( 'NONE', *, *, #60053, .T. ) ;
#52055 = CARTESIAN_POINT ( 'NONE',  ( -2.229367062500000163, -59.47916666530106511, -3.861377020970580443 ) ) ;
#52057 = CARTESIAN_POINT ( 'NONE',  ( -6.972266317189433020E-16, -28.25000000000000000, -5.000000000000000000 ) ) ;
#52059 = ORIENTED_EDGE ( 'NONE', *, *, #2093, .T. ) ;
#52058 = CARTESIAN_POINT ( 'NONE',  ( 2.229367062500001939, -9.229166665301075767, 3.861377020970579999 ) ) ;
#52060 = CARTESIAN_POINT ( 'NONE',  ( -3.535250795749689387E-16, -69.24999999999998579, -5.773502691896257311 ) ) ;
#52061 = CARTESIAN_POINT ( 'NONE',  ( -54.64476657466781973, -139.8125000013656063, -4.444560631937228834 ) ) ;
#52062 = CARTESIAN_POINT ( 'NONE',  ( 9.457646018065525792E-16, -52.31249999863440792, 5.148502694627439702 ) ) ;
#52063 = CARTESIAN_POINT ( 'NONE',  ( -2.500000000000000444, -76.04166666393547303, -4.330127018922193649 ) ) ;
#52065 = ORIENTED_EDGE ( 'NONE', *, *, #14545, .F. ) ;
#52064 = CARTESIAN_POINT ( 'NONE',  ( 3.061616997868383141E-16, -150.8750000027312126, -5.000000000000000000 ) ) ;
#52066 = CARTESIAN_POINT ( 'NONE',  ( -59.81910112700025905, -148.1875000000000284, -2.462841084822630311 ) ) ;
#52067 = CARTESIAN_POINT ( 'NONE',  ( -4.458734124999998549, -24.47916666530107577, 2.574251347313722516 ) ) ;
#52068 = CARTESIAN_POINT ( 'NONE',  ( 4.458734124999998549, -58.97916666530105800, -2.574251347313721627 ) ) ;
#52069 = CYLINDRICAL_SURFACE ( 'NONE', #42642, 5.000000000000000000 ) ;
#52070 = CARTESIAN_POINT ( 'NONE',  ( -1.846868145590737420, -141.7500000013655779, 4.458734124999999437 ) ) ;
#52071 = CARTESIAN_POINT ( 'NONE',  ( -4.458734124999999437, -100.6458333319677223, -2.574251347313719407 ) ) ;
#52072 = CARTESIAN_POINT ( 'NONE',  ( 1.975475456537005874E-15, -52.62499999726880873, 5.000000000000000000 ) ) ;
#52073 = ORIENTED_EDGE ( 'NONE', *, *, #48087, .T. ) ;
#52074 = CARTESIAN_POINT ( 'NONE',  ( -59.29741812935640155, -148.8750000013656063, -2.196230717870135685 ) ) ;
#52075 = CARTESIAN_POINT ( 'NONE',  ( -57.46284108482265651, -141.0625000027312410, 4.819101127000239515 ) ) ;
#52076 =( BOUNDED_CURVE ( )  B_SPLINE_CURVE ( 2, ( #2073, #51580, #12006, #36148, #61554, #21990, #37108, #32262, #12338 ),
 .UNSPECIFIED., .F., .F. ) 
 B_SPLINE_CURVE_WITH_KNOTS ( ( 3, 2, 2, 2, 3 ),
 ( 0.9017857142857143016, 0.9023809523809523947, 0.9035714285714285809, 0.9047619047619047672, 0.9053571428571428603 ),
 .UNSPECIFIED. ) 
 CURVE ( )  GEOMETRIC_REPRESENTATION_ITEM ( )  RATIONAL_B_SPLINE_CURVE ( ( 0.9330127018922194093, 0.9330127018922194093, 1.000000000000000000, 0.8660254037844387076, 1.000000000000000000, 0.8660254037844387076, 1.000000000000000000, 0.9330127018922194093, 0.9330127018922194093 ) ) 
 REPRESENTATION_ITEM ( '' )  );
#52077 = VECTOR ( 'NONE', #21458, 1000.000000000000000 ) ;
#52078 = CARTESIAN_POINT ( 'NONE',  ( 5.000000000000001776, 6.123233995736768255E-16, -9.974600000000000577 ) ) ;
#52079 = CIRCLE ( 'NONE', #17134, 0.7733184030943203169 ) ;
#52080 = CARTESIAN_POINT ( 'NONE',  ( 4.458734124999999437, -5.812499998634403475, -5.460374474430324690E-16 ) ) ;
#52081 = CARTESIAN_POINT ( 'NONE',  ( 4.458734124999998549, -94.97916666530106511, -2.574251347313721627 ) ) ;
#52082 = CARTESIAN_POINT ( 'NONE',  ( -3.152801135295367096, -147.3125000013655779, -3.152801135295367541 ) ) ;
#52083 = CARTESIAN_POINT ( 'NONE',  ( 4.458734125000001214, -22.14583333196773296, 2.574251347313718519 ) ) ;
#52084 = CARTESIAN_POINT ( 'NONE',  ( -7.500000000000000888, 3.988838049906426875, -0.8529248949437632232 ) ) ;
#52085 = CARTESIAN_POINT ( 'NONE',  ( -53.51423613279429503, -138.2500000013656063, 4.591703134518082763 ) ) ;
#52086 = CARTESIAN_POINT ( 'NONE',  ( -2.229367062500000163, -64.72916666530106511, -3.861377020970580443 ) ) ;
#52087 = CARTESIAN_POINT ( 'NONE',  ( -6.972266317189433020E-16, -62.24999999999999289, -5.000000000000000000 ) ) ;
#52088 = CARTESIAN_POINT ( 'NONE',  ( -6.972266317189433020E-16, 1.750000000000000444, -5.000000000000000000 ) ) ;
#52089 = CARTESIAN_POINT ( 'NONE',  ( 4.458734124999999437, -144.3750000013656063, -1.846868145590734978 ) ) ;
#52090 = CARTESIAN_POINT ( 'NONE',  ( -4.458734124999999437, 9.354166668032261711, -2.574251347313719407 ) ) ;
#52091 = VERTEX_POINT ( 'NONE', #58591 ) ;
#52092 = CARTESIAN_POINT ( 'NONE',  ( -5.000000000000000000, -164.6250000027311842, -6.123233995736766282E-16 ) ) ;
#52093 = CARTESIAN_POINT ( 'NONE',  ( 5.000000000000000000, 16.50000000000000000, -6.123233995736766282E-16 ) ) ;
#52095 = CARTESIAN_POINT ( 'NONE',  ( -4.458734124999999437, -24.31249999863440436, 0.000000000000000000 ) ) ;
#52094 = CARTESIAN_POINT ( 'NONE',  ( -2.499999999999996447, -90.83333333333332860, 4.330127018922195425 ) ) ;
#52096 = CARTESIAN_POINT ( 'NONE',  ( 1.339745962155612702, -73.29465819873851729, -5.000000000000000000 ) ) ;
#52097 = CARTESIAN_POINT ( 'NONE',  ( -4.458734124999998549, -71.47916666530107932, 2.574251347313722516 ) ) ;
#52098 = CYLINDRICAL_SURFACE ( 'NONE', #26314, 5.000000000000000000 ) ;
#52099 = CARTESIAN_POINT ( 'NONE',  ( -52.10840900171896806, -146.1875000013656063, 3.393966926194110556 ) ) ;
#52100 = CARTESIAN_POINT ( 'NONE',  ( 4.458734124999998549, 2.270833334698928230, -2.574251347313721627 ) ) ;
#52101 = CARTESIAN_POINT ( 'NONE',  ( 1.339745962155615144, -56.58034179853028434, 4.999999999999999112 ) ) ;
#52102 = CARTESIAN_POINT ( 'NONE',  ( 5.000000000000000888, 21.41666666666666430, 2.886751345948126879 ) ) ;
#52103 = CARTESIAN_POINT ( 'NONE',  ( -3.152548672688508926E-16, 8.437500001365595637, -5.148502694627439702 ) ) ;
#52104 = CARTESIAN_POINT ( 'NONE',  ( 2.229367062500001939, -70.97916666530107932, 3.861377020970579999 ) ) ;
#52105 = CARTESIAN_POINT ( 'NONE',  ( -2.229367062499996610, -21.39583333196774007, 3.861377020970582219 ) ) ;
#52106 = CARTESIAN_POINT ( 'NONE',  ( 5.000000000000000000, 1.500000000000001332, -6.123233995736766282E-16 ) ) ;
#52107 = CARTESIAN_POINT ( 'NONE',  ( 4.458734125000000326, -158.3750000013655779, -1.846868145590734978 ) ) ;
#52108 = CARTESIAN_POINT ( 'NONE',  ( 75.00000000000002842, 0.000000000000000000, 5.000000000000000000 ) ) ;
#52109 = CARTESIAN_POINT ( 'NONE',  ( 9.457646018065525792E-16, -62.06249999863440792, 5.148502694627439702 ) ) ;
#52110 = CARTESIAN_POINT ( 'NONE',  ( -2.499999999999996447, -102.7083333306021444, 4.330127018922195425 ) ) ;
#52111 = CARTESIAN_POINT ( 'NONE',  ( 6.042630808230842148E-15, 26.75000000000000000, -4.999999999999999112 ) ) ;
#52112 = CARTESIAN_POINT ( 'NONE',  ( 9.457646018065525792E-16, -39.06249999863440081, 5.148502694627439702 ) ) ;
#52113 = CARTESIAN_POINT ( 'NONE',  ( -4.458734124999997661, -106.4791666653010793, 2.574251347313722516 ) ) ;
#52114 = CARTESIAN_POINT ( 'NONE',  ( 4.458734124999999437, -70.06249999863439371, -5.460374474430324690E-16 ) ) ;
#52115 = CARTESIAN_POINT ( 'NONE',  ( -5.000000000000000000, -51.08333333333332860, -2.886751345948128211 ) ) ;
#52116 = CARTESIAN_POINT ( 'NONE',  ( -2.499999999999996447, -40.83333333333333570, 4.330127018922195425 ) ) ;
#52117 = CARTESIAN_POINT ( 'NONE',  ( -6.000000000000000000, -114.9999999999999858, 1.499999999999999556 ) ) ;
#52118 = ORIENTED_EDGE ( 'NONE', *, *, #42476, .T. ) ;
#52119 = CARTESIAN_POINT ( 'NONE',  ( 9.457646018065525792E-16, -110.0624999986343795, 5.148502694627439702 ) ) ;
#52120 = CONICAL_SURFACE ( 'NONE', #13084, 5.000000000000001776, 0.9599310885968795892 ) ;
#52121 = CARTESIAN_POINT ( 'NONE',  ( -4.999999999999998224, -99.79166666393545881, 2.886751345948131764 ) ) ;
#52122 = CARTESIAN_POINT ( 'NONE',  ( -2.499999999999996447, -14.83333333333333037, 4.330127018922195425 ) ) ;
#52123 = CARTESIAN_POINT ( 'NONE',  ( -4.458734124999998549, -15.22916666530107754, 2.574251347313722516 ) ) ;
#52124 = VECTOR ( 'NONE', #7108, 1000.000000000000000 ) ;
#52125 = CARTESIAN_POINT ( 'NONE',  ( -2.229367062500000163, -78.47916666530106511, -3.861377020970580443 ) ) ;
#52126 =( GEOMETRIC_REPRESENTATION_CONTEXT ( 3 ) GLOBAL_UNCERTAINTY_ASSIGNED_CONTEXT ( ( #8591 ) ) GLOBAL_UNIT_ASSIGNED_CONTEXT ( ( #9273, #58487, #19557 ) ) REPRESENTATION_CONTEXT ( 'NONE', 'WORKASPACE' ) );
#52127 = CARTESIAN_POINT ( 'NONE',  ( 1.975475456537005874E-15, -72.62499999726878741, 5.000000000000000000 ) ) ;
#52128 = CARTESIAN_POINT ( 'NONE',  ( 5.000000000000000888, -14.45833333060214976, 2.886751345948126879 ) ) ;
#52130 = VERTEX_POINT ( 'NONE', #53752 ) ;
#52129 = CARTESIAN_POINT ( 'NONE',  ( 4.458734124999999437, -43.81249999863440081, -5.460374474430324690E-16 ) ) ;
#52131 = LINE ( 'NONE', #53694, #34332 ) ;
#52133 = ORIENTED_EDGE ( 'NONE', *, *, #8369, .F. ) ;
#52132 = CARTESIAN_POINT ( 'NONE',  ( -4.458734124999998549, 8.520833334698926009, 2.574251347313722516 ) ) ;
#52134 = CARTESIAN_POINT ( 'NONE',  ( 1.339745962155615144, -81.58034179853029855, 4.999999999999999112 ) ) ;
#52135 = CARTESIAN_POINT ( 'NONE',  ( -5.000000000000000000, -55.99999999999999289, 0.000000000000000000 ) ) ;
#52136 = CARTESIAN_POINT ( 'NONE',  ( 1.846868145590736310, -159.8750000013655779, 4.458734124999999437 ) ) ;
#52137 = CARTESIAN_POINT ( 'NONE',  ( 2.229367062499998831, -37.89583333196773651, -3.861377020970580887 ) ) ;
#52138 = CARTESIAN_POINT ( 'NONE',  ( -6.972266317189433020E-16, -11.12499999726881406, -5.000000000000000000 ) ) ;
#52139 = CARTESIAN_POINT ( 'NONE',  ( -4.458734124999999437, -82.31249999863440792, 0.000000000000000000 ) ) ;
#52140 = CARTESIAN_POINT ( 'NONE',  ( 5.000000000000000000, -166.0625000000000000, 2.071067811865478614 ) ) ;
#52141 = CARTESIAN_POINT ( 'NONE',  ( -1.339745962155613812, -30.20534180126148271, -5.000000000000000000 ) ) ;
#52142 = CARTESIAN_POINT ( 'NONE',  ( -56.48576386720575471, -133.0000000013656063, -4.591703134518078322 ) ) ;
#52143 = CARTESIAN_POINT ( 'NONE',  ( 4.458734124999999437, -2.062499998634406584, -5.460374474430324690E-16 ) ) ;
#52144 = CARTESIAN_POINT ( 'NONE',  ( 9.457646018065525792E-16, -43.31249999863440792, 5.148502694627439702 ) ) ;
#52145 = CARTESIAN_POINT ( 'NONE',  ( -5.000000000000000000, -24.87499999726881583, 0.000000000000000000 ) ) ;
#52146 = CARTESIAN_POINT ( 'NONE',  ( -2.229367062500000163, -84.72916666530107932, -3.861377020970580443 ) ) ;
#52147 = CARTESIAN_POINT ( 'NONE',  ( -6.972266317189433020E-16, -86.25000000000001421, -5.000000000000000000 ) ) ;
#52148 = ORIENTED_EDGE ( 'NONE', *, *, #58343, .T. ) ;
#52149 = CARTESIAN_POINT ( 'NONE',  ( -59.98410592259440222, -153.2500000027312410, -0.3983568153799752487 ) ) ;
#52150 = CARTESIAN_POINT ( 'NONE',  ( -5.000000000000000000, -18.95833333060214798, -2.886751345948128211 ) ) ;
#52151 = CARTESIAN_POINT ( 'NONE',  ( 9.457646018065525792E-16, -68.31249999863442213, 5.148502694627439702 ) ) ;
#52152 = CARTESIAN_POINT ( 'NONE',  ( 2.229367062500001939, -7.229166665301073103, 3.861377020970579999 ) ) ;
#52153 = ORIENTED_EDGE ( 'NONE', *, *, #10676, .T. ) ;
#52154 = CARTESIAN_POINT ( 'NONE',  ( -5.000000000000000000, -150.6250000027312126, -6.123233995736766282E-16 ) ) ;
#52155 = FACE_OUTER_BOUND ( 'NONE', #35632, .T. ) ;
#52156 = CARTESIAN_POINT ( 'NONE',  ( -3.152548672688508926E-16, -4.812499998634402587, -5.148502694627439702 ) ) ;
#52157 = CARTESIAN_POINT ( 'NONE',  ( -58.80597590150559739, -147.1250000027312126, 3.242614290531460330 ) ) ;
#52158 = CARTESIAN_POINT ( 'NONE',  ( -4.458734124999999437, 1.604166668032262155, -2.574251347313719407 ) ) ;
#52159 = CARTESIAN_POINT ( 'NONE',  ( -2.500000000000000444, -12.04166666393547835, -4.330127018922193649 ) ) ;
#52160 = CARTESIAN_POINT ( 'NONE',  ( 3.152801135295366208, -158.5625000013656063, 3.152801135295367985 ) ) ;
#52161 = CARTESIAN_POINT ( 'NONE',  ( 9.457646018065525792E-16, 27.68750000136559208, 5.148502694627439702 ) ) ;
#52162 = ORIENTED_EDGE ( 'NONE', *, *, #44364, .T. ) ;
#52163 = CARTESIAN_POINT ( 'NONE',  ( -4.458734124999997661, -87.22916666530107932, 2.574251347313722516 ) ) ;
#52164 = CARTESIAN_POINT ( 'NONE',  ( 9.457646018065525792E-16, -6.062499998634403475, 5.148502694627439702 ) ) ;
#52165 = CARTESIAN_POINT ( 'NONE',  ( 6.123233995736766282E-16, -120.0000000000000000, -5.000000000000000000 ) ) ;
#52166 = CARTESIAN_POINT ( 'NONE',  ( 2.499999999999998668, -48.33333333333332860, -4.330127018922193649 ) ) ;
#52167 = CARTESIAN_POINT ( 'NONE',  ( -49.85088928181150436, -138.5625000000000284, -1.666127454062680480 ) ) ;
#52168 = CARTESIAN_POINT ( 'NONE',  ( 5.000000000000000000, -34.29166666393547303, -2.886751345948129988 ) ) ;
#52169 = FACE_OUTER_BOUND ( 'NONE', #26415, .T. ) ;
#52170 = CARTESIAN_POINT ( 'NONE',  ( -2.229367062500000163, 21.52083333469892779, -3.861377020970580443 ) ) ;
#52171 = CYLINDRICAL_SURFACE ( 'NONE', #49948, 5.000000000000000000 ) ;
#52172 = CARTESIAN_POINT ( 'NONE',  ( 2.229367062499998831, 22.35416666803225993, -3.861377020970580887 ) ) ;
#52173 = CARTESIAN_POINT ( 'NONE',  ( 9.457646018065525792E-16, -58.06249999863440081, 5.148502694627439702 ) ) ;
#52174 = CARTESIAN_POINT ( 'NONE',  ( -4.458734124999999437, -1.562499998634406140, 0.000000000000000000 ) ) ;
#52175 = LINE ( 'NONE', #18068, #1118 ) ;
#52176 = CARTESIAN_POINT ( 'NONE',  ( 2.499999999999998668, 15.66666666666666607, -4.330127018922193649 ) ) ;
#52177 = CARTESIAN_POINT ( 'NONE',  ( -9.184850993605147944E-16, -142.3750000027312126, 5.000000000000000000 ) ) ;
#52178 = CARTESIAN_POINT ( 'NONE',  ( -6.972266317189433020E-16, -46.24999999999999289, -5.000000000000000000 ) ) ;
#52179 = CARTESIAN_POINT ( 'NONE',  ( -2.229367062499996610, -50.14583333196772941, 3.861377020970582219 ) ) ;
#52180 = CARTESIAN_POINT ( 'NONE',  ( -5.000000000000000000, -82.95833333060213022, -2.886751345948128211 ) ) ;
#52181 = CARTESIAN_POINT ( 'NONE',  ( -58.39396692619412477, -136.6875000013656063, 2.891590998281057701 ) ) ;
#52182 = CARTESIAN_POINT ( 'NONE',  ( 1.975475456537005874E-15, -86.75000000000001421, 5.000000000000000000 ) ) ;
#52183 = CYLINDRICAL_SURFACE ( 'NONE', #22381, 5.000000000000000000 ) ;
#52184 = CARTESIAN_POINT ( 'NONE',  ( -4.458734124999999437, -85.64583333196773651, -2.574251347313719407 ) ) ;
#52185 = CARTESIAN_POINT ( 'NONE',  ( 3.152801135295366208, -155.8125000013656063, 3.152801135295367985 ) ) ;
#52186 = CARTESIAN_POINT ( 'NONE',  ( 1.060575238724906964E-15, -31.75000000000000000, 5.773502691896257311 ) ) ;
#52187 = CARTESIAN_POINT ( 'NONE',  ( -2.499999999999996447, 24.16666666666666785, 4.330127018922195425 ) ) ;
#52188 = ORIENTED_EDGE ( 'NONE', *, *, #1539, .F. ) ;
#52189 = CARTESIAN_POINT ( 'NONE',  ( 4.458734124999998549, 16.02083333469892423, -2.574251347313721627 ) ) ;
#52190 = EDGE_LOOP ( 'NONE', ( #22724, #55657, #61251, #38916 ) ) ;
#52191 = CARTESIAN_POINT ( 'NONE',  ( 2.229367062499998831, -94.64583333196773651, -3.861377020970580887 ) ) ;
#52192 = CARTESIAN_POINT ( 'NONE',  ( 9.457646018065525792E-16, 7.687500001365596525, 5.148502694627439702 ) ) ;
#52193 = CARTESIAN_POINT ( 'NONE',  ( 5.000000000000000888, 11.54166666939785202, 2.886751345948126879 ) ) ;
#52194 = CARTESIAN_POINT ( 'NONE',  ( -2.500000000000000444, -29.04166666393548013, -4.330127018922193649 ) ) ;
#52195 = CARTESIAN_POINT ( 'NONE',  ( -4.999999999999999112, 7.083333333333333037, 2.886751345948131764 ) ) ;
#52196 = CARTESIAN_POINT ( 'NONE',  ( 2.229367062500001939, -62.97916666530106511, 3.861377020970579999 ) ) ;
#52197 =( BOUNDED_CURVE ( )  B_SPLINE_CURVE ( 2, ( #59826, #20256, #644, #44042, #53707, #4820, #45014, #30530, #19923 ),
 .UNSPECIFIED., .F., .F. ) 
 B_SPLINE_CURVE_WITH_KNOTS ( ( 3, 2, 2, 2, 3 ),
 ( 0.5750000000000005107, 0.5791666666666672736, 0.5833333333333339255, 0.5875000000000004663, 0.5916666666666671182 ),
 .UNSPECIFIED. ) 
 CURVE ( )  GEOMETRIC_REPRESENTATION_ITEM ( )  RATIONAL_B_SPLINE_CURVE ( ( 0.9999999999999898970, 0.9238795325112968415, 1.000000000000000000, 0.9238795325112867385, 1.000000000000000000, 0.9238795325112867385, 1.000000000000000000, 0.9238795325112786339, 1.000000000000008216 ) ) 
 REPRESENTATION_ITEM ( '' )  );
#52198 = DIRECTION ( 'NONE',  ( 0.000000000000000000, 0.000000000000000000, 1.000000000000000000 ) ) ;
#52199 = CARTESIAN_POINT ( 'NONE',  ( 2.499999999999998668, -80.33333333333332860, -4.330127018922193649 ) ) ;
#52200 = CARTESIAN_POINT ( 'NONE',  ( -4.458734124999999437, -30.39583333196773651, -2.574251347313719407 ) ) ;
#52201 = CARTESIAN_POINT ( 'NONE',  ( 6.158835246850666199E-14, -3.124999997268815388, -4.999999999999999112 ) ) ;
#52202 = DIRECTION ( 'NONE',  ( -0.000000000000000000, 1.000000000000000000, -0.000000000000000000 ) ) ;
#52203 = CARTESIAN_POINT ( 'NONE',  ( -58.24261429053147765, -138.3750000027312126, -3.805975901505573855 ) ) ;
#52204 = CARTESIAN_POINT ( 'NONE',  ( -2.500000000000000444, -38.16666666666667140, -4.330127018922193649 ) ) ;
#52205 = CARTESIAN_POINT ( 'NONE',  ( 6.123233995736766282E-16, -170.0000000000000000, -5.000000000000000000 ) ) ;
#52207 = CARTESIAN_POINT ( 'NONE',  ( 9.457646018065525792E-16, -22.31249999863440792, 5.148502694627439702 ) ) ;
#52206 = CARTESIAN_POINT ( 'NONE',  ( -51.75738570946856498, -138.7500000000000000, 3.805975901505576964 ) ) ;
#52208 = AXIS2_PLACEMENT_3D ( 'NONE', #30137, #19542, #20187 ) ;
#52209 = CYLINDRICAL_SURFACE ( 'NONE', #21450, 5.000000000000000000 ) ;
#52210 = CARTESIAN_POINT ( 'NONE',  ( -4.458734124999999437, -67.39583333196773651, -2.574251347313719407 ) ) ;
#52211 = CARTESIAN_POINT ( 'NONE',  ( -8.190561711645485556E-16, -147.9375000013656063, 4.458734124999999437 ) ) ;
#52213 = EDGE_CURVE ( 'NONE', #26895, #14751, #4247, .T. ) ;
#52212 = CARTESIAN_POINT ( 'NONE',  ( 4.458734124999998549, -73.72916666530106511, -2.574251347313721627 ) ) ;
#52214 = VECTOR ( 'NONE', #18639, 1000.000000000000000 ) ;
#52215 = CARTESIAN_POINT ( 'NONE',  ( -53.51423613279429503, -143.5000000013656347, 4.591703134518082763 ) ) ;
#52216 = CARTESIAN_POINT ( 'NONE',  ( 2.229367062499998831, -25.89583333196773651, -3.861377020970580887 ) ) ;
#52217 = CARTESIAN_POINT ( 'NONE',  ( 2.500000000000002220, -60.54166666393547303, 4.330127018922192761 ) ) ;
#52218 = ORIENTED_EDGE ( 'NONE', *, *, #17254, .T. ) ;
#52219 = LINE ( 'NONE', #45804, #39475 ) ;
#52220 = VERTEX_POINT ( 'NONE', #24491 ) ;
#52221 = CARTESIAN_POINT ( 'NONE',  ( 4.458734124999998549, -65.97916666530106511, -2.574251347313721627 ) ) ;
#52222 = LINE ( 'NONE', #47394, #28637 ) ;
#52223 = CYLINDRICAL_SURFACE ( 'NONE', #62592, 5.000000000000000000 ) ;
#52224 = EDGE_LOOP ( 'NONE', ( #3473, #1851, #19693, #30493 ) ) ;
#52225 = CARTESIAN_POINT ( 'NONE',  ( -49.85088928181150436, -125.5625000000000284, -1.666127454062680702 ) ) ;
#52226 = CARTESIAN_POINT ( 'NONE',  ( -1.339745962155610925, -55.66965819600732601, 5.000000000000000000 ) ) ;
#52227 = CARTESIAN_POINT ( 'NONE',  ( -4.458734124999998549, -56.47916666530107221, 2.574251347313722516 ) ) ;
#52228 = EDGE_LOOP ( 'NONE', ( #42560, #25232, #24038, #56071 ) ) ;
#52229 = AXIS2_PLACEMENT_3D ( 'NONE', #4999, #49377, #54201 ) ;
#52230 = ADVANCED_FACE ( 'NONE', ( #58278 ), #48922, .T. ) ;
#52231 = CARTESIAN_POINT ( 'NONE',  ( -4.999999999999998224, 2.208333336064519870, 2.886751345948131764 ) ) ;
#52232 = EDGE_CURVE ( 'NONE', #45099, #5936, #44096, .T. ) ;
#52233 = CARTESIAN_POINT ( 'NONE',  ( 2.229367062499998831, 8.354166668032261711, -3.861377020970580887 ) ) ;
#52234 = CARTESIAN_POINT ( 'NONE',  ( 2.229367062499998831, 20.35416666803225993, -3.861377020970580887 ) ) ;
#52235 = CARTESIAN_POINT ( 'NONE',  ( -59.59170313451811296, -148.5000000013655779, 1.485763867205729394 ) ) ;
#52236 = CARTESIAN_POINT ( 'NONE',  ( 1.339745962155602488, 20.41965820146970145, 5.000000000000007105 ) ) ;
#52237 = CARTESIAN_POINT ( 'NONE',  ( 3.061616997868383141E-16, -164.7500000000000000, -5.000000000000000000 ) ) ;
#52238 = EDGE_LOOP ( 'NONE', ( #55613, #49536, #21419, #40333 ) ) ;
#52239 = CARTESIAN_POINT ( 'NONE',  ( -4.458734124999997661, -68.22916666530106511, 2.574251347313722516 ) ) ;
#52240 = CARTESIAN_POINT ( 'NONE',  ( 1.339745962155615144, -10.58034179853029144, 4.999999999999999112 ) ) ;
#52241 = CARTESIAN_POINT ( 'NONE',  ( -2.229367062500000163, 7.520833334698929562, -3.861377020970580443 ) ) ;
#52242 = EDGE_CURVE ( 'NONE', #39123, #41613, #49251, .T. ) ;
#52243 = FACE_OUTER_BOUND ( 'NONE', #61247, .T. ) ;
#52244 = CARTESIAN_POINT ( 'NONE',  ( 4.458734124999999437, -59.06249999863440081, -5.460374474430324690E-16 ) ) ;
#52245 = CARTESIAN_POINT ( 'NONE',  ( -2.499999999999996447, -20.70833333060214798, 4.330127018922195425 ) ) ;
#52246 = CARTESIAN_POINT ( 'NONE',  ( 5.000000000000000000, 4.583333333333331261, -2.886751345948130876 ) ) ;
#52247 = CARTESIAN_POINT ( 'NONE',  ( 5.000000000000000000, -161.0000000000000000, 0.000000000000000000 ) ) ;
#52248 = FACE_OUTER_BOUND ( 'NONE', #49815, .T. ) ;
#52249 =( BOUNDED_CURVE ( )  B_SPLINE_CURVE ( 2, ( #37583, #26991, #61417, #26350, #7701, #31482, #61731, #27304, #46929 ),
 .UNSPECIFIED., .F., .F. ) 
 B_SPLINE_CURVE_WITH_KNOTS ( ( 3, 2, 2, 2, 3 ),
 ( 0.2303571428571428714, 0.2309523809523809645, 0.2321428571428571508, 0.2333333333333333370, 0.2339285714285714302 ),
 .UNSPECIFIED. ) 
 CURVE ( )  GEOMETRIC_REPRESENTATION_ITEM ( )  RATIONAL_B_SPLINE_CURVE ( ( 0.9330127018922194093, 0.9330127018922209636, 1.000000000000000000, 0.8660254037844387076, 1.000000000000000000, 0.8660254037844387076, 1.000000000000000000, 0.9330127018922194093, 0.9330127018922194093 ) ) 
 REPRESENTATION_ITEM ( '' )  );
#52250 = CARTESIAN_POINT ( 'NONE',  ( 5.000000000000000000, -65.50000000000000000, -6.123233995736766282E-16 ) ) ;
#52251 = CARTESIAN_POINT ( 'NONE',  ( 4.458734124999998549, -41.72916666530107932, -2.574251347313721627 ) ) ;
#52252 = CARTESIAN_POINT ( 'NONE',  ( -2.229367062500000163, -21.72916666530107221, -3.861377020970580443 ) ) ;
#52253 =( BOUNDED_CURVE ( )  B_SPLINE_CURVE ( 2, ( #2091, #45807, #30694, #26832, #59980, #1134, #20733, #15903, #16540 ),
 .UNSPECIFIED., .F., .F. ) 
 B_SPLINE_CURVE_WITH_KNOTS ( ( 3, 2, 2, 2, 3 ),
 ( 0.8267857142857142350, 0.8273809523809523281, 0.8285714285714286254, 0.8297619047619048116, 0.8303571428571429047 ),
 .UNSPECIFIED. ) 
 CURVE ( )  GEOMETRIC_REPRESENTATION_ITEM ( )  RATIONAL_B_SPLINE_CURVE ( ( 0.9330127018922194093, 0.9330127018922194093, 1.000000000000000000, 0.8660254037844387076, 1.000000000000000000, 0.8660254037844387076, 1.000000000000000000, 0.9330127018922194093, 0.9330127018922194093 ) ) 
 REPRESENTATION_ITEM ( '' )  );
#52254 = VERTEX_POINT ( 'NONE', #23862 ) ;
#52255 = CARTESIAN_POINT ( 'NONE',  ( -55.39835681537999790, -140.0000000027312126, 4.984105922594378235 ) ) ;
#52256 = CARTESIAN_POINT ( 'NONE',  ( 4.458734124999999437, -109.8124999986343937, -5.460374474430324690E-16 ) ) ;
#52257 = CARTESIAN_POINT ( 'NONE',  ( 5.000000000000000888, -155.0625000027312126, -2.071067811865475505 ) ) ;
#52258 = EDGE_LOOP ( 'NONE', ( #70, #35602, #55936, #42777 ) ) ;
#52259 = CARTESIAN_POINT ( 'NONE',  ( 2.229367062500001939, -108.2291666653010651, 3.861377020970579999 ) ) ;
#52260 = VECTOR ( 'NONE', #33298, 1000.000000000000000 ) ;
#52261 = CARTESIAN_POINT ( 'NONE',  ( 4.458734124999999437, -30.81249999863440436, -5.460374474430324690E-16 ) ) ;
#52262 = CARTESIAN_POINT ( 'NONE',  ( 5.000000000000000000, -67.37499999726881583, -6.123233995736766282E-16 ) ) ;
#52263 = CARTESIAN_POINT ( 'NONE',  ( -52.80376928212989185, -149.1250000013656063, -4.297418129356379346 ) ) ;
#52264 = CARTESIAN_POINT ( 'NONE',  ( 2.071067811865476394, -145.1875000000000284, 5.000000000000000000 ) ) ;
#52265 = EDGE_CURVE ( 'NONE', #24051, #37866, #53042, .T. ) ;
#52266 = CARTESIAN_POINT ( 'NONE',  ( -4.458734124999997661, -29.22916666530107221, 2.574251347313722516 ) ) ;
#52267 = CARTESIAN_POINT ( 'NONE',  ( -4.458734124999999437, -67.64583333196773651, -2.574251347313719407 ) ) ;
#52268 = CARTESIAN_POINT ( 'NONE',  ( -1.846868145590737420, -169.0000000013655779, 4.458734124999997661 ) ) ;
#52269 = CARTESIAN_POINT ( 'NONE',  ( -3.152548672688508926E-16, -24.56249999863440792, -5.148502694627439702 ) ) ;
#52270 = CARTESIAN_POINT ( 'NONE',  ( 1.339745962155615144, 14.29465819873852084, 4.999999999999999112 ) ) ;
#52271 = CARTESIAN_POINT ( 'NONE',  ( -6.972266317189433020E-16, 22.87500000273118417, -5.000000000000000000 ) ) ;
#52272 = CARTESIAN_POINT ( 'NONE',  ( 2.499999999999998668, -15.33333333333333037, -4.330127018922193649 ) ) ;
#52273 = CARTESIAN_POINT ( 'NONE',  ( 1.846868145590735200, -148.2500000013656063, -4.458734125000000326 ) ) ;
#52274 = EDGE_LOOP ( 'NONE', ( #60218, #52188, #51462, #5063 ) ) ;
#52275 = CARTESIAN_POINT ( 'NONE',  ( -2.500000000000000444, -82.16666666666667140, -4.330127018922193649 ) ) ;
#52276 = CARTESIAN_POINT ( 'NONE',  ( -4.458734124999999437, -53.56249999863439371, 0.000000000000000000 ) ) ;
#52277 = CARTESIAN_POINT ( 'NONE',  ( -5.000000000000000000, -2.958333330602146649, -2.886751345948128211 ) ) ;
#52278 = CARTESIAN_POINT ( 'NONE',  ( 2.499999999999998668, -81.20833333060213022, -4.330127018922193649 ) ) ;
#52279 = CARTESIAN_POINT ( 'NONE',  ( 1.060575238724906964E-15, 22.24999999999999645, 5.773502691896257311 ) ) ;
#52280 = CARTESIAN_POINT ( 'NONE',  ( 0.000000000000000000, -170.0000000000000000, 0.000000000000000000 ) ) ;
#52281 = CARTESIAN_POINT ( 'NONE',  ( -2.229367062500000163, -3.479166665301069994, -3.861377020970580443 ) ) ;
#52282 = CARTESIAN_POINT ( 'NONE',  ( 5.000000000000000888, -48.58333333333333570, 2.886751345948126879 ) ) ;
#52283 = CARTESIAN_POINT ( 'NONE',  ( -2.071067811865538566, -164.6875000000000284, -4.999999999999937828 ) ) ;
#52284 = CARTESIAN_POINT ( 'NONE',  ( 4.458734125000001214, 10.85416666803225993, 2.574251347313718519 ) ) ;
#52285 =( BOUNDED_CURVE ( )  B_SPLINE_CURVE ( 2, ( #55745, #36123, #15222, #11662, #45130, #54791, #10720, #30327, #44483 ),
 .UNSPECIFIED., .F., .F. ) 
 B_SPLINE_CURVE_WITH_KNOTS ( ( 3, 2, 2, 2, 3 ),
 ( 0.3803571428571428381, 0.3809523809523809312, 0.3821428571428571175, 0.3833333333333333592, 0.3839285714285714524 ),
 .UNSPECIFIED. ) 
 CURVE ( )  GEOMETRIC_REPRESENTATION_ITEM ( )  RATIONAL_B_SPLINE_CURVE ( ( 0.9330127018922194093, 0.9330127018922194093, 1.000000000000000000, 0.8660254037844387076, 1.000000000000000000, 0.8660254037844387076, 1.000000000000000000, 0.9330127018922194093, 0.9330127018922194093 ) ) 
 REPRESENTATION_ITEM ( '' )  );
#52286 = VERTEX_POINT ( 'NONE', #43777 ) ;
#52287 = CARTESIAN_POINT ( 'NONE',  ( 2.500000000000002220, -42.66666666666667140, 4.330127018922192761 ) ) ;
#52288 = VERTEX_POINT ( 'NONE', #63424 ) ;
#52289 = CARTESIAN_POINT ( 'NONE',  ( -2.500000000000000444, -71.16666666666667140, -4.330127018922193649 ) ) ;
#52290 = CARTESIAN_POINT ( 'NONE',  ( -2.229367062500000163, -47.47916666530106511, -3.861377020970580443 ) ) ;
#52291 = CARTESIAN_POINT ( 'NONE',  ( -1.846868145590737420, -159.0000000013656063, 4.458734124999999437 ) ) ;
#52292 = EDGE_CURVE ( 'NONE', #5936, #57819, #45341, .T. ) ;
#52293 = EDGE_CURVE ( 'NONE', #61334, #55226, #15300, .T. ) ;
#52294 = CARTESIAN_POINT ( 'NONE',  ( -4.999999999999999112, -46.79166666393546592, 2.886751345948131764 ) ) ;
#52295 = EDGE_CURVE ( 'NONE', #44414, #34309, #6278, .T. ) ;
#52296 = VERTEX_POINT ( 'NONE', #25771 ) ;
#52297 = CARTESIAN_POINT ( 'NONE',  ( 2.229367062500001939, -25.97916666530106866, 3.861377020970579999 ) ) ;
#52298 = ORIENTED_EDGE ( 'NONE', *, *, #7927, .F. ) ;
#52299 = LINE ( 'NONE', #23029, #23430 ) ;
#52300 = CARTESIAN_POINT ( 'NONE',  ( 1.846868145590735200, -162.2500000013656347, -4.458734125000000326 ) ) ;
#52301 = CIRCLE ( 'NONE', #51300, 4.250000000000000000 ) ;
#52302 =( BOUNDED_SURFACE ( )  B_SPLINE_SURFACE ( 1, 2, ( 
 ( #48537, #24103, #23790, #63037, #38878, #47902, #43699, #48220, #33130, #58192, #39195, #34059, #58820, #24732, #44334, #38563, #300, #19897, #3858, #23479, #43082, #62720, #18645, #8990, #4175, #1272, #31144, #50462, #10258, #45304, #59472, #20873, #35340, #40474, #20555, #40157, #15721, #34695, #25694, #5430, #44657, #15406, #15081, #20229, #6713, #25369, #16036, #59800, #50771, #54320, #16362, #54959, #26322, #45940, #6402, #6083, #60115, #35665, #11528, #50127, #619, #29859, #1903, #21510, #5751, #55290, #49806, #49492, #11209, #25047, #10889, #59149, #40790, #30832, #26011, #45628, #1583, #21183, #60437, #35983, #39829, #35030, #55612, #54642, #10566, #30176, #44989, #955, #30505, #7033, #22142, #42061, #37249, #17308, #57196, #7985, #41424, #46584, #56876, #27583, #27900, #46263, #32094, #36298, #32415, #12481, #11836, #61386, #61703, #47218, #41107, #36934, #37556, #55921, #17932, #61073, #17632, #31782, #13116, #32733, #7670, #3161, #31455, #52360, #7356, #36611, #2222, #3472, #12795, #52046, #8298, #51096, #47521, #16677, #60752, #26644, #56560, #51730, #21826, #26966, #16994, #22780, #56242, #12163, #27277, #42375, #51413, #46903, #2527, #41737, #22464, #2844, #62014, #33361, #28530, #33054, #19185, #53608, #14675, #33988, #18253, #14048, #37880, #23408, #24021, #9542, #29146, #52976, #43625, #38798, #52668, #58437, #63267, #14364, #33672, #23723, #13428, #48148, #24338, #34296, #49090, #39120, #43319, #62955, #18872, #4100, #57512, #48768, #53291, #38489, #8602, #58116, #43939, #53919, #23085, #58747, #9227, #28840, #48464, #4401, #28212, #4713, #47826, #3786, #9844, #29459, #8917, #63586, #13740, #43007, #19507, #62653, #42688, #62332, #18572, #38193, #57818, #20794, #15962, #60037, #6322, #6011, #24655, #40712, #1194, #25927, #40397, #45546, #35904, #15324, #31067, #34611, #49733, #25613, #35584, #44915, #21107, #55211, #5358, #10489, #11128, #30755, #55538, #10179, #59718, #225, #50375, #40075, #39432, #25289, #45227, #1506, #5036, #870, #60361, #19823, #16285, #24977, #11448, #59391, #44261, #59073, #35263, #14998, #54238, #29782, #34948, #541, #49415, #44584, #20152, #39749, #54567, #30102, #5678, #20473, #15647, #54884, #10814, #30426, #50053, #16914, #51015, #38036, #47994, #50691, #46509, #2765, #6960, #17233, #36531, #56163, #32021, #6634, #46188, #60994, #12085, #60678, #46821, #18415, #43164, #61627, #45862, #41657, #1828, #26570, #51658, #57668, #13594, #31708, #7595, #22387, #16601, #41988, #27203, #33213, #52831, #13899, #41348, #51342, #2148, #21429, #21753, #7281, #8765, #26892, #26242, #28373, #3946, #41032, #18723, #23569, #62803, #38347, #57973, #2454, #36219, #55843, #11759, #31378, #22065, #61309, #36858, #56487, #12409, #4256, #68, #59231, #10018, #58907, #48305, #39279, #4879, #39595, #23871, #49263, #9076, #5200, #19668, #34788, #9694, #33835, #53452, #24818, #44424, #384, #19987, #29301, #24181, #28993, #28685, #14834, #54080, #33526, #38649, #15164, #43787, #43476, #58287, #14519, #38963, #29629, #48617, #48931, #24501, #63434, #19349, #34448, #63121, #34141, #4556, #53141, #53760, #54410, #10340, #44104, #29949, #49574, #58601, #5517, #25130, #44742, #703, #20313, #39914, #59562, #19032, #14206, #9383, #51185, #6801, #30268, #1667, #15808, #21269, #55373, #40876, #40560, #60203, #35747, #54731, #45715, #25451, #1038, #35424, #35117, #40248, #26733, #45391, #36064, #16125, #7117, #10652, #36377, #11288, #46348, #2304, #26409, #26094, #60518, #16444, #31550, #6484, #59888, #56007, #30914, #21906, #41503, #46027, #55693, #11607, #31227, #15494, #50857, #55048, #60834, #49888, #6163, #50540, #10971, #5839, #30592, #1990, #11921, #25780, #45071, #21594, #41189, #20644, #50213, #16760, #1356, #20960, #52449, #56647, #18339, #3558, #62420, #57282, #8384, #61785, #51500, #47604, #17079, #31867, #27671, #23166, #37639, #22865, #12253, #3252, #32496, #42775, #7437, #13198, #36698, #32820, #47298, #37961, #37327, #61471, #17405, #27985, #57595, #13523, #33141, #56958, #51807, #12563, #56333, #42456, #18016, #61156, #2609, #52756, #7749, #27046, #22227, #42149, #2934, #8685, #32175, #12878, #52128, #27352, #46985, #62099, #46664, #17712, #22547, #41827, #8070, #28298, #47911, #3868, #23488, #37020, #4484, #29230, #54004, #58828, #38887, #58521, #28922, #34067, #14446, #53690, #48856, #15090, #34376, #57900, #4799, #43400, #24423, #19271, #44025, #24113, #43711, #63355, #18653, #9622, #53060, #28611, #63045, #62731, #4184, #54331, #9308, #63672, #19592, #34706, #38275, #39204, #14758, #59157, #9934, #23798, #24741, #5438, #33756, #29549, #18955, #13824, #38571, #49183, #307, #53374, #43090, #5121, #44344, #33443, #10265, #19905, #39520, #29869, #49499, #58202, #9000, #48227, #14129, #48545, #16371, #25703, #15416, #11536, #44666, #59481, #55301, #50781, #1593, #50471, #39838, #30841, #60124, #31153, #35038, #40799, #626, #60446, #11217, #26330, #1281, #25376, #44998, #35990, #55621, #6721, #45948, #20880, #15729, #20565, #20236, #6410, #45636, #25056, #30185, #1913, #35348, #54649, #49813, #6090, #30512, #21192, #40169, #40482, #16045, #54969, #10897, #26020, #10574, #45314, #59808, #5758, #35674, #21518, #41114, #60762, #16687, #36306, #50135, #55930, #11845, #31463, #51103, #963, #56568, #61710, #42070, #17640, #12804, #42697, #62023, #21835, #56884, #7365, #32425, #46911, #52054, #32102, #51738, #27286, #46272, #37256, #17003, #56251, #26973, #26654, #31790, #18262, #36942, #27593, #7680, #62341, #2231, #27908, #2853, #37889, #57519, #17940, #7992, #37565, #57205, #12490, #47227, #22789, #36618, #42383, #3170, #13124, #32742, #22474, #61081, #52369, #8307, #13437, #33063, #23094, #47529, #3480, #7042, #41432, #12174, #51422, #46592, #2536, #22152, #41746, #17320, #61395, #43325, #3795, #38806, #18579, #28850, #59080, #34303, #9549, #53618, #4720, #63594, #43946, #53926, #29154, #8611, #24662, #48777, #9854, #24346, #29465, #19830, #62965, #15007, #38201, #33681, #19514, #39128, #48472, #5044, #58755, #52983, #58124, #14685, #49098, #39443, #57827, #43634, #47836, #44270, #24031, #23416, #9236, #232, #52677, #28220, #4408, #43019, #62659, #13747, #8924, #33368, #18882, #28537, #48157, #19193, #4110, #23730, #38497, #14056, #53302, #63276, #58447, #14371, #33995, #6642, #44590, #41041, #10188, #31076, #26249, #30433, #50062, #50699, #876, #34955, #21115, #45872, #34620, #6017, #50383, #54573, #1201, #20482, #40081, #15967, #54246, #30110, #44921, #59725, #550, #30762, #1512, #1835, #45554, #29788, #25622, #49421, #10495, #35594, #60369, #5365, #21437, #15652, #49740, #59399, #60688, #11138, #6330, #24983, #20159, #39755, #15332, #5684, #25300, #45235, #20801, #35270, #54892, #10821, #40722, #40404, #60043, #55218, #25935, #16292, #35915, #55544, #11455, #61636, #36227, #12093, #26899, #22072, #26577, #12728, #47149, #8231, #27520, #11767, #7606, #31386, #16923, #17568, #3097, #22714, #46519, #37187, #32352, #46196, #51974, #56811, #7915, #27211, #17241, #6967, #41667, #17872, #27834, #42627, #32665, #36865, #56495, #12416, #61317, #51025, #42311, #21763, #2156, #47456, #23024, #2461, #46828, #7289, #41356, #2775, #61000, #32029, #16608, #61951, #37491, #57132, #13048, #52294, #3408, #55853, #36539, #56172, #31716, #51350, #51664, #22395, #41995, #29385, #8849, #24588, #28150, #43247, #63202, #58370, #38424, #14610, #29076, #62583, #4034, #14297, #48703, #49020, #3720, #53228, #57441, #53542, #33609, #32985, #18801, #19113, #4643, #62266, #58050, #58681, #13363, #39053, #18506, #38731, #52912, #34223, #53850, #28776, #28465, #18191, #9467, #33917, #52604, #4966, #24264, #43869, #9779, #63516, #57751, #19440, #37813, #8538, #47765, #23340, #62888, #42942, #38127, #13675, #33294, #48393, #48079, #23653, #23953, #13980, #4335, #9160, #43557, #58998, #59974, #19756, #15897, #30359, #45479, #20405, #44513, #476, #35516, #55139, #11065, #30689, #40004, #34879, #39682, #39367, #5935, #1127, #44194, #49346, #25864, #54501, #14926, #5291, #25224, #49667, #40332, #59321, #59651, #35202, #10425, #30038, #49981, #34533, #44835, #15254, #160, #799, #50306, #25541, #15583, #45159, #54818, #5610, #20728, #6255, #1443, #10749, #21046, #40652, #60292, #16218, #35841, #55465, #11381, #31002, #54168, #50630, #20077, #6567, #10108, #29714, #24909, #7212, #46443, #1761, #56423, #36158, #11695, #46120, #45802, #50950, #37423, #56095, #46754, #26826, #61882, #21364, #47077, #2389, #57057, #17798, #37118, #36792, #12346, #31957, #42241, #17166, #6891, #7841, #52217, #16848, #21999, #26506, #60615, #2085, #41594, #3025, #27443, #22318, #17496, #61244, #16535, #12657, #40969, #55780, #51591, #51900, #2699, #7527, #31315, #27138, #41920, #32273, #21689, #61562, #41280, #56736, #22641, #12967, #32592, #60928, #36469, #26183, #12015, #31645, #51280, #48009, #62513, #3649, #47389, #33540, #28701, #8162, #13289, #53467, #18430, #3340, #32914, #52845, #13609, #4270, #23262, #23582, #62820, #38051, #57683, #57987, #22956, #8779, #42867, #27762, #28389, #23888, #13913, #3962, #53155, #43178, #33227, #9093, #19047, #43490, #18737, #38361, #48320, #63135, #38663, #58302, #14222, #43802, #33849, #42552, #9397, #8471, #29007, #48633, #4572, #24197, #63449, #19367, #62193, #38978, #18112, #57368, #28079, #37735, #52537, #58616, #14536, #34155, #47696, #26665, #9711, #11858, #54427, #2242, #46284, #1925, #720, #39932, #59578, #7052, #44758, #34464, #36318, #17014, #44441, #34805, #54094, #24518, #10033, #10356, #31474, #401, #53777, #21530, #11548, #44119, #21846, #31165, #50797, #41442, #45961, #49279, #51115, #60774, #20003, #29315, #19685, #29965, #55633, #6733, #49590, #61091, #41126, #29646, #59249, #26342, #16699, #48946, #58922, #20330, #4894, #55943, #25147, #83, #5533, #39295, #14851, #5216, #15511, #24834, #39612, #15180, #35132, #57214, #27295, #8621, #13450, #3180, #62350, #31800, #52686, #2865, #32111, #61406, #62668, #13134, #52381, #28230, #46602, #43028, #12186, #33073, #47845, #32434, #52063, #3803, #22484, #36951, #23103, #23426, #36630, #8002, #8318, #56578, #22799, #42079, #61721, #17950, #56262, #51747, #46920, #17650, #2546, #32753, #3489, #51433, #47539, #7376, #27605, #26983, #12499, #37574, #42707, #18272, #37266, #27917, #37898, #22161, #57528, #41757, #17329, #47237, #56893, #7689, #12813, #42392, #62033, #44599, #34631, #19203, #38817, #58458, #63286, #33378, #24673, #23740, #52993, #29798, #24992, #28859, #9559, #9245, #8933, #4732, #48166, #14381, #18588, #243, #39138, #19524, #34313, #29476, #9866, #19840, #58765, #38214, #54257, #14695, #39455, #53936, #59090, #49430, #57837, #14065, #48482, #24043, #28547, #49109, #5054, #10197, #44280, #13756, #29165, #4119, #18892, #15016, #5374, #43334, #4418, #62977, #38506, #58134, #33692, #53311, #43645, #48789, #34005, #53628, #24356, #43957, #63604, #21446, #31083, #30441, #50068, #6024, #25628, #15342, #40728, #49748, #59411, #26255, #1841, #15660, #20807, #59733, #34966, #15973, #54581, #45242, #559, #35921, #30768, #50389, #25945, #21121, #45560, #55550, #6337, #39764, #6649, #1518, #11461, #60375, #50706, #20168, #1210, #10503, #20492, #60049, #16299, #45878, #55224, #30118, #5693, #40410, #35600, #25308, #44929, #885, #11146, #40091, #10827, #35277, #54899, #28752, #14587, #58980, #44493, #58033, #34207, #54481, #9143, #34860, #14280, #14908, #48683, #30020, #10408, #24570, #20059, #54147, #44175 ),
 ( #10086, #49328, #58664, #48377, #455, #13963, #4319, #142, #39663, #34516, #19736, #23939, #39350, #29367, #59300, #29697, #43540, #5271, #24892, #15232, #49648, #53831, #58352, #33899, #5585, #25202, #44816, #778, #9760, #4623, #53522, #33590, #20385, #53209, #63184, #19095, #38713, #24248, #9450, #29059, #39037, #63498, #43852, #19423, #49000, #4947, #50285, #6232, #26159, #15563, #40630, #11041, #39985, #21023, #36131, #45778, #60273, #1737, #16191, #1424, #21340, #50925, #55753, #35818, #55442, #25842, #30980, #11357, #50604, #40940, #11992, #31289, #54801, #60590, #40317, #16510, #6545, #11670, #6866, #26481, #46095, #35183, #2055, #49962, #25521, #59955, #59630, #1103, #51254, #45459, #21663, #41254, #31619, #10729, #60901, #16824, #7189, #26797, #36443, #56072, #46417, #2366, #30336, #5914, #20712, #45139, #15878, #30664, #35498, #55116, #56398, #22294, #42213, #42845, #32246, #42528, #62165, #12943, #22617, #12324, #27419, #23231, #13585, #47983, #38027, #61858, #17775, #37394, #3000, #36768, #28052, #27114, #31935, #33204, #28362, #51876, #32567, #12629, #51563, #8134, #7502, #57029, #21975, #3624, #18085, #22934, #37708, #32886, #13262, #62488, #57345, #41567, #57659, #52514, #18406, #8449, #52819, #8756, #7816, #61220, #46727, #52189, #47672, #17144, #27737, #2672, #41893, #61538, #47050, #17471, #37092, #56711, #47366, #3314, #55053, #61160, #56011, #51189, #60523, #50218, #46353, #15813, #30597, #26414, #21910, #36381, #21599, #10977, #1994, #31231, #2307, #31556, #6168, #11924, #46031, #41193, #17083, #36068, #60206, #16130, #7121, #26737, #41507, #36703, #55697, #50544, #55377, #35429, #60838, #16764, #59893, #1361, #56337, #6488, #25785, #20965, #40880, #1671, #12257, #11292, #11611, #50861, #26098, #45719, #31871, #45396, #16449, #30918, #40565, #6805, #51504, #7442, #27050, #46668, #2613, #21273, #22231, #35752, #57599, #37643, #57286, #27675, #32824, #42460, #22868, #56651, #47915, #46989, #12567, #53064, #48231, #52132, #52453, #32500, #32180, #27989, #7753, #18021, #4188, #23492, #62425, #42780, #13526, #52760, #33145, #43094, #18343, #61475, #13828, #37965, #62735, #8689, #18657, #9004, #8074, #41832, #27356, #62103, #28302, #3873, #13202, #57904, #38279, #42153, #47302, #33447, #28616, #17409, #37024, #51811, #8387, #2938, #47608, #22551, #3562, #61789, #17716, #37330, #23170, #56963, #12882, #3256, #43715, #44349, #14450, #59486, #631, #54009, #29874, #63049, #15421, #20241, #19276, #48549, #49818, #312, #39524, #35043, #33760, #30190, #18959, #39843, #54655, #19597, #39209, #10578, #53695, #24116, #10270, #23802, #43404, #58833, #59162, #63360, #9939, #9627, #29235, #5126, #38575, #38891, #34072, #48860, #53379, #19910, #54336, #58206, #34711, #14133, #14763, #9312, #58526, #24745, #49504, #5443, #4804, #15094, #25061, #28926, #44671, #4488, #24428, #34381, #44030, #36964, #29554, #49188, #61085, #31794, #21840, #6416, #26025, #41436, #35678, #6095, #55935, #2236, #5763, #1599, #21523, #25708, #35995, #55306, #11222, #50787, #25381, #1287, #16050, #30845, #15735, #1918, #36311, #17007, #16692, #968, #60451, #20570, #45319, #6726, #11850, #31468, #50476, #26336, #41119, #35352, #60767, #45953, #51109, #16376, #45641, #59813, #21197, #7046, #36623, #45002, #56255, #40803, #55626, #11541, #31158, #40176, #26659, #10902, #54973, #12180, #30517, #46277, #50140, #60129, #20885, #40488, #17324, #27598, #57832, #33068, #8312, #52374, #3484, #62345, #42701, #52681, #27912, #7369, #23420, #47534, #8616, #23098, #28224, #18583, #61715, #13751, #36946, #32429, #18266, #37893, #47232, #3799, #57522, #51742, #56888, #13442, #47840, #38206, #51426, #43023, #52058, #62663, #22794, #22156, #7996, #26977, #46596, #2540, #3174, #41750, #61400, #56572, #7684, #12494, #42074, #32106, #27290, #17944, #46915, #2857, #22479, #17644, #37260, #12808, #42387, #62027, #37569, #57209, #13128, #32746, #8928, #29792, #24987, #29159, #48783, #48161, #10192, #53306, #53931, #24037, #5369, #49425, #63599, #39448, #28541, #44594, #554, #28854, #58129, #59404, #9860, #49103, #20163, #43329, #39759, #4114, #33373, #52987, #4726, #24351, #23734, #63281, #33685, #19835, #62970, #18887, #43951, #5049, #9240, #19519, #19198, #38811, #14690, #38501, #48476, #43640, #58453, #14060, #29471, #237, #4413, #44275, #14376, #39133, #34000, #53623, #34308, #59085, #15011, #9554, #24667, #34625, #58760, #54251, #36791, #56422, #7211, #16847, #5687, #21688, #17495, #7840, #42239, #32272, #36468, #56094, #12014, #60927, #30113, #22317, #20486, #49743, #27442, #22640, #26505, #26825, #6890, #25303, #2388, #44924, #31644, #15337, #61561, #12345, #17165, #31956, #27137, #7526, #37117, #51590, #34959, #51899, #46752, #56735, #2698, #12656, #47076, #46119, #54576, #879, #51278, #41919, #3024, #46442, #10498, #40085, #16534, #41279, #59728, #36157, #55778, #11694, #31314, #21998, #50949, #41593, #2084, #61243, #62819, #48319, #61881, #18429, #58301, #13912, #9092, #53154, #63134, #18736, #17797, #33848, #57986, #19046, #33539, #38662, #29006, #8470, #24195, #27761, #42866, #38360, #28699, #38050, #14221, #4269, #62192, #3648, #23887, #43489, #48632, #4571, #53466, #62512, #9396, #33225, #32591, #57682, #37422, #57056, #12966, #13608, #52216, #8161, #47388, #18111, #3339, #52536, #22955, #42551, #28388, #37733, #57367, #13288, #32913, #28078, #47695, #23261, #52844, #8778, #48008, #3961, #23581, #43177, #40263, #35437, #39611, #59248, #59904, #10032, #44118, #30284, #15824, #43801, #15178, #59577, #82, #10355, #29645, #49278, #25146, #63448, #39294, #54093, #5215, #53776, #39931, #10667, #55064, #54747, #38977, #34804, #58615, #19683, #44757, #49904, #5857, #24833, #719, #15510, #9710, #35131, #20329, #25465, #54426, #44440, #34154, #400, #45088, #10987, #6180, #30607, #20002, #29964, #49589, #5532, #14535, #1053, #48945, #29314, #50231, #19366, #20659, #4893, #34463, #24517, #58921, #14850, #2006, #32194, #7455, #46366, #26748, #50874, #11940, #36718, #41520, #21610, #41204, #11621, #16775, #60848, #36392, #31567, #61490, #17095, #40575, #51200, #26110, #7132, #56023, #2318, #6818, #26424, #46041, #1373, #21922, #35763, #11303, #45730, #45406, #50554, #37036, #55708, #61172, #56349, #17422, #20974, #46680, #12271, #56662, #12580, #31883, #51517, #27062, #2626, #41843, #22245, #6498, #51823, #25795, #16459, #60216, #1683, #16140, #21283, #55387, #30928, #36078, #40890, #60537, #31241, #42165, #38586, #28313, #3885, #18971, #62436, #23503, #27690, #2950, #9016, #43106, #62747, #8401, #61801, #57917, #27369, #17727, #37979, #33458, #47930, #33157, #22567, #13537, #42795, #13838, #18668, #37343, #38290, #57610, #52771, #28627, #47620, #8086, #47316, #53078, #48244, #4200, #23813, #3574, #62115, #3268, #47002, #8700, #43416, #7765, #12893, #63059, #18034, #56977, #32513, #52465, #13214, #58219, #22880, #23182, #18354, #37657, #57298, #14146, #52144, #28001, #42474, #32836, #33772, #49516, #39535, #34393, #15107, #54019, #25072, #10281, #29886, #44360, #9953, #43728, #58845, #54666, #45013, #15746, #5774, #29568, #49199, #5139, #24756, #4499, #59497, #58539, #24127, #979, #59825, #6, #323, #44041, #63374, #59173, #19288, #19921, #53392, #35054, #5454, #54351, #44682, #643, #20254, #10590, #39854, #9323, #25394, #15436, #30201, #49830, #20582, #40189, #19608, #28936, #38904, #34722, #48560, #14461, #34083, #53706, #9638, #29246, #14774, #48871, #4818, #24438, #39220, #2246, #36006, #21850, #6737, #6106, #55637, #36321, #41446, #35362, #11552, #31805, #50152, #12190, #55318, #55948, #26037, #7379, #51438, #1930, #61095, #10913, #26987, #46606, #30857, #60141, #61412, #11862, #51121, #2551, #45331, #41763, #30529, #22166, #54984, #31170, #50801, #25721, #1609, #35691, #17019, #1301, #20897, #26346, #7058, #11232, #21534, #21208, #40814, #16703, #40499, #50486, #45651, #60462, #16061, #31478, #36634, #6425, #46289, #16387, #45968, #41131, #60778, #26669, #56268, #28236, #47242, #37903, #33078, #27300, #18278, #13458, #57219, #33383, #47850, #17656, #22804, #52691, #3808, #4124, #23746, #23432, #17955, #43033, #52387, #51752, #37579, #57533, #62673, #17335, #13139, #13761, #32116, #57842, #37271, #8626, #8008, #52999, #8938, #47544, #18594, #56585, #28552, #48172, #12818, #42085, #43339, #38221, #36956, #12504, #46925, #7694, #2873, #22489, #61727, #32758, #8323, #56898, #3187, #32439, #52068, #27612, #42398, #27923, #62038, #3495, #23108, #42712, #62354, #9250, #62984, #14070, #33698, #53316, #38511, #28865, #48487, #24050, #4423, #18897, #58139, #50814, #12521, #12208, #36976, #61745, #2892, #46621, #2567, #36653, #41784, #22181, #61429, #56604, #22824, #42099, #1948, #32133, #51141, #51768, #27002, #7712, #31826, #51458, #7395, #26363, #17352, #60792, #36335, #7075, #6751, #11876, #62057, #17037, #27316, #46944, #42414, #45983, #8024, #22504, #17970, #37594, #17673, #37287, #56916, #12834, #3204, #32454, #31495, #52086, #13154, #41462, #27631, #26689, #21549, #46306, #47259, #57238, #16718, #41145, #55965, #2263, #21866, #61112, #56282, #38239, #34028, #24382, #58789, #48816, #33402, #53017, #8958, #13780, #47563, #38846, #37919, #3513, #43983, #39164, #43050, #23762, #23447, #23125, #18915, #62373, #28568, #32774, #14406, #53334, #33715, #48504, #43667, #24071, #53649, #9268, #52409, #4754, #28883, #9584, #4441, #29189, #63630, #62690, #8340, #18296, #48189, #63308, #19230, #4142, #19550, #58480, #33093, #57859, #27939, #42728, #57549, #13477, #52708, #43359, #8642, #63006, #28255, #38529, #47868, #3827, #18612, #58157, #14091, #29504, #55256, #34665, #35308, #5401, #50426, #11175, #44957, #20838, #53963, #6369, #30798, #10222, #39481, #40756, #54928, #30470, #25975, #24701, #21152, #9895, #45590, #1548, #10533, #30145, #14719, #44627, #15046, #1238, #34339, #49136, #49774, #50097, #54284, #917, #587, #20194, #59762, #5080, #29828, #25017, #39796, #44305, #10854, #45272, #269, #25659, #19867, #59117, #49461, #5720, #40440, #60082, #16004, #59442, #6051, #54609, #15371, #34994, #25335, #40121, #35628, #20522, #15688, #42028, #7002, #55578, #1870, #41390, #2191, #56528, #11804, #12127, #51382, #26611, #46228, #46551, #35950, #61038, #31419, #60405, #16962, #12449, #17602, #22747, #16330, #22110, #21795, #2494, #7637, #32060, #56203, #31750, #36573, #7324, #26934, #41703, #61351, #32384, #51696, #11496, #17274, #60719, #36898, #27242, #46866, #2810, #22431, #61669, #31112, #37218, #6678, #45908, #16642, #50734, #21475, #7950, #56844, #12761, #52009, #27552, #26285, #47184, #3126, #41073, #36264, #55890, #51058, #28496, #48115, #58404, #33327, #23055, #23987, #4676, #33019, #23375, #42660, #13080, #62299, #62617, #63234, #52635, #42345, #53261, #62922, #32700, #9500, #18837, #38455, #53573, #52946, #58083, #18221, #37524, #43592, #14014, #33641, #42975, #52330, #28808, #61983, #8265, #8882, #4370, #9196, #4067, #57165, #23686, #13705, #48427, #19148, #27867, #38765, #43286, #14332, #33953, #18541, #37847, #57480, #29110, #48733, #17902, #47487, #38160, #57785, #3440, #13396, #8569, #28180, #47796, #3753, #35550, #30718, #34571, #15288, #14963, #39084, #10453, #53885, #504, #50342, #5967, #44871, #25254, #40038, #35230, #15612, #25578, #834, #43902, #60003, #20439, #45191, #59680, #1158, #55175, #54202, #24298, #9810, #5323, #54849, #10782, #20111, #40363, #30392, #24619, #29747, #50014, #20757, #11094 ) ),
 .UNSPECIFIED., .F., .F., .F. ) 
 B_SPLINE_SURFACE_WITH_KNOTS ( ( 2, 2 ),
 ( 3, 2, 2, 2, 2, 2, 2, 2, 2, 2, 2, 2, 2, 2, 2, 2, 2, 2, 2, 2, 2, 2, 2, 2, 2, 2, 2, 2, 2, 2, 2, 2, 2, 2, 2, 2, 2, 2, 2, 2, 2, 2, 2, 2, 2, 2, 2, 2, 2, 2, 2, 2, 2, 2, 2, 2, 2, 2, 2, 2, 2, 2, 2, 2, 2, 2, 2, 2, 2, 2, 2, 2, 2, 2, 2, 2, 2, 2, 2, 2, 2, 2, 2, 2, 2, 2, 2, 2, 2, 2, 2, 2, 2, 2, 2, 2, 2, 2, 2, 2, 2, 2, 2, 2, 2, 2, 2, 2, 2, 2, 2, 2, 2, 2, 2, 2, 2, 2, 2, 2, 2, 2, 2, 2, 2, 2, 2, 2, 2, 2, 2, 2, 2, 2, 2, 2, 2, 2, 2, 2, 2, 2, 2, 2, 2, 2, 2, 2, 2, 2, 2, 2, 2, 2, 2, 2, 2, 2, 2, 2, 2, 2, 2, 2, 2, 2, 2, 2, 2, 2, 2, 2, 2, 2, 2, 2, 2, 2, 2, 2, 2, 2, 2, 2, 2, 2, 2, 2, 2, 2, 2, 2, 2, 2, 2, 2, 2, 2, 2, 2, 2, 2, 2, 2, 2, 2, 2, 2, 2, 2, 2, 2, 2, 2, 2, 2, 2, 2, 2, 2, 2, 2, 2, 2, 2, 2, 2, 2, 2, 2, 2, 2, 2, 2, 2, 2, 2, 2, 2, 2, 2, 2, 2, 2, 2, 2, 2, 2, 2, 2, 2, 2, 2, 2, 2, 2, 2, 2, 2, 2, 2, 2, 2, 2, 2, 2, 2, 2, 2, 2, 2, 2, 2, 2, 2, 2, 2, 2, 2, 2, 2, 2, 2, 2, 2, 2, 2, 2, 2, 2, 2, 2, 2, 2, 2, 2, 2, 2, 2, 2, 2, 2, 2, 2, 2, 2, 2, 2, 2, 2, 2, 2, 2, 2, 2, 2, 2, 2, 2, 2, 2, 2, 2, 2, 2, 2, 2, 2, 2, 2, 2, 2, 2, 2, 2, 2, 2, 2, 2, 2, 2, 2, 2, 2, 2, 2, 2, 2, 2, 2, 2, 2, 2, 2, 2, 2, 2, 2, 2, 2, 2, 2, 2, 2, 2, 2, 2, 2, 2, 2, 2, 2, 2, 2, 2, 2, 2, 2, 2, 2, 2, 2, 2, 2, 2, 2, 2, 2, 2, 2, 2, 2, 2, 2, 2, 2, 2, 2, 2, 2, 2, 2, 2, 2, 2, 2, 2, 2, 2, 2, 2, 2, 2, 2, 2, 2, 2, 2, 2, 2, 2, 2, 2, 2, 2, 2, 2, 2, 2, 2, 2, 2, 2, 2, 2, 2, 2, 2, 2, 2, 2, 2, 2, 2, 2, 2, 2, 2, 2, 2, 2, 2, 2, 2, 2, 2, 2, 2, 2, 2, 2, 2, 2, 2, 2, 2, 2, 2, 2, 2, 2, 2, 2, 2, 2, 2, 2, 2, 2, 2, 2, 2, 2, 2, 2, 2, 2, 2, 2, 2, 2, 2, 2, 2, 2, 2, 2, 2, 2, 2, 2, 2, 2, 2, 2, 2, 2, 2, 2, 2, 2, 2, 2, 2, 2, 2, 2, 2, 2, 2, 2, 2, 2, 2, 2, 2, 2, 2, 2, 2, 2, 2, 2, 2, 2, 2, 2, 2, 2, 2, 2, 2, 2, 2, 2, 2, 2, 2, 2, 2, 2, 2, 2, 2, 2, 2, 2, 2, 2, 2, 2, 2, 2, 2, 2, 2, 2, 2, 2, 2, 2, 2, 2, 2, 2, 2, 2, 2, 2, 2, 2, 2, 2, 2, 2, 2, 2, 2, 2, 2, 2, 2, 2, 2, 2, 2, 2, 2, 2, 2, 2, 2, 2, 2, 2, 2, 2, 2, 2, 2, 2, 2, 2, 2, 2, 2, 2, 2, 2, 2, 2, 2, 2, 2, 2, 2, 2, 2, 2, 2, 2, 2, 2, 2, 2, 2, 2, 2, 2, 2, 2, 2, 2, 2, 2, 2, 2, 2, 2, 2, 2, 2, 2, 2, 2, 2, 2, 2, 2, 2, 2, 2, 2, 2, 2, 2, 2, 2, 2, 2, 2, 2, 2, 2, 2, 2, 2, 2, 2, 2, 2, 2, 2, 2, 2, 2, 2, 2, 2, 2, 2, 2, 2, 2, 2, 2, 2, 2, 2, 2, 2, 2, 2, 2, 2, 2, 2, 2, 2, 2, 2, 2, 2, 2, 2, 2, 2, 2, 2, 2, 3 ),
 ( 0.000000000000000000, 1.000000000000000000 ),
 ( 0.000000000000000000, 0.001388888888888888942, 0.002777777777777777884, 0.004166666666666666609, 0.005555555555555555768, 0.006944444444444444059, 0.008333333333333333218, 0.009722222222222222376, 0.01111111111111111154, 0.01250000000000000069, 0.01388888888888888812, 0.01527777777777777728, 0.01666666666666666644, 0.01805555555555555386, 0.01944444444444444475, 0.02083333333333333218, 0.02222222222222222307, 0.02361111111111111049, 0.02500000000000000139, 0.02638888888888888881, 0.02777777777777777624, 0.02916666666666666713, 0.03055555555555555455, 0.03194444444444444198, 0.03333333333333333287, 0.03472222222222222376, 0.03611111111111110772, 0.03749999999999999861, 0.03888888888888888951, 0.04027777777777778040, 0.04166666666666666435, 0.04305555555555555525, 0.04444444444444444614, 0.04583333333333333010, 0.04722222222222222099, 0.04861111111111111188, 0.05000000000000000278, 0.05138888888888888673, 0.05277777777777777762, 0.05416666666666666852, 0.05555555555555555247, 0.05694444444444444337, 0.05833333333333333426, 0.05972222222222222515, 0.06111111111111110911, 0.06250000000000000000, 0.06388888888888888395, 0.06527777777777778179, 0.06666666666666666574, 0.06805555555555554970, 0.06944444444444444753, 0.07083333333333333148, 0.07222222222222221544, 0.07361111111111111327, 0.07499999999999999722, 0.07638888888888889506, 0.07777777777777777901, 0.07916666666666666297, 0.08055555555555556080, 0.08194444444444444475, 0.08333333333333332871, 0.08472222222222222654, 0.08611111111111111049, 0.08749999999999999445, 0.08888888888888889228, 0.09027777777777777624, 0.09166666666666666019, 0.09305555555555555802, 0.09444444444444444198, 0.09583333333333333981, 0.09722222222222222376, 0.09861111111111110772, 0.1000000000000000056, 0.1013888888888888895, 0.1027777777777777735, 0.1041666666666666713, 0.1055555555555555552, 0.1069444444444444392, 0.1083333333333333370, 0.1097222222222222210, 0.1111111111111111049, 0.1125000000000000028, 0.1138888888888888867, 0.1152777777777777846, 0.1166666666666666685, 0.1180555555555555525, 0.1194444444444444503, 0.1208333333333333343, 0.1222222222222222182, 0.1236111111111111160, 0.1250000000000000000, 0.1263888888888888840, 0.1277777777777777679, 0.1291666666666666796, 0.1305555555555555636, 0.1319444444444444475, 0.1333333333333333315, 0.1347222222222222154, 0.1361111111111110994, 0.1375000000000000111, 0.1388888888888888951, 0.1402777777777777790, 0.1416666666666666630, 0.1430555555555555469, 0.1444444444444444309, 0.1458333333333333426, 0.1472222222222222265, 0.1486111111111111105, 0.1499999999999999944, 0.1513888888888888784, 0.1527777777777777901, 0.1541666666666666741, 0.1555555555555555580, 0.1569444444444444420, 0.1583333333333333259, 0.1597222222222222099, 0.1611111111111111216, 0.1625000000000000056, 0.1638888888888888895, 0.1652777777777777735, 0.1666666666666666574, 0.1680555555555555691, 0.1694444444444444531, 0.1708333333333333370, 0.1722222222222222210, 0.1736111111111111049, 0.1749999999999999889, 0.1763888888888889006, 0.1777777777777777846, 0.1791666666666666685, 0.1805555555555555525, 0.1819444444444444364, 0.1833333333333333204, 0.1847222222222222321, 0.1861111111111111160, 0.1875000000000000000, 0.1888888888888888840, 0.1902777777777777679, 0.1916666666666666796, 0.1930555555555555636, 0.1944444444444444475, 0.1958333333333333315, 0.1972222222222222154, 0.1986111111111110994, 0.2000000000000000111, 0.2013888888888888951, 0.2027777777777777790, 0.2041666666666666630, 0.2055555555555555469, 0.2069444444444444309, 0.2083333333333333426, 0.2097222222222222265, 0.2111111111111111105, 0.2124999999999999944, 0.2138888888888888784, 0.2152777777777777901, 0.2166666666666666741, 0.2180555555555555580, 0.2194444444444444420, 0.2208333333333333259, 0.2222222222222222099, 0.2236111111111111216, 0.2250000000000000056, 0.2263888888888888895, 0.2277777777777777735, 0.2291666666666666574, 0.2305555555555555691, 0.2319444444444444531, 0.2333333333333333370, 0.2347222222222222210, 0.2361111111111111049, 0.2374999999999999889, 0.2388888888888889006, 0.2402777777777777846, 0.2416666666666666685, 0.2430555555555555525, 0.2444444444444444364, 0.2458333333333333204, 0.2472222222222222321, 0.2486111111111111160, 0.2500000000000000000, 0.2513888888888888840, 0.2527777777777777679, 0.2541666666666666519, 0.2555555555555555358, 0.2569444444444444198, 0.2583333333333333592, 0.2597222222222222432, 0.2611111111111111271, 0.2625000000000000111, 0.2638888888888888951, 0.2652777777777777790, 0.2666666666666666630, 0.2680555555555555469, 0.2694444444444444309, 0.2708333333333333148, 0.2722222222222221988, 0.2736111111111111382, 0.2750000000000000222, 0.2763888888888889062, 0.2777777777777777901, 0.2791666666666666741, 0.2805555555555555580, 0.2819444444444444420, 0.2833333333333333259, 0.2847222222222222099, 0.2861111111111110938, 0.2874999999999999778, 0.2888888888888888618, 0.2902777777777778012, 0.2916666666666666852, 0.2930555555555555691, 0.2944444444444444531, 0.2958333333333333370, 0.2972222222222222210, 0.2986111111111111049, 0.2999999999999999889, 0.3013888888888888729, 0.3027777777777777568, 0.3041666666666666408, 0.3055555555555555802, 0.3069444444444444642, 0.3083333333333333481, 0.3097222222222222321, 0.3111111111111111160, 0.3125000000000000000, 0.3138888888888888840, 0.3152777777777777679, 0.3166666666666666519, 0.3180555555555555358, 0.3194444444444444198, 0.3208333333333333592, 0.3222222222222222432, 0.3236111111111111271, 0.3250000000000000111, 0.3263888888888888951, 0.3277777777777777790, 0.3291666666666666630, 0.3305555555555555469, 0.3319444444444444309, 0.3333333333333333148, 0.3347222222222221988, 0.3361111111111111382, 0.3375000000000000222, 0.3388888888888889062, 0.3402777777777777901, 0.3416666666666666741, 0.3430555555555555580, 0.3444444444444444420, 0.3458333333333333259, 0.3472222222222222099, 0.3486111111111110938, 0.3499999999999999778, 0.3513888888888888618, 0.3527777777777778012, 0.3541666666666666852, 0.3555555555555555691, 0.3569444444444444531, 0.3583333333333333370, 0.3597222222222222210, 0.3611111111111111049, 0.3624999999999999889, 0.3638888888888888729, 0.3652777777777777568, 0.3666666666666666408, 0.3680555555555555802, 0.3694444444444444642, 0.3708333333333333481, 0.3722222222222222321, 0.3736111111111111160, 0.3750000000000000000, 0.3763888888888888840, 0.3777777777777777679, 0.3791666666666666519, 0.3805555555555555358, 0.3819444444444444198, 0.3833333333333333592, 0.3847222222222222432, 0.3861111111111111271, 0.3875000000000000111, 0.3888888888888888951, 0.3902777777777777790, 0.3916666666666666630, 0.3930555555555555469, 0.3944444444444444309, 0.3958333333333333148, 0.3972222222222221988, 0.3986111111111111382, 0.4000000000000000222, 0.4013888888888889062, 0.4027777777777777901, 0.4041666666666666741, 0.4055555555555555580, 0.4069444444444444420, 0.4083333333333333259, 0.4097222222222222099, 0.4111111111111110938, 0.4124999999999999778, 0.4138888888888888618, 0.4152777777777778012, 0.4166666666666666852, 0.4180555555555555691, 0.4194444444444444531, 0.4208333333333333370, 0.4222222222222222210, 0.4236111111111111049, 0.4249999999999999889, 0.4263888888888888729, 0.4277777777777777568, 0.4291666666666666408, 0.4305555555555555802, 0.4319444444444444642, 0.4333333333333333481, 0.4347222222222222321, 0.4361111111111111160, 0.4375000000000000000, 0.4388888888888888840, 0.4402777777777777679, 0.4416666666666666519, 0.4430555555555555358, 0.4444444444444444198, 0.4458333333333333592, 0.4472222222222222432, 0.4486111111111111271, 0.4500000000000000111, 0.4513888888888888951, 0.4527777777777777790, 0.4541666666666666630, 0.4555555555555555469, 0.4569444444444444309, 0.4583333333333333148, 0.4597222222222221988, 0.4611111111111111382, 0.4625000000000000222, 0.4638888888888889062, 0.4652777777777777901, 0.4666666666666666741, 0.4680555555555555580, 0.4694444444444444420, 0.4708333333333333259, 0.4722222222222222099, 0.4736111111111110938, 0.4749999999999999778, 0.4763888888888888618, 0.4777777777777778012, 0.4791666666666666852, 0.4805555555555555691, 0.4819444444444444531, 0.4833333333333333370, 0.4847222222222222210, 0.4861111111111111049, 0.4874999999999999889, 0.4888888888888888729, 0.4902777777777777568, 0.4916666666666666408, 0.4930555555555555802, 0.4944444444444444642, 0.4958333333333333481, 0.4972222222222222321, 0.4986111111111111160, 0.5000000000000000000, 0.5013888888888888840, 0.5027777777777777679, 0.5041666666666666519, 0.5055555555555555358, 0.5069444444444444198, 0.5083333333333333037, 0.5097222222222221877, 0.5111111111111110716, 0.5124999999999999556, 0.5138888888888888395, 0.5152777777777777235, 0.5166666666666667185, 0.5180555555555556024, 0.5194444444444444864, 0.5208333333333333703, 0.5222222222222222543, 0.5236111111111111382, 0.5250000000000000222, 0.5263888888888889062, 0.5277777777777777901, 0.5291666666666666741, 0.5305555555555555580, 0.5319444444444444420, 0.5333333333333333259, 0.5347222222222222099, 0.5361111111111110938, 0.5374999999999999778, 0.5388888888888888618, 0.5402777777777777457, 0.5416666666666666297, 0.5430555555555555136, 0.5444444444444443976, 0.5458333333333332815, 0.5472222222222222765, 0.5486111111111111605, 0.5500000000000000444, 0.5513888888888889284, 0.5527777777777778123, 0.5541666666666666963, 0.5555555555555555802, 0.5569444444444444642, 0.5583333333333333481, 0.5597222222222222321, 0.5611111111111111160, 0.5625000000000000000, 0.5638888888888888840, 0.5652777777777777679, 0.5666666666666666519, 0.5680555555555555358, 0.5694444444444444198, 0.5708333333333333037, 0.5722222222222221877, 0.5736111111111110716, 0.5749999999999999556, 0.5763888888888888395, 0.5777777777777777235, 0.5791666666666667185, 0.5805555555555556024, 0.5819444444444444864, 0.5833333333333333703, 0.5847222222222222543, 0.5861111111111111382, 0.5875000000000000222, 0.5888888888888889062, 0.5902777777777777901, 0.5916666666666666741, 0.5930555555555555580, 0.5944444444444444420, 0.5958333333333333259, 0.5972222222222222099, 0.5986111111111110938, 0.5999999999999999778, 0.6013888888888888618, 0.6027777777777777457, 0.6041666666666666297, 0.6055555555555555136, 0.6069444444444443976, 0.6083333333333332815, 0.6097222222222222765, 0.6111111111111111605, 0.6125000000000000444, 0.6138888888888889284, 0.6152777777777778123, 0.6166666666666666963, 0.6180555555555555802, 0.6194444444444444642, 0.6208333333333333481, 0.6222222222222222321, 0.6236111111111111160, 0.6250000000000000000, 0.6263888888888888840, 0.6277777777777777679, 0.6291666666666666519, 0.6305555555555555358, 0.6319444444444444198, 0.6333333333333333037, 0.6347222222222221877, 0.6361111111111110716, 0.6374999999999999556, 0.6388888888888888395, 0.6402777777777777235, 0.6416666666666667185, 0.6430555555555556024, 0.6444444444444444864, 0.6458333333333333703, 0.6472222222222222543, 0.6486111111111111382, 0.6500000000000000222, 0.6513888888888889062, 0.6527777777777777901, 0.6541666666666666741, 0.6555555555555555580, 0.6569444444444444420, 0.6583333333333333259, 0.6597222222222222099, 0.6611111111111110938, 0.6624999999999999778, 0.6638888888888888618, 0.6652777777777777457, 0.6666666666666666297, 0.6680555555555555136, 0.6694444444444443976, 0.6708333333333332815, 0.6722222222222222765, 0.6736111111111111605, 0.6750000000000000444, 0.6763888888888889284, 0.6777777777777778123, 0.6791666666666666963, 0.6805555555555555802, 0.6819444444444444642, 0.6833333333333333481, 0.6847222222222222321, 0.6861111111111111160, 0.6875000000000000000, 0.6888888888888888840, 0.6902777777777777679, 0.6916666666666666519, 0.6930555555555555358, 0.6944444444444444198, 0.6958333333333333037, 0.6972222222222221877, 0.6986111111111110716, 0.6999999999999999556, 0.7013888888888888395, 0.7027777777777777235, 0.7041666666666667185, 0.7055555555555556024, 0.7069444444444444864, 0.7083333333333333703, 0.7097222222222222543, 0.7111111111111111382, 0.7125000000000000222, 0.7138888888888889062, 0.7152777777777777901, 0.7166666666666666741, 0.7180555555555555580, 0.7194444444444444420, 0.7208333333333333259, 0.7222222222222222099, 0.7236111111111110938, 0.7249999999999999778, 0.7263888888888888618, 0.7277777777777777457, 0.7291666666666666297, 0.7305555555555555136, 0.7319444444444443976, 0.7333333333333332815, 0.7347222222222222765, 0.7361111111111111605, 0.7375000000000000444, 0.7388888888888889284, 0.7402777777777778123, 0.7416666666666666963, 0.7430555555555555802, 0.7444444444444444642, 0.7458333333333333481, 0.7472222222222222321, 0.7486111111111111160, 0.7500000000000000000, 0.7513888888888888840, 0.7527777777777777679, 0.7541666666666666519, 0.7555555555555555358, 0.7569444444444444198, 0.7583333333333333037, 0.7597222222222221877, 0.7611111111111110716, 0.7624999999999999556, 0.7638888888888888395, 0.7652777777777777235, 0.7666666666666667185, 0.7680555555555556024, 0.7694444444444444864, 0.7708333333333333703, 0.7722222222222222543, 0.7736111111111111382, 0.7750000000000000222, 0.7763888888888889062, 0.7777777777777777901, 0.7791666666666666741, 0.7805555555555555580, 0.7819444444444444420, 0.7833333333333333259, 0.7847222222222222099, 0.7861111111111110938, 0.7874999999999999778, 0.7888888888888888618, 0.7902777777777777457, 0.7916666666666666297, 0.7930555555555555136, 0.7944444444444443976, 0.7958333333333332815, 0.7972222222222222765, 0.7986111111111111605, 0.8000000000000000444, 0.8013888888888889284, 0.8027777777777778123, 0.8041666666666666963, 0.8055555555555555802, 0.8069444444444444642, 0.8083333333333333481, 0.8097222222222222321, 0.8111111111111111160, 0.8125000000000000000, 0.8138888888888888840, 0.8152777777777777679, 0.8166666666666666519, 0.8180555555555555358, 0.8194444444444444198, 0.8208333333333333037, 0.8222222222222221877, 0.8236111111111110716, 0.8249999999999999556, 0.8263888888888888395, 0.8277777777777777235, 0.8291666666666667185, 0.8305555555555556024, 0.8319444444444444864, 0.8333333333333333703, 0.8347222222222222543, 0.8361111111111111382, 0.8375000000000000222, 0.8388888888888889062, 0.8402777777777777901, 0.8416666666666666741, 0.8430555555555555580, 0.8444444444444444420, 0.8458333333333333259, 0.8472222222222222099, 0.8486111111111110938, 0.8499999999999999778, 0.8513888888888888618, 0.8527777777777777457, 0.8541666666666666297, 0.8555555555555555136, 0.8569444444444443976, 0.8583333333333332815, 0.8597222222222222765, 0.8611111111111111605, 0.8625000000000000444, 0.8638888888888889284, 0.8652777777777778123, 0.8666666666666666963, 0.8680555555555555802, 0.8694444444444444642, 0.8708333333333333481, 0.8722222222222222321, 0.8736111111111111160, 0.8750000000000000000, 0.8763888888888888840, 0.8777777777777777679, 0.8791666666666666519, 0.8805555555555555358, 0.8819444444444444198, 0.8833333333333333037, 0.8847222222222221877, 0.8861111111111110716, 0.8874999999999999556, 0.8888888888888888395, 0.8902777777777777235, 0.8916666666666667185, 0.8930555555555556024, 0.8944444444444444864, 0.8958333333333333703, 0.8972222222222222543, 0.8986111111111111382, 0.9000000000000000222, 0.9013888888888889062, 0.9027777777777777901, 0.9041666666666666741, 0.9055555555555555580, 0.9069444444444444420, 0.9083333333333333259, 0.9097222222222222099, 0.9111111111111110938, 0.9124999999999999778, 0.9138888888888888618, 0.9152777777777777457, 0.9166666666666666297, 0.9180555555555555136, 0.9194444444444443976, 0.9208333333333332815, 0.9222222222222222765, 0.9236111111111111605, 0.9250000000000000444, 0.9263888888888889284, 0.9277777777777778123, 0.9291666666666666963, 0.9305555555555555802, 0.9319444444444444642, 0.9333333333333333481, 0.9347222222222222321, 0.9361111111111111160, 0.9375000000000000000, 0.9388888888888888840, 0.9402777777777777679, 0.9416666666666666519, 0.9430555555555555358, 0.9444444444444444198, 0.9458333333333333037, 0.9472222222222221877, 0.9486111111111110716, 0.9499999999999999556, 0.9513888888888888395, 0.9527777777777777235, 0.9541666666666667185, 0.9555555555555556024, 0.9569444444444444864, 0.9583333333333333703, 0.9597222222222222543, 0.9611111111111111382, 0.9625000000000000222, 0.9638888888888889062, 0.9652777777777777901, 0.9666666666666666741, 0.9680555555555555580, 0.9694444444444444420, 0.9708333333333333259, 0.9722222222222222099, 0.9736111111111110938, 0.9749999999999999778, 0.9763888888888888618, 0.9777777777777777457, 0.9791666666666666297, 0.9805555555555555136, 0.9819444444444443976, 0.9833333333333332815, 0.9847222222222222765, 0.9861111111111111605, 0.9875000000000000444, 0.9888888888888889284, 0.9902777777777778123, 0.9916666666666666963, 0.9930555555555555802, 0.9944444444444444642, 0.9958333333333333481, 0.9972222222222222321, 0.9986111111111111160, 1.000000000000000000 ),
 .UNSPECIFIED. ) 
 GEOMETRIC_REPRESENTATION_ITEM ( )  RATIONAL_B_SPLINE_SURFACE ( (
 ( 1.000000000000000000, 0.8660254037844387076, 1.000000000000000000, 0.8660254037844387076, 1.000000000000000000, 0.8660254037844387076, 1.000000000000000000, 0.8660254037844387076, 1.000000000000000000, 0.8660254037844387076, 1.000000000000000000, 0.8660254037844387076, 1.000000000000000000, 0.8660254037844387076, 1.000000000000000000, 0.8660254037844387076, 1.000000000000000000, 0.8660254037844387076, 1.000000000000000000, 0.8660254037844387076, 1.000000000000000000, 0.8660254037844387076, 1.000000000000000000, 0.8660254037844387076, 1.000000000000000000, 0.8660254037844387076, 1.000000000000000000, 0.8660254037844387076, 1.000000000000000000, 0.8660254037844387076, 1.000000000000000000, 0.8660254037844387076, 1.000000000000000000, 0.8660254037844387076, 1.000000000000000000, 0.8660254037844387076, 1.000000000000000000, 0.8660254037844387076, 1.000000000000000000, 0.8660254037844387076, 1.000000000000000000, 0.8660254037844387076, 1.000000000000000000, 0.8660254037844387076, 1.000000000000000000, 0.8660254037844387076, 1.000000000000000000, 0.8660254037844387076, 1.000000000000000000, 0.8660254037844387076, 1.000000000000000000, 0.8660254037844387076, 1.000000000000000000, 0.8660254037844387076, 1.000000000000000000, 0.8660254037844387076, 1.000000000000000000, 0.8660254037844387076, 1.000000000000000000, 0.8660254037844387076, 1.000000000000000000, 0.8660254037844387076, 1.000000000000000000, 0.8660254037844387076, 1.000000000000000000, 0.8660254037844387076, 1.000000000000000000, 0.8660254037844387076, 1.000000000000000000, 0.8660254037844387076, 1.000000000000000000, 0.8660254037844387076, 1.000000000000000000, 0.8660254037844387076, 1.000000000000000000, 0.8660254037844387076, 1.000000000000000000, 0.8660254037844387076, 1.000000000000000000, 0.8660254037844387076, 1.000000000000000000, 0.8660254037844387076, 1.000000000000000000, 0.8660254037844387076, 1.000000000000000000, 0.8660254037844387076, 1.000000000000000000, 0.8660254037844387076, 1.000000000000000000, 0.8660254037844387076, 1.000000000000000000, 0.8660254037844387076, 1.000000000000000000, 0.8660254037844387076, 1.000000000000000000, 0.8660254037844387076, 1.000000000000000000, 0.8660254037844387076, 1.000000000000000000, 0.8660254037844387076, 1.000000000000000000, 0.8660254037844387076, 1.000000000000000000, 0.8660254037844387076, 1.000000000000000000, 0.8660254037844387076, 1.000000000000000000, 0.8660254037844387076, 1.000000000000000000, 0.8660254037844387076, 1.000000000000000000, 0.8660254037844387076, 1.000000000000000000, 0.8660254037844387076, 1.000000000000000000, 0.8660254037844387076, 1.000000000000000000, 0.8660254037844387076, 1.000000000000000000, 0.8660254037844387076, 1.000000000000000000, 0.8660254037844387076, 1.000000000000000000, 0.8660254037844387076, 1.000000000000000000, 0.8660254037844387076, 1.000000000000000000, 0.8660254037844387076, 1.000000000000000000, 0.8660254037844387076, 1.000000000000000000, 0.8660254037844387076, 1.000000000000000000, 0.8660254037844387076, 1.000000000000000000, 0.8660254037844387076, 1.000000000000000000, 0.8660254037844387076, 1.000000000000000000, 0.8660254037844387076, 1.000000000000000000, 0.8660254037844387076, 1.000000000000000000, 0.8660254037844387076, 1.000000000000000000, 0.8660254037844387076, 1.000000000000000000, 0.8660254037844387076, 1.000000000000000000, 0.8660254037844387076, 1.000000000000000000, 0.8660254037844387076, 1.000000000000000000, 0.8660254037844387076, 1.000000000000000000, 0.8660254037844387076, 1.000000000000000000, 0.8660254037844387076, 1.000000000000000000, 0.8660254037844387076, 1.000000000000000000, 0.8660254037844387076, 1.000000000000000000, 0.8660254037844387076, 1.000000000000000000, 0.8660254037844387076, 1.000000000000000000, 0.8660254037844387076, 1.000000000000000000, 0.8660254037844387076, 1.000000000000000000, 0.8660254037844387076, 1.000000000000000000, 0.8660254037844387076, 1.000000000000000000, 0.8660254037844387076, 1.000000000000000000, 0.8660254037844387076, 1.000000000000000000, 0.8660254037844387076, 1.000000000000000000, 0.8660254037844387076, 1.000000000000000000, 0.8660254037844387076, 1.000000000000000000, 0.8660254037844387076, 1.000000000000000000, 0.8660254037844387076, 1.000000000000000000, 0.8660254037844387076, 1.000000000000000000, 0.8660254037844387076, 1.000000000000000000, 0.8660254037844387076, 1.000000000000000000, 0.8660254037844387076, 1.000000000000000000, 0.8660254037844387076, 1.000000000000000000, 0.8660254037844387076, 1.000000000000000000, 0.8660254037844387076, 1.000000000000000000, 0.8660254037844387076, 1.000000000000000000, 0.8660254037844387076, 1.000000000000000000, 0.8660254037844387076, 1.000000000000000000, 0.8660254037844387076, 1.000000000000000000, 0.8660254037844387076, 1.000000000000000000, 0.8660254037844387076, 1.000000000000000000, 0.8660254037844387076, 1.000000000000000000, 0.8660254037844387076, 1.000000000000000000, 0.8660254037844387076, 1.000000000000000000, 0.8660254037844387076, 1.000000000000000000, 0.8660254037844387076, 1.000000000000000000, 0.8660254037844387076, 1.000000000000000000, 0.8660254037844387076, 1.000000000000000000, 0.8660254037844387076, 1.000000000000000000, 0.8660254037844387076, 1.000000000000000000, 0.8660254037844387076, 1.000000000000000000, 0.8660254037844387076, 1.000000000000000000, 0.8660254037844387076, 1.000000000000000000, 0.8660254037844387076, 1.000000000000000000, 0.8660254037844387076, 1.000000000000000000, 0.8660254037844387076, 1.000000000000000000, 0.8660254037844387076, 1.000000000000000000, 0.8660254037844387076, 1.000000000000000000, 0.8660254037844387076, 1.000000000000000000, 0.8660254037844387076, 1.000000000000000000, 0.8660254037844387076, 1.000000000000000000, 0.8660254037844387076, 1.000000000000000000, 0.8660254037844387076, 1.000000000000000000, 0.8660254037844387076, 1.000000000000000000, 0.8660254037844387076, 1.000000000000000000, 0.8660254037844387076, 1.000000000000000000, 0.8660254037844387076, 1.000000000000000000, 0.8660254037844387076, 1.000000000000000000, 0.8660254037844387076, 1.000000000000000000, 0.8660254037844387076, 1.000000000000000000, 0.8660254037844387076, 1.000000000000000000, 0.8660254037844387076, 1.000000000000000000, 0.8660254037844387076, 1.000000000000000000, 0.8660254037844387076, 1.000000000000000000, 0.8660254037844387076, 1.000000000000000000, 0.8660254037844387076, 1.000000000000000000, 0.8660254037844387076, 1.000000000000000000, 0.8660254037844387076, 1.000000000000000000, 0.8660254037844387076, 1.000000000000000000, 0.8660254037844387076, 1.000000000000000000, 0.8660254037844387076, 1.000000000000000000, 0.8660254037844387076, 1.000000000000000000, 0.8660254037844387076, 1.000000000000000000, 0.8660254037844387076, 1.000000000000000000, 0.8660254037844387076, 1.000000000000000000, 0.8660254037844387076, 1.000000000000000000, 0.8660254037844387076, 1.000000000000000000, 0.8660254037844387076, 1.000000000000000000, 0.8660254037844387076, 1.000000000000000000, 0.8660254037844387076, 1.000000000000000000, 0.8660254037844387076, 1.000000000000000000, 0.8660254037844387076, 1.000000000000000000, 0.8660254037844387076, 1.000000000000000000, 0.8660254037844387076, 1.000000000000000000, 0.8660254037844387076, 1.000000000000000000, 0.8660254037844387076, 1.000000000000000000, 0.8660254037844387076, 1.000000000000000000, 0.8660254037844387076, 1.000000000000000000, 0.8660254037844387076, 1.000000000000000000, 0.8660254037844387076, 1.000000000000000000, 0.8660254037844387076, 1.000000000000000000, 0.8660254037844387076, 1.000000000000000000, 0.8660254037844387076, 1.000000000000000000, 0.8660254037844387076, 1.000000000000000000, 0.8660254037844387076, 1.000000000000000000, 0.8660254037844387076, 1.000000000000000000, 0.8660254037844387076, 1.000000000000000000, 0.8660254037844387076, 1.000000000000000000, 0.8660254037844387076, 1.000000000000000000, 0.8660254037844387076, 1.000000000000000000, 0.8660254037844387076, 1.000000000000000000, 0.8660254037844387076, 1.000000000000000000, 0.8660254037844387076, 1.000000000000000000, 0.8660254037844387076, 1.000000000000000000, 0.8660254037844387076, 1.000000000000000000, 0.8660254037844387076, 1.000000000000000000, 0.8660254037844387076, 1.000000000000000000, 0.8660254037844387076, 1.000000000000000000, 0.8660254037844387076, 1.000000000000000000, 0.8660254037844387076, 1.000000000000000000, 0.8660254037844387076, 1.000000000000000000, 0.8660254037844387076, 1.000000000000000000, 0.8660254037844387076, 1.000000000000000000, 0.8660254037844387076, 1.000000000000000000, 0.8660254037844387076, 1.000000000000000000, 0.8660254037844387076, 1.000000000000000000, 0.8660254037844387076, 1.000000000000000000, 0.8660254037844387076, 1.000000000000000000, 0.8660254037844387076, 1.000000000000000000, 0.8660254037844387076, 1.000000000000000000, 0.8660254037844387076, 1.000000000000000000, 0.8660254037844387076, 1.000000000000000000, 0.8660254037844387076, 1.000000000000000000, 0.8660254037844387076, 1.000000000000000000, 0.8660254037844387076, 1.000000000000000000, 0.8660254037844387076, 1.000000000000000000, 0.8660254037844387076, 1.000000000000000000, 0.8660254037844387076, 1.000000000000000000, 0.8660254037844387076, 1.000000000000000000, 0.8660254037844387076, 1.000000000000000000, 0.8660254037844387076, 1.000000000000000000, 0.8660254037844387076, 1.000000000000000000, 0.8660254037844387076, 1.000000000000000000, 0.8660254037844387076, 1.000000000000000000, 0.8660254037844387076, 1.000000000000000000, 0.8660254037844387076, 1.000000000000000000, 0.8660254037844387076, 1.000000000000000000, 0.8660254037844387076, 1.000000000000000000, 0.8660254037844387076, 1.000000000000000000, 0.8660254037844387076, 1.000000000000000000, 0.8660254037844387076, 1.000000000000000000, 0.8660254037844387076, 1.000000000000000000, 0.8660254037844387076, 1.000000000000000000, 0.8660254037844387076, 1.000000000000000000, 0.8660254037844387076, 1.000000000000000000, 0.8660254037844387076, 1.000000000000000000, 0.8660254037844387076, 1.000000000000000000, 0.8660254037844387076, 1.000000000000000000, 0.8660254037844387076, 1.000000000000000000, 0.8660254037844387076, 1.000000000000000000, 0.8660254037844387076, 1.000000000000000000, 0.8660254037844387076, 1.000000000000000000, 0.8660254037844387076, 1.000000000000000000, 0.8660254037844387076, 1.000000000000000000, 0.8660254037844387076, 1.000000000000000000, 0.8660254037844387076, 1.000000000000000000, 0.8660254037844387076, 1.000000000000000000, 0.8660254037844387076, 1.000000000000000000, 0.8660254037844387076, 1.000000000000000000, 0.8660254037844387076, 1.000000000000000000, 0.8660254037844387076, 1.000000000000000000, 0.8660254037844387076, 1.000000000000000000, 0.8660254037844387076, 1.000000000000000000, 0.8660254037844387076, 1.000000000000000000, 0.8660254037844387076, 1.000000000000000000, 0.8660254037844387076, 1.000000000000000000, 0.8660254037844387076, 1.000000000000000000, 0.8660254037844387076, 1.000000000000000000, 0.8660254037844387076, 1.000000000000000000, 0.8660254037844387076, 1.000000000000000000, 0.8660254037844387076, 1.000000000000000000, 0.8660254037844387076, 1.000000000000000000, 0.8660254037844387076, 1.000000000000000000, 0.8660254037844387076, 1.000000000000000000, 0.8660254037844387076, 1.000000000000000000, 0.8660254037844387076, 1.000000000000000000, 0.8660254037844387076, 1.000000000000000000, 0.8660254037844387076, 1.000000000000000000, 0.8660254037844387076, 1.000000000000000000, 0.8660254037844387076, 1.000000000000000000, 0.8660254037844387076, 1.000000000000000000, 0.8660254037844387076, 1.000000000000000000, 0.8660254037844387076, 1.000000000000000000, 0.8660254037844387076, 1.000000000000000000, 0.8660254037844387076, 1.000000000000000000, 0.8660254037844387076, 1.000000000000000000, 0.8660254037844387076, 1.000000000000000000, 0.8660254037844387076, 1.000000000000000000, 0.8660254037844387076, 1.000000000000000000, 0.8660254037844387076, 1.000000000000000000, 0.8660254037844387076, 1.000000000000000000, 0.8660254037844387076, 1.000000000000000000, 0.8660254037844387076, 1.000000000000000000, 0.8660254037844387076, 1.000000000000000000, 0.8660254037844387076, 1.000000000000000000, 0.8660254037844387076, 1.000000000000000000, 0.8660254037844387076, 1.000000000000000000, 0.8660254037844387076, 1.000000000000000000, 0.8660254037844387076, 1.000000000000000000, 0.8660254037844387076, 1.000000000000000000, 0.8660254037844387076, 1.000000000000000000, 0.8660254037844387076, 1.000000000000000000, 0.8660254037844387076, 1.000000000000000000, 0.8660254037844387076, 1.000000000000000000, 0.8660254037844387076, 1.000000000000000000, 0.8660254037844387076, 1.000000000000000000, 0.8660254037844387076, 1.000000000000000000, 0.8660254037844387076, 1.000000000000000000, 0.8660254037844387076, 1.000000000000000000, 0.8660254037844387076, 1.000000000000000000, 0.8660254037844387076, 1.000000000000000000, 0.8660254037844387076, 1.000000000000000000, 0.8660254037844387076, 1.000000000000000000, 0.8660254037844387076, 1.000000000000000000, 0.8660254037844387076, 1.000000000000000000, 0.8660254037844387076, 1.000000000000000000, 0.8660254037844387076, 1.000000000000000000, 0.8660254037844387076, 1.000000000000000000, 0.8660254037844387076, 1.000000000000000000, 0.8660254037844387076, 1.000000000000000000, 0.8660254037844387076, 1.000000000000000000, 0.8660254037844387076, 1.000000000000000000, 0.8660254037844387076, 1.000000000000000000, 0.8660254037844387076, 1.000000000000000000, 0.8660254037844387076, 1.000000000000000000, 0.8660254037844387076, 1.000000000000000000, 0.8660254037844387076, 1.000000000000000000, 0.8660254037844387076, 1.000000000000000000, 0.8660254037844387076, 1.000000000000000000, 0.8660254037844387076, 1.000000000000000000, 0.8660254037844387076, 1.000000000000000000, 0.8660254037844387076, 1.000000000000000000, 0.8660254037844387076, 1.000000000000000000, 0.8660254037844387076, 1.000000000000000000, 0.8660254037844387076, 1.000000000000000000, 0.8660254037844387076, 1.000000000000000000, 0.8660254037844387076, 1.000000000000000000, 0.8660254037844387076, 1.000000000000000000, 0.8660254037844387076, 1.000000000000000000, 0.8660254037844387076, 1.000000000000000000, 0.8660254037844387076, 1.000000000000000000, 0.8660254037844387076, 1.000000000000000000, 0.8660254037844387076, 1.000000000000000000, 0.8660254037844387076, 1.000000000000000000, 0.8660254037844387076, 1.000000000000000000, 0.8660254037844387076, 1.000000000000000000, 0.8660254037844387076, 1.000000000000000000, 0.8660254037844387076, 1.000000000000000000, 0.8660254037844387076, 1.000000000000000000, 0.8660254037844387076, 1.000000000000000000, 0.8660254037844387076, 1.000000000000000000, 0.8660254037844387076, 1.000000000000000000, 0.8660254037844387076, 1.000000000000000000, 0.8660254037844387076, 1.000000000000000000, 0.8660254037844387076, 1.000000000000000000, 0.8660254037844387076, 1.000000000000000000, 0.8660254037844387076, 1.000000000000000000, 0.8660254037844387076, 1.000000000000000000, 0.8660254037844387076, 1.000000000000000000, 0.8660254037844387076, 1.000000000000000000, 0.8660254037844387076, 1.000000000000000000, 0.8660254037844387076, 1.000000000000000000, 0.8660254037844387076, 1.000000000000000000, 0.8660254037844387076, 1.000000000000000000, 0.8660254037844387076, 1.000000000000000000, 0.8660254037844387076, 1.000000000000000000, 0.8660254037844387076, 1.000000000000000000, 0.8660254037844387076, 1.000000000000000000, 0.8660254037844387076, 1.000000000000000000, 0.8660254037844387076, 1.000000000000000000, 0.8660254037844387076, 1.000000000000000000, 0.8660254037844387076, 1.000000000000000000, 0.8660254037844387076, 1.000000000000000000, 0.8660254037844387076, 1.000000000000000000, 0.8660254037844387076, 1.000000000000000000, 0.8660254037844387076, 1.000000000000000000, 0.8660254037844387076, 1.000000000000000000, 0.8660254037844387076, 1.000000000000000000, 0.8660254037844387076, 1.000000000000000000, 0.8660254037844387076, 1.000000000000000000, 0.8660254037844387076, 1.000000000000000000, 0.8660254037844387076, 1.000000000000000000, 0.8660254037844387076, 1.000000000000000000, 0.8660254037844387076, 1.000000000000000000, 0.8660254037844387076, 1.000000000000000000, 0.8660254037844387076, 1.000000000000000000, 0.8660254037844387076, 1.000000000000000000, 0.8660254037844387076, 1.000000000000000000, 0.8660254037844387076, 1.000000000000000000, 0.8660254037844387076, 1.000000000000000000, 0.8660254037844387076, 1.000000000000000000, 0.8660254037844387076, 1.000000000000000000, 0.8660254037844387076, 1.000000000000000000, 0.8660254037844387076, 1.000000000000000000, 0.8660254037844387076, 1.000000000000000000, 0.8660254037844387076, 1.000000000000000000, 0.8660254037844387076, 1.000000000000000000, 0.8660254037844387076, 1.000000000000000000, 0.8660254037844387076, 1.000000000000000000, 0.8660254037844387076, 1.000000000000000000, 0.8660254037844387076, 1.000000000000000000, 0.8660254037844387076, 1.000000000000000000, 0.8660254037844387076, 1.000000000000000000, 0.8660254037844387076, 1.000000000000000000, 0.8660254037844387076, 1.000000000000000000, 0.8660254037844387076, 1.000000000000000000, 0.8660254037844387076, 1.000000000000000000, 0.8660254037844387076, 1.000000000000000000, 0.8660254037844387076, 1.000000000000000000, 0.8660254037844387076, 1.000000000000000000, 0.8660254037844387076, 1.000000000000000000, 0.8660254037844387076, 1.000000000000000000, 0.8660254037844387076, 1.000000000000000000, 0.8660254037844387076, 1.000000000000000000, 0.8660254037844387076, 1.000000000000000000, 0.8660254037844387076, 1.000000000000000000, 0.8660254037844387076, 1.000000000000000000, 0.8660254037844387076, 1.000000000000000000, 0.8660254037844387076, 1.000000000000000000, 0.8660254037844387076, 1.000000000000000000, 0.8660254037844387076, 1.000000000000000000, 0.8660254037844387076, 1.000000000000000000, 0.8660254037844387076, 1.000000000000000000, 0.8660254037844387076, 1.000000000000000000, 0.8660254037844387076, 1.000000000000000000, 0.8660254037844387076, 1.000000000000000000, 0.8660254037844387076, 1.000000000000000000, 0.8660254037844387076, 1.000000000000000000, 0.8660254037844387076, 1.000000000000000000, 0.8660254037844387076, 1.000000000000000000, 0.8660254037844387076, 1.000000000000000000, 0.8660254037844387076, 1.000000000000000000, 0.8660254037844387076, 1.000000000000000000, 0.8660254037844387076, 1.000000000000000000, 0.8660254037844387076, 1.000000000000000000, 0.8660254037844387076, 1.000000000000000000, 0.8660254037844387076, 1.000000000000000000, 0.8660254037844387076, 1.000000000000000000, 0.8660254037844387076, 1.000000000000000000, 0.8660254037844387076, 1.000000000000000000, 0.8660254037844387076, 1.000000000000000000, 0.8660254037844387076, 1.000000000000000000, 0.8660254037844387076, 1.000000000000000000, 0.8660254037844387076, 1.000000000000000000, 0.8660254037844387076, 1.000000000000000000, 0.8660254037844387076, 1.000000000000000000, 0.8660254037844387076, 1.000000000000000000, 0.8660254037844387076, 1.000000000000000000, 0.8660254037844387076, 1.000000000000000000, 0.8660254037844387076, 1.000000000000000000, 0.8660254037844387076, 1.000000000000000000, 0.8660254037844387076, 1.000000000000000000, 0.8660254037844387076, 1.000000000000000000, 0.8660254037844387076, 1.000000000000000000, 0.8660254037844387076, 1.000000000000000000, 0.8660254037844387076, 1.000000000000000000, 0.8660254037844387076, 1.000000000000000000, 0.8660254037844387076, 1.000000000000000000, 0.8660254037844387076, 1.000000000000000000, 0.8660254037844387076, 1.000000000000000000, 0.8660254037844387076, 1.000000000000000000, 0.8660254037844387076, 1.000000000000000000, 0.8660254037844387076, 1.000000000000000000, 0.8660254037844387076, 1.000000000000000000, 0.8660254037844387076, 1.000000000000000000, 0.8660254037844387076, 1.000000000000000000, 0.8660254037844387076, 1.000000000000000000, 0.8660254037844387076, 1.000000000000000000, 0.8660254037844387076, 1.000000000000000000, 0.8660254037844387076, 1.000000000000000000, 0.8660254037844387076, 1.000000000000000000, 0.8660254037844387076, 1.000000000000000000, 0.8660254037844387076, 1.000000000000000000, 0.8660254037844387076, 1.000000000000000000, 0.8660254037844387076, 1.000000000000000000, 0.8660254037844387076, 1.000000000000000000, 0.8660254037844387076, 1.000000000000000000, 0.8660254037844387076, 1.000000000000000000, 0.8660254037844387076, 1.000000000000000000, 0.8660254037844387076, 1.000000000000000000, 0.8660254037844387076, 1.000000000000000000, 0.8660254037844387076, 1.000000000000000000, 0.8660254037844387076, 1.000000000000000000, 0.8660254037844387076, 1.000000000000000000, 0.8660254037844387076, 1.000000000000000000, 0.8660254037844387076, 1.000000000000000000, 0.8660254037844387076, 1.000000000000000000, 0.8660254037844387076, 1.000000000000000000, 0.8660254037844387076, 1.000000000000000000, 0.8660254037844387076, 1.000000000000000000, 0.8660254037844387076, 1.000000000000000000, 0.8660254037844387076, 1.000000000000000000, 0.8660254037844387076, 1.000000000000000000, 0.8660254037844387076, 1.000000000000000000, 0.8660254037844387076, 1.000000000000000000, 0.8660254037844387076, 1.000000000000000000, 0.8660254037844387076, 1.000000000000000000, 0.8660254037844387076, 1.000000000000000000, 0.8660254037844387076, 1.000000000000000000, 0.8660254037844387076, 1.000000000000000000, 0.8660254037844387076, 1.000000000000000000, 0.8660254037844387076, 1.000000000000000000, 0.8660254037844387076, 1.000000000000000000, 0.8660254037844387076, 1.000000000000000000, 0.8660254037844387076, 1.000000000000000000, 0.8660254037844387076, 1.000000000000000000, 0.8660254037844387076, 1.000000000000000000, 0.8660254037844387076, 1.000000000000000000, 0.8660254037844387076, 1.000000000000000000, 0.8660254037844387076, 1.000000000000000000, 0.8660254037844387076, 1.000000000000000000, 0.8660254037844387076, 1.000000000000000000, 0.8660254037844387076, 1.000000000000000000, 0.8660254037844387076, 1.000000000000000000, 0.8660254037844387076, 1.000000000000000000, 0.8660254037844387076, 1.000000000000000000, 0.8660254037844387076, 1.000000000000000000, 0.8660254037844387076, 1.000000000000000000, 0.8660254037844387076, 1.000000000000000000, 0.8660254037844387076, 1.000000000000000000, 0.8660254037844387076, 1.000000000000000000, 0.8660254037844387076, 1.000000000000000000, 0.8660254037844387076, 1.000000000000000000, 0.8660254037844387076, 1.000000000000000000, 0.8660254037844387076, 1.000000000000000000, 0.8660254037844387076, 1.000000000000000000, 0.8660254037844387076, 1.000000000000000000, 0.8660254037844387076, 1.000000000000000000, 0.8660254037844387076, 1.000000000000000000, 0.8660254037844387076, 1.000000000000000000, 0.8660254037844387076, 1.000000000000000000, 0.8660254037844387076, 1.000000000000000000, 0.8660254037844387076, 1.000000000000000000, 0.8660254037844387076, 1.000000000000000000, 0.8660254037844387076, 1.000000000000000000, 0.8660254037844387076, 1.000000000000000000, 0.8660254037844387076, 1.000000000000000000, 0.8660254037844387076, 1.000000000000000000, 0.8660254037844387076, 1.000000000000000000, 0.8660254037844387076, 1.000000000000000000, 0.8660254037844387076, 1.000000000000000000, 0.8660254037844387076, 1.000000000000000000, 0.8660254037844387076, 1.000000000000000000, 0.8660254037844387076, 1.000000000000000000, 0.8660254037844387076, 1.000000000000000000, 0.8660254037844387076, 1.000000000000000000, 0.8660254037844387076, 1.000000000000000000, 0.8660254037844387076, 1.000000000000000000, 0.8660254037844387076, 1.000000000000000000, 0.8660254037844387076, 1.000000000000000000, 0.8660254037844387076, 1.000000000000000000, 0.8660254037844387076, 1.000000000000000000, 0.8660254037844387076, 1.000000000000000000, 0.8660254037844387076, 1.000000000000000000, 0.8660254037844387076, 1.000000000000000000, 0.8660254037844387076, 1.000000000000000000, 0.8660254037844387076, 1.000000000000000000, 0.8660254037844387076, 1.000000000000000000, 0.8660254037844387076, 1.000000000000000000, 0.8660254037844387076, 1.000000000000000000, 0.8660254037844387076, 1.000000000000000000, 0.8660254037844387076, 1.000000000000000000, 0.8660254037844387076, 1.000000000000000000, 0.8660254037844387076, 1.000000000000000000, 0.8660254037844387076, 1.000000000000000000, 0.8660254037844387076, 1.000000000000000000, 0.8660254037844387076, 1.000000000000000000, 0.8660254037844387076, 1.000000000000000000, 0.8660254037844387076, 1.000000000000000000, 0.8660254037844387076, 1.000000000000000000, 0.8660254037844387076, 1.000000000000000000, 0.8660254037844387076, 1.000000000000000000, 0.8660254037844387076, 1.000000000000000000, 0.8660254037844387076, 1.000000000000000000, 0.8660254037844387076, 1.000000000000000000, 0.8660254037844387076, 1.000000000000000000, 0.8660254037844387076, 1.000000000000000000, 0.8660254037844387076, 1.000000000000000000, 0.8660254037844387076, 1.000000000000000000, 0.8660254037844387076, 1.000000000000000000, 0.8660254037844387076, 1.000000000000000000, 0.8660254037844387076, 1.000000000000000000, 0.8660254037844387076, 1.000000000000000000, 0.8660254037844387076, 1.000000000000000000, 0.8660254037844387076, 1.000000000000000000, 0.8660254037844387076, 1.000000000000000000, 0.8660254037844387076, 1.000000000000000000, 0.8660254037844387076, 1.000000000000000000, 0.8660254037844387076, 1.000000000000000000, 0.8660254037844387076, 1.000000000000000000, 0.8660254037844387076, 1.000000000000000000, 0.8660254037844387076, 1.000000000000000000, 0.8660254037844387076, 1.000000000000000000, 0.8660254037844387076, 1.000000000000000000, 0.8660254037844387076, 1.000000000000000000, 0.8660254037844387076, 1.000000000000000000, 0.8660254037844387076, 1.000000000000000000, 0.8660254037844387076, 1.000000000000000000, 0.8660254037844387076, 1.000000000000000000, 0.8660254037844387076, 1.000000000000000000, 0.8660254037844387076, 1.000000000000000000, 0.8660254037844387076, 1.000000000000000000, 0.8660254037844387076, 1.000000000000000000, 0.8660254037844387076, 1.000000000000000000, 0.8660254037844387076, 1.000000000000000000, 0.8660254037844387076, 1.000000000000000000, 0.8660254037844387076, 1.000000000000000000, 0.8660254037844387076, 1.000000000000000000, 0.8660254037844387076, 1.000000000000000000, 0.8660254037844387076, 1.000000000000000000, 0.8660254037844387076, 1.000000000000000000, 0.8660254037844387076, 1.000000000000000000, 0.8660254037844387076, 1.000000000000000000, 0.8660254037844387076, 1.000000000000000000, 0.8660254037844387076, 1.000000000000000000, 0.8660254037844387076, 1.000000000000000000, 0.8660254037844387076, 1.000000000000000000, 0.8660254037844387076, 1.000000000000000000, 0.8660254037844387076, 1.000000000000000000, 0.8660254037844387076, 1.000000000000000000, 0.8660254037844387076, 1.000000000000000000, 0.8660254037844387076, 1.000000000000000000, 0.8660254037844387076, 1.000000000000000000, 0.8660254037844387076, 1.000000000000000000, 0.8660254037844387076, 1.000000000000000000, 0.8660254037844387076, 1.000000000000000000, 0.8660254037844387076, 1.000000000000000000, 0.8660254037844387076, 1.000000000000000000, 0.8660254037844387076, 1.000000000000000000, 0.8660254037844387076, 1.000000000000000000, 0.8660254037844387076, 1.000000000000000000, 0.8660254037844387076, 1.000000000000000000, 0.8660254037844387076, 1.000000000000000000, 0.8660254037844387076, 1.000000000000000000, 0.8660254037844387076, 1.000000000000000000, 0.8660254037844387076, 1.000000000000000000, 0.8660254037844387076, 1.000000000000000000, 0.8660254037844387076, 1.000000000000000000, 0.8660254037844387076, 1.000000000000000000, 0.8660254037844387076, 1.000000000000000000, 0.8660254037844387076, 1.000000000000000000, 0.8660254037844387076, 1.000000000000000000, 0.8660254037844387076, 1.000000000000000000, 0.8660254037844387076, 1.000000000000000000, 0.8660254037844387076, 1.000000000000000000, 0.8660254037844387076, 1.000000000000000000, 0.8660254037844387076, 1.000000000000000000, 0.8660254037844387076, 1.000000000000000000, 0.8660254037844387076, 1.000000000000000000, 0.8660254037844387076, 1.000000000000000000, 0.8660254037844387076, 1.000000000000000000, 0.8660254037844387076, 1.000000000000000000, 0.8660254037844387076, 1.000000000000000000, 0.8660254037844387076, 1.000000000000000000, 0.8660254037844387076, 1.000000000000000000, 0.8660254037844387076, 1.000000000000000000, 0.8660254037844387076, 1.000000000000000000, 0.8660254037844387076, 1.000000000000000000, 0.8660254037844387076, 1.000000000000000000, 0.8660254037844387076, 1.000000000000000000, 0.8660254037844387076, 1.000000000000000000, 0.8660254037844387076, 1.000000000000000000, 0.8660254037844387076, 1.000000000000000000, 0.8660254037844387076, 1.000000000000000000, 0.8660254037844387076, 1.000000000000000000, 0.8660254037844387076, 1.000000000000000000, 0.8660254037844387076, 1.000000000000000000, 0.8660254037844387076, 1.000000000000000000, 0.8660254037844387076, 1.000000000000000000, 0.8660254037844387076, 1.000000000000000000, 0.8660254037844387076, 1.000000000000000000, 0.8660254037844387076, 1.000000000000000000, 0.8660254037844387076, 1.000000000000000000, 0.8660254037844387076, 1.000000000000000000, 0.8660254037844387076, 1.000000000000000000, 0.8660254037844387076, 1.000000000000000000, 0.8660254037844387076, 1.000000000000000000, 0.8660254037844387076, 1.000000000000000000, 0.8660254037844387076, 1.000000000000000000, 0.8660254037844387076, 1.000000000000000000, 0.8660254037844387076, 1.000000000000000000, 0.8660254037844387076, 1.000000000000000000, 0.8660254037844387076, 1.000000000000000000, 0.8660254037844387076, 1.000000000000000000, 0.8660254037844387076, 1.000000000000000000, 0.8660254037844387076, 1.000000000000000000, 0.8660254037844387076, 1.000000000000000000, 0.8660254037844387076, 1.000000000000000000, 0.8660254037844387076, 1.000000000000000000, 0.8660254037844387076, 1.000000000000000000, 0.8660254037844387076, 1.000000000000000000, 0.8660254037844387076, 1.000000000000000000, 0.8660254037844387076, 1.000000000000000000, 0.8660254037844387076, 1.000000000000000000, 0.8660254037844387076, 1.000000000000000000, 0.8660254037844387076, 1.000000000000000000, 0.8660254037844387076, 1.000000000000000000, 0.8660254037844387076, 1.000000000000000000, 0.8660254037844387076, 1.000000000000000000, 0.8660254037844387076, 1.000000000000000000, 0.8660254037844387076, 1.000000000000000000, 0.8660254037844387076, 1.000000000000000000, 0.8660254037844387076, 1.000000000000000000, 0.8660254037844387076, 1.000000000000000000, 0.8660254037844387076, 1.000000000000000000, 0.8660254037844387076, 1.000000000000000000, 0.8660254037844387076, 1.000000000000000000, 0.8660254037844387076, 1.000000000000000000, 0.8660254037844387076, 1.000000000000000000, 0.8660254037844387076, 1.000000000000000000, 0.8660254037844387076, 1.000000000000000000, 0.8660254037844387076, 1.000000000000000000, 0.8660254037844387076, 1.000000000000000000, 0.8660254037844387076, 1.000000000000000000, 0.8660254037844387076, 1.000000000000000000, 0.8660254037844387076, 1.000000000000000000, 0.8660254037844387076, 1.000000000000000000, 0.8660254037844387076, 1.000000000000000000, 0.8660254037844387076, 1.000000000000000000, 0.8660254037844387076, 1.000000000000000000, 0.8660254037844387076, 1.000000000000000000, 0.8660254037844387076, 1.000000000000000000, 0.8660254037844387076, 1.000000000000000000, 0.8660254037844387076, 1.000000000000000000, 0.8660254037844387076, 1.000000000000000000, 0.8660254037844387076, 1.000000000000000000, 0.8660254037844387076, 1.000000000000000000, 0.8660254037844387076, 1.000000000000000000, 0.8660254037844387076, 1.000000000000000000, 0.8660254037844387076, 1.000000000000000000, 0.8660254037844387076, 1.000000000000000000, 0.8660254037844387076, 1.000000000000000000, 0.8660254037844387076, 1.000000000000000000, 0.8660254037844387076, 1.000000000000000000, 0.8660254037844387076, 1.000000000000000000, 0.8660254037844387076, 1.000000000000000000, 0.8660254037844387076, 1.000000000000000000, 0.8660254037844387076, 1.000000000000000000, 0.8660254037844387076, 1.000000000000000000, 0.8660254037844387076, 1.000000000000000000, 0.8660254037844387076, 1.000000000000000000, 0.8660254037844387076, 1.000000000000000000, 0.8660254037844387076, 1.000000000000000000, 0.8660254037844387076, 1.000000000000000000),
 ( 1.000000000000000000, 0.8660254037844387076, 1.000000000000000000, 0.8660254037844387076, 1.000000000000000000, 0.8660254037844387076, 1.000000000000000000, 0.8660254037844387076, 1.000000000000000000, 0.8660254037844387076, 1.000000000000000000, 0.8660254037844387076, 1.000000000000000000, 0.8660254037844387076, 1.000000000000000000, 0.8660254037844387076, 1.000000000000000000, 0.8660254037844387076, 1.000000000000000000, 0.8660254037844387076, 1.000000000000000000, 0.8660254037844387076, 1.000000000000000000, 0.8660254037844387076, 1.000000000000000000, 0.8660254037844387076, 1.000000000000000000, 0.8660254037844387076, 1.000000000000000000, 0.8660254037844387076, 1.000000000000000000, 0.8660254037844387076, 1.000000000000000000, 0.8660254037844387076, 1.000000000000000000, 0.8660254037844387076, 1.000000000000000000, 0.8660254037844387076, 1.000000000000000000, 0.8660254037844387076, 1.000000000000000000, 0.8660254037844387076, 1.000000000000000000, 0.8660254037844387076, 1.000000000000000000, 0.8660254037844387076, 1.000000000000000000, 0.8660254037844387076, 1.000000000000000000, 0.8660254037844387076, 1.000000000000000000, 0.8660254037844387076, 1.000000000000000000, 0.8660254037844387076, 1.000000000000000000, 0.8660254037844387076, 1.000000000000000000, 0.8660254037844387076, 1.000000000000000000, 0.8660254037844387076, 1.000000000000000000, 0.8660254037844387076, 1.000000000000000000, 0.8660254037844387076, 1.000000000000000000, 0.8660254037844387076, 1.000000000000000000, 0.8660254037844387076, 1.000000000000000000, 0.8660254037844387076, 1.000000000000000000, 0.8660254037844387076, 1.000000000000000000, 0.8660254037844387076, 1.000000000000000000, 0.8660254037844387076, 1.000000000000000000, 0.8660254037844387076, 1.000000000000000000, 0.8660254037844387076, 1.000000000000000000, 0.8660254037844387076, 1.000000000000000000, 0.8660254037844387076, 1.000000000000000000, 0.8660254037844387076, 1.000000000000000000, 0.8660254037844387076, 1.000000000000000000, 0.8660254037844387076, 1.000000000000000000, 0.8660254037844387076, 1.000000000000000000, 0.8660254037844387076, 1.000000000000000000, 0.8660254037844387076, 1.000000000000000000, 0.8660254037844387076, 1.000000000000000000, 0.8660254037844387076, 1.000000000000000000, 0.8660254037844387076, 1.000000000000000000, 0.8660254037844387076, 1.000000000000000000, 0.8660254037844387076, 1.000000000000000000, 0.8660254037844387076, 1.000000000000000000, 0.8660254037844387076, 1.000000000000000000, 0.8660254037844387076, 1.000000000000000000, 0.8660254037844387076, 1.000000000000000000, 0.8660254037844387076, 1.000000000000000000, 0.8660254037844387076, 1.000000000000000000, 0.8660254037844387076, 1.000000000000000000, 0.8660254037844387076, 1.000000000000000000, 0.8660254037844387076, 1.000000000000000000, 0.8660254037844387076, 1.000000000000000000, 0.8660254037844387076, 1.000000000000000000, 0.8660254037844387076, 1.000000000000000000, 0.8660254037844387076, 1.000000000000000000, 0.8660254037844387076, 1.000000000000000000, 0.8660254037844387076, 1.000000000000000000, 0.8660254037844387076, 1.000000000000000000, 0.8660254037844387076, 1.000000000000000000, 0.8660254037844387076, 1.000000000000000000, 0.8660254037844387076, 1.000000000000000000, 0.8660254037844387076, 1.000000000000000000, 0.8660254037844387076, 1.000000000000000000, 0.8660254037844387076, 1.000000000000000000, 0.8660254037844387076, 1.000000000000000000, 0.8660254037844387076, 1.000000000000000000, 0.8660254037844387076, 1.000000000000000000, 0.8660254037844387076, 1.000000000000000000, 0.8660254037844387076, 1.000000000000000000, 0.8660254037844387076, 1.000000000000000000, 0.8660254037844387076, 1.000000000000000000, 0.8660254037844387076, 1.000000000000000000, 0.8660254037844387076, 1.000000000000000000, 0.8660254037844387076, 1.000000000000000000, 0.8660254037844387076, 1.000000000000000000, 0.8660254037844387076, 1.000000000000000000, 0.8660254037844387076, 1.000000000000000000, 0.8660254037844387076, 1.000000000000000000, 0.8660254037844387076, 1.000000000000000000, 0.8660254037844387076, 1.000000000000000000, 0.8660254037844387076, 1.000000000000000000, 0.8660254037844387076, 1.000000000000000000, 0.8660254037844387076, 1.000000000000000000, 0.8660254037844387076, 1.000000000000000000, 0.8660254037844387076, 1.000000000000000000, 0.8660254037844387076, 1.000000000000000000, 0.8660254037844387076, 1.000000000000000000, 0.8660254037844387076, 1.000000000000000000, 0.8660254037844387076, 1.000000000000000000, 0.8660254037844387076, 1.000000000000000000, 0.8660254037844387076, 1.000000000000000000, 0.8660254037844387076, 1.000000000000000000, 0.8660254037844387076, 1.000000000000000000, 0.8660254037844387076, 1.000000000000000000, 0.8660254037844387076, 1.000000000000000000, 0.8660254037844387076, 1.000000000000000000, 0.8660254037844387076, 1.000000000000000000, 0.8660254037844387076, 1.000000000000000000, 0.8660254037844387076, 1.000000000000000000, 0.8660254037844387076, 1.000000000000000000, 0.8660254037844387076, 1.000000000000000000, 0.8660254037844387076, 1.000000000000000000, 0.8660254037844387076, 1.000000000000000000, 0.8660254037844387076, 1.000000000000000000, 0.8660254037844387076, 1.000000000000000000, 0.8660254037844387076, 1.000000000000000000, 0.8660254037844387076, 1.000000000000000000, 0.8660254037844387076, 1.000000000000000000, 0.8660254037844387076, 1.000000000000000000, 0.8660254037844387076, 1.000000000000000000, 0.8660254037844387076, 1.000000000000000000, 0.8660254037844387076, 1.000000000000000000, 0.8660254037844387076, 1.000000000000000000, 0.8660254037844387076, 1.000000000000000000, 0.8660254037844387076, 1.000000000000000000, 0.8660254037844387076, 1.000000000000000000, 0.8660254037844387076, 1.000000000000000000, 0.8660254037844387076, 1.000000000000000000, 0.8660254037844387076, 1.000000000000000000, 0.8660254037844387076, 1.000000000000000000, 0.8660254037844387076, 1.000000000000000000, 0.8660254037844387076, 1.000000000000000000, 0.8660254037844387076, 1.000000000000000000, 0.8660254037844387076, 1.000000000000000000, 0.8660254037844387076, 1.000000000000000000, 0.8660254037844387076, 1.000000000000000000, 0.8660254037844387076, 1.000000000000000000, 0.8660254037844387076, 1.000000000000000000, 0.8660254037844387076, 1.000000000000000000, 0.8660254037844387076, 1.000000000000000000, 0.8660254037844387076, 1.000000000000000000, 0.8660254037844387076, 1.000000000000000000, 0.8660254037844387076, 1.000000000000000000, 0.8660254037844387076, 1.000000000000000000, 0.8660254037844387076, 1.000000000000000000, 0.8660254037844387076, 1.000000000000000000, 0.8660254037844387076, 1.000000000000000000, 0.8660254037844387076, 1.000000000000000000, 0.8660254037844387076, 1.000000000000000000, 0.8660254037844387076, 1.000000000000000000, 0.8660254037844387076, 1.000000000000000000, 0.8660254037844387076, 1.000000000000000000, 0.8660254037844387076, 1.000000000000000000, 0.8660254037844387076, 1.000000000000000000, 0.8660254037844387076, 1.000000000000000000, 0.8660254037844387076, 1.000000000000000000, 0.8660254037844387076, 1.000000000000000000, 0.8660254037844387076, 1.000000000000000000, 0.8660254037844387076, 1.000000000000000000, 0.8660254037844387076, 1.000000000000000000, 0.8660254037844387076, 1.000000000000000000, 0.8660254037844387076, 1.000000000000000000, 0.8660254037844387076, 1.000000000000000000, 0.8660254037844387076, 1.000000000000000000, 0.8660254037844387076, 1.000000000000000000, 0.8660254037844387076, 1.000000000000000000, 0.8660254037844387076, 1.000000000000000000, 0.8660254037844387076, 1.000000000000000000, 0.8660254037844387076, 1.000000000000000000, 0.8660254037844387076, 1.000000000000000000, 0.8660254037844387076, 1.000000000000000000, 0.8660254037844387076, 1.000000000000000000, 0.8660254037844387076, 1.000000000000000000, 0.8660254037844387076, 1.000000000000000000, 0.8660254037844387076, 1.000000000000000000, 0.8660254037844387076, 1.000000000000000000, 0.8660254037844387076, 1.000000000000000000, 0.8660254037844387076, 1.000000000000000000, 0.8660254037844387076, 1.000000000000000000, 0.8660254037844387076, 1.000000000000000000, 0.8660254037844387076, 1.000000000000000000, 0.8660254037844387076, 1.000000000000000000, 0.8660254037844387076, 1.000000000000000000, 0.8660254037844387076, 1.000000000000000000, 0.8660254037844387076, 1.000000000000000000, 0.8660254037844387076, 1.000000000000000000, 0.8660254037844387076, 1.000000000000000000, 0.8660254037844387076, 1.000000000000000000, 0.8660254037844387076, 1.000000000000000000, 0.8660254037844387076, 1.000000000000000000, 0.8660254037844387076, 1.000000000000000000, 0.8660254037844387076, 1.000000000000000000, 0.8660254037844387076, 1.000000000000000000, 0.8660254037844387076, 1.000000000000000000, 0.8660254037844387076, 1.000000000000000000, 0.8660254037844387076, 1.000000000000000000, 0.8660254037844387076, 1.000000000000000000, 0.8660254037844387076, 1.000000000000000000, 0.8660254037844387076, 1.000000000000000000, 0.8660254037844387076, 1.000000000000000000, 0.8660254037844387076, 1.000000000000000000, 0.8660254037844387076, 1.000000000000000000, 0.8660254037844387076, 1.000000000000000000, 0.8660254037844387076, 1.000000000000000000, 0.8660254037844387076, 1.000000000000000000, 0.8660254037844387076, 1.000000000000000000, 0.8660254037844387076, 1.000000000000000000, 0.8660254037844387076, 1.000000000000000000, 0.8660254037844387076, 1.000000000000000000, 0.8660254037844387076, 1.000000000000000000, 0.8660254037844387076, 1.000000000000000000, 0.8660254037844387076, 1.000000000000000000, 0.8660254037844387076, 1.000000000000000000, 0.8660254037844387076, 1.000000000000000000, 0.8660254037844387076, 1.000000000000000000, 0.8660254037844387076, 1.000000000000000000, 0.8660254037844387076, 1.000000000000000000, 0.8660254037844387076, 1.000000000000000000, 0.8660254037844387076, 1.000000000000000000, 0.8660254037844387076, 1.000000000000000000, 0.8660254037844387076, 1.000000000000000000, 0.8660254037844387076, 1.000000000000000000, 0.8660254037844387076, 1.000000000000000000, 0.8660254037844387076, 1.000000000000000000, 0.8660254037844387076, 1.000000000000000000, 0.8660254037844387076, 1.000000000000000000, 0.8660254037844387076, 1.000000000000000000, 0.8660254037844387076, 1.000000000000000000, 0.8660254037844387076, 1.000000000000000000, 0.8660254037844387076, 1.000000000000000000, 0.8660254037844387076, 1.000000000000000000, 0.8660254037844387076, 1.000000000000000000, 0.8660254037844387076, 1.000000000000000000, 0.8660254037844387076, 1.000000000000000000, 0.8660254037844387076, 1.000000000000000000, 0.8660254037844387076, 1.000000000000000000, 0.8660254037844387076, 1.000000000000000000, 0.8660254037844387076, 1.000000000000000000, 0.8660254037844387076, 1.000000000000000000, 0.8660254037844387076, 1.000000000000000000, 0.8660254037844387076, 1.000000000000000000, 0.8660254037844387076, 1.000000000000000000, 0.8660254037844387076, 1.000000000000000000, 0.8660254037844387076, 1.000000000000000000, 0.8660254037844387076, 1.000000000000000000, 0.8660254037844387076, 1.000000000000000000, 0.8660254037844387076, 1.000000000000000000, 0.8660254037844387076, 1.000000000000000000, 0.8660254037844387076, 1.000000000000000000, 0.8660254037844387076, 1.000000000000000000, 0.8660254037844387076, 1.000000000000000000, 0.8660254037844387076, 1.000000000000000000, 0.8660254037844387076, 1.000000000000000000, 0.8660254037844387076, 1.000000000000000000, 0.8660254037844387076, 1.000000000000000000, 0.8660254037844387076, 1.000000000000000000, 0.8660254037844387076, 1.000000000000000000, 0.8660254037844387076, 1.000000000000000000, 0.8660254037844387076, 1.000000000000000000, 0.8660254037844387076, 1.000000000000000000, 0.8660254037844387076, 1.000000000000000000, 0.8660254037844387076, 1.000000000000000000, 0.8660254037844387076, 1.000000000000000000, 0.8660254037844387076, 1.000000000000000000, 0.8660254037844387076, 1.000000000000000000, 0.8660254037844387076, 1.000000000000000000, 0.8660254037844387076, 1.000000000000000000, 0.8660254037844387076, 1.000000000000000000, 0.8660254037844387076, 1.000000000000000000, 0.8660254037844387076, 1.000000000000000000, 0.8660254037844387076, 1.000000000000000000, 0.8660254037844387076, 1.000000000000000000, 0.8660254037844387076, 1.000000000000000000, 0.8660254037844387076, 1.000000000000000000, 0.8660254037844387076, 1.000000000000000000, 0.8660254037844387076, 1.000000000000000000, 0.8660254037844387076, 1.000000000000000000, 0.8660254037844387076, 1.000000000000000000, 0.8660254037844387076, 1.000000000000000000, 0.8660254037844387076, 1.000000000000000000, 0.8660254037844387076, 1.000000000000000000, 0.8660254037844387076, 1.000000000000000000, 0.8660254037844387076, 1.000000000000000000, 0.8660254037844387076, 1.000000000000000000, 0.8660254037844387076, 1.000000000000000000, 0.8660254037844387076, 1.000000000000000000, 0.8660254037844387076, 1.000000000000000000, 0.8660254037844387076, 1.000000000000000000, 0.8660254037844387076, 1.000000000000000000, 0.8660254037844387076, 1.000000000000000000, 0.8660254037844387076, 1.000000000000000000, 0.8660254037844387076, 1.000000000000000000, 0.8660254037844387076, 1.000000000000000000, 0.8660254037844387076, 1.000000000000000000, 0.8660254037844387076, 1.000000000000000000, 0.8660254037844387076, 1.000000000000000000, 0.8660254037844387076, 1.000000000000000000, 0.8660254037844387076, 1.000000000000000000, 0.8660254037844387076, 1.000000000000000000, 0.8660254037844387076, 1.000000000000000000, 0.8660254037844387076, 1.000000000000000000, 0.8660254037844387076, 1.000000000000000000, 0.8660254037844387076, 1.000000000000000000, 0.8660254037844387076, 1.000000000000000000, 0.8660254037844387076, 1.000000000000000000, 0.8660254037844387076, 1.000000000000000000, 0.8660254037844387076, 1.000000000000000000, 0.8660254037844387076, 1.000000000000000000, 0.8660254037844387076, 1.000000000000000000, 0.8660254037844387076, 1.000000000000000000, 0.8660254037844387076, 1.000000000000000000, 0.8660254037844387076, 1.000000000000000000, 0.8660254037844387076, 1.000000000000000000, 0.8660254037844387076, 1.000000000000000000, 0.8660254037844387076, 1.000000000000000000, 0.8660254037844387076, 1.000000000000000000, 0.8660254037844387076, 1.000000000000000000, 0.8660254037844387076, 1.000000000000000000, 0.8660254037844387076, 1.000000000000000000, 0.8660254037844387076, 1.000000000000000000, 0.8660254037844387076, 1.000000000000000000, 0.8660254037844387076, 1.000000000000000000, 0.8660254037844387076, 1.000000000000000000, 0.8660254037844387076, 1.000000000000000000, 0.8660254037844387076, 1.000000000000000000, 0.8660254037844387076, 1.000000000000000000, 0.8660254037844387076, 1.000000000000000000, 0.8660254037844387076, 1.000000000000000000, 0.8660254037844387076, 1.000000000000000000, 0.8660254037844387076, 1.000000000000000000, 0.8660254037844387076, 1.000000000000000000, 0.8660254037844387076, 1.000000000000000000, 0.8660254037844387076, 1.000000000000000000, 0.8660254037844387076, 1.000000000000000000, 0.8660254037844387076, 1.000000000000000000, 0.8660254037844387076, 1.000000000000000000, 0.8660254037844387076, 1.000000000000000000, 0.8660254037844387076, 1.000000000000000000, 0.8660254037844387076, 1.000000000000000000, 0.8660254037844387076, 1.000000000000000000, 0.8660254037844387076, 1.000000000000000000, 0.8660254037844387076, 1.000000000000000000, 0.8660254037844387076, 1.000000000000000000, 0.8660254037844387076, 1.000000000000000000, 0.8660254037844387076, 1.000000000000000000, 0.8660254037844387076, 1.000000000000000000, 0.8660254037844387076, 1.000000000000000000, 0.8660254037844387076, 1.000000000000000000, 0.8660254037844387076, 1.000000000000000000, 0.8660254037844387076, 1.000000000000000000, 0.8660254037844387076, 1.000000000000000000, 0.8660254037844387076, 1.000000000000000000, 0.8660254037844387076, 1.000000000000000000, 0.8660254037844387076, 1.000000000000000000, 0.8660254037844387076, 1.000000000000000000, 0.8660254037844387076, 1.000000000000000000, 0.8660254037844387076, 1.000000000000000000, 0.8660254037844387076, 1.000000000000000000, 0.8660254037844387076, 1.000000000000000000, 0.8660254037844387076, 1.000000000000000000, 0.8660254037844387076, 1.000000000000000000, 0.8660254037844387076, 1.000000000000000000, 0.8660254037844387076, 1.000000000000000000, 0.8660254037844387076, 1.000000000000000000, 0.8660254037844387076, 1.000000000000000000, 0.8660254037844387076, 1.000000000000000000, 0.8660254037844387076, 1.000000000000000000, 0.8660254037844387076, 1.000000000000000000, 0.8660254037844387076, 1.000000000000000000, 0.8660254037844387076, 1.000000000000000000, 0.8660254037844387076, 1.000000000000000000, 0.8660254037844387076, 1.000000000000000000, 0.8660254037844387076, 1.000000000000000000, 0.8660254037844387076, 1.000000000000000000, 0.8660254037844387076, 1.000000000000000000, 0.8660254037844387076, 1.000000000000000000, 0.8660254037844387076, 1.000000000000000000, 0.8660254037844387076, 1.000000000000000000, 0.8660254037844387076, 1.000000000000000000, 0.8660254037844387076, 1.000000000000000000, 0.8660254037844387076, 1.000000000000000000, 0.8660254037844387076, 1.000000000000000000, 0.8660254037844387076, 1.000000000000000000, 0.8660254037844387076, 1.000000000000000000, 0.8660254037844387076, 1.000000000000000000, 0.8660254037844387076, 1.000000000000000000, 0.8660254037844387076, 1.000000000000000000, 0.8660254037844387076, 1.000000000000000000, 0.8660254037844387076, 1.000000000000000000, 0.8660254037844387076, 1.000000000000000000, 0.8660254037844387076, 1.000000000000000000, 0.8660254037844387076, 1.000000000000000000, 0.8660254037844387076, 1.000000000000000000, 0.8660254037844387076, 1.000000000000000000, 0.8660254037844387076, 1.000000000000000000, 0.8660254037844387076, 1.000000000000000000, 0.8660254037844387076, 1.000000000000000000, 0.8660254037844387076, 1.000000000000000000, 0.8660254037844387076, 1.000000000000000000, 0.8660254037844387076, 1.000000000000000000, 0.8660254037844387076, 1.000000000000000000, 0.8660254037844387076, 1.000000000000000000, 0.8660254037844387076, 1.000000000000000000, 0.8660254037844387076, 1.000000000000000000, 0.8660254037844387076, 1.000000000000000000, 0.8660254037844387076, 1.000000000000000000, 0.8660254037844387076, 1.000000000000000000, 0.8660254037844387076, 1.000000000000000000, 0.8660254037844387076, 1.000000000000000000, 0.8660254037844387076, 1.000000000000000000, 0.8660254037844387076, 1.000000000000000000, 0.8660254037844387076, 1.000000000000000000, 0.8660254037844387076, 1.000000000000000000, 0.8660254037844387076, 1.000000000000000000, 0.8660254037844387076, 1.000000000000000000, 0.8660254037844387076, 1.000000000000000000, 0.8660254037844387076, 1.000000000000000000, 0.8660254037844387076, 1.000000000000000000, 0.8660254037844387076, 1.000000000000000000, 0.8660254037844387076, 1.000000000000000000, 0.8660254037844387076, 1.000000000000000000, 0.8660254037844387076, 1.000000000000000000, 0.8660254037844387076, 1.000000000000000000, 0.8660254037844387076, 1.000000000000000000, 0.8660254037844387076, 1.000000000000000000, 0.8660254037844387076, 1.000000000000000000, 0.8660254037844387076, 1.000000000000000000, 0.8660254037844387076, 1.000000000000000000, 0.8660254037844387076, 1.000000000000000000, 0.8660254037844387076, 1.000000000000000000, 0.8660254037844387076, 1.000000000000000000, 0.8660254037844387076, 1.000000000000000000, 0.8660254037844387076, 1.000000000000000000, 0.8660254037844387076, 1.000000000000000000, 0.8660254037844387076, 1.000000000000000000, 0.8660254037844387076, 1.000000000000000000, 0.8660254037844387076, 1.000000000000000000, 0.8660254037844387076, 1.000000000000000000, 0.8660254037844387076, 1.000000000000000000, 0.8660254037844387076, 1.000000000000000000, 0.8660254037844387076, 1.000000000000000000, 0.8660254037844387076, 1.000000000000000000, 0.8660254037844387076, 1.000000000000000000, 0.8660254037844387076, 1.000000000000000000, 0.8660254037844387076, 1.000000000000000000, 0.8660254037844387076, 1.000000000000000000, 0.8660254037844387076, 1.000000000000000000, 0.8660254037844387076, 1.000000000000000000, 0.8660254037844387076, 1.000000000000000000, 0.8660254037844387076, 1.000000000000000000, 0.8660254037844387076, 1.000000000000000000, 0.8660254037844387076, 1.000000000000000000, 0.8660254037844387076, 1.000000000000000000, 0.8660254037844387076, 1.000000000000000000, 0.8660254037844387076, 1.000000000000000000, 0.8660254037844387076, 1.000000000000000000, 0.8660254037844387076, 1.000000000000000000, 0.8660254037844387076, 1.000000000000000000, 0.8660254037844387076, 1.000000000000000000, 0.8660254037844387076, 1.000000000000000000, 0.8660254037844387076, 1.000000000000000000, 0.8660254037844387076, 1.000000000000000000, 0.8660254037844387076, 1.000000000000000000, 0.8660254037844387076, 1.000000000000000000, 0.8660254037844387076, 1.000000000000000000, 0.8660254037844387076, 1.000000000000000000, 0.8660254037844387076, 1.000000000000000000, 0.8660254037844387076, 1.000000000000000000, 0.8660254037844387076, 1.000000000000000000, 0.8660254037844387076, 1.000000000000000000, 0.8660254037844387076, 1.000000000000000000, 0.8660254037844387076, 1.000000000000000000, 0.8660254037844387076, 1.000000000000000000, 0.8660254037844387076, 1.000000000000000000, 0.8660254037844387076, 1.000000000000000000, 0.8660254037844387076, 1.000000000000000000, 0.8660254037844387076, 1.000000000000000000, 0.8660254037844387076, 1.000000000000000000, 0.8660254037844387076, 1.000000000000000000, 0.8660254037844387076, 1.000000000000000000, 0.8660254037844387076, 1.000000000000000000, 0.8660254037844387076, 1.000000000000000000, 0.8660254037844387076, 1.000000000000000000, 0.8660254037844387076, 1.000000000000000000, 0.8660254037844387076, 1.000000000000000000, 0.8660254037844387076, 1.000000000000000000, 0.8660254037844387076, 1.000000000000000000, 0.8660254037844387076, 1.000000000000000000, 0.8660254037844387076, 1.000000000000000000, 0.8660254037844387076, 1.000000000000000000, 0.8660254037844387076, 1.000000000000000000, 0.8660254037844387076, 1.000000000000000000, 0.8660254037844387076, 1.000000000000000000, 0.8660254037844387076, 1.000000000000000000, 0.8660254037844387076, 1.000000000000000000, 0.8660254037844387076, 1.000000000000000000, 0.8660254037844387076, 1.000000000000000000, 0.8660254037844387076, 1.000000000000000000, 0.8660254037844387076, 1.000000000000000000, 0.8660254037844387076, 1.000000000000000000, 0.8660254037844387076, 1.000000000000000000, 0.8660254037844387076, 1.000000000000000000, 0.8660254037844387076, 1.000000000000000000, 0.8660254037844387076, 1.000000000000000000, 0.8660254037844387076, 1.000000000000000000, 0.8660254037844387076, 1.000000000000000000, 0.8660254037844387076, 1.000000000000000000, 0.8660254037844387076, 1.000000000000000000, 0.8660254037844387076, 1.000000000000000000, 0.8660254037844387076, 1.000000000000000000, 0.8660254037844387076, 1.000000000000000000, 0.8660254037844387076, 1.000000000000000000, 0.8660254037844387076, 1.000000000000000000, 0.8660254037844387076, 1.000000000000000000, 0.8660254037844387076, 1.000000000000000000, 0.8660254037844387076, 1.000000000000000000, 0.8660254037844387076, 1.000000000000000000, 0.8660254037844387076, 1.000000000000000000, 0.8660254037844387076, 1.000000000000000000, 0.8660254037844387076, 1.000000000000000000, 0.8660254037844387076, 1.000000000000000000, 0.8660254037844387076, 1.000000000000000000, 0.8660254037844387076, 1.000000000000000000, 0.8660254037844387076, 1.000000000000000000, 0.8660254037844387076, 1.000000000000000000, 0.8660254037844387076, 1.000000000000000000, 0.8660254037844387076, 1.000000000000000000, 0.8660254037844387076, 1.000000000000000000, 0.8660254037844387076, 1.000000000000000000, 0.8660254037844387076, 1.000000000000000000, 0.8660254037844387076, 1.000000000000000000, 0.8660254037844387076, 1.000000000000000000, 0.8660254037844387076, 1.000000000000000000, 0.8660254037844387076, 1.000000000000000000, 0.8660254037844387076, 1.000000000000000000, 0.8660254037844387076, 1.000000000000000000, 0.8660254037844387076, 1.000000000000000000, 0.8660254037844387076, 1.000000000000000000, 0.8660254037844387076, 1.000000000000000000, 0.8660254037844387076, 1.000000000000000000, 0.8660254037844387076, 1.000000000000000000, 0.8660254037844387076, 1.000000000000000000, 0.8660254037844387076, 1.000000000000000000, 0.8660254037844387076, 1.000000000000000000, 0.8660254037844387076, 1.000000000000000000, 0.8660254037844387076, 1.000000000000000000, 0.8660254037844387076, 1.000000000000000000, 0.8660254037844387076, 1.000000000000000000, 0.8660254037844387076, 1.000000000000000000, 0.8660254037844387076, 1.000000000000000000, 0.8660254037844387076, 1.000000000000000000, 0.8660254037844387076, 1.000000000000000000, 0.8660254037844387076, 1.000000000000000000, 0.8660254037844387076, 1.000000000000000000, 0.8660254037844387076, 1.000000000000000000, 0.8660254037844387076, 1.000000000000000000, 0.8660254037844387076, 1.000000000000000000, 0.8660254037844387076, 1.000000000000000000, 0.8660254037844387076, 1.000000000000000000, 0.8660254037844387076, 1.000000000000000000, 0.8660254037844387076, 1.000000000000000000, 0.8660254037844387076, 1.000000000000000000, 0.8660254037844387076, 1.000000000000000000, 0.8660254037844387076, 1.000000000000000000, 0.8660254037844387076, 1.000000000000000000, 0.8660254037844387076, 1.000000000000000000, 0.8660254037844387076, 1.000000000000000000, 0.8660254037844387076, 1.000000000000000000, 0.8660254037844387076, 1.000000000000000000, 0.8660254037844387076, 1.000000000000000000, 0.8660254037844387076, 1.000000000000000000, 0.8660254037844387076, 1.000000000000000000, 0.8660254037844387076, 1.000000000000000000, 0.8660254037844387076, 1.000000000000000000, 0.8660254037844387076, 1.000000000000000000, 0.8660254037844387076, 1.000000000000000000, 0.8660254037844387076, 1.000000000000000000, 0.8660254037844387076, 1.000000000000000000, 0.8660254037844387076, 1.000000000000000000, 0.8660254037844387076, 1.000000000000000000, 0.8660254037844387076, 1.000000000000000000, 0.8660254037844387076, 1.000000000000000000, 0.8660254037844387076, 1.000000000000000000, 0.8660254037844387076, 1.000000000000000000, 0.8660254037844387076, 1.000000000000000000, 0.8660254037844387076, 1.000000000000000000, 0.8660254037844387076, 1.000000000000000000, 0.8660254037844387076, 1.000000000000000000, 0.8660254037844387076, 1.000000000000000000, 0.8660254037844387076, 1.000000000000000000, 0.8660254037844387076, 1.000000000000000000, 0.8660254037844387076, 1.000000000000000000, 0.8660254037844387076, 1.000000000000000000, 0.8660254037844387076, 1.000000000000000000, 0.8660254037844387076, 1.000000000000000000, 0.8660254037844387076, 1.000000000000000000, 0.8660254037844387076, 1.000000000000000000, 0.8660254037844387076, 1.000000000000000000, 0.8660254037844387076, 1.000000000000000000, 0.8660254037844387076, 1.000000000000000000, 0.8660254037844387076, 1.000000000000000000, 0.8660254037844387076, 1.000000000000000000, 0.8660254037844387076, 1.000000000000000000, 0.8660254037844387076, 1.000000000000000000, 0.8660254037844387076, 1.000000000000000000, 0.8660254037844387076, 1.000000000000000000, 0.8660254037844387076, 1.000000000000000000, 0.8660254037844387076, 1.000000000000000000, 0.8660254037844387076, 1.000000000000000000, 0.8660254037844387076, 1.000000000000000000, 0.8660254037844387076, 1.000000000000000000, 0.8660254037844387076, 1.000000000000000000, 0.8660254037844387076, 1.000000000000000000, 0.8660254037844387076, 1.000000000000000000, 0.8660254037844387076, 1.000000000000000000, 0.8660254037844387076, 1.000000000000000000, 0.8660254037844387076, 1.000000000000000000, 0.8660254037844387076, 1.000000000000000000, 0.8660254037844387076, 1.000000000000000000, 0.8660254037844387076, 1.000000000000000000, 0.8660254037844387076, 1.000000000000000000, 0.8660254037844387076, 1.000000000000000000, 0.8660254037844387076, 1.000000000000000000, 0.8660254037844387076, 1.000000000000000000, 0.8660254037844387076, 1.000000000000000000, 0.8660254037844387076, 1.000000000000000000, 0.8660254037844387076, 1.000000000000000000, 0.8660254037844387076, 1.000000000000000000, 0.8660254037844387076, 1.000000000000000000, 0.8660254037844387076, 1.000000000000000000, 0.8660254037844387076, 1.000000000000000000, 0.8660254037844387076, 1.000000000000000000, 0.8660254037844387076, 1.000000000000000000, 0.8660254037844387076, 1.000000000000000000, 0.8660254037844387076, 1.000000000000000000, 0.8660254037844387076, 1.000000000000000000, 0.8660254037844387076, 1.000000000000000000, 0.8660254037844387076, 1.000000000000000000, 0.8660254037844387076, 1.000000000000000000, 0.8660254037844387076, 1.000000000000000000, 0.8660254037844387076, 1.000000000000000000, 0.8660254037844387076, 1.000000000000000000, 0.8660254037844387076, 1.000000000000000000, 0.8660254037844387076, 1.000000000000000000, 0.8660254037844387076, 1.000000000000000000, 0.8660254037844387076, 1.000000000000000000, 0.8660254037844387076, 1.000000000000000000, 0.8660254037844387076, 1.000000000000000000, 0.8660254037844387076, 1.000000000000000000, 0.8660254037844387076, 1.000000000000000000, 0.8660254037844387076, 1.000000000000000000, 0.8660254037844387076, 1.000000000000000000, 0.8660254037844387076, 1.000000000000000000, 0.8660254037844387076, 1.000000000000000000, 0.8660254037844387076, 1.000000000000000000, 0.8660254037844387076, 1.000000000000000000, 0.8660254037844387076, 1.000000000000000000, 0.8660254037844387076, 1.000000000000000000, 0.8660254037844387076, 1.000000000000000000, 0.8660254037844387076, 1.000000000000000000, 0.8660254037844387076, 1.000000000000000000, 0.8660254037844387076, 1.000000000000000000, 0.8660254037844387076, 1.000000000000000000, 0.8660254037844387076, 1.000000000000000000, 0.8660254037844387076, 1.000000000000000000, 0.8660254037844387076, 1.000000000000000000, 0.8660254037844387076, 1.000000000000000000, 0.8660254037844387076, 1.000000000000000000, 0.8660254037844387076, 1.000000000000000000, 0.8660254037844387076, 1.000000000000000000, 0.8660254037844387076, 1.000000000000000000, 0.8660254037844387076, 1.000000000000000000, 0.8660254037844387076, 1.000000000000000000, 0.8660254037844387076, 1.000000000000000000, 0.8660254037844387076, 1.000000000000000000, 0.8660254037844387076, 1.000000000000000000, 0.8660254037844387076, 1.000000000000000000, 0.8660254037844387076, 1.000000000000000000, 0.8660254037844387076, 1.000000000000000000, 0.8660254037844387076, 1.000000000000000000, 0.8660254037844387076, 1.000000000000000000, 0.8660254037844387076, 1.000000000000000000, 0.8660254037844387076, 1.000000000000000000, 0.8660254037844387076, 1.000000000000000000, 0.8660254037844387076, 1.000000000000000000, 0.8660254037844387076, 1.000000000000000000, 0.8660254037844387076, 1.000000000000000000, 0.8660254037844387076, 1.000000000000000000, 0.8660254037844387076, 1.000000000000000000, 0.8660254037844387076, 1.000000000000000000, 0.8660254037844387076, 1.000000000000000000, 0.8660254037844387076, 1.000000000000000000, 0.8660254037844387076, 1.000000000000000000, 0.8660254037844387076, 1.000000000000000000, 0.8660254037844387076, 1.000000000000000000, 0.8660254037844387076, 1.000000000000000000, 0.8660254037844387076, 1.000000000000000000, 0.8660254037844387076, 1.000000000000000000, 0.8660254037844387076, 1.000000000000000000, 0.8660254037844387076, 1.000000000000000000, 0.8660254037844387076, 1.000000000000000000, 0.8660254037844387076, 1.000000000000000000, 0.8660254037844387076, 1.000000000000000000, 0.8660254037844387076, 1.000000000000000000, 0.8660254037844387076, 1.000000000000000000, 0.8660254037844387076, 1.000000000000000000, 0.8660254037844387076, 1.000000000000000000, 0.8660254037844387076, 1.000000000000000000, 0.8660254037844387076, 1.000000000000000000, 0.8660254037844387076, 1.000000000000000000, 0.8660254037844387076, 1.000000000000000000, 0.8660254037844387076, 1.000000000000000000, 0.8660254037844387076, 1.000000000000000000, 0.8660254037844387076, 1.000000000000000000, 0.8660254037844387076, 1.000000000000000000, 0.8660254037844387076, 1.000000000000000000, 0.8660254037844387076, 1.000000000000000000, 0.8660254037844387076, 1.000000000000000000, 0.8660254037844387076, 1.000000000000000000) ) ) 
 REPRESENTATION_ITEM ( '' )  SURFACE ( )  );
#52303 = CARTESIAN_POINT ( 'NONE',  ( -1.339745962155610925, -38.66965819600732601, 5.000000000000000000 ) ) ;
#52304 = CARTESIAN_POINT ( 'NONE',  ( -58.80597590150559739, -137.0000000000000284, 3.242614290531460330 ) ) ;
#52305 = AXIS2_PLACEMENT_3D ( 'NONE', #11385, #23268, #31650 ) ;
#52306 = CARTESIAN_POINT ( 'NONE',  ( -4.458734124999998549, -35.47916666530107221, 2.574251347313722516 ) ) ;
#52307 = CARTESIAN_POINT ( 'NONE',  ( -5.000000000000000000, -147.6250000027312126, -6.123233995736766282E-16 ) ) ;
#52308 = VERTEX_POINT ( 'NONE', #35106 ) ;
#52309 = CARTESIAN_POINT ( 'NONE',  ( 2.229367062500001939, -84.97916666530107932, 3.861377020970579999 ) ) ;
#52310 = ADVANCED_FACE ( 'NONE', ( #5828 ), #20306, .T. ) ;
#52311 = CARTESIAN_POINT ( 'NONE',  ( -2.229367062500000163, 24.52083333469892779, -3.861377020970580443 ) ) ;
#52312 = CARTESIAN_POINT ( 'NONE',  ( 5.000000000000000000, -24.29166666393548368, -2.886751345948130876 ) ) ;
#52313 = ORIENTED_EDGE ( 'NONE', *, *, #5512, .T. ) ;
#52314 = CARTESIAN_POINT ( 'NONE',  ( 1.975475456537005874E-15, 14.25000000000000000, 5.000000000000000000 ) ) ;
#52315 = CARTESIAN_POINT ( 'NONE',  ( -54.64476657466781973, -138.0625000013656063, -4.444560631937228834 ) ) ;
#52316 = CARTESIAN_POINT ( 'NONE',  ( -2.229367062499996610, -88.39583333196773651, 3.861377020970582219 ) ) ;
#52317 = CARTESIAN_POINT ( 'NONE',  ( -51.19402409849444524, -130.6250000027312126, -3.242614290531456334 ) ) ;
#52318 = CARTESIAN_POINT ( 'NONE',  ( 5.000000000000000888, 22.41666666666666785, 2.886751345948126879 ) ) ;
#52319 = CARTESIAN_POINT ( 'NONE',  ( 4.458734124999997661, -139.7500000013655779, 1.846868145590737864 ) ) ;
#52320 = CARTESIAN_POINT ( 'NONE',  ( 2.499999999999998668, -13.20833333060214976, -4.330127018922193649 ) ) ;
#52321 = CARTESIAN_POINT ( 'NONE',  ( 4.458734124999999437, -55.81249999863440081, -5.460374474430324690E-16 ) ) ;
#52322 = CARTESIAN_POINT ( 'NONE',  ( 1.975475456537005874E-15, 21.24999999999999289, 5.000000000000000000 ) ) ;
#52323 = CARTESIAN_POINT ( 'NONE',  ( -3.152548672688508926E-16, 25.43750000136559208, -5.148502694627439702 ) ) ;
#52324 = CARTESIAN_POINT ( 'NONE',  ( 5.000000000000000888, -107.5833333333333428, 2.886751345948126879 ) ) ;
#52325 = CARTESIAN_POINT ( 'NONE',  ( -5.000000000000000000, -44.00000000000000000, 0.000000000000000000 ) ) ;
#52326 = CARTESIAN_POINT ( 'NONE',  ( -4.458734124999999437, -42.64583333196773651, -2.574251347313719407 ) ) ;
#52327 = CARTESIAN_POINT ( 'NONE',  ( -4.999999999999999112, -5.791666663935480130, 2.886751345948131764 ) ) ;
#52328 = CARTESIAN_POINT ( 'NONE',  ( -2.499999999999996447, -72.83333333333332860, 4.330127018922195425 ) ) ;
#52329 = CARTESIAN_POINT ( 'NONE',  ( 1.975475456537005874E-15, -45.62499999726880873, 5.000000000000000000 ) ) ;
#52330 = CARTESIAN_POINT ( 'NONE',  ( -4.458734124999999437, -84.64583333196773651, -2.574251347313719407 ) ) ;
#52331 = CARTESIAN_POINT ( 'NONE',  ( 2.229367062500001939, -100.9791666653010651, 3.861377020970579999 ) ) ;
#52332 = CARTESIAN_POINT ( 'NONE',  ( 4.458734124999999437, -7.062499998634404363, -5.460374474430324690E-16 ) ) ;
#52333 = ORIENTED_EDGE ( 'NONE', *, *, #42774, .T. ) ;
#52334 = DIRECTION ( 'NONE',  ( 0.000000000000000000, 0.000000000000000000, 1.000000000000000000 ) ) ;
#52335 = CARTESIAN_POINT ( 'NONE',  ( 4.458734124999998549, -90.72916666530106511, -2.574251347313721627 ) ) ;
#52336 = CARTESIAN_POINT ( 'NONE',  ( 5.000000000000000000, -164.1875000027312126, 2.071067811865478614 ) ) ;
#52337 = CARTESIAN_POINT ( 'NONE',  ( 2.229367062500001939, -93.22916666530106511, 3.861377020970579999 ) ) ;
#52338 = CARTESIAN_POINT ( 'NONE',  ( 4.458734124999999437, 4.937500001365595637, -5.460374474430324690E-16 ) ) ;
#52339 = CARTESIAN_POINT ( 'NONE',  ( -2.499999999999996447, -15.83333333333333037, 4.330127018922195425 ) ) ;
#52340 = CARTESIAN_POINT ( 'NONE',  ( -56.48576386720575471, -131.7500000013656063, -4.591703134518078322 ) ) ;
#52341 = CARTESIAN_POINT ( 'NONE',  ( 4.458734125000000326, -13.89583333196774007, 2.574251347313718519 ) ) ;
#52342 = CARTESIAN_POINT ( 'NONE',  ( -3.152548672688508926E-16, 10.18750000136559564, -5.148502694627439702 ) ) ;
#52343 = CARTESIAN_POINT ( 'NONE',  ( 2.229367062499998831, -54.89583333196773651, -3.861377020970580887 ) ) ;
#52344 = CARTESIAN_POINT ( 'NONE',  ( -1.049326080737009628E-13, -19.75000000000000000, 5.000000000000000000 ) ) ;
#52345 = CARTESIAN_POINT ( 'NONE',  ( -1.339745962155613812, -106.2053418012614685, -5.000000000000000000 ) ) ;
#52346 = CARTESIAN_POINT ( 'NONE',  ( -4.458734124999999437, -9.312499998634406140, 0.000000000000000000 ) ) ;
#52347 = ORIENTED_EDGE ( 'NONE', *, *, #5823, .T. ) ;
#52348 = CARTESIAN_POINT ( 'NONE',  ( -4.458734124999997661, -37.47916666530107221, 2.574251347313722516 ) ) ;
#52349 = VECTOR ( 'NONE', #36053, 1000.000000000000000 ) ;
#52350 = CARTESIAN_POINT ( 'NONE',  ( -50.70258187064364108, -127.3750000013656205, 2.196230717870141014 ) ) ;
#52351 = CYLINDRICAL_SURFACE ( 'NONE', #12120, 5.000000000000000000 ) ;
#52352 = CARTESIAN_POINT ( 'NONE',  ( 2.229367062500001939, -80.97916666530106511, 3.861377020970579999 ) ) ;
#52353 = CARTESIAN_POINT ( 'NONE',  ( 9.457646018065525792E-16, 21.68750000136559208, 5.148502694627439702 ) ) ;
#52354 = CARTESIAN_POINT ( 'NONE',  ( -4.458734124999998549, 12.77083333469892601, 2.574251347313722516 ) ) ;
#52355 = CARTESIAN_POINT ( 'NONE',  ( -4.999999999999998224, -81.79166666393547303, 2.886751345948131764 ) ) ;
#52356 = CARTESIAN_POINT ( 'NONE',  ( -4.769696007084728073, -120.0000000000000000, -1.500000000000000000 ) ) ;
#52357 = CARTESIAN_POINT ( 'NONE',  ( -4.458734124999999437, -82.56249999863440792, 0.000000000000000000 ) ) ;
#52358 = CARTESIAN_POINT ( 'NONE',  ( 5.000000000000000000, -71.50000000000000000, -6.123233995736766282E-16 ) ) ;
#52359 = CARTESIAN_POINT ( 'NONE',  ( 5.000000000000000000, -63.37499999726880873, -6.123233995736766282E-16 ) ) ;
#52360 = CARTESIAN_POINT ( 'NONE',  ( -3.535250795749689387E-16, 18.87500000273118772, -5.773502691896257311 ) ) ;
#52361 = VERTEX_POINT ( 'NONE', #46019 ) ;
#52362 = CARTESIAN_POINT ( 'NONE',  ( 2.071067811865560326, -146.9375000027311842, -4.999999999999914735 ) ) ;
#52363 = CARTESIAN_POINT ( 'NONE',  ( -1.339745962155601378, 15.79465819873851906, -5.000000000000007105 ) ) ;
#52365 = CARTESIAN_POINT ( 'NONE',  ( 5.000000000000000000, -30.41666666666666785, -2.886751345948129988 ) ) ;
#52364 = CARTESIAN_POINT ( 'NONE',  ( -2.480964764533239819E-13, -108.6249999972688016, 5.000000000000000000 ) ) ;
#52366 = CARTESIAN_POINT ( 'NONE',  ( 4.458734125000001214, -33.89583333196773651, 2.574251347313718519 ) ) ;
#52367 = CARTESIAN_POINT ( 'NONE',  ( -1.339745962155610925, -33.79465819873851729, 5.000000000000000000 ) ) ;
#52368 = ADVANCED_FACE ( 'NONE', ( #41181 ), #39690, .T. ) ;
#52369 = CARTESIAN_POINT ( 'NONE',  ( 2.499999999999998668, -30.20833333060214443, -4.330127018922193649 ) ) ;
#52370 = EDGE_CURVE ( 'NONE', #55212, #55214, #12470, .T. ) ;
#52372 = ORIENTED_EDGE ( 'NONE', *, *, #34552, .F. ) ;
#52371 = CARTESIAN_POINT ( 'NONE',  ( 4.458734125000001214, -58.89583333196773651, 2.574251347313718519 ) ) ;
#52373 = CYLINDRICAL_SURFACE ( 'NONE', #59046, 5.000000000000000000 ) ;
#52375 = ORIENTED_EDGE ( 'NONE', *, *, #43639, .F. ) ;
#52374 = CARTESIAN_POINT ( 'NONE',  ( -3.152548672688508926E-16, -6.812499998634404363, -5.148502694627439702 ) ) ;
#52376 = EDGE_CURVE ( 'NONE', #22588, #15620, #27684, .T. ) ;
#52377 = CARTESIAN_POINT ( 'NONE',  ( 5.000000000000000888, -79.58333333333331439, 2.886751345948126879 ) ) ;
#52378 = CARTESIAN_POINT ( 'NONE',  ( -50.55543936806279248, -140.0625000013656063, 0.3552334253322060320 ) ) ;
#52379 = CARTESIAN_POINT ( 'NONE',  ( 2.229367062500001939, -52.22916666530107221, 3.861377020970579999 ) ) ;
#52380 = ADVANCED_FACE ( 'NONE', ( #55999 ), #6791, .T. ) ;
#52381 = CARTESIAN_POINT ( 'NONE',  ( 5.000000000000000000, -75.37499999726880162, -6.123233995736766282E-16 ) ) ;
#52382 = ORIENTED_EDGE ( 'NONE', *, *, #16773, .T. ) ;
#52383 = CARTESIAN_POINT ( 'NONE',  ( -49.85088928181150436, -151.5625000000000284, -1.666127454062680702 ) ) ;
#52384 = EDGE_CURVE ( 'NONE', #7754, #45000, #58854, .T. ) ;
#52385 = CARTESIAN_POINT ( 'NONE',  ( 4.458734124999999437, -22.06249999863440436, -5.460374474430324690E-16 ) ) ;
#52386 = EDGE_CURVE ( 'NONE', #61565, #35439, #45726, .T. ) ;
#52388 = ORIENTED_EDGE ( 'NONE', *, *, #54329, .T. ) ;
#52387 = CARTESIAN_POINT ( 'NONE',  ( 4.458734124999998549, -55.97916666530107932, -2.574251347313721627 ) ) ;
#52389 =( BOUNDED_CURVE ( )  B_SPLINE_CURVE ( 2, ( #34071, #23801, #38890, #4803, #53377, #29873, #5442, #58832, #14762 ),
 .UNSPECIFIED., .F., .F. ) 
 B_SPLINE_CURVE_WITH_KNOTS ( ( 3, 2, 2, 2, 3 ),
 ( 0.4729166666666666519, 0.4736111111111110938, 0.4749999999999999778, 0.4763888888888888618, 0.4770833333333333592 ),
 .UNSPECIFIED. ) 
 CURVE ( )  GEOMETRIC_REPRESENTATION_ITEM ( )  RATIONAL_B_SPLINE_CURVE ( ( 0.9330127018922194093, 0.9330127018922194093, 1.000000000000000000, 0.8660254037844387076, 1.000000000000000000, 0.8660254037844387076, 1.000000000000000000, 0.9330127018922167448, 0.9330127018922194093 ) ) 
 REPRESENTATION_ITEM ( '' )  );
#52390 = CARTESIAN_POINT ( 'NONE',  ( 55.00000000000002132, 14.99999999999998579, 1.734723475976807094E-15 ) ) ;
#52391 = CARTESIAN_POINT ( 'NONE',  ( 1.846868145590736310, -141.6250000013656631, 4.458734124999999437 ) ) ;
#52392 = CARTESIAN_POINT ( 'NONE',  ( 2.229367062499998831, -97.89583333196773651, -3.861377020970580887 ) ) ;
#52393 = CARTESIAN_POINT ( 'NONE',  ( -5.000000000000000000, -167.6250000027312126, -6.123233995736766282E-16 ) ) ;
#52394 = ORIENTED_EDGE ( 'NONE', *, *, #50411, .F. ) ;
#52395 = ADVANCED_FACE ( 'NONE', ( #17705 ), #62408, .T. ) ;
#52396 = CARTESIAN_POINT ( 'NONE',  ( -59.59170313451810586, -151.7500000013656063, 1.485763867205729394 ) ) ;
#52397 = CARTESIAN_POINT ( 'NONE',  ( -50.18089887299979068, -140.8125000027311842, 2.462841084822635640 ) ) ;
#52398 = ORIENTED_EDGE ( 'NONE', *, *, #51583, .T. ) ;
#52399 = EDGE_CURVE ( 'NONE', #24836, #54901, #25998, .T. ) ;
#52400 = EDGE_CURVE ( 'NONE', #30240, #29389, #32812, .T. ) ;
#52401 = CARTESIAN_POINT ( 'NONE',  ( -4.999999999999998224, 1.208333336064518981, 2.886751345948131764 ) ) ;
#52402 = CARTESIAN_POINT ( 'NONE',  ( -2.229367062500000163, -9.479166665301068662, -3.861377020970580443 ) ) ;
#52403 = CARTESIAN_POINT ( 'NONE',  ( -4.458734124999997661, -95.47916666530106511, 2.574251347313722516 ) ) ;
#52404 =( BOUNDED_CURVE ( )  B_SPLINE_CURVE ( 2, ( #43332, #42704, #38504, #53934, #18586, #28857, #62974, #33376, #33071 ),
 .UNSPECIFIED., .F., .F. ) 
 B_SPLINE_CURVE_WITH_KNOTS ( ( 3, 2, 2, 2, 3 ),
 ( 0.002083333333333333738, 0.002777777777777777884, 0.004166666666666666609, 0.005555555555555555768, 0.006250000000000000347 ),
 .UNSPECIFIED. ) 
 CURVE ( )  GEOMETRIC_REPRESENTATION_ITEM ( )  RATIONAL_B_SPLINE_CURVE ( ( 0.9330127018922194093, 0.9330127018922194093, 1.000000000000000000, 0.8660254037844387076, 1.000000000000000000, 0.8660254037844387076, 1.000000000000000000, 0.9330127018922192983, 0.9330127018922194093 ) ) 
 REPRESENTATION_ITEM ( '' )  );
#52405 = CARTESIAN_POINT ( 'NONE',  ( 3.152801135295367541, -147.5625000013655779, -3.152801135295367541 ) ) ;
#52406 = CARTESIAN_POINT ( 'NONE',  ( 4.458734124999998549, -29.97916666530107577, -2.574251347313721627 ) ) ;
#52407 = CARTESIAN_POINT ( 'NONE',  ( 1.975475456537005874E-15, -1.624999997268813834, 5.000000000000000000 ) ) ;
#52408 = CARTESIAN_POINT ( 'NONE',  ( -50.70258187064364108, -136.1250000013656063, 2.196230717870141014 ) ) ;
#52409 = CARTESIAN_POINT ( 'NONE',  ( -4.458734124999999437, -68.64583333196773651, -2.574251347313719407 ) ) ;
#52410 = CARTESIAN_POINT ( 'NONE',  ( 5.000000000000000888, -21.45833333060214798, 2.886751345948126879 ) ) ;
#52411 = CARTESIAN_POINT ( 'NONE',  ( 5.000000000000000000, -88.37499999726880162, -6.123233995736766282E-16 ) ) ;
#52412 = CARTESIAN_POINT ( 'NONE',  ( 2.730187237215162345E-16, -140.1875000013656063, -4.458734124999999437 ) ) ;
#52413 = CARTESIAN_POINT ( 'NONE',  ( 4.458734124999999437, 9.937500001365593860, -5.460374474430324690E-16 ) ) ;
#52414 = ORIENTED_EDGE ( 'NONE', *, *, #51136, .T. ) ;
#52415 = CARTESIAN_POINT ( 'NONE',  ( -2.498395430326213474E-14, 16.24999999999999645, 5.000000000000000000 ) ) ;
#52417 = CARTESIAN_POINT ( 'NONE',  ( 4.458734124999998549, -25.72916666530107221, -2.574251347313721627 ) ) ;
#52416 = CARTESIAN_POINT ( 'NONE',  ( -2.500000000000000444, -89.16666666666665719, -4.330127018922193649 ) ) ;
#52418 = CARTESIAN_POINT ( 'NONE',  ( -6.972266317189433020E-16, -80.24999999999998579, -5.000000000000000000 ) ) ;
#52419 = CARTESIAN_POINT ( 'NONE',  ( -2.229367062500000163, -75.72916666530106511, -3.861377020970580443 ) ) ;
#52420 = CARTESIAN_POINT ( 'NONE',  ( -4.458734124999999437, 28.43750000136559208, 0.000000000000000000 ) ) ;
#52421 = CARTESIAN_POINT ( 'NONE',  ( 5.000000000000000000, -79.29166666393547303, -2.886751345948130876 ) ) ;
#52422 = CARTESIAN_POINT ( 'NONE',  ( -57.89159099828107458, -145.6875000013656063, -3.393966926194107447 ) ) ;
#52423 = CARTESIAN_POINT ( 'NONE',  ( -3.152548672688508926E-16, 1.437500001365596525, -5.148502694627439702 ) ) ;
#52424 = CARTESIAN_POINT ( 'NONE',  ( -5.000000000000000000, -62.95833333060215153, -2.886751345948128211 ) ) ;
#52425 = CARTESIAN_POINT ( 'NONE',  ( -6.972266317189433020E-16, 16.74999999999999645, -5.000000000000000000 ) ) ;
#52426 = CARTESIAN_POINT ( 'NONE',  ( -4.458734124999999437, 6.687500001365593860, 0.000000000000000000 ) ) ;
#52427 = CARTESIAN_POINT ( 'NONE',  ( 2.229367062500001939, -73.97916666530106511, 3.861377020970579999 ) ) ;
#52428 = CARTESIAN_POINT ( 'NONE',  ( -2.229367062499996610, -19.39583333196774007, 3.861377020970582219 ) ) ;
#52429 = CARTESIAN_POINT ( 'NONE',  ( -4.999999999999999112, -7.916666666666668739, 2.886751345948131764 ) ) ;
#52430 = CARTESIAN_POINT ( 'NONE',  ( -4.458734124999999437, -157.9375000013655779, -5.460374474430324690E-16 ) ) ;
#52431 = LINE ( 'NONE', #31849, #45913 ) ;
#52432 = CARTESIAN_POINT ( 'NONE',  ( -2.229367062499996610, -64.14583333196773651, 3.861377020970582219 ) ) ;
#52433 = CARTESIAN_POINT ( 'NONE',  ( 5.000000000000000888, -97.45833333060214443, 2.886751345948126879 ) ) ;
#52434 = CARTESIAN_POINT ( 'NONE',  ( -4.458734124999999437, 29.60416666803225993, -2.574251347313719407 ) ) ;
#52435 = CARTESIAN_POINT ( 'NONE',  ( 2.229367062500001939, -39.97916666530107221, 3.861377020970579999 ) ) ;
#52436 = CARTESIAN_POINT ( 'NONE',  ( 2.499999999999998668, 9.791666669397850242, -4.330127018922193649 ) ) ;
#52437 = CARTESIAN_POINT ( 'NONE',  ( 4.458734124999999437, -106.0624999986344221, -5.460374474430324690E-16 ) ) ;
#52438 = CARTESIAN_POINT ( 'NONE',  ( -2.229367062499996610, -66.39583333196773651, 3.861377020970582219 ) ) ;
#52439 = CARTESIAN_POINT ( 'NONE',  ( 1.060575238724906964E-15, -53.74999999999998579, 5.773502691896257311 ) ) ;
#52440 = CYLINDRICAL_SURFACE ( 'NONE', #37748, 5.000000000000000000 ) ;
#52441 = VERTEX_POINT ( 'NONE', #7742 ) ;
#52442 = CARTESIAN_POINT ( 'NONE',  ( -1.339745962155613812, -85.20534180126148271, -5.000000000000000000 ) ) ;
#52443 = CARTESIAN_POINT ( 'NONE',  ( 5.000000000000000000, -144.1875000027312126, 2.071067811865478614 ) ) ;
#52444 = CARTESIAN_POINT ( 'NONE',  ( -2.500000000000000444, -12.16666666666666607, -4.330127018922193649 ) ) ;
#52445 = CARTESIAN_POINT ( 'NONE',  ( 4.458734125000001214, -15.89583333196773651, 2.574251347313718519 ) ) ;
#52446 = VECTOR ( 'NONE', #57503, 1000.000000000000000 ) ;
#52447 = CARTESIAN_POINT ( 'NONE',  ( -3.152548672688508926E-16, -79.56249999863440792, -5.148502694627439702 ) ) ;
#52448 = CARTESIAN_POINT ( 'NONE',  ( -5.000000000000000000, -4.958333330602148870, -2.886751345948128211 ) ) ;
#52449 = CARTESIAN_POINT ( 'NONE',  ( 5.000000000000000000, -10.29166666393547835, -2.886751345948129988 ) ) ;
#52451 = ORIENTED_EDGE ( 'NONE', *, *, #55529, .F. ) ;
#52450 = CARTESIAN_POINT ( 'NONE',  ( -2.229367062500000163, -43.47916666530106511, -3.861377020970580443 ) ) ;
#52452 = CARTESIAN_POINT ( 'NONE',  ( 2.499999999999998668, -41.33333333333333570, -4.330127018922193649 ) ) ;
#52454 = ORIENTED_EDGE ( 'NONE', *, *, #22790, .T. ) ;
#52453 = CARTESIAN_POINT ( 'NONE',  ( -4.458734124999999437, 8.437500001365595637, 0.000000000000000000 ) ) ;
#52455 = CARTESIAN_POINT ( 'NONE',  ( -9.184850993605147944E-16, -153.2500000000000000, 5.000000000000000000 ) ) ;
#52456 = CARTESIAN_POINT ( 'NONE',  ( 5.000000000000000000, -63.50000000000000000, -6.123233995736766282E-16 ) ) ;
#52457 = CARTESIAN_POINT ( 'NONE',  ( 4.458734124999999437, -161.6875000013655779, 0.000000000000000000 ) ) ;
#52458 = CARTESIAN_POINT ( 'NONE',  ( -2.229367062499996610, -33.39583333196772941, 3.861377020970582219 ) ) ;
#52459 = CARTESIAN_POINT ( 'NONE',  ( -4.458734124999999437, -78.39583333196772230, -2.574251347313719407 ) ) ;
#52460 =( BOUNDED_CURVE ( )  B_SPLINE_CURVE ( 2, ( #756, #30960, #5564, #26139, #29995, #45759, #10386, #1711, #20364 ),
 .UNSPECIFIED., .F., .F. ) 
 B_SPLINE_CURVE_WITH_KNOTS ( ( 3, 2, 2, 2, 3 ),
 ( 0.4767857142857143127, 0.4773809523809524058, 0.4785714285714285920, 0.4797619047619047783, 0.4803571428571428714 ),
 .UNSPECIFIED. ) 
 CURVE ( )  GEOMETRIC_REPRESENTATION_ITEM ( )  RATIONAL_B_SPLINE_CURVE ( ( 0.9330127018922194093, 0.9330127018922225179, 1.000000000000000000, 0.8660254037844387076, 1.000000000000000000, 0.8660254037844387076, 1.000000000000000000, 0.9330127018922194093, 0.9330127018922194093 ) ) 
 REPRESENTATION_ITEM ( '' )  );
#52461 = CARTESIAN_POINT ( 'NONE',  ( 5.000000000000000000, -166.0000000000000000, 0.000000000000000000 ) ) ;
#52462 = CARTESIAN_POINT ( 'NONE',  ( 5.000000000000000888, -167.9375000000000284, -2.071067811865475505 ) ) ;
#52463 = CARTESIAN_POINT ( 'NONE',  ( -57.89159099828107458, -131.9375000013656063, -3.393966926194107447 ) ) ;
#52464 = CARTESIAN_POINT ( 'NONE',  ( 2.229367062499998831, -5.895833331967740953, -3.861377020970580887 ) ) ;
#52465 = CARTESIAN_POINT ( 'NONE',  ( -4.458734124999999437, -42.56249999863440081, 0.000000000000000000 ) ) ;
#52466 = CARTESIAN_POINT ( 'NONE',  ( 1.975475456537005874E-15, -24.62499999726881583, 5.000000000000000000 ) ) ;
#52467 = CARTESIAN_POINT ( 'NONE',  ( 2.229367062500001939, -85.22916666530107932, 3.861377020970579999 ) ) ;
#52468 = DIRECTION ( 'NONE',  ( -0.000000000000000000, 1.000000000000000000, -0.000000000000000000 ) ) ;
#52469 = VERTEX_POINT ( 'NONE', #12870 ) ;
#52470 = CARTESIAN_POINT ( 'NONE',  ( -56.66612745406270335, -153.4375000027311842, -5.149110718188516067 ) ) ;
#52471 = CARTESIAN_POINT ( 'NONE',  ( -6.972266317189433020E-16, -102.1249999972688158, -5.000000000000000000 ) ) ;
#52472 = CARTESIAN_POINT ( 'NONE',  ( -4.458734124999999437, -70.64583333196773651, -2.574251347313719407 ) ) ;
#52473 = CARTESIAN_POINT ( 'NONE',  ( -1.846868145590737420, -145.0000000013656063, 4.458734124999997661 ) ) ;
#52474 = ORIENTED_EDGE ( 'NONE', *, *, #22100, .F. ) ;
#52475 = CARTESIAN_POINT ( 'NONE',  ( -2.071067811865604735, -150.4375000027312126, 4.999999999999872990 ) ) ;
#52476 = EDGE_CURVE ( 'NONE', #19516, #4014, #23562, .T. ) ;
#52477 = CARTESIAN_POINT ( 'NONE',  ( -1.339745962155610925, -1.794658198738520616, 5.000000000000000000 ) ) ;
#52478 = CARTESIAN_POINT ( 'NONE',  ( -4.458734124999999437, -14.56249999863440436, 0.000000000000000000 ) ) ;
#52479 = CARTESIAN_POINT ( 'NONE',  ( -4.999999999999998224, -34.91666666666666430, 2.886751345948131764 ) ) ;
#52480 = CARTESIAN_POINT ( 'NONE',  ( 4.458734124999998549, 0.2708333346989263979, -2.574251347313721627 ) ) ;
#52481 = CARTESIAN_POINT ( 'NONE',  ( -1.339745962155613812, -96.08034179853028434, -5.000000000000000000 ) ) ;
#52482 = CARTESIAN_POINT ( 'NONE',  ( -4.458734124999999437, -158.0000000013656063, -1.846868145590735644 ) ) ;
#52483 =( BOUNDED_CURVE ( )  B_SPLINE_CURVE ( 2, ( #28713, #14549, #39309, #39624, #38996, #43502, #15194, #20344, #58000 ),
 .UNSPECIFIED., .F., .F. ) 
 B_SPLINE_CURVE_WITH_KNOTS ( ( 3, 2, 2, 2, 3 ),
 ( 0.9249999999999998224, 0.9291666666666664742, 0.9333333333333331261, 0.9374999999999998890, 0.9416666666666665408 ),
 .UNSPECIFIED. ) 
 CURVE ( )  GEOMETRIC_REPRESENTATION_ITEM ( )  RATIONAL_B_SPLINE_CURVE ( ( 1.000000000000003997, 0.9238795325112826307, 1.000000000000000000, 0.9238795325112867385, 1.000000000000000000, 0.9238795325112867385, 1.000000000000000000, 0.9238795325112887369, 0.9999999999999980016 ) ) 
 REPRESENTATION_ITEM ( '' )  );
#52484 = CARTESIAN_POINT ( 'NONE',  ( -3.152548672688508926E-16, 27.18750000136559564, -5.148502694627439702 ) ) ;
#52485 = EDGE_LOOP ( 'NONE', ( #36287, #35932, #4758, #4489 ) ) ;
#52486 = CARTESIAN_POINT ( 'NONE',  ( -4.458734124999999437, -94.39583333196773651, -2.574251347313719407 ) ) ;
#52487 = CARTESIAN_POINT ( 'NONE',  ( 1.975475456537005874E-15, -28.74999999999999645, 5.000000000000000000 ) ) ;
#52488 = CARTESIAN_POINT ( 'NONE',  ( -1.339745962155613812, -63.20534180126146850, -5.000000000000000000 ) ) ;
#52489 = CARTESIAN_POINT ( 'NONE',  ( 4.458734124999999437, -8.812499998634406140, -5.460374474430324690E-16 ) ) ;
#52490 = VECTOR ( 'NONE', #32015, 1000.000000000000000 ) ;
#52491 = LINE ( 'NONE', #52165, #5700 ) ;
#52492 = CARTESIAN_POINT ( 'NONE',  ( 2.500000000000002220, -48.66666666666666430, 4.330127018922192761 ) ) ;
#52493 = CARTESIAN_POINT ( 'NONE',  ( 0.000000000000000000, -170.0000000000000000, 0.000000000000000000 ) ) ;
#52494 = CARTESIAN_POINT ( 'NONE',  ( -2.499999999999996447, -33.70833333060213732, 4.330127018922195425 ) ) ;
#52495 = DIRECTION ( 'NONE',  ( -0.000000000000000000, 1.000000000000000000, -0.000000000000000000 ) ) ;
#52496 = CARTESIAN_POINT ( 'NONE',  ( -4.458734124999999437, 16.60416666803225993, -2.574251347313719407 ) ) ;
#52497 = CARTESIAN_POINT ( 'NONE',  ( 2.229367062500001939, 25.02083333469892779, 3.861377020970579999 ) ) ;
#52498 = CARTESIAN_POINT ( 'NONE',  ( -4.458734124999998549, -57.22916666530107932, 2.574251347313722516 ) ) ;
#52499 = CARTESIAN_POINT ( 'NONE',  ( -3.152548672688508926E-16, -3.812499998634408360, -5.148502694627439702 ) ) ;
#52500 = CARTESIAN_POINT ( 'NONE',  ( -5.000000000000000000, -33.87499999726880873, 0.000000000000000000 ) ) ;
#52501 = CARTESIAN_POINT ( 'NONE',  ( 2.499999999999998668, 11.66666666666666607, -4.330127018922193649 ) ) ;
#52502 = CARTESIAN_POINT ( 'NONE',  ( 3.061616997868383141E-16, -139.8750000027312126, -5.000000000000000000 ) ) ;
#52503 = CARTESIAN_POINT ( 'NONE',  ( -58.24261429053147765, -155.0000000000000284, -3.805975901505573411 ) ) ;
#52504 = CARTESIAN_POINT ( 'NONE',  ( -4.458734124999999437, -47.39583333196774362, -2.574251347313719407 ) ) ;
#52505 = CARTESIAN_POINT ( 'NONE',  ( 2.500000000000002220, -83.54166666393547303, 4.330127018922192761 ) ) ;
#52506 = CARTESIAN_POINT ( 'NONE',  ( -57.89159099828107458, -134.9375000013656063, -3.393966926194107447 ) ) ;
#52507 = CARTESIAN_POINT ( 'NONE',  ( 5.000000000000000000, -14.37499999726881228, -6.123233995736766282E-16 ) ) ;
#52508 = CARTESIAN_POINT ( 'NONE',  ( -5.000000000000000000, -104.8749999972688158, 0.000000000000000000 ) ) ;
#52509 = CARTESIAN_POINT ( 'NONE',  ( -4.458734124999997661, -90.47916666530106511, 2.574251347313722516 ) ) ;
#52510 = CARTESIAN_POINT ( 'NONE',  ( 1.846868145590736310, -156.8750000013655779, 4.458734124999997661 ) ) ;
#52511 = CARTESIAN_POINT ( 'NONE',  ( 5.000000000000000000, -32.41666666666665719, -2.886751345948129988 ) ) ;
#52512 = CARTESIAN_POINT ( 'NONE',  ( -3.535533905932737309, -147.6250000000000000, -3.535533905932738197 ) ) ;
#52513 = ORIENTED_EDGE ( 'NONE', *, *, #55150, .T. ) ;
#52514 = CARTESIAN_POINT ( 'NONE',  ( 9.457646018065525792E-16, 16.68750000136559564, 5.148502694627439702 ) ) ;
#52515 = ORIENTED_EDGE ( 'NONE', *, *, #44391, .T. ) ;
#52516 = CARTESIAN_POINT ( 'NONE',  ( 2.229367062499998831, -96.64583333196773651, -3.861377020970580887 ) ) ;
#52517 = CARTESIAN_POINT ( 'NONE',  ( 4.458734125000001214, 6.854166668032259935, 2.574251347313718519 ) ) ;
#52518 = CARTESIAN_POINT ( 'NONE',  ( 5.000000000000000000, 13.62500000273118417, -6.123233995736766282E-16 ) ) ;
#52519 = CARTESIAN_POINT ( 'NONE',  ( -6.972266317189433020E-16, -60.24999999999999289, -5.000000000000000000 ) ) ;
#52520 = CARTESIAN_POINT ( 'NONE',  ( -4.999999999999999112, 4.083333333333334814, 2.886751345948131764 ) ) ;
#52521 = CARTESIAN_POINT ( 'NONE',  ( -2.229367062499996610, -63.14583333196774362, 3.861377020970582219 ) ) ;
#52522 = CARTESIAN_POINT ( 'NONE',  ( 0.000000000000000000, -170.0000000000000000, 0.000000000000000000 ) ) ;
#52523 = CARTESIAN_POINT ( 'NONE',  ( -4.458734124999998549, -27.22916666530107221, 2.574251347313722516 ) ) ;
#52524 = CARTESIAN_POINT ( 'NONE',  ( -4.999999999999998224, -37.79166666393548724, 2.886751345948131764 ) ) ;
#52525 = CARTESIAN_POINT ( 'NONE',  ( -2.500000000000000444, -26.04166666393547658, -4.330127018922193649 ) ) ;
#52526 = DIRECTION ( 'NONE',  ( 0.000000000000000000, 0.000000000000000000, 1.000000000000000000 ) ) ;
#52527 = CARTESIAN_POINT ( 'NONE',  ( -2.500000000000000444, -46.16666666666666430, -4.330127018922193649 ) ) ;
#52528 = DIRECTION ( 'NONE',  ( -0.000000000000000000, 1.000000000000000000, -0.000000000000000000 ) ) ;
#52530 = CARTESIAN_POINT ( 'NONE',  ( -4.458734124999999437, -21.64583333196774362, -2.574251347313719407 ) ) ;
#52529 = CARTESIAN_POINT ( 'NONE',  ( 1.339745962155612702, 6.830341803992665994, -5.000000000000000000 ) ) ;
#52531 = CARTESIAN_POINT ( 'NONE',  ( -6.255257926720099353E-16, -8.716842316802392077, -7.700127545397295492 ) ) ;
#52532 = CARTESIAN_POINT ( 'NONE',  ( 4.458734124999998549, -64.72916666530106511, -2.574251347313721627 ) ) ;
#52533 = CARTESIAN_POINT ( 'NONE',  ( -4.458734125000000326, -147.2500000013656063, -1.846868145590735644 ) ) ;
#52534 = CARTESIAN_POINT ( 'NONE',  ( 4.458734124999998549, -76.72916666530106511, -2.574251347313721627 ) ) ;
#52535 = CARTESIAN_POINT ( 'NONE',  ( -51.60603307380591787, -142.1875000013656063, -2.891590998281053704 ) ) ;
#52536 = CARTESIAN_POINT ( 'NONE',  ( 9.457646018065525792E-16, -26.31249999863440792, 5.148502694627439702 ) ) ;
#52537 = CARTESIAN_POINT ( 'NONE',  ( 2.500000000000002220, -68.54166666393547303, 4.330127018922192761 ) ) ;
#52538 = ORIENTED_EDGE ( 'NONE', *, *, #50870, .T. ) ;
#52539 = LINE ( 'NONE', #28081, #42566 ) ;
#52540 = ORIENTED_EDGE ( 'NONE', *, *, #51602, .F. ) ;
#52541 = CARTESIAN_POINT ( 'NONE',  ( -4.458734124999999437, -68.56249999863439371, 0.000000000000000000 ) ) ;
#52542 = CARTESIAN_POINT ( 'NONE',  ( -1.975475456537005874E-15, 29.25000000000000000, 5.000000000000000000 ) ) ;
#52543 = CYLINDRICAL_SURFACE ( 'NONE', #25617, 5.000000000000000000 ) ;
#52544 = ORIENTED_EDGE ( 'NONE', *, *, #48439, .T. ) ;
#52545 = CARTESIAN_POINT ( 'NONE',  ( -2.499999999999996447, -5.708333330602148870, 4.330127018922195425 ) ) ;
#52546 = CARTESIAN_POINT ( 'NONE',  ( -6.972266317189433020E-16, 15.87500000273118417, -5.000000000000000000 ) ) ;
#52547 = CARTESIAN_POINT ( 'NONE',  ( -4.458734124999999437, -51.56249999863440792, 0.000000000000000000 ) ) ;
#52548 = CARTESIAN_POINT ( 'NONE',  ( -2.229367062499996610, 1.604166668032262155, 3.861377020970582219 ) ) ;
#52549 = ORIENTED_EDGE ( 'NONE', *, *, #33419, .F. ) ;
#52550 = CARTESIAN_POINT ( 'NONE',  ( 5.000000000000000888, -45.58333333333333570, 2.886751345948126879 ) ) ;
#52551 = CARTESIAN_POINT ( 'NONE',  ( -3.152548672688508926E-16, 3.437500001365594748, -5.148502694627439702 ) ) ;
#52552 = CARTESIAN_POINT ( 'NONE',  ( 4.458734124999999437, 19.18750000136559564, -5.460374474430324690E-16 ) ) ;
#52553 = CARTESIAN_POINT ( 'NONE',  ( -55.35523342533222291, -144.3125000013656063, 4.444560631937231499 ) ) ;
#52554 = CARTESIAN_POINT ( 'NONE',  ( 1.339745962155612702, 16.70534180126147916, -5.000000000000000000 ) ) ;
#52555 = CARTESIAN_POINT ( 'NONE',  ( 3.152801135295366208, -167.5625000013656063, 3.152801135295367985 ) ) ;
#52556 = ORIENTED_EDGE ( 'NONE', *, *, #36256, .T. ) ;
#52557 = CARTESIAN_POINT ( 'NONE',  ( -2.229367062500000163, -77.47916666530106511, -3.861377020970580443 ) ) ;
#52558 = DIRECTION ( 'NONE',  ( 0.000000000000000000, 0.000000000000000000, 1.000000000000000000 ) ) ;
#52559 = CARTESIAN_POINT ( 'NONE',  ( 2.229367062500001939, 7.020833334698928674, 3.861377020970579999 ) ) ;
#52560 = CARTESIAN_POINT ( 'NONE',  ( 5.000000000000000888, -140.0625000027312126, -2.071067811865475505 ) ) ;
#52561 = CARTESIAN_POINT ( 'NONE',  ( 4.458734124999999437, -58.06249999863440081, -5.460374474430324690E-16 ) ) ;
#52562 = CARTESIAN_POINT ( 'NONE',  ( 1.060575238724906964E-15, -19.62499999726881583, 5.773502691896257311 ) ) ;
#52563 = LINE ( 'NONE', #53806, #24483 ) ;
#52564 = CARTESIAN_POINT ( 'NONE',  ( -6.972266317189433020E-16, -42.12499999726880873, -5.000000000000000000 ) ) ;
#52565 = CARTESIAN_POINT ( 'NONE',  ( 1.975475456537005874E-15, 19.37500000273118772, 5.000000000000000000 ) ) ;
#52566 = DIRECTION ( 'NONE',  ( -0.000000000000000000, 1.000000000000000000, -0.000000000000000000 ) ) ;
#52567 = DIRECTION ( 'NONE',  ( 0.000000000000000000, 0.000000000000000000, 1.000000000000000000 ) ) ;
#52568 = CARTESIAN_POINT ( 'NONE',  ( -3.152548672688508926E-16, -38.56249999863439371, -5.148502694627439702 ) ) ;
#52569 = CARTESIAN_POINT ( 'NONE',  ( 2.229367062500001939, -27.22916666530106866, 3.861377020970579999 ) ) ;
#52570 = CARTESIAN_POINT ( 'NONE',  ( 0.000000000000000000, -170.0000000000000000, 0.000000000000000000 ) ) ;
#52571 = CARTESIAN_POINT ( 'NONE',  ( 2.499999999999998668, 25.66666666666666430, -4.330127018922193649 ) ) ;
#52572 = CARTESIAN_POINT ( 'NONE',  ( 2.071067811865476394, -152.3125000027312410, 5.000000000000000000 ) ) ;
#52573 = ORIENTED_EDGE ( 'NONE', *, *, #14961, .F. ) ;
#52574 = CARTESIAN_POINT ( 'NONE',  ( -2.229367062499996610, -106.3958333319677365, 3.861377020970582219 ) ) ;
#52575 = EDGE_CURVE ( 'NONE', #44494, #33925, #51920, .T. ) ;
#52576 = CARTESIAN_POINT ( 'NONE',  ( 4.458734125000001214, -29.89583333196773651, 2.574251347313718519 ) ) ;
#52577 = CARTESIAN_POINT ( 'NONE',  ( -3.535250795749689387E-16, -70.12499999726880162, -5.773502691896257311 ) ) ;
#52578 = CARTESIAN_POINT ( 'NONE',  ( -50.40829686548195099, -146.2500000013656063, -1.485763867205728284 ) ) ;
#52579 =( BOUNDED_CURVE ( )  B_SPLINE_CURVE ( 2, ( #52945, #39396, #43901, #44224, #48426, #58713, #38159, #29746, #5322 ),
 .UNSPECIFIED., .F., .F. ) 
 B_SPLINE_CURVE_WITH_KNOTS ( ( 3, 2, 2, 2, 3 ),
 ( 0.7979166666666667185, 0.7986111111111111605, 0.8000000000000000444, 0.8013888888888889284, 0.8020833333333333703 ),
 .UNSPECIFIED. ) 
 CURVE ( )  GEOMETRIC_REPRESENTATION_ITEM ( )  RATIONAL_B_SPLINE_CURVE ( ( 0.9330127018922194093, 0.9330127018922194093, 1.000000000000000000, 0.8660254037844387076, 1.000000000000000000, 0.8660254037844387076, 1.000000000000000000, 0.9330127018922194093, 0.9330127018922194093 ) ) 
 REPRESENTATION_ITEM ( '' )  );
#52580 = CARTESIAN_POINT ( 'NONE',  ( -2.071067811865478170, -148.3125000000000000, 5.000000000000000000 ) ) ;
#52581 = CARTESIAN_POINT ( 'NONE',  ( -4.458734124999997661, -30.22916666530106866, 2.574251347313722516 ) ) ;
#52582 = CARTESIAN_POINT ( 'NONE',  ( 2.229367062499998831, -73.89583333196773651, -3.861377020970580887 ) ) ;
#52583 = CARTESIAN_POINT ( 'NONE',  ( 2.500000000000002220, 22.45833333606451987, 4.330127018922192761 ) ) ;
#52584 = CARTESIAN_POINT ( 'NONE',  ( 2.229367062499998831, -31.64583333196773651, -3.861377020970580887 ) ) ;
#52585 = CARTESIAN_POINT ( 'NONE',  ( -57.46284108482265651, -138.0625000027312126, 4.819101127000238627 ) ) ;
#52586 = CARTESIAN_POINT ( 'NONE',  ( 2.500000000000002220, -18.66666666666666430, 4.330127018922192761 ) ) ;
#52587 = CARTESIAN_POINT ( 'NONE',  ( -8.190561711645485556E-16, -146.6875000013656063, 4.458734124999999437 ) ) ;
#52588 = ORIENTED_EDGE ( 'NONE', *, *, #4795, .F. ) ;
#52589 = FACE_OUTER_BOUND ( 'NONE', #32245, .T. ) ;
#52590 = CARTESIAN_POINT ( 'NONE',  ( -2.229367062499996610, -57.39583333196773651, 3.861377020970582219 ) ) ;
#52591 = CARTESIAN_POINT ( 'NONE',  ( 5.000000000000000888, 25.54166666939784847, 2.886751345948126879 ) ) ;
#52592 = CARTESIAN_POINT ( 'NONE',  ( 5.000000000000000000, 21.50000000000000000, -6.123233995736766282E-16 ) ) ;
#52593 = CARTESIAN_POINT ( 'NONE',  ( -1.339745962155613812, -37.08034179853029144, -5.000000000000000000 ) ) ;
#52594 = CARTESIAN_POINT ( 'NONE',  ( -4.458734124999999437, 0.6875000013655957476, 0.000000000000000000 ) ) ;
#52595 = CARTESIAN_POINT ( 'NONE',  ( -6.972266317189433020E-16, -45.12499999726880162, -5.000000000000000000 ) ) ;
#52596 = FACE_OUTER_BOUND ( 'NONE', #56475, .T. ) ;
#52597 = CARTESIAN_POINT ( 'NONE',  ( 4.458734125000001214, 11.85416666803225993, 2.574251347313718519 ) ) ;
#52598 = ORIENTED_EDGE ( 'NONE', *, *, #45601, .T. ) ;
#52599 = CARTESIAN_POINT ( 'NONE',  ( 0.000000000000000000, -120.0000000000000000, 5.000000000000000000 ) ) ;
#52600 = ORIENTED_EDGE ( 'NONE', *, *, #9817, .T. ) ;
#52601 = CARTESIAN_POINT ( 'NONE',  ( -6.972266317189433020E-16, -7.124999997268814056, -5.000000000000000000 ) ) ;
#52602 = CARTESIAN_POINT ( 'NONE',  ( 2.229367062499998831, -46.64583333196774362, -3.861377020970580887 ) ) ;
#52603 = CARTESIAN_POINT ( 'NONE',  ( -1.846868145590737420, -161.0000000013656063, 4.458734124999999437 ) ) ;
#52604 = CARTESIAN_POINT ( 'NONE',  ( -5.000000000000000000, -50.87499999726881583, 0.000000000000000000 ) ) ;
#52605 = VERTEX_POINT ( 'NONE', #22220 ) ;
#52606 = CARTESIAN_POINT ( 'NONE',  ( -4.458734124999998549, -22.22916666530107221, 2.574251347313722516 ) ) ;
#52607 = ORIENTED_EDGE ( 'NONE', *, *, #16429, .F. ) ;
#52608 = CARTESIAN_POINT ( 'NONE',  ( 5.000000000000000888, -34.58333333333332860, 2.886751345948126879 ) ) ;
#52609 = CARTESIAN_POINT ( 'NONE',  ( 3.152801135295367541, -162.3125000013656063, -3.152801135295367541 ) ) ;
#52610 = CARTESIAN_POINT ( 'NONE',  ( 0.000000000000000000, -120.0000000000000000, 0.000000000000000000 ) ) ;
#52611 = CARTESIAN_POINT ( 'NONE',  ( -59.81910112700025905, -136.1875000000000000, -2.462841084822630311 ) ) ;
#52612 = CARTESIAN_POINT ( 'NONE',  ( 9.457646018065525792E-16, -35.31249999863440792, 5.148502694627439702 ) ) ;
#52613 = ORIENTED_EDGE ( 'NONE', *, *, #29018, .T. ) ;
#52614 = CARTESIAN_POINT ( 'NONE',  ( -2.229367062499996610, -83.14583333196773651, 3.861377020970582219 ) ) ;
#52615 = CARTESIAN_POINT ( 'NONE',  ( 4.458734124999998549, 23.27083333469892423, -2.574251347313721627 ) ) ;
#52616 = CARTESIAN_POINT ( 'NONE',  ( -2.499999999999996447, -17.70833333060214443, 4.330127018922195425 ) ) ;
#52617 =( BOUNDED_CURVE ( )  B_SPLINE_CURVE ( 2, ( #56904, #7062, #32121, #6742, #2251, #21855, #41450, #45972, #1937 ),
 .UNSPECIFIED., .F., .F. ) 
 B_SPLINE_CURVE_WITH_KNOTS ( ( 3, 2, 2, 2, 3 ),
 ( 0.3916666666666669960, 0.3958333333333336479, 0.4000000000000003553, 0.4041666666666670071, 0.4083333333333336590 ),
 .UNSPECIFIED. ) 
 CURVE ( )  GEOMETRIC_REPRESENTATION_ITEM ( )  RATIONAL_B_SPLINE_CURVE ( ( 0.9999999999999938938, 0.9238795325112928447, 1.000000000000000000, 0.9238795325112867385, 1.000000000000000000, 0.9238795325112867385, 1.000000000000000000, 0.9238795325112806323, 1.000000000000005995 ) ) 
 REPRESENTATION_ITEM ( '' )  );
#52618 = EDGE_LOOP ( 'NONE', ( #9272, #41852, #8690, #39474 ) ) ;
#52619 = CARTESIAN_POINT ( 'NONE',  ( -50.40829686548195099, -138.2500000013656063, -1.485763867205728284 ) ) ;
#52620 = CARTESIAN_POINT ( 'NONE',  ( 4.458734124999999437, -86.06249999863439371, -5.460374474430324690E-16 ) ) ;
#52621 = CARTESIAN_POINT ( 'NONE',  ( -50.18089887299979068, -124.8125000027312126, 2.462841084822635640 ) ) ;
#52622 = DIRECTION ( 'NONE',  ( -1.000000000000000000, 0.000000000000000000, 0.000000000000000000 ) ) ;
#52623 = CARTESIAN_POINT ( 'NONE',  ( -6.972266317189433020E-16, 2.875000002731185500, -5.000000000000000000 ) ) ;
#52624 =( BOUNDED_CURVE ( )  B_SPLINE_CURVE ( 2, ( #30973, #26474, #12318, #2666, #41561, #31282, #61852, #7182, #55746 ),
 .UNSPECIFIED., .F., .F. ) 
 B_SPLINE_CURVE_WITH_KNOTS ( ( 3, 2, 2, 2, 3 ),
 ( 0.9812499999999999556, 0.9819444444444443976, 0.9833333333333332815, 0.9847222222222222765, 0.9854166666666667185 ),
 .UNSPECIFIED. ) 
 CURVE ( )  GEOMETRIC_REPRESENTATION_ITEM ( )  RATIONAL_B_SPLINE_CURVE ( ( 0.9330127018922194093, 0.9330127018922194093, 1.000000000000000000, 0.8660254037844387076, 1.000000000000000000, 0.8660254037844387076, 1.000000000000000000, 0.9330127018922194093, 0.9330127018922194093 ) ) 
 REPRESENTATION_ITEM ( '' )  );
#52625 = CARTESIAN_POINT ( 'NONE',  ( 5.000000000000000000, -57.49999999999999289, -6.123233995736766282E-16 ) ) ;
#52626 = CARTESIAN_POINT ( 'NONE',  ( -2.229367062500000163, -60.47916666530106511, -3.861377020970580443 ) ) ;
#52627 = CARTESIAN_POINT ( 'NONE',  ( 1.339745962155612702, -37.29465819873852439, -5.000000000000000000 ) ) ;
#52628 = CARTESIAN_POINT ( 'NONE',  ( 4.458734124999998549, 21.27083333469892779, -2.574251347313721627 ) ) ;
#52629 = DIRECTION ( 'NONE',  ( -0.000000000000000000, 1.000000000000000000, -0.000000000000000000 ) ) ;
#52630 = CARTESIAN_POINT ( 'NONE',  ( -4.999999999999998224, -43.91666666666665719, 2.886751345948131764 ) ) ;
#52631 = CARTESIAN_POINT ( 'NONE',  ( -2.229367062500000163, -42.72916666530107932, -3.861377020970580443 ) ) ;
#52632 = CARTESIAN_POINT ( 'NONE',  ( 2.500000000000002220, -6.541666663935481019, 4.330127018922192761 ) ) ;
#52633 = DIRECTION ( 'NONE',  ( 0.000000000000000000, 0.000000000000000000, 1.000000000000000000 ) ) ;
#52634 = CARTESIAN_POINT ( 'NONE',  ( -59.29741812935640155, -126.6250000013656489, -2.196230717870135685 ) ) ;
#52635 = CARTESIAN_POINT ( 'NONE',  ( 2.229367062500001939, -83.22916666530106511, 3.861377020970579999 ) ) ;
#52636 = CARTESIAN_POINT ( 'NONE',  ( -3.152548672688508926E-16, -104.5624999986343937, -5.148502694627439702 ) ) ;
#52637 = CARTESIAN_POINT ( 'NONE',  ( -2.229367062499996610, -8.395833331967736513, 3.861377020970582219 ) ) ;
#52638 = EDGE_LOOP ( 'NONE', ( #7503, #9889, #57988, #15524 ) ) ;
#52639 = CARTESIAN_POINT ( 'NONE',  ( -5.000000000000000000, 18.04166666939785557, -2.886751345948128211 ) ) ;
#52640 = CARTESIAN_POINT ( 'NONE',  ( -4.458734124999998549, -93.22916666530107932, 2.574251347313722516 ) ) ;
#52641 = CARTESIAN_POINT ( 'NONE',  ( -5.000000000000000888, -166.6875000027311842, -2.071067811865475949 ) ) ;
#52642 = CARTESIAN_POINT ( 'NONE',  ( -4.458734124999999437, -94.56249999863440792, 0.000000000000000000 ) ) ;
#52643 = ADVANCED_FACE ( 'NONE', ( #17396 ), #56640, .F. ) ;
#52644 = CARTESIAN_POINT ( 'NONE',  ( 2.499999999999998668, -50.20833333060213732, -4.330127018922193649 ) ) ;
#52645 = CARTESIAN_POINT ( 'NONE',  ( 6.123233995736766282E-16, -120.0000000000000000, -5.000000000000000000 ) ) ;
#52646 = CARTESIAN_POINT ( 'NONE',  ( -56.48576386720575471, -128.7500000013656063, -4.591703134518078322 ) ) ;
#52647 = CARTESIAN_POINT ( 'NONE',  ( 2.229367062500001939, -14.97916666530107399, 3.861377020970579999 ) ) ;
#52648 = CARTESIAN_POINT ( 'NONE',  ( -2.229367062500000163, 13.27083333469892779, -3.861377020970580443 ) ) ;
#52649 = CARTESIAN_POINT ( 'NONE',  ( -2.229367062499996610, -54.39583333196773651, 3.861377020970582219 ) ) ;
#52650 = CARTESIAN_POINT ( 'NONE',  ( 1.339745962155615144, -86.58034179853028434, 4.999999999999999112 ) ) ;
#52651 = CARTESIAN_POINT ( 'NONE',  ( -3.535533905932738641, -152.3750000000000000, 3.535533905932737309 ) ) ;
#52652 = CARTESIAN_POINT ( 'NONE',  ( -4.458734124999999437, -12.39583333196774184, -2.574251347313719407 ) ) ;
#52653 = FACE_OUTER_BOUND ( 'NONE', #6199, .T. ) ;
#52654 = ORIENTED_EDGE ( 'NONE', *, *, #31628, .T. ) ;
#52655 = CARTESIAN_POINT ( 'NONE',  ( -2.229367062499996610, -39.39583333196773651, 3.861377020970582219 ) ) ;
#52656 = CARTESIAN_POINT ( 'NONE',  ( 5.000000000000000000, -77.41666666666665719, -2.886751345948130876 ) ) ;
#52657 = CARTESIAN_POINT ( 'NONE',  ( -5.926426369611017623E-15, 26.37500000273118417, 5.000000000000000000 ) ) ;
#52658 = EDGE_CURVE ( 'NONE', #11867, #49354, #49839, .T. ) ;
#52659 = DIRECTION ( 'NONE',  ( -0.000000000000000000, 1.000000000000000000, -0.000000000000000000 ) ) ;
#52660 = CARTESIAN_POINT ( 'NONE',  ( -3.152548672688508926E-16, -86.56249999863440792, -5.148502694627439702 ) ) ;
#52661 = CARTESIAN_POINT ( 'NONE',  ( -4.458734124999999437, 25.35416666803225993, -2.574251347313719407 ) ) ;
#52662 = CARTESIAN_POINT ( 'NONE',  ( -3.152548672688508926E-16, 16.43750000136559564, -5.148502694627439702 ) ) ;
#52663 = CARTESIAN_POINT ( 'NONE',  ( 1.975475456537005874E-15, -85.62499999726880162, 5.000000000000000000 ) ) ;
#52664 = EDGE_CURVE ( 'NONE', #34612, #15531, #58484, .T. ) ;
#52665 = CARTESIAN_POINT ( 'NONE',  ( 0.000000000000000000, -170.0000000000000000, 0.000000000000000000 ) ) ;
#52666 = CARTESIAN_POINT ( 'NONE',  ( -2.229367062499996610, -82.39583333196773651, 3.861377020970582219 ) ) ;
#52667 = CARTESIAN_POINT ( 'NONE',  ( -2.499999999999996447, -68.83333333333332860, 4.330127018922195425 ) ) ;
#52668 = CARTESIAN_POINT ( 'NONE',  ( -2.500000000000000444, 14.95833333606451809, -4.330127018922193649 ) ) ;
#52669 = ORIENTED_EDGE ( 'NONE', *, *, #46485, .F. ) ;
#52670 = CARTESIAN_POINT ( 'NONE',  ( 2.500000000000002220, -35.66666666666666430, 4.330127018922192761 ) ) ;
#52671 = CARTESIAN_POINT ( 'NONE',  ( 2.493747252781420335E-13, -90.25000000000000000, -5.000000000000000000 ) ) ;
#52672 =( BOUNDED_CURVE ( )  B_SPLINE_CURVE ( 2, ( #10229, #11180, #34671, #30803, #5406, #59768, #30476, #16009, #40446 ),
 .UNSPECIFIED., .F., .F. ) 
 B_SPLINE_CURVE_WITH_KNOTS ( ( 3, 2, 2, 2, 3 ),
 ( 0.4303571428571428825, 0.4309523809523809756, 0.4321428571428571619, 0.4333333333333333481, 0.4339285714285714413 ),
 .UNSPECIFIED. ) 
 CURVE ( )  GEOMETRIC_REPRESENTATION_ITEM ( )  RATIONAL_B_SPLINE_CURVE ( ( 0.9330127018922194093, 0.9330127018922194093, 1.000000000000000000, 0.8660254037844387076, 1.000000000000000000, 0.8660254037844387076, 1.000000000000000000, 0.9330127018922194093, 0.9330127018922194093 ) ) 
 REPRESENTATION_ITEM ( '' )  );
#52674 = CARTESIAN_POINT ( 'NONE',  ( 2.500000000000002220, -31.66666666666666075, 4.330127018922192761 ) ) ;
#52673 = CARTESIAN_POINT ( 'NONE',  ( -1.339745962155610925, -71.79465819873850307, 5.000000000000000000 ) ) ;
#52675 = CARTESIAN_POINT ( 'NONE',  ( 9.457646018065525792E-16, -31.06249999863440436, 5.148502694627439702 ) ) ;
#52676 = CARTESIAN_POINT ( 'NONE',  ( 0.000000000000000000, -170.0000000000000000, 0.000000000000000000 ) ) ;
#52677 = CARTESIAN_POINT ( 'NONE',  ( 2.499999999999998668, -35.20833333060213732, -4.330127018922193649 ) ) ;
#52679 = VERTEX_POINT ( 'NONE', #57889 ) ;
#52678 = CARTESIAN_POINT ( 'NONE',  ( 2.229367062500001939, -60.97916666530106511, 3.861377020970579999 ) ) ;
#52680 = CARTESIAN_POINT ( 'NONE',  ( -55.35523342533222291, -154.5625000013656347, 4.444560631937231499 ) ) ;
#52682 = ORIENTED_EDGE ( 'NONE', *, *, #2082, .T. ) ;
#52681 = CARTESIAN_POINT ( 'NONE',  ( 4.458734125000001214, -7.145833331967734736, 2.574251347313718519 ) ) ;
#52683 = CARTESIAN_POINT ( 'NONE',  ( -4.999999999999999112, -76.91666666666667140, 2.886751345948131764 ) ) ;
#52684 = CARTESIAN_POINT ( 'NONE',  ( -7.500000000000000000, 4.330127018922191873, -10.00000000000000000 ) ) ;
#52685 = CARTESIAN_POINT ( 'NONE',  ( -2.229367062500000163, -49.72916666530107221, -3.861377020970580443 ) ) ;
#52686 = CARTESIAN_POINT ( 'NONE',  ( -5.000000000000000000, -74.87499999726880162, 0.000000000000000000 ) ) ;
#52687 = EDGE_LOOP ( 'NONE', ( #1141, #33610, #23791, #43539 ) ) ;
#52688 = CARTESIAN_POINT ( 'NONE',  ( -51.75738570946856498, -147.7500000000000284, 3.805975901505576964 ) ) ;
#52689 = EDGE_CURVE ( 'NONE', #52296, #21524, #19027, .T. ) ;
#52690 = CARTESIAN_POINT ( 'NONE',  ( -4.458734124999999437, -19.56249999863440081, 0.000000000000000000 ) ) ;
#52692 = ORIENTED_EDGE ( 'NONE', *, *, #25193, .F. ) ;
#52691 = CARTESIAN_POINT ( 'NONE',  ( -2.229367062499996610, -55.39583333196773651, 3.861377020970582219 ) ) ;
#52693 = CARTESIAN_POINT ( 'NONE',  ( -1.846868145590737420, -168.0000000013655779, 4.458734124999999437 ) ) ;
#52694 = CARTESIAN_POINT ( 'NONE',  ( 4.458734124999999437, -102.0624999986344079, -5.460374474430324690E-16 ) ) ;
#52695 = CARTESIAN_POINT ( 'NONE',  ( -2.499999999999996447, -26.70833333060214798, 4.330127018922195425 ) ) ;
#52696 = ADVANCED_FACE ( 'NONE', ( #9298 ), #8676, .T. ) ;
#52697 = ORIENTED_EDGE ( 'NONE', *, *, #39080, .T. ) ;
#52698 = CARTESIAN_POINT ( 'NONE',  ( -56.48576386720575471, -152.0000000013656063, -4.591703134518078322 ) ) ;
#52699 = CARTESIAN_POINT ( 'NONE',  ( -59.98410592259440222, -142.2500000027312126, -0.3983568153799752487 ) ) ;
#52700 = CARTESIAN_POINT ( 'NONE',  ( 1.975475456537005874E-15, 1.375000002731185500, 5.000000000000000000 ) ) ;
#52701 = CARTESIAN_POINT ( 'NONE',  ( -3.152548672688508926E-16, -9.562499998634406140, -5.148502694627439702 ) ) ;
#52702 = CARTESIAN_POINT ( 'NONE',  ( 9.457646018065525792E-16, -99.31249999863439371, 5.148502694627439702 ) ) ;
#52703 = B_SPLINE_CURVE_WITH_KNOTS ( 'NONE', 3,
 ( #35581, #54564, #60358, #25610, #11125, #55535 ),
 .UNSPECIFIED., .F., .F.,
 ( 4, 2, 4 ),
 ( 0.004444412883774350592, 0.006655097293744440673, 0.008865781703714530754 ),
 .UNSPECIFIED. ) ;
#52704 = CARTESIAN_POINT ( 'NONE',  ( -3.152801135295367985, -146.0625000013655779, 3.152801135295367096 ) ) ;
#52705 = CARTESIAN_POINT ( 'NONE',  ( -4.458734124999999437, -26.56249999863440792, 0.000000000000000000 ) ) ;
#52706 = CARTESIAN_POINT ( 'NONE',  ( -1.339745962155610925, 12.20534180126148094, 5.000000000000000000 ) ) ;
#52707 = CARTESIAN_POINT ( 'NONE',  ( -50.55543936806279248, -136.0625000013656063, 0.3552334253322060320 ) ) ;
#52708 = CARTESIAN_POINT ( 'NONE',  ( -4.458734124999998549, -70.47916666530107932, 2.574251347313722516 ) ) ;
#52709 = LINE ( 'NONE', #43051, #42520 ) ;
#52710 = CARTESIAN_POINT ( 'NONE',  ( 5.000000000000000888, -88.45833333060214443, 2.886751345948126879 ) ) ;
#52711 = CARTESIAN_POINT ( 'NONE',  ( 4.458734124999997661, -139.5000000013655779, 1.846868145590737864 ) ) ;
#52712 = CARTESIAN_POINT ( 'NONE',  ( 2.229367062500001939, 7.770833334698926009, 3.861377020970579999 ) ) ;
#52713 = ORIENTED_EDGE ( 'NONE', *, *, #2516, .F. ) ;
#52714 = PRESENTATION_STYLE_ASSIGNMENT (( #24388 ) ) ;
#52715 = CARTESIAN_POINT ( 'NONE',  ( 2.499999999999998668, 2.666666666666667851, -4.330127018922193649 ) ) ;
#52717 = CARTESIAN_POINT ( 'NONE',  ( -3.152548672688508926E-16, -26.56249999863440792, -5.148502694627439702 ) ) ;
#52716 = CARTESIAN_POINT ( 'NONE',  ( 5.000000000000000888, -91.58333333333332860, 2.886751345948126879 ) ) ;
#52718 = CARTESIAN_POINT ( 'NONE',  ( 5.000000000000000888, -14.45833333060214976, 2.886751345948126879 ) ) ;
#52719 = CARTESIAN_POINT ( 'NONE',  ( 4.458734124999999437, -75.06249999863440792, -5.460374474430324690E-16 ) ) ;
#52720 = CARTESIAN_POINT ( 'NONE',  ( -4.458734124999999437, 22.35416666803225638, -2.574251347313719407 ) ) ;
#52721 = DIRECTION ( 'NONE',  ( 0.000000000000000000, 1.000000000000000000, 0.000000000000000000 ) ) ;
#52722 = CARTESIAN_POINT ( 'NONE',  ( -57.89159099828107458, -142.6875000013656063, -3.393966926194107447 ) ) ;
#52723 = ADVANCED_FACE ( 'NONE', ( #18944 ), #9614, .T. ) ;
#52724 = ADVANCED_FACE ( 'NONE', ( #28914 ), #38267, .T. ) ;
#52725 = CARTESIAN_POINT ( 'NONE',  ( -4.458734124999999437, 5.604166668032261711, -2.574251347313719407 ) ) ;
#52726 = CARTESIAN_POINT ( 'NONE',  ( -2.229367062499996610, 26.60416666803225993, 3.861377020970582219 ) ) ;
#52727 = CARTESIAN_POINT ( 'NONE',  ( -2.229367062500000163, -39.72916666530107221, -3.861377020970580443 ) ) ;
#52729 = EDGE_CURVE ( 'NONE', #3491, #12628, #43392, .T. ) ;
#52728 = CYLINDRICAL_SURFACE ( 'NONE', #26412, 5.000000000000000000 ) ;
#52730 = CARTESIAN_POINT ( 'NONE',  ( -2.229367062499996610, 7.854166668032260823, 3.861377020970582219 ) ) ;
#52731 = CARTESIAN_POINT ( 'NONE',  ( 4.458734124999999437, -72.81249999863439371, -5.460374474430324690E-16 ) ) ;
#52732 = CARTESIAN_POINT ( 'NONE',  ( 4.458734125000000326, -21.14583333196774362, 2.574251347313718519 ) ) ;
#52733 = CARTESIAN_POINT ( 'NONE',  ( -5.000000000000000000, -6.083333333333336590, -2.886751345948128211 ) ) ;
#52734 = CARTESIAN_POINT ( 'NONE',  ( -1.846868145590734756, -157.1250000013656063, -4.458734125000000326 ) ) ;
#52735 = CARTESIAN_POINT ( 'NONE',  ( 0.000000000000000000, -170.0000000000000000, 0.000000000000000000 ) ) ;
#52736 = CARTESIAN_POINT ( 'NONE',  ( 2.229367062500001939, -65.97916666530106511, 3.861377020970579999 ) ) ;
#52737 = CARTESIAN_POINT ( 'NONE',  ( 1.060575238724906964E-15, -100.6249999972688158, 5.773502691896257311 ) ) ;
#52738 = ADVANCED_FACE ( 'NONE', ( #19581 ), #52302, .T. ) ;
#52739 = CARTESIAN_POINT ( 'NONE',  ( -4.458734124999998549, 28.77083333469892779, 2.574251347313722516 ) ) ;
#52740 = CARTESIAN_POINT ( 'NONE',  ( -2.229367062499996610, -41.14583333196773651, 3.861377020970582219 ) ) ;
#52741 = CARTESIAN_POINT ( 'NONE',  ( 1.975475456537005874E-15, -46.62499999726880873, 5.000000000000000000 ) ) ;
#52742 = ADVANCED_FACE ( 'NONE', ( #15927 ), #34910, .T. ) ;
#52743 = CARTESIAN_POINT ( 'NONE',  ( 2.229367062499998831, -105.8958333319677365, -3.861377020970580887 ) ) ;
#52744 = CARTESIAN_POINT ( 'NONE',  ( 4.458734125000000326, -69.14583333196773651, 2.574251347313718519 ) ) ;
#52745 = CARTESIAN_POINT ( 'NONE',  ( 5.000000000000000888, -56.58333333333332860, 2.886751345948126879 ) ) ;
#52746 = CARTESIAN_POINT ( 'NONE',  ( 5.000000000000000888, -57.45833333060214443, 2.886751345948126879 ) ) ;
#52747 = CARTESIAN_POINT ( 'NONE',  ( 2.071067811865603403, -156.3125000027311842, 4.999999999999872990 ) ) ;
#52748 = VERTEX_POINT ( 'NONE', #54532 ) ;
#52749 = DIRECTION ( 'NONE',  ( -0.000000000000000000, 1.000000000000000000, -0.000000000000000000 ) ) ;
#52750 = CARTESIAN_POINT ( 'NONE',  ( 5.000000000000000000, -15.41666666666666963, -2.886751345948129988 ) ) ;
#52751 = CARTESIAN_POINT ( 'NONE',  ( 4.458734125000001214, -17.89583333196774007, 2.574251347313718519 ) ) ;
#52752 = ADVANCED_FACE ( 'NONE', ( #34256 ), #63550, .T. ) ;
#52753 = CARTESIAN_POINT ( 'NONE',  ( 9.457646018065525792E-16, -77.06249999863440792, 5.148502694627439702 ) ) ;
#52754 =( BOUNDED_CURVE ( )  B_SPLINE_CURVE ( 2, ( #10586, #5451, #59170, #34390, #25069, #45010, #59822, #5771, #1298 ),
 .UNSPECIFIED., .F., .F. ) 
 B_SPLINE_CURVE_WITH_KNOTS ( ( 3, 2, 2, 2, 3 ),
 ( 0.1812499999999999944, 0.1819444444444444364, 0.1833333333333333204, 0.1847222222222222321, 0.1854166666666666741 ),
 .UNSPECIFIED. ) 
 CURVE ( )  GEOMETRIC_REPRESENTATION_ITEM ( )  RATIONAL_B_SPLINE_CURVE ( ( 0.9330127018922194093, 0.9330127018922194093, 1.000000000000000000, 0.8660254037844387076, 1.000000000000000000, 0.8660254037844387076, 1.000000000000000000, 0.9330127018922194093, 0.9330127018922194093 ) ) 
 REPRESENTATION_ITEM ( '' )  );
#52755 = CARTESIAN_POINT ( 'NONE',  ( 6.123233995736766282E-16, -170.0000000000000000, -5.000000000000000000 ) ) ;
#52756 = CARTESIAN_POINT ( 'NONE',  ( -2.499999999999996447, -13.70833333060214976, 4.330127018922195425 ) ) ;
#52758 = EDGE_LOOP ( 'NONE', ( #51659, #57498, #2498, #30518 ) ) ;
#52757 = CARTESIAN_POINT ( 'NONE',  ( 4.458734124999999437, -46.81249999863440792, -5.460374474430324690E-16 ) ) ;
#52759 = CARTESIAN_POINT ( 'NONE',  ( 5.000000000000000000, -100.3749999972688158, -6.123233995736766282E-16 ) ) ;
#52761 = ORIENTED_EDGE ( 'NONE', *, *, #2883, .T. ) ;
#52760 = CARTESIAN_POINT ( 'NONE',  ( -4.458734124999998549, 7.520833334698926009, 2.574251347313722516 ) ) ;
#52762 = CARTESIAN_POINT ( 'NONE',  ( -59.29741812935640155, -153.6250000013655779, -2.196230717870135685 ) ) ;
#52763 = CARTESIAN_POINT ( 'NONE',  ( 2.499999999999998668, -59.33333333333333570, -4.330127018922193649 ) ) ;
#52764 = CARTESIAN_POINT ( 'NONE',  ( -3.152801135295367985, -157.0625000013656063, 3.152801135295367096 ) ) ;
#52765 = CARTESIAN_POINT ( 'NONE',  ( -3.152548672688508926E-16, -33.81249999863440792, -5.148502694627439702 ) ) ;
#52766 = CARTESIAN_POINT ( 'NONE',  ( 1.339745962155612702, -14.29465819873851906, -5.000000000000000000 ) ) ;
#52767 = CARTESIAN_POINT ( 'NONE',  ( 3.061616997868383141E-16, -166.7500000000000000, -5.000000000000000000 ) ) ;
#52768 = CARTESIAN_POINT ( 'NONE',  ( 5.000000000000000000, -168.0625000000000000, 2.071067811865478614 ) ) ;
#52769 = CARTESIAN_POINT ( 'NONE',  ( -53.51423613279429503, -132.5000000013656063, 4.591703134518082763 ) ) ;
#52770 = CARTESIAN_POINT ( 'NONE',  ( -2.229367062500000163, -7.729166665301073991, -3.861377020970580443 ) ) ;
#52771 = CARTESIAN_POINT ( 'NONE',  ( -3.152548672688508926E-16, -40.81249999863440081, -5.148502694627439702 ) ) ;
#52772 = AXIS2_PLACEMENT_3D ( 'NONE', #62754, #53089, #32843 ) ;
#52773 = CARTESIAN_POINT ( 'NONE',  ( 5.000000000000000888, -83.45833333060213022, 2.886751345948126879 ) ) ;
#52774 = CARTESIAN_POINT ( 'NONE',  ( 1.846868145590736310, -152.6250000013655495, 4.458734124999999437 ) ) ;
#52775 = CARTESIAN_POINT ( 'NONE',  ( 9.457646018065525792E-16, -81.31249999863440792, 5.148502694627439702 ) ) ;
#52776 = CARTESIAN_POINT ( 'NONE',  ( 2.071067811865495045, -167.3125000027311842, 4.999999999999981348 ) ) ;
#52777 = ORIENTED_EDGE ( 'NONE', *, *, #62138, .T. ) ;
#52778 = CARTESIAN_POINT ( 'NONE',  ( -52.53715891517739323, -153.5625000027312410, -4.819101127000233298 ) ) ;
#52779 = CARTESIAN_POINT ( 'NONE',  ( -1.339745962155610925, -104.7946581987385315, 5.000000000000000000 ) ) ;
#52780 = CARTESIAN_POINT ( 'NONE',  ( 4.458734124999998549, -67.97916666530107932, -2.574251347313721627 ) ) ;
#52781 = CARTESIAN_POINT ( 'NONE',  ( 3.152801135295367541, -145.5625000013655779, -3.152801135295367541 ) ) ;
#52782 = ORIENTED_EDGE ( 'NONE', *, *, #44898, .T. ) ;
#52783 = CYLINDRICAL_SURFACE ( 'NONE', #23664, 5.000000000000000000 ) ;
#52784 = CARTESIAN_POINT ( 'NONE',  ( -4.458734124999998549, -12.47916666530107221, 2.574251347313722516 ) ) ;
#52785 = CARTESIAN_POINT ( 'NONE',  ( -2.500000000000000444, -35.16666666666666430, -4.330127018922193649 ) ) ;
#52786 = CARTESIAN_POINT ( 'NONE',  ( -4.458734124999998549, 3.770833334698929562, 2.574251347313722516 ) ) ;
#52787 = CARTESIAN_POINT ( 'NONE',  ( -2.500000000000000444, -96.04166666393548724, -4.330127018922193649 ) ) ;
#52788 = CARTESIAN_POINT ( 'NONE',  ( 2.730187237215162345E-16, -153.1875000013656063, -4.458734124999999437 ) ) ;
#52789 = CARTESIAN_POINT ( 'NONE',  ( 9.457646018065525792E-16, 28.68750000136559208, 5.148502694627439702 ) ) ;
#52790 = EDGE_LOOP ( 'NONE', ( #59092, #49576, #41078, #28719 ) ) ;
#52791 = CARTESIAN_POINT ( 'NONE',  ( -4.458734124999999437, -90.31249999863440792, 0.000000000000000000 ) ) ;
#52792 = CARTESIAN_POINT ( 'NONE',  ( -1.339745962155613812, -97.20534180126145429, -5.000000000000000000 ) ) ;
#52793 = CARTESIAN_POINT ( 'NONE',  ( 1.339745962155499015, -60.58034179853027723, 5.000000000000065725 ) ) ;
#52794 = CARTESIAN_POINT ( 'NONE',  ( 2.229367062500001939, -9.979166665301068662, 3.861377020970579999 ) ) ;
#52795 = CARTESIAN_POINT ( 'NONE',  ( -2.499999999999996447, 28.29166666939785202, 4.330127018922195425 ) ) ;
#52796 = CARTESIAN_POINT ( 'NONE',  ( -57.46284108482265651, -144.9375000000000000, 4.819101127000238627 ) ) ;
#52797 = CARTESIAN_POINT ( 'NONE',  ( -52.10840900171896806, -154.1875000013656063, 3.393966926194110556 ) ) ;
#52798 = EDGE_CURVE ( 'NONE', #27444, #58830, #60570, .T. ) ;
#52799 = CARTESIAN_POINT ( 'NONE',  ( 5.000000000000000000, -36.29166666393547303, -2.886751345948129988 ) ) ;
#52800 = CARTESIAN_POINT ( 'NONE',  ( 6.123233995736766282E-16, -170.0000000000000000, -5.000000000000000000 ) ) ;
#52801 = CARTESIAN_POINT ( 'NONE',  ( -2.229367062500000163, 20.52083333469892779, -3.861377020970580443 ) ) ;
#52802 = CARTESIAN_POINT ( 'NONE',  ( 4.458734124999999437, 24.18750000136559564, -5.460374474430324690E-16 ) ) ;
#52803 = CARTESIAN_POINT ( 'NONE',  ( -2.229367062499996610, -55.14583333196773651, 3.861377020970582219 ) ) ;
#52804 = CARTESIAN_POINT ( 'NONE',  ( 9.457646018065525792E-16, -2.312499998634407028, 5.148502694627439702 ) ) ;
#52805 = PLANE ( 'NONE',  #10314 ) ;
#52806 = CARTESIAN_POINT ( 'NONE',  ( 2.500000000000002220, 10.33333333333333393, 4.330127018922192761 ) ) ;
#52807 = CARTESIAN_POINT ( 'NONE',  ( -5.000000000000000888, -142.6875000027311842, -2.071067811865475949 ) ) ;
#52808 = CARTESIAN_POINT ( 'NONE',  ( 1.339745962155615144, -69.70534180126148271, 4.999999999999999112 ) ) ;
#52809 = CARTESIAN_POINT ( 'NONE',  ( -3.152548672688508926E-16, -50.56249999863440792, -5.148502694627439702 ) ) ;
#52810 = CARTESIAN_POINT ( 'NONE',  ( 2.500000000000002220, -81.54166666393547303, 4.330127018922192761 ) ) ;
#52811 = CARTESIAN_POINT ( 'NONE',  ( -52.80376928212989185, -134.1250000013656347, -4.297418129356379346 ) ) ;
#52812 = VECTOR ( 'NONE', #59020, 1000.000000000000000 ) ;
#52813 = CARTESIAN_POINT ( 'NONE',  ( -51.75738570946856498, -145.7500000000000284, 3.805975901505576964 ) ) ;
#52814 = CARTESIAN_POINT ( 'NONE',  ( -2.229367062499996610, -88.39583333196773651, 3.861377020970582219 ) ) ;
#52815 = CARTESIAN_POINT ( 'NONE',  ( 2.730187237215162345E-16, -158.4375000013655779, -4.458734124999999437 ) ) ;
#52816 = CARTESIAN_POINT ( 'NONE',  ( -5.000000000000000000, -38.08333333333333570, -2.886751345948128211 ) ) ;
#52817 = ORIENTED_EDGE ( 'NONE', *, *, #38485, .T. ) ;
#52818 = ADVANCED_FACE ( 'NONE', ( #39397 ), #59031, .T. ) ;
#52819 = CARTESIAN_POINT ( 'NONE',  ( -4.458734124999999437, 16.43750000136559564, 0.000000000000000000 ) ) ;
#52820 = ORIENTED_EDGE ( 'NONE', *, *, #45714, .T. ) ;
#52821 = CARTESIAN_POINT ( 'NONE',  ( -4.458734124999998549, -96.22916666530106511, 2.574251347313722516 ) ) ;
#52822 = CARTESIAN_POINT ( 'NONE',  ( 4.458734124999998549, 6.020833334698928674, -2.574251347313721627 ) ) ;
#52823 = CARTESIAN_POINT ( 'NONE',  ( 1.060575238724906964E-15, 13.37500000273118594, 5.773502691896257311 ) ) ;
#52824 =( BOUNDED_CURVE ( )  B_SPLINE_CURVE ( 2, ( #48978, #29344, #34491, #38388, #14883, #29037, #4927, #34835, #43207 ),
 .UNSPECIFIED., .F., .F. ) 
 B_SPLINE_CURVE_WITH_KNOTS ( ( 3, 2, 2, 2, 3 ),
 ( 0.7604166666666666297, 0.7611111111111110716, 0.7624999999999999556, 0.7638888888888888395, 0.7645833333333332815 ),
 .UNSPECIFIED. ) 
 CURVE ( )  GEOMETRIC_REPRESENTATION_ITEM ( )  RATIONAL_B_SPLINE_CURVE ( ( 0.9330127018922194093, 0.9330127018922194093, 1.000000000000000000, 0.8660254037844387076, 1.000000000000000000, 0.8660254037844387076, 1.000000000000000000, 0.9330127018922194093, 0.9330127018922194093 ) ) 
 REPRESENTATION_ITEM ( '' )  );
#52825 = CARTESIAN_POINT ( 'NONE',  ( 0.000000000000000000, -170.0000000000000000, 0.000000000000000000 ) ) ;
#52826 = EDGE_CURVE ( 'NONE', #19379, #46887, #10012, .T. ) ;
#52827 = CARTESIAN_POINT ( 'NONE',  ( 2.500000000000002220, 4.333333333333331261, 4.330127018922192761 ) ) ;
#52828 = CARTESIAN_POINT ( 'NONE',  ( 4.458734124999998549, -60.72916666530106511, -2.574251347313721627 ) ) ;
#52829 = CARTESIAN_POINT ( 'NONE',  ( -2.500000000000000444, -53.04166666393548013, -4.330127018922193649 ) ) ;
#52830 = EDGE_CURVE ( 'NONE', #21155, #59659, #4208, .T. ) ;
#52831 = CARTESIAN_POINT ( 'NONE',  ( 2.499999999999998668, 2.791666669397851130, -4.330127018922193649 ) ) ;
#52832 = CARTESIAN_POINT ( 'NONE',  ( 4.458734124999998549, -28.72916666530107221, -2.574251347313721627 ) ) ;
#52833 = CARTESIAN_POINT ( 'NONE',  ( -5.000000000000000000, -42.08333333333333570, -2.886751345948128211 ) ) ;
#52834 = CARTESIAN_POINT ( 'NONE',  ( 1.975475456537005874E-15, -56.75000000000000000, 5.000000000000000000 ) ) ;
#52835 = DIRECTION ( 'NONE',  ( 0.000000000000000000, 0.000000000000000000, 1.000000000000000000 ) ) ;
#52836 = CARTESIAN_POINT ( 'NONE',  ( 2.500000000000002220, -42.66666666666667140, 4.330127018922192761 ) ) ;
#52838 = CARTESIAN_POINT ( 'NONE',  ( 2.229367062499998831, -19.89583333196774007, -3.861377020970580887 ) ) ;
#52837 = CARTESIAN_POINT ( 'NONE',  ( 2.500000000000002220, -26.54166666393547658, 4.330127018922192761 ) ) ;
#52839 = CARTESIAN_POINT ( 'NONE',  ( -2.498395430326213474E-14, 14.37500000273118417, 5.000000000000000000 ) ) ;
#52840 = CARTESIAN_POINT ( 'NONE',  ( 2.229367062500001939, -63.97916666530106511, 3.861377020970579999 ) ) ;
#52841 = CARTESIAN_POINT ( 'NONE',  ( -3.152801135295367096, -146.3125000013655779, -3.152801135295367541 ) ) ;
#52842 = CARTESIAN_POINT ( 'NONE',  ( -2.229367062500000163, -76.47916666530106511, -3.861377020970580443 ) ) ;
#52843 = CARTESIAN_POINT ( 'NONE',  ( -59.44456063193725015, -143.8125000013656063, -0.3552334253322034230 ) ) ;
#52844 = CARTESIAN_POINT ( 'NONE',  ( 2.229367062500001939, -27.22916666530106866, 3.861377020970579999 ) ) ;
#52845 = CARTESIAN_POINT ( 'NONE',  ( 1.060575238724906964E-15, -64.62499999726881583, 5.773502691896257311 ) ) ;
#52846 = VERTEX_POINT ( 'NONE', #12919 ) ;
#52847 = CARTESIAN_POINT ( 'NONE',  ( 5.000000000000000000, -1.416666666666663410, -2.886751345948130876 ) ) ;
#52848 = VERTEX_POINT ( 'NONE', #62464 ) ;
#52849 = CARTESIAN_POINT ( 'NONE',  ( 2.229367062499998831, -68.89583333196773651, -3.861377020970580887 ) ) ;
#52850 = CARTESIAN_POINT ( 'NONE',  ( 1.975475456537005874E-15, -9.624999997268814056, 5.000000000000000000 ) ) ;
#52851 = CARTESIAN_POINT ( 'NONE',  ( 1.975475456537005874E-15, -5.624999997268812280, 5.000000000000000000 ) ) ;
#52852 = ORIENTED_EDGE ( 'NONE', *, *, #21385, .T. ) ;
#52853 =( BOUNDED_CURVE ( )  B_SPLINE_CURVE ( 2, ( #20672, #60233, #45420, #55720, #55078, #21299, #60862, #6193, #25807 ),
 .UNSPECIFIED., .F., .F. ) 
 B_SPLINE_CURVE_WITH_KNOTS ( ( 3, 2, 2, 2, 3 ),
 ( 0.1979166666666666574, 0.1986111111111110994, 0.2000000000000000111, 0.2013888888888888951, 0.2020833333333333370 ),
 .UNSPECIFIED. ) 
 CURVE ( )  GEOMETRIC_REPRESENTATION_ITEM ( )  RATIONAL_B_SPLINE_CURVE ( ( 0.9330127018922194093, 0.9330127018922194093, 1.000000000000000000, 0.8660254037844387076, 1.000000000000000000, 0.8660254037844387076, 1.000000000000000000, 0.9330127018922194093, 0.9330127018922194093 ) ) 
 REPRESENTATION_ITEM ( '' )  );
#52854 = DIRECTION ( 'NONE',  ( -0.000000000000000000, 1.000000000000000000, -0.000000000000000000 ) ) ;
#52855 = CARTESIAN_POINT ( 'NONE',  ( -4.458734124999999437, -53.56249999863439371, 0.000000000000000000 ) ) ;
#52856 = CARTESIAN_POINT ( 'NONE',  ( 2.229367062500001939, 2.770833334698928674, 3.861377020970579999 ) ) ;
#52857 = ORIENTED_EDGE ( 'NONE', *, *, #11365, .T. ) ;
#52858 = VECTOR ( 'NONE', #63048, 1000.000000000000000 ) ;
#52859 = CARTESIAN_POINT ( 'NONE',  ( -6.972266317189433020E-16, 1.875000002731185722, -5.000000000000000000 ) ) ;
#52860 = CARTESIAN_POINT ( 'NONE',  ( 2.229367062499998831, 1.354166668032261933, -3.861377020970580887 ) ) ;
#52861 = CARTESIAN_POINT ( 'NONE',  ( -4.458734124999998549, 19.77083333469892779, 2.574251347313722516 ) ) ;
#52862 = CARTESIAN_POINT ( 'NONE',  ( -50.70258187064364108, -144.1250000013656063, 2.196230717870141014 ) ) ;
#52863 = CARTESIAN_POINT ( 'NONE',  ( 1.975475456537005874E-15, -92.62499999726881583, 5.000000000000000000 ) ) ;
#52864 = CARTESIAN_POINT ( 'NONE',  ( -4.458734124999999437, -165.0000000013655779, -1.846868145590735644 ) ) ;
#52865 = ORIENTED_EDGE ( 'NONE', *, *, #5603, .T. ) ;
#52866 = CARTESIAN_POINT ( 'NONE',  ( 9.457646018065525792E-16, -78.06249999863440792, 5.148502694627439702 ) ) ;
#52867 = CARTESIAN_POINT ( 'NONE',  ( 1.975475456537005874E-15, -85.62499999726880162, 5.000000000000000000 ) ) ;
#52868 = CARTESIAN_POINT ( 'NONE',  ( 4.458734124999999437, 8.187500001365595637, -5.460374474430324690E-16 ) ) ;
#52869 = EDGE_CURVE ( 'NONE', #51190, #58682, #16983, .T. ) ;
#52870 = DIRECTION ( 'NONE',  ( -0.000000000000000000, 1.000000000000000000, -0.000000000000000000 ) ) ;
#52871 = CARTESIAN_POINT ( 'NONE',  ( 2.229367062500001939, -58.22916666530107932, 3.861377020970579999 ) ) ;
#52872 = CARTESIAN_POINT ( 'NONE',  ( -2.500000000000000444, -20.04166666393548013, -4.330127018922193649 ) ) ;
#52873 = CARTESIAN_POINT ( 'NONE',  ( 1.975475456537005874E-15, 6.249999999999998224, 5.000000000000000000 ) ) ;
#52874 = CARTESIAN_POINT ( 'NONE',  ( 1.975475456537005874E-15, -42.62499999726880873, 5.000000000000000000 ) ) ;
#52875 = DIRECTION ( 'NONE',  ( 0.000000000000000000, 0.000000000000000000, 1.000000000000000000 ) ) ;
#52876 = CARTESIAN_POINT ( 'NONE',  ( 75.00000000000002842, 15.00000000000000000, -5.000000000000000000 ) ) ;
#52877 = CARTESIAN_POINT ( 'NONE',  ( -2.229367062500000163, -39.47916666530107221, -3.861377020970580443 ) ) ;
#52878 = CARTESIAN_POINT ( 'NONE',  ( 2.229367062500001939, -26.22916666530106866, 3.861377020970579999 ) ) ;
#52879 = DIRECTION ( 'NONE',  ( -0.000000000000000000, 1.000000000000000000, -0.000000000000000000 ) ) ;
#52880 = CARTESIAN_POINT ( 'NONE',  ( -3.535250795749689387E-16, 24.75000000000000355, -5.773502691896257311 ) ) ;
#52881 = CARTESIAN_POINT ( 'NONE',  ( -5.000000000000000888, -151.6875000027312126, -2.071067811865475949 ) ) ;
#52882 = ORIENTED_EDGE ( 'NONE', *, *, #7242, .T. ) ;
#52884 = AXIS2_PLACEMENT_3D ( 'NONE', #19845, #20812, #59739 ) ;
#52883 = CARTESIAN_POINT ( 'NONE',  ( 9.457646018065525792E-16, -109.3124999986343937, 5.148502694627439702 ) ) ;
#52885 = CARTESIAN_POINT ( 'NONE',  ( -2.229367062500000163, -30.47916666530107221, -3.861377020970580443 ) ) ;
#52886 = CARTESIAN_POINT ( 'NONE',  ( 5.000000000000000888, -69.45833333060214443, 2.886751345948126879 ) ) ;
#52887 = CARTESIAN_POINT ( 'NONE',  ( -57.89159099828107458, -149.9375000013656063, -3.393966926194107447 ) ) ;
#52888 = CARTESIAN_POINT ( 'NONE',  ( -5.000000000000000000, -143.5000000000000284, -6.123233995736766282E-16 ) ) ;
#52889 = CARTESIAN_POINT ( 'NONE',  ( 4.458734124999999437, -28.81249999863440436, -5.460374474430324690E-16 ) ) ;
#52890 = CARTESIAN_POINT ( 'NONE',  ( 4.458734125000000326, -76.14583333196773651, 2.574251347313718519 ) ) ;
#52891 = CARTESIAN_POINT ( 'NONE',  ( 0.000000000000000000, -170.0000000000000000, 5.000000000000000000 ) ) ;
#52892 = CARTESIAN_POINT ( 'NONE',  ( -4.458734124999999437, -29.31249999863440436, 0.000000000000000000 ) ) ;
#52893 = CARTESIAN_POINT ( 'NONE',  ( -6.972266317189433020E-16, 5.749999999999999112, -5.000000000000000000 ) ) ;
#52894 = CARTESIAN_POINT ( 'NONE',  ( 0.000000000000000000, 15.00000000000000000, 0.000000000000000000 ) ) ;
#52895 = CARTESIAN_POINT ( 'NONE',  ( 2.500000000000002220, -24.66666666666666430, 4.330127018922192761 ) ) ;
#52896 = CARTESIAN_POINT ( 'NONE',  ( -1.846868145590734756, -146.1250000013655779, -4.458734125000000326 ) ) ;
#52897 = ORIENTED_EDGE ( 'NONE', *, *, #5149, .T. ) ;
#52898 = CARTESIAN_POINT ( 'NONE',  ( 5.000000000000000888, -16.45833333060214443, 2.886751345948126879 ) ) ;
#52899 = CARTESIAN_POINT ( 'NONE',  ( 4.458734125000000326, -57.14583333196773651, 2.574251347313718519 ) ) ;
#52900 = CARTESIAN_POINT ( 'NONE',  ( -5.000000000000000000, 29.12500000273118417, 0.000000000000000000 ) ) ;
#52901 = LINE ( 'NONE', #28450, #22701 ) ;
#52902 = CARTESIAN_POINT ( 'NONE',  ( 1.060575238724906964E-15, 19.25000000000000000, 5.773502691896257311 ) ) ;
#52903 = CARTESIAN_POINT ( 'NONE',  ( -2.500000000000000444, -89.16666666666665719, -4.330127018922193649 ) ) ;
#52904 = CARTESIAN_POINT ( 'NONE',  ( 9.457646018065525792E-16, -2.062499998634407028, 5.148502694627439702 ) ) ;
#52905 = CARTESIAN_POINT ( 'NONE',  ( -3.535533905932737309, -154.6250000000000000, -3.535533905932738197 ) ) ;
#52906 = CARTESIAN_POINT ( 'NONE',  ( 1.975475456537005874E-15, -15.75000000000000000, 5.000000000000000000 ) ) ;
#52907 = CARTESIAN_POINT ( 'NONE',  ( 2.229367062500001939, 7.770833334698926009, 3.861377020970579999 ) ) ;
#52908 = CARTESIAN_POINT ( 'NONE',  ( -5.000000000000000000, -87.95833333060213022, -2.886751345948128211 ) ) ;
#52909 = EDGE_LOOP ( 'NONE', ( #1831, #49327, #50951, #23114 ) ) ;
#52910 = CARTESIAN_POINT ( 'NONE',  ( -4.458734124999999437, -51.39583333196772941, -2.574251347313719407 ) ) ;
#52911 = CARTESIAN_POINT ( 'NONE',  ( 4.458734124999999437, -160.7500000013655779, 1.846868145590737864 ) ) ;
#52912 = CARTESIAN_POINT ( 'NONE',  ( 2.499999999999998668, -50.20833333060213732, -4.330127018922193649 ) ) ;
#52913 = ORIENTED_EDGE ( 'NONE', *, *, #25746, .T. ) ;
#52914 = CARTESIAN_POINT ( 'NONE',  ( 4.458734125000001214, -22.89583333196773651, 2.574251347313718519 ) ) ;
#52915 = ORIENTED_EDGE ( 'NONE', *, *, #28898, .F. ) ;
#52917 = DIRECTION ( 'NONE',  ( 0.000000000000000000, 0.000000000000000000, 1.000000000000000000 ) ) ;
#52916 = CARTESIAN_POINT ( 'NONE',  ( -1.339745962155610925, 0.3303418039926660499, 5.000000000000000000 ) ) ;
#52918 = CARTESIAN_POINT ( 'NONE',  ( -4.458734125000000326, -160.0000000013656063, -1.846868145590735644 ) ) ;
#52919 = EDGE_LOOP ( 'NONE', ( #38808, #45237, #55327, #6894 ) ) ;
#52920 = CARTESIAN_POINT ( 'NONE',  ( 5.000000000000000888, -39.45833333060214443, 2.886751345948126879 ) ) ;
#52921 = CARTESIAN_POINT ( 'NONE',  ( -52.53715891517739323, -133.4375000000000284, -4.819101127000233298 ) ) ;
#52922 = EDGE_CURVE ( 'NONE', #19776, #19094, #57325, .T. ) ;
#52923 = CARTESIAN_POINT ( 'NONE',  ( 4.458734124999999437, -37.06249999863440792, -5.460374474430324690E-16 ) ) ;
#52924 = ORIENTED_EDGE ( 'NONE', *, *, #25556, .T. ) ;
#52925 =( BOUNDED_CURVE ( )  B_SPLINE_CURVE ( 2, ( #15702, #55269, #49787, #1561, #60094, #25987, #41085, #10547, #39811 ),
 .UNSPECIFIED., .F., .F. ) 
 B_SPLINE_CURVE_WITH_KNOTS ( ( 3, 2, 2, 2, 3 ),
 ( 0.5910714285714285809, 0.5916666666666666741, 0.5928571428571428603, 0.5940476190476190466, 0.5946428571428571397 ),
 .UNSPECIFIED. ) 
 CURVE ( )  GEOMETRIC_REPRESENTATION_ITEM ( )  RATIONAL_B_SPLINE_CURVE ( ( 0.9330127018922194093, 0.9330127018922194093, 1.000000000000000000, 0.8660254037844387076, 1.000000000000000000, 0.8660254037844387076, 1.000000000000000000, 0.9330127018922194093, 0.9330127018922194093 ) ) 
 REPRESENTATION_ITEM ( '' )  );
#52926 = CARTESIAN_POINT ( 'NONE',  ( -3.152548672688508926E-16, -82.56249999863442213, -5.148502694627439702 ) ) ;
#52927 = CARTESIAN_POINT ( 'NONE',  ( 4.458734124999998549, 17.27083333469892779, -2.574251347313721627 ) ) ;
#52928 = CARTESIAN_POINT ( 'NONE',  ( 5.000000000000000888, -12.45833333060214976, 2.886751345948126879 ) ) ;
#52929 = ORIENTED_EDGE ( 'NONE', *, *, #1720, .T. ) ;
#52930 = CARTESIAN_POINT ( 'NONE',  ( -59.59170313451810586, -138.7500000013655779, 1.485763867205729394 ) ) ;
#52931 = CARTESIAN_POINT ( 'NONE',  ( -3.152548672688508926E-16, -86.81249999863439371, -5.148502694627439702 ) ) ;
#52932 = CARTESIAN_POINT ( 'NONE',  ( -49.85088928181150436, -124.6875000027312268, -1.666127454062680702 ) ) ;
#52933 = CARTESIAN_POINT ( 'NONE',  ( -1.339745962155614034, 25.33034180399266333, 4.999999999999999112 ) ) ;
#52934 = CARTESIAN_POINT ( 'NONE',  ( -54.05457638071479920, -135.0000000000000284, 4.837889621885112845 ) ) ;
#52935 = CARTESIAN_POINT ( 'NONE',  ( 1.339745962155612702, -13.16965819600733489, -5.000000000000000000 ) ) ;
#52936 = CARTESIAN_POINT ( 'NONE',  ( 4.458734124999998549, -61.72916666530106511, -2.574251347313721627 ) ) ;
#52937 = CARTESIAN_POINT ( 'NONE',  ( 5.000000000000000888, 10.41666666666666785, 2.886751345948126879 ) ) ;
#52938 = CARTESIAN_POINT ( 'NONE',  ( -2.229367062499996610, 24.85416666803225993, 3.861377020970582219 ) ) ;
#52939 = CARTESIAN_POINT ( 'NONE',  ( 2.500000000000002220, -109.6666666666666572, 4.330127018922192761 ) ) ;
#52940 = AXIS2_PLACEMENT_3D ( 'NONE', #7386, #56273, #31177 ) ;
#52941 =( BOUNDED_CURVE ( )  B_SPLINE_CURVE ( 2, ( #12048, #22669, #42268, #62221, #32620, #31988, #27168, #57082, #61908 ),
 .UNSPECIFIED., .F., .F. ) 
 B_SPLINE_CURVE_WITH_KNOTS ( ( 3, 2, 2, 2, 3 ),
 ( 0.3482142857142856984, 0.3488095238095237915, 0.3499999999999999778, 0.3511904761904761640, 0.3517857142857143127 ),
 .UNSPECIFIED. ) 
 CURVE ( )  GEOMETRIC_REPRESENTATION_ITEM ( )  RATIONAL_B_SPLINE_CURVE ( ( 0.9330127018922194093, 0.9330127018922194093, 1.000000000000000000, 0.8660254037844387076, 1.000000000000000000, 0.8660254037844387076, 1.000000000000000000, 0.9330127018922163007, 0.9330127018922194093 ) ) 
 REPRESENTATION_ITEM ( '' )  );
#52942 = DIRECTION ( 'NONE',  ( -0.6485228581062915110, 0.000000000000000000, -0.7611951803011149931 ) ) ;
#52943 = CARTESIAN_POINT ( 'NONE',  ( -4.458734124999999437, -43.56249999863440081, 0.000000000000000000 ) ) ;
#52944 = CARTESIAN_POINT ( 'NONE',  ( -5.000000000000000000, -4.958333330602147981, -2.886751345948128211 ) ) ;
#52945 = CARTESIAN_POINT ( 'NONE',  ( 1.975475456537005874E-15, -66.62499999726881583, 5.000000000000000000 ) ) ;
#52946 = CARTESIAN_POINT ( 'NONE',  ( 4.458734124999998549, -83.97916666530107932, -2.574251347313721627 ) ) ;
#52947 = CARTESIAN_POINT ( 'NONE',  ( -4.458734124999999437, -109.3124999986343937, 0.000000000000000000 ) ) ;
#52948 = CARTESIAN_POINT ( 'NONE',  ( 4.458734125000000326, -11.14583333196773829, 2.574251347313718519 ) ) ;
#52949 = ORIENTED_EDGE ( 'NONE', *, *, #51863, .T. ) ;
#52950 = CARTESIAN_POINT ( 'NONE',  ( 5.000000000000000000, -52.41666666666666430, -2.886751345948130876 ) ) ;
#52951 = CARTESIAN_POINT ( 'NONE',  ( 4.458734124999998549, -99.72916666530105090, -2.574251347313721627 ) ) ;
#52952 = CARTESIAN_POINT ( 'NONE',  ( -3.535533905932737309, -165.7500000027312126, -3.535533905932738197 ) ) ;
#52953 = CARTESIAN_POINT ( 'NONE',  ( -4.458734124999998549, -91.47916666530106511, 2.574251347313722516 ) ) ;
#52954 = CARTESIAN_POINT ( 'NONE',  ( 2.500000000000002220, -50.54166666393547303, 4.330127018922192761 ) ) ;
#52955 = CARTESIAN_POINT ( 'NONE',  ( -57.19623071787017210, -130.3750000013656631, 4.297418129356382899 ) ) ;
#52956 = CARTESIAN_POINT ( 'NONE',  ( -55.35523342533222291, -148.3125000013656063, 4.444560631937231499 ) ) ;
#52957 = CARTESIAN_POINT ( 'NONE',  ( -4.458734124999999437, -10.31249999863440792, 0.000000000000000000 ) ) ;
#52958 = CARTESIAN_POINT ( 'NONE',  ( -4.458734124999999437, 11.35416666803225993, -2.574251347313719407 ) ) ;
#52959 = CARTESIAN_POINT ( 'NONE',  ( 2.229367062500001939, -57.22916666530107932, 3.861377020970579999 ) ) ;
#52960 = DIRECTION ( 'NONE',  ( -0.000000000000000000, 1.000000000000000000, -0.000000000000000000 ) ) ;
#52961 = CARTESIAN_POINT ( 'NONE',  ( 5.000000000000000888, 17.41666666666666430, 2.886751345948126879 ) ) ;
#52962 = CARTESIAN_POINT ( 'NONE',  ( 4.458734124999999437, -13.81249999863440259, -5.460374474430324690E-16 ) ) ;
#52963 = CARTESIAN_POINT ( 'NONE',  ( 1.339745962155612702, -71.29465819873850307, -5.000000000000000000 ) ) ;
#52964 = ORIENTED_EDGE ( 'NONE', *, *, #13795, .T. ) ;
#52965 = CARTESIAN_POINT ( 'NONE',  ( -4.458734124999999437, -41.56249999863440081, 0.000000000000000000 ) ) ;
#52966 = CARTESIAN_POINT ( 'NONE',  ( -6.972266317189433020E-16, -77.25000000000000000, -5.000000000000000000 ) ) ;
#52967 = CYLINDRICAL_SURFACE ( 'NONE', #24689, 5.000000000000000000 ) ;
#52968 = CARTESIAN_POINT ( 'NONE',  ( -48.00000000000002132, -155.0000000000000284, -4.041451884327376121 ) ) ;
#52969 = CARTESIAN_POINT ( 'NONE',  ( -4.458734124999999437, -84.31249999863439371, 0.000000000000000000 ) ) ;
#52970 = CARTESIAN_POINT ( 'NONE',  ( 4.458734124999999437, 20.93750000136559208, -5.460374474430324690E-16 ) ) ;
#52971 = CARTESIAN_POINT ( 'NONE',  ( -3.152548672688508926E-16, 14.43750000136559386, -5.148502694627439702 ) ) ;
#52972 = CARTESIAN_POINT ( 'NONE',  ( -1.339745962155613812, -82.08034179853031276, -5.000000000000000000 ) ) ;
#52973 = CARTESIAN_POINT ( 'NONE',  ( -6.972266317189433020E-16, -65.12499999726880162, -5.000000000000000000 ) ) ;
#52974 = CARTESIAN_POINT ( 'NONE',  ( -4.458734124999997661, -87.47916666530107932, 2.574251347313722516 ) ) ;
#52975 = CARTESIAN_POINT ( 'NONE',  ( -3.535250795749689387E-16, -72.24999999999998579, -5.773502691896257311 ) ) ;
#52976 = CARTESIAN_POINT ( 'NONE',  ( -4.999999999999999112, 15.20833333606451987, 2.886751345948131764 ) ) ;
#52977 = ORIENTED_EDGE ( 'NONE', *, *, #32193, .T. ) ;
#52978 = CARTESIAN_POINT ( 'NONE',  ( -5.000000000000000000, -6.874999997268812280, 0.000000000000000000 ) ) ;
#52979 = FACE_OUTER_BOUND ( 'NONE', #41035, .T. ) ;
#52981 = CARTESIAN_POINT ( 'NONE',  ( -4.999999999999999112, -26.91666666666666075, 2.886751345948131764 ) ) ;
#52980 = CARTESIAN_POINT ( 'NONE',  ( -6.972266317189433020E-16, -72.25000000000000000, -5.000000000000000000 ) ) ;
#52982 = CARTESIAN_POINT ( 'NONE',  ( -3.152548672688508926E-16, -32.56249999863440792, -5.148502694627439702 ) ) ;
#52983 = CARTESIAN_POINT ( 'NONE',  ( -3.535250795749689387E-16, -34.12499999726881583, -5.773502691896257311 ) ) ;
#52985 = ORIENTED_EDGE ( 'NONE', *, *, #46347, .F. ) ;
#52984 = CARTESIAN_POINT ( 'NONE',  ( 4.458734124999999437, -62.81249999863440792, -5.460374474430324690E-16 ) ) ;
#52986 = CARTESIAN_POINT ( 'NONE',  ( -52.10840900171896806, -149.4375000013656063, 3.393966926194110556 ) ) ;
#52988 = EDGE_LOOP ( 'NONE', ( #9868, #61918, #55685, #52777 ) ) ;
#52987 = CARTESIAN_POINT ( 'NONE',  ( 4.458734124999998549, -13.97916666530107221, -2.574251347313721627 ) ) ;
#52989 = CARTESIAN_POINT ( 'NONE',  ( 2.499999999999998668, -75.33333333333332860, -4.330127018922193649 ) ) ;
#52990 = CARTESIAN_POINT ( 'NONE',  ( -57.19623071787016499, -136.3750000013656063, 4.297418129356382899 ) ) ;
#52991 = CARTESIAN_POINT ( 'NONE',  ( 2.229367062499998831, -54.89583333196773651, -3.861377020970580887 ) ) ;
#52992 =( BOUNDED_CURVE ( )  B_SPLINE_CURVE ( 2, ( #15720, #6401, #35339, #54958, #26010, #1902, #45627, #10888, #59471 ),
 .UNSPECIFIED., .F., .F. ) 
 B_SPLINE_CURVE_WITH_KNOTS ( ( 3, 2, 2, 2, 3 ),
 ( 0.8517857142857142572, 0.8523809523809523503, 0.8535714285714285365, 0.8547619047619047228, 0.8553571428571428159 ),
 .UNSPECIFIED. ) 
 CURVE ( )  GEOMETRIC_REPRESENTATION_ITEM ( )  RATIONAL_B_SPLINE_CURVE ( ( 0.9330127018922194093, 0.9330127018922194093, 1.000000000000000000, 0.8660254037844387076, 1.000000000000000000, 0.8660254037844387076, 1.000000000000000000, 0.9330127018922194093, 0.9330127018922194093 ) ) 
 REPRESENTATION_ITEM ( '' )  );
#52993 = CARTESIAN_POINT ( 'NONE',  ( 5.000000000000000000, -80.37499999726881583, -6.123233995736766282E-16 ) ) ;
#52995 = ORIENTED_EDGE ( 'NONE', *, *, #37409, .T. ) ;
#52994 = CARTESIAN_POINT ( 'NONE',  ( 5.000000000000000888, -65.45833333060213022, 2.886751345948126879 ) ) ;
#52996 = CARTESIAN_POINT ( 'NONE',  ( -60.14911071818854538, -145.0625000000000284, 1.666127454062681368 ) ) ;
#52997 = ADVANCED_FACE ( 'NONE', ( #32863 ), #27088, .T. ) ;
#52998 = CARTESIAN_POINT ( 'NONE',  ( 4.458734124999998549, -20.97916666530107221, -2.574251347313721627 ) ) ;
#53000 = ORIENTED_EDGE ( 'NONE', *, *, #31152, .T. ) ;
#52999 = CARTESIAN_POINT ( 'NONE',  ( 4.458734124999999437, -57.06249999863440081, -5.460374474430324690E-16 ) ) ;
#53001 = CARTESIAN_POINT ( 'NONE',  ( -3.152801135295367096, -167.3125000013656063, -3.152801135295367541 ) ) ;
#53002 = CARTESIAN_POINT ( 'NONE',  ( -4.458734124999999437, -104.5624999986344079, 0.000000000000000000 ) ) ;
#53003 = CARTESIAN_POINT ( 'NONE',  ( -1.339745962155610925, 18.20534180126147561, 5.000000000000000000 ) ) ;
#53004 = VERTEX_POINT ( 'NONE', #46704 ) ;
#53005 = CARTESIAN_POINT ( 'NONE',  ( -53.51423613279429503, -148.5000000013655779, 4.591703134518083651 ) ) ;
#53006 = CARTESIAN_POINT ( 'NONE',  ( -56.66612745406270335, -137.4375000027312410, -5.149110718188516067 ) ) ;
#53007 = CARTESIAN_POINT ( 'NONE',  ( 4.458734125000000326, -36.89583333196773651, 2.574251347313718519 ) ) ;
#53008 = LINE ( 'NONE', #8948, #10650 ) ;
#53009 = CARTESIAN_POINT ( 'NONE',  ( -4.458734124999999437, -8.395833331967736513, -2.574251347313719407 ) ) ;
#53010 = CARTESIAN_POINT ( 'NONE',  ( -4.458734124999999437, -99.56249999863440792, 0.000000000000000000 ) ) ;
#53011 = EDGE_CURVE ( 'NONE', #60996, #15028, #28028, .T. ) ;
#53012 = CARTESIAN_POINT ( 'NONE',  ( -8.190561711645485556E-16, -142.9375000013656063, 4.458734124999999437 ) ) ;
#53013 = CARTESIAN_POINT ( 'NONE',  ( 4.458734124999999437, -30.06249999863440436, -5.460374474430324690E-16 ) ) ;
#53014 = EDGE_CURVE ( 'NONE', #21047, #61372, #30106, .T. ) ;
#53015 = DIRECTION ( 'NONE',  ( -0.8660254037844410391, 0.4999999999999958367, 0.000000000000000000 ) ) ;
#53016 = CARTESIAN_POINT ( 'NONE',  ( -57.19623071787017210, -134.3750000013656347, 4.297418129356382899 ) ) ;
#53017 = CARTESIAN_POINT ( 'NONE',  ( -4.458734124999999437, -66.56249999863440792, 0.000000000000000000 ) ) ;
#53018 = CARTESIAN_POINT ( 'NONE',  ( -5.000000000000000000, -16.00000000000000000, 0.000000000000000000 ) ) ;
#53019 = CARTESIAN_POINT ( 'NONE',  ( -6.972266317189433020E-16, -34.25000000000000000, -5.000000000000000000 ) ) ;
#53020 = CARTESIAN_POINT ( 'NONE',  ( 3.152801135295366208, -142.5625000013655779, 3.152801135295367985 ) ) ;
#53021 = CARTESIAN_POINT ( 'NONE',  ( 4.458734125000000326, 3.854166668032260823, 2.574251347313718519 ) ) ;
#53022 = VERTEX_POINT ( 'NONE', #21075 ) ;
#53023 =( GEOMETRIC_REPRESENTATION_CONTEXT ( 3 ) GLOBAL_UNCERTAINTY_ASSIGNED_CONTEXT ( ( #18243 ) ) GLOBAL_UNIT_ASSIGNED_CONTEXT ( ( #54126, #14257, #431 ) ) REPRESENTATION_CONTEXT ( 'NONE', 'WORKASPACE' ) );
#53024 = DIRECTION ( 'NONE',  ( -0.000000000000000000, 1.000000000000000000, -0.000000000000000000 ) ) ;
#53025 = CARTESIAN_POINT ( 'NONE',  ( -1.339745962155613812, 15.91965820146970501, -5.000000000000000000 ) ) ;
#53027 = CARTESIAN_POINT ( 'NONE',  ( 2.229367062500001939, -27.97916666530107221, 3.861377020970579999 ) ) ;
#53026 = CARTESIAN_POINT ( 'NONE',  ( -4.999999999999999112, -96.91666666666665719, 2.886751345948131764 ) ) ;
#53028 = CARTESIAN_POINT ( 'NONE',  ( -2.499999999999996447, -76.70833333060214443, 4.330127018922195425 ) ) ;
#53029 = CARTESIAN_POINT ( 'NONE',  ( 2.229367062499998831, -74.89583333196773651, -3.861377020970580887 ) ) ;
#53030 = AXIS2_PLACEMENT_3D ( 'NONE', #10940, #11583, #6458 ) ;
#53031 = CARTESIAN_POINT ( 'NONE',  ( -2.229367062499996610, 21.60416666803226349, 3.861377020970582219 ) ) ;
#53032 = CARTESIAN_POINT ( 'NONE',  ( -2.499999999999996447, -101.7083333306021444, 4.330127018922195425 ) ) ;
#53033 = EDGE_CURVE ( 'NONE', #51665, #25684, #55499, .T. ) ;
#53034 = VECTOR ( 'NONE', #14330, 1000.000000000000000 ) ;
#53035 = CARTESIAN_POINT ( 'NONE',  ( -57.19623071787017210, -143.3750000013656063, 4.297418129356382899 ) ) ;
#53036 = CARTESIAN_POINT ( 'NONE',  ( 4.458734124999999437, 5.187500001365596525, -5.460374474430324690E-16 ) ) ;
#53037 = CARTESIAN_POINT ( 'NONE',  ( -4.458734124999999437, 25.43750000136559208, 0.000000000000000000 ) ) ;
#53038 = CARTESIAN_POINT ( 'NONE',  ( 4.458734125000000326, -42.14583333196773651, 2.574251347313718519 ) ) ;
#53039 = CARTESIAN_POINT ( 'NONE',  ( -1.339745962155613812, -4.080341798530293218, -5.000000000000000000 ) ) ;
#53040 = CARTESIAN_POINT ( 'NONE',  ( 2.229367062499998831, 1.354166668032261933, -3.861377020970580887 ) ) ;
#53041 = CARTESIAN_POINT ( 'NONE',  ( 4.458734124999998549, -25.97916666530107221, -2.574251347313721627 ) ) ;
#53042 =( BOUNDED_CURVE ( )  B_SPLINE_CURVE ( 2, ( #33823, #53442, #9685, #43154, #24173, #38636, #3937, #48609, #58897 ),
 .UNSPECIFIED., .F., .F. ) 
 B_SPLINE_CURVE_WITH_KNOTS ( ( 3, 2, 2, 2, 3 ),
 ( 0.3732142857142857206, 0.3738095238095238138, 0.3750000000000000000, 0.3761904761904761862, 0.3767857142857142794 ),
 .UNSPECIFIED. ) 
 CURVE ( )  GEOMETRIC_REPRESENTATION_ITEM ( )  RATIONAL_B_SPLINE_CURVE ( ( 0.9330127018922194093, 0.9330127018922194093, 1.000000000000000000, 0.8660254037844387076, 1.000000000000000000, 0.8660254037844387076, 1.000000000000000000, 0.9330127018922194093, 0.9330127018922194093 ) ) 
 REPRESENTATION_ITEM ( '' )  );
#53043 = CARTESIAN_POINT ( 'NONE',  ( 1.846868145590735200, -156.2500000013656063, -4.458734125000000326 ) ) ;
#53044 = CARTESIAN_POINT ( 'NONE',  ( -2.229367062500000163, -70.47916666530107932, -3.861377020970580443 ) ) ;
#53045 = CARTESIAN_POINT ( 'NONE',  ( -3.535250795749689387E-16, -99.12499999726881583, -5.773502691896257311 ) ) ;
#53046 = CARTESIAN_POINT ( 'NONE',  ( -4.458734124999999437, 29.68750000136559208, 0.000000000000000000 ) ) ;
#53047 = FACE_OUTER_BOUND ( 'NONE', #59735, .T. ) ;
#53048 = ADVANCED_FACE ( 'NONE', ( #2650 ), #22269, .T. ) ;
#53049 = CARTESIAN_POINT ( 'NONE',  ( 9.457646018065525792E-16, -105.3124999986344221, 5.148502694627439702 ) ) ;
#53050 = CARTESIAN_POINT ( 'NONE',  ( -3.152548672688508926E-16, -70.81249999863439371, -5.148502694627439702 ) ) ;
#53051 = CARTESIAN_POINT ( 'NONE',  ( 5.000000000000000000, -56.41666666666666430, -2.886751345948129988 ) ) ;
#53052 = DIRECTION ( 'NONE',  ( 0.000000000000000000, 0.000000000000000000, 1.000000000000000000 ) ) ;
#53053 = ORIENTED_EDGE ( 'NONE', *, *, #37048, .F. ) ;
#53054 = LINE ( 'NONE', #14752, #59185 ) ;
#53055 = CARTESIAN_POINT ( 'NONE',  ( -2.500000000000000444, 12.83333333333333215, -4.330127018922193649 ) ) ;
#53056 = CARTESIAN_POINT ( 'NONE',  ( 5.000000000000000000, -10.50000000000000178, -6.123233995736766282E-16 ) ) ;
#53057 = CARTESIAN_POINT ( 'NONE',  ( -3.152548672688508926E-16, -17.56249999863440792, -5.148502694627439702 ) ) ;
#53058 = CARTESIAN_POINT ( 'NONE',  ( 9.457646018065525792E-16, -80.06249999863440792, 5.148502694627439702 ) ) ;
#53059 = CARTESIAN_POINT ( 'NONE',  ( 4.458734125000000326, -168.6250000013655779, -1.846868145590734978 ) ) ;
#53060 = CARTESIAN_POINT ( 'NONE',  ( 1.060575238724906964E-15, -17.62499999726881583, 5.773502691896257311 ) ) ;
#53062 = VERTEX_POINT ( 'NONE', #9663 ) ;
#53061 = CARTESIAN_POINT ( 'NONE',  ( 2.229367062499998831, -43.64583333196773651, -3.861377020970580887 ) ) ;
#53063 = CARTESIAN_POINT ( 'NONE',  ( 5.000000000000000000, -45.29166666393547303, -2.886751345948130876 ) ) ;
#53065 = VERTEX_POINT ( 'NONE', #44390 ) ;
#53064 = CARTESIAN_POINT ( 'NONE',  ( 9.457646018065525792E-16, 8.687500001365595637, 5.148502694627439702 ) ) ;
#53066 = CARTESIAN_POINT ( 'NONE',  ( -5.000000000000000000, -86.95833333060214443, -2.886751345948128211 ) ) ;
#53067 = CARTESIAN_POINT ( 'NONE',  ( -5.000000000000000000, -59.00000000000000000, 0.000000000000000000 ) ) ;
#53068 = CARTESIAN_POINT ( 'NONE',  ( -3.152801135295367985, -155.0625000013656063, 3.152801135295367096 ) ) ;
#53069 = CARTESIAN_POINT ( 'NONE',  ( 4.458734124999998549, -40.97916666530107932, -2.574251347313721627 ) ) ;
#53070 = CARTESIAN_POINT ( 'NONE',  ( -1.339745962155610925, -78.79465819873851729, 5.000000000000000000 ) ) ;
#53071 = CARTESIAN_POINT ( 'NONE',  ( 5.000000000000000000, -164.0000000000000000, 0.000000000000000000 ) ) ;
#53072 = CARTESIAN_POINT ( 'NONE',  ( 5.000000000000000000, 5.708333336064518981, -2.886751345948130876 ) ) ;
#53073 = CARTESIAN_POINT ( 'NONE',  ( -51.60603307380591787, -130.1875000013656063, -2.891590998281053704 ) ) ;
#53074 = EDGE_CURVE ( 'NONE', #42260, #54554, #53108, .T. ) ;
#53075 = AXIS2_PLACEMENT_3D ( 'NONE', #31466, #21838, #11539 ) ;
#53076 = CARTESIAN_POINT ( 'NONE',  ( -2.229367062500000163, -4.729166665301071326, -3.861377020970580443 ) ) ;
#53077 = AXIS2_PLACEMENT_3D ( 'NONE', #54623, #11508, #35963 ) ;
#53078 = CARTESIAN_POINT ( 'NONE',  ( 2.229367062500001939, -41.22916666530107932, 3.861377020970579999 ) ) ;
#53079 = EDGE_CURVE ( 'NONE', #100, #56685, #32572, .T. ) ;
#53080 = EDGE_CURVE ( 'NONE', #13129, #33278, #48270, .T. ) ;
#53081 = CARTESIAN_POINT ( 'NONE',  ( 5.000000000000000000, -26.49999999999999645, -6.123233995736766282E-16 ) ) ;
#53082 = CARTESIAN_POINT ( 'NONE',  ( 1.846868145590736310, -147.6250000013655779, 4.458734124999999437 ) ) ;
#53083 = AXIS2_PLACEMENT_3D ( 'NONE', #42119, #17689, #55983 ) ;
#53084 = CARTESIAN_POINT ( 'NONE',  ( 4.458734124999999437, -86.06249999863439371, -5.460374474430324690E-16 ) ) ;
#53085 = DIRECTION ( 'NONE',  ( 0.000000000000000000, 0.000000000000000000, 1.000000000000000000 ) ) ;
#53086 = ORIENTED_EDGE ( 'NONE', *, *, #53178, .F. ) ;
#53087 = CARTESIAN_POINT ( 'NONE',  ( 1.339745962155615144, -99.70534180126146850, 4.999999999999999112 ) ) ;
#53088 = CARTESIAN_POINT ( 'NONE',  ( -51.19402409849444524, -151.6250000027312126, -3.242614290531456334 ) ) ;
#53089 = DIRECTION ( 'NONE',  ( -0.000000000000000000, 1.000000000000000000, -0.000000000000000000 ) ) ;
#53090 = CARTESIAN_POINT ( 'NONE',  ( -2.229367062499996610, -77.39583333196773651, 3.861377020970582219 ) ) ;
#53091 = EDGE_LOOP ( 'NONE', ( #4644, #23158, #11451, #41223 ) ) ;
#53092 = ADVANCED_FACE ( 'NONE', ( #44071 ), #1784, .F. ) ;
#53093 = CARTESIAN_POINT ( 'NONE',  ( -5.000000000000000000, -70.87499999726880162, 0.000000000000000000 ) ) ;
#53094 = CARTESIAN_POINT ( 'NONE',  ( -4.458734124999999437, -12.64583333196774007, -2.574251347313719407 ) ) ;
#53095 = EDGE_CURVE ( 'NONE', #54241, #41751, #39109, .T. ) ;
#53096 = FACE_OUTER_BOUND ( 'NONE', #55479, .T. ) ;
#53097 = CARTESIAN_POINT ( 'NONE',  ( 2.229367062499998831, 1.354166668032261933, -3.861377020970580887 ) ) ;
#53098 = CYLINDRICAL_SURFACE ( 'NONE', #38769, 5.000000000000000000 ) ;
#53099 = CARTESIAN_POINT ( 'NONE',  ( -1.846868145590734756, -154.1250000013655779, -4.458734124999999437 ) ) ;
#53100 = CARTESIAN_POINT ( 'NONE',  ( 2.229367062499998831, 19.10416666803225993, -3.861377020970580887 ) ) ;
#53101 = ORIENTED_EDGE ( 'NONE', *, *, #38227, .F. ) ;
#53102 = CARTESIAN_POINT ( 'NONE',  ( 2.229367062499998831, -89.64583333196773651, -3.861377020970580887 ) ) ;
#53103 = CARTESIAN_POINT ( 'NONE',  ( 1.339745962155615144, -47.70534180126147561, 4.999999999999999112 ) ) ;
#53104 = DIRECTION ( 'NONE',  ( -0.000000000000000000, 1.000000000000000000, -0.000000000000000000 ) ) ;
#53105 = CARTESIAN_POINT ( 'NONE',  ( 9.457646018065525792E-16, -12.06249999863440081, 5.148502694627439702 ) ) ;
#53106 = DIRECTION ( 'NONE',  ( -0.000000000000000000, 1.000000000000000000, -0.000000000000000000 ) ) ;
#53107 = CARTESIAN_POINT ( 'NONE',  ( -5.000000000000000000, -13.08333333333333570, -2.886751345948128211 ) ) ;
#53108 = LINE ( 'NONE', #63089, #2769 ) ;
#53109 = CARTESIAN_POINT ( 'NONE',  ( -5.000000000000000000, -34.87499999726881583, 0.000000000000000000 ) ) ;
#53110 = CARTESIAN_POINT ( 'NONE',  ( 1.975475456537005874E-15, -49.62499999726880873, 5.000000000000000000 ) ) ;
#53111 = CARTESIAN_POINT ( 'NONE',  ( 4.458734124999999437, 19.18750000136559564, -5.460374474430324690E-16 ) ) ;
#53112 = CARTESIAN_POINT ( 'NONE',  ( 1.975475456537005874E-15, -44.74999999999999289, 5.000000000000000000 ) ) ;
#53113 = CARTESIAN_POINT ( 'NONE',  ( -2.229367062500000163, 15.52083333469892779, -3.861377020970580443 ) ) ;
#53114 = CARTESIAN_POINT ( 'NONE',  ( -2.229367062500000163, -57.47916666530107932, -3.861377020970580443 ) ) ;
#53115 = CARTESIAN_POINT ( 'NONE',  ( -4.458734124999997661, -11.47916666530107044, 2.574251347313722516 ) ) ;
#53116 = AXIS2_PLACEMENT_3D ( 'NONE', #27225, #7934, #47470 ) ;
#53117 = CARTESIAN_POINT ( 'NONE',  ( -5.000000000000000000, -63.00000000000000000, 0.000000000000000000 ) ) ;
#53118 = CARTESIAN_POINT ( 'NONE',  ( -5.000000000000000000, 11.91666666666666607, -2.886751345948128211 ) ) ;
#53119 = CARTESIAN_POINT ( 'NONE',  ( -1.846868145590734756, -169.1250000013656347, -4.458734125000000326 ) ) ;
#53120 = DIRECTION ( 'NONE',  ( -0.000000000000000000, 1.000000000000000000, -0.000000000000000000 ) ) ;
#53121 = CARTESIAN_POINT ( 'NONE',  ( 2.229367062500001939, -51.97916666530107221, 3.861377020970579999 ) ) ;
#53122 = CARTESIAN_POINT ( 'NONE',  ( 5.000000000000000888, -81.45833333060213022, 2.886751345948126879 ) ) ;
#53123 = AXIS2_PLACEMENT_3D ( 'NONE', #39491, #10864, #59127 ) ;
#53124 = CARTESIAN_POINT ( 'NONE',  ( -59.59170313451811296, -135.7500000013656063, 1.485763867205729394 ) ) ;
#53125 =( BOUNDED_CURVE ( )  B_SPLINE_CURVE ( 2, ( #37595, #33094, #18614, #57860, #63007, #52410, #13155, #4143, #8341 ),
 .UNSPECIFIED., .F., .F. ) 
 B_SPLINE_CURVE_WITH_KNOTS ( ( 3, 2, 2, 2, 3 ),
 ( 0.3589285714285714302, 0.3595238095238095233, 0.3607142857142857095, 0.3619047619047618958, 0.3624999999999999889 ),
 .UNSPECIFIED. ) 
 CURVE ( )  GEOMETRIC_REPRESENTATION_ITEM ( )  RATIONAL_B_SPLINE_CURVE ( ( 0.9330127018922194093, 0.9330127018922194093, 1.000000000000000000, 0.8660254037844387076, 1.000000000000000000, 0.8660254037844387076, 1.000000000000000000, 0.9330127018922194093, 0.9330127018922194093 ) ) 
 REPRESENTATION_ITEM ( '' )  );
#53126 = CARTESIAN_POINT ( 'NONE',  ( 1.975475456537005874E-15, -45.62499999726880873, 5.000000000000000000 ) ) ;
#53127 = CARTESIAN_POINT ( 'NONE',  ( -1.339745962155613812, -92.20534180126149693, -5.000000000000000000 ) ) ;
#53128 = AXIS2_PLACEMENT_3D ( 'NONE', #30736, #41330, #17212 ) ;
#53129 = CARTESIAN_POINT ( 'NONE',  ( -2.229367062499996610, -91.39583333196773651, 3.861377020970582219 ) ) ;
#53130 = CARTESIAN_POINT ( 'NONE',  ( 2.730187237215162345E-16, -157.4375000013655779, -4.458734124999999437 ) ) ;
#53131 = CARTESIAN_POINT ( 'NONE',  ( -3.535250795749689387E-16, -38.24999999999999289, -5.773502691896257311 ) ) ;
#53132 = CARTESIAN_POINT ( 'NONE',  ( 1.975475456537005874E-15, -19.62499999726881228, 5.000000000000000000 ) ) ;
#53133 = CARTESIAN_POINT ( 'NONE',  ( -58.51875683073618717, -135.0000000000000000, -2.985197606355836086 ) ) ;
#53134 = ORIENTED_EDGE ( 'NONE', *, *, #21746, .F. ) ;
#53135 = CARTESIAN_POINT ( 'NONE',  ( 4.458734124999999437, -93.81249999863440792, -5.460374474430324690E-16 ) ) ;
#53136 = CARTESIAN_POINT ( 'NONE',  ( -4.458734124999999437, 7.354166668032259935, -2.574251347313719407 ) ) ;
#53137 = CARTESIAN_POINT ( 'NONE',  ( 1.060575238724906964E-15, 10.37500000273118594, 5.773502691896257311 ) ) ;
#53138 = CARTESIAN_POINT ( 'NONE',  ( -3.535250795749689387E-16, 2.749999999999999112, -5.773502691896257311 ) ) ;
#53139 = CARTESIAN_POINT ( 'NONE',  ( -2.229367062499996610, -62.14583333196774362, 3.861377020970582219 ) ) ;
#53140 = CARTESIAN_POINT ( 'NONE',  ( -2.500000000000000444, 19.83333333333333570, -4.330127018922193649 ) ) ;
#53141 = CARTESIAN_POINT ( 'NONE',  ( 5.000000000000000888, -3.458333330602147093, 2.886751345948126879 ) ) ;
#53142 = CARTESIAN_POINT ( 'NONE',  ( 2.229367062500001939, -27.97916666530107221, 3.861377020970579999 ) ) ;
#53143 = CARTESIAN_POINT ( 'NONE',  ( -5.000000000000000000, -11.08333333333333393, -2.886751345948128211 ) ) ;
#53144 = CYLINDRICAL_SURFACE ( 'NONE', #17913, 5.000000000000000000 ) ;
#53145 = CARTESIAN_POINT ( 'NONE',  ( 2.500000000000002220, -20.66666666666666785, 4.330127018922192761 ) ) ;
#53146 = CARTESIAN_POINT ( 'NONE',  ( 1.060575238724906964E-15, -46.75000000000000000, 5.773502691896257311 ) ) ;
#53148 = CARTESIAN_POINT ( 'NONE',  ( 9.457646018065525792E-16, -25.31249999863440792, 5.148502694627439702 ) ) ;
#53147 = PLANE ( 'NONE',  #1821 ) ;
#53149 = CARTESIAN_POINT ( 'NONE',  ( -2.499999999999996447, 14.29166666939785202, 4.330127018922195425 ) ) ;
#53150 = CARTESIAN_POINT ( 'NONE',  ( -4.458734124999998549, -70.22916666530107932, 2.574251347313722516 ) ) ;
#53151 = CARTESIAN_POINT ( 'NONE',  ( -4.458734125000000326, -148.2500000013656063, -1.846868145590735644 ) ) ;
#53152 = CARTESIAN_POINT ( 'NONE',  ( -4.458734124999999437, -76.39583333196775072, -2.574251347313719407 ) ) ;
#53153 = CARTESIAN_POINT ( 'NONE',  ( -50.55543936806279248, -141.3125000013656063, 0.3552334253322060320 ) ) ;
#53154 = CARTESIAN_POINT ( 'NONE',  ( 4.458734124999998549, -22.97916666530107221, -2.574251347313721627 ) ) ;
#53155 = CARTESIAN_POINT ( 'NONE',  ( -2.500000000000000444, -66.04166666393547303, -4.330127018922193649 ) ) ;
#53157 = ORIENTED_EDGE ( 'NONE', *, *, #30714, .T. ) ;
#53156 = EDGE_CURVE ( 'NONE', #46264, #18181, #1406, .T. ) ;
#53158 = CARTESIAN_POINT ( 'NONE',  ( 1.339745962155612702, -93.16965819600733312, -5.000000000000000000 ) ) ;
#53159 = VERTEX_POINT ( 'NONE', #9528 ) ;
#53160 = CARTESIAN_POINT ( 'NONE',  ( -4.458734124999999437, -66.56249999863440792, 0.000000000000000000 ) ) ;
#53161 = CARTESIAN_POINT ( 'NONE',  ( -50.01589407740564042, -150.6250000000000284, 0.3983568153799778022 ) ) ;
#53162 = ORIENTED_EDGE ( 'NONE', *, *, #41247, .F. ) ;
#53163 = ADVANCED_FACE ( 'NONE', ( #9217 ), #8592, .T. ) ;
#53164 = VECTOR ( 'NONE', #25882, 1000.000000000000000 ) ;
#53165 = DIRECTION ( 'NONE',  ( -0.000000000000000000, 1.000000000000000000, -0.000000000000000000 ) ) ;
#53166 = CARTESIAN_POINT ( 'NONE',  ( -3.152548672688508926E-16, -56.81249999863439371, -5.148502694627439702 ) ) ;
#53167 = EDGE_CURVE ( 'NONE', #43365, #37277, #13727, .T. ) ;
#53168 = CARTESIAN_POINT ( 'NONE',  ( -4.458734124999998549, -0.4791666653010707710, 2.574251347313722516 ) ) ;
#53169 = VERTEX_POINT ( 'NONE', #63575 ) ;
#53170 = ADVANCED_FACE ( 'NONE', ( #29134 ), #28202, .T. ) ;
#53171 = CARTESIAN_POINT ( 'NONE',  ( 0.000000000000000000, -120.0000000000000000, 0.000000000000000000 ) ) ;
#53172 = EDGE_CURVE ( 'NONE', #63093, #12482, #7973, .T. ) ;
#53173 = CARTESIAN_POINT ( 'NONE',  ( -2.229367062500000163, 17.52083333469892779, -3.861377020970580443 ) ) ;
#53174 = CARTESIAN_POINT ( 'NONE',  ( -50.70258187064364108, -146.1250000013656063, 2.196230717870141014 ) ) ;
#53175 = CARTESIAN_POINT ( 'NONE',  ( -1.339745962155613812, -2.205341801261479162, -5.000000000000000000 ) ) ;
#53176 = CARTESIAN_POINT ( 'NONE',  ( 3.152801135295367541, -163.3125000013656063, -3.152801135295367541 ) ) ;
#53178 = EDGE_CURVE ( 'NONE', #10376, #17008, #36712, .T. ) ;
#53177 = ORIENTED_EDGE ( 'NONE', *, *, #43008, .F. ) ;
#53179 = CARTESIAN_POINT ( 'NONE',  ( -3.152548672688508926E-16, -76.56249999863440792, -5.148502694627439702 ) ) ;
#53180 = CARTESIAN_POINT ( 'NONE',  ( 5.000000000000000888, -39.58333333333333570, 2.886751345948126879 ) ) ;
#53181 = CARTESIAN_POINT ( 'NONE',  ( 4.458734125000001214, 7.104166668032259047, 2.574251347313718519 ) ) ;
#53182 = EDGE_CURVE ( 'NONE', #45744, #43815, #50366, .T. ) ;
#53183 = CARTESIAN_POINT ( 'NONE',  ( -1.339745962155613812, 1.794658198738520616, -5.000000000000000000 ) ) ;
#53184 = CARTESIAN_POINT ( 'NONE',  ( -2.229367062499996610, -59.39583333196773651, 3.861377020970582219 ) ) ;
#53185 = CARTESIAN_POINT ( 'NONE',  ( -2.499999999999996447, -19.70833333060214798, 4.330127018922195425 ) ) ;
#53186 = DIRECTION ( 'NONE',  ( 0.000000000000000000, 0.000000000000000000, 1.000000000000000000 ) ) ;
#53187 = CARTESIAN_POINT ( 'NONE',  ( -6.972266317189433020E-16, -65.12499999726880162, -5.000000000000000000 ) ) ;
#53188 = CARTESIAN_POINT ( 'NONE',  ( -6.972266317189433020E-16, -18.12499999726881228, -5.000000000000000000 ) ) ;
#53189 = DIRECTION ( 'NONE',  ( -0.000000000000000000, 1.000000000000000000, -0.000000000000000000 ) ) ;
#53190 = CARTESIAN_POINT ( 'NONE',  ( -4.458734124999998549, -38.22916666530107932, 2.574251347313722516 ) ) ;
#53191 = CARTESIAN_POINT ( 'NONE',  ( -4.458734124999997661, -29.47916666530106866, 2.574251347313722516 ) ) ;
#53192 =( BOUNDED_CURVE ( )  B_SPLINE_CURVE ( 2, ( #58500, #33112, #23778, #13496, #48834, #19569, #47581, #44003, #13172 ),
 .UNSPECIFIED., .F., .F. ) 
 B_SPLINE_CURVE_WITH_KNOTS ( ( 3, 2, 2, 2, 3 ),
 ( 0.6020833333333333037, 0.6027777777777777457, 0.6041666666666666297, 0.6055555555555555136, 0.6062499999999999556 ),
 .UNSPECIFIED. ) 
 CURVE ( )  GEOMETRIC_REPRESENTATION_ITEM ( )  RATIONAL_B_SPLINE_CURVE ( ( 0.9330127018922194093, 0.9330127018922194093, 1.000000000000000000, 0.8660254037844387076, 1.000000000000000000, 0.8660254037844387076, 1.000000000000000000, 0.9330127018922194093, 0.9330127018922194093 ) ) 
 REPRESENTATION_ITEM ( '' )  );
#53193 = DIRECTION ( 'NONE',  ( -0.000000000000000000, 1.000000000000000000, -0.000000000000000000 ) ) ;
#53194 = CARTESIAN_POINT ( 'NONE',  ( -2.500000000000000444, 26.83333333333333570, -4.330127018922193649 ) ) ;
#53195 = CARTESIAN_POINT ( 'NONE',  ( 5.000000000000000888, -149.0625000027311842, -2.071067811865475505 ) ) ;
#53196 = CARTESIAN_POINT ( 'NONE',  ( 9.457646018065525792E-16, -107.3124999986343937, 5.148502694627439702 ) ) ;
#53197 = CARTESIAN_POINT ( 'NONE',  ( 9.457646018065525792E-16, -30.06249999863440081, 5.148502694627439702 ) ) ;
#53198 = CARTESIAN_POINT ( 'NONE',  ( -5.000000000000000000, -68.87499999726880162, 0.000000000000000000 ) ) ;
#53199 = CARTESIAN_POINT ( 'NONE',  ( -56.48576386720575471, -147.0000000013655779, -4.591703134518078322 ) ) ;
#53200 = CARTESIAN_POINT ( 'NONE',  ( -5.000000000000000888, -142.5625000000000000, -2.071067811865475949 ) ) ;
#53201 = CARTESIAN_POINT ( 'NONE',  ( -4.458734124999999437, -77.64583333196773651, -2.574251347313719407 ) ) ;
#53202 = CARTESIAN_POINT ( 'NONE',  ( -3.152801135295367096, -168.3125000013656063, -3.152801135295367541 ) ) ;
#53203 = CARTESIAN_POINT ( 'NONE',  ( -4.458734124999999437, -30.39583333196773651, -2.574251347313719407 ) ) ;
#53204 = CYLINDRICAL_SURFACE ( 'NONE', #58415, 5.000000000000000000 ) ;
#53205 = DIRECTION ( 'NONE',  ( -0.000000000000000000, 1.000000000000000000, -0.000000000000000000 ) ) ;
#53206 = CARTESIAN_POINT ( 'NONE',  ( -5.000000000000000000, -23.08333333333332860, -2.886751345948128211 ) ) ;
#53207 = CARTESIAN_POINT ( 'NONE',  ( 2.730187237215162345E-16, -146.1875000013656063, -4.458734124999999437 ) ) ;
#53208 = ORIENTED_EDGE ( 'NONE', *, *, #8234, .F. ) ;
#53209 = CARTESIAN_POINT ( 'NONE',  ( 9.457646018065525792E-16, 26.68750000136559564, 5.148502694627439702 ) ) ;
#53210 = CARTESIAN_POINT ( 'NONE',  ( 5.000000000000000888, 1.416666666666666741, 2.886751345948126879 ) ) ;
#53211 = CARTESIAN_POINT ( 'NONE',  ( -2.229367062499996610, -56.39583333196773651, 3.861377020970582219 ) ) ;
#53212 = AXIS2_PLACEMENT_3D ( 'NONE', #46784, #22670, #51930 ) ;
#53213 = CARTESIAN_POINT ( 'NONE',  ( -3.535250795749689387E-16, 24.87500000273118417, -5.773502691896257311 ) ) ;
#53214 = CARTESIAN_POINT ( 'NONE',  ( -3.535533905932737309, -162.6250000000000284, -3.535533905932738197 ) ) ;
#53215 = CARTESIAN_POINT ( 'NONE',  ( -2.499999999999996447, 20.16666666666666430, 4.330127018922195425 ) ) ;
#53216 = VECTOR ( 'NONE', #41174, 1000.000000000000000 ) ;
#53217 = DIRECTION ( 'NONE',  ( -0.000000000000000000, 1.000000000000000000, -0.000000000000000000 ) ) ;
#53218 = CARTESIAN_POINT ( 'NONE',  ( 4.458734124999999437, -5.812499998634403475, -5.460374474430324690E-16 ) ) ;
#53219 = CARTESIAN_POINT ( 'NONE',  ( -3.535533905932738641, -154.3750000000000000, 3.535533905932737309 ) ) ;
#53220 = CARTESIAN_POINT ( 'NONE',  ( -5.000000000000000000, -77.08333333333334281, -2.886751345948128211 ) ) ;
#53221 = CARTESIAN_POINT ( 'NONE',  ( -3.152548672688508926E-16, 9.187500001365593860, -5.148502694627439702 ) ) ;
#53222 = CARTESIAN_POINT ( 'NONE',  ( -5.134616530693477992E-16, 8.895721644649725590, -7.917989418073275942 ) ) ;
#53223 = ORIENTED_EDGE ( 'NONE', *, *, #15023, .F. ) ;
#53224 =( BOUNDED_CURVE ( )  B_SPLINE_CURVE ( 2, ( #43505, #32931, #18448, #28716, #63150, #63466, #19385, #19061, #52863 ),
 .UNSPECIFIED., .F., .F. ) 
 B_SPLINE_CURVE_WITH_KNOTS ( ( 3, 2, 2, 2, 3 ),
 ( 0.8660714285714286031, 0.8666666666666666963, 0.8678571428571428825, 0.8690476190476190688, 0.8696428571428571619 ),
 .UNSPECIFIED. ) 
 CURVE ( )  GEOMETRIC_REPRESENTATION_ITEM ( )  RATIONAL_B_SPLINE_CURVE ( ( 0.9330127018922194093, 0.9330127018922194093, 1.000000000000000000, 0.8660254037844387076, 1.000000000000000000, 0.8660254037844387076, 1.000000000000000000, 0.9330127018922194093, 0.9330127018922194093 ) ) 
 REPRESENTATION_ITEM ( '' )  );
#53225 = CARTESIAN_POINT ( 'NONE',  ( 5.000000000000000888, 10.54166666939785202, 2.886751345948126879 ) ) ;
#53226 = CARTESIAN_POINT ( 'NONE',  ( 4.458734124999998549, -56.72916666530107932, -2.574251347313721627 ) ) ;
#53227 = CARTESIAN_POINT ( 'NONE',  ( -4.458734125000001214, -159.1250000013656063, 1.846868145590734089 ) ) ;
#53228 = CARTESIAN_POINT ( 'NONE',  ( -5.000000000000000000, -48.95833333060213732, -2.886751345948128211 ) ) ;
#53229 = ORIENTED_EDGE ( 'NONE', *, *, #61818, .T. ) ;
#53230 = CARTESIAN_POINT ( 'NONE',  ( -4.458734124999999437, 4.437500001365595637, 0.000000000000000000 ) ) ;
#53231 = ORIENTED_EDGE ( 'NONE', *, *, #21624, .T. ) ;
#53233 = CARTESIAN_POINT ( 'NONE',  ( -5.000000000000000888, -142.5625000027312410, 2.071067811865474617 ) ) ;
#53232 = CARTESIAN_POINT ( 'NONE',  ( 1.339745962155612702, -87.29465819873851729, -5.000000000000000000 ) ) ;
#53234 = CARTESIAN_POINT ( 'NONE',  ( 1.846868145590735200, -160.2500000013656063, -4.458734125000000326 ) ) ;
#53235 = ORIENTED_EDGE ( 'NONE', *, *, #33833, .F. ) ;
#53236 = UNCERTAINTY_MEASURE_WITH_UNIT (LENGTH_MEASURE( 1.000000000000000082E-05 ), #32118, 'distance_accuracy_value', 'NONE');
#53237 = CARTESIAN_POINT ( 'NONE',  ( -51.75738570946856498, -153.7500000000000284, 3.805975901505576964 ) ) ;
#53238 = CARTESIAN_POINT ( 'NONE',  ( -59.98410592259440222, -133.1250000000000284, -0.3983568153799752487 ) ) ;
#53239 = CARTESIAN_POINT ( 'NONE',  ( 1.339745962155612702, -47.16965819600733312, -5.000000000000000000 ) ) ;
#53240 = CARTESIAN_POINT ( 'NONE',  ( -2.229367062500000163, -37.72916666530107221, -3.861377020970580443 ) ) ;
#53241 = ORIENTED_EDGE ( 'NONE', *, *, #43618, .F. ) ;
#53242 = CARTESIAN_POINT ( 'NONE',  ( 4.458734125000001214, -80.89583333196773651, 2.574251347313718519 ) ) ;
#53243 = CARTESIAN_POINT ( 'NONE',  ( -4.458734124999999437, 16.60416666803225993, -2.574251347313719407 ) ) ;
#53244 = CARTESIAN_POINT ( 'NONE',  ( 3.061616997868383141E-16, -156.8750000027311842, -5.000000000000000000 ) ) ;
#53245 = ORIENTED_EDGE ( 'NONE', *, *, #48430, .T. ) ;
#53246 = CARTESIAN_POINT ( 'NONE',  ( 2.229367062499998831, -87.89583333196773651, -3.861377020970580887 ) ) ;
#53247 = CARTESIAN_POINT ( 'NONE',  ( -59.81910112700025905, -125.3125000027312552, -2.462841084822630311 ) ) ;
#53248 = CARTESIAN_POINT ( 'NONE',  ( -2.499999999999996447, 25.29166666939785202, 4.330127018922195425 ) ) ;
#53249 = CARTESIAN_POINT ( 'NONE',  ( -53.86834273333172973, -135.0000000000000284, 4.786490365525540192 ) ) ;
#53250 = CARTESIAN_POINT ( 'NONE',  ( -6.972266317189433020E-16, -45.12499999726880162, -5.000000000000000000 ) ) ;
#53251 = CARTESIAN_POINT ( 'NONE',  ( 2.229367062499998831, -62.64583333196774362, -3.861377020970580887 ) ) ;
#53252 = CARTESIAN_POINT ( 'NONE',  ( -1.339745962155613812, -72.08034179853027013, -5.000000000000000000 ) ) ;
#53253 = CARTESIAN_POINT ( 'NONE',  ( -4.458734124999998549, 23.77083333469892423, 2.574251347313722516 ) ) ;
#53254 = AXIS2_PLACEMENT_3D ( 'NONE', #41198, #12573, #41513 ) ;
#53255 = CARTESIAN_POINT ( 'NONE',  ( -5.000000000000000000, -109.9999999999999858, 0.000000000000000000 ) ) ;
#53256 = CARTESIAN_POINT ( 'NONE',  ( -5.000000000000000000, -82.00000000000000000, 0.000000000000000000 ) ) ;
#53257 = CARTESIAN_POINT ( 'NONE',  ( 9.457646018065525792E-16, -46.31249999863440792, 5.148502694627439702 ) ) ;
#53258 = CARTESIAN_POINT ( 'NONE',  ( -5.000000000000000000, -2.958333330602146649, -2.886751345948128211 ) ) ;
#53259 = CARTESIAN_POINT ( 'NONE',  ( -5.926426369611017623E-15, 26.37500000273118417, 5.000000000000000000 ) ) ;
#53260 = LINE ( 'NONE', #14639, #57382 ) ;
#53261 = CARTESIAN_POINT ( 'NONE',  ( -2.229367062499996610, -83.39583333196773651, 3.861377020970582219 ) ) ;
#53262 = LINE ( 'NONE', #4371, #28546 ) ;
#53263 = CARTESIAN_POINT ( 'NONE',  ( -2.229367062499996610, -11.39583333196773829, 3.861377020970582219 ) ) ;
#53264 = ORIENTED_EDGE ( 'NONE', *, *, #62495, .T. ) ;
#53265 = CARTESIAN_POINT ( 'NONE',  ( 1.975475456537005874E-15, -80.74999999999998579, 5.000000000000000000 ) ) ;
#53266 = CARTESIAN_POINT ( 'NONE',  ( -2.229367062499996610, -96.14583333196773651, 3.861377020970582219 ) ) ;
#53267 = CARTESIAN_POINT ( 'NONE',  ( -5.000000000000000888, -165.5625000027311842, 2.071067811865474617 ) ) ;
#53268 = CARTESIAN_POINT ( 'NONE',  ( 4.458734124999998549, -92.97916666530106511, -2.574251347313721627 ) ) ;
#53269 = CARTESIAN_POINT ( 'NONE',  ( -5.000000000000000000, -50.95833333060213732, -2.886751345948128211 ) ) ;
#53270 = CYLINDRICAL_SURFACE ( 'NONE', #33561, 5.000000000000000000 ) ;
#53271 = CARTESIAN_POINT ( 'NONE',  ( -57.89159099828107458, -130.6875000013656063, -3.393966926194107447 ) ) ;
#53272 = CARTESIAN_POINT ( 'NONE',  ( -53.51423613279429503, -146.2500000013656347, 4.591703134518083651 ) ) ;
#53273 = CARTESIAN_POINT ( 'NONE',  ( -2.229367062499996610, -18.14583333196773651, 3.861377020970582219 ) ) ;
#53274 = CARTESIAN_POINT ( 'NONE',  ( -4.458734124999999437, 9.354166668032261711, -2.574251347313719407 ) ) ;
#53275 = CARTESIAN_POINT ( 'NONE',  ( -4.458734124999999437, -60.64583333196774362, -2.574251347313719407 ) ) ;
#53276 = DIRECTION ( 'NONE',  ( -0.000000000000000000, 1.000000000000000000, -0.000000000000000000 ) ) ;
#53277 = CARTESIAN_POINT ( 'NONE',  ( 4.458734124999998549, -15.72916666530107399, -2.574251347313721627 ) ) ;
#53278 = FACE_OUTER_BOUND ( 'NONE', #15183, .T. ) ;
#53279 = ORIENTED_EDGE ( 'NONE', *, *, #37432, .T. ) ;
#53280 = CARTESIAN_POINT ( 'NONE',  ( -3.152548672688508926E-16, -38.81249999863440081, -5.148502694627439702 ) ) ;
#53281 = CARTESIAN_POINT ( 'NONE',  ( -57.89159099828107458, -124.9375000013656063, -3.393966926194107447 ) ) ;
#53282 = CARTESIAN_POINT ( 'NONE',  ( -2.499999999999996447, -91.70833333060214443, 4.330127018922195425 ) ) ;
#53283 = CARTESIAN_POINT ( 'NONE',  ( -5.000000000000000000, -25.00000000000000000, 0.000000000000000000 ) ) ;
#53284 = CARTESIAN_POINT ( 'NONE',  ( 9.457646018065525792E-16, -88.06249999863439371, 5.148502694627439702 ) ) ;
#53285 = CARTESIAN_POINT ( 'NONE',  ( -2.229367062500000163, 21.27083333469892779, -3.861377020970580443 ) ) ;
#53286 = CARTESIAN_POINT ( 'NONE',  ( 2.229367062499998831, 9.354166668032261711, -3.861377020970580887 ) ) ;
#53287 = DIRECTION ( 'NONE',  ( -0.000000000000000000, 1.000000000000000000, -0.000000000000000000 ) ) ;
#53288 = CARTESIAN_POINT ( 'NONE',  ( -2.499999999999996447, -6.833333333333330373, 4.330127018922195425 ) ) ;
#53289 = CARTESIAN_POINT ( 'NONE',  ( 4.458734125000000326, -88.14583333196773651, 2.574251347313718519 ) ) ;
#53290 = CARTESIAN_POINT ( 'NONE',  ( -5.000000000000000000, -72.00000000000000000, 0.000000000000000000 ) ) ;
#53291 = CARTESIAN_POINT ( 'NONE',  ( 2.500000000000002220, 13.45833333606451987, 4.330127018922192761 ) ) ;
#53292 = ORIENTED_EDGE ( 'NONE', *, *, #36244, .T. ) ;
#53293 = CYLINDRICAL_SURFACE ( 'NONE', #3778, 5.000000000000000000 ) ;
#53294 = ORIENTED_EDGE ( 'NONE', *, *, #63342, .F. ) ;
#53295 = VECTOR ( 'NONE', #21103, 1000.000000000000000 ) ;
#53296 = CARTESIAN_POINT ( 'NONE',  ( -2.499999999999996447, 16.16666666666666430, 4.330127018922195425 ) ) ;
#53298 = CARTESIAN_POINT ( 'NONE',  ( 5.000000000000000888, -28.58333333333333570, 2.886751345948126879 ) ) ;
#53297 = CARTESIAN_POINT ( 'NONE',  ( -4.999999999999998224, -103.9166666666666572, 2.886751345948131764 ) ) ;
#53299 = CARTESIAN_POINT ( 'NONE',  ( 4.458734125000001214, -31.89583333196773651, 2.574251347313718519 ) ) ;
#53300 = AXIS2_PLACEMENT_3D ( 'NONE', #17660, #26675, #12822 ) ;
#53301 =( BOUNDED_CURVE ( )  B_SPLINE_CURVE ( 2, ( #9808, #13703, #28807, #33325, #58712, #53882, #28494, #48113, #23684 ),
 .UNSPECIFIED., .F., .F. ) 
 B_SPLINE_CURVE_WITH_KNOTS ( ( 3, 2, 2, 2, 3 ),
 ( 0.8767857142857142794, 0.8773809523809523725, 0.8785714285714285587, 0.8797619047619047450, 0.8803571428571428381 ),
 .UNSPECIFIED. ) 
 CURVE ( )  GEOMETRIC_REPRESENTATION_ITEM ( )  RATIONAL_B_SPLINE_CURVE ( ( 0.9330127018922194093, 0.9330127018922194093, 1.000000000000000000, 0.8660254037844387076, 1.000000000000000000, 0.8660254037844387076, 1.000000000000000000, 0.9330127018922194093, 0.9330127018922194093 ) ) 
 REPRESENTATION_ITEM ( '' )  );
#53302 = CARTESIAN_POINT ( 'NONE',  ( 2.500000000000002220, -36.54166666393547303, 4.330127018922192761 ) ) ;
#53304 = ORIENTED_EDGE ( 'NONE', *, *, #60231, .T. ) ;
#53303 = CARTESIAN_POINT ( 'NONE',  ( -3.152548672688508926E-16, -64.56249999863440792, -5.148502694627439702 ) ) ;
#53305 = CARTESIAN_POINT ( 'NONE',  ( -59.29741812935640155, -152.8750000013656063, -2.196230717870135685 ) ) ;
#53307 = EDGE_LOOP ( 'NONE', ( #62259, #58053, #21133, #7994 ) ) ;
#53306 = CARTESIAN_POINT ( 'NONE',  ( 9.457646018065525792E-16, -12.31249999863440259, 5.148502694627439702 ) ) ;
#53308 = CARTESIAN_POINT ( 'NONE',  ( 2.500000000000002220, -74.66666666666665719, 4.330127018922192761 ) ) ;
#53309 = CARTESIAN_POINT ( 'NONE',  ( -6.972266317189433020E-16, 23.75000000000000000, -5.000000000000000000 ) ) ;
#53310 = CARTESIAN_POINT ( 'NONE',  ( -4.458734124999999437, -54.56249999863440081, 0.000000000000000000 ) ) ;
#53311 = CARTESIAN_POINT ( 'NONE',  ( 5.000000000000000000, -84.29166666393547303, -2.886751345948129988 ) ) ;
#53313 = VERTEX_POINT ( 'NONE', #15952 ) ;
#53312 = CARTESIAN_POINT ( 'NONE',  ( 1.975475456537005874E-15, -31.75000000000000000, 5.000000000000000000 ) ) ;
#53314 = CARTESIAN_POINT ( 'NONE',  ( -52.53715891517739323, -145.4375000000000284, -4.819101127000233298 ) ) ;
#53315 = CARTESIAN_POINT ( 'NONE',  ( -2.229367062500000163, -23.72916666530107577, -3.861377020970580443 ) ) ;
#53317 = ORIENTED_EDGE ( 'NONE', *, *, #6629, .F. ) ;
#53316 = CARTESIAN_POINT ( 'NONE',  ( 4.458734124999999437, -60.06249999863440081, -5.460374474430324690E-16 ) ) ;
#53318 =( BOUNDED_CURVE ( )  B_SPLINE_CURVE ( 2, ( #16876, #21069, #33178, #62458, #22024, #62136, #46466, #52793, #16559 ),
 .UNSPECIFIED., .F., .F. ) 
 B_SPLINE_CURVE_WITH_KNOTS ( ( 3, 2, 2, 2, 3 ),
 ( 0.6374999999999999556, 0.6380952380952380487, 0.6392857142857142350, 0.6404761904761904212, 0.6410714285714286254 ),
 .UNSPECIFIED. ) 
 CURVE ( )  GEOMETRIC_REPRESENTATION_ITEM ( )  RATIONAL_B_SPLINE_CURVE ( ( 0.9330127018922194093, 0.9330127018922194093, 1.000000000000000000, 0.8660254037844387076, 1.000000000000000000, 0.8660254037844387076, 1.000000000000000000, 0.9330127018922130810, 0.9330127018922194093 ) ) 
 REPRESENTATION_ITEM ( '' )  );
#53319 = CARTESIAN_POINT ( 'NONE',  ( 55.00000000000002842, 24.99999999999999645, 0.000000000000000000 ) ) ;
#53320 = CARTESIAN_POINT ( 'NONE',  ( 4.458734124999999437, -168.7500000013656063, 1.846868145590737864 ) ) ;
#53321 = CARTESIAN_POINT ( 'NONE',  ( -2.229367062499996610, -105.3958333319677365, 3.861377020970582219 ) ) ;
#53322 = CARTESIAN_POINT ( 'NONE',  ( -59.81910112700024484, -135.3125000027312126, -2.462841084822808835 ) ) ;
#53323 = ORIENTED_EDGE ( 'NONE', *, *, #52213, .F. ) ;
#53324 = CARTESIAN_POINT ( 'NONE',  ( -50.70258187064364108, -152.3750000013656063, 2.196230717870141014 ) ) ;
#53325 = CARTESIAN_POINT ( 'NONE',  ( -53.33387254593733928, -139.9375000027311842, 5.149110718188519620 ) ) ;
#53326 = CARTESIAN_POINT ( 'NONE',  ( -4.458734124999999437, -39.39583333196773651, -2.574251347313719407 ) ) ;
#53327 = PLANE ( 'NONE',  #13733 ) ;
#53328 = CARTESIAN_POINT ( 'NONE',  ( -4.458734124999999437, -15.39583333196773474, -2.574251347313719407 ) ) ;
#53329 = CARTESIAN_POINT ( 'NONE',  ( -4.458734124999999437, -99.64583333196773651, -2.574251347313719407 ) ) ;
#53330 = CARTESIAN_POINT ( 'NONE',  ( 1.846868145590736310, -145.8750000013656063, 4.458734124999999437 ) ) ;
#53331 = CARTESIAN_POINT ( 'NONE',  ( -4.458734124999999437, -27.56249999863440081, 0.000000000000000000 ) ) ;
#53332 = DIRECTION ( 'NONE',  ( -0.000000000000000000, 1.000000000000000000, -0.000000000000000000 ) ) ;
#53333 = CARTESIAN_POINT ( 'NONE',  ( -59.59170313451811296, -131.5000000013656347, 1.485763867205729394 ) ) ;
#53334 = CARTESIAN_POINT ( 'NONE',  ( 4.458734124999999437, -68.06249999863440792, -5.460374474430324690E-16 ) ) ;
#53335 = DIRECTION ( 'NONE',  ( 0.000000000000000000, 0.000000000000000000, 1.000000000000000000 ) ) ;
#53336 = CARTESIAN_POINT ( 'NONE',  ( 1.975475456537005874E-15, -109.6249999972688016, 5.000000000000000000 ) ) ;
#53337 = CARTESIAN_POINT ( 'NONE',  ( 1.846868145590735200, -142.2500000013656063, -4.458734124999999437 ) ) ;
#53338 = CARTESIAN_POINT ( 'NONE',  ( -3.152548672688508926E-16, 3.187500001365594304, -5.148502694627439702 ) ) ;
#53339 = VERTEX_POINT ( 'NONE', #40064 ) ;
#53340 = CARTESIAN_POINT ( 'NONE',  ( -2.500000000000000444, 1.833333333333332593, -4.330127018922193649 ) ) ;
#53342 = CARTESIAN_POINT ( 'NONE',  ( 4.458734124999999437, -27.81249999863440081, -5.460374474430324690E-16 ) ) ;
#53341 = CARTESIAN_POINT ( 'NONE',  ( 2.500000000000002220, -93.66666666666665719, 4.330127018922192761 ) ) ;
#53343 = CYLINDRICAL_SURFACE ( 'NONE', #27456, 5.000000000000000000 ) ;
#53344 = CARTESIAN_POINT ( 'NONE',  ( 4.458734124999998549, -73.97916666530106511, -2.574251347313721627 ) ) ;
#53345 = CARTESIAN_POINT ( 'NONE',  ( 2.229367062499998831, 21.10416666803226349, -3.861377020970580887 ) ) ;
#53346 = CARTESIAN_POINT ( 'NONE',  ( 0.000000000000000000, -170.0000000000000000, 0.000000000000000000 ) ) ;
#53347 = CARTESIAN_POINT ( 'NONE',  ( -59.29741812935640155, -143.6250000013655779, -2.196230717870135685 ) ) ;
#53348 = CARTESIAN_POINT ( 'NONE',  ( 4.458734124999999437, 1.187500001365596081, -5.460374474430324690E-16 ) ) ;
#53349 = CARTESIAN_POINT ( 'NONE',  ( -4.458734124999999437, 27.35416666803225993, -2.574251347313719407 ) ) ;
#53350 = CARTESIAN_POINT ( 'NONE',  ( 9.457646018065525792E-16, -43.31249999863440792, 5.148502694627439702 ) ) ;
#53351 = CARTESIAN_POINT ( 'NONE',  ( 2.500000000000002220, -80.66666666666665719, 4.330127018922192761 ) ) ;
#53352 = CARTESIAN_POINT ( 'NONE',  ( 4.458734124999998549, 3.270833334698929118, -2.574251347313721627 ) ) ;
#53353 = CARTESIAN_POINT ( 'NONE',  ( 4.458734124999999437, -27.06249999863440081, -5.460374474430324690E-16 ) ) ;
#53354 = CARTESIAN_POINT ( 'NONE',  ( 4.458734124999999437, -156.5000000013656347, 1.846868145590737864 ) ) ;
#53355 = CARTESIAN_POINT ( 'NONE',  ( 9.457646018065525792E-16, -69.06249999863439371, 5.148502694627439702 ) ) ;
#53356 = CARTESIAN_POINT ( 'NONE',  ( -2.500000000000000444, -104.0416666639354730, -4.330127018922193649 ) ) ;
#53357 = ADVANCED_FACE ( 'NONE', ( #40703 ), #50042, .T. ) ;
#53358 = DIRECTION ( 'NONE',  ( -0.000000000000000000, 1.000000000000000000, -0.000000000000000000 ) ) ;
#53359 = CARTESIAN_POINT ( 'NONE',  ( 0.000000000000000000, -170.0000000000000000, 0.000000000000000000 ) ) ;
#53360 = CARTESIAN_POINT ( 'NONE',  ( 2.229367062500001939, -108.2291666653010651, 3.861377020970579999 ) ) ;
#53361 = CARTESIAN_POINT ( 'NONE',  ( 2.229367062500001939, -71.22916666530107932, 3.861377020970579999 ) ) ;
#53362 = CARTESIAN_POINT ( 'NONE',  ( -5.000000000000000000, -52.08333333333332860, -2.886751345948128211 ) ) ;
#53363 = CARTESIAN_POINT ( 'NONE',  ( 5.000000000000000000, -73.41666666666665719, -2.886751345948130876 ) ) ;
#53364 = CARTESIAN_POINT ( 'NONE',  ( 5.000000000000000888, -156.0625000027312126, -2.071067811865475505 ) ) ;
#53365 = VERTEX_POINT ( 'NONE', #11439 ) ;
#53366 = DIRECTION ( 'NONE',  ( -0.000000000000000000, 1.000000000000000000, -0.000000000000000000 ) ) ;
#53367 =( BOUNDED_CURVE ( )  B_SPLINE_CURVE ( 2, ( #62089, #3240, #52116, #17069, #32487, #62407, #56948, #42447, #12244 ),
 .UNSPECIFIED., .F., .F. ) 
 B_SPLINE_CURVE_WITH_KNOTS ( ( 3, 2, 2, 2, 3 ),
 ( 0.5895833333333333481, 0.5902777777777777901, 0.5916666666666666741, 0.5930555555555555580, 0.5937500000000000000 ),
 .UNSPECIFIED. ) 
 CURVE ( )  GEOMETRIC_REPRESENTATION_ITEM ( )  RATIONAL_B_SPLINE_CURVE ( ( 0.9330127018922194093, 0.9330127018922194093, 1.000000000000000000, 0.8660254037844387076, 1.000000000000000000, 0.8660254037844387076, 1.000000000000000000, 0.9330127018922194093, 0.9330127018922194093 ) ) 
 REPRESENTATION_ITEM ( '' )  );
#53368 = CARTESIAN_POINT ( 'NONE',  ( 1.975475456537005874E-15, -27.62499999726881228, 5.000000000000000000 ) ) ;
#53369 = CARTESIAN_POINT ( 'NONE',  ( -4.999999999999999112, -14.91666666666666785, 2.886751345948131764 ) ) ;
#53370 = CARTESIAN_POINT ( 'NONE',  ( -3.152548672688508926E-16, -19.56249999863440081, -5.148502694627439702 ) ) ;
#53371 = CARTESIAN_POINT ( 'NONE',  ( 2.229367062500001939, -75.97916666530106511, 3.861377020970579999 ) ) ;
#53372 = CARTESIAN_POINT ( 'NONE',  ( -3.152801135295367985, -168.0625000013656063, 3.152801135295367096 ) ) ;
#53373 = ADVANCED_FACE ( 'NONE', ( #15638 ), #529, .T. ) ;
#53374 = CARTESIAN_POINT ( 'NONE',  ( -2.499999999999996447, -19.70833333060214798, 4.330127018922195425 ) ) ;
#53376 = ORIENTED_EDGE ( 'NONE', *, *, #16124, .T. ) ;
#53375 = CARTESIAN_POINT ( 'NONE',  ( -2.229367062500000163, -46.47916666530106511, -3.861377020970580443 ) ) ;
#53377 = CARTESIAN_POINT ( 'NONE',  ( -5.000000000000000000, -27.87499999726880873, 0.000000000000000000 ) ) ;
#53378 = ADVANCED_FACE ( 'NONE', ( #10166 ), #55527, .T. ) ;
#53380 = ORIENTED_EDGE ( 'NONE', *, *, #16921, .F. ) ;
#53379 = CARTESIAN_POINT ( 'NONE',  ( 4.458734124999999437, 0.9375000013655959696, -5.460374474430324690E-16 ) ) ;
#53381 = CARTESIAN_POINT ( 'NONE',  ( -51.60603307380591787, -152.9375000013656063, -2.891590998281053704 ) ) ;
#53382 = CARTESIAN_POINT ( 'NONE',  ( 5.000000000000000888, -63.58333333333332149, 2.886751345948126879 ) ) ;
#53383 = CARTESIAN_POINT ( 'NONE',  ( -1.846868145590737420, -157.0000000013655779, 4.458734124999999437 ) ) ;
#53384 = CARTESIAN_POINT ( 'NONE',  ( 4.458734125000001214, -43.14583333196773651, 2.574251347313718519 ) ) ;
#53385 = AXIS2_PLACEMENT_3D ( 'NONE', #62986, #43035, #37905 ) ;
#53386 = CARTESIAN_POINT ( 'NONE',  ( -2.499999999999996447, -55.83333333333332860, 4.330127018922195425 ) ) ;
#53387 = CARTESIAN_POINT ( 'NONE',  ( 2.071067811865475505, -160.8125000000000284, -5.000000000000000888 ) ) ;
#53388 = CARTESIAN_POINT ( 'NONE',  ( 6.123233995736766282E-16, -120.0000000000000000, -5.000000000000000000 ) ) ;
#53389 = VECTOR ( 'NONE', #10097, 1000.000000000000000 ) ;
#53390 = CARTESIAN_POINT ( 'NONE',  ( -58.39396692619412477, -128.6875000013656063, 2.891590998281057701 ) ) ;
#53391 = CARTESIAN_POINT ( 'NONE',  ( 2.229367062499998831, -7.895833331967735624, -3.861377020970580887 ) ) ;
#53392 = CARTESIAN_POINT ( 'NONE',  ( -4.458734124999998549, -46.47916666530107221, 2.574251347313722516 ) ) ;
#53393 = DIRECTION ( 'NONE',  ( -0.000000000000000000, 1.000000000000000000, -0.000000000000000000 ) ) ;
#53394 = CARTESIAN_POINT ( 'NONE',  ( 4.458734125000000326, -147.3750000013656063, -1.846868145590734978 ) ) ;
#53395 = CARTESIAN_POINT ( 'NONE',  ( -4.458734124999999437, -91.64583333196773651, -2.574251347313719407 ) ) ;
#53396 = CARTESIAN_POINT ( 'NONE',  ( 1.339745962155615144, -34.58034179853028434, 4.999999999999999112 ) ) ;
#53397 = ORIENTED_EDGE ( 'NONE', *, *, #23969, .T. ) ;
#53398 = CARTESIAN_POINT ( 'NONE',  ( -60.14911071818854538, -152.0625000000000000, 1.666127454062681146 ) ) ;
#53399 = CARTESIAN_POINT ( 'NONE',  ( -53.33387254593733928, -151.9375000027312126, 5.149110718188519620 ) ) ;
#53400 = CYLINDRICAL_SURFACE ( 'NONE', #52772, 5.000000000000000000 ) ;
#53401 = EDGE_LOOP ( 'NONE', ( #49130, #17677, #7717, #22578 ) ) ;
#53402 = CARTESIAN_POINT ( 'NONE',  ( 1.975475456537005874E-15, 12.37500000273118417, 5.000000000000000000 ) ) ;
#53403 = EDGE_CURVE ( 'NONE', #17776, #30563, #8344, .T. ) ;
#53404 = CARTESIAN_POINT ( 'NONE',  ( 9.457646018065525792E-16, -10.31249999863440614, 5.148502694627439702 ) ) ;
#53405 = FACE_OUTER_BOUND ( 'NONE', #17497, .T. ) ;
#53406 = CARTESIAN_POINT ( 'NONE',  ( 2.229367062499998831, -2.645833331967738289, -3.861377020970580887 ) ) ;
#53407 = CYLINDRICAL_SURFACE ( 'NONE', #46981, 5.000000000000000000 ) ;
#53408 = CARTESIAN_POINT ( 'NONE',  ( 4.458734124999999437, -154.4375000013655779, 0.000000000000000000 ) ) ;
#53409 =( BOUNDED_CURVE ( )  B_SPLINE_CURVE ( 2, ( #35948, #35626, #44955, #50732, #21472, #20520, #44625, #59115, #1236 ),
 .UNSPECIFIED., .F., .F. ) 
 B_SPLINE_CURVE_WITH_KNOTS ( ( 3, 2, 2, 2, 3 ),
 ( 0.5732142857142856762, 0.5738095238095237693, 0.5749999999999999556, 0.5761904761904761418, 0.5767857142857142350 ),
 .UNSPECIFIED. ) 
 CURVE ( )  GEOMETRIC_REPRESENTATION_ITEM ( )  RATIONAL_B_SPLINE_CURVE ( ( 0.9330127018922194093, 0.9330127018922194093, 1.000000000000000000, 0.8660254037844387076, 1.000000000000000000, 0.8660254037844387076, 1.000000000000000000, 0.9330127018922194093, 0.9330127018922194093 ) ) 
 REPRESENTATION_ITEM ( '' )  );
#53410 = CARTESIAN_POINT ( 'NONE',  ( -2.229367062500000163, 20.27083333469892779, -3.861377020970580443 ) ) ;
#53411 = ORIENTED_EDGE ( 'NONE', *, *, #18866, .F. ) ;
#53412 = CARTESIAN_POINT ( 'NONE',  ( 9.457646018065525792E-16, -94.06249999863439371, 5.148502694627439702 ) ) ;
#53413 = CARTESIAN_POINT ( 'NONE',  ( -51.75738570946856498, -142.7500000000000284, 3.805975901505576964 ) ) ;
#53414 = DIRECTION ( 'NONE',  ( 0.000000000000000000, 1.000000000000000000, 0.000000000000000000 ) ) ;
#53415 = CARTESIAN_POINT ( 'NONE',  ( -4.458734124999999437, -12.31249999863440259, 0.000000000000000000 ) ) ;
#53416 = DIRECTION ( 'NONE',  ( -0.000000000000000000, 1.000000000000000000, -0.000000000000000000 ) ) ;
#53417 = DIRECTION ( 'NONE',  ( -0.000000000000000000, 1.000000000000000000, -0.000000000000000000 ) ) ;
#53418 = CARTESIAN_POINT ( 'NONE',  ( -57.89159099828107458, -152.6875000013656063, -3.393966926194107447 ) ) ;
#53419 = CARTESIAN_POINT ( 'NONE',  ( -5.000000000000000000, -38.87499999726880162, 0.000000000000000000 ) ) ;
#53420 = CARTESIAN_POINT ( 'NONE',  ( 2.229367062500001939, 17.02083333469892779, 3.861377020970579999 ) ) ;
#53421 = CARTESIAN_POINT ( 'NONE',  ( 2.499999999999998668, -46.20833333060214443, -4.330127018922193649 ) ) ;
#53422 = ORIENTED_EDGE ( 'NONE', *, *, #57397, .T. ) ;
#53423 = CARTESIAN_POINT ( 'NONE',  ( -4.458734124999999437, 15.60416666803225993, -2.574251347313719407 ) ) ;
#53424 = CARTESIAN_POINT ( 'NONE',  ( 9.457646018065525792E-16, -62.06249999863440792, 5.148502694627439702 ) ) ;
#53425 = VECTOR ( 'NONE', #57715, 1000.000000000000000 ) ;
#53426 = CARTESIAN_POINT ( 'NONE',  ( 9.457646018065525792E-16, -8.312499998634406140, 5.148502694627439702 ) ) ;
#53427 = CARTESIAN_POINT ( 'NONE',  ( -4.999999999999998224, -33.79166666393547303, 2.886751345948131764 ) ) ;
#53428 = CARTESIAN_POINT ( 'NONE',  ( -4.999999999999999112, 9.083333333333333925, 2.886751345948131764 ) ) ;
#53429 = CARTESIAN_POINT ( 'NONE',  ( -4.458734125000000326, -166.0000000013656063, -1.846868145590735644 ) ) ;
#53430 = CARTESIAN_POINT ( 'NONE',  ( 1.339745962155612702, -88.29465819873851729, -5.000000000000000000 ) ) ;
#53431 = VECTOR ( 'NONE', #4090, 1000.000000000000000 ) ;
#53432 = CARTESIAN_POINT ( 'NONE',  ( 4.458734125000001214, -52.89583333196772941, 2.574251347313718519 ) ) ;
#53433 = CARTESIAN_POINT ( 'NONE',  ( 2.500000000000002220, -87.54166666393547303, 4.330127018922192761 ) ) ;
#53434 = EDGE_CURVE ( 'NONE', #48933, #45427, #3460, .T. ) ;
#53435 = CARTESIAN_POINT ( 'NONE',  ( -57.19623071787017210, -136.6250000013655779, 4.297418129356382899 ) ) ;
#53436 = FACE_OUTER_BOUND ( 'NONE', #57142, .T. ) ;
#53437 = CARTESIAN_POINT ( 'NONE',  ( 0.000000000000000000, -170.0000000000000000, 5.000000000000000000 ) ) ;
#53438 = CARTESIAN_POINT ( 'NONE',  ( 4.458734125000000326, -90.14583333196773651, 2.574251347313718519 ) ) ;
#53439 = CARTESIAN_POINT ( 'NONE',  ( 2.730187237215162345E-16, -152.4375000013655779, -4.458734124999999437 ) ) ;
#53440 = CARTESIAN_POINT ( 'NONE',  ( 2.500000000000002220, -35.66666666666666430, 4.330127018922192761 ) ) ;
#53441 = CARTESIAN_POINT ( 'NONE',  ( -51.75738570946856498, -139.7500000000000000, 3.805975901505576964 ) ) ;
#53442 = CARTESIAN_POINT ( 'NONE',  ( 1.339745962155612702, -22.29465819873851729, -5.000000000000000000 ) ) ;
#53443 = VERTEX_POINT ( 'NONE', #24966 ) ;
#53444 = CARTESIAN_POINT ( 'NONE',  ( -2.229367062500000163, -100.4791666653010651, -3.861377020970580443 ) ) ;
#53445 = CARTESIAN_POINT ( 'NONE',  ( -3.152548672688508926E-16, 9.187500001365593860, -5.148502694627439702 ) ) ;
#53446 = CARTESIAN_POINT ( 'NONE',  ( 0.000000000000000000, -170.0000000000000000, 5.000000000000000000 ) ) ;
#53447 = CARTESIAN_POINT ( 'NONE',  ( -5.000000000000000000, 1.916666666666667407, -2.886751345948128211 ) ) ;
#53448 = EDGE_CURVE ( 'NONE', #57369, #43327, #45218, .T. ) ;
#53449 = CARTESIAN_POINT ( 'NONE',  ( -4.458734124999999437, -62.31249999863440792, 0.000000000000000000 ) ) ;
#53450 = B_SPLINE_CURVE_WITH_KNOTS ( 'NONE', 3,
 ( #56767, #56453, #13001, #61909, #60961, #17829 ),
 .UNSPECIFIED., .F., .F.,
 ( 4, 2, 4 ),
 ( 0.004444412883774334112, 0.006655097293744431999, 0.008865781703714530754 ),
 .UNSPECIFIED. ) ;
#53451 = CARTESIAN_POINT ( 'NONE',  ( -6.324555320336760822, 0.000000000000000000, 8.999999999999998224 ) ) ;
#53452 = CARTESIAN_POINT ( 'NONE',  ( -2.500000000000000444, -1.041666663935479686, -4.330127018922193649 ) ) ;
#53453 = CARTESIAN_POINT ( 'NONE',  ( -4.458734124999998549, -26.22916666530106866, 2.574251347313722516 ) ) ;
#53454 = CARTESIAN_POINT ( 'NONE',  ( 5.000000000000000888, -156.9375000000000000, -2.071067811865475505 ) ) ;
#53455 = EDGE_CURVE ( 'NONE', #61074, #35844, #30495, .T. ) ;
#53456 = CARTESIAN_POINT ( 'NONE',  ( 1.975475456537005874E-15, -20.74999999999999645, 5.000000000000000000 ) ) ;
#53457 = CARTESIAN_POINT ( 'NONE',  ( -5.000000000000000000, -47.00000000000000000, 0.000000000000000000 ) ) ;
#53458 = EDGE_CURVE ( 'NONE', #11542, #141, #41200, .T. ) ;
#53460 = CARTESIAN_POINT ( 'NONE',  ( -4.458734124999998549, -23.47916666530107577, 2.574251347313722516 ) ) ;
#53459 = CARTESIAN_POINT ( 'NONE',  ( -2.499999999999996447, -89.70833333060214443, 4.330127018922195425 ) ) ;
#53461 = LINE ( 'NONE', #48002, #48108 ) ;
#53462 = CARTESIAN_POINT ( 'NONE',  ( 4.458734125000001214, -70.89583333196773651, 2.574251347313718519 ) ) ;
#53463 = CARTESIAN_POINT ( 'NONE',  ( 4.458734125000000326, -145.6250000013655779, -1.846868145590734978 ) ) ;
#53464 = CARTESIAN_POINT ( 'NONE',  ( -4.458734124999998549, -76.22916666530107932, 2.574251347313722516 ) ) ;
#53465 = CARTESIAN_POINT ( 'NONE',  ( -56.48576386720575471, -139.0000000013655779, -4.591703134518078322 ) ) ;
#53466 = CARTESIAN_POINT ( 'NONE',  ( 4.458734124999999437, -25.06249999863440792, -5.460374474430324690E-16 ) ) ;
#53467 = CARTESIAN_POINT ( 'NONE',  ( 5.000000000000000000, -64.29166666393547303, -2.886751345948129988 ) ) ;
#53468 = ORIENTED_EDGE ( 'NONE', *, *, #34579, .T. ) ;
#53469 = DIRECTION ( 'NONE',  ( -0.000000000000000000, 1.000000000000000000, -0.000000000000000000 ) ) ;
#53470 = ORIENTED_EDGE ( 'NONE', *, *, #12141, .T. ) ;
#53471 = CARTESIAN_POINT ( 'NONE',  ( 2.229367062499998831, -71.89583333196773651, -3.861377020970580887 ) ) ;
#53472 = CARTESIAN_POINT ( 'NONE',  ( 3.535533905932738197, -165.8750000000000284, -3.535533905932738197 ) ) ;
#53473 = EDGE_LOOP ( 'NONE', ( #48547, #46697, #2768, #59801 ) ) ;
#53474 = VECTOR ( 'NONE', #17455, 1000.000000000000000 ) ;
#53475 = FACE_OUTER_BOUND ( 'NONE', #15259, .T. ) ;
#53477 = VECTOR ( 'NONE', #41185, 1000.000000000000000 ) ;
#53476 = CARTESIAN_POINT ( 'NONE',  ( -57.46284108482265651, -143.0625000027312126, 4.819101127000238627 ) ) ;
#53478 = EDGE_CURVE ( 'NONE', #9545, #45336, #22377, .T. ) ;
#53479 = CARTESIAN_POINT ( 'NONE',  ( -2.229367062500000163, -59.72916666530106511, -3.861377020970580443 ) ) ;
#53480 = CARTESIAN_POINT ( 'NONE',  ( 4.458734124999998549, 0.02083333469892617584, -2.574251347313721627 ) ) ;
#53481 = VERTEX_POINT ( 'NONE', #16591 ) ;
#53482 = DIRECTION ( 'NONE',  ( 0.000000000000000000, 0.000000000000000000, 1.000000000000000000 ) ) ;
#53483 = CARTESIAN_POINT ( 'NONE',  ( -5.000000000000000000, 29.04166666939785557, -2.886751345948128211 ) ) ;
#53484 = CARTESIAN_POINT ( 'NONE',  ( 9.457646018065525792E-16, 12.93750000136559386, 5.148502694627439702 ) ) ;
#53485 = CARTESIAN_POINT ( 'NONE',  ( -50.40829686548195099, -146.0000000013656347, -1.485763867205728284 ) ) ;
#53486 = CARTESIAN_POINT ( 'NONE',  ( -1.846868145590737420, -166.7500000013655779, 4.458734124999997661 ) ) ;
#53487 = ORIENTED_EDGE ( 'NONE', *, *, #8612, .F. ) ;
#53488 = CARTESIAN_POINT ( 'NONE',  ( -2.229367062500000163, -74.47916666530106511, -3.861377020970580443 ) ) ;
#53489 = CARTESIAN_POINT ( 'NONE',  ( 5.000000000000000888, -0.4583333306021481479, 2.886751345948126879 ) ) ;
#53490 = CARTESIAN_POINT ( 'NONE',  ( -2.229367062500000163, 2.520833334698928230, -3.861377020970580443 ) ) ;
#53491 =( BOUNDED_CURVE ( )  B_SPLINE_CURVE ( 2, ( #12209, #11877, #21867, #1949, #21550, #61430, #17353, #41146, #36977 ),
 .UNSPECIFIED., .F., .F. ) 
 B_SPLINE_CURVE_WITH_KNOTS ( ( 3, 2, 2, 2, 3 ),
 ( 0.9395833333333333259, 0.9402777777777777679, 0.9416666666666666519, 0.9430555555555555358, 0.9437499999999999778 ),
 .UNSPECIFIED. ) 
 CURVE ( )  GEOMETRIC_REPRESENTATION_ITEM ( )  RATIONAL_B_SPLINE_CURVE ( ( 0.9330127018922194093, 0.9330127018922194093, 1.000000000000000000, 0.8660254037844387076, 1.000000000000000000, 0.8660254037844387076, 1.000000000000000000, 0.9330127018922194093, 0.9330127018922194093 ) ) 
 REPRESENTATION_ITEM ( '' )  );
#53492 = CARTESIAN_POINT ( 'NONE',  ( 1.975475456537005874E-15, -19.62499999726881228, 5.000000000000000000 ) ) ;
#53493 = CARTESIAN_POINT ( 'NONE',  ( 4.458734124999998549, -64.97916666530106511, -2.574251347313721627 ) ) ;
#53494 = CARTESIAN_POINT ( 'NONE',  ( -3.535250795749689387E-16, -24.12499999726881583, -5.773502691896257311 ) ) ;
#53495 = CARTESIAN_POINT ( 'NONE',  ( -58.24261429053147765, -142.3750000027312126, -3.805975901505573855 ) ) ;
#53496 = CARTESIAN_POINT ( 'NONE',  ( 5.000000000000000000, -44.29166666393546592, -2.886751345948130876 ) ) ;
#53497 = CARTESIAN_POINT ( 'NONE',  ( 1.975475456537005874E-15, -49.74999999999999289, 5.000000000000000000 ) ) ;
#53498 = CARTESIAN_POINT ( 'NONE',  ( -2.499999999999996447, -105.7083333306021444, 4.330127018922195425 ) ) ;
#53499 = CARTESIAN_POINT ( 'NONE',  ( 5.000000000000000000, -3.291666663935478354, -2.886751345948130876 ) ) ;
#53500 = CARTESIAN_POINT ( 'NONE',  ( 4.458734124999999437, -44.81249999863440081, -5.460374474430324690E-16 ) ) ;
#53501 = CARTESIAN_POINT ( 'NONE',  ( -3.152548672688508926E-16, -26.81249999863440436, -5.148502694627439702 ) ) ;
#53502 = CARTESIAN_POINT ( 'NONE',  ( 9.457646018065525792E-16, 7.687500001365596525, 5.148502694627439702 ) ) ;
#53503 = LINE ( 'NONE', #18146, #14532 ) ;
#53504 = CARTESIAN_POINT ( 'NONE',  ( 1.060575238724906964E-15, 23.25000000000000000, 5.773502691896257311 ) ) ;
#53505 = CARTESIAN_POINT ( 'NONE',  ( -2.071067811865475061, -149.8125000027311842, -5.000000000000000888 ) ) ;
#53506 = CARTESIAN_POINT ( 'NONE',  ( 2.788906526875773208E-15, 28.75000000000000000, -5.000000000000000000 ) ) ;
#53507 = CARTESIAN_POINT ( 'NONE',  ( 4.458734124999999437, -38.81249999863440081, -5.460374474430324690E-16 ) ) ;
#53508 = CARTESIAN_POINT ( 'NONE',  ( -4.999999999999999112, -66.79166666393548724, 2.886751345948131764 ) ) ;
#53509 = CARTESIAN_POINT ( 'NONE',  ( -59.59170313451811296, -149.7500000013656063, 1.485763867205729394 ) ) ;
#53510 = CARTESIAN_POINT ( 'NONE',  ( -9.184850993605147944E-16, -141.2500000000000284, 5.000000000000000000 ) ) ;
#53511 = EDGE_CURVE ( 'NONE', #55695, #47768, #25618, .T. ) ;
#53512 = EDGE_CURVE ( 'NONE', #4271, #38750, #2445, .T. ) ;
#53513 = CARTESIAN_POINT ( 'NONE',  ( 4.458734124999999437, -74.06249999863440792, -5.460374474430324690E-16 ) ) ;
#53514 = CARTESIAN_POINT ( 'NONE',  ( -1.846868145590734756, -166.3750000013656063, -4.458734124999999437 ) ) ;
#53515 = CARTESIAN_POINT ( 'NONE',  ( 2.229367062500001939, -28.97916666530107221, 3.861377020970579999 ) ) ;
#53516 = ADVANCED_FACE ( 'NONE', ( #37477 ), #56478, .T. ) ;
#53517 = DIRECTION ( 'NONE',  ( 0.000000000000000000, 0.000000000000000000, 1.000000000000000000 ) ) ;
#53518 = DIRECTION ( 'NONE',  ( 0.000000000000000000, 0.000000000000000000, 1.000000000000000000 ) ) ;
#53519 = CARTESIAN_POINT ( 'NONE',  ( 2.499999999999998668, -22.33333333333332860, -4.330127018922193649 ) ) ;
#53520 = CARTESIAN_POINT ( 'NONE',  ( 4.458734124999999437, -142.4375000013656063, 0.000000000000000000 ) ) ;
#53521 = ORIENTED_EDGE ( 'NONE', *, *, #24694, .F. ) ;
#53522 = CARTESIAN_POINT ( 'NONE',  ( 4.458734124999999437, 26.93750000136559564, -5.460374474430324690E-16 ) ) ;
#53523 = CARTESIAN_POINT ( 'NONE',  ( -53.33387254593710480, -140.8125000000000284, 5.149110718188539160 ) ) ;
#53524 = CARTESIAN_POINT ( 'NONE',  ( 4.458734124999999437, -55.06249999863440081, -5.460374474430324690E-16 ) ) ;
#53525 = CARTESIAN_POINT ( 'NONE',  ( -2.499999999999996447, 28.29166666939785202, 4.330127018922195425 ) ) ;
#53526 = CARTESIAN_POINT ( 'NONE',  ( -3.535533905932738641, -162.3750000000000284, 3.535533905932737309 ) ) ;
#53527 = CARTESIAN_POINT ( 'NONE',  ( 1.060575238724906964E-15, 21.24999999999999645, 5.773502691896257311 ) ) ;
#53528 = EDGE_CURVE ( 'NONE', #2442, #36547, #47772, .T. ) ;
#53529 = CARTESIAN_POINT ( 'NONE',  ( -2.499999999999996447, -36.70833333060213732, 4.330127018922195425 ) ) ;
#53530 = CARTESIAN_POINT ( 'NONE',  ( -3.152548672688508926E-16, -8.562499998634404363, -5.148502694627439702 ) ) ;
#53531 = CARTESIAN_POINT ( 'NONE',  ( -2.500000000000000444, 3.833333333333334370, -4.330127018922193649 ) ) ;
#53532 = CARTESIAN_POINT ( 'NONE',  ( 3.535533905932738197, -165.0000000027312126, -3.535533905932738197 ) ) ;
#53533 = CARTESIAN_POINT ( 'NONE',  ( 4.406842699996126989, -6.115962218725295330, -6.291760732204942919E-15 ) ) ;
#53534 = EDGE_CURVE ( 'NONE', #34309, #59250, #43255, .T. ) ;
#53535 = EDGE_CURVE ( 'NONE', #43806, #62517, #3831, .T. ) ;
#53536 = CARTESIAN_POINT ( 'NONE',  ( 5.000000000000000000, -12.41666666666666607, -2.886751345948130876 ) ) ;
#53537 = CARTESIAN_POINT ( 'NONE',  ( -2.229367062500000163, -21.47916666530107221, -3.861377020970580443 ) ) ;
#53538 = CARTESIAN_POINT ( 'NONE',  ( -49.85088928181150436, -135.5625000000000000, -1.666127454062680480 ) ) ;
#53539 = CARTESIAN_POINT ( 'NONE',  ( -2.229367062500000163, -52.47916666530107221, -3.861377020970580443 ) ) ;
#53540 = CARTESIAN_POINT ( 'NONE',  ( -4.458734125000001214, -155.1250000013655779, 1.846868145590734089 ) ) ;
#53541 = ADVANCED_FACE ( 'NONE', ( #21743 ), #2756, .T. ) ;
#53542 = CARTESIAN_POINT ( 'NONE',  ( -3.535250795749689387E-16, -49.12499999726881583, -5.773502691896257311 ) ) ;
#53543 = ORIENTED_EDGE ( 'NONE', *, *, #2095, .T. ) ;
#53544 = CARTESIAN_POINT ( 'NONE',  ( 4.458734124999998549, 6.020833334698928674, -2.574251347313721627 ) ) ;
#53545 = EDGE_LOOP ( 'NONE', ( #3162, #52669, #14740, #36593 ) ) ;
#53546 =( BOUNDED_CURVE ( )  B_SPLINE_CURVE ( 2, ( #3813, #23437, #57538, #27928, #58466, #34013, #62678, #18600, #33388 ),
 .UNSPECIFIED., .F., .F. ) 
 B_SPLINE_CURVE_WITH_KNOTS ( ( 3, 2, 2, 2, 3 ),
 ( 0.6604166666666666519, 0.6611111111111110938, 0.6624999999999999778, 0.6638888888888888618, 0.6645833333333333037 ),
 .UNSPECIFIED. ) 
 CURVE ( )  GEOMETRIC_REPRESENTATION_ITEM ( )  RATIONAL_B_SPLINE_CURVE ( ( 0.9330127018922194093, 0.9330127018922194093, 1.000000000000000000, 0.8660254037844387076, 1.000000000000000000, 0.8660254037844387076, 1.000000000000000000, 0.9330127018922194093, 0.9330127018922194093 ) ) 
 REPRESENTATION_ITEM ( '' )  );
#53548 = CARTESIAN_POINT ( 'NONE',  ( -4.999999999999998224, -67.79166666393547303, 2.886751345948131764 ) ) ;
#53547 = CARTESIAN_POINT ( 'NONE',  ( 0.000000000000000000, -120.0000000000000000, 0.000000000000000000 ) ) ;
#53549 = CARTESIAN_POINT ( 'NONE',  ( -3.152801135295367096, -162.0625000013656063, -3.152801135295367541 ) ) ;
#53550 = ORIENTED_EDGE ( 'NONE', *, *, #27265, .T. ) ;
#53551 = CARTESIAN_POINT ( 'NONE',  ( 5.000000000000000888, -87.45833333060214443, 2.886751345948126879 ) ) ;
#53552 = CARTESIAN_POINT ( 'NONE',  ( -60.14911071818854538, -132.0625000000000284, 1.666127454062681368 ) ) ;
#53553 = CARTESIAN_POINT ( 'NONE',  ( 3.061616997868383141E-16, -149.7500000000000284, -5.000000000000000000 ) ) ;
#53554 = CARTESIAN_POINT ( 'NONE',  ( -2.229367062499996610, -45.39583333196774362, 3.861377020970582219 ) ) ;
#53555 = EDGE_LOOP ( 'NONE', ( #51106, #54239, #1915, #35446 ) ) ;
#53556 = CARTESIAN_POINT ( 'NONE',  ( 0.000000000000000000, -120.0000000000000000, 5.000000000000000000 ) ) ;
#53557 = CARTESIAN_POINT ( 'NONE',  ( -4.458734124999999437, 18.68750000136559564, 0.000000000000000000 ) ) ;
#53558 = ORIENTED_EDGE ( 'NONE', *, *, #26806, .F. ) ;
#53559 = CARTESIAN_POINT ( 'NONE',  ( 4.458734125000001214, -88.14583333196773651, 2.574251347313718519 ) ) ;
#53560 = CARTESIAN_POINT ( 'NONE',  ( -56.66612745406270335, -128.4375000027312410, -5.149110718188516067 ) ) ;
#53561 = CARTESIAN_POINT ( 'NONE',  ( 1.975475456537005874E-15, -86.75000000000001421, 5.000000000000000000 ) ) ;
#53562 = CARTESIAN_POINT ( 'NONE',  ( -50.45345700379804299, -135.0000000000000000, -0.05411738794798071767 ) ) ;
#53563 = LINE ( 'NONE', #39705, #9639 ) ;
#53564 = CARTESIAN_POINT ( 'NONE',  ( 2.229367062499998831, -60.64583333196774362, -3.861377020970580887 ) ) ;
#53565 = CARTESIAN_POINT ( 'NONE',  ( 5.147825380264231754, 5.688155668806028409, -7.450218641347809090 ) ) ;
#53566 = AXIS2_PLACEMENT_3D ( 'NONE', #61120, #12528, #17044 ) ;
#53567 = CARTESIAN_POINT ( 'NONE',  ( -3.152548672688508926E-16, 18.43750000136559564, -5.148502694627439702 ) ) ;
#53568 = CARTESIAN_POINT ( 'NONE',  ( 1.339745962155615144, -102.5803417985302843, 4.999999999999999112 ) ) ;
#53569 = CARTESIAN_POINT ( 'NONE',  ( -1.339745962155613812, -44.20534180126147561, -5.000000000000000000 ) ) ;
#53570 = CARTESIAN_POINT ( 'NONE',  ( 2.229367062499998831, -48.89583333196772941, -3.861377020970580887 ) ) ;
#53571 = CARTESIAN_POINT ( 'NONE',  ( -2.500000000000000444, -3.041666663935477910, -4.330127018922193649 ) ) ;
#53572 = DIRECTION ( 'NONE',  ( 0.000000000000000000, 0.000000000000000000, 1.000000000000000000 ) ) ;
#53573 = CARTESIAN_POINT ( 'NONE',  ( 2.229367062499998831, -83.89583333196773651, -3.861377020970580887 ) ) ;
#53574 = PRODUCT_DEFINITION ( 'UNKNOWN', '', #26680, #63075 ) ;
#53575 = CARTESIAN_POINT ( 'NONE',  ( 2.229367062500001939, -105.9791666653010651, 3.861377020970579999 ) ) ;
#53576 = CARTESIAN_POINT ( 'NONE',  ( -4.458734124999999437, -10.64583333196773829, -2.574251347313719407 ) ) ;
#53577 = VERTEX_POINT ( 'NONE', #48064 ) ;
#53578 = CARTESIAN_POINT ( 'NONE',  ( -2.071067811865308972, -155.4375000027312126, 5.000000000000169642 ) ) ;
#53579 = CARTESIAN_POINT ( 'NONE',  ( 4.458734125000001214, -96.89583333196772230, 2.574251347313718519 ) ) ;
#53580 = CARTESIAN_POINT ( 'NONE',  ( 2.071067811865475505, -162.9375000027312126, -5.000000000000000888 ) ) ;
#53581 = CARTESIAN_POINT ( 'NONE',  ( -4.458734124999998549, -93.47916666530106511, 2.574251347313722516 ) ) ;
#53582 = DIRECTION ( 'NONE',  ( -0.000000000000000000, 1.000000000000000000, -0.000000000000000000 ) ) ;
#53583 = CARTESIAN_POINT ( 'NONE',  ( 5.000000000000000000, -54.37499999726880162, -6.123233995736766282E-16 ) ) ;
#53584 = CARTESIAN_POINT ( 'NONE',  ( -6.972266317189433020E-16, -40.12499999726880162, -5.000000000000000000 ) ) ;
#53585 = CARTESIAN_POINT ( 'NONE',  ( -54.64476657466781973, -128.8125000013656063, -4.444560631937228834 ) ) ;
#53586 = CARTESIAN_POINT ( 'NONE',  ( -52.80376928212989185, -144.8750000013656063, -4.297418129356378458 ) ) ;
#53587 = CARTESIAN_POINT ( 'NONE',  ( 4.458734124999998549, -17.72916666530106866, -2.574251347313721627 ) ) ;
#53588 = CARTESIAN_POINT ( 'NONE',  ( 2.229367062500001939, 9.770833334698927786, 3.861377020970579999 ) ) ;
#53589 = CARTESIAN_POINT ( 'NONE',  ( 4.458734124999999437, -59.06249999863440081, -5.460374474430324690E-16 ) ) ;
#53590 = CARTESIAN_POINT ( 'NONE',  ( 0.000000000000000000, -120.0000000000000000, 0.000000000000000000 ) ) ;
#53591 = CARTESIAN_POINT ( 'NONE',  ( -4.458734124999997661, -12.22916666530106866, 2.574251347313722516 ) ) ;
#53592 = CARTESIAN_POINT ( 'NONE',  ( 6.123233995736766282E-16, -170.0000000000000000, -5.000000000000000000 ) ) ;
#53593 = CARTESIAN_POINT ( 'NONE',  ( -5.000000000000000000, -154.5000000000000284, -6.123233995736766282E-16 ) ) ;
#53594 = VERTEX_POINT ( 'NONE', #33902 ) ;
#53595 = CARTESIAN_POINT ( 'NONE',  ( 9.457646018065525792E-16, -39.31249999863439371, 5.148502694627439702 ) ) ;
#53596 =( BOUNDED_CURVE ( )  B_SPLINE_CURVE ( 2, ( #12436, #41692, #11789, #46539, #42331, #52318, #16629, #61339, #55877 ),
 .UNSPECIFIED., .F., .F. ) 
 B_SPLINE_CURVE_WITH_KNOTS ( ( 3, 2, 2, 2, 3 ),
 ( 0.06041666666666666713, 0.06111111111111110911, 0.06250000000000000000, 0.06388888888888888395, 0.06458333333333333981 ),
 .UNSPECIFIED. ) 
 CURVE ( )  GEOMETRIC_REPRESENTATION_ITEM ( )  RATIONAL_B_SPLINE_CURVE ( ( 0.9330127018922194093, 0.9330127018922194093, 1.000000000000000000, 0.8660254037844387076, 1.000000000000000000, 0.8660254037844387076, 1.000000000000000000, 0.9330127018922187432, 0.9330127018922194093 ) ) 
 REPRESENTATION_ITEM ( '' )  );
#53597 = CARTESIAN_POINT ( 'NONE',  ( -52.10840900171896806, -125.4375000013656063, 3.393966926194110556 ) ) ;
#53598 = CARTESIAN_POINT ( 'NONE',  ( -1.249327701954873415, 8.410337540189265937, -7.776713651267812999 ) ) ;
#53599 = CARTESIAN_POINT ( 'NONE',  ( 6.123233995736766282E-16, -120.0000000000000000, -5.000000000000000000 ) ) ;
#53600 = CARTESIAN_POINT ( 'NONE',  ( -2.229367062499996610, -86.14583333196773651, 3.861377020970582219 ) ) ;
#53601 = CARTESIAN_POINT ( 'NONE',  ( -2.229367062500000163, 18.27083333469892779, -3.861377020970580443 ) ) ;
#53602 = CARTESIAN_POINT ( 'NONE',  ( -2.229367062499996610, 8.854166668032261711, 3.861377020970582219 ) ) ;
#53603 = CARTESIAN_POINT ( 'NONE',  ( 2.500000000000002220, -93.66666666666665719, 4.330127018922192761 ) ) ;
#53604 = DIRECTION ( 'NONE',  ( -0.000000000000000000, 1.000000000000000000, -0.000000000000000000 ) ) ;
#53605 = CARTESIAN_POINT ( 'NONE',  ( 4.458734125000000326, -90.14583333196773651, 2.574251347313718519 ) ) ;
#53606 = CARTESIAN_POINT ( 'NONE',  ( -4.458734124999998549, 22.52083333469892423, 2.574251347313722516 ) ) ;
#53607 = CARTESIAN_POINT ( 'NONE',  ( 2.500000000000002220, -72.66666666666667140, 4.330127018922192761 ) ) ;
#53608 = CARTESIAN_POINT ( 'NONE',  ( -5.000000000000000000, 16.04166666939785202, -2.886751345948128211 ) ) ;
#53610 = EDGE_LOOP ( 'NONE', ( #35138, #35133, #30474, #59015 ) ) ;
#53609 = EDGE_CURVE ( 'NONE', #19205, #36935, #21217, .T. ) ;
#53611 = CARTESIAN_POINT ( 'NONE',  ( 1.975475456537005874E-15, -6.624999997268813168, 5.000000000000000000 ) ) ;
#53612 = ORIENTED_EDGE ( 'NONE', *, *, #43702, .T. ) ;
#53614 = CARTESIAN_POINT ( 'NONE',  ( 5.000000000000000000, -34.41666666666666430, -2.886751345948129988 ) ) ;
#53613 = CYLINDRICAL_SURFACE ( 'NONE', #23472, 5.000000000000000000 ) ;
#53615 = CARTESIAN_POINT ( 'NONE',  ( 2.229367062499998831, -35.64583333196772941, -3.861377020970580887 ) ) ;
#53616 = ADVANCED_FACE ( 'NONE', ( #4322 ), #14513, .T. ) ;
#53617 = EDGE_CURVE ( 'NONE', #47264, #3800, #47406, .T. ) ;
#53618 = CARTESIAN_POINT ( 'NONE',  ( 5.000000000000000000, -32.29166666393548724, -2.886751345948129988 ) ) ;
#53620 = EDGE_LOOP ( 'NONE', ( #56028, #22728, #34087, #21116 ) ) ;
#53619 = CARTESIAN_POINT ( 'NONE',  ( 9.457646018065525792E-16, -65.06249999863440792, 5.148502694627439702 ) ) ;
#53621 = CARTESIAN_POINT ( 'NONE',  ( -51.60603307380591787, -150.1875000013656063, -2.891590998281053704 ) ) ;
#53622 = CARTESIAN_POINT ( 'NONE',  ( 4.458734124999999437, -14.81249999863440436, -5.460374474430324690E-16 ) ) ;
#53624 = ORIENTED_EDGE ( 'NONE', *, *, #6348, .F. ) ;
#53623 = CARTESIAN_POINT ( 'NONE',  ( 9.457646018065525792E-16, -16.31249999863440436, 5.148502694627439702 ) ) ;
#53625 = CARTESIAN_POINT ( 'NONE',  ( -2.500000000000000444, -83.16666666666667140, -4.330127018922193649 ) ) ;
#53626 = CARTESIAN_POINT ( 'NONE',  ( 6.123233995736766282E-16, -120.0000000000000000, -5.000000000000000000 ) ) ;
#53627 = CARTESIAN_POINT ( 'NONE',  ( -3.152548672688508926E-16, -57.81249999863440081, -5.148502694627439702 ) ) ;
#53628 = CARTESIAN_POINT ( 'NONE',  ( 1.060575238724906964E-15, -84.62499999726880162, 5.773502691896257311 ) ) ;
#53630 = ORIENTED_EDGE ( 'NONE', *, *, #48718, .F. ) ;
#53629 = CARTESIAN_POINT ( 'NONE',  ( -1.339745962155660663, -17.79465819873852439, 4.999999999999972466 ) ) ;
#53631 = CARTESIAN_POINT ( 'NONE',  ( -55.39835681537999790, -145.8750000000000284, 4.984105922594378235 ) ) ;
#53632 = CARTESIAN_POINT ( 'NONE',  ( -2.229367062499996610, -28.39583333196774007, 3.861377020970582219 ) ) ;
#53633 = ORIENTED_EDGE ( 'NONE', *, *, #43618, .T. ) ;
#53634 = CARTESIAN_POINT ( 'NONE',  ( -1.846868145590737420, -166.0000000013656063, 4.458734124999999437 ) ) ;
#53635 = CARTESIAN_POINT ( 'NONE',  ( 4.458734124999999437, -105.0624999986344079, -5.460374474430324690E-16 ) ) ;
#53636 = VERTEX_POINT ( 'NONE', #30323 ) ;
#53637 = CARTESIAN_POINT ( 'NONE',  ( -59.44456063193725015, -144.8125000013656063, -0.3552334253322034230 ) ) ;
#53638 = CARTESIAN_POINT ( 'NONE',  ( -56.66612745406270335, -140.4375000027312410, -5.149110718188516067 ) ) ;
#53639 = CARTESIAN_POINT ( 'NONE',  ( 9.457646018065525792E-16, -36.06249999863440792, 5.148502694627439702 ) ) ;
#53640 = CARTESIAN_POINT ( 'NONE',  ( -7.897827455343210623, -1.533134349199909208, -7.633632140068262295 ) ) ;
#53641 = CARTESIAN_POINT ( 'NONE',  ( -5.000000000000000000, -2.083333333333333037, -2.886751345948128211 ) ) ;
#53642 = CARTESIAN_POINT ( 'NONE',  ( 4.458734124999998549, -13.72916666530107399, -2.574251347313721627 ) ) ;
#53643 = CARTESIAN_POINT ( 'NONE',  ( -2.229367062499996610, -99.39583333196773651, 3.861377020970582219 ) ) ;
#53644 = ORIENTED_EDGE ( 'NONE', *, *, #25966, .F. ) ;
#53645 = CARTESIAN_POINT ( 'NONE',  ( -4.458734124999999437, -145.1875000013656063, -5.460374474430324690E-16 ) ) ;
#53646 = CARTESIAN_POINT ( 'NONE',  ( -2.229367062500000163, -28.72916666530107221, -3.861377020970580443 ) ) ;
#53647 = CARTESIAN_POINT ( 'NONE',  ( -49.85088928181150436, -139.6875000027311842, -1.666127454062680480 ) ) ;
#53648 = CARTESIAN_POINT ( 'NONE',  ( -57.89159099828107458, -132.6875000013656063, -3.393966926194107447 ) ) ;
#53649 = CARTESIAN_POINT ( 'NONE',  ( -4.458734124999998549, -68.47916666530106511, 2.574251347313722516 ) ) ;
#53650 = CARTESIAN_POINT ( 'NONE',  ( -6.972266317189433020E-16, -16.25000000000000000, -5.000000000000000000 ) ) ;
#53651 = CARTESIAN_POINT ( 'NONE',  ( -54.60164318462004474, -146.5000000027312126, -4.984105922594373794 ) ) ;
#53652 = CARTESIAN_POINT ( 'NONE',  ( -3.152801135295367096, -140.0625000013655779, -3.152801135295367541 ) ) ;
#53653 = CARTESIAN_POINT ( 'NONE',  ( -4.458734124999999437, 2.437500001365593860, 0.000000000000000000 ) ) ;
#53654 = ORIENTED_EDGE ( 'NONE', *, *, #35884, .T. ) ;
#53655 = CARTESIAN_POINT ( 'NONE',  ( -2.500000000000000444, -50.04166666393547303, -4.330127018922193649 ) ) ;
#53656 = LINE ( 'NONE', #38536, #34050 ) ;
#53658 = CARTESIAN_POINT ( 'NONE',  ( -3.152548672688508926E-16, -29.56249999863440436, -5.148502694627439702 ) ) ;
#53657 = CARTESIAN_POINT ( 'NONE',  ( 2.499999999999998668, -95.33333333333332860, -4.330127018922193649 ) ) ;
#53659 = CARTESIAN_POINT ( 'NONE',  ( -50.18089887299977647, -143.8125000027311842, 2.462841084822486426 ) ) ;
#53660 = CARTESIAN_POINT ( 'NONE',  ( -4.458734124999999437, -77.64583333196773651, -2.574251347313719407 ) ) ;
#53661 = CARTESIAN_POINT ( 'NONE',  ( 4.458734124999998549, 21.02083333469892779, -2.574251347313721627 ) ) ;
#53662 = CARTESIAN_POINT ( 'NONE',  ( 1.975475456537005874E-15, -101.6249999972688158, 5.000000000000000000 ) ) ;
#53664 = EDGE_CURVE ( 'NONE', #3550, #7844, #54786, .T. ) ;
#53663 = CARTESIAN_POINT ( 'NONE',  ( -50.40829686548195099, -142.0000000013656063, -1.485763867205728284 ) ) ;
#53665 = CARTESIAN_POINT ( 'NONE',  ( 4.458734124999999437, -3.812499998634408360, -5.460374474430324690E-16 ) ) ;
#53666 = CARTESIAN_POINT ( 'NONE',  ( 4.458734124999998549, 25.02083333469892423, -2.574251347313721627 ) ) ;
#53667 = CARTESIAN_POINT ( 'NONE',  ( -2.229367062499996610, -44.39583333196774362, 3.861377020970582219 ) ) ;
#53668 = CARTESIAN_POINT ( 'NONE',  ( -58.59997141384986463, -154.2812500020484379, 3.067102644406258793 ) ) ;
#53669 = CARTESIAN_POINT ( 'NONE',  ( 4.458734124999998549, 2.270833334698928230, -2.574251347313721627 ) ) ;
#53670 = EDGE_LOOP ( 'NONE', ( #32168, #40078, #43289, #5003 ) ) ;
#53671 = CARTESIAN_POINT ( 'NONE',  ( 4.458734124999998549, -24.97916666530106511, -2.574251347313721627 ) ) ;
#53672 = CARTESIAN_POINT ( 'NONE',  ( -4.458734124999999437, -69.31249999863439371, 0.000000000000000000 ) ) ;
#53673 = CARTESIAN_POINT ( 'NONE',  ( -5.000000000000000000, -107.8749999972687874, 0.000000000000000000 ) ) ;
#53674 =( BOUNDED_CURVE ( )  B_SPLINE_CURVE ( 2, ( #13135, #33693, #8934, #22800, #48483, #61722, #18273, #62978, #37899 ),
 .UNSPECIFIED., .F., .F. ) 
 B_SPLINE_CURVE_WITH_KNOTS ( ( 3, 2, 2, 2, 3 ),
 ( 0.1339285714285714246, 0.1345238095238095177, 0.1357142857142857040, 0.1369047619047619180, 0.1375000000000000111 ),
 .UNSPECIFIED. ) 
 CURVE ( )  GEOMETRIC_REPRESENTATION_ITEM ( )  RATIONAL_B_SPLINE_CURVE ( ( 0.9330127018922194093, 0.9330127018922194093, 1.000000000000000000, 0.8660254037844387076, 1.000000000000000000, 0.8660254037844387076, 1.000000000000000000, 0.9330127018922194093, 0.9330127018922194093 ) ) 
 REPRESENTATION_ITEM ( '' )  );
#53675 = CARTESIAN_POINT ( 'NONE',  ( 4.458734125000001214, 28.10416666803225993, 2.574251347313718519 ) ) ;
#53676 = CARTESIAN_POINT ( 'NONE',  ( 1.975475456537005874E-15, -11.62499999726881406, 5.000000000000000000 ) ) ;
#53677 = CARTESIAN_POINT ( 'NONE',  ( -59.98410592259440222, -153.2500000027312410, -0.3983568153799752487 ) ) ;
#53678 = CARTESIAN_POINT ( 'NONE',  ( 9.457646018065525792E-16, -74.31249999863440792, 5.148502694627439702 ) ) ;
#53679 = CARTESIAN_POINT ( 'NONE',  ( 5.000000000000000000, -53.41666666666667140, -2.886751345948129988 ) ) ;
#53680 = CARTESIAN_POINT ( 'NONE',  ( -4.999999999999998224, -65.91666666666667140, 2.886751345948131764 ) ) ;
#53681 = DIRECTION ( 'NONE',  ( -0.000000000000000000, 1.000000000000000000, -0.000000000000000000 ) ) ;
#53682 = ORIENTED_EDGE ( 'NONE', *, *, #44729, .F. ) ;
#53683 = DIRECTION ( 'NONE',  ( 0.000000000000000000, 0.000000000000000000, 1.000000000000000000 ) ) ;
#53684 = CARTESIAN_POINT ( 'NONE',  ( -5.000000000000000000, 12.91666666666666607, -2.886751345948128211 ) ) ;
#53685 = CARTESIAN_POINT ( 'NONE',  ( -4.999999999999999112, -18.91666666666666430, 2.886751345948131764 ) ) ;
#53686 = CARTESIAN_POINT ( 'NONE',  ( 4.458734124999999437, -24.81249999863440436, -5.460374474430324690E-16 ) ) ;
#53687 = CARTESIAN_POINT ( 'NONE',  ( -4.458734124999997661, -80.22916666530107932, 2.574251347313722516 ) ) ;
#53689 = CARTESIAN_POINT ( 'NONE',  ( 4.458734124999999437, -169.6875000013656063, 0.000000000000000000 ) ) ;
#53688 =( BOUNDED_CURVE ( )  B_SPLINE_CURVE ( 2, ( #34672, #40763, #54935, #25981, #50434, #25023, #29835, #10861, #30477 ),
 .UNSPECIFIED., .F., .F. ) 
 B_SPLINE_CURVE_WITH_KNOTS ( ( 3, 2, 2, 2, 3 ),
 ( 0.3770833333333333259, 0.3777777777777777679, 0.3791666666666666519, 0.3805555555555555358, 0.3812499999999999778 ),
 .UNSPECIFIED. ) 
 CURVE ( )  GEOMETRIC_REPRESENTATION_ITEM ( )  RATIONAL_B_SPLINE_CURVE ( ( 0.9330127018922194093, 0.9330127018922194093, 1.000000000000000000, 0.8660254037844387076, 1.000000000000000000, 0.8660254037844387076, 1.000000000000000000, 0.9330127018922194093, 0.9330127018922194093 ) ) 
 REPRESENTATION_ITEM ( '' )  );
#53690 = CARTESIAN_POINT ( 'NONE',  ( 5.000000000000000000, -16.37499999726881228, -6.123233995736766282E-16 ) ) ;
#53692 = EDGE_LOOP ( 'NONE', ( #39457, #63209, #18123, #41768 ) ) ;
#53691 = CARTESIAN_POINT ( 'NONE',  ( -3.152548672688508926E-16, -52.56249999863440792, -5.148502694627439702 ) ) ;
#53693 = CARTESIAN_POINT ( 'NONE',  ( 1.975475456537005874E-15, -70.62499999726880162, 5.000000000000000000 ) ) ;
#53694 = CARTESIAN_POINT ( 'NONE',  ( -51.75738570946856498, -155.0000000000000284, 3.805975901505577408 ) ) ;
#53696 = VERTEX_POINT ( 'NONE', #19723 ) ;
#53695 = CARTESIAN_POINT ( 'NONE',  ( -2.229367062500000163, 2.270833334698928230, -3.861377020970580443 ) ) ;
#53697 = DIRECTION ( 'NONE',  ( 0.000000000000000000, 1.000000000000000000, 0.000000000000000000 ) ) ;
#53698 = CARTESIAN_POINT ( 'NONE',  ( -4.999999999999999112, -58.91666666666665719, 2.886751345948131764 ) ) ;
#53699 = CARTESIAN_POINT ( 'NONE',  ( -4.458734125000000326, -156.2500000013656063, -1.846868145590735644 ) ) ;
#53700 = CARTESIAN_POINT ( 'NONE',  ( -2.229367062499996610, -42.39583333196773651, 3.861377020970582219 ) ) ;
#53701 = CARTESIAN_POINT ( 'NONE',  ( -5.000000000000000000, -65.08333333333332860, -2.886751345948128211 ) ) ;
#53702 = CARTESIAN_POINT ( 'NONE',  ( 3.061616997868383141E-16, -162.7500000000000000, -5.000000000000000000 ) ) ;
#53703 = CARTESIAN_POINT ( 'NONE',  ( -5.000000000000000000, 10.91666666666666607, -2.886751345948128211 ) ) ;
#53704 = CARTESIAN_POINT ( 'NONE',  ( -56.48576386720575471, -129.0000000013656063, -4.591703134518078322 ) ) ;
#53705 = CARTESIAN_POINT ( 'NONE',  ( -4.458734124999999437, -7.645833331967735624, -2.574251347313719407 ) ) ;
#53706 = CARTESIAN_POINT ( 'NONE',  ( -2.229367062499996610, -48.39583333196772941, 3.861377020970582219 ) ) ;
#53707 = CARTESIAN_POINT ( 'NONE',  ( -51.19402409849444524, -136.6250000027312410, -3.242614290531456334 ) ) ;
#53708 = CARTESIAN_POINT ( 'NONE',  ( 2.730187237215162345E-16, -147.1875000013656063, -4.458734124999999437 ) ) ;
#53709 = CARTESIAN_POINT ( 'NONE',  ( 4.458734125000001214, -90.14583333196773651, 2.574251347313718519 ) ) ;
#53710 = CARTESIAN_POINT ( 'NONE',  ( 1.339745962155612702, 8.705341801261477386, -5.000000000000000000 ) ) ;
#53711 = ORIENTED_EDGE ( 'NONE', *, *, #42579, .T. ) ;
#53712 = CARTESIAN_POINT ( 'NONE',  ( -5.000000000000000000, -47.00000000000000000, 0.000000000000000000 ) ) ;
#53713 = CARTESIAN_POINT ( 'NONE',  ( -1.049326080737009628E-13, -5.624999997268816720, 5.000000000000000000 ) ) ;
#53714 = CARTESIAN_POINT ( 'NONE',  ( -59.98410592259440222, -149.2500000027312126, -0.3983568153799752487 ) ) ;
#53715 = CARTESIAN_POINT ( 'NONE',  ( 1.339745962155612702, -82.16965819600734733, -5.000000000000000000 ) ) ;
#53716 = EDGE_CURVE ( 'NONE', #34465, #16762, #25186, .T. ) ;
#53717 = ORIENTED_EDGE ( 'NONE', *, *, #48287, .T. ) ;
#53718 = CARTESIAN_POINT ( 'NONE',  ( 1.339745962155612702, -78.29465819873851729, -5.000000000000000000 ) ) ;
#53719 = CARTESIAN_POINT ( 'NONE',  ( 4.458734124999998549, -13.97916666530107221, -2.574251347313721627 ) ) ;
#53720 = CARTESIAN_POINT ( 'NONE',  ( -1.339745962155610925, -50.79465819873851018, 5.000000000000000000 ) ) ;
#53721 = CARTESIAN_POINT ( 'NONE',  ( 4.458734124999998549, -1.729166665301068440, -2.574251347313721627 ) ) ;
#53722 = CARTESIAN_POINT ( 'NONE',  ( 2.499999999999998668, -73.20833333060214443, -4.330127018922193649 ) ) ;
#53723 = CARTESIAN_POINT ( 'NONE',  ( 3.152801135295366208, -153.5625000013656063, 3.152801135295367985 ) ) ;
#53724 = CARTESIAN_POINT ( 'NONE',  ( -2.229367062500000163, 22.27083333469892423, -3.861377020970580443 ) ) ;
#53725 = ORIENTED_EDGE ( 'NONE', *, *, #25215, .T. ) ;
#53726 = CARTESIAN_POINT ( 'NONE',  ( -4.458734124999999437, -95.39583333196773651, -2.574251347313719407 ) ) ;
#53727 = CARTESIAN_POINT ( 'NONE',  ( 1.975475456537005874E-15, -33.62499999726880873, 5.000000000000000000 ) ) ;
#53728 = CARTESIAN_POINT ( 'NONE',  ( 2.500000000000002220, -40.66666666666667140, 4.330127018922192761 ) ) ;
#53729 = CARTESIAN_POINT ( 'NONE',  ( 2.229367062499998831, -16.64583333196773651, -3.861377020970580887 ) ) ;
#53730 = CARTESIAN_POINT ( 'NONE',  ( -2.499999999999996447, -84.70833333060214443, 4.330127018922195425 ) ) ;
#53731 = CARTESIAN_POINT ( 'NONE',  ( -2.499999999999996447, -42.70833333060214443, 4.330127018922195425 ) ) ;
#53732 = CYLINDRICAL_SURFACE ( 'NONE', #46242, 5.000000000000000000 ) ;
#53733 = CARTESIAN_POINT ( 'NONE',  ( 4.458734125000000326, 13.10416666803226171, 2.574251347313718519 ) ) ;
#53734 = CARTESIAN_POINT ( 'NONE',  ( 1.975475456537005874E-15, -46.62499999726880873, 5.000000000000000000 ) ) ;
#53735 = ORIENTED_EDGE ( 'NONE', *, *, #443, .F. ) ;
#53736 = CARTESIAN_POINT ( 'NONE',  ( -2.229367062500000163, 17.52083333469892779, -3.861377020970580443 ) ) ;
#53737 = CARTESIAN_POINT ( 'NONE',  ( -3.152548672688508926E-16, -60.56249999863440792, -5.148502694627439702 ) ) ;
#53738 = CARTESIAN_POINT ( 'NONE',  ( 9.457646018065525792E-16, -7.312499998634403475, 5.148502694627439702 ) ) ;
#53739 =( BOUNDED_CURVE ( )  B_SPLINE_CURVE ( 2, ( #35738, #30905, #60508, #11597, #6789, #45703, #55683, #46018, #11913 ),
 .UNSPECIFIED., .F., .F. ) 
 B_SPLINE_CURVE_WITH_KNOTS ( ( 3, 2, 2, 2, 3 ),
 ( 0.3089285714285714413, 0.3095238095238095344, 0.3107142857142857206, 0.3119047619047619069, 0.3125000000000000000 ),
 .UNSPECIFIED. ) 
 CURVE ( )  GEOMETRIC_REPRESENTATION_ITEM ( )  RATIONAL_B_SPLINE_CURVE ( ( 0.9330127018922194093, 0.9330127018922194093, 1.000000000000000000, 0.8660254037844387076, 1.000000000000000000, 0.8660254037844387076, 1.000000000000000000, 0.9330127018922194093, 0.9330127018922194093 ) ) 
 REPRESENTATION_ITEM ( '' )  );
#53740 =( NAMED_UNIT ( * ) SI_UNIT ( $, .STERADIAN. ) SOLID_ANGLE_UNIT ( ) );
#53741 = CARTESIAN_POINT ( 'NONE',  ( -4.999999999999999112, 12.08333333333333037, 2.886751345948131764 ) ) ;
#53742 = CARTESIAN_POINT ( 'NONE',  ( 1.846868145590735200, -166.2500000013656347, -4.458734125000000326 ) ) ;
#53743 = DIRECTION ( 'NONE',  ( -0.000000000000000000, 1.000000000000000000, -0.000000000000000000 ) ) ;
#53744 = CARTESIAN_POINT ( 'NONE',  ( 2.229367062499998831, -55.64583333196773651, -3.861377020970580887 ) ) ;
#53745 = CARTESIAN_POINT ( 'NONE',  ( 2.500000000000002220, -91.54166666393547303, 4.330127018922192761 ) ) ;
#53746 = CARTESIAN_POINT ( 'NONE',  ( 0.000000000000000000, -120.0000000000000000, 0.000000000000000000 ) ) ;
#53747 = CARTESIAN_POINT ( 'NONE',  ( -5.926426369611017623E-15, 25.37500000273118062, 5.000000000000000000 ) ) ;
#53748 = LINE ( 'NONE', #54065, #38774 ) ;
#53749 = CARTESIAN_POINT ( 'NONE',  ( -8.190561711645485556E-16, -151.9375000013655779, 4.458734124999999437 ) ) ;
#53750 = CARTESIAN_POINT ( 'NONE',  ( 5.000000000000000000, -35.50000000000000711, -6.123233995736766282E-16 ) ) ;
#53751 = CARTESIAN_POINT ( 'NONE',  ( -58.80597590150559739, -140.0000000000000284, 3.242614290531460330 ) ) ;
#53752 = CARTESIAN_POINT ( 'NONE',  ( 1.975475456537005874E-15, -70.75000000000000000, 5.000000000000000000 ) ) ;
#53753 = ORIENTED_EDGE ( 'NONE', *, *, #37346, .F. ) ;
#53754 = CARTESIAN_POINT ( 'NONE',  ( 9.457646018065525792E-16, -102.0624999986344079, 5.148502694627439702 ) ) ;
#53755 = CARTESIAN_POINT ( 'NONE',  ( -4.458734124999999437, 3.354166668032260823, -2.574251347313719407 ) ) ;
#53756 = CARTESIAN_POINT ( 'NONE',  ( 5.000000000000000888, 4.416666666666666075, 2.886751345948126879 ) ) ;
#53757 = CARTESIAN_POINT ( 'NONE',  ( -2.229367062499996610, -65.14583333196773651, 3.861377020970582219 ) ) ;
#53758 = AXIS2_PLACEMENT_3D ( 'NONE', #40198, #9965, #15756 ) ;
#53759 = CARTESIAN_POINT ( 'NONE',  ( -6.031010364368858512E-14, 3.249999999999997335, 5.000000000000000000 ) ) ;
#53760 = CARTESIAN_POINT ( 'NONE',  ( 2.500000000000002220, -3.541666663935478354, 4.330127018922192761 ) ) ;
#53762 = VERTEX_POINT ( 'NONE', #49314 ) ;
#53761 = CARTESIAN_POINT ( 'NONE',  ( 2.229367062500001939, -33.97916666530107221, 3.861377020970579999 ) ) ;
#53763 = CARTESIAN_POINT ( 'NONE',  ( 0.000000000000000000, -120.0000000000000000, 0.000000000000000000 ) ) ;
#53764 = CARTESIAN_POINT ( 'NONE',  ( 1.975475456537005874E-15, -59.62499999726880873, 5.000000000000000000 ) ) ;
#53765 = AXIS2_PLACEMENT_3D ( 'NONE', #31051, #50674, #60342 ) ;
#53766 = CARTESIAN_POINT ( 'NONE',  ( 5.000000000000000000, 5.500000000000001776, -6.123233995736766282E-16 ) ) ;
#53767 = CARTESIAN_POINT ( 'NONE',  ( 5.000000000000000000, -47.50000000000000000, -6.123233995736766282E-16 ) ) ;
#53768 =( BOUNDED_CURVE ( )  B_SPLINE_CURVE ( 2, ( #21034, #59640, #16835, #45149, #16521, #36144, #15574, #25213, #60281 ),
 .UNSPECIFIED., .F., .F. ) 
 B_SPLINE_CURVE_WITH_KNOTS ( ( 3, 2, 2, 2, 3 ),
 ( 0.7729166666666666963, 0.7736111111111111382, 0.7750000000000000222, 0.7763888888888889062, 0.7770833333333333481 ),
 .UNSPECIFIED. ) 
 CURVE ( )  GEOMETRIC_REPRESENTATION_ITEM ( )  RATIONAL_B_SPLINE_CURVE ( ( 0.9330127018922194093, 0.9330127018922194093, 1.000000000000000000, 0.8660254037844387076, 1.000000000000000000, 0.8660254037844387076, 1.000000000000000000, 0.9330127018922194093, 0.9330127018922194093 ) ) 
 REPRESENTATION_ITEM ( '' )  );
#53770 = CARTESIAN_POINT ( 'NONE',  ( -2.229367062499996610, -26.39583333196774007, 3.861377020970582219 ) ) ;
#53769 = FACE_OUTER_BOUND ( 'NONE', #3044, .T. ) ;
#53771 = CARTESIAN_POINT ( 'NONE',  ( -5.000000000000000000, 22.04166666939785202, -2.886751345948128211 ) ) ;
#53772 = CARTESIAN_POINT ( 'NONE',  ( -4.458734124999999437, -69.31249999863439371, 0.000000000000000000 ) ) ;
#53773 = CARTESIAN_POINT ( 'NONE',  ( 2.730187237215162345E-16, -145.4375000013656063, -4.458734124999999437 ) ) ;
#53774 = CARTESIAN_POINT ( 'NONE',  ( -2.229367062499996610, -74.14583333196773651, 3.861377020970582219 ) ) ;
#53775 = CARTESIAN_POINT ( 'NONE',  ( -59.29741812935640155, -137.8750000013655779, -2.196230717870135685 ) ) ;
#53776 = CARTESIAN_POINT ( 'NONE',  ( -4.458734124999998549, -29.47916666530106866, 2.574251347313722516 ) ) ;
#53777 = CARTESIAN_POINT ( 'NONE',  ( -5.000000000000000000, -70.87499999726880162, 0.000000000000000000 ) ) ;
#53778 = ORIENTED_EDGE ( 'NONE', *, *, #1642, .F. ) ;
#53779 = LINE ( 'NONE', #39614, #60813 ) ;
#53780 = VERTEX_POINT ( 'NONE', #49945 ) ;
#53781 = CARTESIAN_POINT ( 'NONE',  ( -4.458734124999998549, -75.47916666530107932, 2.574251347313722516 ) ) ;
#53782 = CARTESIAN_POINT ( 'NONE',  ( -54.60164318462004474, -150.3750000000000284, -4.984105922594373794 ) ) ;
#53783 =( LENGTH_UNIT ( ) NAMED_UNIT ( * ) SI_UNIT ( .MILLI., .METRE. ) );
#53784 = ORIENTED_EDGE ( 'NONE', *, *, #40874, .F. ) ;
#53785 = CARTESIAN_POINT ( 'NONE',  ( 1.243387493232115550E-13, -20.12499999726881228, -5.000000000000000000 ) ) ;
#53786 = CARTESIAN_POINT ( 'NONE',  ( -6.972266317189433020E-16, -3.250000000000001332, -5.000000000000000000 ) ) ;
#53788 = EDGE_CURVE ( 'NONE', #16917, #47768, #58965, .T. ) ;
#53787 = CARTESIAN_POINT ( 'NONE',  ( -2.229367062500000163, -61.72916666530106511, -3.861377020970580443 ) ) ;
#53789 = CARTESIAN_POINT ( 'NONE',  ( 2.229367062499998831, 2.104166668032262599, -3.861377020970580887 ) ) ;
#53790 = ORIENTED_EDGE ( 'NONE', *, *, #31528, .T. ) ;
#53791 = CARTESIAN_POINT ( 'NONE',  ( 0.000000000000000000, -170.0000000000000000, 5.000000000000000000 ) ) ;
#53792 = CARTESIAN_POINT ( 'NONE',  ( -5.000000000000000000, -59.95833333060214443, -2.886751345948128211 ) ) ;
#53793 = CARTESIAN_POINT ( 'NONE',  ( -4.458734124999999437, 15.68750000136559564, 0.000000000000000000 ) ) ;
#53794 = CARTESIAN_POINT ( 'NONE',  ( -50.55543936806279248, -144.0625000013656063, 0.3552334253322060320 ) ) ;
#53795 = CARTESIAN_POINT ( 'NONE',  ( 0.000000000000000000, -120.0000000000000000, 0.000000000000000000 ) ) ;
#53796 = CARTESIAN_POINT ( 'NONE',  ( -3.152801135295367985, -163.8125000013656063, 3.152801135295367096 ) ) ;
#53797 = ORIENTED_EDGE ( 'NONE', *, *, #13362, .T. ) ;
#53798 = CARTESIAN_POINT ( 'NONE',  ( 4.458734124999999437, -76.81249999863440792, -5.460374474430324690E-16 ) ) ;
#53799 = CARTESIAN_POINT ( 'NONE',  ( -2.499999999999996447, -51.70833333060213732, 4.330127018922195425 ) ) ;
#53800 = CARTESIAN_POINT ( 'NONE',  ( 4.458734125000001214, 3.104166668032260379, 2.574251347313718519 ) ) ;
#53801 = VECTOR ( 'NONE', #16850, 1000.000000000000000 ) ;
#53802 = CARTESIAN_POINT ( 'NONE',  ( 2.493747252781420335E-13, -43.12499999726882294, -5.000000000000000000 ) ) ;
#53803 = CARTESIAN_POINT ( 'NONE',  ( 4.458734124999998549, -66.97916666530107932, -2.574251347313721627 ) ) ;
#53804 = CARTESIAN_POINT ( 'NONE',  ( 5.000000000000000888, -23.45833333060214443, 2.886751345948126879 ) ) ;
#53805 = EDGE_CURVE ( 'NONE', #52846, #36859, #10716, .T. ) ;
#53806 = CARTESIAN_POINT ( 'NONE',  ( 0.000000000000000000, -170.0000000000000000, 5.000000000000000000 ) ) ;
#53807 = CARTESIAN_POINT ( 'NONE',  ( 1.339745962155612702, -44.16965819600732601, -5.000000000000000000 ) ) ;
#53808 = CARTESIAN_POINT ( 'NONE',  ( -6.972266317189433020E-16, -32.24999999999999289, -5.000000000000000000 ) ) ;
#53809 = CARTESIAN_POINT ( 'NONE',  ( 1.975475456537005874E-15, -20.74999999999999645, 5.000000000000000000 ) ) ;
#53810 = CARTESIAN_POINT ( 'NONE',  ( -2.229367062500000163, -44.47916666530106511, -3.861377020970580443 ) ) ;
#53811 = PRODUCT_DEFINITION_SHAPE ( 'NONE', 'NONE',  #63684 ) ;
#53812 = CARTESIAN_POINT ( 'NONE',  ( -4.458734124999999437, -25.64583333196773651, -2.574251347313719407 ) ) ;
#53813 = CARTESIAN_POINT ( 'NONE',  ( -2.229367062499996610, 4.604166668032261711, 3.861377020970582219 ) ) ;
#53814 = CARTESIAN_POINT ( 'NONE',  ( 5.000000000000000000, -151.0000000000000284, 0.000000000000000000 ) ) ;
#53815 = CARTESIAN_POINT ( 'NONE',  ( -2.499999999999996447, 25.16666666666666430, 4.330127018922195425 ) ) ;
#53816 = CARTESIAN_POINT ( 'NONE',  ( 3.061616997868383141E-16, -147.8750000027312126, -5.000000000000000000 ) ) ;
#53817 = CARTESIAN_POINT ( 'NONE',  ( 0.000000000000000000, -170.0000000000000000, 5.000000000000000000 ) ) ;
#53818 = CARTESIAN_POINT ( 'NONE',  ( 4.458734125000001214, -39.89583333196772941, 2.574251347313718519 ) ) ;
#53819 = CARTESIAN_POINT ( 'NONE',  ( -2.499999999999996447, -74.70833333060214443, 4.330127018922195425 ) ) ;
#53820 = EDGE_CURVE ( 'NONE', #40578, #62567, #56443, .T. ) ;
#53821 = CARTESIAN_POINT ( 'NONE',  ( -56.48576386720575471, -143.0000000013655779, -4.591703134518078322 ) ) ;
#53822 = CARTESIAN_POINT ( 'NONE',  ( 2.071067811865475505, -141.8125000000000284, -5.000000000000000888 ) ) ;
#53823 = CARTESIAN_POINT ( 'NONE',  ( -4.458734124999999437, -73.64583333196773651, -2.574251347313719407 ) ) ;
#53824 = CARTESIAN_POINT ( 'NONE',  ( 3.152801135295367541, -165.5625000013656063, -3.152801135295367541 ) ) ;
#53825 = CARTESIAN_POINT ( 'NONE',  ( -4.458734124999999437, -32.39583333196773651, -2.574251347313719407 ) ) ;
#53826 = CARTESIAN_POINT ( 'NONE',  ( -59.81910112700027327, -136.3125000027311273, -2.462841084822392279 ) ) ;
#53827 = CARTESIAN_POINT ( 'NONE',  ( -58.24261429053147765, -155.0000000000000284, -3.805975901505573411 ) ) ;
#53828 = CARTESIAN_POINT ( 'NONE',  ( 5.000000000000000000, -23.41666666666667140, -2.886751345948129988 ) ) ;
#53829 = CARTESIAN_POINT ( 'NONE',  ( -8.190561711645485556E-16, -143.6875000013656063, 4.458734124999999437 ) ) ;
#53830 = VERTEX_POINT ( 'NONE', #9436 ) ;
#53831 = CARTESIAN_POINT ( 'NONE',  ( 9.457646018065525792E-16, 27.68750000136559208, 5.148502694627439702 ) ) ;
#53832 = ORIENTED_EDGE ( 'NONE', *, *, #4022, .F. ) ;
#53833 = CARTESIAN_POINT ( 'NONE',  ( 9.457646018065525792E-16, -56.31249999863440081, 5.148502694627439702 ) ) ;
#53834 = CARTESIAN_POINT ( 'NONE',  ( 2.500000000000002220, 27.45833333606451632, 4.330127018922192761 ) ) ;
#53835 = CARTESIAN_POINT ( 'NONE',  ( 1.975475456537005874E-15, -29.74999999999999645, 5.000000000000000000 ) ) ;
#53836 = CARTESIAN_POINT ( 'NONE',  ( 5.000000000000000000, 16.50000000000000000, -6.123233995736766282E-16 ) ) ;
#53837 = CARTESIAN_POINT ( 'NONE',  ( -1.339745962155585168, 7.919658201469705006, -5.000000000000015987 ) ) ;
#53838 = CARTESIAN_POINT ( 'NONE',  ( -4.458734124999999437, -6.312499998634403475, 0.000000000000000000 ) ) ;
#53839 = CARTESIAN_POINT ( 'NONE',  ( -3.535533905932738641, -168.3750000000000284, 3.535533905932737309 ) ) ;
#53840 = EDGE_CURVE ( 'NONE', #59502, #38280, #28058, .T. ) ;
#53841 = CARTESIAN_POINT ( 'NONE',  ( -4.999999999999998224, -8.916666666666662522, 2.886751345948131764 ) ) ;
#53842 = CARTESIAN_POINT ( 'NONE',  ( 1.339745962155729053, -91.16965819600733312, -4.999999999999933387 ) ) ;
#53843 = CARTESIAN_POINT ( 'NONE',  ( 1.339745962155612702, -53.16965819600733312, -5.000000000000000000 ) ) ;
#53845 = CARTESIAN_POINT ( 'NONE',  ( 4.458734124999999437, -21.81249999863440436, -5.460374474430324690E-16 ) ) ;
#53844 = CARTESIAN_POINT ( 'NONE',  ( 3.061616997868383141E-16, -142.8750000027312126, -5.000000000000000000 ) ) ;
#53846 = CARTESIAN_POINT ( 'NONE',  ( 1.975475456537005874E-15, -71.62499999726878741, 5.000000000000000000 ) ) ;
#53847 = CARTESIAN_POINT ( 'NONE',  ( -4.458734124999999437, -56.39583333196773651, -2.574251347313719407 ) ) ;
#53848 = CARTESIAN_POINT ( 'NONE',  ( -8.190561711645485556E-16, -157.9375000013655779, 4.458734124999999437 ) ) ;
#53849 = AXIS2_PLACEMENT_3D ( 'NONE', #46988, #12566, #7752 ) ;
#53850 = CARTESIAN_POINT ( 'NONE',  ( 5.000000000000000000, -50.37499999726881583, -6.123233995736766282E-16 ) ) ;
#53851 = ORIENTED_EDGE ( 'NONE', *, *, #58253, .F. ) ;
#53852 = CARTESIAN_POINT ( 'NONE',  ( 4.458734124999999437, 2.937500001365594304, -5.460374474430324690E-16 ) ) ;
#53853 = VERTEX_POINT ( 'NONE', #25506 ) ;
#53854 = CARTESIAN_POINT ( 'NONE',  ( 5.000000000000000888, -56.58333333333333570, 2.886751345948126879 ) ) ;
#53855 = CARTESIAN_POINT ( 'NONE',  ( 4.458734124999999437, -157.4375000013655779, 0.000000000000000000 ) ) ;
#53856 = ORIENTED_EDGE ( 'NONE', *, *, #22740, .F. ) ;
#53857 = CARTESIAN_POINT ( 'NONE',  ( 1.975475456537005874E-15, 11.24999999999999822, 5.000000000000000000 ) ) ;
#53858 = CARTESIAN_POINT ( 'NONE',  ( -51.75738570946856498, -134.7500000000000284, 3.805975901505576964 ) ) ;
#53859 = CARTESIAN_POINT ( 'NONE',  ( -6.972266317189433020E-16, -47.12499999726880873, -5.000000000000000000 ) ) ;
#53861 = EDGE_CURVE ( 'NONE', #50378, #11950, #12838, .T. ) ;
#53860 = CARTESIAN_POINT ( 'NONE',  ( -4.458734124999999437, -40.64583333196773651, -2.574251347313719407 ) ) ;
#53862 = ORIENTED_EDGE ( 'NONE', *, *, #23718, .F. ) ;
#53863 =( BOUNDED_CURVE ( )  B_SPLINE_CURVE ( 2, ( #51753, #35692, #36957, #12192, #26347, #60142, #11863, #31479, #30858 ),
 .UNSPECIFIED., .F., .F. ) 
 B_SPLINE_CURVE_WITH_KNOTS ( ( 3, 2, 2, 2, 3 ),
 ( 0.05178571428571428908, 0.05238095238095238221, 0.05357142857142856845, 0.05476190476190476164, 0.05535714285714286170 ),
 .UNSPECIFIED. ) 
 CURVE ( )  GEOMETRIC_REPRESENTATION_ITEM ( )  RATIONAL_B_SPLINE_CURVE ( ( 0.9330127018922194093, 0.9330127018922197424, 1.000000000000000000, 0.8660254037844387076, 1.000000000000000000, 0.8660254037844387076, 1.000000000000000000, 0.9330127018922189652, 0.9330127018922194093 ) ) 
 REPRESENTATION_ITEM ( '' )  );
#53864 = EDGE_CURVE ( 'NONE', #12680, #43260, #45125, .T. ) ;
#53865 = EDGE_CURVE ( 'NONE', #13785, #26724, #34845, .T. ) ;
#53866 = CARTESIAN_POINT ( 'NONE',  ( -2.500000000000000444, -46.16666666666666430, -4.330127018922193649 ) ) ;
#53867 = CARTESIAN_POINT ( 'NONE',  ( -2.229367062499996610, 18.85416666803225993, 3.861377020970582219 ) ) ;
#53868 = CARTESIAN_POINT ( 'NONE',  ( -50.18089887299978358, -149.6875000000000284, 2.462841084822545934 ) ) ;
#53869 = ORIENTED_EDGE ( 'NONE', *, *, #23584, .F. ) ;
#53870 = CARTESIAN_POINT ( 'NONE',  ( -2.229367062500000163, 26.52083333469892779, -3.861377020970580443 ) ) ;
#53871 = CARTESIAN_POINT ( 'NONE',  ( -59.81910112700025905, -128.3125000027312410, -2.462841084822630311 ) ) ;
#53872 = CARTESIAN_POINT ( 'NONE',  ( 0.000000000000000000, -170.0000000000000000, 0.000000000000000000 ) ) ;
#53873 = CARTESIAN_POINT ( 'NONE',  ( -55.00774582457342632, -134.9999999999999716, 4.994863783263385315 ) ) ;
#53874 = CARTESIAN_POINT ( 'NONE',  ( -6.972266317189433020E-16, -103.2500000000000000, -5.000000000000000000 ) ) ;
#53875 = CARTESIAN_POINT ( 'NONE',  ( -3.152548672688508926E-16, -61.56249999863440081, -5.148502694627439702 ) ) ;
#53876 = CARTESIAN_POINT ( 'NONE',  ( -55.39835681537999790, -145.8750000000000284, 4.984105922594378235 ) ) ;
#53877 = CARTESIAN_POINT ( 'NONE',  ( 4.458734124999999437, 19.18750000136559564, -5.460374474430324690E-16 ) ) ;
#53878 = ADVANCED_FACE ( 'NONE', ( #44801 ), #20372, .T. ) ;
#53879 = CARTESIAN_POINT ( 'NONE',  ( 75.00000000000001421, 15.00000000000000000, -9.000000000000001776 ) ) ;
#53880 = CARTESIAN_POINT ( 'NONE',  ( -4.458734124999999437, -51.56249999863440792, 0.000000000000000000 ) ) ;
#53881 = CARTESIAN_POINT ( 'NONE',  ( -2.500000000000000444, -10.04166666393547658, -4.330127018922193649 ) ) ;
#53882 = CARTESIAN_POINT ( 'NONE',  ( -5.000000000000000000, -93.08333333333332860, -2.886751345948128211 ) ) ;
#53883 = ADVANCED_FACE ( 'NONE', ( #6218 ), #7176, .T. ) ;
#53884 = CARTESIAN_POINT ( 'NONE',  ( -5.000000000000000000, -19.87499999726880873, 0.000000000000000000 ) ) ;
#53885 = CARTESIAN_POINT ( 'NONE',  ( 4.458734124999998549, -87.97916666530107932, -2.574251347313721627 ) ) ;
#53886 = CARTESIAN_POINT ( 'NONE',  ( 4.458734124999999437, -108.8124999986343937, -5.460374474430324690E-16 ) ) ;
#53887 = CARTESIAN_POINT ( 'NONE',  ( -2.229367062499996610, -10.39583333196773829, 3.861377020970582219 ) ) ;
#53888 = ORIENTED_EDGE ( 'NONE', *, *, #3233, .F. ) ;
#53889 = CARTESIAN_POINT ( 'NONE',  ( -2.500000000000000444, -81.16666666666667140, -4.330127018922193649 ) ) ;
#53890 = CARTESIAN_POINT ( 'NONE',  ( 2.229367062499998831, -98.64583333196773651, -3.861377020970580887 ) ) ;
#53891 = CARTESIAN_POINT ( 'NONE',  ( 2.071067811865475505, -159.9375000027312126, -5.000000000000000888 ) ) ;
#53892 = CARTESIAN_POINT ( 'NONE',  ( 4.458734124999999437, -96.06249999863440792, -5.460374474430324690E-16 ) ) ;
#53893 = CARTESIAN_POINT ( 'NONE',  ( -2.499999999999996447, -57.70833333060214443, 4.330127018922195425 ) ) ;
#53894 = CARTESIAN_POINT ( 'NONE',  ( 5.000000000000000888, -5.583333333333336590, 2.886751345948126879 ) ) ;
#53895 = AXIS2_PLACEMENT_3D ( 'NONE', #42470, #18030, #9948 ) ;
#53896 = CARTESIAN_POINT ( 'NONE',  ( -59.59170313451811296, -124.5000000013656063, 1.485763867205729394 ) ) ;
#53897 = CARTESIAN_POINT ( 'NONE',  ( -59.29741812935640155, -146.6250000013656063, -2.196230717870135685 ) ) ;
#53898 = CARTESIAN_POINT ( 'NONE',  ( -4.458734124999999437, -18.31249999863440792, 0.000000000000000000 ) ) ;
#53899 = CARTESIAN_POINT ( 'NONE',  ( 4.458734125000001214, 6.854166668032259935, 2.574251347313718519 ) ) ;
#53900 = CARTESIAN_POINT ( 'NONE',  ( -2.229367062499996610, -56.39583333196773651, 3.861377020970582219 ) ) ;
#53901 = CARTESIAN_POINT ( 'NONE',  ( 2.229367062500001939, -11.97916666530107044, 3.861377020970579999 ) ) ;
#53902 = LINE ( 'NONE', #29439, #50405 ) ;
#53903 = CARTESIAN_POINT ( 'NONE',  ( 5.000000000000000000, -157.0000000000000000, 0.000000000000000000 ) ) ;
#53904 = CARTESIAN_POINT ( 'NONE',  ( 2.499999999999998668, -8.333333333333332149, -4.330127018922193649 ) ) ;
#53905 = ORIENTED_EDGE ( 'NONE', *, *, #31517, .T. ) ;
#53906 = CARTESIAN_POINT ( 'NONE',  ( 4.458734124999999437, -42.06249999863440081, -5.460374474430324690E-16 ) ) ;
#53907 = CARTESIAN_POINT ( 'NONE',  ( -52.80376928212989185, -125.1250000013656205, -4.297418129356379346 ) ) ;
#53908 = CARTESIAN_POINT ( 'NONE',  ( -4.999999999999998224, -91.79166666393547303, 2.886751345948131764 ) ) ;
#53909 = CARTESIAN_POINT ( 'NONE',  ( -58.24261429053147765, -155.0000000000000284, -3.805975901505573411 ) ) ;
#53910 = CARTESIAN_POINT ( 'NONE',  ( 2.229367062499998831, -85.64583333196773651, -3.861377020970580887 ) ) ;
#53911 = CARTESIAN_POINT ( 'NONE',  ( -4.458734124999998549, 16.52083333469892779, 2.574251347313722516 ) ) ;
#53912 = CARTESIAN_POINT ( 'NONE',  ( 9.457646018065525792E-16, 7.937500001365594748, 5.148502694627439702 ) ) ;
#53913 = CARTESIAN_POINT ( 'NONE',  ( 1.339745962155612702, -0.2946581987385212820, -5.000000000000000000 ) ) ;
#53914 = CARTESIAN_POINT ( 'NONE',  ( -2.500000000000000444, -7.166666666666668739, -4.330127018922193649 ) ) ;
#53915 = CARTESIAN_POINT ( 'NONE',  ( 9.457646018065525792E-16, -87.31249999863440792, 5.148502694627439702 ) ) ;
#53916 = CARTESIAN_POINT ( 'NONE',  ( 2.229367062500001939, 22.77083333469892423, 3.861377020970579999 ) ) ;
#53917 = CARTESIAN_POINT ( 'NONE',  ( -5.000000000000000000, -76.08333333333332860, -2.886751345948128211 ) ) ;
#53918 =( BOUNDED_CURVE ( )  B_SPLINE_CURVE ( 2, ( #30128, #49757, #44938, #896, #20503, #40101, #59745, #15670, #22727 ),
 .UNSPECIFIED., .F., .F. ) 
 B_SPLINE_CURVE_WITH_KNOTS ( ( 3, 2, 2, 2, 3 ),
 ( 0.4583333333333337589, 0.4625000000000004663, 0.4666666666666671182, 0.4708333333333337700, 0.4750000000000004219 ),
 .UNSPECIFIED. ) 
 CURVE ( )  GEOMETRIC_REPRESENTATION_ITEM ( )  RATIONAL_B_SPLINE_CURVE ( ( 0.9999999999999918954, 0.9238795325112948431, 1.000000000000000000, 0.9238795325112867385, 1.000000000000000000, 0.9238795325112867385, 1.000000000000000000, 0.9238795325112786339, 1.000000000000008216 ) ) 
 REPRESENTATION_ITEM ( '' )  );
#53919 = CARTESIAN_POINT ( 'NONE',  ( -5.000000000000000000, 13.04166666939785379, -2.886751345948128211 ) ) ;
#53920 = ORIENTED_EDGE ( 'NONE', *, *, #51594, .T. ) ;
#53921 = CARTESIAN_POINT ( 'NONE',  ( 0.000000000000000000, -120.0000000000000000, 0.000000000000000000 ) ) ;
#53922 = ORIENTED_EDGE ( 'NONE', *, *, #51239, .F. ) ;
#53924 = CARTESIAN_POINT ( 'NONE',  ( 1.060575238724906964E-15, -32.75000000000000711, 5.773502691896257311 ) ) ;
#53923 = DIRECTION ( 'NONE',  ( 0.000000000000000000, 0.000000000000000000, 1.000000000000000000 ) ) ;
#53925 = CARTESIAN_POINT ( 'NONE',  ( 4.458734125000001214, -39.89583333196772941, 2.574251347313718519 ) ) ;
#53926 = CARTESIAN_POINT ( 'NONE',  ( 1.060575238724906964E-15, -32.62499999726880873, 5.773502691896257311 ) ) ;
#53928 = ORIENTED_EDGE ( 'NONE', *, *, #59061, .T. ) ;
#53927 = CARTESIAN_POINT ( 'NONE',  ( 4.458734125000001214, -66.89583333196773651, 2.574251347313718519 ) ) ;
#53929 = CARTESIAN_POINT ( 'NONE',  ( -52.80376928212989185, -152.1250000013656063, -4.297418129356379346 ) ) ;
#53930 = CARTESIAN_POINT ( 'NONE',  ( -2.229367062499996610, -15.14583333196773474, 3.861377020970582219 ) ) ;
#53932 = VERTEX_POINT ( 'NONE', #30968 ) ;
#53931 = CARTESIAN_POINT ( 'NONE',  ( -2.229367062499996610, -12.39583333196774007, 3.861377020970582219 ) ) ;
#53933 = CARTESIAN_POINT ( 'NONE',  ( -2.499999999999996447, -82.83333333333332860, 4.330127018922195425 ) ) ;
#53934 = CARTESIAN_POINT ( 'NONE',  ( 5.000000000000000000, 28.70833333606451987, -2.886751345948130876 ) ) ;
#53935 = CARTESIAN_POINT ( 'NONE',  ( -4.458734124999999437, -59.64583333196773651, -2.574251347313719407 ) ) ;
#53936 = CARTESIAN_POINT ( 'NONE',  ( 5.000000000000000000, -82.29166666393548724, -2.886751345948129988 ) ) ;
#53938 = EDGE_LOOP ( 'NONE', ( #13767, #12412, #24910, #50345 ) ) ;
#53937 = CARTESIAN_POINT ( 'NONE',  ( -1.339745962155613812, -32.20534180126148271, -5.000000000000000000 ) ) ;
#53939 = CARTESIAN_POINT ( 'NONE',  ( -56.66612745406270335, -146.3125000000000000, -5.149110718188516067 ) ) ;
#53940 = CARTESIAN_POINT ( 'NONE',  ( 9.457646018065525792E-16, -29.31249999863440436, 5.148502694627439702 ) ) ;
#53941 = VERTEX_POINT ( 'NONE', #36118 ) ;
#53942 = AXIS2_PLACEMENT_3D ( 'NONE', #35209, #16229, #11074 ) ;
#53943 = EDGE_CURVE ( 'NONE', #27774, #6544, #34230, .T. ) ;
#53944 = ITEM_DEFINED_TRANSFORMATION ( 'NONE', 'NONE', #53385,  #43054 ) ;
#53945 = CARTESIAN_POINT ( 'NONE',  ( 3.152801135295366208, -166.8125000013656063, 3.152801135295367985 ) ) ;
#53946 = CARTESIAN_POINT ( 'NONE',  ( -4.458734124999999437, -102.5624999986344079, 0.000000000000000000 ) ) ;
#53947 = CARTESIAN_POINT ( 'NONE',  ( 2.499999999999998668, -55.20833333060214443, -4.330127018922193649 ) ) ;
#53948 = ORIENTED_EDGE ( 'NONE', *, *, #31511, .F. ) ;
#53949 = CARTESIAN_POINT ( 'NONE',  ( -54.64476657466781973, -146.0625000013656063, -4.444560631937228834 ) ) ;
#53950 = CARTESIAN_POINT ( 'NONE',  ( -54.60164318462004474, -139.5000000027312126, -4.984105922594373794 ) ) ;
#53951 = CARTESIAN_POINT ( 'NONE',  ( 4.458734124999999437, -37.81249999863440792, -5.460374474430324690E-16 ) ) ;
#53952 = CARTESIAN_POINT ( 'NONE',  ( 2.730187237215162345E-16, -146.4375000013656063, -4.458734124999999437 ) ) ;
#53953 = LINE ( 'NONE', #25647, #40403 ) ;
#53954 = CARTESIAN_POINT ( 'NONE',  ( -5.000000000000000000, -71.00000000000000000, 0.000000000000000000 ) ) ;
#53955 = CARTESIAN_POINT ( 'NONE',  ( 9.457646018065525792E-16, -12.06249999863440081, 5.148502694627439702 ) ) ;
#53956 = CARTESIAN_POINT ( 'NONE',  ( -4.458734124999997661, -101.4791666653010651, 2.574251347313722516 ) ) ;
#53957 = ORIENTED_EDGE ( 'NONE', *, *, #49457, .T. ) ;
#53958 = CARTESIAN_POINT ( 'NONE',  ( -4.458734125000000326, -143.2500000013655779, -1.846868145590735644 ) ) ;
#53959 = CARTESIAN_POINT ( 'NONE',  ( 2.229367062499998831, -30.89583333196773651, -3.861377020970580887 ) ) ;
#53960 = CARTESIAN_POINT ( 'NONE',  ( 5.000000000000000000, 8.625000002731184168, -6.123233995736766282E-16 ) ) ;
#53961 = CARTESIAN_POINT ( 'NONE',  ( 3.061616997868383141E-16, -140.8750000027312126, -5.000000000000000000 ) ) ;
#53962 = CARTESIAN_POINT ( 'NONE',  ( -57.19623071787017210, -133.3750000013656063, 4.297418129356382899 ) ) ;
#53963 = CARTESIAN_POINT ( 'NONE',  ( 4.458734125000001214, -72.14583333196773651, 2.574251347313718519 ) ) ;
#53964 = ADVANCED_FACE ( 'NONE', ( #46403 ), #36755, .T. ) ;
#53965 = CARTESIAN_POINT ( 'NONE',  ( -3.535533905932737309, -144.7500000027311842, -3.535533905932738197 ) ) ;
#53966 = CARTESIAN_POINT ( 'NONE',  ( -51.75738570946856498, -146.8750000027312126, 3.805975901505576964 ) ) ;
#53967 = CARTESIAN_POINT ( 'NONE',  ( -6.972266317189433020E-16, 12.87500000273118417, -5.000000000000000000 ) ) ;
#53968 =( BOUNDED_CURVE ( )  B_SPLINE_CURVE ( 2, ( #44404, #49555, #14186, #19648, #63100, #363, #43767, #19966, #54392 ),
 .UNSPECIFIED., .F., .F. ) 
 B_SPLINE_CURVE_WITH_KNOTS ( ( 3, 2, 2, 2, 3 ),
 ( 0.6339285714285713969, 0.6345238095238094900, 0.6357142857142856762, 0.6369047619047618625, 0.6374999999999999556 ),
 .UNSPECIFIED. ) 
 CURVE ( )  GEOMETRIC_REPRESENTATION_ITEM ( )  RATIONAL_B_SPLINE_CURVE ( ( 0.9330127018922194093, 0.9330127018922194093, 1.000000000000000000, 0.8660254037844387076, 1.000000000000000000, 0.8660254037844387076, 1.000000000000000000, 0.9330127018922194093, 0.9330127018922194093 ) ) 
 REPRESENTATION_ITEM ( '' )  );
#53969 = CARTESIAN_POINT ( 'NONE',  ( 2.229367062499998831, 5.104166668032261711, -3.861377020970580887 ) ) ;
#53970 = EDGE_LOOP ( 'NONE', ( #53134, #29966, #33168, #16242 ) ) ;
#53971 = DIRECTION ( 'NONE',  ( -0.000000000000000000, -0.000000000000000000, 1.000000000000000000 ) ) ;
#53972 = EDGE_CURVE ( 'NONE', #19776, #42151, #26468, .T. ) ;
#53973 = CARTESIAN_POINT ( 'NONE',  ( 1.339745962155612702, 2.705341801261480050, -5.000000000000000000 ) ) ;
#53975 = CARTESIAN_POINT ( 'NONE',  ( 4.458734124999999437, -28.81249999863440436, -5.460374474430324690E-16 ) ) ;
#53974 = CARTESIAN_POINT ( 'NONE',  ( 5.000000000000000000, -96.50000000000000000, -6.123233995736766282E-16 ) ) ;
#53976 = CARTESIAN_POINT ( 'NONE',  ( 5.000000000000000888, -95.58333333333334281, 2.886751345948126879 ) ) ;
#53977 = CARTESIAN_POINT ( 'NONE',  ( -2.229367062500000163, -81.72916666530106511, -3.861377020970580443 ) ) ;
#53978 = CARTESIAN_POINT ( 'NONE',  ( -3.152548672688508926E-16, 23.18750000136559564, -5.148502694627439702 ) ) ;
#53979 = CARTESIAN_POINT ( 'NONE',  ( -5.000000000000000000, 23.04166666939784847, -2.886751345948128211 ) ) ;
#53980 = CARTESIAN_POINT ( 'NONE',  ( -50.55543936806279248, -140.0625000013656063, 0.3552334253322060320 ) ) ;
#53981 = EDGE_CURVE ( 'NONE', #25633, #2707, #12311, .T. ) ;
#53982 = CARTESIAN_POINT ( 'NONE',  ( 4.458734124999999437, -1.812499998634406584, -5.460374474430324690E-16 ) ) ;
#53983 = CARTESIAN_POINT ( 'NONE',  ( 1.975475456537005874E-15, -81.62499999726881583, 5.000000000000000000 ) ) ;
#53984 = CARTESIAN_POINT ( 'NONE',  ( -2.229367062500000163, -41.72916666530107932, -3.861377020970580443 ) ) ;
#53985 = CARTESIAN_POINT ( 'NONE',  ( -4.999999999999998224, -45.79166666393547303, 2.886751345948131764 ) ) ;
#53986 = CARTESIAN_POINT ( 'NONE',  ( 4.458734125000000326, 4.104166668032260823, 2.574251347313718519 ) ) ;
#53987 = CARTESIAN_POINT ( 'NONE',  ( 4.458734124999999437, -25.06249999863440792, -5.460374474430324690E-16 ) ) ;
#53988 = CARTESIAN_POINT ( 'NONE',  ( -4.458734124999999437, -70.31249999863439371, 0.000000000000000000 ) ) ;
#53989 = CARTESIAN_POINT ( 'NONE',  ( 5.000000000000000000, -105.3749999972688158, -6.123233995736766282E-16 ) ) ;
#53990 = AXIS2_PLACEMENT_3D ( 'NONE', #15959, #24974, #21104 ) ;
#53991 = CARTESIAN_POINT ( 'NONE',  ( -4.458734124999999437, 24.68750000136559208, 0.000000000000000000 ) ) ;
#53992 = CARTESIAN_POINT ( 'NONE',  ( -1.339745962155613812, -65.20534180126146850, -5.000000000000000000 ) ) ;
#53993 = CARTESIAN_POINT ( 'NONE',  ( 6.123233995736766282E-16, -120.0000000000000000, -5.000000000000000000 ) ) ;
#53994 = CARTESIAN_POINT ( 'NONE',  ( 4.458734124999999437, -73.06249999863439371, -5.460374474430324690E-16 ) ) ;
#53995 = CARTESIAN_POINT ( 'NONE',  ( 2.499999999999998668, -58.33333333333333570, -4.330127018922193649 ) ) ;
#53996 = DIRECTION ( 'NONE',  ( -1.000000000000000000, 0.000000000000000000, 1.061635649774262822E-14 ) ) ;
#53997 = ORIENTED_EDGE ( 'NONE', *, *, #34627, .T. ) ;
#53998 = CARTESIAN_POINT ( 'NONE',  ( -51.75738570946856498, -145.7500000000000284, 3.805975901505576964 ) ) ;
#53999 = LINE ( 'NONE', #11212, #51482 ) ;
#54000 = CARTESIAN_POINT ( 'NONE',  ( 5.000000000000000888, -20.58333333333333570, 2.886751345948126879 ) ) ;
#54001 = CARTESIAN_POINT ( 'NONE',  ( -2.229367062499996610, -22.14583333196773651, 3.861377020970582219 ) ) ;
#54002 = CARTESIAN_POINT ( 'NONE',  ( -2.229367062499996610, -85.14583333196773651, 3.861377020970582219 ) ) ;
#54003 = CARTESIAN_POINT ( 'NONE',  ( 2.730187237215162345E-16, -167.4375000013655779, -4.458734124999999437 ) ) ;
#54004 = CARTESIAN_POINT ( 'NONE',  ( -4.999999999999999112, -15.79166666393548191, 2.886751345948131764 ) ) ;
#54006 = ORIENTED_EDGE ( 'NONE', *, *, #45205, .F. ) ;
#54005 = CARTESIAN_POINT ( 'NONE',  ( -2.229367062500000163, -49.47916666530107221, -3.861377020970580443 ) ) ;
#54007 = CARTESIAN_POINT ( 'NONE',  ( -6.972266317189433020E-16, -35.12499999726880873, -5.000000000000000000 ) ) ;
#54008 = DIRECTION ( 'NONE',  ( -0.000000000000000000, 1.000000000000000000, -0.000000000000000000 ) ) ;
#54010 = ORIENTED_EDGE ( 'NONE', *, *, #62138, .F. ) ;
#54009 = CARTESIAN_POINT ( 'NONE',  ( 4.458734125000001214, 3.854166668032260823, 2.574251347313718519 ) ) ;
#54011 = CARTESIAN_POINT ( 'NONE',  ( -1.339745962155610925, -86.66965819600733312, 5.000000000000000000 ) ) ;
#54012 = CARTESIAN_POINT ( 'NONE',  ( -2.499999999999996447, -64.83333333333332860, 4.330127018922195425 ) ) ;
#54013 = CARTESIAN_POINT ( 'NONE',  ( -1.846868145590737420, -156.0000000013656063, 4.458734124999999437 ) ) ;
#54014 = CARTESIAN_POINT ( 'NONE',  ( -4.458734124999998549, -42.47916666530107932, 2.574251347313722516 ) ) ;
#54015 = CARTESIAN_POINT ( 'NONE',  ( -9.184850993605147944E-16, -163.2500000000000000, 5.000000000000000000 ) ) ;
#54016 = CARTESIAN_POINT ( 'NONE',  ( -55.00000000000002132, -155.0000000000000284, 1.734723475976807094E-15 ) ) ;
#54017 = CARTESIAN_POINT ( 'NONE',  ( -59.29741812935640155, -125.8750000013656063, -2.196230717870135685 ) ) ;
#54018 = CARTESIAN_POINT ( 'NONE',  ( -4.458734124999999437, -9.645833331967738289, -2.574251347313719407 ) ) ;
#54019 = CARTESIAN_POINT ( 'NONE',  ( 4.458734124999999437, -44.06249999863440081, -5.460374474430324690E-16 ) ) ;
#54020 = LINE ( 'NONE', #9954, #2059 ) ;
#54021 = CARTESIAN_POINT ( 'NONE',  ( 1.846868145590736310, -146.6250000013655779, 4.458734124999999437 ) ) ;
#54022 = CARTESIAN_POINT ( 'NONE',  ( -2.229367062499996610, -90.39583333196773651, 3.861377020970582219 ) ) ;
#54023 = DIRECTION ( 'NONE',  ( 0.000000000000000000, 1.000000000000000000, 0.000000000000000000 ) ) ;
#54024 = ORIENTED_EDGE ( 'NONE', *, *, #57306, .F. ) ;
#54025 = DIRECTION ( 'NONE',  ( -0.000000000000000000, 1.000000000000000000, -0.000000000000000000 ) ) ;
#54026 = DIRECTION ( 'NONE',  ( -0.000000000000000000, 1.000000000000000000, -0.000000000000000000 ) ) ;
#54027 = CARTESIAN_POINT ( 'NONE',  ( -51.75738570946856498, -148.8750000027312126, 3.805975901505576964 ) ) ;
#54028 = CARTESIAN_POINT ( 'NONE',  ( 2.500000000000002220, -30.66666666666666785, 4.330127018922192761 ) ) ;
#54029 = ORIENTED_EDGE ( 'NONE', *, *, #6782, .T. ) ;
#54030 = CARTESIAN_POINT ( 'NONE',  ( 4.458734124999998549, 3.270833334698929118, -2.574251347313721627 ) ) ;
#54031 = AXIS2_PLACEMENT_3D ( 'NONE', #6595, #17445, #13563 ) ;
#54032 = CARTESIAN_POINT ( 'NONE',  ( 9.457646018065525792E-16, -17.31249999863440436, 5.148502694627439702 ) ) ;
#54033 = CARTESIAN_POINT ( 'NONE',  ( 6.123233995736766282E-16, -170.0000000000000000, -5.000000000000000000 ) ) ;
#54034 = CARTESIAN_POINT ( 'NONE',  ( -4.458734124999999437, -3.395833331967739177, -2.574251347313719407 ) ) ;
#54035 = CARTESIAN_POINT ( 'NONE',  ( -1.339745962155613812, -74.08034179853029855, -5.000000000000000000 ) ) ;
#54036 = CARTESIAN_POINT ( 'NONE',  ( -8.190561711645485556E-16, -150.6875000013656063, 4.458734124999999437 ) ) ;
#54037 = CARTESIAN_POINT ( 'NONE',  ( -3.152548672688508926E-16, 23.18750000136559564, -5.148502694627439702 ) ) ;
#54038 = VERTEX_POINT ( 'NONE', #56385 ) ;
#54039 = CARTESIAN_POINT ( 'NONE',  ( -2.229367062499996610, -95.14583333196773651, 3.861377020970582219 ) ) ;
#54040 = CARTESIAN_POINT ( 'NONE',  ( -6.972266317189433020E-16, -47.24999999999999289, -5.000000000000000000 ) ) ;
#54041 = CARTESIAN_POINT ( 'NONE',  ( 7.264118654998712898, -4.945491722146229563, -7.907633014911220393 ) ) ;
#54042 = CARTESIAN_POINT ( 'NONE',  ( 2.229367062499998831, -11.64583333196774007, -3.861377020970580887 ) ) ;
#54043 = CYLINDRICAL_SURFACE ( 'NONE', #6764, 5.000000000000000000 ) ;
#54044 = CARTESIAN_POINT ( 'NONE',  ( 6.123233995736766282E-16, -170.0000000000000000, -5.000000000000000000 ) ) ;
#54045 =( BOUNDED_CURVE ( )  B_SPLINE_CURVE ( 2, ( #51013, #6958, #36856, #12083, #56802, #26567, #51656, #51966, #46186 ),
 .UNSPECIFIED., .F., .F. ) 
 B_SPLINE_CURVE_WITH_KNOTS ( ( 3, 2, 2, 2, 3 ),
 ( 0.3104166666666666741, 0.3111111111111111160, 0.3125000000000000000, 0.3138888888888888840, 0.3145833333333333259 ),
 .UNSPECIFIED. ) 
 CURVE ( )  GEOMETRIC_REPRESENTATION_ITEM ( )  RATIONAL_B_SPLINE_CURVE ( ( 0.9330127018922194093, 0.9330127018922194093, 1.000000000000000000, 0.8660254037844387076, 1.000000000000000000, 0.8660254037844387076, 1.000000000000000000, 0.9330127018922194093, 0.9330127018922194093 ) ) 
 REPRESENTATION_ITEM ( '' )  );
#54046 = CARTESIAN_POINT ( 'NONE',  ( -52.80376928212989185, -152.8750000013656063, -4.297418129356379346 ) ) ;
#54047 = CARTESIAN_POINT ( 'NONE',  ( 5.000000000000000000, -40.29166666393548013, -2.886751345948129988 ) ) ;
#54048 = CARTESIAN_POINT ( 'NONE',  ( -4.999999999999998224, 21.20833333606451987, 2.886751345948131764 ) ) ;
#54049 = CARTESIAN_POINT ( 'NONE',  ( 4.458734124999999437, 14.18750000136559386, -5.460374474430324690E-16 ) ) ;
#54050 = CARTESIAN_POINT ( 'NONE',  ( 1.975475456537005874E-15, -71.75000000000000000, 5.000000000000000000 ) ) ;
#54051 = ORIENTED_EDGE ( 'NONE', *, *, #40459, .T. ) ;
#54052 = CARTESIAN_POINT ( 'NONE',  ( -3.152548672688508926E-16, 17.43750000136559564, -5.148502694627439702 ) ) ;
#54053 = CARTESIAN_POINT ( 'NONE',  ( 2.229367062500001939, -59.97916666530106511, 3.861377020970579999 ) ) ;
#54054 = VERTEX_POINT ( 'NONE', #40303 ) ;
#54055 = CARTESIAN_POINT ( 'NONE',  ( -2.229367062500000163, -6.729166665301073103, -3.861377020970580443 ) ) ;
#54056 = CARTESIAN_POINT ( 'NONE',  ( 2.499999999999998668, 4.666666666666666075, -4.330127018922193649 ) ) ;
#54057 = CARTESIAN_POINT ( 'NONE',  ( 4.458734125000000326, -168.3750000013655779, -1.846868145590734978 ) ) ;
#54058 = CARTESIAN_POINT ( 'NONE',  ( 1.339745962155615144, -88.70534180126146850, 4.999999999999999112 ) ) ;
#54059 = CARTESIAN_POINT ( 'NONE',  ( -2.229367062500000163, -54.47916666530107221, -3.861377020970580443 ) ) ;
#54060 = CARTESIAN_POINT ( 'NONE',  ( -5.000000000000000000, -89.87499999726880162, 0.000000000000000000 ) ) ;
#54061 = CARTESIAN_POINT ( 'NONE',  ( -2.229367062499996610, -35.14583333196772941, 3.861377020970582219 ) ) ;
#54062 = CARTESIAN_POINT ( 'NONE',  ( 1.339745962155615144, -38.70534180126146850, 4.999999999999999112 ) ) ;
#54063 =( BOUNDED_CURVE ( )  B_SPLINE_CURVE ( 2, ( #20310, #15490, #50209, #1663, #49570, #44737, #40869, #378, #26088 ),
 .UNSPECIFIED., .F., .F. ) 
 B_SPLINE_CURVE_WITH_KNOTS ( ( 3, 2, 2, 2, 3 ),
 ( 0.6374999999999999556, 0.6380952380952380487, 0.6392857142857142350, 0.6404761904761904212, 0.6410714285714286254 ),
 .UNSPECIFIED. ) 
 CURVE ( )  GEOMETRIC_REPRESENTATION_ITEM ( )  RATIONAL_B_SPLINE_CURVE ( ( 0.9330127018922194093, 0.9330127018922194093, 1.000000000000000000, 0.8660254037844387076, 1.000000000000000000, 0.8660254037844387076, 1.000000000000000000, 0.9330127018922130810, 0.9330127018922194093 ) ) 
 REPRESENTATION_ITEM ( '' )  );
#54064 = CARTESIAN_POINT ( 'NONE',  ( 2.500000000000002220, 25.45833333606451987, 4.330127018922192761 ) ) ;
#54065 = CARTESIAN_POINT ( 'NONE',  ( -8.660254037844341113, 30.00000000000000000, 6.047423072554883697E-14 ) ) ;
#54066 = CARTESIAN_POINT ( 'NONE',  ( 4.458734124999999437, -152.6250000013655495, -1.846868145590734978 ) ) ;
#54067 = CARTESIAN_POINT ( 'NONE',  ( 5.000000000000000000, -39.49999999999999289, -6.123233995736766282E-16 ) ) ;
#54068 = CARTESIAN_POINT ( 'NONE',  ( 1.975475456537005874E-15, -98.62499999726880162, 5.000000000000000000 ) ) ;
#54069 = CARTESIAN_POINT ( 'NONE',  ( -59.47615784096000624, -135.0000000000000284, 2.064375355545259527 ) ) ;
#54070 = ORIENTED_EDGE ( 'NONE', *, *, #9786, .T. ) ;
#54071 = CARTESIAN_POINT ( 'NONE',  ( -3.152548672688508926E-16, -99.56249999863440792, -5.148502694627439702 ) ) ;
#54072 = CARTESIAN_POINT ( 'NONE',  ( 4.458734125000001214, 1.854166668032262155, 2.574251347313718519 ) ) ;
#54073 = AXIS2_PLACEMENT_3D ( 'NONE', #21258, #59551, #40865 ) ;
#54074 = CARTESIAN_POINT ( 'NONE',  ( 1.339745962155615144, -80.70534180126146850, 4.999999999999999112 ) ) ;
#54075 = CARTESIAN_POINT ( 'NONE',  ( 1.060575238724906964E-15, 0.2500000000000002220, 5.773502691896257311 ) ) ;
#54076 = CIRCLE ( 'NONE', #53075, 11.00000000000000000 ) ;
#54077 = CARTESIAN_POINT ( 'NONE',  ( -2.229367062500000163, -67.47916666530106511, -3.861377020970580443 ) ) ;
#54078 = VECTOR ( 'NONE', #36181, 1000.000000000000000 ) ;
#54079 = CARTESIAN_POINT ( 'NONE',  ( -1.339745962155613812, -31.08034179853029144, -5.000000000000000000 ) ) ;
#54080 = CARTESIAN_POINT ( 'NONE',  ( -5.000000000000000000, -1.874999997268814944, 0.000000000000000000 ) ) ;
#54082 = ORIENTED_EDGE ( 'NONE', *, *, #26823, .F. ) ;
#54081 = CARTESIAN_POINT ( 'NONE',  ( -2.229367062499996610, -32.14583333196773651, 3.861377020970582219 ) ) ;
#54083 = CARTESIAN_POINT ( 'NONE',  ( -4.999999999999998224, -41.91666666666667140, 2.886751345948131764 ) ) ;
#54084 = CARTESIAN_POINT ( 'NONE',  ( 0.000000000000000000, -170.0000000000000000, 0.000000000000000000 ) ) ;
#54085 = CARTESIAN_POINT ( 'NONE',  ( 1.339745962155612702, -20.29465819873851729, -5.000000000000000000 ) ) ;
#54086 = CARTESIAN_POINT ( 'NONE',  ( 2.499999999999998668, -50.33333333333332860, -4.330127018922193649 ) ) ;
#54087 = CARTESIAN_POINT ( 'NONE',  ( 4.458734125000001214, -27.14583333196774717, 2.574251347313718519 ) ) ;
#54088 = CARTESIAN_POINT ( 'NONE',  ( -5.000000000000000000, 22.12500000273118417, 0.000000000000000000 ) ) ;
#54089 = CARTESIAN_POINT ( 'NONE',  ( -4.458734124999999437, -69.39583333196773651, -2.574251347313719407 ) ) ;
#54090 = CARTESIAN_POINT ( 'NONE',  ( -8.190561711645485556E-16, -142.9375000013656063, 4.458734124999999437 ) ) ;
#54091 = CARTESIAN_POINT ( 'NONE',  ( 2.229367062500001939, -81.97916666530106511, 3.861377020970579999 ) ) ;
#54092 = CARTESIAN_POINT ( 'NONE',  ( -57.89159099828107458, -138.9375000013656063, -3.393966926194107447 ) ) ;
#54093 = CARTESIAN_POINT ( 'NONE',  ( 9.457646018065525792E-16, -29.31249999863440436, 5.148502694627439702 ) ) ;
#54094 = CARTESIAN_POINT ( 'NONE',  ( 5.000000000000000000, -70.37499999726880162, -6.123233995736766282E-16 ) ) ;
#54095 = ORIENTED_EDGE ( 'NONE', *, *, #33623, .T. ) ;
#54096 = DIRECTION ( 'NONE',  ( -0.000000000000000000, 1.000000000000000000, -0.000000000000000000 ) ) ;
#54097 = VERTEX_POINT ( 'NONE', #11977 ) ;
#54098 = CARTESIAN_POINT ( 'NONE',  ( -4.458734124999999437, -70.64583333196773651, -2.574251347313719407 ) ) ;
#54099 = CARTESIAN_POINT ( 'NONE',  ( -52.53715891517739323, -150.4375000000000000, -4.819101127000233298 ) ) ;
#54100 =( NAMED_UNIT ( * ) SI_UNIT ( $, .STERADIAN. ) SOLID_ANGLE_UNIT ( ) );
#54101 = ORIENTED_EDGE ( 'NONE', *, *, #34284, .F. ) ;
#54102 = CARTESIAN_POINT ( 'NONE',  ( -6.972266317189433020E-16, -39.25000000000000000, -5.000000000000000000 ) ) ;
#54103 = CARTESIAN_POINT ( 'NONE',  ( 1.975475456537005874E-15, -48.74999999999999289, 5.000000000000000000 ) ) ;
#54104 = CARTESIAN_POINT ( 'NONE',  ( -4.458734124999999437, -56.56249999863440081, 0.000000000000000000 ) ) ;
#54105 = CARTESIAN_POINT ( 'NONE',  ( -4.458734124999998549, -1.479166665301071770, 2.574251347313722516 ) ) ;
#54106 = EDGE_LOOP ( 'NONE', ( #59233, #18559, #7539, #33661 ) ) ;
#54107 = CYLINDRICAL_SURFACE ( 'NONE', #28590, 5.000000000000000000 ) ;
#54108 = CARTESIAN_POINT ( 'NONE',  ( -4.999999999999998224, -44.91666666666666430, 2.886751345948131764 ) ) ;
#54109 = CARTESIAN_POINT ( 'NONE',  ( 4.458734125000001214, 14.10416666803225993, 2.574251347313718519 ) ) ;
#54110 = CARTESIAN_POINT ( 'NONE',  ( -58.39396692619412477, -140.4375000013656063, 2.891590998281057701 ) ) ;
#54111 = CARTESIAN_POINT ( 'NONE',  ( 5.000000000000000000, -24.41666666666666430, -2.886751345948130876 ) ) ;
#54112 = CARTESIAN_POINT ( 'NONE',  ( 4.458734124999999437, -166.3750000013656063, -1.846868145590734978 ) ) ;
#54113 =( BOUNDED_CURVE ( )  B_SPLINE_CURVE ( 2, ( #15890, #25217, #35509, #44828, #39997, #30680, #6246, #25856, #49339 ),
 .UNSPECIFIED., .F., .F. ) 
 B_SPLINE_CURVE_WITH_KNOTS ( ( 3, 2, 2, 2, 3 ),
 ( 0.7937499999999999556, 0.7944444444444443976, 0.7958333333333332815, 0.7972222222222222765, 0.7979166666666667185 ),
 .UNSPECIFIED. ) 
 CURVE ( )  GEOMETRIC_REPRESENTATION_ITEM ( )  RATIONAL_B_SPLINE_CURVE ( ( 0.9330127018922194093, 0.9330127018922194093, 1.000000000000000000, 0.8660254037844387076, 1.000000000000000000, 0.8660254037844387076, 1.000000000000000000, 0.9330127018922194093, 0.9330127018922194093 ) ) 
 REPRESENTATION_ITEM ( '' )  );
#54114 = VECTOR ( 'NONE', #21890, 1000.000000000000000 ) ;
#54115 = ORIENTED_EDGE ( 'NONE', *, *, #61459, .F. ) ;
#54116 = CARTESIAN_POINT ( 'NONE',  ( 2.229367062500001939, -82.97916666530106511, 3.861377020970579999 ) ) ;
#54117 = CARTESIAN_POINT ( 'NONE',  ( 2.500000000000002220, -39.66666666666667140, 4.330127018922192761 ) ) ;
#54118 = CARTESIAN_POINT ( 'NONE',  ( 4.458734124999999437, 3.187500001365594304, -5.460374474430324690E-16 ) ) ;
#54119 = CARTESIAN_POINT ( 'NONE',  ( 5.000000000000000888, -87.58333333333332860, 2.886751345948126879 ) ) ;
#54120 = CARTESIAN_POINT ( 'NONE',  ( -1.339745962155497683, -43.08034179853029855, -5.000000000000066613 ) ) ;
#54121 = CARTESIAN_POINT ( 'NONE',  ( 2.229367062499998831, -62.89583333196774362, -3.861377020970580887 ) ) ;
#54122 = CARTESIAN_POINT ( 'NONE',  ( 5.000000000000000000, -25.37499999726881583, -6.123233995736766282E-16 ) ) ;
#54123 = CARTESIAN_POINT ( 'NONE',  ( 2.499999999999998668, 12.79166666939785379, -4.330127018922193649 ) ) ;
#54124 = CARTESIAN_POINT ( 'NONE',  ( -4.458734124999999437, 27.68750000136559208, 0.000000000000000000 ) ) ;
#54125 = CARTESIAN_POINT ( 'NONE',  ( 5.000000000000000000, -49.50000000000000000, -6.123233995736766282E-16 ) ) ;
#54126 =( LENGTH_UNIT ( ) NAMED_UNIT ( * ) SI_UNIT ( .MILLI., .METRE. ) );
#54127 = CARTESIAN_POINT ( 'NONE',  ( 2.229367062500001939, -43.97916666530106511, 3.861377020970579999 ) ) ;
#54128 = CARTESIAN_POINT ( 'NONE',  ( 2.229367062499998831, -30.89583333196773651, -3.861377020970580887 ) ) ;
#54129 = CARTESIAN_POINT ( 'NONE',  ( 4.458734124999999437, 5.937500001365593860, -5.460374474430324690E-16 ) ) ;
#54130 = CARTESIAN_POINT ( 'NONE',  ( 3.061616997868383141E-16, -150.7500000000000284, -5.000000000000000000 ) ) ;
#54131 = CARTESIAN_POINT ( 'NONE',  ( 2.499999999999998668, 18.66666666666666430, -4.330127018922193649 ) ) ;
#54132 = CARTESIAN_POINT ( 'NONE',  ( 5.000000000000000000, -150.1250000027312126, 0.000000000000000000 ) ) ;
#54133 = CARTESIAN_POINT ( 'NONE',  ( -4.999999999999998224, -49.91666666666667140, 2.886751345948131764 ) ) ;
#54134 = CARTESIAN_POINT ( 'NONE',  ( 4.458734125000001214, -35.89583333196773651, 2.574251347313718519 ) ) ;
#54135 = CARTESIAN_POINT ( 'NONE',  ( 2.499999999999998668, -71.20833333060214443, -4.330127018922193649 ) ) ;
#54136 = CARTESIAN_POINT ( 'NONE',  ( -59.59170313451811296, -144.7500000013656063, 1.485763867205729394 ) ) ;
#54137 = CARTESIAN_POINT ( 'NONE',  ( 3.535533905932736864, -144.1250000000000000, 3.535533905932738641 ) ) ;
#54138 = DIRECTION ( 'NONE',  ( 0.000000000000000000, 1.000000000000000000, 0.000000000000000000 ) ) ;
#54139 = CARTESIAN_POINT ( 'NONE',  ( -3.152548672688508926E-16, -82.81249999863442213, -5.148502694627439702 ) ) ;
#54140 = CARTESIAN_POINT ( 'NONE',  ( 2.730187237215162345E-16, -167.4375000013655779, -4.458734124999999437 ) ) ;
#54141 = CARTESIAN_POINT ( 'NONE',  ( 4.458734124999999437, -36.81249999863440792, -5.460374474430324690E-16 ) ) ;
#54142 = CARTESIAN_POINT ( 'NONE',  ( 1.975475456537005874E-15, -18.74999999999999645, 5.000000000000000000 ) ) ;
#54143 = CARTESIAN_POINT ( 'NONE',  ( -6.972266317189433020E-16, -45.12499999726880162, -5.000000000000000000 ) ) ;
#54144 = CARTESIAN_POINT ( 'NONE',  ( 5.000000000000000000, -22.41666666666666785, -2.886751345948129988 ) ) ;
#54145 = CARTESIAN_POINT ( 'NONE',  ( -1.846868145590734756, -142.1250000013656063, -4.458734125000000326 ) ) ;
#54146 = ORIENTED_EDGE ( 'NONE', *, *, #42035, .T. ) ;
#54147 = CARTESIAN_POINT ( 'NONE',  ( -4.999999999999999112, -90.79166666393545881, 2.886751345948131764 ) ) ;
#54148 = ORIENTED_EDGE ( 'NONE', *, *, #12605, .T. ) ;
#54149 = CARTESIAN_POINT ( 'NONE',  ( 4.458734125000000326, -62.14583333196774362, 2.574251347313718519 ) ) ;
#54150 = CARTESIAN_POINT ( 'NONE',  ( 1.060575238724906964E-15, 20.37500000273119127, 5.773502691896257311 ) ) ;
#54151 = CARTESIAN_POINT ( 'NONE',  ( -2.352990130084580066E-16, 8.660254037844390851, -7.422398894150034288 ) ) ;
#54152 = CARTESIAN_POINT ( 'NONE',  ( 2.500000000000002220, 11.33333333333333393, 4.330127018922192761 ) ) ;
#54153 = EDGE_CURVE ( 'NONE', #43336, #43748, #16605, .T. ) ;
#54154 = CARTESIAN_POINT ( 'NONE',  ( -4.458734124999997661, -53.22916666530107932, 2.574251347313722516 ) ) ;
#54155 = CARTESIAN_POINT ( 'NONE',  ( 4.458734125000001214, -5.895833331967740953, 2.574251347313718519 ) ) ;
#54156 = DIRECTION ( 'NONE',  ( -0.000000000000000000, 1.000000000000000000, -0.000000000000000000 ) ) ;
#54157 = CARTESIAN_POINT ( 'NONE',  ( 3.535533905932736864, -158.2500000027312126, 3.535533905932738641 ) ) ;
#54158 = DIRECTION ( 'NONE',  ( -0.000000000000000000, -1.000000000000000000, -0.000000000000000000 ) ) ;
#54160 = CARTESIAN_POINT ( 'NONE',  ( -4.458734124999999437, -19.31249999863440081, 0.000000000000000000 ) ) ;
#54159 = CARTESIAN_POINT ( 'NONE',  ( -6.972266317189433020E-16, -79.24999999999998579, -5.000000000000000000 ) ) ;
#54161 = VECTOR ( 'NONE', #59018, 1000.000000000000000 ) ;
#54162 = CARTESIAN_POINT ( 'NONE',  ( 5.000000000000000888, 0.4166666666666659080, 2.886751345948126879 ) ) ;
#54163 = CARTESIAN_POINT ( 'NONE',  ( -4.458734124999999437, -53.31249999863439371, 0.000000000000000000 ) ) ;
#54164 = CARTESIAN_POINT ( 'NONE',  ( -4.458734125000001214, -156.1250000013655779, 1.846868145590734089 ) ) ;
#54165 = AXIS2_PLACEMENT_3D ( 'NONE', #39828, #1271, #60751 ) ;
#54166 = AXIS2_PLACEMENT_3D ( 'NONE', #14842, #39287, #58914 ) ;
#54167 = ADVANCED_FACE ( 'NONE', ( #25830 ), #46716, .T. ) ;
#54168 = CARTESIAN_POINT ( 'NONE',  ( -2.499999999999996447, -57.70833333060214443, 4.330127018922195425 ) ) ;
#54169 = EDGE_LOOP ( 'NONE', ( #57210, #16604, #63348, #43641 ) ) ;
#54171 = TOROIDAL_SURFACE ( 'NONE', #25397, 10.12668159690567649, 0.7733184030943209830 ) ;
#54170 = LINE ( 'NONE', #30361, #29139 ) ;
#54173 = EDGE_CURVE ( 'NONE', #41437, #11139, #32188, .T. ) ;
#54172 = CARTESIAN_POINT ( 'NONE',  ( 4.458734124999999437, 5.937500001365593860, -5.460374474430324690E-16 ) ) ;
#54174 = ORIENTED_EDGE ( 'NONE', *, *, #29384, .T. ) ;
#54175 = CARTESIAN_POINT ( 'NONE',  ( -6.972266317189433020E-16, 21.87500000273118417, -5.000000000000000000 ) ) ;
#54176 = CARTESIAN_POINT ( 'NONE',  ( 3.152801135295366208, -156.5625000013656063, 3.152801135295367985 ) ) ;
#54177 = ORIENTED_EDGE ( 'NONE', *, *, #30575, .F. ) ;
#54178 = CARTESIAN_POINT ( 'NONE',  ( -1.339745962155613812, 10.79465819873852084, -5.000000000000000000 ) ) ;
#54179 = CARTESIAN_POINT ( 'NONE',  ( -57.46284108482265651, -132.9375000000000284, 4.819101127000239515 ) ) ;
#54180 = CARTESIAN_POINT ( 'NONE',  ( -6.972266317189433020E-16, -59.12499999726880873, -5.000000000000000000 ) ) ;
#54181 = CARTESIAN_POINT ( 'NONE',  ( 4.458734124999999437, -43.06249999863440081, -5.460374474430324690E-16 ) ) ;
#54182 = ORIENTED_EDGE ( 'NONE', *, *, #25475, .F. ) ;
#54183 = EDGE_CURVE ( 'NONE', #29896, #143, #31277, .T. ) ;
#54184 = CARTESIAN_POINT ( 'NONE',  ( 5.000000000000000000, -143.1875000027312410, 2.071067811865478614 ) ) ;
#54185 = CARTESIAN_POINT ( 'NONE',  ( 2.229367062500001939, 17.02083333469892779, 3.861377020970579999 ) ) ;
#54186 = CARTESIAN_POINT ( 'NONE',  ( -49.85088928181150436, -149.5625000000000284, -1.666127454062680480 ) ) ;
#54187 = ORIENTED_EDGE ( 'NONE', *, *, #37550, .F. ) ;
#54188 = CARTESIAN_POINT ( 'NONE',  ( -2.229367062500000163, 28.52083333469892779, -3.861377020970580443 ) ) ;
#54189 = CARTESIAN_POINT ( 'NONE',  ( -50.55543936806279248, -152.0625000013656063, 0.3552334253322060320 ) ) ;
#54190 = CARTESIAN_POINT ( 'NONE',  ( 5.000000000000000000, 12.70833333606451809, -2.886751345948130876 ) ) ;
#54191 = CARTESIAN_POINT ( 'NONE',  ( -52.79662235349376687, -135.0000000000000000, 4.334898500269361854 ) ) ;
#54192 = CARTESIAN_POINT ( 'NONE',  ( -1.127183054612291972E-14, 24.25000000000000000, 4.999999999999999112 ) ) ;
#54193 = CARTESIAN_POINT ( 'NONE',  ( 4.458734124999998549, -65.72916666530106511, -2.574251347313721627 ) ) ;
#54194 = DIRECTION ( 'NONE',  ( 0.000000000000000000, 0.000000000000000000, 1.000000000000000000 ) ) ;
#54195 = CARTESIAN_POINT ( 'NONE',  ( 2.229367062499998831, 16.35416666803225993, -3.861377020970580887 ) ) ;
#54196 = LINE ( 'NONE', #53879, #33911 ) ;
#54197 = CARTESIAN_POINT ( 'NONE',  ( -3.152548672688508926E-16, -50.81249999863440792, -5.148502694627439702 ) ) ;
#54198 = EDGE_CURVE ( 'NONE', #11102, #17248, #21111, .T. ) ;
#54199 = CARTESIAN_POINT ( 'NONE',  ( -4.999999999999999112, -11.79166666393547835, 2.886751345948131764 ) ) ;
#54200 = CARTESIAN_POINT ( 'NONE',  ( 5.000000000000000888, -42.45833333060214443, 2.886751345948126879 ) ) ;
#54201 = DIRECTION ( 'NONE',  ( 0.000000000000000000, 0.000000000000000000, -1.000000000000000000 ) ) ;
#54202 = CARTESIAN_POINT ( 'NONE',  ( -4.458734124999998549, -89.47916666530106511, 2.574251347313722516 ) ) ;
#54203 = CARTESIAN_POINT ( 'NONE',  ( -4.458734124999997661, -107.2291666653010651, 2.574251347313722516 ) ) ;
#54204 = CARTESIAN_POINT ( 'NONE',  ( 2.229367062499998831, -13.89583333196774184, -3.861377020970580887 ) ) ;
#54205 = ORIENTED_EDGE ( 'NONE', *, *, #17820, .F. ) ;
#54206 = VECTOR ( 'NONE', #6290, 1000.000000000000000 ) ;
#54207 = CARTESIAN_POINT ( 'NONE',  ( 3.061616997868383141E-16, -143.8750000027312126, -5.000000000000000000 ) ) ;
#54208 = CARTESIAN_POINT ( 'NONE',  ( 2.229367062500001939, -98.97916666530105090, 3.861377020970579999 ) ) ;
#54209 = CARTESIAN_POINT ( 'NONE',  ( -2.071067811865475061, -162.8125000027312126, -5.000000000000000888 ) ) ;
#54210 = CARTESIAN_POINT ( 'NONE',  ( 4.458734125000001214, -100.1458333319677365, 2.574251347313718519 ) ) ;
#54211 = VECTOR ( 'NONE', #21825, 1000.000000000000227 ) ;
#54212 = CARTESIAN_POINT ( 'NONE',  ( 5.000000000000000000, -19.29166666393548013, -2.886751345948130876 ) ) ;
#54213 = CARTESIAN_POINT ( 'NONE',  ( 1.060575238724906964E-15, -59.62499999726880873, 5.773502691896257311 ) ) ;
#54214 = CARTESIAN_POINT ( 'NONE',  ( 1.975475456537005874E-15, -66.74999999999998579, 5.000000000000000000 ) ) ;
#54215 = CARTESIAN_POINT ( 'NONE',  ( -52.80376928212989185, -125.8750000013656063, -4.297418129356379346 ) ) ;
#54216 = CARTESIAN_POINT ( 'NONE',  ( -59.59170313451810586, -146.5000000013656347, 1.485763867205729394 ) ) ;
#54217 = CARTESIAN_POINT ( 'NONE',  ( -4.458734124999999437, -17.31249999863440792, 0.000000000000000000 ) ) ;
#54218 = CARTESIAN_POINT ( 'NONE',  ( -2.229367062500000163, 8.270833334698926009, -3.861377020970580443 ) ) ;
#54219 = CARTESIAN_POINT ( 'NONE',  ( -2.229367062499996610, -61.39583333196774362, 3.861377020970582219 ) ) ;
#54220 = CARTESIAN_POINT ( 'NONE',  ( -1.339745962155610925, -53.79465819873851018, 5.000000000000000000 ) ) ;
#54221 = CARTESIAN_POINT ( 'NONE',  ( -2.229367062499996610, -17.14583333196773651, 3.861377020970582219 ) ) ;
#54222 = CARTESIAN_POINT ( 'NONE',  ( 1.339745962155612702, -75.29465819873853150, -5.000000000000000000 ) ) ;
#54223 = CARTESIAN_POINT ( 'NONE',  ( 3.535533905932736864, -156.1250000000000000, 3.535533905932738641 ) ) ;
#54224 = CARTESIAN_POINT ( 'NONE',  ( -4.999999999999999112, -5.916666666666666963, 2.886751345948131764 ) ) ;
#54225 = ORIENTED_EDGE ( 'NONE', *, *, #23328, .F. ) ;
#54226 = CARTESIAN_POINT ( 'NONE',  ( 9.457646018065525792E-16, -44.31249999863440081, 5.148502694627439702 ) ) ;
#54227 = CARTESIAN_POINT ( 'NONE',  ( -5.000000000000000000, 26.00000000000000000, 0.000000000000000000 ) ) ;
#54228 = CARTESIAN_POINT ( 'NONE',  ( 2.500000000000002220, -66.66666666666667140, 4.330127018922192761 ) ) ;
#54229 = CARTESIAN_POINT ( 'NONE',  ( -4.999999999999998224, -66.79166666393547303, 2.886751345948131764 ) ) ;
#54230 = CARTESIAN_POINT ( 'NONE',  ( 9.457646018065525792E-16, -92.06249999863439371, 5.148502694627439702 ) ) ;
#54231 = CARTESIAN_POINT ( 'NONE',  ( 9.457646018065525792E-16, 18.68750000136559208, 5.148502694627439702 ) ) ;
#54232 = EDGE_CURVE ( 'NONE', #44900, #23690, #39124, .T. ) ;
#54233 = CARTESIAN_POINT ( 'NONE',  ( -2.229367062500000163, 7.520833334698929562, -3.861377020970580443 ) ) ;
#54234 = CARTESIAN_POINT ( 'NONE',  ( -3.535533905932738641, -165.5000000027312126, 3.535533905932737309 ) ) ;
#54235 = CARTESIAN_POINT ( 'NONE',  ( 4.458734124999998549, -86.97916666530107932, -2.574251347313721627 ) ) ;
#54236 = CARTESIAN_POINT ( 'NONE',  ( -4.458734124999999437, 20.35416666803225993, -2.574251347313719407 ) ) ;
#54237 = CARTESIAN_POINT ( 'NONE',  ( -5.000000000000000000, -74.00000000000000000, 0.000000000000000000 ) ) ;
#54238 = CARTESIAN_POINT ( 'NONE',  ( -5.000000000000000000, 7.125000002731185944, 0.000000000000000000 ) ) ;
#54239 = ORIENTED_EDGE ( 'NONE', *, *, #6119, .T. ) ;
#54240 = CARTESIAN_POINT ( 'NONE',  ( 2.499999999999998668, -79.33333333333332860, -4.330127018922193649 ) ) ;
#54241 = VERTEX_POINT ( 'NONE', #57015 ) ;
#54243 = CARTESIAN_POINT ( 'NONE',  ( -5.000000000000000000, -33.00000000000000000, 0.000000000000000000 ) ) ;
#54242 = DIRECTION ( 'NONE',  ( -0.000000000000000000, 1.000000000000000000, -0.000000000000000000 ) ) ;
#54244 = CARTESIAN_POINT ( 'NONE',  ( -3.152548672688508926E-16, -38.56249999863439371, -5.148502694627439702 ) ) ;
#54245 =( BOUNDED_CURVE ( )  B_SPLINE_CURVE ( 2, ( #1382, #59587, #49912, #29656, #35448, #10995, #14859, #10364, #39619 ),
 .UNSPECIFIED., .F., .F. ) 
 B_SPLINE_CURVE_WITH_KNOTS ( ( 3, 2, 2, 2, 3 ),
 ( 0.3520833333333333592, 0.3527777777777778012, 0.3541666666666666852, 0.3555555555555555691, 0.3562500000000000111 ),
 .UNSPECIFIED. ) 
 CURVE ( )  GEOMETRIC_REPRESENTATION_ITEM ( )  RATIONAL_B_SPLINE_CURVE ( ( 0.9330127018922194093, 0.9330127018922220739, 1.000000000000000000, 0.8660254037844387076, 1.000000000000000000, 0.8660254037844387076, 1.000000000000000000, 0.9330127018922194093, 0.9330127018922194093 ) ) 
 REPRESENTATION_ITEM ( '' )  );
#54246 = CARTESIAN_POINT ( 'NONE',  ( -2.499999999999996447, -38.70833333060213732, 4.330127018922195425 ) ) ;
#54247 = EDGE_LOOP ( 'NONE', ( #12255, #25616, #35252, #39368 ) ) ;
#54248 = CARTESIAN_POINT ( 'NONE',  ( -50.40829686548195099, -146.2500000013656063, -1.485763867205728284 ) ) ;
#54250 = EDGE_CURVE ( 'NONE', #32199, #34010, #27407, .T. ) ;
#54249 = CARTESIAN_POINT ( 'NONE',  ( 9.457646018065525792E-16, -14.06249999863440259, 5.148502694627439702 ) ) ;
#54252 = ORIENTED_EDGE ( 'NONE', *, *, #48267, .F. ) ;
#54251 = CARTESIAN_POINT ( 'NONE',  ( 4.458734124999998549, -16.97916666530107221, -2.574251347313721627 ) ) ;
#54253 = CARTESIAN_POINT ( 'NONE',  ( 2.499999999999998668, -84.33333333333332860, -4.330127018922193649 ) ) ;
#54254 = LINE ( 'NONE', #60048, #1167 ) ;
#54255 = CARTESIAN_POINT ( 'NONE',  ( 2.229367062499998831, -59.89583333196774362, -3.861377020970580887 ) ) ;
#54256 = CIRCLE ( 'NONE', #2956, 10.39117206796836079 ) ;
#54257 = CARTESIAN_POINT ( 'NONE',  ( -2.500000000000000444, -82.04166666393547303, -4.330127018922193649 ) ) ;
#54259 = ORIENTED_EDGE ( 'NONE', *, *, #17388, .F. ) ;
#54258 = CARTESIAN_POINT ( 'NONE',  ( -6.972266317189433020E-16, 3.875000002731185500, -5.000000000000000000 ) ) ;
#54260 = CARTESIAN_POINT ( 'NONE',  ( -57.46284108482265651, -143.9375000000000000, 4.819101127000239515 ) ) ;
#54261 = AXIS2_PLACEMENT_3D ( 'NONE', #54717, #39265, #30250 ) ;
#54262 = CARTESIAN_POINT ( 'NONE',  ( 9.457646018065525792E-16, -25.31249999863440792, 5.148502694627439702 ) ) ;
#54263 = CARTESIAN_POINT ( 'NONE',  ( 1.339745962155612702, -5.169658196007333117, -5.000000000000000000 ) ) ;
#54264 = ORIENTED_EDGE ( 'NONE', *, *, #44076, .T. ) ;
#54265 = CARTESIAN_POINT ( 'NONE',  ( 3.152801135295366208, -162.8125000013656063, 3.152801135295367985 ) ) ;
#54266 = CARTESIAN_POINT ( 'NONE',  ( 2.229367062500001939, -107.2291666653010651, 3.861377020970579999 ) ) ;
#54267 = CARTESIAN_POINT ( 'NONE',  ( 5.000000000000000000, -148.0625000000000000, 2.071067811865478614 ) ) ;
#54268 = ORIENTED_EDGE ( 'NONE', *, *, #1265, .T. ) ;
#54269 = CARTESIAN_POINT ( 'NONE',  ( -50.55543936806279248, -146.3125000013656063, 0.3552334253322060320 ) ) ;
#54270 = CARTESIAN_POINT ( 'NONE',  ( -4.458734124999998549, -74.47916666530106511, 2.574251347313722516 ) ) ;
#54271 = CARTESIAN_POINT ( 'NONE',  ( -54.60164318462004474, -137.5000000027312126, -4.984105922594373794 ) ) ;
#54272 = CARTESIAN_POINT ( 'NONE',  ( 4.458734125000000326, -45.89583333196774362, 2.574251347313718519 ) ) ;
#54273 = CARTESIAN_POINT ( 'NONE',  ( -3.152801135295367096, -144.3125000013655779, -3.152801135295367541 ) ) ;
#54274 = CARTESIAN_POINT ( 'NONE',  ( 6.123233995736766282E-16, -170.0000000000000000, -5.000000000000000000 ) ) ;
#54275 = CARTESIAN_POINT ( 'NONE',  ( 1.975475456537005874E-15, -47.62499999726880873, 5.000000000000000000 ) ) ;
#54276 = CARTESIAN_POINT ( 'NONE',  ( 9.457646018065525792E-16, -13.06249999863440259, 5.148502694627439702 ) ) ;
#54277 = CARTESIAN_POINT ( 'NONE',  ( -4.999999999999999112, -99.91666666666665719, 2.886751345948131764 ) ) ;
#54278 = EDGE_LOOP ( 'NONE', ( #20809, #40730, #59487 ) ) ;
#54279 = CARTESIAN_POINT ( 'NONE',  ( 4.458734124999999437, -141.7500000013655779, 1.846868145590737864 ) ) ;
#54280 = CARTESIAN_POINT ( 'NONE',  ( -4.458734124999998549, -33.47916666530107221, 2.574251347313722516 ) ) ;
#54281 = CARTESIAN_POINT ( 'NONE',  ( -5.000000000000000000, 8.125000002731187720, 0.000000000000000000 ) ) ;
#54282 = PLANE ( 'NONE',  #33524 ) ;
#54283 = CARTESIAN_POINT ( 'NONE',  ( -59.29741812935640155, -132.6250000013656347, -2.196230717870135685 ) ) ;
#54284 = CARTESIAN_POINT ( 'NONE',  ( 4.458734125000001214, -74.14583333196773651, 2.574251347313718519 ) ) ;
#54285 = DIRECTION ( 'NONE',  ( 0.000000000000000000, 0.000000000000000000, 1.000000000000000000 ) ) ;
#54286 = FACE_OUTER_BOUND ( 'NONE', #54568, .T. ) ;
#54287 = CARTESIAN_POINT ( 'NONE',  ( 0.000000000000000000, -170.0000000000000000, 0.000000000000000000 ) ) ;
#54288 = CARTESIAN_POINT ( 'NONE',  ( -2.229367062499996610, 4.604166668032261711, 3.861377020970582219 ) ) ;
#54289 = ORIENTED_EDGE ( 'NONE', *, *, #5516, .F. ) ;
#54290 = CARTESIAN_POINT ( 'NONE',  ( 6.123233995736766282E-16, -170.0000000000000000, -5.000000000000000000 ) ) ;
#54291 = CARTESIAN_POINT ( 'NONE',  ( -4.999999999999998224, -59.91666666666665719, 2.886751345948131764 ) ) ;
#54293 = CARTESIAN_POINT ( 'NONE',  ( -4.458734124999999437, -28.31249999863440081, 0.000000000000000000 ) ) ;
#54292 = CARTESIAN_POINT ( 'NONE',  ( -5.000000000000000000, -98.08333333333332860, -2.886751345948128211 ) ) ;
#54294 = CARTESIAN_POINT ( 'NONE',  ( -4.999999999999998224, -22.79166666393548013, 2.886751345948131764 ) ) ;
#54295 = CARTESIAN_POINT ( 'NONE',  ( 4.458734125000001214, -83.14583333196773651, 2.574251347313718519 ) ) ;
#54296 = CARTESIAN_POINT ( 'NONE',  ( -3.152548672688508926E-16, 19.18750000136559208, -5.148502694627439702 ) ) ;
#54297 = DIRECTION ( 'NONE',  ( -0.000000000000000000, 1.000000000000000000, -0.000000000000000000 ) ) ;
#54298 = CARTESIAN_POINT ( 'NONE',  ( -57.89159099828107458, -138.6875000013656347, -3.393966926194107447 ) ) ;
#54299 = CARTESIAN_POINT ( 'NONE',  ( 2.229367062499998831, -3.645833331967739177, -3.861377020970580887 ) ) ;
#54300 = CARTESIAN_POINT ( 'NONE',  ( 9.457646018065525792E-16, 20.68750000136559564, 5.148502694627439702 ) ) ;
#54301 = CARTESIAN_POINT ( 'NONE',  ( -4.458734124999997661, -40.47916666530107221, 2.574251347313722516 ) ) ;
#54302 =( BOUNDED_CURVE ( )  B_SPLINE_CURVE ( 2, ( #57848, #28242, #52695, #23113, #32763, #9255, #4429, #43038, #47856 ),
 .UNSPECIFIED., .F., .F. ) 
 B_SPLINE_CURVE_WITH_KNOTS ( ( 3, 2, 2, 2, 3 ),
 ( 0.3982142857142857428, 0.3988095238095238360, 0.4000000000000000222, 0.4011904761904762085, 0.4017857142857143016 ),
 .UNSPECIFIED. ) 
 CURVE ( )  GEOMETRIC_REPRESENTATION_ITEM ( )  RATIONAL_B_SPLINE_CURVE ( ( 0.9330127018922194093, 0.9330127018922225179, 1.000000000000000000, 0.8660254037844387076, 1.000000000000000000, 0.8660254037844387076, 1.000000000000000000, 0.9330127018922194093, 0.9330127018922194093 ) ) 
 REPRESENTATION_ITEM ( '' )  );
#54303 = CARTESIAN_POINT ( 'NONE',  ( 5.000000000000000888, -15.58333333333332860, 2.886751345948126879 ) ) ;
#54304 = CARTESIAN_POINT ( 'NONE',  ( -3.152548672688508926E-16, 3.437500001365594748, -5.148502694627439702 ) ) ;
#54305 = CARTESIAN_POINT ( 'NONE',  ( 4.458734125000000326, -28.14583333196774007, 2.574251347313718519 ) ) ;
#54306 =( BOUNDED_CURVE ( )  B_SPLINE_CURVE ( 2, ( #47895, #43076, #56943, #23784, #47590, #37623, #3542, #13808, #62714 ),
 .UNSPECIFIED., .F., .F. ) 
 B_SPLINE_CURVE_WITH_KNOTS ( ( 3, 2, 2, 2, 3 ),
 ( 0.1187500000000000083, 0.1194444444444444503, 0.1208333333333333343, 0.1222222222222222182, 0.1229166666666666741 ),
 .UNSPECIFIED. ) 
 CURVE ( )  GEOMETRIC_REPRESENTATION_ITEM ( )  RATIONAL_B_SPLINE_CURVE ( ( 0.9330127018922194093, 0.9330127018922200755, 1.000000000000000000, 0.8660254037844387076, 1.000000000000000000, 0.8660254037844387076, 1.000000000000000000, 0.9330127018922187432, 0.9330127018922194093 ) ) 
 REPRESENTATION_ITEM ( '' )  );
#54307 = VECTOR ( 'NONE', #46495, 1000.000000000000000 ) ;
#54308 = CARTESIAN_POINT ( 'NONE',  ( -4.458734124999999437, -68.39583333196773651, -2.574251347313719407 ) ) ;
#54309 = CARTESIAN_POINT ( 'NONE',  ( 5.000000000000000000, -105.2916666639354730, -2.886751345948129988 ) ) ;
#54310 = VECTOR ( 'NONE', #60610, 1000.000000000000000 ) ;
#54311 = CARTESIAN_POINT ( 'NONE',  ( 4.458734124999998549, 24.27083333469892779, -2.574251347313721627 ) ) ;
#54312 = EDGE_CURVE ( 'NONE', #28777, #27512, #14888, .T. ) ;
#54313 = EDGE_CURVE ( 'NONE', #61372, #15636, #38327, .T. ) ;
#54314 = CARTESIAN_POINT ( 'NONE',  ( 1.975475456537005874E-15, -58.62499999726879452, 5.000000000000000000 ) ) ;
#54315 = CARTESIAN_POINT ( 'NONE',  ( 9.457646018065525792E-16, -109.3124999986343937, 5.148502694627439702 ) ) ;
#54316 = CARTESIAN_POINT ( 'NONE',  ( -2.229367062499996610, -75.39583333196773651, 3.861377020970582219 ) ) ;
#54317 = CARTESIAN_POINT ( 'NONE',  ( 5.000000000000000000, -59.41666666666665719, -2.886751345948129988 ) ) ;
#54318 = EDGE_CURVE ( 'NONE', #39123, #62091, #43630, .T. ) ;
#54319 = CARTESIAN_POINT ( 'NONE',  ( 1.975475456537005874E-15, -21.75000000000000000, 5.000000000000000000 ) ) ;
#54320 = CARTESIAN_POINT ( 'NONE',  ( -5.000000000000000000, 25.04166666939785557, -2.886751345948128211 ) ) ;
#54321 = ORIENTED_EDGE ( 'NONE', *, *, #16921, .T. ) ;
#54322 = CARTESIAN_POINT ( 'NONE',  ( -4.999999999999998224, -26.91666666666666430, 2.886751345948131764 ) ) ;
#54323 = EDGE_CURVE ( 'NONE', #59704, #26446, #40825, .T. ) ;
#54324 = CYLINDRICAL_SURFACE ( 'NONE', #47340, 5.000000000000000000 ) ;
#54325 = CARTESIAN_POINT ( 'NONE',  ( -4.999999999999999112, -19.91666666666666785, 2.886751345948131764 ) ) ;
#54326 = CARTESIAN_POINT ( 'NONE',  ( 4.458734124999998549, -24.72916666530106866, -2.574251347313721627 ) ) ;
#54327 = ADVANCED_FACE ( 'NONE', ( #28041 ), #22281, .T. ) ;
#54328 = CARTESIAN_POINT ( 'NONE',  ( -2.229367062499996610, -84.14583333196773651, 3.861377020970582219 ) ) ;
#54329 = EDGE_CURVE ( 'NONE', #2707, #55393, #63010, .T. ) ;
#54330 = VECTOR ( 'NONE', #55192, 1000.000000000000000 ) ;
#54331 = CARTESIAN_POINT ( 'NONE',  ( -2.500000000000000444, -18.04166666393547658, -4.330127018922193649 ) ) ;
#54333 = VERTEX_POINT ( 'NONE', #5497 ) ;
#54332 = CARTESIAN_POINT ( 'NONE',  ( -2.229367062499996610, -51.14583333196772941, 3.861377020970582219 ) ) ;
#54334 = CARTESIAN_POINT ( 'NONE',  ( -6.972266317189433020E-16, -71.12499999726878741, -5.000000000000000000 ) ) ;
#54335 = LINE ( 'NONE', #9003, #52858 ) ;
#54337 = VERTEX_POINT ( 'NONE', #4538 ) ;
#54336 = CARTESIAN_POINT ( 'NONE',  ( 2.229367062500001939, 0.7708333346989268975, 3.861377020970579999 ) ) ;
#54338 =( BOUNDED_CURVE ( )  B_SPLINE_CURVE ( 2, ( #7660, #33352, #37546, #12783, #56865, #3150, #17296, #42679, #27889 ),
 .UNSPECIFIED., .F., .F. ) 
 B_SPLINE_CURVE_WITH_KNOTS ( ( 3, 2, 2, 2, 3 ),
 ( 0.7589285714285713969, 0.7595238095238094900, 0.7607142857142856762, 0.7619047619047618625, 0.7624999999999999556 ),
 .UNSPECIFIED. ) 
 CURVE ( )  GEOMETRIC_REPRESENTATION_ITEM ( )  RATIONAL_B_SPLINE_CURVE ( ( 0.9330127018922194093, 0.9330127018922194093, 1.000000000000000000, 0.8660254037844387076, 1.000000000000000000, 0.8660254037844387076, 1.000000000000000000, 0.9330127018922194093, 0.9330127018922194093 ) ) 
 REPRESENTATION_ITEM ( '' )  );
#54339 = CARTESIAN_POINT ( 'NONE',  ( -52.80376928212989185, -149.8750000013655779, -4.297418129356378458 ) ) ;
#54340 = CARTESIAN_POINT ( 'NONE',  ( 5.000000000000000000, -67.41666666666665719, -2.886751345948129988 ) ) ;
#54341 = EDGE_CURVE ( 'NONE', #49592, #51345, #5896, .T. ) ;
#54342 = CARTESIAN_POINT ( 'NONE',  ( 4.458734125000000326, -152.6250000013655495, -1.846868145590734978 ) ) ;
#54343 = CARTESIAN_POINT ( 'NONE',  ( -2.229367062500000163, -39.72916666530107221, -3.861377020970580443 ) ) ;
#54344 = CARTESIAN_POINT ( 'NONE',  ( -5.000000000000000000, -76.87499999726880162, 0.000000000000000000 ) ) ;
#54345 = CARTESIAN_POINT ( 'NONE',  ( -9.184850993605147944E-16, -161.2500000000000000, 5.000000000000000000 ) ) ;
#54346 = EDGE_CURVE ( 'NONE', #29467, #9545, #38740, .T. ) ;
#54347 = EDGE_CURVE ( 'NONE', #25868, #10085, #19403, .T. ) ;
#54348 = CARTESIAN_POINT ( 'NONE',  ( 0.000000000000000000, -120.0000000000000000, 0.000000000000000000 ) ) ;
#54349 = CARTESIAN_POINT ( 'NONE',  ( -54.64476657466781973, -129.0625000013656063, -4.444560631937228834 ) ) ;
#54350 = CARTESIAN_POINT ( 'NONE',  ( -4.458734124999998549, -11.47916666530107044, 2.574251347313722516 ) ) ;
#54351 = CARTESIAN_POINT ( 'NONE',  ( -2.229367062500000163, -46.72916666530106511, -3.861377020970580443 ) ) ;
#54352 = DIRECTION ( 'NONE',  ( -0.000000000000000000, 1.000000000000000000, -0.000000000000000000 ) ) ;
#54353 = CARTESIAN_POINT ( 'NONE',  ( -3.152801135295367096, -148.0625000013655779, -3.152801135295367541 ) ) ;
#54354 = CARTESIAN_POINT ( 'NONE',  ( 2.229367062499998831, -89.89583333196773651, -3.861377020970580887 ) ) ;
#54355 = CARTESIAN_POINT ( 'NONE',  ( -53.33387254593725402, -149.8125000000000000, 5.149110718188524949 ) ) ;
#54356 = ORIENTED_EDGE ( 'NONE', *, *, #61818, .F. ) ;
#54357 = DIRECTION ( 'NONE',  ( 0.000000000000000000, 1.000000000000000000, 0.000000000000000000 ) ) ;
#54358 = CARTESIAN_POINT ( 'NONE',  ( 2.229367062500001939, 28.77083333469892779, 3.861377020970579999 ) ) ;
#54359 = CARTESIAN_POINT ( 'NONE',  ( -58.80597590150559739, -151.1250000027312126, 3.242614290531460330 ) ) ;
#54360 = CIRCLE ( 'NONE', #47205, 5.000000000000000000 ) ;
#54361 =( BOUNDED_CURVE ( )  B_SPLINE_CURVE ( 2, ( #26390, #31524, #35404, #26074, #40229, #1973, #50192, #41170, #51166 ),
 .UNSPECIFIED., .F., .F. ) 
 B_SPLINE_CURVE_WITH_KNOTS ( ( 3, 2, 2, 2, 3 ),
 ( 0.5645833333333333259, 0.5652777777777777679, 0.5666666666666666519, 0.5680555555555555358, 0.5687499999999999778 ),
 .UNSPECIFIED. ) 
 CURVE ( )  GEOMETRIC_REPRESENTATION_ITEM ( )  RATIONAL_B_SPLINE_CURVE ( ( 0.9330127018922194093, 0.9330127018922194093, 1.000000000000000000, 0.8660254037844387076, 1.000000000000000000, 0.8660254037844387076, 1.000000000000000000, 0.9330127018922194093, 0.9330127018922194093 ) ) 
 REPRESENTATION_ITEM ( '' )  );
#54362 = CARTESIAN_POINT ( 'NONE',  ( -6.972266317189433020E-16, -30.25000000000000000, -5.000000000000000000 ) ) ;
#54363 = VECTOR ( 'NONE', #63377, 1000.000000000000000 ) ;
#54364 = ORIENTED_EDGE ( 'NONE', *, *, #46874, .F. ) ;
#54365 = CARTESIAN_POINT ( 'NONE',  ( 4.458734124999999437, 5.187500001365596525, -5.460374474430324690E-16 ) ) ;
#54366 = CARTESIAN_POINT ( 'NONE',  ( 5.000000000000000000, -19.41666666666666785, -2.886751345948130876 ) ) ;
#54367 = CARTESIAN_POINT ( 'NONE',  ( 4.458734125000001214, -19.14583333196774007, 2.574251347313718519 ) ) ;
#54368 = LINE ( 'NONE', #54033, #10702 ) ;
#54369 = CARTESIAN_POINT ( 'NONE',  ( 4.458734124999998549, -4.729166665301071326, -2.574251347313721627 ) ) ;
#54370 = CARTESIAN_POINT ( 'NONE',  ( 1.975475456537005874E-15, 1.250000000000000000, 5.000000000000000000 ) ) ;
#54371 = CARTESIAN_POINT ( 'NONE',  ( 3.152801135295367541, -149.3125000013655779, -3.152801135295367541 ) ) ;
#54372 = CARTESIAN_POINT ( 'NONE',  ( -3.152548672688508926E-16, 20.18750000136559208, -5.148502694627439702 ) ) ;
#54373 = VERTEX_POINT ( 'NONE', #19330 ) ;
#54374 = CARTESIAN_POINT ( 'NONE',  ( 4.458734125000000326, -99.89583333196773651, 2.574251347313718519 ) ) ;
#54375 = DIRECTION ( 'NONE',  ( -0.000000000000000000, 1.000000000000000000, -0.000000000000000000 ) ) ;
#54376 = CARTESIAN_POINT ( 'NONE',  ( -6.972266317189433020E-16, -40.24999999999999289, -5.000000000000000000 ) ) ;
#54377 = CARTESIAN_POINT ( 'NONE',  ( 2.229367062500001939, -13.97916666530107221, 3.861377020970579999 ) ) ;
#54378 = CARTESIAN_POINT ( 'NONE',  ( 7.500000000000000000, 4.330127018922199866, -1.000000000000000888 ) ) ;
#54379 = CARTESIAN_POINT ( 'NONE',  ( 6.123233995736766282E-16, -120.0000000000000000, -5.000000000000000000 ) ) ;
#54380 = CARTESIAN_POINT ( 'NONE',  ( -50.70258187064364108, -150.1250000013656063, 2.196230717870141014 ) ) ;
#54381 = CARTESIAN_POINT ( 'NONE',  ( -3.535250795749689387E-16, -39.12499999726880162, -5.773502691896257311 ) ) ;
#54382 = CARTESIAN_POINT ( 'NONE',  ( -6.972266317189433020E-16, -67.12499999726881583, -5.000000000000000000 ) ) ;
#54383 = CARTESIAN_POINT ( 'NONE',  ( 4.458734124999998549, 11.27083333469893134, -2.574251347313721627 ) ) ;
#54384 = CARTESIAN_POINT ( 'NONE',  ( 1.975475456537005874E-15, -89.62499999726880162, 5.000000000000000000 ) ) ;
#54385 = CYLINDRICAL_SURFACE ( 'NONE', #22288, 5.000000000000000000 ) ;
#54386 = CARTESIAN_POINT ( 'NONE',  ( -4.458734124999999437, 16.68750000136559564, 0.000000000000000000 ) ) ;
#54387 = CARTESIAN_POINT ( 'NONE',  ( 9.457646018065525792E-16, -60.06249999863440792, 5.148502694627439702 ) ) ;
#54388 = ORIENTED_EDGE ( 'NONE', *, *, #51926, .F. ) ;
#54389 = CARTESIAN_POINT ( 'NONE',  ( 2.229367062499998831, -8.895833331967736513, -3.861377020970580887 ) ) ;
#54390 = CARTESIAN_POINT ( 'NONE',  ( 5.000000000000000000, 6.499999999999999112, -6.123233995736766282E-16 ) ) ;
#54391 = CARTESIAN_POINT ( 'NONE',  ( 3.535533905932736864, -139.2500000027311842, 3.535533905932738641 ) ) ;
#54392 = CARTESIAN_POINT ( 'NONE',  ( -6.972266317189433020E-16, -60.12499999726880873, -5.000000000000000000 ) ) ;
#54393 = CARTESIAN_POINT ( 'NONE',  ( 4.458734124999998549, -52.72916666530107221, -2.574251347313721627 ) ) ;
#54394 = CARTESIAN_POINT ( 'NONE',  ( -5.000000000000000000, -88.95833333060214443, -2.886751345948128211 ) ) ;
#54395 = CARTESIAN_POINT ( 'NONE',  ( 4.458734124999998549, -31.72916666530107577, -2.574251347313721627 ) ) ;
#54396 = CARTESIAN_POINT ( 'NONE',  ( -4.458734124999999437, -90.56249999863440792, 0.000000000000000000 ) ) ;
#54397 = CARTESIAN_POINT ( 'NONE',  ( 1.975475456537005874E-15, -8.750000000000000000, 5.000000000000000000 ) ) ;
#54398 = CARTESIAN_POINT ( 'NONE',  ( -3.152801135295367096, -155.3125000013656063, -3.152801135295367541 ) ) ;
#54399 = CARTESIAN_POINT ( 'NONE',  ( 5.000000000000000888, -45.58333333333333570, 2.886751345948126879 ) ) ;
#54400 = CARTESIAN_POINT ( 'NONE',  ( 5.000000000000000000, -46.41666666666666430, -2.886751345948130876 ) ) ;
#54401 = CARTESIAN_POINT ( 'NONE',  ( -58.89445808962354079, -135.0000000000000000, -2.539947039722357580 ) ) ;
#54402 = EDGE_LOOP ( 'NONE', ( #23669, #14157, #33603, #58373 ) ) ;
#54403 = CARTESIAN_POINT ( 'NONE',  ( 4.458734124999999437, -102.8124999986344079, -5.460374474430324690E-16 ) ) ;
#54404 = CARTESIAN_POINT ( 'NONE',  ( -4.458734124999999437, 4.437500001365595637, 0.000000000000000000 ) ) ;
#54405 = CARTESIAN_POINT ( 'NONE',  ( 0.000000000000000000, -170.0000000000000000, 0.000000000000000000 ) ) ;
#54406 = CARTESIAN_POINT ( 'NONE',  ( -4.999999999999999112, -3.916666666666665630, 2.886751345948131764 ) ) ;
#54407 = AXIS2_PLACEMENT_3D ( 'NONE', #3388, #43227, #27496 ) ;
#54408 = CARTESIAN_POINT ( 'NONE',  ( -2.229367062500000163, -69.47916666530107932, -3.861377020970580443 ) ) ;
#54409 = CARTESIAN_POINT ( 'NONE',  ( 6.123233995736765296E-16, 0.000000000000000000, -4.999999999999999112 ) ) ;
#54410 = CARTESIAN_POINT ( 'NONE',  ( 1.060575238724906964E-15, -3.624999997268816276, 5.773502691896257311 ) ) ;
#54412 = ORIENTED_EDGE ( 'NONE', *, *, #50683, .T. ) ;
#54411 = CARTESIAN_POINT ( 'NONE',  ( -4.458734124999998549, -35.22916666530107221, 2.574251347313722516 ) ) ;
#54413 = CARTESIAN_POINT ( 'NONE',  ( 1.339745962155615144, -33.70534180126148271, 4.999999999999999112 ) ) ;
#54414 = CARTESIAN_POINT ( 'NONE',  ( 5.000000000000000888, 19.41666666666666785, 2.886751345948126879 ) ) ;
#54415 = VERTEX_POINT ( 'NONE', #19012 ) ;
#54416 = CARTESIAN_POINT ( 'NONE',  ( -5.147856630858197489E-14, 3.249999999999997335, 5.000000000000000000 ) ) ;
#54417 = CARTESIAN_POINT ( 'NONE',  ( -3.535250795749689387E-16, -51.25000000000000000, -5.773502691896257311 ) ) ;
#54418 = ADVANCED_FACE ( 'NONE', ( #5181 ), #58885, .T. ) ;
#54420 = CARTESIAN_POINT ( 'NONE',  ( -2.229367062499996610, -23.39583333196773651, 3.861377020970582219 ) ) ;
#54419 = CARTESIAN_POINT ( 'NONE',  ( 5.000000000000000000, -17.37499999726881583, -6.123233995736766282E-16 ) ) ;
#54421 = CARTESIAN_POINT ( 'NONE',  ( -4.999999999999998224, -41.79166666393548013, 2.886751345948131764 ) ) ;
#54422 = CARTESIAN_POINT ( 'NONE',  ( 4.458734125000001214, -72.89583333196775072, 2.574251347313718519 ) ) ;
#54423 = CARTESIAN_POINT ( 'NONE',  ( 1.846868145590735200, -142.5000000013656347, -4.458734125000000326 ) ) ;
#54424 = CARTESIAN_POINT ( 'NONE',  ( 2.229367062499998831, -81.64583333196773651, -3.861377020970580887 ) ) ;
#54425 = CARTESIAN_POINT ( 'NONE',  ( -55.35523342533222291, -138.5625000013656063, 4.444560631937231499 ) ) ;
#54426 = CARTESIAN_POINT ( 'NONE',  ( 4.458734124999999437, -31.06249999863440436, -5.460374474430324690E-16 ) ) ;
#54427 = CARTESIAN_POINT ( 'NONE',  ( 2.499999999999998668, -69.20833333060214443, -4.330127018922193649 ) ) ;
#54428 = EDGE_CURVE ( 'NONE', #39986, #56905, #53968, .T. ) ;
#54429 = EDGE_LOOP ( 'NONE', ( #34594, #13620, #20094, #2777 ) ) ;
#54430 = CARTESIAN_POINT ( 'NONE',  ( -1.127183054612291972E-14, 24.37500000273118417, 4.999999999999999112 ) ) ;
#54431 = ORIENTED_EDGE ( 'NONE', *, *, #11031, .T. ) ;
#54432 = CARTESIAN_POINT ( 'NONE',  ( 2.229367062500001939, -72.22916666530107932, 3.861377020970579999 ) ) ;
#54433 = CARTESIAN_POINT ( 'NONE',  ( -6.972266317189433020E-16, -21.24999999999999289, -5.000000000000000000 ) ) ;
#54434 = SURFACE_STYLE_USAGE ( .BOTH. , #4275 ) ;
#54435 = ORIENTED_EDGE ( 'NONE', *, *, #43018, .F. ) ;
#54436 = CARTESIAN_POINT ( 'NONE',  ( -49.85088928181150436, -140.5625000000000284, -1.666127454062680480 ) ) ;
#54437 = CARTESIAN_POINT ( 'NONE',  ( 0.000000000000000000, 30.00000000000000000, 0.000000000000000000 ) ) ;
#54438 = CARTESIAN_POINT ( 'NONE',  ( 2.229367062500001939, -58.22916666530107932, 3.861377020970579999 ) ) ;
#54439 = CARTESIAN_POINT ( 'NONE',  ( -2.229367062500000163, -5.729166665301072214, -3.861377020970580443 ) ) ;
#54440 = ORIENTED_EDGE ( 'NONE', *, *, #5364, .T. ) ;
#54441 =( BOUNDED_CURVE ( )  B_SPLINE_CURVE ( 2, ( #40487, #55625, #40174, #36310, #630, #39842, #25380, #30516, #41118 ),
 .UNSPECIFIED., .F., .F. ) 
 B_SPLINE_CURVE_WITH_KNOTS ( ( 3, 2, 2, 2, 3 ),
 ( 0.1267857142857142794, 0.1273809523809523725, 0.1285714285714285587, 0.1297619047619047727, 0.1303571428571428659 ),
 .UNSPECIFIED. ) 
 CURVE ( )  GEOMETRIC_REPRESENTATION_ITEM ( )  RATIONAL_B_SPLINE_CURVE ( ( 0.9330127018922194093, 0.9330127018922194093, 1.000000000000000000, 0.8660254037844387076, 1.000000000000000000, 0.8660254037844387076, 1.000000000000000000, 0.9330127018922194093, 0.9330127018922194093 ) ) 
 REPRESENTATION_ITEM ( '' )  );
#54442 = DIRECTION ( 'NONE',  ( -0.000000000000000000, 1.000000000000000000, -0.000000000000000000 ) ) ;
#54443 = DIRECTION ( 'NONE',  ( -0.000000000000000000, 1.000000000000000000, -0.000000000000000000 ) ) ;
#54444 = CARTESIAN_POINT ( 'NONE',  ( 2.229367062500001939, 12.02083333469892601, 3.861377020970579999 ) ) ;
#54445 = CARTESIAN_POINT ( 'NONE',  ( -55.35523342533222291, -140.3125000013656063, 4.444560631937231499 ) ) ;
#54446 = CARTESIAN_POINT ( 'NONE',  ( 2.500000000000002220, -47.54166666393547303, 4.330127018922192761 ) ) ;
#54447 = CARTESIAN_POINT ( 'NONE',  ( 3.152801135295366208, -160.5625000013656063, 3.152801135295367985 ) ) ;
#54448 = ORIENTED_EDGE ( 'NONE', *, *, #59868, .F. ) ;
#54449 = CARTESIAN_POINT ( 'NONE',  ( 4.458734124999998549, -79.72916666530106511, -2.574251347313721627 ) ) ;
#54450 = LINE ( 'NONE', #10378, #6906 ) ;
#54451 = CARTESIAN_POINT ( 'NONE',  ( -4.458734124999998549, 1.770833334698927786, 2.574251347313722516 ) ) ;
#54452 = VECTOR ( 'NONE', #51806, 1000.000000000000000 ) ;
#54453 =( BOUNDED_CURVE ( )  B_SPLINE_CURVE ( 2, ( #7673, #31458, #21513, #26647, #51416, #46267, #21830, #41740, #47221 ),
 .UNSPECIFIED., .F., .F. ) 
 B_SPLINE_CURVE_WITH_KNOTS ( ( 3, 2, 2, 2, 3 ),
 ( 0.1482142857142857151, 0.1488095238095238082, 0.1499999999999999944, 0.1511904761904761807, 0.1517857142857143016 ),
 .UNSPECIFIED. ) 
 CURVE ( )  GEOMETRIC_REPRESENTATION_ITEM ( )  RATIONAL_B_SPLINE_CURVE ( ( 0.9330127018922194093, 0.9330127018922194093, 1.000000000000000000, 0.8660254037844387076, 1.000000000000000000, 0.8660254037844387076, 1.000000000000000000, 0.9330127018922178550, 0.9330127018922194093 ) ) 
 REPRESENTATION_ITEM ( '' )  );
#54454 = CARTESIAN_POINT ( 'NONE',  ( -5.000000000000000000, -87.08333333333331439, -2.886751345948128211 ) ) ;
#54455 = CARTESIAN_POINT ( 'NONE',  ( 1.339745962155615144, 4.419658201469705894, 4.999999999999999112 ) ) ;
#54456 = CARTESIAN_POINT ( 'NONE',  ( -4.458734124999999437, -64.64583333196772230, -2.574251347313719407 ) ) ;
#54457 = CARTESIAN_POINT ( 'NONE',  ( 5.000000000000000888, -24.45833333060214088, 2.886751345948126879 ) ) ;
#54458 = CARTESIAN_POINT ( 'NONE',  ( -1.339745962155613812, 5.794658198738519950, -5.000000000000000000 ) ) ;
#54459 = CARTESIAN_POINT ( 'NONE',  ( 2.229367062499998831, 27.35416666803225993, -3.861377020970580887 ) ) ;
#54460 = FACE_OUTER_BOUND ( 'NONE', #15513, .T. ) ;
#54461 = PRESENTATION_STYLE_ASSIGNMENT (( #58330 ) ) ;
#54462 = CARTESIAN_POINT ( 'NONE',  ( 2.229367062499998831, -48.64583333196772941, -3.861377020970580887 ) ) ;
#54463 = CARTESIAN_POINT ( 'NONE',  ( -2.229367062499996610, -31.39583333196773651, 3.861377020970582219 ) ) ;
#54464 = CARTESIAN_POINT ( 'NONE',  ( 2.229367062500001939, 5.770833334698927786, 3.861377020970579999 ) ) ;
#54465 = CARTESIAN_POINT ( 'NONE',  ( -6.972266317189433020E-16, -10.12499999726881406, -5.000000000000000000 ) ) ;
#54466 = CARTESIAN_POINT ( 'NONE',  ( -2.499999999999996447, 20.16666666666666430, 4.330127018922195425 ) ) ;
#54467 = CARTESIAN_POINT ( 'NONE',  ( -2.071067811865475061, -148.8125000027312126, -5.000000000000000888 ) ) ;
#54468 = DIRECTION ( 'NONE',  ( -0.000000000000000000, 1.000000000000000000, -0.000000000000000000 ) ) ;
#54469 = CARTESIAN_POINT ( 'NONE',  ( -2.229367062500000163, -37.47916666530107221, -3.861377020970580443 ) ) ;
#54470 = CARTESIAN_POINT ( 'NONE',  ( -2.500000000000000444, -74.04166666393547303, -4.330127018922193649 ) ) ;
#54471 = CARTESIAN_POINT ( 'NONE',  ( -59.59170313451811296, -143.7500000013656063, 1.485763867205729394 ) ) ;
#54472 = DIRECTION ( 'NONE',  ( 0.000000000000000000, 1.000000000000000000, 0.000000000000000000 ) ) ;
#54473 = CARTESIAN_POINT ( 'NONE',  ( 5.000000000000000000, -15.29166666393548191, -2.886751345948130876 ) ) ;
#54474 = CARTESIAN_POINT ( 'NONE',  ( -2.229367062500000163, -82.72916666530106511, -3.861377020970580443 ) ) ;
#54475 = CARTESIAN_POINT ( 'NONE',  ( -4.458734124999999437, -164.1875000013655779, -5.460374474430324690E-16 ) ) ;
#54476 = CARTESIAN_POINT ( 'NONE',  ( -4.999999999999998224, -32.91666666666666430, 2.886751345948131764 ) ) ;
#54477 = DIRECTION ( 'NONE',  ( -0.000000000000000000, 1.000000000000000000, -0.000000000000000000 ) ) ;
#54478 = CARTESIAN_POINT ( 'NONE',  ( 2.500000000000002220, -25.66666666666666430, 4.330127018922192761 ) ) ;
#54479 = CARTESIAN_POINT ( 'NONE',  ( 2.730187237215162345E-16, -144.1875000013656063, -4.458734124999999437 ) ) ;
#54480 = ORIENTED_EDGE ( 'NONE', *, *, #16043, .T. ) ;
#54481 = CARTESIAN_POINT ( 'NONE',  ( -5.000000000000000000, -89.95833333060214443, -2.886751345948128211 ) ) ;
#54482 = ORIENTED_EDGE ( 'NONE', *, *, #98, .F. ) ;
#54483 = CARTESIAN_POINT ( 'NONE',  ( 4.458734124999999437, -63.06249999863440792, -5.460374474430324690E-16 ) ) ;
#54484 = CARTESIAN_POINT ( 'NONE',  ( 5.000000000000000000, 19.70833333606451987, -2.886751345948129988 ) ) ;
#54485 = CYLINDRICAL_SURFACE ( 'NONE', #13453, 5.000000000000000000 ) ;
#54486 = CARTESIAN_POINT ( 'NONE',  ( -2.499999999999996447, 16.16666666666666430, 4.330127018922195425 ) ) ;
#54487 = CARTESIAN_POINT ( 'NONE',  ( 9.457646018065525792E-16, -49.06249999863440792, 5.148502694627439702 ) ) ;
#54488 = CARTESIAN_POINT ( 'NONE',  ( 4.458734124999998549, -4.729166665301071326, -2.574251347313721627 ) ) ;
#54489 = CARTESIAN_POINT ( 'NONE',  ( -9.184850993605147944E-16, -166.3750000027312126, 5.000000000000000000 ) ) ;
#54490 = CARTESIAN_POINT ( 'NONE',  ( 3.535533905932736864, -165.2500000027312126, 3.535533905932738641 ) ) ;
#54491 = CARTESIAN_POINT ( 'NONE',  ( 3.535533905932738197, -158.0000000027312126, -3.535533905932738197 ) ) ;
#54492 = CARTESIAN_POINT ( 'NONE',  ( -50.01589407740564042, -144.7500000027312126, 0.3983568153799778022 ) ) ;
#54493 = CARTESIAN_POINT ( 'NONE',  ( -5.000000000000000000, -10.00000000000000178, 0.000000000000000000 ) ) ;
#54494 = AXIS2_PLACEMENT_3D ( 'NONE', #63097, #12927, #19009 ) ;
#54496 = CARTESIAN_POINT ( 'NONE',  ( 2.229367062499998831, -20.64583333196774007, -3.861377020970580887 ) ) ;
#54495 = CARTESIAN_POINT ( 'NONE',  ( -2.499999999999996447, -78.83333333333332860, 4.330127018922195425 ) ) ;
#54497 = CARTESIAN_POINT ( 'NONE',  ( -50.18089887299980489, -135.8125000027311557, 2.462841084822814164 ) ) ;
#54498 = CARTESIAN_POINT ( 'NONE',  ( 4.458734124999999437, -51.81249999863440792, -5.460374474430324690E-16 ) ) ;
#54499 = CARTESIAN_POINT ( 'NONE',  ( -4.458734125000001214, -154.1250000013656063, 1.846868145590734089 ) ) ;
#54500 = VECTOR ( 'NONE', #10954, 1000.000000000000000 ) ;
#54501 = CARTESIAN_POINT ( 'NONE',  ( -4.999999999999999112, -54.79166666393547303, 2.886751345948131764 ) ) ;
#54502 = ORIENTED_EDGE ( 'NONE', *, *, #59861, .F. ) ;
#54503 = CARTESIAN_POINT ( 'NONE',  ( -56.66612745406293783, -137.3125000000000000, -5.149110718188535607 ) ) ;
#54504 = CARTESIAN_POINT ( 'NONE',  ( -2.229367062500000163, 4.270833334698926897, -3.861377020970580443 ) ) ;
#54505 = VERTEX_POINT ( 'NONE', #39576 ) ;
#54507 = CARTESIAN_POINT ( 'NONE',  ( 1.975475456537005874E-15, -2.750000000000000888, 5.000000000000000000 ) ) ;
#54506 = DIRECTION ( 'NONE',  ( -1.000000000000000000, 0.000000000000000000, 0.000000000000000000 ) ) ;
#54508 = CARTESIAN_POINT ( 'NONE',  ( 4.458734125000000326, -157.3750000013656347, -1.846868145590734978 ) ) ;
#54509 = ORIENTED_EDGE ( 'NONE', *, *, #1565, .F. ) ;
#54510 =( BOUNDED_CURVE ( )  B_SPLINE_CURVE ( 2, ( #19320, #14178, #28967, #33805, #9355, #4531, #38936, #14491, #49547 ),
 .UNSPECIFIED., .F., .F. ) 
 B_SPLINE_CURVE_WITH_KNOTS ( ( 3, 2, 2, 2, 3 ),
 ( 0.1196428571428571480, 0.1202380952380952411, 0.1214285714285714274, 0.1226190476190476136, 0.1232142857142857206 ),
 .UNSPECIFIED. ) 
 CURVE ( )  GEOMETRIC_REPRESENTATION_ITEM ( )  RATIONAL_B_SPLINE_CURVE ( ( 0.9330127018922192983, 0.9330127018922200755, 1.000000000000000000, 0.8660254037844387076, 1.000000000000000000, 0.8660254037844387076, 1.000000000000000000, 0.9330127018922185211, 0.9330127018922192983 ) ) 
 REPRESENTATION_ITEM ( '' )  );
#54511 = CARTESIAN_POINT ( 'NONE',  ( -51.75738570946856498, -140.8750000027312126, 3.805975901505576964 ) ) ;
#54512 = CARTESIAN_POINT ( 'NONE',  ( -54.60164318462004474, -128.3750000000000284, -4.984105922594373794 ) ) ;
#54513 = CARTESIAN_POINT ( 'NONE',  ( -6.972266317189433020E-16, -47.25000000000000000, -5.000000000000000000 ) ) ;
#54514 = CARTESIAN_POINT ( 'NONE',  ( 9.457646018065525792E-16, -43.31249999863440792, 5.148502694627439702 ) ) ;
#54515 = VERTEX_POINT ( 'NONE', #29283 ) ;
#54516 = CARTESIAN_POINT ( 'NONE',  ( 5.275681513340003914E-14, 9.875000002731184168, -5.000000000000000000 ) ) ;
#54517 = CARTESIAN_POINT ( 'NONE',  ( -3.152548672688508926E-16, 13.43750000136559386, -5.148502694627439702 ) ) ;
#54518 = CARTESIAN_POINT ( 'NONE',  ( -3.152548672688508926E-16, 27.43750000136559564, -5.148502694627439702 ) ) ;
#54519 = CARTESIAN_POINT ( 'NONE',  ( -50.70258187064364108, -153.1250000013656063, 2.196230717870141014 ) ) ;
#54520 = CARTESIAN_POINT ( 'NONE',  ( 2.499999999999998668, -44.33333333333333570, -4.330127018922193649 ) ) ;
#54521 = CARTESIAN_POINT ( 'NONE',  ( -5.000000000000000000, -35.95833333060213732, -2.886751345948128211 ) ) ;
#54522 = CARTESIAN_POINT ( 'NONE',  ( -6.972266317189433020E-16, -15.25000000000000000, -5.000000000000000000 ) ) ;
#54523 = CARTESIAN_POINT ( 'NONE',  ( 4.458734124999999437, -63.81249999863440792, -5.460374474430324690E-16 ) ) ;
#54524 = FACE_OUTER_BOUND ( 'NONE', #13914, .T. ) ;
#54525 = CARTESIAN_POINT ( 'NONE',  ( 2.229367062499998831, 17.35416666803225993, -3.861377020970580887 ) ) ;
#54526 = EDGE_CURVE ( 'NONE', #11325, #43978, #21499, .T. ) ;
#54527 = CARTESIAN_POINT ( 'NONE',  ( -4.999999999999998224, 7.083333333333333925, 2.886751345948131764 ) ) ;
#54528 = CARTESIAN_POINT ( 'NONE',  ( -4.458734124999998549, -50.47916666530107221, 2.574251347313722516 ) ) ;
#54529 = CARTESIAN_POINT ( 'NONE',  ( 5.000000000000000000, -7.291666663935481907, -2.886751345948129988 ) ) ;
#54530 = CARTESIAN_POINT ( 'NONE',  ( -5.000000000000000000, -109.0833333333333428, -2.886751345948128211 ) ) ;
#54531 = CYLINDRICAL_SURFACE ( 'NONE', #29613, 5.000000000000000000 ) ;
#54532 = CARTESIAN_POINT ( 'NONE',  ( -58.80597590150559739, -155.0000000000000284, 3.242614290531457666 ) ) ;
#54533 = CARTESIAN_POINT ( 'NONE',  ( 0.000000000000000000, -170.0000000000000000, 0.000000000000000000 ) ) ;
#54534 =( BOUNDED_CURVE ( )  B_SPLINE_CURVE ( 2, ( #835, #16252, #35872, #11415, #35551, #30720, #50343, #15613, #54850 ),
 .UNSPECIFIED., .F., .F. ) 
 B_SPLINE_CURVE_WITH_KNOTS ( ( 3, 2, 2, 2, 3 ),
 ( 0.9517857142857142350, 0.9523809523809523281, 0.9535714285714286254, 0.9547619047619048116, 0.9553571428571429047 ),
 .UNSPECIFIED. ) 
 CURVE ( )  GEOMETRIC_REPRESENTATION_ITEM ( )  RATIONAL_B_SPLINE_CURVE ( ( 0.9330127018922194093, 0.9330127018922194093, 1.000000000000000000, 0.8660254037844387076, 1.000000000000000000, 0.8660254037844387076, 1.000000000000000000, 0.9330127018922194093, 0.9330127018922194093 ) ) 
 REPRESENTATION_ITEM ( '' )  );
#54535 = CARTESIAN_POINT ( 'NONE',  ( -2.229367062500000163, -15.72916666530107399, -3.861377020970580443 ) ) ;
#54536 = ORIENTED_EDGE ( 'NONE', *, *, #6272, .T. ) ;
#54537 = CARTESIAN_POINT ( 'NONE',  ( 4.458734124999999437, -104.8124999986344079, -5.460374474430324690E-16 ) ) ;
#54538 = CARTESIAN_POINT ( 'NONE',  ( 3.535533905932738197, -160.0000000027312126, -3.535533905932738197 ) ) ;
#54539 = ORIENTED_EDGE ( 'NONE', *, *, #12559, .T. ) ;
#54540 = CARTESIAN_POINT ( 'NONE',  ( -4.458734124999999437, -96.56249999863440792, 0.000000000000000000 ) ) ;
#54541 = CARTESIAN_POINT ( 'NONE',  ( -4.999999999999998224, 22.08333333333333215, 2.886751345948131764 ) ) ;
#54542 = CARTESIAN_POINT ( 'NONE',  ( 2.500000000000002220, -58.54166666393548013, 4.330127018922192761 ) ) ;
#54543 = CARTESIAN_POINT ( 'NONE',  ( -50.70258187064364108, -127.1250000013656205, 2.196230717870141014 ) ) ;
#54544 = CARTESIAN_POINT ( 'NONE',  ( -57.19623071787016499, -142.3750000013656063, 4.297418129356382899 ) ) ;
#54545 = CARTESIAN_POINT ( 'NONE',  ( -4.458734124999999437, -18.39583333196774007, -2.574251347313719407 ) ) ;
#54546 = CARTESIAN_POINT ( 'NONE',  ( -3.152548672688508926E-16, 7.187500001365594748, -5.148502694627439702 ) ) ;
#54547 = CARTESIAN_POINT ( 'NONE',  ( -2.229367062499996610, -63.39583333196774362, 3.861377020970582219 ) ) ;
#54548 = CARTESIAN_POINT ( 'NONE',  ( -5.000000000000000000, -141.6250000027312126, -6.123233995736766282E-16 ) ) ;
#54549 = CARTESIAN_POINT ( 'NONE',  ( -4.458734124999997661, -19.22916666530106866, 2.574251347313722516 ) ) ;
#54550 = CYLINDRICAL_SURFACE ( 'NONE', #53765, 5.000000000000000000 ) ;
#54551 = CARTESIAN_POINT ( 'NONE',  ( -3.535533905932737309, -156.6250000000000000, -3.535533905932738197 ) ) ;
#54552 = CARTESIAN_POINT ( 'NONE',  ( 2.500000000000002220, -9.666666666666664298, 4.330127018922192761 ) ) ;
#54553 = CARTESIAN_POINT ( 'NONE',  ( -3.152801135295367985, -157.8125000013656063, 3.152801135295367096 ) ) ;
#54554 = VERTEX_POINT ( 'NONE', #60181 ) ;
#54555 = CARTESIAN_POINT ( 'NONE',  ( -4.458734124999999437, -44.56249999863440081, 0.000000000000000000 ) ) ;
#54556 = CARTESIAN_POINT ( 'NONE',  ( 5.000000000000000000, -44.37499999726880873, -6.123233995736766282E-16 ) ) ;
#54557 = CARTESIAN_POINT ( 'NONE',  ( -5.000000000000000000, -91.87499999726880162, 0.000000000000000000 ) ) ;
#54558 = CARTESIAN_POINT ( 'NONE',  ( 2.229367062499998831, -88.64583333196773651, -3.861377020970580887 ) ) ;
#54559 = CARTESIAN_POINT ( 'NONE',  ( 4.458734124999999437, -90.81249999863440792, -5.460374474430324690E-16 ) ) ;
#54560 = CARTESIAN_POINT ( 'NONE',  ( -4.458734124999998549, 15.52083333469892779, 2.574251347313722516 ) ) ;
#54561 = CARTESIAN_POINT ( 'NONE',  ( -3.152548672688508926E-16, 10.43750000136559386, -5.148502694627439702 ) ) ;
#54562 = CARTESIAN_POINT ( 'NONE',  ( 5.000000000000000888, -82.58333333333334281, 2.886751345948126879 ) ) ;
#54563 = DIRECTION ( 'NONE',  ( 0.000000000000000000, 0.000000000000000000, 1.000000000000000000 ) ) ;
#54564 = CARTESIAN_POINT ( 'NONE',  ( -4.403473400622099909, -6.117907484625868975, -5.839445138371144960E-15 ) ) ;
#54565 = CARTESIAN_POINT ( 'NONE',  ( 4.458734124999998549, 20.02083333469892779, -2.574251347313721627 ) ) ;
#54566 = CARTESIAN_POINT ( 'NONE',  ( 5.000000000000000000, -74.41666666666665719, -2.886751345948129988 ) ) ;
#54567 = CARTESIAN_POINT ( 'NONE',  ( 2.500000000000002220, 6.458333336064519870, 4.330127018922192761 ) ) ;
#54568 = EDGE_LOOP ( 'NONE', ( #47292, #16436, #6111, #50569, #29010, #25486, #18646, #51214 ) ) ;
#54569 = CARTESIAN_POINT ( 'NONE',  ( 5.000000000000000000, -80.37499999726881583, -6.123233995736766282E-16 ) ) ;
#54570 = ORIENTED_EDGE ( 'NONE', *, *, #28773, .T. ) ;
#54571 = DIRECTION ( 'NONE',  ( -0.000000000000000000, 1.000000000000000000, -0.000000000000000000 ) ) ;
#54572 = CARTESIAN_POINT ( 'NONE',  ( -3.152548672688508926E-16, -37.56249999863440792, -5.148502694627439702 ) ) ;
#54573 = CARTESIAN_POINT ( 'NONE',  ( 5.000000000000000000, -38.29166666393548013, -2.886751345948129988 ) ) ;
#54574 = ORIENTED_EDGE ( 'NONE', *, *, #9536, .T. ) ;
#54575 = CARTESIAN_POINT ( 'NONE',  ( -4.458734124999998549, -10.22916666530106866, 2.574251347313722516 ) ) ;
#54577 = ORIENTED_EDGE ( 'NONE', *, *, #31974, .T. ) ;
#54576 = CARTESIAN_POINT ( 'NONE',  ( -2.229367062500000163, -20.72916666530107221, -3.861377020970580443 ) ) ;
#54578 = CARTESIAN_POINT ( 'NONE',  ( 5.000000000000000000, -84.49999999999998579, -6.123233995736766282E-16 ) ) ;
#54579 = CARTESIAN_POINT ( 'NONE',  ( -3.152801135295367096, -169.0625000013656063, -3.152801135295367541 ) ) ;
#54580 = CARTESIAN_POINT ( 'NONE',  ( 4.458734124999999437, -65.06249999863440792, -5.460374474430324690E-16 ) ) ;
#54581 = CARTESIAN_POINT ( 'NONE',  ( 5.000000000000000000, -86.37499999726880162, -6.123233995736766282E-16 ) ) ;
#54583 = VERTEX_POINT ( 'NONE', #16742 ) ;
#54582 = CARTESIAN_POINT ( 'NONE',  ( -6.972266317189433020E-16, -18.25000000000000000, -5.000000000000000000 ) ) ;
#54584 = VECTOR ( 'NONE', #43280, 1000.000000000000000 ) ;
#54585 = CARTESIAN_POINT ( 'NONE',  ( -53.33387254593733928, -141.8125000000000284, 5.149110718188519620 ) ) ;
#54586 = CARTESIAN_POINT ( 'NONE',  ( 9.457646018065525792E-16, -27.31249999863440436, 5.148502694627439702 ) ) ;
#54587 = CARTESIAN_POINT ( 'NONE',  ( 1.975475456537005874E-15, 7.375000002731185944, 5.000000000000000000 ) ) ;
#54588 = VERTEX_POINT ( 'NONE', #1018 ) ;
#54589 = ITEM_DEFINED_TRANSFORMATION ( 'NONE', 'NONE', #47251,  #43054 ) ;
#54590 = CARTESIAN_POINT ( 'NONE',  ( 1.846868145590736310, -162.8750000013655779, 4.458734124999999437 ) ) ;
#54591 = CARTESIAN_POINT ( 'NONE',  ( 4.458734124999998549, -109.9791666653010793, -2.574251347313721627 ) ) ;
#54592 = CARTESIAN_POINT ( 'NONE',  ( 5.000000000000000888, 20.41666666666666785, 2.886751345948126879 ) ) ;
#54593 = VERTEX_POINT ( 'NONE', #46328 ) ;
#54594 = CARTESIAN_POINT ( 'NONE',  ( -54.64476657466781973, -147.0625000013656063, -4.444560631937228834 ) ) ;
#54595 = CARTESIAN_POINT ( 'NONE',  ( -4.458734124999998549, -73.47916666530106511, 2.574251347313722516 ) ) ;
#54596 = CARTESIAN_POINT ( 'NONE',  ( -50.18089887299979068, -134.8125000027312126, 2.462841084822635640 ) ) ;
#54597 = CARTESIAN_POINT ( 'NONE',  ( 9.457646018065525792E-16, -43.06249999863440081, 5.148502694627439702 ) ) ;
#54598 = CARTESIAN_POINT ( 'NONE',  ( -4.458734124999999437, -147.2500000013656063, -1.846868145590735644 ) ) ;
#54599 = CARTESIAN_POINT ( 'NONE',  ( -5.000000000000000000, 23.00000000000000000, 0.000000000000000000 ) ) ;
#54600 = CARTESIAN_POINT ( 'NONE',  ( 4.458734124999998549, -49.72916666530107221, -2.574251347313721627 ) ) ;
#54601 = EDGE_CURVE ( 'NONE', #45912, #52441, #34615, .T. ) ;
#54602 = CARTESIAN_POINT ( 'NONE',  ( -2.229367062500000163, -12.47916666530107044, -3.861377020970580443 ) ) ;
#54603 = CARTESIAN_POINT ( 'NONE',  ( -2.500000000000000444, -102.1666666666666572, -4.330127018922193649 ) ) ;
#54604 = CARTESIAN_POINT ( 'NONE',  ( 3.152801135295367541, -141.5625000013655779, -3.152801135295367541 ) ) ;
#54605 = CARTESIAN_POINT ( 'NONE',  ( 9.457646018065525792E-16, -32.31249999863440792, 5.148502694627439702 ) ) ;
#54606 = CARTESIAN_POINT ( 'NONE',  ( -5.000000000000000000, 4.125000002731186832, 0.000000000000000000 ) ) ;
#54607 = CARTESIAN_POINT ( 'NONE',  ( -2.500000000000000444, -7.041666663935481907, -4.330127018922193649 ) ) ;
#54608 = CARTESIAN_POINT ( 'NONE',  ( -50.55543936806279248, -130.0625000013656063, 0.3552334253322060320 ) ) ;
#54609 = CARTESIAN_POINT ( 'NONE',  ( 4.458734124999999437, -76.06249999863440792, -5.460374474430324690E-16 ) ) ;
#54610 = DIRECTION ( 'NONE',  ( -0.000000000000000000, 1.000000000000000000, -0.000000000000000000 ) ) ;
#54611 = CARTESIAN_POINT ( 'NONE',  ( 3.061616997868383141E-16, -149.8750000027312126, -5.000000000000000000 ) ) ;
#54612 = DIRECTION ( 'NONE',  ( -0.000000000000000000, 1.000000000000000000, -0.000000000000000000 ) ) ;
#54613 = CARTESIAN_POINT ( 'NONE',  ( -2.229367062499996610, -1.395833331967737179, 3.861377020970582219 ) ) ;
#54614 = ORIENTED_EDGE ( 'NONE', *, *, #9536, .F. ) ;
#54615 = CARTESIAN_POINT ( 'NONE',  ( 5.000000000000000000, 24.70833333606452342, -2.886751345948130876 ) ) ;
#54616 = CARTESIAN_POINT ( 'NONE',  ( -2.500000000000000444, -76.16666666666665719, -4.330127018922193649 ) ) ;
#54618 = CARTESIAN_POINT ( 'NONE',  ( -2.229367062499996610, -33.14583333196772941, 3.861377020970582219 ) ) ;
#54617 = CARTESIAN_POINT ( 'NONE',  ( -4.458734124999999437, -85.31249999863439371, 0.000000000000000000 ) ) ;
#54619 = EDGE_CURVE ( 'NONE', #15810, #35184, #20622, .T. ) ;
#54620 = CARTESIAN_POINT ( 'NONE',  ( 2.493747252781420335E-13, -77.25000000000001421, -5.000000000000000000 ) ) ;
#54621 = CARTESIAN_POINT ( 'NONE',  ( -2.229367062500000163, -83.72916666530106511, -3.861377020970580443 ) ) ;
#54622 = CARTESIAN_POINT ( 'NONE',  ( 4.458734124999998549, 18.02083333469892779, -2.574251347313721627 ) ) ;
#54623 = CARTESIAN_POINT ( 'NONE',  ( 0.000000000000000000, -120.0000000000000000, 0.000000000000000000 ) ) ;
#54624 = CARTESIAN_POINT ( 'NONE',  ( -56.48576386720575471, -136.7500000013655779, -4.591703134518078322 ) ) ;
#54625 = CARTESIAN_POINT ( 'NONE',  ( -4.458734124999999437, -1.395833331967737179, -2.574251347313719407 ) ) ;
#54626 = CARTESIAN_POINT ( 'NONE',  ( -4.458734124999999437, 20.35416666803225993, -2.574251347313719407 ) ) ;
#54627 = ADVANCED_FACE ( 'NONE', ( #36045 ), #43822, .T. ) ;
#54628 = CARTESIAN_POINT ( 'NONE',  ( 9.457646018065525792E-16, -48.31249999863440792, 5.148502694627439702 ) ) ;
#54629 = CARTESIAN_POINT ( 'NONE',  ( -2.499999999999996447, -45.70833333060214443, 4.330127018922195425 ) ) ;
#54630 = CARTESIAN_POINT ( 'NONE',  ( 2.229367062500001939, -5.979166665301072214, 3.861377020970579999 ) ) ;
#54631 = CARTESIAN_POINT ( 'NONE',  ( -2.229367062499996610, -31.39583333196773651, 3.861377020970582219 ) ) ;
#54632 = CARTESIAN_POINT ( 'NONE',  ( -50.70258187064364108, -131.3750000013656347, 2.196230717870141014 ) ) ;
#54633 = CARTESIAN_POINT ( 'NONE',  ( 2.229367062500001939, -74.97916666530106511, 3.861377020970579999 ) ) ;
#54634 = CARTESIAN_POINT ( 'NONE',  ( 5.000000000000000888, -104.4583333306021302, 2.886751345948126879 ) ) ;
#54635 =( BOUNDED_CURVE ( )  B_SPLINE_CURVE ( 2, ( #47029, #3294, #27717, #11646, #26775, #61835, #46394, #11966, #2342 ),
 .UNSPECIFIED., .F., .F. ) 
 B_SPLINE_CURVE_WITH_KNOTS ( ( 3, 2, 2, 2, 3 ),
 ( 0.9020833333333333481, 0.9027777777777777901, 0.9041666666666666741, 0.9055555555555555580, 0.9062500000000000000 ),
 .UNSPECIFIED. ) 
 CURVE ( )  GEOMETRIC_REPRESENTATION_ITEM ( )  RATIONAL_B_SPLINE_CURVE ( ( 0.9330127018922194093, 0.9330127018922194093, 1.000000000000000000, 0.8660254037844387076, 1.000000000000000000, 0.8660254037844387076, 1.000000000000000000, 0.9330127018922194093, 0.9330127018922194093 ) ) 
 REPRESENTATION_ITEM ( '' )  );
#54636 = CARTESIAN_POINT ( 'NONE',  ( -4.458734124999999437, 23.60416666803225993, -2.574251347313719407 ) ) ;
#54637 = CARTESIAN_POINT ( 'NONE',  ( 2.500000000000002220, -58.54166666393548013, 4.330127018922192761 ) ) ;
#54638 = DIRECTION ( 'NONE',  ( 0.000000000000000000, 0.000000000000000000, 1.000000000000000000 ) ) ;
#54639 = CARTESIAN_POINT ( 'NONE',  ( 4.458734124999999437, -79.06249999863440792, -5.460374474430324690E-16 ) ) ;
#54640 = CARTESIAN_POINT ( 'NONE',  ( 5.000000000000000888, -61.58333333333334281, 2.886751345948126879 ) ) ;
#54641 = CARTESIAN_POINT ( 'NONE',  ( -4.999999999999998224, -31.79166666393548724, 2.886751345948131764 ) ) ;
#54642 = CARTESIAN_POINT ( 'NONE',  ( -4.999999999999999112, 22.20833333606451987, 2.886751345948131764 ) ) ;
#54643 = ORIENTED_EDGE ( 'NONE', *, *, #43360, .F. ) ;
#54644 = DIRECTION ( 'NONE',  ( 0.000000000000000000, 0.000000000000000000, 1.000000000000000000 ) ) ;
#54645 = DIRECTION ( 'NONE',  ( 0.000000000000000000, 0.000000000000000000, 1.000000000000000000 ) ) ;
#54646 = CARTESIAN_POINT ( 'NONE',  ( -5.000000000000000000, -19.99999999999999645, 0.000000000000000000 ) ) ;
#54647 = CARTESIAN_POINT ( 'NONE',  ( 4.458734124999999437, -21.81249999863440436, -5.460374474430324690E-16 ) ) ;
#54648 = CARTESIAN_POINT ( 'NONE',  ( 4.458734124999998549, -80.72916666530106511, -2.574251347313721627 ) ) ;
#54649 = CARTESIAN_POINT ( 'NONE',  ( -2.500000000000000444, -24.04166666393548368, -4.330127018922193649 ) ) ;
#54650 = EDGE_CURVE ( 'NONE', #56115, #47088, #30895, .T. ) ;
#54652 = ORIENTED_EDGE ( 'NONE', *, *, #7863, .T. ) ;
#54651 = CARTESIAN_POINT ( 'NONE',  ( 4.458734125000001214, -51.89583333196773651, 2.574251347313718519 ) ) ;
#54653 = CARTESIAN_POINT ( 'NONE',  ( -5.000000000000000000, -75.95833333060214443, -2.886751345948128211 ) ) ;
#54654 = CYLINDRICAL_SURFACE ( 'NONE', #39518, 5.000000000000000000 ) ;
#54656 = ORIENTED_EDGE ( 'NONE', *, *, #25296, .F. ) ;
#54655 = CARTESIAN_POINT ( 'NONE',  ( -2.229367062499996610, 2.604166668032259491, 3.861377020970582219 ) ) ;
#54657 = CARTESIAN_POINT ( 'NONE',  ( -50.55543936806279248, -151.0625000013656063, 0.3552334253322060320 ) ) ;
#54658 = CARTESIAN_POINT ( 'NONE',  ( -2.500000000000000444, -68.16666666666667140, -4.330127018922193649 ) ) ;
#54659 = CARTESIAN_POINT ( 'NONE',  ( 2.730187237215162345E-16, -153.4375000013655779, -4.458734124999999437 ) ) ;
#54660 = CARTESIAN_POINT ( 'NONE',  ( -3.152548672688508926E-16, -46.81249999863440081, -5.148502694627439702 ) ) ;
#54661 = CARTESIAN_POINT ( 'NONE',  ( -6.972266317189433020E-16, -77.12499999726881583, -5.000000000000000000 ) ) ;
#54662 = CARTESIAN_POINT ( 'NONE',  ( 2.071067811865476394, -158.1875000000000000, 5.000000000000000000 ) ) ;
#54663 = DIRECTION ( 'NONE',  ( 0.000000000000000000, 1.000000000000000000, 0.000000000000000000 ) ) ;
#54664 = CARTESIAN_POINT ( 'NONE',  ( -58.39396692619412477, -126.6875000013656063, 2.891590998281057701 ) ) ;
#54665 = CARTESIAN_POINT ( 'NONE',  ( 9.457646018065525792E-16, -11.31249999863440792, 5.148502694627439702 ) ) ;
#54666 = CARTESIAN_POINT ( 'NONE',  ( -2.229367062500000163, -44.72916666530106511, -3.861377020970580443 ) ) ;
#54667 = CARTESIAN_POINT ( 'NONE',  ( -1.339745962155610925, -7.669658196007332229, 5.000000000000000000 ) ) ;
#54668 = CARTESIAN_POINT ( 'NONE',  ( 4.458734124999999437, -143.5000000013656063, 1.846868145590737864 ) ) ;
#54669 = CARTESIAN_POINT ( 'NONE',  ( -4.458734124999998549, -89.47916666530106511, 2.574251347313722516 ) ) ;
#54670 = CARTESIAN_POINT ( 'NONE',  ( -9.184850993605147944E-16, -151.3750000027311842, 5.000000000000000000 ) ) ;
#54671 = ORIENTED_EDGE ( 'NONE', *, *, #43417, .T. ) ;
#54672 = LINE ( 'NONE', #14, #31353 ) ;
#54673 = CARTESIAN_POINT ( 'NONE',  ( -4.458734124999998549, 28.52083333469892423, 2.574251347313722516 ) ) ;
#54674 = CARTESIAN_POINT ( 'NONE',  ( -50.18089887299979068, -146.8125000027311842, 2.462841084822635640 ) ) ;
#54675 = CARTESIAN_POINT ( 'NONE',  ( 5.000000000000000000, -30.50000000000000000, -6.123233995736766282E-16 ) ) ;
#54676 = VERTEX_POINT ( 'NONE', #12235 ) ;
#54677 = CARTESIAN_POINT ( 'NONE',  ( 2.229367062500001939, 5.020833334698926897, 3.861377020970579999 ) ) ;
#54678 = EDGE_CURVE ( 'NONE', #3563, #37393, #60498, .T. ) ;
#54679 = EDGE_CURVE ( 'NONE', #6968, #60408, #23176, .T. ) ;
#54680 = CARTESIAN_POINT ( 'NONE',  ( 2.499999999999998668, -106.3333333333333286, -4.330127018922193649 ) ) ;
#54681 = CARTESIAN_POINT ( 'NONE',  ( -3.152548672688508926E-16, -16.81249999863440436, -5.148502694627439702 ) ) ;
#54682 =( BOUNDED_CURVE ( )  B_SPLINE_CURVE ( 2, ( #38285, #13532, #24122, #63674, #24434, #53701, #4494, #9318, #57605 ),
 .UNSPECIFIED., .F., .F. ) 
 B_SPLINE_CURVE_WITH_KNOTS ( ( 3, 2, 2, 2, 3 ),
 ( 0.7895833333333333037, 0.7902777777777777457, 0.7916666666666666297, 0.7930555555555555136, 0.7937499999999999556 ),
 .UNSPECIFIED. ) 
 CURVE ( )  GEOMETRIC_REPRESENTATION_ITEM ( )  RATIONAL_B_SPLINE_CURVE ( ( 0.9330127018922194093, 0.9330127018922194093, 1.000000000000000000, 0.8660254037844387076, 1.000000000000000000, 0.8660254037844387076, 1.000000000000000000, 0.9330127018922194093, 0.9330127018922194093 ) ) 
 REPRESENTATION_ITEM ( '' )  );
#54683 = EDGE_CURVE ( 'NONE', #44005, #11078, #54361, .T. ) ;
#54684 = CARTESIAN_POINT ( 'NONE',  ( -1.339745962155636017, 2.330341803992663774, 4.999999999999985789 ) ) ;
#54685 = CARTESIAN_POINT ( 'NONE',  ( 2.229367062499998831, -1.645833331967737401, -3.861377020970580887 ) ) ;
#54686 = CARTESIAN_POINT ( 'NONE',  ( 2.500000000000002220, -73.54166666393548724, 4.330127018922192761 ) ) ;
#54687 = CARTESIAN_POINT ( 'NONE',  ( -3.152801135295367985, -150.8125000013655779, 3.152801135295367096 ) ) ;
#54688 =( BOUNDED_CURVE ( )  B_SPLINE_CURVE ( 2, ( #6638, #50695, #31382, #61313, #56492, #23021, #32025, #18183, #12413 ),
 .UNSPECIFIED., .F., .F. ) 
 B_SPLINE_CURVE_WITH_KNOTS ( ( 3, 2, 2, 2, 3 ),
 ( 0.01041666666666666782, 0.01111111111111111154, 0.01250000000000000069, 0.01388888888888888812, 0.01458333333333333356 ),
 .UNSPECIFIED. ) 
 CURVE ( )  GEOMETRIC_REPRESENTATION_ITEM ( )  RATIONAL_B_SPLINE_CURVE ( ( 0.9330127018922192983, 0.9330127018922194093, 1.000000000000000000, 0.8660254037844387076, 1.000000000000000000, 0.8660254037844387076, 1.000000000000000000, 0.9330127018922191873, 0.9330127018922192983 ) ) 
 REPRESENTATION_ITEM ( '' )  );
#54689 = CARTESIAN_POINT ( 'NONE',  ( 4.458734125000000326, 14.85416666803225993, 2.574251347313718519 ) ) ;
#54690 = ORIENTED_EDGE ( 'NONE', *, *, #49168, .F. ) ;
#54691 = CARTESIAN_POINT ( 'NONE',  ( 4.458734124999998549, -94.72916666530106511, -2.574251347313721627 ) ) ;
#54692 = CARTESIAN_POINT ( 'NONE',  ( -5.000000000000000000, -18.95833333060214798, -2.886751345948128211 ) ) ;
#54693 = CARTESIAN_POINT ( 'NONE',  ( 5.000000000000000000, -71.37499999726880162, -6.123233995736766282E-16 ) ) ;
#54694 = CARTESIAN_POINT ( 'NONE',  ( -4.458734124999998549, -17.22916666530106866, 2.574251347313722516 ) ) ;
#54696 = EDGE_CURVE ( 'NONE', #48706, #20975, #29722, .T. ) ;
#54695 = CARTESIAN_POINT ( 'NONE',  ( -50.18089887299977647, -143.6875000000000284, 2.462841084822486426 ) ) ;
#54697 = CARTESIAN_POINT ( 'NONE',  ( 2.499999999999998668, -3.333333333333333925, -4.330127018922193649 ) ) ;
#54698 = CARTESIAN_POINT ( 'NONE',  ( -59.29741812935640155, -148.6250000013656063, -2.196230717870135685 ) ) ;
#54699 = CARTESIAN_POINT ( 'NONE',  ( -5.000000000000000000, -43.95833333060214443, -2.886751345948128211 ) ) ;
#54700 = CARTESIAN_POINT ( 'NONE',  ( 6.123233995736766282E-16, -120.0000000000000000, -5.000000000000000000 ) ) ;
#54701 = CARTESIAN_POINT ( 'NONE',  ( -3.152548672688508926E-16, 12.43750000136559208, -5.148502694627439702 ) ) ;
#54702 = CARTESIAN_POINT ( 'NONE',  ( -4.458734124999999437, -110.5624999986343937, 0.000000000000000000 ) ) ;
#54703 = EDGE_CURVE ( 'NONE', #9342, #29478, #60950, .T. ) ;
#54704 = CARTESIAN_POINT ( 'NONE',  ( 1.975475456537005874E-15, 9.250000000000000000, 5.000000000000000000 ) ) ;
#54705 = CARTESIAN_POINT ( 'NONE',  ( -4.458734124999999437, 11.68750000136559564, 0.000000000000000000 ) ) ;
#54706 = CARTESIAN_POINT ( 'NONE',  ( 4.458734125000001214, -61.89583333196773651, 2.574251347313718519 ) ) ;
#54707 = EDGE_LOOP ( 'NONE', ( #51595, #2173, #34806, #62316 ) ) ;
#54708 = CARTESIAN_POINT ( 'NONE',  ( -2.229367062500000163, -11.72916666530107044, -3.861377020970580443 ) ) ;
#54709 = CARTESIAN_POINT ( 'NONE',  ( -5.000000000000000000, 4.000000000000000000, 0.000000000000000000 ) ) ;
#54710 = CARTESIAN_POINT ( 'NONE',  ( -3.152801135295367096, -163.0625000013656063, -3.152801135295367541 ) ) ;
#54712 = EDGE_CURVE ( 'NONE', #26438, #24132, #37620, .T. ) ;
#54711 = CARTESIAN_POINT ( 'NONE',  ( -51.75738570946856498, -142.7500000000000284, 3.805975901505576964 ) ) ;
#54713 = CARTESIAN_POINT ( 'NONE',  ( -2.229367062500000163, -59.47916666530106511, -3.861377020970580443 ) ) ;
#54714 = CARTESIAN_POINT ( 'NONE',  ( -3.535250795749689387E-16, -90.12499999726881583, -5.773502691896257311 ) ) ;
#54715 = CARTESIAN_POINT ( 'NONE',  ( 4.458734124999999437, -31.81249999863440436, -5.460374474430324690E-16 ) ) ;
#54716 = CYLINDRICAL_SURFACE ( 'NONE', #41128, 5.000000000000000000 ) ;
#54717 = CARTESIAN_POINT ( 'NONE',  ( -55.00000000000002132, -155.0000000000000284, 1.734723475976807094E-15 ) ) ;
#54718 = CARTESIAN_POINT ( 'NONE',  ( -51.75738570946856498, -151.8750000027312126, 3.805975901505576964 ) ) ;
#54719 = LINE ( 'NONE', #25767, #18410 ) ;
#54720 = CARTESIAN_POINT ( 'NONE',  ( 4.458734124999999437, -154.6250000013655779, -1.846868145590734978 ) ) ;
#54721 = CARTESIAN_POINT ( 'NONE',  ( 2.499999999999998668, -41.33333333333333570, -4.330127018922193649 ) ) ;
#54722 = CARTESIAN_POINT ( 'NONE',  ( 7.808623696107892975, -4.508310992946673146, -7.999704684617491068 ) ) ;
#54723 = CARTESIAN_POINT ( 'NONE',  ( 1.975475456537005874E-15, -6.624999997268813168, 5.000000000000000000 ) ) ;
#54724 = VERTEX_POINT ( 'NONE', #37003 ) ;
#54725 = CARTESIAN_POINT ( 'NONE',  ( 2.229367062500001939, -99.97916666530106511, 3.861377020970579999 ) ) ;
#54726 = CARTESIAN_POINT ( 'NONE',  ( -2.229367062499996610, 0.6041666680322611560, 3.861377020970582219 ) ) ;
#54727 = CARTESIAN_POINT ( 'NONE',  ( -5.000000000000000000, -8.874999997268814056, 0.000000000000000000 ) ) ;
#54728 = CARTESIAN_POINT ( 'NONE',  ( 2.500000000000002220, -2.666666666666664298, 4.330127018922192761 ) ) ;
#54729 = CARTESIAN_POINT ( 'NONE',  ( -4.458734124999999437, -68.31249999863439371, 0.000000000000000000 ) ) ;
#54730 = CARTESIAN_POINT ( 'NONE',  ( -49.85088928181150436, -147.6875000027312126, -1.666127454062680480 ) ) ;
#54731 = CARTESIAN_POINT ( 'NONE',  ( -5.000000000000000000, -5.874999997268811391, 0.000000000000000000 ) ) ;
#54733 = ORIENTED_EDGE ( 'NONE', *, *, #4797, .T. ) ;
#54732 = CARTESIAN_POINT ( 'NONE',  ( 4.458734124999998549, -31.72916666530107577, -2.574251347313721627 ) ) ;
#54734 = CARTESIAN_POINT ( 'NONE',  ( 2.499999999999998668, -33.33333333333332860, -4.330127018922193649 ) ) ;
#54735 = CARTESIAN_POINT ( 'NONE',  ( -2.500000000000000444, -17.04166666393548368, -4.330127018922193649 ) ) ;
#54736 = EDGE_LOOP ( 'NONE', ( #55812, #13290, #56807, #32247 ) ) ;
#54737 = CARTESIAN_POINT ( 'NONE',  ( -1.339745962155497683, -56.08034179853028434, -5.000000000000066613 ) ) ;
#54738 = CARTESIAN_POINT ( 'NONE',  ( -4.999999999999999112, -50.91666666666667140, 2.886751345948131764 ) ) ;
#54740 = CARTESIAN_POINT ( 'NONE',  ( -2.229367062500000163, -29.72916666530107221, -3.861377020970580443 ) ) ;
#54739 = FACE_OUTER_BOUND ( 'NONE', #15166, .T. ) ;
#54741 = CARTESIAN_POINT ( 'NONE',  ( 1.975475456537005874E-15, -4.624999997268815832, 5.000000000000000000 ) ) ;
#54742 = CARTESIAN_POINT ( 'NONE',  ( 4.458734125000001214, -74.89583333196773651, 2.574251347313718519 ) ) ;
#54743 =( BOUNDED_CURVE ( )  B_SPLINE_CURVE ( 2, ( #42382, #52367, #60608, #35835, #11057, #55130, #6247, #1437, #45473 ),
 .UNSPECIFIED., .F., .F. ) 
 B_SPLINE_CURVE_WITH_KNOTS ( ( 3, 2, 2, 2, 3 ),
 ( 0.5312500000000000000, 0.5319444444444444420, 0.5333333333333333259, 0.5347222222222222099, 0.5354166666666666519 ),
 .UNSPECIFIED. ) 
 CURVE ( )  GEOMETRIC_REPRESENTATION_ITEM ( )  RATIONAL_B_SPLINE_CURVE ( ( 0.9330127018922194093, 0.9330127018922194093, 1.000000000000000000, 0.8660254037844387076, 1.000000000000000000, 0.8660254037844387076, 1.000000000000000000, 0.9330127018922194093, 0.9330127018922194093 ) ) 
 REPRESENTATION_ITEM ( '' )  );
#54744 = CARTESIAN_POINT ( 'NONE',  ( 3.152801135295366208, -145.8125000013655779, 3.152801135295367985 ) ) ;
#54745 = CARTESIAN_POINT ( 'NONE',  ( -2.229367062499996610, -84.14583333196773651, 3.861377020970582219 ) ) ;
#54746 = CARTESIAN_POINT ( 'NONE',  ( -57.19623071787017210, -140.6250000013656063, 4.297418129356382899 ) ) ;
#54747 = CARTESIAN_POINT ( 'NONE',  ( -3.152548672688508926E-16, -29.81249999863440436, -5.148502694627439702 ) ) ;
#54748 = VERTEX_POINT ( 'NONE', #32802 ) ;
#54749 = DIRECTION ( 'NONE',  ( 0.000000000000000000, 0.000000000000000000, 1.000000000000000000 ) ) ;
#54750 = ORIENTED_EDGE ( 'NONE', *, *, #27180, .F. ) ;
#54751 = CARTESIAN_POINT ( 'NONE',  ( -4.458734124999999437, -74.64583333196773651, -2.574251347313719407 ) ) ;
#54752 = LINE ( 'NONE', #15829, #34847 ) ;
#54753 = VERTEX_POINT ( 'NONE', #7419 ) ;
#54754 = CARTESIAN_POINT ( 'NONE',  ( -56.66612745406293783, -140.3125000000000000, -5.149110718188535607 ) ) ;
#54755 = DIRECTION ( 'NONE',  ( 0.000000000000000000, 0.000000000000000000, 1.000000000000000000 ) ) ;
#54756 = CARTESIAN_POINT ( 'NONE',  ( 9.457646018065525792E-16, -62.31249999863440792, 5.148502694627439702 ) ) ;
#54757 = CARTESIAN_POINT ( 'NONE',  ( 4.458734124999998549, -1.979166665301068662, -2.574251347313721627 ) ) ;
#54758 = ORIENTED_EDGE ( 'NONE', *, *, #52004, .T. ) ;
#54759 = EDGE_CURVE ( 'NONE', #46916, #59564, #52431, .T. ) ;
#54760 = CARTESIAN_POINT ( 'NONE',  ( 1.339745962155615144, -62.70534180126146850, 4.999999999999999112 ) ) ;
#54761 = CARTESIAN_POINT ( 'NONE',  ( -2.499999999999996447, -44.83333333333333570, 4.330127018922195425 ) ) ;
#54762 = CARTESIAN_POINT ( 'NONE',  ( 2.229367062500001939, 11.02083333469892956, 3.861377020970579999 ) ) ;
#54763 = CARTESIAN_POINT ( 'NONE',  ( -53.51423613279429503, -142.2500000013656063, 4.591703134518082763 ) ) ;
#54764 = CARTESIAN_POINT ( 'NONE',  ( 1.339745962155615144, -24.70534180126147561, 4.999999999999999112 ) ) ;
#54765 = CARTESIAN_POINT ( 'NONE',  ( 4.458734124999997661, -160.5000000013656347, 1.846868145590737864 ) ) ;
#54766 = ORIENTED_EDGE ( 'NONE', *, *, #45686, .F. ) ;
#54767 = CARTESIAN_POINT ( 'NONE',  ( -2.229367062500000163, -79.47916666530106511, -3.861377020970580443 ) ) ;
#54768 = CARTESIAN_POINT ( 'NONE',  ( -6.972266317189433020E-16, -90.12499999726880162, -5.000000000000000000 ) ) ;
#54769 = CARTESIAN_POINT ( 'NONE',  ( 4.458734124999998549, 0.2708333346989263979, -2.574251347313721627 ) ) ;
#54770 = CARTESIAN_POINT ( 'NONE',  ( 0.000000000000000000, -170.0000000000000000, 0.000000000000000000 ) ) ;
#54771 = CARTESIAN_POINT ( 'NONE',  ( -6.972266317189433020E-16, -36.25000000000000000, -5.000000000000000000 ) ) ;
#54772 = CARTESIAN_POINT ( 'NONE',  ( -2.229367062500000163, -66.72916666530106511, -3.861377020970580443 ) ) ;
#54773 = CARTESIAN_POINT ( 'NONE',  ( -5.000000000000000000, -26.87499999726881583, 0.000000000000000000 ) ) ;
#54774 = CARTESIAN_POINT ( 'NONE',  ( -5.000000000000000000, -72.95833333060214443, -2.886751345948128211 ) ) ;
#54775 = CARTESIAN_POINT ( 'NONE',  ( -4.458734124999999437, 29.60416666803225993, -2.574251347313719407 ) ) ;
#54776 = CARTESIAN_POINT ( 'NONE',  ( 1.339745962155615144, -110.5803417985302985, 4.999999999999999112 ) ) ;
#54777 = CARTESIAN_POINT ( 'NONE',  ( 1.339745962155615144, -3.580341798530293662, 4.999999999999999112 ) ) ;
#54778 = EDGE_CURVE ( 'NONE', #6544, #22858, #10391, .T. ) ;
#54779 = CARTESIAN_POINT ( 'NONE',  ( -2.229367062500000163, -47.47916666530106511, -3.861377020970580443 ) ) ;
#54780 = CARTESIAN_POINT ( 'NONE',  ( -2.229367062500000163, -34.72916666530107221, -3.861377020970580443 ) ) ;
#54781 = CARTESIAN_POINT ( 'NONE',  ( -4.458734124999997661, -0.4791666653010707710, 2.574251347313722516 ) ) ;
#54782 = CARTESIAN_POINT ( 'NONE',  ( -5.000000000000000888, -161.6875000027311842, -2.071067811865475949 ) ) ;
#54783 = CARTESIAN_POINT ( 'NONE',  ( -5.000000000000000000, 19.00000000000000000, 0.000000000000000000 ) ) ;
#54784 = EDGE_CURVE ( 'NONE', #35059, #13136, #36329, .T. ) ;
#54785 = CARTESIAN_POINT ( 'NONE',  ( 3.535533905932736864, -145.2500000027311842, 3.535533905932738641 ) ) ;
#54786 = LINE ( 'NONE', #44479, #61356 ) ;
#54787 = CARTESIAN_POINT ( 'NONE',  ( 4.458734125000001214, -37.89583333196772941, 2.574251347313718519 ) ) ;
#54788 = CARTESIAN_POINT ( 'NONE',  ( 5.000000000000000888, -73.45833333060214443, 2.886751345948126879 ) ) ;
#54789 = CARTESIAN_POINT ( 'NONE',  ( -56.48576386720575471, -145.0000000013656063, -4.591703134518078322 ) ) ;
#54790 = VECTOR ( 'NONE', #5866, 1000.000000000000000 ) ;
#54791 = CARTESIAN_POINT ( 'NONE',  ( 5.000000000000000888, -24.45833333060214798, 2.886751345948126879 ) ) ;
#54792 = EDGE_CURVE ( 'NONE', #14704, #55857, #57577, .T. ) ;
#54793 = CARTESIAN_POINT ( 'NONE',  ( 1.339745962155612702, -37.29465819873852439, -5.000000000000000000 ) ) ;
#54794 = CARTESIAN_POINT ( 'NONE',  ( -4.458734124999999437, -81.56249999863440792, 0.000000000000000000 ) ) ;
#54795 = CARTESIAN_POINT ( 'NONE',  ( 3.152801135295367541, -164.5625000013656063, -3.152801135295367541 ) ) ;
#54796 = CARTESIAN_POINT ( 'NONE',  ( 1.975475456537005874E-15, -32.74999999999999289, 5.000000000000000000 ) ) ;
#54797 = CARTESIAN_POINT ( 'NONE',  ( -3.535533905932738641, -159.5000000027312126, 3.535533905932737309 ) ) ;
#54798 = CARTESIAN_POINT ( 'NONE',  ( -5.000000000000000000, -26.99999999999999645, 0.000000000000000000 ) ) ;
#54799 = CARTESIAN_POINT ( 'NONE',  ( 1.846868145590736310, -144.6250000013655779, 4.458734124999999437 ) ) ;
#54800 = ORIENTED_EDGE ( 'NONE', *, *, #11135, .T. ) ;
#54801 = CARTESIAN_POINT ( 'NONE',  ( -4.458734124999999437, 23.43750000136559564, 0.000000000000000000 ) ) ;
#54802 = ORIENTED_EDGE ( 'NONE', *, *, #30666, .T. ) ;
#54803 = CARTESIAN_POINT ( 'NONE',  ( 2.229367062500001939, -64.22916666530106511, 3.861377020970579999 ) ) ;
#54804 = CARTESIAN_POINT ( 'NONE',  ( -4.999999999999999112, 19.20833333606451632, 2.886751345948131764 ) ) ;
#54805 = DIRECTION ( 'NONE',  ( -0.000000000000000000, 1.000000000000000000, -0.000000000000000000 ) ) ;
#54806 = CARTESIAN_POINT ( 'NONE',  ( 5.000000000000000888, 13.41666666666666607, 2.886751345948126879 ) ) ;
#54807 = CARTESIAN_POINT ( 'NONE',  ( 4.458734124999998549, -49.72916666530107221, -2.574251347313721627 ) ) ;
#54808 = CARTESIAN_POINT ( 'NONE',  ( -2.229367062499996610, -9.145833331967736513, 3.861377020970582219 ) ) ;
#54809 = DIRECTION ( 'NONE',  ( 0.000000000000000000, 0.000000000000000000, 1.000000000000000000 ) ) ;
#54810 = CARTESIAN_POINT ( 'NONE',  ( -6.972266317189433020E-16, -0.2500000000000001665, -5.000000000000000000 ) ) ;
#54811 = CARTESIAN_POINT ( 'NONE',  ( -1.339745962155610925, -9.794658198738520838, 5.000000000000000000 ) ) ;
#54813 = CARTESIAN_POINT ( 'NONE',  ( 9.457646018065525792E-16, -24.06249999863440436, 5.148502694627439702 ) ) ;
#54812 = CARTESIAN_POINT ( 'NONE',  ( 1.975475456537005874E-15, -40.74999999999999289, 5.000000000000000000 ) ) ;
#54814 = CARTESIAN_POINT ( 'NONE',  ( 1.975475456537005874E-15, -31.62499999726880873, 5.000000000000000000 ) ) ;
#54815 = CARTESIAN_POINT ( 'NONE',  ( -3.152548672688508926E-16, -58.56249999863440081, -5.148502694627439702 ) ) ;
#54816 = CARTESIAN_POINT ( 'NONE',  ( -4.458734125000000326, -157.2500000013656063, -1.846868145590735644 ) ) ;
#54817 =( BOUNDED_CURVE ( )  B_SPLINE_CURVE ( 2, ( #14771, #48868, #45328, #34719, #20894, #4814, #5135, #49196, #44038 ),
 .UNSPECIFIED., .F., .F. ) 
 B_SPLINE_CURVE_WITH_KNOTS ( ( 3, 2, 2, 2, 3 ),
 ( 0.6125000000000000444, 0.6130952380952381375, 0.6142857142857143238, 0.6154761904761905100, 0.6160714285714286031 ),
 .UNSPECIFIED. ) 
 CURVE ( )  GEOMETRIC_REPRESENTATION_ITEM ( )  RATIONAL_B_SPLINE_CURVE ( ( 0.9330127018922194093, 0.9330127018922194093, 1.000000000000000000, 0.8660254037844387076, 1.000000000000000000, 0.8660254037844387076, 1.000000000000000000, 0.9330127018922194093, 0.9330127018922194093 ) ) 
 REPRESENTATION_ITEM ( '' )  );
#54818 = CARTESIAN_POINT ( 'NONE',  ( 2.500000000000002220, -56.54166666393548013, 4.330127018922192761 ) ) ;
#54819 = EDGE_LOOP ( 'NONE', ( #37121, #17952, #59552, #25301 ) ) ;
#54820 = DIRECTION ( 'NONE',  ( 0.000000000000000000, 0.000000000000000000, 1.000000000000000000 ) ) ;
#54821 = CARTESIAN_POINT ( 'NONE',  ( -4.458734124999998549, 0.5208333346989265644, 2.574251347313722516 ) ) ;
#54822 = ORIENTED_EDGE ( 'NONE', *, *, #27890, .F. ) ;
#54824 = CARTESIAN_POINT ( 'NONE',  ( -2.500000000000000444, -3.166666666666664742, -4.330127018922193649 ) ) ;
#54823 = CARTESIAN_POINT ( 'NONE',  ( -50.01589407740564042, -141.6250000000000284, 0.3983568153799778022 ) ) ;
#54825 = CARTESIAN_POINT ( 'NONE',  ( 1.846868145590736310, -156.6250000013655779, 4.458734124999999437 ) ) ;
#54826 = ORIENTED_EDGE ( 'NONE', *, *, #11108, .F. ) ;
#54827 = CARTESIAN_POINT ( 'NONE',  ( -1.127183054612291972E-14, 25.24999999999999645, 4.999999999999999112 ) ) ;
#54828 = CARTESIAN_POINT ( 'NONE',  ( -50.01589407740564042, -130.6250000000000284, 0.3983568153799778022 ) ) ;
#54829 = CARTESIAN_POINT ( 'NONE',  ( 3.535533905932738197, -152.8750000000000000, -3.535533905932738197 ) ) ;
#54830 = CARTESIAN_POINT ( 'NONE',  ( -3.152548672688508926E-16, -43.81249999863440081, -5.148502694627439702 ) ) ;
#54831 = ORIENTED_EDGE ( 'NONE', *, *, #24849, .T. ) ;
#54832 = ADVANCED_FACE ( 'NONE', ( #33118 ), #47281, .T. ) ;
#54833 =( BOUNDED_CURVE ( )  B_SPLINE_CURVE ( 2, ( #16759, #11287, #1989, #25779, #26732, #20958, #6483, #35115, #16443 ),
 .UNSPECIFIED., .F., .F. ) 
 B_SPLINE_CURVE_WITH_KNOTS ( ( 3, 2, 2, 2, 3 ),
 ( 0.4270833333333333148, 0.4277777777777777568, 0.4291666666666666408, 0.4305555555555555802, 0.4312500000000000222 ),
 .UNSPECIFIED. ) 
 CURVE ( )  GEOMETRIC_REPRESENTATION_ITEM ( )  RATIONAL_B_SPLINE_CURVE ( ( 0.9330127018922194093, 0.9330127018922194093, 1.000000000000000000, 0.8660254037844387076, 1.000000000000000000, 0.8660254037844387076, 1.000000000000000000, 0.9330127018922194093, 0.9330127018922194093 ) ) 
 REPRESENTATION_ITEM ( '' )  );
#54834 = CARTESIAN_POINT ( 'NONE',  ( -1.339745962155610925, -45.79465819873851729, 5.000000000000000000 ) ) ;
#54835 = CARTESIAN_POINT ( 'NONE',  ( -2.229367062499996610, 14.85416666803226171, 3.861377020970582219 ) ) ;
#54836 = CARTESIAN_POINT ( 'NONE',  ( 2.229367062500001939, -90.22916666530106511, 3.861377020970579999 ) ) ;
#54837 = CARTESIAN_POINT ( 'NONE',  ( -59.59170313451811296, -151.5000000013655779, 1.485763867205729394 ) ) ;
#54838 = FACE_OUTER_BOUND ( 'NONE', #17234, .T. ) ;
#54839 = CARTESIAN_POINT ( 'NONE',  ( -4.999999999999998224, -35.79166666393547303, 2.886751345948131764 ) ) ;
#54840 = CARTESIAN_POINT ( 'NONE',  ( 3.061616997868383141E-16, -159.8750000027311842, -5.000000000000000000 ) ) ;
#54841 = CARTESIAN_POINT ( 'NONE',  ( 4.458734125000000326, -65.89583333196773651, 2.574251347313718519 ) ) ;
#54842 = LINE ( 'NONE', #29411, #4769 ) ;
#54843 = CARTESIAN_POINT ( 'NONE',  ( -4.458734124999998549, 19.77083333469892779, 2.574251347313722516 ) ) ;
#54844 = CARTESIAN_POINT ( 'NONE',  ( 0.000000000000000000, -170.0000000000000000, 0.000000000000000000 ) ) ;
#54845 = CARTESIAN_POINT ( 'NONE',  ( -4.999999999999998224, -26.91666666666666430, 2.886751345948131764 ) ) ;
#54846 = CARTESIAN_POINT ( 'NONE',  ( 2.229367062500001939, -51.22916666530107221, 3.861377020970579999 ) ) ;
#54847 = CARTESIAN_POINT ( 'NONE',  ( -2.499999999999996447, -10.70833333060214621, 4.330127018922195425 ) ) ;
#54848 = CARTESIAN_POINT ( 'NONE',  ( -5.000000000000000000, -19.95833333060214798, -2.886751345948128211 ) ) ;
#54849 = CARTESIAN_POINT ( 'NONE',  ( -3.152548672688508926E-16, -89.81249999863439371, -5.148502694627439702 ) ) ;
#54850 = CARTESIAN_POINT ( 'NONE',  ( 1.975475456537005874E-15, -104.6249999972688016, 5.000000000000000000 ) ) ;
#54851 = CARTESIAN_POINT ( 'NONE',  ( 9.457646018065525792E-16, -15.31249999863440436, 5.148502694627439702 ) ) ;
#54852 = ORIENTED_EDGE ( 'NONE', *, *, #18499, .F. ) ;
#54853 = CARTESIAN_POINT ( 'NONE',  ( -5.000000000000000888, -169.5625000000000284, -2.071067811865475949 ) ) ;
#54854 = CARTESIAN_POINT ( 'NONE',  ( -4.458734124999999437, -103.3124999986344079, 0.000000000000000000 ) ) ;
#54855 = CARTESIAN_POINT ( 'NONE',  ( 5.000000000000000000, -161.1875000027312126, 2.071067811865478614 ) ) ;
#54856 = ORIENTED_EDGE ( 'NONE', *, *, #37346, .T. ) ;
#54857 = CARTESIAN_POINT ( 'NONE',  ( 4.458734124999999437, -99.06249999863440792, -5.460374474430324690E-16 ) ) ;
#54858 = DIRECTION ( 'NONE',  ( -0.000000000000000000, 1.000000000000000000, -0.000000000000000000 ) ) ;
#54859 = CARTESIAN_POINT ( 'NONE',  ( -2.499999999999996447, -55.70833333060214443, 4.330127018922195425 ) ) ;
#54860 = CARTESIAN_POINT ( 'NONE',  ( 0.000000000000000000, -120.0000000000000000, 0.000000000000000000 ) ) ;
#54861 = CARTESIAN_POINT ( 'NONE',  ( -57.89159099828107458, -124.6875000013656063, -3.393966926194107447 ) ) ;
#54862 = CARTESIAN_POINT ( 'NONE',  ( -59.59170313451810586, -142.5000000013656063, 1.485763867205729394 ) ) ;
#54863 = CARTESIAN_POINT ( 'NONE',  ( -2.229367062499996610, -23.14583333196773651, 3.861377020970582219 ) ) ;
#54864 = CARTESIAN_POINT ( 'NONE',  ( 9.457646018065525792E-16, 5.687500001365592972, 5.148502694627439702 ) ) ;
#54865 = CARTESIAN_POINT ( 'NONE',  ( 9.457646018065525792E-16, -66.31249999863440792, 5.148502694627439702 ) ) ;
#54866 = CARTESIAN_POINT ( 'NONE',  ( 1.339745962155615144, -94.58034179853028434, 4.999999999999999112 ) ) ;
#54867 = CARTESIAN_POINT ( 'NONE',  ( -2.229367062499996610, -20.14583333196774007, 3.861377020970582219 ) ) ;
#54868 = CARTESIAN_POINT ( 'NONE',  ( 1.975475456537005874E-15, -32.74999999999999289, 5.000000000000000000 ) ) ;
#54869 = CARTESIAN_POINT ( 'NONE',  ( 5.000000000000000000, -154.0625000000000284, 2.071067811865478614 ) ) ;
#54870 = CARTESIAN_POINT ( 'NONE',  ( 5.000000000000000888, -10.58333333333333393, 2.886751345948126879 ) ) ;
#54871 = CARTESIAN_POINT ( 'NONE',  ( 3.152801135295366208, -154.5625000013656063, 3.152801135295367985 ) ) ;
#54872 = ORIENTED_EDGE ( 'NONE', *, *, #35751, .T. ) ;
#54873 = CARTESIAN_POINT ( 'NONE',  ( -2.229367062500000163, -45.72916666530106511, -3.861377020970580443 ) ) ;
#54874 = CARTESIAN_POINT ( 'NONE',  ( 5.000000000000000888, 21.54166666939785202, 2.886751345948126879 ) ) ;
#54875 = CARTESIAN_POINT ( 'NONE',  ( -6.972266317189433020E-16, -38.12499999726880873, -5.000000000000000000 ) ) ;
#54876 = CARTESIAN_POINT ( 'NONE',  ( -5.000000000000000000, 29.91666666666666430, -2.886751345948128211 ) ) ;
#54877 = AXIS2_PLACEMENT_3D ( 'NONE', #28256, #18916, #53335 ) ;
#54878 = CARTESIAN_POINT ( 'NONE',  ( 2.229367062500001939, 7.020833334698928674, 3.861377020970579999 ) ) ;
#54879 = CARTESIAN_POINT ( 'NONE',  ( 5.000000000000000000, -82.41666666666667140, -2.886751345948130876 ) ) ;
#54880 = DIRECTION ( 'NONE',  ( 0.000000000000000000, 0.000000000000000000, 1.000000000000000000 ) ) ;
#54881 = CARTESIAN_POINT ( 'NONE',  ( 1.339745962155565406, -17.70534180126147916, 5.000000000000028422 ) ) ;
#54882 = CARTESIAN_POINT ( 'NONE',  ( 2.229367062499998831, 23.10416666803225993, -3.861377020970580887 ) ) ;
#54883 = CARTESIAN_POINT ( 'NONE',  ( -2.500000000000000444, -77.16666666666665719, -4.330127018922193649 ) ) ;
#54884 = CARTESIAN_POINT ( 'NONE',  ( -5.000000000000000000, 6.041666669397850242, -2.886751345948128211 ) ) ;
#54885 = VERTEX_POINT ( 'NONE', #7734 ) ;
#54886 = LINE ( 'NONE', #20154, #62324 ) ;
#54887 = EDGE_LOOP ( 'NONE', ( #25278, #60314, #35237, #40045 ) ) ;
#54888 =( BOUNDED_CURVE ( )  B_SPLINE_CURVE ( 2, ( #46774, #32293, #56442, #13309, #51919, #22018, #17186, #22661, #52237 ),
 .UNSPECIFIED., .F., .F. ) 
 B_SPLINE_CURVE_WITH_KNOTS ( ( 3, 2, 2, 2, 3 ),
 ( 0.1583333333333334925, 0.1625000000000001721, 0.1666666666666668239, 0.1708333333333335036, 0.1750000000000001554 ),
 .UNSPECIFIED. ) 
 CURVE ( )  GEOMETRIC_REPRESENTATION_ITEM ( )  RATIONAL_B_SPLINE_CURVE ( ( 0.9999999999999970024, 0.9238795325112897361, 1.000000000000000000, 0.9238795325112867385, 1.000000000000000000, 0.9238795325112867385, 1.000000000000000000, 0.9238795325112837409, 1.000000000000003109 ) ) 
 REPRESENTATION_ITEM ( '' )  );
#54889 = DIRECTION ( 'NONE',  ( -0.000000000000000000, 1.000000000000000000, -0.000000000000000000 ) ) ;
#54890 = CARTESIAN_POINT ( 'NONE',  ( 9.457646018065525792E-16, -37.06249999863440792, 5.148502694627439702 ) ) ;
#54891 = EDGE_CURVE ( 'NONE', #57597, #5493, #10770, .T. ) ;
#54892 = CARTESIAN_POINT ( 'NONE',  ( 5.000000000000000000, -41.37499999726880162, -6.123233995736766282E-16 ) ) ;
#54893 = VERTEX_POINT ( 'NONE', #52108 ) ;
#54894 = CARTESIAN_POINT ( 'NONE',  ( 2.229367062500001939, -12.97916666530107221, 3.861377020970579999 ) ) ;
#54895 = VERTEX_POINT ( 'NONE', #22848 ) ;
#54896 = CARTESIAN_POINT ( 'NONE',  ( 5.000000000000000888, -84.58333333333332860, 2.886751345948126879 ) ) ;
#54897 = CARTESIAN_POINT ( 'NONE',  ( 1.846868145590735200, -169.2500000013655779, -4.458734125000000326 ) ) ;
#54898 = CARTESIAN_POINT ( 'NONE',  ( 2.229367062500001939, -63.22916666530106511, 3.861377020970579999 ) ) ;
#54899 = CARTESIAN_POINT ( 'NONE',  ( 5.000000000000000000, -89.37499999726880162, -6.123233995736766282E-16 ) ) ;
#54901 = VERTEX_POINT ( 'NONE', #42438 ) ;
#54900 = CARTESIAN_POINT ( 'NONE',  ( 0.000000000000000000, 0.000000000000000000, 0.000000000000000000 ) ) ;
#54902 = CARTESIAN_POINT ( 'NONE',  ( -51.19402409849444524, -140.5000000000000000, -3.242614290531456334 ) ) ;
#54903 = CARTESIAN_POINT ( 'NONE',  ( 4.458734125000001214, -26.14583333196774007, 2.574251347313718519 ) ) ;
#54904 = CARTESIAN_POINT ( 'NONE',  ( -4.999999999999998224, -49.91666666666667140, 2.886751345948131764 ) ) ;
#54905 = VERTEX_POINT ( 'NONE', #17994 ) ;
#54906 = CONTEXT_DEPENDENT_SHAPE_REPRESENTATION ( #15832, #39965 ) ;
#54907 = CARTESIAN_POINT ( 'NONE',  ( -1.846868145590734756, -162.3750000013655779, -4.458734125000000326 ) ) ;
#54908 = CARTESIAN_POINT ( 'NONE',  ( -4.458734124999998549, 27.77083333469892423, 2.574251347313722516 ) ) ;
#54909 = CARTESIAN_POINT ( 'NONE',  ( 2.500000000000002220, -23.66666666666666785, 4.330127018922192761 ) ) ;
#54910 = ORIENTED_EDGE ( 'NONE', *, *, #18261, .F. ) ;
#54911 = CARTESIAN_POINT ( 'NONE',  ( -52.80376928212989185, -148.1250000013656063, -4.297418129356378458 ) ) ;
#54912 = CARTESIAN_POINT ( 'NONE',  ( 4.458734124999999437, -77.06249999863440792, -5.460374474430324690E-16 ) ) ;
#54913 = CARTESIAN_POINT ( 'NONE',  ( -58.24261429053147765, -136.3750000027312126, -3.805975901505573855 ) ) ;
#54914 = CARTESIAN_POINT ( 'NONE',  ( 2.229367062499998831, -45.64583333196774362, -3.861377020970580887 ) ) ;
#54915 = CARTESIAN_POINT ( 'NONE',  ( -1.846868145590734756, -142.3750000013656063, -4.458734124999999437 ) ) ;
#54916 =( BOUNDED_CURVE ( )  B_SPLINE_CURVE ( 2, ( #59012, #14943, #34551, #2102, #41295, #1777, #60629, #16548, #45494 ),
 .UNSPECIFIED., .F., .F. ) 
 B_SPLINE_CURVE_WITH_KNOTS ( ( 3, 2, 2, 2, 3 ),
 ( 0.8083333333333331261, 0.8124999999999997780, 0.8166666666666664298, 0.8208333333333330817, 0.8249999999999997335 ),
 .UNSPECIFIED. ) 
 CURVE ( )  GEOMETRIC_REPRESENTATION_ITEM ( )  RATIONAL_B_SPLINE_CURVE ( ( 1.000000000000003997, 0.9238795325112826307, 1.000000000000000000, 0.9238795325112867385, 1.000000000000000000, 0.9238795325112867385, 1.000000000000000000, 0.9238795325112908463, 0.9999999999999958922 ) ) 
 REPRESENTATION_ITEM ( '' )  );
#54917 = CARTESIAN_POINT ( 'NONE',  ( -7.499999999999999112, -4.652405105468739421, -7.929127756970856034 ) ) ;
#54918 = CARTESIAN_POINT ( 'NONE',  ( 2.229367062499998831, -49.64583333196772941, -3.861377020970580887 ) ) ;
#54919 = CARTESIAN_POINT ( 'NONE',  ( -1.339745962155610925, -70.79465819873850307, 5.000000000000000000 ) ) ;
#54920 = CARTESIAN_POINT ( 'NONE',  ( 4.458734124999998549, -17.72916666530106866, -2.574251347313721627 ) ) ;
#54921 = CARTESIAN_POINT ( 'NONE',  ( -3.535250795749689387E-16, -103.2500000000000000, -5.773502691896257311 ) ) ;
#54922 = AXIS2_PLACEMENT_3D ( 'NONE', #30596, #6167, #36067 ) ;
#54923 = CARTESIAN_POINT ( 'NONE',  ( -3.152801135295367096, -140.3125000013655779, -3.152801135295367541 ) ) ;
#54924 = CARTESIAN_POINT ( 'NONE',  ( 9.457646018065525792E-16, -33.31249999863440792, 5.148502694627439702 ) ) ;
#54925 = CARTESIAN_POINT ( 'NONE',  ( -4.999999999999999112, 5.208333336064518981, 2.886751345948131764 ) ) ;
#54926 = CARTESIAN_POINT ( 'NONE',  ( -6.972266317189433020E-16, -72.12499999726878741, -5.000000000000000000 ) ) ;
#54927 = CARTESIAN_POINT ( 'NONE',  ( -59.29741812935640155, -127.6250000013656205, -2.196230717870135685 ) ) ;
#54928 = CARTESIAN_POINT ( 'NONE',  ( -4.458734124999999437, -72.64583333196773651, -2.574251347313719407 ) ) ;
#54929 = CARTESIAN_POINT ( 'NONE',  ( -6.972266317189433020E-16, -65.24999999999998579, -5.000000000000000000 ) ) ;
#54930 = CARTESIAN_POINT ( 'NONE',  ( -4.999999999999998224, -44.79166666393547303, 2.886751345948131764 ) ) ;
#54931 = DIRECTION ( 'NONE',  ( 0.000000000000000000, 0.000000000000000000, 1.000000000000000000 ) ) ;
#54932 = CARTESIAN_POINT ( 'NONE',  ( 4.458734125000000326, -0.1458333319677394824, 2.574251347313718519 ) ) ;
#54933 = ORIENTED_EDGE ( 'NONE', *, *, #4895, .T. ) ;
#54934 = DIRECTION ( 'NONE',  ( -0.000000000000000000, 1.000000000000000000, -0.000000000000000000 ) ) ;
#54935 = CARTESIAN_POINT ( 'NONE',  ( 2.499999999999998668, -15.33333333333333037, -4.330127018922193649 ) ) ;
#54937 = CARTESIAN_POINT ( 'NONE',  ( -2.229367062500000163, -35.47916666530107221, -3.861377020970580443 ) ) ;
#54936 = CARTESIAN_POINT ( 'NONE',  ( 2.229367062500001939, -87.97916666530107932, 3.861377020970579999 ) ) ;
#54938 = FACE_OUTER_BOUND ( 'NONE', #35328, .T. ) ;
#54939 = CARTESIAN_POINT ( 'NONE',  ( -4.458734124999999437, -82.64583333196772230, -2.574251347313719407 ) ) ;
#54940 = CARTESIAN_POINT ( 'NONE',  ( 2.229367062500001939, 15.77083333469892601, 3.861377020970579999 ) ) ;
#54941 = CYLINDRICAL_SURFACE ( 'NONE', #21223, 5.000000000000000000 ) ;
#54942 = CARTESIAN_POINT ( 'NONE',  ( -57.89159099828107458, -137.6875000013656063, -3.393966926194107447 ) ) ;
#54943 = CARTESIAN_POINT ( 'NONE',  ( 9.457646018065525792E-16, -3.062499998634407472, 5.148502694627439702 ) ) ;
#54944 = CARTESIAN_POINT ( 'NONE',  ( 2.229367062499998831, 20.10416666803225993, -3.861377020970580887 ) ) ;
#54945 = CARTESIAN_POINT ( 'NONE',  ( -4.458734124999997661, -47.47916666530106511, 2.574251347313722516 ) ) ;
#54946 = CARTESIAN_POINT ( 'NONE',  ( 5.000000000000000888, -105.5833333333333286, 2.886751345948126879 ) ) ;
#54947 = CARTESIAN_POINT ( 'NONE',  ( -2.229367062499996610, -87.14583333196773651, 3.861377020970582219 ) ) ;
#54948 = CARTESIAN_POINT ( 'NONE',  ( 4.458734124999999437, -2.812499998634407472, -5.460374474430324690E-16 ) ) ;
#54949 = CARTESIAN_POINT ( 'NONE',  ( -2.229367062500000163, -27.72916666530107221, -3.861377020970580443 ) ) ;
#54950 = CARTESIAN_POINT ( 'NONE',  ( -56.48576386720575471, -133.0000000013656063, -4.591703134518078322 ) ) ;
#54951 = CARTESIAN_POINT ( 'NONE',  ( -4.458734124999999437, -72.39583333196775072, -2.574251347313719407 ) ) ;
#54952 = CARTESIAN_POINT ( 'NONE',  ( -5.000000000000000000, -110.8749999972688016, 0.000000000000000000 ) ) ;
#54953 = CARTESIAN_POINT ( 'NONE',  ( -4.458734124999999437, 24.60416666803225993, -2.574251347313719407 ) ) ;
#54954 = CARTESIAN_POINT ( 'NONE',  ( 6.123233995736766282E-16, -120.0000000000000000, -5.000000000000000000 ) ) ;
#54955 = CARTESIAN_POINT ( 'NONE',  ( -51.75738570946856498, -152.8750000027312126, 3.805975901505576964 ) ) ;
#54956 = CARTESIAN_POINT ( 'NONE',  ( 2.229367062499998831, -76.89583333196773651, -3.861377020970580887 ) ) ;
#54957 = CARTESIAN_POINT ( 'NONE',  ( -5.000000000000000000, -61.00000000000000000, 0.000000000000000000 ) ) ;
#54958 = CARTESIAN_POINT ( 'NONE',  ( 5.000000000000000000, -90.29166666393547303, -2.886751345948130876 ) ) ;
#54959 = CARTESIAN_POINT ( 'NONE',  ( -3.535250795749689387E-16, 24.87500000273118417, -5.773502691896257311 ) ) ;
#54960 = ORIENTED_EDGE ( 'NONE', *, *, #1208, .T. ) ;
#54961 = CARTESIAN_POINT ( 'NONE',  ( 4.648177544792955347E-16, 28.87500000273118417, -5.000000000000000000 ) ) ;
#54962 = CARTESIAN_POINT ( 'NONE',  ( -1.339745962155613812, -99.20534180126146850, -5.000000000000000000 ) ) ;
#54964 = CARTESIAN_POINT ( 'NONE',  ( -5.000000000000000000, -20.99999999999999645, 0.000000000000000000 ) ) ;
#54963 = DIRECTION ( 'NONE',  ( 0.000000000000000000, 0.000000000000000000, 1.000000000000000000 ) ) ;
#54965 = CARTESIAN_POINT ( 'NONE',  ( 4.458734124999998549, -21.72916666530107221, -2.574251347313721627 ) ) ;
#54966 = EDGE_CURVE ( 'NONE', #20646, #61326, #37097, .T. ) ;
#54967 = CARTESIAN_POINT ( 'NONE',  ( 4.458734124999999437, -84.81249999863439371, -5.460374474430324690E-16 ) ) ;
#54968 = AXIS2_PLACEMENT_3D ( 'NONE', #44930, #19525, #34006 ) ;
#54969 = CARTESIAN_POINT ( 'NONE',  ( -2.499999999999996447, -24.70833333060214443, 4.330127018922195425 ) ) ;
#54971 = ORIENTED_EDGE ( 'NONE', *, *, #12667, .T. ) ;
#54970 = CARTESIAN_POINT ( 'NONE',  ( -3.152548672688508926E-16, -47.56249999863440792, -5.148502694627439702 ) ) ;
#54972 = CARTESIAN_POINT ( 'NONE',  ( 3.253724281355068545E-15, 27.87500000273118417, -5.000000000000000000 ) ) ;
#54974 = EDGE_LOOP ( 'NONE', ( #34441, #12383, #38073, #41923 ) ) ;
#54973 = CARTESIAN_POINT ( 'NONE',  ( -2.229367062500000163, -5.729166665301072214, -3.861377020970580443 ) ) ;
#54975 = CARTESIAN_POINT ( 'NONE',  ( -53.51423613279429503, -150.2500000013656347, 4.591703134518083651 ) ) ;
#54976 = CARTESIAN_POINT ( 'NONE',  ( -2.500000000000000444, -65.16666666666667140, -4.330127018922193649 ) ) ;
#54977 = CARTESIAN_POINT ( 'NONE',  ( -3.152801135295367985, -153.0625000013656063, 3.152801135295367096 ) ) ;
#54978 = CARTESIAN_POINT ( 'NONE',  ( 4.458734124999999437, -44.06249999863440081, -5.460374474430324690E-16 ) ) ;
#54979 = CARTESIAN_POINT ( 'NONE',  ( 1.339745962155612702, -68.16965819600733312, -5.000000000000000000 ) ) ;
#54980 = CARTESIAN_POINT ( 'NONE',  ( 5.000000000000000000, -160.0625000000000568, 2.071067811865478614 ) ) ;
#54981 = CARTESIAN_POINT ( 'NONE',  ( 1.975475456537005874E-15, -81.62499999726881583, 5.000000000000000000 ) ) ;
#54982 = CARTESIAN_POINT ( 'NONE',  ( -55.39835681537999790, -154.8750000000000284, 4.984105922594378235 ) ) ;
#54983 = CARTESIAN_POINT ( 'NONE',  ( 4.458734125000001214, -9.145833331967736513, 2.574251347313718519 ) ) ;
#54984 = CARTESIAN_POINT ( 'NONE',  ( -3.152548672688508926E-16, -51.81249999863440792, -5.148502694627439702 ) ) ;
#54985 = EDGE_CURVE ( 'NONE', #54333, #46250, #50226, .T. ) ;
#54986 = CARTESIAN_POINT ( 'NONE',  ( -6.972266317189433020E-16, -24.12499999726881228, -5.000000000000000000 ) ) ;
#54987 = CARTESIAN_POINT ( 'NONE',  ( -4.458734125000000326, -146.0000000013655779, -1.846868145590735644 ) ) ;
#54988 = ADVANCED_FACE ( 'NONE', ( #6352 ), #56511, .T. ) ;
#54989 = CARTESIAN_POINT ( 'NONE',  ( -4.458734124999999437, -93.64583333196773651, -2.574251347313719407 ) ) ;
#54990 = CARTESIAN_POINT ( 'NONE',  ( 1.975475456537005874E-15, -106.7499999999999858, 5.000000000000000000 ) ) ;
#54991 = ORIENTED_EDGE ( 'NONE', *, *, #28640, .T. ) ;
#54992 = LINE ( 'NONE', #29574, #20065 ) ;
#54993 = CARTESIAN_POINT ( 'NONE',  ( -2.229367062500000163, 25.27083333469892779, -3.861377020970580443 ) ) ;
#54994 = CARTESIAN_POINT ( 'NONE',  ( -54.60164318462004474, -147.5000000027312126, -4.984105922594373794 ) ) ;
#54995 = CARTESIAN_POINT ( 'NONE',  ( -5.926426369611017623E-15, 27.24999999999999645, 5.000000000000000000 ) ) ;
#54996 = ORIENTED_EDGE ( 'NONE', *, *, #43916, .F. ) ;
#54997 = EDGE_CURVE ( 'NONE', #20011, #44517, #11785, .T. ) ;
#54998 = CARTESIAN_POINT ( 'NONE',  ( 2.229367062499998831, -3.645833331967739177, -3.861377020970580887 ) ) ;
#54999 = CARTESIAN_POINT ( 'NONE',  ( 1.975475456537005874E-15, 6.249999999999998224, 5.000000000000000000 ) ) ;
#55000 = CARTESIAN_POINT ( 'NONE',  ( -4.458734124999999437, -19.64583333196774362, -2.574251347313719407 ) ) ;
#55001 = CARTESIAN_POINT ( 'NONE',  ( 2.229367062499998831, -7.645833331967735624, -3.861377020970580887 ) ) ;
#55002 = CARTESIAN_POINT ( 'NONE',  ( 1.975475456537005874E-15, 4.375000002731185056, 5.000000000000000000 ) ) ;
#55003 = CARTESIAN_POINT ( 'NONE',  ( 4.458734124999999437, -148.4375000013656063, 0.000000000000000000 ) ) ;
#55004 = CARTESIAN_POINT ( 'NONE',  ( -4.458734124999999437, 13.43750000136559386, 0.000000000000000000 ) ) ;
#55005 = EDGE_LOOP ( 'NONE', ( #2020, #49297, #6838, #35279 ) ) ;
#55006 = DIRECTION ( 'NONE',  ( 0.000000000000000000, 0.000000000000000000, 1.000000000000000000 ) ) ;
#55007 = CARTESIAN_POINT ( 'NONE',  ( -2.499999999999996447, -20.83333333333333570, 4.330127018922195425 ) ) ;
#55008 = CARTESIAN_POINT ( 'NONE',  ( 4.458734124999998549, -18.72916666530106866, -2.574251347313721627 ) ) ;
#55009 = CARTESIAN_POINT ( 'NONE',  ( 1.339745962155615144, -25.58034179853029144, 4.999999999999999112 ) ) ;
#55010 = CARTESIAN_POINT ( 'NONE',  ( 5.000000000000000000, -3.500000000000003109, -6.123233995736766282E-16 ) ) ;
#55011 = VECTOR ( 'NONE', #38135, 1000.000000000000000 ) ;
#55012 =( BOUNDED_CURVE ( )  B_SPLINE_CURVE ( 2, ( #60475, #6120, #54680, #36018, #29900, #20267, #10603, #50164, #25733 ),
 .UNSPECIFIED., .F., .F. ) 
 B_SPLINE_CURVE_WITH_KNOTS ( ( 3, 2, 2, 2, 3 ),
 ( 0.9732142857142856984, 0.9738095238095237915, 0.9749999999999999778, 0.9761904761904761640, 0.9767857142857142572 ),
 .UNSPECIFIED. ) 
 CURVE ( )  GEOMETRIC_REPRESENTATION_ITEM ( )  RATIONAL_B_SPLINE_CURVE ( ( 0.9330127018922194093, 0.9330127018922194093, 1.000000000000000000, 0.8660254037844387076, 1.000000000000000000, 0.8660254037844387076, 1.000000000000000000, 0.9330127018922194093, 0.9330127018922194093 ) ) 
 REPRESENTATION_ITEM ( '' )  );
#55013 = CARTESIAN_POINT ( 'NONE',  ( -57.89159099828107458, -151.6875000013656063, -3.393966926194107447 ) ) ;
#55014 = ADVANCED_FACE ( 'NONE', ( #12108 ), #55873, .F. ) ;
#55015 = CARTESIAN_POINT ( 'NONE',  ( -2.499999999999996447, -48.70833333060213732, 4.330127018922195425 ) ) ;
#55016 = CARTESIAN_POINT ( 'NONE',  ( 1.339745962155615144, -74.70534180126148271, 4.999999999999999112 ) ) ;
#55017 = CARTESIAN_POINT ( 'NONE',  ( 4.458734124999999437, 15.18750000136559564, -5.460374474430324690E-16 ) ) ;
#55018 = CARTESIAN_POINT ( 'NONE',  ( 2.499999999999998668, -35.33333333333332860, -4.330127018922193649 ) ) ;
#55019 = CYLINDRICAL_SURFACE ( 'NONE', #48974, 5.000000000000000000 ) ;
#55020 = CARTESIAN_POINT ( 'NONE',  ( -3.152548672688508926E-16, 10.43750000136559386, -5.148502694627439702 ) ) ;
#55021 = CARTESIAN_POINT ( 'NONE',  ( 2.229367062499998831, -67.64583333196773651, -3.861377020970580887 ) ) ;
#55022 = VERTEX_POINT ( 'NONE', #41058 ) ;
#55023 = CARTESIAN_POINT ( 'NONE',  ( 4.458734124999999437, -16.06249999863440436, -5.460374474430324690E-16 ) ) ;
#55024 = CARTESIAN_POINT ( 'NONE',  ( 5.000000000000000888, 3.416666666666665186, 2.886751345948126879 ) ) ;
#55025 = CARTESIAN_POINT ( 'NONE',  ( 4.458734125000000326, -165.3750000013656347, -1.846868145590734978 ) ) ;
#55026 = CARTESIAN_POINT ( 'NONE',  ( -2.499999999999996447, 22.16666666666666785, 4.330127018922195425 ) ) ;
#55027 = CARTESIAN_POINT ( 'NONE',  ( -2.229367062499996610, -58.14583333196773651, 3.861377020970582219 ) ) ;
#55028 = CARTESIAN_POINT ( 'NONE',  ( -2.500000000000000444, -95.04166666393547303, -4.330127018922193649 ) ) ;
#55029 = CARTESIAN_POINT ( 'NONE',  ( -4.458734124999999437, -35.39583333196772941, -2.574251347313719407 ) ) ;
#55030 = CARTESIAN_POINT ( 'NONE',  ( -5.000000000000000000, 20.04166666939785202, -2.886751345948128211 ) ) ;
#55031 = CARTESIAN_POINT ( 'NONE',  ( 1.975475456537005874E-15, -27.74999999999999645, 5.000000000000000000 ) ) ;
#55032 = CYLINDRICAL_SURFACE ( 'NONE', #50089, 4.999999999999999112 ) ;
#55033 = CARTESIAN_POINT ( 'NONE',  ( 2.500000000000002220, 1.333333333333332149, 4.330127018922192761 ) ) ;
#55034 = CARTESIAN_POINT ( 'NONE',  ( 1.846868145590736310, -148.8750000013655779, 4.458734124999997661 ) ) ;
#55035 = CARTESIAN_POINT ( 'NONE',  ( 2.499999999999998668, -44.33333333333333570, -4.330127018922193649 ) ) ;
#55036 = CARTESIAN_POINT ( 'NONE',  ( -2.499999999999996447, -57.70833333060214443, 4.330127018922195425 ) ) ;
#55037 = ORIENTED_EDGE ( 'NONE', *, *, #42935, .T. ) ;
#55038 = CARTESIAN_POINT ( 'NONE',  ( 4.458734124999998549, -108.7291666653010651, -2.574251347313721627 ) ) ;
#55039 = CARTESIAN_POINT ( 'NONE',  ( 4.458734125000001214, 4.854166668032262599, 2.574251347313718519 ) ) ;
#55040 = CYLINDRICAL_SURFACE ( 'NONE', #45263, 5.000000000000000000 ) ;
#55041 = CARTESIAN_POINT ( 'NONE',  ( -5.000000000000000000, -0.08333333333333457771, -2.886751345948128211 ) ) ;
#55042 = VECTOR ( 'NONE', #51853, 1000.000000000000000 ) ;
#55043 = EDGE_CURVE ( 'NONE', #61158, #52679, #41372, .T. ) ;
#55044 = CARTESIAN_POINT ( 'NONE',  ( -2.229367062500000163, -64.47916666530106511, -3.861377020970580443 ) ) ;
#55045 = CARTESIAN_POINT ( 'NONE',  ( 0.000000000000000000, 30.00000000000000000, 0.000000000000000000 ) ) ;
#55046 = EDGE_CURVE ( 'NONE', #55022, #12016, #17357, .T. ) ;
#55047 = ADVANCED_FACE ( 'NONE', ( #46535 ), #31735, .T. ) ;
#55048 = CARTESIAN_POINT ( 'NONE',  ( -2.499999999999996447, -8.708333330602144429, 4.330127018922195425 ) ) ;
#55050 = ORIENTED_EDGE ( 'NONE', *, *, #54341, .F. ) ;
#55049 = CARTESIAN_POINT ( 'NONE',  ( 4.458734125000001214, -34.89583333196772941, 2.574251347313718519 ) ) ;
#55051 = CARTESIAN_POINT ( 'NONE',  ( -51.75738570946856498, -155.0000000000000284, 3.805975901505577408 ) ) ;
#55052 = CARTESIAN_POINT ( 'NONE',  ( -1.339745962155612258, 27.91965820146970856, -5.000000000000000888 ) ) ;
#55054 = ORIENTED_EDGE ( 'NONE', *, *, #40980, .T. ) ;
#55053 = CARTESIAN_POINT ( 'NONE',  ( 4.458734124999999437, 14.93750000136559386, -5.460374474430324690E-16 ) ) ;
#55055 = CARTESIAN_POINT ( 'NONE',  ( -58.24261429053147765, -141.3750000027312126, -3.805975901505573855 ) ) ;
#55056 = CARTESIAN_POINT ( 'NONE',  ( 1.060575238724906964E-15, -48.75000000000000000, 5.773502691896257311 ) ) ;
#55057 = CARTESIAN_POINT ( 'NONE',  ( 2.229367062500001939, -31.22916666530107221, 3.861377020970579999 ) ) ;
#55058 = CARTESIAN_POINT ( 'NONE',  ( -4.999999999999998224, -3.916666666666665630, 2.886751345948131764 ) ) ;
#55059 = CARTESIAN_POINT ( 'NONE',  ( 2.229367062499998831, -74.64583333196773651, -3.861377020970580887 ) ) ;
#55060 = CARTESIAN_POINT ( 'NONE',  ( -4.458734124999999437, -140.1875000013656063, -5.460374474430324690E-16 ) ) ;
#55061 = CARTESIAN_POINT ( 'NONE',  ( -2.229367062500000163, -79.47916666530106511, -3.861377020970580443 ) ) ;
#55062 = CARTESIAN_POINT ( 'NONE',  ( -54.64476657466781973, -134.0625000013656063, -4.444560631937228834 ) ) ;
#55063 = AXIS2_PLACEMENT_3D ( 'NONE', #10303, #1324, #41157 ) ;
#55064 = CARTESIAN_POINT ( 'NONE',  ( -2.229367062500000163, -29.72916666530107221, -3.861377020970580443 ) ) ;
#55065 = VERTEX_POINT ( 'NONE', #22089 ) ;
#55066 = LINE ( 'NONE', #5860, #29972 ) ;
#55068 = EDGE_CURVE ( 'NONE', #35072, #1769, #23921, .T. ) ;
#55067 = VERTEX_POINT ( 'NONE', #51680 ) ;
#55069 = CARTESIAN_POINT ( 'NONE',  ( -4.458734124999999437, -78.64583333196773651, -2.574251347313719407 ) ) ;
#55070 = CARTESIAN_POINT ( 'NONE',  ( 1.975475456537005874E-15, 13.37500000273118417, 5.000000000000000000 ) ) ;
#55071 = ORIENTED_EDGE ( 'NONE', *, *, #49164, .F. ) ;
#55072 = FACE_OUTER_BOUND ( 'NONE', #4647, .T. ) ;
#55073 =( BOUNDED_CURVE ( )  B_SPLINE_CURVE ( 2, ( #5297, #24915, #44519, #481, #45165, #46449, #31321, #50312, #6896 ),
 .UNSPECIFIED., .F., .F. ) 
 B_SPLINE_CURVE_WITH_KNOTS ( ( 3, 2, 2, 2, 3 ),
 ( 0.1232142857142857206, 0.1238095238095238138, 0.1250000000000000000, 0.1261904761904761862, 0.1267857142857142794 ),
 .UNSPECIFIED. ) 
 CURVE ( )  GEOMETRIC_REPRESENTATION_ITEM ( )  RATIONAL_B_SPLINE_CURVE ( ( 0.9330127018922192983, 0.9330127018922200755, 1.000000000000000000, 0.8660254037844387076, 1.000000000000000000, 0.8660254037844387076, 1.000000000000000000, 0.9330127018922194093, 0.9330127018922194093 ) ) 
 REPRESENTATION_ITEM ( '' )  );
#55074 = CARTESIAN_POINT ( 'NONE',  ( -6.972266317189433020E-16, 7.750000000000000000, -5.000000000000000000 ) ) ;
#55075 = CARTESIAN_POINT ( 'NONE',  ( -4.458734124999999437, -63.56249999863440792, 0.000000000000000000 ) ) ;
#55076 = CARTESIAN_POINT ( 'NONE',  ( -4.458734124999999437, -2.645833331967737845, -2.574251347313719407 ) ) ;
#55077 = EDGE_LOOP ( 'NONE', ( #30548, #28243, #30297, #30165 ) ) ;
#55078 = CARTESIAN_POINT ( 'NONE',  ( -5.000000000000000000, 5.125000002731184168, 0.000000000000000000 ) ) ;
#55079 = DIRECTION ( 'NONE',  ( -0.000000000000000000, 1.000000000000000000, -0.000000000000000000 ) ) ;
#55080 = CARTESIAN_POINT ( 'NONE',  ( -2.229367062500000163, 6.520833334698928674, -3.861377020970580443 ) ) ;
#55081 = CARTESIAN_POINT ( 'NONE',  ( -50.40829686548195099, -143.0000000013655779, -1.485763867205728284 ) ) ;
#55082 = CARTESIAN_POINT ( 'NONE',  ( 1.975475456537005874E-15, -0.6249999972688137229, 5.000000000000000000 ) ) ;
#55083 = CARTESIAN_POINT ( 'NONE',  ( -4.458734125000000326, -159.8750000013655779, 1.846868145590734089 ) ) ;
#55084 = CARTESIAN_POINT ( 'NONE',  ( 5.000000000000000000, -75.37499999726880162, -6.123233995736766282E-16 ) ) ;
#55085 = ORIENTED_EDGE ( 'NONE', *, *, #49600, .F. ) ;
#55086 = CARTESIAN_POINT ( 'NONE',  ( 2.229367062500001939, -78.97916666530106511, 3.861377020970579999 ) ) ;
#55087 = CARTESIAN_POINT ( 'NONE',  ( 4.458734124999999437, -5.812499998634403475, -5.460374474430324690E-16 ) ) ;
#55088 = CARTESIAN_POINT ( 'NONE',  ( -6.972266317189433020E-16, -69.12499999726880162, -5.000000000000000000 ) ) ;
#55089 = CARTESIAN_POINT ( 'NONE',  ( 1.975475456537005874E-15, -39.62499999726880162, 5.000000000000000000 ) ) ;
#55090 = CARTESIAN_POINT ( 'NONE',  ( -2.229367062500000163, -70.72916666530107932, -3.861377020970580443 ) ) ;
#55091 = CARTESIAN_POINT ( 'NONE',  ( -5.000000000000000000, -32.87499999726880873, 0.000000000000000000 ) ) ;
#55092 = CARTESIAN_POINT ( 'NONE',  ( -4.999999999999998224, -28.91666666666666430, 2.886751345948131764 ) ) ;
#55093 = CARTESIAN_POINT ( 'NONE',  ( 9.457646018065525792E-16, 27.93750000136559208, 5.148502694627439702 ) ) ;
#55094 = CARTESIAN_POINT ( 'NONE',  ( 2.229367062500001939, 28.02083333469892779, 3.861377020970579999 ) ) ;
#55095 = CARTESIAN_POINT ( 'NONE',  ( 2.229367062500001939, -52.97916666530107221, 3.861377020970579999 ) ) ;
#55096 = CARTESIAN_POINT ( 'NONE',  ( -4.458734124999999437, -31.56249999863440436, 0.000000000000000000 ) ) ;
#55097 = CARTESIAN_POINT ( 'NONE',  ( -2.229367062499996610, 2.604166668032259491, 3.861377020970582219 ) ) ;
#55098 = VECTOR ( 'NONE', #17553, 1000.000000000000000 ) ;
#55099 = CARTESIAN_POINT ( 'NONE',  ( 0.000000000000000000, -120.0000000000000000, 5.000000000000000000 ) ) ;
#55100 = CARTESIAN_POINT ( 'NONE',  ( -5.000000000000000000, 18.91666666666666430, -2.886751345948128211 ) ) ;
#55101 = CARTESIAN_POINT ( 'NONE',  ( 3.535533905932738197, -146.0000000027311842, -3.535533905932738197 ) ) ;
#55102 = DIRECTION ( 'NONE',  ( 0.000000000000000000, 0.000000000000000000, 1.000000000000000000 ) ) ;
#55103 = CARTESIAN_POINT ( 'NONE',  ( -4.458734124999999437, -44.39583333196773651, -2.574251347313719407 ) ) ;
#55104 = CARTESIAN_POINT ( 'NONE',  ( -4.999999999999999112, -71.79166666393547303, 2.886751345948131764 ) ) ;
#55105 = VECTOR ( 'NONE', #52749, 1000.000000000000000 ) ;
#55106 = AXIS2_PLACEMENT_3D ( 'NONE', #40999, #8110, #3911 ) ;
#55107 = CARTESIAN_POINT ( 'NONE',  ( -55.35523342533222291, -142.5625000013656063, 4.444560631937231499 ) ) ;
#55108 = CARTESIAN_POINT ( 'NONE',  ( -9.184850993605147944E-16, -140.2500000000000000, 5.000000000000000000 ) ) ;
#55109 = CARTESIAN_POINT ( 'NONE',  ( -3.152548672688508926E-16, -77.81249999863440792, -5.148502694627439702 ) ) ;
#55110 = CARTESIAN_POINT ( 'NONE',  ( 2.730187237215162345E-16, -162.4375000013655779, -4.458734124999999437 ) ) ;
#55111 = DIRECTION ( 'NONE',  ( -0.000000000000000000, 1.000000000000000000, -0.000000000000000000 ) ) ;
#55112 = CARTESIAN_POINT ( 'NONE',  ( 1.339745962155612702, 13.83034180399266333, -5.000000000000000000 ) ) ;
#55113 = CARTESIAN_POINT ( 'NONE',  ( 5.000000000000000000, -25.41666666666666430, -2.886751345948129988 ) ) ;
#55114 = CARTESIAN_POINT ( 'NONE',  ( -3.152801135295367096, -141.0625000013655779, -3.152801135295367541 ) ) ;
#55115 = ORIENTED_EDGE ( 'NONE', *, *, #56305, .F. ) ;
#55116 = CARTESIAN_POINT ( 'NONE',  ( -4.458734124999999437, 20.35416666803225993, -2.574251347313719407 ) ) ;
#55117 = VERTEX_POINT ( 'NONE', #29022 ) ;
#55118 = CARTESIAN_POINT ( 'NONE',  ( -2.229367062500000163, -62.72916666530106511, -3.861377020970580443 ) ) ;
#55119 = CARTESIAN_POINT ( 'NONE',  ( -2.500000000000000444, 20.95833333606451987, -4.330127018922193649 ) ) ;
#55120 =( BOUNDED_CURVE ( )  B_SPLINE_CURVE ( 2, ( #46434, #27129, #26814, #6883, #41909, #36460, #51581, #26496, #52206 ),
 .UNSPECIFIED., .F., .F. ) 
 B_SPLINE_CURVE_WITH_KNOTS ( ( 3, 2, 2, 2, 3 ),
 ( 0.5250000000000004663, 0.5291666666666671182, 0.5333333333333338810, 0.5375000000000005329, 0.5416666666666671848 ),
 .UNSPECIFIED. ) 
 CURVE ( )  GEOMETRIC_REPRESENTATION_ITEM ( )  RATIONAL_B_SPLINE_CURVE ( ( 0.9999999999999918954, 0.9238795325112948431, 1.000000000000000000, 0.9238795325112867385, 1.000000000000000000, 0.9238795325112867385, 1.000000000000000000, 0.9238795325112766355, 1.000000000000010214 ) ) 
 REPRESENTATION_ITEM ( '' )  );
#55121 = CARTESIAN_POINT ( 'NONE',  ( 1.975475456537005874E-15, -2.624999997268813168, 5.000000000000000000 ) ) ;
#55122 = CARTESIAN_POINT ( 'NONE',  ( 1.060575238724906964E-15, 15.25000000000000000, 5.773502691896257311 ) ) ;
#55123 = CARTESIAN_POINT ( 'NONE',  ( -4.458734124999999437, -52.39583333196773651, -2.574251347313719407 ) ) ;
#55124 = CARTESIAN_POINT ( 'NONE',  ( -4.458734124999999437, -13.31249999863440259, 0.000000000000000000 ) ) ;
#55125 = DIRECTION ( 'NONE',  ( 0.000000000000000000, 0.000000000000000000, 1.000000000000000000 ) ) ;
#55126 = ADVANCED_FACE ( 'NONE', ( #8249 ), #24211, .T. ) ;
#55127 = CARTESIAN_POINT ( 'NONE',  ( 5.000000000000000000, -99.29166666393545881, -2.886751345948130876 ) ) ;
#55128 = CARTESIAN_POINT ( 'NONE',  ( 1.339745962155613146, 28.83034180399266688, -4.999999999999999112 ) ) ;
#55129 = CARTESIAN_POINT ( 'NONE',  ( 0.000000000000000000, -170.0000000000000000, 0.000000000000000000 ) ) ;
#55131 = CARTESIAN_POINT ( 'NONE',  ( -2.229367062500000163, -13.72916666530107221, -3.861377020970580443 ) ) ;
#55130 = CARTESIAN_POINT ( 'NONE',  ( -5.000000000000000000, -34.08333333333332860, -2.886751345948128211 ) ) ;
#55132 = EDGE_CURVE ( 'NONE', #46887, #35992, #56817, .T. ) ;
#55133 = CARTESIAN_POINT ( 'NONE',  ( 5.000000000000000000, 17.70833333606451632, -2.886751345948130876 ) ) ;
#55134 = CARTESIAN_POINT ( 'NONE',  ( -2.229367062500000163, -60.47916666530106511, -3.861377020970580443 ) ) ;
#55135 = CARTESIAN_POINT ( 'NONE',  ( 2.730187237215162345E-16, -150.4375000013656063, -4.458734124999999437 ) ) ;
#55136 = CARTESIAN_POINT ( 'NONE',  ( 2.229367062499998831, -66.64583333196773651, -3.861377020970580887 ) ) ;
#55137 = ADVANCED_FACE ( 'NONE', ( #42643 ), #17585, .F. ) ;
#55138 = EDGE_CURVE ( 'NONE', #10824, #14367, #63382, .T. ) ;
#55139 = CARTESIAN_POINT ( 'NONE',  ( -4.999999999999999112, -53.79166666393548013, 2.886751345948131764 ) ) ;
#55140 = ORIENTED_EDGE ( 'NONE', *, *, #26597, .T. ) ;
#55141 = CARTESIAN_POINT ( 'NONE',  ( -51.19402409849444524, -137.5000000000000284, -3.242614290531456334 ) ) ;
#55142 = CARTESIAN_POINT ( 'NONE',  ( -4.458734124999998549, 1.520833334698927342, 2.574251347313722516 ) ) ;
#55143 = ORIENTED_EDGE ( 'NONE', *, *, #50256, .T. ) ;
#55145 = LINE ( 'NONE', #11071, #40901 ) ;
#55144 = CARTESIAN_POINT ( 'NONE',  ( 5.000000000000000000, -21.50000000000000000, -6.123233995736766282E-16 ) ) ;
#55146 = CARTESIAN_POINT ( 'NONE',  ( -4.458734125000000326, -155.0000000013656063, -1.846868145590735644 ) ) ;
#55147 = EDGE_CURVE ( 'NONE', #30611, #39890, #638, .T. ) ;
#55148 = ORIENTED_EDGE ( 'NONE', *, *, #55043, .T. ) ;
#55149 = AXIS2_PLACEMENT_3D ( 'NONE', #40279, #54443, #49608 ) ;
#55150 = EDGE_CURVE ( 'NONE', #2700, #4593, #11323, .T. ) ;
#55151 = CARTESIAN_POINT ( 'NONE',  ( -51.75738570946856498, -128.7500000000000284, 3.805975901505576964 ) ) ;
#55152 = CARTESIAN_POINT ( 'NONE',  ( -6.972266317189433020E-16, -80.12499999726881583, -5.000000000000000000 ) ) ;
#55153 = CARTESIAN_POINT ( 'NONE',  ( 4.458734124999999437, -51.06249999863440792, -5.460374474430324690E-16 ) ) ;
#55154 = AXIS2_PLACEMENT_3D ( 'NONE', #34950, #6962, #872 ) ;
#55155 = ORIENTED_EDGE ( 'NONE', *, *, #12741, .F. ) ;
#55156 = VECTOR ( 'NONE', #11187, 1000.000000000000000 ) ;
#55157 = EDGE_CURVE ( 'NONE', #17838, #39270, #62262, .T. ) ;
#55158 = LINE ( 'NONE', #6581, #21357 ) ;
#55159 = VECTOR ( 'NONE', #55669, 1000.000000000000000 ) ;
#55160 = CARTESIAN_POINT ( 'NONE',  ( 4.458734124999998549, 13.27083333469892779, -2.574251347313721627 ) ) ;
#55161 = EDGE_CURVE ( 'NONE', #10267, #39251, #2814, .T. ) ;
#55162 = CARTESIAN_POINT ( 'NONE',  ( 4.458734125000001214, 24.10416666803226349, 2.574251347313718519 ) ) ;
#55163 = CARTESIAN_POINT ( 'NONE',  ( -58.39396692619412477, -151.4375000013656063, 2.891590998281057701 ) ) ;
#55164 = CARTESIAN_POINT ( 'NONE',  ( 1.339745962155615144, -44.70534180126146850, 4.999999999999999112 ) ) ;
#55165 = CARTESIAN_POINT ( 'NONE',  ( -6.972266317189433020E-16, 16.87500000273118417, -5.000000000000000000 ) ) ;
#55166 = CARTESIAN_POINT ( 'NONE',  ( -4.458734124999999437, -64.39583333196773651, -2.574251347313719407 ) ) ;
#55167 = CARTESIAN_POINT ( 'NONE',  ( -6.972266317189433020E-16, 0.7499999999999996669, -5.000000000000000000 ) ) ;
#55168 = CARTESIAN_POINT ( 'NONE',  ( -2.229367062499996610, 14.85416666803226171, 3.861377020970582219 ) ) ;
#55169 = CARTESIAN_POINT ( 'NONE',  ( -62.00000000000001421, -155.0000000000000284, -4.041451884327373456 ) ) ;
#55170 = CARTESIAN_POINT ( 'NONE',  ( 1.975475456537005874E-15, -68.62499999726881583, 5.000000000000000000 ) ) ;
#55171 = CARTESIAN_POINT ( 'NONE',  ( 4.458734124999998549, -54.97916666530107221, -2.574251347313721627 ) ) ;
#55172 = CARTESIAN_POINT ( 'NONE',  ( 2.499999999999998668, -11.20833333060214798, -4.330127018922193649 ) ) ;
#55173 = CARTESIAN_POINT ( 'NONE',  ( -2.499999999999996447, -108.8333333333333428, 4.330127018922195425 ) ) ;
#55174 = CARTESIAN_POINT ( 'NONE',  ( -58.24261429053147765, -147.2500000000000284, -3.805975901505573855 ) ) ;
#55175 = CARTESIAN_POINT ( 'NONE',  ( -2.229367062499996610, -89.39583333196773651, 3.861377020970582219 ) ) ;
#55176 = LINE ( 'NONE', #20440, #6991 ) ;
#55177 = CARTESIAN_POINT ( 'NONE',  ( -3.152548672688508926E-16, -13.81249999863440259, -5.148502694627439702 ) ) ;
#55178 = ORIENTED_EDGE ( 'NONE', *, *, #42218, .T. ) ;
#55179 = CARTESIAN_POINT ( 'NONE',  ( 4.458734125000001214, -101.8958333319677365, 2.574251347313718519 ) ) ;
#55180 = CARTESIAN_POINT ( 'NONE',  ( -5.000000000000000888, -156.5625000027312126, 2.071067811865474617 ) ) ;
#55181 = VERTEX_POINT ( 'NONE', #103 ) ;
#55182 = CARTESIAN_POINT ( 'NONE',  ( -3.152548672688508926E-16, -99.81249999863442213, -5.148502694627439702 ) ) ;
#55183 = CARTESIAN_POINT ( 'NONE',  ( -2.229367062499996610, -27.14583333196774007, 3.861377020970582219 ) ) ;
#55184 = CARTESIAN_POINT ( 'NONE',  ( 2.499999999999998668, -59.20833333060214443, -4.330127018922193649 ) ) ;
#55185 = CARTESIAN_POINT ( 'NONE',  ( 5.000000000000000000, -62.37499999726880873, -6.123233995736766282E-16 ) ) ;
#55186 = CARTESIAN_POINT ( 'NONE',  ( -55.35523342533222291, -127.3125000013655921, 4.444560631937231499 ) ) ;
#55187 = CARTESIAN_POINT ( 'NONE',  ( -55.35523342533222291, -144.3125000013656063, 4.444560631937231499 ) ) ;
#55188 = CARTESIAN_POINT ( 'NONE',  ( 9.457646018065525792E-16, -21.06249999863440436, 5.148502694627439702 ) ) ;
#55189 = CARTESIAN_POINT ( 'NONE',  ( 9.457646018065525792E-16, -64.31249999863440792, 5.148502694627439702 ) ) ;
#55190 = CARTESIAN_POINT ( 'NONE',  ( 1.975475456537005874E-15, -53.74999999999999289, 5.000000000000000000 ) ) ;
#55191 = CARTESIAN_POINT ( 'NONE',  ( -3.152548672688508926E-16, -20.56249999863440081, -5.148502694627439702 ) ) ;
#55192 = DIRECTION ( 'NONE',  ( -0.000000000000000000, 1.000000000000000000, -0.000000000000000000 ) ) ;
#55193 = CARTESIAN_POINT ( 'NONE',  ( -3.535533905932738641, -149.3750000000000000, 3.535533905932737309 ) ) ;
#55194 = CARTESIAN_POINT ( 'NONE',  ( -5.000000000000000000, -12.08333333333333393, -2.886751345948128211 ) ) ;
#55195 = CARTESIAN_POINT ( 'NONE',  ( 1.846868145590735200, -152.2500000013656347, -4.458734125000000326 ) ) ;
#55196 = ORIENTED_EDGE ( 'NONE', *, *, #30578, .F. ) ;
#55197 = CARTESIAN_POINT ( 'NONE',  ( -2.229367062500000163, -43.72916666530106511, -3.861377020970580443 ) ) ;
#55198 = VECTOR ( 'NONE', #30222, 1000.000000000000000 ) ;
#55199 = CARTESIAN_POINT ( 'NONE',  ( 0.000000000000000000, -120.0000000000000000, 0.000000000000000000 ) ) ;
#55200 = PLANE ( 'NONE',  #26771 ) ;
#55201 = CARTESIAN_POINT ( 'NONE',  ( 4.458734124999999437, -88.81249999863439371, -5.460374474430324690E-16 ) ) ;
#55202 = VECTOR ( 'NONE', #25442, 1000.000000000000000 ) ;
#55203 = AXIS2_PLACEMENT_3D ( 'NONE', #36416, #45752, #20681 ) ;
#55204 =( BOUNDED_CURVE ( )  B_SPLINE_CURVE ( 2, ( #23189, #28946, #43739, #18674, #8407, #48252, #63069, #58227, #14156 ),
 .UNSPECIFIED., .F., .F. ) 
 B_SPLINE_CURVE_WITH_KNOTS ( ( 3, 2, 2, 2, 3 ),
 ( 0.5232142857142857428, 0.5238095238095238360, 0.5250000000000000222, 0.5261904761904762085, 0.5267857142857143016 ),
 .UNSPECIFIED. ) 
 CURVE ( )  GEOMETRIC_REPRESENTATION_ITEM ( )  RATIONAL_B_SPLINE_CURVE ( ( 0.9330127018922194093, 0.9330127018922194093, 1.000000000000000000, 0.8660254037844387076, 1.000000000000000000, 0.8660254037844387076, 1.000000000000000000, 0.9330127018922194093, 0.9330127018922194093 ) ) 
 REPRESENTATION_ITEM ( '' )  );
#55205 = CARTESIAN_POINT ( 'NONE',  ( 2.229367062500001939, 4.020833334698926009, 3.861377020970579999 ) ) ;
#55206 = CARTESIAN_POINT ( 'NONE',  ( 5.000000000000000000, 1.625000002731184834, -6.123233995736766282E-16 ) ) ;
#55207 = VECTOR ( 'NONE', #39484, 1000.000000000000000 ) ;
#55208 = CARTESIAN_POINT ( 'NONE',  ( 2.499999999999998668, -82.33333333333332860, -4.330127018922193649 ) ) ;
#55209 = CARTESIAN_POINT ( 'NONE',  ( -4.458734124999999437, 14.43750000136559386, 0.000000000000000000 ) ) ;
#55210 = CARTESIAN_POINT ( 'NONE',  ( -3.535250795749689387E-16, -74.25000000000000000, -5.773502691896257311 ) ) ;
#55211 = CARTESIAN_POINT ( 'NONE',  ( 1.060575238724906964E-15, 9.375000002731184168, 5.773502691896257311 ) ) ;
#55212 = VERTEX_POINT ( 'NONE', #19700 ) ;
#55213 = CARTESIAN_POINT ( 'NONE',  ( 0.000000000000000000, -120.0000000000000000, 5.000000000000000000 ) ) ;
#55214 = VERTEX_POINT ( 'NONE', #39310 ) ;
#55215 = CARTESIAN_POINT ( 'NONE',  ( -6.972266317189433020E-16, -54.12499999726880162, -5.000000000000000000 ) ) ;
#55216 = CARTESIAN_POINT ( 'NONE',  ( 4.458734124999998549, -41.72916666530107932, -2.574251347313721627 ) ) ;
#55217 = CARTESIAN_POINT ( 'NONE',  ( 1.975475456537005874E-15, -59.62499999726880873, 5.000000000000000000 ) ) ;
#55218 = CARTESIAN_POINT ( 'NONE',  ( -4.999999999999999112, -41.79166666393548013, 2.886751345948131764 ) ) ;
#55219 = EDGE_LOOP ( 'NONE', ( #6983, #2614, #10890, #6020 ) ) ;
#55220 = CARTESIAN_POINT ( 'NONE',  ( -2.229367062500000163, -20.47916666530107221, -3.861377020970580443 ) ) ;
#55221 = ORIENTED_EDGE ( 'NONE', *, *, #36967, .T. ) ;
#55222 = CARTESIAN_POINT ( 'NONE',  ( -2.500000000000000444, -87.16666666666667140, -4.330127018922193649 ) ) ;
#55223 = DIRECTION ( 'NONE',  ( 0.000000000000000000, -1.000000000000000000, 0.000000000000000000 ) ) ;
#55224 = CARTESIAN_POINT ( 'NONE',  ( 5.000000000000000000, -88.37499999726880162, -6.123233995736766282E-16 ) ) ;
#55226 = VERTEX_POINT ( 'NONE', #14866 ) ;
#55225 = CARTESIAN_POINT ( 'NONE',  ( -6.972266317189433020E-16, -20.12499999726881228, -5.000000000000000000 ) ) ;
#55227 = CARTESIAN_POINT ( 'NONE',  ( -51.75738570946856498, -141.7500000000000284, 3.805975901505576964 ) ) ;
#55228 = CARTESIAN_POINT ( 'NONE',  ( -2.229367062500000163, -30.72916666530107221, -3.861377020970580443 ) ) ;
#55229 = CARTESIAN_POINT ( 'NONE',  ( -2.500000000000000444, -50.16666666666666430, -4.330127018922193649 ) ) ;
#55230 = VERTEX_POINT ( 'NONE', #49292 ) ;
#55231 = ADVANCED_FACE ( 'NONE', ( #59263 ), #5232, .T. ) ;
#55232 = APPLICATION_PROTOCOL_DEFINITION ( 'draft international standard', 'automotive_design', 1998, #23256 ) ;
#55233 = CARTESIAN_POINT ( 'NONE',  ( -4.458734124999999437, -75.31249999863440792, 0.000000000000000000 ) ) ;
#55234 = CARTESIAN_POINT ( 'NONE',  ( -4.458734124999998549, -109.4791666653010651, 2.574251347313722516 ) ) ;
#55235 = CARTESIAN_POINT ( 'NONE',  ( 1.975475456537005874E-15, -23.75000000000000000, 5.000000000000000000 ) ) ;
#55236 = ORIENTED_EDGE ( 'NONE', *, *, #45234, .F. ) ;
#55237 = CARTESIAN_POINT ( 'NONE',  ( -5.000000000000000000, -166.6250000027312126, -6.123233995736766282E-16 ) ) ;
#55238 = CARTESIAN_POINT ( 'NONE',  ( -52.80376928212989185, -142.1250000013656063, -4.297418129356378458 ) ) ;
#55239 = CARTESIAN_POINT ( 'NONE',  ( -3.152548672688508926E-16, -76.81249999863440792, -5.148502694627439702 ) ) ;
#55240 = CARTESIAN_POINT ( 'NONE',  ( -56.66612745406270335, -135.4375000027312410, -5.149110718188516067 ) ) ;
#55241 = CARTESIAN_POINT ( 'NONE',  ( 2.229367062499998831, -44.64583333196774362, -3.861377020970580887 ) ) ;
#55242 = CARTESIAN_POINT ( 'NONE',  ( -4.458734124999999437, -141.2500000013656063, -1.846868145590735644 ) ) ;
#55243 = AXIS2_PLACEMENT_3D ( 'NONE', #46769, #8174, #22335 ) ;
#55244 = CARTESIAN_POINT ( 'NONE',  ( 1.339745962155609149, 24.29465819873852084, 5.000000000000003553 ) ) ;
#55245 = CARTESIAN_POINT ( 'NONE',  ( -4.458734124999999437, -51.39583333196773651, -2.574251347313719407 ) ) ;
#55246 = CARTESIAN_POINT ( 'NONE',  ( 2.229367062499998831, -44.64583333196774362, -3.861377020970580887 ) ) ;
#55247 = CARTESIAN_POINT ( 'NONE',  ( -6.972266317189433020E-16, -73.25000000000000000, -5.000000000000000000 ) ) ;
#55248 = AXIS2_PLACEMENT_3D ( 'NONE', #9297, #4475, #48846 ) ;
#55249 = CARTESIAN_POINT ( 'NONE',  ( -3.152548672688508926E-16, -18.56249999863440792, -5.148502694627439702 ) ) ;
#55250 = CARTESIAN_POINT ( 'NONE',  ( 5.000000000000000888, -102.5833333333333428, 2.886751345948126879 ) ) ;
#55251 = CARTESIAN_POINT ( 'NONE',  ( 4.458734125000000326, -141.6250000013656631, -1.846868145590734978 ) ) ;
#55252 = CARTESIAN_POINT ( 'NONE',  ( 9.457646018065525792E-16, -40.31249999863440081, 5.148502694627439702 ) ) ;
#55253 = CARTESIAN_POINT ( 'NONE',  ( 2.499999999999998668, 4.791666669397852907, -4.330127018922193649 ) ) ;
#55254 = DIRECTION ( 'NONE',  ( 0.000000000000000000, 0.000000000000000000, 1.000000000000000000 ) ) ;
#55255 = CARTESIAN_POINT ( 'NONE',  ( -56.48576386720575471, -129.7500000013656063, -4.591703134518078322 ) ) ;
#55256 = CARTESIAN_POINT ( 'NONE',  ( -4.458734124999998549, -71.47916666530107932, 2.574251347313722516 ) ) ;
#55257 = CARTESIAN_POINT ( 'NONE',  ( -2.071067811865507036, -166.6875000000000284, -4.999999999999968914 ) ) ;
#55258 = CARTESIAN_POINT ( 'NONE',  ( 2.499999999999998668, -30.20833333060214443, -4.330127018922193649 ) ) ;
#55259 = VECTOR ( 'NONE', #53393, 1000.000000000000000 ) ;
#55260 = CARTESIAN_POINT ( 'NONE',  ( -2.229367062500000163, -1.729166665301071992, -3.861377020970580443 ) ) ;
#55261 = VERTEX_POINT ( 'NONE', #26125 ) ;
#55262 = CARTESIAN_POINT ( 'NONE',  ( -6.972266317189433020E-16, 24.87500000273118417, -5.000000000000000000 ) ) ;
#55263 = CARTESIAN_POINT ( 'NONE',  ( 2.500000000000002220, -57.66666666666667140, 4.330127018922192761 ) ) ;
#55265 = CARTESIAN_POINT ( 'NONE',  ( 4.458734124999998549, -35.72916666530107221, -2.574251347313721627 ) ) ;
#55264 = CARTESIAN_POINT ( 'NONE',  ( -4.458734124999999437, -89.39583333196773651, -2.574251347313719407 ) ) ;
#55266 = DIRECTION ( 'NONE',  ( -0.000000000000000000, 1.000000000000000000, -0.000000000000000000 ) ) ;
#55267 = CARTESIAN_POINT ( 'NONE',  ( 4.458734124999999437, -81.06249999863440792, -5.460374474430324690E-16 ) ) ;
#55268 = CARTESIAN_POINT ( 'NONE',  ( -3.152548672688508926E-16, 20.18750000136559208, -5.148502694627439702 ) ) ;
#55269 = CARTESIAN_POINT ( 'NONE',  ( -1.339745962155610925, -52.79465819873851729, 5.000000000000000000 ) ) ;
#55270 = CARTESIAN_POINT ( 'NONE',  ( -56.48576386720575471, -137.7500000013656063, -4.591703134518078322 ) ) ;
#55271 = CARTESIAN_POINT ( 'NONE',  ( -4.458734124999997661, -9.229166665301068662, 2.574251347313722516 ) ) ;
#55272 = CARTESIAN_POINT ( 'NONE',  ( -2.229367062499996610, 20.60416666803225993, 3.861377020970582219 ) ) ;
#55273 = CARTESIAN_POINT ( 'NONE',  ( -2.229367062499996610, -47.39583333196774362, 3.861377020970582219 ) ) ;
#55274 = CARTESIAN_POINT ( 'NONE',  ( 7.500000000000000000, 4.330127018922190096, -7.422398894150032511 ) ) ;
#55275 = CARTESIAN_POINT ( 'NONE',  ( 9.457646018065525792E-16, -86.06249999863439371, 5.148502694627439702 ) ) ;
#55276 = CARTESIAN_POINT ( 'NONE',  ( -2.229367062500000163, -3.479166665301069994, -3.861377020970580443 ) ) ;
#55277 = CARTESIAN_POINT ( 'NONE',  ( -4.330127018922205195, 30.00000000000000000, -7.499999999999943157 ) ) ;
#55278 = ORIENTED_EDGE ( 'NONE', *, *, #45607, .T. ) ;
#55279 = CARTESIAN_POINT ( 'NONE',  ( 2.229367062499998831, -27.89583333196774007, -3.861377020970580887 ) ) ;
#55280 =( BOUNDED_CURVE ( )  B_SPLINE_CURVE ( 2, ( #7093, #46322, #32150, #22204, #47275, #52102, #36671, #12229, #41803 ),
 .UNSPECIFIED., .F., .F. ) 
 B_SPLINE_CURVE_WITH_KNOTS ( ( 3, 2, 2, 2, 3 ),
 ( 0.06875000000000000555, 0.06944444444444444753, 0.07083333333333333148, 0.07222222222222221544, 0.07291666666666667129 ),
 .UNSPECIFIED. ) 
 CURVE ( )  GEOMETRIC_REPRESENTATION_ITEM ( )  RATIONAL_B_SPLINE_CURVE ( ( 0.9330127018922194093, 0.9330127018922200755, 1.000000000000000000, 0.8660254037844387076, 1.000000000000000000, 0.8660254037844387076, 1.000000000000000000, 0.9330127018922187432, 0.9330127018922194093 ) ) 
 REPRESENTATION_ITEM ( '' )  );
#55281 = CARTESIAN_POINT ( 'NONE',  ( -52.80376928212989185, -132.1250000013656347, -4.297418129356379346 ) ) ;
#55282 = CARTESIAN_POINT ( 'NONE',  ( -4.458734124999999437, -74.31249999863440792, 0.000000000000000000 ) ) ;
#55283 = CARTESIAN_POINT ( 'NONE',  ( -4.458734124999998549, 28.52083333469892423, 2.574251347313722516 ) ) ;
#55284 = CARTESIAN_POINT ( 'NONE',  ( -4.458734124999999437, 22.68750000136559564, 0.000000000000000000 ) ) ;
#55285 = DIRECTION ( 'NONE',  ( -0.000000000000000000, 1.000000000000000000, -0.000000000000000000 ) ) ;
#55286 = CARTESIAN_POINT ( 'NONE',  ( 1.062108568985190270E-13, -26.12499999726881583, -4.999999999999999112 ) ) ;
#55287 = CARTESIAN_POINT ( 'NONE',  ( 4.458734124999998549, -76.97916666530106511, -2.574251347313721627 ) ) ;
#55288 = CARTESIAN_POINT ( 'NONE',  ( 1.060575238724906964E-15, -59.74999999999999289, 5.773502691896257311 ) ) ;
#55289 = DIRECTION ( 'NONE',  ( -0.000000000000000000, 1.000000000000000000, -0.000000000000000000 ) ) ;
#55290 = CARTESIAN_POINT ( 'NONE',  ( 5.000000000000000000, 23.70833333606451632, -2.886751345948129988 ) ) ;
#55291 = ORIENTED_EDGE ( 'NONE', *, *, #2434, .F. ) ;
#55292 = CARTESIAN_POINT ( 'NONE',  ( 1.975475456537005874E-15, -56.75000000000000000, 5.000000000000000000 ) ) ;
#55293 = VECTOR ( 'NONE', #42880, 1000.000000000000000 ) ;
#55294 = CARTESIAN_POINT ( 'NONE',  ( -2.499999999999996447, -56.70833333060214443, 4.330127018922195425 ) ) ;
#55296 = CARTESIAN_POINT ( 'NONE',  ( -5.000000000000000000, -25.08333333333333215, -2.886751345948128211 ) ) ;
#55295 = CARTESIAN_POINT ( 'NONE',  ( 1.339745962155612702, -0.2946581987385212820, -5.000000000000000000 ) ) ;
#55297 = CARTESIAN_POINT ( 'NONE',  ( 9.457646018065525792E-16, -28.06249999863440081, 5.148502694627439702 ) ) ;
#55298 =( REPRESENTATION_RELATIONSHIP ('NONE','NONE', #27855, #14320 ) REPRESENTATION_RELATIONSHIP_WITH_TRANSFORMATION ( #35928 )SHAPE_REPRESENTATION_RELATIONSHIP( ) );
#55299 = CIRCLE ( 'NONE', #59362, 5.000000000000000000 ) ;
#55300 = CARTESIAN_POINT ( 'NONE',  ( -4.458734124999997661, -90.22916666530106511, 2.574251347313722516 ) ) ;
#55301 = CARTESIAN_POINT ( 'NONE',  ( 5.000000000000000888, -21.45833333060215153, 2.886751345948126879 ) ) ;
#55303 = ORIENTED_EDGE ( 'NONE', *, *, #56327, .F. ) ;
#55302 = CARTESIAN_POINT ( 'NONE',  ( 4.458734125000001214, -55.89583333196773651, 2.574251347313718519 ) ) ;
#55304 = CARTESIAN_POINT ( 'NONE',  ( -6.972266317189433020E-16, -65.24999999999998579, -5.000000000000000000 ) ) ;
#55305 = CARTESIAN_POINT ( 'NONE',  ( 1.975475456537005874E-15, -74.62499999726880162, 5.000000000000000000 ) ) ;
#55307 = ORIENTED_EDGE ( 'NONE', *, *, #53172, .F. ) ;
#55306 = CARTESIAN_POINT ( 'NONE',  ( 9.457646018065525792E-16, -2.312499998634407028, 5.148502694627439702 ) ) ;
#55308 = CARTESIAN_POINT ( 'NONE',  ( -55.35523342533222291, -149.3125000013656063, 4.444560631937231499 ) ) ;
#55309 = CARTESIAN_POINT ( 'NONE',  ( 2.499999999999998668, -67.33333333333332860, -4.330127018922193649 ) ) ;
#55310 = CARTESIAN_POINT ( 'NONE',  ( -1.846868145590734756, -150.3750000013655779, -4.458734125000000326 ) ) ;
#55311 = CARTESIAN_POINT ( 'NONE',  ( 2.229367062500001939, -44.22916666530106511, 3.861377020970579999 ) ) ;
#55312 = CARTESIAN_POINT ( 'NONE',  ( -1.339745962155610925, -15.66965819600733134, 5.000000000000000000 ) ) ;
#55313 =( BOUNDED_CURVE ( )  B_SPLINE_CURVE ( 2, ( #55968, #17354, #45351, #30874, #60479, #16404, #21552, #36022, #11568 ),
 .UNSPECIFIED., .F., .F. ) 
 B_SPLINE_CURVE_WITH_KNOTS ( ( 3, 2, 2, 2, 3 ),
 ( 0.1854166666666666741, 0.1861111111111111160, 0.1875000000000000000, 0.1888888888888888840, 0.1895833333333333259 ),
 .UNSPECIFIED. ) 
 CURVE ( )  GEOMETRIC_REPRESENTATION_ITEM ( )  RATIONAL_B_SPLINE_CURVE ( ( 0.9330127018922194093, 0.9330127018922194093, 1.000000000000000000, 0.8660254037844387076, 1.000000000000000000, 0.8660254037844387076, 1.000000000000000000, 0.9330127018922194093, 0.9330127018922194093 ) ) 
 REPRESENTATION_ITEM ( '' )  );
#55314 = CARTESIAN_POINT ( 'NONE',  ( -3.535533905932738641, -159.3750000000000284, 3.535533905932737309 ) ) ;
#55315 = DIRECTION ( 'NONE',  ( 0.000000000000000000, 0.000000000000000000, 1.000000000000000000 ) ) ;
#55316 = CARTESIAN_POINT ( 'NONE',  ( -58.80597590150559739, -152.0000000000000284, 3.242614290531460330 ) ) ;
#55317 = CARTESIAN_POINT ( 'NONE',  ( -4.458734124999999437, -13.64583333196774007, -2.574251347313719407 ) ) ;
#55318 = CARTESIAN_POINT ( 'NONE',  ( 4.458734125000001214, -50.14583333196773651, 2.574251347313718519 ) ) ;
#55319 = CARTESIAN_POINT ( 'NONE',  ( -2.500000000000000444, 0.8333333333333317050, -4.330127018922193649 ) ) ;
#55320 = CARTESIAN_POINT ( 'NONE',  ( 2.730187237215162345E-16, -143.1875000013656063, -4.458734124999999437 ) ) ;
#55321 = CARTESIAN_POINT ( 'NONE',  ( 4.458734124999998549, -96.97916666530106511, -2.574251347313721627 ) ) ;
#55322 = CARTESIAN_POINT ( 'NONE',  ( 1.975475456537005874E-15, -87.62499999726880162, 5.000000000000000000 ) ) ;
#55323 = ORIENTED_EDGE ( 'NONE', *, *, #31885, .T. ) ;
#55324 = DIRECTION ( 'NONE',  ( 0.000000000000000000, 0.000000000000000000, -1.000000000000000000 ) ) ;
#55325 = CARTESIAN_POINT ( 'NONE',  ( 4.458734125000001214, 27.85416666803225993, 2.574251347313718519 ) ) ;
#55326 = CARTESIAN_POINT ( 'NONE',  ( -51.19402409849444524, -146.6250000027312126, -3.242614290531456334 ) ) ;
#55327 = ORIENTED_EDGE ( 'NONE', *, *, #48437, .T. ) ;
#55328 = CARTESIAN_POINT ( 'NONE',  ( -2.229367062500000163, -3.479166665301069994, -3.861377020970580443 ) ) ;
#55329 = CARTESIAN_POINT ( 'NONE',  ( -6.972266317189433020E-16, -19.25000000000000000, -5.000000000000000000 ) ) ;
#55330 = CARTESIAN_POINT ( 'NONE',  ( 9.457646018065525792E-16, -16.31249999863440436, 5.148502694627439702 ) ) ;
#55331 = CARTESIAN_POINT ( 'NONE',  ( -4.999999999999998224, 9.083333333333333925, 2.886751345948131764 ) ) ;
#55332 = CARTESIAN_POINT ( 'NONE',  ( 2.229367062499998831, -5.645833331967740953, -3.861377020970580887 ) ) ;
#55333 = DIRECTION ( 'NONE',  ( -0.000000000000000000, 1.000000000000000000, -0.000000000000000000 ) ) ;
#55334 = CARTESIAN_POINT ( 'NONE',  ( -4.458734125000000326, -149.8750000013655779, 1.846868145590734089 ) ) ;
#55335 = AXIS2_PLACEMENT_3D ( 'NONE', #28174, #1072, #6517 ) ;
#55336 = CARTESIAN_POINT ( 'NONE',  ( 2.229367062500001939, 16.77083333469892779, 3.861377020970579999 ) ) ;
#55337 = VERTEX_POINT ( 'NONE', #20019 ) ;
#55338 = CARTESIAN_POINT ( 'NONE',  ( -1.339745962155610925, -26.66965819600732956, 5.000000000000000000 ) ) ;
#55339 = CARTESIAN_POINT ( 'NONE',  ( -2.500000000000000444, -13.16666666666666607, -4.330127018922193649 ) ) ;
#55340 = CARTESIAN_POINT ( 'NONE',  ( -3.152548672688508926E-16, -17.56249999863440792, -5.148502694627439702 ) ) ;
#55341 = ADVANCED_FACE ( 'NONE', ( #35145 ), #45101, .T. ) ;
#55342 = VECTOR ( 'NONE', #6493, 1000.000000000000000 ) ;
#55343 = FACE_OUTER_BOUND ( 'NONE', #18450, .T. ) ;
#55344 = CARTESIAN_POINT ( 'NONE',  ( 5.000000000000000000, -3.416666666666665186, -2.886751345948130876 ) ) ;
#55345 = CARTESIAN_POINT ( 'NONE',  ( -59.44456063193725015, -150.5625000013656063, -0.3552334253322034230 ) ) ;
#55346 = CARTESIAN_POINT ( 'NONE',  ( 5.000000000000000000, -49.29166666393547303, -2.886751345948129988 ) ) ;
#55347 = CARTESIAN_POINT ( 'NONE',  ( -7.922281120364393914, 4.573931137438271399, -8.047472243342930653 ) ) ;
#55348 = CARTESIAN_POINT ( 'NONE',  ( -3.152548672688508926E-16, 9.437500001365593860, -5.148502694627439702 ) ) ;
#55349 = CARTESIAN_POINT ( 'NONE',  ( -1.339745962155555858, -9.080341798530296771, -5.000000000000032863 ) ) ;
#55350 = CARTESIAN_POINT ( 'NONE',  ( 0.000000000000000000, -120.0000000000000000, 0.000000000000000000 ) ) ;
#55351 = CARTESIAN_POINT ( 'NONE',  ( -4.458734124999999437, 11.60416666803225993, -2.574251347313719407 ) ) ;
#55352 = CARTESIAN_POINT ( 'NONE',  ( 2.229367062500001939, -68.97916666530107932, 3.861377020970579999 ) ) ;
#55353 = CARTESIAN_POINT ( 'NONE',  ( -3.152548672688508926E-16, -13.81249999863440259, -5.148502694627439702 ) ) ;
#55354 = CARTESIAN_POINT ( 'NONE',  ( 2.499999999999998668, 3.666666666666665186, -4.330127018922193649 ) ) ;
#55355 = CARTESIAN_POINT ( 'NONE',  ( 4.458734125000000326, -162.3750000013655779, -1.846868145590734978 ) ) ;
#55356 = CARTESIAN_POINT ( 'NONE',  ( -4.999999999999998224, -40.79166666393548724, 2.886751345948131764 ) ) ;
#55357 = CARTESIAN_POINT ( 'NONE',  ( -3.152548672688508926E-16, -57.56249999863439371, -5.148502694627439702 ) ) ;
#55358 = CARTESIAN_POINT ( 'NONE',  ( 2.500000000000002220, -95.54166666393547303, 4.330127018922192761 ) ) ;
#55359 = LINE ( 'NONE', #11273, #40111 ) ;
#55360 = ADVANCED_FACE ( 'NONE', ( #35781 ), #20345, .T. ) ;
#55361 = CYLINDRICAL_SURFACE ( 'NONE', #41917, 5.000000000000000000 ) ;
#55362 = CARTESIAN_POINT ( 'NONE',  ( -53.33387254593731086, -151.9375000027312410, 5.149110718188520508 ) ) ;
#55363 = CARTESIAN_POINT ( 'NONE',  ( 4.458734124999999437, -35.81249999863440792, -5.460374474430324690E-16 ) ) ;
#55364 = CARTESIAN_POINT ( 'NONE',  ( -5.000000000000000000, -43.08333333333332860, -2.886751345948128211 ) ) ;
#55365 = CARTESIAN_POINT ( 'NONE',  ( -4.999999999999998224, -107.9166666666666572, 2.886751345948131764 ) ) ;
#55366 = ORIENTED_EDGE ( 'NONE', *, *, #1987, .F. ) ;
#55367 = CARTESIAN_POINT ( 'NONE',  ( 2.229367062500001939, -106.9791666653010651, 3.861377020970579999 ) ) ;
#55368 = CARTESIAN_POINT ( 'NONE',  ( -4.458734124999999437, -3.645833331967739621, -2.574251347313719407 ) ) ;
#55369 = DIRECTION ( 'NONE',  ( -0.000000000000000000, 1.000000000000000000, -0.000000000000000000 ) ) ;
#55370 = CARTESIAN_POINT ( 'NONE',  ( -3.535250795749689387E-16, -4.249999999999996447, -5.773502691896257311 ) ) ;
#55371 = CARTESIAN_POINT ( 'NONE',  ( 9.457646018065525792E-16, -72.06249999863439371, 5.148502694627439702 ) ) ;
#55372 = DIRECTION ( 'NONE',  ( 0.000000000000000000, 1.000000000000000000, 0.000000000000000000 ) ) ;
#55373 = CARTESIAN_POINT ( 'NONE',  ( 5.000000000000000888, -5.458333330602148870, 2.886751345948126879 ) ) ;
#55375 = ORIENTED_EDGE ( 'NONE', *, *, #62111, .T. ) ;
#55374 = CARTESIAN_POINT ( 'NONE',  ( 2.229367062499998831, -39.64583333196773651, -3.861377020970580887 ) ) ;
#55376 = CARTESIAN_POINT ( 'NONE',  ( 1.339745962155615144, -22.58034179853029144, 4.999999999999999112 ) ) ;
#55378 = EDGE_LOOP ( 'NONE', ( #62302, #88, #24605, #22795 ) ) ;
#55377 = CARTESIAN_POINT ( 'NONE',  ( -2.229367062500000163, 12.27083333469892601, -3.861377020970580443 ) ) ;
#55379 = CARTESIAN_POINT ( 'NONE',  ( 2.500000000000002220, -52.66666666666666430, 4.330127018922192761 ) ) ;
#55380 = CARTESIAN_POINT ( 'NONE',  ( -2.229367062499996610, -32.39583333196773651, 3.861377020970582219 ) ) ;
#55381 = CARTESIAN_POINT ( 'NONE',  ( -2.499999999999996447, -3.833333333333334370, 4.330127018922195425 ) ) ;
#55382 = CARTESIAN_POINT ( 'NONE',  ( -4.458734124999999437, -77.31249999863440792, 0.000000000000000000 ) ) ;
#55383 = CARTESIAN_POINT ( 'NONE',  ( 4.458734124999999437, -140.7500000013655779, 1.846868145590737864 ) ) ;
#55384 = CARTESIAN_POINT ( 'NONE',  ( 4.458734125000001214, -81.89583333196773651, 2.574251347313718519 ) ) ;
#55385 = CARTESIAN_POINT ( 'NONE',  ( -54.64476657466781973, -137.0625000013656063, -4.444560631937228834 ) ) ;
#55386 =( BOUNDED_CURVE ( )  B_SPLINE_CURVE ( 2, ( #37933, #37300, #32791, #52421, #12850, #8655, #57565, #12222, #3841 ),
 .UNSPECIFIED., .F., .F. ) 
 B_SPLINE_CURVE_WITH_KNOTS ( ( 3, 2, 2, 2, 3 ),
 ( 0.7732142857142857428, 0.7738095238095238360, 0.7750000000000000222, 0.7761904761904762085, 0.7767857142857143016 ),
 .UNSPECIFIED. ) 
 CURVE ( )  GEOMETRIC_REPRESENTATION_ITEM ( )  RATIONAL_B_SPLINE_CURVE ( ( 0.9330127018922194093, 0.9330127018922194093, 1.000000000000000000, 0.8660254037844387076, 1.000000000000000000, 0.8660254037844387076, 1.000000000000000000, 0.9330127018922194093, 0.9330127018922194093 ) ) 
 REPRESENTATION_ITEM ( '' )  );
#55387 = CARTESIAN_POINT ( 'NONE',  ( 2.229367062499998831, -37.89583333196773651, -3.861377020970580887 ) ) ;
#55388 = ORIENTED_EDGE ( 'NONE', *, *, #53805, .F. ) ;
#55389 = FACE_OUTER_BOUND ( 'NONE', #33330, .T. ) ;
#55390 = ORIENTED_EDGE ( 'NONE', *, *, #46144, .F. ) ;
#55391 = CARTESIAN_POINT ( 'NONE',  ( -3.152548672688508926E-16, -76.81249999863440792, -5.148502694627439702 ) ) ;
#55392 = FACE_OUTER_BOUND ( 'NONE', #34933, .T. ) ;
#55393 = VERTEX_POINT ( 'NONE', #25480 ) ;
#55394 = CARTESIAN_POINT ( 'NONE',  ( -5.000000000000000000, -14.95833333060214621, -2.886751345948128211 ) ) ;
#55395 = CARTESIAN_POINT ( 'NONE',  ( 5.000000000000000000, -31.29166666393548724, -2.886751345948130876 ) ) ;
#55396 = CARTESIAN_POINT ( 'NONE',  ( -3.152548672688508926E-16, -63.81249999863440792, -5.148502694627439702 ) ) ;
#55397 = CARTESIAN_POINT ( 'NONE',  ( -2.229367062500000163, -2.729166665301069550, -3.861377020970580443 ) ) ;
#55398 = ORIENTED_EDGE ( 'NONE', *, *, #31398, .T. ) ;
#55399 = CARTESIAN_POINT ( 'NONE',  ( 2.500000000000002220, 3.458333336064517205, 4.330127018922192761 ) ) ;
#55400 =( BOUNDED_CURVE ( )  B_SPLINE_CURVE ( 2, ( #59124, #20844, #25668, #35635, #6375, #25341, #45596, #55583, #40447 ),
 .UNSPECIFIED., .F., .F. ) 
 B_SPLINE_CURVE_WITH_KNOTS ( ( 3, 2, 2, 2, 3 ),
 ( 0.04375000000000000416, 0.04444444444444444614, 0.04583333333333333010, 0.04722222222222222099, 0.04791666666666666990 ),
 .UNSPECIFIED. ) 
 CURVE ( )  GEOMETRIC_REPRESENTATION_ITEM ( )  RATIONAL_B_SPLINE_CURVE ( ( 0.9330127018922192983, 0.9330127018922196314, 1.000000000000000000, 0.8660254037844387076, 1.000000000000000000, 0.8660254037844387076, 1.000000000000000000, 0.9330127018922189652, 0.9330127018922192983 ) ) 
 REPRESENTATION_ITEM ( '' )  );
#55401 = LINE ( 'NONE', #26437, #36827 ) ;
#55402 = VERTEX_POINT ( 'NONE', #25808 ) ;
#55403 = DIRECTION ( 'NONE',  ( 0.000000000000000000, 0.000000000000000000, 1.000000000000000000 ) ) ;
#55404 = CARTESIAN_POINT ( 'NONE',  ( 4.458734125000001214, 9.104166668032261711, 2.574251347313718519 ) ) ;
#55405 = CARTESIAN_POINT ( 'NONE',  ( -6.972266317189433020E-16, -78.24999999999998579, -5.000000000000000000 ) ) ;
#55406 = CARTESIAN_POINT ( 'NONE',  ( 1.846868145590736310, -162.6250000013656063, 4.458734124999997661 ) ) ;
#55407 = CARTESIAN_POINT ( 'NONE',  ( 1.975475456537005874E-15, 19.37500000273118772, 5.000000000000000000 ) ) ;
#55408 = ORIENTED_EDGE ( 'NONE', *, *, #22394, .T. ) ;
#55409 = CARTESIAN_POINT ( 'NONE',  ( 4.458734125000000326, -82.89583333196773651, 2.574251347313718519 ) ) ;
#55410 = DIRECTION ( 'NONE',  ( -0.000000000000000000, 1.000000000000000000, -0.000000000000000000 ) ) ;
#55411 = CARTESIAN_POINT ( 'NONE',  ( 2.229367062500001939, -4.979166665301071326, 3.861377020970579999 ) ) ;
#55412 = EDGE_CURVE ( 'NONE', #28777, #43561, #44456, .T. ) ;
#55413 = DIRECTION ( 'NONE',  ( 0.000000000000000000, 0.000000000000000000, 1.000000000000000000 ) ) ;
#55414 = CARTESIAN_POINT ( 'NONE',  ( -7.499999999999999112, 1.443375672974061219, -7.063244554130000630 ) ) ;
#55415 = CARTESIAN_POINT ( 'NONE',  ( -4.458734124999999437, -68.64583333196773651, -2.574251347313719407 ) ) ;
#55416 = CARTESIAN_POINT ( 'NONE',  ( 5.000000000000000888, -30.45833333060214443, 2.886751345948126879 ) ) ;
#55417 = CARTESIAN_POINT ( 'NONE',  ( -1.339745962155610925, -20.79465819873852084, 5.000000000000000000 ) ) ;
#55418 = CARTESIAN_POINT ( 'NONE',  ( 2.229367062500001939, 29.02083333469892779, 3.861377020970579999 ) ) ;
#55419 = CARTESIAN_POINT ( 'NONE',  ( 5.000000000000000000, -104.4166666666666572, -2.886751345948130876 ) ) ;
#55420 = CARTESIAN_POINT ( 'NONE',  ( -3.152548672688508926E-16, 28.43750000136559564, -5.148502694627439702 ) ) ;
#55421 = CARTESIAN_POINT ( 'NONE',  ( -3.152548672688508926E-16, -51.56249999863441502, -5.148502694627439702 ) ) ;
#55422 = CARTESIAN_POINT ( 'NONE',  ( 2.229367062499998831, -33.89583333196772941, -3.861377020970580887 ) ) ;
#55423 = CARTESIAN_POINT ( 'NONE',  ( -2.229367062500000163, 3.270833334698929118, -3.861377020970580443 ) ) ;
#55424 = STYLED_ITEM ( 'NONE', ( #2553 ), #3382 ) ;
#55425 = CARTESIAN_POINT ( 'NONE',  ( 3.061616997868383141E-16, -149.8750000027312126, -5.000000000000000000 ) ) ;
#55426 = CARTESIAN_POINT ( 'NONE',  ( -2.499999999999996447, 19.16666666666666430, 4.330127018922195425 ) ) ;
#55427 = CARTESIAN_POINT ( 'NONE',  ( -3.535533905932738641, -143.5000000027311842, 3.535533905932737309 ) ) ;
#55429 = EDGE_CURVE ( 'NONE', #63665, #6339, #49464, .T. ) ;
#55428 = CARTESIAN_POINT ( 'NONE',  ( 2.071067811865370256, -158.8125000000000284, -5.000000000000105693 ) ) ;
#55430 = CARTESIAN_POINT ( 'NONE',  ( 2.229367062500001939, -43.97916666530106511, 3.861377020970579999 ) ) ;
#55431 = CARTESIAN_POINT ( 'NONE',  ( -5.000000000000000000, -80.87499999726881583, 0.000000000000000000 ) ) ;
#55432 = CARTESIAN_POINT ( 'NONE',  ( -50.70258187064364108, -141.3750000013656063, 2.196230717870141014 ) ) ;
#55433 = CARTESIAN_POINT ( 'NONE',  ( 0.000000000000000000, -170.0000000000000000, 0.000000000000000000 ) ) ;
#55434 = CARTESIAN_POINT ( 'NONE',  ( 5.000000000000000000, -37.41666666666666430, -2.886751345948130876 ) ) ;
#55435 = EDGE_CURVE ( 'NONE', #43959, #20764, #60234, .T. ) ;
#55436 = CARTESIAN_POINT ( 'NONE',  ( 2.229367062499998831, -78.89583333196773651, -3.861377020970580887 ) ) ;
#55437 = CARTESIAN_POINT ( 'NONE',  ( 1.846868145590735200, -161.5000000013656063, -4.458734124999999437 ) ) ;
#55438 = DIRECTION ( 'NONE',  ( -0.000000000000000000, 1.000000000000000000, -0.000000000000000000 ) ) ;
#55439 = CARTESIAN_POINT ( 'NONE',  ( -3.535250795749689387E-16, -28.24999999999999645, -5.773502691896257311 ) ) ;
#55440 = CARTESIAN_POINT ( 'NONE',  ( -1.339745962155613812, -57.20534180126148271, -5.000000000000000000 ) ) ;
#55441 = ORIENTED_EDGE ( 'NONE', *, *, #3507, .F. ) ;
#55442 = CARTESIAN_POINT ( 'NONE',  ( 2.229367062499998831, 24.10416666803225993, -3.861377020970580887 ) ) ;
#55443 = EDGE_LOOP ( 'NONE', ( #29087, #50692, #6489, #19508 ) ) ;
#55444 = CARTESIAN_POINT ( 'NONE',  ( 2.500000000000002220, 23.45833333606451632, 4.330127018922192761 ) ) ;
#55445 = CARTESIAN_POINT ( 'NONE',  ( -5.000000000000000000, -2.958333330602146649, -2.886751345948128211 ) ) ;
#55446 = CARTESIAN_POINT ( 'NONE',  ( -3.535250795749689387E-16, 11.74999999999999822, -5.773502691896257311 ) ) ;
#55447 = CARTESIAN_POINT ( 'NONE',  ( -4.458734124999999437, -48.31249999863440792, 0.000000000000000000 ) ) ;
#55448 = CARTESIAN_POINT ( 'NONE',  ( -3.152548672688508926E-16, -11.56249999863440792, -5.148502694627439702 ) ) ;
#55449 = CARTESIAN_POINT ( 'NONE',  ( 7.500000000000000000, -4.730916290271713898, -7.493595886788494198 ) ) ;
#55450 = CARTESIAN_POINT ( 'NONE',  ( -1.339745962155610925, 20.20534180126147916, 5.000000000000000000 ) ) ;
#55451 = DIRECTION ( 'NONE',  ( -0.000000000000000000, 1.000000000000000000, -0.000000000000000000 ) ) ;
#55452 = CARTESIAN_POINT ( 'NONE',  ( 3.061616997868383141E-16, -153.8750000027311842, -5.000000000000000000 ) ) ;
#55453 = CARTESIAN_POINT ( 'NONE',  ( -6.972266317189433020E-16, -62.24999999999999289, -5.000000000000000000 ) ) ;
#55454 = CARTESIAN_POINT ( 'NONE',  ( 5.000000000000000000, -33.50000000000000000, -6.123233995736766282E-16 ) ) ;
#55455 = CYLINDRICAL_SURFACE ( 'NONE', #7913, 5.000000000000000000 ) ;
#55458 = CARTESIAN_POINT ( 'NONE',  ( 9.457646018065525792E-16, -13.31249999863440259, 5.148502694627439702 ) ) ;
#55457 =( BOUNDED_CURVE ( )  B_SPLINE_CURVE ( 2, ( #1582, #59799, #50770, #16676, #50461, #954, #35664, #20554, #10565 ),
 .UNSPECIFIED., .F., .F. ) 
 B_SPLINE_CURVE_WITH_KNOTS ( ( 3, 2, 2, 2, 3 ),
 ( 0.7482142857142857206, 0.7488095238095238138, 0.7500000000000000000, 0.7511904761904761862, 0.7517857142857142794 ),
 .UNSPECIFIED. ) 
 CURVE ( )  GEOMETRIC_REPRESENTATION_ITEM ( )  RATIONAL_B_SPLINE_CURVE ( ( 0.9330127018922194093, 0.9330127018922194093, 1.000000000000000000, 0.8660254037844387076, 1.000000000000000000, 0.8660254037844387076, 1.000000000000000000, 0.9330127018922194093, 0.9330127018922194093 ) ) 
 REPRESENTATION_ITEM ( '' )  );
#55456 = CARTESIAN_POINT ( 'NONE',  ( -1.339745962155613812, -59.20534180126148271, -5.000000000000000000 ) ) ;
#55459 = CARTESIAN_POINT ( 'NONE',  ( -52.53715891517739323, -135.5625000027312126, -4.819101127000233298 ) ) ;
#55460 = CARTESIAN_POINT ( 'NONE',  ( -3.152548672688508926E-16, -61.56249999863440792, -5.148502694627439702 ) ) ;
#55461 = CARTESIAN_POINT ( 'NONE',  ( -4.458734125000001214, -151.1250000013655779, 1.846868145590734089 ) ) ;
#55462 = ADVANCED_FACE ( 'NONE', ( #45421 ), #10370, .T. ) ;
#55463 = CARTESIAN_POINT ( 'NONE',  ( 4.458734124999999437, -64.81249999863440792, -5.460374474430324690E-16 ) ) ;
#55464 = CARTESIAN_POINT ( 'NONE',  ( -53.51423613279429503, -147.5000000013656063, 4.591703134518082763 ) ) ;
#55465 = CARTESIAN_POINT ( 'NONE',  ( 5.000000000000000888, -57.45833333060214443, 2.886751345948126879 ) ) ;
#55466 = ORIENTED_EDGE ( 'NONE', *, *, #48143, .T. ) ;
#55467 = FACE_OUTER_BOUND ( 'NONE', #12107, .T. ) ;
#55468 = ORIENTED_EDGE ( 'NONE', *, *, #9964, .F. ) ;
#55470 = CARTESIAN_POINT ( 'NONE',  ( 1.975475456537005874E-15, -58.75000000000000000, 5.000000000000000000 ) ) ;
#55469 = CYLINDRICAL_SURFACE ( 'NONE', #52305, 5.000000000000000000 ) ;
#55471 = CARTESIAN_POINT ( 'NONE',  ( 2.730187237215162345E-16, -152.1875000013656063, -4.458734124999999437 ) ) ;
#55472 = ORIENTED_EDGE ( 'NONE', *, *, #45902, .F. ) ;
#55473 = AXIS2_PLACEMENT_3D ( 'NONE', #18280, #18597, #33385 ) ;
#55474 = DIRECTION ( 'NONE',  ( -0.000000000000000000, 1.000000000000000000, -0.000000000000000000 ) ) ;
#55475 = CARTESIAN_POINT ( 'NONE',  ( -58.24261429053147765, -128.2500000000000284, -3.805975901505573855 ) ) ;
#55477 = AXIS2_PLACEMENT_3D ( 'NONE', #1823, #56483, #26565 ) ;
#55476 = CARTESIAN_POINT ( 'NONE',  ( 5.000000000000000000, -153.0625000000000284, 2.071067811865478614 ) ) ;
#55478 = CARTESIAN_POINT ( 'NONE',  ( 9.457646018065525792E-16, -47.31249999863440792, 5.148502694627439702 ) ) ;
#55479 = EDGE_LOOP ( 'NONE', ( #3341, #42805, #58523, #28888 ) ) ;
#55480 = CARTESIAN_POINT ( 'NONE',  ( 1.975475456537005874E-15, 17.37500000273118417, 5.000000000000000000 ) ) ;
#55481 = AXIS2_PLACEMENT_3D ( 'NONE', #56050, #36108, #42821 ) ;
#55482 = CARTESIAN_POINT ( 'NONE',  ( 4.458734125000001214, 13.10416666803226171, 2.574251347313718519 ) ) ;
#55483 = CARTESIAN_POINT ( 'NONE',  ( -4.458734124999999437, 23.68750000136559564, 0.000000000000000000 ) ) ;
#55484 = CARTESIAN_POINT ( 'NONE',  ( -56.66612745406270335, -124.4375000027312126, -5.149110718188516067 ) ) ;
#55485 = CARTESIAN_POINT ( 'NONE',  ( 2.500000000000002220, -44.66666666666665719, 4.330127018922192761 ) ) ;
#55486 = CARTESIAN_POINT ( 'NONE',  ( -6.972266317189433020E-16, -36.12499999726880162, -5.000000000000000000 ) ) ;
#55487 = VERTEX_POINT ( 'NONE', #45745 ) ;
#55488 = CARTESIAN_POINT ( 'NONE',  ( -4.458734124999999437, -63.39583333196772941, -2.574251347313719407 ) ) ;
#55489 = CARTESIAN_POINT ( 'NONE',  ( 0.3875187462248268488, 8.436519985393664101, -7.781689322726965230 ) ) ;
#55490 = CARTESIAN_POINT ( 'NONE',  ( 4.458734124999998549, 15.27083333469893134, -2.574251347313721627 ) ) ;
#55491 = CARTESIAN_POINT ( 'NONE',  ( -4.999999999999998224, -62.91666666666665719, 2.886751345948131764 ) ) ;
#55492 = ADVANCED_FACE ( 'NONE', ( #50245 ), #1699, .F. ) ;
#55493 = CARTESIAN_POINT ( 'NONE',  ( -6.972266317189433020E-16, -51.25000000000000000, -5.000000000000000000 ) ) ;
#55494 = EDGE_CURVE ( 'NONE', #39571, #2897, #46658, .T. ) ;
#55495 = CARTESIAN_POINT ( 'NONE',  ( -4.458734124999998549, -56.47916666530107221, 2.574251347313722516 ) ) ;
#55496 = CARTESIAN_POINT ( 'NONE',  ( 5.000000000000000888, -12.45833333060214976, 2.886751345948126879 ) ) ;
#55497 = CARTESIAN_POINT ( 'NONE',  ( 2.499999999999998668, -25.20833333060214443, -4.330127018922193649 ) ) ;
#55498 = CARTESIAN_POINT ( 'NONE',  ( -59.98410592259440222, -147.1250000000000284, -0.3983568153799752487 ) ) ;
#55499 = LINE ( 'NONE', #11414, #56166 ) ;
#55500 = EDGE_CURVE ( 'NONE', #20861, #9561, #7222, .T. ) ;
#55501 = CARTESIAN_POINT ( 'NONE',  ( 2.229367062500001939, -15.22916666530107399, 3.861377020970579999 ) ) ;
#55502 = ORIENTED_EDGE ( 'NONE', *, *, #53014, .F. ) ;
#55503 =( BOUNDED_CURVE ( )  B_SPLINE_CURVE ( 2, ( #60799, #36341, #25094, #44702, #39877, #54692, #10614, #1001, #35387 ),
 .UNSPECIFIED., .F., .F. ) 
 B_SPLINE_CURVE_WITH_KNOTS ( ( 3, 2, 2, 2, 3 ),
 ( 0.3410714285714285809, 0.3416666666666666741, 0.3428571428571428603, 0.3440476190476190466, 0.3446428571428571397 ),
 .UNSPECIFIED. ) 
 CURVE ( )  GEOMETRIC_REPRESENTATION_ITEM ( )  RATIONAL_B_SPLINE_CURVE ( ( 0.9330127018922194093, 0.9330127018922194093, 1.000000000000000000, 0.8660254037844387076, 1.000000000000000000, 0.8660254037844387076, 1.000000000000000000, 0.9330127018922194093, 0.9330127018922194093 ) ) 
 REPRESENTATION_ITEM ( '' )  );
#55504 = CARTESIAN_POINT ( 'NONE',  ( -3.535533905932738641, -169.3750000000000284, 3.535533905932737309 ) ) ;
#55505 = CARTESIAN_POINT ( 'NONE',  ( 9.457646018065525792E-16, -102.0624999986344079, 5.148502694627439702 ) ) ;
#55506 = CARTESIAN_POINT ( 'NONE',  ( -3.535533905932737309, -155.7500000027312126, -3.535533905932738197 ) ) ;
#55507 = ORIENTED_EDGE ( 'NONE', *, *, #20868, .F. ) ;
#55508 = CARTESIAN_POINT ( 'NONE',  ( 9.457646018065525792E-16, -104.3124999986344221, 5.148502694627439702 ) ) ;
#55509 = CARTESIAN_POINT ( 'NONE',  ( -2.229367062500000163, -28.47916666530107221, -3.861377020970580443 ) ) ;
#55510 = CARTESIAN_POINT ( 'NONE',  ( -3.535250795749689387E-16, -63.12499999726880873, -5.773502691896257311 ) ) ;
#55511 = EDGE_CURVE ( 'NONE', #45629, #11153, #47474, .T. ) ;
#55512 = CARTESIAN_POINT ( 'NONE',  ( -59.44456063193725015, -153.8125000013656347, -0.3552334253322034230 ) ) ;
#55513 = CARTESIAN_POINT ( 'NONE',  ( -50.40829686548195099, -143.0000000013655779, -1.485763867205728284 ) ) ;
#55514 = CARTESIAN_POINT ( 'NONE',  ( -4.458734124999997661, -21.22916666530107221, 2.574251347313722516 ) ) ;
#55515 = ADVANCED_FACE ( 'NONE', ( #27853 ), #22733, .T. ) ;
#55516 = CARTESIAN_POINT ( 'NONE',  ( 2.229367062500001939, -62.22916666530106511, 3.861377020970579999 ) ) ;
#55517 = CARTESIAN_POINT ( 'NONE',  ( 0.000000000000000000, -120.0000000000000000, 5.000000000000000000 ) ) ;
#55518 = CARTESIAN_POINT ( 'NONE',  ( -4.458734124999997661, -17.22916666530106866, 2.574251347313722516 ) ) ;
#55519 = CARTESIAN_POINT ( 'NONE',  ( 6.123233995736766282E-16, -120.0000000000000000, -5.000000000000000000 ) ) ;
#55520 = CARTESIAN_POINT ( 'NONE',  ( 5.000000000000000000, -152.0000000000000284, 0.000000000000000000 ) ) ;
#55521 = CARTESIAN_POINT ( 'NONE',  ( -2.500000000000000444, -12.16666666666666607, -4.330127018922193649 ) ) ;
#55522 = EDGE_CURVE ( 'NONE', #22293, #42943, #35954, .T. ) ;
#55523 = CARTESIAN_POINT ( 'NONE',  ( -8.190561711645485556E-16, -150.6875000013656063, 4.458734124999999437 ) ) ;
#55524 = ORIENTED_EDGE ( 'NONE', *, *, #14231, .F. ) ;
#55525 = AXIS2_PLACEMENT_3D ( 'NONE', #34345, #14412, #43058 ) ;
#55526 = CARTESIAN_POINT ( 'NONE',  ( 4.458734125000000326, -45.14583333196774362, 2.574251347313718519 ) ) ;
#55527 = CYLINDRICAL_SURFACE ( 'NONE', #16072, 5.000000000000000000 ) ;
#55528 = CARTESIAN_POINT ( 'NONE',  ( -6.972266317189433020E-16, -63.25000000000000000, -5.000000000000000000 ) ) ;
#55529 = EDGE_CURVE ( 'NONE', #37570, #54241, #53596, .T. ) ;
#55530 = CARTESIAN_POINT ( 'NONE',  ( 1.060575238724906964E-15, 28.24999999999999645, 5.773502691896257311 ) ) ;
#55531 = VECTOR ( 'NONE', #31610, 1000.000000000000000 ) ;
#55532 = CARTESIAN_POINT ( 'NONE',  ( 9.457646018065525792E-16, 2.937500001365594304, 5.148502694627439702 ) ) ;
#55533 = CARTESIAN_POINT ( 'NONE',  ( 1.975475456537005874E-15, -53.62499999726880162, 5.000000000000000000 ) ) ;
#55534 = FACE_OUTER_BOUND ( 'NONE', #30833, .T. ) ;
#55535 = CARTESIAN_POINT ( 'NONE',  ( -7.500000000000000000, -4.330127018922199866, -1.000000000000000888 ) ) ;
#55536 = CARTESIAN_POINT ( 'NONE',  ( -2.229367062500000163, 13.27083333469892779, -3.861377020970580443 ) ) ;
#55537 = CARTESIAN_POINT ( 'NONE',  ( -2.499999999999996447, -81.83333333333332860, 4.330127018922195425 ) ) ;
#55538 = CARTESIAN_POINT ( 'NONE',  ( -2.500000000000000444, 8.958333336064518093, -4.330127018922193649 ) ) ;
#55539 = ORIENTED_EDGE ( 'NONE', *, *, #22, .T. ) ;
#55540 = ORIENTED_EDGE ( 'NONE', *, *, #2076, .F. ) ;
#55541 = CARTESIAN_POINT ( 'NONE',  ( 1.339745962155611592, 26.29465819873852084, 5.000000000000000888 ) ) ;
#55542 = CARTESIAN_POINT ( 'NONE',  ( -3.152548672688508926E-16, -45.56249999863439371, -5.148502694627439702 ) ) ;
#55543 = CARTESIAN_POINT ( 'NONE',  ( -4.458734125000001214, -163.1250000013656063, 1.846868145590734089 ) ) ;
#55544 = CARTESIAN_POINT ( 'NONE',  ( -3.535250795749689387E-16, -42.12499999726880873, -5.773502691896257311 ) ) ;
#55545 = ORIENTED_EDGE ( 'NONE', *, *, #13014, .T. ) ;
#55546 = CARTESIAN_POINT ( 'NONE',  ( 4.458734124999998549, -15.72916666530107399, -2.574251347313721627 ) ) ;
#55547 = ORIENTED_EDGE ( 'NONE', *, *, #12282, .F. ) ;
#55548 = CARTESIAN_POINT ( 'NONE',  ( 5.000000000000000000, -87.50000000000000000, -6.123233995736766282E-16 ) ) ;
#55549 = CARTESIAN_POINT ( 'NONE',  ( -3.152801135295367096, -163.0625000013656063, -3.152801135295367541 ) ) ;
#55550 = CARTESIAN_POINT ( 'NONE',  ( -3.535250795749689387E-16, -87.12499999726880162, -5.773502691896257311 ) ) ;
#55552 = ORIENTED_EDGE ( 'NONE', *, *, #36926, .F. ) ;
#55551 = CARTESIAN_POINT ( 'NONE',  ( 1.975475456537005874E-15, -60.62499999726880162, 5.000000000000000000 ) ) ;
#55553 = CARTESIAN_POINT ( 'NONE',  ( -54.60164318462004474, -140.3750000000000284, -4.984105922594373794 ) ) ;
#55554 = CARTESIAN_POINT ( 'NONE',  ( -2.229367062500000163, -31.72916666530107577, -3.861377020970580443 ) ) ;
#55555 = CARTESIAN_POINT ( 'NONE',  ( 1.975475456537005874E-15, -83.74999999999998579, 5.000000000000000000 ) ) ;
#55556 = VERTEX_POINT ( 'NONE', #56832 ) ;
#55557 = CARTESIAN_POINT ( 'NONE',  ( -4.458734124999999437, -78.39583333196772230, -2.574251347313719407 ) ) ;
#55558 = CARTESIAN_POINT ( 'NONE',  ( -2.229367062500000163, -108.7291666653010651, -3.861377020970580443 ) ) ;
#55559 = CARTESIAN_POINT ( 'NONE',  ( -53.33387254593703375, -136.9375000027311557, 5.149110718188541824 ) ) ;
#55560 = ORIENTED_EDGE ( 'NONE', *, *, #36683, .T. ) ;
#55561 = CARTESIAN_POINT ( 'NONE',  ( -50.55543936806279248, -142.3125000013656063, 0.3552334253322060320 ) ) ;
#55562 = VECTOR ( 'NONE', #16176, 1000.000000000000000 ) ;
#55563 = CARTESIAN_POINT ( 'NONE',  ( 2.229367062500001939, -82.22916666530106511, 3.861377020970579999 ) ) ;
#55564 = CARTESIAN_POINT ( 'NONE',  ( -52.53715891517739323, -136.5625000027311842, -4.819101127000233298 ) ) ;
#55565 = CARTESIAN_POINT ( 'NONE',  ( -4.458734124999999437, -45.31249999863440081, 0.000000000000000000 ) ) ;
#55566 = CARTESIAN_POINT ( 'NONE',  ( -3.152801135295367096, -143.3125000013655779, -3.152801135295367541 ) ) ;
#55567 = CYLINDRICAL_SURFACE ( 'NONE', #58947, 5.000000000000000000 ) ;
#55568 = CARTESIAN_POINT ( 'NONE',  ( 4.458734124999999437, -49.81249999863440792, -5.460374474430324690E-16 ) ) ;
#55569 = CARTESIAN_POINT ( 'NONE',  ( -3.152548672688508926E-16, -45.56249999863439371, -5.148502694627439702 ) ) ;
#55570 = VECTOR ( 'NONE', #47677, 1000.000000000000000 ) ;
#55571 = CARTESIAN_POINT ( 'NONE',  ( 1.255007937094098239E-14, 22.87500000273118772, -4.999999999999999112 ) ) ;
#55572 = CARTESIAN_POINT ( 'NONE',  ( -3.152548672688508926E-16, -17.56249999863440792, -5.148502694627439702 ) ) ;
#55573 = CARTESIAN_POINT ( 'NONE',  ( 2.499999999999998668, -101.3333333333333286, -4.330127018922193649 ) ) ;
#55574 = DIRECTION ( 'NONE',  ( 0.000000000000000000, 1.000000000000000000, 0.000000000000000000 ) ) ;
#55575 = CARTESIAN_POINT ( 'NONE',  ( 2.229367062499998831, -36.89583333196773651, -3.861377020970580887 ) ) ;
#55576 = CARTESIAN_POINT ( 'NONE',  ( 2.500000000000002220, 0.4583333360645182042, 4.330127018922192761 ) ) ;
#55577 = CARTESIAN_POINT ( 'NONE',  ( -54.64476657466781973, -130.8125000013656063, -4.444560631937228834 ) ) ;
#55578 = CARTESIAN_POINT ( 'NONE',  ( 2.229367062499998831, -76.89583333196773651, -3.861377020970580887 ) ) ;
#55579 = CARTESIAN_POINT ( 'NONE',  ( 2.499999999999998668, 24.66666666666666785, -4.330127018922193649 ) ) ;
#55580 = CARTESIAN_POINT ( 'NONE',  ( 5.000000000000000888, -30.45833333060214443, 2.886751345948126879 ) ) ;
#55581 = CARTESIAN_POINT ( 'NONE',  ( 9.457646018065525792E-16, -2.312499998634407028, 5.148502694627439702 ) ) ;
#55582 = ORIENTED_EDGE ( 'NONE', *, *, #57567, .T. ) ;
#55583 = CARTESIAN_POINT ( 'NONE',  ( 1.339745962155609149, 23.41965820146970856, 5.000000000000003553 ) ) ;
#55584 = CARTESIAN_POINT ( 'NONE',  ( -2.229367062499996610, -88.14583333196773651, 3.861377020970582219 ) ) ;
#55585 = CARTESIAN_POINT ( 'NONE',  ( 3.061616997868383141E-16, -168.8750000027312126, -5.000000000000000000 ) ) ;
#55586 = CARTESIAN_POINT ( 'NONE',  ( -4.458734124999999437, -86.56249999863439371, 0.000000000000000000 ) ) ;
#55587 = CARTESIAN_POINT ( 'NONE',  ( -2.229367062499996610, 17.60416666803225993, 3.861377020970582219 ) ) ;
#55588 = LINE ( 'NONE', #16016, #55156 ) ;
#55589 =( BOUNDED_CURVE ( )  B_SPLINE_CURVE ( 2, ( #28884, #38847, #4443, #47564, #63309, #9585, #29191, #48817, #19551 ),
 .UNSPECIFIED., .F., .F. ) 
 B_SPLINE_CURVE_WITH_KNOTS ( ( 3, 2, 2, 2, 3 ),
 ( 0.3375000000000000222, 0.3380952380952381153, 0.3392857142857143016, 0.3404761904761904878, 0.3410714285714285809 ),
 .UNSPECIFIED. ) 
 CURVE ( )  GEOMETRIC_REPRESENTATION_ITEM ( )  RATIONAL_B_SPLINE_CURVE ( ( 0.9330127018922194093, 0.9330127018922194093, 1.000000000000000000, 0.8660254037844387076, 1.000000000000000000, 0.8660254037844387076, 1.000000000000000000, 0.9330127018922194093, 0.9330127018922194093 ) ) 
 REPRESENTATION_ITEM ( '' )  );
#55590 = CARTESIAN_POINT ( 'NONE',  ( -57.19623071787017210, -138.3750000013656063, 4.297418129356382899 ) ) ;
#55591 = CARTESIAN_POINT ( 'NONE',  ( -4.458734124999997661, -5.229166665301072214, 2.574251347313722516 ) ) ;
#55592 = CARTESIAN_POINT ( 'NONE',  ( -2.229367062500000163, 24.27083333469892779, -3.861377020970580443 ) ) ;
#55593 = CARTESIAN_POINT ( 'NONE',  ( 2.229367062499998831, -47.89583333196774362, -3.861377020970580887 ) ) ;
#55594 = CARTESIAN_POINT ( 'NONE',  ( -2.499999999999996447, -15.70833333060214443, 4.330127018922195425 ) ) ;
#55595 = CARTESIAN_POINT ( 'NONE',  ( -4.458734124999999437, -83.39583333196772230, -2.574251347313719407 ) ) ;
#55596 = CARTESIAN_POINT ( 'NONE',  ( 9.457646018065525792E-16, -4.062499998634408804, 5.148502694627439702 ) ) ;
#55597 = CARTESIAN_POINT ( 'NONE',  ( 0.000000000000000000, 15.00000000000000000, -11.00000000000000000 ) ) ;
#55598 = EDGE_CURVE ( 'NONE', #8450, #38824, #4745, .T. ) ;
#55599 = EDGE_LOOP ( 'NONE', ( #7815, #49734, #47673 ) ) ;
#55600 = CARTESIAN_POINT ( 'NONE',  ( 2.229367062499998831, -31.89583333196773651, -3.861377020970580887 ) ) ;
#55601 = CARTESIAN_POINT ( 'NONE',  ( -52.80376928212989185, -131.1250000013655779, -4.297418129356379346 ) ) ;
#55602 = ADVANCED_FACE ( 'NONE', ( #61022 ), #51994, .T. ) ;
#55603 = CARTESIAN_POINT ( 'NONE',  ( -4.458734124999999437, -75.39583333196773651, -2.574251347313719407 ) ) ;
#55604 = CARTESIAN_POINT ( 'NONE',  ( -5.000000000000000000, -108.9583333306021586, -2.886751345948128211 ) ) ;
#55605 = CARTESIAN_POINT ( 'NONE',  ( 4.458734124999998549, 20.27083333469892779, -2.574251347313721627 ) ) ;
#55606 = ADVANCED_FACE ( 'NONE', ( #61655 ), #37512, .T. ) ;
#55607 = CARTESIAN_POINT ( 'NONE',  ( -2.499999999999996447, -57.70833333060214443, 4.330127018922195425 ) ) ;
#55608 = CARTESIAN_POINT ( 'NONE',  ( 5.000000000000000000, -28.49999999999999645, -6.123233995736766282E-16 ) ) ;
#55609 = CARTESIAN_POINT ( 'NONE',  ( -2.229367062500000163, -75.72916666530106511, -3.861377020970580443 ) ) ;
#55610 = CARTESIAN_POINT ( 'NONE',  ( 5.000000000000000888, -65.58333333333332860, 2.886751345948126879 ) ) ;
#55611 = CARTESIAN_POINT ( 'NONE',  ( -50.01589407740564042, -151.6250000000000284, 0.3983568153799778022 ) ) ;
#55612 = CARTESIAN_POINT ( 'NONE',  ( -2.499999999999996447, 22.29166666939785202, 4.330127018922195425 ) ) ;
#55613 = ORIENTED_EDGE ( 'NONE', *, *, #46945, .F. ) ;
#55614 = CARTESIAN_POINT ( 'NONE',  ( 0.000000000000000000, -170.0000000000000000, 0.000000000000000000 ) ) ;
#55615 = CARTESIAN_POINT ( 'NONE',  ( 1.339745962155615144, -52.58034179853029144, 4.999999999999999112 ) ) ;
#55617 = CARTESIAN_POINT ( 'NONE',  ( -2.500000000000000444, -24.16666666666666430, -4.330127018922193649 ) ) ;
#55616 = CARTESIAN_POINT ( 'NONE',  ( 5.000000000000000000, -0.5000000000000004441, -6.123233995736766282E-16 ) ) ;
#55618 = CARTESIAN_POINT ( 'NONE',  ( -2.229367062500000163, -27.47916666530107221, -3.861377020970580443 ) ) ;
#55619 = AXIS2_PLACEMENT_3D ( 'NONE', #1517, #35599, #34963 ) ;
#55620 = CARTESIAN_POINT ( 'NONE',  ( 4.458734125000000326, -86.89583333196773651, 2.574251347313718519 ) ) ;
#55621 = CARTESIAN_POINT ( 'NONE',  ( -5.000000000000000000, -22.95833333060214798, -2.886751345948128211 ) ) ;
#55623 = EDGE_LOOP ( 'NONE', ( #28116, #63253, #2702, #52414 ) ) ;
#55622 = CARTESIAN_POINT ( 'NONE',  ( 4.458734124999999437, -55.81249999863440081, -5.460374474430324690E-16 ) ) ;
#55624 = CARTESIAN_POINT ( 'NONE',  ( -6.972266317189433020E-16, -49.24999999999999289, -5.000000000000000000 ) ) ;
#55625 = CARTESIAN_POINT ( 'NONE',  ( -1.339745962155610925, 11.33034180399266511, 5.000000000000000000 ) ) ;
#55627 = ORIENTED_EDGE ( 'NONE', *, *, #753, .T. ) ;
#55626 = CARTESIAN_POINT ( 'NONE',  ( 2.229367062500001939, -5.229166665301071326, 3.861377020970579999 ) ) ;
#55628 = CARTESIAN_POINT ( 'NONE',  ( -4.999999999999999112, -72.91666666666665719, 2.886751345948131764 ) ) ;
#55629 = CARTESIAN_POINT ( 'NONE',  ( -1.846868145590737420, -154.0000000013655779, 4.458734124999999437 ) ) ;
#55630 = CARTESIAN_POINT ( 'NONE',  ( -4.458734124999999437, -46.64583333196774362, -2.574251347313719407 ) ) ;
#55631 = CARTESIAN_POINT ( 'NONE',  ( -2.499999999999996447, -95.83333333333332860, 4.330127018922195425 ) ) ;
#55632 = CARTESIAN_POINT ( 'NONE',  ( -2.071067811865475061, -159.6875000000000000, -5.000000000000000888 ) ) ;
#55633 = CARTESIAN_POINT ( 'NONE',  ( 2.499999999999998668, -72.20833333060214443, -4.330127018922193649 ) ) ;
#55634 = CARTESIAN_POINT ( 'NONE',  ( -5.000000000000000000, -53.87499999726880162, 0.000000000000000000 ) ) ;
#55635 = CARTESIAN_POINT ( 'NONE',  ( -49.85088928181150436, -154.5625000000000000, -1.666127454062680702 ) ) ;
#55636 = CARTESIAN_POINT ( 'NONE',  ( -4.458734124999998549, -15.47916666530107399, 2.574251347313722516 ) ) ;
#55637 = CARTESIAN_POINT ( 'NONE',  ( -4.458734124999998549, -49.47916666530106511, 2.574251347313722516 ) ) ;
#55638 = DIRECTION ( 'NONE',  ( -0.000000000000000000, 1.000000000000000000, -0.000000000000000000 ) ) ;
#55639 = CARTESIAN_POINT ( 'NONE',  ( -4.458734125000001214, -144.8750000013655779, 1.846868145590734089 ) ) ;
#55640 = CARTESIAN_POINT ( 'NONE',  ( -3.152548672688508926E-16, -95.81249999863440792, -5.148502694627439702 ) ) ;
#55641 = CARTESIAN_POINT ( 'NONE',  ( -5.000000000000000000, -107.0833333333333428, -2.886751345948128211 ) ) ;
#55642 =( BOUNDED_CURVE ( )  B_SPLINE_CURVE ( 2, ( #61649, #17583, #26916, #46533, #2474, #36879, #37200, #56826, #21456 ),
 .UNSPECIFIED., .F., .F. ) 
 B_SPLINE_CURVE_WITH_KNOTS ( ( 3, 2, 2, 2, 3 ),
 ( 0.03541666666666666574, 0.03611111111111110772, 0.03749999999999999861, 0.03888888888888888951, 0.03958333333333333842 ),
 .UNSPECIFIED. ) 
 CURVE ( )  GEOMETRIC_REPRESENTATION_ITEM ( )  RATIONAL_B_SPLINE_CURVE ( ( 0.9330127018922194093, 0.9330127018922194093, 1.000000000000000000, 0.8660254037844387076, 1.000000000000000000, 0.8660254037844387076, 1.000000000000000000, 0.9330127018922189652, 0.9330127018922192983 ) ) 
 REPRESENTATION_ITEM ( '' )  );
#55643 = ORIENTED_EDGE ( 'NONE', *, *, #55132, .T. ) ;
#55644 = CARTESIAN_POINT ( 'NONE',  ( -52.10840900171896806, -152.4375000013656063, 3.393966926194110556 ) ) ;
#55645 = CARTESIAN_POINT ( 'NONE',  ( -3.152548672688508926E-16, 26.18750000136559564, -5.148502694627439702 ) ) ;
#55646 = CARTESIAN_POINT ( 'NONE',  ( -60.14911071818854538, -146.1875000027311842, 1.666127454062681368 ) ) ;
#55647 = CARTESIAN_POINT ( 'NONE',  ( 0.000000000000000000, -120.0000000000000000, 5.000000000000000000 ) ) ;
#55648 = ORIENTED_EDGE ( 'NONE', *, *, #4109, .T. ) ;
#55649 = CARTESIAN_POINT ( 'NONE',  ( 9.457646018065525792E-16, -0.06249999863440491854, 5.148502694627439702 ) ) ;
#55650 = ADVANCED_FACE ( 'NONE', ( #16948 ), #7625, .T. ) ;
#55651 = CARTESIAN_POINT ( 'NONE',  ( -3.152548672688508926E-16, -23.81249999863440792, -5.148502694627439702 ) ) ;
#55652 = CARTESIAN_POINT ( 'NONE',  ( 5.000000000000000888, -72.58333333333332860, 2.886751345948126879 ) ) ;
#55653 = CARTESIAN_POINT ( 'NONE',  ( -3.152548672688508926E-16, -8.562499998634404363, -5.148502694627439702 ) ) ;
#55654 = CARTESIAN_POINT ( 'NONE',  ( 1.339745962155615144, 23.41965820146970501, 4.999999999999999112 ) ) ;
#55655 = CARTESIAN_POINT ( 'NONE',  ( -4.458734124999999437, -144.0000000013655779, -1.846868145590735644 ) ) ;
#55656 = CARTESIAN_POINT ( 'NONE',  ( -4.458734124999999437, 13.35416666803225993, -2.574251347313719407 ) ) ;
#55657 = ORIENTED_EDGE ( 'NONE', *, *, #23348, .T. ) ;
#55658 = CARTESIAN_POINT ( 'NONE',  ( -5.000000000000000000, -62.95833333060215153, -2.886751345948128211 ) ) ;
#55659 = CARTESIAN_POINT ( 'NONE',  ( 5.000000000000000000, -57.37499999726880162, -6.123233995736766282E-16 ) ) ;
#55661 = CARTESIAN_POINT ( 'NONE',  ( -4.458734124999999437, -21.39583333196774007, -2.574251347313719407 ) ) ;
#55660 = CARTESIAN_POINT ( 'NONE',  ( -2.499999999999996447, -87.83333333333332860, 4.330127018922195425 ) ) ;
#55662 = AXIS2_PLACEMENT_3D ( 'NONE', #33883, #3373, #9433 ) ;
#55663 = FACE_OUTER_BOUND ( 'NONE', #22163, .T. ) ;
#55664 = CARTESIAN_POINT ( 'NONE',  ( 3.061616997868383141E-16, -146.8750000027312126, -5.000000000000000000 ) ) ;
#55665 = CARTESIAN_POINT ( 'NONE',  ( -51.60603307380591787, -149.9375000013656063, -2.891590998281053704 ) ) ;
#55666 = CARTESIAN_POINT ( 'NONE',  ( 2.500000000000002220, -44.54166666393547303, 4.330127018922192761 ) ) ;
#55667 = CARTESIAN_POINT ( 'NONE',  ( 2.071067811865644703, -149.9375000027312126, -4.999999999999831246 ) ) ;
#55668 = CARTESIAN_POINT ( 'NONE',  ( 9.457646018065525792E-16, 5.937500001365593860, 5.148502694627439702 ) ) ;
#55669 = DIRECTION ( 'NONE',  ( -0.000000000000000000, 1.000000000000000000, -0.000000000000000000 ) ) ;
#55670 = CARTESIAN_POINT ( 'NONE',  ( -2.229367062499996610, 11.85416666803225993, 3.861377020970582219 ) ) ;
#55671 = CARTESIAN_POINT ( 'NONE',  ( -4.458734124999998549, -66.22916666530107932, 2.574251347313722516 ) ) ;
#55672 = CARTESIAN_POINT ( 'NONE',  ( 2.229367062499998831, -16.89583333196773651, -3.861377020970580887 ) ) ;
#55673 = CARTESIAN_POINT ( 'NONE',  ( -2.499999999999996447, -0.8333333333333317050, 4.330127018922195425 ) ) ;
#55674 = CARTESIAN_POINT ( 'NONE',  ( 4.458734124999999437, -162.5000000013655779, 1.846868145590737864 ) ) ;
#55675 = CARTESIAN_POINT ( 'NONE',  ( -2.499999999999996447, 26.29166666939785202, 4.330127018922195425 ) ) ;
#55676 = CARTESIAN_POINT ( 'NONE',  ( 2.229367062500001939, -59.97916666530106511, 3.861377020970579999 ) ) ;
#55677 = CARTESIAN_POINT ( 'NONE',  ( -2.499999999999996447, -93.70833333060214443, 4.330127018922195425 ) ) ;
#55678 = FACE_OUTER_BOUND ( 'NONE', #59536, .T. ) ;
#55679 = CARTESIAN_POINT ( 'NONE',  ( -4.999999999999998224, -35.91666666666666430, 2.886751345948131764 ) ) ;
#55680 = CARTESIAN_POINT ( 'NONE',  ( 9.457646018065525792E-16, -38.06249999863440792, 5.148502694627439702 ) ) ;
#55681 = CARTESIAN_POINT ( 'NONE',  ( 5.000000000000000888, -51.45833333060214443, 2.886751345948126879 ) ) ;
#55682 = CARTESIAN_POINT ( 'NONE',  ( -5.000000000000000000, -47.08333333333333570, -2.886751345948128211 ) ) ;
#55683 = CARTESIAN_POINT ( 'NONE',  ( 2.500000000000002220, -13.66666666666666785, 4.330127018922192761 ) ) ;
#55684 = CARTESIAN_POINT ( 'NONE',  ( 2.500000000000002220, -17.54166666393547658, 4.330127018922192761 ) ) ;
#55685 = ORIENTED_EDGE ( 'NONE', *, *, #7948, .T. ) ;
#55686 = CARTESIAN_POINT ( 'NONE',  ( -2.229367062500000163, -107.4791666653010651, -3.861377020970580443 ) ) ;
#55687 = CARTESIAN_POINT ( 'NONE',  ( 4.458734125000001214, -4.145833331967740065, 2.574251347313718519 ) ) ;
#55688 =( BOUNDED_CURVE ( )  B_SPLINE_CURVE ( 2, ( #28644, #18988, #42182, #18372, #38307, #42494, #52787, #52481, #47637 ),
 .UNSPECIFIED., .F., .F. ) 
 B_SPLINE_CURVE_WITH_KNOTS ( ( 3, 2, 2, 2, 3 ),
 ( 0.8910714285714286254, 0.8916666666666667185, 0.8928571428571429047, 0.8940476190476190910, 0.8946428571428571841 ),
 .UNSPECIFIED. ) 
 CURVE ( )  GEOMETRIC_REPRESENTATION_ITEM ( )  RATIONAL_B_SPLINE_CURVE ( ( 0.9330127018922194093, 0.9330127018922256266, 1.000000000000000000, 0.8660254037844387076, 1.000000000000000000, 0.8660254037844387076, 1.000000000000000000, 0.9330127018922194093, 0.9330127018922194093 ) ) 
 REPRESENTATION_ITEM ( '' )  );
#55689 = CARTESIAN_POINT ( 'NONE',  ( 5.000000000000000000, -73.37499999726880162, -6.123233995736766282E-16 ) ) ;
#55690 = CARTESIAN_POINT ( 'NONE',  ( -3.535250795749689387E-16, -10.25000000000000355, -5.773502691896257311 ) ) ;
#55691 = CARTESIAN_POINT ( 'NONE',  ( 4.458734124999998549, -73.72916666530106511, -2.574251347313721627 ) ) ;
#55692 = CARTESIAN_POINT ( 'NONE',  ( -6.972266317189433020E-16, -17.25000000000000000, -5.000000000000000000 ) ) ;
#55693 = CARTESIAN_POINT ( 'NONE',  ( 5.000000000000000000, -8.291666663935481907, -2.886751345948129988 ) ) ;
#55695 = VERTEX_POINT ( 'NONE', #12112 ) ;
#55694 = CARTESIAN_POINT ( 'NONE',  ( 9.457646018065525792E-16, -38.06249999863441502, 5.148502694627439702 ) ) ;
#55696 = CARTESIAN_POINT ( 'NONE',  ( 0.000000000000000000, -170.0000000000000000, 0.000000000000000000 ) ) ;
#55698 = ORIENTED_EDGE ( 'NONE', *, *, #16894, .T. ) ;
#55697 = CARTESIAN_POINT ( 'NONE',  ( -4.458734124999999437, 12.43750000136559564, 0.000000000000000000 ) ) ;
#55699 = CARTESIAN_POINT ( 'NONE',  ( 0.000000000000000000, -170.0000000000000000, 5.000000000000000000 ) ) ;
#55700 = CARTESIAN_POINT ( 'NONE',  ( -2.499999999999996447, -56.83333333333333570, 4.330127018922195425 ) ) ;
#55701 = CARTESIAN_POINT ( 'NONE',  ( -2.229367062500000163, -28.72916666530107221, -3.861377020970580443 ) ) ;
#55702 = CARTESIAN_POINT ( 'NONE',  ( -6.972266317189433020E-16, -32.12499999726880873, -5.000000000000000000 ) ) ;
#55703 = CARTESIAN_POINT ( 'NONE',  ( -3.152548672688508926E-16, -75.56249999863439371, -5.148502694627439702 ) ) ;
#55704 = CARTESIAN_POINT ( 'NONE',  ( -3.535533905932738641, -169.3750000000000284, 3.535533905932737309 ) ) ;
#55706 = EDGE_CURVE ( 'NONE', #39750, #44922, #42512, .T. ) ;
#55705 = CARTESIAN_POINT ( 'NONE',  ( 4.458734125000001214, -85.89583333196773651, 2.574251347313718519 ) ) ;
#55707 = CARTESIAN_POINT ( 'NONE',  ( -53.51423613279429503, -136.5000000013656347, 4.591703134518082763 ) ) ;
#55708 = CARTESIAN_POINT ( 'NONE',  ( 4.458734124999998549, -35.97916666530107221, -2.574251347313721627 ) ) ;
#55709 = CARTESIAN_POINT ( 'NONE',  ( 1.339745962155615144, -72.70534180126148271, 4.999999999999999112 ) ) ;
#55710 = ORIENTED_EDGE ( 'NONE', *, *, #51104, .T. ) ;
#55711 = CARTESIAN_POINT ( 'NONE',  ( 4.458734124999999437, -81.06249999863440792, -5.460374474430324690E-16 ) ) ;
#55712 = CARTESIAN_POINT ( 'NONE',  ( -56.37266686252615955, -135.0000000000000284, -4.242180533871957593 ) ) ;
#55713 = VERTEX_POINT ( 'NONE', #4664 ) ;
#55714 = DIRECTION ( 'NONE',  ( 0.000000000000000000, 0.000000000000000000, 1.000000000000000000 ) ) ;
#55715 = CARTESIAN_POINT ( 'NONE',  ( -4.999999999999998224, -18.79166666393547658, 2.886751345948131764 ) ) ;
#55716 = CARTESIAN_POINT ( 'NONE',  ( 9.457646018065525792E-16, -65.31249999863440792, 5.148502694627439702 ) ) ;
#55717 = CARTESIAN_POINT ( 'NONE',  ( -4.458734124999999437, -10.64583333196773829, -2.574251347313719407 ) ) ;
#55718 = ORIENTED_EDGE ( 'NONE', *, *, #14881, .T. ) ;
#55719 = CARTESIAN_POINT ( 'NONE',  ( -2.500000000000000444, -10.04166666393547658, -4.330127018922193649 ) ) ;
#55720 = CARTESIAN_POINT ( 'NONE',  ( -4.999999999999998224, 5.208333336064518981, 2.886751345948131764 ) ) ;
#55721 = ORIENTED_EDGE ( 'NONE', *, *, #31450, .F. ) ;
#55722 = CARTESIAN_POINT ( 'NONE',  ( 4.458734124999999437, -7.062499998634404363, -5.460374474430324690E-16 ) ) ;
#55723 = CARTESIAN_POINT ( 'NONE',  ( 4.458734124999998549, 9.270833334698927786, -2.574251347313721627 ) ) ;
#55724 = CARTESIAN_POINT ( 'NONE',  ( -8.190561711645485556E-16, -162.6875000013655779, 4.458734124999999437 ) ) ;
#55725 = EDGE_LOOP ( 'NONE', ( #28702, #11219, #27736, #11612 ) ) ;
#55726 = CARTESIAN_POINT ( 'NONE',  ( -4.458734124999997661, -89.22916666530107932, 2.574251347313722516 ) ) ;
#55727 = CARTESIAN_POINT ( 'NONE',  ( -6.972266317189433020E-16, -29.12499999726880873, -5.000000000000000000 ) ) ;
#55728 = CARTESIAN_POINT ( 'NONE',  ( -4.458734124999999437, -4.312499998634401699, 0.000000000000000000 ) ) ;
#55729 = FACE_OUTER_BOUND ( 'NONE', #25150, .T. ) ;
#55730 = CARTESIAN_POINT ( 'NONE',  ( 2.500000000000002220, -30.54166666393548013, 4.330127018922192761 ) ) ;
#55731 = CARTESIAN_POINT ( 'NONE',  ( 4.330127018922154569, 45.00000000000000000, -7.499999999999971578 ) ) ;
#55732 = CARTESIAN_POINT ( 'NONE',  ( 9.457646018065525792E-16, 21.93750000136559208, 5.148502694627439702 ) ) ;
#55733 = CARTESIAN_POINT ( 'NONE',  ( -5.000000000000000000, 23.00000000000000000, 0.000000000000000000 ) ) ;
#55734 = CARTESIAN_POINT ( 'NONE',  ( -2.229367062499996610, 25.85416666803225993, 3.861377020970582219 ) ) ;
#55735 = CARTESIAN_POINT ( 'NONE',  ( -2.229367062499996610, -53.14583333196773651, 3.861377020970582219 ) ) ;
#55736 = CARTESIAN_POINT ( 'NONE',  ( -4.458734124999997661, -35.47916666530107221, 2.574251347313722516 ) ) ;
#55737 = CARTESIAN_POINT ( 'NONE',  ( -2.229367062500000163, 4.270833334698926897, -3.861377020970580443 ) ) ;
#55738 = CARTESIAN_POINT ( 'NONE',  ( 5.000000000000000000, -160.1875000027311842, 2.071067811865478614 ) ) ;
#55739 = CARTESIAN_POINT ( 'NONE',  ( -5.000000000000000000, 14.91666666666666607, -2.886751345948128211 ) ) ;
#55740 = CARTESIAN_POINT ( 'NONE',  ( 3.535533905932736864, -147.2500000027311842, 3.535533905932738641 ) ) ;
#55741 = DIRECTION ( 'NONE',  ( 0.000000000000000000, 0.000000000000000000, 1.000000000000000000 ) ) ;
#55742 = CARTESIAN_POINT ( 'NONE',  ( -4.458734124999998549, -43.22916666530105800, 2.574251347313722516 ) ) ;
#55743 = CARTESIAN_POINT ( 'NONE',  ( 5.000000000000000000, -78.37499999726881583, -6.123233995736766282E-16 ) ) ;
#55744 = CARTESIAN_POINT ( 'NONE',  ( -52.80376928212989185, -139.1250000013656063, -4.297418129356379346 ) ) ;
#55745 = CARTESIAN_POINT ( 'NONE',  ( -6.972266317189433020E-16, -24.12499999726881228, -5.000000000000000000 ) ) ;
#55746 = CARTESIAN_POINT ( 'NONE',  ( -6.972266317189433020E-16, -88.25000000000000000, -5.000000000000000000 ) ) ;
#55747 = CARTESIAN_POINT ( 'NONE',  ( -4.458734124999997661, -83.47916666530106511, 2.574251347313722516 ) ) ;
#55748 = CARTESIAN_POINT ( 'NONE',  ( -1.846868145590734756, -161.3750000013656063, -4.458734124999999437 ) ) ;
#55749 = CARTESIAN_POINT ( 'NONE',  ( -1.060314165522979968, -8.048081368954337123, -7.659344964963557878 ) ) ;
#55750 = CARTESIAN_POINT ( 'NONE',  ( -3.535250795749689387E-16, -25.25000000000000355, -5.773502691896257311 ) ) ;
#55751 = FACE_OUTER_BOUND ( 'NONE', #45344, .T. ) ;
#55752 = VERTEX_POINT ( 'NONE', #23673 ) ;
#55753 = CARTESIAN_POINT ( 'NONE',  ( -2.229367062500000163, 24.27083333469892779, -3.861377020970580443 ) ) ;
#55754 = ORIENTED_EDGE ( 'NONE', *, *, #17387, .F. ) ;
#55755 = CARTESIAN_POINT ( 'NONE',  ( -4.458734124999999437, -91.39583333196773651, -2.574251347313719407 ) ) ;
#55756 = CARTESIAN_POINT ( 'NONE',  ( -2.229367062500000163, 13.27083333469892779, -3.861377020970580443 ) ) ;
#55757 = CARTESIAN_POINT ( 'NONE',  ( -5.000000000000000000, 15.04166666939785202, -2.886751345948128211 ) ) ;
#55758 = CARTESIAN_POINT ( 'NONE',  ( 0.000000000000000000, -170.0000000000000000, 0.000000000000000000 ) ) ;
#55759 = CARTESIAN_POINT ( 'NONE',  ( -4.999999999999999112, 10.08333333333333393, 2.886751345948131764 ) ) ;
#55760 =( BOUNDED_CURVE ( )  B_SPLINE_CURVE ( 2, ( #45879, #41047, #60694, #11147, #31084, #51031, #25629, #45561, #6338 ),
 .UNSPECIFIED., .F., .F. ) 
 B_SPLINE_CURVE_WITH_KNOTS ( ( 3, 2, 2, 2, 3 ),
 ( 0.5312500000000000000, 0.5319444444444444420, 0.5333333333333333259, 0.5347222222222222099, 0.5354166666666666519 ),
 .UNSPECIFIED. ) 
 CURVE ( )  GEOMETRIC_REPRESENTATION_ITEM ( )  RATIONAL_B_SPLINE_CURVE ( ( 0.9330127018922194093, 0.9330127018922194093, 1.000000000000000000, 0.8660254037844387076, 1.000000000000000000, 0.8660254037844387076, 1.000000000000000000, 0.9330127018922194093, 0.9330127018922194093 ) ) 
 REPRESENTATION_ITEM ( '' )  );
#55761 = CARTESIAN_POINT ( 'NONE',  ( 2.229367062499998831, -55.64583333196773651, -3.861377020970580887 ) ) ;
#55762 = CARTESIAN_POINT ( 'NONE',  ( -4.458734124999999437, -11.31249999863440792, 0.000000000000000000 ) ) ;
#55763 = CARTESIAN_POINT ( 'NONE',  ( 0.000000000000000000, -170.0000000000000000, 0.000000000000000000 ) ) ;
#55764 = CARTESIAN_POINT ( 'NONE',  ( -59.59170313451810586, -136.7500000013655779, 1.485763867205729394 ) ) ;
#55765 = CARTESIAN_POINT ( 'NONE',  ( 5.000000000000000000, 15.62500000273118417, -6.123233995736766282E-16 ) ) ;
#55766 = CARTESIAN_POINT ( 'NONE',  ( 1.339745962155641346, -1.294658198738521282, -4.999999999999983125 ) ) ;
#55767 = CARTESIAN_POINT ( 'NONE',  ( 1.975475456537005874E-15, 18.37500000273118062, 5.000000000000000000 ) ) ;
#55768 = CARTESIAN_POINT ( 'NONE',  ( -3.535250795749689387E-16, -33.25000000000000000, -5.773502691896257311 ) ) ;
#55769 = DIRECTION ( 'NONE',  ( -0.000000000000000000, 1.000000000000000000, -0.000000000000000000 ) ) ;
#55771 = CARTESIAN_POINT ( 'NONE',  ( 4.458734125000001214, -12.14583333196774007, 2.574251347313718519 ) ) ;
#55770 = FACE_OUTER_BOUND ( 'NONE', #13725, .T. ) ;
#55772 = CARTESIAN_POINT ( 'NONE',  ( -2.071067811865432873, -140.8125000027312126, -5.000000000000041744 ) ) ;
#55773 = CARTESIAN_POINT ( 'NONE',  ( -2.229367062499996610, -62.14583333196774362, 3.861377020970582219 ) ) ;
#55774 = CARTESIAN_POINT ( 'NONE',  ( 3.152801135295367541, -151.5625000013655779, -3.152801135295367541 ) ) ;
#55776 = EDGE_CURVE ( 'NONE', #44127, #54337, #15844, .T. ) ;
#55775 = CARTESIAN_POINT ( 'NONE',  ( -4.458734124999999437, -71.31249999863439371, 0.000000000000000000 ) ) ;
#55777 = CARTESIAN_POINT ( 'NONE',  ( -56.48576386720575471, -146.0000000013656347, -4.591703134518078322 ) ) ;
#55778 = CARTESIAN_POINT ( 'NONE',  ( -2.229367062500000163, -21.72916666530107221, -3.861377020970580443 ) ) ;
#55779 =( BOUNDED_CURVE ( )  B_SPLINE_CURVE ( 2, ( #19236, #6685, #35315, #54291, #6058, #45278, #20530, #35958, #1244 ),
 .UNSPECIFIED., .F., .F. ) 
 B_SPLINE_CURVE_WITH_KNOTS ( ( 3, 2, 2, 2, 3 ),
 ( 0.7479166666666666741, 0.7486111111111111160, 0.7500000000000000000, 0.7513888888888888840, 0.7520833333333333259 ),
 .UNSPECIFIED. ) 
 CURVE ( )  GEOMETRIC_REPRESENTATION_ITEM ( )  RATIONAL_B_SPLINE_CURVE ( ( 0.9330127018922194093, 0.9330127018922194093, 1.000000000000000000, 0.8660254037844387076, 1.000000000000000000, 0.8660254037844387076, 1.000000000000000000, 0.9330127018922194093, 0.9330127018922194093 ) ) 
 REPRESENTATION_ITEM ( '' )  );
#55780 = CARTESIAN_POINT ( 'NONE',  ( -4.999999999999999112, -61.79166666393546592, 2.886751345948131764 ) ) ;
#55781 = ORIENTED_EDGE ( 'NONE', *, *, #8730, .F. ) ;
#55782 = CARTESIAN_POINT ( 'NONE',  ( -4.999999999999998224, -48.91666666666666430, 2.886751345948131764 ) ) ;
#55783 = VERTEX_POINT ( 'NONE', #14002 ) ;
#55784 = DIRECTION ( 'NONE',  ( -0.000000000000000000, -0.000000000000000000, 1.000000000000000000 ) ) ;
#55785 = CARTESIAN_POINT ( 'NONE',  ( 3.152801135295366208, -153.5625000013656063, 3.152801135295367985 ) ) ;
#55786 = VERTEX_POINT ( 'NONE', #28485 ) ;
#55787 = DIRECTION ( 'NONE',  ( -0.000000000000000000, 1.000000000000000000, -0.000000000000000000 ) ) ;
#55788 = CARTESIAN_POINT ( 'NONE',  ( -50.18089887299979068, -127.6875000000000711, 2.462841084822635640 ) ) ;
#55789 = CARTESIAN_POINT ( 'NONE',  ( 0.000000000000000000, -120.0000000000000000, 5.000000000000000000 ) ) ;
#55790 = CARTESIAN_POINT ( 'NONE',  ( 4.458734124999999437, -48.06249999863440792, -5.460374474430324690E-16 ) ) ;
#55791 = VERTEX_POINT ( 'NONE', #53561 ) ;
#55792 = EDGE_CURVE ( 'NONE', #28361, #13218, #31422, .T. ) ;
#55793 = CARTESIAN_POINT ( 'NONE',  ( 2.499999999999998668, 11.66666666666666607, -4.330127018922193649 ) ) ;
#55794 = ADVANCED_FACE ( 'NONE', ( #14630 ), #52120, .F. ) ;
#55795 = CARTESIAN_POINT ( 'NONE',  ( 4.458734125000001214, 12.10416666803226171, 2.574251347313718519 ) ) ;
#55796 = CARTESIAN_POINT ( 'NONE',  ( -2.229367062500000163, 25.52083333469892779, -3.861377020970580443 ) ) ;
#55797 = CARTESIAN_POINT ( 'NONE',  ( -56.48576386720575471, -150.7500000013655495, -4.591703134518078322 ) ) ;
#55798 = CARTESIAN_POINT ( 'NONE',  ( -53.33387254593727533, -149.9375000027311842, 5.149110718188522284 ) ) ;
#55799 = CARTESIAN_POINT ( 'NONE',  ( -5.000000000000000000, -35.87499999726881583, 0.000000000000000000 ) ) ;
#55800 = ORIENTED_EDGE ( 'NONE', *, *, #61839, .T. ) ;
#55801 = CARTESIAN_POINT ( 'NONE',  ( 4.458734124999999437, -72.81249999863439371, -5.460374474430324690E-16 ) ) ;
#55802 = CARTESIAN_POINT ( 'NONE',  ( -5.000000000000000000, -49.87499999726881583, 0.000000000000000000 ) ) ;
#55803 = CARTESIAN_POINT ( 'NONE',  ( -2.229367062499996610, 11.85416666803225993, 3.861377020970582219 ) ) ;
#55804 = EDGE_CURVE ( 'NONE', #14586, #34023, #29334, .T. ) ;
#55805 = CARTESIAN_POINT ( 'NONE',  ( 6.158835246850667461E-14, 7.875000002731183280, -4.999999999999999112 ) ) ;
#55806 = FACE_OUTER_BOUND ( 'NONE', #42307, .T. ) ;
#55807 = CARTESIAN_POINT ( 'NONE',  ( 2.229367062499998831, -53.89583333196773651, -3.861377020970580887 ) ) ;
#55808 = CARTESIAN_POINT ( 'NONE',  ( 5.000000000000000888, -14.45833333060214976, 2.886751345948126879 ) ) ;
#55809 = CYLINDRICAL_SURFACE ( 'NONE', #1929, 5.000000000000000000 ) ;
#55810 = CARTESIAN_POINT ( 'NONE',  ( -6.972266317189433020E-16, -105.2500000000000000, -5.000000000000000000 ) ) ;
#55811 = CARTESIAN_POINT ( 'NONE',  ( 4.458734124999999437, -21.06249999863440436, -5.460374474430324690E-16 ) ) ;
#55812 = ORIENTED_EDGE ( 'NONE', *, *, #9817, .F. ) ;
#55813 = CARTESIAN_POINT ( 'NONE',  ( -1.339745962155613812, -61.20534180126147561, -5.000000000000000000 ) ) ;
#55814 = CARTESIAN_POINT ( 'NONE',  ( -4.458734124999999437, -105.3124999986344221, 0.000000000000000000 ) ) ;
#55815 = CARTESIAN_POINT ( 'NONE',  ( -9.184850993605147944E-16, -157.3750000027311842, 5.000000000000000000 ) ) ;
#55816 = ORIENTED_EDGE ( 'NONE', *, *, #5933, .T. ) ;
#55817 = CARTESIAN_POINT ( 'NONE',  ( 4.458734124999999437, -105.0624999986344079, -5.460374474430324690E-16 ) ) ;
#55818 = CARTESIAN_POINT ( 'NONE',  ( 4.458734125000001214, -26.89583333196774007, 2.574251347313718519 ) ) ;
#55819 = CARTESIAN_POINT ( 'NONE',  ( -4.999999999999999112, -64.79166666393547303, 2.886751345948131764 ) ) ;
#55820 = CARTESIAN_POINT ( 'NONE',  ( -58.39396692619412477, -152.6875000013656063, 2.891590998281057701 ) ) ;
#55821 = CARTESIAN_POINT ( 'NONE',  ( -50.70258187064364108, -143.1250000013656063, 2.196230717870141014 ) ) ;
#55822 = EDGE_CURVE ( 'NONE', #56685, #6898, #13771, .T. ) ;
#55823 = CARTESIAN_POINT ( 'NONE',  ( 4.458734125000000326, -24.89583333196773651, 2.574251347313718519 ) ) ;
#55824 = CARTESIAN_POINT ( 'NONE',  ( -2.229367062500000163, -66.72916666530106511, -3.861377020970580443 ) ) ;
#55825 = CARTESIAN_POINT ( 'NONE',  ( -6.972266317189433020E-16, -32.12499999726880873, -5.000000000000000000 ) ) ;
#55826 = CARTESIAN_POINT ( 'NONE',  ( -4.458734124999997661, -27.22916666530107221, 2.574251347313722516 ) ) ;
#55827 = CARTESIAN_POINT ( 'NONE',  ( 2.499999999999998668, -32.33333333333332860, -4.330127018922193649 ) ) ;
#55828 = CARTESIAN_POINT ( 'NONE',  ( -3.535533905932738641, -150.3750000000000000, 3.535533905932737309 ) ) ;
#55829 = CARTESIAN_POINT ( 'NONE',  ( 1.060575238724906964E-15, -10.75000000000000178, 5.773502691896257311 ) ) ;
#55830 = CARTESIAN_POINT ( 'NONE',  ( -3.152801135295367096, -151.0625000013655779, -3.152801135295367541 ) ) ;
#55831 = ORIENTED_EDGE ( 'NONE', *, *, #1366, .T. ) ;
#55832 = CARTESIAN_POINT ( 'NONE',  ( -4.458734124999999437, -51.64583333196773651, -2.574251347313719407 ) ) ;
#55833 =( BOUNDED_CURVE ( )  B_SPLINE_CURVE ( 2, ( #21182, #25368, #55611, #44988, #30504, #16035, #41106, #31143, #50126 ),
 .UNSPECIFIED., .F., .F. ) 
 B_SPLINE_CURVE_WITH_KNOTS ( ( 3, 2, 2, 2, 3 ),
 ( 0.1083333333333334203, 0.1125000000000000999, 0.1166666666666667657, 0.1208333333333334314, 0.1250000000000001110 ),
 .UNSPECIFIED. ) 
 CURVE ( )  GEOMETRIC_REPRESENTATION_ITEM ( )  RATIONAL_B_SPLINE_CURVE ( ( 0.9999999999999984457, 0.9238795325112882928, 1.000000000000000000, 0.9238795325112867385, 1.000000000000000000, 0.9238795325112867385, 1.000000000000000000, 0.9238795325112847401, 1.000000000000001998 ) ) 
 REPRESENTATION_ITEM ( '' )  );
#55834 = DIRECTION ( 'NONE',  ( -0.000000000000000000, 1.000000000000000000, -0.000000000000000000 ) ) ;
#55835 = CARTESIAN_POINT ( 'NONE',  ( -7.112481253775184697, 4.553861071372892866, -7.781689322728085223 ) ) ;
#55836 = CARTESIAN_POINT ( 'NONE',  ( -3.535250795749689387E-16, 28.74999999999999645, -5.773502691896257311 ) ) ;
#55837 = CARTESIAN_POINT ( 'NONE',  ( 6.158835246850666199E-14, -2.250000000000001776, -4.999999999999999112 ) ) ;
#55838 = CARTESIAN_POINT ( 'NONE',  ( 4.458734124999999437, 5.187500001365596525, -5.460374474430324690E-16 ) ) ;
#55839 = CARTESIAN_POINT ( 'NONE',  ( -3.535533905932738641, -142.3750000000000000, 3.535533905932737309 ) ) ;
#55840 = DIRECTION ( 'NONE',  ( -0.000000000000000000, 1.000000000000000000, -0.000000000000000000 ) ) ;
#55841 = CARTESIAN_POINT ( 'NONE',  ( 5.000000000000000000, -82.41666666666667140, -2.886751345948130876 ) ) ;
#55842 = CARTESIAN_POINT ( 'NONE',  ( -2.229367062500000163, 14.27083333469892601, -3.861377020970580443 ) ) ;
#55843 = CARTESIAN_POINT ( 'NONE',  ( -5.000000000000000000, 1.041666669397853129, -2.886751345948128211 ) ) ;
#55844 = ORIENTED_EDGE ( 'NONE', *, *, #12199, .T. ) ;
#55845 = FACE_OUTER_BOUND ( 'NONE', #63047, .T. ) ;
#55846 = ORIENTED_EDGE ( 'NONE', *, *, #13302, .F. ) ;
#55847 = DIRECTION ( 'NONE',  ( -0.000000000000000000, 1.000000000000000000, -0.000000000000000000 ) ) ;
#55848 = CARTESIAN_POINT ( 'NONE',  ( -4.458734124999998549, -44.22916666530106511, 2.574251347313722516 ) ) ;
#55849 = CARTESIAN_POINT ( 'NONE',  ( -4.458734125000000326, -162.2500000013656347, -1.846868145590735644 ) ) ;
#55850 = ADVANCED_FACE ( 'NONE', ( #63537 ), #58702, .T. ) ;
#55851 = VECTOR ( 'NONE', #2632, 1000.000000000000000 ) ;
#55852 = EDGE_CURVE ( 'NONE', #33543, #13547, #29491, .T. ) ;
#55853 = CARTESIAN_POINT ( 'NONE',  ( -5.000000000000000000, -46.95833333060215153, -2.886751345948128211 ) ) ;
#55854 = ADVANCED_FACE ( 'NONE', ( #57465 ), #13384, .T. ) ;
#55855 = ORIENTED_EDGE ( 'NONE', *, *, #19301, .F. ) ;
#55856 = CARTESIAN_POINT ( 'NONE',  ( 2.229367062499998831, -17.64583333196773651, -3.861377020970580887 ) ) ;
#55857 = VERTEX_POINT ( 'NONE', #30057 ) ;
#55858 = CARTESIAN_POINT ( 'NONE',  ( -5.000000000000000000, -88.08333333333332860, -2.886751345948128211 ) ) ;
#55859 = CARTESIAN_POINT ( 'NONE',  ( -4.458734125000001214, -165.8750000013656063, 1.846868145590734089 ) ) ;
#55860 =( BOUNDED_CURVE ( )  B_SPLINE_CURVE ( 2, ( #3713, #23329, #32339, #42933, #46818, #2762, #7592, #38119, #57742 ),
 .UNSPECIFIED., .F., .F. ) 
 B_SPLINE_CURVE_WITH_KNOTS ( ( 3, 2, 2, 2, 3 ),
 ( 0.7839285714285714191, 0.7845238095238095122, 0.7857142857142856984, 0.7869047619047618847, 0.7874999999999999778 ),
 .UNSPECIFIED. ) 
 CURVE ( )  GEOMETRIC_REPRESENTATION_ITEM ( )  RATIONAL_B_SPLINE_CURVE ( ( 0.9330127018922194093, 0.9330127018922194093, 1.000000000000000000, 0.8660254037844387076, 1.000000000000000000, 0.8660254037844387076, 1.000000000000000000, 0.9330127018922194093, 0.9330127018922194093 ) ) 
 REPRESENTATION_ITEM ( '' )  );
#55862 = ORIENTED_EDGE ( 'NONE', *, *, #52729, .T. ) ;
#55861 = CARTESIAN_POINT ( 'NONE',  ( 5.000000000000000888, -55.58333333333332860, 2.886751345948126879 ) ) ;
#55863 = CARTESIAN_POINT ( 'NONE',  ( -52.53715891517739323, -143.4375000000000284, -4.819101127000233298 ) ) ;
#55864 = CARTESIAN_POINT ( 'NONE',  ( -3.152548672688508926E-16, -30.81249999863440436, -5.148502694627439702 ) ) ;
#55865 = CARTESIAN_POINT ( 'NONE',  ( 0.000000000000000000, -170.0000000000000000, 0.000000000000000000 ) ) ;
#55866 = EDGE_CURVE ( 'NONE', #35606, #39571, #5133, .T. ) ;
#55867 = ORIENTED_EDGE ( 'NONE', *, *, #46874, .T. ) ;
#55868 = CARTESIAN_POINT ( 'NONE',  ( 2.229367062500001939, -75.97916666530106511, 3.861377020970579999 ) ) ;
#55869 = EDGE_CURVE ( 'NONE', #2392, #54097, #20350, .T. ) ;
#55870 = CARTESIAN_POINT ( 'NONE',  ( -3.152548672688508926E-16, 28.43750000136559208, -5.148502694627439702 ) ) ;
#55871 = CARTESIAN_POINT ( 'NONE',  ( 1.975475456537005874E-15, -53.74999999999999289, 5.000000000000000000 ) ) ;
#55872 = ORIENTED_EDGE ( 'NONE', *, *, #15780, .F. ) ;
#55873 = CYLINDRICAL_SURFACE ( 'NONE', #59268, 4.999999999999999112 ) ;
#55874 = CARTESIAN_POINT ( 'NONE',  ( -50.40829686548195099, -144.2500000013656063, -1.485763867205728284 ) ) ;
#55875 = CARTESIAN_POINT ( 'NONE',  ( 4.458734124999999437, -82.06249999863440792, -5.460374474430324690E-16 ) ) ;
#55876 = CARTESIAN_POINT ( 'NONE',  ( -51.75738570946856498, -133.8750000027312126, 3.805975901505576964 ) ) ;
#55877 = CARTESIAN_POINT ( 'NONE',  ( -2.498395430326213474E-14, 22.25000000000000000, 5.000000000000000000 ) ) ;
#55878 = CARTESIAN_POINT ( 'NONE',  ( 1.846868145590735200, -142.5000000013656063, -4.458734124999999437 ) ) ;
#55879 =( BOUNDED_CURVE ( )  B_SPLINE_CURVE ( 2, ( #39078, #19140, #44541, #24612, #4990, #34902, #24291, #40030, #4360 ),
 .UNSPECIFIED., .F., .F. ) 
 B_SPLINE_CURVE_WITH_KNOTS ( ( 3, 2, 2, 2, 3 ),
 ( 0.1562500000000000000, 0.1569444444444444420, 0.1583333333333333259, 0.1597222222222222099, 0.1604166666666666796 ),
 .UNSPECIFIED. ) 
 CURVE ( )  GEOMETRIC_REPRESENTATION_ITEM ( )  RATIONAL_B_SPLINE_CURVE ( ( 0.9330127018922194093, 0.9330127018922194093, 1.000000000000000000, 0.8660254037844387076, 1.000000000000000000, 0.8660254037844387076, 1.000000000000000000, 0.9330127018922180770, 0.9330127018922194093 ) ) 
 REPRESENTATION_ITEM ( '' )  );
#55880 = CARTESIAN_POINT ( 'NONE',  ( -6.972266317189433020E-16, -58.24999999999999289, -5.000000000000000000 ) ) ;
#55881 = CARTESIAN_POINT ( 'NONE',  ( 4.458734124999999437, -51.81249999863440792, -5.460374474430324690E-16 ) ) ;
#55882 = CARTESIAN_POINT ( 'NONE',  ( -3.152548672688508926E-16, -46.56249999863440792, -5.148502694627439702 ) ) ;
#55883 = CARTESIAN_POINT ( 'NONE',  ( 4.458734124999998549, 28.27083333469892779, -2.574251347313721627 ) ) ;
#55884 = CARTESIAN_POINT ( 'NONE',  ( -4.999999999999999112, -106.9166666666666572, 2.886751345948131764 ) ) ;
#55885 = CARTESIAN_POINT ( 'NONE',  ( -6.972266317189433020E-16, -3.250000000000001332, -5.000000000000000000 ) ) ;
#55886 = CARTESIAN_POINT ( 'NONE',  ( 9.457646018065525792E-16, -38.31249999863441502, 5.148502694627439702 ) ) ;
#55887 = CARTESIAN_POINT ( 'NONE',  ( 5.000000000000000000, -1.291666663935479908, -2.886751345948129988 ) ) ;
#55888 = CARTESIAN_POINT ( 'NONE',  ( -2.071067811865308972, -153.4375000027312410, 5.000000000000169642 ) ) ;
#55889 = CARTESIAN_POINT ( 'NONE',  ( -58.39396692619412477, -130.4375000013656063, 2.891590998281057701 ) ) ;
#55890 = CARTESIAN_POINT ( 'NONE',  ( 2.229367062499998831, -81.89583333196773651, -3.861377020970580887 ) ) ;
#55891 = CARTESIAN_POINT ( 'NONE',  ( 1.339745962155615144, 24.29465819873852084, 4.999999999999999112 ) ) ;
#55892 = CARTESIAN_POINT ( 'NONE',  ( 2.229367062499998831, -97.64583333196773651, -3.861377020970580887 ) ) ;
#55893 = CARTESIAN_POINT ( 'NONE',  ( 2.229367062499998831, -2.895833331967738289, -3.861377020970580887 ) ) ;
#55894 = ORIENTED_EDGE ( 'NONE', *, *, #24846, .F. ) ;
#55895 = CARTESIAN_POINT ( 'NONE',  ( -50.18089887299977647, -146.6875000000000000, 2.462841084822515292 ) ) ;
#55896 = CARTESIAN_POINT ( 'NONE',  ( 0.000000000000000000, -170.0000000000000000, 0.000000000000000000 ) ) ;
#55897 = CARTESIAN_POINT ( 'NONE',  ( -2.229367062499996610, -87.14583333196773651, 3.861377020970582219 ) ) ;
#55898 = FACE_OUTER_BOUND ( 'NONE', #61952, .T. ) ;
#55899 = CARTESIAN_POINT ( 'NONE',  ( -4.458734124999998549, -88.47916666530107932, 2.574251347313722516 ) ) ;
#55900 = CARTESIAN_POINT ( 'NONE',  ( -4.458734124999997661, 14.52083333469892779, 2.574251347313722516 ) ) ;
#55901 = CARTESIAN_POINT ( 'NONE',  ( -6.972266317189433020E-16, -77.12499999726881583, -5.000000000000000000 ) ) ;
#55902 = AXIS2_PLACEMENT_3D ( 'NONE', #3590, #57932, #42808 ) ;
#55903 = CARTESIAN_POINT ( 'NONE',  ( -50.70258187064364108, -133.1250000013656063, 2.196230717870141014 ) ) ;
#55904 = CARTESIAN_POINT ( 'NONE',  ( -2.229367062499996610, -5.145833331967740065, 3.861377020970582219 ) ) ;
#55905 = CARTESIAN_POINT ( 'NONE',  ( 4.458734125000001214, 14.85416666803225993, 2.574251347313718519 ) ) ;
#55906 = CARTESIAN_POINT ( 'NONE',  ( -2.229367062499996610, -46.39583333196774362, 3.861377020970582219 ) ) ;
#55907 = CARTESIAN_POINT ( 'NONE',  ( -5.000000000000000888, -163.5625000000000284, -2.071067811865475949 ) ) ;
#55908 = CARTESIAN_POINT ( 'NONE',  ( 2.229367062500001939, -82.97916666530106511, 3.861377020970579999 ) ) ;
#55909 = CARTESIAN_POINT ( 'NONE',  ( 2.229367062499998831, -4.645833331967740065, -3.861377020970580887 ) ) ;
#55910 = ORIENTED_EDGE ( 'NONE', *, *, #36622, .T. ) ;
#55911 = CARTESIAN_POINT ( 'NONE',  ( 4.458734124999998549, -33.97916666530107221, -2.574251347313721627 ) ) ;
#55912 = CARTESIAN_POINT ( 'NONE',  ( -56.48576386720575471, -128.0000000013656063, -4.591703134518078322 ) ) ;
#55913 = CARTESIAN_POINT ( 'NONE',  ( -2.229367062499996610, -77.14583333196773651, 3.861377020970582219 ) ) ;
#55914 = CARTESIAN_POINT ( 'NONE',  ( 4.458734124999999437, 28.93750000136559208, -5.460374474430324690E-16 ) ) ;
#55915 = CARTESIAN_POINT ( 'NONE',  ( -3.152548672688508926E-16, 18.43750000136559564, -5.148502694627439702 ) ) ;
#55916 = CARTESIAN_POINT ( 'NONE',  ( -1.339745962155610925, -93.79465819873851729, 5.000000000000000000 ) ) ;
#55917 = LINE ( 'NONE', #7029, #10089 ) ;
#55918 = CARTESIAN_POINT ( 'NONE',  ( 2.229367062500001939, -77.22916666530106511, 3.861377020970579999 ) ) ;
#55919 = CARTESIAN_POINT ( 'NONE',  ( -3.535250795749689387E-16, -65.25000000000000000, -5.773502691896257311 ) ) ;
#55920 = CARTESIAN_POINT ( 'NONE',  ( -5.000000000000000000, -31.95833333060214443, -2.886751345948128211 ) ) ;
#55921 = CARTESIAN_POINT ( 'NONE',  ( 5.000000000000000000, 19.70833333606451987, -2.886751345948129988 ) ) ;
#55922 = ORIENTED_EDGE ( 'NONE', *, *, #10976, .F. ) ;
#55923 = CARTESIAN_POINT ( 'NONE',  ( 5.000000000000000000, -1.291666663935479908, -2.886751345948130876 ) ) ;
#55924 = CARTESIAN_POINT ( 'NONE',  ( -60.14911071818854538, -139.1875000027312126, 1.666127454062681146 ) ) ;
#55926 = CARTESIAN_POINT ( 'NONE',  ( 5.000000000000000888, -23.58333333333333215, 2.886751345948126879 ) ) ;
#55925 = LINE ( 'NONE', #11532, #41040 ) ;
#55927 = CARTESIAN_POINT ( 'NONE',  ( 9.457646018065525792E-16, -25.06249999863440792, 5.148502694627439702 ) ) ;
#55928 = CARTESIAN_POINT ( 'NONE',  ( -3.152548672688508926E-16, -86.56249999863440792, -5.148502694627439702 ) ) ;
#55929 = ADVANCED_FACE ( 'NONE', ( #5311 ), #24929, .T. ) ;
#55930 = CARTESIAN_POINT ( 'NONE',  ( -5.000000000000000000, -25.87499999726881583, 0.000000000000000000 ) ) ;
#55932 = EDGE_LOOP ( 'NONE', ( #40586, #39036, #6637, #1451 ) ) ;
#55931 = CARTESIAN_POINT ( 'NONE',  ( -4.458734124999999437, -57.39583333196773651, -2.574251347313719407 ) ) ;
#55933 = CARTESIAN_POINT ( 'NONE',  ( 1.975475456537005874E-15, -91.74999999999998579, 5.000000000000000000 ) ) ;
#55934 = DIRECTION ( 'NONE',  ( 0.000000000000000000, 0.000000000000000000, 1.000000000000000000 ) ) ;
#55936 = ORIENTED_EDGE ( 'NONE', *, *, #35533, .T. ) ;
#55935 = CARTESIAN_POINT ( 'NONE',  ( -2.229367062500000163, -1.729166665301071992, -3.861377020970580443 ) ) ;
#55937 = CARTESIAN_POINT ( 'NONE',  ( 5.000000000000000000, -72.41666666666667140, -2.886751345948129988 ) ) ;
#55938 = CARTESIAN_POINT ( 'NONE',  ( -55.35523342533222291, -140.3125000013656063, 4.444560631937231499 ) ) ;
#55939 = CARTESIAN_POINT ( 'NONE',  ( 9.457646018065525792E-16, -46.31249999863440792, 5.148502694627439702 ) ) ;
#55940 = CARTESIAN_POINT ( 'NONE',  ( -2.500000000000000444, -96.16666666666665719, -4.330127018922193649 ) ) ;
#55941 = EDGE_CURVE ( 'NONE', #28941, #11293, #10443, .T. ) ;
#55942 = CARTESIAN_POINT ( 'NONE',  ( -2.071067811865475061, -158.6875000000000568, -5.000000000000000888 ) ) ;
#55943 = CARTESIAN_POINT ( 'NONE',  ( 5.000000000000000000, -73.29166666393548724, -2.886751345948129988 ) ) ;
#55944 = CARTESIAN_POINT ( 'NONE',  ( -5.000000000000000000, -53.95833333060214443, -2.886751345948128211 ) ) ;
#55945 = CARTESIAN_POINT ( 'NONE',  ( -51.75738570946856498, -152.7500000000000284, 3.805975901505576964 ) ) ;
#55946 = EDGE_CURVE ( 'NONE', #62883, #2464, #16227, .T. ) ;
#55947 = CARTESIAN_POINT ( 'NONE',  ( 9.457646018065525792E-16, -18.31249999863440436, 5.148502694627439702 ) ) ;
#55948 = CARTESIAN_POINT ( 'NONE',  ( 2.229367062500001939, -50.22916666530107221, 3.861377020970579999 ) ) ;
#55949 = CARTESIAN_POINT ( 'NONE',  ( -3.152801135295367985, -144.8125000013655779, 3.152801135295367096 ) ) ;
#55950 = CARTESIAN_POINT ( 'NONE',  ( 9.457646018065525792E-16, -95.31249999863440792, 5.148502694627439702 ) ) ;
#55951 = CARTESIAN_POINT ( 'NONE',  ( 3.535533905932736864, -148.2500000027311842, 3.535533905932738641 ) ) ;
#55952 = EDGE_LOOP ( 'NONE', ( #34356, #35764, #18814, #58162 ) ) ;
#55953 = EDGE_CURVE ( 'NONE', #3670, #44687, #15600, .T. ) ;
#55954 = CARTESIAN_POINT ( 'NONE',  ( -50.55543936806279248, -154.3125000013656347, 0.3552334253322060320 ) ) ;
#55955 = CARTESIAN_POINT ( 'NONE',  ( -2.229367062500000163, 24.27083333469892779, -3.861377020970580443 ) ) ;
#55956 = CARTESIAN_POINT ( 'NONE',  ( -50.18089887299979068, -144.8125000027312126, 2.462841084822635640 ) ) ;
#55957 = ADVANCED_FACE ( 'NONE', ( #54838 ), #10768, .T. ) ;
#55958 = CARTESIAN_POINT ( 'NONE',  ( 2.499999999999998668, -60.33333333333333570, -4.330127018922193649 ) ) ;
#55959 = CARTESIAN_POINT ( 'NONE',  ( -4.458734124999998549, -2.229166665301068662, 2.574251347313722516 ) ) ;
#55960 =( BOUNDED_CURVE ( )  B_SPLINE_CURVE ( 2, ( #36393, #60850, #31568, #51201, #7135, #52773, #14149, #32514, #33159 ),
 .UNSPECIFIED., .F., .F. ) 
 B_SPLINE_CURVE_WITH_KNOTS ( ( 3, 2, 2, 2, 3 ),
 ( 0.8017857142857143238, 0.8023809523809524169, 0.8035714285714286031, 0.8047619047619047894, 0.8053571428571428825 ),
 .UNSPECIFIED. ) 
 CURVE ( )  GEOMETRIC_REPRESENTATION_ITEM ( )  RATIONAL_B_SPLINE_CURVE ( ( 0.9330127018922194093, 0.9330127018922194093, 1.000000000000000000, 0.8660254037844387076, 1.000000000000000000, 0.8660254037844387076, 1.000000000000000000, 0.9330127018922194093, 0.9330127018922194093 ) ) 
 REPRESENTATION_ITEM ( '' )  );
#55961 = CARTESIAN_POINT ( 'NONE',  ( -4.458734124999997661, -97.47916666530105090, 2.574251347313722516 ) ) ;
#55962 = ADVANCED_FACE ( 'NONE', ( #49040 ), #34559, .T. ) ;
#55963 = CARTESIAN_POINT ( 'NONE',  ( -3.152801135295367985, -150.0625000013655779, 3.152801135295367096 ) ) ;
#55964 = CARTESIAN_POINT ( 'NONE',  ( -4.458734124999999437, -24.56249999863440436, 0.000000000000000000 ) ) ;
#55965 = CARTESIAN_POINT ( 'NONE',  ( -4.458734124999999437, -65.64583333196773651, -2.574251347313719407 ) ) ;
#55966 = DIRECTION ( 'NONE',  ( -0.000000000000000000, 1.000000000000000000, -0.000000000000000000 ) ) ;
#55967 = CARTESIAN_POINT ( 'NONE',  ( -4.458734124999999437, -9.395833331967736513, -2.574251347313719407 ) ) ;
#55968 = CARTESIAN_POINT ( 'NONE',  ( -6.972266317189433020E-16, 6.875000002731185944, -5.000000000000000000 ) ) ;
#55969 = CARTESIAN_POINT ( 'NONE',  ( -8.190561711645485556E-16, -144.6875000013656063, 4.458734124999999437 ) ) ;
#55970 = CARTESIAN_POINT ( 'NONE',  ( 2.229367062499998831, 16.10416666803225993, -3.861377020970580887 ) ) ;
#55971 = ORIENTED_EDGE ( 'NONE', *, *, #44976, .F. ) ;
#55972 = CARTESIAN_POINT ( 'NONE',  ( -1.339745962155613812, -27.08034179853029499, -5.000000000000000000 ) ) ;
#55973 = CARTESIAN_POINT ( 'NONE',  ( -6.972266317189433020E-16, -57.12499999726879452, -5.000000000000000000 ) ) ;
#55975 = CARTESIAN_POINT ( 'NONE',  ( -4.458734124999998549, -19.22916666530106866, 2.574251347313722516 ) ) ;
#55974 = CARTESIAN_POINT ( 'NONE',  ( -2.499999999999996447, -83.83333333333332860, 4.330127018922195425 ) ) ;
#55976 = CARTESIAN_POINT ( 'NONE',  ( -3.152548672688508926E-16, 26.18750000136560274, -5.148502694627439702 ) ) ;
#55977 = CARTESIAN_POINT ( 'NONE',  ( 1.975475456537005874E-15, -5.750000000000000000, 5.000000000000000000 ) ) ;
#55978 = CARTESIAN_POINT ( 'NONE',  ( -50.40829686548195099, -147.0000000013655779, -1.485763867205728284 ) ) ;
#55979 = CARTESIAN_POINT ( 'NONE',  ( -5.000000000000000000, -47.87499999726880873, 0.000000000000000000 ) ) ;
#55980 = CARTESIAN_POINT ( 'NONE',  ( 1.339745962155612702, -41.16965819600732601, -5.000000000000000000 ) ) ;
#55981 = CARTESIAN_POINT ( 'NONE',  ( -4.458734124999997661, 7.770833334698926009, 2.574251347313722516 ) ) ;
#55982 = DIRECTION ( 'NONE',  ( 0.000000000000000000, 0.000000000000000000, 1.000000000000000000 ) ) ;
#55983 = DIRECTION ( 'NONE',  ( 0.000000000000000000, 0.000000000000000000, 1.000000000000000000 ) ) ;
#55984 = CARTESIAN_POINT ( 'NONE',  ( -4.458734124999997661, 11.77083333469892601, 2.574251347313722516 ) ) ;
#55985 = CARTESIAN_POINT ( 'NONE',  ( -2.229367062500000163, -65.47916666530106511, -3.861377020970580443 ) ) ;
#55986 = CARTESIAN_POINT ( 'NONE',  ( -4.458734124999999437, -15.64583333196773829, -2.574251347313719407 ) ) ;
#55987 = CARTESIAN_POINT ( 'NONE',  ( -3.535250795749689387E-16, -0.2500000000000002220, -5.773502691896257311 ) ) ;
#55988 = CARTESIAN_POINT ( 'NONE',  ( 1.846868145590736310, -165.6250000013656063, 4.458734124999999437 ) ) ;
#55989 = CARTESIAN_POINT ( 'NONE',  ( -2.500000000000000444, -41.04166666393548013, -4.330127018922193649 ) ) ;
#55990 = CARTESIAN_POINT ( 'NONE',  ( -3.152548672688508926E-16, -58.56249999863440081, -5.148502694627439702 ) ) ;
#55991 = CARTESIAN_POINT ( 'NONE',  ( 2.500000000000002220, -93.54166666393547303, 4.330127018922192761 ) ) ;
#55992 = AXIS2_PLACEMENT_3D ( 'NONE', #14458, #49512, #15102 ) ;
#55993 = CARTESIAN_POINT ( 'NONE',  ( -1.339745962155610925, 10.20534180126147739, 5.000000000000000000 ) ) ;
#55994 = DIRECTION ( 'NONE',  ( -0.000000000000000000, 1.000000000000000000, -0.000000000000000000 ) ) ;
#55995 = CARTESIAN_POINT ( 'NONE',  ( -4.458734124999999437, -36.39583333196773651, -2.574251347313719407 ) ) ;
#55996 = CARTESIAN_POINT ( 'NONE',  ( 1.975475456537005874E-15, -90.62499999726880162, 5.000000000000000000 ) ) ;
#55997 = CARTESIAN_POINT ( 'NONE',  ( 2.499999999999998668, -49.33333333333332860, -4.330127018922193649 ) ) ;
#55998 = CARTESIAN_POINT ( 'NONE',  ( 0.000000000000000000, -120.0000000000000000, 5.000000000000000000 ) ) ;
#55999 = FACE_OUTER_BOUND ( 'NONE', #20016, .T. ) ;
#56000 = ORIENTED_EDGE ( 'NONE', *, *, #4580, .F. ) ;
#56001 = CARTESIAN_POINT ( 'NONE',  ( 9.457646018065525792E-16, -108.0624999986343937, 5.148502694627439702 ) ) ;
#56002 = CARTESIAN_POINT ( 'NONE',  ( -4.458734124999998549, -0.4791666653010707710, 2.574251347313722516 ) ) ;
#56003 = CARTESIAN_POINT ( 'NONE',  ( 2.500000000000002220, -73.54166666393548724, 4.330127018922192761 ) ) ;
#56004 = CARTESIAN_POINT ( 'NONE',  ( -5.000000000000000000, -10.00000000000000178, 0.000000000000000000 ) ) ;
#56005 = CARTESIAN_POINT ( 'NONE',  ( 2.229367062500001939, -73.97916666530106511, 3.861377020970579999 ) ) ;
#56006 = CARTESIAN_POINT ( 'NONE',  ( -1.339745962155613812, -17.20534180126147916, -5.000000000000000000 ) ) ;
#56007 = CARTESIAN_POINT ( 'NONE',  ( -5.000000000000000000, -7.874999997268813168, 0.000000000000000000 ) ) ;
#56009 = ORIENTED_EDGE ( 'NONE', *, *, #57810, .T. ) ;
#56008 = CARTESIAN_POINT ( 'NONE',  ( 4.458734124999999437, -37.81249999863440792, -5.460374474430324690E-16 ) ) ;
#56010 = CARTESIAN_POINT ( 'NONE',  ( -6.972266317189433020E-16, -17.12499999726881583, -5.000000000000000000 ) ) ;
#56012 = ORIENTED_EDGE ( 'NONE', *, *, #25191, .F. ) ;
#56011 = CARTESIAN_POINT ( 'NONE',  ( 2.229367062500001939, 14.77083333469892779, 3.861377020970579999 ) ) ;
#56013 =( BOUNDED_CURVE ( )  B_SPLINE_CURVE ( 2, ( #55871, #41370, #1850, #7304, #60384, #27534, #51039, #12431, #31401 ),
 .UNSPECIFIED., .F., .F. ) 
 B_SPLINE_CURVE_WITH_KNOTS ( ( 3, 2, 2, 2, 3 ),
 ( 0.5982142857142856984, 0.5988095238095237915, 0.5999999999999999778, 0.6011904761904761640, 0.6017857142857142572 ),
 .UNSPECIFIED. ) 
 CURVE ( )  GEOMETRIC_REPRESENTATION_ITEM ( )  RATIONAL_B_SPLINE_CURVE ( ( 0.9330127018922194093, 0.9330127018922194093, 1.000000000000000000, 0.8660254037844387076, 1.000000000000000000, 0.8660254037844387076, 1.000000000000000000, 0.9330127018922194093, 0.9330127018922194093 ) ) 
 REPRESENTATION_ITEM ( '' )  );
#56014 = DIRECTION ( 'NONE',  ( -0.000000000000000000, 1.000000000000000000, -0.000000000000000000 ) ) ;
#56015 = CARTESIAN_POINT ( 'NONE',  ( 5.000000000000000000, -53.41666666666667140, -2.886751345948129988 ) ) ;
#56016 = CARTESIAN_POINT ( 'NONE',  ( 4.458734124999999437, -160.7500000013655779, 1.846868145590737864 ) ) ;
#56017 = CARTESIAN_POINT ( 'NONE',  ( 4.458734125000001214, -29.14583333196774362, 2.574251347313718519 ) ) ;
#56018 = CARTESIAN_POINT ( 'NONE',  ( 1.975475456537005874E-15, -53.74999999999999289, 5.000000000000000000 ) ) ;
#56019 = CARTESIAN_POINT ( 'NONE',  ( -3.152548672688508926E-16, -74.56249999863440792, -5.148502694627439702 ) ) ;
#56020 = CARTESIAN_POINT ( 'NONE',  ( -4.458734124999999437, -141.1875000013656063, -5.460374474430324690E-16 ) ) ;
#56021 = CARTESIAN_POINT ( 'NONE',  ( 2.229367062500001939, -84.97916666530107932, 3.861377020970579999 ) ) ;
#56022 = CARTESIAN_POINT ( 'NONE',  ( -53.51423613279429503, -134.5000000013656063, 4.591703134518082763 ) ) ;
#56023 = CARTESIAN_POINT ( 'NONE',  ( 2.229367062499998831, -34.89583333196772941, -3.861377020970580887 ) ) ;
#56024 = CARTESIAN_POINT ( 'NONE',  ( 1.975475456537005874E-15, -70.62499999726880162, 5.000000000000000000 ) ) ;
#56025 = VERTEX_POINT ( 'NONE', #25563 ) ;
#56026 = CARTESIAN_POINT ( 'NONE',  ( -4.458734124999999437, -80.56249999863440792, 0.000000000000000000 ) ) ;
#56027 = CARTESIAN_POINT ( 'NONE',  ( 2.499999999999998668, 3.666666666666665186, -4.330127018922193649 ) ) ;
#56028 = ORIENTED_EDGE ( 'NONE', *, *, #2870, .F. ) ;
#56029 = CARTESIAN_POINT ( 'NONE',  ( -2.500000000000000444, -4.041666663935479242, -4.330127018922193649 ) ) ;
#56030 = CARTESIAN_POINT ( 'NONE',  ( 6.123233995736766282E-16, -170.0000000000000000, -5.000000000000000000 ) ) ;
#56031 = CARTESIAN_POINT ( 'NONE',  ( 9.457646018065525792E-16, -66.31249999863440792, 5.148502694627439702 ) ) ;
#56032 = CARTESIAN_POINT ( 'NONE',  ( 4.458734125000001214, -7.145833331967734736, 2.574251347313718519 ) ) ;
#56033 = ORIENTED_EDGE ( 'NONE', *, *, #17481, .F. ) ;
#56034 = VECTOR ( 'NONE', #17027, 1000.000000000000000 ) ;
#56035 = CARTESIAN_POINT ( 'NONE',  ( -2.499999999999996447, -84.83333333333332860, 4.330127018922195425 ) ) ;
#56036 = CARTESIAN_POINT ( 'NONE',  ( 5.000000000000000000, -62.41666666666666430, -2.886751345948130876 ) ) ;
#56037 = ORIENTED_EDGE ( 'NONE', *, *, #37679, .F. ) ;
#56038 = CARTESIAN_POINT ( 'NONE',  ( 2.229367062499998831, -5.895833331967740953, -3.861377020970580887 ) ) ;
#56039 = CARTESIAN_POINT ( 'NONE',  ( -50.18089887299978358, -150.8125000027312126, 2.462841084822590787 ) ) ;
#56040 = CARTESIAN_POINT ( 'NONE',  ( -2.229367062500000163, 7.520833334698929562, -3.861377020970580443 ) ) ;
#56041 = CARTESIAN_POINT ( 'NONE',  ( 5.000000000000000000, -154.0000000000000284, 0.000000000000000000 ) ) ;
#56042 = CARTESIAN_POINT ( 'NONE',  ( -3.152801135295367096, -156.0625000013656063, -3.152801135295367541 ) ) ;
#56043 = CARTESIAN_POINT ( 'NONE',  ( -6.972266317189433020E-16, -37.12499999726880873, -5.000000000000000000 ) ) ;
#56044 = ORIENTED_EDGE ( 'NONE', *, *, #59724, .T. ) ;
#56045 = CARTESIAN_POINT ( 'NONE',  ( -4.458734124999997661, -85.22916666530107932, 2.574251347313722516 ) ) ;
#56046 = FACE_OUTER_BOUND ( 'NONE', #26160, .T. ) ;
#56047 = CARTESIAN_POINT ( 'NONE',  ( -4.458734124999999437, -2.395833331967737845, -2.574251347313719407 ) ) ;
#56048 = CARTESIAN_POINT ( 'NONE',  ( 5.000000000000000000, -71.37499999726880162, -6.123233995736766282E-16 ) ) ;
#56049 = CARTESIAN_POINT ( 'NONE',  ( -5.000000000000000000, -28.87499999726881228, 0.000000000000000000 ) ) ;
#56050 = CARTESIAN_POINT ( 'NONE',  ( 0.000000000000000000, -170.0000000000000000, 0.000000000000000000 ) ) ;
#56051 = CARTESIAN_POINT ( 'NONE',  ( 9.457646018065525792E-16, 23.93750000136559564, 5.148502694627439702 ) ) ;
#56052 = CARTESIAN_POINT ( 'NONE',  ( -2.499999999999996447, -94.83333333333332860, 4.330127018922195425 ) ) ;
#56053 = CARTESIAN_POINT ( 'NONE',  ( 4.458734124999998549, 28.27083333469892779, -2.574251347313721627 ) ) ;
#56054 = CARTESIAN_POINT ( 'NONE',  ( 2.229367062499998831, -51.64583333196773651, -3.861377020970580887 ) ) ;
#56055 = CARTESIAN_POINT ( 'NONE',  ( -4.458734124999999437, -38.56249999863440081, 0.000000000000000000 ) ) ;
#56056 = CARTESIAN_POINT ( 'NONE',  ( 2.229367062499998831, 0.1041666680322607397, -3.861377020970580887 ) ) ;
#56057 =( BOUNDED_CURVE ( )  B_SPLINE_CURVE ( 2, ( #29584, #29905, #5793, #59517, #15766, #35382, #19307, #54035, #38921 ),
 .UNSPECIFIED., .F., .F. ) 
 B_SPLINE_CURVE_WITH_KNOTS ( ( 3, 2, 2, 2, 3 ),
 ( 0.7339285714285714857, 0.7345238095238095788, 0.7357142857142857650, 0.7369047619047619513, 0.7375000000000000444 ),
 .UNSPECIFIED. ) 
 CURVE ( )  GEOMETRIC_REPRESENTATION_ITEM ( )  RATIONAL_B_SPLINE_CURVE ( ( 0.9330127018922194093, 0.9330127018922256266, 1.000000000000000000, 0.8660254037844387076, 1.000000000000000000, 0.8660254037844387076, 1.000000000000000000, 0.9330127018922194093, 0.9330127018922194093 ) ) 
 REPRESENTATION_ITEM ( '' )  );
#56058 = CARTESIAN_POINT ( 'NONE',  ( -6.972266317189433020E-16, -18.25000000000000000, -5.000000000000000000 ) ) ;
#56059 = CARTESIAN_POINT ( 'NONE',  ( -5.000000000000000000, 16.00000000000000000, 0.000000000000000000 ) ) ;
#56060 = CARTESIAN_POINT ( 'NONE',  ( -5.000000000000000000, -144.6250000027312126, -6.123233995736766282E-16 ) ) ;
#56061 = CARTESIAN_POINT ( 'NONE',  ( -6.972266317189433020E-16, -75.12499999726880162, -5.000000000000000000 ) ) ;
#56062 = CARTESIAN_POINT ( 'NONE',  ( -2.229367062499996610, -45.14583333196774362, 3.861377020970582219 ) ) ;
#56063 = CARTESIAN_POINT ( 'NONE',  ( 5.000000000000000888, -78.45833333060214443, 2.886751345948126879 ) ) ;
#56064 = CARTESIAN_POINT ( 'NONE',  ( -59.59170313451811296, -138.7500000013656063, 1.485763867205729394 ) ) ;
#56065 = LINE ( 'NONE', #37698, #42146 ) ;
#56066 = CARTESIAN_POINT ( 'NONE',  ( 5.000000000000000000, -22.50000000000000000, -6.123233995736766282E-16 ) ) ;
#56067 = CARTESIAN_POINT ( 'NONE',  ( 9.457646018065525792E-16, -85.31249999863439371, 5.148502694627439702 ) ) ;
#56068 = CARTESIAN_POINT ( 'NONE',  ( -8.190561711645485556E-16, -159.9375000013655779, 4.458734124999999437 ) ) ;
#56069 = CARTESIAN_POINT ( 'NONE',  ( -7.968863443239230016, -4.547634245050486079, -8.057411785091789014 ) ) ;
#56070 = CARTESIAN_POINT ( 'NONE',  ( -3.535250795749689387E-16, -33.25000000000000000, -5.773502691896257311 ) ) ;
#56071 = ORIENTED_EDGE ( 'NONE', *, *, #35372, .T. ) ;
#56072 = CARTESIAN_POINT ( 'NONE',  ( -3.152548672688508926E-16, 21.18750000136559208, -5.148502694627439702 ) ) ;
#56073 = ORIENTED_EDGE ( 'NONE', *, *, #49967, .T. ) ;
#56074 = CARTESIAN_POINT ( 'NONE',  ( -4.458734124999999437, -89.31249999863440792, 0.000000000000000000 ) ) ;
#56075 = CARTESIAN_POINT ( 'NONE',  ( 4.458734124999999437, 12.93750000136559208, -5.460374474430324690E-16 ) ) ;
#56076 = CARTESIAN_POINT ( 'NONE',  ( -3.535250795749689387E-16, 15.87500000273118417, -5.773502691896257311 ) ) ;
#56077 = CARTESIAN_POINT ( 'NONE',  ( -1.336351044127974539E-14, 25.24999999999999645, 5.000000000000000000 ) ) ;
#56078 = CARTESIAN_POINT ( 'NONE',  ( -5.000000000000000000, 9.916666666666667851, -2.886751345948128211 ) ) ;
#56079 = CARTESIAN_POINT ( 'NONE',  ( 4.458734124999998549, -58.72916666530106511, -2.574251347313721627 ) ) ;
#56080 = CARTESIAN_POINT ( 'NONE',  ( 7.897825807688775512, 1.532833846124499910, -7.633607627188418121 ) ) ;
#56081 = CARTESIAN_POINT ( 'NONE',  ( -56.48576386720575471, -137.0000000013655779, -4.591703134518078322 ) ) ;
#56082 = CARTESIAN_POINT ( 'NONE',  ( 5.000000000000000000, 15.70833333606451809, -2.886751345948130876 ) ) ;
#56083 = CARTESIAN_POINT ( 'NONE',  ( -2.500000000000000444, -37.16666666666666430, -4.330127018922193649 ) ) ;
#56084 = CARTESIAN_POINT ( 'NONE',  ( -2.499999999999996447, 18.29166666939785202, 4.330127018922195425 ) ) ;
#56085 = CARTESIAN_POINT ( 'NONE',  ( -5.000000000000000000, -40.08333333333332860, -2.886751345948128211 ) ) ;
#56086 = CARTESIAN_POINT ( 'NONE',  ( 5.000000000000000000, -149.0625000000000000, 2.071067811865478614 ) ) ;
#56088 = CARTESIAN_POINT ( 'NONE',  ( -4.458734124999999437, -12.64583333196774007, -2.574251347313719407 ) ) ;
#56087 = CARTESIAN_POINT ( 'NONE',  ( -1.339745962155613812, 14.79465819873851906, -5.000000000000000000 ) ) ;
#56089 = CARTESIAN_POINT ( 'NONE',  ( -2.500000000000000444, -58.16666666666665719, -4.330127018922193649 ) ) ;
#56090 = CARTESIAN_POINT ( 'NONE',  ( 2.229367062500001939, -59.97916666530106511, 3.861377020970579999 ) ) ;
#56091 = CARTESIAN_POINT ( 'NONE',  ( 4.458734124999999437, -152.6875000013656063, 0.000000000000000000 ) ) ;
#56092 = CARTESIAN_POINT ( 'NONE',  ( -2.229367062500000163, -71.47916666530107932, -3.861377020970580443 ) ) ;
#56093 = CARTESIAN_POINT ( 'NONE',  ( -51.60603307380591787, -147.1875000013656063, -2.891590998281053704 ) ) ;
#56094 = CARTESIAN_POINT ( 'NONE',  ( 4.458734124999998549, -17.97916666530106866, -2.574251347313721627 ) ) ;
#56095 = CARTESIAN_POINT ( 'NONE',  ( -3.535250795749689387E-16, -59.12499999726880873, -5.773502691896257311 ) ) ;
#56096 = VERTEX_POINT ( 'NONE', #1462 ) ;
#56097 = CARTESIAN_POINT ( 'NONE',  ( 6.123233995736766282E-16, -170.0000000000000000, -5.000000000000000000 ) ) ;
#56098 = ORIENTED_EDGE ( 'NONE', *, *, #56171, .T. ) ;
#56099 = CARTESIAN_POINT ( 'NONE',  ( 4.458734124999998549, -61.97916666530106511, -2.574251347313721627 ) ) ;
#56101 = CARTESIAN_POINT ( 'NONE',  ( 2.499999999999998668, -8.333333333333332149, -4.330127018922193649 ) ) ;
#56100 = DIRECTION ( 'NONE',  ( 1.000000000000000000, 0.000000000000000000, 0.000000000000000000 ) ) ;
#56102 = CARTESIAN_POINT ( 'NONE',  ( 4.458734125000000326, -153.3750000013656347, -1.846868145590734978 ) ) ;
#56103 = ORIENTED_EDGE ( 'NONE', *, *, #28594, .F. ) ;
#56104 = CARTESIAN_POINT ( 'NONE',  ( 2.499999999999998668, 25.66666666666666430, -4.330127018922193649 ) ) ;
#56105 = CARTESIAN_POINT ( 'NONE',  ( 3.280815508853482498, 7.221948645665444921, -7.591546097228400569 ) ) ;
#56106 = FACE_OUTER_BOUND ( 'NONE', #39461, .T. ) ;
#56107 = CARTESIAN_POINT ( 'NONE',  ( 2.229367062500001939, -48.22916666530106511, 3.861377020970579999 ) ) ;
#56108 = ORIENTED_EDGE ( 'NONE', *, *, #7870, .F. ) ;
#56109 = CARTESIAN_POINT ( 'NONE',  ( -5.000000000000000000, 17.12500000273118417, 0.000000000000000000 ) ) ;
#56110 = CARTESIAN_POINT ( 'NONE',  ( -3.152548672688508926E-16, 8.437500001365595637, -5.148502694627439702 ) ) ;
#56111 = CARTESIAN_POINT ( 'NONE',  ( -2.229367062499996610, 25.85416666803225993, 3.861377020970582219 ) ) ;
#56112 = CARTESIAN_POINT ( 'NONE',  ( -50.70258187064364108, -149.1250000013656063, 2.196230717870141014 ) ) ;
#56113 = CARTESIAN_POINT ( 'NONE',  ( 5.000000000000000000, -78.29166666393547303, -2.886751345948130876 ) ) ;
#56114 = CARTESIAN_POINT ( 'NONE',  ( 4.458734124999999437, -167.3750000013656347, -1.846868145590734978 ) ) ;
#56115 = VERTEX_POINT ( 'NONE', #39387 ) ;
#56116 = CARTESIAN_POINT ( 'NONE',  ( -2.229367062500000163, -70.47916666530107932, -3.861377020970580443 ) ) ;
#56117 = CARTESIAN_POINT ( 'NONE',  ( -0.2791032213812780771, 8.821394357840562250, -7.929128246061909024 ) ) ;
#56118 = CARTESIAN_POINT ( 'NONE',  ( 9.457646018065525792E-16, 14.93750000136559564, 5.148502694627439702 ) ) ;
#56119 = AXIS2_PLACEMENT_3D ( 'NONE', #50129, #1905, #49808 ) ;
#56120 = AXIS2_PLACEMENT_3D ( 'NONE', #2905, #36989, #51781 ) ;
#56121 = FACE_OUTER_BOUND ( 'NONE', #20307, .T. ) ;
#56122 = DIRECTION ( 'NONE',  ( 0.000000000000000000, 0.000000000000000000, 1.000000000000000000 ) ) ;
#56123 = CARTESIAN_POINT ( 'NONE',  ( 2.229367062500001939, -57.22916666530107932, 3.861377020970579999 ) ) ;
#56124 = CARTESIAN_POINT ( 'NONE',  ( 5.000000000000000000, -14.37499999726881228, -6.123233995736766282E-16 ) ) ;
#56125 = CYLINDRICAL_SURFACE ( 'NONE', #50151, 5.000000000000000000 ) ;
#56126 = CARTESIAN_POINT ( 'NONE',  ( -1.339745962155613812, -45.08034179853028434, -5.000000000000000000 ) ) ;
#56127 = CARTESIAN_POINT ( 'NONE',  ( -58.24261429053147765, -138.2500000000000000, -3.805975901505573855 ) ) ;
#56128 = CARTESIAN_POINT ( 'NONE',  ( -3.152548672688508926E-16, -19.81249999863440081, -5.148502694627439702 ) ) ;
#56129 = ORIENTED_EDGE ( 'NONE', *, *, #43284, .T. ) ;
#56130 = CARTESIAN_POINT ( 'NONE',  ( -58.24261429053147765, -140.3750000027312126, -3.805975901505573855 ) ) ;
#56131 = CARTESIAN_POINT ( 'NONE',  ( -2.500000000000000444, 29.83333333333333215, -4.330127018922193649 ) ) ;
#56133 = CARTESIAN_POINT ( 'NONE',  ( 2.071067811865476394, -156.3125000027312410, 5.000000000000000000 ) ) ;
#56132 = APPLICATION_CONTEXT ( 'automotive_design' ) ;
#56134 = VERTEX_POINT ( 'NONE', #40350 ) ;
#56135 = CARTESIAN_POINT ( 'NONE',  ( 9.457646018065525792E-16, -102.3124999986344221, 5.148502694627439702 ) ) ;
#56136 = EDGE_CURVE ( 'NONE', #56532, #11538, #40668, .T. ) ;
#56137 = CARTESIAN_POINT ( 'NONE',  ( 2.229367062499998831, -26.64583333196774007, -3.861377020970580887 ) ) ;
#56138 = CARTESIAN_POINT ( 'NONE',  ( -5.000000000000000000, -63.95833333060213732, -2.886751345948128211 ) ) ;
#56139 =( BOUNDED_CURVE ( )  B_SPLINE_CURVE ( 2, ( #39765, #29477, #59412, #30119, #24674, #49110, #5694, #886, #35278 ),
 .UNSPECIFIED., .F., .F. ) 
 B_SPLINE_CURVE_WITH_KNOTS ( ( 3, 2, 2, 2, 3 ),
 ( 0.6479166666666666963, 0.6486111111111111382, 0.6500000000000000222, 0.6513888888888889062, 0.6520833333333333481 ),
 .UNSPECIFIED. ) 
 CURVE ( )  GEOMETRIC_REPRESENTATION_ITEM ( )  RATIONAL_B_SPLINE_CURVE ( ( 0.9330127018922194093, 0.9330127018922194093, 1.000000000000000000, 0.8660254037844387076, 1.000000000000000000, 0.8660254037844387076, 1.000000000000000000, 0.9330127018922194093, 0.9330127018922194093 ) ) 
 REPRESENTATION_ITEM ( '' )  );
#56140 = CARTESIAN_POINT ( 'NONE',  ( -56.48576386720575471, -151.0000000013656063, -4.591703134518078322 ) ) ;
#56141 = CARTESIAN_POINT ( 'NONE',  ( 2.071067811865475505, -147.8125000000000284, -5.000000000000000888 ) ) ;
#56142 = CARTESIAN_POINT ( 'NONE',  ( 2.229367062500001939, -22.97916666530107221, 3.861377020970579999 ) ) ;
#56143 = CARTESIAN_POINT ( 'NONE',  ( -3.152548672688508926E-16, -71.81249999863439371, -5.148502694627439702 ) ) ;
#56144 = CARTESIAN_POINT ( 'NONE',  ( -51.75738570946856498, -147.7500000000000284, 3.805975901505576964 ) ) ;
#56145 = CARTESIAN_POINT ( 'NONE',  ( -2.229367062500000163, -27.47916666530107221, -3.861377020970580443 ) ) ;
#56146 = CARTESIAN_POINT ( 'NONE',  ( -9.184850993605147944E-16, -151.2500000000000284, 5.000000000000000000 ) ) ;
#56147 = CARTESIAN_POINT ( 'NONE',  ( -2.500000000000000444, -17.16666666666666430, -4.330127018922193649 ) ) ;
#56148 = CARTESIAN_POINT ( 'NONE',  ( -4.458734124999999437, -150.9375000013656063, -5.460374474430324690E-16 ) ) ;
#56149 = ORIENTED_EDGE ( 'NONE', *, *, #17370, .F. ) ;
#56150 = CARTESIAN_POINT ( 'NONE',  ( 4.458734124999999437, -52.06249999863440792, -5.460374474430324690E-16 ) ) ;
#56151 = DIRECTION ( 'NONE',  ( 0.000000000000000000, 0.000000000000000000, 1.000000000000000000 ) ) ;
#56152 = CARTESIAN_POINT ( 'NONE',  ( 6.123233995736766282E-16, -120.0000000000000000, -5.000000000000000000 ) ) ;
#56153 = CARTESIAN_POINT ( 'NONE',  ( -5.000000000000000000, 23.00000000000000000, 0.000000000000000000 ) ) ;
#56154 = CARTESIAN_POINT ( 'NONE',  ( 6.123233995736766282E-16, -120.0000000000000000, -5.000000000000000000 ) ) ;
#56155 = CARTESIAN_POINT ( 'NONE',  ( 4.458734124999998549, 2.270833334698928230, -2.574251347313721627 ) ) ;
#56156 =( BOUNDED_CURVE ( )  B_SPLINE_CURVE ( 2, ( #40254, #39920, #11294, #40567, #21275, #59568, #50546, #59895, #15815 ),
 .UNSPECIFIED., .F., .F. ) 
 B_SPLINE_CURVE_WITH_KNOTS ( ( 3, 2, 2, 2, 3 ),
 ( 0.9375000000000000000, 0.9380952380952380931, 0.9392857142857142794, 0.9404761904761904656, 0.9410714285714285587 ),
 .UNSPECIFIED. ) 
 CURVE ( )  GEOMETRIC_REPRESENTATION_ITEM ( )  RATIONAL_B_SPLINE_CURVE ( ( 0.9330127018922194093, 0.9330127018922194093, 1.000000000000000000, 0.8660254037844387076, 1.000000000000000000, 0.8660254037844387076, 1.000000000000000000, 0.9330127018922194093, 0.9330127018922194093 ) ) 
 REPRESENTATION_ITEM ( '' )  );
#56157 = EDGE_CURVE ( 'NONE', #51535, #51665, #16240, .T. ) ;
#56158 = CARTESIAN_POINT ( 'NONE',  ( -5.000000000000000888, -142.5625000000000000, -2.071067811865475949 ) ) ;
#56159 = EDGE_CURVE ( 'NONE', #8173, #10657, #47035, .T. ) ;
#56160 = CARTESIAN_POINT ( 'NONE',  ( 1.975475456537005874E-15, -37.62499999726880873, 5.000000000000000000 ) ) ;
#56161 = CYLINDRICAL_SURFACE ( 'NONE', #49903, 5.000000000000000000 ) ;
#56162 = CARTESIAN_POINT ( 'NONE',  ( 4.458734124999999437, 17.93750000136559208, -5.460374474430324690E-16 ) ) ;
#56163 = CARTESIAN_POINT ( 'NONE',  ( -3.535250795749689387E-16, 4.875000002731184168, -5.773502691896257311 ) ) ;
#56164 = ORIENTED_EDGE ( 'NONE', *, *, #38743, .T. ) ;
#56165 = ORIENTED_EDGE ( 'NONE', *, *, #13377, .T. ) ;
#56166 = VECTOR ( 'NONE', #31033, 1000.000000000000000 ) ;
#56167 = CARTESIAN_POINT ( 'NONE',  ( -1.339745962155610925, -70.79465819873850307, 5.000000000000000000 ) ) ;
#56168 = CARTESIAN_POINT ( 'NONE',  ( 2.229367062499998831, -41.64583333196773651, -3.861377020970580887 ) ) ;
#56169 = CARTESIAN_POINT ( 'NONE',  ( -3.152801135295367985, -162.0625000013656063, 3.152801135295367096 ) ) ;
#56170 = VECTOR ( 'NONE', #62578, 1000.000000000000000 ) ;
#56171 = EDGE_CURVE ( 'NONE', #29860, #33989, #44961, .T. ) ;
#56172 = CARTESIAN_POINT ( 'NONE',  ( -3.535250795749689387E-16, -47.12499999726880873, -5.773502691896257311 ) ) ;
#56173 = VERTEX_POINT ( 'NONE', #22660 ) ;
#56174 = CARTESIAN_POINT ( 'NONE',  ( -2.229367062500000163, -19.47916666530106866, -3.861377020970580443 ) ) ;
#56175 = ORIENTED_EDGE ( 'NONE', *, *, #8811, .T. ) ;
#56176 = CARTESIAN_POINT ( 'NONE',  ( 5.000000000000000888, -89.58333333333334281, 2.886751345948126879 ) ) ;
#56177 = CARTESIAN_POINT ( 'NONE',  ( -8.190561711645485556E-16, -165.6875000013655779, 4.458734124999999437 ) ) ;
#56179 = EDGE_LOOP ( 'NONE', ( #62674, #54690, #36543, #10576 ) ) ;
#56178 = LINE ( 'NONE', #61325, #37480 ) ;
#56180 = CARTESIAN_POINT ( 'NONE',  ( -60.14911071818854538, -137.0625000000000284, 1.666127454062681368 ) ) ;
#56181 = CARTESIAN_POINT ( 'NONE',  ( 4.458734124999999437, -33.06249999863440792, -5.460374474430324690E-16 ) ) ;
#56182 = EDGE_LOOP ( 'NONE', ( #19120, #49115, #26535, #21540 ) ) ;
#56183 = EDGE_CURVE ( 'NONE', #7429, #59301, #49076, .T. ) ;
#56184 = CARTESIAN_POINT ( 'NONE',  ( 9.457646018065525792E-16, -77.06249999863440792, 5.148502694627439702 ) ) ;
#56185 = CARTESIAN_POINT ( 'NONE',  ( 2.229367062499998831, 25.35416666803225993, -3.861377020970580887 ) ) ;
#56186 = CARTESIAN_POINT ( 'NONE',  ( -1.339745962155610925, -28.66965819600733312, 5.000000000000000000 ) ) ;
#56187 = ORIENTED_EDGE ( 'NONE', *, *, #11497, .F. ) ;
#56188 = CARTESIAN_POINT ( 'NONE',  ( -5.000000000000000000, -161.5000000000000000, -6.123233995736766282E-16 ) ) ;
#56189 = CARTESIAN_POINT ( 'NONE',  ( -51.60603307380591787, -142.1875000013656063, -2.891590998281053704 ) ) ;
#56190 = CARTESIAN_POINT ( 'NONE',  ( -3.152548672688508926E-16, -80.81249999863440792, -5.148502694627439702 ) ) ;
#56191 = CARTESIAN_POINT ( 'NONE',  ( -59.98410592259440222, -129.2500000027312126, -0.3983568153799752487 ) ) ;
#56192 = DIRECTION ( 'NONE',  ( 0.000000000000000000, -0.000000000000000000, 1.000000000000000000 ) ) ;
#56193 = CARTESIAN_POINT ( 'NONE',  ( -1.846868145590734756, -143.3750000013656063, -4.458734124999999437 ) ) ;
#56194 = CARTESIAN_POINT ( 'NONE',  ( 1.339745962155612702, -84.16965819600731891, -5.000000000000000000 ) ) ;
#56195 = CARTESIAN_POINT ( 'NONE',  ( -4.458734124999999437, -57.31249999863440081, 0.000000000000000000 ) ) ;
#56196 = CARTESIAN_POINT ( 'NONE',  ( 4.458734124999998549, -45.72916666530106511, -2.574251347313721627 ) ) ;
#56197 = CARTESIAN_POINT ( 'NONE',  ( 2.229367062499998831, 26.35416666803225993, -3.861377020970580887 ) ) ;
#56198 = CARTESIAN_POINT ( 'NONE',  ( -5.000000000000000000, -106.9999999999999858, 0.000000000000000000 ) ) ;
#56199 = CARTESIAN_POINT ( 'NONE',  ( -2.500000000000000444, 3.833333333333334370, -4.330127018922193649 ) ) ;
#56200 = CARTESIAN_POINT ( 'NONE',  ( 4.458734124999999437, -39.06249999863440081, -5.460374474430324690E-16 ) ) ;
#56201 = CARTESIAN_POINT ( 'NONE',  ( 5.000000000000000000, -1.374999997268814500, -6.123233995736766282E-16 ) ) ;
#56202 = LINE ( 'NONE', #37523, #56373 ) ;
#56203 = CARTESIAN_POINT ( 'NONE',  ( 4.458734124999998549, -78.97916666530106511, -2.574251347313721627 ) ) ;
#56204 = CARTESIAN_POINT ( 'NONE',  ( -59.98410592259440222, -142.2500000027312126, -0.3983568153799752487 ) ) ;
#56205 = CARTESIAN_POINT ( 'NONE',  ( 9.457646018065525792E-16, -105.0624999986344079, 5.148502694627439702 ) ) ;
#56206 = CARTESIAN_POINT ( 'NONE',  ( 2.229367062499998831, -5.895833331967740953, -3.861377020970580887 ) ) ;
#56207 =( BOUNDED_CURVE ( )  B_SPLINE_CURVE ( 2, ( #39567, #30559, #55018, #20928, #60491, #20285, #30887, #40532, #60174 ),
 .UNSPECIFIED., .F., .F. ) 
 B_SPLINE_CURVE_WITH_KNOTS ( ( 3, 2, 2, 2, 3 ),
 ( 0.4660714285714285809, 0.4666666666666666741, 0.4678571428571428603, 0.4690476190476190466, 0.4696428571428571397 ),
 .UNSPECIFIED. ) 
 CURVE ( )  GEOMETRIC_REPRESENTATION_ITEM ( )  RATIONAL_B_SPLINE_CURVE ( ( 0.9330127018922194093, 0.9330127018922194093, 1.000000000000000000, 0.8660254037844387076, 1.000000000000000000, 0.8660254037844387076, 1.000000000000000000, 0.9330127018922194093, 0.9330127018922194093 ) ) 
 REPRESENTATION_ITEM ( '' )  );
#56208 = ORIENTED_EDGE ( 'NONE', *, *, #26033, .T. ) ;
#56209 = AXIS2_PLACEMENT_3D ( 'NONE', #11001, #20673, #55403 ) ;
#56210 = CARTESIAN_POINT ( 'NONE',  ( -6.972266317189433020E-16, -47.12499999726880873, -5.000000000000000000 ) ) ;
#56211 = CARTESIAN_POINT ( 'NONE',  ( -1.339745962155613812, -36.08034179853029144, -5.000000000000000000 ) ) ;
#56212 = CARTESIAN_POINT ( 'NONE',  ( 2.229367062500001939, -94.97916666530106511, 3.861377020970579999 ) ) ;
#56213 = CARTESIAN_POINT ( 'NONE',  ( -2.071067811865475061, -168.8125000027312126, -5.000000000000000888 ) ) ;
#56214 = CARTESIAN_POINT ( 'NONE',  ( 9.457646018065525792E-16, -89.31249999863440792, 5.148502694627439702 ) ) ;
#56215 = EDGE_CURVE ( 'NONE', #49700, #62694, #38378, .T. ) ;
#56216 = AXIS2_PLACEMENT_3D ( 'NONE', #39319, #29339, #48972 ) ;
#56217 = CARTESIAN_POINT ( 'NONE',  ( 4.458734125000000326, 14.85416666803225993, 2.574251347313718519 ) ) ;
#56218 = CARTESIAN_POINT ( 'NONE',  ( 1.975475456537005874E-15, -73.62499999726878741, 5.000000000000000000 ) ) ;
#56219 = VECTOR ( 'NONE', #45277, 1000.000000000000000 ) ;
#56220 = CARTESIAN_POINT ( 'NONE',  ( -51.60603307380591787, -132.9375000013656063, -2.891590998281053704 ) ) ;
#56221 = VECTOR ( 'NONE', #41967, 1000.000000000000000 ) ;
#56222 = CARTESIAN_POINT ( 'NONE',  ( -4.458734124999999437, -9.395833331967736513, -2.574251347313719407 ) ) ;
#56223 = CARTESIAN_POINT ( 'NONE',  ( -2.229367062500000163, 16.27083333469892779, -3.861377020970580443 ) ) ;
#56224 = CARTESIAN_POINT ( 'NONE',  ( -4.458734124999997661, -52.47916666530107221, 2.574251347313722516 ) ) ;
#56225 = CARTESIAN_POINT ( 'NONE',  ( -1.339745962155599601, 16.91965820146970501, -5.000000000000007994 ) ) ;
#56226 = CARTESIAN_POINT ( 'NONE',  ( 4.458734124999998549, -85.72916666530106511, -2.574251347313721627 ) ) ;
#56227 = CARTESIAN_POINT ( 'NONE',  ( -4.458734124999999437, -8.395833331967736513, -2.574251347313719407 ) ) ;
#56228 = CARTESIAN_POINT ( 'NONE',  ( 5.000000000000000888, -106.4583333306021586, 2.886751345948126879 ) ) ;
#56229 = ORIENTED_EDGE ( 'NONE', *, *, #51725, .T. ) ;
#56230 = CARTESIAN_POINT ( 'NONE',  ( -4.458734124999999437, -34.64583333196772941, -2.574251347313719407 ) ) ;
#56231 = CARTESIAN_POINT ( 'NONE',  ( -53.51423613279429503, -127.5000000013656347, 4.591703134518082763 ) ) ;
#56232 = CARTESIAN_POINT ( 'NONE',  ( -4.458734124999998549, -81.22916666530106511, 2.574251347313722516 ) ) ;
#56233 = CARTESIAN_POINT ( 'NONE',  ( -4.999999999999999112, -109.7916666639354730, 2.886751345948131764 ) ) ;
#56234 = CARTESIAN_POINT ( 'NONE',  ( 3.152801135295367541, -148.5625000013655779, -3.152801135295367541 ) ) ;
#56235 = CARTESIAN_POINT ( 'NONE',  ( -2.229367062500000163, 21.52083333469892779, -3.861377020970580443 ) ) ;
#56236 = LINE ( 'NONE', #22137, #17459 ) ;
#56237 = EDGE_CURVE ( 'NONE', #19793, #7158, #34650, .T. ) ;
#56238 = CARTESIAN_POINT ( 'NONE',  ( 2.500000000000002220, 1.333333333333332149, 4.330127018922192761 ) ) ;
#56239 = CARTESIAN_POINT ( 'NONE',  ( -3.152548672688508926E-16, -83.81249999863437949, -5.148502694627439702 ) ) ;
#56240 = CARTESIAN_POINT ( 'NONE',  ( 2.500000000000002220, -64.66666666666665719, 4.330127018922192761 ) ) ;
#56241 = CARTESIAN_POINT ( 'NONE',  ( 5.000000000000000888, -63.45833333060215153, 2.886751345948126879 ) ) ;
#56242 = CARTESIAN_POINT ( 'NONE',  ( -2.499999999999996447, 17.29166666939785557, 4.330127018922195425 ) ) ;
#56243 = ORIENTED_EDGE ( 'NONE', *, *, #14083, .T. ) ;
#56244 = CARTESIAN_POINT ( 'NONE',  ( 5.000000000000000000, -147.1875000027312410, 2.071067811865478614 ) ) ;
#56245 =( BOUNDED_CURVE ( )  B_SPLINE_CURVE ( 2, ( #15958, #1190, #31705, #11756, #31374, #1825, #36528, #21426, #40392 ),
 .UNSPECIFIED., .F., .F. ) 
 B_SPLINE_CURVE_WITH_KNOTS ( ( 3, 2, 2, 2, 3 ),
 ( 0.8874999999999999556, 0.8880952380952380487, 0.8892857142857142350, 0.8904761904761904212, 0.8910714285714286254 ),
 .UNSPECIFIED. ) 
 CURVE ( )  GEOMETRIC_REPRESENTATION_ITEM ( )  RATIONAL_B_SPLINE_CURVE ( ( 0.9330127018922194093, 0.9330127018922194093, 1.000000000000000000, 0.8660254037844387076, 1.000000000000000000, 0.8660254037844387076, 1.000000000000000000, 0.9330127018922130810, 0.9330127018922194093 ) ) 
 REPRESENTATION_ITEM ( '' )  );
#56246 = CARTESIAN_POINT ( 'NONE',  ( -1.975475456537005874E-15, 28.25000000000000000, 5.000000000000000000 ) ) ;
#56248 = CARTESIAN_POINT ( 'NONE',  ( 1.060575238724906964E-15, -21.75000000000000000, 5.773502691896257311 ) ) ;
#56247 = LINE ( 'NONE', #16681, #36925 ) ;
#56249 = CARTESIAN_POINT ( 'NONE',  ( 2.229367062500001939, -29.97916666530107221, 3.861377020970579999 ) ) ;
#56250 = CARTESIAN_POINT ( 'NONE',  ( -3.152548672688508926E-16, -89.56249999863439371, -5.148502694627439702 ) ) ;
#56251 = CARTESIAN_POINT ( 'NONE',  ( -5.000000000000000000, -27.87499999726880873, 0.000000000000000000 ) ) ;
#56253 = ORIENTED_EDGE ( 'NONE', *, *, #28252, .T. ) ;
#56252 = CARTESIAN_POINT ( 'NONE',  ( 4.458734124999998549, -53.72916666530106511, -2.574251347313721627 ) ) ;
#56254 = CARTESIAN_POINT ( 'NONE',  ( -53.51423613279429503, -153.5000000013656063, 4.591703134518082763 ) ) ;
#56256 = ORIENTED_EDGE ( 'NONE', *, *, #39714, .T. ) ;
#56255 = CARTESIAN_POINT ( 'NONE',  ( 4.458734124999999437, -5.062499998634402587, -5.460374474430324690E-16 ) ) ;
#56257 = CARTESIAN_POINT ( 'NONE',  ( -3.535250795749689387E-16, -71.25000000000000000, -5.773502691896257311 ) ) ;
#56258 = CARTESIAN_POINT ( 'NONE',  ( -50.70258187064364108, -140.1250000013656347, 2.196230717870141014 ) ) ;
#56259 = CARTESIAN_POINT ( 'NONE',  ( 9.457646018065525792E-16, -51.31249999863440792, 5.148502694627439702 ) ) ;
#56260 = CARTESIAN_POINT ( 'NONE',  ( -51.75738570946856498, -141.8750000027312126, 3.805975901505576964 ) ) ;
#56261 = VECTOR ( 'NONE', #31584, 1000.000000000000000 ) ;
#56262 = CARTESIAN_POINT ( 'NONE',  ( 2.499999999999998668, -77.20833333060214443, -4.330127018922193649 ) ) ;
#56263 = CARTESIAN_POINT ( 'NONE',  ( -4.999999999999998224, -85.91666666666667140, 2.886751345948131764 ) ) ;
#56264 = CARTESIAN_POINT ( 'NONE',  ( -60.14911071818854538, -151.0625000000000000, 1.666127454062681368 ) ) ;
#56265 = EDGE_CURVE ( 'NONE', #26190, #56652, #60197, .T. ) ;
#56266 = CARTESIAN_POINT ( 'NONE',  ( 4.458734124999999437, -18.06249999863440792, -5.460374474430324690E-16 ) ) ;
#56267 = AXIS2_PLACEMENT_3D ( 'NONE', #62253, #38415, #58039 ) ;
#56268 = CARTESIAN_POINT ( 'NONE',  ( 9.457646018065525792E-16, -54.31249999863440081, 5.148502694627439702 ) ) ;
#56269 = CARTESIAN_POINT ( 'NONE',  ( 1.846868145590736310, -140.6250000013656063, 4.458734124999999437 ) ) ;
#56270 = CARTESIAN_POINT ( 'NONE',  ( -4.458734124999999437, -99.64583333196773651, -2.574251347313719407 ) ) ;
#56271 = CARTESIAN_POINT ( 'NONE',  ( -6.972266317189433020E-16, -21.12499999726881228, -5.000000000000000000 ) ) ;
#56272 = EDGE_LOOP ( 'NONE', ( #62125, #31936, #25314, #17431 ) ) ;
#56273 = DIRECTION ( 'NONE',  ( -0.000000000000000000, 1.000000000000000000, -0.000000000000000000 ) ) ;
#56274 = CARTESIAN_POINT ( 'NONE',  ( -58.24261429053147765, -142.3750000027312126, -3.805975901505573855 ) ) ;
#56275 = CARTESIAN_POINT ( 'NONE',  ( 1.975475456537005874E-15, -60.75000000000000000, 5.000000000000000000 ) ) ;
#56276 = CARTESIAN_POINT ( 'NONE',  ( -4.458734124999999437, -3.312499998634407916, 0.000000000000000000 ) ) ;
#56277 = CARTESIAN_POINT ( 'NONE',  ( 9.457646018065525792E-16, -95.31249999863440792, 5.148502694627439702 ) ) ;
#56278 = CARTESIAN_POINT ( 'NONE',  ( 4.458734125000000326, -147.6250000013655779, -1.846868145590734978 ) ) ;
#56279 = CARTESIAN_POINT ( 'NONE',  ( 2.229367062500001939, -25.22916666530106866, 3.861377020970579999 ) ) ;
#56280 = CARTESIAN_POINT ( 'NONE',  ( -7.500000000000000888, 2.575910028905295857, -0.3641256808890092067 ) ) ;
#56281 = CARTESIAN_POINT ( 'NONE',  ( -59.59170313451811296, -140.5000000013656347, 1.485763867205729394 ) ) ;
#56282 = CARTESIAN_POINT ( 'NONE',  ( 4.458734124999998549, -65.97916666530106511, -2.574251347313721627 ) ) ;
#56283 = CARTESIAN_POINT ( 'NONE',  ( 2.500000000000002220, -72.66666666666667140, 4.330127018922192761 ) ) ;
#56284 = CARTESIAN_POINT ( 'NONE',  ( -6.972266317189433020E-16, -55.24999999999999289, -5.000000000000000000 ) ) ;
#56285 = CARTESIAN_POINT ( 'NONE',  ( 1.846868145590735200, -144.2500000013656063, -4.458734124999999437 ) ) ;
#56286 = CARTESIAN_POINT ( 'NONE',  ( 9.457646018065525792E-16, 10.68750000136559386, 5.148502694627439702 ) ) ;
#56287 = EDGE_LOOP ( 'NONE', ( #4112, #61901, #54268, #25466, #52782 ) ) ;
#56288 = LINE ( 'NONE', #62379, #13047 ) ;
#56290 = CARTESIAN_POINT ( 'NONE',  ( 4.458734124999999437, -23.81249999863440436, -5.460374474430324690E-16 ) ) ;
#56289 = CARTESIAN_POINT ( 'NONE',  ( 5.000000000000000000, -87.50000000000000000, -6.123233995736766282E-16 ) ) ;
#56291 = CARTESIAN_POINT ( 'NONE',  ( 2.229367062500001939, 28.77083333469892779, 3.861377020970579999 ) ) ;
#56292 = CARTESIAN_POINT ( 'NONE',  ( -1.339745962155613812, -18.08034179853029499, -5.000000000000000000 ) ) ;
#56293 = CARTESIAN_POINT ( 'NONE',  ( -52.80376928212989185, -143.8750000013655779, -4.297418129356379346 ) ) ;
#56294 = EDGE_CURVE ( 'NONE', #16469, #12275, #24857, .T. ) ;
#56295 = EDGE_CURVE ( 'NONE', #44367, #49592, #57699, .T. ) ;
#56296 = CARTESIAN_POINT ( 'NONE',  ( 2.499999999999998668, -47.20833333060214443, -4.330127018922193649 ) ) ;
#56297 = CARTESIAN_POINT ( 'NONE',  ( 6.158835246850667461E-14, -2.124999997268816276, -4.999999999999999112 ) ) ;
#56298 = CARTESIAN_POINT ( 'NONE',  ( 9.457646018065525792E-16, 7.937500001365596525, 5.148502694627439702 ) ) ;
#56299 = FACE_OUTER_BOUND ( 'NONE', #50349, .T. ) ;
#56301 = EDGE_CURVE ( 'NONE', #50806, #11542, #11704, .T. ) ;
#56300 = CARTESIAN_POINT ( 'NONE',  ( -50.01589407740564042, -141.7500000027312126, 0.3983568153799778022 ) ) ;
#56302 = CARTESIAN_POINT ( 'NONE',  ( 2.229367062500001939, 9.020833334698927786, 3.861377020970579999 ) ) ;
#56303 = CARTESIAN_POINT ( 'NONE',  ( 2.229367062500001939, -64.97916666530106511, 3.861377020970579999 ) ) ;
#56304 = CARTESIAN_POINT ( 'NONE',  ( -4.458734124999997661, -18.47916666530106511, 2.574251347313722516 ) ) ;
#56305 = EDGE_CURVE ( 'NONE', #62567, #5493, #28408, .T. ) ;
#56306 = VECTOR ( 'NONE', #50983, 1000.000000000000000 ) ;
#56307 = CARTESIAN_POINT ( 'NONE',  ( -2.500000000000000444, -0.1666666666666656582, -4.330127018922193649 ) ) ;
#56308 = CARTESIAN_POINT ( 'NONE',  ( 3.152801135295367541, -161.3125000013656063, -3.152801135295367541 ) ) ;
#56309 = CARTESIAN_POINT ( 'NONE',  ( -3.152548672688508926E-16, -62.56249999863440792, -5.148502694627439702 ) ) ;
#56310 = CARTESIAN_POINT ( 'NONE',  ( -2.500000000000000444, -93.04166666393547303, -4.330127018922193649 ) ) ;
#56311 = CIRCLE ( 'NONE', #36788, 5.000000000000000000 ) ;
#56312 = EDGE_CURVE ( 'NONE', #5760, #47469, #3092, .T. ) ;
#56313 = EDGE_CURVE ( 'NONE', #18131, #45003, #53224, .T. ) ;
#56314 = CARTESIAN_POINT ( 'NONE',  ( -5.000000000000000000, -80.00000000000000000, 0.000000000000000000 ) ) ;
#56315 = CARTESIAN_POINT ( 'NONE',  ( 5.000000000000000888, -56.58333333333333570, 2.886751345948126879 ) ) ;
#56316 = CARTESIAN_POINT ( 'NONE',  ( -4.458734124999997661, -33.22916666530106511, 2.574251347313722516 ) ) ;
#56317 = EDGE_CURVE ( 'NONE', #456, #11867, #25233, .T. ) ;
#56318 = CARTESIAN_POINT ( 'NONE',  ( 6.123233995736766282E-16, -114.9999999999999858, -5.000000000000000000 ) ) ;
#56319 = CARTESIAN_POINT ( 'NONE',  ( -3.152548672688508926E-16, -69.81249999863439371, -5.148502694627439702 ) ) ;
#56320 = CARTESIAN_POINT ( 'NONE',  ( -2.499999999999996447, -48.83333333333332860, 4.330127018922195425 ) ) ;
#56321 = CARTESIAN_POINT ( 'NONE',  ( -6.972266317189433020E-16, -72.12499999726878741, -5.000000000000000000 ) ) ;
#56322 = EDGE_CURVE ( 'NONE', #62531, #25786, #23598, .T. ) ;
#56323 = EDGE_LOOP ( 'NONE', ( #17749, #39662, #39513, #238 ) ) ;
#56324 = CARTESIAN_POINT ( 'NONE',  ( -4.458734124999999437, -106.3958333319677507, -2.574251347313719407 ) ) ;
#56325 = CARTESIAN_POINT ( 'NONE',  ( 4.458734124999998549, -2.979166665301069994, -2.574251347313721627 ) ) ;
#56326 = DIRECTION ( 'NONE',  ( -0.000000000000000000, 1.000000000000000000, -0.000000000000000000 ) ) ;
#56327 = EDGE_CURVE ( 'NONE', #14198, #52848, #14243, .T. ) ;
#56328 = CARTESIAN_POINT ( 'NONE',  ( 5.000000000000000000, -8.416666666666669627, -2.886751345948129988 ) ) ;
#56329 = EDGE_CURVE ( 'NONE', #40984, #143, #48696, .T. ) ;
#56330 = CARTESIAN_POINT ( 'NONE',  ( 4.458734124999999437, -70.81249999863439371, -5.460374474430324690E-16 ) ) ;
#56331 = VECTOR ( 'NONE', #12276, 1000.000000000000000 ) ;
#56332 = LINE ( 'NONE', #62098, #25718 ) ;
#56333 = CARTESIAN_POINT ( 'NONE',  ( 5.000000000000000000, -13.29166666393548191, -2.886751345948129988 ) ) ;
#56335 = VERTEX_POINT ( 'NONE', #62529 ) ;
#56334 = CARTESIAN_POINT ( 'NONE',  ( 4.458734124999999437, -40.81249999863440081, -5.460374474430324690E-16 ) ) ;
#56336 = CARTESIAN_POINT ( 'NONE',  ( 1.975475456537005874E-15, -41.74999999999999289, 5.000000000000000000 ) ) ;
#56338 = ORIENTED_EDGE ( 'NONE', *, *, #42224, .F. ) ;
#56337 = CARTESIAN_POINT ( 'NONE',  ( 2.229367062500001939, 11.77083333469892601, 3.861377020970579999 ) ) ;
#56339 = CARTESIAN_POINT ( 'NONE',  ( -2.071067811865348496, -151.6875000000000000, -5.000000000000127898 ) ) ;
#56340 = CARTESIAN_POINT ( 'NONE',  ( -4.999999999999999112, -57.91666666666665719, 2.886751345948131764 ) ) ;
#56341 = CARTESIAN_POINT ( 'NONE',  ( -8.190561711645485556E-16, -160.9375000013655779, 4.458734124999999437 ) ) ;
#56342 = CARTESIAN_POINT ( 'NONE',  ( -3.152548672688508926E-16, -36.81249999863440792, -5.148502694627439702 ) ) ;
#56343 = LINE ( 'NONE', #22237, #22472 ) ;
#56344 = CARTESIAN_POINT ( 'NONE',  ( 4.458734125000001214, -79.89583333196773651, 2.574251347313718519 ) ) ;
#56345 = CARTESIAN_POINT ( 'NONE',  ( 3.535533905932738197, -169.8750000000000284, -3.535533905932738197 ) ) ;
#56346 = CARTESIAN_POINT ( 'NONE',  ( 4.458734124999998549, -86.72916666530107932, -2.574251347313721627 ) ) ;
#56347 = CARTESIAN_POINT ( 'NONE',  ( -56.48576386720575471, -134.0000000013656063, -4.591703134518078322 ) ) ;
#56348 = CARTESIAN_POINT ( 'NONE',  ( 9.457646018065525792E-16, -0.3124999986344051961, 5.148502694627439702 ) ) ;
#56349 = CARTESIAN_POINT ( 'NONE',  ( 4.458734125000001214, -36.14583333196773651, 2.574251347313718519 ) ) ;
#56350 =( BOUNDED_CURVE ( )  B_SPLINE_CURVE ( 2, ( #23504, #28002, #3577, #23183, #62437, #37980, #57611, #9324, #43731 ),
 .UNSPECIFIED., .F., .F. ) 
 B_SPLINE_CURVE_WITH_KNOTS ( ( 3, 2, 2, 2, 3 ),
 ( 0.8020833333333333703, 0.8027777777777778123, 0.8041666666666666963, 0.8055555555555555802, 0.8062500000000000222 ),
 .UNSPECIFIED. ) 
 CURVE ( )  GEOMETRIC_REPRESENTATION_ITEM ( )  RATIONAL_B_SPLINE_CURVE ( ( 0.9330127018922194093, 0.9330127018922194093, 1.000000000000000000, 0.8660254037844387076, 1.000000000000000000, 0.8660254037844387076, 1.000000000000000000, 0.9330127018922194093, 0.9330127018922194093 ) ) 
 REPRESENTATION_ITEM ( '' )  );
#56351 = CARTESIAN_POINT ( 'NONE',  ( -6.972266317189433020E-16, -72.25000000000000000, -5.000000000000000000 ) ) ;
#56352 = CARTESIAN_POINT ( 'NONE',  ( -4.458734124999999437, -78.56249999863440792, 0.000000000000000000 ) ) ;
#56353 = CARTESIAN_POINT ( 'NONE',  ( 1.339745962155612702, 3.705341801261478718, -5.000000000000000000 ) ) ;
#56354 = ORIENTED_EDGE ( 'NONE', *, *, #42929, .T. ) ;
#56355 = CARTESIAN_POINT ( 'NONE',  ( -5.000000000000000000, -14.87499999726881228, 0.000000000000000000 ) ) ;
#56356 = VECTOR ( 'NONE', #5069, 1000.000000000000000 ) ;
#56357 = LINE ( 'NONE', #32521, #46578 ) ;
#56358 = CARTESIAN_POINT ( 'NONE',  ( 2.229367062499998831, -70.89583333196773651, -3.861377020970580887 ) ) ;
#56359 = CARTESIAN_POINT ( 'NONE',  ( 2.229367062499998831, -9.895833331967738289, -3.861377020970580887 ) ) ;
#56360 = ORIENTED_EDGE ( 'NONE', *, *, #35745, .F. ) ;
#56361 = CARTESIAN_POINT ( 'NONE',  ( -3.535533905932738641, -150.5000000027312126, 3.535533905932737309 ) ) ;
#56362 = CARTESIAN_POINT ( 'NONE',  ( 5.000000000000000000, 17.50000000000000000, -6.123233995736766282E-16 ) ) ;
#56363 = CARTESIAN_POINT ( 'NONE',  ( 2.229367062500001939, -6.229166665301072214, 3.861377020970579999 ) ) ;
#56364 = CARTESIAN_POINT ( 'NONE',  ( 4.458734125000001214, 7.104166668032259047, 2.574251347313718519 ) ) ;
#56365 = LINE ( 'NONE', #61188, #4855 ) ;
#56366 = CARTESIAN_POINT ( 'NONE',  ( -3.152801135295367985, -158.8125000013656063, 3.152801135295367096 ) ) ;
#56367 = CARTESIAN_POINT ( 'NONE',  ( -3.152548672688508926E-16, 29.18750000136559208, -5.148502694627439702 ) ) ;
#56368 = ORIENTED_EDGE ( 'NONE', *, *, #15269, .F. ) ;
#56369 = CARTESIAN_POINT ( 'NONE',  ( 9.457646018065525792E-16, -86.06249999863439371, 5.148502694627439702 ) ) ;
#56370 = CARTESIAN_POINT ( 'NONE',  ( -5.000000000000000000, -67.99999999999998579, 0.000000000000000000 ) ) ;
#56371 = CARTESIAN_POINT ( 'NONE',  ( 4.458734125000001214, -0.8958333319677401763, 2.574251347313718519 ) ) ;
#56372 = CARTESIAN_POINT ( 'NONE',  ( 2.071067811865434205, -140.1874999999999716, 5.000000000000041744 ) ) ;
#56373 = VECTOR ( 'NONE', #57164, 1000.000000000000000 ) ;
#56374 = CARTESIAN_POINT ( 'NONE',  ( 5.000000000000000000, -32.29166666393548724, -2.886751345948129988 ) ) ;
#56375 = DIRECTION ( 'NONE',  ( -1.000000000000000000, 0.000000000000000000, 0.000000000000000000 ) ) ;
#56376 = CARTESIAN_POINT ( 'NONE',  ( -2.229367062500000163, 22.52083333469892423, -3.861377020970580443 ) ) ;
#56377 = CARTESIAN_POINT ( 'NONE',  ( -2.500000000000000444, -21.04166666393548013, -4.330127018922193649 ) ) ;
#56378 = CARTESIAN_POINT ( 'NONE',  ( -4.458734124999999437, 27.68750000136559208, 0.000000000000000000 ) ) ;
#56379 = CARTESIAN_POINT ( 'NONE',  ( 9.457646018065525792E-16, -50.06249999863440792, 5.148502694627439702 ) ) ;
#56380 = CARTESIAN_POINT ( 'NONE',  ( -3.152548672688508926E-16, -37.81249999863440792, -5.148502694627439702 ) ) ;
#56381 = CARTESIAN_POINT ( 'NONE',  ( -4.458734124999997661, -3.479166665301069994, 2.574251347313722516 ) ) ;
#56382 = CARTESIAN_POINT ( 'NONE',  ( 2.499999999999998668, -0.2083333306021478704, -4.330127018922193649 ) ) ;
#56383 = CARTESIAN_POINT ( 'NONE',  ( -3.535250795749689387E-16, 13.75000000000000000, -5.773502691896257311 ) ) ;
#56384 = CARTESIAN_POINT ( 'NONE',  ( 3.535533905932736864, -143.2500000027311842, 3.535533905932738641 ) ) ;
#56385 = CARTESIAN_POINT ( 'NONE',  ( 1.975475456537005874E-15, -70.62499999726880162, 5.000000000000000000 ) ) ;
#56386 = CARTESIAN_POINT ( 'NONE',  ( 4.458734124999999437, -42.81249999863440081, -5.460374474430324690E-16 ) ) ;
#56387 = CARTESIAN_POINT ( 'NONE',  ( -2.500000000000000444, -81.04166666393547303, -4.330127018922193649 ) ) ;
#56388 = CARTESIAN_POINT ( 'NONE',  ( -59.44456063193725015, -139.8125000013656063, -0.3552334253322034230 ) ) ;
#56389 = CARTESIAN_POINT ( 'NONE',  ( 0.000000000000000000, -170.0000000000000000, 5.000000000000000000 ) ) ;
#56390 = CARTESIAN_POINT ( 'NONE',  ( -2.500000000000000444, -64.04166666393547303, -4.330127018922193649 ) ) ;
#56391 = CARTESIAN_POINT ( 'NONE',  ( -4.458734124999999437, -87.64583333196773651, -2.574251347313719407 ) ) ;
#56392 = CARTESIAN_POINT ( 'NONE',  ( -4.458734124999999437, -162.2500000013656063, -1.846868145590735644 ) ) ;
#56393 =( BOUNDED_CURVE ( )  B_SPLINE_CURVE ( 2, ( #59492, #35049, #25715, #35684, #54344, #40183, #29880, #44355, #54661 ),
 .UNSPECIFIED., .F., .F. ) 
 B_SPLINE_CURVE_WITH_KNOTS ( ( 3, 2, 2, 2, 3 ),
 ( 0.8812499999999999778, 0.8819444444444444198, 0.8833333333333333037, 0.8847222222222221877, 0.8854166666666666297 ),
 .UNSPECIFIED. ) 
 CURVE ( )  GEOMETRIC_REPRESENTATION_ITEM ( )  RATIONAL_B_SPLINE_CURVE ( ( 0.9330127018922194093, 0.9330127018922194093, 1.000000000000000000, 0.8660254037844387076, 1.000000000000000000, 0.8660254037844387076, 1.000000000000000000, 0.9330127018922194093, 0.9330127018922194093 ) ) 
 REPRESENTATION_ITEM ( '' )  );
#56394 = CARTESIAN_POINT ( 'NONE',  ( -5.000000000000000000, -33.08333333333332149, -2.886751345948128211 ) ) ;
#56395 = CARTESIAN_POINT ( 'NONE',  ( -55.00000000000002132, -155.0000000000000284, 1.734723475976807094E-15 ) ) ;
#56396 = VERTEX_POINT ( 'NONE', #38071 ) ;
#56397 = EDGE_CURVE ( 'NONE', #54515, #3670, #22433, .T. ) ;
#56398 = CARTESIAN_POINT ( 'NONE',  ( -2.229367062500000163, 20.27083333469892779, -3.861377020970580443 ) ) ;
#56399 = ORIENTED_EDGE ( 'NONE', *, *, #28053, .F. ) ;
#56400 = CARTESIAN_POINT ( 'NONE',  ( 4.458734124999999437, -89.81249999863440792, -5.460374474430324690E-16 ) ) ;
#56401 = CARTESIAN_POINT ( 'NONE',  ( 2.229367062499998831, 16.10416666803225993, -3.861377020970580887 ) ) ;
#56402 =( BOUNDED_CURVE ( )  B_SPLINE_CURVE ( 2, ( #38123, #48075, #4029, #53538, #8846, #23648, #13671, #19752, #5288 ),
 .UNSPECIFIED., .F., .F. ) 
 B_SPLINE_CURVE_WITH_KNOTS ( ( 3, 2, 2, 2, 3 ),
 ( 0.6416666666666662744, 0.6458333333333329263, 0.6499999999999996891, 0.6541666666666663410, 0.6583333333333329929 ),
 .UNSPECIFIED. ) 
 CURVE ( )  GEOMETRIC_REPRESENTATION_ITEM ( )  RATIONAL_B_SPLINE_CURVE ( ( 1.000000000000008216, 0.9238795325112786339, 1.000000000000000000, 0.9238795325112867385, 1.000000000000000000, 0.9238795325112867385, 1.000000000000000000, 0.9238795325112928447, 0.9999999999999938938 ) ) 
 REPRESENTATION_ITEM ( '' )  );
#56403 = CARTESIAN_POINT ( 'NONE',  ( 2.499999999999998668, 13.79166666939785202, -4.330127018922193649 ) ) ;
#56404 = CARTESIAN_POINT ( 'NONE',  ( -1.339745962155613812, -29.08034179853029144, -5.000000000000000000 ) ) ;
#56405 = CARTESIAN_POINT ( 'NONE',  ( -5.000000000000000000, 9.000000000000001776, 0.000000000000000000 ) ) ;
#56406 = CARTESIAN_POINT ( 'NONE',  ( -2.229367062500000163, -54.47916666530107221, -3.861377020970580443 ) ) ;
#56407 = CARTESIAN_POINT ( 'NONE',  ( 7.500000000000000888, -4.651016565836964212, -7.928861822685564498 ) ) ;
#56408 = EDGE_CURVE ( 'NONE', #2867, #5270, #35574, .T. ) ;
#56409 = CARTESIAN_POINT ( 'NONE',  ( -6.972266317189433020E-16, -52.25000000000000711, -5.000000000000000000 ) ) ;
#56410 = LINE ( 'NONE', #41904, #50223 ) ;
#56411 = CARTESIAN_POINT ( 'NONE',  ( -2.500000000000000444, -64.16666666666665719, -4.330127018922193649 ) ) ;
#56412 = DIRECTION ( 'NONE',  ( 0.000000000000000000, 1.000000000000000000, 0.000000000000000000 ) ) ;
#56413 = CARTESIAN_POINT ( 'NONE',  ( 1.060575238724906964E-15, -39.75000000000000000, 5.773502691896257311 ) ) ;
#56414 = CARTESIAN_POINT ( 'NONE',  ( -1.339745962155613812, 12.91965820146970678, -5.000000000000000000 ) ) ;
#56416 = CARTESIAN_POINT ( 'NONE',  ( 4.458734125000001214, -14.14583333196774184, 2.574251347313718519 ) ) ;
#56415 = CARTESIAN_POINT ( 'NONE',  ( -4.999999999999998224, 15.08333333333333215, 2.886751345948131764 ) ) ;
#56417 = CARTESIAN_POINT ( 'NONE',  ( -5.000000000000000000, 13.00000000000000178, 0.000000000000000000 ) ) ;
#56418 = CARTESIAN_POINT ( 'NONE',  ( 9.457646018065525792E-16, -66.06249999863440792, 5.148502694627439702 ) ) ;
#56419 = CARTESIAN_POINT ( 'NONE',  ( 3.152801135295367541, -152.5625000013655779, -3.152801135295367541 ) ) ;
#56420 = CARTESIAN_POINT ( 'NONE',  ( -4.458734124999999437, -71.39583333196773651, -2.574251347313719407 ) ) ;
#56421 = CARTESIAN_POINT ( 'NONE',  ( -55.35523342533222291, -146.5625000013656063, 4.444560631937231499 ) ) ;
#56422 = CARTESIAN_POINT ( 'NONE',  ( 4.458734125000001214, -17.14583333196773651, 2.574251347313718519 ) ) ;
#56423 = CARTESIAN_POINT ( 'NONE',  ( 2.500000000000002220, -58.54166666393548013, 4.330127018922192761 ) ) ;
#56424 = ORIENTED_EDGE ( 'NONE', *, *, #59779, .F. ) ;
#56425 = CARTESIAN_POINT ( 'NONE',  ( 1.339745962155615144, -85.58034179853028434, 4.999999999999999112 ) ) ;
#56426 = ORIENTED_EDGE ( 'NONE', *, *, #26357, .T. ) ;
#56427 =( BOUNDED_CURVE ( )  B_SPLINE_CURVE ( 2, ( #6549, #40321, #1428, #30984, #15567, #5589, #60595, #50930, #21027 ),
 .UNSPECIFIED., .F., .F. ) 
 B_SPLINE_CURVE_WITH_KNOTS ( ( 3, 2, 2, 2, 3 ),
 ( 0.6410714285714286254, 0.6416666666666667185, 0.6428571428571429047, 0.6440476190476190910, 0.6446428571428571841 ),
 .UNSPECIFIED. ) 
 CURVE ( )  GEOMETRIC_REPRESENTATION_ITEM ( )  RATIONAL_B_SPLINE_CURVE ( ( 0.9330127018922194093, 0.9330127018922256266, 1.000000000000000000, 0.8660254037844387076, 1.000000000000000000, 0.8660254037844387076, 1.000000000000000000, 0.9330127018922194093, 0.9330127018922194093 ) ) 
 REPRESENTATION_ITEM ( '' )  );
#56428 = CARTESIAN_POINT ( 'NONE',  ( 2.229367062499998831, -61.89583333196774362, -3.861377020970580887 ) ) ;
#56429 = DIRECTION ( 'NONE',  ( 0.000000000000000000, 1.000000000000000000, 0.000000000000000000 ) ) ;
#56430 = CARTESIAN_POINT ( 'NONE',  ( -4.458734124999999437, -151.9375000013655779, -5.460374474430324690E-16 ) ) ;
#56431 = ORIENTED_EDGE ( 'NONE', *, *, #40450, .T. ) ;
#56432 = CARTESIAN_POINT ( 'NONE',  ( 3.535533905932736864, -155.2500000027312126, 3.535533905932738641 ) ) ;
#56433 = CARTESIAN_POINT ( 'NONE',  ( -52.53715891517739323, -125.4375000000000284, -4.819101127000233298 ) ) ;
#56434 = CARTESIAN_POINT ( 'NONE',  ( -6.972266317189433020E-16, -85.25000000000000000, -5.000000000000000000 ) ) ;
#56435 = CARTESIAN_POINT ( 'NONE',  ( -2.229367062500000163, -50.72916666530107221, -3.861377020970580443 ) ) ;
#56436 = EDGE_LOOP ( 'NONE', ( #3357, #20343, #31246, #39696 ) ) ;
#56437 = CARTESIAN_POINT ( 'NONE',  ( 1.975475456537005874E-15, -109.6249999972688158, 5.000000000000000000 ) ) ;
#56438 = CARTESIAN_POINT ( 'NONE',  ( 4.458734125000001214, 9.104166668032261711, 2.574251347313718519 ) ) ;
#56439 = CARTESIAN_POINT ( 'NONE',  ( 2.229367062500001939, 26.02083333469892779, 3.861377020970579999 ) ) ;
#56440 = CARTESIAN_POINT ( 'NONE',  ( -57.89159099828107458, -147.6875000013656063, -3.393966926194107447 ) ) ;
#56441 = DIRECTION ( 'NONE',  ( 0.000000000000000000, 1.000000000000000000, 0.000000000000000000 ) ) ;
#56442 = CARTESIAN_POINT ( 'NONE',  ( 3.535533905932736864, -165.1250000000000284, 3.535533905932738641 ) ) ;
#56443 =( BOUNDED_CURVE ( )  B_SPLINE_CURVE ( 2, ( #33886, #14892, #29352, #14266, #34499, #30005, #35170, #20698, #53506 ),
 .UNSPECIFIED., .F., .F. ) 
 B_SPLINE_CURVE_WITH_KNOTS ( ( 3, 2, 2, 2, 3 ),
 ( 0.006250000000000000347, 0.006944444444444444059, 0.008333333333333333218, 0.009722222222222222376, 0.01041666666666666782 ),
 .UNSPECIFIED. ) 
 CURVE ( )  GEOMETRIC_REPRESENTATION_ITEM ( )  RATIONAL_B_SPLINE_CURVE ( ( 0.9330127018922194093, 0.9330127018922194093, 1.000000000000000000, 0.8660254037844387076, 1.000000000000000000, 0.8660254037844387076, 1.000000000000000000, 0.9330127018922191873, 0.9330127018922192983 ) ) 
 REPRESENTATION_ITEM ( '' )  );
#56444 = ORIENTED_EDGE ( 'NONE', *, *, #62832, .F. ) ;
#56445 = CARTESIAN_POINT ( 'NONE',  ( 4.458734125000000326, -68.89583333196773651, 2.574251347313718519 ) ) ;
#56446 = DIRECTION ( 'NONE',  ( -0.000000000000000000, 1.000000000000000000, -0.000000000000000000 ) ) ;
#56447 = CARTESIAN_POINT ( 'NONE',  ( -4.458734124999999437, 13.60416666803226349, -2.574251347313719407 ) ) ;
#56448 = VECTOR ( 'NONE', #6397, 1000.000000000000000 ) ;
#56449 = DIRECTION ( 'NONE',  ( -0.000000000000000000, 1.000000000000000000, -0.000000000000000000 ) ) ;
#56450 = CARTESIAN_POINT ( 'NONE',  ( -4.458734124999998549, -53.47916666530106511, 2.574251347313722516 ) ) ;
#56451 = CARTESIAN_POINT ( 'NONE',  ( -3.535250795749689387E-16, -12.12499999726881761, -5.773502691896257311 ) ) ;
#56452 = FACE_OUTER_BOUND ( 'NONE', #58502, .T. ) ;
#56453 = CARTESIAN_POINT ( 'NONE',  ( -3.096526599377909417, 6.872473572140716414, 1.143494478793305063E-15 ) ) ;
#56454 = CARTESIAN_POINT ( 'NONE',  ( -6.972266317189433020E-16, 18.74999999999999645, -5.000000000000000000 ) ) ;
#56455 = CARTESIAN_POINT ( 'NONE',  ( 2.229367062499998831, -33.64583333196772941, -3.861377020970580887 ) ) ;
#56456 = CARTESIAN_POINT ( 'NONE',  ( 2.229367062500001939, -22.22916666530107221, 3.861377020970579999 ) ) ;
#56457 = ORIENTED_EDGE ( 'NONE', *, *, #8306, .F. ) ;
#56458 = DIRECTION ( 'NONE',  ( -0.000000000000000000, 1.000000000000000000, -0.000000000000000000 ) ) ;
#56459 = CARTESIAN_POINT ( 'NONE',  ( -4.999999999999999112, 29.08333333333333215, 2.886751345948131764 ) ) ;
#56460 = CARTESIAN_POINT ( 'NONE',  ( -9.184850993605147944E-16, -155.3750000027311842, 5.000000000000000000 ) ) ;
#56461 = ORIENTED_EDGE ( 'NONE', *, *, #25667, .F. ) ;
#56462 = CARTESIAN_POINT ( 'NONE',  ( 4.458734125000001214, -102.1458333319677365, 2.574251347313718519 ) ) ;
#56463 = CARTESIAN_POINT ( 'NONE',  ( -2.229367062500000163, -27.47916666530107221, -3.861377020970580443 ) ) ;
#56464 = CARTESIAN_POINT ( 'NONE',  ( -2.500000000000000444, -63.04166666393547303, -4.330127018922193649 ) ) ;
#56465 = CARTESIAN_POINT ( 'NONE',  ( -54.64476657466781973, -152.0625000013656063, -4.444560631937228834 ) ) ;
#56466 = CARTESIAN_POINT ( 'NONE',  ( -2.071067811865478170, -146.3125000000000000, 5.000000000000000000 ) ) ;
#56467 = CARTESIAN_POINT ( 'NONE',  ( -4.458734124999999437, -30.31249999863440436, 0.000000000000000000 ) ) ;
#56468 = CARTESIAN_POINT ( 'NONE',  ( -4.458734124999999437, -68.56249999863439371, 0.000000000000000000 ) ) ;
#56469 = CARTESIAN_POINT ( 'NONE',  ( -1.339745962155610925, -89.79465819873851729, 5.000000000000000000 ) ) ;
#56470 = CARTESIAN_POINT ( 'NONE',  ( 4.458734124999998549, -25.72916666530107221, -2.574251347313721627 ) ) ;
#56471 = CARTESIAN_POINT ( 'NONE',  ( -1.339745962155613812, -33.20534180126147561, -5.000000000000000000 ) ) ;
#56472 = CARTESIAN_POINT ( 'NONE',  ( -51.75738570946856498, -137.8750000027312126, 3.805975901505576964 ) ) ;
#56473 = CARTESIAN_POINT ( 'NONE',  ( -2.500000000000000444, -14.16666666666666785, -4.330127018922193649 ) ) ;
#56474 = CARTESIAN_POINT ( 'NONE',  ( -4.458734125000000326, -152.0000000013655779, -1.846868145590735644 ) ) ;
#56475 = EDGE_LOOP ( 'NONE', ( #32626, #59844, #34469, #57346 ) ) ;
#56476 = CARTESIAN_POINT ( 'NONE',  ( -6.031010364368858512E-14, 3.249999999999997335, 5.000000000000000000 ) ) ;
#56477 = CARTESIAN_POINT ( 'NONE',  ( 2.229367062500001939, -53.22916666530107221, 3.861377020970579999 ) ) ;
#56478 = CYLINDRICAL_SURFACE ( 'NONE', #12988, 5.000000000000000000 ) ;
#56479 = CARTESIAN_POINT ( 'NONE',  ( 1.975475456537005874E-15, -81.62499999726881583, 5.000000000000000000 ) ) ;
#56480 = CARTESIAN_POINT ( 'NONE',  ( -2.499999999999996447, 26.16666666666666430, 4.330127018922195425 ) ) ;
#56481 = CARTESIAN_POINT ( 'NONE',  ( 5.000000000000000000, -76.37499999726880162, -6.123233995736766282E-16 ) ) ;
#56482 = CARTESIAN_POINT ( 'NONE',  ( 9.457646018065525792E-16, 0.9375000013655959696, 5.148502694627439702 ) ) ;
#56483 = DIRECTION ( 'NONE',  ( -0.000000000000000000, 0.000000000000000000, -1.000000000000000000 ) ) ;
#56484 = CARTESIAN_POINT ( 'NONE',  ( -5.000000000000000888, -164.5625000000000000, -2.071067811865475949 ) ) ;
#56485 = CYLINDRICAL_SURFACE ( 'NONE', #8821, 5.000000000000000000 ) ;
#56486 = CARTESIAN_POINT ( 'NONE',  ( -4.458734124999999437, 15.43750000136559386, 0.000000000000000000 ) ) ;
#56487 = CARTESIAN_POINT ( 'NONE',  ( 5.000000000000000888, 0.5416666693978527958, 2.886751345948126879 ) ) ;
#56488 = VERTEX_POINT ( 'NONE', #55082 ) ;
#56489 = CARTESIAN_POINT ( 'NONE',  ( 6.042630808230842148E-15, 26.75000000000000000, -4.999999999999999112 ) ) ;
#56490 = ORIENTED_EDGE ( 'NONE', *, *, #27184, .F. ) ;
#56491 = PRODUCT_DEFINITION_FORMATION_WITH_SPECIFIED_SOURCE ( 'ANY', '', #24548, .NOT_KNOWN. ) ;
#56492 = CARTESIAN_POINT ( 'NONE',  ( 5.000000000000000000, 27.62500000273118417, -6.123233995736766282E-16 ) ) ;
#56493 = CARTESIAN_POINT ( 'NONE',  ( -2.229367062499996610, -45.14583333196774362, 3.861377020970582219 ) ) ;
#56494 = CARTESIAN_POINT ( 'NONE',  ( -3.152801135295367096, -165.3125000013656063, -3.152801135295367541 ) ) ;
#56495 = CARTESIAN_POINT ( 'NONE',  ( -2.500000000000000444, -45.04166666393547303, -4.330127018922193649 ) ) ;
#56496 = ORIENTED_EDGE ( 'NONE', *, *, #11489, .F. ) ;
#56497 = CARTESIAN_POINT ( 'NONE',  ( 2.229367062500001939, -19.97916666530107221, 3.861377020970579999 ) ) ;
#56498 = ORIENTED_EDGE ( 'NONE', *, *, #57098, .T. ) ;
#56499 = CARTESIAN_POINT ( 'NONE',  ( -3.535250795749689387E-16, -89.25000000000000000, -5.773502691896257311 ) ) ;
#56500 = CARTESIAN_POINT ( 'NONE',  ( 3.152801135295367541, -163.3125000013656063, -3.152801135295367541 ) ) ;
#56501 = DIRECTION ( 'NONE',  ( -0.000000000000000000, 1.000000000000000000, -0.000000000000000000 ) ) ;
#56502 = CARTESIAN_POINT ( 'NONE',  ( -59.81910112700025905, -137.1875000000000000, -2.462841084822630311 ) ) ;
#56503 = EDGE_CURVE ( 'NONE', #39231, #27765, #22813, .T. ) ;
#56504 = CARTESIAN_POINT ( 'NONE',  ( 2.229367062499998831, -30.89583333196773651, -3.861377020970580887 ) ) ;
#56505 = CARTESIAN_POINT ( 'NONE',  ( -2.500000000000000444, 20.83333333333333215, -4.330127018922193649 ) ) ;
#56506 = ORIENTED_EDGE ( 'NONE', *, *, #58695, .T. ) ;
#56507 = CARTESIAN_POINT ( 'NONE',  ( -3.152548672688508926E-16, -76.56249999863440792, -5.148502694627439702 ) ) ;
#56508 = CARTESIAN_POINT ( 'NONE',  ( -4.458734124999999437, 26.68750000136559564, 0.000000000000000000 ) ) ;
#56509 = LINE ( 'NONE', #11783, #948 ) ;
#56510 = ORIENTED_EDGE ( 'NONE', *, *, #55822, .F. ) ;
#56511 = CYLINDRICAL_SURFACE ( 'NONE', #34596, 5.000000000000000000 ) ;
#56512 = CARTESIAN_POINT ( 'NONE',  ( -59.29741812935640155, -141.8750000013655779, -2.196230717870135685 ) ) ;
#56513 = CARTESIAN_POINT ( 'NONE',  ( 2.229367062499998831, -77.89583333196773651, -3.861377020970580887 ) ) ;
#56514 = CARTESIAN_POINT ( 'NONE',  ( -52.53715891517739323, -130.5625000027311842, -4.819101127000233298 ) ) ;
#56515 = CARTESIAN_POINT ( 'NONE',  ( 1.339745962155612702, -74.16965819600731891, -5.000000000000000000 ) ) ;
#56516 = CARTESIAN_POINT ( 'NONE',  ( -4.769696007084728073, -114.9999999999999858, 1.499999999999999556 ) ) ;
#56517 = CARTESIAN_POINT ( 'NONE',  ( 2.500000000000002220, 24.33333333333333215, 4.330127018922192761 ) ) ;
#56518 = CARTESIAN_POINT ( 'NONE',  ( 2.229367062500001939, -54.97916666530107221, 3.861377020970579999 ) ) ;
#56519 = CARTESIAN_POINT ( 'NONE',  ( 4.458734125000000326, -43.89583333196773651, 2.574251347313718519 ) ) ;
#56520 = CARTESIAN_POINT ( 'NONE',  ( -6.972266317189433020E-16, 20.74999999999999645, -5.000000000000000000 ) ) ;
#56521 =( BOUNDED_CURVE ( )  B_SPLINE_CURVE ( 2, ( #33759, #37972, #28614, #53063, #44029, #48230, #62734, #39523, #19275 ),
 .UNSPECIFIED., .F., .F. ) 
 B_SPLINE_CURVE_WITH_KNOTS ( ( 3, 2, 2, 2, 3 ),
 ( 0.5303571428571428603, 0.5309523809523809534, 0.5321428571428571397, 0.5333333333333333259, 0.5339285714285714191 ),
 .UNSPECIFIED. ) 
 CURVE ( )  GEOMETRIC_REPRESENTATION_ITEM ( )  RATIONAL_B_SPLINE_CURVE ( ( 0.9330127018922194093, 0.9330127018922194093, 1.000000000000000000, 0.8660254037844387076, 1.000000000000000000, 0.8660254037844387076, 1.000000000000000000, 0.9330127018922194093, 0.9330127018922194093 ) ) 
 REPRESENTATION_ITEM ( '' )  );
#56522 = CARTESIAN_POINT ( 'NONE',  ( -5.000000000000000000, -104.0833333333333428, -2.886751345948128211 ) ) ;
#56523 = CARTESIAN_POINT ( 'NONE',  ( 2.071067811865582087, -159.3125000027311842, 4.999999999999894307 ) ) ;
#56524 = CARTESIAN_POINT ( 'NONE',  ( 4.458734124999999437, -41.06249999863440081, -5.460374474430324690E-16 ) ) ;
#56525 = CARTESIAN_POINT ( 'NONE',  ( -4.999999999999999112, -0.7916666639354794643, 2.886751345948131764 ) ) ;
#56526 = CARTESIAN_POINT ( 'NONE',  ( -6.972266317189433020E-16, -95.12499999726880162, -5.000000000000000000 ) ) ;
#56527 = CARTESIAN_POINT ( 'NONE',  ( -50.40829686548195099, -126.0000000013656063, -1.485763867205728284 ) ) ;
#56528 = CARTESIAN_POINT ( 'NONE',  ( 2.229367062500001939, -77.22916666530106511, 3.861377020970579999 ) ) ;
#56529 = CARTESIAN_POINT ( 'NONE',  ( 2.500000000000002220, 24.33333333333333215, 4.330127018922192761 ) ) ;
#56530 = CARTESIAN_POINT ( 'NONE',  ( 2.229367062499998831, -101.6458333319677365, -3.861377020970580887 ) ) ;
#56531 = CARTESIAN_POINT ( 'NONE',  ( 9.457646018065525792E-16, -8.312499998634406140, 5.148502694627439702 ) ) ;
#56532 = VERTEX_POINT ( 'NONE', #10374 ) ;
#56533 = CARTESIAN_POINT ( 'NONE',  ( 5.000000000000000000, -47.41666666666666430, -2.886751345948130876 ) ) ;
#56534 = CARTESIAN_POINT ( 'NONE',  ( 4.458734124999999437, -92.81249999863440792, -5.460374474430324690E-16 ) ) ;
#56535 = CARTESIAN_POINT ( 'NONE',  ( 5.000000000000000888, -169.0625000027312126, -2.071067811865475505 ) ) ;
#56536 = CARTESIAN_POINT ( 'NONE',  ( -3.152548672688508926E-16, -86.81249999863439371, -5.148502694627439702 ) ) ;
#56537 = VECTOR ( 'NONE', #38331, 1000.000000000000114 ) ;
#56538 = CARTESIAN_POINT ( 'NONE',  ( -4.458734124999997661, 10.52083333469892779, 2.574251347313722516 ) ) ;
#56539 = CARTESIAN_POINT ( 'NONE',  ( 6.123233995736766282E-16, -120.0000000000000000, -5.000000000000000000 ) ) ;
#56540 = CARTESIAN_POINT ( 'NONE',  ( -58.39396692619412477, -135.4375000013656063, 2.891590998281057701 ) ) ;
#56541 =( BOUNDED_CURVE ( )  B_SPLINE_CURVE ( 2, ( #61225, #37713, #56716, #47055, #51260, #46732, #12634, #57034, #52519 ),
 .UNSPECIFIED., .F., .F. ) 
 B_SPLINE_CURVE_WITH_KNOTS ( ( 3, 2, 2, 2, 3 ),
 ( 0.6410714285714286254, 0.6416666666666667185, 0.6428571428571429047, 0.6440476190476190910, 0.6446428571428571841 ),
 .UNSPECIFIED. ) 
 CURVE ( )  GEOMETRIC_REPRESENTATION_ITEM ( )  RATIONAL_B_SPLINE_CURVE ( ( 0.9330127018922194093, 0.9330127018922256266, 1.000000000000000000, 0.8660254037844387076, 1.000000000000000000, 0.8660254037844387076, 1.000000000000000000, 0.9330127018922194093, 0.9330127018922194093 ) ) 
 REPRESENTATION_ITEM ( '' )  );
#56542 = CARTESIAN_POINT ( 'NONE',  ( 2.229367062500001939, -8.979166665301075767, 3.861377020970579999 ) ) ;
#56543 = CARTESIAN_POINT ( 'NONE',  ( 4.458734125000001214, 18.85416666803226349, 2.574251347313718519 ) ) ;
#56544 = CARTESIAN_POINT ( 'NONE',  ( -4.458734124999999437, -54.56249999863440081, 0.000000000000000000 ) ) ;
#56545 = CARTESIAN_POINT ( 'NONE',  ( -2.500000000000000444, 16.95833333606451987, -4.330127018922193649 ) ) ;
#56546 = CARTESIAN_POINT ( 'NONE',  ( 1.975475456537005874E-15, -21.62499999726880873, 5.000000000000000000 ) ) ;
#56547 = CARTESIAN_POINT ( 'NONE',  ( -3.152548672688508926E-16, -11.56249999863440792, -5.148502694627439702 ) ) ;
#56548 = ORIENTED_EDGE ( 'NONE', *, *, #16412, .F. ) ;
#56549 = CARTESIAN_POINT ( 'NONE',  ( 4.458734124999999437, -36.06249999863440792, -5.460374474430324690E-16 ) ) ;
#56550 = CARTESIAN_POINT ( 'NONE',  ( -59.29741812935640155, -127.8750000013656063, -2.196230717870135685 ) ) ;
#56551 = LINE ( 'NONE', #22770, #52446 ) ;
#56552 = CARTESIAN_POINT ( 'NONE',  ( 4.458734124999999437, -80.81249999863440792, -5.460374474430324690E-16 ) ) ;
#56553 = CARTESIAN_POINT ( 'NONE',  ( 4.458734124999999437, 23.93750000136559564, -5.460374474430324690E-16 ) ) ;
#56554 = CARTESIAN_POINT ( 'NONE',  ( 1.846868145590735200, -151.5000000013655779, -4.458734124999999437 ) ) ;
#56555 = CARTESIAN_POINT ( 'NONE',  ( -4.458734124999999437, 20.60416666803225993, -2.574251347313719407 ) ) ;
#56556 = DIRECTION ( 'NONE',  ( 0.000000000000000000, 0.000000000000000000, 1.000000000000000000 ) ) ;
#56557 = CARTESIAN_POINT ( 'NONE',  ( -4.458734124999999437, -82.64583333196773651, -2.574251347313719407 ) ) ;
#56558 = CARTESIAN_POINT ( 'NONE',  ( 1.060575238724906964E-15, -64.75000000000000000, 5.773502691896257311 ) ) ;
#56559 = DIRECTION ( 'NONE',  ( -0.000000000000000000, 1.000000000000000000, -0.000000000000000000 ) ) ;
#56560 = CARTESIAN_POINT ( 'NONE',  ( 2.499999999999998668, 17.79166666939785557, -4.330127018922193649 ) ) ;
#56561 = ORIENTED_EDGE ( 'NONE', *, *, #59400, .T. ) ;
#56562 = CARTESIAN_POINT ( 'NONE',  ( -2.499999999999996447, -61.70833333060214443, 4.330127018922195425 ) ) ;
#56563 = CARTESIAN_POINT ( 'NONE',  ( -57.46284108482265651, -139.0625000027312126, 4.819101127000238627 ) ) ;
#56565 = CARTESIAN_POINT ( 'NONE',  ( -2.500000000000000444, -25.16666666666666430, -4.330127018922193649 ) ) ;
#56564 = FACE_OUTER_BOUND ( 'NONE', #47629, .T. ) ;
#56566 = CARTESIAN_POINT ( 'NONE',  ( -2.229367062499996610, -30.14583333196773651, 3.861377020970582219 ) ) ;
#56567 = CARTESIAN_POINT ( 'NONE',  ( -4.458734124999999437, -87.31249999863439371, 0.000000000000000000 ) ) ;
#56568 = CARTESIAN_POINT ( 'NONE',  ( 5.000000000000000000, -26.29166666393547658, -2.886751345948129988 ) ) ;
#56570 = ORIENTED_EDGE ( 'NONE', *, *, #19321, .F. ) ;
#56569 = CARTESIAN_POINT ( 'NONE',  ( -2.229367062500000163, -60.47916666530106511, -3.861377020970580443 ) ) ;
#56571 = CARTESIAN_POINT ( 'NONE',  ( 1.339745962155615144, -28.70534180126147561, 4.999999999999999112 ) ) ;
#56573 = EDGE_LOOP ( 'NONE', ( #51018, #22709, #51527, #33445 ) ) ;
#56572 = CARTESIAN_POINT ( 'NONE',  ( 4.458734125000001214, -10.14583333196773829, 2.574251347313718519 ) ) ;
#56574 = CARTESIAN_POINT ( 'NONE',  ( 2.500000000000002220, -73.66666666666665719, 4.330127018922192761 ) ) ;
#56575 = CARTESIAN_POINT ( 'NONE',  ( -52.80376928212989185, -139.8750000013655779, -4.297418129356378458 ) ) ;
#56576 = AXIS2_PLACEMENT_3D ( 'NONE', #52570, #18469, #8503 ) ;
#56577 = CARTESIAN_POINT ( 'NONE',  ( -3.152548672688508926E-16, -51.81249999863440792, -5.148502694627439702 ) ) ;
#56578 = CARTESIAN_POINT ( 'NONE',  ( -4.999999999999999112, -76.79166666393547303, 2.886751345948131764 ) ) ;
#56580 = ORIENTED_EDGE ( 'NONE', *, *, #13807, .T. ) ;
#56579 = CARTESIAN_POINT ( 'NONE',  ( -6.972266317189433020E-16, -54.12499999726880162, -5.000000000000000000 ) ) ;
#56581 = CIRCLE ( 'NONE', #5225, 5.000000000000000000 ) ;
#56582 = CARTESIAN_POINT ( 'NONE',  ( -58.24261429053147765, -148.2500000000000284, -3.805975901505573855 ) ) ;
#56583 = EDGE_CURVE ( 'NONE', #52748, #59502, #27308, .T. ) ;
#56584 = CARTESIAN_POINT ( 'NONE',  ( -3.152548672688508926E-16, -14.81249999863440436, -5.148502694627439702 ) ) ;
#56585 = CARTESIAN_POINT ( 'NONE',  ( -2.229367062499996610, -57.39583333196773651, 3.861377020970582219 ) ) ;
#56586 = CARTESIAN_POINT ( 'NONE',  ( -4.999999999999998224, -29.79166666393548013, 2.886751345948131764 ) ) ;
#56587 =( NAMED_UNIT ( * ) SI_UNIT ( $, .STERADIAN. ) SOLID_ANGLE_UNIT ( ) );
#56588 = CARTESIAN_POINT ( 'NONE',  ( 4.458734124999999437, -169.6875000013656063, 0.000000000000000000 ) ) ;
#56589 = CARTESIAN_POINT ( 'NONE',  ( -4.458734124999999437, -97.64583333196772230, -2.574251347313719407 ) ) ;
#56590 = CARTESIAN_POINT ( 'NONE',  ( 5.000000000000000000, -148.1250000027312126, 0.000000000000000000 ) ) ;
#56591 = VERTEX_POINT ( 'NONE', #34823 ) ;
#56592 = CARTESIAN_POINT ( 'NONE',  ( -53.51423613279429503, -153.5000000013656063, 4.591703134518083651 ) ) ;
#56593 = CARTESIAN_POINT ( 'NONE',  ( -53.33387254593733928, -142.9375000027312410, 5.149110718188519620 ) ) ;
#56594 =( BOUNDED_CURVE ( )  B_SPLINE_CURVE ( 2, ( #56489, #41350, #26894, #16916, #22389, #18180, #2150, #61311, #46512 ),
 .UNSPECIFIED., .F., .F. ) 
 B_SPLINE_CURVE_WITH_KNOTS ( ( 3, 2, 2, 2, 3 ),
 ( 0.02708333333333333426, 0.02777777777777777624, 0.02916666666666666713, 0.03055555555555555455, 0.03125000000000000000 ),
 .UNSPECIFIED. ) 
 CURVE ( )  GEOMETRIC_REPRESENTATION_ITEM ( )  RATIONAL_B_SPLINE_CURVE ( ( 0.9330127018922194093, 0.9330127018922195203, 1.000000000000000000, 0.8660254037844387076, 1.000000000000000000, 0.8660254037844387076, 1.000000000000000000, 0.9330127018922191873, 0.9330127018922194093 ) ) 
 REPRESENTATION_ITEM ( '' )  );
#56595 = ADVANCED_FACE ( 'NONE', ( #29664 ), #40282, .T. ) ;
#56596 = CARTESIAN_POINT ( 'NONE',  ( -75.00000000000000000, 15.00000000000000000, 8.999999999999998224 ) ) ;
#56597 = CARTESIAN_POINT ( 'NONE',  ( -4.458734124999999437, -8.312499998634406140, 0.000000000000000000 ) ) ;
#56598 = CARTESIAN_POINT ( 'NONE',  ( 4.458734124999998549, -97.97916666530105090, -2.574251347313721627 ) ) ;
#56599 = CARTESIAN_POINT ( 'NONE',  ( -1.846868145590734756, -147.3750000013656063, -4.458734125000000326 ) ) ;
#56600 = CARTESIAN_POINT ( 'NONE',  ( -2.229367062499996610, -24.39583333196773651, 3.861377020970582219 ) ) ;
#56601 = EDGE_CURVE ( 'NONE', #38122, #38750, #26937, .T. ) ;
#56602 = CARTESIAN_POINT ( 'NONE',  ( 1.339745962155615144, -46.70534180126147561, 4.999999999999999112 ) ) ;
#56603 = CARTESIAN_POINT ( 'NONE',  ( -51.60603307380591787, -137.9375000013656063, -2.891590998281053704 ) ) ;
#56604 = CARTESIAN_POINT ( 'NONE',  ( -2.229367062500000163, -61.72916666530106511, -3.861377020970580443 ) ) ;
#56605 = CARTESIAN_POINT ( 'NONE',  ( -6.972266317189433020E-16, -50.12499999726881583, -5.000000000000000000 ) ) ;
#56606 = CARTESIAN_POINT ( 'NONE',  ( -0.04606493828583551470, -9.175055303659563677, -8.057411785091794343 ) ) ;
#56607 = CARTESIAN_POINT ( 'NONE',  ( -1.846868145590734756, -143.1250000013656063, -4.458734124999999437 ) ) ;
#56608 = CARTESIAN_POINT ( 'NONE',  ( -2.229367062500000163, 10.27083333469892779, -3.861377020970580443 ) ) ;
#56609 = ORIENTED_EDGE ( 'NONE', *, *, #41756, .F. ) ;
#56610 = CARTESIAN_POINT ( 'NONE',  ( -4.999999999999998224, -52.79166666393548013, 2.886751345948131764 ) ) ;
#56611 = CARTESIAN_POINT ( 'NONE',  ( 1.339745962155615144, -61.70534180126146850, 4.999999999999999112 ) ) ;
#56613 = CARTESIAN_POINT ( 'NONE',  ( -4.458734124999999437, -23.39583333196773296, -2.574251347313719407 ) ) ;
#56612 = CARTESIAN_POINT ( 'NONE',  ( 1.060575238724906964E-15, -91.75000000000000000, 5.773502691896257311 ) ) ;
#56614 = DIRECTION ( 'NONE',  ( 0.000000000000000000, 0.000000000000000000, 1.000000000000000000 ) ) ;
#56615 = CARTESIAN_POINT ( 'NONE',  ( -4.458734124999998549, -68.47916666530106511, 2.574251347313722516 ) ) ;
#56616 = CARTESIAN_POINT ( 'NONE',  ( 6.123233995736766282E-16, -120.0000000000000000, -5.000000000000000000 ) ) ;
#56617 = CARTESIAN_POINT ( 'NONE',  ( -6.972266317189433020E-16, -76.12499999726880162, -5.000000000000000000 ) ) ;
#56618 = CARTESIAN_POINT ( 'NONE',  ( -55.35523342533222291, -145.3125000013656063, 4.444560631937231499 ) ) ;
#56619 = CARTESIAN_POINT ( 'NONE',  ( -4.999999999999999112, -51.79166666393548013, 2.886751345948131764 ) ) ;
#56620 = CARTESIAN_POINT ( 'NONE',  ( 5.000000000000000000, -24.50000000000000000, -6.123233995736766282E-16 ) ) ;
#56621 = CARTESIAN_POINT ( 'NONE',  ( 4.458734125000000326, 8.104166668032261711, 2.574251347313718519 ) ) ;
#56622 = CARTESIAN_POINT ( 'NONE',  ( -6.972266317189433020E-16, -89.24999999999998579, -5.000000000000000000 ) ) ;
#56623 = CARTESIAN_POINT ( 'NONE',  ( 0.000000000000000000, -120.0000000000000000, 0.000000000000000000 ) ) ;
#56624 = CARTESIAN_POINT ( 'NONE',  ( 4.458734124999999437, 5.187500001365596525, -5.460374474430324690E-16 ) ) ;
#56625 = CARTESIAN_POINT ( 'NONE',  ( 4.458734125000001214, -73.89583333196773651, 2.574251347313718519 ) ) ;
#56626 = CARTESIAN_POINT ( 'NONE',  ( 4.458734125000000326, -20.14583333196774007, 2.574251347313718519 ) ) ;
#56627 =( BOUNDED_CURVE ( )  B_SPLINE_CURVE ( 2, ( #62499, #18417, #12642, #51266, #57670, #3012, #32257, #51887, #7828 ),
 .UNSPECIFIED., .F., .F. ) 
 B_SPLINE_CURVE_WITH_KNOTS ( ( 3, 2, 2, 2, 3 ),
 ( 0.4946428571428571619, 0.4952380952380952550, 0.4964285714285714413, 0.4976190476190476275, 0.4982142857142857206 ),
 .UNSPECIFIED. ) 
 CURVE ( )  GEOMETRIC_REPRESENTATION_ITEM ( )  RATIONAL_B_SPLINE_CURVE ( ( 0.9330127018922194093, 0.9330127018922194093, 1.000000000000000000, 0.8660254037844387076, 1.000000000000000000, 0.8660254037844387076, 1.000000000000000000, 0.9330127018922194093, 0.9330127018922194093 ) ) 
 REPRESENTATION_ITEM ( '' )  );
#56628 = CARTESIAN_POINT ( 'NONE',  ( 5.000000000000000888, -1.583333333333332593, 2.886751345948126879 ) ) ;
#56629 = CARTESIAN_POINT ( 'NONE',  ( -3.152801135295367096, -159.0625000013656063, -3.152801135295367541 ) ) ;
#56630 = CARTESIAN_POINT ( 'NONE',  ( -5.000000000000000888, -158.5625000000000284, -2.071067811865475949 ) ) ;
#56631 = CARTESIAN_POINT ( 'NONE',  ( -2.229367062499996610, -66.14583333196773651, 3.861377020970582219 ) ) ;
#56632 = CARTESIAN_POINT ( 'NONE',  ( 5.000000000000000000, -99.29166666393545881, -2.886751345948129988 ) ) ;
#56633 = CARTESIAN_POINT ( 'NONE',  ( 0.000000000000000000, -120.0000000000000000, 5.000000000000000000 ) ) ;
#56634 = CARTESIAN_POINT ( 'NONE',  ( 2.229367062500001939, -38.97916666530107221, 3.861377020970579999 ) ) ;
#56635 = EDGE_CURVE ( 'NONE', #19199, #15810, #28972, .T. ) ;
#56636 = CARTESIAN_POINT ( 'NONE',  ( 6.123233995736766282E-16, -170.0000000000000000, -5.000000000000000000 ) ) ;
#56637 = CARTESIAN_POINT ( 'NONE',  ( -2.229367062499996610, -65.39583333196773651, 3.861377020970582219 ) ) ;
#56638 = CARTESIAN_POINT ( 'NONE',  ( -3.535250795749689387E-16, -47.25000000000000000, -5.773502691896257311 ) ) ;
#56639 = CARTESIAN_POINT ( 'NONE',  ( -2.499999999999996447, 27.16666666666666430, 4.330127018922195425 ) ) ;
#56640 = PLANE ( 'NONE',  #47923 ) ;
#56641 = ORIENTED_EDGE ( 'NONE', *, *, #56664, .F. ) ;
#56642 = CARTESIAN_POINT ( 'NONE',  ( 1.339745962155612702, -94.29465819873851729, -5.000000000000000000 ) ) ;
#56643 = CARTESIAN_POINT ( 'NONE',  ( -6.972266317189433020E-16, 11.74999999999999645, -5.000000000000000000 ) ) ;
#56644 = CARTESIAN_POINT ( 'NONE',  ( -2.500000000000000444, -8.166666666666669627, -4.330127018922193649 ) ) ;
#56645 = CARTESIAN_POINT ( 'NONE',  ( -2.229367062500000163, -71.47916666530107932, -3.861377020970580443 ) ) ;
#56646 = CARTESIAN_POINT ( 'NONE',  ( -58.59997141384986463, -154.8437500006828031, 3.067102644406258793 ) ) ;
#56647 = CARTESIAN_POINT ( 'NONE',  ( 5.000000000000000000, -10.37499999726881583, -6.123233995736766282E-16 ) ) ;
#56649 = ORIENTED_EDGE ( 'NONE', *, *, #59560, .T. ) ;
#56648 = CARTESIAN_POINT ( 'NONE',  ( -3.152548672688508926E-16, -41.56249999863439371, -5.148502694627439702 ) ) ;
#56650 = CARTESIAN_POINT ( 'NONE',  ( -6.972266317189433020E-16, 14.74999999999999822, -5.000000000000000000 ) ) ;
#56652 = VERTEX_POINT ( 'NONE', #51532 ) ;
#56651 = CARTESIAN_POINT ( 'NONE',  ( 4.458734124999998549, 9.020833334698927786, -2.574251347313721627 ) ) ;
#56653 = CARTESIAN_POINT ( 'NONE',  ( -5.000000000000000000, -57.99999999999999289, 0.000000000000000000 ) ) ;
#56654 = CARTESIAN_POINT ( 'NONE',  ( 1.846868145590735200, -161.5000000013656063, -4.458734125000000326 ) ) ;
#56655 = CARTESIAN_POINT ( 'NONE',  ( -2.229367062499996610, -35.39583333196772941, 3.861377020970582219 ) ) ;
#56656 = CARTESIAN_POINT ( 'NONE',  ( -4.999999999999998224, -34.91666666666666430, 2.886751345948131764 ) ) ;
#56657 = CARTESIAN_POINT ( 'NONE',  ( -2.229367062499996610, -82.14583333196773651, 3.861377020970582219 ) ) ;
#56658 = CARTESIAN_POINT ( 'NONE',  ( 3.061616997868383141E-16, -164.7500000000000000, -5.000000000000000000 ) ) ;
#56659 = CARTESIAN_POINT ( 'NONE',  ( -4.458734124999999437, -89.31249999863440792, 0.000000000000000000 ) ) ;
#56660 = CARTESIAN_POINT ( 'NONE',  ( -59.29741812935640155, -130.8750000013656063, -2.196230717870135685 ) ) ;
#56661 = CARTESIAN_POINT ( 'NONE',  ( 4.458734124999999437, 0.9375000013655959696, -5.460374474430324690E-16 ) ) ;
#56662 = CARTESIAN_POINT ( 'NONE',  ( -4.458734124999999437, -36.56249999863440792, 0.000000000000000000 ) ) ;
#56663 = ADVANCED_FACE ( 'NONE', ( #51218 ), #26127, .T. ) ;
#56664 = EDGE_CURVE ( 'NONE', #28553, #10085, #7469, .T. ) ;
#56665 = CARTESIAN_POINT ( 'NONE',  ( -5.000000000000000000, 24.04166666939785202, -2.886751345948128211 ) ) ;
#56666 = CARTESIAN_POINT ( 'NONE',  ( -3.152548672688508926E-16, -82.81249999863442213, -5.148502694627439702 ) ) ;
#56667 = CARTESIAN_POINT ( 'NONE',  ( 2.500000000000002220, -86.66666666666667140, 4.330127018922192761 ) ) ;
#56668 = ORIENTED_EDGE ( 'NONE', *, *, #53820, .T. ) ;
#56669 = CARTESIAN_POINT ( 'NONE',  ( -57.46284108482265651, -154.0625000027312126, 4.819101127000239515 ) ) ;
#56670 = CARTESIAN_POINT ( 'NONE',  ( 2.071067811865645591, -152.1875000000000000, 4.999999999999830358 ) ) ;
#56671 = CARTESIAN_POINT ( 'NONE',  ( 4.458734124999999437, -72.06249999863439371, -5.460374474430324690E-16 ) ) ;
#56672 = CARTESIAN_POINT ( 'NONE',  ( -4.458734124999997661, -36.22916666530106511, 2.574251347313722516 ) ) ;
#56673 = CARTESIAN_POINT ( 'NONE',  ( -2.229367062499996610, -7.395833331967735624, 3.861377020970582219 ) ) ;
#56674 = VERTEX_POINT ( 'NONE', #41220 ) ;
#56675 = EDGE_CURVE ( 'NONE', #22477, #20545, #56365, .T. ) ;
#56676 = CARTESIAN_POINT ( 'NONE',  ( -5.000000000000000888, -150.6875000027312126, -2.071067811865475949 ) ) ;
#56677 = CARTESIAN_POINT ( 'NONE',  ( 5.000000000000000888, -3.458333330602147093, 2.886751345948126879 ) ) ;
#56678 = CARTESIAN_POINT ( 'NONE',  ( -4.458734124999999437, -6.645833331967741842, -2.574251347313719407 ) ) ;
#56679 = EDGE_CURVE ( 'NONE', #43575, #1059, #42142, .T. ) ;
#56680 = PLANE ( 'NONE',  #62051 ) ;
#56681 = CARTESIAN_POINT ( 'NONE',  ( -2.229367062500000163, 2.520833334698928230, -3.861377020970580443 ) ) ;
#56682 = DIRECTION ( 'NONE',  ( -0.000000000000000000, 1.000000000000000000, -0.000000000000000000 ) ) ;
#56683 = CARTESIAN_POINT ( 'NONE',  ( 3.152801135295367541, -157.3125000013656063, -3.152801135295367541 ) ) ;
#56684 = CARTESIAN_POINT ( 'NONE',  ( -4.458734124999999437, 28.35416666803225993, -2.574251347313719407 ) ) ;
#56685 = VERTEX_POINT ( 'NONE', #61507 ) ;
#56686 = CARTESIAN_POINT ( 'NONE',  ( -4.458734124999999437, -87.39583333196773651, -2.574251347313719407 ) ) ;
#56687 = CARTESIAN_POINT ( 'NONE',  ( 3.061616997868383141E-16, -167.8750000027312126, -5.000000000000000000 ) ) ;
#56688 = CARTESIAN_POINT ( 'NONE',  ( -4.458734124999999437, -9.395833331967736513, -2.574251347313719407 ) ) ;
#56689 = CARTESIAN_POINT ( 'NONE',  ( 0.000000000000000000, -120.0000000000000000, 5.000000000000000000 ) ) ;
#56690 = DIRECTION ( 'NONE',  ( -0.000000000000000000, 1.000000000000000000, -0.000000000000000000 ) ) ;
#56691 = CARTESIAN_POINT ( 'NONE',  ( 2.500000000000002220, -67.66666666666667140, 4.330127018922192761 ) ) ;
#56692 = CARTESIAN_POINT ( 'NONE',  ( -2.500000000000000444, -36.04166666393547303, -4.330127018922193649 ) ) ;
#56693 = LINE ( 'NONE', #60878, #55042 ) ;
#56694 = CARTESIAN_POINT ( 'NONE',  ( -4.458734124999997661, 26.77083333469892779, 2.574251347313722516 ) ) ;
#56695 = CARTESIAN_POINT ( 'NONE',  ( -4.999999999999998224, -20.79166666393548013, 2.886751345948131764 ) ) ;
#56696 = CARTESIAN_POINT ( 'NONE',  ( 2.229367062499998831, 21.35416666803226349, -3.861377020970580887 ) ) ;
#56697 = CARTESIAN_POINT ( 'NONE',  ( -4.458734124999998549, -58.22916666530105800, 2.574251347313722516 ) ) ;
#56698 = CARTESIAN_POINT ( 'NONE',  ( 9.457646018065525792E-16, -3.312499998634407916, 5.148502694627439702 ) ) ;
#56699 = DIRECTION ( 'NONE',  ( 1.000000000000000000, 0.000000000000000000, 0.000000000000000000 ) ) ;
#56700 = CARTESIAN_POINT ( 'NONE',  ( -2.500000000000000444, 15.83333333333333037, -4.330127018922193649 ) ) ;
#56701 = CARTESIAN_POINT ( 'NONE',  ( 5.000000000000000888, -141.0625000027312410, -2.071067811865475505 ) ) ;
#56702 = CARTESIAN_POINT ( 'NONE',  ( 2.229367062500001939, -48.97916666530107221, 3.861377020970579999 ) ) ;
#56703 = CARTESIAN_POINT ( 'NONE',  ( 5.000000000000000000, -81.37499999726881583, -6.123233995736766282E-16 ) ) ;
#56704 = CARTESIAN_POINT ( 'NONE',  ( -54.64476657466781973, -141.0625000013656063, -4.444560631937228834 ) ) ;
#56705 = CARTESIAN_POINT ( 'NONE',  ( 0.000000000000000000, -170.0000000000000000, 5.000000000000000000 ) ) ;
#56706 = CARTESIAN_POINT ( 'NONE',  ( 2.229367062500001939, -88.22916666530107932, 3.861377020970579999 ) ) ;
#56707 = CARTESIAN_POINT ( 'NONE',  ( 3.152801135295366208, -158.8125000013656063, 3.152801135295367985 ) ) ;
#56708 = CARTESIAN_POINT ( 'NONE',  ( 5.000000000000000000, -33.50000000000000000, -6.123233995736766282E-16 ) ) ;
#56709 = CARTESIAN_POINT ( 'NONE',  ( 0.000000000000000000, -170.0000000000000000, 0.000000000000000000 ) ) ;
#56710 = EDGE_LOOP ( 'NONE', ( #8376, #15440, #3458, #55388 ) ) ;
#56711 = CARTESIAN_POINT ( 'NONE',  ( -3.152548672688508926E-16, 15.18750000136559386, -5.148502694627439702 ) ) ;
#56712 = ORIENTED_EDGE ( 'NONE', *, *, #3219, .F. ) ;
#56713 = CARTESIAN_POINT ( 'NONE',  ( 4.458734125000001214, -95.89583333196773651, 2.574251347313718519 ) ) ;
#56714 = CARTESIAN_POINT ( 'NONE',  ( -2.229367062500000163, 15.27083333469892779, -3.861377020970580443 ) ) ;
#56715 = CARTESIAN_POINT ( 'NONE',  ( -4.999999999999999112, 15.20833333606451987, 2.886751345948131764 ) ) ;
#56716 = CARTESIAN_POINT ( 'NONE',  ( -2.499999999999996447, -59.83333333333333570, 4.330127018922195425 ) ) ;
#56717 = CARTESIAN_POINT ( 'NONE',  ( 5.000000000000000888, 8.416666666666666075, 2.886751345948126879 ) ) ;
#56718 = CARTESIAN_POINT ( 'NONE',  ( -4.458734124999997661, -56.22916666530107221, 2.574251347313722516 ) ) ;
#56719 =( BOUNDED_CURVE ( )  B_SPLINE_CURVE ( 2, ( #9672, #1570, #24476, #9993, #29606, #46, #32718, #32078, #37542 ),
 .UNSPECIFIED., .F., .F. ) 
 B_SPLINE_CURVE_WITH_KNOTS ( ( 3, 2, 2, 2, 3 ),
 ( 0.9875000000000000444, 0.9880952380952381375, 0.9892857142857143238, 0.9904761904761905100, 0.9910714285714286031 ),
 .UNSPECIFIED. ) 
 CURVE ( )  GEOMETRIC_REPRESENTATION_ITEM ( )  RATIONAL_B_SPLINE_CURVE ( ( 0.9330127018922194093, 0.9330127018922194093, 1.000000000000000000, 0.8660254037844387076, 1.000000000000000000, 0.8660254037844387076, 1.000000000000000000, 0.9330127018922194093, 0.9330127018922194093 ) ) 
 REPRESENTATION_ITEM ( '' )  );
#56720 = DIRECTION ( 'NONE',  ( -0.000000000000000000, 1.000000000000000000, -0.000000000000000000 ) ) ;
#56721 = CARTESIAN_POINT ( 'NONE',  ( 1.060575238724906964E-15, -81.75000000000000000, 5.773502691896257311 ) ) ;
#56722 = CARTESIAN_POINT ( 'NONE',  ( -59.44456063193725015, -135.8125000013656063, -0.3552334253322034230 ) ) ;
#56723 = FACE_OUTER_BOUND ( 'NONE', #11717, .T. ) ;
#56724 = CARTESIAN_POINT ( 'NONE',  ( -1.339745962155613812, -26.08034179853029499, -5.000000000000000000 ) ) ;
#56725 = CARTESIAN_POINT ( 'NONE',  ( 5.000000000000000000, -109.4999999999999858, -6.123233995736766282E-16 ) ) ;
#56726 = CARTESIAN_POINT ( 'NONE',  ( 5.000000000000000888, -40.58333333333333570, 2.886751345948126879 ) ) ;
#56727 = DIRECTION ( 'NONE',  ( -0.000000000000000000, 1.000000000000000000, -0.000000000000000000 ) ) ;
#56729 = CARTESIAN_POINT ( 'NONE',  ( 2.229367062499998831, -17.89583333196773651, -3.861377020970580887 ) ) ;
#56728 = CARTESIAN_POINT ( 'NONE',  ( -6.972266317189433020E-16, 14.74999999999999822, -5.000000000000000000 ) ) ;
#56730 = CARTESIAN_POINT ( 'NONE',  ( 0.000000000000000000, -170.0000000000000000, 0.000000000000000000 ) ) ;
#56731 = CARTESIAN_POINT ( 'NONE',  ( 4.458734124999998549, -65.72916666530106511, -2.574251347313721627 ) ) ;
#56732 = CARTESIAN_POINT ( 'NONE',  ( -1.846868145590734756, -149.3750000013656347, -4.458734125000000326 ) ) ;
#56733 = CARTESIAN_POINT ( 'NONE',  ( -4.458734124999999437, -73.31249999863439371, 0.000000000000000000 ) ) ;
#56734 = CARTESIAN_POINT ( 'NONE',  ( -56.48576386720575471, -143.0000000013655779, -4.591703134518078322 ) ) ;
#56735 = CARTESIAN_POINT ( 'NONE',  ( 9.457646018065525792E-16, -20.31249999863440081, 5.148502694627439702 ) ) ;
#56736 = CARTESIAN_POINT ( 'NONE',  ( -4.999999999999999112, -62.79166666393546592, 2.886751345948131764 ) ) ;
#56738 = ORIENTED_EDGE ( 'NONE', *, *, #41773, .T. ) ;
#56737 = EDGE_CURVE ( 'NONE', #60194, #61583, #18288, .T. ) ;
#56739 = CARTESIAN_POINT ( 'NONE',  ( 1.975475456537005874E-15, -46.74999999999999289, 5.000000000000000000 ) ) ;
#56740 = EDGE_LOOP ( 'NONE', ( #60472, #61713, #44931, #57718 ) ) ;
#56741 = CARTESIAN_POINT ( 'NONE',  ( 2.229367062499998831, -66.89583333196773651, -3.861377020970580887 ) ) ;
#56742 = CARTESIAN_POINT ( 'NONE',  ( 5.000000000000000888, -21.45833333060214798, 2.886751345948126879 ) ) ;
#56743 = CARTESIAN_POINT ( 'NONE',  ( 7.922281120364393914, 4.573931137438269623, -8.047472243342930653 ) ) ;
#56744 = EDGE_LOOP ( 'NONE', ( #16233, #19169, #13026, #30846 ) ) ;
#56745 = CARTESIAN_POINT ( 'NONE',  ( -51.75738570946856498, -151.7500000000000284, 3.805975901505576964 ) ) ;
#56746 = CARTESIAN_POINT ( 'NONE',  ( -51.75738570946856498, -125.7500000000000284, 3.805975901505576964 ) ) ;
#56747 = CARTESIAN_POINT ( 'NONE',  ( -1.339745962155613812, -75.08034179853029855, -5.000000000000000000 ) ) ;
#56748 = CARTESIAN_POINT ( 'NONE',  ( -4.458734124999998549, -51.47916666530106511, 2.574251347313722516 ) ) ;
#56749 = ORIENTED_EDGE ( 'NONE', *, *, #48630, .T. ) ;
#56750 = CARTESIAN_POINT ( 'NONE',  ( -5.000000000000000000, -90.43749999863440792, 0.000000000000000000 ) ) ;
#56751 = CARTESIAN_POINT ( 'NONE',  ( 9.457646018065525792E-16, 5.937500001365592972, 5.148502694627439702 ) ) ;
#56752 = EDGE_CURVE ( 'NONE', #14934, #49037, #27078, .T. ) ;
#56753 = CARTESIAN_POINT ( 'NONE',  ( -4.458734124999999437, 19.60416666803225993, -2.574251347313719407 ) ) ;
#56754 = CARTESIAN_POINT ( 'NONE',  ( -52.80376928212989185, -150.8750000013656063, -4.297418129356379346 ) ) ;
#56755 = CARTESIAN_POINT ( 'NONE',  ( 0.000000000000000000, 0.000000000000000000, 0.000000000000000000 ) ) ;
#56756 = CARTESIAN_POINT ( 'NONE',  ( -3.152801135295367985, -168.8125000013656063, 3.152801135295367096 ) ) ;
#56758 = EDGE_CURVE ( 'NONE', #36444, #43336, #31815, .T. ) ;
#56757 = ORIENTED_EDGE ( 'NONE', *, *, #5906, .F. ) ;
#56759 = CARTESIAN_POINT ( 'NONE',  ( 9.457646018065525792E-16, -72.06249999863439371, 5.148502694627439702 ) ) ;
#56760 = CARTESIAN_POINT ( 'NONE',  ( 5.000000000000000000, -10.37499999726881583, -6.123233995736766282E-16 ) ) ;
#56761 = CARTESIAN_POINT ( 'NONE',  ( 4.458734125000001214, 8.104166668032261711, 2.574251347313718519 ) ) ;
#56762 = EDGE_CURVE ( 'NONE', #38362, #24136, #42885, .T. ) ;
#56763 = CARTESIAN_POINT ( 'NONE',  ( 2.071067811865517694, -139.9375000027311557, -4.999999999999958256 ) ) ;
#56764 = CARTESIAN_POINT ( 'NONE',  ( 4.458734125000001214, -61.14583333196773651, 2.574251347313718519 ) ) ;
#56765 = CARTESIAN_POINT ( 'NONE',  ( 2.499999999999998668, -14.20833333060214976, -4.330127018922193649 ) ) ;
#56766 = CARTESIAN_POINT ( 'NONE',  ( -58.24261429053147765, -142.3750000027312126, -3.805975901505573855 ) ) ;
#56767 = CARTESIAN_POINT ( 'NONE',  ( -3.750000000000004885, 6.495190528383289141, 0.000000000000000000 ) ) ;
#56768 = CARTESIAN_POINT ( 'NONE',  ( 2.500000000000002220, -30.54166666393548013, 4.330127018922192761 ) ) ;
#56769 =( BOUNDED_CURVE ( )  B_SPLINE_CURVE ( 2, ( #47623, #31571, #22883, #41523, #12895, #36722, #3579, #22571, #41207 ),
 .UNSPECIFIED., .F., .F. ) 
 B_SPLINE_CURVE_WITH_KNOTS ( ( 3, 2, 2, 2, 3 ),
 ( 0.9520833333333332815, 0.9527777777777777235, 0.9541666666666667185, 0.9555555555555556024, 0.9562500000000000444 ),
 .UNSPECIFIED. ) 
 CURVE ( )  GEOMETRIC_REPRESENTATION_ITEM ( )  RATIONAL_B_SPLINE_CURVE ( ( 0.9330127018922194093, 0.9330127018922194093, 1.000000000000000000, 0.8660254037844387076, 1.000000000000000000, 0.8660254037844387076, 1.000000000000000000, 0.9330127018922194093, 0.9330127018922194093 ) ) 
 REPRESENTATION_ITEM ( '' )  );
#56770 = CARTESIAN_POINT ( 'NONE',  ( -4.999999999999998224, -83.79166666393545881, 2.886751345948131764 ) ) ;
#56771 = CARTESIAN_POINT ( 'NONE',  ( 2.229367062499998831, -35.64583333196772941, -3.861377020970580887 ) ) ;
#56772 = CARTESIAN_POINT ( 'NONE',  ( -4.458734124999999437, -21.64583333196774007, -2.574251347313719407 ) ) ;
#56773 =( BOUNDED_CURVE ( )  B_SPLINE_CURVE ( 2, ( #3413, #7920, #47154, #32991, #32356, #3101, #23958, #4039, #28781 ),
 .UNSPECIFIED., .F., .F. ) 
 B_SPLINE_CURVE_WITH_KNOTS ( ( 3, 2, 2, 2, 3 ),
 ( 0.2982142857142857095, 0.2988095238095238027, 0.2999999999999999889, 0.3011904761904761751, 0.3017857142857142683 ),
 .UNSPECIFIED. ) 
 CURVE ( )  GEOMETRIC_REPRESENTATION_ITEM ( )  RATIONAL_B_SPLINE_CURVE ( ( 0.9330127018922194093, 0.9330127018922194093, 1.000000000000000000, 0.8660254037844387076, 1.000000000000000000, 0.8660254037844387076, 1.000000000000000000, 0.9330127018922194093, 0.9330127018922194093 ) ) 
 REPRESENTATION_ITEM ( '' )  );
#56774 = ORIENTED_EDGE ( 'NONE', *, *, #7951, .F. ) ;
#56775 = CARTESIAN_POINT ( 'NONE',  ( -5.000000000000000000, -4.958333330602148870, -2.886751345948128211 ) ) ;
#56776 = CARTESIAN_POINT ( 'NONE',  ( -3.535250795749689387E-16, 28.74999999999999645, -5.773502691896257311 ) ) ;
#56777 = CARTESIAN_POINT ( 'NONE',  ( 5.000000000000000000, -153.1875000027312410, 2.071067811865478614 ) ) ;
#56778 = ORIENTED_EDGE ( 'NONE', *, *, #2870, .T. ) ;
#56779 = CARTESIAN_POINT ( 'NONE',  ( -2.229367062499996610, -105.3958333319677365, 3.861377020970582219 ) ) ;
#56780 = CARTESIAN_POINT ( 'NONE',  ( 4.458734124999998549, -33.72916666530106511, -2.574251347313721627 ) ) ;
#56781 = CARTESIAN_POINT ( 'NONE',  ( 2.500000000000002220, -63.54166666393547303, 4.330127018922192761 ) ) ;
#56782 = CARTESIAN_POINT ( 'NONE',  ( -53.51423613279429503, -151.5000000013655779, 4.591703134518082763 ) ) ;
#56783 = CARTESIAN_POINT ( 'NONE',  ( -3.535533905932737309, -145.6250000000000000, -3.535533905932738197 ) ) ;
#56784 = CARTESIAN_POINT ( 'NONE',  ( 2.229367062499998831, -29.64583333196773296, -3.861377020970580887 ) ) ;
#56785 = CARTESIAN_POINT ( 'NONE',  ( -4.458734124999999437, -68.64583333196773651, -2.574251347313719407 ) ) ;
#56786 = DIRECTION ( 'NONE',  ( -0.000000000000000000, 1.000000000000000000, -0.000000000000000000 ) ) ;
#56787 = CARTESIAN_POINT ( 'NONE',  ( 2.229367062499998831, -25.64583333196773651, -3.861377020970580887 ) ) ;
#56788 = DIRECTION ( 'NONE',  ( -0.000000000000000000, 1.000000000000000000, -0.000000000000000000 ) ) ;
#56789 = CARTESIAN_POINT ( 'NONE',  ( 1.975475456537005874E-15, 18.37500000273118062, 5.000000000000000000 ) ) ;
#56790 = CARTESIAN_POINT ( 'NONE',  ( -5.000000000000000000, -18.08333333333333570, -2.886751345948128211 ) ) ;
#56791 = CARTESIAN_POINT ( 'NONE',  ( -1.846868145590734756, -149.1250000013656063, -4.458734125000000326 ) ) ;
#56792 = EDGE_LOOP ( 'NONE', ( #48232, #60680, #680, #23990 ) ) ;
#56793 = CARTESIAN_POINT ( 'NONE',  ( -9.184850993605147944E-16, -150.2500000000000284, 5.000000000000000000 ) ) ;
#56794 = CARTESIAN_POINT ( 'NONE',  ( -3.152548672688508926E-16, -50.81249999863440792, -5.148502694627439702 ) ) ;
#56795 = CARTESIAN_POINT ( 'NONE',  ( 5.000000000000000888, -58.45833333060214443, 2.886751345948126879 ) ) ;
#56796 = DIRECTION ( 'NONE',  ( 0.000000000000000000, 0.000000000000000000, 1.000000000000000000 ) ) ;
#56797 = CARTESIAN_POINT ( 'NONE',  ( -5.000000000000000000, 24.91666666666666430, -2.886751345948128211 ) ) ;
#56798 = CARTESIAN_POINT ( 'NONE',  ( 2.499999999999998668, 25.66666666666666430, -4.330127018922193649 ) ) ;
#56799 = CARTESIAN_POINT ( 'NONE',  ( 2.229367062499998831, -1.645833331967737401, -3.861377020970580887 ) ) ;
#56800 = CARTESIAN_POINT ( 'NONE',  ( -2.499999999999996447, -51.70833333060213732, 4.330127018922195425 ) ) ;
#56801 = CARTESIAN_POINT ( 'NONE',  ( 3.535533905932736864, -141.1250000000000000, 3.535533905932738641 ) ) ;
#56802 = CARTESIAN_POINT ( 'NONE',  ( 5.000000000000000000, -7.500000000000000000, -6.123233995736766282E-16 ) ) ;
#56803 = CARTESIAN_POINT ( 'NONE',  ( -2.229367062500000163, 12.27083333469892601, -3.861377020970580443 ) ) ;
#56804 =( BOUNDED_CURVE ( )  B_SPLINE_CURVE ( 2, ( #5275, #24253, #18786, #29063, #460, #9147, #24896, #19427, #38717 ),
 .UNSPECIFIED., .F., .F. ) 
 B_SPLINE_CURVE_WITH_KNOTS ( ( 3, 2, 2, 2, 3 ),
 ( 0.5517857142857143238, 0.5523809523809524169, 0.5535714285714286031, 0.5547619047619047894, 0.5553571428571428825 ),
 .UNSPECIFIED. ) 
 CURVE ( )  GEOMETRIC_REPRESENTATION_ITEM ( )  RATIONAL_B_SPLINE_CURVE ( ( 0.9330127018922194093, 0.9330127018922194093, 1.000000000000000000, 0.8660254037844387076, 1.000000000000000000, 0.8660254037844387076, 1.000000000000000000, 0.9330127018922194093, 0.9330127018922194093 ) ) 
 REPRESENTATION_ITEM ( '' )  );
#56805 = ORIENTED_EDGE ( 'NONE', *, *, #35657, .F. ) ;
#56806 = FACE_OUTER_BOUND ( 'NONE', #4051, .T. ) ;
#56807 = ORIENTED_EDGE ( 'NONE', *, *, #44054, .T. ) ;
#56808 = CARTESIAN_POINT ( 'NONE',  ( 5.000000000000000000, -168.1875000027311842, 2.071067811865478614 ) ) ;
#56809 = CARTESIAN_POINT ( 'NONE',  ( 4.458734124999998549, -47.72916666530106511, -2.574251347313721627 ) ) ;
#56810 = CARTESIAN_POINT ( 'NONE',  ( 2.730187237215162345E-16, -163.4375000013655779, -4.458734124999999437 ) ) ;
#56811 = CARTESIAN_POINT ( 'NONE',  ( -3.535250795749689387E-16, -44.12499999726880873, -5.773502691896257311 ) ) ;
#56812 = ORIENTED_EDGE ( 'NONE', *, *, #54784, .F. ) ;
#56813 = CARTESIAN_POINT ( 'NONE',  ( 2.229367062500001939, -21.97916666530107221, 3.861377020970579999 ) ) ;
#56814 = ORIENTED_EDGE ( 'NONE', *, *, #14087, .T. ) ;
#56815 = FACE_OUTER_BOUND ( 'NONE', #8235, .T. ) ;
#56816 = CARTESIAN_POINT ( 'NONE',  ( -4.458734125000000326, -164.0000000013656063, -1.846868145590735644 ) ) ;
#56817 =( BOUNDED_CURVE ( )  B_SPLINE_CURVE ( 2, ( #62284, #17888, #57148, #57461, #46846, #27849, #42327, #7621, #52314 ),
 .UNSPECIFIED., .F., .F. ) 
 B_SPLINE_CURVE_WITH_KNOTS ( ( 3, 2, 2, 2, 3 ),
 ( 0.1089285714285714302, 0.1095238095238095233, 0.1107142857142857095, 0.1119047619047619097, 0.1125000000000000028 ),
 .UNSPECIFIED. ) 
 CURVE ( )  GEOMETRIC_REPRESENTATION_ITEM ( )  RATIONAL_B_SPLINE_CURVE ( ( 0.9330127018922194093, 0.9330127018922194093, 1.000000000000000000, 0.8660254037844387076, 1.000000000000000000, 0.8660254037844387076, 1.000000000000000000, 0.9330127018922194093, 0.9330127018922194093 ) ) 
 REPRESENTATION_ITEM ( '' )  );
#56818 = CARTESIAN_POINT ( 'NONE',  ( 0.000000000000000000, 0.000000000000000000, 0.000000000000000000 ) ) ;
#56819 = CARTESIAN_POINT ( 'NONE',  ( -49.85088928181150436, -139.5625000000000284, -1.666127454062680702 ) ) ;
#56820 = CARTESIAN_POINT ( 'NONE',  ( -4.458734124999998549, -39.47916666530107932, 2.574251347313722516 ) ) ;
#56821 = FACE_OUTER_BOUND ( 'NONE', #58620, .T. ) ;
#56822 = ORIENTED_EDGE ( 'NONE', *, *, #5436, .F. ) ;
#56823 = CARTESIAN_POINT ( 'NONE',  ( -2.229367062500000163, -80.47916666530106511, -3.861377020970580443 ) ) ;
#56824 = VECTOR ( 'NONE', #50359, 1000.000000000000000 ) ;
#56825 = CARTESIAN_POINT ( 'NONE',  ( -4.458734124999999437, 24.60416666803225993, -2.574251347313719407 ) ) ;
#56826 = CARTESIAN_POINT ( 'NONE',  ( 1.339745962155609149, 24.41965820146970856, 5.000000000000003553 ) ) ;
#56827 = ORIENTED_EDGE ( 'NONE', *, *, #2863, .F. ) ;
#56828 = CARTESIAN_POINT ( 'NONE',  ( -1.339745962155613812, -23.08034179853029144, -5.000000000000000000 ) ) ;
#56829 = CARTESIAN_POINT ( 'NONE',  ( -59.29741812935640155, -139.8750000013655779, -2.196230717870135685 ) ) ;
#56830 = CARTESIAN_POINT ( 'NONE',  ( -2.229367062499996610, -78.39583333196773651, 3.861377020970582219 ) ) ;
#56831 = CARTESIAN_POINT ( 'NONE',  ( -50.01589407740564042, -129.7500000027312126, 0.3983568153799778022 ) ) ;
#56832 = CARTESIAN_POINT ( 'NONE',  ( 1.975475456537005874E-15, -85.75000000000000000, 5.000000000000000000 ) ) ;
#56833 = FACE_OUTER_BOUND ( 'NONE', #13126, .T. ) ;
#56834 = DIRECTION ( 'NONE',  ( -0.000000000000000000, 1.000000000000000000, -0.000000000000000000 ) ) ;
#56835 = CARTESIAN_POINT ( 'NONE',  ( -4.458734124999999437, -52.31249999863440792, 0.000000000000000000 ) ) ;
#56836 = CARTESIAN_POINT ( 'NONE',  ( -59.98410592259440222, -151.2500000027312410, -0.3983568153799752487 ) ) ;
#56837 = CARTESIAN_POINT ( 'NONE',  ( -5.000000000000000000, 20.91666666666666785, -2.886751345948128211 ) ) ;
#56838 = CARTESIAN_POINT ( 'NONE',  ( -5.000000000000000000, -106.0833333333333286, -2.886751345948128211 ) ) ;
#56839 = CARTESIAN_POINT ( 'NONE',  ( 2.071067811865370256, -158.9375000027311842, -5.000000000000105693 ) ) ;
#56840 = CARTESIAN_POINT ( 'NONE',  ( -3.152548672688508926E-16, -43.81249999863440081, -5.148502694627439702 ) ) ;
#56841 = CARTESIAN_POINT ( 'NONE',  ( -3.535250795749689387E-16, -1.124999997268814056, -5.773502691896257311 ) ) ;
#56842 = CARTESIAN_POINT ( 'NONE',  ( -4.999999999999998224, -72.91666666666667140, 2.886751345948131764 ) ) ;
#56843 = DIRECTION ( 'NONE',  ( -0.000000000000000000, 1.000000000000000000, -0.000000000000000000 ) ) ;
#56844 = CARTESIAN_POINT ( 'NONE',  ( 4.458734125000001214, -81.14583333196773651, 2.574251347313718519 ) ) ;
#56845 = CARTESIAN_POINT ( 'NONE',  ( 4.458734124999999437, -101.8124999986344079, -5.460374474430324690E-16 ) ) ;
#56846 = CARTESIAN_POINT ( 'NONE',  ( -4.458734124999997661, -6.479166665301072214, 2.574251347313722516 ) ) ;
#56847 = ORIENTED_EDGE ( 'NONE', *, *, #52575, .F. ) ;
#56848 = CARTESIAN_POINT ( 'NONE',  ( -5.000000000000000000, -35.95833333060213732, -2.886751345948128211 ) ) ;
#56849 = CARTESIAN_POINT ( 'NONE',  ( -4.458734124999999437, -91.39583333196773651, -2.574251347313719407 ) ) ;
#56850 = CARTESIAN_POINT ( 'NONE',  ( -5.000000000000000000, -164.6250000027311842, -6.123233995736766282E-16 ) ) ;
#56851 = CARTESIAN_POINT ( 'NONE',  ( 4.458734124999998549, -84.97916666530106511, -2.574251347313721627 ) ) ;
#56852 = CARTESIAN_POINT ( 'NONE',  ( -2.229367062499996610, 12.60416666803226171, 3.861377020970582219 ) ) ;
#56853 = DIRECTION ( 'NONE',  ( -0.000000000000000000, 1.000000000000000000, -0.000000000000000000 ) ) ;
#56854 = CARTESIAN_POINT ( 'NONE',  ( -52.10840900171896806, -134.1875000013656063, 3.393966926194110556 ) ) ;
#56855 = CARTESIAN_POINT ( 'NONE',  ( 4.458734124999999437, -13.81249999863440259, -5.460374474430324690E-16 ) ) ;
#56856 = CARTESIAN_POINT ( 'NONE',  ( -4.458734124999999437, 16.43750000136559564, 0.000000000000000000 ) ) ;
#56857 = CARTESIAN_POINT ( 'NONE',  ( -4.458734124999999437, -51.64583333196773651, -2.574251347313719407 ) ) ;
#56858 = CARTESIAN_POINT ( 'NONE',  ( -5.000000000000000888, -163.4375000000000000, 2.071067811865474617 ) ) ;
#56859 = CARTESIAN_POINT ( 'NONE',  ( -2.500000000000000444, -106.1666666666666572, -4.330127018922193649 ) ) ;
#56860 = CARTESIAN_POINT ( 'NONE',  ( 2.229367062500001939, -8.979166665301075767, 3.861377020970579999 ) ) ;
#56861 = CARTESIAN_POINT ( 'NONE',  ( -1.339745962155610925, -38.79465819873851729, 5.000000000000000000 ) ) ;
#56862 = ORIENTED_EDGE ( 'NONE', *, *, #48453, .T. ) ;
#56863 = CARTESIAN_POINT ( 'NONE',  ( 2.229367062500001939, -35.22916666530107221, 3.861377020970579999 ) ) ;
#56864 = CARTESIAN_POINT ( 'NONE',  ( -59.29741812935640155, -128.8750000013656063, -2.196230717870135685 ) ) ;
#56865 = CARTESIAN_POINT ( 'NONE',  ( 5.000000000000000000, -76.50000000000000000, -6.123233995736766282E-16 ) ) ;
#56866 = CARTESIAN_POINT ( 'NONE',  ( -4.458734124999999437, -79.39583333196773651, -2.574251347313719407 ) ) ;
#56867 = CARTESIAN_POINT ( 'NONE',  ( -3.152548672688508926E-16, 22.18750000136559564, -5.148502694627439702 ) ) ;
#56868 = CARTESIAN_POINT ( 'NONE',  ( -8.190561711645485556E-16, -149.9375000013656063, 4.458734124999999437 ) ) ;
#56869 = VECTOR ( 'NONE', #2957, 1000.000000000000000 ) ;
#56870 = CARTESIAN_POINT ( 'NONE',  ( -3.152548672688508926E-16, 17.43750000136559564, -5.148502694627439702 ) ) ;
#56871 = LINE ( 'NONE', #41419, #56448 ) ;
#56872 = CARTESIAN_POINT ( 'NONE',  ( -9.184850993605147944E-16, -161.2500000000000000, 5.000000000000000000 ) ) ;
#56873 = CARTESIAN_POINT ( 'NONE',  ( -2.229367062499996610, -83.39583333196773651, 3.861377020970582219 ) ) ;
#56874 = CARTESIAN_POINT ( 'NONE',  ( 2.499999999999998668, -65.33333333333332860, -4.330127018922193649 ) ) ;
#56875 = CARTESIAN_POINT ( 'NONE',  ( -2.500000000000000444, 29.83333333333333215, -4.330127018922193649 ) ) ;
#56876 = CARTESIAN_POINT ( 'NONE',  ( -2.500000000000000444, 20.95833333606451987, -4.330127018922193649 ) ) ;
#56877 = ORIENTED_EDGE ( 'NONE', *, *, #24758, .F. ) ;
#56878 = CARTESIAN_POINT ( 'NONE',  ( 1.339745962155612702, -79.29465819873851729, -5.000000000000000000 ) ) ;
#56879 = CARTESIAN_POINT ( 'NONE',  ( -58.80597590150559739, -139.1250000027312410, 3.242614290531460330 ) ) ;
#56881 = CARTESIAN_POINT ( 'NONE',  ( 1.060575238724906964E-15, -30.75000000000000000, 5.773502691896257311 ) ) ;
#56880 = CARTESIAN_POINT ( 'NONE',  ( 1.339745962155612702, -52.29465819873851729, -5.000000000000000000 ) ) ;
#56882 = CARTESIAN_POINT ( 'NONE',  ( 4.458734124999998549, -34.72916666530107221, -2.574251347313721627 ) ) ;
#56883 = CARTESIAN_POINT ( 'NONE',  ( 2.500000000000002220, -62.66666666666666430, 4.330127018922192761 ) ) ;
#56884 = CARTESIAN_POINT ( 'NONE',  ( -5.000000000000000000, -26.95833333060214798, -2.886751345948128211 ) ) ;
#56886 = ORIENTED_EDGE ( 'NONE', *, *, #17311, .T. ) ;
#56885 = CARTESIAN_POINT ( 'NONE',  ( 9.457646018065525792E-16, -58.06249999863440081, 5.148502694627439702 ) ) ;
#56887 = CARTESIAN_POINT ( 'NONE',  ( 5.000000000000000000, -62.37499999726880873, -6.123233995736766282E-16 ) ) ;
#56889 = ORIENTED_EDGE ( 'NONE', *, *, #29529, .T. ) ;
#56888 = CARTESIAN_POINT ( 'NONE',  ( -2.229367062500000163, -8.729166665301073991, -3.861377020970580443 ) ) ;
#56890 = CARTESIAN_POINT ( 'NONE',  ( 5.000000000000000888, -72.58333333333334281, 2.886751345948126879 ) ) ;
#56891 = CARTESIAN_POINT ( 'NONE',  ( -50.55543936806279248, -137.0625000013656063, 0.3552334253322060320 ) ) ;
#56892 = CARTESIAN_POINT ( 'NONE',  ( 4.458734124999998549, -50.97916666530107221, -2.574251347313721627 ) ) ;
#56893 = CARTESIAN_POINT ( 'NONE',  ( 2.499999999999998668, -79.20833333060213022, -4.330127018922193649 ) ) ;
#56895 = VERTEX_POINT ( 'NONE', #55405 ) ;
#56894 = CARTESIAN_POINT ( 'NONE',  ( -5.000000000000000000, -54.95833333060214443, -2.886751345948128211 ) ) ;
#56896 = CARTESIAN_POINT ( 'NONE',  ( -58.24261429053147765, -149.2500000000000284, -3.805975901505573855 ) ) ;
#56897 = CARTESIAN_POINT ( 'NONE',  ( 2.229367062500001939, -14.22916666530107221, 3.861377020970579999 ) ) ;
#56898 = CARTESIAN_POINT ( 'NONE',  ( -2.229367062500000163, -58.72916666530106511, -3.861377020970580443 ) ) ;
#56899 =( BOUNDED_CURVE ( )  B_SPLINE_CURVE ( 2, ( #9461, #24581, #48694, #4635, #24259, #43862, #63509, #30991, #45150 ),
 .UNSPECIFIED., .F., .F. ) 
 B_SPLINE_CURVE_WITH_KNOTS ( ( 3, 2, 2, 2, 3 ),
 ( 0.8446428571428571397, 0.8452380952380952328, 0.8464285714285714191, 0.8476190476190476053, 0.8482142857142856984 ),
 .UNSPECIFIED. ) 
 CURVE ( )  GEOMETRIC_REPRESENTATION_ITEM ( )  RATIONAL_B_SPLINE_CURVE ( ( 0.9330127018922194093, 0.9330127018922194093, 1.000000000000000000, 0.8660254037844387076, 1.000000000000000000, 0.8660254037844387076, 1.000000000000000000, 0.9330127018922194093, 0.9330127018922194093 ) ) 
 REPRESENTATION_ITEM ( '' )  );
#56900 = CARTESIAN_POINT ( 'NONE',  ( -1.339745962155613812, -24.20534180126147206, -5.000000000000000000 ) ) ;
#56901 =( NAMED_UNIT ( * ) SI_UNIT ( $, .STERADIAN. ) SOLID_ANGLE_UNIT ( ) );
#56902 = CARTESIAN_POINT ( 'NONE',  ( -4.458734125000000326, -141.0000000013656063, -1.846868145590735644 ) ) ;
#56903 = CARTESIAN_POINT ( 'NONE',  ( -4.458734124999999437, -100.5624999986344079, 0.000000000000000000 ) ) ;
#56904 = CARTESIAN_POINT ( 'NONE',  ( -9.184850993605147944E-16, -158.2500000000000000, 5.000000000000000000 ) ) ;
#56905 = VERTEX_POINT ( 'NONE', #21628 ) ;
#56906 = CARTESIAN_POINT ( 'NONE',  ( -57.89159099828107458, -152.9375000013656063, -3.393966926194107447 ) ) ;
#56907 = CARTESIAN_POINT ( 'NONE',  ( -50.18089887299979068, -142.8125000027311842, 2.462841084822635640 ) ) ;
#56908 = CARTESIAN_POINT ( 'NONE',  ( 1.339745962155615144, 18.29465819873851729, 4.999999999999999112 ) ) ;
#56909 = CARTESIAN_POINT ( 'NONE',  ( -4.458734124999999437, -9.312499998634406140, 0.000000000000000000 ) ) ;
#56910 = CARTESIAN_POINT ( 'NONE',  ( 2.229367062499998831, -94.89583333196773651, -3.861377020970580887 ) ) ;
#56911 =( BOUNDED_CURVE ( )  B_SPLINE_CURVE ( 2, ( #958, #15085, #34699, #10261, #25372, #20558, #40161, #54962, #10892 ),
 .UNSPECIFIED., .F., .F. ) 
 B_SPLINE_CURVE_WITH_KNOTS ( ( 3, 2, 2, 2, 3 ),
 ( 0.9196428571428570953, 0.9202380952380951884, 0.9214285714285713746, 0.9226190476190476719, 0.9232142857142857650 ),
 .UNSPECIFIED. ) 
 CURVE ( )  GEOMETRIC_REPRESENTATION_ITEM ( )  RATIONAL_B_SPLINE_CURVE ( ( 0.9330127018922194093, 0.9330127018922194093, 1.000000000000000000, 0.8660254037844387076, 1.000000000000000000, 0.8660254037844387076, 1.000000000000000000, 0.9330127018922194093, 0.9330127018922194093 ) ) 
 REPRESENTATION_ITEM ( '' )  );
#56912 = CARTESIAN_POINT ( 'NONE',  ( 1.846868145590735200, -146.5000000013656347, -4.458734125000000326 ) ) ;
#56913 = CARTESIAN_POINT ( 'NONE',  ( -4.458734124999999437, -22.56249999863440436, 0.000000000000000000 ) ) ;
#56914 = DIRECTION ( 'NONE',  ( -0.000000000000000000, 1.000000000000000000, -0.000000000000000000 ) ) ;
#56915 = CARTESIAN_POINT ( 'NONE',  ( -50.40829686548195099, -136.0000000013656063, -1.485763867205728284 ) ) ;
#56916 = CARTESIAN_POINT ( 'NONE',  ( 9.457646018065525792E-16, -64.31249999863440792, 5.148502694627439702 ) ) ;
#56917 = CARTESIAN_POINT ( 'NONE',  ( -55.00000000000002132, -155.0000000000000284, 1.734723475976807094E-15 ) ) ;
#56918 = CARTESIAN_POINT ( 'NONE',  ( 0.000000000000000000, -120.0000000000000000, 0.000000000000000000 ) ) ;
#56919 = CARTESIAN_POINT ( 'NONE',  ( 3.152801135295366208, -144.5625000013655779, 3.152801135295367985 ) ) ;
#56920 = CARTESIAN_POINT ( 'NONE',  ( 4.458734124999999437, 8.937500001365592084, -5.460374474430324690E-16 ) ) ;
#56921 = ORIENTED_EDGE ( 'NONE', *, *, #30283, .F. ) ;
#56922 = CARTESIAN_POINT ( 'NONE',  ( -5.000000000000000888, -164.6875000027311842, -2.071067811865475949 ) ) ;
#56923 = CARTESIAN_POINT ( 'NONE',  ( 1.339745962155615144, -66.58034179853028434, 4.999999999999999112 ) ) ;
#56925 = CARTESIAN_POINT ( 'NONE',  ( 4.458734124999998549, -22.72916666530107221, -2.574251347313721627 ) ) ;
#56924 = CARTESIAN_POINT ( 'NONE',  ( -5.000000000000000000, -89.08333333333334281, -2.886751345948128211 ) ) ;
#56926 = CARTESIAN_POINT ( 'NONE',  ( -5.000000000000000000, -76.87499999726880162, 0.000000000000000000 ) ) ;
#56927 = CARTESIAN_POINT ( 'NONE',  ( -3.152548672688508926E-16, -70.81249999863440792, -5.148502694627439702 ) ) ;
#56928 = CARTESIAN_POINT ( 'NONE',  ( -4.458734124999997661, 27.52083333469892779, 2.574251347313722516 ) ) ;
#56929 = CARTESIAN_POINT ( 'NONE',  ( -4.999999999999998224, -17.79166666393547658, 2.886751345948131764 ) ) ;
#56930 = CARTESIAN_POINT ( 'NONE',  ( -57.19623071787017210, -145.3750000013656347, 4.297418129356382899 ) ) ;
#56931 = CARTESIAN_POINT ( 'NONE',  ( 2.229367062499998831, 3.354166668032259935, -3.861377020970580887 ) ) ;
#56932 = DIRECTION ( 'NONE',  ( -0.000000000000000000, 1.000000000000000000, -0.000000000000000000 ) ) ;
#56933 = CARTESIAN_POINT ( 'NONE',  ( -1.049326080737009628E-13, -2.750000000000003109, 5.000000000000000000 ) ) ;
#56934 = CARTESIAN_POINT ( 'NONE',  ( 4.458734124999999437, 8.187500001365595637, -5.460374474430324690E-16 ) ) ;
#56935 = CARTESIAN_POINT ( 'NONE',  ( 2.229367062499998831, -73.64583333196773651, -3.861377020970580887 ) ) ;
#56936 = CARTESIAN_POINT ( 'NONE',  ( 2.229367062500001939, -17.22916666530106866, 3.861377020970579999 ) ) ;
#56937 = CARTESIAN_POINT ( 'NONE',  ( -2.499999999999996447, -2.833333333333333481, 4.330127018922195425 ) ) ;
#56938 = CARTESIAN_POINT ( 'NONE',  ( -4.458734125000000326, -158.0000000013655779, -1.846868145590735644 ) ) ;
#56939 = CARTESIAN_POINT ( 'NONE',  ( -5.000000000000000000, 29.04166666939785557, -2.886751345948128211 ) ) ;
#56940 = CARTESIAN_POINT ( 'NONE',  ( -4.458734124999999437, -62.39583333196774362, -2.574251347313719407 ) ) ;
#56941 = CARTESIAN_POINT ( 'NONE',  ( 1.060575238724906964E-15, -98.62499999726883004, 5.773502691896257311 ) ) ;
#56942 = EDGE_CURVE ( 'NONE', #48295, #42800, #33868, .T. ) ;
#56943 = CARTESIAN_POINT ( 'NONE',  ( 2.499999999999998668, 15.66666666666666607, -4.330127018922193649 ) ) ;
#56944 = CARTESIAN_POINT ( 'NONE',  ( -2.229367062500000163, -38.47916666530107221, -3.861377020970580443 ) ) ;
#56945 = CARTESIAN_POINT ( 'NONE',  ( 4.458734125000000326, -105.1458333319677365, 2.574251347313718519 ) ) ;
#56946 = CARTESIAN_POINT ( 'NONE',  ( -3.152548672688508926E-16, -66.81249999863440792, -5.148502694627439702 ) ) ;
#56947 = CARTESIAN_POINT ( 'NONE',  ( 5.000000000000000000, -50.41666666666666430, -2.886751345948129988 ) ) ;
#56948 = CARTESIAN_POINT ( 'NONE',  ( -2.500000000000000444, -41.16666666666667140, -4.330127018922193649 ) ) ;
#56949 = CARTESIAN_POINT ( 'NONE',  ( 2.499999999999998668, -36.20833333060213732, -4.330127018922193649 ) ) ;
#56950 = ORIENTED_EDGE ( 'NONE', *, *, #18815, .T. ) ;
#56951 = CARTESIAN_POINT ( 'NONE',  ( 2.500000000000002220, -94.66666666666665719, 4.330127018922192761 ) ) ;
#56952 = CARTESIAN_POINT ( 'NONE',  ( -1.339745962155610925, -99.66965819600733312, 5.000000000000000000 ) ) ;
#56953 = CARTESIAN_POINT ( 'NONE',  ( -3.535250795749689387E-16, -7.249999999999999112, -5.773502691896257311 ) ) ;
#56954 = CARTESIAN_POINT ( 'NONE',  ( -4.458734124999998549, -13.22916666530107221, 2.574251347313722516 ) ) ;
#56955 = CARTESIAN_POINT ( 'NONE',  ( -2.229367062499996610, -76.14583333196773651, 3.861377020970582219 ) ) ;
#56956 = VECTOR ( 'NONE', #32178, 1000.000000000000000 ) ;
#56957 = ADVANCED_FACE ( 'NONE', ( #28018 ), #53098, .T. ) ;
#56958 = CARTESIAN_POINT ( 'NONE',  ( -2.500000000000000444, -13.04166666393548013, -4.330127018922193649 ) ) ;
#56960 = ORIENTED_EDGE ( 'NONE', *, *, #7496, .F. ) ;
#56959 = CARTESIAN_POINT ( 'NONE',  ( 2.229367062500001939, -44.97916666530106511, 3.861377020970579999 ) ) ;
#56961 = CARTESIAN_POINT ( 'NONE',  ( 5.000000000000000888, -100.4583333306021444, 2.886751345948126879 ) ) ;
#56962 = EDGE_CURVE ( 'NONE', #12680, #7140, #33499, .T. ) ;
#56964 = VERTEX_POINT ( 'NONE', #33476 ) ;
#56963 = CARTESIAN_POINT ( 'NONE',  ( -4.458734124999998549, 4.520833334698926009, 2.574251347313722516 ) ) ;
#56965 = FACE_OUTER_BOUND ( 'NONE', #45412, .T. ) ;
#56966 = CARTESIAN_POINT ( 'NONE',  ( -3.535250795749689387E-16, -53.24999999999999289, -5.773502691896257311 ) ) ;
#56967 = CARTESIAN_POINT ( 'NONE',  ( 4.458734125000000326, -158.6250000013655779, -1.846868145590734978 ) ) ;
#56968 = CARTESIAN_POINT ( 'NONE',  ( -4.458734124999999437, -37.64583333196773651, -2.574251347313719407 ) ) ;
#56969 = DIRECTION ( 'NONE',  ( -0.000000000000000000, 1.000000000000000000, -0.000000000000000000 ) ) ;
#56970 = CARTESIAN_POINT ( 'NONE',  ( 4.458734124999999437, -79.81249999863440792, -5.460374474430324690E-16 ) ) ;
#56971 =( BOUNDED_CURVE ( )  B_SPLINE_CURVE ( 2, ( #41016, #1488, #60976, #32005, #31689, #36203, #11740, #50357, #61290 ),
 .UNSPECIFIED., .F., .F. ) 
 B_SPLINE_CURVE_WITH_KNOTS ( ( 3, 2, 2, 2, 3 ),
 ( 0.008333333333333340157, 0.01250000000000001110, 0.01666666666666668031, 0.02083333333333334952, 0.02500000000000002220 ),
 .UNSPECIFIED. ) 
 CURVE ( )  GEOMETRIC_REPRESENTATION_ITEM ( )  RATIONAL_B_SPLINE_CURVE ( ( 0.9999999999999998890, 0.9238795325112868495, 1.000000000000000000, 0.9238795325112867385, 1.000000000000000000, 0.9238795325112867385, 1.000000000000000000, 0.9238795325112864054, 1.000000000000000444 ) ) 
 REPRESENTATION_ITEM ( '' )  );
#56972 = CARTESIAN_POINT ( 'NONE',  ( -2.071067811865475061, -166.6875000000000568, -5.000000000000000888 ) ) ;
#56973 = CARTESIAN_POINT ( 'NONE',  ( 4.458734125000001214, -84.89583333196773651, 2.574251347313718519 ) ) ;
#56974 = CARTESIAN_POINT ( 'NONE',  ( -57.89159099828107458, -129.9375000013656063, -3.393966926194107447 ) ) ;
#56975 = CARTESIAN_POINT ( 'NONE',  ( 9.457646018065525792E-16, -2.312499998634407028, 5.148502694627439702 ) ) ;
#56976 = EDGE_CURVE ( 'NONE', #26112, #52286, #55688, .T. ) ;
#56977 = CARTESIAN_POINT ( 'NONE',  ( -2.229367062499996610, -42.39583333196773651, 3.861377020970582219 ) ) ;
#56978 = CARTESIAN_POINT ( 'NONE',  ( -2.229367062500000163, -83.72916666530106511, -3.861377020970580443 ) ) ;
#56979 = CARTESIAN_POINT ( 'NONE',  ( 1.975475456537005874E-15, 16.37500000273118417, 5.000000000000000000 ) ) ;
#56980 = ORIENTED_EDGE ( 'NONE', *, *, #22183, .F. ) ;
#56981 = CARTESIAN_POINT ( 'NONE',  ( -1.339745962155610925, -94.66965819600731891, 5.000000000000000000 ) ) ;
#56982 = CARTESIAN_POINT ( 'NONE',  ( 0.000000000000000000, -170.0000000000000000, 5.000000000000000000 ) ) ;
#56983 = CARTESIAN_POINT ( 'NONE',  ( 4.458734124999999437, -71.06249999863439371, -5.460374474430324690E-16 ) ) ;
#56984 = CARTESIAN_POINT ( 'NONE',  ( -3.152548672688508926E-16, -39.56249999863440081, -5.148502694627439702 ) ) ;
#56985 = CARTESIAN_POINT ( 'NONE',  ( 2.229367062500001939, -8.229166665301073991, 3.861377020970579999 ) ) ;
#56986 = ORIENTED_EDGE ( 'NONE', *, *, #53403, .T. ) ;
#56987 = CARTESIAN_POINT ( 'NONE',  ( 0.000000000000000000, -170.0000000000000000, 0.000000000000000000 ) ) ;
#56988 = CARTESIAN_POINT ( 'NONE',  ( -2.500000000000000444, -2.166666666666663854, -4.330127018922193649 ) ) ;
#56989 = EDGE_CURVE ( 'NONE', #21118, #34811, #9633, .T. ) ;
#56990 = CARTESIAN_POINT ( 'NONE',  ( 4.458734124999999437, -6.062499998634403475, -5.460374474430324690E-16 ) ) ;
#56991 = CYLINDRICAL_SURFACE ( 'NONE', #27105, 5.000000000000000000 ) ;
#56992 = CARTESIAN_POINT ( 'NONE',  ( -4.458734124999999437, 0.6875000013655957476, 0.000000000000000000 ) ) ;
#56993 = CARTESIAN_POINT ( 'NONE',  ( 1.975475456537005874E-15, -30.62499999726881583, 5.000000000000000000 ) ) ;
#56994 = CARTESIAN_POINT ( 'NONE',  ( 2.730187237215162345E-16, -156.1875000013655779, -4.458734124999999437 ) ) ;
#56995 =( BOUNDED_CURVE ( )  B_SPLINE_CURVE ( 2, ( #56437, #26518, #46134, #61257, #15911, #36807, #16236, #60307, #11079 ),
 .UNSPECIFIED., .F., .F. ) 
 B_SPLINE_CURVE_WITH_KNOTS ( ( 3, 2, 2, 2, 3 ),
 ( 0.9910714285714286031, 0.9916666666666666963, 0.9928571428571428825, 0.9940476190476190688, 0.9946428571428571619 ),
 .UNSPECIFIED. ) 
 CURVE ( )  GEOMETRIC_REPRESENTATION_ITEM ( )  RATIONAL_B_SPLINE_CURVE ( ( 0.9330127018922194093, 0.9330127018922194093, 1.000000000000000000, 0.8660254037844387076, 1.000000000000000000, 0.8660254037844387076, 1.000000000000000000, 0.9330127018922194093, 0.9330127018922194093 ) ) 
 REPRESENTATION_ITEM ( '' )  );
#56996 = CARTESIAN_POINT ( 'NONE',  ( 4.458734124999999437, 25.93750000136559564, -5.460374474430324690E-16 ) ) ;
#56997 = ORIENTED_EDGE ( 'NONE', *, *, #23885, .F. ) ;
#56998 = CARTESIAN_POINT ( 'NONE',  ( 4.458734125000000326, -88.89583333196773651, 2.574251347313718519 ) ) ;
#56999 = CYLINDRICAL_SURFACE ( 'NONE', #58269, 5.000000000000000000 ) ;
#57000 = CARTESIAN_POINT ( 'NONE',  ( -4.458734124999999437, -11.31249999863440792, 0.000000000000000000 ) ) ;
#57001 = CYLINDRICAL_SURFACE ( 'NONE', #32378, 5.000000000000000000 ) ;
#57002 = FACE_OUTER_BOUND ( 'NONE', #61264, .T. ) ;
#57003 = AXIS2_PLACEMENT_3D ( 'NONE', #54016, #30198, #34080 ) ;
#57004 = CARTESIAN_POINT ( 'NONE',  ( 1.339745962155612702, -67.29465819873851729, -5.000000000000000000 ) ) ;
#57005 = CARTESIAN_POINT ( 'NONE',  ( 5.000000000000000000, -37.37499999726881583, -6.123233995736766282E-16 ) ) ;
#57006 = CARTESIAN_POINT ( 'NONE',  ( 1.975475456537005874E-15, -29.62499999726881228, 5.000000000000000000 ) ) ;
#57007 = CARTESIAN_POINT ( 'NONE',  ( 4.458734124999998549, 26.27083333469892423, -2.574251347313721627 ) ) ;
#57008 = CARTESIAN_POINT ( 'NONE',  ( -5.000000000000000000, -95.00000000000000000, 0.000000000000000000 ) ) ;
#57009 = CARTESIAN_POINT ( 'NONE',  ( 4.458734124999999437, 23.18750000136559564, -5.460374474430324690E-16 ) ) ;
#57010 = CARTESIAN_POINT ( 'NONE',  ( -4.458734124999998549, -56.22916666530107221, 2.574251347313722516 ) ) ;
#57011 = CARTESIAN_POINT ( 'NONE',  ( 4.458734124999999437, -3.062499998634407472, -5.460374474430324690E-16 ) ) ;
#57012 = CYLINDRICAL_SURFACE ( 'NONE', #9301, 5.000000000000000000 ) ;
#57013 = CARTESIAN_POINT ( 'NONE',  ( -5.000000000000000000, 17.00000000000000000, 0.000000000000000000 ) ) ;
#57014 = CARTESIAN_POINT ( 'NONE',  ( 3.535533905932736864, -142.2500000027311842, 3.535533905932738641 ) ) ;
#57015 = CARTESIAN_POINT ( 'NONE',  ( -2.498395430326213474E-14, 22.25000000000000000, 5.000000000000000000 ) ) ;
#57016 = CARTESIAN_POINT ( 'NONE',  ( 9.457646018065525792E-16, -50.06249999863440792, 5.148502694627439702 ) ) ;
#57017 = CARTESIAN_POINT ( 'NONE',  ( 2.499999999999998668, -85.20833333060214443, -4.330127018922193649 ) ) ;
#57018 = EDGE_CURVE ( 'NONE', #41628, #48755, #58105, .T. ) ;
#57019 = CARTESIAN_POINT ( 'NONE',  ( -58.39396692619412477, -135.6875000013656063, 2.891590998281057701 ) ) ;
#57020 = CARTESIAN_POINT ( 'NONE',  ( 5.000000000000000000, -65.29166666393547303, -2.886751345948130876 ) ) ;
#57021 = ADVANCED_FACE ( 'NONE', ( #12908 ), #53407, .T. ) ;
#57022 = CARTESIAN_POINT ( 'NONE',  ( 1.975475456537005874E-15, -89.62499999726880162, 5.000000000000000000 ) ) ;
#57023 = EDGE_CURVE ( 'NONE', #32043, #34883, #38011, .T. ) ;
#57024 = CARTESIAN_POINT ( 'NONE',  ( -2.229367062500000163, -84.72916666530107932, -3.861377020970580443 ) ) ;
#57025 = CARTESIAN_POINT ( 'NONE',  ( 1.846868145590736310, -155.8750000013655779, 4.458734124999997661 ) ) ;
#57026 = CARTESIAN_POINT ( 'NONE',  ( -4.999999999999999112, -31.91666666666666430, 2.886751345948131764 ) ) ;
#57027 =( NAMED_UNIT ( * ) SI_UNIT ( $, .STERADIAN. ) SOLID_ANGLE_UNIT ( ) );
#57028 = ORIENTED_EDGE ( 'NONE', *, *, #39005, .F. ) ;
#57029 = CARTESIAN_POINT ( 'NONE',  ( 9.457646018065525792E-16, 17.68750000136559564, 5.148502694627439702 ) ) ;
#57030 = ORIENTED_EDGE ( 'NONE', *, *, #21310, .F. ) ;
#57031 = CARTESIAN_POINT ( 'NONE',  ( -4.458734124999999437, -97.31249999863440792, 0.000000000000000000 ) ) ;
#57032 = CARTESIAN_POINT ( 'NONE',  ( 4.458734125000001214, 7.854166668032260823, 2.574251347313718519 ) ) ;
#57033 = CARTESIAN_POINT ( 'NONE',  ( -5.000000000000000000, 12.12500000273118772, 0.000000000000000000 ) ) ;
#57034 = CARTESIAN_POINT ( 'NONE',  ( -1.339745962155613812, -60.20534180126147561, -5.000000000000000000 ) ) ;
#57035 = CARTESIAN_POINT ( 'NONE',  ( -2.500000000000000444, 9.833333333333332149, -4.330127018922193649 ) ) ;
#57036 = VECTOR ( 'NONE', #16304, 1000.000000000000000 ) ;
#57037 = CARTESIAN_POINT ( 'NONE',  ( -4.458734124999999437, -56.31249999863440081, 0.000000000000000000 ) ) ;
#57038 = CARTESIAN_POINT ( 'NONE',  ( -5.000000000000000000, -8.083333333333332149, -2.886751345948128211 ) ) ;
#57039 = CARTESIAN_POINT ( 'NONE',  ( 2.500000000000002220, -80.66666666666665719, 4.330127018922192761 ) ) ;
#57040 = ADVANCED_BREP_SHAPE_REPRESENTATION ( '', ( #50087, #43054 ), #24596 ) ;
#57041 = CARTESIAN_POINT ( 'NONE',  ( -4.458734124999999437, -29.31249999863440436, 0.000000000000000000 ) ) ;
#57042 = CARTESIAN_POINT ( 'NONE',  ( 3.535533905932736864, -153.2500000027312126, 3.535533905932738641 ) ) ;
#57043 = CARTESIAN_POINT ( 'NONE',  ( 6.123233995736766282E-16, -120.0000000000000000, -5.000000000000000000 ) ) ;
#57044 = EDGE_CURVE ( 'NONE', #62422, #44925, #1034, .T. ) ;
#57045 = CARTESIAN_POINT ( 'NONE',  ( -5.000000000000000000, -151.6250000027312126, -6.123233995736766282E-16 ) ) ;
#57046 = CARTESIAN_POINT ( 'NONE',  ( -5.000000000000000000, -41.99999999999999289, 0.000000000000000000 ) ) ;
#57047 = CARTESIAN_POINT ( 'NONE',  ( 5.000000000000000000, -107.4999999999999858, -6.123233995736766282E-16 ) ) ;
#57049 = CARTESIAN_POINT ( 'NONE',  ( 4.458734124999999437, -22.06249999863440436, -5.460374474430324690E-16 ) ) ;
#57048 = DIRECTION ( 'NONE',  ( 0.000000000000000000, 0.000000000000000000, 1.000000000000000000 ) ) ;
#57050 = CARTESIAN_POINT ( 'NONE',  ( -1.339745962155610925, -57.79465819873852439, 5.000000000000000000 ) ) ;
#57051 = CARTESIAN_POINT ( 'NONE',  ( 4.458734124999999437, -65.81249999863440792, -5.460374474430324690E-16 ) ) ;
#57052 = CARTESIAN_POINT ( 'NONE',  ( -1.846868145590734756, -148.3750000013655779, -4.458734125000000326 ) ) ;
#57053 = CARTESIAN_POINT ( 'NONE',  ( -2.229367062499996610, -69.14583333196773651, 3.861377020970582219 ) ) ;
#57054 = CARTESIAN_POINT ( 'NONE',  ( -54.64476657466781973, -143.0625000013656063, -4.444560631937228834 ) ) ;
#57055 = VECTOR ( 'NONE', #55474, 1000.000000000000000 ) ;
#57056 = CARTESIAN_POINT ( 'NONE',  ( -4.458734124999999437, -25.64583333196773651, -2.574251347313719407 ) ) ;
#57057 = CARTESIAN_POINT ( 'NONE',  ( -2.499999999999996447, -59.70833333060214443, 4.330127018922195425 ) ) ;
#57058 = ORIENTED_EDGE ( 'NONE', *, *, #39697, .F. ) ;
#57059 = DIRECTION ( 'NONE',  ( 0.000000000000000000, 0.000000000000000000, 1.000000000000000000 ) ) ;
#57060 = VERTEX_POINT ( 'NONE', #54370 ) ;
#57061 = CARTESIAN_POINT ( 'NONE',  ( -3.152548672688508926E-16, -65.81249999863440792, -5.148502694627439702 ) ) ;
#57062 = CARTESIAN_POINT ( 'NONE',  ( 6.123233995736766282E-16, -170.0000000000000000, -5.000000000000000000 ) ) ;
#57063 = LINE ( 'NONE', #22324, #26632 ) ;
#57064 = VERTEX_POINT ( 'NONE', #29262 ) ;
#57065 = DIRECTION ( 'NONE',  ( -7.709882115452477180E-16, 0.000000000000000000, -1.000000000000000000 ) ) ;
#57066 = CYLINDRICAL_SURFACE ( 'NONE', #28275, 5.000000000000000000 ) ;
#57067 = CARTESIAN_POINT ( 'NONE',  ( 2.229367062499998831, -55.89583333196773651, -3.861377020970580887 ) ) ;
#57068 = ORIENTED_EDGE ( 'NONE', *, *, #4704, .F. ) ;
#57069 = CARTESIAN_POINT ( 'NONE',  ( -6.972266317189433020E-16, -88.12499999726880162, -5.000000000000000000 ) ) ;
#57070 = CARTESIAN_POINT ( 'NONE',  ( -3.152548672688508926E-16, 7.437500001365594748, -5.148502694627439702 ) ) ;
#57071 = CARTESIAN_POINT ( 'NONE',  ( -2.229367062499996610, 19.85416666803225993, 3.861377020970582219 ) ) ;
#57072 = CARTESIAN_POINT ( 'NONE',  ( -57.19623071787017210, -149.3750000013656347, 4.297418129356382899 ) ) ;
#57073 = CARTESIAN_POINT ( 'NONE',  ( -51.75738570946856498, -149.8750000027312126, 3.805975901505576964 ) ) ;
#57074 = CARTESIAN_POINT ( 'NONE',  ( -4.458734124999999437, -168.9375000013656063, -5.460374474430324690E-16 ) ) ;
#57075 = EDGE_LOOP ( 'NONE', ( #35916, #59814, #45863, #40398 ) ) ;
#57076 = CARTESIAN_POINT ( 'NONE',  ( -4.458734124999999437, -68.31249999863439371, 0.000000000000000000 ) ) ;
#57077 = CARTESIAN_POINT ( 'NONE',  ( -1.339745962155613812, -86.08034179853028434, -5.000000000000000000 ) ) ;
#57078 = CARTESIAN_POINT ( 'NONE',  ( 4.458734124999999437, 7.187500001365594748, -5.460374474430324690E-16 ) ) ;
#57079 = CARTESIAN_POINT ( 'NONE',  ( 1.975475456537005874E-15, -78.74999999999998579, 5.000000000000000000 ) ) ;
#57080 = CARTESIAN_POINT ( 'NONE',  ( 2.229367062499998831, -61.89583333196774362, -3.861377020970580887 ) ) ;
#57081 = CARTESIAN_POINT ( 'NONE',  ( -5.000000000000000000, -18.95833333060214443, -2.886751345948128211 ) ) ;
#57082 = CARTESIAN_POINT ( 'NONE',  ( -1.339745962155555858, -19.20534180126148271, -5.000000000000032863 ) ) ;
#57083 = CARTESIAN_POINT ( 'NONE',  ( -51.19402409849444524, -140.6250000027312126, -3.242614290531456334 ) ) ;
#57084 = CARTESIAN_POINT ( 'NONE',  ( -6.972266317189433020E-16, -84.12499999726880162, -5.000000000000000000 ) ) ;
#57085 = CARTESIAN_POINT ( 'NONE',  ( 4.458734124999998549, -39.72916666530107932, -2.574251347313721627 ) ) ;
#57086 = CARTESIAN_POINT ( 'NONE',  ( 4.458734125000000326, -19.14583333196774007, 2.574251347313718519 ) ) ;
#57087 = VERTEX_POINT ( 'NONE', #39552 ) ;
#57088 = CARTESIAN_POINT ( 'NONE',  ( -6.972266317189433020E-16, -102.2499999999999858, -5.000000000000000000 ) ) ;
#57089 = CARTESIAN_POINT ( 'NONE',  ( 4.458734124999998549, -109.7291666653010793, -2.574251347313721627 ) ) ;
#57090 = CARTESIAN_POINT ( 'NONE',  ( 5.000000000000000888, -154.0625000027312126, -2.071067811865475505 ) ) ;
#57091 = VERTEX_POINT ( 'NONE', #5156 ) ;
#57092 = CARTESIAN_POINT ( 'NONE',  ( -4.458734124999999437, -109.5624999986343937, 0.000000000000000000 ) ) ;
#57093 = CARTESIAN_POINT ( 'NONE',  ( -4.458734124999999437, -34.39583333196772941, -2.574251347313719407 ) ) ;
#57094 = CARTESIAN_POINT ( 'NONE',  ( -5.000000000000000000, -65.87499999726881583, 0.000000000000000000 ) ) ;
#57095 = CARTESIAN_POINT ( 'NONE',  ( -50.55543936806279248, -146.3125000013656063, 0.3552334253322060320 ) ) ;
#57096 =( BOUNDED_CURVE ( )  B_SPLINE_CURVE ( 2, ( #30638, #21318, #30958, #55092, #6208, #15208, #5244, #59277, #40605 ),
 .UNSPECIFIED., .F., .F. ) 
 B_SPLINE_CURVE_WITH_KNOTS ( ( 3, 2, 2, 2, 3 ),
 ( 0.4895833333333333148, 0.4902777777777777568, 0.4916666666666666408, 0.4930555555555555802, 0.4937500000000000222 ),
 .UNSPECIFIED. ) 
 CURVE ( )  GEOMETRIC_REPRESENTATION_ITEM ( )  RATIONAL_B_SPLINE_CURVE ( ( 0.9330127018922194093, 0.9330127018922194093, 1.000000000000000000, 0.8660254037844387076, 1.000000000000000000, 0.8660254037844387076, 1.000000000000000000, 0.9330127018922194093, 0.9330127018922194093 ) ) 
 REPRESENTATION_ITEM ( '' )  );
#57097 = CARTESIAN_POINT ( 'NONE',  ( 5.000000000000000888, -146.9375000000000284, -2.071067811865475505 ) ) ;
#57098 = EDGE_CURVE ( 'NONE', #15518, #62343, #44571, .T. ) ;
#57099 = EDGE_CURVE ( 'NONE', #38204, #47541, #7600, .T. ) ;
#57100 = CARTESIAN_POINT ( 'NONE',  ( -2.229367062499996610, -27.14583333196774007, 3.861377020970582219 ) ) ;
#57101 = CARTESIAN_POINT ( 'NONE',  ( 4.458734125000000326, -67.14583333196773651, 2.574251347313718519 ) ) ;
#57102 = LINE ( 'NONE', #52891, #22336 ) ;
#57103 = CARTESIAN_POINT ( 'NONE',  ( 2.229367062499998831, -26.64583333196774007, -3.861377020970580887 ) ) ;
#57104 = ADVANCED_FACE ( 'NONE', ( #19626 ), #9653, .T. ) ;
#57105 = CARTESIAN_POINT ( 'NONE',  ( 1.339745962155612702, -32.29465819873852439, -5.000000000000000000 ) ) ;
#57106 = CARTESIAN_POINT ( 'NONE',  ( 5.000000000000000000, -5.291666663935480130, -2.886751345948130876 ) ) ;
#57107 = CARTESIAN_POINT ( 'NONE',  ( -3.535250795749689387E-16, -14.25000000000000178, -5.773502691896257311 ) ) ;
#57108 = CARTESIAN_POINT ( 'NONE',  ( -8.190561711645485556E-16, -148.6875000013656063, 4.458734124999999437 ) ) ;
#57109 = ORIENTED_EDGE ( 'NONE', *, *, #23403, .T. ) ;
#57110 = CARTESIAN_POINT ( 'NONE',  ( 6.123233995736766282E-16, -120.0000000000000000, -5.000000000000000000 ) ) ;
#57111 = CARTESIAN_POINT ( 'NONE',  ( 4.458734124999999437, -53.06249999863440792, -5.460374474430324690E-16 ) ) ;
#57112 = CARTESIAN_POINT ( 'NONE',  ( 5.000000000000000888, -2.583333333333333481, 2.886751345948126879 ) ) ;
#57113 = CARTESIAN_POINT ( 'NONE',  ( -4.999999999999998224, -0.9166666666666664076, 2.886751345948131764 ) ) ;
#57114 = CARTESIAN_POINT ( 'NONE',  ( 2.500000000000002220, 23.33333333333333215, 4.330127018922192761 ) ) ;
#57115 = EDGE_CURVE ( 'NONE', #14315, #59250, #40205, .T. ) ;
#57116 = EDGE_CURVE ( 'NONE', #34696, #21297, #39236, .T. ) ;
#57117 = CARTESIAN_POINT ( 'NONE',  ( 2.499999999999998668, -76.20833333060214443, -4.330127018922193649 ) ) ;
#57118 = CARTESIAN_POINT ( 'NONE',  ( 4.458734124999998549, -2.729166665301069550, -2.574251347313721627 ) ) ;
#57119 = CARTESIAN_POINT ( 'NONE',  ( -2.499999999999996447, -10.83333333333333393, 4.330127018922195425 ) ) ;
#57120 = CARTESIAN_POINT ( 'NONE',  ( 5.000000000000000000, -141.0625000000000000, 2.071067811865478614 ) ) ;
#57121 = CARTESIAN_POINT ( 'NONE',  ( 5.000000000000000888, -87.45833333060214443, 2.886751345948126879 ) ) ;
#57122 = CARTESIAN_POINT ( 'NONE',  ( -2.229367062499996610, 10.60416666803225993, 3.861377020970582219 ) ) ;
#57124 = VERTEX_POINT ( 'NONE', #25089 ) ;
#57123 = EDGE_CURVE ( 'NONE', #61001, #21194, #19940, .T. ) ;
#57125 = CARTESIAN_POINT ( 'NONE',  ( 0.000000000000000000, -120.0000000000000000, 0.000000000000000000 ) ) ;
#57126 = VERTEX_POINT ( 'NONE', #10297 ) ;
#57127 = CARTESIAN_POINT ( 'NONE',  ( -6.972266317189433020E-16, -85.25000000000000000, -5.000000000000000000 ) ) ;
#57128 = CARTESIAN_POINT ( 'NONE',  ( -4.458734124999998549, -49.22916666530106511, 2.574251347313722516 ) ) ;
#57129 = EDGE_CURVE ( 'NONE', #44174, #39750, #56057, .T. ) ;
#57130 = CARTESIAN_POINT ( 'NONE',  ( -3.152801135295367096, -158.3125000013656063, -3.152801135295367541 ) ) ;
#57131 = EDGE_CURVE ( 'NONE', #59301, #34883, #25, .T. ) ;
#57132 = CARTESIAN_POINT ( 'NONE',  ( 1.060575238724906964E-15, -46.62499999726880873, 5.773502691896257311 ) ) ;
#57133 = ORIENTED_EDGE ( 'NONE', *, *, #40308, .F. ) ;
#57134 = CARTESIAN_POINT ( 'NONE',  ( -3.152548672688508926E-16, -21.56249999863440081, -5.148502694627439702 ) ) ;
#57135 = ORIENTED_EDGE ( 'NONE', *, *, #32539, .F. ) ;
#57136 = CARTESIAN_POINT ( 'NONE',  ( -2.499999999999996447, -102.7083333306021444, 4.330127018922195425 ) ) ;
#57137 = CARTESIAN_POINT ( 'NONE',  ( -1.846868145590734756, -161.1250000013656063, -4.458734125000000326 ) ) ;
#57138 = CARTESIAN_POINT ( 'NONE',  ( -52.53715891517739323, -139.4375000000000000, -4.819101127000233298 ) ) ;
#57139 = CARTESIAN_POINT ( 'NONE',  ( 4.458734125000001214, -37.14583333196773651, 2.574251347313718519 ) ) ;
#57141 = AXIS2_PLACEMENT_3D ( 'NONE', #14722, #40442, #49777 ) ;
#57140 = CARTESIAN_POINT ( 'NONE',  ( 6.123233995736766282E-16, -120.0000000000000000, -5.000000000000000000 ) ) ;
#57142 = EDGE_LOOP ( 'NONE', ( #24348, #35271, #13329, #56886 ) ) ;
#57143 = AXIS2_PLACEMENT_3D ( 'NONE', #32058, #3124, #37522 ) ;
#57144 = CARTESIAN_POINT ( 'NONE',  ( 4.458734124999999437, -81.81249999863440792, -5.460374474430324690E-16 ) ) ;
#57145 = CARTESIAN_POINT ( 'NONE',  ( 4.458734125000001214, 25.10416666803225638, 2.574251347313718519 ) ) ;
#57146 = DIRECTION ( 'NONE',  ( -0.000000000000000000, 1.000000000000000000, -0.000000000000000000 ) ) ;
#57147 = ORIENTED_EDGE ( 'NONE', *, *, #47211, .F. ) ;
#57148 = CARTESIAN_POINT ( 'NONE',  ( 2.499999999999998668, 14.66666666666666607, -4.330127018922193649 ) ) ;
#57149 = CARTESIAN_POINT ( 'NONE',  ( -57.19623071787016499, -138.6250000013656063, 4.297418129356382899 ) ) ;
#57150 = CARTESIAN_POINT ( 'NONE',  ( -2.229367062500000163, -87.72916666530107932, -3.861377020970580443 ) ) ;
#57151 = CARTESIAN_POINT ( 'NONE',  ( -60.14911071818854538, -129.1875000027312126, 1.666127454062681368 ) ) ;
#57152 = DIRECTION ( 'NONE',  ( 0.000000000000000000, 0.000000000000000000, 1.000000000000000000 ) ) ;
#57153 = CARTESIAN_POINT ( 'NONE',  ( -2.499999999999996447, -6.833333333333330373, 4.330127018922195425 ) ) ;
#57154 =( BOUNDED_CURVE ( )  B_SPLINE_CURVE ( 2, ( #9680, #49245, #1342, #49873, #4865, #35099, #24485, #14504, #10637 ),
 .UNSPECIFIED., .F., .F. ) 
 B_SPLINE_CURVE_WITH_KNOTS ( ( 3, 2, 2, 2, 3 ),
 ( 0.6979166666666666297, 0.6986111111111110716, 0.6999999999999999556, 0.7013888888888888395, 0.7020833333333332815 ),
 .UNSPECIFIED. ) 
 CURVE ( )  GEOMETRIC_REPRESENTATION_ITEM ( )  RATIONAL_B_SPLINE_CURVE ( ( 0.9330127018922194093, 0.9330127018922194093, 1.000000000000000000, 0.8660254037844387076, 1.000000000000000000, 0.8660254037844387076, 1.000000000000000000, 0.9330127018922194093, 0.9330127018922194093 ) ) 
 REPRESENTATION_ITEM ( '' )  );
#57155 = CARTESIAN_POINT ( 'NONE',  ( -1.339745962155613812, -47.08034179853029144, -5.000000000000000000 ) ) ;
#57156 = CARTESIAN_POINT ( 'NONE',  ( 9.457646018065525792E-16, -55.06249999863440081, 5.148502694627439702 ) ) ;
#57157 = CARTESIAN_POINT ( 'NONE',  ( -6.972266317189433020E-16, 10.75000000000000000, -5.000000000000000000 ) ) ;
#57158 = CARTESIAN_POINT ( 'NONE',  ( 4.458734124999998549, 22.27083333469893134, -2.574251347313721627 ) ) ;
#57159 = CARTESIAN_POINT ( 'NONE',  ( -5.000000000000000000, -107.0833333333333428, -2.886751345948128211 ) ) ;
#57160 = CARTESIAN_POINT ( 'NONE',  ( 0.000000000000000000, -170.0000000000000000, 5.000000000000000000 ) ) ;
#57161 = CARTESIAN_POINT ( 'NONE',  ( 2.229367062500001939, -45.22916666530106511, 3.861377020970579999 ) ) ;
#57162 = CARTESIAN_POINT ( 'NONE',  ( -5.000000000000000000, -4.874999997268810503, 0.000000000000000000 ) ) ;
#57163 = CARTESIAN_POINT ( 'NONE',  ( -55.39835681537999790, -153.8750000000000284, 4.984105922594378235 ) ) ;
#57164 = DIRECTION ( 'NONE',  ( -0.000000000000000000, 1.000000000000000000, -0.000000000000000000 ) ) ;
#57165 = CARTESIAN_POINT ( 'NONE',  ( 9.457646018065525792E-16, -85.31249999863439371, 5.148502694627439702 ) ) ;
#57166 = CARTESIAN_POINT ( 'NONE',  ( -2.229367062499996610, -104.1458333319677365, 3.861377020970582219 ) ) ;
#57167 = CARTESIAN_POINT ( 'NONE',  ( -4.458734124999999437, -5.645833331967740953, -2.574251347313719407 ) ) ;
#57168 = ORIENTED_EDGE ( 'NONE', *, *, #30730, .F. ) ;
#57169 = FACE_OUTER_BOUND ( 'NONE', #8410, .T. ) ;
#57170 = CARTESIAN_POINT ( 'NONE',  ( -4.458734124999999437, -95.39583333196772230, -2.574251347313719407 ) ) ;
#57171 = CARTESIAN_POINT ( 'NONE',  ( -5.000000000000000888, -164.5625000027312126, 2.071067811865474617 ) ) ;
#57172 = CARTESIAN_POINT ( 'NONE',  ( -3.152548672688508926E-16, -89.81249999863439371, -5.148502694627439702 ) ) ;
#57173 = CARTESIAN_POINT ( 'NONE',  ( -2.229367062500000163, 14.27083333469892601, -3.861377020970580443 ) ) ;
#57174 = DIRECTION ( 'NONE',  ( -0.6485228581062915110, 0.000000000000000000, -0.7611951803011149931 ) ) ;
#57175 = CARTESIAN_POINT ( 'NONE',  ( -51.60603307380591787, -131.9375000013656063, -2.891590998281053704 ) ) ;
#57176 = CARTESIAN_POINT ( 'NONE',  ( -2.229367062499996610, -12.14583333196774007, 3.861377020970582219 ) ) ;
#57177 = CARTESIAN_POINT ( 'NONE',  ( -4.458734124999999437, 12.43750000136559564, 0.000000000000000000 ) ) ;
#57178 = CARTESIAN_POINT ( 'NONE',  ( 4.458734125000000326, -56.14583333196773651, 2.574251347313718519 ) ) ;
#57179 = CARTESIAN_POINT ( 'NONE',  ( -5.000000000000000000, -69.08333333333332860, -2.886751345948128211 ) ) ;
#57180 = CARTESIAN_POINT ( 'NONE',  ( 4.458734124999998549, -9.729166665301068662, -2.574251347313721627 ) ) ;
#57181 = SURFACE_SIDE_STYLE ('',( #41721 ) ) ;
#57182 = EDGE_LOOP ( 'NONE', ( #25153, #4353, #46913, #46274, #23418, #43778 ) ) ;
#57183 = CARTESIAN_POINT ( 'NONE',  ( -4.458734124999997661, -35.47916666530107221, 2.574251347313722516 ) ) ;
#57184 = AXIS2_PLACEMENT_3D ( 'NONE', #41338, #36521, #56151 ) ;
#57185 = CARTESIAN_POINT ( 'NONE',  ( -57.19623071787017210, -128.6250000013656347, 4.297418129356382899 ) ) ;
#57186 = DIRECTION ( 'NONE',  ( 0.000000000000000000, 0.000000000000000000, 1.000000000000000000 ) ) ;
#57187 = CARTESIAN_POINT ( 'NONE',  ( -2.229367062500000163, -80.47916666530106511, -3.861377020970580443 ) ) ;
#57188 = CARTESIAN_POINT ( 'NONE',  ( 9.457646018065525792E-16, 25.68750000136559208, 5.148502694627439702 ) ) ;
#57189 = AXIS2_PLACEMENT_3D ( 'NONE', #13090, #51707, #12770 ) ;
#57190 = CARTESIAN_POINT ( 'NONE',  ( 4.458734124999998549, 13.27083333469892779, -2.574251347313721627 ) ) ;
#57191 = CARTESIAN_POINT ( 'NONE',  ( -5.000000000000000000, -81.95833333060213022, -2.886751345948128211 ) ) ;
#57192 = DIRECTION ( 'NONE',  ( -0.000000000000000000, 1.000000000000000000, -0.000000000000000000 ) ) ;
#57193 = CARTESIAN_POINT ( 'NONE',  ( 4.458734124999998549, -83.97916666530106511, -2.574251347313721627 ) ) ;
#57194 = CARTESIAN_POINT ( 'NONE',  ( 2.499999999999998668, -69.33333333333332860, -4.330127018922193649 ) ) ;
#57195 = CARTESIAN_POINT ( 'NONE',  ( -5.000000000000000000, 29.91666666666666430, -2.886751345948128211 ) ) ;
#57196 = CARTESIAN_POINT ( 'NONE',  ( -2.499999999999996447, 21.29166666939785202, 4.330127018922195425 ) ) ;
#57197 = ORIENTED_EDGE ( 'NONE', *, *, #40512, .T. ) ;
#57198 = CARTESIAN_POINT ( 'NONE',  ( 3.061616997868383141E-16, -146.8750000027312126, -5.000000000000000000 ) ) ;
#57199 = DIRECTION ( 'NONE',  ( 0.000000000000000000, 0.000000000000000000, 1.000000000000000000 ) ) ;
#57200 =( BOUNDED_CURVE ( )  B_SPLINE_CURVE ( 2, ( #5247, #39963, #24871, #53499, #4928, #10387, #19716, #54777, #29345 ),
 .UNSPECIFIED., .F., .F. ) 
 B_SPLINE_CURVE_WITH_KNOTS ( ( 3, 2, 2, 2, 3 ),
 ( 0.2303571428571428714, 0.2309523809523809645, 0.2321428571428571508, 0.2333333333333333370, 0.2339285714285714302 ),
 .UNSPECIFIED. ) 
 CURVE ( )  GEOMETRIC_REPRESENTATION_ITEM ( )  RATIONAL_B_SPLINE_CURVE ( ( 0.9330127018922194093, 0.9330127018922209636, 1.000000000000000000, 0.8660254037844387076, 1.000000000000000000, 0.8660254037844387076, 1.000000000000000000, 0.9330127018922194093, 0.9330127018922194093 ) ) 
 REPRESENTATION_ITEM ( '' )  );
#57202 = CARTESIAN_POINT ( 'NONE',  ( -5.000000000000000000, -28.99999999999999645, 0.000000000000000000 ) ) ;
#57201 = DIRECTION ( 'NONE',  ( -0.000000000000000000, 1.000000000000000000, -0.000000000000000000 ) ) ;
#57203 = CARTESIAN_POINT ( 'NONE',  ( -4.458734124999999437, -34.31249999863440792, 0.000000000000000000 ) ) ;
#57204 = EDGE_CURVE ( 'NONE', #15879, #23303, #9260, .T. ) ;
#57205 = CARTESIAN_POINT ( 'NONE',  ( 5.000000000000000000, -29.29166666393547658, -2.886751345948129988 ) ) ;
#57207 = ORIENTED_EDGE ( 'NONE', *, *, #3657, .F. ) ;
#57206 = CARTESIAN_POINT ( 'NONE',  ( -3.152548672688508926E-16, -58.56249999863440081, -5.148502694627439702 ) ) ;
#57208 = DIRECTION ( 'NONE',  ( 0.000000000000000000, 0.000000000000000000, 1.000000000000000000 ) ) ;
#57210 = ORIENTED_EDGE ( 'NONE', *, *, #35281, .F. ) ;
#57209 = CARTESIAN_POINT ( 'NONE',  ( -4.458734124999998549, -11.47916666530107044, 2.574251347313722516 ) ) ;
#57211 = CARTESIAN_POINT ( 'NONE',  ( 5.000000000000000888, -76.58333333333332860, 2.886751345948126879 ) ) ;
#57212 = CARTESIAN_POINT ( 'NONE',  ( -57.89159099828107458, -139.6875000013656063, -3.393966926194107447 ) ) ;
#57213 = CARTESIAN_POINT ( 'NONE',  ( -4.458734124999998549, -51.47916666530106511, 2.574251347313722516 ) ) ;
#57214 = CARTESIAN_POINT ( 'NONE',  ( 5.000000000000000000, -74.29166666393547303, -2.886751345948129988 ) ) ;
#57216 = ORIENTED_EDGE ( 'NONE', *, *, #41328, .F. ) ;
#57215 = CARTESIAN_POINT ( 'NONE',  ( -1.339745962155610925, -54.66965819600732601, 5.000000000000000000 ) ) ;
#57217 = CARTESIAN_POINT ( 'NONE',  ( -60.14911071818854538, -148.0625000000000000, 1.666127454062681368 ) ) ;
#57218 = CARTESIAN_POINT ( 'NONE',  ( -4.458734124999999437, -21.64583333196774362, -2.574251347313719407 ) ) ;
#57220 = VERTEX_POINT ( 'NONE', #12210 ) ;
#57219 = CARTESIAN_POINT ( 'NONE',  ( 4.458734124999998549, -54.97916666530107221, -2.574251347313721627 ) ) ;
#57221 = CARTESIAN_POINT ( 'NONE',  ( 55.00000000000002132, -10.00000000000000178, 0.000000000000000000 ) ) ;
#57222 = CARTESIAN_POINT ( 'NONE',  ( -1.846868145590734756, -141.1250000013655779, -4.458734125000000326 ) ) ;
#57223 = CARTESIAN_POINT ( 'NONE',  ( -2.229367062499996610, -102.3958333319677365, 3.861377020970582219 ) ) ;
#57224 = CARTESIAN_POINT ( 'NONE',  ( 6.123233995736766282E-16, -170.0000000000000000, -5.000000000000000000 ) ) ;
#57225 = VERTEX_POINT ( 'NONE', #21868 ) ;
#57226 = CARTESIAN_POINT ( 'NONE',  ( -52.80376928212989185, -150.1250000013656063, -4.297418129356378458 ) ) ;
#57227 = CARTESIAN_POINT ( 'NONE',  ( -55.39835681537999790, -141.0000000027312126, 4.984105922594378235 ) ) ;
#57228 = VECTOR ( 'NONE', #54468, 1000.000000000000000 ) ;
#57229 = DIRECTION ( 'NONE',  ( 0.8191520442889907994, 1.003171929053523514E-16, -0.5735764363510474917 ) ) ;
#57230 = CARTESIAN_POINT ( 'NONE',  ( -4.458734124999999437, -5.312499998634402587, 0.000000000000000000 ) ) ;
#57231 = MECHANICAL_DESIGN_GEOMETRIC_PRESENTATION_REPRESENTATION (  '', ( #36696 ), #52126 ) ;
#57232 = CARTESIAN_POINT ( 'NONE',  ( -3.152548672688508926E-16, -96.81249999863440792, -5.148502694627439702 ) ) ;
#57233 = CARTESIAN_POINT ( 'NONE',  ( 3.152801135295367541, -148.5625000013655779, -3.152801135295367541 ) ) ;
#57234 = CARTESIAN_POINT ( 'NONE',  ( 2.229367062500001939, -29.22916666530107221, 3.861377020970579999 ) ) ;
#57235 = CLOSED_SHELL ( 'NONE', ( #28326, #55794, #38821, #10682, #4101, #28285, #55492, #36348, #34257, #17402, #28615, #31026, #25223, #12915, #33049, #1713, #52368, #832, #54627, #42477, #5262, #24842, #51443, #17871, #57380, #36605, #19620, #21731, #48368, #42553, #63429, #61740 ) ) ;
#57236 = CARTESIAN_POINT ( 'NONE',  ( 1.975475456537005874E-15, -66.62499999726881583, 5.000000000000000000 ) ) ;
#57237 = CARTESIAN_POINT ( 'NONE',  ( -55.35523342533222291, -138.3125000013656063, 4.444560631937231499 ) ) ;
#57238 = CARTESIAN_POINT ( 'NONE',  ( -2.229367062499996610, -65.39583333196773651, 3.861377020970582219 ) ) ;
#57239 = CARTESIAN_POINT ( 'NONE',  ( -2.499999999999996447, -15.83333333333333037, 4.330127018922195425 ) ) ;
#57240 = DIRECTION ( 'NONE',  ( -0.000000000000000000, 1.000000000000000000, -0.000000000000000000 ) ) ;
#57241 = CARTESIAN_POINT ( 'NONE',  ( -8.190561711645485556E-16, -141.6875000013656063, 4.458734124999999437 ) ) ;
#57242 = CARTESIAN_POINT ( 'NONE',  ( -2.229367062500000163, 8.270833334698926009, -3.861377020970580443 ) ) ;
#57243 = ORIENTED_EDGE ( 'NONE', *, *, #18804, .F. ) ;
#57244 = CARTESIAN_POINT ( 'NONE',  ( 1.975475456537005874E-15, -49.62499999726880873, 5.000000000000000000 ) ) ;
#57245 = CARTESIAN_POINT ( 'NONE',  ( 1.975475456537005874E-15, -6.624999997268813168, 5.000000000000000000 ) ) ;
#57247 = CARTESIAN_POINT ( 'NONE',  ( 4.458734124999998549, -23.72916666530107221, -2.574251347313721627 ) ) ;
#57246 = CARTESIAN_POINT ( 'NONE',  ( -2.500000000000000444, -93.16666666666665719, -4.330127018922193649 ) ) ;
#57248 = CARTESIAN_POINT ( 'NONE',  ( 1.975475456537005874E-15, -76.62499999726880162, 5.000000000000000000 ) ) ;
#57249 = CARTESIAN_POINT ( 'NONE',  ( 2.229367062499998831, -76.89583333196773651, -3.861377020970580887 ) ) ;
#57250 = CARTESIAN_POINT ( 'NONE',  ( 2.229367062499998831, 26.10416666803225993, -3.861377020970580887 ) ) ;
#57251 = CARTESIAN_POINT ( 'NONE',  ( 6.123233995736766282E-16, -120.0000000000000000, -5.000000000000000000 ) ) ;
#57252 = CARTESIAN_POINT ( 'NONE',  ( -58.39396692619412477, -144.4375000013656063, 2.891590998281057701 ) ) ;
#57253 = CARTESIAN_POINT ( 'NONE',  ( 2.229367062500001939, 5.020833334698926897, 3.861377020970579999 ) ) ;
#57254 = LINE ( 'NONE', #42431, #11938 ) ;
#57255 = LINE ( 'NONE', #48522, #20211 ) ;
#57256 = CARTESIAN_POINT ( 'NONE',  ( -4.458734124999999437, 8.687500001365595637, 0.000000000000000000 ) ) ;
#57257 = CARTESIAN_POINT ( 'NONE',  ( -4.458734124999999437, -73.31249999863439371, 0.000000000000000000 ) ) ;
#57258 = CARTESIAN_POINT ( 'NONE',  ( 4.458734124999998549, -16.97916666530107577, -2.574251347313721627 ) ) ;
#57259 = CARTESIAN_POINT ( 'NONE',  ( 1.060575238724906964E-15, -7.749999999999999112, 5.773502691896257311 ) ) ;
#57260 = CARTESIAN_POINT ( 'NONE',  ( -1.846868145590734756, -160.1250000013655779, -4.458734125000000326 ) ) ;
#57261 = CARTESIAN_POINT ( 'NONE',  ( 2.500000000000002220, 15.45833333606451987, 4.330127018922192761 ) ) ;
#57262 = CARTESIAN_POINT ( 'NONE',  ( 2.229367062500001939, -63.97916666530106511, 3.861377020970579999 ) ) ;
#57263 = CARTESIAN_POINT ( 'NONE',  ( -5.000000000000000000, -97.95833333060214443, -2.886751345948128211 ) ) ;
#57264 = FACE_OUTER_BOUND ( 'NONE', #42175, .T. ) ;
#57265 = CARTESIAN_POINT ( 'NONE',  ( 4.458734125000000326, -40.89583333196773651, 2.574251347313718519 ) ) ;
#57266 = FACE_OUTER_BOUND ( 'NONE', #54247, .T. ) ;
#57267 = CARTESIAN_POINT ( 'NONE',  ( 2.229367062499998831, -104.8958333319677365, -3.861377020970580887 ) ) ;
#57268 = CARTESIAN_POINT ( 'NONE',  ( -2.229367062499996610, -67.39583333196773651, 3.861377020970582219 ) ) ;
#57269 = CARTESIAN_POINT ( 'NONE',  ( -5.000000000000000000, -56.08333333333332860, -2.886751345948128211 ) ) ;
#57270 = CARTESIAN_POINT ( 'NONE',  ( 1.975475456537005874E-15, -57.62499999726880873, 5.000000000000000000 ) ) ;
#57271 = CARTESIAN_POINT ( 'NONE',  ( -5.000000000000000000, 15.91666666666666430, -2.886751345948128211 ) ) ;
#57272 = EDGE_LOOP ( 'NONE', ( #62514, #43092, #43687, #2086 ) ) ;
#57273 = CARTESIAN_POINT ( 'NONE',  ( -4.999999999999998224, 15.20833333606451987, 2.886751345948131764 ) ) ;
#57274 = VECTOR ( 'NONE', #20913, 1000.000000000000000 ) ;
#57275 = CARTESIAN_POINT ( 'NONE',  ( 5.000000000000000888, -13.58333333333333570, 2.886751345948126879 ) ) ;
#57276 = CARTESIAN_POINT ( 'NONE',  ( 4.458734125000001214, -14.89583333196773474, 2.574251347313718519 ) ) ;
#57277 = AXIS2_PLACEMENT_3D ( 'NONE', #35638, #11184, #60413 ) ;
#57278 = CARTESIAN_POINT ( 'NONE',  ( -2.229367062500000163, -75.47916666530106511, -3.861377020970580443 ) ) ;
#57279 = AXIS2_PLACEMENT_3D ( 'NONE', #52676, #42696, #8609 ) ;
#57280 =( BOUNDED_CURVE ( )  B_SPLINE_CURVE ( 2, ( #42334, #24289, #9801, #19138, #4358, #39389, #49042, #63223, #181 ),
 .UNSPECIFIED., .F., .F. ) 
 B_SPLINE_CURVE_WITH_KNOTS ( ( 3, 2, 2, 2, 3 ),
 ( 0.6770833333333333703, 0.6777777777777778123, 0.6791666666666666963, 0.6805555555555555802, 0.6812500000000000222 ),
 .UNSPECIFIED. ) 
 CURVE ( )  GEOMETRIC_REPRESENTATION_ITEM ( )  RATIONAL_B_SPLINE_CURVE ( ( 0.9330127018922194093, 0.9330127018922194093, 1.000000000000000000, 0.8660254037844387076, 1.000000000000000000, 0.8660254037844387076, 1.000000000000000000, 0.9330127018922194093, 0.9330127018922194093 ) ) 
 REPRESENTATION_ITEM ( '' )  );
#57281 = CARTESIAN_POINT ( 'NONE',  ( 7.204675194429079505E-15, 27.74999999999999645, -5.000000000000000000 ) ) ;
#57282 = CARTESIAN_POINT ( 'NONE',  ( -2.499999999999996447, -10.70833333060214621, 4.330127018922195425 ) ) ;
#57284 = VERTEX_POINT ( 'NONE', #27004 ) ;
#57283 = CARTESIAN_POINT ( 'NONE',  ( -4.458734124999999437, -45.39583333196773651, -2.574251347313719407 ) ) ;
#57285 = CARTESIAN_POINT ( 'NONE',  ( 5.000000000000000888, -143.9375000000000000, -2.071067811865475505 ) ) ;
#57287 = ORIENTED_EDGE ( 'NONE', *, *, #9862, .T. ) ;
#57286 = CARTESIAN_POINT ( 'NONE',  ( -4.458734124999999437, 9.437500001365593860, 0.000000000000000000 ) ) ;
#57288 = CARTESIAN_POINT ( 'NONE',  ( -6.972266317189433020E-16, -81.24999999999998579, -5.000000000000000000 ) ) ;
#57289 = CARTESIAN_POINT ( 'NONE',  ( -3.535250795749689387E-16, -59.25000000000000000, -5.773502691896257311 ) ) ;
#57290 = CARTESIAN_POINT ( 'NONE',  ( 1.846868145590736310, -160.8750000013655779, 4.458734124999999437 ) ) ;
#57291 = CARTESIAN_POINT ( 'NONE',  ( -4.458734124999998549, -38.47916666530107221, 2.574251347313722516 ) ) ;
#57292 = CARTESIAN_POINT ( 'NONE',  ( 5.000000000000000000, -14.41666666666666785, -2.886751345948130876 ) ) ;
#57293 = CARTESIAN_POINT ( 'NONE',  ( -4.458734124999998549, -81.22916666530106511, 2.574251347313722516 ) ) ;
#57294 = CARTESIAN_POINT ( 'NONE',  ( -2.071067811865478170, -166.3125000000000000, 5.000000000000000000 ) ) ;
#57295 = CARTESIAN_POINT ( 'NONE',  ( -4.458734124999999437, -90.31249999863440792, 0.000000000000000000 ) ) ;
#57296 = CARTESIAN_POINT ( 'NONE',  ( -51.60603307380591787, -132.1875000013656063, -2.891590998281053704 ) ) ;
#57297 = CARTESIAN_POINT ( 'NONE',  ( -3.152548672688508926E-16, -5.812499998634404363, -5.148502694627439702 ) ) ;
#57298 = CARTESIAN_POINT ( 'NONE',  ( 4.458734125000001214, -43.14583333196773651, 2.574251347313718519 ) ) ;
#57299 = CARTESIAN_POINT ( 'NONE',  ( 5.000000000000000888, -26.58333333333333215, 2.886751345948126879 ) ) ;
#57300 = CARTESIAN_POINT ( 'NONE',  ( -4.458734124999999437, -85.56249999863439371, 0.000000000000000000 ) ) ;
#57301 = CARTESIAN_POINT ( 'NONE',  ( 5.000000000000000888, 3.416666666666665186, 2.886751345948126879 ) ) ;
#57302 = VERTEX_POINT ( 'NONE', #11879 ) ;
#57303 = CARTESIAN_POINT ( 'NONE',  ( -58.80597590150559739, -153.1250000027312126, 3.242614290531460330 ) ) ;
#57304 = CARTESIAN_POINT ( 'NONE',  ( -2.499999999999996447, -104.8333333333333286, 4.330127018922195425 ) ) ;
#57306 = EDGE_CURVE ( 'NONE', #45731, #14852, #36655, .T. ) ;
#57305 = CARTESIAN_POINT ( 'NONE',  ( -2.229367062499996610, -67.39583333196773651, 3.861377020970582219 ) ) ;
#57307 = CARTESIAN_POINT ( 'NONE',  ( 4.458734124999997661, -146.7500000013656063, 1.846868145590737864 ) ) ;
#57308 = ORIENTED_EDGE ( 'NONE', *, *, #24062, .T. ) ;
#57309 = CARTESIAN_POINT ( 'NONE',  ( 5.000000000000000000, -5.416666666666666963, -2.886751345948130876 ) ) ;
#57310 = CARTESIAN_POINT ( 'NONE',  ( -2.071067811865391128, -146.8125000027312126, -5.000000000000086153 ) ) ;
#57311 = CARTESIAN_POINT ( 'NONE',  ( 9.457646018065525792E-16, -12.31249999863440259, 5.148502694627439702 ) ) ;
#57312 = CARTESIAN_POINT ( 'NONE',  ( -4.458734124999999437, 3.687500001365594748, 0.000000000000000000 ) ) ;
#57313 = CARTESIAN_POINT ( 'NONE',  ( -1.846868145590734756, -155.1250000013656063, -4.458734124999999437 ) ) ;
#57314 = VECTOR ( 'NONE', #43831, 1000.000000000000000 ) ;
#57315 = CARTESIAN_POINT ( 'NONE',  ( -3.152548672688508926E-16, 28.18750000136558853, -5.148502694627439702 ) ) ;
#57316 = ORIENTED_EDGE ( 'NONE', *, *, #31089, .T. ) ;
#57317 = CARTESIAN_POINT ( 'NONE',  ( 4.458734125000000326, -89.89583333196773651, 2.574251347313718519 ) ) ;
#57318 = CARTESIAN_POINT ( 'NONE',  ( -5.000000000000000000, -97.08333333333332860, -2.886751345948128211 ) ) ;
#57319 = CARTESIAN_POINT ( 'NONE',  ( 1.975475456537005874E-15, -62.74999999999998579, 5.000000000000000000 ) ) ;
#57320 = CARTESIAN_POINT ( 'NONE',  ( 2.229367062499998831, -7.645833331967735624, -3.861377020970580887 ) ) ;
#57321 = AXIS2_PLACEMENT_3D ( 'NONE', #39901, #20629, #48918 ) ;
#57322 = CYLINDRICAL_SURFACE ( 'NONE', #4631, 5.000000000000000000 ) ;
#57323 = CARTESIAN_POINT ( 'NONE',  ( 5.000000000000000888, -23.45833333060214443, 2.886751345948126879 ) ) ;
#57324 = EDGE_CURVE ( 'NONE', #59413, #56396, #50817, .T. ) ;
#57325 = LINE ( 'NONE', #40680, #23283 ) ;
#57326 = CARTESIAN_POINT ( 'NONE',  ( -3.535250795749689387E-16, -37.12499999726881583, -5.773502691896257311 ) ) ;
#57327 = CARTESIAN_POINT ( 'NONE',  ( 2.500000000000002220, -29.66666666666666785, 4.330127018922192761 ) ) ;
#57328 = CARTESIAN_POINT ( 'NONE',  ( -2.229367062499996610, 18.85416666803225993, 3.861377020970582219 ) ) ;
#57329 = CARTESIAN_POINT ( 'NONE',  ( -2.229367062500000163, 21.52083333469892779, -3.861377020970580443 ) ) ;
#57330 = CARTESIAN_POINT ( 'NONE',  ( -2.229367062500000163, -58.47916666530106511, -3.861377020970580443 ) ) ;
#57331 = CARTESIAN_POINT ( 'NONE',  ( -3.152548672688508926E-16, -5.812499998634404363, -5.148502694627439702 ) ) ;
#57332 = CARTESIAN_POINT ( 'NONE',  ( 0.000000000000000000, -120.0000000000000000, 0.000000000000000000 ) ) ;
#57333 = CARTESIAN_POINT ( 'NONE',  ( -4.999999999999999112, 10.08333333333333393, 2.886751345948131764 ) ) ;
#57334 = CARTESIAN_POINT ( 'NONE',  ( -3.535533905932738641, -141.5000000027311842, 3.535533905932737309 ) ) ;
#57335 = CARTESIAN_POINT ( 'NONE',  ( 0.000000000000000000, -170.0000000000000000, 0.000000000000000000 ) ) ;
#57336 = CARTESIAN_POINT ( 'NONE',  ( -4.458734124999999437, -46.39583333196774362, -2.574251347313719407 ) ) ;
#57337 = CARTESIAN_POINT ( 'NONE',  ( -2.500000000000000444, -83.04166666393547303, -4.330127018922193649 ) ) ;
#57338 = CARTESIAN_POINT ( 'NONE',  ( -59.29741812935640155, -135.8750000013655779, -2.196230717870135685 ) ) ;
#57339 = CARTESIAN_POINT ( 'NONE',  ( 1.975475456537005874E-15, -65.62499999726881583, 5.000000000000000000 ) ) ;
#57340 = DIRECTION ( 'NONE',  ( 1.000000000000000000, 0.000000000000000000, 0.000000000000000000 ) ) ;
#57341 = CARTESIAN_POINT ( 'NONE',  ( -4.458734124999997661, -91.47916666530106511, 2.574251347313722516 ) ) ;
#57342 = CARTESIAN_POINT ( 'NONE',  ( 4.458734124999999437, -155.6875000013655779, 0.000000000000000000 ) ) ;
#57343 = CARTESIAN_POINT ( 'NONE',  ( 5.000000000000000888, -31.58333333333333215, 2.886751345948126879 ) ) ;
#57344 = ORIENTED_EDGE ( 'NONE', *, *, #7133, .T. ) ;
#57345 = CARTESIAN_POINT ( 'NONE',  ( 4.458734124999999437, 16.93750000136559564, -5.460374474430324690E-16 ) ) ;
#57346 = ORIENTED_EDGE ( 'NONE', *, *, #8811, .F. ) ;
#57347 = CARTESIAN_POINT ( 'NONE',  ( 4.458734125000001214, -94.89583333196773651, 2.574251347313718519 ) ) ;
#57348 = CARTESIAN_POINT ( 'NONE',  ( -4.458734124999999437, 8.437500001365595637, 0.000000000000000000 ) ) ;
#57349 = CARTESIAN_POINT ( 'NONE',  ( -2.500000000000000444, 12.95833333606451809, -4.330127018922193649 ) ) ;
#57350 =( BOUNDED_CURVE ( )  B_SPLINE_CURVE ( 2, ( #46801, #40695, #7262, #60340, #46170, #16268, #26875, #2748, #35887 ),
 .UNSPECIFIED., .F., .F. ) 
 B_SPLINE_CURVE_WITH_KNOTS ( ( 3, 2, 2, 2, 3 ),
 ( 0.4910714285714285476, 0.4916666666666666408, 0.4928571428571428825, 0.4940476190476190688, 0.4946428571428571619 ),
 .UNSPECIFIED. ) 
 CURVE ( )  GEOMETRIC_REPRESENTATION_ITEM ( )  RATIONAL_B_SPLINE_CURVE ( ( 0.9330127018922194093, 0.9330127018922194093, 1.000000000000000000, 0.8660254037844387076, 1.000000000000000000, 0.8660254037844387076, 1.000000000000000000, 0.9330127018922194093, 0.9330127018922194093 ) ) 
 REPRESENTATION_ITEM ( '' )  );
#57351 = CARTESIAN_POINT ( 'NONE',  ( -6.972266317189433020E-16, -29.12499999726880873, -5.000000000000000000 ) ) ;
#57352 = CARTESIAN_POINT ( 'NONE',  ( -2.500000000000000444, 1.833333333333332593, -4.330127018922193649 ) ) ;
#57353 = CARTESIAN_POINT ( 'NONE',  ( 9.457646018065525792E-16, -63.06249999863440792, 5.148502694627439702 ) ) ;
#57354 = CARTESIAN_POINT ( 'NONE',  ( 5.000000000000000888, -78.58333333333334281, 2.886751345948126879 ) ) ;
#57355 = CARTESIAN_POINT ( 'NONE',  ( -4.458734124999999437, -28.31249999863440081, 0.000000000000000000 ) ) ;
#57356 = CARTESIAN_POINT ( 'NONE',  ( -2.499999999999996447, 26.29166666939785202, 4.330127018922195425 ) ) ;
#57357 = CARTESIAN_POINT ( 'NONE',  ( 2.500000000000002220, -38.66666666666667140, 4.330127018922192761 ) ) ;
#57358 = CARTESIAN_POINT ( 'NONE',  ( 2.499999999999998668, -70.20833333060214443, -4.330127018922193649 ) ) ;
#57360 = CARTESIAN_POINT ( 'NONE',  ( -2.229367062499996610, -20.39583333196774007, 3.861377020970582219 ) ) ;
#57359 = CARTESIAN_POINT ( 'NONE',  ( 1.975475456537005874E-15, -14.74999999999999822, 5.000000000000000000 ) ) ;
#57361 = CARTESIAN_POINT ( 'NONE',  ( -2.499999999999996447, 13.16666666666666607, 4.330127018922195425 ) ) ;
#57362 = CARTESIAN_POINT ( 'NONE',  ( -2.229367062500000163, -64.47916666530106511, -3.861377020970580443 ) ) ;
#57363 = CARTESIAN_POINT ( 'NONE',  ( 4.458734124999999437, -149.7500000013656063, 1.846868145590737864 ) ) ;
#57364 = CARTESIAN_POINT ( 'NONE',  ( 2.229367062500001939, -75.97916666530106511, 3.861377020970579999 ) ) ;
#57365 = AXIS2_PLACEMENT_3D ( 'NONE', #27968, #18323, #62401 ) ;
#57366 = CARTESIAN_POINT ( 'NONE',  ( -55.35523342533222291, -142.5625000013656063, 4.444560631937231499 ) ) ;
#57367 = CARTESIAN_POINT ( 'NONE',  ( -2.229367062500000163, -26.72916666530106866, -3.861377020970580443 ) ) ;
#57368 = CARTESIAN_POINT ( 'NONE',  ( 5.000000000000000000, -68.29166666393547303, -2.886751345948129988 ) ) ;
#57369 = VERTEX_POINT ( 'NONE', #31498 ) ;
#57370 = CARTESIAN_POINT ( 'NONE',  ( -6.972266317189433020E-16, -1.250000000000000000, -5.000000000000000000 ) ) ;
#57371 = ORIENTED_EDGE ( 'NONE', *, *, #63171, .T. ) ;
#57372 = CARTESIAN_POINT ( 'NONE',  ( -2.229367062499996610, -68.39583333196773651, 3.861377020970582219 ) ) ;
#57373 = CYLINDRICAL_SURFACE ( 'NONE', #50229, 5.000000000000000000 ) ;
#57374 = CARTESIAN_POINT ( 'NONE',  ( -6.972266317189433020E-16, -6.124999997268813168, -5.000000000000000000 ) ) ;
#57375 = VERTEX_POINT ( 'NONE', #56284 ) ;
#57376 =( BOUNDED_CURVE ( )  B_SPLINE_CURVE ( 2, ( #7352, #31451, #6080, #41103, #51092, #36606, #1899, #17303, #55286 ),
 .UNSPECIFIED., .F., .F. ) 
 B_SPLINE_CURVE_WITH_KNOTS ( ( 3, 2, 2, 2, 3 ),
 ( 0.4562499999999999889, 0.4569444444444444309, 0.4583333333333333148, 0.4597222222222221988, 0.4604166666666666963 ),
 .UNSPECIFIED. ) 
 CURVE ( )  GEOMETRIC_REPRESENTATION_ITEM ( )  RATIONAL_B_SPLINE_CURVE ( ( 0.9330127018922194093, 0.9330127018922194093, 1.000000000000000000, 0.8660254037844387076, 1.000000000000000000, 0.8660254037844387076, 1.000000000000000000, 0.9330127018922167448, 0.9330127018922194093 ) ) 
 REPRESENTATION_ITEM ( '' )  );
#57377 = CARTESIAN_POINT ( 'NONE',  ( 4.458734124999998549, 28.02083333469892779, -2.574251347313721627 ) ) ;
#57378 = CARTESIAN_POINT ( 'NONE',  ( -2.500000000000000444, -83.16666666666667140, -4.330127018922193649 ) ) ;
#57380 = ADVANCED_FACE ( 'NONE', ( #11250 ), #51548, .F. ) ;
#57379 = CARTESIAN_POINT ( 'NONE',  ( -2.229367062499996610, -54.39583333196773651, 3.861377020970582219 ) ) ;
#57381 = VERTEX_POINT ( 'NONE', #36337 ) ;
#57382 = VECTOR ( 'NONE', #4369, 1000.000000000000000 ) ;
#57383 = CARTESIAN_POINT ( 'NONE',  ( -51.75738570946856498, -154.7500000000000284, 3.805975901505576964 ) ) ;
#57384 = CARTESIAN_POINT ( 'NONE',  ( -2.229367062500000163, 1.520833334698927564, -3.861377020970580443 ) ) ;
#57385 = CARTESIAN_POINT ( 'NONE',  ( 4.458734125000001214, 18.10416666803225638, 2.574251347313718519 ) ) ;
#57386 = CARTESIAN_POINT ( 'NONE',  ( -57.19623071787017210, -145.3750000013656347, 4.297418129356382899 ) ) ;
#57387 = CARTESIAN_POINT ( 'NONE',  ( 1.975475456537005874E-15, -1.749999999999999334, 5.000000000000000000 ) ) ;
#57388 = CARTESIAN_POINT ( 'NONE',  ( -3.152801135295367985, -167.8125000013656063, 3.152801135295367096 ) ) ;
#57389 = VERTEX_POINT ( 'NONE', #16082 ) ;
#57390 = CARTESIAN_POINT ( 'NONE',  ( 2.229367062500001939, -74.97916666530106511, 3.861377020970579999 ) ) ;
#57391 = EDGE_CURVE ( 'NONE', #29720, #19705, #55313, .T. ) ;
#57392 = CARTESIAN_POINT ( 'NONE',  ( 0.000000000000000000, 30.00000000000000000, 0.000000000000000000 ) ) ;
#57393 = CARTESIAN_POINT ( 'NONE',  ( -3.152548672688508926E-16, 6.437500001365592972, -5.148502694627439702 ) ) ;
#57394 = CARTESIAN_POINT ( 'NONE',  ( 5.000000000000000000, -140.1250000027312126, 0.000000000000000000 ) ) ;
#57395 = CARTESIAN_POINT ( 'NONE',  ( -4.458734124999999437, -62.56249999863440792, 0.000000000000000000 ) ) ;
#57396 = CARTESIAN_POINT ( 'NONE',  ( 5.000000000000000000, -19.29166666393548013, -2.886751345948129988 ) ) ;
#57397 = EDGE_CURVE ( 'NONE', #5237, #456, #57746, .T. ) ;
#57398 = CARTESIAN_POINT ( 'NONE',  ( 1.339745962155590275, 4.294658198738519062, 5.000000000000013323 ) ) ;
#57399 = CARTESIAN_POINT ( 'NONE',  ( 1.339745962155615144, -28.58034179853029144, 4.999999999999999112 ) ) ;
#57400 = CARTESIAN_POINT ( 'NONE',  ( -51.75738570946856498, -140.7500000000000000, 3.805975901505576964 ) ) ;
#57401 = CARTESIAN_POINT ( 'NONE',  ( -2.500000000000000444, -84.04166666393547303, -4.330127018922193649 ) ) ;
#57402 = FACE_OUTER_BOUND ( 'NONE', #47084, .T. ) ;
#57403 = CARTESIAN_POINT ( 'NONE',  ( -2.229367062499996610, -39.14583333196773651, 3.861377020970582219 ) ) ;
#57404 = CARTESIAN_POINT ( 'NONE',  ( 4.458734124999998549, -26.97916666530107221, -2.574251347313721627 ) ) ;
#57405 = VECTOR ( 'NONE', #42057, 1000.000000000000000 ) ;
#57406 = CARTESIAN_POINT ( 'NONE',  ( 5.275681513340003914E-14, 11.74999999999999645, -5.000000000000000000 ) ) ;
#57407 = CARTESIAN_POINT ( 'NONE',  ( -4.458734124999998549, -108.2291666653010651, 2.574251347313722516 ) ) ;
#57408 = CARTESIAN_POINT ( 'NONE',  ( -5.000000000000000888, -152.6875000027311842, -2.071067811865475949 ) ) ;
#57409 = EDGE_LOOP ( 'NONE', ( #50157, #28090, #38372, #41363 ) ) ;
#57410 = CARTESIAN_POINT ( 'NONE',  ( 4.458734125000001214, -106.1458333319677365, 2.574251347313718519 ) ) ;
#57411 = CARTESIAN_POINT ( 'NONE',  ( -3.152548672688508926E-16, -34.56249999863440792, -5.148502694627439702 ) ) ;
#57412 = CARTESIAN_POINT ( 'NONE',  ( -5.000000000000000000, -69.95833333060214443, -2.886751345948128211 ) ) ;
#57413 = CARTESIAN_POINT ( 'NONE',  ( -57.19623071787017210, -147.6250000013655779, 4.297418129356382899 ) ) ;
#57414 = CARTESIAN_POINT ( 'NONE',  ( -9.184850993605147944E-16, -146.2500000000000284, 5.000000000000000000 ) ) ;
#57415 = CARTESIAN_POINT ( 'NONE',  ( 4.458734125000000326, -28.89583333196774007, 2.574251347313718519 ) ) ;
#57416 = CARTESIAN_POINT ( 'NONE',  ( -2.229367062499996610, -71.39583333196773651, 3.861377020970582219 ) ) ;
#57417 = CARTESIAN_POINT ( 'NONE',  ( 1.846868145590736310, -167.8750000013656063, 4.458734124999997661 ) ) ;
#57418 = CARTESIAN_POINT ( 'NONE',  ( 4.458734124999998549, -27.72916666530107221, -2.574251347313721627 ) ) ;
#57419 = FACE_OUTER_BOUND ( 'NONE', #55443, .T. ) ;
#57420 = CARTESIAN_POINT ( 'NONE',  ( 2.499999999999998668, 22.79166666939785202, -4.330127018922193649 ) ) ;
#57421 = CARTESIAN_POINT ( 'NONE',  ( 5.000000000000000888, -18.58333333333333215, 2.886751345948126879 ) ) ;
#57422 = CARTESIAN_POINT ( 'NONE',  ( 1.846868145590736310, -148.6250000013655779, 4.458734124999999437 ) ) ;
#57423 = VERTEX_POINT ( 'NONE', #43052 ) ;
#57424 = CARTESIAN_POINT ( 'NONE',  ( -6.972266317189433020E-16, -0.2500000000000001665, -5.000000000000000000 ) ) ;
#57425 = CARTESIAN_POINT ( 'NONE',  ( 9.457646018065525792E-16, -58.31249999863440792, 5.148502694627439702 ) ) ;
#57426 = CARTESIAN_POINT ( 'NONE',  ( -5.000000000000000000, 29.04166666939784847, -2.886751345948128211 ) ) ;
#57427 = CARTESIAN_POINT ( 'NONE',  ( 1.975475456537005874E-15, -0.7499999999999996669, 5.000000000000000000 ) ) ;
#57428 = CARTESIAN_POINT ( 'NONE',  ( 1.060575238724906964E-15, 24.24999999999999645, 5.773502691896257311 ) ) ;
#57429 = ADVANCED_FACE ( 'NONE', ( #3829 ), #32777, .T. ) ;
#57430 = CARTESIAN_POINT ( 'NONE',  ( 1.975475456537005874E-15, -88.74999999999998579, 5.000000000000000000 ) ) ;
#57431 = CARTESIAN_POINT ( 'NONE',  ( 4.458734124999998549, 0.2708333346989263979, -2.574251347313721627 ) ) ;
#57432 = LINE ( 'NONE', #13352, #29775 ) ;
#57433 = CARTESIAN_POINT ( 'NONE',  ( -9.184850993605147944E-16, -141.2500000000000284, 5.000000000000000000 ) ) ;
#57434 = CARTESIAN_POINT ( 'NONE',  ( -4.458734124999998549, 10.52083333469892779, 2.574251347313722516 ) ) ;
#57435 = ORIENTED_EDGE ( 'NONE', *, *, #26376, .T. ) ;
#57436 = CARTESIAN_POINT ( 'NONE',  ( 5.000000000000000000, -42.49999999999999289, -6.123233995736766282E-16 ) ) ;
#57437 = ORIENTED_EDGE ( 'NONE', *, *, #60578, .F. ) ;
#57438 = CARTESIAN_POINT ( 'NONE',  ( -9.184850993605147944E-16, -168.3750000027312126, 5.000000000000000000 ) ) ;
#57439 = CARTESIAN_POINT ( 'NONE',  ( 4.458734125000001214, -47.89583333196775072, 2.574251347313718519 ) ) ;
#57440 = CARTESIAN_POINT ( 'NONE',  ( -4.458734124999999437, -158.1875000013655779, -5.460374474430324690E-16 ) ) ;
#57441 = CARTESIAN_POINT ( 'NONE',  ( -2.500000000000000444, -49.04166666393547303, -4.330127018922193649 ) ) ;
#57442 = VERTEX_POINT ( 'NONE', #18917 ) ;
#57443 = CARTESIAN_POINT ( 'NONE',  ( 4.458734124999998549, -24.72916666530106866, -2.574251347313721627 ) ) ;
#57444 = EDGE_LOOP ( 'NONE', ( #34644, #31620, #52515, #17717 ) ) ;
#57446 = DIRECTION ( 'NONE',  ( 0.000000000000000000, 1.000000000000000000, 0.000000000000000000 ) ) ;
#57445 = LINE ( 'NONE', #18510, #4993 ) ;
#57447 = CARTESIAN_POINT ( 'NONE',  ( 3.152801135295367541, -161.3125000013656063, -3.152801135295367541 ) ) ;
#57448 = CARTESIAN_POINT ( 'NONE',  ( 0.000000000000000000, -120.0000000000000000, 0.000000000000000000 ) ) ;
#57449 = CARTESIAN_POINT ( 'NONE',  ( -50.18089887299979068, -136.6875000000000284, 2.462841084822635640 ) ) ;
#57450 = AXIS2_PLACEMENT_3D ( 'NONE', #34810, #5539, #21289 ) ;
#57451 = CARTESIAN_POINT ( 'NONE',  ( -2.229367062499996610, -37.39583333196773651, 3.861377020970582219 ) ) ;
#57452 = ORIENTED_EDGE ( 'NONE', *, *, #12202, .F. ) ;
#57453 =( BOUNDED_CURVE ( )  B_SPLINE_CURVE ( 2, ( #48106, #22737, #13388, #62608, #37516, #14006, #18531, #2801, #28801 ),
 .UNSPECIFIED., .F., .F. ) 
 B_SPLINE_CURVE_WITH_KNOTS ( ( 3, 2, 2, 2, 3 ),
 ( 0.9479166666666666297, 0.9486111111111110716, 0.9499999999999999556, 0.9513888888888888395, 0.9520833333333332815 ),
 .UNSPECIFIED. ) 
 CURVE ( )  GEOMETRIC_REPRESENTATION_ITEM ( )  RATIONAL_B_SPLINE_CURVE ( ( 0.9330127018922194093, 0.9330127018922194093, 1.000000000000000000, 0.8660254037844387076, 1.000000000000000000, 0.8660254037844387076, 1.000000000000000000, 0.9330127018922194093, 0.9330127018922194093 ) ) 
 REPRESENTATION_ITEM ( '' )  );
#57454 = EDGE_CURVE ( 'NONE', #61001, #23800, #20736, .T. ) ;
#57455 = EDGE_CURVE ( 'NONE', #5237, #26195, #13479, .T. ) ;
#57456 = CARTESIAN_POINT ( 'NONE',  ( -4.458734124999998549, -80.22916666530106511, 2.574251347313722516 ) ) ;
#57457 = CARTESIAN_POINT ( 'NONE',  ( 2.229367062500001939, 23.02083333469892423, 3.861377020970579999 ) ) ;
#57458 = CARTESIAN_POINT ( 'NONE',  ( 1.975475456537005874E-15, 11.24999999999999822, 5.000000000000000000 ) ) ;
#57459 = EDGE_CURVE ( 'NONE', #59581, #5972, #61889, .T. ) ;
#57460 = ORIENTED_EDGE ( 'NONE', *, *, #7152, .T. ) ;
#57461 = CARTESIAN_POINT ( 'NONE',  ( 5.000000000000000000, 14.58333333333333215, -2.886751345948130876 ) ) ;
#57462 = CARTESIAN_POINT ( 'NONE',  ( -50.70258187064364108, -139.3750000013656063, 2.196230717870141014 ) ) ;
#57463 = CARTESIAN_POINT ( 'NONE',  ( 9.457646018065525792E-16, -85.31249999863439371, 5.148502694627439702 ) ) ;
#57464 = CARTESIAN_POINT ( 'NONE',  ( -59.98410592259440222, -130.2500000027312126, -0.3983568153799752487 ) ) ;
#57465 = FACE_OUTER_BOUND ( 'NONE', #50661, .T. ) ;
#57466 = CARTESIAN_POINT ( 'NONE',  ( 0.000000000000000000, -120.0000000000000000, 0.000000000000000000 ) ) ;
#57467 = CARTESIAN_POINT ( 'NONE',  ( -6.972266317189433020E-16, -57.25000000000000000, -5.000000000000000000 ) ) ;
#57468 = CARTESIAN_POINT ( 'NONE',  ( -4.458734124999999437, -56.39583333196773651, -2.574251347313719407 ) ) ;
#57469 = DIRECTION ( 'NONE',  ( -0.000000000000000000, 1.000000000000000000, -0.000000000000000000 ) ) ;
#57470 = CARTESIAN_POINT ( 'NONE',  ( 2.229367062499998831, 21.35416666803226349, -3.861377020970580887 ) ) ;
#57471 = ADVANCED_FACE ( 'NONE', ( #51770 ), #2894, .T. ) ;
#57472 = PLANE ( 'NONE',  #62505 ) ;
#57473 =( BOUNDED_CURVE ( )  B_SPLINE_CURVE ( 2, ( #58882, #16024, #43764, #25995, #48910, #60740, #35971, #44401, #38941 ),
 .UNSPECIFIED., .F., .F. ) 
 B_SPLINE_CURVE_WITH_KNOTS ( ( 3, 2, 2, 2, 3 ),
 ( 0.5062499999999999778, 0.5069444444444444198, 0.5083333333333333037, 0.5097222222222221877, 0.5104166666666666297 ),
 .UNSPECIFIED. ) 
 CURVE ( )  GEOMETRIC_REPRESENTATION_ITEM ( )  RATIONAL_B_SPLINE_CURVE ( ( 0.9330127018922194093, 0.9330127018922194093, 1.000000000000000000, 0.8660254037844387076, 1.000000000000000000, 0.8660254037844387076, 1.000000000000000000, 0.9330127018922194093, 0.9330127018922194093 ) ) 
 REPRESENTATION_ITEM ( '' )  );
#57474 = CARTESIAN_POINT ( 'NONE',  ( 1.975475456537005874E-15, -23.75000000000000000, 5.000000000000000000 ) ) ;
#57475 = CARTESIAN_POINT ( 'NONE',  ( 2.229367062500001939, -43.22916666530107932, 3.861377020970579999 ) ) ;
#57476 = CARTESIAN_POINT ( 'NONE',  ( 2.499999999999998668, -6.208333330602149758, -4.330127018922193649 ) ) ;
#57477 = LINE ( 'NONE', #38763, #53034 ) ;
#57478 = EDGE_CURVE ( 'NONE', #47300, #23480, #51180, .T. ) ;
#57479 = FACE_OUTER_BOUND ( 'NONE', #4917, .T. ) ;
#57480 = CARTESIAN_POINT ( 'NONE',  ( 9.457646018065525792E-16, -86.31249999863440792, 5.148502694627439702 ) ) ;
#57481 = CARTESIAN_POINT ( 'NONE',  ( -3.152548672688508926E-16, -103.5624999986344079, -5.148502694627439702 ) ) ;
#57482 = CARTESIAN_POINT ( 'NONE',  ( 2.229367062500001939, -5.229166665301071326, 3.861377020970579999 ) ) ;
#57483 = ORIENTED_EDGE ( 'NONE', *, *, #26107, .T. ) ;
#57484 = CARTESIAN_POINT ( 'NONE',  ( 2.499999999999998668, -9.208333330602146205, -4.330127018922193649 ) ) ;
#57485 = CARTESIAN_POINT ( 'NONE',  ( -4.458734124999999437, -92.31249999863440792, 0.000000000000000000 ) ) ;
#57486 = ADVANCED_FACE ( 'NONE', ( #61747 ), #37289, .T. ) ;
#57487 = CARTESIAN_POINT ( 'NONE',  ( -2.071067811865475061, -166.8125000027312126, -5.000000000000000888 ) ) ;
#57488 = CARTESIAN_POINT ( 'NONE',  ( 9.457646018065525792E-16, -91.31249999863440792, 5.148502694627439702 ) ) ;
#57489 = CARTESIAN_POINT ( 'NONE',  ( -55.00000000000002132, -155.0000000000000284, 1.734723475976807094E-15 ) ) ;
#57490 = CARTESIAN_POINT ( 'NONE',  ( -50.40829686548195099, -130.0000000013656063, -1.485763867205728284 ) ) ;
#57491 = CARTESIAN_POINT ( 'NONE',  ( -3.152548672688508926E-16, -14.56249999863440259, -5.148502694627439702 ) ) ;
#57492 = CARTESIAN_POINT ( 'NONE',  ( 4.458734124999998549, 12.02083333469892601, -2.574251347313721627 ) ) ;
#57493 = CARTESIAN_POINT ( 'NONE',  ( -4.458734124999997661, -51.47916666530107932, 2.574251347313722516 ) ) ;
#57494 = CARTESIAN_POINT ( 'NONE',  ( 5.000000000000000888, -86.45833333060213022, 2.886751345948126879 ) ) ;
#57495 = CARTESIAN_POINT ( 'NONE',  ( -6.972266317189433020E-16, -106.2500000000000000, -5.000000000000000000 ) ) ;
#57496 = CARTESIAN_POINT ( 'NONE',  ( -4.458734124999999437, -11.31249999863440792, 0.000000000000000000 ) ) ;
#57497 = CARTESIAN_POINT ( 'NONE',  ( -6.972266317189433020E-16, -106.1249999972688016, -5.000000000000000000 ) ) ;
#57498 = ORIENTED_EDGE ( 'NONE', *, *, #33158, .F. ) ;
#57499 = CARTESIAN_POINT ( 'NONE',  ( 4.458734124999998549, -38.97916666530107221, -2.574251347313721627 ) ) ;
#57500 = COLOUR_RGB ( '',1.000000000000000000, 0.9490196078431372140, 0.9098039215686274384 ) ;
#57501 = UNCERTAINTY_MEASURE_WITH_UNIT (LENGTH_MEASURE( 1.000000000000000082E-05 ), #53783, 'distance_accuracy_value', 'NONE');
#57502 = CARTESIAN_POINT ( 'NONE',  ( 1.975475456537005874E-15, -77.75000000000000000, 5.000000000000000000 ) ) ;
#57503 = DIRECTION ( 'NONE',  ( -0.000000000000000000, 1.000000000000000000, -0.000000000000000000 ) ) ;
#57504 = CARTESIAN_POINT ( 'NONE',  ( -5.000000000000000000, -27.99999999999999645, 0.000000000000000000 ) ) ;
#57505 = CARTESIAN_POINT ( 'NONE',  ( -4.458734124999999437, -80.31249999863440792, 0.000000000000000000 ) ) ;
#57506 = CARTESIAN_POINT ( 'NONE',  ( 2.229367062500001939, 23.77083333469892779, 3.861377020970579999 ) ) ;
#57507 = CARTESIAN_POINT ( 'NONE',  ( 4.458734125000001214, 15.10416666803225993, 2.574251347313718519 ) ) ;
#57508 = CARTESIAN_POINT ( 'NONE',  ( -2.500000000000000444, 6.833333333333333925, -4.330127018922193649 ) ) ;
#57509 = DIRECTION ( 'NONE',  ( -0.000000000000000000, 1.000000000000000000, -0.000000000000000000 ) ) ;
#57510 = CARTESIAN_POINT ( 'NONE',  ( 4.458734124999999437, -81.06249999863440792, -5.460374474430324690E-16 ) ) ;
#57511 = CARTESIAN_POINT ( 'NONE',  ( -2.499999999999996447, -67.83333333333332860, 4.330127018922195425 ) ) ;
#57512 = CARTESIAN_POINT ( 'NONE',  ( 5.000000000000000000, 13.62500000273118417, -6.123233995736766282E-16 ) ) ;
#57513 = ORIENTED_EDGE ( 'NONE', *, *, #37432, .F. ) ;
#57514 = CARTESIAN_POINT ( 'NONE',  ( -1.339745962155610925, -61.66965819600733312, 5.000000000000000000 ) ) ;
#57516 = CARTESIAN_POINT ( 'NONE',  ( 5.000000000000000888, -29.58333333333332504, 2.886751345948126879 ) ) ;
#57515 = CARTESIAN_POINT ( 'NONE',  ( 5.000000000000000000, -40.41666666666667140, -2.886751345948130876 ) ) ;
#57517 = CARTESIAN_POINT ( 'NONE',  ( 4.458734125000001214, -34.89583333196772941, 2.574251347313718519 ) ) ;
#57518 = FACE_OUTER_BOUND ( 'NONE', #61732, .T. ) ;
#57519 = CARTESIAN_POINT ( 'NONE',  ( -5.000000000000000000, -28.95833333060215153, -2.886751345948128211 ) ) ;
#57521 = ORIENTED_EDGE ( 'NONE', *, *, #9495, .T. ) ;
#57520 = CARTESIAN_POINT ( 'NONE',  ( 9.457646018065525792E-16, -60.06249999863440792, 5.148502694627439702 ) ) ;
#57523 = ORIENTED_EDGE ( 'NONE', *, *, #5455, .F. ) ;
#57522 = CARTESIAN_POINT ( 'NONE',  ( -4.458734124999999437, -8.562499998634406140, 0.000000000000000000 ) ) ;
#57524 = CARTESIAN_POINT ( 'NONE',  ( -3.535250795749689387E-16, -76.24999999999998579, -5.773502691896257311 ) ) ;
#57525 = DIRECTION ( 'NONE',  ( -1.000000000000000000, 0.000000000000000000, 0.000000000000000000 ) ) ;
#57526 = CARTESIAN_POINT ( 'NONE',  ( 4.458734125000001214, -54.14583333196773651, 2.574251347313718519 ) ) ;
#57527 =( BOUNDED_CURVE ( )  B_SPLINE_CURVE ( 2, ( #61702, #57195, #56875, #22141, #17631 ),
 .UNSPECIFIED., .F., .F. ) 
 B_SPLINE_CURVE_WITH_KNOTS ( ( 3, 2, 3 ),
 ( 0.000000000000000000, 0.001190476190476190584, 0.001785714285714286092 ),
 .UNSPECIFIED. ) 
 CURVE ( )  GEOMETRIC_REPRESENTATION_ITEM ( )  RATIONAL_B_SPLINE_CURVE ( ( 1.000000000000000000, 0.8660254037844387076, 1.000000000000000000, 0.9330127018922192983, 0.9330127018922194093 ) ) 
 REPRESENTATION_ITEM ( '' )  );
#57528 = CARTESIAN_POINT ( 'NONE',  ( -5.000000000000000000, -78.87499999726881583, 0.000000000000000000 ) ) ;
#57530 = EDGE_LOOP ( 'NONE', ( #50880, #11421, #5366, #19277 ) ) ;
#57529 = CARTESIAN_POINT ( 'NONE',  ( -4.999999999999998224, -54.79166666393548013, 2.886751345948131764 ) ) ;
#57531 = CARTESIAN_POINT ( 'NONE',  ( -55.39835681537999790, -147.8750000000000284, 4.984105922594378235 ) ) ;
#57532 = CARTESIAN_POINT ( 'NONE',  ( 2.229367062500001939, -20.22916666530107221, 3.861377020970579999 ) ) ;
#57534 = VERTEX_POINT ( 'NONE', #52088 ) ;
#57533 = CARTESIAN_POINT ( 'NONE',  ( 2.229367062500001939, -56.22916666530107221, 3.861377020970579999 ) ) ;
#57535 = ADVANCED_FACE ( 'NONE', ( #8026 ), #42416, .T. ) ;
#57536 = CARTESIAN_POINT ( 'NONE',  ( 4.458734124999999437, -166.7500000013655779, 1.846868145590737864 ) ) ;
#57537 = CARTESIAN_POINT ( 'NONE',  ( -4.458734124999999437, -97.56249999863440792, 0.000000000000000000 ) ) ;
#57538 = CARTESIAN_POINT ( 'NONE',  ( 2.499999999999998668, -50.20833333060213732, -4.330127018922193649 ) ) ;
#57539 = EDGE_LOOP ( 'NONE', ( #3500, #36868, #23200, #12511 ) ) ;
#57540 = CARTESIAN_POINT ( 'NONE',  ( -59.44456063193725015, -149.8125000013656063, -0.3552334253322034230 ) ) ;
#57541 = CARTESIAN_POINT ( 'NONE',  ( -58.24261429053147765, -143.3750000027312126, -3.805975901505573855 ) ) ;
#57542 = CARTESIAN_POINT ( 'NONE',  ( -6.972266317189433020E-16, -83.24999999999998579, -5.000000000000000000 ) ) ;
#57543 = CARTESIAN_POINT ( 'NONE',  ( -4.458734124999998549, -7.229166665301073103, 2.574251347313722516 ) ) ;
#57544 = CARTESIAN_POINT ( 'NONE',  ( -2.229367062499996610, -103.3958333319677365, 3.861377020970582219 ) ) ;
#57545 = CARTESIAN_POINT ( 'NONE',  ( -4.458734125000000326, -145.2500000013655779, -1.846868145590735644 ) ) ;
#57546 = CARTESIAN_POINT ( 'NONE',  ( 4.458734124999999437, -26.06249999863440792, -5.460374474430324690E-16 ) ) ;
#57547 = CARTESIAN_POINT ( 'NONE',  ( 1.975475456537005874E-15, -55.62499999726880873, 5.000000000000000000 ) ) ;
#57548 = CARTESIAN_POINT ( 'NONE',  ( -50.55543936806279248, -135.0625000013656063, 0.3552334253322060320 ) ) ;
#57549 = CARTESIAN_POINT ( 'NONE',  ( 9.457646018065525792E-16, -70.31249999863439371, 5.148502694627439702 ) ) ;
#57550 = EDGE_CURVE ( 'NONE', #40253, #57381, #2708, .T. ) ;
#57551 = CARTESIAN_POINT ( 'NONE',  ( 5.000000000000000888, -43.58333333333333570, 2.886751345948126879 ) ) ;
#57552 = EDGE_CURVE ( 'NONE', #57658, #55786, #34341, .T. ) ;
#57553 = CARTESIAN_POINT ( 'NONE',  ( -1.339745962155610925, -33.79465819873851729, 5.000000000000000000 ) ) ;
#57554 = CARTESIAN_POINT ( 'NONE',  ( -8.190561711645485556E-16, -142.6875000013656063, 4.458734124999999437 ) ) ;
#57555 = CARTESIAN_POINT ( 'NONE',  ( 4.458734124999999437, 11.93750000136559564, -5.460374474430324690E-16 ) ) ;
#57556 = ORIENTED_EDGE ( 'NONE', *, *, #33015, .T. ) ;
#57557 = CARTESIAN_POINT ( 'NONE',  ( -5.000000000000000000, -49.95833333060213022, -2.886751345948128211 ) ) ;
#57558 = EDGE_CURVE ( 'NONE', #28144, #4881, #20524, .T. ) ;
#57559 = CARTESIAN_POINT ( 'NONE',  ( 3.535533905932736864, -160.1250000000000284, 3.535533905932738641 ) ) ;
#57561 = CARTESIAN_POINT ( 'NONE',  ( -3.152548672688508926E-16, -22.56249999863440081, -5.148502694627439702 ) ) ;
#57560 = CARTESIAN_POINT ( 'NONE',  ( -3.535250795749689387E-16, -92.25000000000001421, -5.773502691896257311 ) ) ;
#57562 = CARTESIAN_POINT ( 'NONE',  ( -6.972266317189433020E-16, -54.12499999726880162, -5.000000000000000000 ) ) ;
#57563 = CARTESIAN_POINT ( 'NONE',  ( -2.229367062499996610, -74.39583333196773651, 3.861377020970582219 ) ) ;
#57564 = CARTESIAN_POINT ( 'NONE',  ( -4.458734124999999437, 22.43750000136559564, 0.000000000000000000 ) ) ;
#57565 = CARTESIAN_POINT ( 'NONE',  ( 2.500000000000002220, -79.54166666393547303, 4.330127018922192761 ) ) ;
#57566 = CARTESIAN_POINT ( 'NONE',  ( -52.10840900171896806, -142.1875000013656063, 3.393966926194110556 ) ) ;
#57567 = EDGE_CURVE ( 'NONE', #7190, #15348, #40063, .T. ) ;
#57568 = CARTESIAN_POINT ( 'NONE',  ( 2.229367062500001939, 4.020833334698926009, 3.861377020970579999 ) ) ;
#57569 = CARTESIAN_POINT ( 'NONE',  ( 9.457646018065525792E-16, 26.68750000136559564, 5.148502694627439702 ) ) ;
#57570 = CARTESIAN_POINT ( 'NONE',  ( 2.229367062499998831, -38.89583333196773651, -3.861377020970580887 ) ) ;
#57571 = CARTESIAN_POINT ( 'NONE',  ( -4.458734124999997661, 4.770833334698926009, 2.574251347313722516 ) ) ;
#57572 = CARTESIAN_POINT ( 'NONE',  ( 4.458734125000001214, -71.89583333196773651, 2.574251347313718519 ) ) ;
#57573 = CARTESIAN_POINT ( 'NONE',  ( 9.457646018065525792E-16, -19.31249999863440792, 5.148502694627439702 ) ) ;
#57574 =( BOUNDED_CURVE ( )  B_SPLINE_CURVE ( 2, ( #51010, #7901, #56798, #26563, #46182, #27506, #3082, #21747, #42299 ),
 .UNSPECIFIED., .F., .F. ) 
 B_SPLINE_CURVE_WITH_KNOTS ( ( 3, 2, 2, 2, 3 ),
 ( 0.03035714285714285685, 0.03095238095238095344, 0.03214285714285713969, 0.03333333333333333287, 0.03392857142857143293 ),
 .UNSPECIFIED. ) 
 CURVE ( )  GEOMETRIC_REPRESENTATION_ITEM ( )  RATIONAL_B_SPLINE_CURVE ( ( 0.9330127018922194093, 0.9330127018922194093, 1.000000000000000000, 0.8660254037844387076, 1.000000000000000000, 0.8660254037844387076, 1.000000000000000000, 0.9330127018922189652, 0.9330127018922194093 ) ) 
 REPRESENTATION_ITEM ( '' )  );
#57575 = CARTESIAN_POINT ( 'NONE',  ( 5.000000000000000000, -8.500000000000000000, -6.123233995736766282E-16 ) ) ;
#57576 = CARTESIAN_POINT ( 'NONE',  ( 4.458734124999999437, -154.5000000013656347, 1.846868145590737864 ) ) ;
#57577 = LINE ( 'NONE', #61454, #50041 ) ;
#57578 = CARTESIAN_POINT ( 'NONE',  ( 2.229367062499998831, -64.64583333196773651, -3.861377020970580887 ) ) ;
#57579 = CARTESIAN_POINT ( 'NONE',  ( -5.000000000000000000, -98.95833333060213022, -2.886751345948128211 ) ) ;
#57580 = CARTESIAN_POINT ( 'NONE',  ( 4.458734125000001214, 29.10416666803225993, 2.574251347313718519 ) ) ;
#57581 = CARTESIAN_POINT ( 'NONE',  ( -2.229367062499996610, -39.14583333196773651, 3.861377020970582219 ) ) ;
#57582 = LINE ( 'NONE', #9293, #22564 ) ;
#57583 = CARTESIAN_POINT ( 'NONE',  ( 2.229367062499998831, -103.8958333319677365, -3.861377020970580887 ) ) ;
#57584 = CARTESIAN_POINT ( 'NONE',  ( 9.457646018065525792E-16, -67.31249999863440792, 5.148502694627439702 ) ) ;
#57585 = CARTESIAN_POINT ( 'NONE',  ( -3.535250795749689387E-16, -55.24999999999998579, -5.773502691896257311 ) ) ;
#57586 = CARTESIAN_POINT ( 'NONE',  ( 1.062108568985190270E-13, -13.12499999726881583, -4.999999999999999112 ) ) ;
#57587 = DIRECTION ( 'NONE',  ( -0.000000000000000000, 1.000000000000000000, -0.000000000000000000 ) ) ;
#57588 = ORIENTED_EDGE ( 'NONE', *, *, #28767, .F. ) ;
#57589 = LINE ( 'NONE', #57891, #22242 ) ;
#57590 = CARTESIAN_POINT ( 'NONE',  ( 2.500000000000002220, 2.458333336064519870, 4.330127018922192761 ) ) ;
#57591 = CARTESIAN_POINT ( 'NONE',  ( 5.000000000000000888, -14.58333333333333037, 2.886751345948126879 ) ) ;
#57592 = CARTESIAN_POINT ( 'NONE',  ( -4.458734124999999437, -14.31249999863440436, 0.000000000000000000 ) ) ;
#57593 = CARTESIAN_POINT ( 'NONE',  ( 9.457646018065525792E-16, -78.06249999863440792, 5.148502694627439702 ) ) ;
#57594 = CARTESIAN_POINT ( 'NONE',  ( -5.000000000000000000, -4.874999997268810503, 0.000000000000000000 ) ) ;
#57595 = CARTESIAN_POINT ( 'NONE',  ( -4.999999999999999112, -12.79166666393547835, 2.886751345948131764 ) ) ;
#57597 = VERTEX_POINT ( 'NONE', #44307 ) ;
#57596 = CARTESIAN_POINT ( 'NONE',  ( 4.458734125000001214, -43.89583333196775072, 2.574251347313718519 ) ) ;
#57598 = CARTESIAN_POINT ( 'NONE',  ( -1.339745962155613368, 29.79465819873851729, -5.000000000000000000 ) ) ;
#57600 = ORIENTED_EDGE ( 'NONE', *, *, #52232, .F. ) ;
#57599 = CARTESIAN_POINT ( 'NONE',  ( -2.229367062499996610, 9.604166668032261711, 3.861377020970582219 ) ) ;
#57601 = CARTESIAN_POINT ( 'NONE',  ( -55.35523342533222291, -154.3125000013656347, 4.444560631937231499 ) ) ;
#57602 = CARTESIAN_POINT ( 'NONE',  ( -2.499999999999996447, -58.83333333333333570, 4.330127018922195425 ) ) ;
#57603 = CARTESIAN_POINT ( 'NONE',  ( 1.846868145590736310, -157.8750000013656063, 4.458734124999999437 ) ) ;
#57604 = CARTESIAN_POINT ( 'NONE',  ( -2.229367062500000163, -37.72916666530107221, -3.861377020970580443 ) ) ;
#57605 = CARTESIAN_POINT ( 'NONE',  ( -6.972266317189433020E-16, -65.24999999999998579, -5.000000000000000000 ) ) ;
#57606 = CARTESIAN_POINT ( 'NONE',  ( 3.535533905932738197, -165.8750000000000284, -3.535533905932738197 ) ) ;
#57607 = CARTESIAN_POINT ( 'NONE',  ( 5.000000000000000000, -11.41666666666666607, -2.886751345948130876 ) ) ;
#57608 = CARTESIAN_POINT ( 'NONE',  ( -57.19623071787017210, -131.6250000013655779, 4.297418129356382899 ) ) ;
#57609 = CARTESIAN_POINT ( 'NONE',  ( -2.229367062499996610, -4.395833331967740065, 3.861377020970582219 ) ) ;
#57610 = CARTESIAN_POINT ( 'NONE',  ( -2.229367062500000163, -40.72916666530107221, -3.861377020970580443 ) ) ;
#57611 = CARTESIAN_POINT ( 'NONE',  ( 2.500000000000002220, -67.54166666393547303, 4.330127018922192761 ) ) ;
#57612 = CARTESIAN_POINT ( 'NONE',  ( -4.458734125000000326, -152.0000000013655779, -1.846868145590735644 ) ) ;
#57613 = CARTESIAN_POINT ( 'NONE',  ( -2.229367062499996610, -86.39583333196773651, 3.861377020970582219 ) ) ;
#57614 = CARTESIAN_POINT ( 'NONE',  ( -9.184850993605147944E-16, -167.3750000027312126, 5.000000000000000000 ) ) ;
#57615 = ORIENTED_EDGE ( 'NONE', *, *, #47661, .F. ) ;
#57616 = CARTESIAN_POINT ( 'NONE',  ( -5.000000000000000888, -148.5625000027311842, 2.071067811865474617 ) ) ;
#57617 = CARTESIAN_POINT ( 'NONE',  ( -7.922281120364393914, 4.573931137438271399, -8.047472243342930653 ) ) ;
#57618 = CARTESIAN_POINT ( 'NONE',  ( 2.229367062499998831, -69.89583333196773651, -3.861377020970580887 ) ) ;
#57619 = CARTESIAN_POINT ( 'NONE',  ( 2.730187237215162345E-16, -147.4375000013656063, -4.458734124999999437 ) ) ;
#57620 = ORIENTED_EDGE ( 'NONE', *, *, #2512, .T. ) ;
#57621 = CARTESIAN_POINT ( 'NONE',  ( -6.972266317189433020E-16, -14.24999999999999822, -5.000000000000000000 ) ) ;
#57622 = CARTESIAN_POINT ( 'NONE',  ( -4.458734124999998549, -13.47916666530107221, 2.574251347313722516 ) ) ;
#57623 = CARTESIAN_POINT ( 'NONE',  ( 1.339745962155612702, -105.1696581960073331, -5.000000000000000000 ) ) ;
#57624 = CARTESIAN_POINT ( 'NONE',  ( -2.229367062499996610, -0.1458333319677394824, 3.861377020970582219 ) ) ;
#57625 = CARTESIAN_POINT ( 'NONE',  ( 1.975475456537005874E-15, -79.74999999999998579, 5.000000000000000000 ) ) ;
#57626 = CARTESIAN_POINT ( 'NONE',  ( -8.190561711645485556E-16, -151.6875000013656063, 4.458734124999999437 ) ) ;
#57627 = CARTESIAN_POINT ( 'NONE',  ( -4.458734124999999437, 26.43750000136559564, 0.000000000000000000 ) ) ;
#57628 = VERTEX_POINT ( 'NONE', #54611 ) ;
#57629 = CARTESIAN_POINT ( 'NONE',  ( 4.458734124999998549, -90.72916666530106511, -2.574251347313721627 ) ) ;
#57630 = DIRECTION ( 'NONE',  ( 0.000000000000000000, 0.000000000000000000, 1.000000000000000000 ) ) ;
#57631 = CARTESIAN_POINT ( 'NONE',  ( 1.975475456537005874E-15, 7.375000002731186832, 5.000000000000000000 ) ) ;
#57632 = CARTESIAN_POINT ( 'NONE',  ( -2.229367062500000163, -9.479166665301068662, -3.861377020970580443 ) ) ;
#57633 = VECTOR ( 'NONE', #9070, 1000.000000000000000 ) ;
#57634 = DIRECTION ( 'NONE',  ( -0.000000000000000000, 1.000000000000000000, -0.000000000000000000 ) ) ;
#57635 = DIRECTION ( 'NONE',  ( -0.000000000000000000, 1.000000000000000000, -0.000000000000000000 ) ) ;
#57636 = CARTESIAN_POINT ( 'NONE',  ( 5.000000000000000888, -87.58333333333332860, 2.886751345948126879 ) ) ;
#57637 = CARTESIAN_POINT ( 'NONE',  ( -3.535250795749689387E-16, -38.12499999726881583, -5.773502691896257311 ) ) ;
#57638 = DIRECTION ( 'NONE',  ( -0.000000000000000000, 1.000000000000000000, -0.000000000000000000 ) ) ;
#57639 = CARTESIAN_POINT ( 'NONE',  ( -4.458734124999999437, 17.68750000136559208, 0.000000000000000000 ) ) ;
#57640 = CARTESIAN_POINT ( 'NONE',  ( -2.500000000000000444, -95.16666666666667140, -4.330127018922193649 ) ) ;
#57641 = CARTESIAN_POINT ( 'NONE',  ( -4.458734124999999437, 22.68750000136559564, 0.000000000000000000 ) ) ;
#57642 = CARTESIAN_POINT ( 'NONE',  ( -4.458734124999999437, -56.39583333196773651, -2.574251347313719407 ) ) ;
#57643 = CARTESIAN_POINT ( 'NONE',  ( -2.229367062500000163, -4.729166665301071326, -3.861377020970580443 ) ) ;
#57644 = DIRECTION ( 'NONE',  ( 0.000000000000000000, 0.000000000000000000, 1.000000000000000000 ) ) ;
#57645 = CARTESIAN_POINT ( 'NONE',  ( 5.000000000000000888, 9.416666666666666075, 2.886751345948126879 ) ) ;
#57646 = CARTESIAN_POINT ( 'NONE',  ( 5.000000000000000000, -142.1250000027312126, 0.000000000000000000 ) ) ;
#57647 = CARTESIAN_POINT ( 'NONE',  ( 5.000000000000000000, -75.37499999726880162, -6.123233995736766282E-16 ) ) ;
#57648 = CARTESIAN_POINT ( 'NONE',  ( 2.229367062500001939, -49.97916666530107221, 3.861377020970579999 ) ) ;
#57649 = CARTESIAN_POINT ( 'NONE',  ( 2.500000000000002220, -86.54166666393547303, 4.330127018922192761 ) ) ;
#57650 = CARTESIAN_POINT ( 'NONE',  ( -54.64476657466781973, -137.0625000013656063, -4.444560631937228834 ) ) ;
#57651 =( BOUNDED_CURVE ( )  B_SPLINE_CURVE ( 2, ( #17, #653, #19618, #40509, #58855, #19933, #15445, #30214, #49525 ),
 .UNSPECIFIED., .F., .F. ) 
 B_SPLINE_CURVE_WITH_KNOTS ( ( 3, 2, 2, 2, 3 ),
 ( 0.4874999999999999889, 0.4880952380952380820, 0.4892857142857142683, 0.4904761904761904545, 0.4910714285714285476 ),
 .UNSPECIFIED. ) 
 CURVE ( )  GEOMETRIC_REPRESENTATION_ITEM ( )  RATIONAL_B_SPLINE_CURVE ( ( 0.9330127018922194093, 0.9330127018922194093, 1.000000000000000000, 0.8660254037844387076, 1.000000000000000000, 0.8660254037844387076, 1.000000000000000000, 0.9330127018922194093, 0.9330127018922194093 ) ) 
 REPRESENTATION_ITEM ( '' )  );
#57652 = CARTESIAN_POINT ( 'NONE',  ( 1.975475456537005874E-15, -42.74999999999999289, 5.000000000000000000 ) ) ;
#57653 = DIRECTION ( 'NONE',  ( -0.000000000000000000, 1.000000000000000000, -0.000000000000000000 ) ) ;
#57654 = CARTESIAN_POINT ( 'NONE',  ( 2.229367062499998831, -91.89583333196773651, -3.861377020970580887 ) ) ;
#57655 = CARTESIAN_POINT ( 'NONE',  ( -8.190561711645485556E-16, -158.9375000013655779, 4.458734124999999437 ) ) ;
#57656 = CARTESIAN_POINT ( 'NONE',  ( 1.060575238724906964E-15, -39.75000000000000000, 5.773502691896257311 ) ) ;
#57657 = CARTESIAN_POINT ( 'NONE',  ( 1.975475456537005874E-15, 24.24999999999999645, 5.000000000000000000 ) ) ;
#57658 = VERTEX_POINT ( 'NONE', #33717 ) ;
#57659 = CARTESIAN_POINT ( 'NONE',  ( 2.229367062500001939, 16.77083333469892779, 3.861377020970579999 ) ) ;
#57660 = ORIENTED_EDGE ( 'NONE', *, *, #45686, .T. ) ;
#57661 = CARTESIAN_POINT ( 'NONE',  ( -4.458734124999999437, -94.31249999863440792, 0.000000000000000000 ) ) ;
#57662 = CARTESIAN_POINT ( 'NONE',  ( -2.229367062500000163, 10.27083333469892779, -3.861377020970580443 ) ) ;
#57663 = CARTESIAN_POINT ( 'NONE',  ( -2.500000000000000444, 10.95833333606451632, -4.330127018922193649 ) ) ;
#57664 = CARTESIAN_POINT ( 'NONE',  ( 5.000000000000000000, -162.0000000000000000, 0.000000000000000000 ) ) ;
#57665 = CARTESIAN_POINT ( 'NONE',  ( -5.000000000000000000, 5.000000000000000888, 0.000000000000000000 ) ) ;
#57666 = ADVANCED_FACE ( 'NONE', ( #20196 ), #10535, .T. ) ;
#57667 = CARTESIAN_POINT ( 'NONE',  ( 4.458734124999999437, -63.81249999863440792, -5.460374474430324690E-16 ) ) ;
#57668 = CARTESIAN_POINT ( 'NONE',  ( 5.000000000000000888, 3.541666669397852019, 2.886751345948126879 ) ) ;
#57669 = CARTESIAN_POINT ( 'NONE',  ( -4.458734124999999437, -30.31249999863440436, 0.000000000000000000 ) ) ;
#57670 = CARTESIAN_POINT ( 'NONE',  ( 5.000000000000000000, -40.37499999726880162, -6.123233995736766282E-16 ) ) ;
#57671 = CARTESIAN_POINT ( 'NONE',  ( -4.764381983412779477E-15, 26.37500000273118417, 5.000000000000000000 ) ) ;
#57672 = CARTESIAN_POINT ( 'NONE',  ( 3.061616997868383141E-16, -151.8750000027311842, -5.000000000000000000 ) ) ;
#57673 = CARTESIAN_POINT ( 'NONE',  ( 1.060575238724906964E-15, -44.74999999999999289, 5.773502691896257311 ) ) ;
#57675 = CARTESIAN_POINT ( 'NONE',  ( -3.152548672688508926E-16, -17.81249999863440792, -5.148502694627439702 ) ) ;
#57674 = CARTESIAN_POINT ( 'NONE',  ( 5.000000000000000000, -26.37499999726881583, -6.123233995736766282E-16 ) ) ;
#57676 = CARTESIAN_POINT ( 'NONE',  ( 2.071067811865306751, -154.8125000000000000, -5.000000000000171418 ) ) ;
#57677 = CARTESIAN_POINT ( 'NONE',  ( 9.457646018065525792E-16, -63.06249999863440081, 5.148502694627439702 ) ) ;
#57678 = CARTESIAN_POINT ( 'NONE',  ( -4.458734124999999437, -148.1875000013656063, -5.460374474430324690E-16 ) ) ;
#57679 = VECTOR ( 'NONE', #50092, 1000.000000000000000 ) ;
#57680 = CARTESIAN_POINT ( 'NONE',  ( 9.457646018065525792E-16, -75.06249999863439371, 5.148502694627439702 ) ) ;
#57681 = CARTESIAN_POINT ( 'NONE',  ( -59.29741812935640155, -142.8750000013656063, -2.196230717870135685 ) ) ;
#57682 = CARTESIAN_POINT ( 'NONE',  ( -4.458734124999998549, -25.47916666530106866, 2.574251347313722516 ) ) ;
#57683 = CARTESIAN_POINT ( 'NONE',  ( 2.499999999999998668, -65.20833333060213022, -4.330127018922193649 ) ) ;
#57684 = VERTEX_POINT ( 'NONE', #30147 ) ;
#57685 = CARTESIAN_POINT ( 'NONE',  ( -7.500000000000000000, -4.330127018922198090, -7.422398894150034288 ) ) ;
#57686 = ORIENTED_EDGE ( 'NONE', *, *, #24410, .F. ) ;
#57687 = CARTESIAN_POINT ( 'NONE',  ( -2.229367062500000163, -67.72916666530106511, -3.861377020970580443 ) ) ;
#57688 = CARTESIAN_POINT ( 'NONE',  ( 5.000000000000000000, -21.29166666393548013, -2.886751345948130876 ) ) ;
#57689 = VERTEX_POINT ( 'NONE', #53336 ) ;
#57690 = CARTESIAN_POINT ( 'NONE',  ( 75.00000000000001421, 15.00000000000000000, -9.000000000000001776 ) ) ;
#57691 = CARTESIAN_POINT ( 'NONE',  ( 4.458734125000001214, -53.14583333196773651, 2.574251347313718519 ) ) ;
#57692 = CARTESIAN_POINT ( 'NONE',  ( 4.458734124999998549, 4.020833334698926009, -2.574251347313721627 ) ) ;
#57693 = ORIENTED_EDGE ( 'NONE', *, *, #18173, .F. ) ;
#57694 = CARTESIAN_POINT ( 'NONE',  ( -2.500000000000000444, 1.958333336064519647, -4.330127018922193649 ) ) ;
#57695 = CARTESIAN_POINT ( 'NONE',  ( 2.229367062500001939, 3.020833334698928674, 3.861377020970579999 ) ) ;
#57696 =( BOUNDED_SURFACE ( )  B_SPLINE_SURFACE ( 3, 2, ( 
 ( #60586, #45135, #56069 ),
 ( #1099, #26477, #26155 ),
 ( #45774, #20708, #1733 ),
 ( #16820, #40313, #26793 ),
 ( #36439, #59951, #6228 ),
 ( #36127, #55749, #11666 ),
 ( #31285, #46091, #2051 ),
 ( #48215, #33125, #24098 ) ),
 .UNSPECIFIED., .F., .F., .F. ) 
 B_SPLINE_SURFACE_WITH_KNOTS ( ( 4, 2, 2, 4 ),
 ( 3, 3 ),
 ( 0.03861844051980971304, 0.04325213341840642572, 0.04556897986770477860, 0.04788582631700313841 ),
 ( 0.000000000000000000, 1.000000000000000000 ),
 .UNSPECIFIED. ) 
 GEOMETRIC_REPRESENTATION_ITEM ( )  RATIONAL_B_SPLINE_SURFACE ( (
 ( 1.000000000000000000, 0.8047781759831923454, 1.000000000000000000),
 ( 1.000000000000000000, 0.8123762462805160789, 1.000000000000000000),
 ( 1.000000000000000000, 0.8190659850616602844, 1.000000000000000000),
 ( 1.000000000000000000, 0.8191937571013702124, 1.000000000000000000),
 ( 1.000000000000000000, 0.8176092952780309453, 1.000000000000000000),
 ( 1.000000000000000000, 0.8122962088596628050, 1.000000000000000000),
 ( 1.000000000000000000, 0.8086311330827828936, 1.000000000000000000),
 ( 1.000000000000000000, 0.8047712282214327661, 1.000000000000000000) ) ) 
 REPRESENTATION_ITEM ( '' )  SURFACE ( )  );
#57697 = CARTESIAN_POINT ( 'NONE',  ( 2.229367062499998831, 17.35416666803225993, -3.861377020970580887 ) ) ;
#57698 = CARTESIAN_POINT ( 'NONE',  ( -50.55543936806279248, -143.0625000013656063, 0.3552334253322060320 ) ) ;
#57699 = LINE ( 'NONE', #13308, #36735 ) ;
#57700 = CARTESIAN_POINT ( 'NONE',  ( -1.846868145590734756, -165.1250000013656347, -4.458734124999999437 ) ) ;
#57701 = EDGE_LOOP ( 'NONE', ( #22000, #41116, #28153, #21341 ) ) ;
#57702 = CARTESIAN_POINT ( 'NONE',  ( -2.229367062499996610, -77.14583333196773651, 3.861377020970582219 ) ) ;
#57703 = CARTESIAN_POINT ( 'NONE',  ( 0.000000000000000000, -170.0000000000000000, 0.000000000000000000 ) ) ;
#57704 = CARTESIAN_POINT ( 'NONE',  ( -4.458734124999998549, 5.770833334698927786, 2.574251347313722516 ) ) ;
#57705 = CARTESIAN_POINT ( 'NONE',  ( -5.000000000000000000, -41.99999999999999289, 0.000000000000000000 ) ) ;
#57706 = CARTESIAN_POINT ( 'NONE',  ( -4.458734124999999437, -61.64583333196773651, -2.574251347313719407 ) ) ;
#57707 = CARTESIAN_POINT ( 'NONE',  ( -4.999999999999999112, -21.79166666393547658, 2.886751345948131764 ) ) ;
#57708 = CARTESIAN_POINT ( 'NONE',  ( 5.000000000000000000, -96.37499999726881583, -6.123233995736766282E-16 ) ) ;
#57709 = CARTESIAN_POINT ( 'NONE',  ( 0.000000000000000000, -120.0000000000000000, 0.000000000000000000 ) ) ;
#57710 = CYLINDRICAL_SURFACE ( 'NONE', #13093, 5.000000000000000000 ) ;
#57711 = CARTESIAN_POINT ( 'NONE',  ( 6.123233995736766282E-16, -170.0000000000000000, -5.000000000000000000 ) ) ;
#57712 = CARTESIAN_POINT ( 'NONE',  ( -58.24261429053147765, -146.2500000000000284, -3.805975901505573855 ) ) ;
#57713 = CARTESIAN_POINT ( 'NONE',  ( -4.458734124999998549, -39.22916666530107221, 2.574251347313722516 ) ) ;
#57714 = CARTESIAN_POINT ( 'NONE',  ( 4.458734124999999437, -29.06249999863440436, -5.460374474430324690E-16 ) ) ;
#57715 = DIRECTION ( 'NONE',  ( -0.000000000000000000, 1.000000000000000000, -0.000000000000000000 ) ) ;
#57716 = CARTESIAN_POINT ( 'NONE',  ( 2.500000000000002220, 26.33333333333333215, 4.330127018922192761 ) ) ;
#57717 = CARTESIAN_POINT ( 'NONE',  ( 2.071067811865475505, -151.9375000027312126, -5.000000000000000888 ) ) ;
#57718 = ORIENTED_EDGE ( 'NONE', *, *, #43588, .F. ) ;
#57719 = CARTESIAN_POINT ( 'NONE',  ( -1.339745962155610925, -49.79465819873851729, 5.000000000000000000 ) ) ;
#57720 = CARTESIAN_POINT ( 'NONE',  ( -3.152548672688508926E-16, -31.56249999863440436, -5.148502694627439702 ) ) ;
#57721 = CARTESIAN_POINT ( 'NONE',  ( -2.499999999999996447, -70.70833333060214443, 4.330127018922195425 ) ) ;
#57722 = CARTESIAN_POINT ( 'NONE',  ( -50.70258187064364108, -149.3750000013656347, 2.196230717870141014 ) ) ;
#57723 = CARTESIAN_POINT ( 'NONE',  ( -3.535533905932738641, -142.3750000000000000, 3.535533905932737309 ) ) ;
#57724 = CARTESIAN_POINT ( 'NONE',  ( -2.229367062500000163, -27.47916666530107221, -3.861377020970580443 ) ) ;
#57725 = CARTESIAN_POINT ( 'NONE',  ( 2.229367062500001939, -73.22916666530107932, 3.861377020970579999 ) ) ;
#57726 = CARTESIAN_POINT ( 'NONE',  ( 1.975475456537005874E-15, -7.750000000000000000, 5.000000000000000000 ) ) ;
#57727 = CARTESIAN_POINT ( 'NONE',  ( -4.458734124999997661, -32.22916666530106511, 2.574251347313722516 ) ) ;
#57728 = CARTESIAN_POINT ( 'NONE',  ( 1.975475456537005874E-15, -23.62499999726880873, 5.000000000000000000 ) ) ;
#57729 = DIRECTION ( 'NONE',  ( -0.000000000000000000, 1.000000000000000000, -0.000000000000000000 ) ) ;
#57730 = CARTESIAN_POINT ( 'NONE',  ( -2.500000000000000444, -21.16666666666666785, -4.330127018922193649 ) ) ;
#57731 = CARTESIAN_POINT ( 'NONE',  ( -3.152801135295367985, -147.8125000013655779, 3.152801135295367096 ) ) ;
#57732 = ORIENTED_EDGE ( 'NONE', *, *, #22398, .F. ) ;
#57733 = CARTESIAN_POINT ( 'NONE',  ( -6.972266317189433020E-16, -79.12499999726881583, -5.000000000000000000 ) ) ;
#57734 = CARTESIAN_POINT ( 'NONE',  ( -4.458734124999997661, -55.47916666530106511, 2.574251347313722516 ) ) ;
#57735 = CARTESIAN_POINT ( 'NONE',  ( 5.000000000000000000, 25.70833333606452342, -2.886751345948129988 ) ) ;
#57736 = CYLINDRICAL_SURFACE ( 'NONE', #26820, 5.000000000000000000 ) ;
#57737 = CARTESIAN_POINT ( 'NONE',  ( -3.535250795749689387E-16, 19.74999999999999645, -5.773502691896257311 ) ) ;
#57738 = EDGE_CURVE ( 'NONE', #45744, #4902, #59820, .T. ) ;
#57739 = CARTESIAN_POINT ( 'NONE',  ( 0.000000000000000000, -120.0000000000000000, 5.000000000000000000 ) ) ;
#57740 = CARTESIAN_POINT ( 'NONE',  ( 2.229367062500001939, -1.979166665301068662, 3.861377020970579999 ) ) ;
#57741 = CARTESIAN_POINT ( 'NONE',  ( -5.000000000000000000, -11.08333333333333393, -2.886751345948128211 ) ) ;
#57742 = CARTESIAN_POINT ( 'NONE',  ( -6.972266317189433020E-16, -81.12499999726881583, -5.000000000000000000 ) ) ;
#57743 = CARTESIAN_POINT ( 'NONE',  ( 4.458734124999998549, 10.02083333469892779, -2.574251347313721627 ) ) ;
#57744 = DIRECTION ( 'NONE',  ( -0.000000000000000000, 1.000000000000000000, -0.000000000000000000 ) ) ;
#57745 = ORIENTED_EDGE ( 'NONE', *, *, #8289, .F. ) ;
#57746 =( BOUNDED_CURVE ( )  B_SPLINE_CURVE ( 2, ( #1951, #60795, #7714, #23126, #32456, #47869, #18615, #28570, #32135 ),
 .UNSPECIFIED., .F., .F. ) 
 B_SPLINE_CURVE_WITH_KNOTS ( ( 3, 2, 2, 2, 3 ),
 ( 0.09107142857142856707, 0.09166666666666666019, 0.09285714285714286031, 0.09404761904761904656, 0.09464285714285713969 ),
 .UNSPECIFIED. ) 
 CURVE ( )  GEOMETRIC_REPRESENTATION_ITEM ( )  RATIONAL_B_SPLINE_CURVE ( ( 0.9330127018922194093, 0.9330127018922194093, 1.000000000000000000, 0.8660254037844387076, 1.000000000000000000, 0.8660254037844387076, 1.000000000000000000, 0.9330127018922194093, 0.9330127018922194093 ) ) 
 REPRESENTATION_ITEM ( '' )  );
#57747 = CARTESIAN_POINT ( 'NONE',  ( 5.000000000000000000, 10.62500000273118594, -6.123233995736766282E-16 ) ) ;
#57748 = CARTESIAN_POINT ( 'NONE',  ( 4.458734125000001214, -50.89583333196772230, 2.574251347313718519 ) ) ;
#57749 = CARTESIAN_POINT ( 'NONE',  ( 4.458734125000000326, -160.6250000013655779, -1.846868145590734978 ) ) ;
#57750 = ADVANCED_FACE ( 'NONE', ( #54286 ), #63310, .T. ) ;
#57751 = CARTESIAN_POINT ( 'NONE',  ( 5.000000000000000000, -51.37499999726881583, -6.123233995736766282E-16 ) ) ;
#57752 = ORIENTED_EDGE ( 'NONE', *, *, #54312, .F. ) ;
#57754 = EDGE_CURVE ( 'NONE', #56488, #35184, #62640, .T. ) ;
#57753 = CARTESIAN_POINT ( 'NONE',  ( 4.458734125000001214, -20.89583333196774007, 2.574251347313718519 ) ) ;
#57755 = ORIENTED_EDGE ( 'NONE', *, *, #53864, .F. ) ;
#57757 = CARTESIAN_POINT ( 'NONE',  ( 2.499999999999998668, -53.33333333333332860, -4.330127018922193649 ) ) ;
#57756 = CARTESIAN_POINT ( 'NONE',  ( -1.339745962155613812, -96.20534180126146850, -5.000000000000000000 ) ) ;
#57758 = CARTESIAN_POINT ( 'NONE',  ( -4.458734125000001214, -161.8750000013656063, 1.846868145590734089 ) ) ;
#57759 = ORIENTED_EDGE ( 'NONE', *, *, #48740, .T. ) ;
#57760 = CARTESIAN_POINT ( 'NONE',  ( 0.000000000000000000, -170.0000000000000000, 0.000000000000000000 ) ) ;
#57761 = CARTESIAN_POINT ( 'NONE',  ( -53.33387254593733928, -133.8125000000000284, 5.149110718188519620 ) ) ;
#57762 = CARTESIAN_POINT ( 'NONE',  ( 2.229367062499998831, -36.89583333196773651, -3.861377020970580887 ) ) ;
#57763 = ORIENTED_EDGE ( 'NONE', *, *, #37421, .F. ) ;
#57764 = ADVANCED_FACE ( 'NONE', ( #48818 ), #24384, .T. ) ;
#57765 = CARTESIAN_POINT ( 'NONE',  ( 9.457646018065525792E-16, -83.06249999863439371, 5.148502694627439702 ) ) ;
#57766 = CARTESIAN_POINT ( 'NONE',  ( 2.229367062500001939, 18.02083333469892779, 3.861377020970579999 ) ) ;
#57767 = CARTESIAN_POINT ( 'NONE',  ( -6.972266317189433020E-16, -12.12499999726881406, -5.000000000000000000 ) ) ;
#57768 = ORIENTED_EDGE ( 'NONE', *, *, #4296, .F. ) ;
#57769 = CARTESIAN_POINT ( 'NONE',  ( -59.44456063193725015, -137.8125000013656063, -0.3552334253322034230 ) ) ;
#57770 = CARTESIAN_POINT ( 'NONE',  ( -4.458734124999999437, -86.64583333196773651, -2.574251347313719407 ) ) ;
#57771 = CARTESIAN_POINT ( 'NONE',  ( -59.98410592259440222, -127.2500000027312126, -0.3983568153799752487 ) ) ;
#57772 = CARTESIAN_POINT ( 'NONE',  ( 5.000000000000000000, -88.50000000000000000, -6.123233995736766282E-16 ) ) ;
#57773 = CYLINDRICAL_SURFACE ( 'NONE', #1824, 5.000000000000000000 ) ;
#57774 = CARTESIAN_POINT ( 'NONE',  ( -6.972266317189433020E-16, 4.749999999999999112, -5.000000000000000000 ) ) ;
#57775 = CARTESIAN_POINT ( 'NONE',  ( -2.229367062499996610, -61.14583333196774362, 3.861377020970582219 ) ) ;
#57776 = LINE ( 'NONE', #38447, #35643 ) ;
#57777 = CARTESIAN_POINT ( 'NONE',  ( 2.229367062499998831, 24.35416666803225993, -3.861377020970580887 ) ) ;
#57778 = CARTESIAN_POINT ( 'NONE',  ( -4.999999999999999112, -109.9166666666666572, 2.886751345948131764 ) ) ;
#57779 = CARTESIAN_POINT ( 'NONE',  ( 1.975475456537005874E-15, 5.375000002731185944, 5.000000000000000000 ) ) ;
#57780 = CARTESIAN_POINT ( 'NONE',  ( 4.458734125000001214, -45.14583333196774362, 2.574251347313718519 ) ) ;
#57781 = EDGE_CURVE ( 'NONE', #1040, #22477, #5509, .T. ) ;
#57782 = CARTESIAN_POINT ( 'NONE',  ( 2.500000000000002220, -4.541666663935479242, 4.330127018922192761 ) ) ;
#57783 = CARTESIAN_POINT ( 'NONE',  ( -4.330127018922101279, 30.00000000000000000, 7.500000000000002665 ) ) ;
#57784 = CARTESIAN_POINT ( 'NONE',  ( -1.339745962155610925, -60.79465819873851729, 5.000000000000000000 ) ) ;
#57785 = CARTESIAN_POINT ( 'NONE',  ( -3.152548672688508926E-16, -86.81249999863439371, -5.148502694627439702 ) ) ;
#57786 = CARTESIAN_POINT ( 'NONE',  ( 2.229367062499998831, -105.6458333319677365, -3.861377020970580887 ) ) ;
#57787 = CARTESIAN_POINT ( 'NONE',  ( 4.458734124999999437, -9.062499998634406140, -5.460374474430324690E-16 ) ) ;
#57788 = ORIENTED_EDGE ( 'NONE', *, *, #18939, .T. ) ;
#57789 = CARTESIAN_POINT ( 'NONE',  ( 1.975475456537005874E-15, 18.37500000273118062, 5.000000000000000000 ) ) ;
#57790 = CARTESIAN_POINT ( 'NONE',  ( 4.458734125000001214, -97.89583333196773651, 2.574251347313718519 ) ) ;
#57791 = CARTESIAN_POINT ( 'NONE',  ( -5.000000000000000000, -166.6250000027312126, -6.123233995736766282E-16 ) ) ;
#57792 = CARTESIAN_POINT ( 'NONE',  ( -4.458734124999999437, -89.64583333196773651, -2.574251347313719407 ) ) ;
#57793 = CARTESIAN_POINT ( 'NONE',  ( -5.000000000000000000, -53.95833333060214443, -2.886751345948128211 ) ) ;
#57794 = CARTESIAN_POINT ( 'NONE',  ( -7.922281120364393914, -4.573931137438277617, -8.047472243342932430 ) ) ;
#57795 = CARTESIAN_POINT ( 'NONE',  ( -52.10840900171896806, -131.1875000013656063, 3.393966926194110556 ) ) ;
#57796 = CARTESIAN_POINT ( 'NONE',  ( -4.458734124999999437, -15.31249999863440436, 0.000000000000000000 ) ) ;
#57797 = CARTESIAN_POINT ( 'NONE',  ( -2.229367062499996610, 12.60416666803226171, 3.861377020970582219 ) ) ;
#57798 = CARTESIAN_POINT ( 'NONE',  ( 2.229367062500001939, -59.22916666530106511, 3.861377020970579999 ) ) ;
#57799 = CARTESIAN_POINT ( 'NONE',  ( -6.972266317189433020E-16, 16.74999999999999645, -5.000000000000000000 ) ) ;
#57800 = CARTESIAN_POINT ( 'NONE',  ( -2.499999999999996447, -36.83333333333332860, 4.330127018922195425 ) ) ;
#57801 = CARTESIAN_POINT ( 'NONE',  ( 4.458734125000000326, -14.89583333196773474, 2.574251347313718519 ) ) ;
#57802 = CYLINDRICAL_SURFACE ( 'NONE', #22694, 5.000000000000000000 ) ;
#57803 = ORIENTED_EDGE ( 'NONE', *, *, #61399, .F. ) ;
#57804 = CARTESIAN_POINT ( 'NONE',  ( -4.458734124999997661, -42.47916666530106511, 2.574251347313722516 ) ) ;
#57805 = CARTESIAN_POINT ( 'NONE',  ( 1.339745962155615144, -77.70534180126146850, 4.999999999999999112 ) ) ;
#57806 = CARTESIAN_POINT ( 'NONE',  ( 5.000000000000000888, -68.58333333333332860, 2.886751345948126879 ) ) ;
#57807 = CARTESIAN_POINT ( 'NONE',  ( -2.499999999999996447, -66.70833333060214443, 4.330127018922195425 ) ) ;
#57808 = CARTESIAN_POINT ( 'NONE',  ( -3.152548672688508926E-16, -83.56249999863440792, -5.148502694627439702 ) ) ;
#57809 = CARTESIAN_POINT ( 'NONE',  ( 4.458734124999998549, 24.02083333469892423, -2.574251347313721627 ) ) ;
#57810 = EDGE_CURVE ( 'NONE', #1054, #17081, #16881, .T. ) ;
#57811 = CARTESIAN_POINT ( 'NONE',  ( 2.229367062499998831, 14.35416666803226171, -3.861377020970580887 ) ) ;
#57812 = EDGE_CURVE ( 'NONE', #57126, #19298, #12089, .T. ) ;
#57813 = ADVANCED_FACE ( 'NONE', ( #7871 ), #61273, .T. ) ;
#57814 = CARTESIAN_POINT ( 'NONE',  ( -2.499999999999996447, 7.166666666666665186, 4.330127018922195425 ) ) ;
#57815 = CARTESIAN_POINT ( 'NONE',  ( -2.500000000000000444, -65.04166666393547303, -4.330127018922193649 ) ) ;
#57816 = CARTESIAN_POINT ( 'NONE',  ( 2.229367062500001939, -87.22916666530107932, 3.861377020970579999 ) ) ;
#57817 = CARTESIAN_POINT ( 'NONE',  ( -4.999999999999999112, -70.91666666666667140, 2.886751345948131764 ) ) ;
#57818 = CARTESIAN_POINT ( 'NONE',  ( -5.000000000000000000, 11.12500000273118594, 0.000000000000000000 ) ) ;
#57819 = VERTEX_POINT ( 'NONE', #42269 ) ;
#57820 = CARTESIAN_POINT ( 'NONE',  ( 0.000000000000000000, -120.0000000000000000, 0.000000000000000000 ) ) ;
#57821 = CARTESIAN_POINT ( 'NONE',  ( -4.999999999999998224, 16.08333333333333215, 2.886751345948131764 ) ) ;
#57823 = CARTESIAN_POINT ( 'NONE',  ( -2.499999999999996447, -27.83333333333333570, 4.330127018922195425 ) ) ;
#57822 = CARTESIAN_POINT ( 'NONE',  ( 0.000000000000000000, -170.0000000000000000, 0.000000000000000000 ) ) ;
#57824 = CARTESIAN_POINT ( 'NONE',  ( 2.229367062499998831, -30.64583333196773651, -3.861377020970580887 ) ) ;
#57825 = EDGE_CURVE ( 'NONE', #26615, #15325, #7247, .T. ) ;
#57826 =( BOUNDED_CURVE ( )  B_SPLINE_CURVE ( 2, ( #329, #16069, #44047, #19615, #649, #19928, #35369, #39227, #44688 ),
 .UNSPECIFIED., .F., .F. ) 
 B_SPLINE_CURVE_WITH_KNOTS ( ( 3, 2, 2, 2, 3 ),
 ( 0.3446428571428571397, 0.3452380952380952328, 0.3464285714285714191, 0.3476190476190476053, 0.3482142857142856984 ),
 .UNSPECIFIED. ) 
 CURVE ( )  GEOMETRIC_REPRESENTATION_ITEM ( )  RATIONAL_B_SPLINE_CURVE ( ( 0.9330127018922194093, 0.9330127018922194093, 1.000000000000000000, 0.8660254037844387076, 1.000000000000000000, 0.8660254037844387076, 1.000000000000000000, 0.9330127018922194093, 0.9330127018922194093 ) ) 
 REPRESENTATION_ITEM ( '' )  );
#57827 = CARTESIAN_POINT ( 'NONE',  ( 2.500000000000002220, -34.54166666393547303, 4.330127018922192761 ) ) ;
#57829 = ORIENTED_EDGE ( 'NONE', *, *, #7928, .F. ) ;
#57828 = CARTESIAN_POINT ( 'NONE',  ( 4.458734124999998549, -62.72916666530106511, -2.574251347313721627 ) ) ;
#57830 = CARTESIAN_POINT ( 'NONE',  ( -52.80376928212989185, -150.1250000013656063, -4.297418129356379346 ) ) ;
#57831 = EDGE_CURVE ( 'NONE', #4973, #21052, #53450, .T. ) ;
#57833 = ORIENTED_EDGE ( 'NONE', *, *, #52798, .T. ) ;
#57832 = CARTESIAN_POINT ( 'NONE',  ( -4.458734124999999437, -6.562499998634403475, 0.000000000000000000 ) ) ;
#57834 = CARTESIAN_POINT ( 'NONE',  ( -2.500000000000000444, -78.16666666666665719, -4.330127018922193649 ) ) ;
#57835 = CARTESIAN_POINT ( 'NONE',  ( -54.64476657466781973, -135.8125000013656063, -4.444560631937228834 ) ) ;
#57836 = CARTESIAN_POINT ( 'NONE',  ( -4.458734124999999437, -54.64583333196774362, -2.574251347313719407 ) ) ;
#57837 = CARTESIAN_POINT ( 'NONE',  ( 2.500000000000002220, -82.54166666393547303, 4.330127018922192761 ) ) ;
#57839 = VERTEX_POINT ( 'NONE', #17526 ) ;
#57838 = CYLINDRICAL_SURFACE ( 'NONE', #17957, 5.000000000000000000 ) ;
#57840 = CARTESIAN_POINT ( 'NONE',  ( -59.81910112700025905, -146.1875000000000284, -2.462841084822630311 ) ) ;
#57841 = CARTESIAN_POINT ( 'NONE',  ( 2.229367062499998831, -20.89583333196774007, -3.861377020970580887 ) ) ;
#57843 = VERTEX_POINT ( 'NONE', #2731 ) ;
#57842 = CARTESIAN_POINT ( 'NONE',  ( -2.229367062500000163, -56.72916666530107221, -3.861377020970580443 ) ) ;
#57844 =( BOUNDED_CURVE ( )  B_SPLINE_CURVE ( 2, ( #63167, #62549, #19078, #24230, #38394, #19404, #13326, #43836, #14263 ),
 .UNSPECIFIED., .F., .F. ) 
 B_SPLINE_CURVE_WITH_KNOTS ( ( 3, 2, 2, 2, 3 ),
 ( 0.3583333333333336146, 0.3625000000000002665, 0.3666666666666669183, 0.3708333333333336257, 0.3750000000000002776 ),
 .UNSPECIFIED. ) 
 CURVE ( )  GEOMETRIC_REPRESENTATION_ITEM ( )  RATIONAL_B_SPLINE_CURVE ( ( 0.9999999999999948930, 0.9238795325112918455, 1.000000000000000000, 0.9238795325112867385, 1.000000000000000000, 0.9238795325112867385, 1.000000000000000000, 0.9238795325112816315, 1.000000000000005107 ) ) 
 REPRESENTATION_ITEM ( '' )  );
#57845 =( NAMED_UNIT ( * ) SI_UNIT ( $, .STERADIAN. ) SOLID_ANGLE_UNIT ( ) );
#57846 = CARTESIAN_POINT ( 'NONE',  ( -3.152801135295367985, -165.0625000013656063, 3.152801135295367096 ) ) ;
#57847 = CARTESIAN_POINT ( 'NONE',  ( 9.457646018065525792E-16, -106.3124999986343795, 5.148502694627439702 ) ) ;
#57848 = CARTESIAN_POINT ( 'NONE',  ( -1.230605004983934782E-13, -26.62499999726881583, 5.000000000000000000 ) ) ;
#57849 = ORIENTED_EDGE ( 'NONE', *, *, #33680, .F. ) ;
#57850 = CARTESIAN_POINT ( 'NONE',  ( -50.55543936806279248, -149.3125000013656063, 0.3552334253322060320 ) ) ;
#57851 = CARTESIAN_POINT ( 'NONE',  ( -51.19402409849444524, -139.6250000027312126, -3.242614290531456334 ) ) ;
#57852 = CARTESIAN_POINT ( 'NONE',  ( -48.00000000000002132, -155.0000000000000284, 4.041451884327384114 ) ) ;
#57853 = CARTESIAN_POINT ( 'NONE',  ( 4.458734124999999437, -7.812499998634405252, -5.460374474430324690E-16 ) ) ;
#57854 = CARTESIAN_POINT ( 'NONE',  ( -4.458734124999997661, -103.4791666653010651, 2.574251347313722516 ) ) ;
#57855 = CARTESIAN_POINT ( 'NONE',  ( -4.458734125000001214, -143.1250000013656063, 1.846868145590734089 ) ) ;
#57856 = CARTESIAN_POINT ( 'NONE',  ( 4.458734124999998549, -25.97916666530106866, -2.574251347313721627 ) ) ;
#57857 = CARTESIAN_POINT ( 'NONE',  ( -4.729367062499999719, 29.84375000068279604, 0.000000000000000000 ) ) ;
#57858 = CARTESIAN_POINT ( 'NONE',  ( -50.55543936806279248, -138.0625000013656063, 0.3552334253322060320 ) ) ;
#57859 = CARTESIAN_POINT ( 'NONE',  ( 4.458734124999999437, -70.06249999863439371, -5.460374474430324690E-16 ) ) ;
#57860 = CARTESIAN_POINT ( 'NONE',  ( 5.000000000000000000, -21.29166666393548013, -2.886751345948130876 ) ) ;
#57861 = CARTESIAN_POINT ( 'NONE',  ( -4.458734124999999437, -141.9375000013656063, -5.460374474430324690E-16 ) ) ;
#57862 = CARTESIAN_POINT ( 'NONE',  ( -2.229367062499996610, 5.604166668032261711, 3.861377020970582219 ) ) ;
#57863 = ORIENTED_EDGE ( 'NONE', *, *, #9170, .F. ) ;
#57864 = DIRECTION ( 'NONE',  ( -0.000000000000000000, 1.000000000000000000, -0.000000000000000000 ) ) ;
#57865 = FACE_OUTER_BOUND ( 'NONE', #61961, .T. ) ;
#57867 = CARTESIAN_POINT ( 'NONE',  ( -3.152548672688508926E-16, -30.56249999863440436, -5.148502694627439702 ) ) ;
#57866 = CARTESIAN_POINT ( 'NONE',  ( -4.999999999999999112, -92.91666666666665719, 2.886751345948131764 ) ) ;
#57868 = CARTESIAN_POINT ( 'NONE',  ( 1.339745962155612702, -14.16965819600733312, -5.000000000000000000 ) ) ;
#57869 = CARTESIAN_POINT ( 'NONE',  ( 2.229367062499998831, -75.89583333196773651, -3.861377020970580887 ) ) ;
#57870 = CARTESIAN_POINT ( 'NONE',  ( -2.229367062500000163, 24.27083333469892779, -3.861377020970580443 ) ) ;
#57871 = CARTESIAN_POINT ( 'NONE',  ( -1.127183054612291972E-14, 23.37500000273118772, 4.999999999999999112 ) ) ;
#57872 = CARTESIAN_POINT ( 'NONE',  ( -56.48576386720575471, -139.7500000013656347, -4.591703134518078322 ) ) ;
#57873 = CARTESIAN_POINT ( 'NONE',  ( 9.457646018065525792E-16, 3.937500001365595192, 5.148502694627439702 ) ) ;
#57874 = CARTESIAN_POINT ( 'NONE',  ( 4.458734124999999437, 25.93750000136559564, -5.460374474430324690E-16 ) ) ;
#57875 = CARTESIAN_POINT ( 'NONE',  ( 9.457646018065525792E-16, -40.31249999863440081, 5.148502694627439702 ) ) ;
#57876 = CARTESIAN_POINT ( 'NONE',  ( 1.339745962155615144, -60.58034179853027723, 4.999999999999999112 ) ) ;
#57877 = CARTESIAN_POINT ( 'NONE',  ( -4.458734124999997661, 3.770833334698929562, 2.574251347313722516 ) ) ;
#57878 = CARTESIAN_POINT ( 'NONE',  ( -2.229367062500000163, -23.72916666530107577, -3.861377020970580443 ) ) ;
#57879 = CARTESIAN_POINT ( 'NONE',  ( 3.152801135295366208, -155.5625000013656063, 3.152801135295367985 ) ) ;
#57880 = CARTESIAN_POINT ( 'NONE',  ( -4.458734124999998549, -70.22916666530107932, 2.574251347313722516 ) ) ;
#57881 = CARTESIAN_POINT ( 'NONE',  ( -4.999999999999999112, -97.79166666393545881, 2.886751345948131764 ) ) ;
#57882 = CARTESIAN_POINT ( 'NONE',  ( -4.458734124999999437, 28.60416666803226349, -2.574251347313719407 ) ) ;
#57883 = EDGE_CURVE ( 'NONE', #45091, #44922, #8188, .T. ) ;
#57884 = CARTESIAN_POINT ( 'NONE',  ( 2.500000000000002220, 9.458333336064519870, 4.330127018922192761 ) ) ;
#57885 = CARTESIAN_POINT ( 'NONE',  ( 4.458734125000000326, -107.1458333319677365, 2.574251347313718519 ) ) ;
#57886 = CARTESIAN_POINT ( 'NONE',  ( 4.458734124999999437, -75.06249999863440792, -5.460374474430324690E-16 ) ) ;
#57887 = CARTESIAN_POINT ( 'NONE',  ( 2.500000000000002220, -55.66666666666667140, 4.330127018922192761 ) ) ;
#57888 = CARTESIAN_POINT ( 'NONE',  ( 1.975475456537005874E-15, -65.62499999726881583, 5.000000000000000000 ) ) ;
#57889 = CARTESIAN_POINT ( 'NONE',  ( -6.972266317189433020E-16, -10.12499999726881406, -5.000000000000000000 ) ) ;
#57890 = ORIENTED_EDGE ( 'NONE', *, *, #60657, .T. ) ;
#57891 = CARTESIAN_POINT ( 'NONE',  ( 6.123233995736766282E-16, -170.0000000000000000, -5.000000000000000000 ) ) ;
#57892 =( BOUNDED_CURVE ( )  B_SPLINE_CURVE ( 2, ( #49302, #24541, #33562, #116, #59274, #39011, #62844, #53183, #44467 ),
 .UNSPECIFIED., .F., .F. ) 
 B_SPLINE_CURVE_WITH_KNOTS ( ( 3, 2, 2, 2, 3 ),
 ( 0.2312500000000000111, 0.2319444444444444531, 0.2333333333333333370, 0.2347222222222222210, 0.2354166666666666630 ),
 .UNSPECIFIED. ) 
 CURVE ( )  GEOMETRIC_REPRESENTATION_ITEM ( )  RATIONAL_B_SPLINE_CURVE ( ( 0.9330127018922194093, 0.9330127018922194093, 1.000000000000000000, 0.8660254037844387076, 1.000000000000000000, 0.8660254037844387076, 1.000000000000000000, 0.9330127018922194093, 0.9330127018922194093 ) ) 
 REPRESENTATION_ITEM ( '' )  );
#57893 = EDGE_CURVE ( 'NONE', #61326, #53004, #18663, .T. ) ;
#57894 = CARTESIAN_POINT ( 'NONE',  ( -5.000000000000000000, 12.12500000273118772, 0.000000000000000000 ) ) ;
#57895 = CARTESIAN_POINT ( 'NONE',  ( 5.000000000000000000, -12.49999999999999645, -6.123233995736766282E-16 ) ) ;
#57896 = CARTESIAN_POINT ( 'NONE',  ( -3.152548672688508926E-16, -16.56249999863440792, -5.148502694627439702 ) ) ;
#57897 = EDGE_CURVE ( 'NONE', #45293, #47799, #3366, .T. ) ;
#57898 = CARTESIAN_POINT ( 'NONE',  ( -2.229367062499996610, -75.14583333196773651, 3.861377020970582219 ) ) ;
#57899 = CARTESIAN_POINT ( 'NONE',  ( 4.458734124999999437, -167.6875000013655779, 0.000000000000000000 ) ) ;
#57900 = CARTESIAN_POINT ( 'NONE',  ( -2.499999999999996447, -16.70833333060214443, 4.330127018922195425 ) ) ;
#57902 = ORIENTED_EDGE ( 'NONE', *, *, #35467, .T. ) ;
#57901 = CARTESIAN_POINT ( 'NONE',  ( -3.152548672688508926E-16, -46.56249999863440792, -5.148502694627439702 ) ) ;
#57903 = DIRECTION ( 'NONE',  ( -0.000000000000000000, 1.000000000000000000, -0.000000000000000000 ) ) ;
#57905 = VERTEX_POINT ( 'NONE', #6923 ) ;
#57904 = CARTESIAN_POINT ( 'NONE',  ( 4.458734124999998549, 6.020833334698928674, -2.574251347313721627 ) ) ;
#57906 = CARTESIAN_POINT ( 'NONE',  ( -56.48576386720575471, -151.7500000013656063, -4.591703134518078322 ) ) ;
#57907 = CARTESIAN_POINT ( 'NONE',  ( -3.535250795749689387E-16, -60.25000000000000000, -5.773502691896257311 ) ) ;
#57908 = EDGE_CURVE ( 'NONE', #20484, #40086, #31673, .T. ) ;
#57909 = CARTESIAN_POINT ( 'NONE',  ( -4.458734124999999437, -155.1875000013655779, -5.460374474430324690E-16 ) ) ;
#57910 = CARTESIAN_POINT ( 'NONE',  ( -3.152548672688508926E-16, -40.81249999863440081, -5.148502694627439702 ) ) ;
#57911 = LINE ( 'NONE', #48555, #38870 ) ;
#57912 = CARTESIAN_POINT ( 'NONE',  ( -5.000000000000000000, -165.5000000000000000, -6.123233995736766282E-16 ) ) ;
#57913 = EDGE_CURVE ( 'NONE', #59810, #29588, #14140, .T. ) ;
#57914 = CARTESIAN_POINT ( 'NONE',  ( -6.972266317189433020E-16, 5.875000002731184168, -5.000000000000000000 ) ) ;
#57915 = CARTESIAN_POINT ( 'NONE',  ( -59.44456063193725015, -131.8125000013656063, -0.3552334253322034230 ) ) ;
#57916 = CARTESIAN_POINT ( 'NONE',  ( -3.152548672688508926E-16, -3.812499998634408360, -5.148502694627439702 ) ) ;
#57917 = CARTESIAN_POINT ( 'NONE',  ( -4.458734124999999437, -39.56249999863440081, 0.000000000000000000 ) ) ;
#57918 = VECTOR ( 'NONE', #6747, 1000.000000000000000 ) ;
#57919 = ADVANCED_FACE ( 'NONE', ( #8807 ), #24224, .T. ) ;
#57920 = DIRECTION ( 'NONE',  ( -0.000000000000000000, 1.000000000000000000, -0.000000000000000000 ) ) ;
#57921 = CARTESIAN_POINT ( 'NONE',  ( 3.152801135295366208, -149.5625000013655779, 3.152801135295367985 ) ) ;
#57922 = CARTESIAN_POINT ( 'NONE',  ( -2.229367062499996610, -84.39583333196773651, 3.861377020970582219 ) ) ;
#57923 = CARTESIAN_POINT ( 'NONE',  ( 5.000000000000000000, -34.29166666393547303, -2.886751345948130876 ) ) ;
#57924 = VERTEX_POINT ( 'NONE', #4926 ) ;
#57925 = PRODUCT_DEFINITION_SHAPE ( 'NONE', 'NONE',  #63682 ) ;
#57926 = CARTESIAN_POINT ( 'NONE',  ( -59.81910112700025905, -150.3125000027312410, -2.462841084822630311 ) ) ;
#57927 = CARTESIAN_POINT ( 'NONE',  ( 5.000000000000000000, -2.374999997268815388, -6.123233995736766282E-16 ) ) ;
#57928 = CARTESIAN_POINT ( 'NONE',  ( 2.229367062499998831, -75.89583333196773651, -3.861377020970580887 ) ) ;
#57929 = ORIENTED_EDGE ( 'NONE', *, *, #11857, .T. ) ;
#57930 = CARTESIAN_POINT ( 'NONE',  ( 1.975475456537005874E-15, -78.74999999999998579, 5.000000000000000000 ) ) ;
#57931 = CARTESIAN_POINT ( 'NONE',  ( 4.458734124999998549, -9.979166665301068662, -2.574251347313721627 ) ) ;
#57932 = DIRECTION ( 'NONE',  ( -0.000000000000000000, 1.000000000000000000, -0.000000000000000000 ) ) ;
#57933 = CARTESIAN_POINT ( 'NONE',  ( -4.458734124999998549, 0.7708333346989267865, 2.574251347313722516 ) ) ;
#57934 = CARTESIAN_POINT ( 'NONE',  ( -5.000000000000000000, -11.87499999726881761, 0.000000000000000000 ) ) ;
#57935 = CARTESIAN_POINT ( 'NONE',  ( 2.730187237215162345E-16, -151.1875000013656063, -4.458734124999999437 ) ) ;
#57936 =( BOUNDED_CURVE ( )  B_SPLINE_CURVE ( 2, ( #6453, #60803, #15774, #26062, #11577, #6131, #26700, #31197, #15460 ),
 .UNSPECIFIED., .F., .F. ) 
 B_SPLINE_CURVE_WITH_KNOTS ( ( 3, 2, 2, 2, 3 ),
 ( 0.9770833333333333037, 0.9777777777777777457, 0.9791666666666666297, 0.9805555555555555136, 0.9812499999999999556 ),
 .UNSPECIFIED. ) 
 CURVE ( )  GEOMETRIC_REPRESENTATION_ITEM ( )  RATIONAL_B_SPLINE_CURVE ( ( 0.9330127018922194093, 0.9330127018922194093, 1.000000000000000000, 0.8660254037844387076, 1.000000000000000000, 0.8660254037844387076, 1.000000000000000000, 0.9330127018922194093, 0.9330127018922194093 ) ) 
 REPRESENTATION_ITEM ( '' )  );
#57937 = CARTESIAN_POINT ( 'NONE',  ( -2.229367062499996610, 22.60416666803225993, 3.861377020970582219 ) ) ;
#57938 = ORIENTED_EDGE ( 'NONE', *, *, #29400, .F. ) ;
#57939 = CARTESIAN_POINT ( 'NONE',  ( -4.458734124999999437, -89.39583333196773651, -2.574251347313719407 ) ) ;
#57940 = CARTESIAN_POINT ( 'NONE',  ( 5.000000000000000000, -47.50000000000000000, -6.123233995736766282E-16 ) ) ;
#57941 = CARTESIAN_POINT ( 'NONE',  ( 1.339745962155612702, -12.16965819600733667, -5.000000000000000000 ) ) ;
#57942 = CARTESIAN_POINT ( 'NONE',  ( 9.457646018065525792E-16, -10.06249999863440792, 5.148502694627439702 ) ) ;
#57943 = CARTESIAN_POINT ( 'NONE',  ( 1.975475456537005874E-15, -2.624999997268813168, 5.000000000000000000 ) ) ;
#57944 = LINE ( 'NONE', #47957, #2727 ) ;
#57945 = CARTESIAN_POINT ( 'NONE',  ( -51.60603307380591787, -151.9375000013656063, -2.891590998281053704 ) ) ;
#57946 = CARTESIAN_POINT ( 'NONE',  ( 2.500000000000002220, -34.54166666393547303, 4.330127018922192761 ) ) ;
#57947 = CARTESIAN_POINT ( 'NONE',  ( 1.975475456537005874E-15, -64.62499999726880162, 5.000000000000000000 ) ) ;
#57948 = CARTESIAN_POINT ( 'NONE',  ( -3.152548672688508926E-16, 19.43750000136559208, -5.148502694627439702 ) ) ;
#57949 = CARTESIAN_POINT ( 'NONE',  ( 5.000000000000000888, -44.58333333333333570, 2.886751345948126879 ) ) ;
#57950 = CARTESIAN_POINT ( 'NONE',  ( -2.229367062499996610, 21.85416666803226349, 3.861377020970582219 ) ) ;
#57951 = CARTESIAN_POINT ( 'NONE',  ( -4.458734124999999437, -55.39583333196773651, -2.574251347313719407 ) ) ;
#57952 = CARTESIAN_POINT ( 'NONE',  ( -4.458734124999997661, -6.479166665301072214, 2.574251347313722516 ) ) ;
#57953 = CARTESIAN_POINT ( 'NONE',  ( 0.000000000000000000, -170.0000000000000000, 0.000000000000000000 ) ) ;
#57954 = CARTESIAN_POINT ( 'NONE',  ( -2.499999999999996447, 10.16666666666666785, 4.330127018922195425 ) ) ;
#57955 = CARTESIAN_POINT ( 'NONE',  ( 3.152801135295367541, -166.3125000013656063, -3.152801135295367541 ) ) ;
#57956 = CARTESIAN_POINT ( 'NONE',  ( 1.339745962155612702, -69.29465819873850307, -5.000000000000000000 ) ) ;
#57957 = CARTESIAN_POINT ( 'NONE',  ( 4.458734124999999437, -46.81249999863440792, -5.460374474430324690E-16 ) ) ;
#57958 = CARTESIAN_POINT ( 'NONE',  ( 5.000000000000000888, -83.45833333060213022, 2.886751345948126879 ) ) ;
#57959 = CARTESIAN_POINT ( 'NONE',  ( -59.59170313451811296, -134.7500000013656063, 1.485763867205729394 ) ) ;
#57960 = DIRECTION ( 'NONE',  ( -0.000000000000000000, 1.000000000000000000, -0.000000000000000000 ) ) ;
#57961 = CYLINDRICAL_SURFACE ( 'NONE', #18276, 5.000000000000000000 ) ;
#57962 = CARTESIAN_POINT ( 'NONE',  ( 4.458734125000000326, -92.14583333196773651, 2.574251347313718519 ) ) ;
#57963 = CARTESIAN_POINT ( 'NONE',  ( -3.152801135295367096, -156.3125000013656063, -3.152801135295367541 ) ) ;
#57964 = CARTESIAN_POINT ( 'NONE',  ( 2.500000000000002220, -38.66666666666667140, 4.330127018922192761 ) ) ;
#57965 = CARTESIAN_POINT ( 'NONE',  ( -59.00781279294024984, -134.9999999999999432, -2.380179661103284161 ) ) ;
#57966 = ORIENTED_EDGE ( 'NONE', *, *, #6409, .F. ) ;
#57967 = CARTESIAN_POINT ( 'NONE',  ( -2.229367062500000163, -97.47916666530105090, -3.861377020970580443 ) ) ;
#57968 = CARTESIAN_POINT ( 'NONE',  ( 4.458734124999999437, 10.93750000136559386, -5.460374474430324690E-16 ) ) ;
#57969 = CARTESIAN_POINT ( 'NONE',  ( 5.000000000000000000, 11.70833333606451809, -2.886751345948129988 ) ) ;
#57970 = CARTESIAN_POINT ( 'NONE',  ( -6.972266317189433020E-16, -88.12499999726880162, -5.000000000000000000 ) ) ;
#57971 = CARTESIAN_POINT ( 'NONE',  ( 5.000000000000000000, 1.500000000000001332, -6.123233995736766282E-16 ) ) ;
#57972 = CARTESIAN_POINT ( 'NONE',  ( -4.458734124999999437, -60.39583333196774362, -2.574251347313719407 ) ) ;
#57973 = CARTESIAN_POINT ( 'NONE',  ( -2.499999999999996447, 1.291666669397853351, 4.330127018922195425 ) ) ;
#57974 = CARTESIAN_POINT ( 'NONE',  ( -4.458734124999999437, -29.39583333196773296, -2.574251347313719407 ) ) ;
#57975 = CARTESIAN_POINT ( 'NONE',  ( -58.80597590150559739, -144.1250000027312126, 3.242614290531460330 ) ) ;
#57976 = CARTESIAN_POINT ( 'NONE',  ( 1.339745962155612702, 19.70534180126147561, -5.000000000000000000 ) ) ;
#57977 = CARTESIAN_POINT ( 'NONE',  ( 1.339745962155615144, -19.70534180126147561, 4.999999999999999112 ) ) ;
#57978 = CARTESIAN_POINT ( 'NONE',  ( -2.499999999999996447, -45.83333333333333570, 4.330127018922195425 ) ) ;
#57980 = CARTESIAN_POINT ( 'NONE',  ( 4.458734124999998549, -21.97916666530107221, -2.574251347313721627 ) ) ;
#57979 = CARTESIAN_POINT ( 'NONE',  ( -1.336351044127974539E-14, 24.37500000273118417, 5.000000000000000000 ) ) ;
#57981 = CARTESIAN_POINT ( 'NONE',  ( 5.000000000000000000, -155.0625000000000284, 2.071067811865478614 ) ) ;
#57982 = CARTESIAN_POINT ( 'NONE',  ( 4.458734125000001214, -68.89583333196773651, 2.574251347313718519 ) ) ;
#57983 = CARTESIAN_POINT ( 'NONE',  ( 2.730187237215162345E-16, -149.4375000013656063, -4.458734124999999437 ) ) ;
#57984 = CARTESIAN_POINT ( 'NONE',  ( -4.458734124999999437, -74.31249999863440792, 0.000000000000000000 ) ) ;
#57985 = CARTESIAN_POINT ( 'NONE',  ( -51.60603307380591787, -144.1875000013656063, -2.891590998281053704 ) ) ;
#57986 = CARTESIAN_POINT ( 'NONE',  ( -2.229367062499996610, -23.39583333196773651, 3.861377020970582219 ) ) ;
#57987 = CARTESIAN_POINT ( 'NONE',  ( 5.000000000000000000, -65.29166666393548724, -2.886751345948129988 ) ) ;
#57988 = ORIENTED_EDGE ( 'NONE', *, *, #20766, .T. ) ;
#57989 = CARTESIAN_POINT ( 'NONE',  ( -5.000000000000000000, -152.6250000027312126, -6.123233995736766282E-16 ) ) ;
#57990 = ORIENTED_EDGE ( 'NONE', *, *, #20223, .F. ) ;
#57991 = CARTESIAN_POINT ( 'NONE',  ( 4.458734125000001214, -68.14583333196773651, 2.574251347313718519 ) ) ;
#57992 = CARTESIAN_POINT ( 'NONE',  ( -6.972266317189433020E-16, -82.12499999726881583, -5.000000000000000000 ) ) ;
#57993 = DIRECTION ( 'NONE',  ( 0.000000000000000000, 0.000000000000000000, 1.000000000000000000 ) ) ;
#57994 = ORIENTED_EDGE ( 'NONE', *, *, #15760, .F. ) ;
#57995 = CARTESIAN_POINT ( 'NONE',  ( -2.499999999999996447, -82.83333333333332860, 4.330127018922195425 ) ) ;
#57996 = CARTESIAN_POINT ( 'NONE',  ( -4.458734124999999437, -52.56249999863440792, 0.000000000000000000 ) ) ;
#57997 = CARTESIAN_POINT ( 'NONE',  ( 4.458734124999999437, 3.937500001365595192, -5.460374474430324690E-16 ) ) ;
#57998 = ORIENTED_EDGE ( 'NONE', *, *, #17229, .T. ) ;
#57999 = VECTOR ( 'NONE', #61246, 1000.000000000000000 ) ;
#58000 = CARTESIAN_POINT ( 'NONE',  ( 3.061616997868383141E-16, -141.7500000000000284, -5.000000000000000000 ) ) ;
#58001 = CARTESIAN_POINT ( 'NONE',  ( 4.458734124999999437, 20.18750000136559208, -5.460374474430324690E-16 ) ) ;
#58002 = CARTESIAN_POINT ( 'NONE',  ( -57.19623071787017210, -144.3750000013656063, 4.297418129356382899 ) ) ;
#58003 = CARTESIAN_POINT ( 'NONE',  ( 6.123233995736766282E-16, -170.0000000000000000, -5.000000000000000000 ) ) ;
#58004 = CARTESIAN_POINT ( 'NONE',  ( 4.458734124999999437, -166.4375000013655779, 0.000000000000000000 ) ) ;
#58005 = ORIENTED_EDGE ( 'NONE', *, *, #48798, .F. ) ;
#58006 = CARTESIAN_POINT ( 'NONE',  ( -4.458734124999999437, -74.31249999863440792, 0.000000000000000000 ) ) ;
#58007 = CARTESIAN_POINT ( 'NONE',  ( -5.000000000000000888, -153.5625000000000853, -2.071067811865475949 ) ) ;
#58008 = CARTESIAN_POINT ( 'NONE',  ( -3.152548672688508926E-16, 9.437500001365593860, -5.148502694627439702 ) ) ;
#58009 =( BOUNDED_CURVE ( )  B_SPLINE_CURVE ( 2, ( #24844, #25154, #58931, #23034, #39618, #58308, #15187, #34163, #33857 ),
 .UNSPECIFIED., .F., .F. ) 
 B_SPLINE_CURVE_WITH_KNOTS ( ( 3, 2, 2, 2, 3 ),
 ( 0.1062499999999999972, 0.1069444444444444392, 0.1083333333333333370, 0.1097222222222222210, 0.1104166666666666630 ),
 .UNSPECIFIED. ) 
 CURVE ( )  GEOMETRIC_REPRESENTATION_ITEM ( )  RATIONAL_B_SPLINE_CURVE ( ( 0.9330127018922194093, 0.9330127018922194093, 1.000000000000000000, 0.8660254037844387076, 1.000000000000000000, 0.8660254037844387076, 1.000000000000000000, 0.9330127018922194093, 0.9330127018922194093 ) ) 
 REPRESENTATION_ITEM ( '' )  );
#58010 = LINE ( 'NONE', #13936, #14079 ) ;
#58011 = CARTESIAN_POINT ( 'NONE',  ( 4.458734124999999437, -60.06249999863440081, -5.460374474430324690E-16 ) ) ;
#58012 = CARTESIAN_POINT ( 'NONE',  ( -2.500000000000000444, -19.04166666393547658, -4.330127018922193649 ) ) ;
#58013 = CARTESIAN_POINT ( 'NONE',  ( 1.339745962155615144, -20.70534180126147916, 4.999999999999999112 ) ) ;
#58014 = DIRECTION ( 'NONE',  ( -0.000000000000000000, 1.000000000000000000, -0.000000000000000000 ) ) ;
#58015 = CARTESIAN_POINT ( 'NONE',  ( -1.339745962155610925, -58.79465819873852439, 5.000000000000000000 ) ) ;
#58016 = CARTESIAN_POINT ( 'NONE',  ( -4.458734124999999437, -41.39583333196773651, -2.574251347313719407 ) ) ;
#58017 = CARTESIAN_POINT ( 'NONE',  ( 2.229367062500001939, -29.22916666530107221, 3.861377020970579999 ) ) ;
#58018 = CARTESIAN_POINT ( 'NONE',  ( 2.499999999999998668, 11.66666666666666607, -4.330127018922193649 ) ) ;
#58019 = CARTESIAN_POINT ( 'NONE',  ( -5.000000000000000000, 24.00000000000000000, 0.000000000000000000 ) ) ;
#58020 = CARTESIAN_POINT ( 'NONE',  ( -5.000000000000000888, -148.5625000027312126, 2.071067811865474617 ) ) ;
#58021 = CARTESIAN_POINT ( 'NONE',  ( 2.229367062499998831, -106.8958333319677365, -3.861377020970580887 ) ) ;
#58022 = CARTESIAN_POINT ( 'NONE',  ( -3.152548672688508926E-16, -32.56249999863440792, -5.148502694627439702 ) ) ;
#58023 = CARTESIAN_POINT ( 'NONE',  ( 2.499999999999998668, -67.20833333060214443, -4.330127018922193649 ) ) ;
#58024 = CARTESIAN_POINT ( 'NONE',  ( -52.80376928212989185, -148.1250000013656063, -4.297418129356379346 ) ) ;
#58025 = CARTESIAN_POINT ( 'NONE',  ( 3.535533905932738197, -144.8750000000000000, -3.535533905932738197 ) ) ;
#58026 = CARTESIAN_POINT ( 'NONE',  ( -2.229367062499996610, -77.39583333196773651, 3.861377020970582219 ) ) ;
#58027 = CARTESIAN_POINT ( 'NONE',  ( -4.458734124999999437, -169.1875000013656063, -5.460374474430324690E-16 ) ) ;
#58028 = CARTESIAN_POINT ( 'NONE',  ( 4.458734124999999437, -30.81249999863440436, -5.460374474430324690E-16 ) ) ;
#58029 = CYLINDRICAL_SURFACE ( 'NONE', #60575, 5.000000000000000000 ) ;
#58030 = CARTESIAN_POINT ( 'NONE',  ( -2.499999999999996447, -19.83333333333333570, 4.330127018922195425 ) ) ;
#58031 = CARTESIAN_POINT ( 'NONE',  ( -4.458734124999999437, -146.9375000013656063, -5.460374474430324690E-16 ) ) ;
#58032 = EDGE_LOOP ( 'NONE', ( #30105, #29875, #32030, #46340 ) ) ;
#58033 = CARTESIAN_POINT ( 'NONE',  ( -4.999999999999999112, -89.79166666393547303, 2.886751345948131764 ) ) ;
#58034 = CARTESIAN_POINT ( 'NONE',  ( 2.500000000000002220, -16.54166666393548368, 4.330127018922192761 ) ) ;
#58035 = CARTESIAN_POINT ( 'NONE',  ( -3.152548672688508926E-16, -54.81249999863440081, -5.148502694627439702 ) ) ;
#58036 = CARTESIAN_POINT ( 'NONE',  ( -2.500000000000000444, 26.95833333606451632, -4.330127018922193649 ) ) ;
#58037 = CARTESIAN_POINT ( 'NONE',  ( 5.000000000000000000, 4.625000002731187720, -6.123233995736766282E-16 ) ) ;
#58038 = CARTESIAN_POINT ( 'NONE',  ( -2.500000000000000444, 20.83333333333333215, -4.330127018922193649 ) ) ;
#58039 = DIRECTION ( 'NONE',  ( 0.000000000000000000, 0.000000000000000000, 1.000000000000000000 ) ) ;
#58040 = AXIS2_PLACEMENT_3D ( 'NONE', #19929, #44689, #15114 ) ;
#58041 = CARTESIAN_POINT ( 'NONE',  ( 2.229367062500001939, -7.979166665301073991, 3.861377020970579999 ) ) ;
#58042 = CARTESIAN_POINT ( 'NONE',  ( 2.500000000000002220, -48.66666666666666430, 4.330127018922192761 ) ) ;
#58043 = CARTESIAN_POINT ( 'NONE',  ( -4.999999999999998224, -76.91666666666667140, 2.886751345948131764 ) ) ;
#58044 = CARTESIAN_POINT ( 'NONE',  ( 2.229367062499998831, 12.10416666803226171, -3.861377020970580887 ) ) ;
#58045 = CARTESIAN_POINT ( 'NONE',  ( 5.000000000000000888, -53.45833333060213732, 2.886751345948126879 ) ) ;
#58046 = ORIENTED_EDGE ( 'NONE', *, *, #5012, .T. ) ;
#58047 = CARTESIAN_POINT ( 'NONE',  ( 5.000000000000000000, -97.29166666393547303, -2.886751345948130876 ) ) ;
#58048 = CARTESIAN_POINT ( 'NONE',  ( -4.458734124999998549, -50.22916666530107221, 2.574251347313722516 ) ) ;
#58049 = CARTESIAN_POINT ( 'NONE',  ( -8.190561711645485556E-16, -161.9375000013655779, 4.458734124999999437 ) ) ;
#58050 = CARTESIAN_POINT ( 'NONE',  ( -2.499999999999996447, -49.70833333060213732, 4.330127018922195425 ) ) ;
#58051 = ORIENTED_EDGE ( 'NONE', *, *, #62887, .F. ) ;
#58052 = CARTESIAN_POINT ( 'NONE',  ( -2.229367062499996610, -24.14583333196773651, 3.861377020970582219 ) ) ;
#58053 = ORIENTED_EDGE ( 'NONE', *, *, #26206, .F. ) ;
#58054 =( BOUNDED_CURVE ( )  B_SPLINE_CURVE ( 2, ( #17105, #42176, #22891, #57309, #61183, #51528, #2637, #27700, #3279 ),
 .UNSPECIFIED., .F., .F. ) 
 B_SPLINE_CURVE_WITH_KNOTS ( ( 3, 2, 2, 2, 3 ),
 ( 0.2937500000000000111, 0.2944444444444444531, 0.2958333333333333370, 0.2972222222222222210, 0.2979166666666666630 ),
 .UNSPECIFIED. ) 
 CURVE ( )  GEOMETRIC_REPRESENTATION_ITEM ( )  RATIONAL_B_SPLINE_CURVE ( ( 0.9330127018922194093, 0.9330127018922194093, 1.000000000000000000, 0.8660254037844387076, 1.000000000000000000, 0.8660254037844387076, 1.000000000000000000, 0.9330127018922194093, 0.9330127018922194093 ) ) 
 REPRESENTATION_ITEM ( '' )  );
#58056 = CARTESIAN_POINT ( 'NONE',  ( 1.975475456537005874E-15, -102.6249999972688158, 5.000000000000000000 ) ) ;
#58055 = CARTESIAN_POINT ( 'NONE',  ( 6.123233995736766282E-16, -170.0000000000000000, -5.000000000000000000 ) ) ;
#58057 = CARTESIAN_POINT ( 'NONE',  ( -4.458734125000001214, -158.8750000013655779, 1.846868145590734089 ) ) ;
#58058 = VERTEX_POINT ( 'NONE', #63476 ) ;
#58059 = CARTESIAN_POINT ( 'NONE',  ( -5.000000000000000000, -38.95833333060214443, -2.886751345948128211 ) ) ;
#58060 = CARTESIAN_POINT ( 'NONE',  ( -58.80597590150559739, -132.0000000000000284, 3.242614290531460330 ) ) ;
#58061 = CARTESIAN_POINT ( 'NONE',  ( -6.972266317189433020E-16, -20.24999999999999645, -5.000000000000000000 ) ) ;
#58062 = CARTESIAN_POINT ( 'NONE',  ( 4.458734124999999437, -38.06249999863440792, -5.460374474430324690E-16 ) ) ;
#58063 = EDGE_LOOP ( 'NONE', ( #13367, #2635, #51301, #22935 ) ) ;
#58064 = CARTESIAN_POINT ( 'NONE',  ( 9.457646018065525792E-16, -80.06249999863439371, 5.148502694627439702 ) ) ;
#58065 = CARTESIAN_POINT ( 'NONE',  ( -4.458734124999999437, 21.68750000136559208, 0.000000000000000000 ) ) ;
#58066 = CARTESIAN_POINT ( 'NONE',  ( -2.500000000000000444, -18.04166666393547658, -4.330127018922193649 ) ) ;
#58067 = EDGE_LOOP ( 'NONE', ( #7907, #20980, #57216, #57763 ) ) ;
#58068 = CARTESIAN_POINT ( 'NONE',  ( 2.229367062500001939, -85.22916666530107932, 3.861377020970579999 ) ) ;
#58069 = CARTESIAN_POINT ( 'NONE',  ( -60.14911071818854538, -126.1875000027312410, 1.666127454062681368 ) ) ;
#58070 = CARTESIAN_POINT ( 'NONE',  ( 1.339745962155615144, -74.58034179853031276, 4.999999999999999112 ) ) ;
#58071 = CARTESIAN_POINT ( 'NONE',  ( -50.55945893837505167, -135.0000000000000568, 1.298165042310468031 ) ) ;
#58072 = CARTESIAN_POINT ( 'NONE',  ( -4.999999999999998224, -44.79166666393547303, 2.886751345948131764 ) ) ;
#58073 = CARTESIAN_POINT ( 'NONE',  ( 2.229367062499998831, -57.64583333196773651, -3.861377020970580887 ) ) ;
#58074 = CARTESIAN_POINT ( 'NONE',  ( 1.339745962155615144, 10.29465819873852084, 4.999999999999999112 ) ) ;
#58075 = CARTESIAN_POINT ( 'NONE',  ( -2.229367062500000163, 24.52083333469892779, -3.861377020970580443 ) ) ;
#58076 = ADVANCED_FACE ( 'NONE', ( #43206 ), #48660, .T. ) ;
#58077 = DIRECTION ( 'NONE',  ( 0.000000000000000000, 1.000000000000000000, 0.000000000000000000 ) ) ;
#58078 = VECTOR ( 'NONE', #57634, 1000.000000000000000 ) ;
#58079 = LINE ( 'NONE', #48728, #54584 ) ;
#58080 = CARTESIAN_POINT ( 'NONE',  ( -4.458734124999999437, -43.64583333196774362, -2.574251347313719407 ) ) ;
#58081 = CARTESIAN_POINT ( 'NONE',  ( -5.000000000000000000, -2.874999997268815832, 0.000000000000000000 ) ) ;
#58082 = CARTESIAN_POINT ( 'NONE',  ( 1.975475456537005874E-15, -69.74999999999998579, 5.000000000000000000 ) ) ;
#58083 = CARTESIAN_POINT ( 'NONE',  ( 4.458734124999999437, -84.06249999863439371, -5.460374474430324690E-16 ) ) ;
#58084 = CARTESIAN_POINT ( 'NONE',  ( 2.229367062499998831, -106.6458333319677365, -3.861377020970580887 ) ) ;
#58085 = CARTESIAN_POINT ( 'NONE',  ( 2.229367062499998831, -10.89583333196773829, -3.861377020970580887 ) ) ;
#58086 = ORIENTED_EDGE ( 'NONE', *, *, #37086, .T. ) ;
#58087 = CARTESIAN_POINT ( 'NONE',  ( -4.999999999999998224, 18.20833333606451632, 2.886751345948131764 ) ) ;
#58088 = CARTESIAN_POINT ( 'NONE',  ( 4.458734124999999437, -100.8124999986344079, -5.460374474430324690E-16 ) ) ;
#58089 = CARTESIAN_POINT ( 'NONE',  ( -3.535533905932738641, -163.5000000027312126, 3.535533905932737309 ) ) ;
#58090 = CARTESIAN_POINT ( 'NONE',  ( 2.229367062500001939, -92.22916666530106511, 3.861377020970579999 ) ) ;
#58091 = CARTESIAN_POINT ( 'NONE',  ( 1.060575238724906964E-15, -54.62499999726880873, 5.773502691896257311 ) ) ;
#58092 = CARTESIAN_POINT ( 'NONE',  ( -5.000000000000000000, -30.00000000000000000, 0.000000000000000000 ) ) ;
#58093 = CARTESIAN_POINT ( 'NONE',  ( -59.59170313451811296, -131.5000000013656347, 1.485763867205729394 ) ) ;
#58094 = ADVANCED_FACE ( 'NONE', ( #4601 ), #28423, .T. ) ;
#58095 = CARTESIAN_POINT ( 'NONE',  ( -59.44456063193725015, -145.5625000013656063, -0.3552334253322034230 ) ) ;
#58096 = CARTESIAN_POINT ( 'NONE',  ( -2.229367062500000163, -10.47916666530106866, -3.861377020970580443 ) ) ;
#58097 = CARTESIAN_POINT ( 'NONE',  ( -2.229367062499996610, 11.60416666803225993, 3.861377020970582219 ) ) ;
#58098 = ADVANCED_FACE ( 'NONE', ( #4298 ), #38691, .T. ) ;
#58099 = CARTESIAN_POINT ( 'NONE',  ( 4.458734125000000326, -60.14583333196774362, 2.574251347313718519 ) ) ;
#58100 = CARTESIAN_POINT ( 'NONE',  ( -1.339745962155613812, -69.20534180126148271, -5.000000000000000000 ) ) ;
#58101 = CARTESIAN_POINT ( 'NONE',  ( 9.457646018065525792E-16, -15.06249999863440259, 5.148502694627439702 ) ) ;
#58102 = CARTESIAN_POINT ( 'NONE',  ( 1.975475456537005874E-15, -106.6249999972687874, 5.000000000000000000 ) ) ;
#58103 = ORIENTED_EDGE ( 'NONE', *, *, #23608, .T. ) ;
#58104 = CARTESIAN_POINT ( 'NONE',  ( 4.458734125000000326, -39.14583333196773651, 2.574251347313718519 ) ) ;
#58105 =( BOUNDED_CURVE ( )  B_SPLINE_CURVE ( 2, ( #62131, #42810, #43433, #32853, #3592, #38603, #33791, #61821, #56993 ),
 .UNSPECIFIED., .F., .F. ) 
 B_SPLINE_CURVE_WITH_KNOTS ( ( 3, 2, 2, 2, 3 ),
 ( 0.4937500000000000222, 0.4944444444444444642, 0.4958333333333333481, 0.4972222222222222321, 0.4979166666666666741 ),
 .UNSPECIFIED. ) 
 CURVE ( )  GEOMETRIC_REPRESENTATION_ITEM ( )  RATIONAL_B_SPLINE_CURVE ( ( 0.9330127018922194093, 0.9330127018922194093, 1.000000000000000000, 0.8660254037844387076, 1.000000000000000000, 0.8660254037844387076, 1.000000000000000000, 0.9330127018922194093, 0.9330127018922194093 ) ) 
 REPRESENTATION_ITEM ( '' )  );
#58106 = CARTESIAN_POINT ( 'NONE',  ( 1.339745962155612702, -77.29465819873853150, -5.000000000000000000 ) ) ;
#58107 = CARTESIAN_POINT ( 'NONE',  ( -5.000000000000000000, -12.08333333333333570, -2.886751345948128211 ) ) ;
#58108 = CARTESIAN_POINT ( 'NONE',  ( -2.499999999999996447, -24.83333333333333215, 4.330127018922195425 ) ) ;
#58109 = CARTESIAN_POINT ( 'NONE',  ( 2.229367062499998831, -83.64583333196773651, -3.861377020970580887 ) ) ;
#58110 = CARTESIAN_POINT ( 'NONE',  ( -3.152548672688508926E-16, 17.18750000136559919, -5.148502694627439702 ) ) ;
#58111 = CARTESIAN_POINT ( 'NONE',  ( -3.152548672688508926E-16, 9.437500001365593860, -5.148502694627439702 ) ) ;
#58112 = CARTESIAN_POINT ( 'NONE',  ( -1.339745962155610925, -81.66965819600736154, 5.000000000000000000 ) ) ;
#58113 = CARTESIAN_POINT ( 'NONE',  ( -58.24261429053147765, -137.3750000027312126, -3.805975901505573855 ) ) ;
#58114 = CARTESIAN_POINT ( 'NONE',  ( -4.458734124999999437, -90.56249999863440792, 0.000000000000000000 ) ) ;
#58115 = CARTESIAN_POINT ( 'NONE',  ( 1.060575238724906964E-15, -71.75000000000000000, 5.773502691896257311 ) ) ;
#58116 = CARTESIAN_POINT ( 'NONE',  ( -4.999999999999999112, 13.20833333606451809, 2.886751345948131764 ) ) ;
#58117 = ORIENTED_EDGE ( 'NONE', *, *, #31908, .T. ) ;
#58118 = CARTESIAN_POINT ( 'NONE',  ( 5.000000000000000888, -79.58333333333332860, 2.886751345948126879 ) ) ;
#58119 = ORIENTED_EDGE ( 'NONE', *, *, #32997, .T. ) ;
#58120 = CARTESIAN_POINT ( 'NONE',  ( 3.535533905932738197, -166.8750000000000284, -3.535533905932738197 ) ) ;
#58122 = CARTESIAN_POINT ( 'NONE',  ( 2.500000000000002220, -28.66666666666666785, 4.330127018922192761 ) ) ;
#58121 = CARTESIAN_POINT ( 'NONE',  ( 1.975475456537005874E-15, -70.75000000000000000, 5.000000000000000000 ) ) ;
#58123 = CARTESIAN_POINT ( 'NONE',  ( 9.457646018065525792E-16, -34.06249999863440792, 5.148502694627439702 ) ) ;
#58124 = CARTESIAN_POINT ( 'NONE',  ( 2.499999999999998668, -34.20833333060213732, -4.330127018922193649 ) ) ;
#58125 = EDGE_CURVE ( 'NONE', #62202, #57126, #40443, .T. ) ;
#58127 = ORIENTED_EDGE ( 'NONE', *, *, #49085, .F. ) ;
#58126 = CARTESIAN_POINT ( 'NONE',  ( -3.152548672688508926E-16, -68.56249999863439371, -5.148502694627439702 ) ) ;
#58128 = CARTESIAN_POINT ( 'NONE',  ( -52.10840900171896806, -150.4375000013656063, 3.393966926194110556 ) ) ;
#58130 = ORIENTED_EDGE ( 'NONE', *, *, #27592, .T. ) ;
#58129 = CARTESIAN_POINT ( 'NONE',  ( 2.229367062500001939, -13.22916666530107221, 3.861377020970579999 ) ) ;
#58131 = CARTESIAN_POINT ( 'NONE',  ( 2.499999999999998668, -78.33333333333332860, -4.330127018922193649 ) ) ;
#58132 = CARTESIAN_POINT ( 'NONE',  ( -59.44456063193725015, -136.5625000013656063, -0.3552334253322034230 ) ) ;
#58133 = CARTESIAN_POINT ( 'NONE',  ( -4.458734124999998549, -58.47916666530106511, 2.574251347313722516 ) ) ;
#58134 = CARTESIAN_POINT ( 'NONE',  ( -3.535250795749689387E-16, -84.12499999726880162, -5.773502691896257311 ) ) ;
#58136 = EDGE_LOOP ( 'NONE', ( #43735, #923, #35749, #52540 ) ) ;
#58135 = CARTESIAN_POINT ( 'NONE',  ( 1.975475456537005874E-15, 10.37500000273118417, 5.000000000000000000 ) ) ;
#58137 = CARTESIAN_POINT ( 'NONE',  ( -50.01589407740564042, -145.6250000000000284, 0.3983568153799778022 ) ) ;
#58138 = CARTESIAN_POINT ( 'NONE',  ( -4.458734124999999437, -23.56249999863440436, 0.000000000000000000 ) ) ;
#58140 = EDGE_LOOP ( 'NONE', ( #32011, #28300, #59322, #10116 ) ) ;
#58139 = CARTESIAN_POINT ( 'NONE',  ( -4.458734124999999437, -60.64583333196774362, -2.574251347313719407 ) ) ;
#58141 = DIRECTION ( 'NONE',  ( 1.000000000000000000, 0.000000000000000000, 0.000000000000000000 ) ) ;
#58142 = CARTESIAN_POINT ( 'NONE',  ( -4.458734124999999437, -168.1875000013655779, -5.460374474430324690E-16 ) ) ;
#58143 = CARTESIAN_POINT ( 'NONE',  ( -2.229367062500000163, -103.7291666653010651, -3.861377020970580443 ) ) ;
#58144 = CARTESIAN_POINT ( 'NONE',  ( -55.39835672516371545, -134.9999999999999716, 4.984105929804953483 ) ) ;
#58145 = ORIENTED_EDGE ( 'NONE', *, *, #60733, .F. ) ;
#58146 = CARTESIAN_POINT ( 'NONE',  ( -57.89159099828107458, -149.9375000013656063, -3.393966926194107447 ) ) ;
#58147 = CARTESIAN_POINT ( 'NONE',  ( -59.81910112700025905, -140.3125000027312126, -2.462841084822630311 ) ) ;
#58148 = CARTESIAN_POINT ( 'NONE',  ( -4.458734124999997661, -40.22916666530107932, 2.574251347313722516 ) ) ;
#58149 = DIRECTION ( 'NONE',  ( -0.000000000000000000, 1.000000000000000000, -0.000000000000000000 ) ) ;
#58150 = EDGE_CURVE ( 'NONE', #54054, #52029, #62542, .T. ) ;
#58151 = CARTESIAN_POINT ( 'NONE',  ( 2.229367062500001939, -13.97916666530107221, 3.861377020970579999 ) ) ;
#58152 = CARTESIAN_POINT ( 'NONE',  ( 2.229367062499998831, -100.8958333319677365, -3.861377020970580887 ) ) ;
#58153 = CARTESIAN_POINT ( 'NONE',  ( 3.152801135295366208, -142.8125000013655779, 3.152801135295367985 ) ) ;
#58154 = CARTESIAN_POINT ( 'NONE',  ( -3.152548672688508926E-16, -26.81249999863440436, -5.148502694627439702 ) ) ;
#58155 = CARTESIAN_POINT ( 'NONE',  ( -58.24261429053147765, -153.2500000000000284, -3.805975901505573855 ) ) ;
#58156 = CARTESIAN_POINT ( 'NONE',  ( -57.19623071787017210, -131.3750000013656347, 4.297418129356382899 ) ) ;
#58157 = CARTESIAN_POINT ( 'NONE',  ( 2.229367062500001939, -71.22916666530107932, 3.861377020970579999 ) ) ;
#58158 = CARTESIAN_POINT ( 'NONE',  ( -4.999999999999998224, -90.91666666666665719, 2.886751345948131764 ) ) ;
#58159 = CARTESIAN_POINT ( 'NONE',  ( 0.000000000000000000, -170.0000000000000000, 0.000000000000000000 ) ) ;
#58160 = CARTESIAN_POINT ( 'NONE',  ( 2.730187237215162345E-16, -141.1875000013656063, -4.458734124999999437 ) ) ;
#58161 = CARTESIAN_POINT ( 'NONE',  ( -2.229367062500000163, 3.270833334698929118, -3.861377020970580443 ) ) ;
#58162 = ORIENTED_EDGE ( 'NONE', *, *, #49598, .T. ) ;
#58163 = MECHANICAL_DESIGN_GEOMETRIC_PRESENTATION_REPRESENTATION (  '', ( #36743 ), #53023 ) ;
#58164 = CARTESIAN_POINT ( 'NONE',  ( 0.000000000000000000, -170.0000000000000000, 0.000000000000000000 ) ) ;
#58165 = CARTESIAN_POINT ( 'NONE',  ( -9.184850993605147944E-16, -144.3750000027312126, 5.000000000000000000 ) ) ;
#58167 = CARTESIAN_POINT ( 'NONE',  ( 9.457646018065525792E-16, -30.06249999863440081, 5.148502694627439702 ) ) ;
#58166 = CARTESIAN_POINT ( 'NONE',  ( -2.500000000000000444, -95.16666666666667140, -4.330127018922193649 ) ) ;
#58168 = CARTESIAN_POINT ( 'NONE',  ( 0.000000000000000000, -120.0000000000000000, 5.000000000000000000 ) ) ;
#58169 = CARTESIAN_POINT ( 'NONE',  ( -2.229367062499996610, -77.39583333196773651, 3.861377020970582219 ) ) ;
#58170 = AXIS2_PLACEMENT_3D ( 'NONE', #12872, #27665, #13817 ) ;
#58171 = CARTESIAN_POINT ( 'NONE',  ( -4.458734124999997661, 22.52083333469892423, 2.574251347313722516 ) ) ;
#58172 = FACE_OUTER_BOUND ( 'NONE', #42449, .T. ) ;
#58173 = AXIS2_PLACEMENT_3D ( 'NONE', #42973, #3751, #52633 ) ;
#58174 = CARTESIAN_POINT ( 'NONE',  ( -59.44456063193725015, -140.5625000013656063, -0.3552334253322034230 ) ) ;
#58175 = CARTESIAN_POINT ( 'NONE',  ( 9.457646018065525792E-16, 1.937500001365593416, 5.148502694627439702 ) ) ;
#58176 = CARTESIAN_POINT ( 'NONE',  ( 4.458734124999998549, 29.02083333469893134, -2.574251347313721627 ) ) ;
#58177 = EDGE_CURVE ( 'NONE', #4805, #11153, #63553, .T. ) ;
#58178 = CARTESIAN_POINT ( 'NONE',  ( -4.458734124999999437, -41.64583333196773651, -2.574251347313719407 ) ) ;
#58179 = CARTESIAN_POINT ( 'NONE',  ( -5.000000000000000000, -3.874999997268816720, 0.000000000000000000 ) ) ;
#58180 = CARTESIAN_POINT ( 'NONE',  ( 2.229367062499998831, -0.6458333319677399542, -3.861377020970580887 ) ) ;
#58181 = EDGE_CURVE ( 'NONE', #47937, #26829, #17159, .T. ) ;
#58182 = CARTESIAN_POINT ( 'NONE',  ( 4.458734124999998549, -23.97916666530107577, -2.574251347313721627 ) ) ;
#58183 = CARTESIAN_POINT ( 'NONE',  ( 4.458734124999999437, -155.4375000013655779, 0.000000000000000000 ) ) ;
#58184 = CARTESIAN_POINT ( 'NONE',  ( -2.229367062500000163, -69.47916666530107932, -3.861377020970580443 ) ) ;
#58185 = CARTESIAN_POINT ( 'NONE',  ( -3.535250795749689387E-16, -103.1249999972688300, -5.773502691896257311 ) ) ;
#58186 =( BOUNDED_CURVE ( )  B_SPLINE_CURVE ( 2, ( #13152, #61743, #3511, #36650, #17968, #2565, #32772, #27937, #41782 ),
 .UNSPECIFIED., .F., .F. ) 
 B_SPLINE_CURVE_WITH_KNOTS ( ( 3, 2, 2, 2, 3 ),
 ( 0.6910714285714285587, 0.6916666666666666519, 0.6928571428571428381, 0.6940476190476190244, 0.6946428571428571175 ),
 .UNSPECIFIED. ) 
 CURVE ( )  GEOMETRIC_REPRESENTATION_ITEM ( )  RATIONAL_B_SPLINE_CURVE ( ( 0.9330127018922194093, 0.9330127018922194093, 1.000000000000000000, 0.8660254037844387076, 1.000000000000000000, 0.8660254037844387076, 1.000000000000000000, 0.9330127018922194093, 0.9330127018922194093 ) ) 
 REPRESENTATION_ITEM ( '' )  );
#58187 = DIRECTION ( 'NONE',  ( 0.000000000000000000, 0.000000000000000000, 1.000000000000000000 ) ) ;
#58188 = CARTESIAN_POINT ( 'NONE',  ( 4.458734125000000326, -108.1458333319677365, 2.574251347313718519 ) ) ;
#58189 = CARTESIAN_POINT ( 'NONE',  ( 9.457646018065525792E-16, -72.31249999863439371, 5.148502694627439702 ) ) ;
#58190 = CARTESIAN_POINT ( 'NONE',  ( 1.060575238724906964E-15, -51.75000000000000711, 5.773502691896257311 ) ) ;
#58191 = CARTESIAN_POINT ( 'NONE',  ( -5.000000000000000000, -65.87499999726881583, 0.000000000000000000 ) ) ;
#58192 = CARTESIAN_POINT ( 'NONE',  ( 1.060575238724906964E-15, 28.37500000273118417, 5.773502691896257311 ) ) ;
#58193 = ORIENTED_EDGE ( 'NONE', *, *, #49558, .T. ) ;
#58194 = CARTESIAN_POINT ( 'NONE',  ( -5.000000000000000888, -140.5625000000000000, -2.071067811865475949 ) ) ;
#58195 = CARTESIAN_POINT ( 'NONE',  ( 5.000000000000000888, -27.45833333060214798, 2.886751345948126879 ) ) ;
#58196 = CARTESIAN_POINT ( 'NONE',  ( -5.000000000000000000, -12.99999999999999822, 0.000000000000000000 ) ) ;
#58197 = CARTESIAN_POINT ( 'NONE',  ( 2.229367062500001939, -17.97916666530106866, 3.861377020970579999 ) ) ;
#58198 = EDGE_CURVE ( 'NONE', #51032, #33480, #50016, .T. ) ;
#58199 = CARTESIAN_POINT ( 'NONE',  ( 4.458734124999999437, -79.81249999863440792, -5.460374474430324690E-16 ) ) ;
#58201 = CARTESIAN_POINT ( 'NONE',  ( -8.190561711645485556E-16, -167.9375000013655779, 4.458734124999999437 ) ) ;
#58200 =( BOUNDED_CURVE ( )  B_SPLINE_CURVE ( 2, ( #63014, #48823, #57559, #33101, #48511, #13786, #43990, #33409, #18921 ),
 .UNSPECIFIED., .F., .F. ) 
 B_SPLINE_CURVE_WITH_KNOTS ( ( 3, 2, 2, 2, 3 ),
 ( 0.3250000000000002887, 0.3291666666666669405, 0.3333333333333335924, 0.3375000000000002998, 0.3416666666666669516 ),
 .UNSPECIFIED. ) 
 CURVE ( )  GEOMETRIC_REPRESENTATION_ITEM ( )  RATIONAL_B_SPLINE_CURVE ( ( 0.9999999999999948930, 0.9238795325112918455, 1.000000000000000000, 0.9238795325112867385, 1.000000000000000000, 0.9238795325112867385, 1.000000000000000000, 0.9238795325112816315, 1.000000000000005107 ) ) 
 REPRESENTATION_ITEM ( '' )  );
#58202 = CARTESIAN_POINT ( 'NONE',  ( 2.500000000000002220, -20.54166666393548013, 4.330127018922192761 ) ) ;
#58204 = ORIENTED_EDGE ( 'NONE', *, *, #17205, .F. ) ;
#58203 = CARTESIAN_POINT ( 'NONE',  ( 9.457646018065525792E-16, -45.06249999863440792, 5.148502694627439702 ) ) ;
#58205 = CARTESIAN_POINT ( 'NONE',  ( 2.500000000000002220, -98.66666666666665719, 4.330127018922192761 ) ) ;
#58207 = ORIENTED_EDGE ( 'NONE', *, *, #31958, .T. ) ;
#58206 = CARTESIAN_POINT ( 'NONE',  ( 9.457646018065525792E-16, 0.6875000013655957476, 5.148502694627439702 ) ) ;
#58208 = CARTESIAN_POINT ( 'NONE',  ( -53.51423613279429503, -153.2500000013656063, 4.591703134518083651 ) ) ;
#58209 = CARTESIAN_POINT ( 'NONE',  ( 2.499999999999998668, -63.33333333333332149, -4.330127018922193649 ) ) ;
#58210 = CARTESIAN_POINT ( 'NONE',  ( 3.152801135295367541, -154.5625000013656063, -3.152801135295367541 ) ) ;
#58211 = CARTESIAN_POINT ( 'NONE',  ( 4.458734124999998549, -41.97916666530107932, -2.574251347313721627 ) ) ;
#58212 = CARTESIAN_POINT ( 'NONE',  ( 0.000000000000000000, -120.0000000000000000, 0.000000000000000000 ) ) ;
#58213 = CARTESIAN_POINT ( 'NONE',  ( 5.000000000000000000, -163.0625000000000000, 2.071067811865478614 ) ) ;
#58214 = FACE_OUTER_BOUND ( 'NONE', #18084, .T. ) ;
#58215 = CARTESIAN_POINT ( 'NONE',  ( -50.40829686548195099, -127.2500000013656347, -1.485763867205728284 ) ) ;
#58216 = VECTOR ( 'NONE', #57744, 1000.000000000000000 ) ;
#58217 = CARTESIAN_POINT ( 'NONE',  ( 2.229367062500001939, -3.229166665301069550, 3.861377020970579999 ) ) ;
#58218 = AXIS2_PLACEMENT_3D ( 'NONE', #51393, #42354, #32070 ) ;
#58219 = CARTESIAN_POINT ( 'NONE',  ( -2.229367062500000163, -42.72916666530107932, -3.861377020970580443 ) ) ;
#58220 = CARTESIAN_POINT ( 'NONE',  ( -5.000000000000000000, -24.95833333060214443, -2.886751345948128211 ) ) ;
#58221 = CARTESIAN_POINT ( 'NONE',  ( 1.846868145590736310, -148.6250000013655779, 4.458734124999999437 ) ) ;
#58222 = CARTESIAN_POINT ( 'NONE',  ( -2.229367062499996610, -91.39583333196773651, 3.861377020970582219 ) ) ;
#58223 = CARTESIAN_POINT ( 'NONE',  ( 5.000000000000000888, -34.45833333060213732, 2.886751345948126879 ) ) ;
#58224 = VERTEX_POINT ( 'NONE', #34834 ) ;
#58225 = CARTESIAN_POINT ( 'NONE',  ( -6.972266317189433020E-16, -33.12499999726880873, -5.000000000000000000 ) ) ;
#58226 = CARTESIAN_POINT ( 'NONE',  ( -60.14911071818854538, -152.1875000027312126, 1.666127454062681368 ) ) ;
#58227 = CARTESIAN_POINT ( 'NONE',  ( 1.339745962155615144, -43.70534180126147561, 4.999999999999999112 ) ) ;
#58228 = ORIENTED_EDGE ( 'NONE', *, *, #50321, .F. ) ;
#58229 = EDGE_CURVE ( 'NONE', #14032, #39802, #46283, .T. ) ;
#58230 = EDGE_CURVE ( 'NONE', #54554, #56173, #26558, .T. ) ;
#58231 = FACE_OUTER_BOUND ( 'NONE', #19374, .T. ) ;
#58232 = CARTESIAN_POINT ( 'NONE',  ( 2.229367062499998831, -13.89583333196774184, -3.861377020970580887 ) ) ;
#58233 = EDGE_CURVE ( 'NONE', #44335, #41004, #44791, .T. ) ;
#58234 = CARTESIAN_POINT ( 'NONE',  ( 5.000000000000000000, -79.29166666393547303, -2.886751345948130876 ) ) ;
#58235 = CARTESIAN_POINT ( 'NONE',  ( -4.458734124999998549, -1.229166665301071326, 2.574251347313722516 ) ) ;
#58236 = CARTESIAN_POINT ( 'NONE',  ( -2.499999999999996447, -79.83333333333332860, 4.330127018922195425 ) ) ;
#58237 = CARTESIAN_POINT ( 'NONE',  ( 4.458734124999999437, -153.3750000013656063, -1.846868145590734978 ) ) ;
#58238 = CARTESIAN_POINT ( 'NONE',  ( -2.229367062500000163, 19.27083333469892779, -3.861377020970580443 ) ) ;
#58239 = ORIENTED_EDGE ( 'NONE', *, *, #27108, .T. ) ;
#58240 = CARTESIAN_POINT ( 'NONE',  ( -3.152548672688508926E-16, -92.56249999863439371, -5.148502694627439702 ) ) ;
#58241 = CARTESIAN_POINT ( 'NONE',  ( -1.339745962155613812, -34.08034179853029144, -5.000000000000000000 ) ) ;
#58242 = DIRECTION ( 'NONE',  ( -0.000000000000000000, 1.000000000000000000, -0.000000000000000000 ) ) ;
#58243 = CARTESIAN_POINT ( 'NONE',  ( -2.229367062499996610, -15.14583333196773474, 3.861377020970582219 ) ) ;
#58244 = EDGE_CURVE ( 'NONE', #62968, #20764, #48330, .T. ) ;
#58246 = EDGE_CURVE ( 'NONE', #29631, #9470, #53262, .T. ) ;
#58245 = FACE_OUTER_BOUND ( 'NONE', #14383, .T. ) ;
#58247 = CARTESIAN_POINT ( 'NONE',  ( 2.500000000000002220, 8.458333336064518093, 4.330127018922192761 ) ) ;
#58248 = CARTESIAN_POINT ( 'NONE',  ( -54.64476657466781973, -153.8125000013656347, -4.444560631937228834 ) ) ;
#58249 = CARTESIAN_POINT ( 'NONE',  ( -2.500000000000000444, -39.04166666393548013, -4.330127018922193649 ) ) ;
#58250 = CARTESIAN_POINT ( 'NONE',  ( 2.499999999999998668, -29.33333333333332860, -4.330127018922193649 ) ) ;
#58251 = CARTESIAN_POINT ( 'NONE',  ( -4.458734124999997661, 17.77083333469892779, 2.574251347313722516 ) ) ;
#58252 = CARTESIAN_POINT ( 'NONE',  ( 1.339745962155612702, -44.29465819873851729, -5.000000000000000000 ) ) ;
#58253 = EDGE_CURVE ( 'NONE', #56396, #54905, #54534, .T. ) ;
#58254 = ORIENTED_EDGE ( 'NONE', *, *, #30207, .F. ) ;
#58255 = CARTESIAN_POINT ( 'NONE',  ( -4.458734124999999437, 15.68750000136559564, 0.000000000000000000 ) ) ;
#58256 = EDGE_CURVE ( 'NONE', #45174, #55117, #55176, .T. ) ;
#58257 = CARTESIAN_POINT ( 'NONE',  ( -4.458734124999999437, -64.31249999863440792, 0.000000000000000000 ) ) ;
#58258 = CARTESIAN_POINT ( 'NONE',  ( -4.458734124999997661, -9.479166665301068662, 2.574251347313722516 ) ) ;
#58259 =( BOUNDED_CURVE ( )  B_SPLINE_CURVE ( 2, ( #10491, #11131, #20475, #15326, #25929, #6013, #45548, #21431, #30757 ),
 .UNSPECIFIED., .F., .F. ) 
 B_SPLINE_CURVE_WITH_KNOTS ( ( 3, 2, 2, 2, 3 ),
 ( 0.1812499999999999944, 0.1819444444444444364, 0.1833333333333333204, 0.1847222222222222321, 0.1854166666666666741 ),
 .UNSPECIFIED. ) 
 CURVE ( )  GEOMETRIC_REPRESENTATION_ITEM ( )  RATIONAL_B_SPLINE_CURVE ( ( 0.9330127018922194093, 0.9330127018922194093, 1.000000000000000000, 0.8660254037844387076, 1.000000000000000000, 0.8660254037844387076, 1.000000000000000000, 0.9330127018922194093, 0.9330127018922194093 ) ) 
 REPRESENTATION_ITEM ( '' )  );
#58260 = DIRECTION ( 'NONE',  ( -0.000000000000000000, 1.000000000000000000, -0.000000000000000000 ) ) ;
#58261 = CARTESIAN_POINT ( 'NONE',  ( 1.060575238724906964E-15, 10.24999999999999822, 5.773502691896257311 ) ) ;
#58262 = EDGE_CURVE ( 'NONE', #52748, #43968, #25895, .T. ) ;
#58263 = CARTESIAN_POINT ( 'NONE',  ( 2.730187237215162345E-16, -168.1875000013655779, -4.458734124999999437 ) ) ;
#58265 = ADVANCED_FACE ( 'NONE', ( #50015 ), #31034, .T. ) ;
#58264 = CARTESIAN_POINT ( 'NONE',  ( -50.18089887299977647, -142.6875000000000000, 2.462841084822456672 ) ) ;
#58266 = CARTESIAN_POINT ( 'NONE',  ( -4.458734124999999437, -55.39583333196773651, -2.574251347313719407 ) ) ;
#58267 = CARTESIAN_POINT ( 'NONE',  ( 5.000000000000000000, -83.37499999726881583, -6.123233995736766282E-16 ) ) ;
#58268 = VECTOR ( 'NONE', #47878, 1000.000000000000000 ) ;
#58269 = AXIS2_PLACEMENT_3D ( 'NONE', #22266, #42187, #57630 ) ;
#58270 = CARTESIAN_POINT ( 'NONE',  ( -52.10840900171896806, -136.4375000013656063, 3.393966926194110556 ) ) ;
#58271 = CARTESIAN_POINT ( 'NONE',  ( 0.000000000000000000, -120.0000000000000000, 0.000000000000000000 ) ) ;
#58272 = CARTESIAN_POINT ( 'NONE',  ( -6.972266317189433020E-16, -105.1249999972687874, -5.000000000000000000 ) ) ;
#58273 = AXIS2_PLACEMENT_3D ( 'NONE', #28195, #47810, #42991 ) ;
#58274 = CARTESIAN_POINT ( 'NONE',  ( -4.458734124999999437, -89.56249999863440792, 0.000000000000000000 ) ) ;
#58275 = CARTESIAN_POINT ( 'NONE',  ( -1.846868145590734756, -153.3750000013656063, -4.458734124999999437 ) ) ;
#58276 = CARTESIAN_POINT ( 'NONE',  ( -2.500000000000000444, -37.16666666666666430, -4.330127018922193649 ) ) ;
#58277 = CARTESIAN_POINT ( 'NONE',  ( 1.975475456537005874E-15, -56.62499999726880162, 5.000000000000000000 ) ) ;
#58278 = FACE_OUTER_BOUND ( 'NONE', #28183, .T. ) ;
#58279 = EDGE_LOOP ( 'NONE', ( #35266, #53725, #49329, #44990 ) ) ;
#58280 = CARTESIAN_POINT ( 'NONE',  ( -2.229367062500000163, -101.4791666653010651, -3.861377020970580443 ) ) ;
#58281 = CARTESIAN_POINT ( 'NONE',  ( -2.229367062500000163, 9.270833334698927786, -3.861377020970580443 ) ) ;
#58282 = CARTESIAN_POINT ( 'NONE',  ( 1.060575238724906964E-15, 12.37500000273118417, 5.773502691896257311 ) ) ;
#58283 = CARTESIAN_POINT ( 'NONE',  ( 2.071067811865561215, -162.1874999999999432, 4.999999999999913847 ) ) ;
#58284 = CARTESIAN_POINT ( 'NONE',  ( 5.000000000000000000, 3.583333333333333925, -2.886751345948129988 ) ) ;
#58285 = CARTESIAN_POINT ( 'NONE',  ( -2.229367062499996610, -60.14583333196774362, 3.861377020970582219 ) ) ;
#58286 = CARTESIAN_POINT ( 'NONE',  ( -6.972266317189433020E-16, -32.24999999999999289, -5.000000000000000000 ) ) ;
#58287 = CARTESIAN_POINT ( 'NONE',  ( 5.000000000000000000, -2.374999997268815388, -6.123233995736766282E-16 ) ) ;
#58288 = CARTESIAN_POINT ( 'NONE',  ( -2.229367062499996610, -27.14583333196774007, 3.861377020970582219 ) ) ;
#58289 = CARTESIAN_POINT ( 'NONE',  ( -1.339745962155610925, -41.79465819873852439, 5.000000000000000000 ) ) ;
#58290 = CYLINDRICAL_SURFACE ( 'NONE', #4542, 5.000000000000000000 ) ;
#58291 = CARTESIAN_POINT ( 'NONE',  ( 5.000000000000000888, 5.416666666666666963, 2.886751345948126879 ) ) ;
#58292 = CARTESIAN_POINT ( 'NONE',  ( -2.499999999999996447, -42.83333333333333570, 4.330127018922195425 ) ) ;
#58293 =( BOUNDED_CURVE ( )  B_SPLINE_CURVE ( 2, ( #35427, #25454, #49577, #25783, #15167, #10343, #10974, #25133, #45074 ),
 .UNSPECIFIED., .F., .F. ) 
 B_SPLINE_CURVE_WITH_KNOTS ( ( 3, 2, 2, 2, 3 ),
 ( 0.8979166666666666963, 0.8986111111111111382, 0.9000000000000000222, 0.9013888888888889062, 0.9020833333333333481 ),
 .UNSPECIFIED. ) 
 CURVE ( )  GEOMETRIC_REPRESENTATION_ITEM ( )  RATIONAL_B_SPLINE_CURVE ( ( 0.9330127018922194093, 0.9330127018922194093, 1.000000000000000000, 0.8660254037844387076, 1.000000000000000000, 0.8660254037844387076, 1.000000000000000000, 0.9330127018922194093, 0.9330127018922194093 ) ) 
 REPRESENTATION_ITEM ( '' )  );
#58295 = CARTESIAN_POINT ( 'NONE',  ( 2.229367062499998831, -26.89583333196774007, -3.861377020970580887 ) ) ;
#58294 = DIRECTION ( 'NONE',  ( 0.000000000000000000, 0.000000000000000000, -1.000000000000000000 ) ) ;
#58296 = CARTESIAN_POINT ( 'NONE',  ( 2.499999999999998668, -64.33333333333332860, -4.330127018922193649 ) ) ;
#58297 = CARTESIAN_POINT ( 'NONE',  ( -3.152548672688508926E-16, -68.56249999863439371, -5.148502694627439702 ) ) ;
#58298 = CARTESIAN_POINT ( 'NONE',  ( 1.846868145590736310, -143.8750000013656063, 4.458734124999999437 ) ) ;
#58299 = CARTESIAN_POINT ( 'NONE',  ( -2.229367062500000163, -74.47916666530106511, -3.861377020970580443 ) ) ;
#58300 = CARTESIAN_POINT ( 'NONE',  ( -59.44456063193725015, -138.8125000013656063, -0.3552334253322034230 ) ) ;
#58301 = CARTESIAN_POINT ( 'NONE',  ( -2.229367062500000163, -22.72916666530107221, -3.861377020970580443 ) ) ;
#58302 = CARTESIAN_POINT ( 'NONE',  ( -5.000000000000000000, -66.95833333060214443, -2.886751345948128211 ) ) ;
#58303 = EDGE_LOOP ( 'NONE', ( #2101, #54831, #9022, #58757 ) ) ;
#58304 = ORIENTED_EDGE ( 'NONE', *, *, #10239, .T. ) ;
#58305 = CARTESIAN_POINT ( 'NONE',  ( -4.458734124999999437, -70.56249999863439371, 0.000000000000000000 ) ) ;
#58306 = FILL_AREA_STYLE_COLOUR ( '', #36920 ) ;
#58307 = ORIENTED_EDGE ( 'NONE', *, *, #28314, .T. ) ;
#58308 = CARTESIAN_POINT ( 'NONE',  ( -5.000000000000000000, 16.91666666666666785, -2.886751345948128211 ) ) ;
#58309 = AXIS2_PLACEMENT_3D ( 'NONE', #43362, #23763, #62691 ) ;
#58310 = CARTESIAN_POINT ( 'NONE',  ( -1.339745962155613812, -83.20534180126146850, -5.000000000000000000 ) ) ;
#58311 = CARTESIAN_POINT ( 'NONE',  ( 9.457646018065525792E-16, -61.31249999863440792, 5.148502694627439702 ) ) ;
#58312 = AXIS2_PLACEMENT_3D ( 'NONE', #27164, #41944, #27472 ) ;
#58313 = CARTESIAN_POINT ( 'NONE',  ( 4.458734124999999437, -1.062499998634405696, -5.460374474430324690E-16 ) ) ;
#58314 = VERTEX_POINT ( 'NONE', #25255 ) ;
#58315 = DIRECTION ( 'NONE',  ( -0.000000000000000000, 1.000000000000000000, -0.000000000000000000 ) ) ;
#58316 = CARTESIAN_POINT ( 'NONE',  ( 4.458734124999998549, 15.27083333469893134, -2.574251347313721627 ) ) ;
#58317 = CARTESIAN_POINT ( 'NONE',  ( -52.80376928212989185, -144.8750000013655779, -4.297418129356379346 ) ) ;
#58318 = CARTESIAN_POINT ( 'NONE',  ( 5.000000000000000000, 16.58333333333333215, -2.886751345948130876 ) ) ;
#58319 = CARTESIAN_POINT ( 'NONE',  ( -3.152801135295367096, -165.0625000013656063, -3.152801135295367541 ) ) ;
#58320 = EDGE_LOOP ( 'NONE', ( #25581, #46807, #13401, #61149 ) ) ;
#58321 = CARTESIAN_POINT ( 'NONE',  ( -4.458734124999999437, -73.39583333196772230, -2.574251347313719407 ) ) ;
#58322 = CARTESIAN_POINT ( 'NONE',  ( -1.339745962155610925, -69.66965819600731891, 5.000000000000000000 ) ) ;
#58323 = CARTESIAN_POINT ( 'NONE',  ( 4.458734124999999437, 4.187500001365595637, -5.460374474430324690E-16 ) ) ;
#58324 = CARTESIAN_POINT ( 'NONE',  ( -3.535533905932738641, -162.5000000027312126, 3.535533905932737309 ) ) ;
#58325 = CARTESIAN_POINT ( 'NONE',  ( 4.458734124999999437, -68.06249999863440792, -5.460374474430324690E-16 ) ) ;
#58326 = CARTESIAN_POINT ( 'NONE',  ( 5.000000000000000000, -25.29166666393547658, -2.886751345948129988 ) ) ;
#58327 = CARTESIAN_POINT ( 'NONE',  ( 5.000000000000000000, -45.50000000000000000, -6.123233995736766282E-16 ) ) ;
#58328 = CARTESIAN_POINT ( 'NONE',  ( 0.000000000000000000, -170.0000000000000000, 0.000000000000000000 ) ) ;
#58329 = CARTESIAN_POINT ( 'NONE',  ( 5.000000000000000000, -18.37499999726881583, -6.123233995736766282E-16 ) ) ;
#58330 = SURFACE_STYLE_USAGE ( .BOTH. , #20037 ) ;
#58331 = EDGE_CURVE ( 'NONE', #30770, #21697, #37633, .T. ) ;
#58332 = CARTESIAN_POINT ( 'NONE',  ( -3.152548672688508926E-16, -42.56249999863440792, -5.148502694627439702 ) ) ;
#58333 = CARTESIAN_POINT ( 'NONE',  ( -2.229367062499996610, -24.39583333196773651, 3.861377020970582219 ) ) ;
#58334 = CARTESIAN_POINT ( 'NONE',  ( -3.152548672688508926E-16, 9.187500001365592084, -5.148502694627439702 ) ) ;
#58335 = CARTESIAN_POINT ( 'NONE',  ( 0.000000000000000000, -170.0000000000000000, 0.000000000000000000 ) ) ;
#58336 = CARTESIAN_POINT ( 'NONE',  ( 5.000000000000000000, 24.50000000000000000, -6.123233995736766282E-16 ) ) ;
#58337 = CARTESIAN_POINT ( 'NONE',  ( -9.184850993605147944E-16, -151.3750000027311842, 5.000000000000000000 ) ) ;
#58338 = CARTESIAN_POINT ( 'NONE',  ( -2.499999999999996447, -49.83333333333332860, 4.330127018922195425 ) ) ;
#58339 = CARTESIAN_POINT ( 'NONE',  ( 4.458734124999999437, -35.81249999863440792, -5.460374474430324690E-16 ) ) ;
#58340 = CARTESIAN_POINT ( 'NONE',  ( 5.000000000000000000, -66.37499999726881583, -6.123233995736766282E-16 ) ) ;
#58341 = CARTESIAN_POINT ( 'NONE',  ( -55.35523342533222291, -146.5625000013656063, 4.444560631937231499 ) ) ;
#58342 = CARTESIAN_POINT ( 'NONE',  ( -3.535533905932738641, -141.3750000000000000, 3.535533905932737309 ) ) ;
#58343 = EDGE_CURVE ( 'NONE', #37814, #44139, #1795, .T. ) ;
#58344 = CARTESIAN_POINT ( 'NONE',  ( -2.229367062500000163, -74.72916666530106511, -3.861377020970580443 ) ) ;
#58345 = CARTESIAN_POINT ( 'NONE',  ( 3.152801135295366208, -164.8125000013656063, 3.152801135295367985 ) ) ;
#58346 = CARTESIAN_POINT ( 'NONE',  ( -3.152548672688508926E-16, -31.56249999863440436, -5.148502694627439702 ) ) ;
#58347 = CARTESIAN_POINT ( 'NONE',  ( 1.975475456537005874E-15, -27.62499999726881228, 5.000000000000000000 ) ) ;
#58348 = DIRECTION ( 'NONE',  ( -0.000000000000000000, 1.000000000000000000, -0.000000000000000000 ) ) ;
#58349 = CARTESIAN_POINT ( 'NONE',  ( -2.500000000000000444, -22.16666666666666785, -4.330127018922193649 ) ) ;
#58350 = CARTESIAN_POINT ( 'NONE',  ( 3.152801135295367541, -142.3125000013655779, -3.152801135295367541 ) ) ;
#58351 = ORIENTED_EDGE ( 'NONE', *, *, #58951, .F. ) ;
#58352 = CARTESIAN_POINT ( 'NONE',  ( -2.229367062499996610, 27.60416666803225993, 3.861377020970582219 ) ) ;
#58353 = CARTESIAN_POINT ( 'NONE',  ( -55.39835681537999790, -140.8750000000000284, 4.984105922594378235 ) ) ;
#58354 = CARTESIAN_POINT ( 'NONE',  ( -4.458734124999999437, -54.56249999863440081, 0.000000000000000000 ) ) ;
#58355 = VECTOR ( 'NONE', #50643, 1000.000000000000000 ) ;
#58356 = CARTESIAN_POINT ( 'NONE',  ( 5.000000000000000000, 28.70833333606451987, -2.886751345948129988 ) ) ;
#58357 = DIRECTION ( 'NONE',  ( -0.000000000000000000, 1.000000000000000000, -0.000000000000000000 ) ) ;
#58358 = CARTESIAN_POINT ( 'NONE',  ( 2.500000000000002220, 21.33333333333333215, 4.330127018922192761 ) ) ;
#58359 = AXIS2_PLACEMENT_3D ( 'NONE', #19762, #58686, #20411 ) ;
#58360 = CARTESIAN_POINT ( 'NONE',  ( -2.500000000000000444, -37.04166666393548013, -4.330127018922193649 ) ) ;
#58361 = CARTESIAN_POINT ( 'NONE',  ( -2.229367062500000163, -8.479166665301073991, -3.861377020970580443 ) ) ;
#58362 = CARTESIAN_POINT ( 'NONE',  ( -9.184850993605147944E-16, -168.2500000000000000, 5.000000000000000000 ) ) ;
#58363 = CARTESIAN_POINT ( 'NONE',  ( -51.19402409849444524, -145.6250000027312126, -3.242614290531456334 ) ) ;
#58364 = CYLINDRICAL_SURFACE ( 'NONE', #41544, 5.000000000000000000 ) ;
#58365 = CARTESIAN_POINT ( 'NONE',  ( 1.339745962155615144, -53.58034179853029144, 4.999999999999999112 ) ) ;
#58366 = CARTESIAN_POINT ( 'NONE',  ( 9.457646018065525792E-16, -19.06249999863440792, 5.148502694627439702 ) ) ;
#58367 = CARTESIAN_POINT ( 'NONE',  ( 9.457646018065525792E-16, -56.06249999863440792, 5.148502694627439702 ) ) ;
#58368 = CARTESIAN_POINT ( 'NONE',  ( -4.458734124999999437, -160.1875000013655779, -5.460374474430324690E-16 ) ) ;
#58369 = AXIS2_PLACEMENT_3D ( 'NONE', #47486, #56843, #7949 ) ;
#58370 = CARTESIAN_POINT ( 'NONE',  ( -3.535250795749689387E-16, -48.12499999726880873, -5.773502691896257311 ) ) ;
#58371 = ORIENTED_EDGE ( 'NONE', *, *, #54966, .T. ) ;
#58372 = CARTESIAN_POINT ( 'NONE',  ( 4.458734124999999437, 4.937500001365595637, -5.460374474430324690E-16 ) ) ;
#58373 = ORIENTED_EDGE ( 'NONE', *, *, #47226, .T. ) ;
#58375 = CARTESIAN_POINT ( 'NONE',  ( -5.000000000000000000, -3.083333333333333925, -2.886751345948128211 ) ) ;
#58374 = FACE_OUTER_BOUND ( 'NONE', #24025, .T. ) ;
#58376 = CARTESIAN_POINT ( 'NONE',  ( 1.846868145590735200, -161.2500000013655779, -4.458734125000000326 ) ) ;
#58377 = VERTEX_POINT ( 'NONE', #16567 ) ;
#58378 = UNCERTAINTY_MEASURE_WITH_UNIT (LENGTH_MEASURE( 1.000000000000000082E-05 ), #17021, 'distance_accuracy_value', 'NONE');
#58379 = CARTESIAN_POINT ( 'NONE',  ( 1.975475456537005874E-15, -17.62499999726881583, 5.000000000000000000 ) ) ;
#58380 = CARTESIAN_POINT ( 'NONE',  ( -50.18089887299979068, -134.6875000000000000, 2.462841084822635640 ) ) ;
#58381 = CARTESIAN_POINT ( 'NONE',  ( 5.000000000000000000, -47.37499999726880873, -6.123233995736766282E-16 ) ) ;
#58382 = CARTESIAN_POINT ( 'NONE',  ( 9.457646018065525792E-16, -45.31249999863440081, 5.148502694627439702 ) ) ;
#58383 = ORIENTED_EDGE ( 'NONE', *, *, #55429, .T. ) ;
#58384 =( BOUNDED_CURVE ( )  B_SPLINE_CURVE ( 2, ( #46637, #31840, #27019, #2583, #56620, #17052, #21564, #50829, #12536 ),
 .UNSPECIFIED., .F., .F. ) 
 B_SPLINE_CURVE_WITH_KNOTS ( ( 3, 2, 2, 2, 3 ),
 ( 0.3875000000000000111, 0.3880952380952381042, 0.3892857142857142905, 0.3904761904761904767, 0.3910714285714285698 ),
 .UNSPECIFIED. ) 
 CURVE ( )  GEOMETRIC_REPRESENTATION_ITEM ( )  RATIONAL_B_SPLINE_CURVE ( ( 0.9330127018922194093, 0.9330127018922194093, 1.000000000000000000, 0.8660254037844387076, 1.000000000000000000, 0.8660254037844387076, 1.000000000000000000, 0.9330127018922194093, 0.9330127018922194093 ) ) 
 REPRESENTATION_ITEM ( '' )  );
#58385 = ADVANCED_FACE ( 'NONE', ( #44873 ), #11726, .T. ) ;
#58386 = LINE ( 'NONE', #49035, #20339 ) ;
#58387 = CARTESIAN_POINT ( 'NONE',  ( 4.458734124999999437, 21.18750000136559208, -5.460374474430324690E-16 ) ) ;
#58388 = CARTESIAN_POINT ( 'NONE',  ( 5.000000000000000000, -24.37499999726881228, -6.123233995736766282E-16 ) ) ;
#58389 = ORIENTED_EDGE ( 'NONE', *, *, #25646, .F. ) ;
#58390 = CARTESIAN_POINT ( 'NONE',  ( 4.458734124999998549, -87.97916666530107932, -2.574251347313721627 ) ) ;
#58391 = CARTESIAN_POINT ( 'NONE',  ( -58.80597590150559739, -127.1250000027312268, 3.242614290531460330 ) ) ;
#58392 = CARTESIAN_POINT ( 'NONE',  ( -2.500000000000000444, 24.95833333606451987, -4.330127018922193649 ) ) ;
#58393 = CARTESIAN_POINT ( 'NONE',  ( 5.000000000000000000, -169.0625000000000000, 2.071067811865478614 ) ) ;
#58394 = CARTESIAN_POINT ( 'NONE',  ( -4.458734124999999437, -59.31249999863440081, 0.000000000000000000 ) ) ;
#58395 = CARTESIAN_POINT ( 'NONE',  ( 1.975475456537005874E-15, -61.62499999726880873, 5.000000000000000000 ) ) ;
#58396 = CARTESIAN_POINT ( 'NONE',  ( 4.458734124999999437, 21.18750000136559208, -5.460374474430324690E-16 ) ) ;
#58397 = AXIS2_PLACEMENT_3D ( 'NONE', #58212, #43101, #62431 ) ;
#58398 = CARTESIAN_POINT ( 'NONE',  ( 5.000000000000000888, -102.4583333306021586, 2.886751345948126879 ) ) ;
#58399 = LINE ( 'NONE', #8877, #29914 ) ;
#58400 = CARTESIAN_POINT ( 'NONE',  ( 4.458734125000001214, -50.14583333196773651, 2.574251347313718519 ) ) ;
#58401 = CARTESIAN_POINT ( 'NONE',  ( 2.500000000000002220, -3.541666663935478354, 4.330127018922192761 ) ) ;
#58402 = CARTESIAN_POINT ( 'NONE',  ( 6.123233995736766282E-16, -170.0000000000000000, -5.000000000000000000 ) ) ;
#58403 = DIRECTION ( 'NONE',  ( 0.000000000000000000, 0.000000000000000000, 1.000000000000000000 ) ) ;
#58404 = CARTESIAN_POINT ( 'NONE',  ( 2.229367062500001939, -82.22916666530106511, 3.861377020970579999 ) ) ;
#58405 = CARTESIAN_POINT ( 'NONE',  ( 9.457646018065525792E-16, -108.0624999986343937, 5.148502694627439702 ) ) ;
#58406 = CARTESIAN_POINT ( 'NONE',  ( 9.457646018065525792E-16, -13.31249999863440259, 5.148502694627439702 ) ) ;
#58407 = VERTEX_POINT ( 'NONE', #11095 ) ;
#58408 = CARTESIAN_POINT ( 'NONE',  ( 3.061616997868383141E-16, -155.8750000027311842, -5.000000000000000000 ) ) ;
#58409 = CARTESIAN_POINT ( 'NONE',  ( 2.229367062499998831, -100.6458333319677365, -3.861377020970580887 ) ) ;
#58410 = CARTESIAN_POINT ( 'NONE',  ( 2.071067811865475505, -160.9375000027312126, -5.000000000000000888 ) ) ;
#58411 = CARTESIAN_POINT ( 'NONE',  ( 4.458734124999999437, -90.06249999863440792, -5.460374474430324690E-16 ) ) ;
#58412 = CARTESIAN_POINT ( 'NONE',  ( -6.972266317189433020E-16, -49.12499999726880162, -5.000000000000000000 ) ) ;
#58413 = CARTESIAN_POINT ( 'NONE',  ( 5.000000000000000000, -50.37499999726881583, -6.123233995736766282E-16 ) ) ;
#58414 = CARTESIAN_POINT ( 'NONE',  ( -2.500000000000000444, -37.04166666393548013, -4.330127018922193649 ) ) ;
#58415 = AXIS2_PLACEMENT_3D ( 'NONE', #19418, #42605, #48678 ) ;
#58416 = CARTESIAN_POINT ( 'NONE',  ( -50.55543936806279248, -129.0625000013656063, 0.3552334253322060320 ) ) ;
#58417 = CARTESIAN_POINT ( 'NONE',  ( -50.40829686548195099, -145.0000000013656063, -1.485763867205728284 ) ) ;
#58418 = CARTESIAN_POINT ( 'NONE',  ( 4.458734124999998549, -18.72916666530106866, -2.574251347313721627 ) ) ;
#58419 = CARTESIAN_POINT ( 'NONE',  ( -3.152548672688508926E-16, 12.18750000136559564, -5.148502694627439702 ) ) ;
#58420 = CARTESIAN_POINT ( 'NONE',  ( 2.229367062499998831, -57.89583333196773651, -3.861377020970580887 ) ) ;
#58421 = CARTESIAN_POINT ( 'NONE',  ( 3.061616997868383141E-16, -139.8750000027312126, -5.000000000000000000 ) ) ;
#58422 = CARTESIAN_POINT ( 'NONE',  ( -2.229367062499996610, -16.14583333196773651, 3.861377020970582219 ) ) ;
#58423 = CARTESIAN_POINT ( 'NONE',  ( 5.000000000000000000, -71.41666666666667140, -2.886751345948130876 ) ) ;
#58424 = CARTESIAN_POINT ( 'NONE',  ( -3.535533905932738641, -155.3750000000000000, 3.535533905932737309 ) ) ;
#58425 = ORIENTED_EDGE ( 'NONE', *, *, #34127, .T. ) ;
#58426 = CARTESIAN_POINT ( 'NONE',  ( 2.229367062500001939, -43.22916666530107932, 3.861377020970579999 ) ) ;
#58427 = CARTESIAN_POINT ( 'NONE',  ( -1.339745962155610925, -37.79465819873851729, 5.000000000000000000 ) ) ;
#58428 = LINE ( 'NONE', #53909, #9041 ) ;
#58429 = CARTESIAN_POINT ( 'NONE',  ( -3.152548672688508926E-16, -85.56249999863439371, -5.148502694627439702 ) ) ;
#58430 = CARTESIAN_POINT ( 'NONE',  ( -4.458734124999999437, 20.43750000136559208, 0.000000000000000000 ) ) ;
#58431 = CARTESIAN_POINT ( 'NONE',  ( 4.458734124999998549, 10.27083333469892779, -2.574251347313721627 ) ) ;
#58432 = CARTESIAN_POINT ( 'NONE',  ( -1.339745962155610925, -88.66965819600733312, 5.000000000000000000 ) ) ;
#58433 = CARTESIAN_POINT ( 'NONE',  ( -1.339745962155613812, -69.20534180126148271, -5.000000000000000000 ) ) ;
#58434 = CARTESIAN_POINT ( 'NONE',  ( -4.458734124999997661, -86.47916666530107932, 2.574251347313722516 ) ) ;
#58435 = CARTESIAN_POINT ( 'NONE',  ( 2.500000000000002220, -69.66666666666667140, 4.330127018922192761 ) ) ;
#58436 =( BOUNDED_CURVE ( )  B_SPLINE_CURVE ( 2, ( #15984, #5384, #35609, #25955, #15352, #54592, #20178, #1528, #21132 ),
 .UNSPECIFIED., .F., .F. ) 
 B_SPLINE_CURVE_WITH_KNOTS ( ( 3, 2, 2, 2, 3 ),
 ( 0.06607142857142857262, 0.06666666666666666574, 0.06785714285714285199, 0.06904761904761905211, 0.06964285714285714524 ),
 .UNSPECIFIED. ) 
 CURVE ( )  GEOMETRIC_REPRESENTATION_ITEM ( )  RATIONAL_B_SPLINE_CURVE ( ( 0.9330127018922194093, 0.9330127018922194093, 1.000000000000000000, 0.8660254037844387076, 1.000000000000000000, 0.8660254037844387076, 1.000000000000000000, 0.9330127018922194093, 0.9330127018922194093 ) ) 
 REPRESENTATION_ITEM ( '' )  );
#58437 = CARTESIAN_POINT ( 'NONE',  ( -3.535250795749689387E-16, 14.87500000273118594, -5.773502691896257311 ) ) ;
#58438 = EDGE_LOOP ( 'NONE', ( #6351, #26480, #43405, #13999 ) ) ;
#58439 = CARTESIAN_POINT ( 'NONE',  ( 1.339745962155612702, -79.29465819873851729, -5.000000000000000000 ) ) ;
#58440 = VERTEX_POINT ( 'NONE', #55810 ) ;
#58441 = CARTESIAN_POINT ( 'NONE',  ( 0.000000000000000000, -170.0000000000000000, 0.000000000000000000 ) ) ;
#58443 = CARTESIAN_POINT ( 'NONE',  ( 5.000000000000000000, -34.50000000000000000, -6.123233995736766282E-16 ) ) ;
#58442 = CYLINDRICAL_SURFACE ( 'NONE', #49163, 5.000000000000000000 ) ;
#58444 = CARTESIAN_POINT ( 'NONE',  ( -2.229367062499996610, -37.14583333196773651, 3.861377020970582219 ) ) ;
#58445 = ADVANCED_FACE ( 'NONE', ( #31342 ), #40364, .T. ) ;
#58446 = VECTOR ( 'NONE', #33855, 1000.000000000000000 ) ;
#58447 = CARTESIAN_POINT ( 'NONE',  ( -2.499999999999996447, -36.70833333060213732, 4.330127018922195425 ) ) ;
#58448 = B_SPLINE_CURVE_WITH_KNOTS ( 'NONE', 3,
 ( #7598, #12087, #27205, #31710, #7283, #32344, #42306, #37486 ),
 .UNSPECIFIED., .F., .F.,
 ( 4, 2, 2, 4 ),
 ( 0.006061689441712453386, 0.007174127271521677299, 0.008286565101330901212, 0.01051144076094934904 ),
 .UNSPECIFIED. ) ;
#58450 = ORIENTED_EDGE ( 'NONE', *, *, #9177, .T. ) ;
#58449 = CARTESIAN_POINT ( 'NONE',  ( 2.229367062500001939, -66.97916666530106511, 3.861377020970579999 ) ) ;
#58451 = CARTESIAN_POINT ( 'NONE',  ( -59.29741812935640155, -150.8750000013656063, -2.196230717870135685 ) ) ;
#58452 = CARTESIAN_POINT ( 'NONE',  ( -3.152548672688508926E-16, -14.56249999863440436, -5.148502694627439702 ) ) ;
#58454 = ORIENTED_EDGE ( 'NONE', *, *, #28756, .F. ) ;
#58453 = CARTESIAN_POINT ( 'NONE',  ( -4.458734124999999437, -15.56249999863440436, 0.000000000000000000 ) ) ;
#58455 = CARTESIAN_POINT ( 'NONE',  ( -2.500000000000000444, -75.16666666666665719, -4.330127018922193649 ) ) ;
#58456 = LINE ( 'NONE', #53626, #10414 ) ;
#58457 = CARTESIAN_POINT ( 'NONE',  ( 4.458734124999998549, -57.97916666530107221, -2.574251347313721627 ) ) ;
#58458 = CARTESIAN_POINT ( 'NONE',  ( -5.000000000000000000, -79.95833333060213022, -2.886751345948128211 ) ) ;
#58460 = VERTEX_POINT ( 'NONE', #45511 ) ;
#58459 = CARTESIAN_POINT ( 'NONE',  ( 5.000000000000000000, 3.708333336064517649, -2.886751345948130876 ) ) ;
#58461 = CARTESIAN_POINT ( 'NONE',  ( -59.98410592259440222, -145.1250000000000284, -0.3983568153799752487 ) ) ;
#58462 = CARTESIAN_POINT ( 'NONE',  ( -2.229367062499996610, -24.39583333196773651, 3.861377020970582219 ) ) ;
#58463 = EDGE_LOOP ( 'NONE', ( #32719, #2237, #3182, #21926 ) ) ;
#58464 = CARTESIAN_POINT ( 'NONE',  ( -4.458734124999999437, -166.1875000013655779, -5.460374474430324690E-16 ) ) ;
#58465 = CARTESIAN_POINT ( 'NONE',  ( 2.229367062499998831, -106.8958333319677365, -3.861377020970580887 ) ) ;
#58466 = CARTESIAN_POINT ( 'NONE',  ( 5.000000000000000000, -50.37499999726881583, -6.123233995736766282E-16 ) ) ;
#58467 = ORIENTED_EDGE ( 'NONE', *, *, #18156, .T. ) ;
#58468 = CARTESIAN_POINT ( 'NONE',  ( -54.64476657466781973, -149.0625000013656063, -4.444560631937228834 ) ) ;
#58469 = CARTESIAN_POINT ( 'NONE',  ( -50.01589407740564042, -137.7500000027312126, 0.3983568153799778022 ) ) ;
#58470 = CARTESIAN_POINT ( 'NONE',  ( 2.229367062499998831, -40.64583333196773651, -3.861377020970580887 ) ) ;
#58471 = DIRECTION ( 'NONE',  ( 0.000000000000000000, 0.000000000000000000, 1.000000000000000000 ) ) ;
#58472 = CARTESIAN_POINT ( 'NONE',  ( -3.535533905932738641, -146.5000000027311842, 3.535533905932737309 ) ) ;
#58473 = CARTESIAN_POINT ( 'NONE',  ( -2.229367062499996610, -12.14583333196774007, 3.861377020970582219 ) ) ;
#58474 = CARTESIAN_POINT ( 'NONE',  ( 4.458734124999999437, -101.0624999986344079, -5.460374474430324690E-16 ) ) ;
#58475 = ORIENTED_EDGE ( 'NONE', *, *, #29547, .F. ) ;
#58476 = CARTESIAN_POINT ( 'NONE',  ( 2.730187237215162345E-16, -142.4375000013656063, -4.458734124999999437 ) ) ;
#58477 = CARTESIAN_POINT ( 'NONE',  ( 2.229367062499998831, -28.89583333196774007, -3.861377020970580887 ) ) ;
#58478 = CARTESIAN_POINT ( 'NONE',  ( -52.53715891517739323, -139.5625000027312126, -4.819101127000233298 ) ) ;
#58479 = CARTESIAN_POINT ( 'NONE',  ( -57.89159099828107458, -134.6875000013656063, -3.393966926194107447 ) ) ;
#58480 = CARTESIAN_POINT ( 'NONE',  ( 2.229367062499998831, -69.89583333196773651, -3.861377020970580887 ) ) ;
#58481 = DIRECTION ( 'NONE',  ( 0.000000000000000000, 1.000000000000000000, 0.000000000000000000 ) ) ;
#58482 = DIRECTION ( 'NONE',  ( -0.000000000000000000, 1.000000000000000000, -0.000000000000000000 ) ) ;
#58483 = CARTESIAN_POINT ( 'NONE',  ( 4.458734124999999437, -141.4375000013656063, 0.000000000000000000 ) ) ;
#58484 =( BOUNDED_CURVE ( )  B_SPLINE_CURVE ( 2, ( #61777, #19261, #49173, #4789, #5113, #39512, #29536, #14121, #33747 ),
 .UNSPECIFIED., .F., .F. ) 
 B_SPLINE_CURVE_WITH_KNOTS ( ( 3, 2, 2, 2, 3 ),
 ( 0.3312499999999999889, 0.3319444444444444309, 0.3333333333333333148, 0.3347222222222221988, 0.3354166666666666963 ),
 .UNSPECIFIED. ) 
 CURVE ( )  GEOMETRIC_REPRESENTATION_ITEM ( )  RATIONAL_B_SPLINE_CURVE ( ( 0.9330127018922194093, 0.9330127018922194093, 1.000000000000000000, 0.8660254037844387076, 1.000000000000000000, 0.8660254037844387076, 1.000000000000000000, 0.9330127018922167448, 0.9330127018922194093 ) ) 
 REPRESENTATION_ITEM ( '' )  );
#58485 = CARTESIAN_POINT ( 'NONE',  ( -2.229367062499996610, 6.604166668032259935, 3.861377020970582219 ) ) ;
#58486 = ORIENTED_EDGE ( 'NONE', *, *, #12665, .T. ) ;
#58487 =( NAMED_UNIT ( * ) PLANE_ANGLE_UNIT ( ) SI_UNIT ( $, .RADIAN. ) );
#58488 = DIRECTION ( 'NONE',  ( 0.000000000000000000, 0.000000000000000000, 1.000000000000000000 ) ) ;
#58490 = CARTESIAN_POINT ( 'NONE',  ( -4.458734124999999437, -32.31249999863440792, 0.000000000000000000 ) ) ;
#58489 = CARTESIAN_POINT ( 'NONE',  ( -3.535250795749689387E-16, -98.25000000000000000, -5.773502691896257311 ) ) ;
#58491 = CARTESIAN_POINT ( 'NONE',  ( -58.24261429053147765, -143.2500000000000284, -3.805975901505573855 ) ) ;
#58492 = CARTESIAN_POINT ( 'NONE',  ( 2.229367062500001939, -74.22916666530106511, 3.861377020970579999 ) ) ;
#58493 = VECTOR ( 'NONE', #40478, 1000.000000000000000 ) ;
#58494 = CARTESIAN_POINT ( 'NONE',  ( 4.458734124999998549, 23.02083333469892423, -2.574251347313721627 ) ) ;
#58495 = CARTESIAN_POINT ( 'NONE',  ( 6.324555320336756381, 0.000000000000000000, -9.000000000000001776 ) ) ;
#58496 = CARTESIAN_POINT ( 'NONE',  ( -59.59170313451811296, -142.5000000013656347, 1.485763867205729394 ) ) ;
#58497 = CARTESIAN_POINT ( 'NONE',  ( 2.229367062499998831, 0.3541666680322609340, -3.861377020970580887 ) ) ;
#58498 = CARTESIAN_POINT ( 'NONE',  ( -3.152548672688508926E-16, 25.18750000136558853, -5.148502694627439702 ) ) ;
#58499 = CARTESIAN_POINT ( 'NONE',  ( 2.229367062500001939, -44.22916666530106511, 3.861377020970579999 ) ) ;
#58500 = CARTESIAN_POINT ( 'NONE',  ( -6.972266317189433020E-16, -43.12499999726880873, -5.000000000000000000 ) ) ;
#58501 = CARTESIAN_POINT ( 'NONE',  ( 2.229367062500001939, -0.9791666653010712151, 3.861377020970579999 ) ) ;
#58502 = EDGE_LOOP ( 'NONE', ( #55547, #63450, #53231, #4946 ) ) ;
#58503 = CARTESIAN_POINT ( 'NONE',  ( -2.229367062499996610, -23.39583333196773651, 3.861377020970582219 ) ) ;
#58504 = CARTESIAN_POINT ( 'NONE',  ( 9.457646018065525792E-16, -72.06249999863439371, 5.148502694627439702 ) ) ;
#58505 = CARTESIAN_POINT ( 'NONE',  ( 1.060575238724906964E-15, -103.6249999972688158, 5.773502691896257311 ) ) ;
#58506 = CARTESIAN_POINT ( 'NONE',  ( 9.457646018065525792E-16, 25.93750000136559564, 5.148502694627439702 ) ) ;
#58507 = CARTESIAN_POINT ( 'NONE',  ( -5.000000000000000000, -64.00000000000000000, 0.000000000000000000 ) ) ;
#58508 = CARTESIAN_POINT ( 'NONE',  ( -4.458734124999999437, -110.5624999986343937, 0.000000000000000000 ) ) ;
#58509 = CARTESIAN_POINT ( 'NONE',  ( -4.458734124999999437, -71.64583333196773651, -2.574251347313719407 ) ) ;
#58510 = CARTESIAN_POINT ( 'NONE',  ( 2.499999999999998668, -52.33333333333332860, -4.330127018922193649 ) ) ;
#58511 = CARTESIAN_POINT ( 'NONE',  ( 1.975475456537005874E-15, -65.74999999999998579, 5.000000000000000000 ) ) ;
#58512 = DIRECTION ( 'NONE',  ( -0.000000000000000000, 1.000000000000000000, -0.000000000000000000 ) ) ;
#58513 = ORIENTED_EDGE ( 'NONE', *, *, #45176, .F. ) ;
#58514 = CARTESIAN_POINT ( 'NONE',  ( -5.000000000000000000, -27.08333333333333215, -2.886751345948128211 ) ) ;
#58515 = CARTESIAN_POINT ( 'NONE',  ( 5.000000000000000000, -6.374999997268812280, -6.123233995736766282E-16 ) ) ;
#58516 = CARTESIAN_POINT ( 'NONE',  ( 2.500000000000002220, -14.66666666666666785, 4.330127018922192761 ) ) ;
#58517 = CARTESIAN_POINT ( 'NONE',  ( 2.229367062499998831, -17.64583333196773651, -3.861377020970580887 ) ) ;
#58518 = EDGE_CURVE ( 'NONE', #41205, #1843, #22054, .T. ) ;
#58519 = CARTESIAN_POINT ( 'NONE',  ( 4.458734124999999437, -80.81249999863440792, -5.460374474430324690E-16 ) ) ;
#58520 = CARTESIAN_POINT ( 'NONE',  ( 4.458734124999999437, -166.7500000013655779, 1.846868145590737864 ) ) ;
#58521 = CARTESIAN_POINT ( 'NONE',  ( -2.500000000000000444, -16.04166666393548368, -4.330127018922193649 ) ) ;
#58523 = ORIENTED_EDGE ( 'NONE', *, *, #62536, .T. ) ;
#58522 = CARTESIAN_POINT ( 'NONE',  ( -4.458734124999999437, -52.31249999863440792, 0.000000000000000000 ) ) ;
#58524 = CARTESIAN_POINT ( 'NONE',  ( 5.000000000000000000, -70.29166666393547303, -2.886751345948130876 ) ) ;
#58525 = CARTESIAN_POINT ( 'NONE',  ( -9.184850993605147944E-16, -168.3750000027312126, 5.000000000000000000 ) ) ;
#58527 = ORIENTED_EDGE ( 'NONE', *, *, #19247, .T. ) ;
#58526 = CARTESIAN_POINT ( 'NONE',  ( -2.229367062500000163, 0.2708333346989263979, -3.861377020970580443 ) ) ;
#58528 = CARTESIAN_POINT ( 'NONE',  ( -59.29741812935640155, -152.6250000013656063, -2.196230717870135685 ) ) ;
#58529 = CARTESIAN_POINT ( 'NONE',  ( -5.000000000000000000, -61.00000000000000000, 0.000000000000000000 ) ) ;
#58530 = CARTESIAN_POINT ( 'NONE',  ( -3.152801135295367096, -157.3125000013656063, -3.152801135295367541 ) ) ;
#58531 = CARTESIAN_POINT ( 'NONE',  ( -4.458734124999999437, -39.64583333196774362, -2.574251347313719407 ) ) ;
#58532 = CARTESIAN_POINT ( 'NONE',  ( 1.975475456537005874E-15, -10.75000000000000000, 5.000000000000000000 ) ) ;
#58533 = CARTESIAN_POINT ( 'NONE',  ( -3.535533905932737309, -160.6250000000000284, -3.535533905932738197 ) ) ;
#58534 = EDGE_CURVE ( 'NONE', #44207, #8918, #35231, .T. ) ;
#58535 = CARTESIAN_POINT ( 'NONE',  ( -2.499999999999996447, 11.16666666666666430, 4.330127018922195425 ) ) ;
#58536 = VECTOR ( 'NONE', #59639, 1000.000000000000000 ) ;
#58537 = CARTESIAN_POINT ( 'NONE',  ( -57.89159099828107458, -125.9375000013656063, -3.393966926194107447 ) ) ;
#58538 = CARTESIAN_POINT ( 'NONE',  ( 4.458734124999999437, -6.062499998634403475, -5.460374474430324690E-16 ) ) ;
#58539 = CARTESIAN_POINT ( 'NONE',  ( -4.458734124999999437, -45.56249999863440081, 0.000000000000000000 ) ) ;
#58540 = CARTESIAN_POINT ( 'NONE',  ( -6.972266317189433020E-16, -89.24999999999998579, -5.000000000000000000 ) ) ;
#58541 = CARTESIAN_POINT ( 'NONE',  ( 1.846868145590735200, -147.2500000013656063, -4.458734125000000326 ) ) ;
#58542 = EDGE_CURVE ( 'NONE', #32095, #58407, #20758, .T. ) ;
#58543 = CARTESIAN_POINT ( 'NONE',  ( -2.229367062499996610, -87.39583333196773651, 3.861377020970582219 ) ) ;
#58544 = CARTESIAN_POINT ( 'NONE',  ( -55.00000000000002132, -155.0000000000000284, 1.734723475976807094E-15 ) ) ;
#58545 = ORIENTED_EDGE ( 'NONE', *, *, #46136, .F. ) ;
#58546 = CARTESIAN_POINT ( 'NONE',  ( -1.975475456537005874E-15, 27.37500000273118417, 5.000000000000000000 ) ) ;
#58547 = DIRECTION ( 'NONE',  ( -0.000000000000000000, 1.000000000000000000, -0.000000000000000000 ) ) ;
#58548 = CARTESIAN_POINT ( 'NONE',  ( -50.01589407740564042, -149.7500000027312126, 0.3983568153799778022 ) ) ;
#58549 = LINE ( 'NONE', #34091, #51723 ) ;
#58550 = ORIENTED_EDGE ( 'NONE', *, *, #62179, .F. ) ;
#58551 = EDGE_CURVE ( 'NONE', #50889, #38824, #13003, .T. ) ;
#58552 = DIRECTION ( 'NONE',  ( 0.000000000000000000, 0.000000000000000000, 1.000000000000000000 ) ) ;
#58553 = CARTESIAN_POINT ( 'NONE',  ( -2.229367062499996610, -13.39583333196774007, 3.861377020970582219 ) ) ;
#58554 = CARTESIAN_POINT ( 'NONE',  ( 5.000000000000000888, -105.4583333306021444, 2.886751345948126879 ) ) ;
#58555 = CARTESIAN_POINT ( 'NONE',  ( 2.229367062499998831, -3.645833331967739177, -3.861377020970580887 ) ) ;
#58556 = CARTESIAN_POINT ( 'NONE',  ( -1.339745962155610925, 4.330341803992665106, 5.000000000000000000 ) ) ;
#58557 = CARTESIAN_POINT ( 'NONE',  ( -4.458734124999999437, -154.0000000013656063, -1.846868145590735644 ) ) ;
#58558 = CARTESIAN_POINT ( 'NONE',  ( -4.458734124999997661, 21.52083333469893134, 2.574251347313722516 ) ) ;
#58559 = ORIENTED_EDGE ( 'NONE', *, *, #33927, .F. ) ;
#58560 = CARTESIAN_POINT ( 'NONE',  ( 4.458734124999998549, -93.72916666530105090, -2.574251347313721627 ) ) ;
#58561 = LINE ( 'NONE', #24460, #50046 ) ;
#58562 = CARTESIAN_POINT ( 'NONE',  ( 5.000000000000000888, -40.58333333333334281, 2.886751345948126879 ) ) ;
#58563 = CARTESIAN_POINT ( 'NONE',  ( 4.458734125000001214, -15.89583333196773651, 2.574251347313718519 ) ) ;
#58564 = CARTESIAN_POINT ( 'NONE',  ( -5.000000000000000000, 28.12500000273118417, 0.000000000000000000 ) ) ;
#58565 = FACE_OUTER_BOUND ( 'NONE', #31580, .T. ) ;
#58566 =( BOUNDED_CURVE ( )  B_SPLINE_CURVE ( 2, ( #57671, #42540, #57356, #13276, #43167, #47997, #32900, #3949, #62806 ),
 .UNSPECIFIED., .F., .F. ) 
 B_SPLINE_CURVE_WITH_KNOTS ( ( 3, 2, 2, 2, 3 ),
 ( 0.02291666666666666852, 0.02361111111111111049, 0.02500000000000000139, 0.02638888888888888881, 0.02708333333333333426 ),
 .UNSPECIFIED. ) 
 CURVE ( )  GEOMETRIC_REPRESENTATION_ITEM ( )  RATIONAL_B_SPLINE_CURVE ( ( 0.9330127018922194093, 0.9330127018922195203, 1.000000000000000000, 0.8660254037844387076, 1.000000000000000000, 0.8660254037844387076, 1.000000000000000000, 0.9330127018922191873, 0.9330127018922194093 ) ) 
 REPRESENTATION_ITEM ( '' )  );
#58567 = CARTESIAN_POINT ( 'NONE',  ( -53.51423613279429503, -152.2500000013656347, 4.591703134518082763 ) ) ;
#58568 = EDGE_CURVE ( 'NONE', #49961, #47640, #18142, .T. ) ;
#58569 = CARTESIAN_POINT ( 'NONE',  ( 2.499999999999998668, -41.20833333060214443, -4.330127018922193649 ) ) ;
#58570 = LINE ( 'NONE', #52800, #48289 ) ;
#58571 = CARTESIAN_POINT ( 'NONE',  ( 4.458734125000000326, 18.10416666803225993, 2.574251347313718519 ) ) ;
#58572 = DIRECTION ( 'NONE',  ( -0.000000000000000000, 1.000000000000000000, -0.000000000000000000 ) ) ;
#58573 = ORIENTED_EDGE ( 'NONE', *, *, #22568, .F. ) ;
#58574 = CARTESIAN_POINT ( 'NONE',  ( -3.152548672688508926E-16, 18.43750000136559564, -5.148502694627439702 ) ) ;
#58575 = CARTESIAN_POINT ( 'NONE',  ( -2.229367062499996610, -62.14583333196774362, 3.861377020970582219 ) ) ;
#58576 = CARTESIAN_POINT ( 'NONE',  ( 2.229367062499998831, -6.895833331967741842, -3.861377020970580887 ) ) ;
#58577 = CARTESIAN_POINT ( 'NONE',  ( 3.535533905932738197, -169.0000000027312126, -3.535533905932738197 ) ) ;
#58578 = CARTESIAN_POINT ( 'NONE',  ( 5.000000000000000888, 8.416666666666666075, 2.886751345948126879 ) ) ;
#58579 = CARTESIAN_POINT ( 'NONE',  ( 4.458734125000000326, -166.3750000013655779, -1.846868145590734978 ) ) ;
#58580 = CARTESIAN_POINT ( 'NONE',  ( -2.500000000000000444, -99.04166666393545881, -4.330127018922193649 ) ) ;
#58581 = AXIS2_PLACEMENT_3D ( 'NONE', #7435, #32173, #7748 ) ;
#58582 = CARTESIAN_POINT ( 'NONE',  ( 4.458734124999998549, -54.72916666530107932, -2.574251347313721627 ) ) ;
#58583 = CARTESIAN_POINT ( 'NONE',  ( -2.500000000000000444, -91.04166666393547303, -4.330127018922193649 ) ) ;
#58584 = CARTESIAN_POINT ( 'NONE',  ( -6.972266317189433020E-16, 21.75000000000000000, -5.000000000000000000 ) ) ;
#58585 =( BOUNDED_CURVE ( )  B_SPLINE_CURVE ( 2, ( #10570, #5116, #55294, #44338, #49809, #19900, #39514, #5754, #59152 ),
 .UNSPECIFIED., .F., .F. ) 
 B_SPLINE_CURVE_WITH_KNOTS ( ( 3, 2, 2, 2, 3 ),
 ( 0.7145833333333333481, 0.7152777777777777901, 0.7166666666666666741, 0.7180555555555555580, 0.7187500000000000000 ),
 .UNSPECIFIED. ) 
 CURVE ( )  GEOMETRIC_REPRESENTATION_ITEM ( )  RATIONAL_B_SPLINE_CURVE ( ( 0.9330127018922194093, 0.9330127018922194093, 1.000000000000000000, 0.8660254037844387076, 1.000000000000000000, 0.8660254037844387076, 1.000000000000000000, 0.9330127018922194093, 0.9330127018922194093 ) ) 
 REPRESENTATION_ITEM ( '' )  );
#58586 = CARTESIAN_POINT ( 'NONE',  ( 1.339745962155611592, 25.41965820146970501, 5.000000000000000888 ) ) ;
#58587 = DIRECTION ( 'NONE',  ( -0.000000000000000000, 1.000000000000000000, -0.000000000000000000 ) ) ;
#58588 = CARTESIAN_POINT ( 'NONE',  ( -3.152801135295367985, -152.0625000013655779, 3.152801135295367096 ) ) ;
#58589 = CARTESIAN_POINT ( 'NONE',  ( 2.500000000000002220, -39.66666666666667140, 4.330127018922192761 ) ) ;
#58590 = CARTESIAN_POINT ( 'NONE',  ( 5.000000000000000888, -98.45833333060213022, 2.886751345948126879 ) ) ;
#58591 = CARTESIAN_POINT ( 'NONE',  ( 1.975475456537005874E-15, 15.37500000273118417, 5.000000000000000000 ) ) ;
#58592 = EDGE_LOOP ( 'NONE', ( #15157, #22884, #22359, #4420 ) ) ;
#58593 = CARTESIAN_POINT ( 'NONE',  ( 4.458734124999998549, -101.7291666653010793, -2.574251347313721627 ) ) ;
#58594 = CARTESIAN_POINT ( 'NONE',  ( 9.457646018065525792E-16, 4.687500001365596525, 5.148502694627439702 ) ) ;
#58595 = CARTESIAN_POINT ( 'NONE',  ( -6.972266317189433020E-16, 12.75000000000000178, -5.000000000000000000 ) ) ;
#58596 = CARTESIAN_POINT ( 'NONE',  ( 2.499999999999998668, 4.666666666666666075, -4.330127018922193649 ) ) ;
#58597 = CARTESIAN_POINT ( 'NONE',  ( 4.458734125000000326, -62.89583333196774362, 2.574251347313718519 ) ) ;
#58598 = DIRECTION ( 'NONE',  ( 0.000000000000000000, 0.000000000000000000, 1.000000000000000000 ) ) ;
#58599 = ADVANCED_FACE ( 'NONE', ( #61594 ), #51310, .F. ) ;
#58600 = EDGE_CURVE ( 'NONE', #26022, #55695, #6463, .T. ) ;
#58601 = CARTESIAN_POINT ( 'NONE',  ( -2.500000000000000444, -4.041666663935479242, -4.330127018922193649 ) ) ;
#58603 = ORIENTED_EDGE ( 'NONE', *, *, #61045, .T. ) ;
#58602 = CARTESIAN_POINT ( 'NONE',  ( -2.229367062500000163, -31.47916666530107577, -3.861377020970580443 ) ) ;
#58604 = CARTESIAN_POINT ( 'NONE',  ( -2.500000000000000444, -42.16666666666667140, -4.330127018922193649 ) ) ;
#58605 = CARTESIAN_POINT ( 'NONE',  ( -6.972266317189433020E-16, -42.24999999999998579, -5.000000000000000000 ) ) ;
#58606 = CARTESIAN_POINT ( 'NONE',  ( -5.000000000000000000, 24.91666666666666785, -2.886751345948128211 ) ) ;
#58607 = CARTESIAN_POINT ( 'NONE',  ( -3.535250795749689387E-16, -43.24999999999999289, -5.773502691896257311 ) ) ;
#58608 = CARTESIAN_POINT ( 'NONE',  ( 2.229367062500001939, -23.22916666530107221, 3.861377020970579999 ) ) ;
#58609 = DIRECTION ( 'NONE',  ( -0.000000000000000000, 1.000000000000000000, -0.000000000000000000 ) ) ;
#58610 = CARTESIAN_POINT ( 'NONE',  ( 2.229367062500001939, -67.97916666530106511, 3.861377020970579999 ) ) ;
#58611 = CARTESIAN_POINT ( 'NONE',  ( -4.458734124999999437, -144.1875000013656063, -5.460374474430324690E-16 ) ) ;
#58612 = CARTESIAN_POINT ( 'NONE',  ( -2.229367062500000163, -75.47916666530106511, -3.861377020970580443 ) ) ;
#58613 = CARTESIAN_POINT ( 'NONE',  ( -59.44456063193725015, -140.8125000013656063, -0.3552334253322034230 ) ) ;
#58614 = ADVANCED_FACE ( 'NONE', ( #8499 ), #32623, .T. ) ;
#58615 = CARTESIAN_POINT ( 'NONE',  ( 4.458734124999999437, -30.06249999863440436, -5.460374474430324690E-16 ) ) ;
#58616 = CARTESIAN_POINT ( 'NONE',  ( 1.060575238724906964E-15, -68.62499999726881583, 5.773502691896257311 ) ) ;
#58617 = ORIENTED_EDGE ( 'NONE', *, *, #19949, .F. ) ;
#58618 = CARTESIAN_POINT ( 'NONE',  ( -59.98410592259440222, -148.2500000027312126, -0.3983568153799752487 ) ) ;
#58620 = EDGE_LOOP ( 'NONE', ( #7385, #32444, #32605, #48335 ) ) ;
#58619 = EDGE_CURVE ( 'NONE', #17564, #35972, #39303, .T. ) ;
#58621 = CARTESIAN_POINT ( 'NONE',  ( 2.229367062500001939, -75.22916666530106511, 3.861377020970579999 ) ) ;
#58622 = CARTESIAN_POINT ( 'NONE',  ( -5.000000000000000000, 28.99999999999999645, 0.000000000000000000 ) ) ;
#58623 = VERTEX_POINT ( 'NONE', #46156 ) ;
#58624 = VECTOR ( 'NONE', #14569, 1000.000000000000000 ) ;
#58625 = CARTESIAN_POINT ( 'NONE',  ( 1.975475456537005874E-15, -106.6249999972687874, 5.000000000000000000 ) ) ;
#58626 = CARTESIAN_POINT ( 'NONE',  ( -4.458734124999999437, -58.64583333196774362, -2.574251347313719407 ) ) ;
#58627 = CARTESIAN_POINT ( 'NONE',  ( 9.457646018065525792E-16, 3.687500001365594748, 5.148502694627439702 ) ) ;
#58628 = ORIENTED_EDGE ( 'NONE', *, *, #9512, .F. ) ;
#58629 = CARTESIAN_POINT ( 'NONE',  ( -5.000000000000000000, -146.5000000000000284, -6.123233995736766282E-16 ) ) ;
#58630 = CARTESIAN_POINT ( 'NONE',  ( -1.339745962155613368, 28.91965820146970501, -5.000000000000000000 ) ) ;
#58631 = CARTESIAN_POINT ( 'NONE',  ( 4.458734124999998549, 13.27083333469892779, -2.574251347313721627 ) ) ;
#58632 = CARTESIAN_POINT ( 'NONE',  ( -50.70258187064364108, -145.1250000013655779, 2.196230717870141014 ) ) ;
#58633 = CARTESIAN_POINT ( 'NONE',  ( 2.500000000000002220, -32.66666666666666430, 4.330127018922192761 ) ) ;
#58634 = CARTESIAN_POINT ( 'NONE',  ( 2.730187237215162345E-16, -166.1875000013655779, -4.458734124999999437 ) ) ;
#58635 =( BOUNDED_CURVE ( )  B_SPLINE_CURVE ( 2, ( #35993, #6724, #40486, #26334, #7045, #45951, #20883, #1916, #60127 ),
 .UNSPECIFIED., .F., .F. ) 
 B_SPLINE_CURVE_WITH_KNOTS ( ( 3, 2, 2, 2, 3 ),
 ( 0.4770833333333333592, 0.4777777777777778012, 0.4791666666666666852, 0.4805555555555555691, 0.4812500000000000111 ),
 .UNSPECIFIED. ) 
 CURVE ( )  GEOMETRIC_REPRESENTATION_ITEM ( )  RATIONAL_B_SPLINE_CURVE ( ( 0.9330127018922194093, 0.9330127018922220739, 1.000000000000000000, 0.8660254037844387076, 1.000000000000000000, 0.8660254037844387076, 1.000000000000000000, 0.9330127018922194093, 0.9330127018922194093 ) ) 
 REPRESENTATION_ITEM ( '' )  );
#58636 = ORIENTED_EDGE ( 'NONE', *, *, #62620, .T. ) ;
#58637 = CARTESIAN_POINT ( 'NONE',  ( -4.458734124999999437, -76.39583333196773651, -2.574251347313719407 ) ) ;
#58638 = CARTESIAN_POINT ( 'NONE',  ( 1.975475456537005874E-15, -16.74999999999999645, 5.000000000000000000 ) ) ;
#58639 = CARTESIAN_POINT ( 'NONE',  ( -4.458734124999998549, 3.770833334698929562, 2.574251347313722516 ) ) ;
#58640 = CARTESIAN_POINT ( 'NONE',  ( -2.499999999999996447, -42.70833333060214443, 4.330127018922195425 ) ) ;
#58641 = CARTESIAN_POINT ( 'NONE',  ( 2.229367062499998831, -65.89583333196773651, -3.861377020970580887 ) ) ;
#58642 = CARTESIAN_POINT ( 'NONE',  ( -4.999999999999999112, -22.79166666393548013, 2.886751345948131764 ) ) ;
#58643 = LINE ( 'NONE', #48352, #33709 ) ;
#58644 = CARTESIAN_POINT ( 'NONE',  ( 1.339745962155615144, -44.58034179853027723, 4.999999999999999112 ) ) ;
#58645 = DIRECTION ( 'NONE',  ( 0.000000000000000000, 1.000000000000000000, 0.000000000000000000 ) ) ;
#58646 = CARTESIAN_POINT ( 'NONE',  ( -2.229367062499996610, -46.14583333196774362, 3.861377020970582219 ) ) ;
#58647 = CARTESIAN_POINT ( 'NONE',  ( -3.152548672688508926E-16, -24.81249999863440436, -5.148502694627439702 ) ) ;
#58648 = CARTESIAN_POINT ( 'NONE',  ( -4.458734124999997661, 8.520833334698926009, 2.574251347313722516 ) ) ;
#58649 = CARTESIAN_POINT ( 'NONE',  ( -2.500000000000000444, 25.83333333333333215, -4.330127018922193649 ) ) ;
#58650 = CARTESIAN_POINT ( 'NONE',  ( 2.071067811865476394, -148.3125000027312126, 5.000000000000000000 ) ) ;
#58651 = CARTESIAN_POINT ( 'NONE',  ( -5.000000000000000000, -50.08333333333332860, -2.886751345948128211 ) ) ;
#58652 = CARTESIAN_POINT ( 'NONE',  ( 4.458734124999999437, -39.81249999863440081, -5.460374474430324690E-16 ) ) ;
#58653 = CARTESIAN_POINT ( 'NONE',  ( -5.000000000000000000, -72.95833333060214443, -2.886751345948128211 ) ) ;
#58654 = CARTESIAN_POINT ( 'NONE',  ( -51.60603307380591787, -144.1875000013656063, -2.891590998281053704 ) ) ;
#58655 = CARTESIAN_POINT ( 'NONE',  ( 5.000000000000000888, -141.9375000000000000, -2.071067811865475505 ) ) ;
#58656 = CARTESIAN_POINT ( 'NONE',  ( -4.458734124999997661, -74.47916666530106511, 2.574251347313722516 ) ) ;
#58657 = CARTESIAN_POINT ( 'NONE',  ( 3.152801135295366208, -166.8125000013656063, 3.152801135295367985 ) ) ;
#58658 = CARTESIAN_POINT ( 'NONE',  ( 4.458734125000000326, -31.89583333196773651, 2.574251347313718519 ) ) ;
#58659 = CARTESIAN_POINT ( 'NONE',  ( 7.500000000000000000, -4.330127018922199866, -7.422398894150035176 ) ) ;
#58660 = CARTESIAN_POINT ( 'NONE',  ( 2.500000000000002220, -45.54166666393547303, 4.330127018922192761 ) ) ;
#58661 = CARTESIAN_POINT ( 'NONE',  ( -5.000000000000000000, -24.00000000000000000, 0.000000000000000000 ) ) ;
#58662 = CARTESIAN_POINT ( 'NONE',  ( 1.846868145590735200, -143.2500000013655779, -4.458734125000000326 ) ) ;
#58663 = ORIENTED_EDGE ( 'NONE', *, *, #14961, .T. ) ;
#58664 = CARTESIAN_POINT ( 'NONE',  ( -2.229367062500000163, 29.27083333469892779, -3.861377020970580443 ) ) ;
#58665 = CARTESIAN_POINT ( 'NONE',  ( 2.229367062499998831, -56.89583333196773651, -3.861377020970580887 ) ) ;
#58666 =( BOUNDED_CURVE ( )  B_SPLINE_CURVE ( 2, ( #60991, #50371, #11444, #7278, #26889, #2452, #45542, #31063, #6630 ),
 .UNSPECIFIED., .F., .F. ) 
 B_SPLINE_CURVE_WITH_KNOTS ( ( 3, 2, 2, 2, 3 ),
 ( 0.3354166666666666963, 0.3361111111111111382, 0.3375000000000000222, 0.3388888888888889062, 0.3395833333333333481 ),
 .UNSPECIFIED. ) 
 CURVE ( )  GEOMETRIC_REPRESENTATION_ITEM ( )  RATIONAL_B_SPLINE_CURVE ( ( 0.9330127018922194093, 0.9330127018922220739, 1.000000000000000000, 0.8660254037844387076, 1.000000000000000000, 0.8660254037844387076, 1.000000000000000000, 0.9330127018922194093, 0.9330127018922194093 ) ) 
 REPRESENTATION_ITEM ( '' )  );
#58667 = CARTESIAN_POINT ( 'NONE',  ( 2.499999999999998668, 28.79166666939784847, -4.330127018922193649 ) ) ;
#58668 = CARTESIAN_POINT ( 'NONE',  ( 5.000000000000000888, 17.41666666666666430, 2.886751345948126879 ) ) ;
#58669 = CARTESIAN_POINT ( 'NONE',  ( -1.339745962155610925, -88.79465819873851729, 5.000000000000000000 ) ) ;
#58670 = CARTESIAN_POINT ( 'NONE',  ( -2.229367062499996610, -4.145833331967739177, 3.861377020970582219 ) ) ;
#58671 = CARTESIAN_POINT ( 'NONE',  ( -2.500000000000000444, -23.16666666666666785, -4.330127018922193649 ) ) ;
#58672 = EDGE_CURVE ( 'NONE', #13547, #47522, #42586, .T. ) ;
#58673 = CARTESIAN_POINT ( 'NONE',  ( 0.000000000000000000, -170.0000000000000000, 0.000000000000000000 ) ) ;
#58674 = CARTESIAN_POINT ( 'NONE',  ( 1.975475456537005874E-15, 0.2500000000000001665, 5.000000000000000000 ) ) ;
#58675 = LINE ( 'NONE', #63197, #19178 ) ;
#58677 = CARTESIAN_POINT ( 'NONE',  ( 4.458734124999998549, -22.72916666530107221, -2.574251347313721627 ) ) ;
#58676 = CARTESIAN_POINT ( 'NONE',  ( -1.339745962155613812, 4.794658198738519950, -5.000000000000000000 ) ) ;
#58678 = PLANE ( 'NONE',  #8094 ) ;
#58679 = CARTESIAN_POINT ( 'NONE',  ( 2.229367062500001939, -52.97916666530107221, 3.861377020970579999 ) ) ;
#58680 = CARTESIAN_POINT ( 'NONE',  ( -1.846868145590737420, -158.0000000013655779, 4.458734124999999437 ) ) ;
#58681 = CARTESIAN_POINT ( 'NONE',  ( -4.999999999999999112, -49.79166666393547303, 2.886751345948131764 ) ) ;
#58682 = VERTEX_POINT ( 'NONE', #56127 ) ;
#58683 = CARTESIAN_POINT ( 'NONE',  ( 4.458734125000001214, 3.854166668032260823, 2.574251347313718519 ) ) ;
#58684 = ORIENTED_EDGE ( 'NONE', *, *, #39442, .F. ) ;
#58686 = DIRECTION ( 'NONE',  ( -0.000000000000000000, 1.000000000000000000, -0.000000000000000000 ) ) ;
#58685 = DIRECTION ( 'NONE',  ( -0.000000000000000000, 1.000000000000000000, -0.000000000000000000 ) ) ;
#58687 = CARTESIAN_POINT ( 'NONE',  ( 1.846868145590735200, -158.2500000013656063, -4.458734125000000326 ) ) ;
#58688 = EDGE_CURVE ( 'NONE', #46066, #2855, #22672, .T. ) ;
#58689 = ORIENTED_EDGE ( 'NONE', *, *, #56301, .T. ) ;
#58690 = ADVANCED_FACE ( 'NONE', ( #27792 ), #42271, .T. ) ;
#58691 = CARTESIAN_POINT ( 'NONE',  ( 2.500000000000002220, -23.54166666393548368, 4.330127018922192761 ) ) ;
#58692 = CARTESIAN_POINT ( 'NONE',  ( -59.98410592259440222, -132.1250000000000284, -0.3983568153799752487 ) ) ;
#58693 = CARTESIAN_POINT ( 'NONE',  ( 4.458734124999999437, -41.06249999863440081, -5.460374474430324690E-16 ) ) ;
#58694 = VERTEX_POINT ( 'NONE', #13322 ) ;
#58695 = EDGE_CURVE ( 'NONE', #49893, #25625, #23739, .T. ) ;
#58696 = CARTESIAN_POINT ( 'NONE',  ( -2.499999999999996447, -45.83333333333333570, 4.330127018922195425 ) ) ;
#58697 = CARTESIAN_POINT ( 'NONE',  ( -2.229367062499996610, 19.85416666803225993, 3.861377020970582219 ) ) ;
#58698 = DIRECTION ( 'NONE',  ( 0.000000000000000000, 0.000000000000000000, 1.000000000000000000 ) ) ;
#58699 = VERTEX_POINT ( 'NONE', #12376 ) ;
#58700 = CARTESIAN_POINT ( 'NONE',  ( 4.458734124999998549, 27.27083333469892423, -2.574251347313721627 ) ) ;
#58701 = CARTESIAN_POINT ( 'NONE',  ( -56.66612745406270335, -125.4375000027312126, -5.149110718188516067 ) ) ;
#58702 = CYLINDRICAL_SURFACE ( 'NONE', #48018, 5.000000000000000000 ) ;
#58703 = CARTESIAN_POINT ( 'NONE',  ( 5.000000000000000000, -100.4166666666666572, -2.886751345948130876 ) ) ;
#58704 = LINE ( 'NONE', #14951, #28148 ) ;
#58705 = CARTESIAN_POINT ( 'NONE',  ( 4.458734124999998549, -59.72916666530106511, -2.574251347313721627 ) ) ;
#58706 = DIRECTION ( 'NONE',  ( 0.000000000000000000, 1.000000000000000000, 0.000000000000000000 ) ) ;
#58707 = VECTOR ( 'NONE', #56458, 1000.000000000000000 ) ;
#58708 = CARTESIAN_POINT ( 'NONE',  ( -2.229367062499996610, 15.85416666803226171, 3.861377020970582219 ) ) ;
#58709 = CARTESIAN_POINT ( 'NONE',  ( -5.000000000000000000, -90.00000000000000000, 0.000000000000000000 ) ) ;
#58710 = CARTESIAN_POINT ( 'NONE',  ( 2.229367062499998831, -49.89583333196772941, -3.861377020970580887 ) ) ;
#58711 = CARTESIAN_POINT ( 'NONE',  ( 5.000000000000000888, -9.458333330602144429, 2.886751345948126879 ) ) ;
#58712 = CARTESIAN_POINT ( 'NONE',  ( -5.000000000000000000, -93.00000000000000000, 0.000000000000000000 ) ) ;
#58713 = CARTESIAN_POINT ( 'NONE',  ( -5.000000000000000000, -66.95833333060214443, -2.886751345948128211 ) ) ;
#58714 = DIRECTION ( 'NONE',  ( 0.000000000000000000, 0.000000000000000000, 1.000000000000000000 ) ) ;
#58715 = CARTESIAN_POINT ( 'NONE',  ( -2.229367062500000163, -109.4791666653010651, -3.861377020970580443 ) ) ;
#58716 = CARTESIAN_POINT ( 'NONE',  ( 9.457646018065525792E-16, -12.31249999863440259, 5.148502694627439702 ) ) ;
#58717 = VERTEX_POINT ( 'NONE', #31989 ) ;
#58718 = CARTESIAN_POINT ( 'NONE',  ( 5.000000000000000000, -9.291666663935483683, -2.886751345948130876 ) ) ;
#58719 = CARTESIAN_POINT ( 'NONE',  ( -4.458734124999998549, -96.22916666530106511, 2.574251347313722516 ) ) ;
#58720 = CARTESIAN_POINT ( 'NONE',  ( 2.071067811865476394, -160.3125000027312410, 5.000000000000000000 ) ) ;
#58721 = CARTESIAN_POINT ( 'NONE',  ( -2.229367062500000163, -97.72916666530105090, -3.861377020970580443 ) ) ;
#58722 = CARTESIAN_POINT ( 'NONE',  ( 5.000000000000000000, -49.37499999726880873, -6.123233995736766282E-16 ) ) ;
#58723 = CARTESIAN_POINT ( 'NONE',  ( 5.000000000000000000, -50.29166666393548013, -2.886751345948129988 ) ) ;
#58724 = CARTESIAN_POINT ( 'NONE',  ( -62.00000000000001421, -155.0000000000000284, 4.041451884327384114 ) ) ;
#58725 = CARTESIAN_POINT ( 'NONE',  ( -52.10840900171896806, -129.1875000013656063, 3.393966926194110556 ) ) ;
#58726 = CARTESIAN_POINT ( 'NONE',  ( -59.59170313451810586, -147.5000000013656063, 1.485763867205729394 ) ) ;
#58727 = CARTESIAN_POINT ( 'NONE',  ( 4.458734124999999437, -20.81249999863440081, -5.460374474430324690E-16 ) ) ;
#58728 = CARTESIAN_POINT ( 'NONE',  ( 4.458734125000001214, 4.854166668032262599, 2.574251347313718519 ) ) ;
#58729 = CARTESIAN_POINT ( 'NONE',  ( 4.458734125000000326, -57.14583333196773651, 2.574251347313718519 ) ) ;
#58730 = CARTESIAN_POINT ( 'NONE',  ( -4.999999999999998224, -53.91666666666667140, 2.886751345948131764 ) ) ;
#58731 = CARTESIAN_POINT ( 'NONE',  ( 4.458734125000000326, -11.89583333196774184, 2.574251347313718519 ) ) ;
#58732 = DIRECTION ( 'NONE',  ( 0.000000000000000000, 0.000000000000000000, -1.000000000000000000 ) ) ;
#58733 = CARTESIAN_POINT ( 'NONE',  ( -9.184850993605147944E-16, -155.2500000000000000, 5.000000000000000000 ) ) ;
#58734 = CARTESIAN_POINT ( 'NONE',  ( 1.060575238724906964E-15, -8.750000000000000000, 5.773502691896257311 ) ) ;
#58735 = ORIENTED_EDGE ( 'NONE', *, *, #29916, .F. ) ;
#58736 = CARTESIAN_POINT ( 'NONE',  ( -4.458734124999997661, -41.47916666530107932, 2.574251347313722516 ) ) ;
#58737 = DIRECTION ( 'NONE',  ( 0.000000000000000000, 0.000000000000000000, 1.000000000000000000 ) ) ;
#58738 = CARTESIAN_POINT ( 'NONE',  ( -4.406466114815342117, 6.116179640280717145, -7.446478553995464544 ) ) ;
#58739 = CARTESIAN_POINT ( 'NONE',  ( -6.972266317189433020E-16, -2.250000000000000000, -5.000000000000000000 ) ) ;
#58740 = CARTESIAN_POINT ( 'NONE',  ( 4.458734125000001214, -83.89583333196773651, 2.574251347313718519 ) ) ;
#58741 = CARTESIAN_POINT ( 'NONE',  ( -4.458734124999999437, 18.35416666803225993, -2.574251347313719407 ) ) ;
#58742 = CARTESIAN_POINT ( 'NONE',  ( 2.229367062499998831, 11.35416666803225993, -3.861377020970580887 ) ) ;
#58743 = CARTESIAN_POINT ( 'NONE',  ( 2.499999999999998668, -0.3333333333333348136, -4.330127018922193649 ) ) ;
#58744 = CARTESIAN_POINT ( 'NONE',  ( 4.458734125000000326, -89.14583333196773651, 2.574251347313718519 ) ) ;
#58745 = CARTESIAN_POINT ( 'NONE',  ( 4.458734124999999437, 21.93750000136559208, -5.460374474430324690E-16 ) ) ;
#58746 = CARTESIAN_POINT ( 'NONE',  ( -5.000000000000000000, -75.08333333333332860, -2.886751345948128211 ) ) ;
#58747 = CARTESIAN_POINT ( 'NONE',  ( -3.535250795749689387E-16, 12.87500000273118417, -5.773502691896257311 ) ) ;
#58748 = VERTEX_POINT ( 'NONE', #7557 ) ;
#58749 = CARTESIAN_POINT ( 'NONE',  ( -4.999999999999998224, -6.791666663935481019, 2.886751345948131764 ) ) ;
#58750 = ORIENTED_EDGE ( 'NONE', *, *, #16773, .F. ) ;
#58752 = CARTESIAN_POINT ( 'NONE',  ( 2.500000000000002220, -34.66666666666666430, 4.330127018922192761 ) ) ;
#58751 = FACE_OUTER_BOUND ( 'NONE', #58880, .T. ) ;
#58753 = CARTESIAN_POINT ( 'NONE',  ( 2.229367062500001939, -38.97916666530107221, 3.861377020970579999 ) ) ;
#58754 =( BOUNDED_CURVE ( )  B_SPLINE_CURVE ( 2, ( #22330, #7225, #61254, #51911, #22652, #42562, #60940, #46765, #50961 ),
 .UNSPECIFIED., .F., .F. ) 
 B_SPLINE_CURVE_WITH_KNOTS ( ( 3, 2, 2, 2, 3 ),
 ( 0.3187499999999999778, 0.3194444444444444198, 0.3208333333333333592, 0.3222222222222222432, 0.3229166666666666852 ),
 .UNSPECIFIED. ) 
 CURVE ( )  GEOMETRIC_REPRESENTATION_ITEM ( )  RATIONAL_B_SPLINE_CURVE ( ( 0.9330127018922194093, 0.9330127018922194093, 1.000000000000000000, 0.8660254037844387076, 1.000000000000000000, 0.8660254037844387076, 1.000000000000000000, 0.9330127018922194093, 0.9330127018922194093 ) ) 
 REPRESENTATION_ITEM ( '' )  );
#58755 = CARTESIAN_POINT ( 'NONE',  ( -2.500000000000000444, -34.04166666393547303, -4.330127018922193649 ) ) ;
#58757 = ORIENTED_EDGE ( 'NONE', *, *, #10205, .F. ) ;
#58756 = CARTESIAN_POINT ( 'NONE',  ( 2.229367062499998831, -63.64583333196772941, -3.861377020970580887 ) ) ;
#58758 = CARTESIAN_POINT ( 'NONE',  ( -58.39396692619412477, -152.6875000013656063, 2.891590998281057701 ) ) ;
#58759 = CARTESIAN_POINT ( 'NONE',  ( 2.229367062499998831, -10.64583333196773829, -3.861377020970580887 ) ) ;
#58761 = ORIENTED_EDGE ( 'NONE', *, *, #18161, .F. ) ;
#58760 = CARTESIAN_POINT ( 'NONE',  ( 2.229367062499998831, -16.89583333196773651, -3.861377020970580887 ) ) ;
#58762 = CARTESIAN_POINT ( 'NONE',  ( -5.000000000000000000, -82.00000000000000000, 0.000000000000000000 ) ) ;
#58763 = CARTESIAN_POINT ( 'NONE',  ( 1.975475456537005874E-15, -103.7500000000000000, 5.000000000000000000 ) ) ;
#58764 = CARTESIAN_POINT ( 'NONE',  ( -4.458734124999999437, -58.64583333196774362, -2.574251347313719407 ) ) ;
#58765 = CARTESIAN_POINT ( 'NONE',  ( -5.000000000000000000, -81.87499999726881583, 0.000000000000000000 ) ) ;
#58767 = VERTEX_POINT ( 'NONE', #2732 ) ;
#58766 = CARTESIAN_POINT ( 'NONE',  ( 1.339745962155586056, 3.419658201469704562, 5.000000000000015987 ) ) ;
#58768 = CARTESIAN_POINT ( 'NONE',  ( -50.18089887299979068, -144.6875000000000568, 2.462841084822635640 ) ) ;
#58769 = CARTESIAN_POINT ( 'NONE',  ( 4.458734124999999437, -27.06249999863440081, -5.460374474430324690E-16 ) ) ;
#58770 = EDGE_LOOP ( 'NONE', ( #44122, #13676, #52118, #49963 ) ) ;
#58771 = APPLICATION_PROTOCOL_DEFINITION ( 'draft international standard', 'automotive_design', 1998, #4731 ) ;
#58772 = CARTESIAN_POINT ( 'NONE',  ( -1.846868145590734756, -165.3750000013656347, -4.458734125000000326 ) ) ;
#58773 = CARTESIAN_POINT ( 'NONE',  ( -2.229367062500000163, -107.7291666653010651, -3.861377020970580443 ) ) ;
#58774 = VERTEX_POINT ( 'NONE', #19073 ) ;
#58775 = CARTESIAN_POINT ( 'NONE',  ( -59.44456063193725015, -147.8125000013656063, -0.3552334253322034230 ) ) ;
#58776 = CARTESIAN_POINT ( 'NONE',  ( -51.75738570946856498, -137.8750000027312126, 3.805975901505576964 ) ) ;
#58777 = CARTESIAN_POINT ( 'NONE',  ( -2.229367062499996610, -40.14583333196773651, 3.861377020970582219 ) ) ;
#58778 = CARTESIAN_POINT ( 'NONE',  ( 4.458734124999999437, -144.6875000013656063, 0.000000000000000000 ) ) ;
#58779 = CARTESIAN_POINT ( 'NONE',  ( 0.000000000000000000, -170.0000000000000000, 0.000000000000000000 ) ) ;
#58780 = CARTESIAN_POINT ( 'NONE',  ( 1.975475456537005874E-15, 0.2500000000000001665, 5.000000000000000000 ) ) ;
#58781 = CARTESIAN_POINT ( 'NONE',  ( -4.458734124999999437, -10.31249999863440792, 0.000000000000000000 ) ) ;
#58782 = CARTESIAN_POINT ( 'NONE',  ( -4.458734124999997661, -99.47916666530105090, 2.574251347313722516 ) ) ;
#58783 = EDGE_LOOP ( 'NONE', ( #13983, #28410, #59879, #37983 ) ) ;
#58784 = CARTESIAN_POINT ( 'NONE',  ( 4.458734124999999437, -143.6875000013656063, 0.000000000000000000 ) ) ;
#58785 = CARTESIAN_POINT ( 'NONE',  ( 4.458734125000001214, -36.14583333196773651, 2.574251347313718519 ) ) ;
#58786 = CARTESIAN_POINT ( 'NONE',  ( 2.500000000000002220, 7.458333336064517205, 4.330127018922192761 ) ) ;
#58787 = CARTESIAN_POINT ( 'NONE',  ( -5.000000000000000000, 11.91666666666666607, -2.886751345948128211 ) ) ;
#58788 = CARTESIAN_POINT ( 'NONE',  ( -52.80376928212989185, -133.8750000013656063, -4.297418129356379346 ) ) ;
#58789 = CARTESIAN_POINT ( 'NONE',  ( 9.457646018065525792E-16, -66.31249999863440792, 5.148502694627439702 ) ) ;
#58790 = DIRECTION ( 'NONE',  ( -0.000000000000000000, 1.000000000000000000, -0.000000000000000000 ) ) ;
#58791 = CARTESIAN_POINT ( 'NONE',  ( -58.24261429053147765, -146.3750000027312126, -3.805975901505573855 ) ) ;
#58792 = CARTESIAN_POINT ( 'NONE',  ( -6.602753909532903975, -5.319290460493544259, -7.792447862505333056 ) ) ;
#58793 = CARTESIAN_POINT ( 'NONE',  ( -4.458734124999999437, 5.354166668032261711, -2.574251347313719407 ) ) ;
#58794 = ORIENTED_EDGE ( 'NONE', *, *, #4010, .F. ) ;
#58795 = DIRECTION ( 'NONE',  ( -0.000000000000000000, 1.000000000000000000, -0.000000000000000000 ) ) ;
#58797 = CARTESIAN_POINT ( 'NONE',  ( -4.458734124999998549, -28.22916666530106866, 2.574251347313722516 ) ) ;
#58796 = CARTESIAN_POINT ( 'NONE',  ( 5.000000000000000000, -94.41666666666665719, -2.886751345948129988 ) ) ;
#58798 = CARTESIAN_POINT ( 'NONE',  ( -2.499999999999996447, -22.70833333060214443, 4.330127018922195425 ) ) ;
#58799 = CARTESIAN_POINT ( 'NONE',  ( -2.229367062500000163, -79.72916666530106511, -3.861377020970580443 ) ) ;
#58800 = CARTESIAN_POINT ( 'NONE',  ( -2.229367062500000163, 22.27083333469892423, -3.861377020970580443 ) ) ;
#58801 = CARTESIAN_POINT ( 'NONE',  ( 5.000000000000000888, -18.58333333333333215, 2.886751345948126879 ) ) ;
#58802 = CARTESIAN_POINT ( 'NONE',  ( -58.39396692619412477, -140.4375000013656063, 2.891590998281057701 ) ) ;
#58803 = CARTESIAN_POINT ( 'NONE',  ( 4.458734124999998549, -1.729166665301068440, -2.574251347313721627 ) ) ;
#58804 = CARTESIAN_POINT ( 'NONE',  ( 9.457646018065525792E-16, 24.68750000136559208, 5.148502694627439702 ) ) ;
#58805 = CARTESIAN_POINT ( 'NONE',  ( 4.458734124999999437, -42.06249999863440081, -5.460374474430324690E-16 ) ) ;
#58806 =( BOUNDED_CURVE ( )  B_SPLINE_CURVE ( 2, ( #25869, #36474, #35206, #31005, #55144, #5615, #35845, #50311, #16222 ),
 .UNSPECIFIED., .F., .F. ) 
 B_SPLINE_CURVE_WITH_KNOTS ( ( 3, 2, 2, 2, 3 ),
 ( 0.3660714285714285476, 0.3666666666666666408, 0.3678571428571428825, 0.3690476190476190688, 0.3696428571428571619 ),
 .UNSPECIFIED. ) 
 CURVE ( )  GEOMETRIC_REPRESENTATION_ITEM ( )  RATIONAL_B_SPLINE_CURVE ( ( 0.9330127018922194093, 0.9330127018922194093, 1.000000000000000000, 0.8660254037844387076, 1.000000000000000000, 0.8660254037844387076, 1.000000000000000000, 0.9330127018922194093, 0.9330127018922194093 ) ) 
 REPRESENTATION_ITEM ( '' )  );
#58807 = CARTESIAN_POINT ( 'NONE',  ( -1.339745962155610925, -45.66965819600733312, 5.000000000000000000 ) ) ;
#58808 = CARTESIAN_POINT ( 'NONE',  ( 4.458734124999999437, 4.187500001365595637, -5.460374474430324690E-16 ) ) ;
#58809 = ORIENTED_EDGE ( 'NONE', *, *, #52399, .F. ) ;
#58810 = CARTESIAN_POINT ( 'NONE',  ( -2.229367062499996610, -24.39583333196773651, 3.861377020970582219 ) ) ;
#58811 =( BOUNDED_CURVE ( )  B_SPLINE_CURVE ( 2, ( #17465, #31611, #51247, #47044, #32239, #51868, #7811, #18078, #18400 ),
 .UNSPECIFIED., .F., .F. ) 
 B_SPLINE_CURVE_WITH_KNOTS ( ( 3, 2, 2, 2, 3 ),
 ( 0.4732142857142856984, 0.4738095238095237915, 0.4749999999999999778, 0.4761904761904761640, 0.4767857142857143127 ),
 .UNSPECIFIED. ) 
 CURVE ( )  GEOMETRIC_REPRESENTATION_ITEM ( )  RATIONAL_B_SPLINE_CURVE ( ( 0.9330127018922194093, 0.9330127018922194093, 1.000000000000000000, 0.8660254037844387076, 1.000000000000000000, 0.8660254037844387076, 1.000000000000000000, 0.9330127018922163007, 0.9330127018922194093 ) ) 
 REPRESENTATION_ITEM ( '' )  );
#58812 = CARTESIAN_POINT ( 'NONE',  ( 9.457646018065525792E-16, -67.06249999863440792, 5.148502694627439702 ) ) ;
#58813 = CARTESIAN_POINT ( 'NONE',  ( 5.000000000000000888, -106.4583333306021586, 2.886751345948126879 ) ) ;
#58814 = CARTESIAN_POINT ( 'NONE',  ( 4.458734124999999437, 25.18750000136559208, -5.460374474430324690E-16 ) ) ;
#58815 = CARTESIAN_POINT ( 'NONE',  ( 6.158835246850667461E-14, 9.749999999999996447, -4.999999999999999112 ) ) ;
#58816 = PLANE ( 'NONE',  #13177 ) ;
#58817 = CARTESIAN_POINT ( 'NONE',  ( -4.458734124999999437, -70.64583333196773651, -2.574251347313719407 ) ) ;
#58818 = CARTESIAN_POINT ( 'NONE',  ( 5.000000000000000000, -60.50000000000000000, -6.123233995736766282E-16 ) ) ;
#58819 = DIRECTION ( 'NONE',  ( 0.000000000000000000, 0.000000000000000000, 1.000000000000000000 ) ) ;
#58820 = CARTESIAN_POINT ( 'NONE',  ( -5.000000000000000000, 28.12500000273118417, 0.000000000000000000 ) ) ;
#58821 = ORIENTED_EDGE ( 'NONE', *, *, #62515, .F. ) ;
#58822 = CARTESIAN_POINT ( 'NONE',  ( -5.000000000000000000, -140.5000000000000000, -6.123233995736766282E-16 ) ) ;
#58823 = CARTESIAN_POINT ( 'NONE',  ( 3.044556291839386294E-14, 12.75000000000000000, -5.000000000000000000 ) ) ;
#58824 = CARTESIAN_POINT ( 'NONE',  ( -2.500000000000000444, -20.16666666666666430, -4.330127018922193649 ) ) ;
#58825 = CARTESIAN_POINT ( 'NONE',  ( 9.457646018065525792E-16, -22.06249999863440436, 5.148502694627439702 ) ) ;
#58826 = CARTESIAN_POINT ( 'NONE',  ( -2.229367062500000163, -80.47916666530106511, -3.861377020970580443 ) ) ;
#58827 = CARTESIAN_POINT ( 'NONE',  ( -3.152801135295367096, -167.3125000013656063, -3.152801135295367541 ) ) ;
#58828 = CARTESIAN_POINT ( 'NONE',  ( -5.000000000000000000, -15.87499999726881406, 0.000000000000000000 ) ) ;
#58830 = VERTEX_POINT ( 'NONE', #62850 ) ;
#58829 = CARTESIAN_POINT ( 'NONE',  ( -2.229367062499996610, -48.14583333196772941, 3.861377020970582219 ) ) ;
#58831 = CARTESIAN_POINT ( 'NONE',  ( 0.000000000000000000, -120.0000000000000000, 5.000000000000000000 ) ) ;
#58832 = CARTESIAN_POINT ( 'NONE',  ( -1.339745962155564296, -28.08034179853029144, -5.000000000000028422 ) ) ;
#58834 = ORIENTED_EDGE ( 'NONE', *, *, #13111, .T. ) ;
#58833 = CARTESIAN_POINT ( 'NONE',  ( 4.458734125000001214, 1.854166668032262155, 2.574251347313718519 ) ) ;
#58835 =( BOUNDED_CURVE ( )  B_SPLINE_CURVE ( 2, ( #26408, #35423, #60833, #15807, #51184, #7116, #49887, #46346, #59561 ),
 .UNSPECIFIED., .F., .F. ) 
 B_SPLINE_CURVE_WITH_KNOTS ( ( 3, 2, 2, 2, 3 ),
 ( 0.3982142857142857428, 0.3988095238095238360, 0.4000000000000000222, 0.4011904761904762085, 0.4017857142857143016 ),
 .UNSPECIFIED. ) 
 CURVE ( )  GEOMETRIC_REPRESENTATION_ITEM ( )  RATIONAL_B_SPLINE_CURVE ( ( 0.9330127018922194093, 0.9330127018922225179, 1.000000000000000000, 0.8660254037844387076, 1.000000000000000000, 0.8660254037844387076, 1.000000000000000000, 0.9330127018922194093, 0.9330127018922194093 ) ) 
 REPRESENTATION_ITEM ( '' )  );
#58836 = CARTESIAN_POINT ( 'NONE',  ( -53.51423613279429503, -154.2500000013656063, 4.591703134518083651 ) ) ;
#58837 = CARTESIAN_POINT ( 'NONE',  ( -2.499999999999996447, -66.83333333333332860, 4.330127018922195425 ) ) ;
#58838 = CARTESIAN_POINT ( 'NONE',  ( -4.458734124999999437, -157.1875000013655779, -5.460374474430324690E-16 ) ) ;
#58839 = CARTESIAN_POINT ( 'NONE',  ( 4.458734125000001214, -42.14583333196773651, 2.574251347313718519 ) ) ;
#58840 = CARTESIAN_POINT ( 'NONE',  ( 1.975475456537005874E-15, -39.75000000000000000, 5.000000000000000000 ) ) ;
#58841 = CARTESIAN_POINT ( 'NONE',  ( 5.000000000000000888, -162.9375000000000000, -2.071067811865475505 ) ) ;
#58842 = CARTESIAN_POINT ( 'NONE',  ( -6.972266317189433020E-16, -30.12499999726880873, -5.000000000000000000 ) ) ;
#58843 = CARTESIAN_POINT ( 'NONE',  ( -53.51423613279429503, -126.5000000013656063, 4.591703134518082763 ) ) ;
#58844 = CARTESIAN_POINT ( 'NONE',  ( 2.229367062500001939, -10.22916666530106866, 3.861377020970579999 ) ) ;
#58845 = CARTESIAN_POINT ( 'NONE',  ( -4.458734124999999437, -44.64583333196773651, -2.574251347313719407 ) ) ;
#58846 = CYLINDRICAL_SURFACE ( 'NONE', #48340, 5.000000000000000000 ) ;
#58847 = CARTESIAN_POINT ( 'NONE',  ( -3.152801135295367985, -146.8125000013655779, 3.152801135295367096 ) ) ;
#58848 = CARTESIAN_POINT ( 'NONE',  ( 2.229367062500001939, -88.22916666530107932, 3.861377020970579999 ) ) ;
#58849 = CARTESIAN_POINT ( 'NONE',  ( 1.975475456537005874E-15, 8.249999999999998224, 5.000000000000000000 ) ) ;
#58850 = ORIENTED_EDGE ( 'NONE', *, *, #5485, .T. ) ;
#58851 = DIRECTION ( 'NONE',  ( 0.000000000000000000, -1.000000000000000000, 0.000000000000000000 ) ) ;
#58852 = CARTESIAN_POINT ( 'NONE',  ( 1.975475456537005874E-15, -68.62499999726881583, 5.000000000000000000 ) ) ;
#58853 = CARTESIAN_POINT ( 'NONE',  ( -49.85088928181150436, -149.6875000027311842, -1.666127454062680702 ) ) ;
#58854 =( BOUNDED_CURVE ( )  B_SPLINE_CURVE ( 2, ( #50533, #44733, #693, #35416, #26084, #39906, #30906, #15486, #54723 ),
 .UNSPECIFIED., .F., .F. ) 
 B_SPLINE_CURVE_WITH_KNOTS ( ( 3, 2, 2, 2, 3 ),
 ( 0.2517857142857142794, 0.2523809523809523725, 0.2535714285714285587, 0.2547619047619047450, 0.2553571428571428381 ),
 .UNSPECIFIED. ) 
 CURVE ( )  GEOMETRIC_REPRESENTATION_ITEM ( )  RATIONAL_B_SPLINE_CURVE ( ( 0.9330127018922194093, 0.9330127018922194093, 1.000000000000000000, 0.8660254037844387076, 1.000000000000000000, 0.8660254037844387076, 1.000000000000000000, 0.9330127018922194093, 0.9330127018922194093 ) ) 
 REPRESENTATION_ITEM ( '' )  );
#58855 = CARTESIAN_POINT ( 'NONE',  ( 5.000000000000000000, -38.49999999999999289, -6.123233995736766282E-16 ) ) ;
#58856 = ORIENTED_EDGE ( 'NONE', *, *, #61532, .T. ) ;
#58857 = CARTESIAN_POINT ( 'NONE',  ( -4.458734124999999437, 0.6041666680322611560, -2.574251347313719407 ) ) ;
#58858 = CARTESIAN_POINT ( 'NONE',  ( -51.75738570946856498, -155.0000000000000284, 3.805975901505577408 ) ) ;
#58859 = CARTESIAN_POINT ( 'NONE',  ( 4.458734124999998549, -15.97916666530107221, -2.574251347313721627 ) ) ;
#58860 = CARTESIAN_POINT ( 'NONE',  ( -6.972266317189433020E-16, -51.25000000000000000, -5.000000000000000000 ) ) ;
#58861 = CARTESIAN_POINT ( 'NONE',  ( -3.152548672688508926E-16, -2.562499998634407028, -5.148502694627439702 ) ) ;
#58862 = CARTESIAN_POINT ( 'NONE',  ( 0.000000000000000000, -120.0000000000000000, 5.000000000000000000 ) ) ;
#58863 = CARTESIAN_POINT ( 'NONE',  ( 4.458734124999999437, -153.4375000013655779, 0.000000000000000000 ) ) ;
#58864 = CARTESIAN_POINT ( 'NONE',  ( 4.458734125000000326, 18.85416666803225993, 2.574251347313718519 ) ) ;
#58865 = ORIENTED_EDGE ( 'NONE', *, *, #27013, .F. ) ;
#58866 = CARTESIAN_POINT ( 'NONE',  ( -2.229367062499996610, -96.14583333196773651, 3.861377020970582219 ) ) ;
#58867 = CARTESIAN_POINT ( 'NONE',  ( -5.000000000000000000, -75.00000000000000000, 0.000000000000000000 ) ) ;
#58868 = CYLINDRICAL_SURFACE ( 'NONE', #21627, 5.000000000000000000 ) ;
#58869 = CARTESIAN_POINT ( 'NONE',  ( -4.458734124999999437, -13.39583333196774184, -2.574251347313719407 ) ) ;
#58870 = EDGE_CURVE ( 'NONE', #57924, #50850, #38694, .T. ) ;
#58871 = CARTESIAN_POINT ( 'NONE',  ( 1.975475456537005874E-15, -76.62499999726880162, 5.000000000000000000 ) ) ;
#58872 = CARTESIAN_POINT ( 'NONE',  ( 6.972266317189433020E-16, 29.74999999999999645, -5.000000000000000000 ) ) ;
#58873 = CARTESIAN_POINT ( 'NONE',  ( -57.19623071787017210, -153.3750000013656347, 4.297418129356382899 ) ) ;
#58874 = CARTESIAN_POINT ( 'NONE',  ( 5.000000000000000888, -41.45833333060213732, 2.886751345948126879 ) ) ;
#58875 = CARTESIAN_POINT ( 'NONE',  ( 4.458734124999999437, 16.18750000136559564, -5.460374474430324690E-16 ) ) ;
#58876 = CARTESIAN_POINT ( 'NONE',  ( 6.250000000000000000, -5.051814855409237026, -7.198902722707430257 ) ) ;
#58877 = ORIENTED_EDGE ( 'NONE', *, *, #11751, .T. ) ;
#58878 = CARTESIAN_POINT ( 'NONE',  ( 4.458734125000000326, 16.10416666803225993, 2.574251347313718519 ) ) ;
#58879 = CARTESIAN_POINT ( 'NONE',  ( 4.458734124999998549, -60.72916666530106511, -2.574251347313721627 ) ) ;
#58880 = EDGE_LOOP ( 'NONE', ( #7702, #61575, #19057, #44282 ) ) ;
#58881 = CARTESIAN_POINT ( 'NONE',  ( -4.458734124999997661, -8.479166665301073991, 2.574251347313722516 ) ) ;
#58882 = CARTESIAN_POINT ( 'NONE',  ( 1.975475456537005874E-15, -30.74999999999999645, 5.000000000000000000 ) ) ;
#58883 = CARTESIAN_POINT ( 'NONE',  ( 5.000000000000000000, 5.500000000000001776, -6.123233995736766282E-16 ) ) ;
#58884 = CARTESIAN_POINT ( 'NONE',  ( -3.152801135295367985, -168.8125000013656063, 3.152801135295367096 ) ) ;
#58885 = CYLINDRICAL_SURFACE ( 'NONE', #10965, 5.000000000000000000 ) ;
#58886 = CARTESIAN_POINT ( 'NONE',  ( -4.458734124999998549, -52.22916666530106511, 2.574251347313722516 ) ) ;
#58887 = CARTESIAN_POINT ( 'NONE',  ( -4.999999999999999112, -87.79166666393550145, 2.886751345948131764 ) ) ;
#58888 = CARTESIAN_POINT ( 'NONE',  ( -4.458734124999999437, -34.39583333196772941, -2.574251347313719407 ) ) ;
#58889 = CARTESIAN_POINT ( 'NONE',  ( 1.339745962155615144, -14.58034179853029322, 4.999999999999999112 ) ) ;
#58890 = EDGE_CURVE ( 'NONE', #25930, #27870, #41755, .T. ) ;
#58891 = CARTESIAN_POINT ( 'NONE',  ( 2.071067811865392461, -142.3125000027312410, 5.000000000000084377 ) ) ;
#58892 = CARTESIAN_POINT ( 'NONE',  ( 1.339745962155615144, -69.70534180126148271, 4.999999999999999112 ) ) ;
#58893 = EDGE_CURVE ( 'NONE', #28617, #41864, #32752, .T. ) ;
#58894 = CARTESIAN_POINT ( 'NONE',  ( -3.152801135295367985, -155.0625000013656063, 3.152801135295367096 ) ) ;
#58895 = CARTESIAN_POINT ( 'NONE',  ( 5.000000000000000000, -40.41666666666667140, -2.886751345948129988 ) ) ;
#58896 = CARTESIAN_POINT ( 'NONE',  ( -1.339745962155610925, -19.66965819600733667, 5.000000000000000000 ) ) ;
#58897 = CARTESIAN_POINT ( 'NONE',  ( 1.975475456537005874E-15, -22.74999999999999645, 5.000000000000000000 ) ) ;
#58898 = ORIENTED_EDGE ( 'NONE', *, *, #37056, .T. ) ;
#58899 = CARTESIAN_POINT ( 'NONE',  ( -4.458734124999999437, -103.3124999986344079, 0.000000000000000000 ) ) ;
#58900 = CARTESIAN_POINT ( 'NONE',  ( -4.458734124999999437, 5.354166668032262599, -2.574251347313719407 ) ) ;
#58901 = DIRECTION ( 'NONE',  ( 0.000000000000000000, 0.000000000000000000, 1.000000000000000000 ) ) ;
#58902 = CARTESIAN_POINT ( 'NONE',  ( 5.000000000000000888, -2.583333333333333481, 2.886751345948126879 ) ) ;
#58903 = EDGE_CURVE ( 'NONE', #15666, #7607, #9428, .T. ) ;
#58904 = CARTESIAN_POINT ( 'NONE',  ( 9.457646018065525792E-16, -69.06249999863439371, 5.148502694627439702 ) ) ;
#58905 = AXIS2_PLACEMENT_3D ( 'NONE', #23756, #42721, #42405 ) ;
#58906 = CARTESIAN_POINT ( 'NONE',  ( -4.250000000000000000, 5.204748896376250699E-16, -9.449444346342714240 ) ) ;
#58907 = CARTESIAN_POINT ( 'NONE',  ( -5.000000000000000000, 0.04166666939785235169, -2.886751345948128211 ) ) ;
#58909 = ORIENTED_EDGE ( 'NONE', *, *, #8583, .T. ) ;
#58908 = CARTESIAN_POINT ( 'NONE',  ( 9.457646018065525792E-16, -32.06249999863440792, 5.148502694627439702 ) ) ;
#58910 = CARTESIAN_POINT ( 'NONE',  ( -10.39117206796836079, 0.000000000000000000, -8.499999999999998224 ) ) ;
#58911 = DIRECTION ( 'NONE',  ( -0.000000000000000000, 1.000000000000000000, -0.000000000000000000 ) ) ;
#58912 = CARTESIAN_POINT ( 'NONE',  ( 5.000000000000000000, -20.49999999999999645, -6.123233995736766282E-16 ) ) ;
#58913 = CARTESIAN_POINT ( 'NONE',  ( -4.999999999999999112, -45.91666666666665719, 2.886751345948131764 ) ) ;
#58915 = CARTESIAN_POINT ( 'NONE',  ( 2.229367062499998831, -24.89583333196773651, -3.861377020970580887 ) ) ;
#58914 = DIRECTION ( 'NONE',  ( 0.000000000000000000, 0.000000000000000000, 1.000000000000000000 ) ) ;
#58916 = CARTESIAN_POINT ( 'NONE',  ( -9.184850993605147944E-16, -155.2500000000000000, 5.000000000000000000 ) ) ;
#58917 = CARTESIAN_POINT ( 'NONE',  ( -2.229367062500000163, -71.47916666530107932, -3.861377020970580443 ) ) ;
#58918 = CARTESIAN_POINT ( 'NONE',  ( -4.458734124999999437, -143.1875000013656063, -5.460374474430324690E-16 ) ) ;
#58919 = CARTESIAN_POINT ( 'NONE',  ( -2.229367062499996610, -83.14583333196773651, 3.861377020970582219 ) ) ;
#58920 = CARTESIAN_POINT ( 'NONE',  ( -57.19623071787017210, -137.6250000013655779, 4.297418129356382899 ) ) ;
#58921 = CARTESIAN_POINT ( 'NONE',  ( 2.229367062499998831, -32.89583333196773651, -3.861377020970580887 ) ) ;
#58922 = CARTESIAN_POINT ( 'NONE',  ( -2.500000000000000444, -73.04166666393548724, -4.330127018922193649 ) ) ;
#58923 = VERTEX_POINT ( 'NONE', #43517 ) ;
#58924 = EDGE_CURVE ( 'NONE', #46451, #34949, #13399, .T. ) ;
#58925 = LINE ( 'NONE', #14853, #37172 ) ;
#58926 = EDGE_LOOP ( 'NONE', ( #35290, #19208, #30337, #38134 ) ) ;
#58927 = CARTESIAN_POINT ( 'NONE',  ( 4.458734124999999437, -71.06249999863439371, -5.460374474430324690E-16 ) ) ;
#58928 = CARTESIAN_POINT ( 'NONE',  ( 3.253724281355068545E-15, 28.75000000000000000, -5.000000000000000000 ) ) ;
#58929 =( NAMED_UNIT ( * ) SI_UNIT ( $, .STERADIAN. ) SOLID_ANGLE_UNIT ( ) );
#58930 = ORIENTED_EDGE ( 'NONE', *, *, #9512, .T. ) ;
#58931 = CARTESIAN_POINT ( 'NONE',  ( -2.499999999999996447, 17.16666666666666430, 4.330127018922195425 ) ) ;
#58932 = CARTESIAN_POINT ( 'NONE',  ( 1.339745962155615144, -31.58034179853029499, 4.999999999999999112 ) ) ;
#58933 = CARTESIAN_POINT ( 'NONE',  ( -4.458734124999998549, -59.47916666530106511, 2.574251347313722516 ) ) ;
#58934 = CARTESIAN_POINT ( 'NONE',  ( -4.458734124999999437, 1.354166668032261933, -2.574251347313719407 ) ) ;
#58935 = VERTEX_POINT ( 'NONE', #33256 ) ;
#58936 =( BOUNDED_CURVE ( )  B_SPLINE_CURVE ( 2, ( #61884, #46123, #26185, #11697, #46756, #2087, #31317, #26828, #60930 ),
 .UNSPECIFIED., .F., .F. ) 
 B_SPLINE_CURVE_WITH_KNOTS ( ( 3, 2, 2, 2, 3 ),
 ( 0.5020833333333333259, 0.5027777777777777679, 0.5041666666666666519, 0.5055555555555555358, 0.5062499999999999778 ),
 .UNSPECIFIED. ) 
 CURVE ( )  GEOMETRIC_REPRESENTATION_ITEM ( )  RATIONAL_B_SPLINE_CURVE ( ( 0.9330127018922194093, 0.9330127018922194093, 1.000000000000000000, 0.8660254037844387076, 1.000000000000000000, 0.8660254037844387076, 1.000000000000000000, 0.9330127018922194093, 0.9330127018922194093 ) ) 
 REPRESENTATION_ITEM ( '' )  );
#58937 = FACE_OUTER_BOUND ( 'NONE', #28574, .T. ) ;
#58938 = CARTESIAN_POINT ( 'NONE',  ( -4.999999999999998224, -22.79166666393548013, 2.886751345948131764 ) ) ;
#58939 = CARTESIAN_POINT ( 'NONE',  ( 4.458734124999999437, 15.18750000136559564, -5.460374474430324690E-16 ) ) ;
#58940 = CARTESIAN_POINT ( 'NONE',  ( -59.29741812935640155, -142.6250000013655779, -2.196230717870135685 ) ) ;
#58941 = CARTESIAN_POINT ( 'NONE',  ( -1.846868145590737420, -163.7500000013655779, 4.458734124999997661 ) ) ;
#58942 = EDGE_LOOP ( 'NONE', ( #24104, #49675, #34960, #13200 ) ) ;
#58943 = CARTESIAN_POINT ( 'NONE',  ( 9.457646018065525792E-16, -82.06249999863440792, 5.148502694627439702 ) ) ;
#58944 = DIRECTION ( 'NONE',  ( -0.000000000000000000, 1.000000000000000000, -0.000000000000000000 ) ) ;
#58945 = CARTESIAN_POINT ( 'NONE',  ( 4.458734124999999437, 0.1875000013655953035, -5.460374474430324690E-16 ) ) ;
#58946 = EDGE_CURVE ( 'NONE', #14245, #50889, #15084, .T. ) ;
#58947 = AXIS2_PLACEMENT_3D ( 'NONE', #22096, #1858, #35617 ) ;
#58948 =( BOUNDED_CURVE ( )  B_SPLINE_CURVE ( 2, ( #40116, #40751, #15683, #34659, #35302, #24695, #10849, #16326, #30464 ),
 .UNSPECIFIED., .F., .F. ) 
 B_SPLINE_CURVE_WITH_KNOTS ( ( 3, 2, 2, 2, 3 ),
 ( 0.07500000000000005274, 0.07916666666666671848, 0.08333333333333339810, 0.08750000000000007772, 0.09166666666666674346 ),
 .UNSPECIFIED. ) 
 CURVE ( )  GEOMETRIC_REPRESENTATION_ITEM ( )  RATIONAL_B_SPLINE_CURVE ( ( 0.9999999999999990008, 0.9238795325112877377, 1.000000000000000000, 0.9238795325112867385, 1.000000000000000000, 0.9238795325112867385, 1.000000000000000000, 0.9238795325112851842, 1.000000000000001554 ) ) 
 REPRESENTATION_ITEM ( '' )  );
#58949 = CARTESIAN_POINT ( 'NONE',  ( -5.000000000000000000, -83.08333333333332860, -2.886751345948128211 ) ) ;
#58950 = CARTESIAN_POINT ( 'NONE',  ( 6.123233995736766282E-16, -120.0000000000000000, -5.000000000000000000 ) ) ;
#58951 = EDGE_CURVE ( 'NONE', #53159, #8589, #50410, .T. ) ;
#58952 = CARTESIAN_POINT ( 'NONE',  ( -4.458734124999999437, -63.56249999863440792, 0.000000000000000000 ) ) ;
#58953 = CARTESIAN_POINT ( 'NONE',  ( 5.000000000000000000, -24.29166666393548368, -2.886751345948129988 ) ) ;
#58954 = CARTESIAN_POINT ( 'NONE',  ( 2.500000000000002220, -20.66666666666666785, 4.330127018922192761 ) ) ;
#58955 = CARTESIAN_POINT ( 'NONE',  ( 4.458734124999998549, 29.27083333469893134, -2.574251347313721627 ) ) ;
#58956 = CYLINDRICAL_SURFACE ( 'NONE', #49022, 5.000000000000000000 ) ;
#58957 = SURFACE_STYLE_FILL_AREA ( #25179 ) ;
#58958 = CARTESIAN_POINT ( 'NONE',  ( -4.458734124999999437, -48.39583333196772941, -2.574251347313719407 ) ) ;
#58959 = PRODUCT_DEFINITION_SHAPE ( 'NONE', 'NONE',  #63677 ) ;
#58960 = CARTESIAN_POINT ( 'NONE',  ( 9.457646018065525792E-16, -31.31249999863440436, 5.148502694627439702 ) ) ;
#58961 = CARTESIAN_POINT ( 'NONE',  ( -2.229367062500000163, 6.270833334698928674, -3.861377020970580443 ) ) ;
#58962 = CARTESIAN_POINT ( 'NONE',  ( 3.535533905932738197, -146.0000000027311842, -3.535533905932738197 ) ) ;
#58963 = CARTESIAN_POINT ( 'NONE',  ( -2.500000000000000444, 24.83333333333333215, -4.330127018922193649 ) ) ;
#58964 = CARTESIAN_POINT ( 'NONE',  ( 2.071067811865475505, -150.9375000027311842, -5.000000000000000888 ) ) ;
#58965 = LINE ( 'NONE', #15549, #57228 ) ;
#58966 = CARTESIAN_POINT ( 'NONE',  ( -3.152548672688508926E-16, -36.56249999863441502, -5.148502694627439702 ) ) ;
#58967 = CARTESIAN_POINT ( 'NONE',  ( -5.000000000000000000, -74.95833333060214443, -2.886751345948128211 ) ) ;
#58968 = CARTESIAN_POINT ( 'NONE',  ( -58.39396692619412477, -144.6875000013656063, 2.891590998281057701 ) ) ;
#58969 = CARTESIAN_POINT ( 'NONE',  ( -5.000000000000000888, -143.5625000000000568, -2.071067811865475949 ) ) ;
#58970 = LINE ( 'NONE', #11032, #61410 ) ;
#58971 = EDGE_CURVE ( 'NONE', #21496, #36016, #44208, .T. ) ;
#58972 = CARTESIAN_POINT ( 'NONE',  ( 4.458734125000000326, -75.14583333196775072, 2.574251347313718519 ) ) ;
#58973 = CARTESIAN_POINT ( 'NONE',  ( 2.730187237215162345E-16, -164.4375000013655779, -4.458734124999999437 ) ) ;
#58974 = CARTESIAN_POINT ( 'NONE',  ( -4.458734124999999437, -34.31249999863440792, 0.000000000000000000 ) ) ;
#58975 = CARTESIAN_POINT ( 'NONE',  ( -2.071067811865372921, -160.3125000000000000, 5.000000000000104805 ) ) ;
#58976 = CARTESIAN_POINT ( 'NONE',  ( -6.972266317189433020E-16, -65.24999999999998579, -5.000000000000000000 ) ) ;
#58977 = CARTESIAN_POINT ( 'NONE',  ( 5.000000000000000000, -22.50000000000000000, -6.123233995736766282E-16 ) ) ;
#58978 = CARTESIAN_POINT ( 'NONE',  ( 4.458734124999999437, -145.5000000013655779, 1.846868145590737864 ) ) ;
#58979 = ORIENTED_EDGE ( 'NONE', *, *, #55522, .T. ) ;
#58980 = CARTESIAN_POINT ( 'NONE',  ( 1.060575238724906964E-15, -89.62499999726881583, 5.773502691896257311 ) ) ;
#58981 = VERTEX_POINT ( 'NONE', #24923 ) ;
#58982 = CARTESIAN_POINT ( 'NONE',  ( -4.458734124999997661, -62.47916666530106511, 2.574251347313722516 ) ) ;
#58983 = CARTESIAN_POINT ( 'NONE',  ( -4.999999999999999112, 22.20833333606451987, 2.886751345948131764 ) ) ;
#58984 = CARTESIAN_POINT ( 'NONE',  ( -2.071067811865548780, -162.6874999999999716, -4.999999999999926281 ) ) ;
#58985 = CARTESIAN_POINT ( 'NONE',  ( 5.000000000000000888, 15.41666666666666607, 2.886751345948126879 ) ) ;
#58986 = CARTESIAN_POINT ( 'NONE',  ( 9.457646018065525792E-16, -51.06249999863440792, 5.148502694627439702 ) ) ;
#58987 = CARTESIAN_POINT ( 'NONE',  ( 4.458734124999998549, -3.729166665301070438, -2.574251347313721627 ) ) ;
#58988 = DIRECTION ( 'NONE',  ( 0.000000000000000000, 0.000000000000000000, -1.000000000000000000 ) ) ;
#58989 = CARTESIAN_POINT ( 'NONE',  ( 2.493747252781420335E-13, -77.25000000000001421, -5.000000000000000000 ) ) ;
#58990 = LINE ( 'NONE', #29377, #32286 ) ;
#58991 = DIRECTION ( 'NONE',  ( -0.6485228581062915110, 0.000000000000000000, -0.7611951803011149931 ) ) ;
#58993 = CARTESIAN_POINT ( 'NONE',  ( 4.458734125000001214, -18.89583333196773651, 2.574251347313718519 ) ) ;
#58992 = CARTESIAN_POINT ( 'NONE',  ( 5.000000000000000888, 0.4166666666666659080, 2.886751345948126879 ) ) ;
#58994 = LINE ( 'NONE', #14923, #28595 ) ;
#58995 = CARTESIAN_POINT ( 'NONE',  ( -4.458734124999998549, -54.22916666530107221, 2.574251347313722516 ) ) ;
#58996 = CARTESIAN_POINT ( 'NONE',  ( 4.458734125000000326, -155.6250000013656063, -1.846868145590734978 ) ) ;
#58997 = VECTOR ( 'NONE', #57903, 1000.000000000000000 ) ;
#58998 = CARTESIAN_POINT ( 'NONE',  ( -5.000000000000000000, -52.95833333060214443, -2.886751345948128211 ) ) ;
#58999 = ORIENTED_EDGE ( 'NONE', *, *, #17029, .F. ) ;
#59000 = CARTESIAN_POINT ( 'NONE',  ( 5.000000000000000000, -26.41666666666666430, -2.886751345948130876 ) ) ;
#59001 = CARTESIAN_POINT ( 'NONE',  ( -2.229367062500000163, 7.270833334698929562, -3.861377020970580443 ) ) ;
#59002 = ORIENTED_EDGE ( 'NONE', *, *, #6002, .T. ) ;
#59004 = CARTESIAN_POINT ( 'NONE',  ( -2.500000000000000444, -68.04166666393547303, -4.330127018922193649 ) ) ;
#59003 = CARTESIAN_POINT ( 'NONE',  ( 1.339745962155615144, -56.70534180126148271, 4.999999999999999112 ) ) ;
#59005 = CARTESIAN_POINT ( 'NONE',  ( 2.730187237215162345E-16, -155.1875000013655779, -4.458734124999999437 ) ) ;
#59006 = ORIENTED_EDGE ( 'NONE', *, *, #60235, .F. ) ;
#59007 =( BOUNDED_CURVE ( )  B_SPLINE_CURVE ( 2, ( #26458, #46076, #39962, #59610, #11019, #15541, #35161, #54776, #10708 ),
 .UNSPECIFIED., .F., .F. ) 
 B_SPLINE_CURVE_WITH_KNOTS ( ( 3, 2, 2, 2, 3 ),
 ( 0.9946428571428571619, 0.9952380952380952550, 0.9964285714285714413, 0.9976190476190476275, 0.9982142857142857206 ),
 .UNSPECIFIED. ) 
 CURVE ( )  GEOMETRIC_REPRESENTATION_ITEM ( )  RATIONAL_B_SPLINE_CURVE ( ( 0.9330127018922194093, 0.9330127018922194093, 1.000000000000000000, 0.8660254037844387076, 1.000000000000000000, 0.8660254037844387076, 1.000000000000000000, 0.9330127018922194093, 0.9330127018922194093 ) ) 
 REPRESENTATION_ITEM ( '' )  );
#59008 = CARTESIAN_POINT ( 'NONE',  ( -50.01589407740564042, -132.6250000000000284, 0.3983568153799778022 ) ) ;
#59009 = CARTESIAN_POINT ( 'NONE',  ( -4.999999999999998224, -58.79166666393546592, 2.886751345948131764 ) ) ;
#59010 = CARTESIAN_POINT ( 'NONE',  ( 4.458734125000001214, -41.14583333196774362, 2.574251347313718519 ) ) ;
#59011 = ORIENTED_EDGE ( 'NONE', *, *, #12202, .T. ) ;
#59012 = CARTESIAN_POINT ( 'NONE',  ( 3.061616997868383141E-16, -145.7500000000000284, -5.000000000000000000 ) ) ;
#59013 = CARTESIAN_POINT ( 'NONE',  ( -3.152548672688508926E-16, 17.43750000136559564, -5.148502694627439702 ) ) ;
#59014 = FACE_OUTER_BOUND ( 'NONE', #5858, .T. ) ;
#59015 = ORIENTED_EDGE ( 'NONE', *, *, #61739, .F. ) ;
#59016 = CARTESIAN_POINT ( 'NONE',  ( 2.229367062499998831, 29.35416666803225993, -3.861377020970580887 ) ) ;
#59017 = CARTESIAN_POINT ( 'NONE',  ( -52.10840900171896806, -154.1875000013656063, 3.393966926194110556 ) ) ;
#59018 = DIRECTION ( 'NONE',  ( 0.000000000000000000, -1.000000000000000000, 0.000000000000000000 ) ) ;
#59019 = CARTESIAN_POINT ( 'NONE',  ( -50.66154591918759564, -135.0000000000001137, 1.672849277080756147 ) ) ;
#59020 = DIRECTION ( 'NONE',  ( -0.000000000000000000, 1.000000000000000000, -0.000000000000000000 ) ) ;
#59021 = CARTESIAN_POINT ( 'NONE',  ( 4.458734125000000326, -60.89583333196774362, 2.574251347313718519 ) ) ;
#59022 = CARTESIAN_POINT ( 'NONE',  ( 3.295171437449806451, 7.213553046161976567, -7.590212325761626744 ) ) ;
#59023 = CARTESIAN_POINT ( 'NONE',  ( -4.458734124999999437, 18.60416666803225993, -2.574251347313719407 ) ) ;
#59024 = DIRECTION ( 'NONE',  ( 0.000000000000000000, 0.000000000000000000, 1.000000000000000000 ) ) ;
#59025 = EDGE_CURVE ( 'NONE', #49354, #1660, #58386, .T. ) ;
#59026 = EDGE_CURVE ( 'NONE', #62409, #58377, #36887, .T. ) ;
#59027 = CARTESIAN_POINT ( 'NONE',  ( -4.458734124999998549, -51.47916666530106511, 2.574251347313722516 ) ) ;
#59028 = CARTESIAN_POINT ( 'NONE',  ( 5.000000000000000000, -8.374999997268814056, -6.123233995736766282E-16 ) ) ;
#59029 = CARTESIAN_POINT ( 'NONE',  ( 0.000000000000000000, -170.0000000000000000, 0.000000000000000000 ) ) ;
#59030 = FACE_OUTER_BOUND ( 'NONE', #27901, .T. ) ;
#59031 = CYLINDRICAL_SURFACE ( 'NONE', #42787, 5.000000000000000000 ) ;
#59032 = ADVANCED_FACE ( 'NONE', ( #4350 ), #5627, .T. ) ;
#59033 = CARTESIAN_POINT ( 'NONE',  ( 2.229367062500001939, -108.9791666653010651, 3.861377020970579999 ) ) ;
#59034 =( BOUNDED_CURVE ( )  B_SPLINE_CURVE ( 2, ( #15077, #59468, #53677, #63343, #10254, #39825, #29855, #19257, #54955 ),
 .UNSPECIFIED., .F., .F. ) 
 B_SPLINE_CURVE_WITH_KNOTS ( ( 3, 2, 2, 2, 3 ),
 ( 0.02500000000000002220, 0.02916666666666669488, 0.03333333333333336757, 0.03750000000000003331, 0.04166666666666670599 ),
 .UNSPECIFIED. ) 
 CURVE ( )  GEOMETRIC_REPRESENTATION_ITEM ( )  RATIONAL_B_SPLINE_CURVE ( ( 0.9999999999999996669, 0.9238795325112870716, 1.000000000000000000, 0.9238795325112867385, 1.000000000000000000, 0.9238795325112867385, 1.000000000000000000, 0.9238795325112859613, 1.000000000000000666 ) ) 
 REPRESENTATION_ITEM ( '' )  );
#59035 = CARTESIAN_POINT ( 'NONE',  ( 9.457646018065525792E-16, -14.31249999863440614, 5.148502694627439702 ) ) ;
#59036 = ORIENTED_EDGE ( 'NONE', *, *, #3135, .F. ) ;
#59037 = CARTESIAN_POINT ( 'NONE',  ( -5.000000000000000888, -163.6875000027311842, -2.071067811865475949 ) ) ;
#59038 = CARTESIAN_POINT ( 'NONE',  ( -3.152548672688508926E-16, -97.56249999863440792, -5.148502694627439702 ) ) ;
#59039 = CARTESIAN_POINT ( 'NONE',  ( -5.000000000000000000, -161.6250000027311842, -6.123233995736766282E-16 ) ) ;
#59040 = CARTESIAN_POINT ( 'NONE',  ( -2.229367062500000163, -99.72916666530106511, -3.861377020970580443 ) ) ;
#59041 = CARTESIAN_POINT ( 'NONE',  ( -6.972266317189433020E-16, -19.12499999726880873, -5.000000000000000000 ) ) ;
#59043 = EDGE_CURVE ( 'NONE', #60943, #19776, #25238, .T. ) ;
#59042 = CARTESIAN_POINT ( 'NONE',  ( -4.999999999999999112, -54.79166666393547303, 2.886751345948131764 ) ) ;
#59044 = LINE ( 'NONE', #52645, #63373 ) ;
#59045 = EDGE_CURVE ( 'NONE', #62028, #6651, #20420, .T. ) ;
#59046 = AXIS2_PLACEMENT_3D ( 'NONE', #12493, #12178, #27597 ) ;
#59047 = CARTESIAN_POINT ( 'NONE',  ( -57.19623071787017210, -154.6250000013656063, 4.297418129356382899 ) ) ;
#59048 = CARTESIAN_POINT ( 'NONE',  ( -50.55543936806279248, -147.0625000013656063, 0.3552334253322060320 ) ) ;
#59049 = CARTESIAN_POINT ( 'NONE',  ( 4.458734125000000326, -18.89583333196774362, 2.574251347313718519 ) ) ;
#59050 = CARTESIAN_POINT ( 'NONE',  ( -4.458734124999999437, 7.354166668032259935, -2.574251347313719407 ) ) ;
#59051 = CARTESIAN_POINT ( 'NONE',  ( 4.458734124999998549, -57.97916666530107932, -2.574251347313721627 ) ) ;
#59052 = LINE ( 'NONE', #11111, #44910 ) ;
#59053 = CARTESIAN_POINT ( 'NONE',  ( 4.458734124999999437, -16.81249999863440436, -5.460374474430324690E-16 ) ) ;
#59054 = CARTESIAN_POINT ( 'NONE',  ( 1.339745962155615144, -71.70534180126148271, 4.999999999999999112 ) ) ;
#59055 = CARTESIAN_POINT ( 'NONE',  ( 3.535533905932736864, -153.1250000000000000, 3.535533905932738641 ) ) ;
#59056 = CARTESIAN_POINT ( 'NONE',  ( 1.060575238724906964E-15, -5.749999999999998224, 5.773502691896257311 ) ) ;
#59057 = EDGE_CURVE ( 'NONE', #8105, #62409, #48406, .T. ) ;
#59058 = EDGE_LOOP ( 'NONE', ( #56129, #50463, #9966, #51935 ) ) ;
#59059 = CARTESIAN_POINT ( 'NONE',  ( -3.152548672688508926E-16, -48.81249999863440792, -5.148502694627439702 ) ) ;
#59060 = CARTESIAN_POINT ( 'NONE',  ( 1.339745962155619807, 21.83034180399265978, -4.999999999999996447 ) ) ;
#59061 = EDGE_CURVE ( 'NONE', #29588, #1043, #35196, .T. ) ;
#59062 = CARTESIAN_POINT ( 'NONE',  ( -0.9763930676156993282, 8.096533237421580154, -7.213065638943424673 ) ) ;
#59063 = EDGE_CURVE ( 'NONE', #60836, #15263, #54916, .T. ) ;
#59064 = DIRECTION ( 'NONE',  ( 0.000000000000000000, 1.000000000000000000, 0.000000000000000000 ) ) ;
#59065 = CARTESIAN_POINT ( 'NONE',  ( -2.229367062499996610, -85.14583333196773651, 3.861377020970582219 ) ) ;
#59066 = CARTESIAN_POINT ( 'NONE',  ( -3.152548672688508926E-16, 19.18750000136559208, -5.148502694627439702 ) ) ;
#59067 = CARTESIAN_POINT ( 'NONE',  ( 2.229367062500001939, 10.02083333469892779, 3.861377020970579999 ) ) ;
#59068 = CARTESIAN_POINT ( 'NONE',  ( -6.972266317189433020E-16, -93.24999999999998579, -5.000000000000000000 ) ) ;
#59069 = CARTESIAN_POINT ( 'NONE',  ( 2.500000000000002220, -37.54166666393548013, 4.330127018922192761 ) ) ;
#59070 = CARTESIAN_POINT ( 'NONE',  ( -2.229367062500000163, -86.72916666530107932, -3.861377020970580443 ) ) ;
#59071 = CARTESIAN_POINT ( 'NONE',  ( 2.229367062499998831, 20.10416666803225993, -3.861377020970580887 ) ) ;
#59072 = CARTESIAN_POINT ( 'NONE',  ( 5.000000000000000000, -73.50000000000000000, -6.123233995736766282E-16 ) ) ;
#59073 = CARTESIAN_POINT ( 'NONE',  ( 1.060575238724906964E-15, 7.375000002731186832, 5.773502691896257311 ) ) ;
#59074 = EDGE_LOOP ( 'NONE', ( #5395, #38138, #8647, #26117 ) ) ;
#59075 = LINE ( 'NONE', #34613, #41775 ) ;
#59076 = EDGE_LOOP ( 'NONE', ( #41367, #52697, #9624, #10515 ) ) ;
#59078 = CARTESIAN_POINT ( 'NONE',  ( -3.535250795749689387E-16, -35.25000000000000000, -5.773502691896257311 ) ) ;
#59077 = DIRECTION ( 'NONE',  ( 0.000000000000000000, 1.000000000000000000, 0.000000000000000000 ) ) ;
#59079 = CARTESIAN_POINT ( 'NONE',  ( 4.458734124999998549, -39.72916666530107932, -2.574251347313721627 ) ) ;
#59080 = CARTESIAN_POINT ( 'NONE',  ( -2.500000000000000444, -32.04166666393548724, -4.330127018922193649 ) ) ;
#59082 = ORIENTED_EDGE ( 'NONE', *, *, #62972, .T. ) ;
#59081 = CARTESIAN_POINT ( 'NONE',  ( -3.152548672688508926E-16, -66.56249999863440792, -5.148502694627439702 ) ) ;
#59083 = CARTESIAN_POINT ( 'NONE',  ( -57.19623071787017210, -149.6250000013655779, 4.297418129356382899 ) ) ;
#59084 = CARTESIAN_POINT ( 'NONE',  ( -2.229367062500000163, -10.47916666530106866, -3.861377020970580443 ) ) ;
#59086 = ORIENTED_EDGE ( 'NONE', *, *, #48459, .F. ) ;
#59085 = CARTESIAN_POINT ( 'NONE',  ( -4.458734124999998549, -16.47916666530107577, 2.574251347313722516 ) ) ;
#59087 = CARTESIAN_POINT ( 'NONE',  ( -5.000000000000000000, -83.99999999999998579, 0.000000000000000000 ) ) ;
#59088 = CARTESIAN_POINT ( 'NONE',  ( -4.458734125000001214, -167.8750000013656063, 1.846868145590734089 ) ) ;
#59089 = CARTESIAN_POINT ( 'NONE',  ( -3.152548672688508926E-16, -55.81249999863440081, -5.148502694627439702 ) ) ;
#59090 = CARTESIAN_POINT ( 'NONE',  ( 5.000000000000000000, -82.37499999726881583, -6.123233995736766282E-16 ) ) ;
#59092 = ORIENTED_EDGE ( 'NONE', *, *, #22922, .F. ) ;
#59091 = CYLINDRICAL_SURFACE ( 'NONE', #13863, 5.000000000000000000 ) ;
#59093 = CARTESIAN_POINT ( 'NONE',  ( -60.14911071818854538, -146.0624999999999716, 1.666127454062681368 ) ) ;
#59094 = CARTESIAN_POINT ( 'NONE',  ( -4.458734124999999437, -26.64583333196773651, -2.574251347313719407 ) ) ;
#59095 = FACE_OUTER_BOUND ( 'NONE', #274, .T. ) ;
#59096 = ORIENTED_EDGE ( 'NONE', *, *, #27600, .F. ) ;
#59097 = VECTOR ( 'NONE', #48878, 1000.000000000000000 ) ;
#59098 = CARTESIAN_POINT ( 'NONE',  ( -4.458734124999999437, -164.1875000013655779, -5.460374474430324690E-16 ) ) ;
#59099 = CARTESIAN_POINT ( 'NONE',  ( -3.152548672688508926E-16, -105.8124999986344079, -5.148502694627439702 ) ) ;
#59100 = CARTESIAN_POINT ( 'NONE',  ( -5.000000000000000000, -38.95833333060214443, -2.886751345948128211 ) ) ;
#59101 = ORIENTED_EDGE ( 'NONE', *, *, #47645, .F. ) ;
#59102 = CARTESIAN_POINT ( 'NONE',  ( -50.70258187064364108, -146.3750000013655779, 2.196230717870141014 ) ) ;
#59103 = CARTESIAN_POINT ( 'NONE',  ( -2.229367062500000163, -74.72916666530106511, -3.861377020970580443 ) ) ;
#59104 = CARTESIAN_POINT ( 'NONE',  ( -52.53715891517739323, -139.5625000027311842, -4.819101127000233298 ) ) ;
#59105 = CARTESIAN_POINT ( 'NONE',  ( 9.457646018065525792E-16, -45.06249999863440081, 5.148502694627439702 ) ) ;
#59106 = CARTESIAN_POINT ( 'NONE',  ( 4.458734124999999437, -147.6250000013655779, -1.846868145590734978 ) ) ;
#59107 = CARTESIAN_POINT ( 'NONE',  ( -75.00000000000001421, 0.000000000000000000, -9.000000000000001776 ) ) ;
#59108 = CYLINDRICAL_SURFACE ( 'NONE', #52208, 5.000000000000000000 ) ;
#59109 = CARTESIAN_POINT ( 'NONE',  ( 4.458734125000001214, -12.89583333196774184, 2.574251347313718519 ) ) ;
#59110 = CARTESIAN_POINT ( 'NONE',  ( -5.000000000000000000, -102.0833333333333286, -2.886751345948128211 ) ) ;
#59111 = VERTEX_POINT ( 'NONE', #26844 ) ;
#59112 = CARTESIAN_POINT ( 'NONE',  ( -1.846868145590734756, -141.3750000013656063, -4.458734125000000326 ) ) ;
#59113 = CARTESIAN_POINT ( 'NONE',  ( -4.458734124999999437, -34.64583333196773651, -2.574251347313719407 ) ) ;
#59114 = CARTESIAN_POINT ( 'NONE',  ( 5.000000000000000888, 7.541666669397851130, 2.886751345948126879 ) ) ;
#59115 = CARTESIAN_POINT ( 'NONE',  ( 1.339745962155615144, -50.70534180126148271, 4.999999999999999112 ) ) ;
#59116 = CARTESIAN_POINT ( 'NONE',  ( -50.40829686548195099, -134.0000000013656063, -1.485763867205728284 ) ) ;
#59117 = CARTESIAN_POINT ( 'NONE',  ( -2.229367062499996610, -75.39583333196773651, 3.861377020970582219 ) ) ;
#59118 = CARTESIAN_POINT ( 'NONE',  ( -3.535533905932738641, -166.3750000000000284, 3.535533905932737309 ) ) ;
#59119 = CARTESIAN_POINT ( 'NONE',  ( -5.000000000000000000, -69.99999999999998579, 0.000000000000000000 ) ) ;
#59120 = DIRECTION ( 'NONE',  ( 0.000000000000000000, 0.000000000000000000, 1.000000000000000000 ) ) ;
#59121 = CARTESIAN_POINT ( 'NONE',  ( -3.152548672688508926E-16, 5.187500001365592972, -5.148502694627439702 ) ) ;
#59122 = VERTEX_POINT ( 'NONE', #1142 ) ;
#59123 = CARTESIAN_POINT ( 'NONE',  ( 1.339745962155627135, 16.83034180399266688, -4.999999999999991118 ) ) ;
#59124 = CARTESIAN_POINT ( 'NONE',  ( 1.255007937094098239E-14, 23.87500000273118417, -4.999999999999999112 ) ) ;
#59126 = CARTESIAN_POINT ( 'NONE',  ( -4.458734124999998549, -30.22916666530106866, 2.574251347313722516 ) ) ;
#59125 = CARTESIAN_POINT ( 'NONE',  ( 1.060575238724906964E-15, -96.75000000000001421, 5.773502691896257311 ) ) ;
#59127 = DIRECTION ( 'NONE',  ( 0.000000000000000000, 0.000000000000000000, 1.000000000000000000 ) ) ;
#59128 = CARTESIAN_POINT ( 'NONE',  ( -4.458734124999999437, -79.64583333196772230, -2.574251347313719407 ) ) ;
#59129 = CARTESIAN_POINT ( 'NONE',  ( 4.458734124999999437, 18.93750000136559564, -5.460374474430324690E-16 ) ) ;
#59130 = CARTESIAN_POINT ( 'NONE',  ( 0.000000000000000000, -120.0000000000000000, 5.000000000000000000 ) ) ;
#59131 = CARTESIAN_POINT ( 'NONE',  ( -57.19623071787017210, -139.3750000013656063, 4.297418129356382899 ) ) ;
#59132 = CARTESIAN_POINT ( 'NONE',  ( -4.458734124999999437, -2.395833331967737845, -2.574251347313719407 ) ) ;
#59133 = CARTESIAN_POINT ( 'NONE',  ( 4.458734124999999437, 20.93750000136559208, -5.460374474430324690E-16 ) ) ;
#59134 = CARTESIAN_POINT ( 'NONE',  ( -2.229367062499996610, -40.39583333196773651, 3.861377020970582219 ) ) ;
#59135 = CARTESIAN_POINT ( 'NONE',  ( -2.500000000000000444, -51.04166666393547303, -4.330127018922193649 ) ) ;
#59136 = CARTESIAN_POINT ( 'NONE',  ( 2.229367062500001939, 2.020833334698927786, 3.861377020970579999 ) ) ;
#59137 = ORIENTED_EDGE ( 'NONE', *, *, #34729, .F. ) ;
#59138 = CARTESIAN_POINT ( 'NONE',  ( 9.457646018065525792E-16, -26.31249999863440792, 5.148502694627439702 ) ) ;
#59139 = CARTESIAN_POINT ( 'NONE',  ( 2.229367062499998831, -67.64583333196773651, -3.861377020970580887 ) ) ;
#59140 = CARTESIAN_POINT ( 'NONE',  ( 2.500000000000002220, -106.5416666639354730, 4.330127018922192761 ) ) ;
#59141 =( BOUNDED_CURVE ( )  B_SPLINE_CURVE ( 2, ( #41311, #41947, #7246, #22981, #12687, #7555, #61272, #2416, #13319 ),
 .UNSPECIFIED., .F., .F. ) 
 B_SPLINE_CURVE_WITH_KNOTS ( ( 3, 2, 2, 2, 3 ),
 ( 0.9267857142857143238, 0.9273809523809524169, 0.9285714285714286031, 0.9297619047619047894, 0.9303571428571428825 ),
 .UNSPECIFIED. ) 
 CURVE ( )  GEOMETRIC_REPRESENTATION_ITEM ( )  RATIONAL_B_SPLINE_CURVE ( ( 0.9330127018922194093, 0.9330127018922194093, 1.000000000000000000, 0.8660254037844387076, 1.000000000000000000, 0.8660254037844387076, 1.000000000000000000, 0.9330127018922194093, 0.9330127018922194093 ) ) 
 REPRESENTATION_ITEM ( '' )  );
#59142 = CARTESIAN_POINT ( 'NONE',  ( -4.458734124999999437, 25.60416666803225993, -2.574251347313719407 ) ) ;
#59143 = EDGE_CURVE ( 'NONE', #23270, #16611, #41378, .T. ) ;
#59144 = CARTESIAN_POINT ( 'NONE',  ( 5.000000000000000000, -58.29166666393548013, -2.886751345948130876 ) ) ;
#59145 = CARTESIAN_POINT ( 'NONE',  ( 1.975475456537005874E-15, -14.74999999999999822, 5.000000000000000000 ) ) ;
#59146 = CARTESIAN_POINT ( 'NONE',  ( 2.229367062500001939, -75.22916666530106511, 3.861377020970579999 ) ) ;
#59147 = CARTESIAN_POINT ( 'NONE',  ( -2.499999999999996447, -58.83333333333333570, 4.330127018922195425 ) ) ;
#59148 = CARTESIAN_POINT ( 'NONE',  ( -6.972266317189433020E-16, -66.24999999999998579, -5.000000000000000000 ) ) ;
#59149 = CARTESIAN_POINT ( 'NONE',  ( -4.999999999999999112, 23.20833333606451632, 2.886751345948131764 ) ) ;
#59150 = EDGE_LOOP ( 'NONE', ( #56496, #15311, #39281, #40760 ) ) ;
#59151 = CARTESIAN_POINT ( 'NONE',  ( -6.972266317189433020E-16, 6.750000000000000000, -5.000000000000000000 ) ) ;
#59152 = CARTESIAN_POINT ( 'NONE',  ( -6.972266317189433020E-16, -57.12499999726879452, -5.000000000000000000 ) ) ;
#59153 = CARTESIAN_POINT ( 'NONE',  ( -2.500000000000000444, -19.16666666666666430, -4.330127018922193649 ) ) ;
#59154 = CARTESIAN_POINT ( 'NONE',  ( -4.458734124999998549, -24.22916666530107577, 2.574251347313722516 ) ) ;
#59155 = CARTESIAN_POINT ( 'NONE',  ( -2.229367062500000163, -85.47916666530107932, -3.861377020970580443 ) ) ;
#59156 = CARTESIAN_POINT ( 'NONE',  ( 1.846868145590736310, -168.8750000013655779, 4.458734124999999437 ) ) ;
#59157 = CARTESIAN_POINT ( 'NONE',  ( -2.499999999999996447, -18.70833333060214798, 4.330127018922195425 ) ) ;
#59159 = ORIENTED_EDGE ( 'NONE', *, *, #62275, .F. ) ;
#59158 = CARTESIAN_POINT ( 'NONE',  ( -4.458734124999999437, -49.31249999863440792, 0.000000000000000000 ) ) ;
#59160 = CARTESIAN_POINT ( 'NONE',  ( 1.339745962155612702, -35.16965819600734022, -5.000000000000000000 ) ) ;
#59161 = CARTESIAN_POINT ( 'NONE',  ( 0.000000000000000000, -120.0000000000000000, 5.000000000000000000 ) ) ;
#59163 = ORIENTED_EDGE ( 'NONE', *, *, #2887, .F. ) ;
#59162 = CARTESIAN_POINT ( 'NONE',  ( 2.229367062500001939, 1.770833334698927786, 3.861377020970579999 ) ) ;
#59164 = CARTESIAN_POINT ( 'NONE',  ( -50.40829686548195099, -150.0000000013656063, -1.485763867205728284 ) ) ;
#59165 = CARTESIAN_POINT ( 'NONE',  ( -5.000000000000000000, -67.08333333333332860, -2.886751345948128211 ) ) ;
#59166 = CARTESIAN_POINT ( 'NONE',  ( 2.730187237215162345E-16, -151.4375000013656063, -4.458734124999999437 ) ) ;
#59167 = CARTESIAN_POINT ( 'NONE',  ( 2.229367062500001939, -41.22916666530107932, 3.861377020970579999 ) ) ;
#59168 = CARTESIAN_POINT ( 'NONE',  ( -1.339745962155613812, -16.08034179853029499, -5.000000000000000000 ) ) ;
#59169 = CARTESIAN_POINT ( 'NONE',  ( -3.535533905932737309, -162.6250000000000284, -3.535533905932738197 ) ) ;
#59170 = CARTESIAN_POINT ( 'NONE',  ( -2.499999999999996447, 7.291666669397852019, 4.330127018922195425 ) ) ;
#59171 = CARTESIAN_POINT ( 'NONE',  ( -50.55543936806279248, -127.3125000013655921, 0.3552334253322060320 ) ) ;
#59172 = CARTESIAN_POINT ( 'NONE',  ( -3.152548672688508926E-16, -8.812499998634406140, -5.148502694627439702 ) ) ;
#59173 = CARTESIAN_POINT ( 'NONE',  ( 2.229367062500001939, -46.22916666530106511, 3.861377020970579999 ) ) ;
#59174 = CARTESIAN_POINT ( 'NONE',  ( 5.000000000000000000, -89.41666666666665719, -2.886751345948130876 ) ) ;
#59175 = CARTESIAN_POINT ( 'NONE',  ( 4.458734124999999437, -149.4375000013656063, 0.000000000000000000 ) ) ;
#59176 = CARTESIAN_POINT ( 'NONE',  ( -2.229367062499996610, -89.39583333196773651, 3.861377020970582219 ) ) ;
#59177 = CARTESIAN_POINT ( 'NONE',  ( -6.972266317189433020E-16, 27.74999999999999645, -5.000000000000000000 ) ) ;
#59178 = ORIENTED_EDGE ( 'NONE', *, *, #12586, .T. ) ;
#59179 = CARTESIAN_POINT ( 'NONE',  ( 1.975475456537005874E-15, -31.75000000000000000, 5.000000000000000000 ) ) ;
#59180 = CARTESIAN_POINT ( 'NONE',  ( -4.458734124999999437, 29.35416666803225993, -2.574251347313719407 ) ) ;
#59181 = CARTESIAN_POINT ( 'NONE',  ( -54.60164318462004474, -151.5000000027312410, -4.984105922594373794 ) ) ;
#59182 = VECTOR ( 'NONE', #41980, 1000.000000000000000 ) ;
#59183 = CARTESIAN_POINT ( 'NONE',  ( 5.000000000000000000, -82.29166666393547303, -2.886751345948130876 ) ) ;
#59184 = ORIENTED_EDGE ( 'NONE', *, *, #46516, .F. ) ;
#59185 = VECTOR ( 'NONE', #25049, 1000.000000000000000 ) ;
#59186 = CARTESIAN_POINT ( 'NONE',  ( -2.229367062499996610, 4.854166668032261711, 3.861377020970582219 ) ) ;
#59187 = AXIS2_PLACEMENT_3D ( 'NONE', #59029, #44223, #21073 ) ;
#59188 = CARTESIAN_POINT ( 'NONE',  ( -6.972266317189433020E-16, -1.124999997268814278, -5.000000000000000000 ) ) ;
#59189 = CARTESIAN_POINT ( 'NONE',  ( -3.152548672688508926E-16, -18.81249999863440792, -5.148502694627439702 ) ) ;
#59190 =( BOUNDED_CURVE ( )  B_SPLINE_CURVE ( 2, ( #23893, #43495, #29320, #19053, #24523, #38668, #53472, #9403, #29012 ),
 .UNSPECIFIED., .F., .F. ) 
 B_SPLINE_CURVE_WITH_KNOTS ( ( 3, 2, 2, 2, 3 ),
 ( 0.1250000000000001110, 0.1291666666666667906, 0.1333333333333334425, 0.1375000000000001221, 0.1416666666666667740 ),
 .UNSPECIFIED. ) 
 CURVE ( )  GEOMETRIC_REPRESENTATION_ITEM ( )  RATIONAL_B_SPLINE_CURVE ( ( 0.9999999999999980016, 0.9238795325112887369, 1.000000000000000000, 0.9238795325112867385, 1.000000000000000000, 0.9238795325112867385, 1.000000000000000000, 0.9238795325112847401, 1.000000000000001998 ) ) 
 REPRESENTATION_ITEM ( '' )  );
#59191 = CARTESIAN_POINT ( 'NONE',  ( -5.000000000000000000, 8.916666666666666075, -2.886751345948128211 ) ) ;
#59192 = CARTESIAN_POINT ( 'NONE',  ( 4.458734124999998549, -0.7291666653010709931, -2.574251347313721627 ) ) ;
#59193 = CARTESIAN_POINT ( 'NONE',  ( 1.339745962155615144, -55.58034179853028434, 4.999999999999999112 ) ) ;
#59194 = CARTESIAN_POINT ( 'NONE',  ( 1.846868145590736310, -150.6250000013655779, 4.458734124999997661 ) ) ;
#59195 =( BOUNDED_CURVE ( )  B_SPLINE_CURVE ( 2, ( #52813, #14192, #12937, #43772, #42838, #47359, #32880, #3307, #62788 ),
 .UNSPECIFIED., .F., .F. ) 
 B_SPLINE_CURVE_WITH_KNOTS ( ( 3, 2, 2, 2, 3 ),
 ( 0.3083333333333336257, 0.3125000000000002776, 0.3166666666666669294, 0.3208333333333336368, 0.3250000000000002887 ),
 .UNSPECIFIED. ) 
 CURVE ( )  GEOMETRIC_REPRESENTATION_ITEM ( )  RATIONAL_B_SPLINE_CURVE ( ( 0.9999999999999948930, 0.9238795325112918455, 1.000000000000000000, 0.9238795325112867385, 1.000000000000000000, 0.9238795325112867385, 1.000000000000000000, 0.9238795325112816315, 1.000000000000005107 ) ) 
 REPRESENTATION_ITEM ( '' )  );
#59196 = CARTESIAN_POINT ( 'NONE',  ( -4.458734124999997661, 20.52083333469892423, 2.574251347313722516 ) ) ;
#59197 = ORIENTED_EDGE ( 'NONE', *, *, #15034, .T. ) ;
#59198 = CARTESIAN_POINT ( 'NONE',  ( 9.457646018065525792E-16, -97.06249999863439371, 5.148502694627439702 ) ) ;
#59199 = CARTESIAN_POINT ( 'NONE',  ( -51.75738570946856498, -155.0000000000000284, 3.805975901505577408 ) ) ;
#59200 = CARTESIAN_POINT ( 'NONE',  ( 4.613983237546155358, -6.452243898629820507, -7.591546097228409451 ) ) ;
#59201 = CARTESIAN_POINT ( 'NONE',  ( -4.458734124999998549, -13.22916666530107221, 2.574251347313722516 ) ) ;
#59202 = CARTESIAN_POINT ( 'NONE',  ( 2.788906526875773208E-15, 27.87500000273118417, -5.000000000000000000 ) ) ;
#59203 = CARTESIAN_POINT ( 'NONE',  ( -2.499999999999996447, -12.83333333333333570, 4.330127018922195425 ) ) ;
#59204 = CARTESIAN_POINT ( 'NONE',  ( -59.44456063193725015, -152.5625000013656063, -0.3552334253322034230 ) ) ;
#59205 = CARTESIAN_POINT ( 'NONE',  ( -5.000000000000000000, -40.87499999726880162, 0.000000000000000000 ) ) ;
#59206 = CARTESIAN_POINT ( 'NONE',  ( -3.152548672688508926E-16, 13.43750000136559386, -5.148502694627439702 ) ) ;
#59207 = FACE_OUTER_BOUND ( 'NONE', #32666, .T. ) ;
#59208 = FACE_OUTER_BOUND ( 'NONE', #44610, .T. ) ;
#59209 = CARTESIAN_POINT ( 'NONE',  ( -2.229367062499996610, 16.85416666803225993, 3.861377020970582219 ) ) ;
#59210 = CARTESIAN_POINT ( 'NONE',  ( -4.458734124999999437, -59.39583333196773651, -2.574251347313719407 ) ) ;
#59211 = ORIENTED_EDGE ( 'NONE', *, *, #43621, .F. ) ;
#59212 = CARTESIAN_POINT ( 'NONE',  ( 2.229367062500001939, -8.229166665301073991, 3.861377020970579999 ) ) ;
#59213 = CARTESIAN_POINT ( 'NONE',  ( -4.999999999999999112, 7.083333333333333037, 2.886751345948131764 ) ) ;
#59214 = CARTESIAN_POINT ( 'NONE',  ( 3.152801135295367541, -168.3125000013656063, -3.152801135295367541 ) ) ;
#59215 = CARTESIAN_POINT ( 'NONE',  ( 2.229367062500001939, -54.97916666530107221, 3.861377020970579999 ) ) ;
#59216 = CARTESIAN_POINT ( 'NONE',  ( 5.000000000000000000, -91.37499999726880162, -6.123233995736766282E-16 ) ) ;
#59217 = CARTESIAN_POINT ( 'NONE',  ( -4.458734124999997661, -35.22916666530107221, 2.574251347313722516 ) ) ;
#59218 = CARTESIAN_POINT ( 'NONE',  ( 0.000000000000000000, -120.0000000000000000, 0.000000000000000000 ) ) ;
#59219 = FACE_OUTER_BOUND ( 'NONE', #30373, .T. ) ;
#59220 = LINE ( 'NONE', #15794, #2869 ) ;
#59221 = CARTESIAN_POINT ( 'NONE',  ( 1.846868145590735200, -155.5000000013656063, -4.458734124999999437 ) ) ;
#59222 = CARTESIAN_POINT ( 'NONE',  ( 5.000000000000000888, -44.58333333333333570, 2.886751345948126879 ) ) ;
#59223 = CARTESIAN_POINT ( 'NONE',  ( -6.972266317189433020E-16, 0.8750000027311866102, -5.000000000000000000 ) ) ;
#59224 = CARTESIAN_POINT ( 'NONE',  ( -59.47495026108718008, -134.9999999999999716, -1.537000407889604459 ) ) ;
#59225 = VERTEX_POINT ( 'NONE', #22013 ) ;
#59226 = CARTESIAN_POINT ( 'NONE',  ( 9.457646018065525792E-16, -100.0624999986344221, 5.148502694627439702 ) ) ;
#59227 = CARTESIAN_POINT ( 'NONE',  ( -4.458734124999998549, 1.520833334698927342, 2.574251347313722516 ) ) ;
#59228 = CARTESIAN_POINT ( 'NONE',  ( -5.000000000000000000, -3.083333333333333925, -2.886751345948128211 ) ) ;
#59229 = VECTOR ( 'NONE', #32979, 1000.000000000000000 ) ;
#59230 = CARTESIAN_POINT ( 'NONE',  ( 4.458734124999998549, -68.72916666530107932, -2.574251347313721627 ) ) ;
#59231 = CARTESIAN_POINT ( 'NONE',  ( -4.999999999999999112, 0.2083333360645180099, 2.886751345948131764 ) ) ;
#59233 = ORIENTED_EDGE ( 'NONE', *, *, #40356, .F. ) ;
#59232 = CARTESIAN_POINT ( 'NONE',  ( -3.152548672688508926E-16, -31.56249999863440436, -5.148502694627439702 ) ) ;
#59234 = CARTESIAN_POINT ( 'NONE',  ( 5.000000000000000000, -153.1250000027312126, 0.000000000000000000 ) ) ;
#59235 = CARTESIAN_POINT ( 'NONE',  ( 1.975475456537005874E-15, -47.62499999726880873, 5.000000000000000000 ) ) ;
#59236 = ORIENTED_EDGE ( 'NONE', *, *, #33494, .F. ) ;
#59237 = CARTESIAN_POINT ( 'NONE',  ( -51.19402409849444524, -136.5000000000000284, -3.242614290531456334 ) ) ;
#59238 = CARTESIAN_POINT ( 'NONE',  ( -5.000000000000000000, -48.00000000000000000, 0.000000000000000000 ) ) ;
#59240 = CARTESIAN_POINT ( 'NONE',  ( 2.229367062500001939, -25.22916666530106866, 3.861377020970579999 ) ) ;
#59239 = CARTESIAN_POINT ( 'NONE',  ( 1.339745962155615144, -26.58034179853029855, 4.999999999999999112 ) ) ;
#59241 = CARTESIAN_POINT ( 'NONE',  ( -5.000000000000000000, -3.999999999999996447, 0.000000000000000000 ) ) ;
#59242 = CARTESIAN_POINT ( 'NONE',  ( -2.229367062499996610, -69.14583333196773651, 3.861377020970582219 ) ) ;
#59243 =( BOUNDED_CURVE ( )  B_SPLINE_CURVE ( 2, ( #14212, #4886, #53459, #62503, #9389, #28692, #48311, #13600, #13280 ),
 .UNSPECIFIED., .F., .F. ) 
 B_SPLINE_CURVE_WITH_KNOTS ( ( 3, 2, 2, 2, 3 ),
 ( 0.8482142857142856984, 0.8488095238095237915, 0.8499999999999999778, 0.8511904761904761640, 0.8517857142857142572 ),
 .UNSPECIFIED. ) 
 CURVE ( )  GEOMETRIC_REPRESENTATION_ITEM ( )  RATIONAL_B_SPLINE_CURVE ( ( 0.9330127018922194093, 0.9330127018922194093, 1.000000000000000000, 0.8660254037844387076, 1.000000000000000000, 0.8660254037844387076, 1.000000000000000000, 0.9330127018922194093, 0.9330127018922194093 ) ) 
 REPRESENTATION_ITEM ( '' )  );
#59244 = CARTESIAN_POINT ( 'NONE',  ( 4.458734125000000326, -142.6250000013655779, -1.846868145590734978 ) ) ;
#59246 = EDGE_CURVE ( 'NONE', #1843, #41941, #17552, .T. ) ;
#59245 = CARTESIAN_POINT ( 'NONE',  ( -3.152548672688508926E-16, -83.56249999863440792, -5.148502694627439702 ) ) ;
#59247 = CARTESIAN_POINT ( 'NONE',  ( -57.19623071787017210, -138.6250000013655779, 4.297418129356382899 ) ) ;
#59248 = CARTESIAN_POINT ( 'NONE',  ( 4.458734124999998549, -27.97916666530107577, -2.574251347313721627 ) ) ;
#59249 = CARTESIAN_POINT ( 'NONE',  ( -2.499999999999996447, -72.70833333060214443, 4.330127018922195425 ) ) ;
#59250 = VERTEX_POINT ( 'NONE', #20742 ) ;
#59251 = CYLINDRICAL_SURFACE ( 'NONE', #2283, 5.000000000000000000 ) ;
#59252 = ORIENTED_EDGE ( 'NONE', *, *, #25938, .F. ) ;
#59253 = CARTESIAN_POINT ( 'NONE',  ( -4.458734124999999437, -73.64583333196773651, -2.574251347313719407 ) ) ;
#59254 = CYLINDRICAL_SURFACE ( 'NONE', #57450, 5.000000000000000000 ) ;
#59255 =( LENGTH_UNIT ( ) NAMED_UNIT ( * ) SI_UNIT ( .MILLI., .METRE. ) );
#59256 = EDGE_LOOP ( 'NONE', ( #1205, #12710, #25806, #63555 ) ) ;
#59257 = CARTESIAN_POINT ( 'NONE',  ( 2.500000000000002220, 12.33333333333333215, 4.330127018922192761 ) ) ;
#59258 = CARTESIAN_POINT ( 'NONE',  ( 2.499999999999998668, -31.20833333060214443, -4.330127018922193649 ) ) ;
#59259 = CARTESIAN_POINT ( 'NONE',  ( -2.229367062500000163, -57.72916666530107932, -3.861377020970580443 ) ) ;
#59260 = CARTESIAN_POINT ( 'NONE',  ( -2.229367062499996610, -5.395833331967740953, 3.861377020970582219 ) ) ;
#59261 = ORIENTED_EDGE ( 'NONE', *, *, #20933, .T. ) ;
#59262 = CARTESIAN_POINT ( 'NONE',  ( -9.184850993605147944E-16, -146.2500000000000284, 5.000000000000000000 ) ) ;
#59263 = FACE_OUTER_BOUND ( 'NONE', #63038, .T. ) ;
#59264 = CARTESIAN_POINT ( 'NONE',  ( -4.458734124999999437, 11.68750000136559564, 0.000000000000000000 ) ) ;
#59265 = CARTESIAN_POINT ( 'NONE',  ( -50.70258187064364108, -141.1250000013655779, 2.196230717870141014 ) ) ;
#59266 = CARTESIAN_POINT ( 'NONE',  ( 2.499999999999998668, -32.33333333333332860, -4.330127018922193649 ) ) ;
#59267 = CARTESIAN_POINT ( 'NONE',  ( 4.458734124999999437, -162.4375000013655779, 0.000000000000000000 ) ) ;
#59268 = AXIS2_PLACEMENT_3D ( 'NONE', #45890, #15986, #31096 ) ;
#59269 = EDGE_LOOP ( 'NONE', ( #46611, #53317, #15584, #29793 ) ) ;
#59270 = CARTESIAN_POINT ( 'NONE',  ( 4.458734124999998549, -82.72916666530106511, -2.574251347313721627 ) ) ;
#59271 = CARTESIAN_POINT ( 'NONE',  ( 4.458734124999998549, 2.270833334698928230, -2.574251347313721627 ) ) ;
#59272 = CIRCLE ( 'NONE', #15106, 5.000000000000000000 ) ;
#59273 = CARTESIAN_POINT ( 'NONE',  ( 5.000000000000000000, -85.49999999999998579, -6.123233995736766282E-16 ) ) ;
#59274 = CARTESIAN_POINT ( 'NONE',  ( -5.000000000000000000, 1.999999999999998224, 0.000000000000000000 ) ) ;
#59275 = CARTESIAN_POINT ( 'NONE',  ( 9.457646018065525792E-16, -64.31249999863440792, 5.148502694627439702 ) ) ;
#59276 = CARTESIAN_POINT ( 'NONE',  ( -4.999999999999999112, -27.79166666393547658, 2.886751345948131764 ) ) ;
#59277 = CARTESIAN_POINT ( 'NONE',  ( -1.339745962155613812, -29.20534180126147916, -5.000000000000000000 ) ) ;
#59278 = CARTESIAN_POINT ( 'NONE',  ( -4.458734124999999437, 28.68750000136559208, 0.000000000000000000 ) ) ;
#59279 = LINE ( 'NONE', #48354, #18232 ) ;
#59280 = FACE_OUTER_BOUND ( 'NONE', #41152, .T. ) ;
#59281 = CARTESIAN_POINT ( 'NONE',  ( -4.458734124999998549, -48.22916666530106511, 2.574251347313722516 ) ) ;
#59282 = CARTESIAN_POINT ( 'NONE',  ( 9.457646018065525792E-16, -32.31249999863440792, 5.148502694627439702 ) ) ;
#59283 = CARTESIAN_POINT ( 'NONE',  ( -4.458734124999999437, 9.354166668032261711, -2.574251347313719407 ) ) ;
#59284 = CARTESIAN_POINT ( 'NONE',  ( -2.499999999999996447, -9.708333330602146205, 4.330127018922195425 ) ) ;
#59285 = CARTESIAN_POINT ( 'NONE',  ( 5.000000000000000000, 21.50000000000000000, -6.123233995736766282E-16 ) ) ;
#59286 = CARTESIAN_POINT ( 'NONE',  ( 3.535533905932736864, -149.2500000027311842, 3.535533905932738641 ) ) ;
#59287 = CARTESIAN_POINT ( 'NONE',  ( 1.339745962155615144, -54.58034179853029144, 4.999999999999999112 ) ) ;
#59288 = CARTESIAN_POINT ( 'NONE',  ( 2.229367062499998831, -36.64583333196773651, -3.861377020970580887 ) ) ;
#59289 = CARTESIAN_POINT ( 'NONE',  ( 2.500000000000002220, -75.54166666393547303, 4.330127018922192761 ) ) ;
#59290 = CARTESIAN_POINT ( 'NONE',  ( -59.44456063193725015, -144.8125000013656063, -0.3552334253322034230 ) ) ;
#59291 = CARTESIAN_POINT ( 'NONE',  ( 5.000000000000000000, -140.0625000000000000, 2.071067811865478614 ) ) ;
#59292 = CARTESIAN_POINT ( 'NONE',  ( 2.071067811865392461, -141.3125000027312410, 5.000000000000084377 ) ) ;
#59293 = CARTESIAN_POINT ( 'NONE',  ( 4.458734125000000326, -79.14583333196773651, 2.574251347313718519 ) ) ;
#59294 = CARTESIAN_POINT ( 'NONE',  ( -4.458734125000000326, -167.1250000013656063, 1.846868145590734089 ) ) ;
#59295 = CARTESIAN_POINT ( 'NONE',  ( -5.000000000000000888, -160.5625000000000284, -2.071067811865475949 ) ) ;
#59296 = CARTESIAN_POINT ( 'NONE',  ( 1.975475456537005874E-15, -45.62499999726880873, 5.000000000000000000 ) ) ;
#59297 = CARTESIAN_POINT ( 'NONE',  ( -3.535250795749689387E-16, -27.24999999999999645, -5.773502691896257311 ) ) ;
#59298 = CARTESIAN_POINT ( 'NONE',  ( -3.152801135295367985, -144.8125000013655779, 3.152801135295367096 ) ) ;
#59299 = ORIENTED_EDGE ( 'NONE', *, *, #45025, .T. ) ;
#59300 = CARTESIAN_POINT ( 'NONE',  ( -2.229367062500000163, 28.27083333469892779, -3.861377020970580443 ) ) ;
#59301 = VERTEX_POINT ( 'NONE', #7229 ) ;
#59302 = CARTESIAN_POINT ( 'NONE',  ( -2.229367062500000163, -61.72916666530106511, -3.861377020970580443 ) ) ;
#59303 = CARTESIAN_POINT ( 'NONE',  ( 5.000000000000000888, 20.54166666939784847, 2.886751345948126879 ) ) ;
#59304 = CARTESIAN_POINT ( 'NONE',  ( 5.000000000000000000, 13.62500000273118417, -6.123233995736766282E-16 ) ) ;
#59305 = CARTESIAN_POINT ( 'NONE',  ( -3.535250795749689387E-16, 14.75000000000000000, -5.773502691896257311 ) ) ;
#59306 = CARTESIAN_POINT ( 'NONE',  ( -2.229367062500000163, -50.47916666530107221, -3.861377020970580443 ) ) ;
#59307 = CARTESIAN_POINT ( 'NONE',  ( 9.457646018065525792E-16, -6.062499998634403475, 5.148502694627439702 ) ) ;
#59308 = CYLINDRICAL_SURFACE ( 'NONE', #20535, 11.00000000000000000 ) ;
#59309 = CARTESIAN_POINT ( 'NONE',  ( -2.500000000000000444, -77.16666666666665719, -4.330127018922193649 ) ) ;
#59310 = CARTESIAN_POINT ( 'NONE',  ( 1.975475456537005874E-15, 13.37500000273118417, 5.000000000000000000 ) ) ;
#59311 = CYLINDRICAL_SURFACE ( 'NONE', #700, 5.000000000000000000 ) ;
#59313 = CARTESIAN_POINT ( 'NONE',  ( -4.458734124999999437, -23.31249999863440436, 0.000000000000000000 ) ) ;
#59312 = CARTESIAN_POINT ( 'NONE',  ( -1.339745962155610925, -58.79465819873852439, 5.000000000000000000 ) ) ;
#59314 = VECTOR ( 'NONE', #55333, 1000.000000000000000 ) ;
#59315 = CARTESIAN_POINT ( 'NONE',  ( -1.339745962155610925, -77.66965819600730470, 5.000000000000000000 ) ) ;
#59316 = CARTESIAN_POINT ( 'NONE',  ( 9.457646018065525792E-16, -55.06249999863439371, 5.148502694627439702 ) ) ;
#59317 = CARTESIAN_POINT ( 'NONE',  ( 3.152801135295367541, -154.5625000013656063, -3.152801135295367541 ) ) ;
#59318 = EDGE_CURVE ( 'NONE', #55261, #1258, #55158, .T. ) ;
#59319 = VECTOR ( 'NONE', #46556, 1000.000000000000000 ) ;
#59320 =( BOUNDED_CURVE ( )  B_SPLINE_CURVE ( 2, ( #49827, #25389, #58535, #19605, #39851, #53703, #976, #9635, #59494 ),
 .UNSPECIFIED., .F., .F. ) 
 B_SPLINE_CURVE_WITH_KNOTS ( ( 3, 2, 2, 2, 3 ),
 ( 0.1562500000000000000, 0.1569444444444444420, 0.1583333333333333259, 0.1597222222222222099, 0.1604166666666666796 ),
 .UNSPECIFIED. ) 
 CURVE ( )  GEOMETRIC_REPRESENTATION_ITEM ( )  RATIONAL_B_SPLINE_CURVE ( ( 0.9330127018922194093, 0.9330127018922194093, 1.000000000000000000, 0.8660254037844387076, 1.000000000000000000, 0.8660254037844387076, 1.000000000000000000, 0.9330127018922180770, 0.9330127018922194093 ) ) 
 REPRESENTATION_ITEM ( '' )  );
#59321 = CARTESIAN_POINT ( 'NONE',  ( 5.000000000000000000, -55.29166666393548013, -2.886751345948129988 ) ) ;
#59322 = ORIENTED_EDGE ( 'NONE', *, *, #6329, .T. ) ;
#59323 = CARTESIAN_POINT ( 'NONE',  ( -1.339745962155610925, -48.79465819873850307, 5.000000000000000000 ) ) ;
#59324 = CARTESIAN_POINT ( 'NONE',  ( -4.458734124999999437, 4.354166668032260823, -2.574251347313719407 ) ) ;
#59325 = EDGE_LOOP ( 'NONE', ( #59598, #12131, #23378, #5346 ) ) ;
#59327 = CARTESIAN_POINT ( 'NONE',  ( -6.972266317189433020E-16, -29.25000000000000000, -5.000000000000000000 ) ) ;
#59326 = CARTESIAN_POINT ( 'NONE',  ( 2.499999999999998668, -87.33333333333332860, -4.330127018922193649 ) ) ;
#59328 = CARTESIAN_POINT ( 'NONE',  ( 1.846868145590736310, -155.6250000013656063, 4.458734124999999437 ) ) ;
#59329 = ORIENTED_EDGE ( 'NONE', *, *, #5455, .T. ) ;
#59330 = EDGE_CURVE ( 'NONE', #34549, #26676, #51294, .T. ) ;
#59331 = CYLINDRICAL_SURFACE ( 'NONE', #28281, 5.000000000000000000 ) ;
#59332 = CARTESIAN_POINT ( 'NONE',  ( -60.14911071818854538, -130.0625000000000284, 1.666127454062681368 ) ) ;
#59333 = CYLINDRICAL_SURFACE ( 'NONE', #14907, 5.000000000000000000 ) ;
#59334 = CARTESIAN_POINT ( 'NONE',  ( -4.458734124999999437, -43.64583333196774362, -2.574251347313719407 ) ) ;
#59335 = ORIENTED_EDGE ( 'NONE', *, *, #46043, .T. ) ;
#59336 =( BOUNDED_SURFACE ( )  B_SPLINE_SURFACE ( 1, 2, ( 
 ( #53689, #38570, #9621, #48544, #18954, #23797, #24740, #19591, #43089, #24422, #14128, #30761, #35591, #59156, #24112, #33442, #29229, #53059, #33755, #23487, #9307, #4483, #28609, #34066, #50382, #62730, #53372, #39202, #58201, #48855, #28921, #44343, #57899, #43710, #4798, #39519, #54003, #63354, #58827, #49182, #19270, #14444, #13823, #8999, #48226, #38886, #15089, #58520, #44024, #63671, #14757, #306, #4183, #19904, #43399, #63044, #34375, #9932, #29548, #11765, #25933, #51348, #36537, #2460, #32350, #46517, #6328, #41994, #35912, #60367, #56494, #26576, #36864, #51022, #21114, #16920, #45552, #1834, #7287, #31384, #16607, #11454, #22071, #12092, #61634, #32027, #6966, #46194, #12415, #27209, #21435, #26898, #2155, #31714, #60686, #37185, #2772, #41663, #61315, #17240, #56810, #26248, #46827, #51663, #17567, #55543, #45870, #36225, #1511, #40719, #7603, #12727, #22393, #16291, #21761, #31073, #50697, #6640, #41039, #55849, #41355, #60998, #56169, #3719, #58049, #18186, #19111, #13360, #62582, #27517, #8848, #32663, #62886, #28462, #48077, #13045, #8228, #13979, #32983, #52603, #18799, #9158, #47455, #52911, #8537, #57749, #42626, #38730, #48392, #4032, #23650, #33292, #58368, #27833, #28772, #13673, #23951, #17869, #3407, #62265, #47147, #3095, #43246, #43555, #38423, #51973, #28147, #63201, #33607, #53227, #7912, #52291, #4334, #14296, #22712, #23337, #42310, #37812, #61950, #47764, #18504, #37490, #57130, #23023, #57440, #42940, #38125, #58680, #53848, #9777, #40002, #29383, #34531, #24587, #49017, #40331, #43867, #25222, #4965, #54816, #796, #44193, #59649, #158, #25540, #49980, #4640, #15582, #5932, #20075, #19754, #10747, #24263, #39365, #15252, #45157, #20403, #54164, #49666, #35201, #10105, #24908, #20727, #29075, #1123, #58996, #59973, #14925, #29713, #49344, #5606, #30356, #33915, #53540, #63515, #9466, #5290, #44511, #473, #39681, #48700, #34878, #59317, #30037, #19439, #10424, #39051, #14607, #34222, #54499, #44833, #36154, #46439, #60612, #30686, #26501, #41915, #11377, #16843, #40964, #26179, #21043, #31640, #21685, #51585, #46116, #15894, #27134, #6564, #51275, #30998, #6887, #56091, #1441, #56419, #11062, #50303, #50946, #12342, #40650, #31953, #1758, #2385, #36786, #60289, #21995, #16529, #2079, #35514, #45798, #55774, #12011, #7523, #46749, #36464, #16213, #7208, #55461, #45477, #35839, #11691, #50625, #21360, #41274, #2694, #31310, #60924, #22314, #55135, #61240, #41588, #26819, #17162, #6251, #25861, #38046, #17492, #62814, #18732, #57363, #37113, #43174, #42548, #38357, #57983, #56732, #12963, #12652, #32267, #37418, #13908, #32910, #7837, #18108, #9087, #61878, #33536, #28075, #32588, #47692, #22952, #57052, #17794, #53151, #57678, #51896, #37730, #8158, #52211, #27757, #33222, #62187, #47385, #3336, #42235, #27438, #28696, #13284, #48004, #52533, #42863, #47072, #8467, #3644, #23255, #23883, #61558, #3021, #22637, #23578, #62508, #18425, #13605, #48315, #52841, #4265, #8775, #28385, #3957, #44436, #34151, #10664, #54744, #15507, #44115, #53463, #49275, #9392, #53773, #43486, #29310, #24513, #48628, #9705, #38974, #48942, #15175, #4890, #14531, #79, #24191, #38659, #25143, #19679, #29961, #43798, #24830, #63131, #58611, #63445, #19362, #5854, #19042, #58298, #33844, #5528, #14217, #29003, #4568, #35128, #39291, #30280, #397, #49900, #58918, #19999, #14847, #34459, #54090, #10029, #29641, #5211, #39607, #59244, #34800, #54423, #10352, #49586, #44754, #715, #20325, #39927, #59574, #41201, #20971, #16456, #2002, #10984, #2315, #20656, #40260, #60532, #21918, #50227, #41515, #11300, #56020, #46361, #6175, #31564, #50551, #36075, #51513, #55383, #6495, #21606, #61168, #17091, #46038, #30604, #60845, #1369, #55060, #45403, #21280, #40572, #60213, #31238, #36713, #25792, #16137 ),
 ( #7129, #26106, #56345, #26745, #1050, #35759, #59900, #15821, #30924, #12266, #55704, #35434, #45727, #31879, #1678, #25462, #11618, #40887, #50869, #6814, #26421, #16771, #45084, #36389, #11934, #51197, #13533, #37338, #38286, #32508, #18029, #46676, #27997, #51819, #18350, #47616, #3569, #32189, #27364, #46998, #33153, #2946, #8082, #61797, #22561, #13834, #17417, #62432, #42161, #28308, #37974, #17723, #52767, #56972, #62742, #23499, #41839, #8696, #43102, #57294, #12889, #47924, #61485, #52140, #52461, #18664, #57606, #27685, #23177, #3880, #47311, #62110, #57912, #2621, #33454, #3264, #7450, #22876, #42469, #37651, #42788, #27058, #22239, #37032, #56658, #12575, #13210, #32832, #8396, #7761, #9011, #34389, #19604, #49195, #15429, #29562, #53071, #25068, #18967, #43412, #39531, #9634, #19917, #34079, #4196, #1, #28623, #48556, #54015, #14457, #63368, #58213, #5134, #58841, #44678, #15101, #53702, #29242, #59169, #10276, #4495, #9947, #48867, #14770, #43723, #20248, #49511, #24751, #44356, #319, #39850, #9319, #29882, #34718, #639, #38582, #28933, #19284, #48239, #23809, #54345, #59493, #5450, #63055, #4812, #14141, #33767, #53387, #24123, #38899, #58533, #24435, #44037, #39216, #1924, #49826, #31164, #21529, #30852, #54980, #26341, #5770, #10909, #26032, #41125, #55632, #20893, #40809, #50795, #40495, #55314, #36317, #10585, #60773, #30524, #16698, #50147, #35358, #60136, #60457, #6732, #55942, #45960, #25388, #35050, #16057, #6102, #25716, #1295, #54662, #21203, #45647, #36002, #30197, #45009, #975, #20577, #45327, #35686, #40184, #1605, #59821, #16383, #11228, #11547, #15742, #50482, #6421, #53903, #39105, #33973, #44567, #34592, #856, #54551, #9829, #29440, #59374, #49717, #24317, #29766, #49072, #54223, #19490, #59701, #25275, #49400, #24962, #10161, #15633, #48753, #5662, #5344, #20459, #58424, #4695, #58733, #24007, #43610, #525, #40058, #15308, #28827, #5020, #35249, #10474, #39734, #48448, #53593, #20134, #34930, #44896, #44246, #30087, #14659, #54869, #24639, #39417, #4388, #63252, #9523, #19168, #38785, #14351, #29130, #43924, #63571, #34278, #210, #19808, #59055, #14983, #17215, #20778, #2134, #25912, #31692, #41332, #50360, #36516, #30739, #2439, #46491, #40383, #1178, #60979, #31052, #16900, #55520, #25599, #21416, #36842, #6308, #11743, #35890, #21094, #15947, #26553, #16586, #22048, #56146, #11434, #50675, #12067, #51327, #45530, #31361, #6617, #36206, #1491, #41641, #7265, #51002, #6942, #55828, #61293, #40698, #26877, #46173, #10800, #60024, #60343, #16271, #5994, #45212, #21737, #30412, #50036, #35569, #26230, #55193, #11113, #45850, #1812, #41019, #60662, #31686, #32955, #42600, #60973, #51321, #3381, #3695, #41326, #16893, #13334, #7569, #52580, #61923, #28121, #36510, #42284, #32002, #8511, #47738, #56141, #41964, #7259, #47119, #26872, #51636, #12061, #27182, #22364, #46484, #51946, #2432, #22042, #46798, #57097, #36836, #32315, #17843, #41634, #18154, #61287, #17209, #12702, #37783, #56466, #57414, #2744, #8202, #62237, #12388, #47430, #61606, #7886, #17540, #37159, #56783, #37466, #27489, #3067, #13016, #22684, #32635, #52264, #27805, #22998, #19086, #62862, #58025, #29050, #44165, #28438, #23626, #19727, #42908, #18775, #24239, #43531, #48674, #13954, #54137, #39336, #43843, #19413, #4614, #10076, #43222, #133, #63489, #58969, #52888, #38402, #33580, #18477, #38098, #39028, #14897, #9751, #23308, #23929, #34506, #48991, #34198, #62557, #48052, #53200, #49318, #9134, #57723, #29358, #28740, #29688, #48367, #33890, #13649, #58655, #4004, #53822, #14575, #4938, #4310, #63175, #38705, #24561, #58342, #14271, #53510, #9440, #33269, #8823, #60265, #20376, #26151, #35808, #44806, #30972, #25190, #60580, #21332, #39654, #50597, #40932, #55108, #39977, #45770, #59291, #59622 ) ),
 .UNSPECIFIED., .F., .F., .F. ) 
 B_SPLINE_SURFACE_WITH_KNOTS ( ( 2, 2 ),
 ( 3, 2, 2, 2, 2, 2, 2, 2, 2, 2, 2, 2, 2, 2, 2, 2, 2, 2, 2, 2, 2, 2, 2, 2, 2, 2, 2, 2, 2, 2, 2, 2, 2, 2, 2, 2, 2, 2, 2, 2, 2, 2, 2, 2, 2, 2, 2, 2, 2, 2, 2, 2, 2, 2, 2, 2, 2, 2, 2, 2, 2, 2, 2, 2, 2, 2, 2, 2, 2, 2, 2, 2, 2, 2, 2, 2, 2, 2, 2, 2, 2, 2, 2, 2, 2, 2, 2, 2, 2, 2, 2, 2, 2, 2, 2, 2, 2, 2, 2, 2, 2, 2, 2, 2, 2, 2, 2, 2, 2, 2, 2, 2, 2, 2, 2, 2, 2, 2, 2, 2, 2, 2, 2, 2, 2, 2, 2, 2, 2, 2, 2, 2, 2, 2, 2, 2, 2, 2, 2, 2, 2, 2, 2, 2, 2, 2, 2, 2, 2, 2, 2, 2, 2, 2, 2, 2, 2, 2, 2, 2, 2, 2, 2, 2, 2, 2, 2, 2, 2, 2, 2, 2, 2, 2, 2, 2, 2, 2, 2, 2, 2, 2, 2, 2, 2, 2, 2, 2, 2, 2, 2, 2, 2, 2, 2, 2, 2, 2, 2, 2, 2, 2, 2, 2, 2, 2, 2, 2, 2, 2, 2, 2, 2, 2, 2, 2, 2, 2, 2, 2, 2, 2, 2, 2, 2, 2, 2, 2, 2, 2, 2, 2, 2, 2, 2, 2, 2, 2, 2, 2, 3 ),
 ( 0.000000000000000000, 1.000000000000000000 ),
 ( 0.000000000000000000, 0.004166666666666666609, 0.008333333333333333218, 0.01250000000000000069, 0.01666666666666666644, 0.02083333333333333218, 0.02500000000000000139, 0.02916666666666666713, 0.03333333333333333287, 0.03749999999999999861, 0.04166666666666666435, 0.04583333333333333010, 0.05000000000000000278, 0.05416666666666666852, 0.05833333333333333426, 0.06250000000000000000, 0.06666666666666666574, 0.07083333333333333148, 0.07499999999999999722, 0.07916666666666666297, 0.08333333333333332871, 0.08749999999999999445, 0.09166666666666666019, 0.09583333333333333981, 0.1000000000000000056, 0.1041666666666666713, 0.1083333333333333370, 0.1125000000000000028, 0.1166666666666666685, 0.1208333333333333343, 0.1250000000000000000, 0.1291666666666666796, 0.1333333333333333315, 0.1375000000000000111, 0.1416666666666666630, 0.1458333333333333426, 0.1499999999999999944, 0.1541666666666666741, 0.1583333333333333259, 0.1625000000000000056, 0.1666666666666666574, 0.1708333333333333370, 0.1749999999999999889, 0.1791666666666666685, 0.1833333333333333204, 0.1875000000000000000, 0.1916666666666666796, 0.1958333333333333315, 0.2000000000000000111, 0.2041666666666666630, 0.2083333333333333426, 0.2124999999999999944, 0.2166666666666666741, 0.2208333333333333259, 0.2250000000000000056, 0.2291666666666666574, 0.2333333333333333370, 0.2374999999999999889, 0.2416666666666666685, 0.2458333333333333204, 0.2500000000000000000, 0.2541666666666666519, 0.2583333333333333592, 0.2625000000000000111, 0.2666666666666666630, 0.2708333333333333148, 0.2750000000000000222, 0.2791666666666666741, 0.2833333333333333259, 0.2874999999999999778, 0.2916666666666666852, 0.2958333333333333370, 0.2999999999999999889, 0.3041666666666666408, 0.3083333333333333481, 0.3125000000000000000, 0.3166666666666666519, 0.3208333333333333592, 0.3250000000000000111, 0.3291666666666666630, 0.3333333333333333148, 0.3375000000000000222, 0.3416666666666666741, 0.3458333333333333259, 0.3499999999999999778, 0.3541666666666666852, 0.3583333333333333370, 0.3624999999999999889, 0.3666666666666666408, 0.3708333333333333481, 0.3750000000000000000, 0.3791666666666666519, 0.3833333333333333592, 0.3875000000000000111, 0.3916666666666666630, 0.3958333333333333148, 0.4000000000000000222, 0.4041666666666666741, 0.4083333333333333259, 0.4124999999999999778, 0.4166666666666666852, 0.4208333333333333370, 0.4249999999999999889, 0.4291666666666666408, 0.4333333333333333481, 0.4375000000000000000, 0.4416666666666666519, 0.4458333333333333592, 0.4500000000000000111, 0.4541666666666666630, 0.4583333333333333148, 0.4625000000000000222, 0.4666666666666666741, 0.4708333333333333259, 0.4749999999999999778, 0.4791666666666666852, 0.4833333333333333370, 0.4874999999999999889, 0.4916666666666666408, 0.4958333333333333481, 0.5000000000000000000, 0.5041666666666666519, 0.5083333333333333037, 0.5124999999999999556, 0.5166666666666667185, 0.5208333333333333703, 0.5250000000000000222, 0.5291666666666666741, 0.5333333333333333259, 0.5374999999999999778, 0.5416666666666666297, 0.5458333333333332815, 0.5500000000000000444, 0.5541666666666666963, 0.5583333333333333481, 0.5625000000000000000, 0.5666666666666666519, 0.5708333333333333037, 0.5749999999999999556, 0.5791666666666667185, 0.5833333333333333703, 0.5875000000000000222, 0.5916666666666666741, 0.5958333333333333259, 0.5999999999999999778, 0.6041666666666666297, 0.6083333333333332815, 0.6125000000000000444, 0.6166666666666666963, 0.6208333333333333481, 0.6250000000000000000, 0.6291666666666666519, 0.6333333333333333037, 0.6374999999999999556, 0.6416666666666667185, 0.6458333333333333703, 0.6500000000000000222, 0.6541666666666666741, 0.6583333333333333259, 0.6624999999999999778, 0.6666666666666666297, 0.6708333333333332815, 0.6750000000000000444, 0.6791666666666666963, 0.6833333333333333481, 0.6875000000000000000, 0.6916666666666666519, 0.6958333333333333037, 0.6999999999999999556, 0.7041666666666667185, 0.7083333333333333703, 0.7125000000000000222, 0.7166666666666666741, 0.7208333333333333259, 0.7249999999999999778, 0.7291666666666666297, 0.7333333333333332815, 0.7375000000000000444, 0.7416666666666666963, 0.7458333333333333481, 0.7500000000000000000, 0.7541666666666666519, 0.7583333333333333037, 0.7624999999999999556, 0.7666666666666667185, 0.7708333333333333703, 0.7750000000000000222, 0.7791666666666666741, 0.7833333333333333259, 0.7874999999999999778, 0.7916666666666666297, 0.7958333333333332815, 0.8000000000000000444, 0.8041666666666666963, 0.8083333333333333481, 0.8125000000000000000, 0.8166666666666666519, 0.8208333333333333037, 0.8249999999999999556, 0.8291666666666667185, 0.8333333333333333703, 0.8375000000000000222, 0.8416666666666666741, 0.8458333333333333259, 0.8499999999999999778, 0.8541666666666666297, 0.8583333333333332815, 0.8625000000000000444, 0.8666666666666666963, 0.8708333333333333481, 0.8750000000000000000, 0.8791666666666666519, 0.8833333333333333037, 0.8874999999999999556, 0.8916666666666667185, 0.8958333333333333703, 0.9000000000000000222, 0.9041666666666666741, 0.9083333333333333259, 0.9124999999999999778, 0.9166666666666666297, 0.9208333333333332815, 0.9250000000000000444, 0.9291666666666666963, 0.9333333333333333481, 0.9375000000000000000, 0.9416666666666666519, 0.9458333333333333037, 0.9499999999999999556, 0.9541666666666667185, 0.9583333333333333703, 0.9625000000000000222, 0.9666666666666666741, 0.9708333333333333259, 0.9749999999999999778, 0.9791666666666666297, 0.9833333333333332815, 0.9875000000000000444, 0.9916666666666666963, 0.9958333333333333481, 1.000000000000000000 ),
 .UNSPECIFIED. ) 
 GEOMETRIC_REPRESENTATION_ITEM ( )  RATIONAL_B_SPLINE_SURFACE ( (
 ( 1.000000000000000000, 0.9238795325112867385, 1.000000000000000000, 0.9238795325112867385, 1.000000000000000000, 0.9238795325112867385, 1.000000000000000000, 0.9238795325112867385, 1.000000000000000000, 0.9238795325112867385, 1.000000000000000000, 0.9238795325112867385, 1.000000000000000000, 0.9238795325112867385, 1.000000000000000000, 0.9238795325112867385, 1.000000000000000000, 0.9238795325112867385, 1.000000000000000000, 0.9238795325112867385, 1.000000000000000000, 0.9238795325112867385, 1.000000000000000000, 0.9238795325112867385, 1.000000000000000000, 0.9238795325112867385, 1.000000000000000000, 0.9238795325112867385, 1.000000000000000000, 0.9238795325112867385, 1.000000000000000000, 0.9238795325112867385, 1.000000000000000000, 0.9238795325112867385, 1.000000000000000000, 0.9238795325112867385, 1.000000000000000000, 0.9238795325112867385, 1.000000000000000000, 0.9238795325112867385, 1.000000000000000000, 0.9238795325112867385, 1.000000000000000000, 0.9238795325112867385, 1.000000000000000000, 0.9238795325112867385, 1.000000000000000000, 0.9238795325112867385, 1.000000000000000000, 0.9238795325112867385, 1.000000000000000000, 0.9238795325112867385, 1.000000000000000000, 0.9238795325112867385, 1.000000000000000000, 0.9238795325112867385, 1.000000000000000000, 0.9238795325112867385, 1.000000000000000000, 0.9238795325112867385, 1.000000000000000000, 0.9238795325112867385, 1.000000000000000000, 0.9238795325112867385, 1.000000000000000000, 0.9238795325112867385, 1.000000000000000000, 0.9238795325112867385, 1.000000000000000000, 0.9238795325112867385, 1.000000000000000000, 0.9238795325112867385, 1.000000000000000000, 0.9238795325112867385, 1.000000000000000000, 0.9238795325112867385, 1.000000000000000000, 0.9238795325112867385, 1.000000000000000000, 0.9238795325112867385, 1.000000000000000000, 0.9238795325112867385, 1.000000000000000000, 0.9238795325112867385, 1.000000000000000000, 0.9238795325112867385, 1.000000000000000000, 0.9238795325112867385, 1.000000000000000000, 0.9238795325112867385, 1.000000000000000000, 0.9238795325112867385, 1.000000000000000000, 0.9238795325112867385, 1.000000000000000000, 0.9238795325112867385, 1.000000000000000000, 0.9238795325112867385, 1.000000000000000000, 0.9238795325112867385, 1.000000000000000000, 0.9238795325112867385, 1.000000000000000000, 0.9238795325112867385, 1.000000000000000000, 0.9238795325112867385, 1.000000000000000000, 0.9238795325112867385, 1.000000000000000000, 0.9238795325112867385, 1.000000000000000000, 0.9238795325112867385, 1.000000000000000000, 0.9238795325112867385, 1.000000000000000000, 0.9238795325112867385, 1.000000000000000000, 0.9238795325112867385, 1.000000000000000000, 0.9238795325112867385, 1.000000000000000000, 0.9238795325112867385, 1.000000000000000000, 0.9238795325112867385, 1.000000000000000000, 0.9238795325112867385, 1.000000000000000000, 0.9238795325112867385, 1.000000000000000000, 0.9238795325112867385, 1.000000000000000000, 0.9238795325112867385, 1.000000000000000000, 0.9238795325112867385, 1.000000000000000000, 0.9238795325112867385, 1.000000000000000000, 0.9238795325112867385, 1.000000000000000000, 0.9238795325112867385, 1.000000000000000000, 0.9238795325112867385, 1.000000000000000000, 0.9238795325112867385, 1.000000000000000000, 0.9238795325112867385, 1.000000000000000000, 0.9238795325112867385, 1.000000000000000000, 0.9238795325112867385, 1.000000000000000000, 0.9238795325112867385, 1.000000000000000000, 0.9238795325112867385, 1.000000000000000000, 0.9238795325112867385, 1.000000000000000000, 0.9238795325112867385, 1.000000000000000000, 0.9238795325112867385, 1.000000000000000000, 0.9238795325112867385, 1.000000000000000000, 0.9238795325112867385, 1.000000000000000000, 0.9238795325112867385, 1.000000000000000000, 0.9238795325112867385, 1.000000000000000000, 0.9238795325112867385, 1.000000000000000000, 0.9238795325112867385, 1.000000000000000000, 0.9238795325112867385, 1.000000000000000000, 0.9238795325112867385, 1.000000000000000000, 0.9238795325112867385, 1.000000000000000000, 0.9238795325112867385, 1.000000000000000000, 0.9238795325112867385, 1.000000000000000000, 0.9238795325112867385, 1.000000000000000000, 0.9238795325112867385, 1.000000000000000000, 0.9238795325112867385, 1.000000000000000000, 0.9238795325112867385, 1.000000000000000000, 0.9238795325112867385, 1.000000000000000000, 0.9238795325112867385, 1.000000000000000000, 0.9238795325112867385, 1.000000000000000000, 0.9238795325112867385, 1.000000000000000000, 0.9238795325112867385, 1.000000000000000000, 0.9238795325112867385, 1.000000000000000000, 0.9238795325112867385, 1.000000000000000000, 0.9238795325112867385, 1.000000000000000000, 0.9238795325112867385, 1.000000000000000000, 0.9238795325112867385, 1.000000000000000000, 0.9238795325112867385, 1.000000000000000000, 0.9238795325112867385, 1.000000000000000000, 0.9238795325112867385, 1.000000000000000000, 0.9238795325112867385, 1.000000000000000000, 0.9238795325112867385, 1.000000000000000000, 0.9238795325112867385, 1.000000000000000000, 0.9238795325112867385, 1.000000000000000000, 0.9238795325112867385, 1.000000000000000000, 0.9238795325112867385, 1.000000000000000000, 0.9238795325112867385, 1.000000000000000000, 0.9238795325112867385, 1.000000000000000000, 0.9238795325112867385, 1.000000000000000000, 0.9238795325112867385, 1.000000000000000000, 0.9238795325112867385, 1.000000000000000000, 0.9238795325112867385, 1.000000000000000000, 0.9238795325112867385, 1.000000000000000000, 0.9238795325112867385, 1.000000000000000000, 0.9238795325112867385, 1.000000000000000000, 0.9238795325112867385, 1.000000000000000000, 0.9238795325112867385, 1.000000000000000000, 0.9238795325112867385, 1.000000000000000000, 0.9238795325112867385, 1.000000000000000000, 0.9238795325112867385, 1.000000000000000000, 0.9238795325112867385, 1.000000000000000000, 0.9238795325112867385, 1.000000000000000000, 0.9238795325112867385, 1.000000000000000000, 0.9238795325112867385, 1.000000000000000000, 0.9238795325112867385, 1.000000000000000000, 0.9238795325112867385, 1.000000000000000000, 0.9238795325112867385, 1.000000000000000000, 0.9238795325112867385, 1.000000000000000000, 0.9238795325112867385, 1.000000000000000000, 0.9238795325112867385, 1.000000000000000000, 0.9238795325112867385, 1.000000000000000000, 0.9238795325112867385, 1.000000000000000000, 0.9238795325112867385, 1.000000000000000000, 0.9238795325112867385, 1.000000000000000000, 0.9238795325112867385, 1.000000000000000000, 0.9238795325112867385, 1.000000000000000000, 0.9238795325112867385, 1.000000000000000000, 0.9238795325112867385, 1.000000000000000000, 0.9238795325112867385, 1.000000000000000000, 0.9238795325112867385, 1.000000000000000000, 0.9238795325112867385, 1.000000000000000000, 0.9238795325112867385, 1.000000000000000000, 0.9238795325112867385, 1.000000000000000000, 0.9238795325112867385, 1.000000000000000000, 0.9238795325112867385, 1.000000000000000000, 0.9238795325112867385, 1.000000000000000000, 0.9238795325112867385, 1.000000000000000000, 0.9238795325112867385, 1.000000000000000000, 0.9238795325112867385, 1.000000000000000000, 0.9238795325112867385, 1.000000000000000000, 0.9238795325112867385, 1.000000000000000000, 0.9238795325112867385, 1.000000000000000000, 0.9238795325112867385, 1.000000000000000000, 0.9238795325112867385, 1.000000000000000000, 0.9238795325112867385, 1.000000000000000000, 0.9238795325112867385, 1.000000000000000000, 0.9238795325112867385, 1.000000000000000000, 0.9238795325112867385, 1.000000000000000000, 0.9238795325112867385, 1.000000000000000000, 0.9238795325112867385, 1.000000000000000000, 0.9238795325112867385, 1.000000000000000000, 0.9238795325112867385, 1.000000000000000000, 0.9238795325112867385, 1.000000000000000000, 0.9238795325112867385, 1.000000000000000000, 0.9238795325112867385, 1.000000000000000000, 0.9238795325112867385, 1.000000000000000000, 0.9238795325112867385, 1.000000000000000000, 0.9238795325112867385, 1.000000000000000000, 0.9238795325112867385, 1.000000000000000000, 0.9238795325112867385, 1.000000000000000000, 0.9238795325112867385, 1.000000000000000000, 0.9238795325112867385, 1.000000000000000000, 0.9238795325112867385, 1.000000000000000000, 0.9238795325112867385, 1.000000000000000000, 0.9238795325112867385, 1.000000000000000000, 0.9238795325112867385, 1.000000000000000000, 0.9238795325112867385, 1.000000000000000000, 0.9238795325112867385, 1.000000000000000000, 0.9238795325112867385, 1.000000000000000000, 0.9238795325112867385, 1.000000000000000000, 0.9238795325112867385, 1.000000000000000000, 0.9238795325112867385, 1.000000000000000000, 0.9238795325112867385, 1.000000000000000000, 0.9238795325112867385, 1.000000000000000000, 0.9238795325112867385, 1.000000000000000000, 0.9238795325112867385, 1.000000000000000000, 0.9238795325112867385, 1.000000000000000000, 0.9238795325112867385, 1.000000000000000000, 0.9238795325112867385, 1.000000000000000000, 0.9238795325112867385, 1.000000000000000000, 0.9238795325112867385, 1.000000000000000000, 0.9238795325112867385, 1.000000000000000000, 0.9238795325112867385, 1.000000000000000000, 0.9238795325112867385, 1.000000000000000000, 0.9238795325112867385, 1.000000000000000000, 0.9238795325112867385, 1.000000000000000000, 0.9238795325112867385, 1.000000000000000000, 0.9238795325112867385, 1.000000000000000000, 0.9238795325112867385, 1.000000000000000000, 0.9238795325112867385, 1.000000000000000000, 0.9238795325112867385, 1.000000000000000000, 0.9238795325112867385, 1.000000000000000000, 0.9238795325112867385, 1.000000000000000000, 0.9238795325112867385, 1.000000000000000000, 0.9238795325112867385, 1.000000000000000000, 0.9238795325112867385, 1.000000000000000000, 0.9238795325112867385, 1.000000000000000000, 0.9238795325112867385, 1.000000000000000000, 0.9238795325112867385, 1.000000000000000000, 0.9238795325112867385, 1.000000000000000000, 0.9238795325112867385, 1.000000000000000000, 0.9238795325112867385, 1.000000000000000000, 0.9238795325112867385, 1.000000000000000000, 0.9238795325112867385, 1.000000000000000000, 0.9238795325112867385, 1.000000000000000000, 0.9238795325112867385, 1.000000000000000000, 0.9238795325112867385, 1.000000000000000000, 0.9238795325112867385, 1.000000000000000000, 0.9238795325112867385, 1.000000000000000000, 0.9238795325112867385, 1.000000000000000000, 0.9238795325112867385, 1.000000000000000000, 0.9238795325112867385, 1.000000000000000000, 0.9238795325112867385, 1.000000000000000000, 0.9238795325112867385, 1.000000000000000000, 0.9238795325112867385, 1.000000000000000000, 0.9238795325112867385, 1.000000000000000000, 0.9238795325112867385, 1.000000000000000000, 0.9238795325112867385, 1.000000000000000000, 0.9238795325112867385, 1.000000000000000000, 0.9238795325112867385, 1.000000000000000000, 0.9238795325112867385, 1.000000000000000000, 0.9238795325112867385, 1.000000000000000000),
 ( 1.000000000000000000, 0.9238795325112867385, 1.000000000000000000, 0.9238795325112867385, 1.000000000000000000, 0.9238795325112867385, 1.000000000000000000, 0.9238795325112867385, 1.000000000000000000, 0.9238795325112867385, 1.000000000000000000, 0.9238795325112867385, 1.000000000000000000, 0.9238795325112867385, 1.000000000000000000, 0.9238795325112867385, 1.000000000000000000, 0.9238795325112867385, 1.000000000000000000, 0.9238795325112867385, 1.000000000000000000, 0.9238795325112867385, 1.000000000000000000, 0.9238795325112867385, 1.000000000000000000, 0.9238795325112867385, 1.000000000000000000, 0.9238795325112867385, 1.000000000000000000, 0.9238795325112867385, 1.000000000000000000, 0.9238795325112867385, 1.000000000000000000, 0.9238795325112867385, 1.000000000000000000, 0.9238795325112867385, 1.000000000000000000, 0.9238795325112867385, 1.000000000000000000, 0.9238795325112867385, 1.000000000000000000, 0.9238795325112867385, 1.000000000000000000, 0.9238795325112867385, 1.000000000000000000, 0.9238795325112867385, 1.000000000000000000, 0.9238795325112867385, 1.000000000000000000, 0.9238795325112867385, 1.000000000000000000, 0.9238795325112867385, 1.000000000000000000, 0.9238795325112867385, 1.000000000000000000, 0.9238795325112867385, 1.000000000000000000, 0.9238795325112867385, 1.000000000000000000, 0.9238795325112867385, 1.000000000000000000, 0.9238795325112867385, 1.000000000000000000, 0.9238795325112867385, 1.000000000000000000, 0.9238795325112867385, 1.000000000000000000, 0.9238795325112867385, 1.000000000000000000, 0.9238795325112867385, 1.000000000000000000, 0.9238795325112867385, 1.000000000000000000, 0.9238795325112867385, 1.000000000000000000, 0.9238795325112867385, 1.000000000000000000, 0.9238795325112867385, 1.000000000000000000, 0.9238795325112867385, 1.000000000000000000, 0.9238795325112867385, 1.000000000000000000, 0.9238795325112867385, 1.000000000000000000, 0.9238795325112867385, 1.000000000000000000, 0.9238795325112867385, 1.000000000000000000, 0.9238795325112867385, 1.000000000000000000, 0.9238795325112867385, 1.000000000000000000, 0.9238795325112867385, 1.000000000000000000, 0.9238795325112867385, 1.000000000000000000, 0.9238795325112867385, 1.000000000000000000, 0.9238795325112867385, 1.000000000000000000, 0.9238795325112867385, 1.000000000000000000, 0.9238795325112867385, 1.000000000000000000, 0.9238795325112867385, 1.000000000000000000, 0.9238795325112867385, 1.000000000000000000, 0.9238795325112867385, 1.000000000000000000, 0.9238795325112867385, 1.000000000000000000, 0.9238795325112867385, 1.000000000000000000, 0.9238795325112867385, 1.000000000000000000, 0.9238795325112867385, 1.000000000000000000, 0.9238795325112867385, 1.000000000000000000, 0.9238795325112867385, 1.000000000000000000, 0.9238795325112867385, 1.000000000000000000, 0.9238795325112867385, 1.000000000000000000, 0.9238795325112867385, 1.000000000000000000, 0.9238795325112867385, 1.000000000000000000, 0.9238795325112867385, 1.000000000000000000, 0.9238795325112867385, 1.000000000000000000, 0.9238795325112867385, 1.000000000000000000, 0.9238795325112867385, 1.000000000000000000, 0.9238795325112867385, 1.000000000000000000, 0.9238795325112867385, 1.000000000000000000, 0.9238795325112867385, 1.000000000000000000, 0.9238795325112867385, 1.000000000000000000, 0.9238795325112867385, 1.000000000000000000, 0.9238795325112867385, 1.000000000000000000, 0.9238795325112867385, 1.000000000000000000, 0.9238795325112867385, 1.000000000000000000, 0.9238795325112867385, 1.000000000000000000, 0.9238795325112867385, 1.000000000000000000, 0.9238795325112867385, 1.000000000000000000, 0.9238795325112867385, 1.000000000000000000, 0.9238795325112867385, 1.000000000000000000, 0.9238795325112867385, 1.000000000000000000, 0.9238795325112867385, 1.000000000000000000, 0.9238795325112867385, 1.000000000000000000, 0.9238795325112867385, 1.000000000000000000, 0.9238795325112867385, 1.000000000000000000, 0.9238795325112867385, 1.000000000000000000, 0.9238795325112867385, 1.000000000000000000, 0.9238795325112867385, 1.000000000000000000, 0.9238795325112867385, 1.000000000000000000, 0.9238795325112867385, 1.000000000000000000, 0.9238795325112867385, 1.000000000000000000, 0.9238795325112867385, 1.000000000000000000, 0.9238795325112867385, 1.000000000000000000, 0.9238795325112867385, 1.000000000000000000, 0.9238795325112867385, 1.000000000000000000, 0.9238795325112867385, 1.000000000000000000, 0.9238795325112867385, 1.000000000000000000, 0.9238795325112867385, 1.000000000000000000, 0.9238795325112867385, 1.000000000000000000, 0.9238795325112867385, 1.000000000000000000, 0.9238795325112867385, 1.000000000000000000, 0.9238795325112867385, 1.000000000000000000, 0.9238795325112867385, 1.000000000000000000, 0.9238795325112867385, 1.000000000000000000, 0.9238795325112867385, 1.000000000000000000, 0.9238795325112867385, 1.000000000000000000, 0.9238795325112867385, 1.000000000000000000, 0.9238795325112867385, 1.000000000000000000, 0.9238795325112867385, 1.000000000000000000, 0.9238795325112867385, 1.000000000000000000, 0.9238795325112867385, 1.000000000000000000, 0.9238795325112867385, 1.000000000000000000, 0.9238795325112867385, 1.000000000000000000, 0.9238795325112867385, 1.000000000000000000, 0.9238795325112867385, 1.000000000000000000, 0.9238795325112867385, 1.000000000000000000, 0.9238795325112867385, 1.000000000000000000, 0.9238795325112867385, 1.000000000000000000, 0.9238795325112867385, 1.000000000000000000, 0.9238795325112867385, 1.000000000000000000, 0.9238795325112867385, 1.000000000000000000, 0.9238795325112867385, 1.000000000000000000, 0.9238795325112867385, 1.000000000000000000, 0.9238795325112867385, 1.000000000000000000, 0.9238795325112867385, 1.000000000000000000, 0.9238795325112867385, 1.000000000000000000, 0.9238795325112867385, 1.000000000000000000, 0.9238795325112867385, 1.000000000000000000, 0.9238795325112867385, 1.000000000000000000, 0.9238795325112867385, 1.000000000000000000, 0.9238795325112867385, 1.000000000000000000, 0.9238795325112867385, 1.000000000000000000, 0.9238795325112867385, 1.000000000000000000, 0.9238795325112867385, 1.000000000000000000, 0.9238795325112867385, 1.000000000000000000, 0.9238795325112867385, 1.000000000000000000, 0.9238795325112867385, 1.000000000000000000, 0.9238795325112867385, 1.000000000000000000, 0.9238795325112867385, 1.000000000000000000, 0.9238795325112867385, 1.000000000000000000, 0.9238795325112867385, 1.000000000000000000, 0.9238795325112867385, 1.000000000000000000, 0.9238795325112867385, 1.000000000000000000, 0.9238795325112867385, 1.000000000000000000, 0.9238795325112867385, 1.000000000000000000, 0.9238795325112867385, 1.000000000000000000, 0.9238795325112867385, 1.000000000000000000, 0.9238795325112867385, 1.000000000000000000, 0.9238795325112867385, 1.000000000000000000, 0.9238795325112867385, 1.000000000000000000, 0.9238795325112867385, 1.000000000000000000, 0.9238795325112867385, 1.000000000000000000, 0.9238795325112867385, 1.000000000000000000, 0.9238795325112867385, 1.000000000000000000, 0.9238795325112867385, 1.000000000000000000, 0.9238795325112867385, 1.000000000000000000, 0.9238795325112867385, 1.000000000000000000, 0.9238795325112867385, 1.000000000000000000, 0.9238795325112867385, 1.000000000000000000, 0.9238795325112867385, 1.000000000000000000, 0.9238795325112867385, 1.000000000000000000, 0.9238795325112867385, 1.000000000000000000, 0.9238795325112867385, 1.000000000000000000, 0.9238795325112867385, 1.000000000000000000, 0.9238795325112867385, 1.000000000000000000, 0.9238795325112867385, 1.000000000000000000, 0.9238795325112867385, 1.000000000000000000, 0.9238795325112867385, 1.000000000000000000, 0.9238795325112867385, 1.000000000000000000, 0.9238795325112867385, 1.000000000000000000, 0.9238795325112867385, 1.000000000000000000, 0.9238795325112867385, 1.000000000000000000, 0.9238795325112867385, 1.000000000000000000, 0.9238795325112867385, 1.000000000000000000, 0.9238795325112867385, 1.000000000000000000, 0.9238795325112867385, 1.000000000000000000, 0.9238795325112867385, 1.000000000000000000, 0.9238795325112867385, 1.000000000000000000, 0.9238795325112867385, 1.000000000000000000, 0.9238795325112867385, 1.000000000000000000, 0.9238795325112867385, 1.000000000000000000, 0.9238795325112867385, 1.000000000000000000, 0.9238795325112867385, 1.000000000000000000, 0.9238795325112867385, 1.000000000000000000, 0.9238795325112867385, 1.000000000000000000, 0.9238795325112867385, 1.000000000000000000, 0.9238795325112867385, 1.000000000000000000, 0.9238795325112867385, 1.000000000000000000, 0.9238795325112867385, 1.000000000000000000, 0.9238795325112867385, 1.000000000000000000, 0.9238795325112867385, 1.000000000000000000, 0.9238795325112867385, 1.000000000000000000, 0.9238795325112867385, 1.000000000000000000, 0.9238795325112867385, 1.000000000000000000, 0.9238795325112867385, 1.000000000000000000, 0.9238795325112867385, 1.000000000000000000, 0.9238795325112867385, 1.000000000000000000, 0.9238795325112867385, 1.000000000000000000, 0.9238795325112867385, 1.000000000000000000, 0.9238795325112867385, 1.000000000000000000, 0.9238795325112867385, 1.000000000000000000, 0.9238795325112867385, 1.000000000000000000, 0.9238795325112867385, 1.000000000000000000, 0.9238795325112867385, 1.000000000000000000, 0.9238795325112867385, 1.000000000000000000, 0.9238795325112867385, 1.000000000000000000, 0.9238795325112867385, 1.000000000000000000, 0.9238795325112867385, 1.000000000000000000, 0.9238795325112867385, 1.000000000000000000, 0.9238795325112867385, 1.000000000000000000, 0.9238795325112867385, 1.000000000000000000, 0.9238795325112867385, 1.000000000000000000, 0.9238795325112867385, 1.000000000000000000, 0.9238795325112867385, 1.000000000000000000, 0.9238795325112867385, 1.000000000000000000, 0.9238795325112867385, 1.000000000000000000, 0.9238795325112867385, 1.000000000000000000, 0.9238795325112867385, 1.000000000000000000, 0.9238795325112867385, 1.000000000000000000, 0.9238795325112867385, 1.000000000000000000, 0.9238795325112867385, 1.000000000000000000, 0.9238795325112867385, 1.000000000000000000, 0.9238795325112867385, 1.000000000000000000, 0.9238795325112867385, 1.000000000000000000, 0.9238795325112867385, 1.000000000000000000, 0.9238795325112867385, 1.000000000000000000, 0.9238795325112867385, 1.000000000000000000, 0.9238795325112867385, 1.000000000000000000, 0.9238795325112867385, 1.000000000000000000, 0.9238795325112867385, 1.000000000000000000, 0.9238795325112867385, 1.000000000000000000, 0.9238795325112867385, 1.000000000000000000, 0.9238795325112867385, 1.000000000000000000, 0.9238795325112867385, 1.000000000000000000, 0.9238795325112867385, 1.000000000000000000, 0.9238795325112867385, 1.000000000000000000, 0.9238795325112867385, 1.000000000000000000, 0.9238795325112867385, 1.000000000000000000) ) ) 
 REPRESENTATION_ITEM ( '' )  SURFACE ( )  );
#59337 = CARTESIAN_POINT ( 'NONE',  ( 5.000000000000000000, -103.3749999972688158, -6.123233995736766282E-16 ) ) ;
#59338 = EDGE_CURVE ( 'NONE', #55857, #17257, #49998, .T. ) ;
#59339 = CARTESIAN_POINT ( 'NONE',  ( 2.229367062499998831, 11.35416666803225993, -3.861377020970580887 ) ) ;
#59340 = ORIENTED_EDGE ( 'NONE', *, *, #23243, .T. ) ;
#59341 = CARTESIAN_POINT ( 'NONE',  ( 4.458734124999998549, 28.27083333469892779, -2.574251347313721627 ) ) ;
#59342 = CARTESIAN_POINT ( 'NONE',  ( -58.39396692619412477, -153.4375000013656063, 2.891590998281057701 ) ) ;
#59343 = CARTESIAN_POINT ( 'NONE',  ( 2.500000000000002220, 12.45833333606451809, 4.330127018922192761 ) ) ;
#59344 = CARTESIAN_POINT ( 'NONE',  ( 5.000000000000000888, -39.58333333333333570, 2.886751345948126879 ) ) ;
#59345 = CARTESIAN_POINT ( 'NONE',  ( -1.339745962155610925, -102.7946581987385031, 5.000000000000000000 ) ) ;
#59346 = CARTESIAN_POINT ( 'NONE',  ( -3.152548672688508926E-16, -67.56249999863440792, -5.148502694627439702 ) ) ;
#59347 = CARTESIAN_POINT ( 'NONE',  ( 5.174575781541291164, 5.672711317429402378, -7.030005583190089169 ) ) ;
#59348 = CARTESIAN_POINT ( 'NONE',  ( 4.458734124999998549, 18.27083333469893134, -2.574251347313721627 ) ) ;
#59349 = CARTESIAN_POINT ( 'NONE',  ( 5.000000000000000888, -33.58333333333332860, 2.886751345948126879 ) ) ;
#59350 = CARTESIAN_POINT ( 'NONE',  ( 4.458734124999999437, -49.06249999863440792, -5.460374474430324690E-16 ) ) ;
#59351 = CARTESIAN_POINT ( 'NONE',  ( -3.535250795749689387E-16, -7.124999997268813168, -5.773502691896257311 ) ) ;
#59352 = CARTESIAN_POINT ( 'NONE',  ( 3.750000000000005329, 6.495190528383288253, 0.000000000000000000 ) ) ;
#59353 = CARTESIAN_POINT ( 'NONE',  ( -2.499999999999996447, -73.83333333333332860, 4.330127018922195425 ) ) ;
#59354 = CARTESIAN_POINT ( 'NONE',  ( -2.499999999999996447, 11.29166666939785202, 4.330127018922195425 ) ) ;
#59355 = CARTESIAN_POINT ( 'NONE',  ( -2.229367062500000163, -17.72916666530106866, -3.861377020970580443 ) ) ;
#59356 = VERTEX_POINT ( 'NONE', #45816 ) ;
#59357 = CARTESIAN_POINT ( 'NONE',  ( -5.000000000000000888, -169.4375000000000284, 2.071067811865474617 ) ) ;
#59358 = CARTESIAN_POINT ( 'NONE',  ( -4.458734124999998549, -102.2291666653010651, 2.574251347313722516 ) ) ;
#59359 = CARTESIAN_POINT ( 'NONE',  ( -3.535533905932737309, -161.7500000027312126, -3.535533905932738197 ) ) ;
#59360 = CARTESIAN_POINT ( 'NONE',  ( 4.458734125000001214, -97.14583333196773651, 2.574251347313718519 ) ) ;
#59361 = EDGE_CURVE ( 'NONE', #57689, #43948, #56995, .T. ) ;
#59362 = AXIS2_PLACEMENT_3D ( 'NONE', #29391, #49673, #5616 ) ;
#59363 = CARTESIAN_POINT ( 'NONE',  ( 1.339745962155612702, -19.16965819600733312, -5.000000000000000000 ) ) ;
#59364 = CARTESIAN_POINT ( 'NONE',  ( -2.499999999999996447, -56.70833333060214443, 4.330127018922195425 ) ) ;
#59365 = CARTESIAN_POINT ( 'NONE',  ( -6.972266317189433020E-16, -62.12499999726880162, -5.000000000000000000 ) ) ;
#59366 = CARTESIAN_POINT ( 'NONE',  ( -51.60603307380591787, -154.1875000013656063, -2.891590998281053704 ) ) ;
#59367 = CARTESIAN_POINT ( 'NONE',  ( -50.55543936806279248, -142.0625000013656063, 0.3552334253322060320 ) ) ;
#59368 = CARTESIAN_POINT ( 'NONE',  ( -4.458734124999997661, -18.22916666530106866, 2.574251347313722516 ) ) ;
#59369 = CARTESIAN_POINT ( 'NONE',  ( -2.229367062499996610, 8.604166668032261711, 3.861377020970582219 ) ) ;
#59370 = CARTESIAN_POINT ( 'NONE',  ( 4.458734124999999437, -62.06249999863440792, -5.460374474430324690E-16 ) ) ;
#59371 = CYLINDRICAL_SURFACE ( 'NONE', #61365, 5.000000000000000000 ) ;
#59372 = CARTESIAN_POINT ( 'NONE',  ( -4.458734124999999437, -21.39583333196774007, -2.574251347313719407 ) ) ;
#59373 = FACE_OUTER_BOUND ( 'NONE', #52228, .T. ) ;
#59374 = CARTESIAN_POINT ( 'NONE',  ( -5.000000000000000888, -156.4375000000000284, 2.071067811865474617 ) ) ;
#59375 = CARTESIAN_POINT ( 'NONE',  ( -3.535250795749689387E-16, -4.249999999999996447, -5.773502691896257311 ) ) ;
#59376 = CARTESIAN_POINT ( 'NONE',  ( 3.152801135295367541, -157.3125000013656063, -3.152801135295367541 ) ) ;
#59377 = ORIENTED_EDGE ( 'NONE', *, *, #62536, .F. ) ;
#59378 = CARTESIAN_POINT ( 'NONE',  ( -3.152548672688508926E-16, -43.81249999863440081, -5.148502694627439702 ) ) ;
#59379 = CARTESIAN_POINT ( 'NONE',  ( 1.339745962155612702, -44.16965819600732601, -5.000000000000000000 ) ) ;
#59380 = CARTESIAN_POINT ( 'NONE',  ( 1.975475456537005874E-15, -91.62499999726877320, 5.000000000000000000 ) ) ;
#59381 = CARTESIAN_POINT ( 'NONE',  ( 9.457646018065525792E-16, -90.06249999863440792, 5.148502694627439702 ) ) ;
#59382 = CARTESIAN_POINT ( 'NONE',  ( 4.458734124999998549, -89.72916666530106511, -2.574251347313721627 ) ) ;
#59383 = CARTESIAN_POINT ( 'NONE',  ( 4.458734124999998549, 17.02083333469892423, -2.574251347313721627 ) ) ;
#59384 = AXIS2_PLACEMENT_3D ( 'NONE', #35770, #45095, #55714 ) ;
#59385 = CARTESIAN_POINT ( 'NONE',  ( 4.458734124999998549, 7.270833334698928674, -2.574251347313721627 ) ) ;
#59386 = CARTESIAN_POINT ( 'NONE',  ( -1.339745962155613812, -89.08034179853027013, -5.000000000000000000 ) ) ;
#59387 = CARTESIAN_POINT ( 'NONE',  ( 0.000000000000000000, -120.0000000000000000, 0.000000000000000000 ) ) ;
#59388 = DIRECTION ( 'NONE',  ( -0.8660254037844414832, 0.000000000000000000, -0.4999999999999951705 ) ) ;
#59389 = CARTESIAN_POINT ( 'NONE',  ( 2.229367062499998831, 19.10416666803225993, -3.861377020970580887 ) ) ;
#59390 = CARTESIAN_POINT ( 'NONE',  ( -3.535250795749689387E-16, -75.25000000000001421, -5.773502691896257311 ) ) ;
#59391 = CARTESIAN_POINT ( 'NONE',  ( 5.000000000000000888, 7.541666669397851130, 2.886751345948126879 ) ) ;
#59392 = EDGE_LOOP ( 'NONE', ( #47609, #27944, #46534, #40827 ) ) ;
#59393 = CARTESIAN_POINT ( 'NONE',  ( 3.061616997868383141E-16, -161.8750000027311842, -5.000000000000000000 ) ) ;
#59394 = EDGE_LOOP ( 'NONE', ( #50100, #20153, #46049, #25444 ) ) ;
#59395 =( BOUNDED_CURVE ( )  B_SPLINE_CURVE ( 2, ( #26068, #25104, #10941, #44714, #677, #60492, #1011, #60175, #20286 ),
 .UNSPECIFIED., .F., .F. ) 
 B_SPLINE_CURVE_WITH_KNOTS ( ( 3, 2, 2, 2, 3 ),
 ( 0.5482142857142857650, 0.5488095238095238582, 0.5500000000000000444, 0.5511904761904762307, 0.5517857142857143238 ),
 .UNSPECIFIED. ) 
 CURVE ( )  GEOMETRIC_REPRESENTATION_ITEM ( )  RATIONAL_B_SPLINE_CURVE ( ( 0.9330127018922194093, 0.9330127018922194093, 1.000000000000000000, 0.8660254037844387076, 1.000000000000000000, 0.8660254037844387076, 1.000000000000000000, 0.9330127018922194093, 0.9330127018922194093 ) ) 
 REPRESENTATION_ITEM ( '' )  );
#59396 = DIRECTION ( 'NONE',  ( 0.000000000000000000, 0.000000000000000000, 1.000000000000000000 ) ) ;
#59397 = CARTESIAN_POINT ( 'NONE',  ( -4.458734124999998549, -38.22916666530107932, 2.574251347313722516 ) ) ;
#59398 = EDGE_CURVE ( 'NONE', #53636, #1992, #10569, .T. ) ;
#59399 = CARTESIAN_POINT ( 'NONE',  ( 5.000000000000000000, -40.29166666393548013, -2.886751345948129988 ) ) ;
#59400 = EDGE_CURVE ( 'NONE', #60943, #10189, #31014, .T. ) ;
#59401 = ORIENTED_EDGE ( 'NONE', *, *, #12282, .T. ) ;
#59402 = CARTESIAN_POINT ( 'NONE',  ( -54.64476657466781973, -146.0625000013656063, -4.444560631937228834 ) ) ;
#59403 = CARTESIAN_POINT ( 'NONE',  ( -4.458734124999998549, -12.22916666530106866, 2.574251347313722516 ) ) ;
#59405 = ORIENTED_EDGE ( 'NONE', *, *, #45623, .F. ) ;
#59404 = CARTESIAN_POINT ( 'NONE',  ( 9.457646018065525792E-16, -13.31249999863440259, 5.148502694627439702 ) ) ;
#59406 = ADVANCED_FACE ( 'NONE', ( #3037 ), #28091, .T. ) ;
#59407 = CARTESIAN_POINT ( 'NONE',  ( -2.499999999999996447, -79.83333333333332860, 4.330127018922195425 ) ) ;
#59408 = CARTESIAN_POINT ( 'NONE',  ( -1.846868145590737420, -167.7500000013655779, 4.458734124999999437 ) ) ;
#59409 = CARTESIAN_POINT ( 'NONE',  ( 9.457646018065525792E-16, -61.31249999863440792, 5.148502694627439702 ) ) ;
#59410 = VECTOR ( 'NONE', #49488, 1000.000000000000000 ) ;
#59411 = CARTESIAN_POINT ( 'NONE',  ( -2.499999999999996447, -85.70833333060214443, 4.330127018922195425 ) ) ;
#59413 = VERTEX_POINT ( 'NONE', #62525 ) ;
#59412 = CARTESIAN_POINT ( 'NONE',  ( -2.499999999999996447, -48.70833333060213732, 4.330127018922195425 ) ) ;
#59414 = CARTESIAN_POINT ( 'NONE',  ( -50.01589407740564042, -141.6250000000000284, 0.3983568153799778022 ) ) ;
#59415 = VECTOR ( 'NONE', #55847, 1000.000000000000000 ) ;
#59416 = CARTESIAN_POINT ( 'NONE',  ( 4.458734125000001214, -25.14583333196774007, 2.574251347313718519 ) ) ;
#59417 = CYLINDRICAL_SURFACE ( 'NONE', #39150, 5.000000000000000000 ) ;
#59418 = ADVANCED_FACE ( 'NONE', ( #8792 ), #41935, .T. ) ;
#59419 = ORIENTED_EDGE ( 'NONE', *, *, #36683, .F. ) ;
#59420 = CARTESIAN_POINT ( 'NONE',  ( -4.458734124999999437, -163.1875000013655779, -5.460374474430324690E-16 ) ) ;
#59421 = EDGE_CURVE ( 'NONE', #20741, #32024, #18444, .T. ) ;
#59422 = CARTESIAN_POINT ( 'NONE',  ( -3.152548672688508926E-16, -108.8124999986343937, -5.148502694627439702 ) ) ;
#59423 = CARTESIAN_POINT ( 'NONE',  ( -1.339745962155610925, -38.66965819600732601, 5.000000000000000000 ) ) ;
#59424 = VERTEX_POINT ( 'NONE', #62833 ) ;
#59425 = CARTESIAN_POINT ( 'NONE',  ( -53.51423613279429503, -147.5000000013656063, 4.591703134518083651 ) ) ;
#59426 = CARTESIAN_POINT ( 'NONE',  ( 2.229367062499998831, -76.89583333196773651, -3.861377020970580887 ) ) ;
#59427 = CARTESIAN_POINT ( 'NONE',  ( -57.46284108482265651, -134.0625000027312126, 4.819101127000239515 ) ) ;
#59428 = CARTESIAN_POINT ( 'NONE',  ( 2.229367062499998831, -46.64583333196774362, -3.861377020970580887 ) ) ;
#59429 = CARTESIAN_POINT ( 'NONE',  ( 3.152801135295366208, -146.8125000013655779, 3.152801135295367985 ) ) ;
#59430 =( BOUNDED_CURVE ( )  B_SPLINE_CURVE ( 2, ( #10694, #33012, #4363, #23981, #38759, #58398, #33947, #53568, #38154 ),
 .UNSPECIFIED., .F., .F. ) 
 B_SPLINE_CURVE_WITH_KNOTS ( ( 3, 2, 2, 2, 3 ),
 ( 0.9375000000000000000, 0.9380952380952380931, 0.9392857142857142794, 0.9404761904761904656, 0.9410714285714285587 ),
 .UNSPECIFIED. ) 
 CURVE ( )  GEOMETRIC_REPRESENTATION_ITEM ( )  RATIONAL_B_SPLINE_CURVE ( ( 0.9330127018922194093, 0.9330127018922194093, 1.000000000000000000, 0.8660254037844387076, 1.000000000000000000, 0.8660254037844387076, 1.000000000000000000, 0.9330127018922194093, 0.9330127018922194093 ) ) 
 REPRESENTATION_ITEM ( '' )  );
#59431 = EDGE_CURVE ( 'NONE', #50402, #58314, #45896, .T. ) ;
#59432 = LINE ( 'NONE', #34984, #59945 ) ;
#59433 = CARTESIAN_POINT ( 'NONE',  ( -3.152548672688508926E-16, -48.56249999863440792, -5.148502694627439702 ) ) ;
#59434 = CARTESIAN_POINT ( 'NONE',  ( -7.500000000000000000, 4.330127018922191873, -0.9999999999999970024 ) ) ;
#59435 = CARTESIAN_POINT ( 'NONE',  ( -4.458734124999999437, -13.39583333196774184, -2.574251347313719407 ) ) ;
#59436 = CARTESIAN_POINT ( 'NONE',  ( -5.000000000000000000, -101.0000000000000000, 0.000000000000000000 ) ) ;
#59437 = CARTESIAN_POINT ( 'NONE',  ( 3.152801135295366208, -141.8125000013655779, 3.152801135295367985 ) ) ;
#59438 = CARTESIAN_POINT ( 'NONE',  ( 2.229367062500001939, -32.22916666530106511, 3.861377020970579999 ) ) ;
#59439 = CARTESIAN_POINT ( 'NONE',  ( -2.500000000000000444, 7.958333336064518093, -4.330127018922193649 ) ) ;
#59440 = CARTESIAN_POINT ( 'NONE',  ( -2.499999999999996447, -39.70833333060214443, 4.330127018922195425 ) ) ;
#59441 = CARTESIAN_POINT ( 'NONE',  ( -56.48576386720575471, -131.7500000013656063, -4.591703134518078322 ) ) ;
#59442 = CARTESIAN_POINT ( 'NONE',  ( 2.229367062499998831, -75.89583333196773651, -3.861377020970580887 ) ) ;
#59443 = LINE ( 'NONE', #14720, #32236 ) ;
#59444 = CARTESIAN_POINT ( 'NONE',  ( 5.000000000000000888, 14.54166666939785202, 2.886751345948126879 ) ) ;
#59445 = CARTESIAN_POINT ( 'NONE',  ( -4.458734124999999437, 1.437500001365592972, 0.000000000000000000 ) ) ;
#59446 = EDGE_LOOP ( 'NONE', ( #42394, #54614, #49616, #29399, #55366 ) ) ;
#59447 = CARTESIAN_POINT ( 'NONE',  ( 5.000000000000000888, -57.58333333333332860, 2.886751345948126879 ) ) ;
#59449 = CARTESIAN_POINT ( 'NONE',  ( -2.229367062499996610, -35.14583333196772941, 3.861377020970582219 ) ) ;
#59448 = CARTESIAN_POINT ( 'NONE',  ( -2.499999999999996447, -96.83333333333332860, 4.330127018922195425 ) ) ;
#59450 = CARTESIAN_POINT ( 'NONE',  ( -6.972266317189433020E-16, -23.12499999726880873, -5.000000000000000000 ) ) ;
#59451 = CARTESIAN_POINT ( 'NONE',  ( 2.229367062500001939, -79.22916666530106511, 3.861377020970579999 ) ) ;
#59452 = CARTESIAN_POINT ( 'NONE',  ( -2.229367062500000163, 18.27083333469892779, -3.861377020970580443 ) ) ;
#59453 = FACE_OUTER_BOUND ( 'NONE', #56740, .T. ) ;
#59454 = CARTESIAN_POINT ( 'NONE',  ( -50.55543936806279248, -136.0625000013656063, 0.3552334253322060320 ) ) ;
#59455 = CARTESIAN_POINT ( 'NONE',  ( -4.458734124999997661, -1.229166665301071548, 2.574251347313722516 ) ) ;
#59456 = CARTESIAN_POINT ( 'NONE',  ( 2.229367062499998831, 23.10416666803225993, -3.861377020970580887 ) ) ;
#59457 = CARTESIAN_POINT ( 'NONE',  ( -4.458734124999999437, -43.56249999863440081, 0.000000000000000000 ) ) ;
#59458 = CARTESIAN_POINT ( 'NONE',  ( -6.972266317189433020E-16, -15.25000000000000000, -5.000000000000000000 ) ) ;
#59459 = CARTESIAN_POINT ( 'NONE',  ( 4.458734124999999437, -4.812499998634402587, -5.460374474430324690E-16 ) ) ;
#59460 = CARTESIAN_POINT ( 'NONE',  ( 2.229367062500001939, -31.22916666530107221, 3.861377020970579999 ) ) ;
#59461 = AXIS2_PLACEMENT_3D ( 'NONE', #22062, #36216, #60357 ) ;
#59462 = CARTESIAN_POINT ( 'NONE',  ( -59.29741812935640155, -130.8750000013656063, -2.196230717870135685 ) ) ;
#59463 = CARTESIAN_POINT ( 'NONE',  ( -3.152548672688508926E-16, -72.56249999863439371, -5.148502694627439702 ) ) ;
#59464 = CARTESIAN_POINT ( 'NONE',  ( 1.060575238724906964E-15, -105.6249999972688158, 5.773502691896257311 ) ) ;
#59465 = AXIS2_PLACEMENT_3D ( 'NONE', #49351, #4038, #46126 ) ;
#59466 = CARTESIAN_POINT ( 'NONE',  ( 9.457646018065525792E-16, 27.93750000136559208, 5.148502694627439702 ) ) ;
#59467 = CARTESIAN_POINT ( 'NONE',  ( -5.000000000000000000, -65.00000000000000000, 0.000000000000000000 ) ) ;
#59468 = CARTESIAN_POINT ( 'NONE',  ( -59.81910112700025905, -153.3125000027312410, -2.462841084822619209 ) ) ;
#59469 = CARTESIAN_POINT ( 'NONE',  ( 2.229367062499998831, -77.89583333196773651, -3.861377020970580887 ) ) ;
#59470 = CARTESIAN_POINT ( 'NONE',  ( 2.499999999999998668, -61.33333333333333570, -4.330127018922193649 ) ) ;
#59471 = CARTESIAN_POINT ( 'NONE',  ( 1.975475456537005874E-15, -90.62499999726880162, 5.000000000000000000 ) ) ;
#59472 = CARTESIAN_POINT ( 'NONE',  ( 5.000000000000000000, 26.62500000273118772, -6.123233995736766282E-16 ) ) ;
#59473 = ORIENTED_EDGE ( 'NONE', *, *, #48459, .T. ) ;
#59474 = CARTESIAN_POINT ( 'NONE',  ( -1.339745962155613812, -27.20534180126147916, -5.000000000000000000 ) ) ;
#59475 = CARTESIAN_POINT ( 'NONE',  ( 1.339745962155615144, -67.70534180126149693, 4.999999999999999112 ) ) ;
#59476 = CARTESIAN_POINT ( 'NONE',  ( 5.000000000000000888, -17.58333333333333215, 2.886751345948126879 ) ) ;
#59477 = CARTESIAN_POINT ( 'NONE',  ( -4.458734124999999437, -23.39583333196773296, -2.574251347313719407 ) ) ;
#59478 = CARTESIAN_POINT ( 'NONE',  ( 4.458734125000000326, -82.89583333196773651, 2.574251347313718519 ) ) ;
#59479 = AXIS2_PLACEMENT_3D ( 'NONE', #62867, #37789, #18779 ) ;
#59480 = EDGE_CURVE ( 'NONE', #2897, #28777, #61135, .T. ) ;
#59481 = CARTESIAN_POINT ( 'NONE',  ( 5.000000000000000000, -21.37499999726881228, -6.123233995736766282E-16 ) ) ;
#59483 = ORIENTED_EDGE ( 'NONE', *, *, #53972, .T. ) ;
#59482 = CARTESIAN_POINT ( 'NONE',  ( -2.229367062500000163, -51.47916666530107221, -3.861377020970580443 ) ) ;
#59484 = CARTESIAN_POINT ( 'NONE',  ( -5.000000000000000000, -24.08333333333333215, -2.886751345948128211 ) ) ;
#59485 = CARTESIAN_POINT ( 'NONE',  ( 1.339745962155613146, 27.41965820146970145, 5.000000000000000888 ) ) ;
#59487 = ORIENTED_EDGE ( 'NONE', *, *, #56583, .T. ) ;
#59486 = CARTESIAN_POINT ( 'NONE',  ( 4.458734124999998549, 4.020833334698926009, -2.574251347313721627 ) ) ;
#59488 = CARTESIAN_POINT ( 'NONE',  ( -52.80376928212989185, -150.8750000013656063, -4.297418129356378458 ) ) ;
#59489 = CARTESIAN_POINT ( 'NONE',  ( -3.535250795749689387E-16, -65.25000000000000000, -5.773502691896257311 ) ) ;
#59490 = CARTESIAN_POINT ( 'NONE',  ( -1.846868145590734756, -153.3750000013656347, -4.458734125000000326 ) ) ;
#59491 = CARTESIAN_POINT ( 'NONE',  ( -3.152548672688508926E-16, -47.81249999863440792, -5.148502694627439702 ) ) ;
#59492 = CARTESIAN_POINT ( 'NONE',  ( 1.975475456537005874E-15, -76.62499999726880162, 5.000000000000000000 ) ) ;
#59493 = CARTESIAN_POINT ( 'NONE',  ( 2.071067811865476394, -161.1875000000000284, 5.000000000000000000 ) ) ;
#59494 = CARTESIAN_POINT ( 'NONE',  ( 5.275681513340003914E-14, 10.74999999999999645, -5.000000000000000000 ) ) ;
#59495 = CARTESIAN_POINT ( 'NONE',  ( -50.70258187064364108, -128.3750000013656631, 2.196230717870141014 ) ) ;
#59496 = CARTESIAN_POINT ( 'NONE',  ( 4.458734124999998549, -8.979166665301073991, -2.574251347313721627 ) ) ;
#59497 = CARTESIAN_POINT ( 'NONE',  ( -4.458734124999998549, -45.47916666530105800, 2.574251347313722516 ) ) ;
#59498 = CARTESIAN_POINT ( 'NONE',  ( -2.500000000000000444, -8.041666663935481907, -4.330127018922193649 ) ) ;
#59499 = CARTESIAN_POINT ( 'NONE',  ( -4.458734125000001214, -143.8750000013656063, 1.846868145590734089 ) ) ;
#59500 = CARTESIAN_POINT ( 'NONE',  ( 4.458734124999998549, -87.97916666530107932, -2.574251347313721627 ) ) ;
#59501 = CARTESIAN_POINT ( 'NONE',  ( -2.499999999999996447, 21.29166666939785202, 4.330127018922195425 ) ) ;
#59502 = VERTEX_POINT ( 'NONE', #57383 ) ;
#59503 = EDGE_CURVE ( 'NONE', #52308, #26333, #39676, .T. ) ;
#59504 = CARTESIAN_POINT ( 'NONE',  ( -2.499999999999996447, -31.83333333333333215, 4.330127018922195425 ) ) ;
#59505 = CARTESIAN_POINT ( 'NONE',  ( 4.458734124999999437, 28.93750000136559208, -5.460374474430324690E-16 ) ) ;
#59506 = CARTESIAN_POINT ( 'NONE',  ( -49.85088928181150436, -144.6875000027312126, -1.666127454062680702 ) ) ;
#59507 = VECTOR ( 'NONE', #41492, 1000.000000000000000 ) ;
#59508 = ADVANCED_FACE ( 'NONE', ( #27153 ), #7540, .T. ) ;
#59509 = CARTESIAN_POINT ( 'NONE',  ( 2.500000000000002220, -29.54166666393548013, 4.330127018922192761 ) ) ;
#59510 = ORIENTED_EDGE ( 'NONE', *, *, #27609, .T. ) ;
#59511 =( BOUNDED_CURVE ( )  B_SPLINE_CURVE ( 2, ( #13629, #61585, #7549, #62216, #38381, #31982, #62841, #42262, #22976 ),
 .UNSPECIFIED., .F., .F. ) 
 B_SPLINE_CURVE_WITH_KNOTS ( ( 3, 2, 2, 2, 3 ),
 ( 0.1017857142857142849, 0.1023809523809523780, 0.1035714285714285782, 0.1047619047619047644, 0.1053571428571428575 ),
 .UNSPECIFIED. ) 
 CURVE ( )  GEOMETRIC_REPRESENTATION_ITEM ( )  RATIONAL_B_SPLINE_CURVE ( ( 0.9330127018922194093, 0.9330127018922194093, 1.000000000000000000, 0.8660254037844387076, 1.000000000000000000, 0.8660254037844387076, 1.000000000000000000, 0.9330127018922194093, 0.9330127018922194093 ) ) 
 REPRESENTATION_ITEM ( '' )  );
#59512 = CARTESIAN_POINT ( 'NONE',  ( 4.458734124999998549, 5.270833334698926897, -2.574251347313721627 ) ) ;
#59513 = EDGE_CURVE ( 'NONE', #21052, #31318, #9577, .T. ) ;
#59514 = CARTESIAN_POINT ( 'NONE',  ( 2.500000000000002220, -19.66666666666666430, 4.330127018922192761 ) ) ;
#59515 = CARTESIAN_POINT ( 'NONE',  ( -4.458734124999999437, -17.56249999863440792, 0.000000000000000000 ) ) ;
#59516 = CARTESIAN_POINT ( 'NONE',  ( -4.458734124999999437, -5.395833331967740953, -2.574251347313719407 ) ) ;
#59517 = CARTESIAN_POINT ( 'NONE',  ( -4.999999999999998224, -73.79166666393547303, 2.886751345948131764 ) ) ;
#59518 = CARTESIAN_POINT ( 'NONE',  ( 4.458734124999997661, -149.5000000013656063, 1.846868145590737864 ) ) ;
#59519 = CARTESIAN_POINT ( 'NONE',  ( 4.458734124999998549, 13.02083333469892779, -2.574251347313721627 ) ) ;
#59520 = ORIENTED_EDGE ( 'NONE', *, *, #47653, .F. ) ;
#59521 = CARTESIAN_POINT ( 'NONE',  ( -4.458734124999999437, -97.39583333196773651, -2.574251347313719407 ) ) ;
#59522 = LINE ( 'NONE', #31192, #30528 ) ;
#59523 = CARTESIAN_POINT ( 'NONE',  ( 1.339745962155615144, -57.58034179853029144, 4.999999999999999112 ) ) ;
#59524 = CARTESIAN_POINT ( 'NONE',  ( -4.458734124999998549, -16.22916666530107577, 2.574251347313722516 ) ) ;
#59525 = CARTESIAN_POINT ( 'NONE',  ( 2.499999999999998668, -25.20833333060214443, -4.330127018922193649 ) ) ;
#59526 = CARTESIAN_POINT ( 'NONE',  ( -2.499999999999996447, -72.83333333333332860, 4.330127018922195425 ) ) ;
#59527 =( BOUNDED_CURVE ( )  B_SPLINE_CURVE ( 2, ( #21616, #21292, #41209, #46372, #7141, #16781, #56029, #40897, #60543 ),
 .UNSPECIFIED., .F., .F. ) 
 B_SPLINE_CURVE_WITH_KNOTS ( ( 3, 2, 2, 2, 3 ),
 ( 0.2729166666666666963, 0.2736111111111111382, 0.2750000000000000222, 0.2763888888888889062, 0.2770833333333333481 ),
 .UNSPECIFIED. ) 
 CURVE ( )  GEOMETRIC_REPRESENTATION_ITEM ( )  RATIONAL_B_SPLINE_CURVE ( ( 0.9330127018922194093, 0.9330127018922220739, 1.000000000000000000, 0.8660254037844387076, 1.000000000000000000, 0.8660254037844387076, 1.000000000000000000, 0.9330127018922194093, 0.9330127018922194093 ) ) 
 REPRESENTATION_ITEM ( '' )  );
#59528 = CARTESIAN_POINT ( 'NONE',  ( -57.19623071787017210, -148.3750000013656063, 4.297418129356382899 ) ) ;
#59529 = CARTESIAN_POINT ( 'NONE',  ( 1.060575238724906964E-15, -43.62499999726880873, 5.773502691896257311 ) ) ;
#59530 = DIRECTION ( 'NONE',  ( 0.000000000000000000, 0.000000000000000000, 1.000000000000000000 ) ) ;
#59531 = CARTESIAN_POINT ( 'NONE',  ( 2.229367062500001939, 15.02083333469892779, 3.861377020970579999 ) ) ;
#59532 = CARTESIAN_POINT ( 'NONE',  ( 0.000000000000000000, 30.00000000000000000, 0.000000000000000000 ) ) ;
#59533 = CARTESIAN_POINT ( 'NONE',  ( 2.500000000000002220, 9.333333333333332149, 4.330127018922192761 ) ) ;
#59534 = CARTESIAN_POINT ( 'NONE',  ( -4.458734124999997661, 17.77083333469892779, 2.574251347313722516 ) ) ;
#59535 = CARTESIAN_POINT ( 'NONE',  ( 2.229367062499998831, -61.64583333196774362, -3.861377020970580887 ) ) ;
#59536 = EDGE_LOOP ( 'NONE', ( #15648, #19151, #48965, #24279 ) ) ;
#59537 = CARTESIAN_POINT ( 'NONE',  ( -3.152548672688508926E-16, -11.81249999863440969, -5.148502694627439702 ) ) ;
#59538 = CARTESIAN_POINT ( 'NONE',  ( -5.000000000000000000, 5.916666666666666963, -2.886751345948128211 ) ) ;
#59539 = CARTESIAN_POINT ( 'NONE',  ( -3.152801135295367985, -162.8125000013656063, 3.152801135295367096 ) ) ;
#59540 = CARTESIAN_POINT ( 'NONE',  ( 5.000000000000000000, -63.29166666393547303, -2.886751345948130876 ) ) ;
#59541 = CARTESIAN_POINT ( 'NONE',  ( -2.229367062499996610, -56.14583333196773651, 3.861377020970582219 ) ) ;
#59542 = CARTESIAN_POINT ( 'NONE',  ( -4.999999999999999112, -88.79166666393547303, 2.886751345948131764 ) ) ;
#59543 = CARTESIAN_POINT ( 'NONE',  ( 9.457646018065525792E-16, -32.06249999863440792, 5.148502694627439702 ) ) ;
#59544 = CARTESIAN_POINT ( 'NONE',  ( 5.000000000000000000, -38.41666666666667140, -2.886751345948130876 ) ) ;
#59545 = CARTESIAN_POINT ( 'NONE',  ( 3.061616997868383141E-16, -141.8750000027312126, -5.000000000000000000 ) ) ;
#59546 = CARTESIAN_POINT ( 'NONE',  ( -58.24261429053147765, -151.3750000027312126, -3.805975901505573855 ) ) ;
#59547 = CARTESIAN_POINT ( 'NONE',  ( 1.975475456537005874E-15, -48.74999999999999289, 5.000000000000000000 ) ) ;
#59548 = CARTESIAN_POINT ( 'NONE',  ( -8.190561711645485556E-16, -154.9375000013655779, 4.458734124999999437 ) ) ;
#59549 = CARTESIAN_POINT ( 'NONE',  ( -5.000000000000000000, -44.00000000000000000, 0.000000000000000000 ) ) ;
#59550 = CARTESIAN_POINT ( 'NONE',  ( 7.703928834700296768, -4.447865386531944409, -7.917997657324732153 ) ) ;
#59551 = DIRECTION ( 'NONE',  ( 0.000000000000000000, 0.000000000000000000, -1.000000000000000000 ) ) ;
#59552 = ORIENTED_EDGE ( 'NONE', *, *, #33496, .T. ) ;
#59553 = CARTESIAN_POINT ( 'NONE',  ( 2.229367062499998831, -102.6458333319677365, -3.861377020970580887 ) ) ;
#59554 = CARTESIAN_POINT ( 'NONE',  ( 4.458734124999998549, 5.020833334698926897, -2.574251347313721627 ) ) ;
#59555 = COLOUR_RGB ( '',0.8941176470588234615, 0.8941176470588234615, 0.8941176470588234615 ) ;
#59556 = LINE ( 'NONE', #29945, #15521 ) ;
#59557 = CARTESIAN_POINT ( 'NONE',  ( -2.499999999999996447, -4.833333333333335702, 4.330127018922195425 ) ) ;
#59558 = VECTOR ( 'NONE', #19256, 1000.000000000000000 ) ;
#59559 = CARTESIAN_POINT ( 'NONE',  ( -2.229367062500000163, -65.47916666530106511, -3.861377020970580443 ) ) ;
#59560 = EDGE_CURVE ( 'NONE', #11671, #25951, #37131, .T. ) ;
#59561 = CARTESIAN_POINT ( 'NONE',  ( -6.972266317189433020E-16, -26.25000000000000000, -5.000000000000000000 ) ) ;
#59562 = CARTESIAN_POINT ( 'NONE',  ( 1.060575238724906964E-15, -4.624999997268816720, 5.773502691896257311 ) ) ;
#59564 = VERTEX_POINT ( 'NONE', #32288 ) ;
#59563 = CARTESIAN_POINT ( 'NONE',  ( -4.458734124999999437, -34.31249999863440792, 0.000000000000000000 ) ) ;
#59565 = CARTESIAN_POINT ( 'NONE',  ( 2.500000000000002220, -33.66666666666666430, 4.330127018922192761 ) ) ;
#59566 = DIRECTION ( 'NONE',  ( 1.000000000000000000, 0.000000000000000000, 0.000000000000000000 ) ) ;
#59567 = ORIENTED_EDGE ( 'NONE', *, *, #6282, .F. ) ;
#59568 = CARTESIAN_POINT ( 'NONE',  ( 5.000000000000000888, -101.5833333333333286, 2.886751345948126879 ) ) ;
#59569 = CARTESIAN_POINT ( 'NONE',  ( 5.000000000000000000, -50.41666666666666430, -2.886751345948129988 ) ) ;
#59571 = CARTESIAN_POINT ( 'NONE',  ( -2.229367062500000163, -22.72916666530107221, -3.861377020970580443 ) ) ;
#59570 = CARTESIAN_POINT ( 'NONE',  ( 5.000000000000000888, -46.45833333060214443, 2.886751345948126879 ) ) ;
#59572 = CARTESIAN_POINT ( 'NONE',  ( -1.339745962155610925, -41.66965819600731891, 5.000000000000000000 ) ) ;
#59573 = CARTESIAN_POINT ( 'NONE',  ( -3.152548672688508926E-16, -76.56249999863440792, -5.148502694627439702 ) ) ;
#59574 = CARTESIAN_POINT ( 'NONE',  ( -3.152801135295367985, -142.0625000013655779, 3.152801135295367096 ) ) ;
#59575 = CARTESIAN_POINT ( 'NONE',  ( -3.152548672688508926E-16, -79.56249999863440792, -5.148502694627439702 ) ) ;
#59576 = CARTESIAN_POINT ( 'NONE',  ( -52.10840900171896806, -138.4375000013656063, 3.393966926194110556 ) ) ;
#59577 = CARTESIAN_POINT ( 'NONE',  ( -4.458734124999999437, -28.64583333196774007, -2.574251347313719407 ) ) ;
#59578 = CARTESIAN_POINT ( 'NONE',  ( -2.499999999999996447, -69.70833333060214443, 4.330127018922195425 ) ) ;
#59579 = ORIENTED_EDGE ( 'NONE', *, *, #9884, .T. ) ;
#59580 = CARTESIAN_POINT ( 'NONE',  ( 5.000000000000000888, -51.58333333333332149, 2.886751345948126879 ) ) ;
#59581 = VERTEX_POINT ( 'NONE', #57069 ) ;
#59582 = CARTESIAN_POINT ( 'NONE',  ( -3.152548672688508926E-16, -71.81249999863439371, -5.148502694627439702 ) ) ;
#59583 = CARTESIAN_POINT ( 'NONE',  ( 5.000000000000000000, -21.50000000000000000, -6.123233995736766282E-16 ) ) ;
#59584 = VERTEX_POINT ( 'NONE', #47090 ) ;
#59585 = CARTESIAN_POINT ( 'NONE',  ( 5.000000000000000000, 27.50000000000000000, -6.123233995736766282E-16 ) ) ;
#59586 =( BOUNDED_CURVE ( )  B_SPLINE_CURVE ( 2, ( #31781, #13115, #41736, #46262, #22779, #12162, #7355, #36933, #26643 ),
 .UNSPECIFIED., .F., .F. ) 
 B_SPLINE_CURVE_WITH_KNOTS ( ( 3, 2, 2, 2, 3 ),
 ( 0.8437500000000000000, 0.8444444444444444420, 0.8458333333333333259, 0.8472222222222222099, 0.8479166666666666519 ),
 .UNSPECIFIED. ) 
 CURVE ( )  GEOMETRIC_REPRESENTATION_ITEM ( )  RATIONAL_B_SPLINE_CURVE ( ( 0.9330127018922194093, 0.9330127018922194093, 1.000000000000000000, 0.8660254037844387076, 1.000000000000000000, 0.8660254037844387076, 1.000000000000000000, 0.9330127018922194093, 0.9330127018922194093 ) ) 
 REPRESENTATION_ITEM ( '' )  );
#59587 = CARTESIAN_POINT ( 'NONE',  ( 1.339745962155661996, -12.29465819873852084, -4.999999999999970690 ) ) ;
#59588 = CARTESIAN_POINT ( 'NONE',  ( -4.458734124999999437, -58.56249999863440081, 0.000000000000000000 ) ) ;
#59589 = CARTESIAN_POINT ( 'NONE',  ( -2.229367062499996610, -6.395833331967741842, 3.861377020970582219 ) ) ;
#59590 = EDGE_LOOP ( 'NONE', ( #27039, #24319, #44880, #37221 ) ) ;
#59591 = LINE ( 'NONE', #5870, #40898 ) ;
#59592 = CARTESIAN_POINT ( 'NONE',  ( -6.972266317189433020E-16, -45.24999999999999289, -5.000000000000000000 ) ) ;
#59593 = CARTESIAN_POINT ( 'NONE',  ( 4.458734125000001214, 15.10416666803225993, 2.574251347313718519 ) ) ;
#59594 = CARTESIAN_POINT ( 'NONE',  ( -57.19623071787017210, -141.3750000013656063, 4.297418129356382899 ) ) ;
#59595 = CARTESIAN_POINT ( 'NONE',  ( 1.339745962155615144, -47.58034179853029144, 4.999999999999999112 ) ) ;
#59596 = CARTESIAN_POINT ( 'NONE',  ( -1.846868145590737420, -161.7500000013655779, 4.458734124999997661 ) ) ;
#59597 = CARTESIAN_POINT ( 'NONE',  ( 6.123233995736766282E-16, -170.0000000000000000, -5.000000000000000000 ) ) ;
#59598 = ORIENTED_EDGE ( 'NONE', *, *, #5172, .F. ) ;
#59599 = CARTESIAN_POINT ( 'NONE',  ( 4.458734125000000326, -80.89583333196773651, 2.574251347313718519 ) ) ;
#59600 = CYLINDRICAL_SURFACE ( 'NONE', #13091, 5.000000000000000000 ) ;
#59601 = CARTESIAN_POINT ( 'NONE',  ( -4.458734124999999437, 4.604166668032261711, -2.574251347313719407 ) ) ;
#59602 = AXIS2_PLACEMENT_3D ( 'NONE', #22775, #62010, #13735 ) ;
#59603 = CARTESIAN_POINT ( 'NONE',  ( 0.000000000000000000, -120.0000000000000000, 0.000000000000000000 ) ) ;
#59604 = CARTESIAN_POINT ( 'NONE',  ( -4.999999999999999112, -84.91666666666667140, 2.886751345948131764 ) ) ;
#59605 = CARTESIAN_POINT ( 'NONE',  ( -7.500000000000000000, -2.886751345948133984, -7.198902722707428481 ) ) ;
#59606 = CARTESIAN_POINT ( 'NONE',  ( -4.458734124999999437, -67.64583333196773651, -2.574251347313719407 ) ) ;
#59607 = CARTESIAN_POINT ( 'NONE',  ( 2.500000000000002220, -26.54166666393547658, 4.330127018922192761 ) ) ;
#59608 = CARTESIAN_POINT ( 'NONE',  ( -4.999999999999998224, -20.91666666666666785, 2.886751345948131764 ) ) ;
#59609 = CARTESIAN_POINT ( 'NONE',  ( -4.999999999999998224, -40.91666666666667140, 2.886751345948131764 ) ) ;
#59610 = CARTESIAN_POINT ( 'NONE',  ( 5.000000000000000000, -110.2916666639354730, -2.886751345948130876 ) ) ;
#59611 = CARTESIAN_POINT ( 'NONE',  ( 4.458734125000001214, -46.89583333196773651, 2.574251347313718519 ) ) ;
#59612 = CARTESIAN_POINT ( 'NONE',  ( -3.152548672688508926E-16, -32.81249999863440792, -5.148502694627439702 ) ) ;
#59613 = CARTESIAN_POINT ( 'NONE',  ( 9.457646018065525792E-16, 9.687500001365593860, 5.148502694627439702 ) ) ;
#59614 = CARTESIAN_POINT ( 'NONE',  ( 3.061616997868383141E-16, -161.8750000027311842, -5.000000000000000000 ) ) ;
#59615 = CARTESIAN_POINT ( 'NONE',  ( 2.500000000000002220, 21.33333333333333215, 4.330127018922192761 ) ) ;
#59616 = CARTESIAN_POINT ( 'NONE',  ( 2.071067811865475505, -143.9375000027311842, -5.000000000000000888 ) ) ;
#59617 = CARTESIAN_POINT ( 'NONE',  ( 0.000000000000000000, -170.0000000000000000, 0.000000000000000000 ) ) ;
#59618 = EDGE_CURVE ( 'NONE', #45305, #37025, #13029, .T. ) ;
#59619 = CARTESIAN_POINT ( 'NONE',  ( 4.458734125000001214, -38.89583333196773651, 2.574251347313718519 ) ) ;
#59620 = CARTESIAN_POINT ( 'NONE',  ( -3.535250795749689387E-16, -74.12499999726880162, -5.773502691896257311 ) ) ;
#59621 = CARTESIAN_POINT ( 'NONE',  ( -53.51423613279429503, -145.5000000013656063, 4.591703134518082763 ) ) ;
#59622 = CARTESIAN_POINT ( 'NONE',  ( 5.000000000000000000, -140.0000000000000000, 0.000000000000000000 ) ) ;
#59623 = CARTESIAN_POINT ( 'NONE',  ( 5.000000000000000000, -141.1250000027312126, 0.000000000000000000 ) ) ;
#59624 = CARTESIAN_POINT ( 'NONE',  ( -4.458734124999999437, -80.64583333196773651, -2.574251347313719407 ) ) ;
#59625 = CARTESIAN_POINT ( 'NONE',  ( 4.458734124999999437, -164.6875000013655779, 0.000000000000000000 ) ) ;
#59626 = CARTESIAN_POINT ( 'NONE',  ( -1.339745962155613812, -33.20534180126147561, -5.000000000000000000 ) ) ;
#59627 = CARTESIAN_POINT ( 'NONE',  ( -4.999999999999999112, -27.91666666666666430, 2.886751345948131764 ) ) ;
#59628 = CARTESIAN_POINT ( 'NONE',  ( 3.152801135295366208, -145.5625000013655779, 3.152801135295367985 ) ) ;
#59629 = ORIENTED_EDGE ( 'NONE', *, *, #50683, .F. ) ;
#59630 = CARTESIAN_POINT ( 'NONE',  ( -2.229367062500000163, 22.27083333469892423, -3.861377020970580443 ) ) ;
#59631 = VERTEX_POINT ( 'NONE', #29660 ) ;
#59632 = CARTESIAN_POINT ( 'NONE',  ( -4.458734124999999437, -61.64583333196774362, -2.574251347313719407 ) ) ;
#59633 = CARTESIAN_POINT ( 'NONE',  ( 1.060575238724906964E-15, 19.37500000273118772, 5.773502691896257311 ) ) ;
#59634 =( BOUNDED_CURVE ( )  B_SPLINE_CURVE ( 2, ( #35634, #59123, #20201, #11502, #5726, #44633, #39803, #35314, #924 ),
 .UNSPECIFIED., .F., .F. ) 
 B_SPLINE_CURVE_WITH_KNOTS ( ( 3, 2, 2, 2, 3 ),
 ( 0.08750000000000000833, 0.08809523809523810145, 0.08928571428571428770, 0.09047619047619047394, 0.09107142857142856707 ),
 .UNSPECIFIED. ) 
 CURVE ( )  GEOMETRIC_REPRESENTATION_ITEM ( )  RATIONAL_B_SPLINE_CURVE ( ( 0.9330127018922192983, 0.9330127018922200755, 1.000000000000000000, 0.8660254037844387076, 1.000000000000000000, 0.8660254037844387076, 1.000000000000000000, 0.9330127018922194093, 0.9330127018922194093 ) ) 
 REPRESENTATION_ITEM ( '' )  );
#59635 = CARTESIAN_POINT ( 'NONE',  ( 1.975475456537005874E-15, 2.249999999999999556, 5.000000000000000000 ) ) ;
#59636 = CARTESIAN_POINT ( 'NONE',  ( -5.000000000000000000, 13.91666666666666785, -2.886751345948128211 ) ) ;
#59637 = CARTESIAN_POINT ( 'NONE',  ( -2.229367062500000163, -49.47916666530107221, -3.861377020970580443 ) ) ;
#59638 = CARTESIAN_POINT ( 'NONE',  ( 9.457646018065525792E-16, -12.06249999863440081, 5.148502694627439702 ) ) ;
#59639 = DIRECTION ( 'NONE',  ( -0.000000000000000000, 1.000000000000000000, -0.000000000000000000 ) ) ;
#59640 = CARTESIAN_POINT ( 'NONE',  ( -1.339745962155610925, -63.66965819600734022, 5.000000000000000000 ) ) ;
#59641 = DIRECTION ( 'NONE',  ( 0.000000000000000000, 0.000000000000000000, 1.000000000000000000 ) ) ;
#59642 = CARTESIAN_POINT ( 'NONE',  ( 1.975475456537005874E-15, -74.62499999726880162, 5.000000000000000000 ) ) ;
#59643 = CARTESIAN_POINT ( 'NONE',  ( -6.972266317189433020E-16, -74.25000000000000000, -5.000000000000000000 ) ) ;
#59644=STYLED_ITEM('',(#63698),#29015);
#59646 = CARTESIAN_POINT ( 'NONE',  ( 4.458734124999999437, -22.81249999863440436, -5.460374474430324690E-16 ) ) ;
#59645 = CARTESIAN_POINT ( 'NONE',  ( -2.500000000000000444, -59.16666666666665719, -4.330127018922193649 ) ) ;
#59647 = CARTESIAN_POINT ( 'NONE',  ( 6.123233995736766282E-16, -120.0000000000000000, -5.000000000000000000 ) ) ;
#59648 = CARTESIAN_POINT ( 'NONE',  ( 4.458734124999999437, -54.81249999863440081, -5.460374474430324690E-16 ) ) ;
#59649 = CARTESIAN_POINT ( 'NONE',  ( -3.152801135295367985, -157.0625000013656063, 3.152801135295367096 ) ) ;
#59650 = AXIS2_PLACEMENT_3D ( 'NONE', #2665, #22286, #41885 ) ;
#59651 = CARTESIAN_POINT ( 'NONE',  ( 5.000000000000000000, -55.37499999726880162, -6.123233995736766282E-16 ) ) ;
#59652 = EDGE_LOOP ( 'NONE', ( #31569, #37431, #7292, #63497 ) ) ;
#59653 = CARTESIAN_POINT ( 'NONE',  ( -50.01589407740564042, -137.6250000000000284, 0.3983568153799778022 ) ) ;
#59654 = CARTESIAN_POINT ( 'NONE',  ( 4.458734124999999437, -3.062499998634407472, -5.460374474430324690E-16 ) ) ;
#59655 = EDGE_LOOP ( 'NONE', ( #44299, #16141, #1764, #17642, #655, #26754 ) ) ;
#59657 = CARTESIAN_POINT ( 'NONE',  ( -1.339745962155610925, -28.79465819873852084, 5.000000000000000000 ) ) ;
#59656 = CARTESIAN_POINT ( 'NONE',  ( -58.24261429053147765, -141.2500000000000284, -3.805975901505573855 ) ) ;
#59658 = CARTESIAN_POINT ( 'NONE',  ( -8.190561711645485556E-16, -157.6875000013655779, 4.458734124999999437 ) ) ;
#59659 = VERTEX_POINT ( 'NONE', #34168 ) ;
#59660 = CARTESIAN_POINT ( 'NONE',  ( 1.339745962155609149, 25.29465819873851729, 5.000000000000003553 ) ) ;
#59661 = CARTESIAN_POINT ( 'NONE',  ( -52.53715891517739323, -131.4375000000000284, -4.819101127000233298 ) ) ;
#59662 = CARTESIAN_POINT ( 'NONE',  ( 5.000000000000000000, -80.37499999726881583, -6.123233995736766282E-16 ) ) ;
#59663 = CARTESIAN_POINT ( 'NONE',  ( -2.229367062499996610, -44.39583333196774362, 3.861377020970582219 ) ) ;
#59664 = VERTEX_POINT ( 'NONE', #33551 ) ;
#59665 = CARTESIAN_POINT ( 'NONE',  ( -6.972266317189433020E-16, -103.1249999972688158, -5.000000000000000000 ) ) ;
#59666 = CARTESIAN_POINT ( 'NONE',  ( -2.229367062500000163, 15.52083333469892779, -3.861377020970580443 ) ) ;
#59667 = CARTESIAN_POINT ( 'NONE',  ( 4.458734125000001214, -90.14583333196773651, 2.574251347313718519 ) ) ;
#59668 = CARTESIAN_POINT ( 'NONE',  ( -53.51423613279429503, -153.2500000013655779, 4.591703134518082763 ) ) ;
#59669 = DIRECTION ( 'NONE',  ( -0.000000000000000000, 1.000000000000000000, -0.000000000000000000 ) ) ;
#59670 = CARTESIAN_POINT ( 'NONE',  ( 5.000000000000000000, -25.50000000000000355, -6.123233995736766282E-16 ) ) ;
#59671 = LINE ( 'NONE', #15602, #15806 ) ;
#59672 = CARTESIAN_POINT ( 'NONE',  ( -2.229367062499996610, -67.14583333196773651, 3.861377020970582219 ) ) ;
#59673 = CARTESIAN_POINT ( 'NONE',  ( -60.14911071818854538, -146.0624999999999716, 1.666127454062681146 ) ) ;
#59674 = CARTESIAN_POINT ( 'NONE',  ( -4.458734124999999437, 16.60416666803225993, -2.574251347313719407 ) ) ;
#59675 = CARTESIAN_POINT ( 'NONE',  ( -1.339745962155610925, -26.79465819873852084, 5.000000000000000000 ) ) ;
#59676 = CARTESIAN_POINT ( 'NONE',  ( -4.458734124999998549, -48.47916666530106511, 2.574251347313722516 ) ) ;
#59677 = CARTESIAN_POINT ( 'NONE',  ( -2.500000000000000444, -7.041666663935481907, -4.330127018922193649 ) ) ;
#59678 = CARTESIAN_POINT ( 'NONE',  ( 5.000000000000000000, -25.37499999726881583, -6.123233995736766282E-16 ) ) ;
#59679 = DIRECTION ( 'NONE',  ( -0.000000000000000000, 1.000000000000000000, -0.000000000000000000 ) ) ;
#59680 = CARTESIAN_POINT ( 'NONE',  ( 2.229367062500001939, -89.22916666530106511, 3.861377020970579999 ) ) ;
#59681 = DIRECTION ( 'NONE',  ( 0.000000000000000000, 0.000000000000000000, 1.000000000000000000 ) ) ;
#59682 = CARTESIAN_POINT ( 'NONE',  ( 2.229367062500001939, -18.22916666530106866, 3.861377020970579999 ) ) ;
#59683 = ORIENTED_EDGE ( 'NONE', *, *, #29997, .T. ) ;
#59684 = CARTESIAN_POINT ( 'NONE',  ( -5.000000000000000000, -143.6250000027312126, -6.123233995736766282E-16 ) ) ;
#59685 = CARTESIAN_POINT ( 'NONE',  ( -3.152548672688508926E-16, -104.5624999986343937, -5.148502694627439702 ) ) ;
#59686 = CARTESIAN_POINT ( 'NONE',  ( 2.071067811865476394, -161.3125000027312126, 5.000000000000000000 ) ) ;
#59687 = ORIENTED_EDGE ( 'NONE', *, *, #54250, .F. ) ;
#59688 = CARTESIAN_POINT ( 'NONE',  ( 2.229367062499998831, -95.89583333196773651, -3.861377020970580887 ) ) ;
#59689 = AXIS2_PLACEMENT_3D ( 'NONE', #7584, #18170, #42613 ) ;
#59690 = EDGE_CURVE ( 'NONE', #44836, #13136, #24850, .T. ) ;
#59691 = LINE ( 'NONE', #512, #25346 ) ;
#59692 = CARTESIAN_POINT ( 'NONE',  ( 5.000000000000000000, -58.29166666393548724, -2.886751345948129988 ) ) ;
#59693 = CARTESIAN_POINT ( 'NONE',  ( 2.500000000000002220, -62.54166666393547303, 4.330127018922192761 ) ) ;
#59694 = CARTESIAN_POINT ( 'NONE',  ( -59.59170313451811296, -126.5000000013656063, 1.485763867205729394 ) ) ;
#59695 = CARTESIAN_POINT ( 'NONE',  ( -55.35523342533222291, -143.3125000013656063, 4.444560631937231499 ) ) ;
#59696 = CARTESIAN_POINT ( 'NONE',  ( -2.229367062499996610, -16.14583333196773651, 3.861377020970582219 ) ) ;
#59697 = CARTESIAN_POINT ( 'NONE',  ( -2.229367062499996610, 5.604166668032261711, 3.861377020970582219 ) ) ;
#59698 = CARTESIAN_POINT ( 'NONE',  ( -3.152548672688508926E-16, -61.81249999863440081, -5.148502694627439702 ) ) ;
#59699 = CARTESIAN_POINT ( 'NONE',  ( -4.458734124999997661, -22.22916666530107221, 2.574251347313722516 ) ) ;
#59700 = DIRECTION ( 'NONE',  ( 0.000000000000000000, -1.000000000000000000, 0.000000000000000000 ) ) ;
#59701 = CARTESIAN_POINT ( 'NONE',  ( 5.000000000000000000, -156.0000000000000000, 0.000000000000000000 ) ) ;
#59702 = CARTESIAN_POINT ( 'NONE',  ( 5.000000000000000888, -9.583333333333333925, 2.886751345948126879 ) ) ;
#59703 = CARTESIAN_POINT ( 'NONE',  ( 1.846868145590736310, -155.6250000013656063, 4.458734124999999437 ) ) ;
#59704 = VERTEX_POINT ( 'NONE', #14239 ) ;
#59705 = CARTESIAN_POINT ( 'NONE',  ( 4.458734124999999437, -45.06249999863440081, -5.460374474430324690E-16 ) ) ;
#59706 = DIRECTION ( 'NONE',  ( 0.000000000000000000, 0.000000000000000000, 1.000000000000000000 ) ) ;
#59707 = DIRECTION ( 'NONE',  ( -0.000000000000000000, 1.000000000000000000, -0.000000000000000000 ) ) ;
#59708 = CARTESIAN_POINT ( 'NONE',  ( -4.458734124999999437, -88.31249999863439371, 0.000000000000000000 ) ) ;
#59709 =( BOUNDED_CURVE ( )  B_SPLINE_CURVE ( 2, ( #35629, #55257, #44958, #919, #16005, #15689, #59118, #25661, #10855 ),
 .UNSPECIFIED., .F., .F. ) 
 B_SPLINE_CURVE_WITH_KNOTS ( ( 3, 2, 2, 2, 3 ),
 ( 0.1083333333333334203, 0.1125000000000000999, 0.1166666666666667657, 0.1208333333333334314, 0.1250000000000001110 ),
 .UNSPECIFIED. ) 
 CURVE ( )  GEOMETRIC_REPRESENTATION_ITEM ( )  RATIONAL_B_SPLINE_CURVE ( ( 0.9999999999999984457, 0.9238795325112882928, 1.000000000000000000, 0.9238795325112867385, 1.000000000000000000, 0.9238795325112867385, 1.000000000000000000, 0.9238795325112847401, 1.000000000000001998 ) ) 
 REPRESENTATION_ITEM ( '' )  );
#59710 = CARTESIAN_POINT ( 'NONE',  ( -2.229367062500000163, 4.520833334698926897, -3.861377020970580443 ) ) ;
#59711 = ADVANCED_FACE ( 'NONE', ( #14865 ), #19058, .T. ) ;
#59712 = CYLINDRICAL_SURFACE ( 'NONE', #31864, 5.000000000000000000 ) ;
#59713 = ADVANCED_FACE ( 'NONE', ( #4910 ), #54107, .T. ) ;
#59714 = CARTESIAN_POINT ( 'NONE',  ( 5.000000000000000000, 13.58333333333333215, -2.886751345948130876 ) ) ;
#59715 = CARTESIAN_POINT ( 'NONE',  ( -9.184850993605147944E-16, -152.3750000027311842, 5.000000000000000000 ) ) ;
#59716 = CARTESIAN_POINT ( 'NONE',  ( 4.458734124999998549, 22.02083333469892779, -2.574251347313721627 ) ) ;
#59717 = CARTESIAN_POINT ( 'NONE',  ( 2.499999999999998668, -77.33333333333334281, -4.330127018922193649 ) ) ;
#59718 = CARTESIAN_POINT ( 'NONE',  ( 2.499999999999998668, 8.791666669397853795, -4.330127018922193649 ) ) ;
#59719 = EDGE_LOOP ( 'NONE', ( #212, #52682, #41217, #49034 ) ) ;
#59720 = CARTESIAN_POINT ( 'NONE',  ( 1.339745962155615144, -80.58034179853028434, 4.999999999999999112 ) ) ;
#59721 = ORIENTED_EDGE ( 'NONE', *, *, #56752, .T. ) ;
#59722 = CARTESIAN_POINT ( 'NONE',  ( 0.000000000000000000, -120.0000000000000000, 5.000000000000000000 ) ) ;
#59723 = CARTESIAN_POINT ( 'NONE',  ( 4.458734124999998549, -36.72916666530107221, -2.574251347313721627 ) ) ;
#59724 = EDGE_CURVE ( 'NONE', #56134, #29294, #28604, .T. ) ;
#59725 = CARTESIAN_POINT ( 'NONE',  ( -5.000000000000000000, -38.95833333060214443, -2.886751345948128211 ) ) ;
#59726 = ORIENTED_EDGE ( 'NONE', *, *, #1696, .T. ) ;
#59727 = CARTESIAN_POINT ( 'NONE',  ( 4.458734125000001214, -12.89583333196774184, 2.574251347313718519 ) ) ;
#59729 = ORIENTED_EDGE ( 'NONE', *, *, #56317, .T. ) ;
#59728 = CARTESIAN_POINT ( 'NONE',  ( -4.458734124999999437, -21.56249999863440436, 0.000000000000000000 ) ) ;
#59730 = CARTESIAN_POINT ( 'NONE',  ( -3.535250795749689387E-16, -80.25000000000000000, -5.773502691896257311 ) ) ;
#59731 = CARTESIAN_POINT ( 'NONE',  ( -6.972266317189433020E-16, -46.12499999726880873, -5.000000000000000000 ) ) ;
#59732 = CARTESIAN_POINT ( 'NONE',  ( 4.458734124999999437, -62.06249999863440792, -5.460374474430324690E-16 ) ) ;
#59733 = CARTESIAN_POINT ( 'NONE',  ( -3.535250795749689387E-16, -86.12499999726880162, -5.773502691896257311 ) ) ;
#59735 = EDGE_LOOP ( 'NONE', ( #41660, #5699, #9251, #25542 ) ) ;
#59734 = CARTESIAN_POINT ( 'NONE',  ( -6.972266317189433020E-16, -32.24999999999999289, -5.000000000000000000 ) ) ;
#59736 = AXIS2_PLACEMENT_3D ( 'NONE', #43096, #53697, #63363 ) ;
#59737 = CARTESIAN_POINT ( 'NONE',  ( -59.98410592259440222, -143.1250000000000284, -0.3983568153799752487 ) ) ;
#59738 = CARTESIAN_POINT ( 'NONE',  ( -3.152548672688508926E-16, -25.81249999863440792, -5.148502694627439702 ) ) ;
#59739 = DIRECTION ( 'NONE',  ( 0.000000000000000000, 0.000000000000000000, 1.000000000000000000 ) ) ;
#59740 = ORIENTED_EDGE ( 'NONE', *, *, #62196, .F. ) ;
#59741 = PRODUCT_CONTEXT ( 'NONE', #23256, 'mechanical' ) ;
#59742 = CARTESIAN_POINT ( 'NONE',  ( -3.152801135295367985, -163.0625000013656063, 3.152801135295367096 ) ) ;
#59743 = EDGE_CURVE ( 'NONE', #28871, #55230, #52483, .T. ) ;
#59744 = CARTESIAN_POINT ( 'NONE',  ( -2.229367062499996610, 28.85416666803226349, 3.861377020970582219 ) ) ;
#59745 = CARTESIAN_POINT ( 'NONE',  ( 3.535533905932738197, -155.8750000000000000, -3.535533905932738197 ) ) ;
#59746 = ORIENTED_EDGE ( 'NONE', *, *, #38485, .F. ) ;
#59747 = CARTESIAN_POINT ( 'NONE',  ( -59.29741812935640155, -147.8750000013655779, -2.196230717870135685 ) ) ;
#59748 = CARTESIAN_POINT ( 'NONE',  ( 2.229367062499998831, -74.89583333196773651, -3.861377020970580887 ) ) ;
#59749 = CARTESIAN_POINT ( 'NONE',  ( -59.98410592259440222, -133.2500000027312126, -0.3983568153799752487 ) ) ;
#59750 = CARTESIAN_POINT ( 'NONE',  ( -4.458734124999997661, -43.22916666530106511, 2.574251347313722516 ) ) ;
#59751 = CARTESIAN_POINT ( 'NONE',  ( 3.152801135295367541, -140.5625000013655779, -3.152801135295367541 ) ) ;
#59752 = CARTESIAN_POINT ( 'NONE',  ( 6.123233995736766282E-16, -120.0000000000000000, -5.000000000000000000 ) ) ;
#59753 = CARTESIAN_POINT ( 'NONE',  ( -2.229367062499996610, -51.14583333196772941, 3.861377020970582219 ) ) ;
#59754 = LINE ( 'NONE', #40431, #60440 ) ;
#59755 = CARTESIAN_POINT ( 'NONE',  ( -4.458734124999998549, -17.22916666530106866, 2.574251347313722516 ) ) ;
#59756 = CARTESIAN_POINT ( 'NONE',  ( -2.500000000000000444, -103.1666666666666572, -4.330127018922193649 ) ) ;
#59757 = CARTESIAN_POINT ( 'NONE',  ( -4.458734124999999437, -140.1875000013656063, -5.460374474430324690E-16 ) ) ;
#59758 = CARTESIAN_POINT ( 'NONE',  ( 4.458734124999999437, -31.06249999863440436, -5.460374474430324690E-16 ) ) ;
#59759 = CARTESIAN_POINT ( 'NONE',  ( -5.000000000000000000, 7.125000002731185944, 0.000000000000000000 ) ) ;
#59760 = DIRECTION ( 'NONE',  ( 0.000000000000000000, -0.000000000000000000, 1.000000000000000000 ) ) ;
#59761 = CARTESIAN_POINT ( 'NONE',  ( -51.60603307380591787, -129.9375000013656063, -2.891590998281053704 ) ) ;
#59762 = CARTESIAN_POINT ( 'NONE',  ( -4.458734124999998549, -74.47916666530106511, 2.574251347313722516 ) ) ;
#59763 = FACE_OUTER_BOUND ( 'NONE', #39371, .T. ) ;
#59764 = CARTESIAN_POINT ( 'NONE',  ( -5.000000000000000888, -139.5625000027312126, 2.071067811865474617 ) ) ;
#59765 = CARTESIAN_POINT ( 'NONE',  ( -9.184850993605147944E-16, -165.2500000000000000, 5.000000000000000000 ) ) ;
#59766 = CARTESIAN_POINT ( 'NONE',  ( 4.458734124999998549, 2.020833334698927786, -2.574251347313721627 ) ) ;
#59767 = ORIENTED_EDGE ( 'NONE', *, *, #4629, .F. ) ;
#59768 = CARTESIAN_POINT ( 'NONE',  ( 5.000000000000000888, -30.58333333333333215, 2.886751345948126879 ) ) ;
#59769 = DIRECTION ( 'NONE',  ( 0.000000000000000000, 1.000000000000000000, 0.000000000000000000 ) ) ;
#59771 = CARTESIAN_POINT ( 'NONE',  ( -2.229367062499996610, -37.14583333196773651, 3.861377020970582219 ) ) ;
#59770 = CARTESIAN_POINT ( 'NONE',  ( -4.458734124999998549, -87.22916666530107932, 2.574251347313722516 ) ) ;
#59772 = CARTESIAN_POINT ( 'NONE',  ( 2.499999999999998668, -9.333333333333332149, -4.330127018922193649 ) ) ;
#59773 = CARTESIAN_POINT ( 'NONE',  ( 4.458734124999999437, -80.06249999863440792, -5.460374474430324690E-16 ) ) ;
#59774 = EDGE_CURVE ( 'NONE', #55214, #16469, #10369, .T. ) ;
#59775 = CARTESIAN_POINT ( 'NONE',  ( 4.458734124999999437, 15.93750000136559564, -5.460374474430324690E-16 ) ) ;
#59776 = DIRECTION ( 'NONE',  ( 0.000000000000000000, 0.000000000000000000, 1.000000000000000000 ) ) ;
#59777 = CARTESIAN_POINT ( 'NONE',  ( -50.70258187064364108, -137.1250000013655779, 2.196230717870141014 ) ) ;
#59778 = ADVANCED_FACE ( 'NONE', ( #58937 ), #29021, .T. ) ;
#59779 = EDGE_CURVE ( 'NONE', #57628, #34331, #4283, .T. ) ;
#59780 = CARTESIAN_POINT ( 'NONE',  ( 4.458734125000000326, -1.895833331967737623, 2.574251347313718519 ) ) ;
#59781 = CARTESIAN_POINT ( 'NONE',  ( -2.229367062500000163, 22.27083333469892423, -3.861377020970580443 ) ) ;
#59782 = CARTESIAN_POINT ( 'NONE',  ( -2.229367062500000163, -46.72916666530106511, -3.861377020970580443 ) ) ;
#59783 = CARTESIAN_POINT ( 'NONE',  ( 1.975475456537005874E-15, -45.62499999726880873, 5.000000000000000000 ) ) ;
#59784 = CARTESIAN_POINT ( 'NONE',  ( 4.458734124999999437, -83.81249999863439371, -5.460374474430324690E-16 ) ) ;
#59785 = CARTESIAN_POINT ( 'NONE',  ( -4.458734124999997661, -4.229166665301070438, 2.574251347313722516 ) ) ;
#59786 = ORIENTED_EDGE ( 'NONE', *, *, #59861, .T. ) ;
#59787 = CARTESIAN_POINT ( 'NONE',  ( -4.458734124999999437, -31.64583333196773651, -2.574251347313719407 ) ) ;
#59788 =( BOUNDED_CURVE ( )  B_SPLINE_CURVE ( 2, ( #3143, #4082, #24004, #29127, #62633, #57179, #22764, #58100, #18555 ),
 .UNSPECIFIED., .F., .F. ) 
 B_SPLINE_CURVE_WITH_KNOTS ( ( 3, 2, 2, 2, 3 ),
 ( 0.7053571428571429047, 0.7059523809523809978, 0.7071428571428571841, 0.7083333333333333703, 0.7089285714285714635 ),
 .UNSPECIFIED. ) 
 CURVE ( )  GEOMETRIC_REPRESENTATION_ITEM ( )  RATIONAL_B_SPLINE_CURVE ( ( 0.9330127018922194093, 0.9330127018922194093, 1.000000000000000000, 0.8660254037844387076, 1.000000000000000000, 0.8660254037844387076, 1.000000000000000000, 0.9330127018922194093, 0.9330127018922194093 ) ) 
 REPRESENTATION_ITEM ( '' )  );
#59789 = CARTESIAN_POINT ( 'NONE',  ( -57.89159099828107458, -131.9375000013656063, -3.393966926194107447 ) ) ;
#59790 = CARTESIAN_POINT ( 'NONE',  ( 4.458734124999998549, -74.72916666530106511, -2.574251347313721627 ) ) ;
#59791 = CARTESIAN_POINT ( 'NONE',  ( 5.000000000000000000, -110.3749999972688016, -6.123233995736766282E-16 ) ) ;
#59792 = ADVANCED_FACE ( 'NONE', ( #44773 ), #63147, .T. ) ;
#59793 = CARTESIAN_POINT ( 'NONE',  ( 4.458734124999999437, 23.18750000136559564, -5.460374474430324690E-16 ) ) ;
#59794 = CYLINDRICAL_SURFACE ( 'NONE', #28682, 5.000000000000000000 ) ;
#59795 = ADVANCED_FACE ( 'NONE', ( #43816 ), #63463, .T. ) ;
#59796 = CARTESIAN_POINT ( 'NONE',  ( 3.061616997868383141E-16, -145.8750000027312126, -5.000000000000000000 ) ) ;
#59797 = CARTESIAN_POINT ( 'NONE',  ( -2.229367062500000163, -79.72916666530106511, -3.861377020970580443 ) ) ;
#59798 = CARTESIAN_POINT ( 'NONE',  ( 5.000000000000000888, -59.58333333333334281, 2.886751345948126879 ) ) ;
#59799 = CARTESIAN_POINT ( 'NONE',  ( -1.339745962155610925, -74.79465819873854571, 5.000000000000000000 ) ) ;
#59800 = CARTESIAN_POINT ( 'NONE',  ( -4.999999999999999112, 25.20833333606451987, 2.886751345948131764 ) ) ;
#59801 = ORIENTED_EDGE ( 'NONE', *, *, #33149, .T. ) ;
#59802 = CARTESIAN_POINT ( 'NONE',  ( 5.000000000000000888, -1.458333330602148870, 2.886751345948126879 ) ) ;
#59803 = CYLINDRICAL_SURFACE ( 'NONE', #23743, 5.000000000000000000 ) ;
#59805 = CARTESIAN_POINT ( 'NONE',  ( -4.999999999999999112, -16.91666666666666430, 2.886751345948131764 ) ) ;
#59804 = CARTESIAN_POINT ( 'NONE',  ( 75.00000000000001421, 0.000000000000000000, -9.000000000000001776 ) ) ;
#59806 = CARTESIAN_POINT ( 'NONE',  ( 4.458734125000001214, -23.89583333196774007, 2.574251347313718519 ) ) ;
#59807 = CARTESIAN_POINT ( 'NONE',  ( -2.229367062500000163, -84.47916666530107932, -3.861377020970580443 ) ) ;
#59808 = CARTESIAN_POINT ( 'NONE',  ( -3.535250795749689387E-16, -25.12499999726881228, -5.773502691896257311 ) ) ;
#59810 = VERTEX_POINT ( 'NONE', #40278 ) ;
#59809 = CARTESIAN_POINT ( 'NONE',  ( -2.229367062499996610, -52.14583333196773651, 3.861377020970582219 ) ) ;
#59811 = CARTESIAN_POINT ( 'NONE',  ( 1.339745962155615144, -65.70534180126148271, 4.999999999999999112 ) ) ;
#59812 = CARTESIAN_POINT ( 'NONE',  ( 5.000000000000000000, -74.37499999726880162, -6.123233995736766282E-16 ) ) ;
#59814 = ORIENTED_EDGE ( 'NONE', *, *, #50727, .T. ) ;
#59813 = CARTESIAN_POINT ( 'NONE',  ( -4.458734124999999437, -4.645833331967739177, -2.574251347313719407 ) ) ;
#59815 = CARTESIAN_POINT ( 'NONE',  ( -59.44456063193725015, -149.5625000013656063, -0.3552334253322034230 ) ) ;
#59816 = CARTESIAN_POINT ( 'NONE',  ( 5.000000000000000888, -67.58333333333332860, 2.886751345948126879 ) ) ;
#59817 = CARTESIAN_POINT ( 'NONE',  ( -4.458734124999999437, -151.1875000013656063, -5.460374474430324690E-16 ) ) ;
#59818 = CARTESIAN_POINT ( 'NONE',  ( -4.458734124999998549, -46.47916666530107221, 2.574251347313722516 ) ) ;
#59819 = CARTESIAN_POINT ( 'NONE',  ( -6.972266317189433020E-16, -79.24999999999998579, -5.000000000000000000 ) ) ;
#59820 =( BOUNDED_CURVE ( )  B_SPLINE_CURVE ( 2, ( #271, #63632, #19869, #39483, #59119, #49776, #5403, #28885, #15049 ),
 .UNSPECIFIED., .F., .F. ) 
 B_SPLINE_CURVE_WITH_KNOTS ( ( 3, 2, 2, 2, 3 ),
 ( 0.8312500000000000444, 0.8319444444444444864, 0.8333333333333333703, 0.8347222222222222543, 0.8354166666666666963 ),
 .UNSPECIFIED. ) 
 CURVE ( )  GEOMETRIC_REPRESENTATION_ITEM ( )  RATIONAL_B_SPLINE_CURVE ( ( 0.9330127018922194093, 0.9330127018922194093, 1.000000000000000000, 0.8660254037844387076, 1.000000000000000000, 0.8660254037844387076, 1.000000000000000000, 0.9330127018922194093, 0.9330127018922194093 ) ) 
 REPRESENTATION_ITEM ( '' )  );
#59821 = CARTESIAN_POINT ( 'NONE',  ( -5.000000000000000888, -157.4375000000000000, 2.071067811865474617 ) ) ;
#59822 = CARTESIAN_POINT ( 'NONE',  ( -2.500000000000000444, 6.958333336064520758, -4.330127018922193649 ) ) ;
#59823 = CARTESIAN_POINT ( 'NONE',  ( -59.59170313451811296, -124.7500000013655921, 1.485763867205729394 ) ) ;
#59824 = CARTESIAN_POINT ( 'NONE',  ( 4.458734125000001214, -13.14583333196774184, 2.574251347313718519 ) ) ;
#59825 = CARTESIAN_POINT ( 'NONE',  ( -3.152548672688508926E-16, -45.81249999863440081, -5.148502694627439702 ) ) ;
#59826 = CARTESIAN_POINT ( 'NONE',  ( -51.75738570946856498, -136.8750000027312126, 3.805975901505576964 ) ) ;
#59827 = CARTESIAN_POINT ( 'NONE',  ( -1.846868145590734756, -146.1250000013655779, -4.458734125000000326 ) ) ;
#59828 = CARTESIAN_POINT ( 'NONE',  ( 4.458734124999999437, -92.06249999863440792, -5.460374474430324690E-16 ) ) ;
#59829 = CARTESIAN_POINT ( 'NONE',  ( -5.000000000000000000, 21.04166666939784847, -2.886751345948128211 ) ) ;
#59830 = EDGE_LOOP ( 'NONE', ( #58513, #6865, #22075, #35842 ) ) ;
#59831 = CYLINDRICAL_SURFACE ( 'NONE', #30343, 5.000000000000000000 ) ;
#59832 = CARTESIAN_POINT ( 'NONE',  ( -4.458734124999998549, 26.52083333469892779, 2.574251347313722516 ) ) ;
#59833 = CARTESIAN_POINT ( 'NONE',  ( -60.14911071818854538, -145.1875000027312126, 1.666127454062681368 ) ) ;
#59834 = CARTESIAN_POINT ( 'NONE',  ( 2.500000000000002220, -82.54166666393547303, 4.330127018922192761 ) ) ;
#59835 = VERTEX_POINT ( 'NONE', #30942 ) ;
#59836 = CARTESIAN_POINT ( 'NONE',  ( 4.458734124999999437, -1.812499998634406584, -5.460374474430324690E-16 ) ) ;
#59837 = CARTESIAN_POINT ( 'NONE',  ( 1.339745962155615144, 6.294658198738519062, 4.999999999999999112 ) ) ;
#59838 = CARTESIAN_POINT ( 'NONE',  ( 2.229367062500001939, -18.22916666530106866, 3.861377020970579999 ) ) ;
#59839 = CARTESIAN_POINT ( 'NONE',  ( -6.972266317189433020E-16, -101.2499999999999858, -5.000000000000000000 ) ) ;
#59840 = CARTESIAN_POINT ( 'NONE',  ( 4.458734125000001214, -9.895833331967736513, 2.574251347313718519 ) ) ;
#59841 = CARTESIAN_POINT ( 'NONE',  ( 5.000000000000000888, -73.45833333060214443, 2.886751345948126879 ) ) ;
#59842 = CARTESIAN_POINT ( 'NONE',  ( -4.458734124999999437, -150.0000000013656063, -1.846868145590735644 ) ) ;
#59843 = CARTESIAN_POINT ( 'NONE',  ( 4.458734124999998549, 16.02083333469892779, -2.574251347313721627 ) ) ;
#59844 = ORIENTED_EDGE ( 'NONE', *, *, #14545, .T. ) ;
#59845 = CARTESIAN_POINT ( 'NONE',  ( 1.975475456537005874E-15, -26.62499999726881228, 5.000000000000000000 ) ) ;
#59846 = CARTESIAN_POINT ( 'NONE',  ( 1.975475456537005874E-15, -20.74999999999999645, 5.000000000000000000 ) ) ;
#59847 = CARTESIAN_POINT ( 'NONE',  ( -4.458734124999998549, -21.22916666530107221, 2.574251347313722516 ) ) ;
#59848 = CARTESIAN_POINT ( 'NONE',  ( 6.123233995736766282E-16, -170.0000000000000000, -5.000000000000000000 ) ) ;
#59849 = CYLINDRICAL_SURFACE ( 'NONE', #1682, 5.000000000000000000 ) ;
#59850 = CARTESIAN_POINT ( 'NONE',  ( -56.48576386720575471, -147.7500000013655779, -4.591703134518078322 ) ) ;
#59851 = EDGE_CURVE ( 'NONE', #57225, #24352, #54256, .T. ) ;
#59852 = CARTESIAN_POINT ( 'NONE',  ( -2.499999999999996447, -45.70833333060214443, 4.330127018922195425 ) ) ;
#59853 = CARTESIAN_POINT ( 'NONE',  ( 5.000000000000000000, -74.50000000000000000, -6.123233995736766282E-16 ) ) ;
#59854 = CARTESIAN_POINT ( 'NONE',  ( 4.458734124999998549, 16.27083333469892779, -2.574251347313721627 ) ) ;
#59855 = LINE ( 'NONE', #1641, #43784 ) ;
#59856 = CARTESIAN_POINT ( 'NONE',  ( -55.00000000000001421, -135.0000000000000284, 8.082903768654762899 ) ) ;
#59857 = CARTESIAN_POINT ( 'NONE',  ( 2.229367062500001939, 14.02083333469892779, 3.861377020970579999 ) ) ;
#59858 = CARTESIAN_POINT ( 'NONE',  ( -4.458734124999998549, -67.22916666530106511, 2.574251347313722516 ) ) ;
#59859 = ORIENTED_EDGE ( 'NONE', *, *, #10148, .T. ) ;
#59860 = CARTESIAN_POINT ( 'NONE',  ( 2.229367062500001939, -12.22916666530107044, 3.861377020970579999 ) ) ;
#59861 = EDGE_CURVE ( 'NONE', #47452, #1619, #19584, .T. ) ;
#59862 = CARTESIAN_POINT ( 'NONE',  ( 1.060575238724906964E-15, 5.250000000000000888, 5.773502691896257311 ) ) ;
#59863 = CARTESIAN_POINT ( 'NONE',  ( -4.458734125000000326, -164.0000000013656063, -1.846868145590735644 ) ) ;
#59864 = CARTESIAN_POINT ( 'NONE',  ( 6.324555320336756381, 15.00000000000000000, -9.000000000000001776 ) ) ;
#59865 = CARTESIAN_POINT ( 'NONE',  ( -2.229367062500000163, -56.47916666530107221, -3.861377020970580443 ) ) ;
#59866 = CARTESIAN_POINT ( 'NONE',  ( 5.000000000000000000, -90.29166666393547303, -2.886751345948129988 ) ) ;
#59867 = CARTESIAN_POINT ( 'NONE',  ( -2.229367062499996610, -33.14583333196772941, 3.861377020970582219 ) ) ;
#59868 = EDGE_CURVE ( 'NONE', #38026, #176, #4016, .T. ) ;
#59869 = EDGE_CURVE ( 'NONE', #29404, #15518, #55401, .T. ) ;
#59870 = DIRECTION ( 'NONE',  ( -0.000000000000000000, 1.000000000000000000, -0.000000000000000000 ) ) ;
#59871 = DIRECTION ( 'NONE',  ( -0.000000000000000000, 1.000000000000000000, -0.000000000000000000 ) ) ;
#59872 = DIRECTION ( 'NONE',  ( -0.000000000000000000, 1.000000000000000000, -0.000000000000000000 ) ) ;
#59873 = FACE_OUTER_BOUND ( 'NONE', #23035, .T. ) ;
#59874 = CARTESIAN_POINT ( 'NONE',  ( -3.152801135295367985, -149.0625000013655779, 3.152801135295367096 ) ) ;
#59875 = CARTESIAN_POINT ( 'NONE',  ( 2.500000000000002220, -41.66666666666667140, 4.330127018922192761 ) ) ;
#59876 = CARTESIAN_POINT ( 'NONE',  ( 1.975475456537005874E-15, -1.749999999999999334, 5.000000000000000000 ) ) ;
#59877 = ADVANCED_FACE ( 'NONE', ( #60549 ), #50244, .T. ) ;
#59878 = CARTESIAN_POINT ( 'NONE',  ( -6.972266317189433020E-16, -86.12499999726880162, -5.000000000000000000 ) ) ;
#59879 = ORIENTED_EDGE ( 'NONE', *, *, #26837, .F. ) ;
#59880 = CARTESIAN_POINT ( 'NONE',  ( 2.229367062500001939, -108.9791666653010651, 3.861377020970579999 ) ) ;
#59881 = CARTESIAN_POINT ( 'NONE',  ( -4.458734124999999437, 1.354166668032261933, -2.574251347313719407 ) ) ;
#59882 = CARTESIAN_POINT ( 'NONE',  ( -2.499999999999996447, -96.70833333060213022, 4.330127018922195425 ) ) ;
#59883 = EDGE_CURVE ( 'NONE', #45003, #57302, #21680, .T. ) ;
#59884 = CARTESIAN_POINT ( 'NONE',  ( 1.060575238724906964E-15, -2.750000000000002220, 5.773502691896257311 ) ) ;
#59885 = CARTESIAN_POINT ( 'NONE',  ( 4.458734124999999437, -65.81249999863440792, -5.460374474430324690E-16 ) ) ;
#59886 = CARTESIAN_POINT ( 'NONE',  ( -52.53715891517739323, -147.5625000027312126, -4.819101127000233298 ) ) ;
#59887 = EDGE_CURVE ( 'NONE', #25786, #10271, #52853, .T. ) ;
#59888 = CARTESIAN_POINT ( 'NONE',  ( -4.999999999999999112, -7.791666663935482795, 2.886751345948131764 ) ) ;
#59890 = VERTEX_POINT ( 'NONE', #49917 ) ;
#59889 = CARTESIAN_POINT ( 'NONE',  ( -3.152548672688508926E-16, -34.56249999863440792, -5.148502694627439702 ) ) ;
#59891 = FACE_OUTER_BOUND ( 'NONE', #57539, .T. ) ;
#59892 = CARTESIAN_POINT ( 'NONE',  ( 2.500000000000002220, -22.54166666393548013, 4.330127018922192761 ) ) ;
#59894 = ORIENTED_EDGE ( 'NONE', *, *, #49609, .T. ) ;
#59893 = CARTESIAN_POINT ( 'NONE',  ( 4.458734124999999437, 11.93750000136559564, -5.460374474430324690E-16 ) ) ;
#59895 = CARTESIAN_POINT ( 'NONE',  ( 1.339745962155615144, -101.7053418012614827, 4.999999999999999112 ) ) ;
#59896 = CARTESIAN_POINT ( 'NONE',  ( -3.535250795749689387E-16, -52.25000000000001421, -5.773502691896257311 ) ) ;
#59897 = CARTESIAN_POINT ( 'NONE',  ( 4.458734124999998549, -27.97916666530107577, -2.574251347313721627 ) ) ;
#59898 = CARTESIAN_POINT ( 'NONE',  ( 6.123233995736766282E-16, -120.0000000000000000, -5.000000000000000000 ) ) ;
#59899 = CARTESIAN_POINT ( 'NONE',  ( 2.229367062500001939, -73.97916666530106511, 3.861377020970579999 ) ) ;
#59900 = CARTESIAN_POINT ( 'NONE',  ( -3.535533905932737309, -169.6250000000000284, -3.535533905932738197 ) ) ;
#59901 = CARTESIAN_POINT ( 'NONE',  ( -2.229367062500000163, -84.47916666530107932, -3.861377020970580443 ) ) ;
#59902 = CARTESIAN_POINT ( 'NONE',  ( -57.89159099828107458, -136.9375000013655779, -3.393966926194107447 ) ) ;
#59903 =( BOUNDED_CURVE ( )  B_SPLINE_CURVE ( 2, ( #10055, #58322, #23908, #44463, #422, #33871, #9418, #15202, #34827 ),
 .UNSPECIFIED., .F., .F. ) 
 B_SPLINE_CURVE_WITH_KNOTS ( ( 3, 2, 2, 2, 3 ),
 ( 0.8229166666666666297, 0.8236111111111110716, 0.8249999999999999556, 0.8263888888888888395, 0.8270833333333332815 ),
 .UNSPECIFIED. ) 
 CURVE ( )  GEOMETRIC_REPRESENTATION_ITEM ( )  RATIONAL_B_SPLINE_CURVE ( ( 0.9330127018922194093, 0.9330127018922194093, 1.000000000000000000, 0.8660254037844387076, 1.000000000000000000, 0.8660254037844387076, 1.000000000000000000, 0.9330127018922194093, 0.9330127018922194093 ) ) 
 REPRESENTATION_ITEM ( '' )  );
#59904 = CARTESIAN_POINT ( 'NONE',  ( 4.458734124999999437, -28.06249999863440081, -5.460374474430324690E-16 ) ) ;
#59905 = ORIENTED_EDGE ( 'NONE', *, *, #29741, .F. ) ;
#59906 = CARTESIAN_POINT ( 'NONE',  ( 2.499999999999998668, -51.33333333333332860, -4.330127018922193649 ) ) ;
#59907 = ORIENTED_EDGE ( 'NONE', *, *, #38995, .F. ) ;
#59908 = CARTESIAN_POINT ( 'NONE',  ( -4.458734124999998549, -79.47916666530106511, 2.574251347313722516 ) ) ;
#59909 = CARTESIAN_POINT ( 'NONE',  ( -52.00883452924551165, -135.0000000000000284, -3.319254266616502136 ) ) ;
#59910 = ORIENTED_EDGE ( 'NONE', *, *, #53156, .T. ) ;
#59911 = DIRECTION ( 'NONE',  ( 0.000000000000000000, 0.000000000000000000, 1.000000000000000000 ) ) ;
#59912 = CARTESIAN_POINT ( 'NONE',  ( -5.000000000000000000, 8.000000000000000000, 0.000000000000000000 ) ) ;
#59913 = CARTESIAN_POINT ( 'NONE',  ( 4.458734124999999437, -67.06249999863440792, -5.460374474430324690E-16 ) ) ;
#59914 = CARTESIAN_POINT ( 'NONE',  ( 9.457646018065525792E-16, -2.312499998634407028, 5.148502694627439702 ) ) ;
#59915 = ORIENTED_EDGE ( 'NONE', *, *, #3220, .F. ) ;
#59916 =( BOUNDED_CURVE ( )  B_SPLINE_CURVE ( 2, ( #24079, #4761, #44312, #47875, #4150, #39170, #23768, #53025, #43368 ),
 .UNSPECIFIED., .F., .F. ) 
 B_SPLINE_CURVE_WITH_KNOTS ( ( 3, 2, 2, 2, 3 ),
 ( 0.09107142857142856707, 0.09166666666666666019, 0.09285714285714286031, 0.09404761904761904656, 0.09464285714285713969 ),
 .UNSPECIFIED. ) 
 CURVE ( )  GEOMETRIC_REPRESENTATION_ITEM ( )  RATIONAL_B_SPLINE_CURVE ( ( 0.9330127018922194093, 0.9330127018922194093, 1.000000000000000000, 0.8660254037844387076, 1.000000000000000000, 0.8660254037844387076, 1.000000000000000000, 0.9330127018922194093, 0.9330127018922194093 ) ) 
 REPRESENTATION_ITEM ( '' )  );
#59917 = CARTESIAN_POINT ( 'NONE',  ( -2.500000000000000444, -93.04166666393547303, -4.330127018922193649 ) ) ;
#59918 = CARTESIAN_POINT ( 'NONE',  ( -6.972266317189433020E-16, -91.24999999999998579, -5.000000000000000000 ) ) ;
#59919 = CARTESIAN_POINT ( 'NONE',  ( -4.458734124999998549, 6.770833334698928674, 2.574251347313722516 ) ) ;
#59920 = CARTESIAN_POINT ( 'NONE',  ( -50.55543936806279248, -140.0625000013656063, 0.3552334253322060320 ) ) ;
#59921 = CARTESIAN_POINT ( 'NONE',  ( -4.458734124999999437, -161.0000000013656063, -1.846868145590735644 ) ) ;
#59922 = CARTESIAN_POINT ( 'NONE',  ( 2.229367062499998831, 29.10416666803225993, -3.861377020970580887 ) ) ;
#59923 = ORIENTED_EDGE ( 'NONE', *, *, #31896, .F. ) ;
#59924 = CARTESIAN_POINT ( 'NONE',  ( -2.229367062499996610, -81.14583333196773651, 3.861377020970582219 ) ) ;
#59925 = CARTESIAN_POINT ( 'NONE',  ( 3.535533905932738197, -164.0000000027312126, -3.535533905932738197 ) ) ;
#59926 = CARTESIAN_POINT ( 'NONE',  ( -4.458734124999999437, -5.395833331967740953, -2.574251347313719407 ) ) ;
#59927 = CARTESIAN_POINT ( 'NONE',  ( 0.000000000000000000, -170.0000000000000000, 5.000000000000000000 ) ) ;
#59928 = CARTESIAN_POINT ( 'NONE',  ( 2.499999999999998668, 4.791666669397852907, -4.330127018922193649 ) ) ;
#59929 = CARTESIAN_POINT ( 'NONE',  ( 4.458734124999999437, -69.06249999863439371, -5.460374474430324690E-16 ) ) ;
#59930 = CARTESIAN_POINT ( 'NONE',  ( 1.060575238724906964E-15, -31.62499999726880873, 5.773502691896257311 ) ) ;
#59931 = CARTESIAN_POINT ( 'NONE',  ( -1.339745962155613812, -15.20534180126147916, -5.000000000000000000 ) ) ;
#59932 = CARTESIAN_POINT ( 'NONE',  ( 1.975475456537005874E-15, -78.62499999726881583, 5.000000000000000000 ) ) ;
#59933 = CARTESIAN_POINT ( 'NONE',  ( -5.000000000000000000, 22.91666666666666430, -2.886751345948128211 ) ) ;
#59934 = CARTESIAN_POINT ( 'NONE',  ( -4.458734124999997661, 27.77083333469892423, 2.574251347313722516 ) ) ;
#59935 = CARTESIAN_POINT ( 'NONE',  ( -2.229367062500000163, -43.47916666530106511, -3.861377020970580443 ) ) ;
#59936 = CARTESIAN_POINT ( 'NONE',  ( 2.229367062499998831, -32.89583333196773651, -3.861377020970580887 ) ) ;
#59937 = CARTESIAN_POINT ( 'NONE',  ( 4.458734124999999437, 2.937500001365594304, -5.460374474430324690E-16 ) ) ;
#59938 = CARTESIAN_POINT ( 'NONE',  ( 0.000000000000000000, 0.000000000000000000, -10.00000000000000000 ) ) ;
#59939 = CARTESIAN_POINT ( 'NONE',  ( 5.000000000000000888, 19.41666666666666075, 2.886751345948126879 ) ) ;
#59940 = CARTESIAN_POINT ( 'NONE',  ( -3.535533905932738641, -146.5000000027311842, 3.535533905932737309 ) ) ;
#59941 = CARTESIAN_POINT ( 'NONE',  ( 3.535533905932738197, -158.8750000000000284, -3.535533905932738197 ) ) ;
#59942 = CARTESIAN_POINT ( 'NONE',  ( -3.152548672688508926E-16, -40.56249999863440081, -5.148502694627439702 ) ) ;
#59943 = CARTESIAN_POINT ( 'NONE',  ( 5.000000000000000888, -71.45833333060214443, 2.886751345948126879 ) ) ;
#59944 = CARTESIAN_POINT ( 'NONE',  ( -59.44456063193725015, -142.8125000013656063, -0.3552334253322034230 ) ) ;
#59945 = VECTOR ( 'NONE', #50085, 1000.000000000000000 ) ;
#59946 = LINE ( 'NONE', #15868, #33916 ) ;
#59947 = CARTESIAN_POINT ( 'NONE',  ( -6.972266317189433020E-16, -37.25000000000000000, -5.000000000000000000 ) ) ;
#59948 = CARTESIAN_POINT ( 'NONE',  ( 9.457646018065525792E-16, -78.31249999863440792, 5.148502694627439702 ) ) ;
#59949 = CARTESIAN_POINT ( 'NONE',  ( 1.846868145590735200, -162.5000000013655779, -4.458734124999999437 ) ) ;
#59950 = CARTESIAN_POINT ( 'NONE',  ( -9.184850993605147944E-16, -160.2500000000000000, 5.000000000000000000 ) ) ;
#59951 = CARTESIAN_POINT ( 'NONE',  ( -2.411464220262952818, -7.267994521134228059, -7.491772860715828486 ) ) ;
#59952 = CARTESIAN_POINT ( 'NONE',  ( 5.000000000000000000, -25.50000000000000355, -6.123233995736766282E-16 ) ) ;
#59953 = CARTESIAN_POINT ( 'NONE',  ( 3.152801135295366208, -139.5625000013655779, 3.152801135295367985 ) ) ;
#59954 = ORIENTED_EDGE ( 'NONE', *, *, #54712, .T. ) ;
#59955 = CARTESIAN_POINT ( 'NONE',  ( -4.458734124999999437, 22.35416666803225638, -2.574251347313719407 ) ) ;
#59956 = ORIENTED_EDGE ( 'NONE', *, *, #18613, .T. ) ;
#59957 = CARTESIAN_POINT ( 'NONE',  ( -4.458734124999997661, -61.47916666530106511, 2.574251347313722516 ) ) ;
#59958 = CARTESIAN_POINT ( 'NONE',  ( 1.060575238724906964E-15, 21.37500000273118417, 5.773502691896257311 ) ) ;
#59959 = DIRECTION ( 'NONE',  ( -0.000000000000000000, 1.000000000000000000, -0.000000000000000000 ) ) ;
#59960 = CARTESIAN_POINT ( 'NONE',  ( -5.000000000000000000, 16.00000000000000000, 0.000000000000000000 ) ) ;
#59961 = CARTESIAN_POINT ( 'NONE',  ( -3.152548672688508926E-16, -49.56249999863441502, -5.148502694627439702 ) ) ;
#59962 = CARTESIAN_POINT ( 'NONE',  ( -2.229367062500000163, -12.47916666530107044, -3.861377020970580443 ) ) ;
#59963 = CARTESIAN_POINT ( 'NONE',  ( 7.500000000000000000, 4.732328341851997244, -7.493855119309152713 ) ) ;
#59964 = EDGE_CURVE ( 'NONE', #47465, #47715, #59591, .T. ) ;
#59965 = CARTESIAN_POINT ( 'NONE',  ( -1.339745962155610925, 14.20534180126148094, 5.000000000000000000 ) ) ;
#59966 = CARTESIAN_POINT ( 'NONE',  ( 0.000000000000000000, -120.0000000000000000, 0.000000000000000000 ) ) ;
#59967 = CARTESIAN_POINT ( 'NONE',  ( 1.339745962155615144, -11.58034179853029499, 4.999999999999999112 ) ) ;
#59968 = CARTESIAN_POINT ( 'NONE',  ( 1.339745962155612702, -74.29465819873853150, -5.000000000000000000 ) ) ;
#59971 = CARTESIAN_POINT ( 'NONE',  ( -4.458734124999999437, -13.56249999863440259, 0.000000000000000000 ) ) ;
#59970 =( BOUNDED_CURVE ( )  B_SPLINE_CURVE ( 2, ( #54319, #28913, #38266, #24731, #23789, #38562, #24102, #39194, #28601 ),
 .UNSPECIFIED., .F., .F. ) 
 B_SPLINE_CURVE_WITH_KNOTS ( ( 3, 2, 2, 2, 3 ),
 ( 0.3696428571428571619, 0.3702380952380952550, 0.3714285714285714413, 0.3726190476190476275, 0.3732142857142857206 ),
 .UNSPECIFIED. ) 
 CURVE ( )  GEOMETRIC_REPRESENTATION_ITEM ( )  RATIONAL_B_SPLINE_CURVE ( ( 0.9330127018922194093, 0.9330127018922194093, 1.000000000000000000, 0.8660254037844387076, 1.000000000000000000, 0.8660254037844387076, 1.000000000000000000, 0.9330127018922194093, 0.9330127018922194093 ) ) 
 REPRESENTATION_ITEM ( '' )  );
#59969 = CARTESIAN_POINT ( 'NONE',  ( -6.972266317189433020E-16, -33.24999999999999289, -5.000000000000000000 ) ) ;
#59972 = CARTESIAN_POINT ( 'NONE',  ( 4.458734125000001214, -59.89583333196774362, 2.574251347313718519 ) ) ;
#59973 = CARTESIAN_POINT ( 'NONE',  ( 3.152801135295367541, -155.5625000013656063, -3.152801135295367541 ) ) ;
#59974 = CARTESIAN_POINT ( 'NONE',  ( -2.500000000000000444, -53.04166666393548013, -4.330127018922193649 ) ) ;
#59975 = VERTEX_POINT ( 'NONE', #25479 ) ;
#59976 = CARTESIAN_POINT ( 'NONE',  ( -5.000000000000000000, 25.12500000273118417, 0.000000000000000000 ) ) ;
#59977 = CARTESIAN_POINT ( 'NONE',  ( 2.229367062499998831, 1.104166668032261711, -3.861377020970580887 ) ) ;
#59978 = EDGE_LOOP ( 'NONE', ( #56012, #46446, #56426, #36947, #3443, #60764, #24571, #46096, #22082, #877, #39700, #22767, #32978, #53279, #19826, #5948, #52995, #25979, #44734, #49779, #14827, #51222, #58636, #8623, #10286, #34808, #45073, #41525, #17620, #19293, #22750, #45320, #24601, #11923, #41320, #46597, #35205, #58425, #30743, #61256, #40489, #25132 ) ) ;
#59980 = CARTESIAN_POINT ( 'NONE',  ( -5.000000000000000000, -86.00000000000000000, 0.000000000000000000 ) ) ;
#59979 = CARTESIAN_POINT ( 'NONE',  ( -50.18089887299976937, -141.6875000000000000, 2.462841084822427362 ) ) ;
#59981 = CARTESIAN_POINT ( 'NONE',  ( 3.152801135295366208, -157.5625000013656063, 3.152801135295367985 ) ) ;
#59982 = ORIENTED_EDGE ( 'NONE', *, *, #60236, .F. ) ;
#59983 = CYLINDRICAL_SURFACE ( 'NONE', #6720, 5.000000000000000000 ) ;
#59984 = CARTESIAN_POINT ( 'NONE',  ( -57.46284108482265651, -129.9375000000000000, 4.819101127000239515 ) ) ;
#59985 = DIRECTION ( 'NONE',  ( -0.000000000000000000, 1.000000000000000000, -0.000000000000000000 ) ) ;
#59986 = CARTESIAN_POINT ( 'NONE',  ( 4.458734124999998549, -50.97916666530107221, -2.574251347313721627 ) ) ;
#59987 = ORIENTED_EDGE ( 'NONE', *, *, #30367, .T. ) ;
#59988 = DIRECTION ( 'NONE',  ( 7.709882115452476194E-16, 0.000000000000000000, -1.000000000000000000 ) ) ;
#59989 = CARTESIAN_POINT ( 'NONE',  ( -3.152548672688508926E-16, 16.43750000136559564, -5.148502694627439702 ) ) ;
#59990 = CARTESIAN_POINT ( 'NONE',  ( 9.457646018065525792E-16, 26.93750000136559564, 5.148502694627439702 ) ) ;
#59991 = CARTESIAN_POINT ( 'NONE',  ( -52.80376928212989185, -151.8750000013655779, -4.297418129356379346 ) ) ;
#59992 = CARTESIAN_POINT ( 'NONE',  ( 6.123233995736766282E-16, -170.0000000000000000, -5.000000000000000000 ) ) ;
#59993 = CARTESIAN_POINT ( 'NONE',  ( 6.123233995736766282E-16, -120.0000000000000000, -5.000000000000000000 ) ) ;
#59994 = CARTESIAN_POINT ( 'NONE',  ( 4.458734125000000326, -64.89583333196773651, 2.574251347313718519 ) ) ;
#59995 = CARTESIAN_POINT ( 'NONE',  ( 2.411464220263165092, 7.267994521134541586, -7.491772860716163329 ) ) ;
#59996 = CARTESIAN_POINT ( 'NONE',  ( 4.458734124999999437, 12.18750000136559564, -5.460374474430324690E-16 ) ) ;
#59997 = CARTESIAN_POINT ( 'NONE',  ( 1.975475456537005874E-15, 7.249999999999998224, 5.000000000000000000 ) ) ;
#59998 = CARTESIAN_POINT ( 'NONE',  ( 3.061616997868383141E-16, -157.7500000000000000, -5.000000000000000000 ) ) ;
#59999 = CARTESIAN_POINT ( 'NONE',  ( -4.458734124999999437, -53.64583333196772941, -2.574251347313719407 ) ) ;
#60000 = CARTESIAN_POINT ( 'NONE',  ( -5.000000000000000000, -6.874999997268812280, 0.000000000000000000 ) ) ;
#60001 = CARTESIAN_POINT ( 'NONE',  ( -6.972266317189433020E-16, -25.12499999726881228, -5.000000000000000000 ) ) ;
#60002 = CARTESIAN_POINT ( 'NONE',  ( -6.972266317189433020E-16, -66.12499999726881583, -5.000000000000000000 ) ) ;
#60003 = CARTESIAN_POINT ( 'NONE',  ( 4.458734124999998549, -88.97916666530107932, -2.574251347313721627 ) ) ;
#60004 = CARTESIAN_POINT ( 'NONE',  ( 0.000000000000000000, -170.0000000000000000, 5.000000000000000000 ) ) ;
#60005 = CARTESIAN_POINT ( 'NONE',  ( -2.229367062500000163, -18.72916666530106866, -3.861377020970580443 ) ) ;
#60006 = ORIENTED_EDGE ( 'NONE', *, *, #56503, .T. ) ;
#60007 =( BOUNDED_CURVE ( )  B_SPLINE_CURVE ( 2, ( #57871, #13793, #34350, #33415, #49474, #53979, #9907, #48517, #29517 ),
 .UNSPECIFIED., .F., .F. ) 
 B_SPLINE_CURVE_WITH_KNOTS ( ( 3, 2, 2, 2, 3 ),
 ( 0.04791666666666666990, 0.04861111111111111188, 0.05000000000000000278, 0.05138888888888888673, 0.05208333333333333565 ),
 .UNSPECIFIED. ) 
 CURVE ( )  GEOMETRIC_REPRESENTATION_ITEM ( )  RATIONAL_B_SPLINE_CURVE ( ( 0.9330127018922192983, 0.9330127018922196314, 1.000000000000000000, 0.8660254037844387076, 1.000000000000000000, 0.8660254037844387076, 1.000000000000000000, 0.9330127018922189652, 0.9330127018922192983 ) ) 
 REPRESENTATION_ITEM ( '' )  );
#60008 = CARTESIAN_POINT ( 'NONE',  ( 2.500000000000002220, -31.66666666666666075, 4.330127018922192761 ) ) ;
#60009 = CARTESIAN_POINT ( 'NONE',  ( -2.229367062499996610, -106.1458333319677365, 3.861377020970582219 ) ) ;
#60010 = CARTESIAN_POINT ( 'NONE',  ( -3.535533905932737309, -156.7500000027312126, -3.535533905932738197 ) ) ;
#60011 = VERTEX_POINT ( 'NONE', #10999 ) ;
#60012 = CARTESIAN_POINT ( 'NONE',  ( 4.458734125000001214, -98.14583333196773651, 2.574251347313718519 ) ) ;
#60013 = CARTESIAN_POINT ( 'NONE',  ( 2.229367062499998831, -24.64583333196773651, -3.861377020970580887 ) ) ;
#60014 = CARTESIAN_POINT ( 'NONE',  ( -2.500000000000000444, -59.04166666393546592, -4.330127018922193649 ) ) ;
#60015 = DIRECTION ( 'NONE',  ( 0.000000000000000000, 0.000000000000000000, 1.000000000000000000 ) ) ;
#60016 = CARTESIAN_POINT ( 'NONE',  ( -57.19623071787017210, -126.3750000013656489, 4.297418129356382899 ) ) ;
#60017 = CARTESIAN_POINT ( 'NONE',  ( -50.70258187064364108, -144.1250000013656063, 2.196230717870141014 ) ) ;
#60018 = CARTESIAN_POINT ( 'NONE',  ( 4.458734125000000326, -25.89583333196773651, 2.574251347313718519 ) ) ;
#60019 = CARTESIAN_POINT ( 'NONE',  ( -3.152548672688508926E-16, 6.187500001365593860, -5.148502694627439702 ) ) ;
#60020 = CARTESIAN_POINT ( 'NONE',  ( 2.229367062499998831, -62.89583333196774362, -3.861377020970580887 ) ) ;
#60021 = DIRECTION ( 'NONE',  ( -0.000000000000000000, 1.000000000000000000, -0.000000000000000000 ) ) ;
#60022 = CARTESIAN_POINT ( 'NONE',  ( 4.458734124999998549, -19.72916666530107221, -2.574251347313721627 ) ) ;
#60023 = CARTESIAN_POINT ( 'NONE',  ( 0.000000000000000000, -120.0000000000000000, 0.000000000000000000 ) ) ;
#60024 = CARTESIAN_POINT ( 'NONE',  ( 5.000000000000000000, -150.0000000000000284, 0.000000000000000000 ) ) ;
#60025 = CARTESIAN_POINT ( 'NONE',  ( 2.499999999999998668, -11.33333333333333393, -4.330127018922193649 ) ) ;
#60026 = CARTESIAN_POINT ( 'NONE',  ( 4.458734125000000326, -150.3750000013655779, -1.846868145590734978 ) ) ;
#60027 = EDGE_LOOP ( 'NONE', ( #16311, #54051, #63623, #28948 ) ) ;
#60028 = CARTESIAN_POINT ( 'NONE',  ( 4.458734124999999437, -46.06249999863440081, -5.460374474430324690E-16 ) ) ;
#60029 = CARTESIAN_POINT ( 'NONE',  ( -6.972266317189433020E-16, -44.12499999726880162, -5.000000000000000000 ) ) ;
#60030 = CARTESIAN_POINT ( 'NONE',  ( -6.625705691649848461, 5.306270977113102916, -7.795653906409009792 ) ) ;
#60031 = CARTESIAN_POINT ( 'NONE',  ( -2.229367062499996610, -89.14583333196773651, 3.861377020970582219 ) ) ;
#60032 = CARTESIAN_POINT ( 'NONE',  ( -2.229367062500000163, 6.520833334698928674, -3.861377020970580443 ) ) ;
#60033 = CARTESIAN_POINT ( 'NONE',  ( 1.339745962155615144, -41.58034179853029144, 4.999999999999999112 ) ) ;
#60034 = CARTESIAN_POINT ( 'NONE',  ( -4.999999999999998224, 26.08333333333332860, 2.886751345948131764 ) ) ;
#60035 = CARTESIAN_POINT ( 'NONE',  ( -2.229367062500000163, 18.27083333469892779, -3.861377020970580443 ) ) ;
#60036 = CARTESIAN_POINT ( 'NONE',  ( 5.000000000000000000, -75.50000000000000000, -6.123233995736766282E-16 ) ) ;
#60037 = CARTESIAN_POINT ( 'NONE',  ( -3.535250795749689387E-16, 10.87500000273118417, -5.773502691896257311 ) ) ;
#60038 = EDGE_LOOP ( 'NONE', ( #57803, #32032, #18179, #3061 ) ) ;
#60039 = CARTESIAN_POINT ( 'NONE',  ( 5.000000000000000888, -162.0625000027312410, -2.071067811865475505 ) ) ;
#60040 = ORIENTED_EDGE ( 'NONE', *, *, #56976, .F. ) ;
#60041 = DIRECTION ( 'NONE',  ( 0.000000000000000000, 0.000000000000000000, 1.000000000000000000 ) ) ;
#60042 = CARTESIAN_POINT ( 'NONE',  ( -2.229367062499996610, -44.14583333196774362, 3.861377020970582219 ) ) ;
#60043 = CARTESIAN_POINT ( 'NONE',  ( -2.499999999999996447, -41.70833333060214443, 4.330127018922195425 ) ) ;
#60044 = ORIENTED_EDGE ( 'NONE', *, *, #46767, .F. ) ;
#60045 = CARTESIAN_POINT ( 'NONE',  ( -2.229367062499996610, -20.14583333196774007, 3.861377020970582219 ) ) ;
#60046 = ORIENTED_EDGE ( 'NONE', *, *, #61844, .T. ) ;
#60047 = CARTESIAN_POINT ( 'NONE',  ( -4.999999999999999112, -82.91666666666667140, 2.886751345948131764 ) ) ;
#60048 = CARTESIAN_POINT ( 'NONE',  ( -55.00000000000001421, -135.0000000000000284, -8.082903768654752241 ) ) ;
#60049 = CARTESIAN_POINT ( 'NONE',  ( -3.535250795749689387E-16, -88.12499999726878741, -5.773502691896257311 ) ) ;
#60051 = EDGE_LOOP ( 'NONE', ( #4403, #16536, #39349, #9861 ) ) ;
#60050 = CARTESIAN_POINT ( 'NONE',  ( 2.500000000000002220, -55.66666666666667140, 4.330127018922192761 ) ) ;
#60052 = CARTESIAN_POINT ( 'NONE',  ( -59.98410592259440222, -140.1250000000000284, -0.3983568153799752487 ) ) ;
#60053 = EDGE_CURVE ( 'NONE', #34132, #48396, #30622, .T. ) ;
#60054 = CARTESIAN_POINT ( 'NONE',  ( 9.457646018065525792E-16, -28.31249999863440081, 5.148502694627439702 ) ) ;
#60055 = ORIENTED_EDGE ( 'NONE', *, *, #40513, .F. ) ;
#60056 = ITEM_DEFINED_TRANSFORMATION ( 'NONE', 'NONE', #35953,  #43054 ) ;
#60057 = CARTESIAN_POINT ( 'NONE',  ( 1.846868145590735200, -163.5000000013655779, -4.458734125000000326 ) ) ;
#60058 = CARTESIAN_POINT ( 'NONE',  ( -2.229367062500000163, -77.47916666530106511, -3.861377020970580443 ) ) ;
#60059 = CARTESIAN_POINT ( 'NONE',  ( 2.229367062499998831, -109.8958333319677365, -3.861377020970580887 ) ) ;
#60060 = CARTESIAN_POINT ( 'NONE',  ( 5.000000000000000000, -148.0000000000000284, 0.000000000000000000 ) ) ;
#60061 = VERTEX_POINT ( 'NONE', #12283 ) ;
#60062 = DIRECTION ( 'NONE',  ( 0.000000000000000000, 0.000000000000000000, 1.000000000000000000 ) ) ;
#60063 = CARTESIAN_POINT ( 'NONE',  ( -55.35523342533222291, -147.5625000013656063, 4.444560631937231499 ) ) ;
#60064 = CARTESIAN_POINT ( 'NONE',  ( -2.229367062499996610, -74.39583333196773651, 3.861377020970582219 ) ) ;
#60065 = CARTESIAN_POINT ( 'NONE',  ( -55.39835681537999790, -136.0000000027312126, 4.984105922594378235 ) ) ;
#60066 = CARTESIAN_POINT ( 'NONE',  ( 4.458734124999999437, -41.81249999863440081, -5.460374474430324690E-16 ) ) ;
#60067 = CARTESIAN_POINT ( 'NONE',  ( 1.846868145590735200, -141.5000000013655779, -4.458734124999999437 ) ) ;
#60068 = CARTESIAN_POINT ( 'NONE',  ( 2.499999999999998668, 24.66666666666666785, -4.330127018922193649 ) ) ;
#60069 = CARTESIAN_POINT ( 'NONE',  ( 4.458734124999998549, -50.72916666530106511, -2.574251347313721627 ) ) ;
#60070 = CARTESIAN_POINT ( 'NONE',  ( 2.229367062499998831, -46.64583333196774362, -3.861377020970580887 ) ) ;
#60071 = CARTESIAN_POINT ( 'NONE',  ( 5.000000000000000000, 2.625000002731185500, -6.123233995736766282E-16 ) ) ;
#60072 = CARTESIAN_POINT ( 'NONE',  ( -4.458734124999999437, -18.31249999863440792, 0.000000000000000000 ) ) ;
#60073 = CARTESIAN_POINT ( 'NONE',  ( -2.500000000000000444, -101.1666666666666572, -4.330127018922193649 ) ) ;
#60074 = VECTOR ( 'NONE', #5780, 1000.000000000000227 ) ;
#60075 = EDGE_CURVE ( 'NONE', #46520, #859, #1970, .T. ) ;
#60076 = CARTESIAN_POINT ( 'NONE',  ( 1.846868145590735200, -141.5000000013655779, -4.458734125000000326 ) ) ;
#60077 = CARTESIAN_POINT ( 'NONE',  ( 4.458734124999998549, -35.97916666530107221, -2.574251347313721627 ) ) ;
#60078 = EDGE_CURVE ( 'NONE', #31090, #44817, #28014, .T. ) ;
#60079 = CARTESIAN_POINT ( 'NONE',  ( 2.499999999999998668, 6.791666669397851130, -4.330127018922193649 ) ) ;
#60080 = CARTESIAN_POINT ( 'NONE',  ( -1.339745962155613812, -53.20534180126147561, -5.000000000000000000 ) ) ;
#60081 = CARTESIAN_POINT ( 'NONE',  ( -59.44456063193725015, -127.5625000013655921, -0.3552334253322034230 ) ) ;
#60082 = CARTESIAN_POINT ( 'NONE',  ( -2.229367062500000163, -75.72916666530106511, -3.861377020970580443 ) ) ;
#60083 = CARTESIAN_POINT ( 'NONE',  ( -59.81910112700026616, -146.3125000027311842, -2.462841084822510851 ) ) ;
#60084 = FACE_OUTER_BOUND ( 'NONE', #59256, .T. ) ;
#60085 = CARTESIAN_POINT ( 'NONE',  ( -2.229367062500000163, 1.270833334698927342, -3.861377020970580443 ) ) ;
#60086 = ORIENTED_EDGE ( 'NONE', *, *, #21609, .T. ) ;
#60087 = CARTESIAN_POINT ( 'NONE',  ( 3.061616997868383141E-16, -159.7500000000000000, -5.000000000000000000 ) ) ;
#60088 = CARTESIAN_POINT ( 'NONE',  ( -6.972266317189433020E-16, -34.12499999726881583, -5.000000000000000000 ) ) ;
#60090 = CARTESIAN_POINT ( 'NONE',  ( -4.458734124999999437, -36.31249999863440792, 0.000000000000000000 ) ) ;
#60089 = CARTESIAN_POINT ( 'NONE',  ( 4.458734125000001214, -87.89583333196773651, 2.574251347313718519 ) ) ;
#60091 = CARTESIAN_POINT ( 'NONE',  ( -5.926426369611017623E-15, 27.24999999999999645, 5.000000000000000000 ) ) ;
#60092 = CARTESIAN_POINT ( 'NONE',  ( -2.229367062499996610, -80.39583333196773651, 3.861377020970582219 ) ) ;
#60093 = CARTESIAN_POINT ( 'NONE',  ( 4.458734124999998549, 17.02083333469892779, -2.574251347313721627 ) ) ;
#60094 = CARTESIAN_POINT ( 'NONE',  ( -5.000000000000000000, -52.99999999999999289, 0.000000000000000000 ) ) ;
#60095 =( BOUNDED_CURVE ( )  B_SPLINE_CURVE ( 2, ( #62374, #14407, #42415, #62058, #3514, #57551, #24072, #38240, #18297 ),
 .UNSPECIFIED., .F., .F. ) 
 B_SPLINE_CURVE_WITH_KNOTS ( ( 3, 2, 2, 2, 3 ),
 ( 0.6104166666666667185, 0.6111111111111111605, 0.6125000000000000444, 0.6138888888888889284, 0.6145833333333333703 ),
 .UNSPECIFIED. ) 
 CURVE ( )  GEOMETRIC_REPRESENTATION_ITEM ( )  RATIONAL_B_SPLINE_CURVE ( ( 0.9330127018922194093, 0.9330127018922194093, 1.000000000000000000, 0.8660254037844387076, 1.000000000000000000, 0.8660254037844387076, 1.000000000000000000, 0.9330127018922194093, 0.9330127018922194093 ) ) 
 REPRESENTATION_ITEM ( '' )  );
#60096 = CARTESIAN_POINT ( 'NONE',  ( -52.80376928212989185, -136.8750000013656063, -4.297418129356379346 ) ) ;
#60097 = CARTESIAN_POINT ( 'NONE',  ( -2.229367062499996610, -9.145833331967736513, 3.861377020970582219 ) ) ;
#60098 = CARTESIAN_POINT ( 'NONE',  ( 2.229367062499998831, 21.10416666803226349, -3.861377020970580887 ) ) ;
#60099 = CARTESIAN_POINT ( 'NONE',  ( 4.458734125000000326, -49.14583333196772941, 2.574251347313718519 ) ) ;
#60100 = DIRECTION ( 'NONE',  ( 0.000000000000000000, 0.000000000000000000, 1.000000000000000000 ) ) ;
#60101 = CARTESIAN_POINT ( 'NONE',  ( -4.458734124999998549, -84.22916666530107932, 2.574251347313722516 ) ) ;
#60102 = CARTESIAN_POINT ( 'NONE',  ( -2.229367062499996610, -1.145833331967736957, 3.861377020970582219 ) ) ;
#60103 = CARTESIAN_POINT ( 'NONE',  ( 1.975475456537005874E-15, -97.74999999999998579, 5.000000000000000000 ) ) ;
#60104 = ORIENTED_EDGE ( 'NONE', *, *, #61039, .F. ) ;
#60105 = CARTESIAN_POINT ( 'NONE',  ( 9.457646018065525792E-16, -32.31249999863440792, 5.148502694627439702 ) ) ;
#60106 = CARTESIAN_POINT ( 'NONE',  ( -57.19623071787017210, -130.6250000013656347, 4.297418129356382899 ) ) ;
#60107 = CARTESIAN_POINT ( 'NONE',  ( -4.458734124999998549, -72.22916666530107932, 2.574251347313722516 ) ) ;
#60108 = CARTESIAN_POINT ( 'NONE',  ( -2.229367062499996610, 28.60416666803226349, 3.861377020970582219 ) ) ;
#60109 = CARTESIAN_POINT ( 'NONE',  ( 2.229367062500001939, 20.02083333469892779, 3.861377020970579999 ) ) ;
#60110 = LINE ( 'NONE', #10884, #23565 ) ;
#60111 = CARTESIAN_POINT ( 'NONE',  ( 1.062108568985190270E-13, -10.25000000000000355, -4.999999999999999112 ) ) ;
#60112 = CARTESIAN_POINT ( 'NONE',  ( 2.229367062499998831, -80.89583333196773651, -3.861377020970580887 ) ) ;
#60113 = CARTESIAN_POINT ( 'NONE',  ( 5.000000000000000000, -58.41666666666665719, -2.886751345948129988 ) ) ;
#60114 = CYLINDRICAL_SURFACE ( 'NONE', #12077, 5.000000000000000000 ) ;
#60115 = CARTESIAN_POINT ( 'NONE',  ( 2.500000000000002220, 24.45833333606451987, 4.330127018922192761 ) ) ;
#60116 = ORIENTED_EDGE ( 'NONE', *, *, #37074, .F. ) ;
#60117 = CARTESIAN_POINT ( 'NONE',  ( -5.000000000000000000, -56.99999999999999289, 0.000000000000000000 ) ) ;
#60118 = CARTESIAN_POINT ( 'NONE',  ( 5.000000000000000888, -52.45833333060213732, 2.886751345948126879 ) ) ;
#60120 = CARTESIAN_POINT ( 'NONE',  ( 5.000000000000000888, -21.58333333333332860, 2.886751345948126879 ) ) ;
#60119 = CARTESIAN_POINT ( 'NONE',  ( 0.000000000000000000, -170.0000000000000000, 0.000000000000000000 ) ) ;
#60121 = CARTESIAN_POINT ( 'NONE',  ( -4.458734124999999437, -27.31249999863440081, 0.000000000000000000 ) ) ;
#60122 = CARTESIAN_POINT ( 'NONE',  ( -2.229367062500000163, -88.47916666530106511, -3.861377020970580443 ) ) ;
#60123 = VECTOR ( 'NONE', #23819, 1000.000000000000000 ) ;
#60124 = CARTESIAN_POINT ( 'NONE',  ( -5.000000000000000000, -21.95833333060214798, -2.886751345948128211 ) ) ;
#60126 = ORIENTED_EDGE ( 'NONE', *, *, #1416, .F. ) ;
#60125 = CARTESIAN_POINT ( 'NONE',  ( 4.458734124999998549, -57.72916666530107221, -2.574251347313721627 ) ) ;
#60127 = CARTESIAN_POINT ( 'NONE',  ( 1.975475456537005874E-15, -27.74999999999999645, 5.000000000000000000 ) ) ;
#60128 = CARTESIAN_POINT ( 'NONE',  ( 2.499999999999998668, 27.79166666939785202, -4.330127018922193649 ) ) ;
#60130 = ORIENTED_EDGE ( 'NONE', *, *, #43546, .T. ) ;
#60129 = CARTESIAN_POINT ( 'NONE',  ( 4.458734125000001214, -6.145833331967741842, 2.574251347313718519 ) ) ;
#60131 = CARTESIAN_POINT ( 'NONE',  ( -59.29741812935640155, -150.6250000013656063, -2.196230717870135685 ) ) ;
#60132 = CARTESIAN_POINT ( 'NONE',  ( -5.000000000000000000, -67.99999999999998579, 0.000000000000000000 ) ) ;
#60133 = CARTESIAN_POINT ( 'NONE',  ( 4.458734125000000326, -150.6250000013655779, -1.846868145590734978 ) ) ;
#60134 = CARTESIAN_POINT ( 'NONE',  ( 4.458734124999999437, -49.06249999863440792, -5.460374474430324690E-16 ) ) ;
#60135 = CARTESIAN_POINT ( 'NONE',  ( 1.339745962155615144, -23.70534180126148271, 4.999999999999999112 ) ) ;
#60136 = CARTESIAN_POINT ( 'NONE',  ( 3.535533905932738197, -158.8750000000000284, -3.535533905932738197 ) ) ;
#60137 = CARTESIAN_POINT ( 'NONE',  ( 0.000000000000000000, -170.0000000000000000, 0.000000000000000000 ) ) ;
#60138 = CARTESIAN_POINT ( 'NONE',  ( -59.44456063193725015, -124.8125000013655921, -0.3552334253322034230 ) ) ;
#60139 = ADVANCED_FACE ( 'NONE', ( #41856 ), #51836, .T. ) ;
#60140 = CARTESIAN_POINT ( 'NONE',  ( -4.458734124999999437, -8.562499998634406140, 0.000000000000000000 ) ) ;
#60141 = CARTESIAN_POINT ( 'NONE',  ( 4.458734124999999437, -51.06249999863440792, -5.460374474430324690E-16 ) ) ;
#60142 = CARTESIAN_POINT ( 'NONE',  ( 5.000000000000000888, 22.41666666666666785, 2.886751345948126879 ) ) ;
#60143 = CARTESIAN_POINT ( 'NONE',  ( 4.458734124999999437, -143.4375000013656063, 0.000000000000000000 ) ) ;
#60144 = CARTESIAN_POINT ( 'NONE',  ( -2.229367062500000163, -96.72916666530105090, -3.861377020970580443 ) ) ;
#60145 = CARTESIAN_POINT ( 'NONE',  ( 0.000000000000000000, -170.0000000000000000, 5.000000000000000000 ) ) ;
#60146 =( BOUNDED_CURVE ( )  B_SPLINE_CURVE ( 2, ( #42009, #12744, #13061, #4352, #23038, #38439, #18204, #14314, #32680 ),
 .UNSPECIFIED., .F., .F. ) 
 B_SPLINE_CURVE_WITH_KNOTS ( ( 3, 2, 2, 2, 3 ),
 ( 0.7437500000000000222, 0.7444444444444444642, 0.7458333333333333481, 0.7472222222222222321, 0.7479166666666666741 ),
 .UNSPECIFIED. ) 
 CURVE ( )  GEOMETRIC_REPRESENTATION_ITEM ( )  RATIONAL_B_SPLINE_CURVE ( ( 0.9330127018922194093, 0.9330127018922194093, 1.000000000000000000, 0.8660254037844387076, 1.000000000000000000, 0.8660254037844387076, 1.000000000000000000, 0.9330127018922194093, 0.9330127018922194093 ) ) 
 REPRESENTATION_ITEM ( '' )  );
#60147 = ORIENTED_EDGE ( 'NONE', *, *, #50340, .F. ) ;
#60148 = DIRECTION ( 'NONE',  ( -0.000000000000000000, 1.000000000000000000, -0.000000000000000000 ) ) ;
#60149 = CARTESIAN_POINT ( 'NONE',  ( 4.458734124999998549, 25.02083333469892423, -2.574251347313721627 ) ) ;
#60150 = CARTESIAN_POINT ( 'NONE',  ( -55.39835681537999790, -147.0000000027312126, 4.984105922594378235 ) ) ;
#60151 = EDGE_CURVE ( 'NONE', #59975, #5237, #61509, .T. ) ;
#60152 = CARTESIAN_POINT ( 'NONE',  ( 0.000000000000000000, -120.0000000000000000, 5.000000000000000000 ) ) ;
#60153 = ORIENTED_EDGE ( 'NONE', *, *, #13887, .T. ) ;
#60154 = CARTESIAN_POINT ( 'NONE',  ( -3.152548672688508926E-16, -0.5624999986344053626, -5.148502694627439702 ) ) ;
#60155 = CARTESIAN_POINT ( 'NONE',  ( 0.000000000000000000, -170.0000000000000000, 0.000000000000000000 ) ) ;
#60156 = CARTESIAN_POINT ( 'NONE',  ( 2.229367062499998831, -18.89583333196774007, -3.861377020970580887 ) ) ;
#60157 = EDGE_CURVE ( 'NONE', #14479, #12628, #50794, .T. ) ;
#60158 = CARTESIAN_POINT ( 'NONE',  ( -2.500000000000000444, -101.0416666639354588, -4.330127018922193649 ) ) ;
#60160 = ADVANCED_FACE ( 'NONE', ( #52155 ), #14398, .T. ) ;
#60159 = CARTESIAN_POINT ( 'NONE',  ( 4.458734125000001214, -7.895833331967735624, 2.574251347313718519 ) ) ;
#60161 = CARTESIAN_POINT ( 'NONE',  ( 7.112481253774308954, -4.553861071371678726, -7.781689322728511549 ) ) ;
#60162 = CARTESIAN_POINT ( 'NONE',  ( -1.846868145590734756, -147.1250000013656063, -4.458734124999999437 ) ) ;
#60163 = CARTESIAN_POINT ( 'NONE',  ( -4.458734124999999437, 14.35416666803226171, -2.574251347313719407 ) ) ;
#60164 = ORIENTED_EDGE ( 'NONE', *, *, #28411, .T. ) ;
#60165 = DIRECTION ( 'NONE',  ( -0.000000000000000000, 1.000000000000000000, -0.000000000000000000 ) ) ;
#60166 = CARTESIAN_POINT ( 'NONE',  ( 2.500000000000002220, -71.54166666393547303, 4.330127018922192761 ) ) ;
#60167 = CARTESIAN_POINT ( 'NONE',  ( -4.458734124999998549, -18.22916666530107221, 2.574251347313722516 ) ) ;
#60168 = CARTESIAN_POINT ( 'NONE',  ( 5.000000000000000888, -85.45833333060213022, 2.886751345948126879 ) ) ;
#60169 = CARTESIAN_POINT ( 'NONE',  ( -59.81910112700027327, -138.1875000000000000, -2.462841084822392279 ) ) ;
#60170 = CARTESIAN_POINT ( 'NONE',  ( -55.35523342533222291, -148.3125000013656063, 4.444560631937231499 ) ) ;
#60171 = CARTESIAN_POINT ( 'NONE',  ( 2.500000000000002220, -48.54166666393547303, 4.330127018922192761 ) ) ;
#60172 = CYLINDRICAL_SURFACE ( 'NONE', #1444, 5.000000000000000000 ) ;
#60173 = CARTESIAN_POINT ( 'NONE',  ( 4.458734124999998549, 13.27083333469892779, -2.574251347313721627 ) ) ;
#60174 = CARTESIAN_POINT ( 'NONE',  ( 1.975475456537005874E-15, -35.75000000000000711, 5.000000000000000000 ) ) ;
#60175 = CARTESIAN_POINT ( 'NONE',  ( -1.339745962155613812, -48.08034179853029144, -5.000000000000000000 ) ) ;
#60176 = CARTESIAN_POINT ( 'NONE',  ( -4.458734124999999437, 13.68750000136559386, 0.000000000000000000 ) ) ;
#60177 = CARTESIAN_POINT ( 'NONE',  ( 2.229367062499998831, -69.64583333196773651, -3.861377020970580887 ) ) ;
#60178 = CARTESIAN_POINT ( 'NONE',  ( 9.457646018065525792E-16, -16.31249999863440436, 5.148502694627439702 ) ) ;
#60179 = CARTESIAN_POINT ( 'NONE',  ( 1.060575238724906964E-15, 4.250000000000000000, 5.773502691896257311 ) ) ;
#60180 = CARTESIAN_POINT ( 'NONE',  ( -8.190561711645485556E-16, -164.6875000013655779, 4.458734124999999437 ) ) ;
#60181 = CARTESIAN_POINT ( 'NONE',  ( 1.975475456537005874E-15, -0.6249999972688137229, 5.000000000000000000 ) ) ;
#60182 = CARTESIAN_POINT ( 'NONE',  ( -2.229367062499996610, -57.14583333196773651, 3.861377020970582219 ) ) ;
#60183 = CARTESIAN_POINT ( 'NONE',  ( -3.535250795749689387E-16, -96.12499999726880162, -5.773502691896257311 ) ) ;
#60184 = EDGE_CURVE ( 'NONE', #13829, #6026, #47014, .T. ) ;
#60185 = CARTESIAN_POINT ( 'NONE',  ( -5.000000000000000000, -41.87499999726880873, 0.000000000000000000 ) ) ;
#60186 = CARTESIAN_POINT ( 'NONE',  ( -6.972266317189433020E-16, -30.25000000000000000, -5.000000000000000000 ) ) ;
#60187 = CARTESIAN_POINT ( 'NONE',  ( 2.500000000000002220, -56.66666666666667140, 4.330127018922192761 ) ) ;
#60188 = CARTESIAN_POINT ( 'NONE',  ( -4.458734124999999437, -35.31249999863440792, 0.000000000000000000 ) ) ;
#60189 = CARTESIAN_POINT ( 'NONE',  ( 0.000000000000000000, -120.0000000000000000, 5.000000000000000000 ) ) ;
#60190 = CARTESIAN_POINT ( 'NONE',  ( -3.152801135295367096, -150.3125000013655779, -3.152801135295367541 ) ) ;
#60191 = CARTESIAN_POINT ( 'NONE',  ( 5.000000000000000000, -44.41666666666665719, -2.886751345948129988 ) ) ;
#60192 = CARTESIAN_POINT ( 'NONE',  ( -6.972266317189433020E-16, -58.12499999726880162, -5.000000000000000000 ) ) ;
#60193 = CARTESIAN_POINT ( 'NONE',  ( -2.499999999999996447, -107.8333333333333428, 4.330127018922195425 ) ) ;
#60194 = VERTEX_POINT ( 'NONE', #47329 ) ;
#60195 = CARTESIAN_POINT ( 'NONE',  ( -4.458734124999998549, -109.2291666653010793, 2.574251347313722516 ) ) ;
#60196 = CARTESIAN_POINT ( 'NONE',  ( 4.458734125000001214, -1.145833331967740509, 2.574251347313718519 ) ) ;
#60197 =( BOUNDED_CURVE ( )  B_SPLINE_CURVE ( 2, ( #12363, #51298, #40989, #56113, #51918, #61899, #31019, #26848, #17817 ),
 .UNSPECIFIED., .F., .F. ) 
 B_SPLINE_CURVE_WITH_KNOTS ( ( 3, 2, 2, 2, 3 ),
 ( 0.7660714285714286254, 0.7666666666666667185, 0.7678571428571429047, 0.7690476190476190910, 0.7696428571428571841 ),
 .UNSPECIFIED. ) 
 CURVE ( )  GEOMETRIC_REPRESENTATION_ITEM ( )  RATIONAL_B_SPLINE_CURVE ( ( 0.9330127018922194093, 0.9330127018922256266, 1.000000000000000000, 0.8660254037844387076, 1.000000000000000000, 0.8660254037844387076, 1.000000000000000000, 0.9330127018922194093, 0.9330127018922194093 ) ) 
 REPRESENTATION_ITEM ( '' )  );
#60198 = B_SPLINE_CURVE_WITH_KNOTS ( 'NONE', 3,
 ( #50204, #31535, #36055, #59550, #54722, #26083 ),
 .UNSPECIFIED., .F., .F.,
 ( 4, 2, 4 ),
 ( 0.000000000000000000, 0.0004189869898913725285, 0.0008379739797827450570 ),
 .UNSPECIFIED. ) ;
#60199 = CARTESIAN_POINT ( 'NONE',  ( -2.500000000000000444, -9.041666663935483683, -4.330127018922193649 ) ) ;
#60200 = CARTESIAN_POINT ( 'NONE',  ( 5.000000000000000000, -0.4166666666666659080, -2.886751345948129988 ) ) ;
#60201 = CARTESIAN_POINT ( 'NONE',  ( 2.229367062499998831, -68.64583333196773651, -3.861377020970580887 ) ) ;
#60202 = CARTESIAN_POINT ( 'NONE',  ( -5.000000000000000000, -17.00000000000000000, 0.000000000000000000 ) ) ;
#60203 = CARTESIAN_POINT ( 'NONE',  ( -2.499999999999996447, -5.708333330602148870, 4.330127018922195425 ) ) ;
#60205 = ORIENTED_EDGE ( 'NONE', *, *, #18363, .T. ) ;
#60204 = CARTESIAN_POINT ( 'NONE',  ( 4.458734124999998549, -36.72916666530107221, -2.574251347313721627 ) ) ;
#60207 = ORIENTED_EDGE ( 'NONE', *, *, #55529, .T. ) ;
#60206 = CARTESIAN_POINT ( 'NONE',  ( 4.458734124999999437, 12.93750000136559208, -5.460374474430324690E-16 ) ) ;
#60208 = CARTESIAN_POINT ( 'NONE',  ( -59.98410592259440222, -141.2500000027312126, -0.3983568153799752487 ) ) ;
#60209 = CARTESIAN_POINT ( 'NONE',  ( -2.500000000000000444, -49.16666666666666430, -4.330127018922193649 ) ) ;
#60210 = CARTESIAN_POINT ( 'NONE',  ( -2.229367062500000163, -32.72916666530106511, -3.861377020970580443 ) ) ;
#60211 = CARTESIAN_POINT ( 'NONE',  ( 1.339745962155565406, -4.705341801261480050, 5.000000000000028422 ) ) ;
#60212 = CARTESIAN_POINT ( 'NONE',  ( 9.457646018065525792E-16, -77.06249999863440792, 5.148502694627439702 ) ) ;
#60213 = CARTESIAN_POINT ( 'NONE',  ( -8.190561711645485556E-16, -139.9375000013656063, 4.458734124999999437 ) ) ;
#60214 = CARTESIAN_POINT ( 'NONE',  ( -4.458734124999998549, -83.22916666530106511, 2.574251347313722516 ) ) ;
#60215 = CARTESIAN_POINT ( 'NONE',  ( -50.40829686548195099, -136.2500000013656063, -1.485763867205728284 ) ) ;
#60216 = CARTESIAN_POINT ( 'NONE',  ( -4.458734124999999437, -37.56249999863440792, 0.000000000000000000 ) ) ;
#60218 = ORIENTED_EDGE ( 'NONE', *, *, #29190, .F. ) ;
#60217 = EDGE_CURVE ( 'NONE', #7933, #51679, #258, .T. ) ;
#60219 = EDGE_CURVE ( 'NONE', #1619, #52308, #4372, .T. ) ;
#60220 = CARTESIAN_POINT ( 'NONE',  ( 1.339745962155615144, -20.58034179853029144, 4.999999999999999112 ) ) ;
#60221 = VERTEX_POINT ( 'NONE', #59434 ) ;
#60222 = CARTESIAN_POINT ( 'NONE',  ( 4.458734125000001214, -79.14583333196772230, 2.574251347313718519 ) ) ;
#60223 = CARTESIAN_POINT ( 'NONE',  ( -55.22501343921605610, -134.9999999999999432, -4.462558208288625039 ) ) ;
#60224 = EDGE_CURVE ( 'NONE', #12070, #7250, #10946, .T. ) ;
#60225 = ORIENTED_EDGE ( 'NONE', *, *, #23961, .F. ) ;
#60226 = CARTESIAN_POINT ( 'NONE',  ( -2.499999999999996447, -14.70833333060214976, 4.330127018922195425 ) ) ;
#60227 = CARTESIAN_POINT ( 'NONE',  ( 3.061616997868383141E-16, -163.8750000027311842, -5.000000000000000000 ) ) ;
#60228 = CARTESIAN_POINT ( 'NONE',  ( 4.458734124999999437, -65.06249999863440792, -5.460374474430324690E-16 ) ) ;
#60229 = CARTESIAN_POINT ( 'NONE',  ( -2.229367062500000163, -4.729166665301071326, -3.861377020970580443 ) ) ;
#60230 = ORIENTED_EDGE ( 'NONE', *, *, #60236, .T. ) ;
#60231 = EDGE_CURVE ( 'NONE', #5205, #46124, #24106, .T. ) ;
#60232 = CARTESIAN_POINT ( 'NONE',  ( 5.000000000000000000, 3.625000002731186388, -6.123233995736766282E-16 ) ) ;
#60233 = CARTESIAN_POINT ( 'NONE',  ( -1.339745962155610925, 5.330341803992665994, 5.000000000000000000 ) ) ;
#60234 = LINE ( 'NONE', #35456, #21263 ) ;
#60235 = EDGE_CURVE ( 'NONE', #25203, #15879, #1230, .T. ) ;
#60236 = EDGE_CURVE ( 'NONE', #22221, #21052, #40112, .T. ) ;
#60237 = CARTESIAN_POINT ( 'NONE',  ( -3.152548672688508926E-16, 7.437500001365594748, -5.148502694627439702 ) ) ;
#60238 = CARTESIAN_POINT ( 'NONE',  ( 5.000000000000000888, -153.9375000000000000, -2.071067811865475505 ) ) ;
#60239 = CARTESIAN_POINT ( 'NONE',  ( 4.458734124999999437, -159.4375000013655779, 0.000000000000000000 ) ) ;
#60240 = CYLINDRICAL_SURFACE ( 'NONE', #25524, 5.000000000000000000 ) ;
#60241 = ORIENTED_EDGE ( 'NONE', *, *, #826, .T. ) ;
#60242 = CARTESIAN_POINT ( 'NONE',  ( 4.458734124999999437, -82.81249999863440792, -5.460374474430324690E-16 ) ) ;
#60243 = EDGE_CURVE ( 'NONE', #56895, #14032, #59754, .T. ) ;
#60244 = CARTESIAN_POINT ( 'NONE',  ( 2.500000000000002220, -75.66666666666665719, 4.330127018922192761 ) ) ;
#60245 = CARTESIAN_POINT ( 'NONE',  ( 9.457646018065525792E-16, -4.062499998634408804, 5.148502694627439702 ) ) ;
#60246 = CARTESIAN_POINT ( 'NONE',  ( -50.18089887299977647, -147.6875000000000284, 2.462841084822530835 ) ) ;
#60247 = CARTESIAN_POINT ( 'NONE',  ( -5.000000000000000000, -68.08333333333332860, -2.886751345948128211 ) ) ;
#60248 = CARTESIAN_POINT ( 'NONE',  ( -4.458734124999999437, -71.56249999863439371, 0.000000000000000000 ) ) ;
#60249 = CARTESIAN_POINT ( 'NONE',  ( -4.999999999999999112, -28.79166666393548013, 2.886751345948131764 ) ) ;
#60250 = CARTESIAN_POINT ( 'NONE',  ( 1.975475456537005874E-15, 12.37500000273118417, 5.000000000000000000 ) ) ;
#60251 = CARTESIAN_POINT ( 'NONE',  ( 0.000000000000000000, -170.0000000000000000, 5.000000000000000000 ) ) ;
#60252 = CARTESIAN_POINT ( 'NONE',  ( -4.999999999999998224, -55.91666666666667140, 2.886751345948131764 ) ) ;
#60253 = CARTESIAN_POINT ( 'NONE',  ( -2.229367062500000163, 26.52083333469892779, -3.861377020970580443 ) ) ;
#60254 = CARTESIAN_POINT ( 'NONE',  ( -4.458734124999999437, -51.31249999863440792, 0.000000000000000000 ) ) ;
#60255 = CARTESIAN_POINT ( 'NONE',  ( -2.229367062499996610, -32.39583333196773651, 3.861377020970582219 ) ) ;
#60256 = CARTESIAN_POINT ( 'NONE',  ( -4.458734124999999437, 3.354166668032260823, -2.574251347313719407 ) ) ;
#60257 = VECTOR ( 'NONE', #57587, 1000.000000000000000 ) ;
#60258 = CARTESIAN_POINT ( 'NONE',  ( 1.975475456537005874E-15, -0.6249999972688137229, 5.000000000000000000 ) ) ;
#60259 = CARTESIAN_POINT ( 'NONE',  ( 1.060575238724906964E-15, 22.24999999999999645, 5.773502691896257311 ) ) ;
#60260 = CARTESIAN_POINT ( 'NONE',  ( -5.000000000000000888, -143.5625000027311842, 2.071067811865474617 ) ) ;
#60261 = CARTESIAN_POINT ( 'NONE',  ( 2.229367062499998831, -40.64583333196773651, -3.861377020970580887 ) ) ;
#60262 = CARTESIAN_POINT ( 'NONE',  ( -5.000000000000000000, -78.95833333060213022, -2.886751345948128211 ) ) ;
#60263 = AXIS2_PLACEMENT_3D ( 'NONE', #27332, #46963, #2908 ) ;
#60264 = CARTESIAN_POINT ( 'NONE',  ( -50.70258187064364108, -140.3750000013656063, 2.196230717870141014 ) ) ;
#60265 = CARTESIAN_POINT ( 'NONE',  ( 5.000000000000000000, -141.0000000000000000, 0.000000000000000000 ) ) ;
#60266 = CARTESIAN_POINT ( 'NONE',  ( 2.071067811865517694, -140.9375000027311557, -4.999999999999958256 ) ) ;
#60267 = CARTESIAN_POINT ( 'NONE',  ( 4.458734125000000326, -78.14583333196775072, 2.574251347313718519 ) ) ;
#60268 = CARTESIAN_POINT ( 'NONE',  ( -4.458734125000000326, -162.1250000013656347, 1.846868145590734089 ) ) ;
#60269 = CARTESIAN_POINT ( 'NONE',  ( -5.000000000000000888, -159.6875000027312126, -2.071067811865475949 ) ) ;
#60270 = CARTESIAN_POINT ( 'NONE',  ( -5.000000000000000000, -27.08333333333333215, -2.886751345948128211 ) ) ;
#60271 = CARTESIAN_POINT ( 'NONE',  ( -2.499999999999996447, -56.83333333333333570, 4.330127018922195425 ) ) ;
#60272 = ORIENTED_EDGE ( 'NONE', *, *, #35911, .F. ) ;
#60273 = CARTESIAN_POINT ( 'NONE',  ( 2.229367062500001939, 24.77083333469892779, 3.861377020970579999 ) ) ;
#60274 = ORIENTED_EDGE ( 'NONE', *, *, #50161, .T. ) ;
#60275 = CARTESIAN_POINT ( 'NONE',  ( 5.000000000000000000, 22.62500000273118772, -6.123233995736766282E-16 ) ) ;
#60276 = CARTESIAN_POINT ( 'NONE',  ( -3.535250795749689387E-16, 12.75000000000000000, -5.773502691896257311 ) ) ;
#60277 =( BOUNDED_CURVE ( )  B_SPLINE_CURVE ( 2, ( #61890, #19294, #32281, #48250, #27452, #61571, #41601, #27147, #38912 ),
 .UNSPECIFIED., .F., .F. ) 
 B_SPLINE_CURVE_WITH_KNOTS ( ( 3, 2, 2, 2, 3 ),
 ( 0.2145833333333333481, 0.2152777777777777901, 0.2166666666666666741, 0.2180555555555555580, 0.2187500000000000000 ),
 .UNSPECIFIED. ) 
 CURVE ( )  GEOMETRIC_REPRESENTATION_ITEM ( )  RATIONAL_B_SPLINE_CURVE ( ( 0.9330127018922194093, 0.9330127018922207416, 1.000000000000000000, 0.8660254037844387076, 1.000000000000000000, 0.8660254037844387076, 1.000000000000000000, 0.9330127018922194093, 0.9330127018922194093 ) ) 
 REPRESENTATION_ITEM ( '' )  );
#60278 = CARTESIAN_POINT ( 'NONE',  ( -4.458734124999997661, -50.22916666530107221, 2.574251347313722516 ) ) ;
#60279 = CARTESIAN_POINT ( 'NONE',  ( 9.457646018065525792E-16, -13.06249999863440259, 5.148502694627439702 ) ) ;
#60280 = CARTESIAN_POINT ( 'NONE',  ( 6.123233995736766282E-16, -120.0000000000000000, -5.000000000000000000 ) ) ;
#60281 = CARTESIAN_POINT ( 'NONE',  ( -6.972266317189433020E-16, -64.12499999726880162, -5.000000000000000000 ) ) ;
#60282 = CARTESIAN_POINT ( 'NONE',  ( 4.648177544792955347E-16, 28.87500000273118417, -5.000000000000000000 ) ) ;
#60283 = CARTESIAN_POINT ( 'NONE',  ( -2.499999999999996447, -32.83333333333332860, 4.330127018922195425 ) ) ;
#60284 = DIRECTION ( 'NONE',  ( -1.000000000000000000, 0.000000000000000000, 0.000000000000000000 ) ) ;
#60286 = CARTESIAN_POINT ( 'NONE',  ( 4.458734124999998549, -15.97916666530107221, -2.574251347313721627 ) ) ;
#60285 = CARTESIAN_POINT ( 'NONE',  ( 1.975475456537005874E-15, -55.62499999726880873, 5.000000000000000000 ) ) ;
#60287 = FACE_BOUND ( 'NONE', #28842, .T. ) ;
#60288 = CARTESIAN_POINT ( 'NONE',  ( -2.229367062499996610, -58.14583333196773651, 3.861377020970582219 ) ) ;
#60289 = CARTESIAN_POINT ( 'NONE',  ( -8.190561711645485556E-16, -151.9375000013655779, 4.458734124999999437 ) ) ;
#60290 = CARTESIAN_POINT ( 'NONE',  ( 4.458734124999999437, -66.81249999863440792, -5.460374474430324690E-16 ) ) ;
#60291 =( BOUNDED_CURVE ( )  B_SPLINE_CURVE ( 2, ( #39805, #10541, #5727, #44964, #16648, #31755, #27871, #17279, #60726 ),
 .UNSPECIFIED., .F., .F. ) 
 B_SPLINE_CURVE_WITH_KNOTS ( ( 3, 2, 2, 2, 3 ),
 ( 0.3645833333333333148, 0.3652777777777777568, 0.3666666666666666408, 0.3680555555555555802, 0.3687500000000000222 ),
 .UNSPECIFIED. ) 
 CURVE ( )  GEOMETRIC_REPRESENTATION_ITEM ( )  RATIONAL_B_SPLINE_CURVE ( ( 0.9330127018922194093, 0.9330127018922194093, 1.000000000000000000, 0.8660254037844387076, 1.000000000000000000, 0.8660254037844387076, 1.000000000000000000, 0.9330127018922194093, 0.9330127018922194093 ) ) 
 REPRESENTATION_ITEM ( '' )  );
#60292 = CARTESIAN_POINT ( 'NONE',  ( 2.499999999999998668, -57.20833333060214443, -4.330127018922193649 ) ) ;
#60293 = ORIENTED_EDGE ( 'NONE', *, *, #20924, .T. ) ;
#60294 = DIRECTION ( 'NONE',  ( 0.000000000000000000, 0.000000000000000000, 1.000000000000000000 ) ) ;
#60295 = VERTEX_POINT ( 'NONE', #24690 ) ;
#60297 = CARTESIAN_POINT ( 'NONE',  ( 2.500000000000002220, -58.66666666666665719, 4.330127018922192761 ) ) ;
#60296 = CARTESIAN_POINT ( 'NONE',  ( -58.80597590150559739, -149.1250000027312126, 3.242614290531460330 ) ) ;
#60298 = CARTESIAN_POINT ( 'NONE',  ( -1.846868145590734756, -154.1250000013656063, -4.458734125000000326 ) ) ;
#60299 = ORIENTED_EDGE ( 'NONE', *, *, #6272, .F. ) ;
#60300 = CARTESIAN_POINT ( 'NONE',  ( -6.972266317189433020E-16, -8.124999997268814056, -5.000000000000000000 ) ) ;
#60301 = CARTESIAN_POINT ( 'NONE',  ( -58.24261429053147765, -131.2500000000000284, -3.805975901505573855 ) ) ;
#60302 = CARTESIAN_POINT ( 'NONE',  ( 5.000000000000000000, -80.29166666393547303, -2.886751345948130876 ) ) ;
#60303 = CARTESIAN_POINT ( 'NONE',  ( -2.229367062499996610, -46.39583333196774362, 3.861377020970582219 ) ) ;
#60304 = VECTOR ( 'NONE', #20448, 1000.000000000000000 ) ;
#60305 = VERTEX_POINT ( 'NONE', #55247 ) ;
#60306 = VECTOR ( 'NONE', #56853, 1000.000000000000000 ) ;
#60307 = CARTESIAN_POINT ( 'NONE',  ( -1.339745962155613812, -110.0803417985302843, -5.000000000000000000 ) ) ;
#60308 = CARTESIAN_POINT ( 'NONE',  ( -4.458734124999999437, 13.68750000136559386, 0.000000000000000000 ) ) ;
#60309 = EDGE_CURVE ( 'NONE', #61181, #61334, #30681, .T. ) ;
#60310 = CARTESIAN_POINT ( 'NONE',  ( -3.152548672688508926E-16, 23.43750000136559564, -5.148502694627439702 ) ) ;
#60311 = CARTESIAN_POINT ( 'NONE',  ( -58.39396692619412477, -154.4375000013656063, 2.891590998281057701 ) ) ;
#60312 = CARTESIAN_POINT ( 'NONE',  ( -48.00000000000002132, -135.0000000000000284, -4.041451884327376121 ) ) ;
#60313 = CARTESIAN_POINT ( 'NONE',  ( 7.500000000000000888, 1.443375672974060109, -7.063244554130000630 ) ) ;
#60315 = ADVANCED_FACE ( 'NONE', ( #30790 ), #59108, .T. ) ;
#60314 = ORIENTED_EDGE ( 'NONE', *, *, #13018, .F. ) ;
#60316 = CARTESIAN_POINT ( 'NONE',  ( 4.458734124999998549, -64.72916666530106511, -2.574251347313721627 ) ) ;
#60317 = CARTESIAN_POINT ( 'NONE',  ( 6.123233995736766282E-16, -120.0000000000000000, -5.000000000000000000 ) ) ;
#60318 = CARTESIAN_POINT ( 'NONE',  ( 4.458734124999998549, 11.27083333469892779, -2.574251347313721627 ) ) ;
#60319 = CARTESIAN_POINT ( 'NONE',  ( -1.339745962155613812, -70.08034179853029855, -5.000000000000000000 ) ) ;
#60320 = EDGE_CURVE ( 'NONE', #63065, #62891, #43435, .T. ) ;
#60321 = CARTESIAN_POINT ( 'NONE',  ( 4.458734124999998549, -52.97916666530107932, -2.574251347313721627 ) ) ;
#60322 = CARTESIAN_POINT ( 'NONE',  ( 2.499999999999998668, -17.20833333060214443, -4.330127018922193649 ) ) ;
#60323 = CARTESIAN_POINT ( 'NONE',  ( -2.500000000000000444, -109.1666666666666572, -4.330127018922193649 ) ) ;
#60324 = CARTESIAN_POINT ( 'NONE',  ( 7.500000000000000888, -3.640541674360523228, -0.7158139487964624292 ) ) ;
#60325 = CARTESIAN_POINT ( 'NONE',  ( 0.000000000000000000, -120.0000000000000000, 5.000000000000000000 ) ) ;
#60326 = CARTESIAN_POINT ( 'NONE',  ( 5.000000000000000000, -64.37499999726881583, -6.123233995736766282E-16 ) ) ;
#60327 = CARTESIAN_POINT ( 'NONE',  ( 2.229367062500001939, -16.22916666530107577, 3.861377020970579999 ) ) ;
#60328 = ORIENTED_EDGE ( 'NONE', *, *, #10239, .F. ) ;
#60329 = CARTESIAN_POINT ( 'NONE',  ( 0.000000000000000000, -120.0000000000000000, 0.000000000000000000 ) ) ;
#60330 = CARTESIAN_POINT ( 'NONE',  ( 2.229367062500001939, -103.9791666653010651, 3.861377020970579999 ) ) ;
#60331 = CARTESIAN_POINT ( 'NONE',  ( 2.071067811865476394, -157.3125000027312126, 5.000000000000000000 ) ) ;
#60332 = EDGE_LOOP ( 'NONE', ( #58204, #12975, #4801, #13856, #15836, #51877, #13670, #39449, #21440, #19765, #9872, #21287, #5688, #60299, #14074, #36159, #25136 ) ) ;
#60333 = CARTESIAN_POINT ( 'NONE',  ( 4.458734124999998549, -101.9791666653010651, -2.574251347313721627 ) ) ;
#60334 = CARTESIAN_POINT ( 'NONE',  ( 2.229367062500001939, -26.97916666530106866, 3.861377020970579999 ) ) ;
#60335 = CARTESIAN_POINT ( 'NONE',  ( -3.535250795749689387E-16, -60.12499999726880162, -5.773502691896257311 ) ) ;
#60336 = CARTESIAN_POINT ( 'NONE',  ( -54.64476657466781973, -124.8125000013655921, -4.444560631937228834 ) ) ;
#60337 = CARTESIAN_POINT ( 'NONE',  ( -50.40829686548195099, -141.0000000013655779, -1.485763867205728284 ) ) ;
#60338 = CARTESIAN_POINT ( 'NONE',  ( 4.458734124999999437, -22.81249999863440436, -5.460374474430324690E-16 ) ) ;
#60339 = CARTESIAN_POINT ( 'NONE',  ( -2.229367062499996610, -62.39583333196774362, 3.861377020970582219 ) ) ;
#60340 = CARTESIAN_POINT ( 'NONE',  ( -4.999999999999998224, -39.79166666393548013, 2.886751345948131764 ) ) ;
#60341 = CARTESIAN_POINT ( 'NONE',  ( 2.229367062499998831, -20.64583333196774007, -3.861377020970580887 ) ) ;
#60342 = DIRECTION ( 'NONE',  ( 0.000000000000000000, 0.000000000000000000, 1.000000000000000000 ) ) ;
#60343 = CARTESIAN_POINT ( 'NONE',  ( 5.000000000000000888, -149.9375000000000000, -2.071067811865475505 ) ) ;
#60344 = CARTESIAN_POINT ( 'NONE',  ( -2.499999999999996447, -10.83333333333333393, 4.330127018922195425 ) ) ;
#60345 = CARTESIAN_POINT ( 'NONE',  ( -4.458734125000001214, -151.8750000013655779, 1.846868145590734089 ) ) ;
#60346 = VERTEX_POINT ( 'NONE', #54275 ) ;
#60347 = CARTESIAN_POINT ( 'NONE',  ( 4.458734124999999437, -48.06249999863440792, -5.460374474430324690E-16 ) ) ;
#60348 =( BOUNDED_CURVE ( )  B_SPLINE_CURVE ( 2, ( #12869, #41494, #56639, #8060, #23156, #51490, #46977, #12553, #13513 ),
 .UNSPECIFIED., .F., .F. ) 
 B_SPLINE_CURVE_WITH_KNOTS ( ( 3, 2, 2, 2, 3 ),
 ( 0.01964285714285714593, 0.02023809523809523905, 0.02142857142857142877, 0.02261904761904761849, 0.02321428571428571508 ),
 .UNSPECIFIED. ) 
 CURVE ( )  GEOMETRIC_REPRESENTATION_ITEM ( )  RATIONAL_B_SPLINE_CURVE ( ( 0.9330127018922194093, 0.9330127018922195203, 1.000000000000000000, 0.8660254037844387076, 1.000000000000000000, 0.8660254037844387076, 1.000000000000000000, 0.9330127018922191873, 0.9330127018922194093 ) ) 
 REPRESENTATION_ITEM ( '' )  );
#60349 = AXIS2_PLACEMENT_3D ( 'NONE', #33005, #59669, #34898 ) ;
#60350 = DIRECTION ( 'NONE',  ( -0.000000000000000000, 1.000000000000000000, -0.000000000000000000 ) ) ;
#60351 = CARTESIAN_POINT ( 'NONE',  ( -6.972266317189433020E-16, -52.12499999726880873, -5.000000000000000000 ) ) ;
#60352 = CARTESIAN_POINT ( 'NONE',  ( 1.060575238724906964E-15, 27.25000000000000000, 5.773502691896257311 ) ) ;
#60353 = VECTOR ( 'NONE', #29196, 1000.000000000000000 ) ;
#60354 = CARTESIAN_POINT ( 'NONE',  ( -3.152548672688508926E-16, 3.437500001365594748, -5.148502694627439702 ) ) ;
#60355 = CARTESIAN_POINT ( 'NONE',  ( 1.339745962155612702, 1.830341803992665772, -5.000000000000000000 ) ) ;
#60356 = VECTOR ( 'NONE', #45274, 1000.000000000000000 ) ;
#60357 = DIRECTION ( 'NONE',  ( 0.000000000000000000, 0.000000000000000000, 1.000000000000000000 ) ) ;
#60358 = CARTESIAN_POINT ( 'NONE',  ( -5.040301471719076609, -5.750234626350520628, -0.09933465333851741741 ) ) ;
#60359 = CARTESIAN_POINT ( 'NONE',  ( -3.152548672688508926E-16, 13.18750000136559208, -5.148502694627439702 ) ) ;
#60360 = CARTESIAN_POINT ( 'NONE',  ( 5.000000000000000888, -81.58333333333332860, 2.886751345948126879 ) ) ;
#60361 = CARTESIAN_POINT ( 'NONE',  ( -2.500000000000000444, 7.958333336064518093, -4.330127018922193649 ) ) ;
#60362 = ORIENTED_EDGE ( 'NONE', *, *, #32193, .F. ) ;
#60363 = DIRECTION ( 'NONE',  ( -0.000000000000000000, 1.000000000000000000, -0.000000000000000000 ) ) ;
#60364 = ORIENTED_EDGE ( 'NONE', *, *, #13796, .T. ) ;
#60365 = CARTESIAN_POINT ( 'NONE',  ( 2.499999999999998668, -85.33333333333332860, -4.330127018922193649 ) ) ;
#60366 = CARTESIAN_POINT ( 'NONE',  ( 4.458734125000001214, -44.89583333196774362, 2.574251347313718519 ) ) ;
#60367 = CARTESIAN_POINT ( 'NONE',  ( -1.846868145590734756, -165.3750000013656347, -4.458734125000000326 ) ) ;
#60368 = EDGE_CURVE ( 'NONE', #27206, #15666, #37265, .T. ) ;
#60369 = CARTESIAN_POINT ( 'NONE',  ( -5.000000000000000000, -39.87499999726880162, 0.000000000000000000 ) ) ;
#60370 = ORIENTED_EDGE ( 'NONE', *, *, #62495, .F. ) ;
#60371 = CARTESIAN_POINT ( 'NONE',  ( 2.229367062499998831, -15.64583333196773651, -3.861377020970580887 ) ) ;
#60372 = VERTEX_POINT ( 'NONE', #55571 ) ;
#60373 = CARTESIAN_POINT ( 'NONE',  ( -2.499999999999996447, -86.83333333333332860, 4.330127018922195425 ) ) ;
#60374 = CARTESIAN_POINT ( 'NONE',  ( 2.730187237215162345E-16, -168.1875000013655779, -4.458734124999999437 ) ) ;
#60375 = CARTESIAN_POINT ( 'NONE',  ( 1.060575238724906964E-15, -87.62499999726880162, 5.773502691896257311 ) ) ;
#60377 = ORIENTED_EDGE ( 'NONE', *, *, #56635, .T. ) ;
#60376 = CARTESIAN_POINT ( 'NONE',  ( -8.660254037844341113, 30.00000000000000000, 6.047423072554883697E-14 ) ) ;
#60378 = CARTESIAN_POINT ( 'NONE',  ( -54.60164318462004474, -141.3750000000000284, -4.984105922594373794 ) ) ;
#60379 = CARTESIAN_POINT ( 'NONE',  ( 4.458734125000001214, -35.14583333196772941, 2.574251347313718519 ) ) ;
#60380 = CARTESIAN_POINT ( 'NONE',  ( 2.499999999999998668, -5.208333330602148870, -4.330127018922193649 ) ) ;
#60381 = ORIENTED_EDGE ( 'NONE', *, *, #52040, .T. ) ;
#60382 = CARTESIAN_POINT ( 'NONE',  ( 4.458734124999998549, -76.72916666530106511, -2.574251347313721627 ) ) ;
#60383 = CARTESIAN_POINT ( 'NONE',  ( 9.457646018065525792E-16, -108.3124999986343937, 5.148502694627439702 ) ) ;
#60384 = CARTESIAN_POINT ( 'NONE',  ( -5.000000000000000000, -53.99999999999999289, 0.000000000000000000 ) ) ;
#60385 = ORIENTED_EDGE ( 'NONE', *, *, #15761, .T. ) ;
#60386 = CARTESIAN_POINT ( 'NONE',  ( 6.123233995736766282E-16, -170.0000000000000000, -5.000000000000000000 ) ) ;
#60387 = CARTESIAN_POINT ( 'NONE',  ( -59.44456063193725015, -140.8125000013656063, -0.3552334253322034230 ) ) ;
#60388 = CARTESIAN_POINT ( 'NONE',  ( -3.152548672688508926E-16, -81.81249999863440792, -5.148502694627439702 ) ) ;
#60389 = CARTESIAN_POINT ( 'NONE',  ( -50.01589407740564042, -132.7500000027312126, 0.3983568153799778022 ) ) ;
#60390 = CARTESIAN_POINT ( 'NONE',  ( 4.458734125000000326, -41.89583333196772941, 2.574251347313718519 ) ) ;
#60391 = CARTESIAN_POINT ( 'NONE',  ( 4.458734124999999437, -143.6875000013656063, 0.000000000000000000 ) ) ;
#60392 = AXIS2_PLACEMENT_3D ( 'NONE', #43985, #19552, #36822 ) ;
#60393 = CARTESIAN_POINT ( 'NONE',  ( -1.339745962155610925, -57.79465819873852439, 5.000000000000000000 ) ) ;
#60394 = CARTESIAN_POINT ( 'NONE',  ( -4.458734124999999437, -47.39583333196774362, -2.574251347313719407 ) ) ;
#60395 = CARTESIAN_POINT ( 'NONE',  ( 2.229367062500001939, -46.97916666530106511, 3.861377020970579999 ) ) ;
#60396 = CARTESIAN_POINT ( 'NONE',  ( 4.458734124999998549, 27.27083333469892423, -2.574251347313721627 ) ) ;
#60397 = VECTOR ( 'NONE', #56559, 1000.000000000000000 ) ;
#60398 = CARTESIAN_POINT ( 'NONE',  ( -2.229367062499996610, -17.14583333196773651, 3.861377020970582219 ) ) ;
#60399 = CARTESIAN_POINT ( 'NONE',  ( 1.060575238724906964E-15, -98.75000000000000000, 5.773502691896257311 ) ) ;
#60400 = CARTESIAN_POINT ( 'NONE',  ( -6.324555320336756381, 15.00000000000000000, -9.000000000000001776 ) ) ;
#60401 = CARTESIAN_POINT ( 'NONE',  ( -4.458734124999999437, -40.64583333196773651, -2.574251347313719407 ) ) ;
#60402 = CARTESIAN_POINT ( 'NONE',  ( 5.000000000000000000, 0.7083333360645184262, -2.886751345948129988 ) ) ;
#60403 = CARTESIAN_POINT ( 'NONE',  ( -5.000000000000000000, -6.958333330602150646, -2.886751345948128211 ) ) ;
#60404 = CARTESIAN_POINT ( 'NONE',  ( -50.40829686548195099, -128.0000000013656063, -1.485763867205728284 ) ) ;
#60405 = CARTESIAN_POINT ( 'NONE',  ( 4.458734124999999437, -78.06249999863440792, -5.460374474430324690E-16 ) ) ;
#60406 = CARTESIAN_POINT ( 'NONE',  ( 2.500000000000002220, -71.66666666666667140, 4.330127018922192761 ) ) ;
#60407 = CARTESIAN_POINT ( 'NONE',  ( 4.458734125000000326, 1.854166668032262599, 2.574251347313718519 ) ) ;
#60408 = VERTEX_POINT ( 'NONE', #6361 ) ;
#60409 = CARTESIAN_POINT ( 'NONE',  ( 2.500000000000002220, 24.45833333606451987, 4.330127018922192761 ) ) ;
#60410 = CARTESIAN_POINT ( 'NONE',  ( 1.339745962155615144, -57.70534180126147561, 4.999999999999999112 ) ) ;
#60412 = CARTESIAN_POINT ( 'NONE',  ( -4.458734124999999437, -37.31249999863440792, 0.000000000000000000 ) ) ;
#60411 = CARTESIAN_POINT ( 'NONE',  ( -4.458734124999998549, -86.22916666530106511, 2.574251347313722516 ) ) ;
#60413 = DIRECTION ( 'NONE',  ( 0.000000000000000000, 0.000000000000000000, 1.000000000000000000 ) ) ;
#60414 = CARTESIAN_POINT ( 'NONE',  ( 9.457646018065525792E-16, -85.31249999863439371, 5.148502694627439702 ) ) ;
#60415 = CARTESIAN_POINT ( 'NONE',  ( 4.458734125000000326, 18.85416666803225993, 2.574251347313718519 ) ) ;
#60416 = CYLINDRICAL_SURFACE ( 'NONE', #46936, 5.000000000000000000 ) ;
#60417 = CARTESIAN_POINT ( 'NONE',  ( -59.59170313451811296, -137.5000000013656063, 1.485763867205729394 ) ) ;
#60418 = CARTESIAN_POINT ( 'NONE',  ( -4.458734124999999437, -9.312499998634406140, 0.000000000000000000 ) ) ;
#60419 = CARTESIAN_POINT ( 'NONE',  ( 4.458734124999999437, 22.93750000136559564, -5.460374474430324690E-16 ) ) ;
#60420 = CARTESIAN_POINT ( 'NONE',  ( 2.229367062499998831, -46.89583333196774362, -3.861377020970580887 ) ) ;
#60421 = CARTESIAN_POINT ( 'NONE',  ( -5.000000000000000000, 17.04166666939785202, -2.886751345948128211 ) ) ;
#60422 = CARTESIAN_POINT ( 'NONE',  ( 2.229367062500001939, -86.97916666530107932, 3.861377020970579999 ) ) ;
#60423 = CARTESIAN_POINT ( 'NONE',  ( -3.152548672688508926E-16, -1.562499998634406140, -5.148502694627439702 ) ) ;
#60424 = PRESENTATION_STYLE_ASSIGNMENT (( #21170 ) ) ;
#60425 = ORIENTED_EDGE ( 'NONE', *, *, #12576, .F. ) ;
#60426 = CARTESIAN_POINT ( 'NONE',  ( -4.458734124999997661, -31.47916666530107577, 2.574251347313722516 ) ) ;
#60427 = CARTESIAN_POINT ( 'NONE',  ( -50.40829686548195099, -131.2500000013656347, -1.485763867205728284 ) ) ;
#60428 = CARTESIAN_POINT ( 'NONE',  ( -4.458734124999999437, -73.39583333196773651, -2.574251347313719407 ) ) ;
#60429 = CARTESIAN_POINT ( 'NONE',  ( -2.229367062500000163, 27.27083333469892779, -3.861377020970580443 ) ) ;
#60430 = EDGE_CURVE ( 'NONE', #35906, #25520, #6836, .T. ) ;
#60431 = CARTESIAN_POINT ( 'NONE',  ( 9.457646018065525792E-16, 20.93750000136558853, 5.148502694627439702 ) ) ;
#60432 = CARTESIAN_POINT ( 'NONE',  ( 1.339745962155615144, -53.70534180126147561, 4.999999999999999112 ) ) ;
#60433 = CARTESIAN_POINT ( 'NONE',  ( 2.499999999999998668, -28.33333333333333570, -4.330127018922193649 ) ) ;
#60434 = CARTESIAN_POINT ( 'NONE',  ( -2.229367062499996610, -76.39583333196773651, 3.861377020970582219 ) ) ;
#60435 = CARTESIAN_POINT ( 'NONE',  ( 5.000000000000000000, -62.50000000000000000, -6.123233995736766282E-16 ) ) ;
#60436 = CARTESIAN_POINT ( 'NONE',  ( -9.184850993605147944E-16, -143.2500000000000284, 5.000000000000000000 ) ) ;
#60437 = CARTESIAN_POINT ( 'NONE',  ( 5.000000000000000000, 22.62500000273118772, -6.123233995736766282E-16 ) ) ;
#60438 = EDGE_LOOP ( 'NONE', ( #1797, #14966, #36165, #52388 ) ) ;
#60439 = CARTESIAN_POINT ( 'NONE',  ( -2.499999999999996447, -72.70833333060214443, 4.330127018922195425 ) ) ;
#60440 = VECTOR ( 'NONE', #25649, 1000.000000000000000 ) ;
#60441 = CARTESIAN_POINT ( 'NONE',  ( 0.000000000000000000, -170.0000000000000000, 0.000000000000000000 ) ) ;
#60443 = CARTESIAN_POINT ( 'NONE',  ( -3.535250795749689387E-16, -22.24999999999999645, -5.773502691896257311 ) ) ;
#60442 = CARTESIAN_POINT ( 'NONE',  ( 5.000000000000000000, -0.4166666666666659080, -2.886751345948130876 ) ) ;
#60444 = CARTESIAN_POINT ( 'NONE',  ( 4.458734125000001214, -28.89583333196774007, 2.574251347313718519 ) ) ;
#60445 = CARTESIAN_POINT ( 'NONE',  ( -2.229367062499996610, -89.14583333196773651, 3.861377020970582219 ) ) ;
#60446 = CARTESIAN_POINT ( 'NONE',  ( 5.000000000000000000, -22.37499999726881228, -6.123233995736766282E-16 ) ) ;
#60448 = ORIENTED_EDGE ( 'NONE', *, *, #35378, .F. ) ;
#60447 = CARTESIAN_POINT ( 'NONE',  ( 4.458734125000001214, -57.89583333196773651, 2.574251347313718519 ) ) ;
#60449 = CARTESIAN_POINT ( 'NONE',  ( 2.499999999999998668, -49.33333333333332860, -4.330127018922193649 ) ) ;
#60450 = CARTESIAN_POINT ( 'NONE',  ( 1.339745962155612702, -59.16965819600732601, -5.000000000000000000 ) ) ;
#60452 = EDGE_LOOP ( 'NONE', ( #47697, #35040, #35121, #60520 ) ) ;
#60451 = CARTESIAN_POINT ( 'NONE',  ( -2.229367062499996610, -3.395833331967738733, 3.861377020970582219 ) ) ;
#60453 = CARTESIAN_POINT ( 'NONE',  ( 1.060575238724906964E-15, -72.74999999999998579, 5.773502691896257311 ) ) ;
#60454 = CARTESIAN_POINT ( 'NONE',  ( -8.190561711645485556E-16, -150.9375000013656063, 4.458734124999999437 ) ) ;
#60455 = CARTESIAN_POINT ( 'NONE',  ( -4.458734124999999437, -48.56249999863440792, 0.000000000000000000 ) ) ;
#60456 = CARTESIAN_POINT ( 'NONE',  ( -5.000000000000000000, 0.1250000027311869155, 0.000000000000000000 ) ) ;
#60457 = CARTESIAN_POINT ( 'NONE',  ( 2.071067811865475505, -158.8125000000000284, -5.000000000000000888 ) ) ;
#60458 = CARTESIAN_POINT ( 'NONE',  ( -1.339745962155610925, -85.79465819873851729, 5.000000000000000000 ) ) ;
#60459 = CARTESIAN_POINT ( 'NONE',  ( -51.19402409849444524, -153.5000000000000284, -3.242614290531456334 ) ) ;
#60460 = CARTESIAN_POINT ( 'NONE',  ( 4.458734124999998549, -14.97916666530107221, -2.574251347313721627 ) ) ;
#60461 = VECTOR ( 'NONE', #46470, 1000.000000000000000 ) ;
#60462 = CARTESIAN_POINT ( 'NONE',  ( -2.229367062499996610, -53.39583333196773651, 3.861377020970582219 ) ) ;
#60463 = CARTESIAN_POINT ( 'NONE',  ( -1.339745962155613812, -59.08034179853028434, -5.000000000000000000 ) ) ;
#60464 = CARTESIAN_POINT ( 'NONE',  ( 2.730187237215162345E-16, -144.1875000013656063, -4.458734124999999437 ) ) ;
#60465 = CARTESIAN_POINT ( 'NONE',  ( -4.458734124999999437, -94.56249999863440792, 0.000000000000000000 ) ) ;
#60466 = CARTESIAN_POINT ( 'NONE',  ( -57.46284108482265651, -149.9375000000000284, 4.819101127000238627 ) ) ;
#60467 = ORIENTED_EDGE ( 'NONE', *, *, #51450, .F. ) ;
#60468 = CARTESIAN_POINT ( 'NONE',  ( -59.59170313451810586, -152.7500000013655779, 1.485763867205729394 ) ) ;
#60469 = CARTESIAN_POINT ( 'NONE',  ( 2.229367062499998831, 25.10416666803225993, -3.861377020970580887 ) ) ;
#60470 = CARTESIAN_POINT ( 'NONE',  ( -58.80597590150559739, -145.1250000027312126, 3.242614290531460330 ) ) ;
#60471 = CARTESIAN_POINT ( 'NONE',  ( 5.000000000000000000, -50.50000000000000000, -6.123233995736766282E-16 ) ) ;
#60472 = ORIENTED_EDGE ( 'NONE', *, *, #16531, .F. ) ;
#60473 = CARTESIAN_POINT ( 'NONE',  ( 4.458734124999998549, -4.729166665301071326, -2.574251347313721627 ) ) ;
#60474 =( BOUNDED_CURVE ( )  B_SPLINE_CURVE ( 2, ( #21210, #17020, #22167, #7059, #40816, #31171, #50803, #60463, #1932 ),
 .UNSPECIFIED., .F., .F. ) 
 B_SPLINE_CURVE_WITH_KNOTS ( ( 3, 2, 2, 2, 3 ),
 ( 0.6267857142857142794, 0.6273809523809523725, 0.6285714285714285587, 0.6297619047619047450, 0.6303571428571428381 ),
 .UNSPECIFIED. ) 
 CURVE ( )  GEOMETRIC_REPRESENTATION_ITEM ( )  RATIONAL_B_SPLINE_CURVE ( ( 0.9330127018922194093, 0.9330127018922194093, 1.000000000000000000, 0.8660254037844387076, 1.000000000000000000, 0.8660254037844387076, 1.000000000000000000, 0.9330127018922194093, 0.9330127018922194093 ) ) 
 REPRESENTATION_ITEM ( '' )  );
#60475 = CARTESIAN_POINT ( 'NONE',  ( -6.972266317189433020E-16, -106.2500000000000000, -5.000000000000000000 ) ) ;
#60476 = CARTESIAN_POINT ( 'NONE',  ( 4.458734125000001214, -23.14583333196773651, 2.574251347313718519 ) ) ;
#60477 = FACE_OUTER_BOUND ( 'NONE', #53610, .T. ) ;
#60478 = CARTESIAN_POINT ( 'NONE',  ( 2.229367062499998831, -8.645833331967736513, -3.861377020970580887 ) ) ;
#60479 = CARTESIAN_POINT ( 'NONE',  ( 5.000000000000000000, 6.625000002731185944, -6.123233995736766282E-16 ) ) ;
#60480 = CARTESIAN_POINT ( 'NONE',  ( -1.846868145590734756, -150.1250000013655779, -4.458734124999999437 ) ) ;
#60481 = CARTESIAN_POINT ( 'NONE',  ( -2.229367062500000163, 14.27083333469892601, -3.861377020970580443 ) ) ;
#60482 = EDGE_LOOP ( 'NONE', ( #26252, #45140, #7909, #48848 ) ) ;
#60483 = DIRECTION ( 'NONE',  ( 0.000000000000000000, 0.000000000000000000, 1.000000000000000000 ) ) ;
#60484 = CARTESIAN_POINT ( 'NONE',  ( 2.229367062500001939, -21.97916666530107221, 3.861377020970579999 ) ) ;
#60485 = VECTOR ( 'NONE', #43484, 1000.000000000000000 ) ;
#60486 = DIRECTION ( 'NONE',  ( -0.000000000000000000, 1.000000000000000000, -0.000000000000000000 ) ) ;
#60487 = CARTESIAN_POINT ( 'NONE',  ( -52.10840900171896806, -149.1875000013656063, 3.393966926194110556 ) ) ;
#60488 = CARTESIAN_POINT ( 'NONE',  ( -3.535250795749689387E-16, -45.12499999726880162, -5.773502691896257311 ) ) ;
#60489 = CARTESIAN_POINT ( 'NONE',  ( 3.535533905932736864, -150.2500000027312126, 3.535533905932738641 ) ) ;
#60490 = CARTESIAN_POINT ( 'NONE',  ( -2.229367062500000163, 6.520833334698928674, -3.861377020970580443 ) ) ;
#60491 = CARTESIAN_POINT ( 'NONE',  ( 5.000000000000000000, -35.50000000000000711, -6.123233995736766282E-16 ) ) ;
#60492 = CARTESIAN_POINT ( 'NONE',  ( -5.000000000000000000, -47.95833333060215153, -2.886751345948128211 ) ) ;
#60493 = CARTESIAN_POINT ( 'NONE',  ( 2.229367062500001939, 11.02083333469892956, 3.861377020970579999 ) ) ;
#60494 = CARTESIAN_POINT ( 'NONE',  ( 4.458734124999998549, -69.72916666530107932, -2.574251347313721627 ) ) ;
#60495 = CARTESIAN_POINT ( 'NONE',  ( 4.458734124999998549, -14.97916666530107399, -2.574251347313721627 ) ) ;
#60496 = CARTESIAN_POINT ( 'NONE',  ( 2.499999999999998668, 1.666666666666666963, -4.330127018922193649 ) ) ;
#60497 = CARTESIAN_POINT ( 'NONE',  ( 1.846868145590736310, -163.6250000013656063, 4.458734124999999437 ) ) ;
#60498 = LINE ( 'NONE', #31210, #54114 ) ;
#60499 = CARTESIAN_POINT ( 'NONE',  ( 2.229367062500001939, -58.97916666530106511, 3.861377020970579999 ) ) ;
#60500 = CARTESIAN_POINT ( 'NONE',  ( 5.000000000000000888, -93.45833333060214443, 2.886751345948126879 ) ) ;
#60501 = ADVANCED_FACE ( 'NONE', ( #46856 ), #43811, .T. ) ;
#60502 = VECTOR ( 'NONE', #7264, 1000.000000000000000 ) ;
#60503 = CARTESIAN_POINT ( 'NONE',  ( 0.000000000000000000, -120.0000000000000000, 0.000000000000000000 ) ) ;
#60504 = LINE ( 'NONE', #56633, #21362 ) ;
#60505 = CARTESIAN_POINT ( 'NONE',  ( 2.229367062500001939, -35.97916666530107221, 3.861377020970579999 ) ) ;
#60506 = CARTESIAN_POINT ( 'NONE',  ( 2.499999999999998668, 19.79166666939785202, -4.330127018922193649 ) ) ;
#60507 = CARTESIAN_POINT ( 'NONE',  ( -4.999999999999999112, -45.91666666666665719, 2.886751345948131764 ) ) ;
#60508 = CARTESIAN_POINT ( 'NONE',  ( 2.499999999999998668, -13.33333333333333570, -4.330127018922193649 ) ) ;
#60509 = CARTESIAN_POINT ( 'NONE',  ( -1.339745962155727277, -107.7946581987385173, 4.999999999999933387 ) ) ;
#60510 = ORIENTED_EDGE ( 'NONE', *, *, #23403, .F. ) ;
#60511 = CARTESIAN_POINT ( 'NONE',  ( -4.458734124999999437, -109.3124999986343937, 0.000000000000000000 ) ) ;
#60512 = CARTESIAN_POINT ( 'NONE',  ( 4.458734124999998549, -3.979166665301070438, -2.574251347313721627 ) ) ;
#60513 = CARTESIAN_POINT ( 'NONE',  ( 5.000000000000000000, -73.29166666393548724, -2.886751345948130876 ) ) ;
#60514 = CARTESIAN_POINT ( 'NONE',  ( 1.060575238724906964E-15, -6.749999999999999112, 5.773502691896257311 ) ) ;
#60515 = CARTESIAN_POINT ( 'NONE',  ( -4.458734124999999437, -73.39583333196772230, -2.574251347313719407 ) ) ;
#60516 = CARTESIAN_POINT ( 'NONE',  ( 1.975475456537005874E-15, 14.25000000000000000, 5.000000000000000000 ) ) ;
#60517 = EDGE_CURVE ( 'NONE', #46456, #28793, #31057, .T. ) ;
#60518 = CARTESIAN_POINT ( 'NONE',  ( 5.000000000000000888, -7.458333330602143540, 2.886751345948126879 ) ) ;
#60520 = ORIENTED_EDGE ( 'NONE', *, *, #13712, .T. ) ;
#60519 = CARTESIAN_POINT ( 'NONE',  ( -4.458734124999999437, -37.39583333196773651, -2.574251347313719407 ) ) ;
#60521 = CARTESIAN_POINT ( 'NONE',  ( 2.500000000000002220, -6.666666666666667851, 4.330127018922192761 ) ) ;
#60522 = EDGE_CURVE ( 'NONE', #31783, #42322, #44188, .T. ) ;
#60524 = ORIENTED_EDGE ( 'NONE', *, *, #20143, .F. ) ;
#60523 = CARTESIAN_POINT ( 'NONE',  ( -2.229367062499996610, 14.60416666803226171, 3.861377020970582219 ) ) ;
#60525 =( BOUNDED_CURVE ( )  B_SPLINE_CURVE ( 2, ( #45571, #59423, #25318, #44290, #35289, #59100, #25638, #30452, #50077 ),
 .UNSPECIFIED., .F., .F. ) 
 B_SPLINE_CURVE_WITH_KNOTS ( ( 3, 2, 2, 2, 3 ),
 ( 0.5645833333333333259, 0.5652777777777777679, 0.5666666666666666519, 0.5680555555555555358, 0.5687499999999999778 ),
 .UNSPECIFIED. ) 
 CURVE ( )  GEOMETRIC_REPRESENTATION_ITEM ( )  RATIONAL_B_SPLINE_CURVE ( ( 0.9330127018922194093, 0.9330127018922194093, 1.000000000000000000, 0.8660254037844387076, 1.000000000000000000, 0.8660254037844387076, 1.000000000000000000, 0.9330127018922194093, 0.9330127018922194093 ) ) 
 REPRESENTATION_ITEM ( '' )  );
#60526 = CARTESIAN_POINT ( 'NONE',  ( -5.000000000000000000, -55.87499999726880162, 0.000000000000000000 ) ) ;
#60527 = CARTESIAN_POINT ( 'NONE',  ( -5.000000000000000000, -50.08333333333332149, -2.886751345948128211 ) ) ;
#60528 = CARTESIAN_POINT ( 'NONE',  ( -3.152548672688508926E-16, -28.81249999863440436, -5.148502694627439702 ) ) ;
#60529 = VECTOR ( 'NONE', #13027, 1000.000000000000000 ) ;
#60530 = CARTESIAN_POINT ( 'NONE',  ( 1.339745962155612702, -4.294658198738519062, -5.000000000000000000 ) ) ;
#60531 = CARTESIAN_POINT ( 'NONE',  ( 4.458734125000001214, -77.89583333196773651, 2.574251347313718519 ) ) ;
#60532 = CARTESIAN_POINT ( 'NONE',  ( 1.846868145590735200, -141.5000000013655779, -4.458734125000000326 ) ) ;
#60533 = CARTESIAN_POINT ( 'NONE',  ( 4.458734125000001214, -88.89583333196773651, 2.574251347313718519 ) ) ;
#60534 = VECTOR ( 'NONE', #16391, 1000.000000000000000 ) ;
#60535 = CARTESIAN_POINT ( 'NONE',  ( -50.40829686548195099, -133.2500000013656347, -1.485763867205728284 ) ) ;
#60536 = ADVANCED_FACE ( 'NONE', ( #18534 ), #57472, .T. ) ;
#60537 = CARTESIAN_POINT ( 'NONE',  ( 2.229367062500001939, -38.22916666530107221, 3.861377020970579999 ) ) ;
#60538 = CARTESIAN_POINT ( 'NONE',  ( -1.339745962155613812, -94.08034179853028434, -5.000000000000000000 ) ) ;
#60539 = VERTEX_POINT ( 'NONE', #43585 ) ;
#60540 = CARTESIAN_POINT ( 'NONE',  ( -4.458734124999999437, -79.64583333196772230, -2.574251347313719407 ) ) ;
#60541 = DIRECTION ( 'NONE',  ( -0.000000000000000000, 1.000000000000000000, -0.000000000000000000 ) ) ;
#60542 = ORIENTED_EDGE ( 'NONE', *, *, #40149, .F. ) ;
#60543 = CARTESIAN_POINT ( 'NONE',  ( -6.972266317189433020E-16, -4.124999997268814056, -5.000000000000000000 ) ) ;
#60544 = CYLINDRICAL_SURFACE ( 'NONE', #7551, 5.000000000000000000 ) ;
#60545 = CARTESIAN_POINT ( 'NONE',  ( 2.229367062500001939, -64.22916666530106511, 3.861377020970579999 ) ) ;
#60546 = CARTESIAN_POINT ( 'NONE',  ( -4.458734124999999437, -6.645833331967741842, -2.574251347313719407 ) ) ;
#60547 = ORIENTED_EDGE ( 'NONE', *, *, #58924, .F. ) ;
#60548 = CARTESIAN_POINT ( 'NONE',  ( -54.60164318462004474, -149.3750000000000284, -4.984105922594373794 ) ) ;
#60549 = FACE_OUTER_BOUND ( 'NONE', #18053, .T. ) ;
#60550 = ORIENTED_EDGE ( 'NONE', *, *, #40533, .T. ) ;
#60551 = ADVANCED_FACE ( 'NONE', ( #14325 ), #9190, .F. ) ;
#60552 = DIRECTION ( 'NONE',  ( 0.000000000000000000, 0.000000000000000000, 1.000000000000000000 ) ) ;
#60553 = CARTESIAN_POINT ( 'NONE',  ( 4.458734124999999437, 7.187500001365594748, -5.460374474430324690E-16 ) ) ;
#60554 = CARTESIAN_POINT ( 'NONE',  ( -1.339745962155613812, -33.08034179853029144, -5.000000000000000000 ) ) ;
#60555 = CARTESIAN_POINT ( 'NONE',  ( 1.846868145590735200, -162.2500000013656063, -4.458734124999999437 ) ) ;
#60556 = CARTESIAN_POINT ( 'NONE',  ( 0.000000000000000000, -170.0000000000000000, 5.000000000000000000 ) ) ;
#60557 = ORIENTED_EDGE ( 'NONE', *, *, #63292, .F. ) ;
#60558 = CARTESIAN_POINT ( 'NONE',  ( 4.458734125000000326, -87.89583333196773651, 2.574251347313718519 ) ) ;
#60559 = CARTESIAN_POINT ( 'NONE',  ( 5.000000000000000000, -29.29166666393548013, -2.886751345948130876 ) ) ;
#60560 = CARTESIAN_POINT ( 'NONE',  ( -2.229367062500000163, -3.479166665301069994, -3.861377020970580443 ) ) ;
#60561 = CARTESIAN_POINT ( 'NONE',  ( 2.500000000000002220, -71.54166666393547303, 4.330127018922192761 ) ) ;
#60562 = CARTESIAN_POINT ( 'NONE',  ( -2.500000000000000444, -31.04166666393548368, -4.330127018922193649 ) ) ;
#60563 = CARTESIAN_POINT ( 'NONE',  ( 4.458734125000000326, 22.10416666803225993, 2.574251347313718519 ) ) ;
#60564 = CARTESIAN_POINT ( 'NONE',  ( 1.975475456537005874E-15, -55.74999999999999289, 5.000000000000000000 ) ) ;
#60565 = CARTESIAN_POINT ( 'NONE',  ( 4.458734124999999437, 28.18750000136559208, -5.460374474430324690E-16 ) ) ;
#60566 = CARTESIAN_POINT ( 'NONE',  ( 4.458734124999998549, -50.72916666530107932, -2.574251347313721627 ) ) ;
#60567 = CARTESIAN_POINT ( 'NONE',  ( 9.457646018065525792E-16, -36.31249999863440792, 5.148502694627439702 ) ) ;
#60568 = CARTESIAN_POINT ( 'NONE',  ( -3.152548672688508926E-16, 0.1875000013655953035, -5.148502694627439702 ) ) ;
#60569 =( GEOMETRIC_REPRESENTATION_CONTEXT ( 3 ) GLOBAL_UNCERTAINTY_ASSIGNED_CONTEXT ( ( #53236 ) ) GLOBAL_UNIT_ASSIGNED_CONTEXT ( ( #32118, #60780, #62041 ) ) REPRESENTATION_CONTEXT ( 'NONE', 'WORKASPACE' ) );
#60570 =( BOUNDED_CURVE ( )  B_SPLINE_CURVE ( 2, ( #39716, #29420, #59353, #44225, #49051, #5000, #191, #30068, #19790 ),
 .UNSPECIFIED., .F., .F. ) 
 B_SPLINE_CURVE_WITH_KNOTS ( ( 3, 2, 2, 2, 3 ),
 ( 0.7410714285714286031, 0.7416666666666666963, 0.7428571428571428825, 0.7440476190476190688, 0.7446428571428571619 ),
 .UNSPECIFIED. ) 
 CURVE ( )  GEOMETRIC_REPRESENTATION_ITEM ( )  RATIONAL_B_SPLINE_CURVE ( ( 0.9330127018922194093, 0.9330127018922194093, 1.000000000000000000, 0.8660254037844387076, 1.000000000000000000, 0.8660254037844387076, 1.000000000000000000, 0.9330127018922194093, 0.9330127018922194093 ) ) 
 REPRESENTATION_ITEM ( '' )  );
#60571 = LINE ( 'NONE', #51237, #55562 ) ;
#60572 = CARTESIAN_POINT ( 'NONE',  ( -2.500000000000000444, 18.83333333333333215, -4.330127018922193649 ) ) ;
#60573 = CARTESIAN_POINT ( 'NONE',  ( -9.184850993605147944E-16, -145.3750000027312126, 5.000000000000000000 ) ) ;
#60574 = CARTESIAN_POINT ( 'NONE',  ( 5.000000000000000000, -159.0000000000000000, 0.000000000000000000 ) ) ;
#60575 = AXIS2_PLACEMENT_3D ( 'NONE', #4619, #53205, #24244 ) ;
#60576 = CARTESIAN_POINT ( 'NONE',  ( 2.229367062499998831, -41.64583333196773651, -3.861377020970580887 ) ) ;
#60577 = CARTESIAN_POINT ( 'NONE',  ( -5.000000000000000000, -76.87499999726880162, 0.000000000000000000 ) ) ;
#60578 = EDGE_CURVE ( 'NONE', #35769, #62971, #59430, .T. ) ;
#60579 = CARTESIAN_POINT ( 'NONE',  ( -58.39396692619412477, -141.6875000013656063, 2.891590998281057701 ) ) ;
#60580 = CARTESIAN_POINT ( 'NONE',  ( -5.000000000000000888, -140.5625000000000000, -2.071067811865475949 ) ) ;
#60581 = ADVANCED_FACE ( 'NONE', ( #9492 ), #29984, .T. ) ;
#60582 = CARTESIAN_POINT ( 'NONE',  ( 6.123233995736766282E-16, -120.0000000000000000, -5.000000000000000000 ) ) ;
#60583 = EDGE_CURVE ( 'NONE', #63065, #1762, #44779, .T. ) ;
#60584 = CARTESIAN_POINT ( 'NONE',  ( 2.229367062500001939, -79.22916666530106511, 3.861377020970579999 ) ) ;
#60585 = CARTESIAN_POINT ( 'NONE',  ( 4.458734124999999437, -160.6250000013656063, -1.846868145590734978 ) ) ;
#60586 = CARTESIAN_POINT ( 'NONE',  ( -7.847095227763516867, -4.129731495738496960, -7.493596212620239783 ) ) ;
#60587 = CARTESIAN_POINT ( 'NONE',  ( -5.000000000000000000, -29.08333333333332860, -2.886751345948128211 ) ) ;
#60588 = CARTESIAN_POINT ( 'NONE',  ( -3.152801135295367096, -140.0625000013655779, -3.152801135295367541 ) ) ;
#60589 = ORIENTED_EDGE ( 'NONE', *, *, #49598, .F. ) ;
#60590 = CARTESIAN_POINT ( 'NONE',  ( -4.458734124999999437, 23.35416666803226349, -2.574251347313719407 ) ) ;
#60591 = ORIENTED_EDGE ( 'NONE', *, *, #16209, .F. ) ;
#60592 = CARTESIAN_POINT ( 'NONE',  ( 9.457646018065525792E-16, -89.06249999863439371, 5.148502694627439702 ) ) ;
#60593 = CARTESIAN_POINT ( 'NONE',  ( -4.458734124999999437, 12.35416666803225993, -2.574251347313719407 ) ) ;
#60594 = CARTESIAN_POINT ( 'NONE',  ( 5.000000000000000888, 15.54166666939785024, 2.886751345948126879 ) ) ;
#60595 = CARTESIAN_POINT ( 'NONE',  ( -2.500000000000000444, -61.04166666393547303, -4.330127018922193649 ) ) ;
#60596 = CARTESIAN_POINT ( 'NONE',  ( 2.500000000000002220, 8.333333333333332149, 4.330127018922192761 ) ) ;
#60597 = EDGE_CURVE ( 'NONE', #2792, #10271, #39949, .T. ) ;
#60598 = CARTESIAN_POINT ( 'NONE',  ( 4.458734124999999437, -56.81249999863440081, -5.460374474430324690E-16 ) ) ;
#60599 = CARTESIAN_POINT ( 'NONE',  ( -4.458734124999999437, -9.312499998634406140, 0.000000000000000000 ) ) ;
#60600 = CARTESIAN_POINT ( 'NONE',  ( -6.972266317189433020E-16, -5.124999997268812280, -5.000000000000000000 ) ) ;
#60601 = CARTESIAN_POINT ( 'NONE',  ( -52.80376928212989185, -135.1250000013656063, -4.297418129356378458 ) ) ;
#60602 = CARTESIAN_POINT ( 'NONE',  ( -5.000000000000000000, 13.99999999999999822, 0.000000000000000000 ) ) ;
#60603 = CARTESIAN_POINT ( 'NONE',  ( -6.972266317189433020E-16, -64.24999999999998579, -5.000000000000000000 ) ) ;
#60604 = ADVANCED_FACE ( 'NONE', ( #15530 ), #47481, .T. ) ;
#60605 = CARTESIAN_POINT ( 'NONE',  ( -6.972266317189433020E-16, -22.24999999999999645, -5.000000000000000000 ) ) ;
#60606 = CARTESIAN_POINT ( 'NONE',  ( 5.000000000000000000, -36.41666666666666430, -2.886751345948129988 ) ) ;
#60607 = CARTESIAN_POINT ( 'NONE',  ( 2.499999999999998668, -74.33333333333332860, -4.330127018922193649 ) ) ;
#60609 = CARTESIAN_POINT ( 'NONE',  ( -4.458734124999999437, -16.64583333196773651, -2.574251347313719407 ) ) ;
#60608 = CARTESIAN_POINT ( 'NONE',  ( -2.499999999999996447, -33.83333333333332860, 4.330127018922195425 ) ) ;
#60610 = DIRECTION ( 'NONE',  ( -0.000000000000000000, 1.000000000000000000, -0.000000000000000000 ) ) ;
#60611 = CARTESIAN_POINT ( 'NONE',  ( 4.458734125000001214, -61.89583333196773651, 2.574251347313718519 ) ) ;
#60612 = CARTESIAN_POINT ( 'NONE',  ( 1.846868145590736310, -153.8750000013655779, 4.458734124999999437 ) ) ;
#60613 = CARTESIAN_POINT ( 'NONE',  ( -3.152548672688508926E-16, -71.56249999863440792, -5.148502694627439702 ) ) ;
#60614 = CARTESIAN_POINT ( 'NONE',  ( -59.29741812935640155, -147.8750000013656063, -2.196230717870135685 ) ) ;
#60615 = CARTESIAN_POINT ( 'NONE',  ( -5.000000000000000000, -60.87499999726880873, 0.000000000000000000 ) ) ;
#60616 = ORIENTED_EDGE ( 'NONE', *, *, #19300, .T. ) ;
#60617 = CARTESIAN_POINT ( 'NONE',  ( -2.071067811865604735, -150.3125000000000284, 4.999999999999872990 ) ) ;
#60618 = ORIENTED_EDGE ( 'NONE', *, *, #20787, .T. ) ;
#60620 = CARTESIAN_POINT ( 'NONE',  ( 1.339745962155615144, -103.7053418012614827, 4.999999999999999112 ) ) ;
#60619 = CARTESIAN_POINT ( 'NONE',  ( -6.972266317189433020E-16, -4.249999999999997335, -5.000000000000000000 ) ) ;
#60621 = CARTESIAN_POINT ( 'NONE',  ( 4.458734124999999437, -153.4375000013655779, 0.000000000000000000 ) ) ;
#60622 = ORIENTED_EDGE ( 'NONE', *, *, #26451, .F. ) ;
#60623 = CARTESIAN_POINT ( 'NONE',  ( 2.500000000000002220, -54.66666666666667140, 4.330127018922192761 ) ) ;
#60624 = CARTESIAN_POINT ( 'NONE',  ( -55.39835681537999790, -127.8750000000000142, 4.984105922594378235 ) ) ;
#60626 = CIRCLE ( 'NONE', #50319, 5.000000000000000000 ) ;
#60625 = CARTESIAN_POINT ( 'NONE',  ( -9.184850993605147944E-16, -161.3750000027311842, 5.000000000000000000 ) ) ;
#60627 = CARTESIAN_POINT ( 'NONE',  ( 4.458734124999998549, -47.97916666530107221, -2.574251347313721627 ) ) ;
#60628 = ORIENTED_EDGE ( 'NONE', *, *, #54683, .F. ) ;
#60629 = CARTESIAN_POINT ( 'NONE',  ( -3.535533905932738641, -145.3750000000000000, 3.535533905932737309 ) ) ;
#60630 = CARTESIAN_POINT ( 'NONE',  ( 4.458734124999998549, 16.27083333469892779, -2.574251347313721627 ) ) ;
#60631 = CARTESIAN_POINT ( 'NONE',  ( -2.229367062500000163, 22.52083333469892423, -3.861377020970580443 ) ) ;
#60632 = CARTESIAN_POINT ( 'NONE',  ( -59.59170313451811296, -150.5000000013655779, 1.485763867205729394 ) ) ;
#60633 = CARTESIAN_POINT ( 'NONE',  ( 5.000000000000000000, -108.2916666639354730, -2.886751345948130876 ) ) ;
#60634 = CARTESIAN_POINT ( 'NONE',  ( -2.500000000000000444, -36.04166666393547303, -4.330127018922193649 ) ) ;
#60635 = EDGE_LOOP ( 'NONE', ( #35848, #14131, #9002, #20567 ) ) ;
#60636 = CARTESIAN_POINT ( 'NONE',  ( -4.458734124999999437, -65.39583333196773651, -2.574251347313719407 ) ) ;
#60637 = CARTESIAN_POINT ( 'NONE',  ( 0.6169862416622686752, 8.783631307150953305, -7.913704048099833521 ) ) ;
#60638 = CARTESIAN_POINT ( 'NONE',  ( 2.229367062499998831, 13.35416666803226171, -3.861377020970580887 ) ) ;
#60639 = CARTESIAN_POINT ( 'NONE',  ( -6.972266317189433020E-16, -57.25000000000000000, -5.000000000000000000 ) ) ;
#60640 = CARTESIAN_POINT ( 'NONE',  ( -51.19402409849444524, -152.6250000027312126, -3.242614290531456334 ) ) ;
#60641 = CARTESIAN_POINT ( 'NONE',  ( 9.457646018065525792E-16, -52.31249999863440792, 5.148502694627439702 ) ) ;
#60642 = CARTESIAN_POINT ( 'NONE',  ( 5.000000000000000000, -13.37499999726881050, -6.123233995736766282E-16 ) ) ;
#60643 = CARTESIAN_POINT ( 'NONE',  ( -57.46284108482265651, -146.9375000000000000, 4.819101127000238627 ) ) ;
#60644 = DIRECTION ( 'NONE',  ( -0.8660254037844387076, 0.000000000000000000, -0.4999999999999997780 ) ) ;
#60645 = CARTESIAN_POINT ( 'NONE',  ( 2.229367062499998831, -19.89583333196774007, -3.861377020970580887 ) ) ;
#60646 = VERTEX_POINT ( 'NONE', #56043 ) ;
#60647 = CARTESIAN_POINT ( 'NONE',  ( -6.972266317189433020E-16, -5.124999997268812280, -5.000000000000000000 ) ) ;
#60648 = CARTESIAN_POINT ( 'NONE',  ( 4.458734124999998549, -101.7291666653010793, -2.574251347313721627 ) ) ;
#60649 = CARTESIAN_POINT ( 'NONE',  ( -9.184850993605147944E-16, -158.3750000027311842, 5.000000000000000000 ) ) ;
#60650 = ORIENTED_EDGE ( 'NONE', *, *, #49530, .T. ) ;
#60651 = CARTESIAN_POINT ( 'NONE',  ( -4.458734124999999437, -104.5624999986344079, 0.000000000000000000 ) ) ;
#60652 = CARTESIAN_POINT ( 'NONE',  ( -4.458734124999999437, -29.39583333196773296, -2.574251347313719407 ) ) ;
#60653 = CARTESIAN_POINT ( 'NONE',  ( 5.000000000000000888, -64.45833333060213022, 2.886751345948126879 ) ) ;
#60654 =( BOUNDED_CURVE ( )  B_SPLINE_CURVE ( 2, ( #1708, #50255, #21314, #30953, #11644, #6204, #50579, #45112, #6522 ),
 .UNSPECIFIED., .F., .F. ) 
 B_SPLINE_CURVE_WITH_KNOTS ( ( 3, 2, 2, 2, 3 ),
 ( 0.02708333333333333426, 0.02777777777777777624, 0.02916666666666666713, 0.03055555555555555455, 0.03125000000000000000 ),
 .UNSPECIFIED. ) 
 CURVE ( )  GEOMETRIC_REPRESENTATION_ITEM ( )  RATIONAL_B_SPLINE_CURVE ( ( 0.9330127018922194093, 0.9330127018922195203, 1.000000000000000000, 0.8660254037844387076, 1.000000000000000000, 0.8660254037844387076, 1.000000000000000000, 0.9330127018922191873, 0.9330127018922194093 ) ) 
 REPRESENTATION_ITEM ( '' )  );
#60655 = CARTESIAN_POINT ( 'NONE',  ( -58.39396692619412477, -151.6875000013656063, 2.891590998281057701 ) ) ;
#60656 = CARTESIAN_POINT ( 'NONE',  ( -50.40829686548195099, -144.0000000013656063, -1.485763867205728284 ) ) ;
#60657 = EDGE_CURVE ( 'NONE', #1513, #50070, #30948, .T. ) ;
#60658 = CARTESIAN_POINT ( 'NONE',  ( -4.458734124999997661, -23.22916666530107221, 2.574251347313722516 ) ) ;
#60659 = CARTESIAN_POINT ( 'NONE',  ( 4.458734124999999437, -66.06249999863440792, -5.460374474430324690E-16 ) ) ;
#60660 = CARTESIAN_POINT ( 'NONE',  ( -4.458734124999997661, -18.22916666530106866, 2.574251347313722516 ) ) ;
#60661 = CARTESIAN_POINT ( 'NONE',  ( 5.000000000000000000, -147.0000000000000284, 0.000000000000000000 ) ) ;
#60662 = CARTESIAN_POINT ( 'NONE',  ( 5.000000000000000000, -149.0625000000000000, 2.071067811865478614 ) ) ;
#60663 = CARTESIAN_POINT ( 'NONE',  ( 5.000000000000000000, -9.500000000000001776, -6.123233995736766282E-16 ) ) ;
#60664 = CARTESIAN_POINT ( 'NONE',  ( 4.458734124999999437, -151.5000000013655779, 1.846868145590737864 ) ) ;
#60665 = EDGE_LOOP ( 'NONE', ( #60272, #62045, #20966, #51414 ) ) ;
#60666 = AXIS2_PLACEMENT_3D ( 'NONE', #32705, #37528, #52334 ) ;
#60667 = CARTESIAN_POINT ( 'NONE',  ( 2.229367062500001939, -51.22916666530107221, 3.861377020970579999 ) ) ;
#60668 = CARTESIAN_POINT ( 'NONE',  ( 1.339745962155565406, -2.705341801261481383, 5.000000000000028422 ) ) ;
#60669 = CARTESIAN_POINT ( 'NONE',  ( -59.98410592259440222, -136.1250000000000284, -0.3983568153799752487 ) ) ;
#60670 = CARTESIAN_POINT ( 'NONE',  ( -3.535250795749689387E-16, 29.74999999999999645, -5.773502691896257311 ) ) ;
#60671 = ADVANCED_FACE ( 'NONE', ( #11324 ), #21630, .F. ) ;
#60672 = DIRECTION ( 'NONE',  ( 0.000000000000000000, 0.000000000000000000, 1.000000000000000000 ) ) ;
#60673 = CARTESIAN_POINT ( 'NONE',  ( -2.229367062499996610, 1.854166668032262377, 3.861377020970582219 ) ) ;
#60674 =( BOUNDED_CURVE ( )  B_SPLINE_CURVE ( 2, ( #38040, #21988, #42228, #12336, #51578, #61872, #13598, #12956, #46742 ),
 .UNSPECIFIED., .F., .F. ) 
 B_SPLINE_CURVE_WITH_KNOTS ( ( 3, 2, 2, 2, 3 ),
 ( 0.4479166666666666852, 0.4486111111111111271, 0.4500000000000000111, 0.4513888888888888951, 0.4520833333333333370 ),
 .UNSPECIFIED. ) 
 CURVE ( )  GEOMETRIC_REPRESENTATION_ITEM ( )  RATIONAL_B_SPLINE_CURVE ( ( 0.9330127018922194093, 0.9330127018922194093, 1.000000000000000000, 0.8660254037844387076, 1.000000000000000000, 0.8660254037844387076, 1.000000000000000000, 0.9330127018922194093, 0.9330127018922194093 ) ) 
 REPRESENTATION_ITEM ( '' )  );
#60675 = CARTESIAN_POINT ( 'NONE',  ( -6.972266317189433020E-16, -82.12499999726881583, -5.000000000000000000 ) ) ;
#60676 = CARTESIAN_POINT ( 'NONE',  ( 2.499999999999998668, -17.33333333333333215, -4.330127018922193649 ) ) ;
#60677 = CARTESIAN_POINT ( 'NONE',  ( -3.152548672688508926E-16, 15.18750000136559386, -5.148502694627439702 ) ) ;
#60678 = CARTESIAN_POINT ( 'NONE',  ( 1.060575238724906964E-15, 4.375000002731186832, 5.773502691896257311 ) ) ;
#60680 = ORIENTED_EDGE ( 'NONE', *, *, #18833, .F. ) ;
#60679 = ADVANCED_FACE ( 'NONE', ( #30304 ), #50894, .T. ) ;
#60681 = CARTESIAN_POINT ( 'NONE',  ( 75.00000000000000000, 15.00000000000000000, 8.999999999999998224 ) ) ;
#60682 = ORIENTED_EDGE ( 'NONE', *, *, #43376, .F. ) ;
#60683 = DIRECTION ( 'NONE',  ( -0.000000000000000000, 1.000000000000000000, -0.000000000000000000 ) ) ;
#60684 = CARTESIAN_POINT ( 'NONE',  ( 9.457646018065525792E-16, -46.06249999863440081, 5.148502694627439702 ) ) ;
#60685 = ADVANCED_FACE ( 'NONE', ( #40596 ), #2334, .T. ) ;
#60686 = CARTESIAN_POINT ( 'NONE',  ( 3.152801135295366208, -163.8125000013656063, 3.152801135295367985 ) ) ;
#60687 = ADVANCED_FACE ( 'NONE', ( #5878 ), #60240, .T. ) ;
#60688 = CARTESIAN_POINT ( 'NONE',  ( 5.000000000000000000, -40.37499999726880162, -6.123233995736766282E-16 ) ) ;
#60689 = VERTEX_POINT ( 'NONE', #50574 ) ;
#60690 = CARTESIAN_POINT ( 'NONE',  ( 2.229367062499998831, -16.64583333196773651, -3.861377020970580887 ) ) ;
#60691 = ORIENTED_EDGE ( 'NONE', *, *, #19949, .T. ) ;
#60692 = CARTESIAN_POINT ( 'NONE',  ( -3.535250795749689387E-16, -86.25000000000000000, -5.773502691896257311 ) ) ;
#60693 = CARTESIAN_POINT ( 'NONE',  ( 4.458734125000000326, -165.3750000013656347, -1.846868145590734978 ) ) ;
#60695 = ORIENTED_EDGE ( 'NONE', *, *, #53788, .T. ) ;
#60694 = CARTESIAN_POINT ( 'NONE',  ( -2.499999999999996447, -34.70833333060213732, 4.330127018922195425 ) ) ;
#60696 = CARTESIAN_POINT ( 'NONE',  ( -58.24261429053147765, -141.2500000000000284, -3.805975901505573855 ) ) ;
#60697 = CARTESIAN_POINT ( 'NONE',  ( 4.458734124999998549, -32.97916666530106511, -2.574251347313721627 ) ) ;
#60698 = CARTESIAN_POINT ( 'NONE',  ( -1.339745962155610925, -38.79465819873851729, 5.000000000000000000 ) ) ;
#60699 = ORIENTED_EDGE ( 'NONE', *, *, #48201, .F. ) ;
#60700 = CARTESIAN_POINT ( 'NONE',  ( 4.458734124999998549, -78.72916666530106511, -2.574251347313721627 ) ) ;
#60701 = CARTESIAN_POINT ( 'NONE',  ( 4.458734124999998549, -107.9791666653010651, -2.574251347313721627 ) ) ;
#60702 = CARTESIAN_POINT ( 'NONE',  ( -58.24261429053147765, -137.3750000027312126, -3.805975901505573855 ) ) ;
#60703 = ORIENTED_EDGE ( 'NONE', *, *, #50764, .T. ) ;
#60704 = CARTESIAN_POINT ( 'NONE',  ( -3.535533905932737309, -161.6250000000000284, -3.535533905932738197 ) ) ;
#60705 = CARTESIAN_POINT ( 'NONE',  ( -50.70258187064364108, -141.3750000013656063, 2.196230717870141014 ) ) ;
#60706 = VECTOR ( 'NONE', #50755, 1000.000000000000114 ) ;
#60707 = CARTESIAN_POINT ( 'NONE',  ( 4.458734125000001214, -80.14583333196773651, 2.574251347313718519 ) ) ;
#60708 = CARTESIAN_POINT ( 'NONE',  ( -56.66612745406270335, -134.4375000027312410, -5.149110718188516067 ) ) ;
#60709 = CARTESIAN_POINT ( 'NONE',  ( 5.000000000000000000, 0.6250000027311873874, -6.123233995736766282E-16 ) ) ;
#60710 = CARTESIAN_POINT ( 'NONE',  ( 4.458734124999997661, -143.7500000013655779, 1.846868145590737864 ) ) ;
#60711 = CARTESIAN_POINT ( 'NONE',  ( 9.457646018065525792E-16, -51.06249999863440792, 5.148502694627439702 ) ) ;
#60712 = CARTESIAN_POINT ( 'NONE',  ( 2.229367062500001939, -43.97916666530106511, 3.861377020970579999 ) ) ;
#60713 = CARTESIAN_POINT ( 'NONE',  ( 2.499999999999998668, -105.3333333333333286, -4.330127018922193649 ) ) ;
#60714 = CARTESIAN_POINT ( 'NONE',  ( 1.975475456537005874E-15, -3.750000000000001776, 5.000000000000000000 ) ) ;
#60715 = CARTESIAN_POINT ( 'NONE',  ( 2.229367062500001939, -41.22916666530107932, 3.861377020970579999 ) ) ;
#60716 = CARTESIAN_POINT ( 'NONE',  ( 2.499999999999998668, -1.208333330602148870, -4.330127018922193649 ) ) ;
#60717 = CARTESIAN_POINT ( 'NONE',  ( 1.339745962155612702, 16.83034180399266688, -5.000000000000000000 ) ) ;
#60718 = CARTESIAN_POINT ( 'NONE',  ( -57.89159099828107458, -128.6875000013656063, -3.393966926194107447 ) ) ;
#60719 = CARTESIAN_POINT ( 'NONE',  ( 2.229367062499998831, -79.89583333196773651, -3.861377020970580887 ) ) ;
#60720 = CARTESIAN_POINT ( 'NONE',  ( 1.339745962155612702, -71.29465819873850307, -5.000000000000000000 ) ) ;
#60721 = CARTESIAN_POINT ( 'NONE',  ( 4.458734125000000326, -95.89583333196773651, 2.574251347313718519 ) ) ;
#60722 = CARTESIAN_POINT ( 'NONE',  ( -4.458734124999997661, -1.479166665301071992, 2.574251347313722516 ) ) ;
#60723 =( BOUNDED_CURVE ( )  B_SPLINE_CURVE ( 2, ( #22309, #16839, #51270, #47380, #7832, #26813, #22631, #56414, #7518 ),
 .UNSPECIFIED., .F., .F. ) 
 B_SPLINE_CURVE_WITH_KNOTS ( ( 3, 2, 2, 2, 3 ),
 ( 0.1312500000000000056, 0.1319444444444444475, 0.1333333333333333315, 0.1347222222222222154, 0.1354166666666666574 ),
 .UNSPECIFIED. ) 
 CURVE ( )  GEOMETRIC_REPRESENTATION_ITEM ( )  RATIONAL_B_SPLINE_CURVE ( ( 0.9330127018922194093, 0.9330127018922194093, 1.000000000000000000, 0.8660254037844387076, 1.000000000000000000, 0.8660254037844387076, 1.000000000000000000, 0.9330127018922194093, 0.9330127018922194093 ) ) 
 REPRESENTATION_ITEM ( '' )  );
#60724 = ORIENTED_EDGE ( 'NONE', *, *, #47925, .F. ) ;
#60725 = CARTESIAN_POINT ( 'NONE',  ( -58.24261429053147765, -139.2500000000000000, -3.805975901505573855 ) ) ;
#60726 = CARTESIAN_POINT ( 'NONE',  ( -6.972266317189433020E-16, -15.12499999726881050, -5.000000000000000000 ) ) ;
#60727 = CARTESIAN_POINT ( 'NONE',  ( 4.458734124999998549, -87.72916666530107932, -2.574251347313721627 ) ) ;
#60728 = CARTESIAN_POINT ( 'NONE',  ( 0.000000000000000000, -120.0000000000000000, 0.000000000000000000 ) ) ;
#60729 = CARTESIAN_POINT ( 'NONE',  ( 9.457646018065525792E-16, -87.31249999863440792, 5.148502694627439702 ) ) ;
#60730 = CARTESIAN_POINT ( 'NONE',  ( 4.458734125000000326, 11.85416666803225993, 2.574251347313718519 ) ) ;
#60731 = CARTESIAN_POINT ( 'NONE',  ( -6.031010364368858512E-14, 3.375000002731183280, 5.000000000000000000 ) ) ;
#60733 = EDGE_CURVE ( 'NONE', #14373, #50115, #11959, .T. ) ;
#60732 = CARTESIAN_POINT ( 'NONE',  ( -59.59170313451811296, -135.5000000013656063, 1.485763867205729394 ) ) ;
#60734 = CARTESIAN_POINT ( 'NONE',  ( 4.458734125000000326, -6.895833331967734736, 2.574251347313718519 ) ) ;
#60735 = CARTESIAN_POINT ( 'NONE',  ( 4.458734124999998549, 17.02083333469892423, -2.574251347313721627 ) ) ;
#60736 = CARTESIAN_POINT ( 'NONE',  ( -4.458734124999999437, -48.64583333196773651, -2.574251347313719407 ) ) ;
#60737 = CARTESIAN_POINT ( 'NONE',  ( -1.339745962155613812, -14.08034179853029144, -5.000000000000000000 ) ) ;
#60738 = CARTESIAN_POINT ( 'NONE',  ( -2.229367062499996610, -85.14583333196773651, 3.861377020970582219 ) ) ;
#60739 = CARTESIAN_POINT ( 'NONE',  ( 4.458734124999998549, -2.729166665301069550, -2.574251347313721627 ) ) ;
#60740 = CARTESIAN_POINT ( 'NONE',  ( -5.000000000000000000, -31.08333333333332860, -2.886751345948128211 ) ) ;
#60741 = EDGE_LOOP ( 'NONE', ( #2971, #39419, #9401, #39950 ) ) ;
#60742 = CARTESIAN_POINT ( 'NONE',  ( -3.152548672688508926E-16, -32.81249999863440792, -5.148502694627439702 ) ) ;
#60743 = CARTESIAN_POINT ( 'NONE',  ( -57.19623071787017210, -131.6250000013655779, 4.297418129356382899 ) ) ;
#60744 = CARTESIAN_POINT ( 'NONE',  ( 2.229367062499998831, -74.64583333196773651, -3.861377020970580887 ) ) ;
#60745 = CARTESIAN_POINT ( 'NONE',  ( 1.060575238724906964E-15, -110.6249999972687874, 5.773502691896257311 ) ) ;
#60746 = CARTESIAN_POINT ( 'NONE',  ( 9.457646018065525792E-16, 19.93750000136559208, 5.148502694627439702 ) ) ;
#60747 = CARTESIAN_POINT ( 'NONE',  ( -1.339745962155610925, -57.66965819600732601, 5.000000000000000000 ) ) ;
#60748 = CARTESIAN_POINT ( 'NONE',  ( 1.975475456537005874E-15, 1.250000000000000000, 5.000000000000000000 ) ) ;
#60749 = CARTESIAN_POINT ( 'NONE',  ( -2.229367062500000163, -78.72916666530106511, -3.861377020970580443 ) ) ;
#60750 = CARTESIAN_POINT ( 'NONE',  ( -3.535250795749689387E-16, -66.25000000000000000, -5.773502691896257311 ) ) ;
#60751 = DIRECTION ( 'NONE',  ( 0.000000000000000000, 0.000000000000000000, 1.000000000000000000 ) ) ;
#60752 = CARTESIAN_POINT ( 'NONE',  ( -2.500000000000000444, 17.95833333606451632, -4.330127018922193649 ) ) ;
#60753 = ORIENTED_EDGE ( 'NONE', *, *, #62515, .T. ) ;
#60754 = FACE_OUTER_BOUND ( 'NONE', #63071, .T. ) ;
#60755 =( BOUNDED_CURVE ( )  B_SPLINE_CURVE ( 2, ( #48387, #466, #4329, #53841, #49337, #29070, #5281, #24900, #39673 ),
 .UNSPECIFIED., .F., .F. ) 
 B_SPLINE_CURVE_WITH_KNOTS ( ( 3, 2, 2, 2, 3 ),
 ( 0.3229166666666666852, 0.3236111111111111271, 0.3250000000000000111, 0.3263888888888888951, 0.3270833333333333370 ),
 .UNSPECIFIED. ) 
 CURVE ( )  GEOMETRIC_REPRESENTATION_ITEM ( )  RATIONAL_B_SPLINE_CURVE ( ( 0.9330127018922194093, 0.9330127018922194093, 1.000000000000000000, 0.8660254037844387076, 1.000000000000000000, 0.8660254037844387076, 1.000000000000000000, 0.9330127018922194093, 0.9330127018922194093 ) ) 
 REPRESENTATION_ITEM ( '' )  );
#60756 = CARTESIAN_POINT ( 'NONE',  ( -5.000000000000000888, -168.6875000027311842, -2.071067811865475949 ) ) ;
#60758 = CARTESIAN_POINT ( 'NONE',  ( -5.000000000000000000, -23.08333333333332860, -2.886751345948128211 ) ) ;
#60757 = CARTESIAN_POINT ( 'NONE',  ( 1.339745962155615144, -0.7053418012614794952, 4.999999999999999112 ) ) ;
#60759 = CARTESIAN_POINT ( 'NONE',  ( -3.152548672688508926E-16, -28.56249999863440436, -5.148502694627439702 ) ) ;
#60760 = AXIS2_PLACEMENT_3D ( 'NONE', #8150, #28068, #3329 ) ;
#60761 = CARTESIAN_POINT ( 'NONE',  ( 2.229367062500001939, -89.97916666530106511, 3.861377020970579999 ) ) ;
#60762 = CARTESIAN_POINT ( 'NONE',  ( 2.500000000000002220, -25.54166666393547658, 4.330127018922192761 ) ) ;
#60764 = ORIENTED_EDGE ( 'NONE', *, *, #8923, .T. ) ;
#60763 = CARTESIAN_POINT ( 'NONE',  ( -4.458734124999998549, -57.22916666530107932, 2.574251347313722516 ) ) ;
#60765 = CARTESIAN_POINT ( 'NONE',  ( 1.339745962155615144, -49.70534180126148271, 4.999999999999999112 ) ) ;
#60766 = DIRECTION ( 'NONE',  ( 0.000000000000000000, 0.000000000000000000, 1.000000000000000000 ) ) ;
#60768 = ORIENTED_EDGE ( 'NONE', *, *, #6440, .F. ) ;
#60767 = CARTESIAN_POINT ( 'NONE',  ( 2.229367062500001939, -4.229166665301070438, 3.861377020970579999 ) ) ;
#60769 = CARTESIAN_POINT ( 'NONE',  ( 2.500000000000002220, -71.66666666666667140, 4.330127018922192761 ) ) ;
#60770 = CARTESIAN_POINT ( 'NONE',  ( -56.48576386720575471, -138.7500000013655779, -4.591703134518078322 ) ) ;
#60771 = CARTESIAN_POINT ( 'NONE',  ( 4.458734124999998549, -44.97916666530107221, -2.574251347313721627 ) ) ;
#60772 = DIRECTION ( 'NONE',  ( -0.000000000000000000, 1.000000000000000000, -0.000000000000000000 ) ) ;
#60773 = CARTESIAN_POINT ( 'NONE',  ( 2.071067811865476394, -159.1875000000000000, 5.000000000000000000 ) ) ;
#60774 = CARTESIAN_POINT ( 'NONE',  ( -4.999999999999999112, -71.79166666393547303, 2.886751345948131764 ) ) ;
#60775 = CARTESIAN_POINT ( 'NONE',  ( -5.000000000000000000, -21.87499999726881228, 0.000000000000000000 ) ) ;
#60776 = CARTESIAN_POINT ( 'NONE',  ( -56.66612745406270335, -154.3125000000000284, -5.149110718188516067 ) ) ;
#60777 = CARTESIAN_POINT ( 'NONE',  ( 4.458734124999999437, -17.06249999863440792, -5.460374474430324690E-16 ) ) ;
#60778 = CARTESIAN_POINT ( 'NONE',  ( 4.458734125000001214, -54.14583333196773651, 2.574251347313718519 ) ) ;
#60779 = CARTESIAN_POINT ( 'NONE',  ( 5.000000000000000000, 10.58333333333333393, -2.886751345948130876 ) ) ;
#60780 =( NAMED_UNIT ( * ) PLANE_ANGLE_UNIT ( ) SI_UNIT ( $, .RADIAN. ) );
#60781 = CARTESIAN_POINT ( 'NONE',  ( 1.846868145590735200, -143.2500000013655779, -4.458734125000000326 ) ) ;
#60782 = CARTESIAN_POINT ( 'NONE',  ( 4.458734124999998549, -91.97916666530107932, -2.574251347313721627 ) ) ;
#60783 = CARTESIAN_POINT ( 'NONE',  ( 0.000000000000000000, -170.0000000000000000, 5.000000000000000000 ) ) ;
#60784 = ORIENTED_EDGE ( 'NONE', *, *, #51104, .F. ) ;
#60785 = CARTESIAN_POINT ( 'NONE',  ( 0.000000000000000000, -170.0000000000000000, 5.000000000000000000 ) ) ;
#60786 = CARTESIAN_POINT ( 'NONE',  ( -2.229367062499996610, 24.60416666803225993, 3.861377020970582219 ) ) ;
#60787 = CARTESIAN_POINT ( 'NONE',  ( -58.24261429053147765, -147.3750000027312126, -3.805975901505573855 ) ) ;
#60788 = CYLINDRICAL_SURFACE ( 'NONE', #4457, 5.000000000000000000 ) ;
#60789 = CARTESIAN_POINT ( 'NONE',  ( 2.229367062500001939, -2.979166665301069550, 3.861377020970579999 ) ) ;
#60790 = CARTESIAN_POINT ( 'NONE',  ( -1.846868145590737420, -149.0000000013656063, 4.458734124999999437 ) ) ;
#60791 = CARTESIAN_POINT ( 'NONE',  ( 9.457646018065525792E-16, -24.31249999863440792, 5.148502694627439702 ) ) ;
#60792 = CARTESIAN_POINT ( 'NONE',  ( 2.229367062499998831, -62.89583333196774362, -3.861377020970580887 ) ) ;
#60793 = CARTESIAN_POINT ( 'NONE',  ( 4.729367062499999719, -139.8437500006828031, 0.000000000000000000 ) ) ;
#60794 = CARTESIAN_POINT ( 'NONE',  ( -2.229367062500000163, -8.479166665301073991, -3.861377020970580443 ) ) ;
#60795 = CARTESIAN_POINT ( 'NONE',  ( -1.339745962155610925, 17.20534180126147916, 5.000000000000000000 ) ) ;
#60796 = CARTESIAN_POINT ( 'NONE',  ( -3.152801135295367985, -143.8125000013655779, 3.152801135295367096 ) ) ;
#60797 = CARTESIAN_POINT ( 'NONE',  ( 2.229367062499998831, 14.10416666803226171, -3.861377020970580887 ) ) ;
#60798 = EDGE_LOOP ( 'NONE', ( #48957, #18267, #16542, #63357 ) ) ;
#60799 = CARTESIAN_POINT ( 'NONE',  ( 1.975475456537005874E-15, -18.62499999726881228, 5.000000000000000000 ) ) ;
#60801 = CARTESIAN_POINT ( 'NONE',  ( 4.458734125000001214, -18.89583333196773651, 2.574251347313718519 ) ) ;
#60800 = CARTESIAN_POINT ( 'NONE',  ( -5.000000000000000000, -84.99999999999998579, 0.000000000000000000 ) ) ;
#60802 = CARTESIAN_POINT ( 'NONE',  ( -3.152548672688508926E-16, 27.18750000136559564, -5.148502694627439702 ) ) ;
#60803 = CARTESIAN_POINT ( 'NONE',  ( 1.339745962155612702, -88.16965819600733312, -5.000000000000000000 ) ) ;
#60804 = CARTESIAN_POINT ( 'NONE',  ( -57.89159099828107458, -150.6875000013656063, -3.393966926194107447 ) ) ;
#60805 = CARTESIAN_POINT ( 'NONE',  ( 5.000000000000000000, -44.29166666393546592, -2.886751345948129988 ) ) ;
#60806 = CARTESIAN_POINT ( 'NONE',  ( 5.000000000000000000, -150.1250000027312126, 0.000000000000000000 ) ) ;
#60807 = CARTESIAN_POINT ( 'NONE',  ( -4.458734124999999437, 8.604166668032261711, -2.574251347313719407 ) ) ;
#60808 = FACE_OUTER_BOUND ( 'NONE', #58783, .T. ) ;
#60809 = UNCERTAINTY_MEASURE_WITH_UNIT (LENGTH_MEASURE( 1.000000000000000082E-05 ), #29172, 'distance_accuracy_value', 'NONE');
#60810 = CARTESIAN_POINT ( 'NONE',  ( 1.339745962155612702, -60.16965819600731891, -5.000000000000000000 ) ) ;
#60811 = CARTESIAN_POINT ( 'NONE',  ( 9.457646018065525792E-16, 13.93750000136559564, 5.148502694627439702 ) ) ;
#60812 = CARTESIAN_POINT ( 'NONE',  ( 4.458734125000001214, -64.89583333196773651, 2.574251347313718519 ) ) ;
#60813 = VECTOR ( 'NONE', #722, 1000.000000000000000 ) ;
#60814 = CARTESIAN_POINT ( 'NONE',  ( -4.458734124999999437, -12.64583333196774007, -2.574251347313719407 ) ) ;
#60815 = CARTESIAN_POINT ( 'NONE',  ( 5.000000000000000000, -3.416666666666665186, -2.886751345948129988 ) ) ;
#60816 = CARTESIAN_POINT ( 'NONE',  ( 3.152801135295366208, -164.5625000013656063, 3.152801135295367985 ) ) ;
#60817 = CARTESIAN_POINT ( 'NONE',  ( -6.972266317189433020E-16, -41.12499999726880162, -5.000000000000000000 ) ) ;
#60818 = CARTESIAN_POINT ( 'NONE',  ( -2.229367062500000163, -58.47916666530106511, -3.861377020970580443 ) ) ;
#60819 = CARTESIAN_POINT ( 'NONE',  ( 5.000000000000000000, -97.37499999726881583, -6.123233995736766282E-16 ) ) ;
#60820 = DIRECTION ( 'NONE',  ( -0.000000000000000000, 1.000000000000000000, -0.000000000000000000 ) ) ;
#60821 = CARTESIAN_POINT ( 'NONE',  ( -55.39835681537999790, -152.0000000027312410, 4.984105922594378235 ) ) ;
#60822 = CARTESIAN_POINT ( 'NONE',  ( -3.152548672688508926E-16, -35.56249999863440792, -5.148502694627439702 ) ) ;
#60823 = LINE ( 'NONE', #51173, #34841 ) ;
#60824 = CARTESIAN_POINT ( 'NONE',  ( -3.535250795749689387E-16, -50.25000000000000711, -5.773502691896257311 ) ) ;
#60825 = CARTESIAN_POINT ( 'NONE',  ( -2.499999999999996447, 19.16666666666666430, 4.330127018922195425 ) ) ;
#60826 = CARTESIAN_POINT ( 'NONE',  ( -2.480964764533239819E-13, -107.7500000000000000, 5.000000000000000000 ) ) ;
#60827 = ORIENTED_EDGE ( 'NONE', *, *, #19267, .F. ) ;
#60828 = CARTESIAN_POINT ( 'NONE',  ( -4.458734124999998549, -104.2291666653010651, 2.574251347313722516 ) ) ;
#60829 = CARTESIAN_POINT ( 'NONE',  ( 4.458734124999998549, -1.979166665301068662, -2.574251347313721627 ) ) ;
#60830 = CARTESIAN_POINT ( 'NONE',  ( -1.339745962155613812, -100.0803417985302843, -5.000000000000000000 ) ) ;
#60831 = CARTESIAN_POINT ( 'NONE',  ( 5.000000000000000000, -5.499999999999998224, -6.123233995736766282E-16 ) ) ;
#60832 = CARTESIAN_POINT ( 'NONE',  ( -4.458734124999997661, -74.22916666530106511, 2.574251347313722516 ) ) ;
#60833 = CARTESIAN_POINT ( 'NONE',  ( -2.499999999999996447, -25.83333333333333215, 4.330127018922195425 ) ) ;
#60834 = CARTESIAN_POINT ( 'NONE',  ( -4.999999999999999112, -8.791666663935483683, 2.886751345948131764 ) ) ;
#60836 = VERTEX_POINT ( 'NONE', #46387 ) ;
#60835 = CARTESIAN_POINT ( 'NONE',  ( 4.458734124999999437, -36.81249999863440792, -5.460374474430324690E-16 ) ) ;
#60837 = CARTESIAN_POINT ( 'NONE',  ( -4.999999999999998224, -16.79166666393548368, 2.886751345948131764 ) ) ;
#60839 = ORIENTED_EDGE ( 'NONE', *, *, #9152, .T. ) ;
#60838 = CARTESIAN_POINT ( 'NONE',  ( 2.229367062499998831, 12.10416666803226171, -3.861377020970580887 ) ) ;
#60840 = CARTESIAN_POINT ( 'NONE',  ( 0.000000000000000000, -120.0000000000000000, 5.000000000000000000 ) ) ;
#60841 = CARTESIAN_POINT ( 'NONE',  ( -3.535250795749689387E-16, -56.25000000000000000, -5.773502691896257311 ) ) ;
#60842 = CARTESIAN_POINT ( 'NONE',  ( 4.458734124999999437, -31.06249999863440436, -5.460374474430324690E-16 ) ) ;
#60843 = CARTESIAN_POINT ( 'NONE',  ( -4.999999999999998224, -10.79166666393547835, 2.886751345948131764 ) ) ;
#60844 = CARTESIAN_POINT ( 'NONE',  ( -4.458734124999999437, -74.31249999863440792, 0.000000000000000000 ) ) ;
#60845 = CARTESIAN_POINT ( 'NONE',  ( -3.152801135295367096, -140.3125000013655779, -3.152801135295367541 ) ) ;
#60846 = CARTESIAN_POINT ( 'NONE',  ( 4.458734125000001214, -87.89583333196773651, 2.574251347313718519 ) ) ;
#60847 = CARTESIAN_POINT ( 'NONE',  ( -58.39396692619412477, -134.6875000013656063, 2.891590998281057701 ) ) ;
#60848 = CARTESIAN_POINT ( 'NONE',  ( 4.458734125000001214, -34.14583333196772941, 2.574251347313718519 ) ) ;
#60849 =( BOUNDED_CURVE ( )  B_SPLINE_CURVE ( 2, ( #40583, #44451, #59258, #55395, #410, #15520, #49287, #58932, #30617 ),
 .UNSPECIFIED., .F., .F. ) 
 B_SPLINE_CURVE_WITH_KNOTS ( ( 3, 2, 2, 2, 3 ),
 ( 0.4303571428571428825, 0.4309523809523809756, 0.4321428571428571619, 0.4333333333333333481, 0.4339285714285714413 ),
 .UNSPECIFIED. ) 
 CURVE ( )  GEOMETRIC_REPRESENTATION_ITEM ( )  RATIONAL_B_SPLINE_CURVE ( ( 0.9330127018922194093, 0.9330127018922194093, 1.000000000000000000, 0.8660254037844387076, 1.000000000000000000, 0.8660254037844387076, 1.000000000000000000, 0.9330127018922194093, 0.9330127018922194093 ) ) 
 REPRESENTATION_ITEM ( '' )  );
#60850 = CARTESIAN_POINT ( 'NONE',  ( 1.339745962155612702, -83.16965819600733312, -5.000000000000000000 ) ) ;
#60851 = VERTEX_POINT ( 'NONE', #40284 ) ;
#60852 = CARTESIAN_POINT ( 'NONE',  ( -2.229367062500000163, -77.72916666530106511, -3.861377020970580443 ) ) ;
#60853 = CARTESIAN_POINT ( 'NONE',  ( 1.339745962155612702, -86.29465819873851729, -5.000000000000000000 ) ) ;
#60854 = EDGE_LOOP ( 'NONE', ( #57732, #57133, #54440, #26184 ) ) ;
#60855 = DIRECTION ( 'NONE',  ( 0.000000000000000000, 0.000000000000000000, 1.000000000000000000 ) ) ;
#60856 = CARTESIAN_POINT ( 'NONE',  ( 3.535533905932736864, -152.1250000000000000, 3.535533905932738641 ) ) ;
#60858 = EDGE_CURVE ( 'NONE', #45518, #43569, #26174, .T. ) ;
#60857 = CARTESIAN_POINT ( 'NONE',  ( 2.229367062500001939, -66.22916666530106511, 3.861377020970579999 ) ) ;
#60859 = CARTESIAN_POINT ( 'NONE',  ( -2.229367062500000163, -11.72916666530107044, -3.861377020970580443 ) ) ;
#60860 = ORIENTED_EDGE ( 'NONE', *, *, #7231, .T. ) ;
#60861 = CARTESIAN_POINT ( 'NONE',  ( -2.499999999999996447, -9.708333330602146205, 4.330127018922195425 ) ) ;
#60862 = CARTESIAN_POINT ( 'NONE',  ( -2.500000000000000444, 4.958333336064518981, -4.330127018922193649 ) ) ;
#60863 = ORIENTED_EDGE ( 'NONE', *, *, #62096, .T. ) ;
#60864 = CARTESIAN_POINT ( 'NONE',  ( -4.458734124999998549, -7.479166665301073991, 2.574251347313722516 ) ) ;
#60865 = CARTESIAN_POINT ( 'NONE',  ( -54.60164318462004474, -148.5000000027312126, -4.984105922594373794 ) ) ;
#60866 = CARTESIAN_POINT ( 'NONE',  ( -4.458734124999998549, 7.770833334698925121, 2.574251347313722516 ) ) ;
#60867 = CARTESIAN_POINT ( 'NONE',  ( 5.000000000000000888, -64.58333333333332860, 2.886751345948126879 ) ) ;
#60868 = CARTESIAN_POINT ( 'NONE',  ( -1.846868145590734756, -156.1250000013655779, -4.458734124999999437 ) ) ;
#60869 = DIRECTION ( 'NONE',  ( 0.000000000000000000, 0.000000000000000000, 1.000000000000000000 ) ) ;
#60870 = ORIENTED_EDGE ( 'NONE', *, *, #61030, .T. ) ;
#60871 = CARTESIAN_POINT ( 'NONE',  ( -4.458734124999999437, -88.31249999863439371, 0.000000000000000000 ) ) ;
#60872 = CARTESIAN_POINT ( 'NONE',  ( 2.071067811865412445, -163.9375000027311842, -5.000000000000063949 ) ) ;
#60873 = CARTESIAN_POINT ( 'NONE',  ( 2.229367062499998831, -1.645833331967737401, -3.861377020970580887 ) ) ;
#60874 = CYLINDRICAL_SURFACE ( 'NONE', #25248, 5.000000000000000000 ) ;
#60875 = EDGE_CURVE ( 'NONE', #551, #29321, #2333, .T. ) ;
#60876 = CARTESIAN_POINT ( 'NONE',  ( 5.000000000000000888, -32.45833333060215153, 2.886751345948126879 ) ) ;
#60877 = ADVANCED_FACE ( 'NONE', ( #1391 ), #36099, .T. ) ;
#60878 = CARTESIAN_POINT ( 'NONE',  ( 6.123233995736766282E-16, -120.0000000000000000, -5.000000000000000000 ) ) ;
#60879 = CARTESIAN_POINT ( 'NONE',  ( -2.229367062499996610, 23.85416666803225993, 3.861377020970582219 ) ) ;
#60880 = CARTESIAN_POINT ( 'NONE',  ( 4.458734124999998549, 29.27083333469893134, -2.574251347313721627 ) ) ;
#60881 = CARTESIAN_POINT ( 'NONE',  ( 4.458734125000001214, -53.89583333196773651, 2.574251347313718519 ) ) ;
#60882 = CARTESIAN_POINT ( 'NONE',  ( 4.458734125000000326, -35.14583333196772941, 2.574251347313718519 ) ) ;
#60883 = CARTESIAN_POINT ( 'NONE',  ( -4.458734124999999437, 3.437500001365594748, 0.000000000000000000 ) ) ;
#60884 = CARTESIAN_POINT ( 'NONE',  ( -2.499999999999996447, -17.83333333333333215, 4.330127018922195425 ) ) ;
#60885 = CARTESIAN_POINT ( 'NONE',  ( 2.499999999999998668, 16.66666666666666785, -4.330127018922193649 ) ) ;
#60886 = CARTESIAN_POINT ( 'NONE',  ( -5.000000000000000000, -146.6250000027312126, -6.123233995736766282E-16 ) ) ;
#60887 = CARTESIAN_POINT ( 'NONE',  ( 5.000000000000000000, -33.37499999726880873, -6.123233995736766282E-16 ) ) ;
#60888 = CARTESIAN_POINT ( 'NONE',  ( 4.458734124999998549, -43.72916666530106511, -2.574251347313721627 ) ) ;
#60889 = CARTESIAN_POINT ( 'NONE',  ( -3.535250795749689387E-16, -77.12499999726880162, -5.773502691896257311 ) ) ;
#60890 = EDGE_CURVE ( 'NONE', #39916, #3550, #19962, .T. ) ;
#60891 = CARTESIAN_POINT ( 'NONE',  ( -57.89159099828107458, -138.9375000013656063, -3.393966926194107447 ) ) ;
#60892 = LINE ( 'NONE', #36435, #55531 ) ;
#60893 = LINE ( 'NONE', #37388, #35731 ) ;
#60894 = CARTESIAN_POINT ( 'NONE',  ( -2.229367062499996610, -87.39583333196773651, 3.861377020970582219 ) ) ;
#60895 = CARTESIAN_POINT ( 'NONE',  ( -4.458734124999999437, -160.1875000013655779, -5.460374474430324690E-16 ) ) ;
#60896 =( BOUNDED_CURVE ( )  B_SPLINE_CURVE ( 2, ( #31320, #35521, #16853, #11070, #60296, #25229, #6572, #49986, #50955 ),
 .UNSPECIFIED., .F., .F. ) 
 B_SPLINE_CURVE_WITH_KNOTS ( ( 3, 2, 2, 2, 3 ),
 ( 0.1583333333333334925, 0.1625000000000001721, 0.1666666666666668239, 0.1708333333333335036, 0.1750000000000001554 ),
 .UNSPECIFIED. ) 
 CURVE ( )  GEOMETRIC_REPRESENTATION_ITEM ( )  RATIONAL_B_SPLINE_CURVE ( ( 0.9999999999999970024, 0.9238795325112897361, 1.000000000000000000, 0.9238795325112867385, 1.000000000000000000, 0.9238795325112867385, 1.000000000000000000, 0.9238795325112837409, 1.000000000000003109 ) ) 
 REPRESENTATION_ITEM ( '' )  );
#60897 = CARTESIAN_POINT ( 'NONE',  ( 1.975475456537005874E-15, 7.249999999999998224, 5.000000000000000000 ) ) ;
#60898 = CARTESIAN_POINT ( 'NONE',  ( -2.499999999999996447, -32.83333333333332860, 4.330127018922195425 ) ) ;
#60899 = CARTESIAN_POINT ( 'NONE',  ( -1.846868145590737420, -141.7500000013655779, 4.458734124999999437 ) ) ;
#60900 = ORIENTED_EDGE ( 'NONE', *, *, #19682, .F. ) ;
#60901 = CARTESIAN_POINT ( 'NONE',  ( -2.229367062499996610, 21.60416666803226349, 3.861377020970582219 ) ) ;
#60902 = VERTEX_POINT ( 'NONE', #615 ) ;
#60903 = CARTESIAN_POINT ( 'NONE',  ( 4.458734124999998549, -92.72916666530107932, -2.574251347313721627 ) ) ;
#60904 = CARTESIAN_POINT ( 'NONE',  ( 9.457646018065525792E-16, 11.68750000136559564, 5.148502694627439702 ) ) ;
#60905 =( BOUNDED_CURVE ( )  B_SPLINE_CURVE ( 2, ( #34529, #48390, #14294, #34220, #43244, #54162, #33913, #9464, #4332 ),
 .UNSPECIFIED., .F., .F. ) 
 B_SPLINE_CURVE_WITH_KNOTS ( ( 3, 2, 2, 2, 3 ),
 ( 0.2089285714285714357, 0.2095238095238095288, 0.2107142857142857151, 0.2119047619047619013, 0.2124999999999999944 ),
 .UNSPECIFIED. ) 
 CURVE ( )  GEOMETRIC_REPRESENTATION_ITEM ( )  RATIONAL_B_SPLINE_CURVE ( ( 0.9330127018922194093, 0.9330127018922194093, 1.000000000000000000, 0.8660254037844387076, 1.000000000000000000, 0.8660254037844387076, 1.000000000000000000, 0.9330127018922194093, 0.9330127018922194093 ) ) 
 REPRESENTATION_ITEM ( '' )  );
#60906 = CARTESIAN_POINT ( 'NONE',  ( 5.000000000000000000, 14.62500000273118594, -6.123233995736766282E-16 ) ) ;
#60907 = CARTESIAN_POINT ( 'NONE',  ( 1.339745962155612702, 2.705341801261480050, -5.000000000000000000 ) ) ;
#60908 = CARTESIAN_POINT ( 'NONE',  ( 5.000000000000000000, 10.58333333333333393, -2.886751345948129988 ) ) ;
#60909 = CARTESIAN_POINT ( 'NONE',  ( -3.152548672688508926E-16, -53.56249999863439371, -5.148502694627439702 ) ) ;
#60910 = CARTESIAN_POINT ( 'NONE',  ( 2.229367062500001939, -10.97916666530107044, 3.861377020970579999 ) ) ;
#60911 = CARTESIAN_POINT ( 'NONE',  ( 7.499999999999999112, -1.614186302720606481, -7.450236204328171574 ) ) ;
#60912 = ADVANCED_BREP_SHAPE_REPRESENTATION ( '', ( #28816, #43054 ), #60569 ) ;
#60913 = EDGE_CURVE ( 'NONE', #11078, #33613, #29217, .T. ) ;
#60914 = CARTESIAN_POINT ( 'NONE',  ( -4.999999999999998224, -51.91666666666666430, 2.886751345948131764 ) ) ;
#60915 = LINE ( 'NONE', #11367, #8138 ) ;
#60916 = CARTESIAN_POINT ( 'NONE',  ( -6.972266317189433020E-16, -33.12499999726880873, -5.000000000000000000 ) ) ;
#60917 = CARTESIAN_POINT ( 'NONE',  ( 2.499999999999998668, 28.79166666939784847, -4.330127018922193649 ) ) ;
#60918 = CARTESIAN_POINT ( 'NONE',  ( 5.000000000000000000, -37.41666666666666430, -2.886751345948129988 ) ) ;
#60919 = CARTESIAN_POINT ( 'NONE',  ( 5.000000000000000888, -107.5833333333333428, 2.886751345948126879 ) ) ;
#60921 = CARTESIAN_POINT ( 'NONE',  ( 4.458734124999998549, -11.97916666530107044, -2.574251347313721627 ) ) ;
#60920 = CARTESIAN_POINT ( 'NONE',  ( -51.75738570946856498, -138.7500000000000000, 3.805975901505576964 ) ) ;
#60922 = CARTESIAN_POINT ( 'NONE',  ( 1.339745962155615144, -107.5803417985302985, 4.999999999999999112 ) ) ;
#60923 = CARTESIAN_POINT ( 'NONE',  ( -2.229367062500000163, -61.47916666530106511, -3.861377020970580443 ) ) ;
#60924 = CARTESIAN_POINT ( 'NONE',  ( 3.152801135295367541, -150.5625000013655779, -3.152801135295367541 ) ) ;
#60925 = CARTESIAN_POINT ( 'NONE',  ( 4.458734125000001214, -68.89583333196773651, 2.574251347313718519 ) ) ;
#60926 = CARTESIAN_POINT ( 'NONE',  ( -56.48576386720575471, -147.0000000013655779, -4.591703134518078322 ) ) ;
#60927 = CARTESIAN_POINT ( 'NONE',  ( 4.458734125000001214, -18.14583333196773651, 2.574251347313718519 ) ) ;
#60928 = CARTESIAN_POINT ( 'NONE',  ( -3.535250795749689387E-16, -63.12499999726880873, -5.773502691896257311 ) ) ;
#60929 = ORIENTED_EDGE ( 'NONE', *, *, #26376, .F. ) ;
#60930 = CARTESIAN_POINT ( 'NONE',  ( 1.975475456537005874E-15, -31.62499999726880873, 5.000000000000000000 ) ) ;
#60931 = ORIENTED_EDGE ( 'NONE', *, *, #50411, .T. ) ;
#60932 =( BOUNDED_CURVE ( )  B_SPLINE_CURVE ( 2, ( #17623, #46891, #33042, #2834, #22452, #37240, #8285, #61692, #52657 ),
 .UNSPECIFIED., .F., .F. ) 
 B_SPLINE_CURVE_WITH_KNOTS ( ( 3, 2, 2, 2, 3 ),
 ( 0.01607142857142857331, 0.01666666666666666644, 0.01785714285714285615, 0.01904761904761904934, 0.01964285714285714593 ),
 .UNSPECIFIED. ) 
 CURVE ( )  GEOMETRIC_REPRESENTATION_ITEM ( )  RATIONAL_B_SPLINE_CURVE ( ( 0.9330127018922194093, 0.9330127018922195203, 1.000000000000000000, 0.8660254037844387076, 1.000000000000000000, 0.8660254037844387076, 1.000000000000000000, 0.9330127018922191873, 0.9330127018922194093 ) ) 
 REPRESENTATION_ITEM ( '' )  );
#60933 = CARTESIAN_POINT ( 'NONE',  ( -3.152548672688508926E-16, -61.81249999863440081, -5.148502694627439702 ) ) ;
#60935 = CARTESIAN_POINT ( 'NONE',  ( 2.500000000000002220, -103.6666666666666572, 4.330127018922192761 ) ) ;
#60934 = CARTESIAN_POINT ( 'NONE',  ( -4.999999999999998224, -27.91666666666666430, 2.886751345948131764 ) ) ;
#60936 = CARTESIAN_POINT ( 'NONE',  ( -4.458734124999999437, -153.9375000013655779, -5.460374474430324690E-16 ) ) ;
#60937 = ORIENTED_EDGE ( 'NONE', *, *, #8743, .F. ) ;
#60938 = CARTESIAN_POINT ( 'NONE',  ( 5.000000000000000000, -54.49999999999999289, -6.123233995736766282E-16 ) ) ;
#60939 = CARTESIAN_POINT ( 'NONE',  ( -50.18089887299979068, -125.6875000000000711, 2.462841084822635640 ) ) ;
#60940 = CARTESIAN_POINT ( 'NONE',  ( 2.500000000000002220, -8.666666666666669627, 4.330127018922192761 ) ) ;
#60942 = EDGE_CURVE ( 'NONE', #54724, #10579, #14746, .T. ) ;
#60941 = CARTESIAN_POINT ( 'NONE',  ( -4.458734124999999437, -49.56249999863440792, 0.000000000000000000 ) ) ;
#60943 = VERTEX_POINT ( 'NONE', #296 ) ;
#60944 = CARTESIAN_POINT ( 'NONE',  ( 5.000000000000000888, 10.54166666939785202, 2.886751345948126879 ) ) ;
#60945 = CARTESIAN_POINT ( 'NONE',  ( -2.229367062499996610, 10.85416666803225993, 3.861377020970582219 ) ) ;
#60946 = CARTESIAN_POINT ( 'NONE',  ( -4.458734124999998549, 22.77083333469892423, 2.574251347313722516 ) ) ;
#60947 = CARTESIAN_POINT ( 'NONE',  ( -58.39396692619412477, -149.4375000013656063, 2.891590998281057701 ) ) ;
#60948 = CARTESIAN_POINT ( 'NONE',  ( -5.000000000000000000, -23.95833333060214443, -2.886751345948128211 ) ) ;
#60949 = CYLINDRICAL_SURFACE ( 'NONE', #21176, 5.000000000000000000 ) ;
#60950 =( BOUNDED_CURVE ( )  B_SPLINE_CURVE ( 2, ( #1649, #40540, #11270, #18319, #12543, #13502, #51792, #3230, #62081 ),
 .UNSPECIFIED., .F., .F. ) 
 B_SPLINE_CURVE_WITH_KNOTS ( ( 3, 2, 2, 2, 3 ),
 ( 0.05208333333333333565, 0.05277777777777777762, 0.05416666666666666852, 0.05555555555555555247, 0.05625000000000000139 ),
 .UNSPECIFIED. ) 
 CURVE ( )  GEOMETRIC_REPRESENTATION_ITEM ( )  RATIONAL_B_SPLINE_CURVE ( ( 0.9330127018922192983, 0.9330127018922196314, 1.000000000000000000, 0.8660254037844387076, 1.000000000000000000, 0.8660254037844387076, 1.000000000000000000, 0.9330127018922189652, 0.9330127018922192983 ) ) 
 REPRESENTATION_ITEM ( '' )  );
#60951 = ORIENTED_EDGE ( 'NONE', *, *, #5182, .F. ) ;
#60952 = CARTESIAN_POINT ( 'NONE',  ( 4.458734124999999437, -71.81249999863439371, -5.460374474430324690E-16 ) ) ;
#60953 = CARTESIAN_POINT ( 'NONE',  ( 2.621328321948289020, 7.606199919103058704, -7.633618187056857352 ) ) ;
#60954 = CARTESIAN_POINT ( 'NONE',  ( 2.229367062500001939, 10.02083333469892779, 3.861377020970579999 ) ) ;
#60955 = CARTESIAN_POINT ( 'NONE',  ( 1.339745962155615144, -63.70534180126147561, 4.999999999999999112 ) ) ;
#60956 = CARTESIAN_POINT ( 'NONE',  ( 0.000000000000000000, -120.0000000000000000, 0.000000000000000000 ) ) ;
#60957 = CARTESIAN_POINT ( 'NONE',  ( 9.457646018065525792E-16, -53.31249999863441502, 5.148502694627439702 ) ) ;
#60958 = CARTESIAN_POINT ( 'NONE',  ( -5.000000000000000000, -15.95833333060214443, -2.886751345948128211 ) ) ;
#60959 = ADVANCED_FACE ( 'NONE', ( #34055 ), #58816, .T. ) ;
#60960 = CARTESIAN_POINT ( 'NONE',  ( 2.499999999999998668, 4.666666666666666075, -4.330127018922193649 ) ) ;
#60961 = CARTESIAN_POINT ( 'NONE',  ( -0.5974722283283655511, 8.315303285985683246, -0.7026937717022859742 ) ) ;
#60962 = CARTESIAN_POINT ( 'NONE',  ( 0.000000000000000000, -170.0000000000000000, 0.000000000000000000 ) ) ;
#60963 = CARTESIAN_POINT ( 'NONE',  ( 4.458734124999999437, -23.06249999863440436, -5.460374474430324690E-16 ) ) ;
#60964 = ORIENTED_EDGE ( 'NONE', *, *, #3572, .T. ) ;
#60965 = CARTESIAN_POINT ( 'NONE',  ( 1.975475456537005874E-15, 6.249999999999998224, 5.000000000000000000 ) ) ;
#60966 = CARTESIAN_POINT ( 'NONE',  ( -3.152548672688508926E-16, -106.5624999986343937, -5.148502694627439702 ) ) ;
#60967 = CARTESIAN_POINT ( 'NONE',  ( 3.535533905932736864, -158.2500000027312126, 3.535533905932738641 ) ) ;
#60968 = ORIENTED_EDGE ( 'NONE', *, *, #14103, .F. ) ;
#60969 = CARTESIAN_POINT ( 'NONE',  ( 4.458734124999999437, -102.0624999986344079, -5.460374474430324690E-16 ) ) ;
#60970 = CARTESIAN_POINT ( 'NONE',  ( -4.458734124999998549, -26.22916666530106866, 2.574251347313722516 ) ) ;
#60971 = CARTESIAN_POINT ( 'NONE',  ( 5.000000000000000000, -60.37499999726880873, -6.123233995736766282E-16 ) ) ;
#60972 = CARTESIAN_POINT ( 'NONE',  ( -52.10840900171896806, -150.4375000013656063, 3.393966926194110556 ) ) ;
#60973 = CARTESIAN_POINT ( 'NONE',  ( 2.071067811865475505, -148.8125000000000284, -5.000000000000000888 ) ) ;
#60974 = CARTESIAN_POINT ( 'NONE',  ( -2.229367062499996610, -21.14583333196774007, 3.861377020970582219 ) ) ;
#60975 = CARTESIAN_POINT ( 'NONE',  ( -4.458734124999997661, -67.47916666530106511, 2.574251347313722516 ) ) ;
#60976 = CARTESIAN_POINT ( 'NONE',  ( -50.01589407740564042, -153.7500000027312410, 0.3983568153799778022 ) ) ;
#60977 = CARTESIAN_POINT ( 'NONE',  ( 2.229367062500001939, -25.97916666530106866, 3.861377020970579999 ) ) ;
#60978 = CARTESIAN_POINT ( 'NONE',  ( 5.000000000000000888, -32.45833333060215153, 2.886751345948126879 ) ) ;
#60979 = CARTESIAN_POINT ( 'NONE',  ( 2.071067811865476394, -152.1875000000000000, 5.000000000000000000 ) ) ;
#60980 = CARTESIAN_POINT ( 'NONE',  ( -2.500000000000000444, -11.16666666666666430, -4.330127018922193649 ) ) ;
#60981 = CARTESIAN_POINT ( 'NONE',  ( -1.846868145590737420, -152.7500000013656063, 4.458734124999999437 ) ) ;
#60982 = VERTEX_POINT ( 'NONE', #39508 ) ;
#60983 = CARTESIAN_POINT ( 'NONE',  ( 2.229367062500001939, -49.22916666530107221, 3.861377020970579999 ) ) ;
#60984 = CARTESIAN_POINT ( 'NONE',  ( -1.339745962155610925, -2.669658196007334450, 5.000000000000000000 ) ) ;
#60985 = CARTESIAN_POINT ( 'NONE',  ( 1.339745962155612702, -92.29465819873853150, -5.000000000000000000 ) ) ;
#60986 = CARTESIAN_POINT ( 'NONE',  ( -5.000000000000000000, 24.99999999999999645, 0.000000000000000000 ) ) ;
#60987 = EDGE_CURVE ( 'NONE', #2721, #34069, #20225, .T. ) ;
#60988 = CARTESIAN_POINT ( 'NONE',  ( 1.975475456537005874E-15, -76.62499999726880162, 5.000000000000000000 ) ) ;
#60989 = CARTESIAN_POINT ( 'NONE',  ( -2.229367062500000163, 2.520833334698928230, -3.861377020970580443 ) ) ;
#60990 = CARTESIAN_POINT ( 'NONE',  ( -2.499999999999996447, -73.70833333060214443, 4.330127018922195425 ) ) ;
#60991 = CARTESIAN_POINT ( 'NONE',  ( 1.062108568985190270E-13, -11.12499999726881761, -4.999999999999999112 ) ) ;
#60992 = CARTESIAN_POINT ( 'NONE',  ( 1.975475456537005874E-15, -24.62499999726881583, 5.000000000000000000 ) ) ;
#60993 = CARTESIAN_POINT ( 'NONE',  ( 4.458734124999999437, 13.93750000136559386, -5.460374474430324690E-16 ) ) ;
#60994 = CARTESIAN_POINT ( 'NONE',  ( 5.000000000000000888, 4.541666669397852019, 2.886751345948126879 ) ) ;
#60995 = VERTEX_POINT ( 'NONE', #9920 ) ;
#60996 = VERTEX_POINT ( 'NONE', #59145 ) ;
#60997 = CARTESIAN_POINT ( 'NONE',  ( -4.458734124999999437, -44.31249999863440081, 0.000000000000000000 ) ) ;
#60998 = CARTESIAN_POINT ( 'NONE',  ( -4.458734125000001214, -162.1250000013655779, 1.846868145590734089 ) ) ;
#60999 = VECTOR ( 'NONE', #8634, 1000.000000000000000 ) ;
#61000 = CARTESIAN_POINT ( 'NONE',  ( 2.499999999999998668, -46.20833333060214443, -4.330127018922193649 ) ) ;
#61001 = VERTEX_POINT ( 'NONE', #48843 ) ;
#61002 = CARTESIAN_POINT ( 'NONE',  ( -4.458734124999999437, -15.39583333196773474, -2.574251347313719407 ) ) ;
#61003 = EDGE_LOOP ( 'NONE', ( #3312, #46463, #57287, #31040 ) ) ;
#61004 = CARTESIAN_POINT ( 'NONE',  ( 2.500000000000002220, -89.66666666666665719, 4.330127018922192761 ) ) ;
#61005 = CARTESIAN_POINT ( 'NONE',  ( 4.458734124999999437, -163.5000000013655779, 1.846868145590737864 ) ) ;
#61007 = ORIENTED_EDGE ( 'NONE', *, *, #22199, .F. ) ;
#61006 = CARTESIAN_POINT ( 'NONE',  ( -2.499999999999996447, -60.70833333060214443, 4.330127018922195425 ) ) ;
#61008 = CARTESIAN_POINT ( 'NONE',  ( -51.19402409849444524, -139.5000000000000284, -3.242614290531456334 ) ) ;
#61009 = CARTESIAN_POINT ( 'NONE',  ( 2.229367062499998831, -33.89583333196772941, -3.861377020970580887 ) ) ;
#61010 = CARTESIAN_POINT ( 'NONE',  ( -5.000000000000000000, -38.99999999999999289, 0.000000000000000000 ) ) ;
#61011 = ORIENTED_EDGE ( 'NONE', *, *, #51725, .F. ) ;
#61012 = EDGE_CURVE ( 'NONE', #11458, #9785, #59034, .T. ) ;
#61013 = ADVANCED_FACE ( 'NONE', ( #15401 ), #40152, .T. ) ;
#61014 = CARTESIAN_POINT ( 'NONE',  ( 4.458734124999999437, -78.81249999863440792, -5.460374474430324690E-16 ) ) ;
#61015 = CARTESIAN_POINT ( 'NONE',  ( -3.152548672688508926E-16, 25.43750000136559208, -5.148502694627439702 ) ) ;
#61016 = EDGE_CURVE ( 'NONE', #15515, #62517, #9610, .T. ) ;
#61017 = ORIENTED_EDGE ( 'NONE', *, *, #9495, .F. ) ;
#61018 = CARTESIAN_POINT ( 'NONE',  ( -1.339745962155613812, 4.919658201469705006, -5.000000000000000000 ) ) ;
#61019 = CARTESIAN_POINT ( 'NONE',  ( -59.59170313451810586, -142.7500000013655779, 1.485763867205729394 ) ) ;
#61020 = CARTESIAN_POINT ( 'NONE',  ( -4.458734124999998549, -81.47916666530106511, 2.574251347313722516 ) ) ;
#61021 = CARTESIAN_POINT ( 'NONE',  ( -58.24261429053147765, -130.3750000027312126, -3.805975901505573855 ) ) ;
#61022 = FACE_OUTER_BOUND ( 'NONE', #38889, .T. ) ;
#61023 = CARTESIAN_POINT ( 'NONE',  ( 3.152801135295367541, -141.5625000013655779, -3.152801135295367541 ) ) ;
#61024 = EDGE_CURVE ( 'NONE', #57124, #41833, #8523, .T. ) ;
#61025 = CARTESIAN_POINT ( 'NONE',  ( -6.972266317189433020E-16, -84.12499999726880162, -5.000000000000000000 ) ) ;
#61026 = CARTESIAN_POINT ( 'NONE',  ( 9.457646018065525792E-16, -57.06249999863440081, 5.148502694627439702 ) ) ;
#61027 = CARTESIAN_POINT ( 'NONE',  ( -4.458734124999997661, -47.22916666530105800, 2.574251347313722516 ) ) ;
#61028 = CARTESIAN_POINT ( 'NONE',  ( -2.229367062500000163, 27.52083333469892779, -3.861377020970580443 ) ) ;
#61029 = ADVANCED_FACE ( 'NONE', ( #26006 ), #16032, .T. ) ;
#61030 = EDGE_CURVE ( 'NONE', #19898, #61397, #49108, .T. ) ;
#61031 =( BOUNDED_CURVE ( )  B_SPLINE_CURVE ( 2, ( #20407, #21048, #59653, #50632, #55141, #10427, #1446, #54503, #40654 ),
 .UNSPECIFIED., .F., .F. ) 
 B_SPLINE_CURVE_WITH_KNOTS ( ( 3, 2, 2, 2, 3 ),
 ( 0.5750000000000005107, 0.5791666666666672736, 0.5833333333333339255, 0.5875000000000004663, 0.5916666666666671182 ),
 .UNSPECIFIED. ) 
 CURVE ( )  GEOMETRIC_REPRESENTATION_ITEM ( )  RATIONAL_B_SPLINE_CURVE ( ( 0.9999999999999898970, 0.9238795325112968415, 1.000000000000000000, 0.9238795325112867385, 1.000000000000000000, 0.9238795325112867385, 1.000000000000000000, 0.9238795325112786339, 1.000000000000008216 ) ) 
 REPRESENTATION_ITEM ( '' )  );
#61032 = CARTESIAN_POINT ( 'NONE',  ( 5.000000000000000000, -106.4999999999999858, -6.123233995736766282E-16 ) ) ;
#61033 = FACE_OUTER_BOUND ( 'NONE', #35587, .T. ) ;
#61034 = CARTESIAN_POINT ( 'NONE',  ( -4.458734124999998549, -36.47916666530107221, 2.574251347313722516 ) ) ;
#61035 = CARTESIAN_POINT ( 'NONE',  ( 5.000000000000000888, 0.5416666693978527958, 2.886751345948126879 ) ) ;
#61036 = CARTESIAN_POINT ( 'NONE',  ( 5.000000000000000000, 16.62500000273118417, -6.123233995736766282E-16 ) ) ;
#61037 = CARTESIAN_POINT ( 'NONE',  ( -59.59170313451811296, -124.5000000013656063, 1.485763867205729394 ) ) ;
#61038 = CARTESIAN_POINT ( 'NONE',  ( 2.229367062499998831, -77.89583333196773651, -3.861377020970580887 ) ) ;
#61039 = EDGE_CURVE ( 'NONE', #6898, #5972, #55917, .T. ) ;
#61040 = CARTESIAN_POINT ( 'NONE',  ( 1.464175926609780648E-14, 24.74999999999999645, -5.000000000000000000 ) ) ;
#61041 = CARTESIAN_POINT ( 'NONE',  ( 4.458734124999998549, -96.72916666530105090, -2.574251347313721627 ) ) ;
#61042 = CARTESIAN_POINT ( 'NONE',  ( 9.457646018065525792E-16, -4.312499998634408804, 5.148502694627439702 ) ) ;
#61043 = EDGE_LOOP ( 'NONE', ( #3147, #23266, #14451, #10789 ) ) ;
#61044 = CARTESIAN_POINT ( 'NONE',  ( -49.85088928181150436, -146.5625000000000000, -1.666127454062680480 ) ) ;
#61045 = EDGE_CURVE ( 'NONE', #16689, #53339, #28229, .T. ) ;
#61046 = CARTESIAN_POINT ( 'NONE',  ( 1.339745962155615144, -47.70534180126147561, 4.999999999999999112 ) ) ;
#61047 = CARTESIAN_POINT ( 'NONE',  ( -4.458734124999999437, -93.39583333196773651, -2.574251347313719407 ) ) ;
#61048 = EDGE_CURVE ( 'NONE', #29621, #21623, #57376, .T. ) ;
#61049 = CARTESIAN_POINT ( 'NONE',  ( 2.071067811865475505, -168.9375000027311842, -5.000000000000000888 ) ) ;
#61050 = CARTESIAN_POINT ( 'NONE',  ( 4.458734125000001214, -89.14583333196775072, 2.574251347313718519 ) ) ;
#61051 = CARTESIAN_POINT ( 'NONE',  ( 4.458734124999998549, 14.02083333469892779, -2.574251347313721627 ) ) ;
#61052 = VECTOR ( 'NONE', #24688, 1000.000000000000000 ) ;
#61053 = CARTESIAN_POINT ( 'NONE',  ( -52.10840900171896806, -132.1875000013656063, 3.393966926194110556 ) ) ;
#61054 =( BOUNDED_CURVE ( )  B_SPLINE_CURVE ( 2, ( #56246, #12167, #7359, #46906, #26968, #46587, #22468, #2530, #42065 ),
 .UNSPECIFIED., .F., .F. ) 
 B_SPLINE_CURVE_WITH_KNOTS ( ( 3, 2, 2, 2, 3 ),
 ( 0.01250000000000000069, 0.01309523809523809555, 0.01428571428571428527, 0.01547619047619047672, 0.01607142857142857331 ),
 .UNSPECIFIED. ) 
 CURVE ( )  GEOMETRIC_REPRESENTATION_ITEM ( )  RATIONAL_B_SPLINE_CURVE ( ( 0.9330127018922192983, 0.9330127018922194093, 1.000000000000000000, 0.8660254037844387076, 1.000000000000000000, 0.8660254037844387076, 1.000000000000000000, 0.9330127018922191873, 0.9330127018922194093 ) ) 
 REPRESENTATION_ITEM ( '' )  );
#61055 = CARTESIAN_POINT ( 'NONE',  ( 2.229367062500001939, -5.979166665301072214, 3.861377020970579999 ) ) ;
#61056 = CARTESIAN_POINT ( 'NONE',  ( -3.152548672688508926E-16, 15.18750000136559386, -5.148502694627439702 ) ) ;
#61057 = CARTESIAN_POINT ( 'NONE',  ( -4.458734124999999437, -51.56249999863440792, 0.000000000000000000 ) ) ;
#61058 = CARTESIAN_POINT ( 'NONE',  ( -1.339745962155610925, -13.66965819600733489, 5.000000000000000000 ) ) ;
#61059 = CARTESIAN_POINT ( 'NONE',  ( 2.229367062499998831, -87.64583333196773651, -3.861377020970580887 ) ) ;
#61060 = CARTESIAN_POINT ( 'NONE',  ( -4.458734124999997661, -11.22916666530107044, 2.574251347313722516 ) ) ;
#61061 =( NAMED_UNIT ( * ) SI_UNIT ( $, .STERADIAN. ) SOLID_ANGLE_UNIT ( ) );
#61062 = EDGE_LOOP ( 'NONE', ( #11066, #9759, #20442, #45167 ) ) ;
#61063 = CARTESIAN_POINT ( 'NONE',  ( -3.152548672688508926E-16, -37.81249999863440792, -5.148502694627439702 ) ) ;
#61064 = CARTESIAN_POINT ( 'NONE',  ( -59.59170313451811296, -129.7500000013656063, 1.485763867205729394 ) ) ;
#61065 = CARTESIAN_POINT ( 'NONE',  ( 4.458734124999998549, -79.72916666530107932, -2.574251347313721627 ) ) ;
#61066 = CARTESIAN_POINT ( 'NONE',  ( -4.999999999999999112, -108.7916666639354730, 2.886751345948131764 ) ) ;
#61067 = CARTESIAN_POINT ( 'NONE',  ( 2.229367062499998831, 19.35416666803225993, -3.861377020970580887 ) ) ;
#61068 = CARTESIAN_POINT ( 'NONE',  ( -1.339745962155613812, -94.20534180126146850, -5.000000000000000000 ) ) ;
#61069 = CARTESIAN_POINT ( 'NONE',  ( 5.000000000000000000, -66.41666666666667140, -2.886751345948130876 ) ) ;
#61070 = CARTESIAN_POINT ( 'NONE',  ( -2.229367062499996610, -84.39583333196773651, 3.861377020970582219 ) ) ;
#61071 = CARTESIAN_POINT ( 'NONE',  ( -2.500000000000000444, -64.16666666666665719, -4.330127018922193649 ) ) ;
#61072 = CARTESIAN_POINT ( 'NONE',  ( 2.499999999999998668, -63.20833333060215153, -4.330127018922193649 ) ) ;
#61073 = CARTESIAN_POINT ( 'NONE',  ( 5.000000000000000888, 19.54166666939785202, 2.886751345948126879 ) ) ;
#61074 = VERTEX_POINT ( 'NONE', #6398 ) ;
#61075 = CARTESIAN_POINT ( 'NONE',  ( -6.972266317189433020E-16, -81.24999999999998579, -5.000000000000000000 ) ) ;
#61076 = CARTESIAN_POINT ( 'NONE',  ( -2.071067811865470620, -168.4375000027311557, 5.000000000000007105 ) ) ;
#61078 = CARTESIAN_POINT ( 'NONE',  ( -5.000000000000000000, -25.00000000000000000, 0.000000000000000000 ) ) ;
#61077 = DIRECTION ( 'NONE',  ( -0.000000000000000000, 1.000000000000000000, -0.000000000000000000 ) ) ;
#61079 = CARTESIAN_POINT ( 'NONE',  ( 4.458734124999998549, -27.72916666530107221, -2.574251347313721627 ) ) ;
#61080 = CARTESIAN_POINT ( 'NONE',  ( 4.458734124999999437, -89.81249999863440792, -5.460374474430324690E-16 ) ) ;
#61081 = CARTESIAN_POINT ( 'NONE',  ( -3.535250795749689387E-16, -30.12499999726881228, -5.773502691896257311 ) ) ;
#61083 = ORIENTED_EDGE ( 'NONE', *, *, #2009, .F. ) ;
#61082 = CARTESIAN_POINT ( 'NONE',  ( 9.457646018065525792E-16, -53.06249999863441502, 5.148502694627439702 ) ) ;
#61084 = CARTESIAN_POINT ( 'NONE',  ( 1.975475456537005874E-15, -28.74999999999999645, 5.000000000000000000 ) ) ;
#61086 = ORIENTED_EDGE ( 'NONE', *, *, #44784, .F. ) ;
#61085 = CARTESIAN_POINT ( 'NONE',  ( 4.458734124999999437, -1.062499998634405696, -5.460374474430324690E-16 ) ) ;
#61087 = CARTESIAN_POINT ( 'NONE',  ( -4.999999999999999112, -73.91666666666664298, 2.886751345948131764 ) ) ;
#61088 = CARTESIAN_POINT ( 'NONE',  ( -59.44456063193725015, -140.5625000013656063, -0.3552334253322034230 ) ) ;
#61089 = CARTESIAN_POINT ( 'NONE',  ( -4.458734124999998549, -52.47916666530107221, 2.574251347313722516 ) ) ;
#61090 = CARTESIAN_POINT ( 'NONE',  ( 1.975475456537005874E-15, 0.3750000027311862216, 5.000000000000000000 ) ) ;
#61091 = CARTESIAN_POINT ( 'NONE',  ( 5.000000000000000888, -72.45833333060213022, 2.886751345948126879 ) ) ;
#61092 = CARTESIAN_POINT ( 'NONE',  ( -2.500000000000000444, -22.04166666393548013, -4.330127018922193649 ) ) ;
#61093 = CARTESIAN_POINT ( 'NONE',  ( -55.39835681537999790, -152.8750000000000284, 4.984105922594378235 ) ) ;
#61094 = CARTESIAN_POINT ( 'NONE',  ( 9.457646018065525792E-16, -15.31249999863440436, 5.148502694627439702 ) ) ;
#61095 = CARTESIAN_POINT ( 'NONE',  ( -4.458734124999999437, -50.64583333196773651, -2.574251347313719407 ) ) ;
#61096 = CARTESIAN_POINT ( 'NONE',  ( 1.975475456537005874E-15, -29.62499999726881228, 5.000000000000000000 ) ) ;
#61097 =( LENGTH_UNIT ( ) NAMED_UNIT ( * ) SI_UNIT ( .MILLI., .METRE. ) );
#61098 = CARTESIAN_POINT ( 'NONE',  ( 4.458734124999999437, -141.5000000013655779, 1.846868145590737864 ) ) ;
#61099 = CARTESIAN_POINT ( 'NONE',  ( -4.458734124999999437, -96.56249999863440792, 0.000000000000000000 ) ) ;
#61100 = CARTESIAN_POINT ( 'NONE',  ( 2.071067811865349828, -148.3125000027312126, 5.000000000000126121 ) ) ;
#61101 = VERTEX_POINT ( 'NONE', #36294 ) ;
#61102 = CARTESIAN_POINT ( 'NONE',  ( -4.458734124999998549, 23.52083333469892779, 2.574251347313722516 ) ) ;
#61103 = CARTESIAN_POINT ( 'NONE',  ( -54.60164318462004474, -141.5000000027312126, -4.984105922594373794 ) ) ;
#61104 =( BOUNDED_CURVE ( )  B_SPLINE_CURVE ( 2, ( #41163, #13170, #2279, #37613, #22523, #52424, #21566, #32149, #42118 ),
 .UNSPECIFIED., .F., .F. ) 
 B_SPLINE_CURVE_WITH_KNOTS ( ( 3, 2, 2, 2, 3 ),
 ( 0.6553571428571428603, 0.6559523809523809534, 0.6571428571428571397, 0.6583333333333333259, 0.6589285714285714191 ),
 .UNSPECIFIED. ) 
 CURVE ( )  GEOMETRIC_REPRESENTATION_ITEM ( )  RATIONAL_B_SPLINE_CURVE ( ( 0.9330127018922194093, 0.9330127018922194093, 1.000000000000000000, 0.8660254037844387076, 1.000000000000000000, 0.8660254037844387076, 1.000000000000000000, 0.9330127018922194093, 0.9330127018922194093 ) ) 
 REPRESENTATION_ITEM ( '' )  );
#61105 = DIRECTION ( 'NONE',  ( 0.000000000000000000, 0.000000000000000000, 1.000000000000000000 ) ) ;
#61106 = CARTESIAN_POINT ( 'NONE',  ( -3.152548672688508926E-16, 0.4375000013655955255, -5.148502694627439702 ) ) ;
#61107 = CARTESIAN_POINT ( 'NONE',  ( -4.458734124999999437, -94.56249999863440792, 0.000000000000000000 ) ) ;
#61108 = CARTESIAN_POINT ( 'NONE',  ( -3.152801135295367985, -149.0625000013655779, 3.152801135295367096 ) ) ;
#61109 = CARTESIAN_POINT ( 'NONE',  ( 4.458734124999998549, -24.97916666530106511, -2.574251347313721627 ) ) ;
#61110 = FACE_OUTER_BOUND ( 'NONE', #23187, .T. ) ;
#61111 = CARTESIAN_POINT ( 'NONE',  ( -59.44456063193725015, -142.5625000013656063, -0.3552334253322034230 ) ) ;
#61112 = CARTESIAN_POINT ( 'NONE',  ( 2.229367062499998831, -65.89583333196773651, -3.861377020970580887 ) ) ;
#61113 = EDGE_CURVE ( 'NONE', #37331, #57060, #34813, .T. ) ;
#61114 = CARTESIAN_POINT ( 'NONE',  ( -3.535533905932738641, -154.5000000027312126, 3.535533905932737309 ) ) ;
#61115 = CARTESIAN_POINT ( 'NONE',  ( 7.779103221381273414, -4.168986698926031131, -7.929128246061905472 ) ) ;
#61116 = CARTESIAN_POINT ( 'NONE',  ( 4.458734124999999437, -145.4375000013656063, 0.000000000000000000 ) ) ;
#61117 = CARTESIAN_POINT ( 'NONE',  ( -4.458734124999997661, 12.52083333469892601, 2.574251347313722516 ) ) ;
#61118 = ORIENTED_EDGE ( 'NONE', *, *, #43702, .F. ) ;
#61119 = CARTESIAN_POINT ( 'NONE',  ( 0.000000000000000000, -120.0000000000000000, 0.000000000000000000 ) ) ;
#61120 = CARTESIAN_POINT ( 'NONE',  ( 0.000000000000000000, -170.0000000000000000, 0.000000000000000000 ) ) ;
#61122 = CARTESIAN_POINT ( 'NONE',  ( 2.229367062499998831, -22.64583333196773651, -3.861377020970580887 ) ) ;
#61121 = CARTESIAN_POINT ( 'NONE',  ( -4.999999999999999112, -85.91666666666667140, 2.886751345948131764 ) ) ;
#61123 = CARTESIAN_POINT ( 'NONE',  ( 9.457646018065525792E-16, 27.68750000136559208, 5.148502694627439702 ) ) ;
#61124 = LINE ( 'NONE', #3217, #15006 ) ;
#61125 = CARTESIAN_POINT ( 'NONE',  ( -51.60603307380591787, -143.9375000013656063, -2.891590998281053704 ) ) ;
#61126 = ADVANCED_FACE ( 'NONE', ( #21821 ), #31778, .T. ) ;
#61127 = CARTESIAN_POINT ( 'NONE',  ( -3.535250795749689387E-16, -46.12499999726881583, -5.773502691896257311 ) ) ;
#61128 = CARTESIAN_POINT ( 'NONE',  ( 3.061616997868383141E-16, -149.8750000027312126, -5.000000000000000000 ) ) ;
#61129 = CARTESIAN_POINT ( 'NONE',  ( 9.457646018065525792E-16, 10.93750000136559208, 5.148502694627439702 ) ) ;
#61130 = CARTESIAN_POINT ( 'NONE',  ( -6.972266317189433020E-16, -50.24999999999999289, -5.000000000000000000 ) ) ;
#61131 = CARTESIAN_POINT ( 'NONE',  ( -6.972266317189433020E-16, -8.124999997268814056, -5.000000000000000000 ) ) ;
#61132 = CARTESIAN_POINT ( 'NONE',  ( 2.229367062499998831, 9.354166668032261711, -3.861377020970580887 ) ) ;
#61133 = CARTESIAN_POINT ( 'NONE',  ( 4.458734125000001214, -66.89583333196773651, 2.574251347313718519 ) ) ;
#61134 = CARTESIAN_POINT ( 'NONE',  ( 4.458734124999999437, -22.06249999863440436, -5.460374474430324690E-16 ) ) ;
#61135 =( BOUNDED_CURVE ( )  B_SPLINE_CURVE ( 2, ( #32927, #33239, #42254, #7855, #38373, #52550, #42567, #12981, #2714 ),
 .UNSPECIFIED., .F., .F. ) 
 B_SPLINE_CURVE_WITH_KNOTS ( ( 3, 2, 2, 2, 3 ),
 ( 0.5374999999999999778, 0.5380952380952380709, 0.5392857142857142572, 0.5404761904761904434, 0.5410714285714285365 ),
 .UNSPECIFIED. ) 
 CURVE ( )  GEOMETRIC_REPRESENTATION_ITEM ( )  RATIONAL_B_SPLINE_CURVE ( ( 0.9330127018922194093, 0.9330127018922194093, 1.000000000000000000, 0.8660254037844387076, 1.000000000000000000, 0.8660254037844387076, 1.000000000000000000, 0.9330127018922194093, 0.9330127018922194093 ) ) 
 REPRESENTATION_ITEM ( '' )  );
#61136 = CARTESIAN_POINT ( 'NONE',  ( 2.500000000000002220, -2.666666666666664298, 4.330127018922192761 ) ) ;
#61137 = CARTESIAN_POINT ( 'NONE',  ( -1.846868145590737420, -159.7500000013656063, 4.458734124999999437 ) ) ;
#61138 = CARTESIAN_POINT ( 'NONE',  ( -1.339745962155610259, 25.91965820146970856, -5.000000000000002665 ) ) ;
#61139 = CARTESIAN_POINT ( 'NONE',  ( 4.458734125000001214, -62.89583333196775072, 2.574251347313718519 ) ) ;
#61140 = CARTESIAN_POINT ( 'NONE',  ( 5.000000000000000888, -94.45833333060213022, 2.886751345948126879 ) ) ;
#61141 = CARTESIAN_POINT ( 'NONE',  ( -5.000000000000000000, -69.99999999999998579, 0.000000000000000000 ) ) ;
#61142 = CARTESIAN_POINT ( 'NONE',  ( -5.000000000000000000, 30.00000000000000000, 0.000000000000000000 ) ) ;
#61143 = CARTESIAN_POINT ( 'NONE',  ( 4.458734124999999437, -34.81249999863440792, -5.460374474430324690E-16 ) ) ;
#61144 = CARTESIAN_POINT ( 'NONE',  ( 2.499999999999998668, -60.33333333333333570, -4.330127018922193649 ) ) ;
#61145 = CARTESIAN_POINT ( 'NONE',  ( -3.152548672688508926E-16, -62.81249999863440792, -5.148502694627439702 ) ) ;
#61146 = CARTESIAN_POINT ( 'NONE',  ( 2.499999999999998668, -51.33333333333332860, -4.330127018922193649 ) ) ;
#61147 = FACE_OUTER_BOUND ( 'NONE', #3874, .T. ) ;
#61148 = CARTESIAN_POINT ( 'NONE',  ( 3.061616997868383141E-16, -151.8750000027311842, -5.000000000000000000 ) ) ;
#61149 = ORIENTED_EDGE ( 'NONE', *, *, #26834, .T. ) ;
#61150 = CARTESIAN_POINT ( 'NONE',  ( 2.229367062499998831, -105.6458333319677365, -3.861377020970580887 ) ) ;
#61151 = CARTESIAN_POINT ( 'NONE',  ( -2.229367062499996610, -3.395833331967738733, 3.861377020970582219 ) ) ;
#61152 = FACE_OUTER_BOUND ( 'NONE', #56323, .T. ) ;
#61153 = CARTESIAN_POINT ( 'NONE',  ( 5.000000000000000000, -6.499999999999999112, -6.123233995736766282E-16 ) ) ;
#61154 = CARTESIAN_POINT ( 'NONE',  ( -4.458734124999999437, -74.31249999863440792, 0.000000000000000000 ) ) ;
#61155 = CARTESIAN_POINT ( 'NONE',  ( 1.975475456537005874E-15, -30.62499999726881583, 5.000000000000000000 ) ) ;
#61156 = CARTESIAN_POINT ( 'NONE',  ( 2.500000000000002220, -13.54166666393548013, 4.330127018922192761 ) ) ;
#61158 = VERTEX_POINT ( 'NONE', #60111 ) ;
#61157 = CARTESIAN_POINT ( 'NONE',  ( -4.458734124999999437, -39.39583333196773651, -2.574251347313719407 ) ) ;
#61159 = CARTESIAN_POINT ( 'NONE',  ( 0.000000000000000000, -120.0000000000000000, 5.000000000000000000 ) ) ;
#61161 = EDGE_LOOP ( 'NONE', ( #47916, #50451, #33920, #61646 ) ) ;
#61160 = CARTESIAN_POINT ( 'NONE',  ( 4.458734125000001214, 14.85416666803225993, 2.574251347313718519 ) ) ;
#61162 = CARTESIAN_POINT ( 'NONE',  ( 5.000000000000000000, -81.41666666666667140, -2.886751345948130876 ) ) ;
#61163 = CARTESIAN_POINT ( 'NONE',  ( -2.500000000000000444, -56.16666666666667140, -4.330127018922193649 ) ) ;
#61164 = CARTESIAN_POINT ( 'NONE',  ( -3.152801135295367096, -159.3125000013656063, -3.152801135295367541 ) ) ;
#61165 = CARTESIAN_POINT ( 'NONE',  ( 2.229367062499998831, -29.89583333196773296, -3.861377020970580887 ) ) ;
#61166 = CARTESIAN_POINT ( 'NONE',  ( 6.123233995736766282E-16, -120.0000000000000000, -5.000000000000000000 ) ) ;
#61167 = CARTESIAN_POINT ( 'NONE',  ( -2.229367062500000163, -81.47916666530106511, -3.861377020970580443 ) ) ;
#61168 = CARTESIAN_POINT ( 'NONE',  ( 3.152801135295367541, -140.5625000013655779, -3.152801135295367541 ) ) ;
#61169 = CARTESIAN_POINT ( 'NONE',  ( -2.229367062500000163, -86.47916666530107932, -3.861377020970580443 ) ) ;
#61170 = CARTESIAN_POINT ( 'NONE',  ( -50.55543936806279248, -134.3125000013656063, 0.3552334253322060320 ) ) ;
#61171 = CARTESIAN_POINT ( 'NONE',  ( -4.458734124999999437, -2.562499998634407028, 0.000000000000000000 ) ) ;
#61172 = CARTESIAN_POINT ( 'NONE',  ( 4.458734124999999437, -36.06249999863440792, -5.460374474430324690E-16 ) ) ;
#61173 = CARTESIAN_POINT ( 'NONE',  ( 1.339745962155612702, -16.16965819600733667, -5.000000000000000000 ) ) ;
#61174 = CARTESIAN_POINT ( 'NONE',  ( 2.229367062499998831, -77.89583333196773651, -3.861377020970580887 ) ) ;
#61175 = CARTESIAN_POINT ( 'NONE',  ( -6.874999999999995559, 4.690970937165706900, -7.298562697733101068 ) ) ;
#61176 = ORIENTED_EDGE ( 'NONE', *, *, #19239, .T. ) ;
#61177 = CARTESIAN_POINT ( 'NONE',  ( -58.24261429053147765, -155.0000000000000284, -3.805975901505573411 ) ) ;
#61178 = CARTESIAN_POINT ( 'NONE',  ( 0.000000000000000000, -170.0000000000000000, 0.000000000000000000 ) ) ;
#61179 = CARTESIAN_POINT ( 'NONE',  ( 2.229367062499998831, -66.89583333196773651, -3.861377020970580887 ) ) ;
#61180 = CARTESIAN_POINT ( 'NONE',  ( 4.458734124999998549, -9.979166665301068662, -2.574251347313721627 ) ) ;
#61181 = VERTEX_POINT ( 'NONE', #26962 ) ;
#61182 = AXIS2_PLACEMENT_3D ( 'NONE', #3011, #51574, #61231 ) ;
#61183 = CARTESIAN_POINT ( 'NONE',  ( 5.000000000000000000, -5.499999999999998224, -6.123233995736766282E-16 ) ) ;
#61184 = CARTESIAN_POINT ( 'NONE',  ( 1.975475456537005874E-15, -1.749999999999999334, 5.000000000000000000 ) ) ;
#61185 = CARTESIAN_POINT ( 'NONE',  ( -3.152548672688508926E-16, -8.812499998634406140, -5.148502694627439702 ) ) ;
#61186 = CARTESIAN_POINT ( 'NONE',  ( -58.24261429053147765, -147.3750000027312126, -3.805975901505573855 ) ) ;
#61187 = CARTESIAN_POINT ( 'NONE',  ( 2.229367062499998831, 7.354166668032259935, -3.861377020970580887 ) ) ;
#61188 = CARTESIAN_POINT ( 'NONE',  ( 0.000000000000000000, -170.0000000000000000, 5.000000000000000000 ) ) ;
#61189 = CARTESIAN_POINT ( 'NONE',  ( -1.846868145590737420, -155.7500000013656063, 4.458734124999997661 ) ) ;
#61190 = CARTESIAN_POINT ( 'NONE',  ( 0.000000000000000000, -120.0000000000000000, 0.000000000000000000 ) ) ;
#61191 = ORIENTED_EDGE ( 'NONE', *, *, #16566, .T. ) ;
#61192 = CARTESIAN_POINT ( 'NONE',  ( -3.152548672688508926E-16, -86.56249999863440792, -5.148502694627439702 ) ) ;
#61193 = CARTESIAN_POINT ( 'NONE',  ( -5.000000000000000000, -78.00000000000000000, 0.000000000000000000 ) ) ;
#61194 = CARTESIAN_POINT ( 'NONE',  ( 4.458734124999998549, -3.729166665301070438, -2.574251347313721627 ) ) ;
#61195 = CARTESIAN_POINT ( 'NONE',  ( 1.975475456537005874E-15, -75.74999999999998579, 5.000000000000000000 ) ) ;
#61196 = CARTESIAN_POINT ( 'NONE',  ( 5.000000000000000888, -31.45833333060214798, 2.886751345948126879 ) ) ;
#61197 = FACE_BOUND ( 'NONE', #25545, .T. ) ;
#61198 = CARTESIAN_POINT ( 'NONE',  ( -4.458734124999999437, 26.68750000136559564, 0.000000000000000000 ) ) ;
#61199 = CARTESIAN_POINT ( 'NONE',  ( -6.972266317189433020E-16, -21.12499999726881228, -5.000000000000000000 ) ) ;
#61200 = CARTESIAN_POINT ( 'NONE',  ( -2.229367062500000163, 27.52083333469892779, -3.861377020970580443 ) ) ;
#61201 = CARTESIAN_POINT ( 'NONE',  ( -4.458734124999999437, -49.31249999863440792, 0.000000000000000000 ) ) ;
#61202 = CARTESIAN_POINT ( 'NONE',  ( -4.458734124999997661, -36.47916666530107221, 2.574251347313722516 ) ) ;
#61203 = CARTESIAN_POINT ( 'NONE',  ( -4.458734124999999437, -0.5624999986344053626, 0.000000000000000000 ) ) ;
#61204 = CARTESIAN_POINT ( 'NONE',  ( 3.061616997868383141E-16, -159.8750000027311842, -5.000000000000000000 ) ) ;
#61205 = CARTESIAN_POINT ( 'NONE',  ( -2.499999999999996447, 14.16666666666666785, 4.330127018922195425 ) ) ;
#61206 = CARTESIAN_POINT ( 'NONE',  ( -5.000000000000000000, -140.6250000027312126, -6.123233995736766282E-16 ) ) ;
#61207 = DIRECTION ( 'NONE',  ( -0.000000000000000000, 1.000000000000000000, -0.000000000000000000 ) ) ;
#61208 = CARTESIAN_POINT ( 'NONE',  ( -2.229367062500000163, -42.47916666530107932, -3.861377020970580443 ) ) ;
#61209 = CARTESIAN_POINT ( 'NONE',  ( -2.499999999999996447, -76.70833333060214443, 4.330127018922195425 ) ) ;
#61210 = CARTESIAN_POINT ( 'NONE',  ( -59.29741812935640155, -139.8750000013655779, -2.196230717870135685 ) ) ;
#61211 = LINE ( 'NONE', #61850, #12356 ) ;
#61212 = DIRECTION ( 'NONE',  ( -0.000000000000000000, 1.000000000000000000, -0.000000000000000000 ) ) ;
#61213 = CARTESIAN_POINT ( 'NONE',  ( 9.457646018065525792E-16, -86.31249999863439371, 5.148502694627439702 ) ) ;
#61214 = CARTESIAN_POINT ( 'NONE',  ( -3.152801135295367985, -160.0625000013656063, 3.152801135295367096 ) ) ;
#61215 = CARTESIAN_POINT ( 'NONE',  ( 1.975475456537005874E-15, -95.75000000000000000, 5.000000000000000000 ) ) ;
#61216 = CARTESIAN_POINT ( 'NONE',  ( -3.535250795749689387E-16, -30.24999999999999645, -5.773502691896257311 ) ) ;
#61217 = CARTESIAN_POINT ( 'NONE',  ( 1.975475456537005874E-15, -56.75000000000000000, 5.000000000000000000 ) ) ;
#61218 = EDGE_LOOP ( 'NONE', ( #56009, #52153, #14643, #24945, #48894, #14863, #42949, #9256, #40318, #58663, #4486, #41644, #60046, #54321, #10684, #32355, #12666, #723, #58371, #28647, #18573, #48493, #43650, #51956, #36470, #54480, #56175, #48795, #13525, #41568, #47395, #30124, #60616, #34378, #22465, #38670, #26694, #38028, #2471, #56253, #7842, #5584, #36245, #3100, #48591, #21600, #42244, #10829, #56044, #14510, #1306, #35353, #22644, #6373, #36866, #32064, #49093, #51630, #62839, #45368, #9214, #62721, #38268, #16447 ) ) ;
#61219 = AXIS2_PLACEMENT_3D ( 'NONE', #45332, #26038, #21851 ) ;
#61220 = CARTESIAN_POINT ( 'NONE',  ( -3.152548672688508926E-16, 16.18750000136559564, -5.148502694627439702 ) ) ;
#61221 = ORIENTED_EDGE ( 'NONE', *, *, #29373, .F. ) ;
#61222 = CARTESIAN_POINT ( 'NONE',  ( 2.229367062499998831, -92.64583333196773651, -3.861377020970580887 ) ) ;
#61223 = CARTESIAN_POINT ( 'NONE',  ( 4.458734124999999437, 14.93750000136559386, -5.460374474430324690E-16 ) ) ;
#61224 = CARTESIAN_POINT ( 'NONE',  ( -5.000000000000000000, 14.04166666939785202, -2.886751345948128211 ) ) ;
#61225 = CARTESIAN_POINT ( 'NONE',  ( -2.480964764533239819E-13, -59.75000000000000711, 5.000000000000000000 ) ) ;
#61226 = CARTESIAN_POINT ( 'NONE',  ( 1.060575238724906964E-15, 6.249999999999998224, 5.773502691896257311 ) ) ;
#61227 = EDGE_CURVE ( 'NONE', #42031, #49174, #33133, .T. ) ;
#61228 = CARTESIAN_POINT ( 'NONE',  ( 4.458734124999998549, -54.72916666530107221, -2.574251347313721627 ) ) ;
#61229 =( BOUNDED_CURVE ( )  B_SPLINE_CURVE ( 2, ( #13566, #3915, #58250, #28965, #48903, #9665, #57327, #8735, #43757 ),
 .UNSPECIFIED., .F., .F. ) 
 B_SPLINE_CURVE_WITH_KNOTS ( ( 3, 2, 2, 2, 3 ),
 ( 0.4232142857142857095, 0.4238095238095238027, 0.4249999999999999889, 0.4261904761904761751, 0.4267857142857142683 ),
 .UNSPECIFIED. ) 
 CURVE ( )  GEOMETRIC_REPRESENTATION_ITEM ( )  RATIONAL_B_SPLINE_CURVE ( ( 0.9330127018922194093, 0.9330127018922194093, 1.000000000000000000, 0.8660254037844387076, 1.000000000000000000, 0.8660254037844387076, 1.000000000000000000, 0.9330127018922194093, 0.9330127018922194093 ) ) 
 REPRESENTATION_ITEM ( '' )  );
#61230 = CARTESIAN_POINT ( 'NONE',  ( 7.500000000000000000, 1.545478204151513157, -7.491761935628701075 ) ) ;
#61231 = DIRECTION ( 'NONE',  ( 0.000000000000000000, 0.000000000000000000, 1.000000000000000000 ) ) ;
#61232 = CARTESIAN_POINT ( 'NONE',  ( 1.339745962155612702, 7.830341803992665106, -5.000000000000000000 ) ) ;
#61233 = CARTESIAN_POINT ( 'NONE',  ( 0.000000000000000000, -170.0000000000000000, 0.000000000000000000 ) ) ;
#61234 = CARTESIAN_POINT ( 'NONE',  ( -5.000000000000000000, -39.08333333333332860, -2.886751345948128211 ) ) ;
#61235 = CYLINDRICAL_SURFACE ( 'NONE', #44849, 5.000000000000000000 ) ;
#61237 = CARTESIAN_POINT ( 'NONE',  ( -2.229367062499996610, -12.39583333196774007, 3.861377020970582219 ) ) ;
#61236 = DIRECTION ( 'NONE',  ( -0.000000000000000000, 1.000000000000000000, -0.000000000000000000 ) ) ;
#61238 = CARTESIAN_POINT ( 'NONE',  ( -9.184850993605147944E-16, -143.2500000000000284, 5.000000000000000000 ) ) ;
#61239 = CARTESIAN_POINT ( 'NONE',  ( 9.457646018065525792E-16, -67.06249999863440792, 5.148502694627439702 ) ) ;
#61240 = CARTESIAN_POINT ( 'NONE',  ( -1.846868145590734756, -150.3750000013655779, -4.458734125000000326 ) ) ;
#61241 = CARTESIAN_POINT ( 'NONE',  ( -2.229367062500000163, -73.47916666530106511, -3.861377020970580443 ) ) ;
#61242 = CARTESIAN_POINT ( 'NONE',  ( -59.29741812935640155, -145.8750000013655779, -2.196230717870135685 ) ) ;
#61243 = CARTESIAN_POINT ( 'NONE',  ( 9.457646018065525792E-16, -22.31249999863440792, 5.148502694627439702 ) ) ;
#61244 = CARTESIAN_POINT ( 'NONE',  ( 5.000000000000000888, -61.45833333060214443, 2.886751345948126879 ) ) ;
#61245 = ORIENTED_EDGE ( 'NONE', *, *, #62997, .F. ) ;
#61246 = DIRECTION ( 'NONE',  ( -0.000000000000000000, 1.000000000000000000, -0.000000000000000000 ) ) ;
#61247 = EDGE_LOOP ( 'NONE', ( #8075, #46950, #5359, #40270 ) ) ;
#61248 = CARTESIAN_POINT ( 'NONE',  ( 2.229367062500001939, -64.22916666530106511, 3.861377020970579999 ) ) ;
#61249 = DIRECTION ( 'NONE',  ( -0.6485228581062915110, 0.000000000000000000, -0.7611951803011149931 ) ) ;
#61250 = CARTESIAN_POINT ( 'NONE',  ( -1.846868145590734756, -152.1250000013655779, -4.458734125000000326 ) ) ;
#61251 = ORIENTED_EDGE ( 'NONE', *, *, #47312, .T. ) ;
#61252 = CARTESIAN_POINT ( 'NONE',  ( -9.184850993605147944E-16, -155.3750000027311842, 5.000000000000000000 ) ) ;
#61253 = DIRECTION ( 'NONE',  ( -0.000000000000000000, 1.000000000000000000, -0.000000000000000000 ) ) ;
#61254 = CARTESIAN_POINT ( 'NONE',  ( 2.499999999999998668, -8.333333333333332149, -4.330127018922193649 ) ) ;
#61255 = CARTESIAN_POINT ( 'NONE',  ( -4.458734124999998549, -49.47916666530106511, 2.574251347313722516 ) ) ;
#61256 = ORIENTED_EDGE ( 'NONE', *, *, #12660, .T. ) ;
#61257 = CARTESIAN_POINT ( 'NONE',  ( -4.999999999999998224, -109.7916666639354872, 2.886751345948131764 ) ) ;
#61258 = CARTESIAN_POINT ( 'NONE',  ( 4.458734124999999437, 9.187500001365592084, -5.460374474430324690E-16 ) ) ;
#61259 = CARTESIAN_POINT ( 'NONE',  ( -2.229367062499996610, 21.85416666803226349, 3.861377020970582219 ) ) ;
#61260 = CARTESIAN_POINT ( 'NONE',  ( -59.59170313451811296, -147.5000000013656063, 1.485763867205729394 ) ) ;
#61261 = CARTESIAN_POINT ( 'NONE',  ( -59.81910112700025905, -150.3125000027311842, -2.462841084822570359 ) ) ;
#61262 = DIRECTION ( 'NONE',  ( 0.000000000000000000, 0.000000000000000000, 1.000000000000000000 ) ) ;
#61263 = AXIS2_PLACEMENT_3D ( 'NONE', #23093, #33061, #32741 ) ;
#61264 = EDGE_LOOP ( 'NONE', ( #60225, #34537, #25062, #59687 ) ) ;
#61265 = CARTESIAN_POINT ( 'NONE',  ( -2.229367062499996610, -71.14583333196773651, 3.861377020970582219 ) ) ;
#61266 = DIRECTION ( 'NONE',  ( -0.000000000000000000, 1.000000000000000000, -0.000000000000000000 ) ) ;
#61267 = CARTESIAN_POINT ( 'NONE',  ( -4.458734124999999437, 11.68750000136559564, 0.000000000000000000 ) ) ;
#61268 = VECTOR ( 'NONE', #47274, 1000.000000000000000 ) ;
#61269 = CARTESIAN_POINT ( 'NONE',  ( 1.975475456537005874E-15, -41.74999999999999289, 5.000000000000000000 ) ) ;
#61270 = CARTESIAN_POINT ( 'NONE',  ( 4.458734124999998549, -56.97916666530107932, -2.574251347313721627 ) ) ;
#61271 = CARTESIAN_POINT ( 'NONE',  ( 5.000000000000000000, -15.37499999726881228, -6.123233995736766282E-16 ) ) ;
#61272 = CARTESIAN_POINT ( 'NONE',  ( -2.500000000000000444, -100.1666666666666572, -4.330127018922193649 ) ) ;
#61273 = CYLINDRICAL_SURFACE ( 'NONE', #53212, 5.000000000000000000 ) ;
#61274 =( BOUNDED_CURVE ( )  B_SPLINE_CURVE ( 2, ( #12020, #1766, #49672, #60934, #15588, #40010, #36162, #6261, #16539 ),
 .UNSPECIFIED., .F., .F. ) 
 B_SPLINE_CURVE_WITH_KNOTS ( ( 3, 2, 2, 2, 3 ),
 ( 0.4124999999999999778, 0.4130952380952380709, 0.4142857142857143127, 0.4154761904761904989, 0.4160714285714285920 ),
 .UNSPECIFIED. ) 
 CURVE ( )  GEOMETRIC_REPRESENTATION_ITEM ( )  RATIONAL_B_SPLINE_CURVE ( ( 0.9330127018922194093, 0.9330127018922194093, 1.000000000000000000, 0.8660254037844387076, 1.000000000000000000, 0.8660254037844387076, 1.000000000000000000, 0.9330127018922194093, 0.9330127018922194093 ) ) 
 REPRESENTATION_ITEM ( '' )  );
#61275 = CARTESIAN_POINT ( 'NONE',  ( -5.000000000000000000, 19.00000000000000000, 0.000000000000000000 ) ) ;
#61276 = CARTESIAN_POINT ( 'NONE',  ( -2.229367062500000163, -19.72916666530107221, -3.861377020970580443 ) ) ;
#61277 =( BOUNDED_CURVE ( )  B_SPLINE_CURVE ( 2, ( #1449, #45485, #21050, #21695, #11701, #50956, #60297, #40974, #55470 ),
 .UNSPECIFIED., .F., .F. ) 
 B_SPLINE_CURVE_WITH_KNOTS ( ( 3, 2, 2, 2, 3 ),
 ( 0.6303571428571428381, 0.6309523809523809312, 0.6321428571428571175, 0.6333333333333333037, 0.6339285714285713969 ),
 .UNSPECIFIED. ) 
 CURVE ( )  GEOMETRIC_REPRESENTATION_ITEM ( )  RATIONAL_B_SPLINE_CURVE ( ( 0.9330127018922194093, 0.9330127018922194093, 1.000000000000000000, 0.8660254037844387076, 1.000000000000000000, 0.8660254037844387076, 1.000000000000000000, 0.9330127018922194093, 0.9330127018922194093 ) ) 
 REPRESENTATION_ITEM ( '' )  );
#61278 = VERTEX_POINT ( 'NONE', #61699 ) ;
#61279 = CARTESIAN_POINT ( 'NONE',  ( -5.000000000000000000, -61.00000000000000000, 0.000000000000000000 ) ) ;
#61280 = CARTESIAN_POINT ( 'NONE',  ( 2.229367062499998831, -106.6458333319677365, -3.861377020970580887 ) ) ;
#61281 = CARTESIAN_POINT ( 'NONE',  ( 2.071067811865476394, -158.3125000027312410, 5.000000000000000000 ) ) ;
#61282 = ORIENTED_EDGE ( 'NONE', *, *, #46485, .T. ) ;
#61283 = CARTESIAN_POINT ( 'NONE',  ( 2.229367062499998831, -102.8958333319677365, -3.861377020970580887 ) ) ;
#61284 = CARTESIAN_POINT ( 'NONE',  ( 4.458734124999999437, -25.81249999863440792, -5.460374474430324690E-16 ) ) ;
#61285 = CARTESIAN_POINT ( 'NONE',  ( 1.060575238724906964E-15, -62.62499999726880873, 5.773502691896257311 ) ) ;
#61286 = CARTESIAN_POINT ( 'NONE',  ( -53.51423613279429503, -153.5000000013656063, 4.591703134518082763 ) ) ;
#61287 = CARTESIAN_POINT ( 'NONE',  ( -5.000000000000000888, -146.5625000000000284, -2.071067811865475949 ) ) ;
#61288 = CARTESIAN_POINT ( 'NONE',  ( 9.457646018065525792E-16, -23.06249999863440792, 5.148502694627439702 ) ) ;
#61289 = CARTESIAN_POINT ( 'NONE',  ( -4.458734124999999437, -70.56249999863439371, 0.000000000000000000 ) ) ;
#61290 = CARTESIAN_POINT ( 'NONE',  ( -58.24261429053147765, -153.3750000027312126, -3.805975901505573855 ) ) ;
#61291 = CARTESIAN_POINT ( 'NONE',  ( -4.458734124999999437, -24.31249999863440436, 0.000000000000000000 ) ) ;
#61292 = CARTESIAN_POINT ( 'NONE',  ( 2.500000000000002220, 14.33333333333333393, 4.330127018922192761 ) ) ;
#61293 = CARTESIAN_POINT ( 'NONE',  ( -2.071067811865478170, -150.3125000000000284, 5.000000000000000000 ) ) ;
#61294 = CARTESIAN_POINT ( 'NONE',  ( 5.000000000000000000, -14.41666666666666963, -2.886751345948129988 ) ) ;
#61295 = CARTESIAN_POINT ( 'NONE',  ( 4.458734124999999437, -152.4375000013655779, 0.000000000000000000 ) ) ;
#61296 = EDGE_LOOP ( 'NONE', ( #33622, #18451, #41658, #52454 ) ) ;
#61297 = CYLINDRICAL_SURFACE ( 'NONE', #15328, 5.000000000000000000 ) ;
#61298 = CARTESIAN_POINT ( 'NONE',  ( -3.152548672688508926E-16, -52.81249999863440792, -5.148502694627439702 ) ) ;
#61299 = CARTESIAN_POINT ( 'NONE',  ( 1.339745962155612702, -84.16965819600731891, -5.000000000000000000 ) ) ;
#61300 = CARTESIAN_POINT ( 'NONE',  ( -2.500000000000000444, 24.83333333333333215, -4.330127018922193649 ) ) ;
#61301 = EDGE_CURVE ( 'NONE', #58748, #44248, #37877, .T. ) ;
#61302 = LINE ( 'NONE', #7589, #59182 ) ;
#61303 = CARTESIAN_POINT ( 'NONE',  ( 2.229367062499998831, 0.3541666680322609340, -3.861377020970580887 ) ) ;
#61304 = CARTESIAN_POINT ( 'NONE',  ( -5.000000000000000888, -142.4375000000000000, 2.071067811865474617 ) ) ;
#61305 = CARTESIAN_POINT ( 'NONE',  ( -6.972266317189433020E-16, -52.25000000000000711, -5.000000000000000000 ) ) ;
#61306 = CARTESIAN_POINT ( 'NONE',  ( 1.975475456537005874E-15, -87.62499999726880162, 5.000000000000000000 ) ) ;
#61307 = CARTESIAN_POINT ( 'NONE',  ( -2.229367062500000163, 17.27083333469892779, -3.861377020970580443 ) ) ;
#61308 =( BOUNDED_CURVE ( )  B_SPLINE_CURVE ( 2, ( #57427, #51960, #12401, #57113, #33282, #22378, #8215, #32331, #17554 ),
 .UNSPECIFIED., .F., .F. ) 
 B_SPLINE_CURVE_WITH_KNOTS ( ( 3, 2, 2, 2, 3 ),
 ( 0.2196428571428571397, 0.2202380952380952328, 0.2214285714285714191, 0.2226190476190476053, 0.2232142857142857262 ),
 .UNSPECIFIED. ) 
 CURVE ( )  GEOMETRIC_REPRESENTATION_ITEM ( )  RATIONAL_B_SPLINE_CURVE ( ( 0.9330127018922194093, 0.9330127018922194093, 1.000000000000000000, 0.8660254037844387076, 1.000000000000000000, 0.8660254037844387076, 1.000000000000000000, 0.9330127018922178550, 0.9330127018922194093 ) ) 
 REPRESENTATION_ITEM ( '' )  );
#61309 = CARTESIAN_POINT ( 'NONE',  ( 5.000000000000000000, 0.7083333360645184262, -2.886751345948129988 ) ) ;
#61310 = ORIENTED_EDGE ( 'NONE', *, *, #35011, .F. ) ;
#61311 = CARTESIAN_POINT ( 'NONE',  ( 1.339745962155612258, 26.29465819873852084, 5.000000000000000888 ) ) ;
#61312 = ORIENTED_EDGE ( 'NONE', *, *, #15706, .F. ) ;
#61313 = CARTESIAN_POINT ( 'NONE',  ( 5.000000000000000000, 27.70833333606451987, -2.886751345948130876 ) ) ;
#61314 = CARTESIAN_POINT ( 'NONE',  ( 2.229367062500001939, -41.97916666530107932, 3.861377020970579999 ) ) ;
#61315 = CARTESIAN_POINT ( 'NONE',  ( 3.152801135295367541, -163.5625000013656063, -3.152801135295367541 ) ) ;
#61316 = ADVANCED_FACE ( 'NONE', ( #8294 ), #27897, .T. ) ;
#61317 = CARTESIAN_POINT ( 'NONE',  ( 2.499999999999998668, -45.20833333060214443, -4.330127018922193649 ) ) ;
#61318 = ORIENTED_EDGE ( 'NONE', *, *, #52370, .T. ) ;
#61320 = ADVANCED_FACE ( 'NONE', ( #32090 ), #33358, .T. ) ;
#61319 = CARTESIAN_POINT ( 'NONE',  ( 2.229367062500001939, -18.97916666530106866, 3.861377020970579999 ) ) ;
#61321 = ORIENTED_EDGE ( 'NONE', *, *, #26460, .F. ) ;
#61322 = CARTESIAN_POINT ( 'NONE',  ( -5.000000000000000000, -88.00000000000000000, 0.000000000000000000 ) ) ;
#61323 = CARTESIAN_POINT ( 'NONE',  ( -1.846868145590737420, -165.7500000013655495, 4.458734124999999437 ) ) ;
#61324 =( BOUNDED_CURVE ( )  B_SPLINE_CURVE ( 2, ( #6520, #6201, #35788, #2028, #41225, #45429, #59925, #60872, #40599 ),
 .UNSPECIFIED., .F., .F. ) 
 B_SPLINE_CURVE_WITH_KNOTS ( ( 3, 2, 2, 2, 3 ),
 ( 0.1583333333333334925, 0.1625000000000001721, 0.1666666666666668239, 0.1708333333333335036, 0.1750000000000001554 ),
 .UNSPECIFIED. ) 
 CURVE ( )  GEOMETRIC_REPRESENTATION_ITEM ( )  RATIONAL_B_SPLINE_CURVE ( ( 0.9999999999999970024, 0.9238795325112897361, 1.000000000000000000, 0.9238795325112867385, 1.000000000000000000, 0.9238795325112867385, 1.000000000000000000, 0.9238795325112837409, 1.000000000000003109 ) ) 
 REPRESENTATION_ITEM ( '' )  );
#61326 = VERTEX_POINT ( 'NONE', #56872 ) ;
#61325 = CARTESIAN_POINT ( 'NONE',  ( 6.123233995736766282E-16, -120.0000000000000000, -5.000000000000000000 ) ) ;
#61327 = CARTESIAN_POINT ( 'NONE',  ( -49.85088928181150436, -138.5625000000000284, -1.666127454062680702 ) ) ;
#61328 = CARTESIAN_POINT ( 'NONE',  ( 4.458734124999998549, -29.97916666530107577, -2.574251347313721627 ) ) ;
#61329 = CARTESIAN_POINT ( 'NONE',  ( -1.339745962155613812, 20.79465819873852084, -5.000000000000000000 ) ) ;
#61330 = ORIENTED_EDGE ( 'NONE', *, *, #2418, .T. ) ;
#61331 = CARTESIAN_POINT ( 'NONE',  ( -4.458734124999999437, -75.39583333196773651, -2.574251347313719407 ) ) ;
#61332 = CARTESIAN_POINT ( 'NONE',  ( -4.458734124999999437, 22.68750000136559564, 0.000000000000000000 ) ) ;
#61333 = CARTESIAN_POINT ( 'NONE',  ( 5.000000000000000000, -18.41666666666666430, -2.886751345948130876 ) ) ;
#61334 = VERTEX_POINT ( 'NONE', #37552 ) ;
#61335 = CARTESIAN_POINT ( 'NONE',  ( 0.000000000000000000, -120.0000000000000000, 0.000000000000000000 ) ) ;
#61336 = CARTESIAN_POINT ( 'NONE',  ( -57.89159099828107458, -143.9375000013656063, -3.393966926194107447 ) ) ;
#61337 = CARTESIAN_POINT ( 'NONE',  ( -3.152548672688508926E-16, -79.81249999863440792, -5.148502694627439702 ) ) ;
#61338 = CARTESIAN_POINT ( 'NONE',  ( -50.01589407740564042, -131.7500000027312126, 0.3983568153799778022 ) ) ;
#61339 = CARTESIAN_POINT ( 'NONE',  ( 1.339745962155602488, 22.29465819873851729, 5.000000000000007105 ) ) ;
#61340 = DIRECTION ( 'NONE',  ( -0.000000000000000000, 1.000000000000000000, -0.000000000000000000 ) ) ;
#61341 = CARTESIAN_POINT ( 'NONE',  ( 5.000000000000000000, 24.58333333333333215, -2.886751345948130876 ) ) ;
#61342 = CARTESIAN_POINT ( 'NONE',  ( -4.458734124999999437, -53.31249999863439371, 0.000000000000000000 ) ) ;
#61343 = CARTESIAN_POINT ( 'NONE',  ( -3.152548672688508926E-16, -47.56249999863442213, -5.148502694627439702 ) ) ;
#61344 = CARTESIAN_POINT ( 'NONE',  ( 2.499999999999998668, -108.3333333333333428, -4.330127018922193649 ) ) ;
#61345 = CARTESIAN_POINT ( 'NONE',  ( -2.499999999999996447, 4.166666666666666075, 4.330127018922195425 ) ) ;
#61346 = CARTESIAN_POINT ( 'NONE',  ( -3.152548672688508926E-16, -40.81249999863440081, -5.148502694627439702 ) ) ;
#61347 = EDGE_CURVE ( 'NONE', #57375, #23803, #30293, .T. ) ;
#61348 = CARTESIAN_POINT ( 'NONE',  ( 5.000000000000000888, 1.541666669397853573, 2.886751345948126879 ) ) ;
#61349 = FACE_OUTER_BOUND ( 'NONE', #45865, .T. ) ;
#61350 = CARTESIAN_POINT ( 'NONE',  ( -55.35523342533222291, -126.3125000013655921, 4.444560631937231499 ) ) ;
#61351 = CARTESIAN_POINT ( 'NONE',  ( -4.458734124999998549, -79.47916666530106511, 2.574251347313722516 ) ) ;
#61352 = FACE_OUTER_BOUND ( 'NONE', #39683, .T. ) ;
#61353 = CARTESIAN_POINT ( 'NONE',  ( 4.458734124999998549, -100.7291666653010651, -2.574251347313721627 ) ) ;
#61354 = CARTESIAN_POINT ( 'NONE',  ( 4.458734125000000326, -8.145833331967736513, 2.574251347313718519 ) ) ;
#61355 = ORIENTED_EDGE ( 'NONE', *, *, #601, .T. ) ;
#61356 = VECTOR ( 'NONE', #19408, 1000.000000000000114 ) ;
#61357 = CARTESIAN_POINT ( 'NONE',  ( -6.972266317189433020E-16, -36.12499999726880162, -5.000000000000000000 ) ) ;
#61358 = CARTESIAN_POINT ( 'NONE',  ( 9.457646018065525792E-16, -94.06249999863439371, 5.148502694627439702 ) ) ;
#61359 = CARTESIAN_POINT ( 'NONE',  ( 5.000000000000000000, 27.58333333333333215, -2.886751345948130876 ) ) ;
#61360 = CARTESIAN_POINT ( 'NONE',  ( -3.152548672688508926E-16, -85.81249999863440792, -5.148502694627439702 ) ) ;
#61361 = CARTESIAN_POINT ( 'NONE',  ( -2.229367062500000163, 13.27083333469892779, -3.861377020970580443 ) ) ;
#61362 = CARTESIAN_POINT ( 'NONE',  ( 6.123233995736766282E-16, -170.0000000000000000, -5.000000000000000000 ) ) ;
#61363 = AXIS2_PLACEMENT_3D ( 'NONE', #28261, #53971, #8964 ) ;
#61364 = CARTESIAN_POINT ( 'NONE',  ( -50.55543936806279248, -135.0625000013656063, 0.3552334253322060320 ) ) ;
#61365 = AXIS2_PLACEMENT_3D ( 'NONE', #49070, #10471, #24636 ) ;
#61366 = CARTESIAN_POINT ( 'NONE',  ( 2.229367062500001939, -9.979166665301068662, 3.861377020970579999 ) ) ;
#61367 = CARTESIAN_POINT ( 'NONE',  ( -3.152548672688508926E-16, 18.18750000136559564, -5.148502694627439702 ) ) ;
#61368 = CARTESIAN_POINT ( 'NONE',  ( -4.458734124999999437, -54.64583333196773651, -2.574251347313719407 ) ) ;
#61369 = CARTESIAN_POINT ( 'NONE',  ( -5.000000000000000000, -105.9999999999999858, 0.000000000000000000 ) ) ;
#61370 = CARTESIAN_POINT ( 'NONE',  ( 2.229367062499998831, -7.645833331967735624, -3.861377020970580887 ) ) ;
#61371 = LINE ( 'NONE', #47507, #51430 ) ;
#61372 = VERTEX_POINT ( 'NONE', #22776 ) ;
#61373 = CARTESIAN_POINT ( 'NONE',  ( -4.458734124999999437, -36.56249999863440792, 0.000000000000000000 ) ) ;
#61374 = CARTESIAN_POINT ( 'NONE',  ( -52.10840900171896806, -127.4375000013656063, 3.393966926194110556 ) ) ;
#61375 = CARTESIAN_POINT ( 'NONE',  ( 3.061616997868383141E-16, -155.8750000027311842, -5.000000000000000000 ) ) ;
#61376 = CARTESIAN_POINT ( 'NONE',  ( -3.152548672688508926E-16, -81.56249999863440792, -5.148502694627439702 ) ) ;
#61377 = CARTESIAN_POINT ( 'NONE',  ( 2.229367062500001939, 25.77083333469892779, 3.861377020970579999 ) ) ;
#61378 = CARTESIAN_POINT ( 'NONE',  ( 4.458734124999999437, -150.6875000013656063, 0.000000000000000000 ) ) ;
#61379 = CARTESIAN_POINT ( 'NONE',  ( -4.458734124999999437, 20.68750000136559208, 0.000000000000000000 ) ) ;
#61380 = ADVANCED_FACE ( 'NONE', ( #42685 ), #12790, .T. ) ;
#61381 = ADVANCED_FACE ( 'NONE', ( #23405 ), #62329, .T. ) ;
#61382 = CARTESIAN_POINT ( 'NONE',  ( 0.000000000000000000, -120.0000000000000000, 0.000000000000000000 ) ) ;
#61383 = CARTESIAN_POINT ( 'NONE',  ( 1.339745962155612702, -66.29465819873851729, -5.000000000000000000 ) ) ;
#61384 = CARTESIAN_POINT ( 'NONE',  ( 9.457646018065525792E-16, -85.31249999863439371, 5.148502694627439702 ) ) ;
#61385 = CARTESIAN_POINT ( 'NONE',  ( -5.000000000000000000, -64.08333333333332860, -2.886751345948128211 ) ) ;
#61386 = CARTESIAN_POINT ( 'NONE',  ( -4.999999999999999112, 20.20833333606451987, 2.886751345948131764 ) ) ;
#61387 = ORIENTED_EDGE ( 'NONE', *, *, #48439, .F. ) ;
#61388 = FACE_OUTER_BOUND ( 'NONE', #20409, .T. ) ;
#61389 = CARTESIAN_POINT ( 'NONE',  ( -6.972266317189433020E-16, -67.12499999726881583, -5.000000000000000000 ) ) ;
#61391 = CARTESIAN_POINT ( 'NONE',  ( -3.535250795749689387E-16, -24.24999999999999645, -5.773502691896257311 ) ) ;
#61390 = CARTESIAN_POINT ( 'NONE',  ( -2.500000000000000444, -72.16666666666667140, -4.330127018922193649 ) ) ;
#61392 = CARTESIAN_POINT ( 'NONE',  ( -4.458734124999999437, -29.31249999863440436, 0.000000000000000000 ) ) ;
#61393 = CARTESIAN_POINT ( 'NONE',  ( -4.458734124999999437, -86.39583333196772230, -2.574251347313719407 ) ) ;
#61394 = EDGE_CURVE ( 'NONE', #34762, #35874, #47949, .T. ) ;
#61395 = CARTESIAN_POINT ( 'NONE',  ( 2.500000000000002220, -31.54166666393548724, 4.330127018922192761 ) ) ;
#61397 = VERTEX_POINT ( 'NONE', #43316 ) ;
#61396 = CARTESIAN_POINT ( 'NONE',  ( -4.458734124999999437, -56.39583333196773651, -2.574251347313719407 ) ) ;
#61398 = CARTESIAN_POINT ( 'NONE',  ( -54.64476657466781973, -154.0625000013656347, -4.444560631937228834 ) ) ;
#61399 = EDGE_CURVE ( 'NONE', #40939, #49453, #17904, .T. ) ;
#61401 = EDGE_LOOP ( 'NONE', ( #39617, #18618, #10815, #45198 ) ) ;
#61400 = CARTESIAN_POINT ( 'NONE',  ( 4.458734124999999437, -10.06249999863440614, -5.460374474430324690E-16 ) ) ;
#61402 = CARTESIAN_POINT ( 'NONE',  ( 2.499999999999998668, -70.33333333333332860, -4.330127018922193649 ) ) ;
#61403 = CARTESIAN_POINT ( 'NONE',  ( -51.60603307380591787, -138.9375000013656063, -2.891590998281053704 ) ) ;
#61404 = CARTESIAN_POINT ( 'NONE',  ( 2.229367062500001939, -49.22916666530107221, 3.861377020970579999 ) ) ;
#61405 = VECTOR ( 'NONE', #56682, 1000.000000000000000 ) ;
#61406 = CARTESIAN_POINT ( 'NONE',  ( -3.535250795749689387E-16, -75.12499999726880162, -5.773502691896257311 ) ) ;
#61408 = ORIENTED_EDGE ( 'NONE', *, *, #27956, .T. ) ;
#61407 = CARTESIAN_POINT ( 'NONE',  ( 1.975475456537005874E-15, -85.75000000000000000, 5.000000000000000000 ) ) ;
#61409 = CARTESIAN_POINT ( 'NONE',  ( -54.60164318462004474, -151.3750000000000284, -4.984105922594373794 ) ) ;
#61410 = VECTOR ( 'NONE', #40309, 1000.000000000000000 ) ;
#61411 = CARTESIAN_POINT ( 'NONE',  ( -4.458734124999998549, -16.47916666530107577, 2.574251347313722516 ) ) ;
#61412 = CARTESIAN_POINT ( 'NONE',  ( 4.458734125000001214, -51.14583333196772941, 2.574251347313718519 ) ) ;
#61413 =( BOUNDED_CURVE ( )  B_SPLINE_CURVE ( 2, ( #58674, #152, #49338, #34216, #10740, #30348, #467, #39674, #54810 ),
 .UNSPECIFIED., .F., .F. ) 
 B_SPLINE_CURVE_WITH_KNOTS ( ( 3, 2, 2, 2, 3 ),
 ( 0.2124999999999999944, 0.2130952380952380876, 0.2142857142857142738, 0.2154761904761904878, 0.2160714285714285809 ),
 .UNSPECIFIED. ) 
 CURVE ( )  GEOMETRIC_REPRESENTATION_ITEM ( )  RATIONAL_B_SPLINE_CURVE ( ( 0.9330127018922194093, 0.9330127018922194093, 1.000000000000000000, 0.8660254037844387076, 1.000000000000000000, 0.8660254037844387076, 1.000000000000000000, 0.9330127018922194093, 0.9330127018922194093 ) ) 
 REPRESENTATION_ITEM ( '' )  );
#61414 = CARTESIAN_POINT ( 'NONE',  ( -4.999999999999998224, 1.083333333333331927, 2.886751345948131764 ) ) ;
#61415 = CARTESIAN_POINT ( 'NONE',  ( 1.846868145590736310, -139.6250000013656347, 4.458734124999999437 ) ) ;
#61416 = CARTESIAN_POINT ( 'NONE',  ( 4.458734124999999437, -101.0624999986344079, -5.460374474430324690E-16 ) ) ;
#61417 = CARTESIAN_POINT ( 'NONE',  ( 2.499999999999998668, -2.333333333333333037, -4.330127018922193649 ) ) ;
#61418 = ORIENTED_EDGE ( 'NONE', *, *, #15730, .T. ) ;
#61419 = CARTESIAN_POINT ( 'NONE',  ( -59.44456063193725015, -153.8125000013656347, -0.3552334253322034230 ) ) ;
#61420 = CARTESIAN_POINT ( 'NONE',  ( -50.01589407740564042, -143.7500000027312126, 0.3983568153799778022 ) ) ;
#61421 = CARTESIAN_POINT ( 'NONE',  ( 5.000000000000000000, 18.50000000000000000, -6.123233995736766282E-16 ) ) ;
#61422 = CARTESIAN_POINT ( 'NONE',  ( 2.229367062499998831, -5.645833331967740953, -3.861377020970580887 ) ) ;
#61423 = CARTESIAN_POINT ( 'NONE',  ( 4.458734124999999437, -94.06249999863440792, -5.460374474430324690E-16 ) ) ;
#61424 =( BOUNDED_CURVE ( )  B_SPLINE_CURVE ( 2, ( #27984, #27045, #12877, #33140, #57594, #52448, #46663, #41826, #37638 ),
 .UNSPECIFIED., .F., .F. ) 
 B_SPLINE_CURVE_WITH_KNOTS ( ( 3, 2, 2, 2, 3 ),
 ( 0.2410714285714285754, 0.2416666666666666685, 0.2428571428571428548, 0.2440476190476190410, 0.2446428571428571341 ),
 .UNSPECIFIED. ) 
 CURVE ( )  GEOMETRIC_REPRESENTATION_ITEM ( )  RATIONAL_B_SPLINE_CURVE ( ( 0.9330127018922194093, 0.9330127018922194093, 1.000000000000000000, 0.8660254037844387076, 1.000000000000000000, 0.8660254037844387076, 1.000000000000000000, 0.9330127018922194093, 0.9330127018922194093 ) ) 
 REPRESENTATION_ITEM ( '' )  );
#61425 = CARTESIAN_POINT ( 'NONE',  ( 1.846868145590735200, -149.5000000013655779, -4.458734125000000326 ) ) ;
#61426 = CARTESIAN_POINT ( 'NONE',  ( -2.229367062500000163, -20.72916666530107221, -3.861377020970580443 ) ) ;
#61427 = LINE ( 'NONE', #36974, #35542 ) ;
#61428 = CARTESIAN_POINT ( 'NONE',  ( -50.40829686548195099, -137.0000000013655779, -1.485763867205728284 ) ) ;
#61429 = CARTESIAN_POINT ( 'NONE',  ( -4.458734124999999437, -61.64583333196773651, -2.574251347313719407 ) ) ;
#61430 = CARTESIAN_POINT ( 'NONE',  ( -5.000000000000000000, -83.95833333060214443, -2.886751345948128211 ) ) ;
#61431 = CARTESIAN_POINT ( 'NONE',  ( 3.152801135295367541, -143.3125000013655779, -3.152801135295367541 ) ) ;
#61432 = CARTESIAN_POINT ( 'NONE',  ( -4.458734124999997661, 10.52083333469892779, 2.574251347313722516 ) ) ;
#61433 = ORIENTED_EDGE ( 'NONE', *, *, #8743, .T. ) ;
#61434 = CYLINDRICAL_SURFACE ( 'NONE', #23339, 5.000000000000000000 ) ;
#61435 = CARTESIAN_POINT ( 'NONE',  ( 5.000000000000000000, -61.50000000000000000, -6.123233995736766282E-16 ) ) ;
#61437 = CARTESIAN_POINT ( 'NONE',  ( 4.458734125000001214, -22.89583333196773651, 2.574251347313718519 ) ) ;
#61436 = CARTESIAN_POINT ( 'NONE',  ( 5.000000000000000888, -89.58333333333334281, 2.886751345948126879 ) ) ;
#61438 = CARTESIAN_POINT ( 'NONE',  ( -7.500000000000000000, -4.330127018922198090, -7.422398894150034288 ) ) ;
#61439 = CARTESIAN_POINT ( 'NONE',  ( -2.229367062499996610, -70.39583333196773651, 3.861377020970582219 ) ) ;
#61440 = FACE_OUTER_BOUND ( 'NONE', #16855, .T. ) ;
#61441 = CARTESIAN_POINT ( 'NONE',  ( 10.12668159690567649, 0.000000000000000000, -9.226681596905677907 ) ) ;
#61442 = CARTESIAN_POINT ( 'NONE',  ( -59.44456063193725015, -147.5625000013656063, -0.3552334253322034230 ) ) ;
#61443 = CARTESIAN_POINT ( 'NONE',  ( 5.000000000000000000, -52.37499999726881583, -6.123233995736766282E-16 ) ) ;
#61444 = CARTESIAN_POINT ( 'NONE',  ( -5.000000000000000000, -1.874999997268814944, 0.000000000000000000 ) ) ;
#61445 = CARTESIAN_POINT ( 'NONE',  ( -3.152548672688508926E-16, 6.437500001365592972, -5.148502694627439702 ) ) ;
#61446 = DIRECTION ( 'NONE',  ( -0.000000000000000000, 1.000000000000000000, -0.000000000000000000 ) ) ;
#61447 = FACE_OUTER_BOUND ( 'NONE', #53091, .T. ) ;
#61448 = CARTESIAN_POINT ( 'NONE',  ( 2.229367062499998831, 5.354166668032261711, -3.861377020970580887 ) ) ;
#61449 = CARTESIAN_POINT ( 'NONE',  ( -4.458734124999999437, -72.31249999863439371, 0.000000000000000000 ) ) ;
#61450 = CARTESIAN_POINT ( 'NONE',  ( -3.152548672688508926E-16, -17.81249999863440792, -5.148502694627439702 ) ) ;
#61451 = AXIS2_PLACEMENT_3D ( 'NONE', #50984, #6924, #59681 ) ;
#61452 = CARTESIAN_POINT ( 'NONE',  ( -5.000000000000000000, 0.000000000000000000, 0.000000000000000000 ) ) ;
#61453 = CARTESIAN_POINT ( 'NONE',  ( 1.846868145590735200, -159.2500000013656063, -4.458734125000000326 ) ) ;
#61454 = CARTESIAN_POINT ( 'NONE',  ( 75.00000000000002842, 0.000000000000000000, -5.000000000000000000 ) ) ;
#61455 = CARTESIAN_POINT ( 'NONE',  ( -4.458734124999999437, -64.39583333196772230, -2.574251347313719407 ) ) ;
#61456 = CARTESIAN_POINT ( 'NONE',  ( -5.000000000000000000, -97.87499999726881583, 0.000000000000000000 ) ) ;
#61457 = CARTESIAN_POINT ( 'NONE',  ( 5.000000000000000000, 5.708333336064518981, -2.886751345948130876 ) ) ;
#61458 = CARTESIAN_POINT ( 'NONE',  ( -2.229367062499996610, -40.14583333196773651, 3.861377020970582219 ) ) ;
#61459 = EDGE_CURVE ( 'NONE', #14760, #24668, #46899, .T. ) ;
#61460 = CARTESIAN_POINT ( 'NONE',  ( 1.339745962155615144, -60.70534180126147561, 4.999999999999999112 ) ) ;
#61461 = CARTESIAN_POINT ( 'NONE',  ( -3.152548672688508926E-16, -67.81249999863440792, -5.148502694627439702 ) ) ;
#61462 = CARTESIAN_POINT ( 'NONE',  ( -5.000000000000000000, -47.00000000000000000, 0.000000000000000000 ) ) ;
#61463 = CARTESIAN_POINT ( 'NONE',  ( 2.500000000000002220, -72.54166666393548724, 4.330127018922192761 ) ) ;
#61464 = CARTESIAN_POINT ( 'NONE',  ( 1.975475456537005874E-15, -68.62499999726881583, 5.000000000000000000 ) ) ;
#61465 = ORIENTED_EDGE ( 'NONE', *, *, #39441, .T. ) ;
#61466 = CARTESIAN_POINT ( 'NONE',  ( 6.123233995736766282E-16, -120.0000000000000000, -5.000000000000000000 ) ) ;
#61467 = DIRECTION ( 'NONE',  ( 0.000000000000000000, 0.000000000000000000, 1.000000000000000000 ) ) ;
#61468 = CARTESIAN_POINT ( 'NONE',  ( -5.000000000000000000, -6.083333333333336590, -2.886751345948128211 ) ) ;
#61469 = CARTESIAN_POINT ( 'NONE',  ( -3.152548672688508926E-16, -72.56249999863439371, -5.148502694627439702 ) ) ;
#61470 = CARTESIAN_POINT ( 'NONE',  ( -2.499999999999996447, -30.70833333060214443, 4.330127018922195425 ) ) ;
#61471 = CARTESIAN_POINT ( 'NONE',  ( 2.500000000000002220, -12.54166666393548013, 4.330127018922192761 ) ) ;
#61473 = ORIENTED_EDGE ( 'NONE', *, *, #53079, .F. ) ;
#61472 = CARTESIAN_POINT ( 'NONE',  ( -4.458734124999999437, -41.39583333196773651, -2.574251347313719407 ) ) ;
#61474 = CYLINDRICAL_SURFACE ( 'NONE', #3556, 5.000000000000000000 ) ;
#61476 = ORIENTED_EDGE ( 'NONE', *, *, #14861, .F. ) ;
#61475 = CARTESIAN_POINT ( 'NONE',  ( -3.152548672688508926E-16, 7.187500001365594748, -5.148502694627439702 ) ) ;
#61477 = CARTESIAN_POINT ( 'NONE',  ( -5.000000000000000888, -151.5625000000001137, -2.071067811865475949 ) ) ;
#61478 = CARTESIAN_POINT ( 'NONE',  ( -2.500000000000000444, -57.16666666666667140, -4.330127018922193649 ) ) ;
#61479 = EDGE_CURVE ( 'NONE', #19582, #42594, #24475, .T. ) ;
#61480 = CARTESIAN_POINT ( 'NONE',  ( -3.152801135295367985, -161.0625000013656063, 3.152801135295367096 ) ) ;
#61481 = CARTESIAN_POINT ( 'NONE',  ( -2.229367062500000163, -33.72916666530107221, -3.861377020970580443 ) ) ;
#61482 = CARTESIAN_POINT ( 'NONE',  ( 5.000000000000000000, -10.50000000000000178, -6.123233995736766282E-16 ) ) ;
#61483 = CARTESIAN_POINT ( 'NONE',  ( 4.458734124999998549, -81.72916666530106511, -2.574251347313721627 ) ) ;
#61484 =( BOUNDED_CURVE ( )  B_SPLINE_CURVE ( 2, ( #19488, #14980, #20775, #15305, #25272, #35566, #15630, #54866, #9826 ),
 .UNSPECIFIED., .F., .F. ) 
 B_SPLINE_CURVE_WITH_KNOTS ( ( 3, 2, 2, 2, 3 ),
 ( 0.8803571428571428381, 0.8809523809523809312, 0.8821428571428571175, 0.8833333333333333037, 0.8839285714285713969 ),
 .UNSPECIFIED. ) 
 CURVE ( )  GEOMETRIC_REPRESENTATION_ITEM ( )  RATIONAL_B_SPLINE_CURVE ( ( 0.9330127018922194093, 0.9330127018922194093, 1.000000000000000000, 0.8660254037844387076, 1.000000000000000000, 0.8660254037844387076, 1.000000000000000000, 0.9330127018922194093, 0.9330127018922194093 ) ) 
 REPRESENTATION_ITEM ( '' )  );
#61485 = CARTESIAN_POINT ( 'NONE',  ( 3.535533905932736864, -166.1250000000000284, 3.535533905932738641 ) ) ;
#61486 = EDGE_CURVE ( 'NONE', #34014, #11394, #8884, .T. ) ;
#61487 = CARTESIAN_POINT ( 'NONE',  ( -2.229367062499996610, -89.14583333196773651, 3.861377020970582219 ) ) ;
#61488 = CARTESIAN_POINT ( 'NONE',  ( -50.40829686548195099, -132.2500000013656063, -1.485763867205728284 ) ) ;
#61489 = CARTESIAN_POINT ( 'NONE',  ( 4.458734124999998549, 0.02083333469892617584, -2.574251347313721627 ) ) ;
#61490 = CARTESIAN_POINT ( 'NONE',  ( -2.229367062499996610, -34.39583333196772941, 3.861377020970582219 ) ) ;
#61491 = EDGE_CURVE ( 'NONE', #27115, #3560, #15472, .T. ) ;
#61492 = CARTESIAN_POINT ( 'NONE',  ( 5.000000000000000000, -16.29166666393548368, -2.886751345948130876 ) ) ;
#61493 = CARTESIAN_POINT ( 'NONE',  ( -3.152548672688508926E-16, -81.81249999863440792, -5.148502694627439702 ) ) ;
#61494 = CARTESIAN_POINT ( 'NONE',  ( -5.000000000000000000, 16.04166666939785202, -2.886751345948128211 ) ) ;
#61495 = ORIENTED_EDGE ( 'NONE', *, *, #26301, .T. ) ;
#61496 = CARTESIAN_POINT ( 'NONE',  ( -3.535533905932737309, -148.7500000027311842, -3.535533905932738197 ) ) ;
#61497 = FACE_OUTER_BOUND ( 'NONE', #35182, .T. ) ;
#61498 = CARTESIAN_POINT ( 'NONE',  ( 4.458734125000001214, -72.14583333196773651, 2.574251347313718519 ) ) ;
#61499 = AXIS2_PLACEMENT_3D ( 'NONE', #21202, #46601, #23028 ) ;
#61500 = CARTESIAN_POINT ( 'NONE',  ( -2.229367062500000163, -8.729166665301073991, -3.861377020970580443 ) ) ;
#61501 = ORIENTED_EDGE ( 'NONE', *, *, #52922, .F. ) ;
#61502 = CARTESIAN_POINT ( 'NONE',  ( 5.000000000000000000, -164.0000000000000000, 0.000000000000000000 ) ) ;
#61503 = CARTESIAN_POINT ( 'NONE',  ( 0.000000000000000000, -120.0000000000000000, 0.000000000000000000 ) ) ;
#61504 = CARTESIAN_POINT ( 'NONE',  ( -2.229367062499996610, -9.395833331967736513, 3.861377020970582219 ) ) ;
#61505 = CARTESIAN_POINT ( 'NONE',  ( -60.14911071818854538, -147.1875000027312410, 1.666127454062681146 ) ) ;
#61506 = CARTESIAN_POINT ( 'NONE',  ( -4.458734124999999437, 2.604166668032263043, -2.574251347313719407 ) ) ;
#61507 = CARTESIAN_POINT ( 'NONE',  ( -6.972266317189433020E-16, -88.25000000000000000, -5.000000000000000000 ) ) ;
#61508 = CARTESIAN_POINT ( 'NONE',  ( 4.458734124999999437, -157.3750000013655779, -1.846868145590734978 ) ) ;
#61509 =( BOUNDED_CURVE ( )  B_SPLINE_CURVE ( 2, ( #7779, #21934, #32849, #42489, #56362, #27382, #18044, #61816, #41532 ),
 .UNSPECIFIED., .F., .F. ) 
 B_SPLINE_CURVE_WITH_KNOTS ( ( 3, 2, 2, 2, 3 ),
 ( 0.08750000000000000833, 0.08809523809523810145, 0.08928571428571428770, 0.09047619047619047394, 0.09107142857142856707 ),
 .UNSPECIFIED. ) 
 CURVE ( )  GEOMETRIC_REPRESENTATION_ITEM ( )  RATIONAL_B_SPLINE_CURVE ( ( 0.9330127018922192983, 0.9330127018922200755, 1.000000000000000000, 0.8660254037844387076, 1.000000000000000000, 0.8660254037844387076, 1.000000000000000000, 0.9330127018922194093, 0.9330127018922194093 ) ) 
 REPRESENTATION_ITEM ( '' )  );
#61510 = CARTESIAN_POINT ( 'NONE',  ( -4.458734124999999437, 25.35416666803225993, -2.574251347313719407 ) ) ;
#61511 = ORIENTED_EDGE ( 'NONE', *, *, #10608, .F. ) ;
#61512 = CARTESIAN_POINT ( 'NONE',  ( -4.458734124999997661, -84.22916666530107932, 2.574251347313722516 ) ) ;
#61513 = CARTESIAN_POINT ( 'NONE',  ( -5.000000000000000000, -78.08333333333332860, -2.886751345948128211 ) ) ;
#61514 = CARTESIAN_POINT ( 'NONE',  ( -2.229367062500000163, -10.47916666530106866, -3.861377020970580443 ) ) ;
#61515 = DIRECTION ( 'NONE',  ( 0.000000000000000000, 0.000000000000000000, 1.000000000000000000 ) ) ;
#61516 = DIRECTION ( 'NONE',  ( 0.000000000000000000, 0.000000000000000000, 1.000000000000000000 ) ) ;
#61517 = DIRECTION ( 'NONE',  ( 0.000000000000000000, 0.000000000000000000, 1.000000000000000000 ) ) ;
#61518 = CARTESIAN_POINT ( 'NONE',  ( 1.060575238724906964E-15, -33.62499999726880873, 5.773502691896257311 ) ) ;
#61519 = CARTESIAN_POINT ( 'NONE',  ( 6.123233995736766282E-16, -170.0000000000000000, -5.000000000000000000 ) ) ;
#61520 = CARTESIAN_POINT ( 'NONE',  ( -4.458734124999999437, 26.60416666803225993, -2.574251347313719407 ) ) ;
#61521 = CARTESIAN_POINT ( 'NONE',  ( -1.339745962155727277, -94.79465819873854571, 4.999999999999933387 ) ) ;
#61522 = CARTESIAN_POINT ( 'NONE',  ( -4.458734124999997661, 21.77083333469892779, 2.574251347313722516 ) ) ;
#61523 = CARTESIAN_POINT ( 'NONE',  ( -3.152548672688508926E-16, -52.56249999863440792, -5.148502694627439702 ) ) ;
#61524 = CARTESIAN_POINT ( 'NONE',  ( -2.229367062499996610, -2.395833331967737845, 3.861377020970582219 ) ) ;
#61525 = CARTESIAN_POINT ( 'NONE',  ( 5.000000000000000000, 16.50000000000000000, -6.123233995736766282E-16 ) ) ;
#61526 = CARTESIAN_POINT ( 'NONE',  ( 5.000000000000000888, -142.0625000027311842, -2.071067811865475505 ) ) ;
#61527 = CARTESIAN_POINT ( 'NONE',  ( -6.972266317189433020E-16, -69.24999999999998579, -5.000000000000000000 ) ) ;
#61528 = CARTESIAN_POINT ( 'NONE',  ( -4.458734124999999437, -49.39583333196773651, -2.574251347313719407 ) ) ;
#61529 = CARTESIAN_POINT ( 'NONE',  ( 2.499999999999998668, -79.20833333060213022, -4.330127018922193649 ) ) ;
#61530 = CARTESIAN_POINT ( 'NONE',  ( -58.39396692619412477, -138.6875000013656347, 2.891590998281057701 ) ) ;
#61531 = LINE ( 'NONE', #17463, #4181 ) ;
#61532 = EDGE_CURVE ( 'NONE', #33389, #54885, #39116, .T. ) ;
#61533 = CARTESIAN_POINT ( 'NONE',  ( 1.975475456537005874E-15, 6.249999999999998224, 5.000000000000000000 ) ) ;
#61534 = CARTESIAN_POINT ( 'NONE',  ( -4.458734124999999437, -83.64583333196773651, -2.574251347313719407 ) ) ;
#61535 = CARTESIAN_POINT ( 'NONE',  ( 1.846868145590735200, -157.5000000013656063, -4.458734124999999437 ) ) ;
#61536 = CARTESIAN_POINT ( 'NONE',  ( 5.000000000000000888, -32.58333333333333570, 2.886751345948126879 ) ) ;
#61537 = VERTEX_POINT ( 'NONE', #14045 ) ;
#61538 = CARTESIAN_POINT ( 'NONE',  ( -4.458734124999998549, 15.52083333469892779, 2.574251347313722516 ) ) ;
#61539 = ORIENTED_EDGE ( 'NONE', *, *, #37842, .F. ) ;
#61540 = CARTESIAN_POINT ( 'NONE',  ( 9.457646018065525792E-16, -98.06249999863440792, 5.148502694627439702 ) ) ;
#61541 = CARTESIAN_POINT ( 'NONE',  ( -2.229367062500000163, 14.27083333469892601, -3.861377020970580443 ) ) ;
#61542 = AXIS2_PLACEMENT_3D ( 'NONE', #58673, #30676, #25852 ) ;
#61543 = CARTESIAN_POINT ( 'NONE',  ( 5.000000000000000000, 18.70833333606451632, -2.886751345948129988 ) ) ;
#61544 = CARTESIAN_POINT ( 'NONE',  ( 1.975475456537005874E-15, -10.75000000000000000, 5.000000000000000000 ) ) ;
#61545 = CARTESIAN_POINT ( 'NONE',  ( 5.000000000000000000, 6.499999999999999112, -6.123233995736766282E-16 ) ) ;
#61546 = VECTOR ( 'NONE', #18819, 1000.000000000000000 ) ;
#61547 = CARTESIAN_POINT ( 'NONE',  ( 2.229367062499998831, -56.64583333196773651, -3.861377020970580887 ) ) ;
#61548 = CARTESIAN_POINT ( 'NONE',  ( -2.500000000000000444, -40.16666666666667140, -4.330127018922193649 ) ) ;
#61549 = CARTESIAN_POINT ( 'NONE',  ( 2.499999999999998668, -78.33333333333332860, -4.330127018922193649 ) ) ;
#61550 = CARTESIAN_POINT ( 'NONE',  ( -56.37266686252615955, -135.0000000000000284, -4.242180533871957593 ) ) ;
#61551 = LINE ( 'NONE', #17154, #4987 ) ;
#61552 = CARTESIAN_POINT ( 'NONE',  ( -51.75738570946856498, -145.8750000027312126, 3.805975901505576964 ) ) ;
#61553 = CARTESIAN_POINT ( 'NONE',  ( 5.000000000000000000, -39.41666666666666430, -2.886751345948129988 ) ) ;
#61554 = CARTESIAN_POINT ( 'NONE',  ( 5.000000000000000000, -96.50000000000000000, -6.123233995736766282E-16 ) ) ;
#61556 = CARTESIAN_POINT ( 'NONE',  ( 9.457646018065525792E-16, -20.31249999863440081, 5.148502694627439702 ) ) ;
#61555 = CARTESIAN_POINT ( 'NONE',  ( -1.339745962155610925, -47.79465819873851729, 5.000000000000000000 ) ) ;
#61557 = CARTESIAN_POINT ( 'NONE',  ( 2.229367062499998831, -62.64583333196774362, -3.861377020970580887 ) ) ;
#61558 = CARTESIAN_POINT ( 'NONE',  ( 3.152801135295366208, -146.8125000013655779, 3.152801135295367985 ) ) ;
#61559 = CARTESIAN_POINT ( 'NONE',  ( -4.458734124999998549, -73.22916666530106511, 2.574251347313722516 ) ) ;
#61560 = CARTESIAN_POINT ( 'NONE',  ( -59.59170313451811296, -148.7500000013655779, 1.485763867205729394 ) ) ;
#61561 = CARTESIAN_POINT ( 'NONE',  ( -2.229367062499996610, -19.39583333196774007, 3.861377020970582219 ) ) ;
#61562 = CARTESIAN_POINT ( 'NONE',  ( 1.060575238724906964E-15, -62.62499999726880873, 5.773502691896257311 ) ) ;
#61563 = ORIENTED_EDGE ( 'NONE', *, *, #58600, .F. ) ;
#61564 = CYLINDRICAL_SURFACE ( 'NONE', #28190, 5.000000000000000000 ) ;
#61565 = VERTEX_POINT ( 'NONE', #34944 ) ;
#61566 = CARTESIAN_POINT ( 'NONE',  ( 2.229367062500001939, -62.22916666530106511, 3.861377020970579999 ) ) ;
#61567 = CARTESIAN_POINT ( 'NONE',  ( 5.000000000000000000, -21.37499999726881228, -6.123233995736766282E-16 ) ) ;
#61568 = DIRECTION ( 'NONE',  ( -0.000000000000000000, 1.000000000000000000, -0.000000000000000000 ) ) ;
#61569 = CARTESIAN_POINT ( 'NONE',  ( -4.458734124999999437, -152.9375000013655779, -5.460374474430324690E-16 ) ) ;
#61570 = ORIENTED_EDGE ( 'NONE', *, *, #46256, .F. ) ;
#61571 = CARTESIAN_POINT ( 'NONE',  ( -5.000000000000000000, 3.041666669397851130, -2.886751345948128211 ) ) ;
#61572 = CARTESIAN_POINT ( 'NONE',  ( -58.80597590150559739, -125.0000000000000284, 3.242614290531460330 ) ) ;
#61573 = FACE_OUTER_BOUND ( 'NONE', #49925, .T. ) ;
#61574 = CARTESIAN_POINT ( 'NONE',  ( -3.152548672688508926E-16, -52.81249999863440792, -5.148502694627439702 ) ) ;
#61575 = ORIENTED_EDGE ( 'NONE', *, *, #58903, .T. ) ;
#61576 = CARTESIAN_POINT ( 'NONE',  ( 1.206569728928466700, 7.963640680051486953, -0.4524126574264497602 ) ) ;
#61577 = CARTESIAN_POINT ( 'NONE',  ( -4.458734124999998549, 7.770833334698925121, 2.574251347313722516 ) ) ;
#61578 = CARTESIAN_POINT ( 'NONE',  ( 4.458734124999999437, 21.18750000136559208, -5.460374474430324690E-16 ) ) ;
#61579 = CARTESIAN_POINT ( 'NONE',  ( -52.80376928212989185, -149.8750000013655779, -4.297418129356379346 ) ) ;
#61580 = CARTESIAN_POINT ( 'NONE',  ( 5.000000000000000000, -77.41666666666665719, -2.886751345948130876 ) ) ;
#61581 = CARTESIAN_POINT ( 'NONE',  ( 3.152801135295367541, -169.3125000013656063, -3.152801135295367541 ) ) ;
#61582 = AXIS2_PLACEMENT_3D ( 'NONE', #8168, #32279, #3968 ) ;
#61583 = VERTEX_POINT ( 'NONE', #25285 ) ;
#61584 = CARTESIAN_POINT ( 'NONE',  ( -3.152548672688508926E-16, -70.56249999863439371, -5.148502694627439702 ) ) ;
#61585 = CARTESIAN_POINT ( 'NONE',  ( 1.339745962155612702, 14.83034180399266511, -5.000000000000000000 ) ) ;
#61586 = CARTESIAN_POINT ( 'NONE',  ( 9.457646018065525792E-16, 5.937500001365592972, 5.148502694627439702 ) ) ;
#61587 = EDGE_CURVE ( 'NONE', #23020, #31090, #1209, .T. ) ;
#61588 = AXIS2_PLACEMENT_3D ( 'NONE', #10404, #14583, #53518 ) ;
#61589 = CARTESIAN_POINT ( 'NONE',  ( -2.229367062499996610, -60.39583333196774362, 3.861377020970582219 ) ) ;
#61590 = CARTESIAN_POINT ( 'NONE',  ( -5.000000000000000000, -16.95833333060214443, -2.886751345948128211 ) ) ;
#61591 = DIRECTION ( 'NONE',  ( 0.000000000000000000, 0.000000000000000000, -1.000000000000000000 ) ) ;
#61592 = CARTESIAN_POINT ( 'NONE',  ( -9.184850993605147944E-16, -161.2500000000000000, 5.000000000000000000 ) ) ;
#61593 = CARTESIAN_POINT ( 'NONE',  ( 5.000000000000000000, 19.70833333606451632, -2.886751345948130876 ) ) ;
#61594 = FACE_OUTER_BOUND ( 'NONE', #17252, .T. ) ;
#61595 = CARTESIAN_POINT ( 'NONE',  ( 2.229367062500001939, -34.97916666530107221, 3.861377020970579999 ) ) ;
#61596 = CARTESIAN_POINT ( 'NONE',  ( -3.152548672688508926E-16, -23.81249999863440792, -5.148502694627439702 ) ) ;
#61597 = ORIENTED_EDGE ( 'NONE', *, *, #17302, .F. ) ;
#61598 = CARTESIAN_POINT ( 'NONE',  ( -2.229367062500000163, -109.4791666653010651, -3.861377020970580443 ) ) ;
#61599 = CARTESIAN_POINT ( 'NONE',  ( 5.000000000000000000, -154.1250000027312126, 0.000000000000000000 ) ) ;
#61600 = VERTEX_POINT ( 'NONE', #63264 ) ;
#61601 = CARTESIAN_POINT ( 'NONE',  ( -2.229367062500000163, -100.7291666653010651, -3.861377020970580443 ) ) ;
#61602 = CARTESIAN_POINT ( 'NONE',  ( -2.229367062500000163, -33.47916666530107221, -3.861377020970580443 ) ) ;
#61603 = CARTESIAN_POINT ( 'NONE',  ( 1.060575238724906964E-15, -60.62499999726880873, 5.773502691896257311 ) ) ;
#61604 = CARTESIAN_POINT ( 'NONE',  ( -57.19623071787017210, -153.6250000013655779, 4.297418129356382899 ) ) ;
#61605 =( BOUNDED_CURVE ( )  B_SPLINE_CURVE ( 2, ( #22573, #47323, #61496, #38298, #42170, #57616, #3891, #28321, #46684 ),
 .UNSPECIFIED., .F., .F. ) 
 B_SPLINE_CURVE_WITH_KNOTS ( ( 3, 2, 2, 2, 3 ),
 ( 0.6749999999999996003, 0.6791666666666662522, 0.6833333333333329040, 0.6874999999999996669, 0.6916666666666663188 ),
 .UNSPECIFIED. ) 
 CURVE ( )  GEOMETRIC_REPRESENTATION_ITEM ( )  RATIONAL_B_SPLINE_CURVE ( ( 1.000000000000008216, 0.9238795325112786339, 1.000000000000000000, 0.9238795325112867385, 1.000000000000000000, 0.9238795325112867385, 1.000000000000000000, 0.9238795325112928447, 0.9999999999999938938 ) ) 
 REPRESENTATION_ITEM ( '' )  );
#61606 = CARTESIAN_POINT ( 'NONE',  ( 3.535533905932738197, -145.8750000000000000, -3.535533905932738197 ) ) ;
#61607 = CARTESIAN_POINT ( 'NONE',  ( -4.458734124999997661, -26.22916666530106866, 2.574251347313722516 ) ) ;
#61608 = CARTESIAN_POINT ( 'NONE',  ( -2.229367062499996610, -68.39583333196773651, 3.861377020970582219 ) ) ;
#61609 = CARTESIAN_POINT ( 'NONE',  ( 1.975475456537005874E-15, -74.75000000000000000, 5.000000000000000000 ) ) ;
#61610 = CARTESIAN_POINT ( 'NONE',  ( 2.229367062499998831, -23.64583333196773651, -3.861377020970580887 ) ) ;
#61611 = CARTESIAN_POINT ( 'NONE',  ( -58.24261429053147765, -135.3750000027312410, -3.805975901505573855 ) ) ;
#61612 = CARTESIAN_POINT ( 'NONE',  ( -5.000000000000000000, 9.125000002731184168, 0.000000000000000000 ) ) ;
#61613 = CARTESIAN_POINT ( 'NONE',  ( -3.535250795749689387E-16, -17.25000000000000000, -5.773502691896257311 ) ) ;
#61614 = CARTESIAN_POINT ( 'NONE',  ( 4.458734125000000326, -148.3750000013655779, -1.846868145590734978 ) ) ;
#61615 = ORIENTED_EDGE ( 'NONE', *, *, #22697, .T. ) ;
#61616 = CARTESIAN_POINT ( 'NONE',  ( -55.39835681537999790, -152.8750000000000284, 4.984105922594378235 ) ) ;
#61617 = CARTESIAN_POINT ( 'NONE',  ( -2.229367062499996610, -53.39583333196773651, 3.861377020970582219 ) ) ;
#61618 = CARTESIAN_POINT ( 'NONE',  ( 5.000000000000000000, -2.416666666666663410, -2.886751345948130876 ) ) ;
#61619 = CARTESIAN_POINT ( 'NONE',  ( 1.975475456537005874E-15, -51.62499999726880873, 5.000000000000000000 ) ) ;
#61620 = CARTESIAN_POINT ( 'NONE',  ( 5.000000000000000000, 24.58333333333333215, -2.886751345948129988 ) ) ;
#61621 = CARTESIAN_POINT ( 'NONE',  ( -2.916731409357579869E-14, 18.25000000000000000, 5.000000000000000888 ) ) ;
#61622 = CARTESIAN_POINT ( 'NONE',  ( -4.458734124999999437, -1.395833331967737179, -2.574251347313719407 ) ) ;
#61623 = CARTESIAN_POINT ( 'NONE',  ( 2.500000000000002220, 28.33333333333333215, 4.330127018922192761 ) ) ;
#61624 = CARTESIAN_POINT ( 'NONE',  ( 1.339745962155612702, -14.29465819873851906, -5.000000000000000000 ) ) ;
#61625 = CARTESIAN_POINT ( 'NONE',  ( 2.499999999999998668, -87.20833333060214443, -4.330127018922193649 ) ) ;
#61626 = CARTESIAN_POINT ( 'NONE',  ( -4.458734124999998549, 8.520833334698926009, 2.574251347313722516 ) ) ;
#61627 = CARTESIAN_POINT ( 'NONE',  ( -5.000000000000000000, 4.041666669397852019, -2.886751345948128211 ) ) ;
#61628 = ORIENTED_EDGE ( 'NONE', *, *, #59774, .T. ) ;
#61629 = CARTESIAN_POINT ( 'NONE',  ( -1.339745962155613812, -30.08034179853029144, -5.000000000000000000 ) ) ;
#61630 = ORIENTED_EDGE ( 'NONE', *, *, #18363, .F. ) ;
#61631 =( GEOMETRIC_REPRESENTATION_CONTEXT ( 3 ) GLOBAL_UNCERTAINTY_ASSIGNED_CONTEXT ( ( #58378 ) ) GLOBAL_UNIT_ASSIGNED_CONTEXT ( ( #17021, #17337, #56587 ) ) REPRESENTATION_CONTEXT ( 'NONE', 'WORKASPACE' ) );
#61632 = FACE_OUTER_BOUND ( 'NONE', #32989, .T. ) ;
#61633 = CARTESIAN_POINT ( 'NONE',  ( -2.229367062499996610, -49.14583333196772941, 3.861377020970582219 ) ) ;
#61634 = CARTESIAN_POINT ( 'NONE',  ( 2.730187237215162345E-16, -164.4375000013655779, -4.458734124999999437 ) ) ;
#61635 = AXIS2_PLACEMENT_3D ( 'NONE', #52522, #3632, #42853 ) ;
#61636 = CARTESIAN_POINT ( 'NONE',  ( 5.000000000000000000, -42.29166666393548724, -2.886751345948129988 ) ) ;
#61637 = EDGE_LOOP ( 'NONE', ( #37424, #15022, #60164, #3188 ) ) ;
#61638 = CARTESIAN_POINT ( 'NONE',  ( 2.229367062499998831, -23.64583333196773651, -3.861377020970580887 ) ) ;
#61639 = VERTEX_POINT ( 'NONE', #10175 ) ;
#61640 = CARTESIAN_POINT ( 'NONE',  ( 2.500000000000002220, -88.66666666666665719, 4.330127018922192761 ) ) ;
#61641 = CARTESIAN_POINT ( 'NONE',  ( 3.152801135295366208, -162.5625000013656063, 3.152801135295367985 ) ) ;
#61642 = CARTESIAN_POINT ( 'NONE',  ( -5.000000000000000000, -50.95833333060213732, -2.886751345948128211 ) ) ;
#61643 = CARTESIAN_POINT ( 'NONE',  ( -50.01589407740564042, -137.6250000000000284, 0.3983568153799778022 ) ) ;
#61644 = CARTESIAN_POINT ( 'NONE',  ( -2.229367062499996610, -36.39583333196773651, 3.861377020970582219 ) ) ;
#61645 = CARTESIAN_POINT ( 'NONE',  ( -5.000000000000000000, 20.04166666939785202, -2.886751345948128211 ) ) ;
#61646 = ORIENTED_EDGE ( 'NONE', *, *, #44001, .T. ) ;
#61647 = CARTESIAN_POINT ( 'NONE',  ( 9.457646018065525792E-16, -82.06249999863442213, 5.148502694627439702 ) ) ;
#61648 = CARTESIAN_POINT ( 'NONE',  ( -3.152548672688508926E-16, 26.43750000136559208, -5.148502694627439702 ) ) ;
#61649 = CARTESIAN_POINT ( 'NONE',  ( -6.972266317189433020E-16, 24.87500000273118417, -5.000000000000000000 ) ) ;
#61650 = ORIENTED_EDGE ( 'NONE', *, *, #56183, .F. ) ;
#61651 = DIRECTION ( 'NONE',  ( 0.000000000000000000, 0.000000000000000000, 1.000000000000000000 ) ) ;
#61652 = CARTESIAN_POINT ( 'NONE',  ( -51.60603307380591787, -137.1875000013656063, -2.891590998281053704 ) ) ;
#61653 = CARTESIAN_POINT ( 'NONE',  ( 4.458734124999998549, -78.97916666530106511, -2.574251347313721627 ) ) ;
#61654 = CARTESIAN_POINT ( 'NONE',  ( -58.24261429053147765, -132.3750000027312126, -3.805975901505573855 ) ) ;
#61655 = FACE_OUTER_BOUND ( 'NONE', #4898, .T. ) ;
#61656 = CARTESIAN_POINT ( 'NONE',  ( -4.999999999999998224, -82.91666666666667140, 2.886751345948131764 ) ) ;
#61657 =( BOUNDED_CURVE ( )  B_SPLINE_CURVE ( 2, ( #59947, #54793, #24883, #55434, #39339, #34852, #444, #1417, #5905 ),
 .UNSPECIFIED., .F., .F. ) 
 B_SPLINE_CURVE_WITH_KNOTS ( ( 3, 2, 2, 2, 3 ),
 ( 0.4803571428571428714, 0.4809523809523809645, 0.4821428571428571508, 0.4833333333333333370, 0.4839285714285714302 ),
 .UNSPECIFIED. ) 
 CURVE ( )  GEOMETRIC_REPRESENTATION_ITEM ( )  RATIONAL_B_SPLINE_CURVE ( ( 0.9330127018922194093, 0.9330127018922194093, 1.000000000000000000, 0.8660254037844387076, 1.000000000000000000, 0.8660254037844387076, 1.000000000000000000, 0.9330127018922194093, 0.9330127018922194093 ) ) 
 REPRESENTATION_ITEM ( '' )  );
#61658 = CARTESIAN_POINT ( 'NONE',  ( -2.500000000000000444, -47.04166666393547303, -4.330127018922193649 ) ) ;
#61659 = CARTESIAN_POINT ( 'NONE',  ( -2.229367062499996610, -55.14583333196773651, 3.861377020970582219 ) ) ;
#61660 = CARTESIAN_POINT ( 'NONE',  ( -58.24261429053147765, -151.3750000027312126, -3.805975901505573855 ) ) ;
#61661 = CARTESIAN_POINT ( 'NONE',  ( -3.152548672688508926E-16, 26.43750000136559208, -5.148502694627439702 ) ) ;
#61662 = ADVANCED_FACE ( 'NONE', ( #10486 ), #221, .T. ) ;
#61663 = CARTESIAN_POINT ( 'NONE',  ( -3.535250795749689387E-16, -105.2500000000000000, -5.773502691896257311 ) ) ;
#61664 = CARTESIAN_POINT ( 'NONE',  ( 6.123233995736766282E-16, -120.0000000000000000, -5.000000000000000000 ) ) ;
#61665 = CARTESIAN_POINT ( 'NONE',  ( -2.229367062500000163, -39.72916666530107221, -3.861377020970580443 ) ) ;
#61666 = CARTESIAN_POINT ( 'NONE',  ( 5.000000000000000888, 2.541666669397851130, 2.886751345948126879 ) ) ;
#61667 = CARTESIAN_POINT ( 'NONE',  ( 0.000000000000000000, -170.0000000000000000, 0.000000000000000000 ) ) ;
#61668 = CARTESIAN_POINT ( 'NONE',  ( -50.70258187064364108, -126.1250000013656205, 2.196230717870141014 ) ) ;
#61669 = CARTESIAN_POINT ( 'NONE',  ( -2.229367062499996610, -80.39583333196773651, 3.861377020970582219 ) ) ;
#61670 = CARTESIAN_POINT ( 'NONE',  ( 4.458734125000000326, -102.8958333319677365, 2.574251347313718519 ) ) ;
#61671 = CARTESIAN_POINT ( 'NONE',  ( 4.458734124999999437, -6.062499998634403475, -5.460374474430324690E-16 ) ) ;
#61672 = ORIENTED_EDGE ( 'NONE', *, *, #62612, .T. ) ;
#61673 = CARTESIAN_POINT ( 'NONE',  ( 0.000000000000000000, -170.0000000000000000, 5.000000000000000000 ) ) ;
#61674 = CARTESIAN_POINT ( 'NONE',  ( 2.229367062500001939, -90.97916666530106511, 3.861377020970579999 ) ) ;
#61675 = CARTESIAN_POINT ( 'NONE',  ( -9.184850993605147944E-16, -165.3750000027312126, 5.000000000000000000 ) ) ;
#61676 = CARTESIAN_POINT ( 'NONE',  ( -4.458734124999999437, -84.64583333196773651, -2.574251347313719407 ) ) ;
#61677 = CARTESIAN_POINT ( 'NONE',  ( -3.152548672688508926E-16, 12.18750000136559564, -5.148502694627439702 ) ) ;
#61678 = LINE ( 'NONE', #22121, #24329 ) ;
#61679 = CARTESIAN_POINT ( 'NONE',  ( -51.60603307380591787, -134.9375000013656063, -2.891590998281053704 ) ) ;
#61680 = ADVANCED_FACE ( 'NONE', ( #14361 ), #33984, .T. ) ;
#61681 = CARTESIAN_POINT ( 'NONE',  ( -3.152548672688508926E-16, -10.56249999863440792, -5.148502694627439702 ) ) ;
#61682 = CARTESIAN_POINT ( 'NONE',  ( 9.457646018065525792E-16, 16.68750000136559564, 5.148502694627439702 ) ) ;
#61683 = EDGE_CURVE ( 'NONE', #46689, #25400, #5692, .T. ) ;
#61684 = CARTESIAN_POINT ( 'NONE',  ( -4.458734124999999437, -52.56249999863440792, 0.000000000000000000 ) ) ;
#61685 = CARTESIAN_POINT ( 'NONE',  ( 1.339745962155615144, -38.58034179853029144, 4.999999999999999112 ) ) ;
#61686 = CARTESIAN_POINT ( 'NONE',  ( -5.000000000000000000, -21.87499999726881228, 0.000000000000000000 ) ) ;
#61687 = CARTESIAN_POINT ( 'NONE',  ( 4.458734124999998549, -8.729166665301073991, -2.574251347313721627 ) ) ;
#61688 = CYLINDRICAL_SURFACE ( 'NONE', #31903, 5.000000000000000000 ) ;
#61689 = EDGE_LOOP ( 'NONE', ( #56360, #13826, #10344, #46728 ) ) ;
#61690 = CARTESIAN_POINT ( 'NONE',  ( 9.457646018065525792E-16, -35.31249999863440792, 5.148502694627439702 ) ) ;
#61691 = CARTESIAN_POINT ( 'NONE',  ( -51.60603307380591787, -126.1875000013656063, -2.891590998281053704 ) ) ;
#61692 = CARTESIAN_POINT ( 'NONE',  ( 1.339745962155611592, 26.41965820146970501, 5.000000000000000888 ) ) ;
#61693 = CARTESIAN_POINT ( 'NONE',  ( -4.458734124999999437, -78.31249999863440792, 0.000000000000000000 ) ) ;
#61694 = CARTESIAN_POINT ( 'NONE',  ( 4.458734125000001214, 25.85416666803225638, 2.574251347313718519 ) ) ;
#61695 = ADVANCED_FACE ( 'NONE', ( #11124 ), #1502, .T. ) ;
#61696 = CARTESIAN_POINT ( 'NONE',  ( 2.730187237215162345E-16, -150.4375000013656063, -4.458734124999999437 ) ) ;
#61697 = CARTESIAN_POINT ( 'NONE',  ( -4.458734124999999437, 16.68750000136559564, 0.000000000000000000 ) ) ;
#61698 = CARTESIAN_POINT ( 'NONE',  ( -1.339745962155610925, -43.66965819600732601, 5.000000000000000000 ) ) ;
#61699 = CARTESIAN_POINT ( 'NONE',  ( -9.184850993605147944E-16, -155.2500000000000000, 5.000000000000000000 ) ) ;
#61700 = CARTESIAN_POINT ( 'NONE',  ( -4.458734124999999437, -85.56249999863439371, 0.000000000000000000 ) ) ;
#61701 = CARTESIAN_POINT ( 'NONE',  ( -4.999999999999999112, -64.91666666666667140, 2.886751345948131764 ) ) ;
#61702 = CARTESIAN_POINT ( 'NONE',  ( -5.000000000000000000, 30.00000000000000000, 0.000000000000000000 ) ) ;
#61703 = CARTESIAN_POINT ( 'NONE',  ( -5.000000000000000000, 20.12500000273118772, 0.000000000000000000 ) ) ;
#61704 = ORIENTED_EDGE ( 'NONE', *, *, #411, .F. ) ;
#61705 = CARTESIAN_POINT ( 'NONE',  ( 1.975475456537005874E-15, -35.75000000000000711, 5.000000000000000000 ) ) ;
#61706 =( BOUNDED_CURVE ( )  B_SPLINE_CURVE ( 2, ( #7519, #61555, #46745, #2690, #17488, #8154, #27753, #47381, #3332 ),
 .UNSPECIFIED., .F., .F. ) 
 B_SPLINE_CURVE_WITH_KNOTS ( ( 3, 2, 2, 2, 3 ),
 ( 0.6479166666666666963, 0.6486111111111111382, 0.6500000000000000222, 0.6513888888888889062, 0.6520833333333333481 ),
 .UNSPECIFIED. ) 
 CURVE ( )  GEOMETRIC_REPRESENTATION_ITEM ( )  RATIONAL_B_SPLINE_CURVE ( ( 0.9330127018922194093, 0.9330127018922194093, 1.000000000000000000, 0.8660254037844387076, 1.000000000000000000, 0.8660254037844387076, 1.000000000000000000, 0.9330127018922194093, 0.9330127018922194093 ) ) 
 REPRESENTATION_ITEM ( '' )  );
#61707 = CARTESIAN_POINT ( 'NONE',  ( -5.000000000000000000, -30.00000000000000000, 0.000000000000000000 ) ) ;
#61708 = CARTESIAN_POINT ( 'NONE',  ( -4.458734124999999437, -33.31249999863440792, 0.000000000000000000 ) ) ;
#61709 = CARTESIAN_POINT ( 'NONE',  ( 1.975475456537005874E-15, 5.250000000000000000, 5.000000000000000000 ) ) ;
#61710 = CARTESIAN_POINT ( 'NONE',  ( 5.000000000000000000, -26.37499999726881583, -6.123233995736766282E-16 ) ) ;
#61711 = ADVANCED_FACE ( 'NONE', ( #55534 ), #20790, .T. ) ;
#61713 = ORIENTED_EDGE ( 'NONE', *, *, #53716, .T. ) ;
#61712 = CARTESIAN_POINT ( 'NONE',  ( 4.458734124999999437, -61.81249999863440081, -5.460374474430324690E-16 ) ) ;
#61714 = CARTESIAN_POINT ( 'NONE',  ( -58.24261429053147765, -149.2500000000000284, -3.805975901505573855 ) ) ;
#61716 = ORIENTED_EDGE ( 'NONE', *, *, #58951, .T. ) ;
#61715 = CARTESIAN_POINT ( 'NONE',  ( 2.229367062499998831, -7.895833331967735624, -3.861377020970580887 ) ) ;
#61717 = CARTESIAN_POINT ( 'NONE',  ( -4.999999999999999112, -70.91666666666667140, 2.886751345948131764 ) ) ;
#61718 = CARTESIAN_POINT ( 'NONE',  ( -59.44456063193725015, -139.5625000013656063, -0.3552334253322034230 ) ) ;
#61719 = VECTOR ( 'NONE', #44245, 1000.000000000000000 ) ;
#61720 = CARTESIAN_POINT ( 'NONE',  ( 4.458734124999998549, -53.97916666530107221, -2.574251347313721627 ) ) ;
#61721 = CARTESIAN_POINT ( 'NONE',  ( -2.500000000000000444, -77.04166666393547303, -4.330127018922193649 ) ) ;
#61723 = ORIENTED_EDGE ( 'NONE', *, *, #30719, .T. ) ;
#61722 = CARTESIAN_POINT ( 'NONE',  ( -5.000000000000000000, 10.04166666939785024, -2.886751345948128211 ) ) ;
#61724 = VECTOR ( 'NONE', #48540, 1000.000000000000000 ) ;
#61725 = CARTESIAN_POINT ( 'NONE',  ( -57.46284108482265651, -150.9375000000000284, 4.819101127000239515 ) ) ;
#61726 = CARTESIAN_POINT ( 'NONE',  ( -4.458734124999998549, -17.47916666530106866, 2.574251347313722516 ) ) ;
#61727 = CARTESIAN_POINT ( 'NONE',  ( -4.458734124999998549, -58.47916666530106511, 2.574251347313722516 ) ) ;
#61728 = CARTESIAN_POINT ( 'NONE',  ( -5.000000000000000000, -24.00000000000000000, 0.000000000000000000 ) ) ;
#61729 = CARTESIAN_POINT ( 'NONE',  ( -8.190561711645485556E-16, -140.6875000013656063, 4.458734124999999437 ) ) ;
#61730 = CARTESIAN_POINT ( 'NONE',  ( -2.229367062499996610, -97.39583333196773651, 3.861377020970582219 ) ) ;
#61731 = CARTESIAN_POINT ( 'NONE',  ( 2.500000000000002220, -2.666666666666664298, 4.330127018922192761 ) ) ;
#61732 = EDGE_LOOP ( 'NONE', ( #57693, #42481, #8489, #34556 ) ) ;
#61733 = CARTESIAN_POINT ( 'NONE',  ( -50.55543936806279248, -153.3125000013656063, 0.3552334253322060320 ) ) ;
#61734 = CARTESIAN_POINT ( 'NONE',  ( -59.98410592259440222, -141.2500000027312126, -0.3983568153799752487 ) ) ;
#61735 = CARTESIAN_POINT ( 'NONE',  ( -2.500000000000000444, -13.04166666393548013, -4.330127018922193649 ) ) ;
#61736 = EDGE_CURVE ( 'NONE', #14373, #51592, #36498, .T. ) ;
#61737 = CARTESIAN_POINT ( 'NONE',  ( -4.458734124999998549, -5.229166665301072214, 2.574251347313722516 ) ) ;
#61738 = CARTESIAN_POINT ( 'NONE',  ( 9.457646018065525792E-16, -93.31249999863439371, 5.148502694627439702 ) ) ;
#61739 = EDGE_CURVE ( 'NONE', #52296, #34949, #41029, .T. ) ;
#61740 = ADVANCED_FACE ( 'NONE', ( #15643 ), #35259, .F. ) ;
#61741 = CARTESIAN_POINT ( 'NONE',  ( -3.152801135295367985, -147.0625000013655779, 3.152801135295367096 ) ) ;
#61742 = CARTESIAN_POINT ( 'NONE',  ( -4.458734124999999437, -21.56249999863440436, 0.000000000000000000 ) ) ;
#61743 = CARTESIAN_POINT ( 'NONE',  ( -1.339745962155610925, -66.79465819873851729, 5.000000000000000000 ) ) ;
#61744 = CARTESIAN_POINT ( 'NONE',  ( -50.40829686548195099, -138.0000000013656063, -1.485763867205728284 ) ) ;
#61745 = CARTESIAN_POINT ( 'NONE',  ( 4.458734124999999437, -61.06249999863440081, -5.460374474430324690E-16 ) ) ;
#61746 = FACE_OUTER_BOUND ( 'NONE', #54278, .T. ) ;
#61747 = FACE_OUTER_BOUND ( 'NONE', #44454, .T. ) ;
#61748 = CARTESIAN_POINT ( 'NONE',  ( -1.846868145590737420, -146.7500000013656063, 4.458734124999997661 ) ) ;
#61749 = CARTESIAN_POINT ( 'NONE',  ( -2.229367062500000163, 9.270833334698927786, -3.861377020970580443 ) ) ;
#61750 = ORIENTED_EDGE ( 'NONE', *, *, #19636, .F. ) ;
#61751 = CARTESIAN_POINT ( 'NONE',  ( -2.071067811865517250, -164.8125000027312126, -4.999999999999958256 ) ) ;
#61752 = FACE_OUTER_BOUND ( 'NONE', #55378, .T. ) ;
#61754 = CARTESIAN_POINT ( 'NONE',  ( -4.458734124999999437, -25.31249999863440792, 0.000000000000000000 ) ) ;
#61753 = CARTESIAN_POINT ( 'NONE',  ( -5.000000000000000000, -88.08333333333332860, -2.886751345948128211 ) ) ;
#61755 = DIRECTION ( 'NONE',  ( -0.000000000000000000, 1.000000000000000000, -0.000000000000000000 ) ) ;
#61756 = CARTESIAN_POINT ( 'NONE',  ( 4.458734124999999437, -73.06249999863439371, -5.460374474430324690E-16 ) ) ;
#61757 = CARTESIAN_POINT ( 'NONE',  ( -4.458734124999999437, 27.43750000136559208, 0.000000000000000000 ) ) ;
#61758 = CARTESIAN_POINT ( 'NONE',  ( -54.64476657466781973, -145.8125000013656063, -4.444560631937228834 ) ) ;
#61759 = CARTESIAN_POINT ( 'NONE',  ( 2.229367062499998831, 4.354166668032260823, -3.861377020970580887 ) ) ;
#61760 = CARTESIAN_POINT ( 'NONE',  ( 0.000000000000000000, -170.0000000000000000, 0.000000000000000000 ) ) ;
#61761 = EDGE_CURVE ( 'NONE', #18747, #57597, #25609, .T. ) ;
#61762 = DIRECTION ( 'NONE',  ( 0.000000000000000000, 1.000000000000000000, 0.000000000000000000 ) ) ;
#61763 = CARTESIAN_POINT ( 'NONE',  ( 2.229367062499998831, 6.354166668032262599, -3.861377020970580887 ) ) ;
#61764 = CARTESIAN_POINT ( 'NONE',  ( -2.229367062499996610, -73.14583333196773651, 3.861377020970582219 ) ) ;
#61765 = CARTESIAN_POINT ( 'NONE',  ( 9.457646018065525792E-16, -20.31249999863439726, 5.148502694627439702 ) ) ;
#61766 = CARTESIAN_POINT ( 'NONE',  ( 1.060575238724906964E-15, 1.250000000000001110, 5.773502691896257311 ) ) ;
#61767 = CARTESIAN_POINT ( 'NONE',  ( 2.730187237215162345E-16, -158.1875000013655779, -4.458734124999999437 ) ) ;
#61768 = CARTESIAN_POINT ( 'NONE',  ( 0.000000000000000000, -170.0000000000000000, 5.000000000000000000 ) ) ;
#61769 = VECTOR ( 'NONE', #18535, 1000.000000000000000 ) ;
#61770 = CARTESIAN_POINT ( 'NONE',  ( 2.229367062499998831, -66.64583333196773651, -3.861377020970580887 ) ) ;
#61771 = CARTESIAN_POINT ( 'NONE',  ( 2.500000000000002220, -97.54166666393545881, 4.330127018922192761 ) ) ;
#61772 = CARTESIAN_POINT ( 'NONE',  ( -60.14911071818854538, -149.0625000000000000, 1.666127454062681146 ) ) ;
#61773 = CARTESIAN_POINT ( 'NONE',  ( -3.152548672688508926E-16, -41.56249999863440081, -5.148502694627439702 ) ) ;
#61774 = CARTESIAN_POINT ( 'NONE',  ( -2.229367062500000163, -105.7291666653010651, -3.861377020970580443 ) ) ;
#61775 = CARTESIAN_POINT ( 'NONE',  ( -4.458734124999997661, -67.47916666530106511, 2.574251347313722516 ) ) ;
#61776 = CARTESIAN_POINT ( 'NONE',  ( 2.500000000000002220, -47.66666666666666430, 4.330127018922192761 ) ) ;
#61777 = CARTESIAN_POINT ( 'NONE',  ( 1.975475456537005874E-15, -10.62499999726881228, 5.000000000000000000 ) ) ;
#61778 = EDGE_LOOP ( 'NONE', ( #15587, #42957, #12764, #42169, #56649, #23058, #35417, #27347 ) ) ;
#61779 = CARTESIAN_POINT ( 'NONE',  ( 1.975475456537005874E-15, -89.74999999999998579, 5.000000000000000000 ) ) ;
#61780 = FACE_OUTER_BOUND ( 'NONE', #54974, .T. ) ;
#61781 = CARTESIAN_POINT ( 'NONE',  ( 5.000000000000000000, -8.500000000000000000, -6.123233995736766282E-16 ) ) ;
#61782 = CARTESIAN_POINT ( 'NONE',  ( 4.458734124999998549, -77.72916666530106511, -2.574251347313721627 ) ) ;
#61783 =( BOUNDED_CURVE ( )  B_SPLINE_CURVE ( 2, ( #19231, #33403, #57239, #33716, #53018, #8959, #28569, #48190, #53650 ),
 .UNSPECIFIED., .F., .F. ) 
 B_SPLINE_CURVE_WITH_KNOTS ( ( 3, 2, 2, 2, 3 ),
 ( 0.3267857142857142905, 0.3273809523809523836, 0.3285714285714285698, 0.3297619047619047561, 0.3303571428571428492 ),
 .UNSPECIFIED. ) 
 CURVE ( )  GEOMETRIC_REPRESENTATION_ITEM ( )  RATIONAL_B_SPLINE_CURVE ( ( 0.9330127018922194093, 0.9330127018922194093, 1.000000000000000000, 0.8660254037844387076, 1.000000000000000000, 0.8660254037844387076, 1.000000000000000000, 0.9330127018922194093, 0.9330127018922194093 ) ) 
 REPRESENTATION_ITEM ( '' )  );
#61784 = FACE_OUTER_BOUND ( 'NONE', #5223, .T. ) ;
#61785 = CARTESIAN_POINT ( 'NONE',  ( -5.000000000000000000, -10.87499999726881583, 0.000000000000000000 ) ) ;
#61787 = ORIENTED_EDGE ( 'NONE', *, *, #56397, .F. ) ;
#61786 = CARTESIAN_POINT ( 'NONE',  ( -2.229367062500000163, -42.47916666530107932, -3.861377020970580443 ) ) ;
#61788 = CARTESIAN_POINT ( 'NONE',  ( 2.071067811865392461, -144.1875000000000284, 5.000000000000084377 ) ) ;
#61790 = VERTEX_POINT ( 'NONE', #45859 ) ;
#61789 = CARTESIAN_POINT ( 'NONE',  ( 4.458734125000001214, 4.854166668032262599, 2.574251347313718519 ) ) ;
#61791 = CYLINDRICAL_SURFACE ( 'NONE', #13503, 5.000000000000000000 ) ;
#61792 = CARTESIAN_POINT ( 'NONE',  ( 1.060575238724906964E-15, -57.75000000000000000, 5.773502691896257311 ) ) ;
#61793 = CARTESIAN_POINT ( 'NONE',  ( 1.846868145590736310, -158.8750000013655779, 4.458734124999999437 ) ) ;
#61794 = CARTESIAN_POINT ( 'NONE',  ( -4.458734124999999437, -34.56249999863440792, 0.000000000000000000 ) ) ;
#61795 = CARTESIAN_POINT ( 'NONE',  ( -5.000000000000000000, -10.87499999726881583, 0.000000000000000000 ) ) ;
#61796 = CARTESIAN_POINT ( 'NONE',  ( 4.458734125000001214, -81.89583333196773651, 2.574251347313718519 ) ) ;
#61797 = CARTESIAN_POINT ( 'NONE',  ( -2.071067811865478170, -167.3125000000000000, 5.000000000000000000 ) ) ;
#61798 = CARTESIAN_POINT ( 'NONE',  ( 4.458734124999999437, -89.81249999863440792, -5.460374474430324690E-16 ) ) ;
#61799 = CARTESIAN_POINT ( 'NONE',  ( -52.10840900171896806, -131.4375000013656063, 3.393966926194110556 ) ) ;
#61800 = CARTESIAN_POINT ( 'NONE',  ( -3.152548672688508926E-16, 0.1875000013655953035, -5.148502694627439702 ) ) ;
#61801 = CARTESIAN_POINT ( 'NONE',  ( -4.458734124999998549, -39.47916666530107932, 2.574251347313722516 ) ) ;
#61802 = CARTESIAN_POINT ( 'NONE',  ( 1.339745962155615144, -70.58034179853028434, 4.999999999999999112 ) ) ;
#61803 = CARTESIAN_POINT ( 'NONE',  ( -2.229367062499996610, -82.39583333196773651, 3.861377020970582219 ) ) ;
#61804 = CARTESIAN_POINT ( 'NONE',  ( -7.500000000000000000, 4.330127018922191873, -7.422398894150032511 ) ) ;
#61805 = ORIENTED_EDGE ( 'NONE', *, *, #33469, .T. ) ;
#61806 = DIRECTION ( 'NONE',  ( -0.000000000000000000, 1.000000000000000000, -0.000000000000000000 ) ) ;
#61808 = AXIS2_PLACEMENT_3D ( 'NONE', #31668, #28024, #3598 ) ;
#61807 = CARTESIAN_POINT ( 'NONE',  ( 5.000000000000000000, -152.0625000000000284, 2.071067811865478614 ) ) ;
#61809 = CARTESIAN_POINT ( 'NONE',  ( 4.458734125000001214, -70.14583333196773651, 2.574251347313718519 ) ) ;
#61810 = CARTESIAN_POINT ( 'NONE',  ( 2.229367062500001939, -36.97916666530107221, 3.861377020970579999 ) ) ;
#61811 = CARTESIAN_POINT ( 'NONE',  ( -4.458734124999999437, -8.645833331967736513, -2.574251347313719407 ) ) ;
#61812 = EDGE_LOOP ( 'NONE', ( #34299, #17706, #50542, #21908 ) ) ;
#61813 = LINE ( 'NONE', #32206, #20480 ) ;
#61814 = EDGE_CURVE ( 'NONE', #45642, #26112, #56245, .T. ) ;
#61815 = EDGE_CURVE ( 'NONE', #60408, #21932, #23364, .T. ) ;
#61816 = CARTESIAN_POINT ( 'NONE',  ( 1.339745962155615144, 17.29465819873852084, 4.999999999999999112 ) ) ;
#61817 = CARTESIAN_POINT ( 'NONE',  ( 9.457646018065525792E-16, -4.312499998634408804, 5.148502694627439702 ) ) ;
#61818 = EDGE_CURVE ( 'NONE', #15531, #18022, #58666, .T. ) ;
#61819 = CARTESIAN_POINT ( 'NONE',  ( -50.18089887299978358, -148.8125000027311842, 2.462841084822545934 ) ) ;
#61820 = CARTESIAN_POINT ( 'NONE',  ( 2.229367062500001939, 4.020833334698926009, 3.861377020970579999 ) ) ;
#61821 = CARTESIAN_POINT ( 'NONE',  ( 1.339745962155615144, -30.58034179853029499, 4.999999999999999112 ) ) ;
#61822 = CARTESIAN_POINT ( 'NONE',  ( 4.458734124999999437, -157.4375000013655779, 0.000000000000000000 ) ) ;
#61823 = EDGE_CURVE ( 'NONE', #37557, #8687, #32372, .T. ) ;
#61824 = CARTESIAN_POINT ( 'NONE',  ( 4.458734124999998549, 26.02083333469892779, -2.574251347313721627 ) ) ;
#61825 = ORIENTED_EDGE ( 'NONE', *, *, #35378, .T. ) ;
#61826 = CARTESIAN_POINT ( 'NONE',  ( -2.229367062500000163, -87.47916666530107932, -3.861377020970580443 ) ) ;
#61827 = CARTESIAN_POINT ( 'NONE',  ( -2.500000000000000444, -25.16666666666666430, -4.330127018922193649 ) ) ;
#61828 = CARTESIAN_POINT ( 'NONE',  ( 4.458734124999999437, -10.81249999863440792, -5.460374474430324690E-16 ) ) ;
#61829 = EDGE_CURVE ( 'NONE', #5205, #39251, #42619, .T. ) ;
#61831 = ADVANCED_FACE ( 'NONE', ( #36855 ), #28455, .T. ) ;
#61830 = CARTESIAN_POINT ( 'NONE',  ( 0.000000000000000000, -170.0000000000000000, 5.000000000000000000 ) ) ;
#61832 = CARTESIAN_POINT ( 'NONE',  ( 5.000000000000000000, -23.37499999726881228, -6.123233995736766282E-16 ) ) ;
#61833 = CARTESIAN_POINT ( 'NONE',  ( 1.339745962155615144, -67.70534180126149693, 4.999999999999999112 ) ) ;
#61834 = CARTESIAN_POINT ( 'NONE',  ( -3.535250795749689387E-16, -36.12499999726880873, -5.773502691896257311 ) ) ;
#61835 = CARTESIAN_POINT ( 'NONE',  ( 5.000000000000000888, -78.58333333333334281, 2.886751345948126879 ) ) ;
#61836 = CARTESIAN_POINT ( 'NONE',  ( -2.229367062500000163, 23.52083333469892779, -3.861377020970580443 ) ) ;
#61837 = CARTESIAN_POINT ( 'NONE',  ( 1.339745962155615144, -10.70534180126147916, 4.999999999999999112 ) ) ;
#61838 = CARTESIAN_POINT ( 'NONE',  ( 2.229367062500001939, 24.02083333469892779, 3.861377020970579999 ) ) ;
#61839 = EDGE_CURVE ( 'NONE', #21770, #60996, #16406, .T. ) ;
#61840 = CARTESIAN_POINT ( 'NONE',  ( -2.229367062500000163, -55.47916666530107221, -3.861377020970580443 ) ) ;
#61841 = CARTESIAN_POINT ( 'NONE',  ( -4.458734124999999437, -4.562499998634401699, 0.000000000000000000 ) ) ;
#61842 = CARTESIAN_POINT ( 'NONE',  ( -5.007715329123872641E-16, -8.660254037844399733, -10.00000000000000000 ) ) ;
#61843 = CARTESIAN_POINT ( 'NONE',  ( -5.000000000000000000, 15.00000000000000000, 0.000000000000000000 ) ) ;
#61844 = EDGE_CURVE ( 'NONE', #30447, #56964, #16782, .T. ) ;
#61845 = CARTESIAN_POINT ( 'NONE',  ( 5.000000000000000000, -141.1250000027312126, 0.000000000000000000 ) ) ;
#61846 = CARTESIAN_POINT ( 'NONE',  ( -5.000000000000000000, -52.08333333333332860, -2.886751345948128211 ) ) ;
#61847 = CARTESIAN_POINT ( 'NONE',  ( 2.229367062500001939, -47.97916666530106511, 3.861377020970579999 ) ) ;
#61848 = CARTESIAN_POINT ( 'NONE',  ( -2.500000000000000444, -85.04166666393547303, -4.330127018922193649 ) ) ;
#61849 = CARTESIAN_POINT ( 'NONE',  ( -57.89159099828107458, -137.9375000013656063, -3.393966926194107447 ) ) ;
#61850 = CARTESIAN_POINT ( 'NONE',  ( 4.174999999999999822, 0.000000000000000000, -0.5776712190230133270 ) ) ;
#61851 = ADVANCED_FACE ( 'NONE', ( #52596 ), #8530, .T. ) ;
#61852 = CARTESIAN_POINT ( 'NONE',  ( -2.500000000000000444, -88.16666666666665719, -4.330127018922193649 ) ) ;
#61853 = CARTESIAN_POINT ( 'NONE',  ( 4.458734124999999437, -88.06249999863439371, -5.460374474430324690E-16 ) ) ;
#61854 = CARTESIAN_POINT ( 'NONE',  ( 1.846868145590735200, -159.5000000013656063, -4.458734124999999437 ) ) ;
#61855 = CARTESIAN_POINT ( 'NONE',  ( -5.000000000000000000, -33.00000000000000000, 0.000000000000000000 ) ) ;
#61856 =( NAMED_UNIT ( * ) PLANE_ANGLE_UNIT ( ) SI_UNIT ( $, .RADIAN. ) );
#61857 = ORIENTED_EDGE ( 'NONE', *, *, #40609, .F. ) ;
#61858 = CARTESIAN_POINT ( 'NONE',  ( 4.458734124999998549, 19.02083333469892779, -2.574251347313721627 ) ) ;
#61859 = ORIENTED_EDGE ( 'NONE', *, *, #33768, .T. ) ;
#61860 = CARTESIAN_POINT ( 'NONE',  ( 4.458734124999998549, -95.72916666530109353, -2.574251347313721627 ) ) ;
#61861 = CARTESIAN_POINT ( 'NONE',  ( 4.458734125000001214, 13.85416666803226171, 2.574251347313718519 ) ) ;
#61862 = CARTESIAN_POINT ( 'NONE',  ( 2.499999999999998668, 18.79166666939785202, -4.330127018922193649 ) ) ;
#61863 =( BOUNDED_CURVE ( )  B_SPLINE_CURVE ( 2, ( #21884, #60810, #16736, #48208, #29209, #19249, #18633, #57876, #4162 ),
 .UNSPECIFIED., .F., .F. ) 
 B_SPLINE_CURVE_WITH_KNOTS ( ( 3, 2, 2, 2, 3 ),
 ( 0.7437500000000000222, 0.7444444444444444642, 0.7458333333333333481, 0.7472222222222222321, 0.7479166666666666741 ),
 .UNSPECIFIED. ) 
 CURVE ( )  GEOMETRIC_REPRESENTATION_ITEM ( )  RATIONAL_B_SPLINE_CURVE ( ( 0.9330127018922194093, 0.9330127018922194093, 1.000000000000000000, 0.8660254037844387076, 1.000000000000000000, 0.8660254037844387076, 1.000000000000000000, 0.9330127018922194093, 0.9330127018922194093 ) ) 
 REPRESENTATION_ITEM ( '' )  );
#61864 = CARTESIAN_POINT ( 'NONE',  ( 0.000000000000000000, -120.0000000000000000, 5.000000000000000000 ) ) ;
#61865 = CARTESIAN_POINT ( 'NONE',  ( 2.499999999999998668, 5.666666666666666963, -4.330127018922193649 ) ) ;
#61866 = CARTESIAN_POINT ( 'NONE',  ( -4.458734124999997661, -54.22916666530107221, 2.574251347313722516 ) ) ;
#61867 = CARTESIAN_POINT ( 'NONE',  ( -6.972266317189433020E-16, -35.12499999726880873, -5.000000000000000000 ) ) ;
#61868 = CARTESIAN_POINT ( 'NONE',  ( 5.000000000000000888, -82.58333333333332860, 2.886751345948126879 ) ) ;
#61869 = CARTESIAN_POINT ( 'NONE',  ( 1.975475456537005874E-15, -75.62499999726880162, 5.000000000000000000 ) ) ;
#61870 = CARTESIAN_POINT ( 'NONE',  ( 2.499999999999998668, 7.791666669397852019, -4.330127018922193649 ) ) ;
#61871 = CARTESIAN_POINT ( 'NONE',  ( 1.975475456537005874E-15, -25.62499999726881228, 5.000000000000000000 ) ) ;
#61872 = CARTESIAN_POINT ( 'NONE',  ( -5.000000000000000000, -24.95833333060214443, -2.886751345948128211 ) ) ;
#61873 = CARTESIAN_POINT ( 'NONE',  ( 2.499999999999998668, -40.33333333333332860, -4.330127018922193649 ) ) ;
#61875 = CARTESIAN_POINT ( 'NONE',  ( 4.458734124999998549, -18.97916666530107221, -2.574251347313721627 ) ) ;
#61874 = CARTESIAN_POINT ( 'NONE',  ( 6.123233995736766282E-16, -120.0000000000000000, -5.000000000000000000 ) ) ;
#61876 = DIRECTION ( 'NONE',  ( -0.000000000000000000, 1.000000000000000000, -0.000000000000000000 ) ) ;
#61877 = CARTESIAN_POINT ( 'NONE',  ( -2.229367062499996610, -65.14583333196773651, 3.861377020970582219 ) ) ;
#61878 = CARTESIAN_POINT ( 'NONE',  ( 4.458734124999999437, -148.7500000013656063, 1.846868145590737864 ) ) ;
#61879 = CARTESIAN_POINT ( 'NONE',  ( 2.229367062499998831, -70.64583333196773651, -3.861377020970580887 ) ) ;
#61880 = CARTESIAN_POINT ( 'NONE',  ( -52.80376928212989185, -142.1250000013656063, -4.297418129356379346 ) ) ;
#61881 = CARTESIAN_POINT ( 'NONE',  ( -4.458734124999999437, -22.56249999863440436, 0.000000000000000000 ) ) ;
#61882 = CARTESIAN_POINT ( 'NONE',  ( 5.000000000000000000, -59.37499999726880873, -6.123233995736766282E-16 ) ) ;
#61883 = ORIENTED_EDGE ( 'NONE', *, *, #27518, .T. ) ;
#61884 = CARTESIAN_POINT ( 'NONE',  ( -6.972266317189433020E-16, -31.12499999726880873, -5.000000000000000000 ) ) ;
#61885 = ORIENTED_EDGE ( 'NONE', *, *, #2070, .F. ) ;
#61886 = CARTESIAN_POINT ( 'NONE',  ( 2.229367062500001939, -69.22916666530107932, 3.861377020970579999 ) ) ;
#61887 = FACE_OUTER_BOUND ( 'NONE', #32933, .T. ) ;
#61888 = ORIENTED_EDGE ( 'NONE', *, *, #59045, .T. ) ;
#61889 =( BOUNDED_CURVE ( )  B_SPLINE_CURVE ( 2, ( #38531, #13782, #33095, #27633, #52411, #52710, #42730, #17972, #62375 ),
 .UNSPECIFIED., .F., .F. ) 
 B_SPLINE_CURVE_WITH_KNOTS ( ( 3, 2, 2, 2, 3 ),
 ( 0.8375000000000000222, 0.8380952380952381153, 0.8392857142857143016, 0.8404761904761904878, 0.8410714285714285809 ),
 .UNSPECIFIED. ) 
 CURVE ( )  GEOMETRIC_REPRESENTATION_ITEM ( )  RATIONAL_B_SPLINE_CURVE ( ( 0.9330127018922194093, 0.9330127018922194093, 1.000000000000000000, 0.8660254037844387076, 1.000000000000000000, 0.8660254037844387076, 1.000000000000000000, 0.9330127018922194093, 0.9330127018922194093 ) ) 
 REPRESENTATION_ITEM ( '' )  );
#61890 = CARTESIAN_POINT ( 'NONE',  ( -5.147856630858197489E-14, 3.375000002731183280, 5.000000000000000000 ) ) ;
#61891 = PLANE ( 'NONE',  #16955 ) ;
#61892 = CARTESIAN_POINT ( 'NONE',  ( -6.972266317189433020E-16, -39.12499999726880162, -5.000000000000000000 ) ) ;
#61893 = CARTESIAN_POINT ( 'NONE',  ( 9.457646018065525792E-16, -54.31249999863440081, 5.148502694627439702 ) ) ;
#61894 = ORIENTED_EDGE ( 'NONE', *, *, #55869, .T. ) ;
#61895 = CARTESIAN_POINT ( 'NONE',  ( 2.452879891156805492, 7.244083172395185954, -0.1007566405101774504 ) ) ;
#61896 = CARTESIAN_POINT ( 'NONE',  ( 9.457646018065525792E-16, 10.93750000136559208, 5.148502694627439702 ) ) ;
#61897 = CARTESIAN_POINT ( 'NONE',  ( 2.229367062500001939, 19.02083333469892779, 3.861377020970579999 ) ) ;
#61898 = CARTESIAN_POINT ( 'NONE',  ( -53.51423613279429503, -150.2500000013656063, 4.591703134518082763 ) ) ;
#61899 = CARTESIAN_POINT ( 'NONE',  ( 5.000000000000000888, -78.45833333060214443, 2.886751345948126879 ) ) ;
#61900 = CARTESIAN_POINT ( 'NONE',  ( -3.152801135295367096, -169.0625000013656063, -3.152801135295367541 ) ) ;
#61901 = ORIENTED_EDGE ( 'NONE', *, *, #6876, .T. ) ;
#61902 = CARTESIAN_POINT ( 'NONE',  ( -2.229367062499996610, -70.14583333196773651, 3.861377020970582219 ) ) ;
#61903 = CARTESIAN_POINT ( 'NONE',  ( -5.000000000000000000, -40.08333333333332860, -2.886751345948128211 ) ) ;
#61904 = CARTESIAN_POINT ( 'NONE',  ( -4.458734124999999437, 7.687500001365594748, 0.000000000000000000 ) ) ;
#61905 = CARTESIAN_POINT ( 'NONE',  ( 6.123233995736766282E-16, -120.0000000000000000, -5.000000000000000000 ) ) ;
#61906 = CARTESIAN_POINT ( 'NONE',  ( -2.229367062500000163, -61.72916666530106511, -3.861377020970580443 ) ) ;
#61907 = CARTESIAN_POINT ( 'NONE',  ( -2.500000000000000444, -21.04166666393548013, -4.330127018922193649 ) ) ;
#61908 = CARTESIAN_POINT ( 'NONE',  ( 1.243387493232115550E-13, -19.25000000000000000, -5.000000000000000000 ) ) ;
#61909 = CARTESIAN_POINT ( 'NONE',  ( -1.211595439868048629, 7.960739084487649109, -0.4504974108211966533 ) ) ;
#61910 = CARTESIAN_POINT ( 'NONE',  ( 2.499999999999998668, 19.79166666939785202, -4.330127018922193649 ) ) ;
#61911 = CARTESIAN_POINT ( 'NONE',  ( -4.999999999999998224, 19.08333333333333570, 2.886751345948131764 ) ) ;
#61912 = CARTESIAN_POINT ( 'NONE',  ( 2.229367062500001939, -42.97916666530107932, 3.861377020970579999 ) ) ;
#61913 = CARTESIAN_POINT ( 'NONE',  ( 9.457646018065525792E-16, -24.31249999863440436, 5.148502694627439702 ) ) ;
#61914 = ORIENTED_EDGE ( 'NONE', *, *, #42909, .T. ) ;
#61915 = CARTESIAN_POINT ( 'NONE',  ( -6.972266317189433020E-16, 19.87500000273118417, -5.000000000000000000 ) ) ;
#61916 = CARTESIAN_POINT ( 'NONE',  ( -4.458734124999998549, -107.2291666653010509, 2.574251347313722516 ) ) ;
#61917 = CARTESIAN_POINT ( 'NONE',  ( 2.071067811865475505, -152.9375000027312126, -5.000000000000000888 ) ) ;
#61918 = ORIENTED_EDGE ( 'NONE', *, *, #58198, .F. ) ;
#61919 = CARTESIAN_POINT ( 'NONE',  ( 2.229367062500001939, -109.2291666653010651, 3.861377020970579999 ) ) ;
#61920 = CARTESIAN_POINT ( 'NONE',  ( -2.229367062500000163, -32.47916666530106511, -3.861377020970580443 ) ) ;
#61921 = CARTESIAN_POINT ( 'NONE',  ( 1.060575238724906964E-15, -67.62499999726881583, 5.773502691896257311 ) ) ;
#61922 = CARTESIAN_POINT ( 'NONE',  ( -57.19623071787017210, -150.6250000013656063, 4.297418129356382899 ) ) ;
#61923 = CARTESIAN_POINT ( 'NONE',  ( -9.184850993605147944E-16, -148.2500000000000284, 5.000000000000000000 ) ) ;
#61924 = EDGE_CURVE ( 'NONE', #8918, #2572, #55860, .T. ) ;
#61925 = CARTESIAN_POINT ( 'NONE',  ( -4.458734124999999437, -29.39583333196773296, -2.574251347313719407 ) ) ;
#61926 = CARTESIAN_POINT ( 'NONE',  ( -4.458734124999999437, -69.64583333196773651, -2.574251347313719407 ) ) ;
#61927 = CARTESIAN_POINT ( 'NONE',  ( -3.152801135295367096, -169.3125000013656063, -3.152801135295367541 ) ) ;
#61928 = CARTESIAN_POINT ( 'NONE',  ( -2.229367062500000163, -24.47916666530106866, -3.861377020970580443 ) ) ;
#61929 = CARTESIAN_POINT ( 'NONE',  ( -5.000000000000000000, -33.08333333333332860, -2.886751345948128211 ) ) ;
#61930 = CARTESIAN_POINT ( 'NONE',  ( -6.972266317189433020E-16, -5.124999997268812280, -5.000000000000000000 ) ) ;
#61931 = CARTESIAN_POINT ( 'NONE',  ( -2.500000000000000444, -19.16666666666666430, -4.330127018922193649 ) ) ;
#61932 = CARTESIAN_POINT ( 'NONE',  ( -8.190561711645485556E-16, -149.6875000013656063, 4.458734124999999437 ) ) ;
#61933 = VERTEX_POINT ( 'NONE', #13667 ) ;
#61934 = LINE ( 'NONE', #38110, #17356 ) ;
#61935 = CARTESIAN_POINT ( 'NONE',  ( -4.458734124999999437, -52.56249999863440792, 0.000000000000000000 ) ) ;
#61936 = CARTESIAN_POINT ( 'NONE',  ( 1.339745962155615144, -84.58034179853028434, 4.999999999999999112 ) ) ;
#61937 = DIRECTION ( 'NONE',  ( 0.000000000000000000, 0.000000000000000000, 1.000000000000000000 ) ) ;
#61938 = CARTESIAN_POINT ( 'NONE',  ( 5.000000000000000888, 26.41666666666666430, 2.886751345948126879 ) ) ;
#61939 = CYLINDRICAL_SURFACE ( 'NONE', #6813, 5.000000000000000000 ) ;
#61940 = CARTESIAN_POINT ( 'NONE',  ( 2.229367062500001939, -0.9791666653010712151, 3.861377020970579999 ) ) ;
#61941 = CARTESIAN_POINT ( 'NONE',  ( 1.339745962155614700, 28.70534180126147561, -4.999999999999999112 ) ) ;
#61942 = CARTESIAN_POINT ( 'NONE',  ( 1.975475456537005874E-15, -14.74999999999999822, 5.000000000000000000 ) ) ;
#61943 = CARTESIAN_POINT ( 'NONE',  ( 2.500000000000002220, -87.54166666393547303, 4.330127018922192761 ) ) ;
#61944 = CARTESIAN_POINT ( 'NONE',  ( 2.229367062499998831, 11.10416666803225993, -3.861377020970580887 ) ) ;
#61945 = ORIENTED_EDGE ( 'NONE', *, *, #57883, .F. ) ;
#61946 = DIRECTION ( 'NONE',  ( -0.000000000000000000, 1.000000000000000000, -0.000000000000000000 ) ) ;
#61947 = ORIENTED_EDGE ( 'NONE', *, *, #29034, .F. ) ;
#61948 = CARTESIAN_POINT ( 'NONE',  ( 75.00000000000002842, 0.000000000000000000, 5.000000000000000000 ) ) ;
#61949 = CARTESIAN_POINT ( 'NONE',  ( 9.457646018065525792E-16, -47.06249999863440792, 5.148502694627439702 ) ) ;
#61950 = CARTESIAN_POINT ( 'NONE',  ( 3.152801135295367541, -158.5625000013656063, -3.152801135295367541 ) ) ;
#61951 = CARTESIAN_POINT ( 'NONE',  ( 5.000000000000000888, -46.45833333060214443, 2.886751345948126879 ) ) ;
#61952 = EDGE_LOOP ( 'NONE', ( #30629, #13, #32353, #7530 ) ) ;
#61953 = CARTESIAN_POINT ( 'NONE',  ( 4.458734124999999437, -25.81249999863440792, -5.460374474430324690E-16 ) ) ;
#61954 = ORIENTED_EDGE ( 'NONE', *, *, #34737, .F. ) ;
#61955 = CARTESIAN_POINT ( 'NONE',  ( 3.061616997868383141E-16, -169.7500000000000000, -5.000000000000000000 ) ) ;
#61956 = CARTESIAN_POINT ( 'NONE',  ( 4.458734124999999437, -165.5000000013655779, 1.846868145590737864 ) ) ;
#61957 = DIRECTION ( 'NONE',  ( 0.000000000000000000, 0.000000000000000000, 1.000000000000000000 ) ) ;
#61958 = CARTESIAN_POINT ( 'NONE',  ( -50.01589407740564042, -138.6250000000000284, 0.3983568153799778022 ) ) ;
#61959 = CARTESIAN_POINT ( 'NONE',  ( -4.458734124999999437, -35.64583333196772941, -2.574251347313719407 ) ) ;
#61960 = CARTESIAN_POINT ( 'NONE',  ( -2.499999999999996447, 20.29166666939784847, 4.330127018922195425 ) ) ;
#61961 = EDGE_LOOP ( 'NONE', ( #17440, #17325, #32022, #14661, #57371, #13300, #30594, #7954, #19188, #53558, #24247, #10109, #33143, #43466, #14808, #40715, #52897 ) ) ;
#61962 =( BOUNDED_CURVE ( )  B_SPLINE_CURVE ( 2, ( #8038, #22196, #37610, #56929, #42427, #23136, #46634, #56292, #47271 ),
 .UNSPECIFIED., .F., .F. ) 
 B_SPLINE_CURVE_WITH_KNOTS ( ( 3, 2, 2, 2, 3 ),
 ( 0.3895833333333333370, 0.3902777777777777790, 0.3916666666666666630, 0.3930555555555555469, 0.3937499999999999889 ),
 .UNSPECIFIED. ) 
 CURVE ( )  GEOMETRIC_REPRESENTATION_ITEM ( )  RATIONAL_B_SPLINE_CURVE ( ( 0.9330127018922194093, 0.9330127018922194093, 1.000000000000000000, 0.8660254037844387076, 1.000000000000000000, 0.8660254037844387076, 1.000000000000000000, 0.9330127018922194093, 0.9330127018922194093 ) ) 
 REPRESENTATION_ITEM ( '' )  );
#61963 = CARTESIAN_POINT ( 'NONE',  ( 4.458734124999998549, -82.72916666530106511, -2.574251347313721627 ) ) ;
#61964 = CARTESIAN_POINT ( 'NONE',  ( 2.229367062500001939, 27.02083333469892423, 3.861377020970579999 ) ) ;
#61965 = CARTESIAN_POINT ( 'NONE',  ( 1.975475456537005874E-15, -17.62499999726881938, 5.000000000000000000 ) ) ;
#61966 = ORIENTED_EDGE ( 'NONE', *, *, #39709, .F. ) ;
#61967 = CARTESIAN_POINT ( 'NONE',  ( -5.000000000000000000, -22.87499999726881228, 0.000000000000000000 ) ) ;
#61968 = CARTESIAN_POINT ( 'NONE',  ( -59.44456063193725015, -138.8125000013656063, -0.3552334253322034230 ) ) ;
#61969 = CARTESIAN_POINT ( 'NONE',  ( -2.229367062500000163, -83.72916666530106511, -3.861377020970580443 ) ) ;
#61970 = CARTESIAN_POINT ( 'NONE',  ( -57.46284108482265651, -132.0625000027312126, 4.819101127000239515 ) ) ;
#61971 = DIRECTION ( 'NONE',  ( -0.000000000000000000, 1.000000000000000000, -0.000000000000000000 ) ) ;
#61972 = DIRECTION ( 'NONE',  ( -0.000000000000000000, 1.000000000000000000, -0.000000000000000000 ) ) ;
#61973 = CARTESIAN_POINT ( 'NONE',  ( -6.972266317189433020E-16, -47.12499999726880873, -5.000000000000000000 ) ) ;
#61974 = CARTESIAN_POINT ( 'NONE',  ( -3.152548672688508926E-16, -53.56249999863439371, -5.148502694627439702 ) ) ;
#61975 = CARTESIAN_POINT ( 'NONE',  ( -4.458734124999998549, 20.77083333469892779, 2.574251347313722516 ) ) ;
#61976 = CARTESIAN_POINT ( 'NONE',  ( -2.499999999999996447, -104.8333333333333286, 4.330127018922195425 ) ) ;
#61977 =( BOUNDED_CURVE ( )  B_SPLINE_CURVE ( 2, ( #22512, #2574, #3211, #22190, #61435, #42421, #51774, #56611, #2899 ),
 .UNSPECIFIED., .F., .F. ) 
 B_SPLINE_CURVE_WITH_KNOTS ( ( 3, 2, 2, 2, 3 ),
 ( 0.6517857142857143016, 0.6523809523809523947, 0.6535714285714285809, 0.6547619047619047672, 0.6553571428571428603 ),
 .UNSPECIFIED. ) 
 CURVE ( )  GEOMETRIC_REPRESENTATION_ITEM ( )  RATIONAL_B_SPLINE_CURVE ( ( 0.9330127018922194093, 0.9330127018922194093, 1.000000000000000000, 0.8660254037844387076, 1.000000000000000000, 0.8660254037844387076, 1.000000000000000000, 0.9330127018922194093, 0.9330127018922194093 ) ) 
 REPRESENTATION_ITEM ( '' )  );
#61978 = CARTESIAN_POINT ( 'NONE',  ( 2.500000000000002220, -3.666666666666665186, 4.330127018922192761 ) ) ;
#61979 = CARTESIAN_POINT ( 'NONE',  ( 4.458734124999998549, -41.97916666530107932, -2.574251347313721627 ) ) ;
#61980 = CARTESIAN_POINT ( 'NONE',  ( -2.499999999999996447, -4.708333330602147981, 4.330127018922195425 ) ) ;
#61981 = CARTESIAN_POINT ( 'NONE',  ( -3.535533905932738641, -153.5000000027312126, 3.535533905932737309 ) ) ;
#61982 = CYLINDRICAL_SURFACE ( 'NONE', #58369, 5.000000000000000000 ) ;
#61983 = CARTESIAN_POINT ( 'NONE',  ( -3.152548672688508926E-16, -84.81249999863439371, -5.148502694627439702 ) ) ;
#61984 = CARTESIAN_POINT ( 'NONE',  ( 9.457646018065525792E-16, -104.0624999986344079, 5.148502694627439702 ) ) ;
#61985 = CARTESIAN_POINT ( 'NONE',  ( -3.152548672688508926E-16, -4.812499998634402587, -5.148502694627439702 ) ) ;
#61986 = VERTEX_POINT ( 'NONE', #48071 ) ;
#61987 = CARTESIAN_POINT ( 'NONE',  ( 1.975475456537005874E-15, -73.75000000000000000, 5.000000000000000000 ) ) ;
#61988 = CARTESIAN_POINT ( 'NONE',  ( 4.458734125000001214, -94.89583333196773651, 2.574251347313718519 ) ) ;
#61989 = CARTESIAN_POINT ( 'NONE',  ( 5.000000000000000888, -165.0625000027312126, -2.071067811865475505 ) ) ;
#61991 = VECTOR ( 'NONE', #26704, 1000.000000000000000 ) ;
#61990 = CARTESIAN_POINT ( 'NONE',  ( -4.458734124999999437, -93.64583333196773651, -2.574251347313719407 ) ) ;
#61992 = CARTESIAN_POINT ( 'NONE',  ( 2.229367062500001939, 14.77083333469892779, 3.861377020970579999 ) ) ;
#61993 = DIRECTION ( 'NONE',  ( -0.000000000000000000, 1.000000000000000000, -0.000000000000000000 ) ) ;
#61994 = CARTESIAN_POINT ( 'NONE',  ( -53.51423613279429503, -132.2500000013656063, 4.591703134518082763 ) ) ;
#61995 = CARTESIAN_POINT ( 'NONE',  ( -4.458734124999999437, -11.39583333196774007, -2.574251347313719407 ) ) ;
#61996 = CARTESIAN_POINT ( 'NONE',  ( -4.458734124999999437, 14.43750000136559386, 0.000000000000000000 ) ) ;
#61997 = CARTESIAN_POINT ( 'NONE',  ( -4.458734124999999437, -52.64583333196773651, -2.574251347313719407 ) ) ;
#61998 = CARTESIAN_POINT ( 'NONE',  ( 0.000000000000000000, -120.0000000000000000, 0.000000000000000000 ) ) ;
#61999 = CARTESIAN_POINT ( 'NONE',  ( -6.972266317189433020E-16, -22.12499999726881228, -5.000000000000000000 ) ) ;
#62000 = CARTESIAN_POINT ( 'NONE',  ( -4.458734124999999437, -7.312499998634404363, 0.000000000000000000 ) ) ;
#62001 = CARTESIAN_POINT ( 'NONE',  ( 1.975475456537005874E-15, -30.74999999999999645, 5.000000000000000000 ) ) ;
#62002 = ORIENTED_EDGE ( 'NONE', *, *, #9441, .F. ) ;
#62003 = CARTESIAN_POINT ( 'NONE',  ( -2.229367062500000163, -36.72916666530107221, -3.861377020970580443 ) ) ;
#62004 = CARTESIAN_POINT ( 'NONE',  ( -59.44456063193725015, -129.8125000013656063, -0.3552334253322034230 ) ) ;
#62005 = CARTESIAN_POINT ( 'NONE',  ( 1.975475456537005874E-15, -100.7499999999999858, 5.000000000000000000 ) ) ;
#62006 = CARTESIAN_POINT ( 'NONE',  ( -2.229367062500000163, -77.47916666530106511, -3.861377020970580443 ) ) ;
#62007 = CARTESIAN_POINT ( 'NONE',  ( 4.458734124999999437, 25.93750000136559564, -5.460374474430324690E-16 ) ) ;
#62008 = AXIS2_PLACEMENT_3D ( 'NONE', #51761, #26681, #17665 ) ;
#62009 = CARTESIAN_POINT ( 'NONE',  ( 2.229367062499998831, 15.35416666803225993, -3.861377020970580887 ) ) ;
#62010 = DIRECTION ( 'NONE',  ( -0.000000000000000000, -0.000000000000000000, -1.000000000000000000 ) ) ;
#62011 = CARTESIAN_POINT ( 'NONE',  ( 2.229367062500001939, -81.22916666530106511, 3.861377020970579999 ) ) ;
#62012 = CARTESIAN_POINT ( 'NONE',  ( -4.999999999999999112, -71.91666666666667140, 2.886751345948131764 ) ) ;
#62013 = DIRECTION ( 'NONE',  ( 0.000000000000000000, 0.000000000000000000, 1.000000000000000000 ) ) ;
#62014 = CARTESIAN_POINT ( 'NONE',  ( 2.500000000000002220, 16.45833333606451987, 4.330127018922192761 ) ) ;
#62015 = ORIENTED_EDGE ( 'NONE', *, *, #19513, .F. ) ;
#62016 = CARTESIAN_POINT ( 'NONE',  ( 2.071067811865349828, -147.3125000027311842, 5.000000000000126121 ) ) ;
#62017 = LINE ( 'NONE', #32418, #44234 ) ;
#62019 = CARTESIAN_POINT ( 'NONE',  ( -2.500000000000000444, -28.16666666666666785, -4.330127018922193649 ) ) ;
#62018 = CARTESIAN_POINT ( 'NONE',  ( -5.000000000000000000, -72.08333333333332860, -2.886751345948128211 ) ) ;
#62020 = CARTESIAN_POINT ( 'NONE',  ( -4.458734124999999437, -32.39583333196773651, -2.574251347313719407 ) ) ;
#62021 = EDGE_CURVE ( 'NONE', #19898, #16398, #22384, .T. ) ;
#62022 = CARTESIAN_POINT ( 'NONE',  ( -5.000000000000000000, 4.916666666666666075, -2.886751345948128211 ) ) ;
#62023 = CARTESIAN_POINT ( 'NONE',  ( -4.999999999999999112, -26.79166666393548013, 2.886751345948131764 ) ) ;
#62025 = ORIENTED_EDGE ( 'NONE', *, *, #29916, .T. ) ;
#62024 = CARTESIAN_POINT ( 'NONE',  ( -4.458734124999998549, -59.22916666530106511, 2.574251347313722516 ) ) ;
#62026 = CARTESIAN_POINT ( 'NONE',  ( -51.60603307380591787, -154.1875000013656063, -2.891590998281053704 ) ) ;
#62028 = VERTEX_POINT ( 'NONE', #52906 ) ;
#62027 = CARTESIAN_POINT ( 'NONE',  ( 9.457646018065525792E-16, -11.31249999863440792, 5.148502694627439702 ) ) ;
#62029 = CARTESIAN_POINT ( 'NONE',  ( 5.000000000000000000, -79.50000000000000000, -6.123233995736766282E-16 ) ) ;
#62030 = CARTESIAN_POINT ( 'NONE',  ( -50.55543936806279248, -139.0625000013656063, 0.3552334253322060320 ) ) ;
#62031 = CARTESIAN_POINT ( 'NONE',  ( 4.458734125000001214, -50.14583333196773651, 2.574251347313718519 ) ) ;
#62032 =( BOUNDED_CURVE ( )  B_SPLINE_CURVE ( 2, ( #45939, #35029, #25693, #45303, #11835, #21509, #5429, #25046, #618 ),
 .UNSPECIFIED., .F., .F. ) 
 B_SPLINE_CURVE_WITH_KNOTS ( ( 3, 2, 2, 2, 3 ),
 ( 0.4660714285714285809, 0.4666666666666666741, 0.4678571428571428603, 0.4690476190476190466, 0.4696428571428571397 ),
 .UNSPECIFIED. ) 
 CURVE ( )  GEOMETRIC_REPRESENTATION_ITEM ( )  RATIONAL_B_SPLINE_CURVE ( ( 0.9330127018922194093, 0.9330127018922194093, 1.000000000000000000, 0.8660254037844387076, 1.000000000000000000, 0.8660254037844387076, 1.000000000000000000, 0.9330127018922194093, 0.9330127018922194093 ) ) 
 REPRESENTATION_ITEM ( '' )  );
#62033 = CARTESIAN_POINT ( 'NONE',  ( 2.500000000000002220, -79.54166666393547303, 4.330127018922192761 ) ) ;
#62035 = VERTEX_POINT ( 'NONE', #37177 ) ;
#62034 = CARTESIAN_POINT ( 'NONE',  ( 2.499999999999998668, -65.20833333060213022, -4.330127018922193649 ) ) ;
#62036 = CARTESIAN_POINT ( 'NONE',  ( -49.85088928181150436, -150.5625000000000284, -1.666127454062680702 ) ) ;
#62037 = CARTESIAN_POINT ( 'NONE',  ( -3.152548672688508926E-16, -21.81249999863440436, -5.148502694627439702 ) ) ;
#62039 = ORIENTED_EDGE ( 'NONE', *, *, #46867, .T. ) ;
#62038 = CARTESIAN_POINT ( 'NONE',  ( 9.457646018065525792E-16, -59.31249999863440081, 5.148502694627439702 ) ) ;
#62040 = EDGE_CURVE ( 'NONE', #44900, #10824, #12719, .T. ) ;
#62041 =( NAMED_UNIT ( * ) SI_UNIT ( $, .STERADIAN. ) SOLID_ANGLE_UNIT ( ) );
#62042 = CARTESIAN_POINT ( 'NONE',  ( 1.846868145590736310, -168.8750000013655779, 4.458734124999999437 ) ) ;
#62043 = CARTESIAN_POINT ( 'NONE',  ( -4.458734124999999437, -99.56249999863440792, 0.000000000000000000 ) ) ;
#62044 = CARTESIAN_POINT ( 'NONE',  ( -6.972266317189433020E-16, -8.124999997268814056, -5.000000000000000000 ) ) ;
#62045 = ORIENTED_EDGE ( 'NONE', *, *, #16924, .T. ) ;
#62046 = CARTESIAN_POINT ( 'NONE',  ( -59.44456063193725015, -151.8125000013656063, -0.3552334253322034230 ) ) ;
#62047 = CARTESIAN_POINT ( 'NONE',  ( -51.75738570946856498, -141.8750000027312126, 3.805975901505576964 ) ) ;
#62048 = DIRECTION ( 'NONE',  ( -0.6485228581062915110, 0.000000000000000000, -0.7611951803011149931 ) ) ;
#62049 = CARTESIAN_POINT ( 'NONE',  ( 9.457646018065525792E-16, -6.062499998634403475, 5.148502694627439702 ) ) ;
#62050 = CARTESIAN_POINT ( 'NONE',  ( 2.229367062500001939, -95.22916666530106511, 3.861377020970579999 ) ) ;
#62051 = AXIS2_PLACEMENT_3D ( 'NONE', #31901, #7467, #8100 ) ;
#62052 = CARTESIAN_POINT ( 'NONE',  ( -4.458734125000000326, -150.2500000013656063, -1.846868145590735644 ) ) ;
#62053 = CARTESIAN_POINT ( 'NONE',  ( 4.458734124999998549, -28.97916666530107577, -2.574251347313721627 ) ) ;
#62054 = AXIS2_PLACEMENT_3D ( 'NONE', #29765, #35889, #30086 ) ;
#62055 = CARTESIAN_POINT ( 'NONE',  ( 2.500000000000002220, -46.66666666666666430, 4.330127018922192761 ) ) ;
#62056 = CARTESIAN_POINT ( 'NONE',  ( -50.40829686548195099, -139.0000000013655779, -1.485763867205728284 ) ) ;
#62057 = CARTESIAN_POINT ( 'NONE',  ( 9.457646018065525792E-16, -63.31249999863440081, 5.148502694627439702 ) ) ;
#62058 = CARTESIAN_POINT ( 'NONE',  ( 5.000000000000000000, -43.41666666666666430, -2.886751345948130876 ) ) ;
#62059 = DIRECTION ( 'NONE',  ( 0.000000000000000000, 0.000000000000000000, 1.000000000000000000 ) ) ;
#62060 = CARTESIAN_POINT ( 'NONE',  ( 3.152801135295367541, -144.3125000013655779, -3.152801135295367541 ) ) ;
#62061 = CARTESIAN_POINT ( 'NONE',  ( 2.229367062499998831, 10.10416666803225993, -3.861377020970580887 ) ) ;
#62062 = EDGE_LOOP ( 'NONE', ( #54148, #18512, #23275, #35766 ) ) ;
#62063 = CARTESIAN_POINT ( 'NONE',  ( 1.975475456537005874E-15, 19.25000000000000000, 5.000000000000000000 ) ) ;
#62064 = CARTESIAN_POINT ( 'NONE',  ( 0.000000000000000000, -114.9999999999999858, 0.000000000000000000 ) ) ;
#62066 = CARTESIAN_POINT ( 'NONE',  ( -4.458734124999998549, -23.22916666530107221, 2.574251347313722516 ) ) ;
#62065 = CARTESIAN_POINT ( 'NONE',  ( -2.500000000000000444, -91.16666666666665719, -4.330127018922193649 ) ) ;
#62067 = CARTESIAN_POINT ( 'NONE',  ( 5.000000000000000000, -14.29166666393548013, -2.886751345948130876 ) ) ;
#62068 = CARTESIAN_POINT ( 'NONE',  ( 4.458734124999999437, -71.06249999863439371, -5.460374474430324690E-16 ) ) ;
#62069 = CARTESIAN_POINT ( 'NONE',  ( 0.000000000000000000, -120.0000000000000000, 0.000000000000000000 ) ) ;
#62070 = CARTESIAN_POINT ( 'NONE',  ( 1.339745962155612702, -76.16965819600731891, -5.000000000000000000 ) ) ;
#62071 = CARTESIAN_POINT ( 'NONE',  ( -51.60603307380591787, -144.9375000013656063, -2.891590998281053704 ) ) ;
#62072 = CARTESIAN_POINT ( 'NONE',  ( 4.458734125000000326, 3.104166668032260379, 2.574251347313718519 ) ) ;
#62073 = DIRECTION ( 'NONE',  ( 0.000000000000000000, 0.000000000000000000, 1.000000000000000000 ) ) ;
#62074 = CYLINDRICAL_SURFACE ( 'NONE', #53083, 5.000000000000000000 ) ;
#62075 = CARTESIAN_POINT ( 'NONE',  ( 2.229367062500001939, 5.020833334698926897, 3.861377020970579999 ) ) ;
#62076 = CARTESIAN_POINT ( 'NONE',  ( -4.458734124999999437, -74.39583333196775072, -2.574251347313719407 ) ) ;
#62077 = CARTESIAN_POINT ( 'NONE',  ( -2.229367062500000163, -18.72916666530106866, -3.861377020970580443 ) ) ;
#62078 =( BOUNDED_CURVE ( )  B_SPLINE_CURVE ( 2, ( #45110, #30951, #10699, #50897, #11327, #30307, #60244, #40914, #25488 ),
 .UNSPECIFIED., .F., .F. ) 
 B_SPLINE_CURVE_WITH_KNOTS ( ( 3, 2, 2, 2, 3 ),
 ( 0.7517857142857142794, 0.7523809523809523725, 0.7535714285714285587, 0.7547619047619047450, 0.7553571428571428381 ),
 .UNSPECIFIED. ) 
 CURVE ( )  GEOMETRIC_REPRESENTATION_ITEM ( )  RATIONAL_B_SPLINE_CURVE ( ( 0.9330127018922194093, 0.9330127018922194093, 1.000000000000000000, 0.8660254037844387076, 1.000000000000000000, 0.8660254037844387076, 1.000000000000000000, 0.9330127018922194093, 0.9330127018922194093 ) ) 
 REPRESENTATION_ITEM ( '' )  );
#62079 = CARTESIAN_POINT ( 'NONE',  ( 5.000000000000000000, -7.500000000000000000, -6.123233995736766282E-16 ) ) ;
#62080 = CARTESIAN_POINT ( 'NONE',  ( -3.152801135295367985, -159.8125000013656063, 3.152801135295367096 ) ) ;
#62081 = CARTESIAN_POINT ( 'NONE',  ( -1.127183054612291972E-14, 23.25000000000000000, 4.999999999999999112 ) ) ;
#62082 = CARTESIAN_POINT ( 'NONE',  ( 4.458734125000001214, -61.89583333196773651, 2.574251347313718519 ) ) ;
#62083 = CARTESIAN_POINT ( 'NONE',  ( 2.500000000000002220, -100.5416666639354588, 4.330127018922192761 ) ) ;
#62084 = CARTESIAN_POINT ( 'NONE',  ( 5.000000000000000000, -41.49999999999999289, -6.123233995736766282E-16 ) ) ;
#62085 = CARTESIAN_POINT ( 'NONE',  ( -2.229367062500000163, -42.47916666530107932, -3.861377020970580443 ) ) ;
#62086 = CARTESIAN_POINT ( 'NONE',  ( 4.458734124999999437, -108.0624999986343937, -5.460374474430324690E-16 ) ) ;
#62087 = CARTESIAN_POINT ( 'NONE',  ( 2.229367062499998831, -66.89583333196773651, -3.861377020970580887 ) ) ;
#62088 = CARTESIAN_POINT ( 'NONE',  ( 2.499999999999998668, -48.33333333333332860, -4.330127018922193649 ) ) ;
#62089 = CARTESIAN_POINT ( 'NONE',  ( 1.975475456537005874E-15, -40.74999999999999289, 5.000000000000000000 ) ) ;
#62090 = CARTESIAN_POINT ( 'NONE',  ( 1.339745962155615144, -68.58034179853028434, 4.999999999999999112 ) ) ;
#62091 = VERTEX_POINT ( 'NONE', #61305 ) ;
#62092 = CARTESIAN_POINT ( 'NONE',  ( -2.499999999999996447, 15.29166666939785202, 4.330127018922195425 ) ) ;
#62093 = DIRECTION ( 'NONE',  ( 0.000000000000000000, 0.000000000000000000, -1.000000000000000000 ) ) ;
#62094 = CARTESIAN_POINT ( 'NONE',  ( -2.500000000000000444, -13.16666666666666607, -4.330127018922193649 ) ) ;
#62095 = CARTESIAN_POINT ( 'NONE',  ( 4.458734124999999437, -18.81249999863440792, -5.460374474430324690E-16 ) ) ;
#62096 = EDGE_CURVE ( 'NONE', #11394, #40265, #40633, .T. ) ;
#62097 = CARTESIAN_POINT ( 'NONE',  ( -4.458734124999997661, -79.22916666530106511, 2.574251347313722516 ) ) ;
#62098 = CARTESIAN_POINT ( 'NONE',  ( 6.123233995736766282E-16, -120.0000000000000000, -5.000000000000000000 ) ) ;
#62099 = CARTESIAN_POINT ( 'NONE',  ( -2.499999999999996447, -14.70833333060214976, 4.330127018922195425 ) ) ;
#62101 = ORIENTED_EDGE ( 'NONE', *, *, #50975, .T. ) ;
#62100 = CARTESIAN_POINT ( 'NONE',  ( 2.229367062500001939, -42.97916666530107932, 3.861377020970579999 ) ) ;
#62102 = CARTESIAN_POINT ( 'NONE',  ( -6.972266317189433020E-16, -41.24999999999998579, -5.000000000000000000 ) ) ;
#62104 = ORIENTED_EDGE ( 'NONE', *, *, #26651, .T. ) ;
#62103 = CARTESIAN_POINT ( 'NONE',  ( -4.458734124999999437, 6.354166668032259047, -2.574251347313719407 ) ) ;
#62105 = CARTESIAN_POINT ( 'NONE',  ( 2.499999999999998668, -61.33333333333333570, -4.330127018922193649 ) ) ;
#62106 = CARTESIAN_POINT ( 'NONE',  ( -4.458734125000000326, -159.2500000013656063, -1.846868145590735644 ) ) ;
#62107 = CARTESIAN_POINT ( 'NONE',  ( -2.229367062499996610, -38.39583333196773651, 3.861377020970582219 ) ) ;
#62108 = CARTESIAN_POINT ( 'NONE',  ( 2.071067811865560326, -144.8124999999999716, -4.999999999999914735 ) ) ;
#62109 = CARTESIAN_POINT ( 'NONE',  ( 4.458734124999998549, -78.72916666530106511, -2.574251347313721627 ) ) ;
#62110 = CARTESIAN_POINT ( 'NONE',  ( -5.000000000000000888, -165.5625000000000568, -2.071067811865475949 ) ) ;
#62111 = EDGE_CURVE ( 'NONE', #62654, #7429, #29525, .T. ) ;
#62112 = CARTESIAN_POINT ( 'NONE',  ( -6.972266317189433020E-16, -30.25000000000000000, -5.000000000000000000 ) ) ;
#62113 = CARTESIAN_POINT ( 'NONE',  ( -50.70258187064364108, -129.3750000013656347, 2.196230717870141014 ) ) ;
#62114 = CARTESIAN_POINT ( 'NONE',  ( -2.229367062499996610, -3.395833331967738733, 3.861377020970582219 ) ) ;
#62115 = CARTESIAN_POINT ( 'NONE',  ( -4.458734124999999437, -41.64583333196773651, -2.574251347313719407 ) ) ;
#62116 = CARTESIAN_POINT ( 'NONE',  ( 3.535533905932736864, -151.2500000027312126, 3.535533905932738641 ) ) ;
#62117 = EDGE_CURVE ( 'NONE', #3560, #59122, #33909, .T. ) ;
#62118 = CARTESIAN_POINT ( 'NONE',  ( 4.458734124999998549, -84.97916666530106511, -2.574251347313721627 ) ) ;
#62119 = CARTESIAN_POINT ( 'NONE',  ( 5.000000000000000888, -86.58333333333332860, 2.886751345948126879 ) ) ;
#62120 = ORIENTED_EDGE ( 'NONE', *, *, #19972, .F. ) ;
#62121 = CARTESIAN_POINT ( 'NONE',  ( -5.000000000000000000, -94.87499999726881583, 0.000000000000000000 ) ) ;
#62122 = CARTESIAN_POINT ( 'NONE',  ( 2.500000000000002220, -2.541666663935477466, 4.330127018922192761 ) ) ;
#62123 = CARTESIAN_POINT ( 'NONE',  ( -2.229367062499996610, -71.39583333196773651, 3.861377020970582219 ) ) ;
#62124 = CARTESIAN_POINT ( 'NONE',  ( 1.846868145590736310, -145.8750000013656063, 4.458734124999997661 ) ) ;
#62125 = ORIENTED_EDGE ( 'NONE', *, *, #5916, .F. ) ;
#62126 = CARTESIAN_POINT ( 'NONE',  ( 0.000000000000000000, -170.0000000000000000, 5.000000000000000000 ) ) ;
#62127 = DIRECTION ( 'NONE',  ( 0.000000000000000000, 0.000000000000000000, 1.000000000000000000 ) ) ;
#62128 = CARTESIAN_POINT ( 'NONE',  ( 4.458734124999998549, -5.979166665301073103, -2.574251347313721627 ) ) ;
#62129 = CARTESIAN_POINT ( 'NONE',  ( -2.499999999999996447, 3.166666666666664742, 4.330127018922195425 ) ) ;
#62130 = CARTESIAN_POINT ( 'NONE',  ( -4.458734124999999437, 4.604166668032261711, -2.574251347313719407 ) ) ;
#62131 = CARTESIAN_POINT ( 'NONE',  ( -6.972266317189433020E-16, -30.12499999726880873, -5.000000000000000000 ) ) ;
#62132 = CARTESIAN_POINT ( 'NONE',  ( -4.458734124999999437, -155.9375000013655779, -5.460374474430324690E-16 ) ) ;
#62133 = CARTESIAN_POINT ( 'NONE',  ( 4.458734124999999437, 24.93750000136559208, -5.460374474430324690E-16 ) ) ;
#62134 = ORIENTED_EDGE ( 'NONE', *, *, #42834, .F. ) ;
#62135 = CARTESIAN_POINT ( 'NONE',  ( -4.458734124999997661, -91.22916666530106511, 2.574251347313722516 ) ) ;
#62136 = CARTESIAN_POINT ( 'NONE',  ( 5.000000000000000888, -60.45833333060213732, 2.886751345948126879 ) ) ;
#62137 = CARTESIAN_POINT ( 'NONE',  ( -3.152548672688508926E-16, -7.562499998634404363, -5.148502694627439702 ) ) ;
#62138 = EDGE_CURVE ( 'NONE', #3809, #55181, #38923, .T. ) ;
#62139 = CYLINDRICAL_SURFACE ( 'NONE', #13911, 5.000000000000000000 ) ;
#62140 = DIRECTION ( 'NONE',  ( -0.6485228581062915110, 0.000000000000000000, -0.7611951803011149931 ) ) ;
#62141 = CARTESIAN_POINT ( 'NONE',  ( -5.000000000000000000, 15.00000000000000000, 0.000000000000000000 ) ) ;
#62142 = CARTESIAN_POINT ( 'NONE',  ( -4.999999999999999112, -34.79166666393547303, 2.886751345948131764 ) ) ;
#62143 = DIRECTION ( 'NONE',  ( 0.000000000000000000, 0.000000000000000000, 1.000000000000000000 ) ) ;
#62144 = CARTESIAN_POINT ( 'NONE',  ( 4.458734124999999437, 17.18750000136559564, -5.460374474430324690E-16 ) ) ;
#62145 = CARTESIAN_POINT ( 'NONE',  ( 5.000000000000000888, -7.583333333333330373, 2.886751345948126879 ) ) ;
#62146 = EDGE_CURVE ( 'NONE', #2325, #54415, #60755, .T. ) ;
#62147 = CARTESIAN_POINT ( 'NONE',  ( 2.229367062499998831, 20.35416666803225993, -3.861377020970580887 ) ) ;
#62148 = CARTESIAN_POINT ( 'NONE',  ( -2.229367062499996610, -56.14583333196773651, 3.861377020970582219 ) ) ;
#62149 = CARTESIAN_POINT ( 'NONE',  ( -3.152548672688508926E-16, -1.812499998634406584, -5.148502694627439702 ) ) ;
#62150 = CARTESIAN_POINT ( 'NONE',  ( 0.000000000000000000, -120.0000000000000000, 0.000000000000000000 ) ) ;
#62151 = CARTESIAN_POINT ( 'NONE',  ( 2.499999999999998668, 10.66666666666666430, -4.330127018922193649 ) ) ;
#62152 = CARTESIAN_POINT ( 'NONE',  ( 3.535533905932738197, -140.0000000027311842, -3.535533905932738197 ) ) ;
#62153 = CARTESIAN_POINT ( 'NONE',  ( 1.339745962155615144, -75.58034179853029855, 4.999999999999999112 ) ) ;
#62154 = CARTESIAN_POINT ( 'NONE',  ( -4.458734124999998549, -48.22916666530106511, 2.574251347313722516 ) ) ;
#62155 = CARTESIAN_POINT ( 'NONE',  ( 2.499999999999998668, -82.20833333060214443, -4.330127018922193649 ) ) ;
#62156 = CARTESIAN_POINT ( 'NONE',  ( -58.39396692619412477, -134.6875000013656063, 2.891590998281057701 ) ) ;
#62157 =( BOUNDED_CURVE ( )  B_SPLINE_CURVE ( 2, ( #20827, #60393, #6358, #45579, #1535, #21140, #31102, #35939, #55880 ),
 .UNSPECIFIED., .F., .F. ) 
 B_SPLINE_CURVE_WITH_KNOTS ( ( 3, 2, 2, 2, 3 ),
 ( 0.7312499999999999556, 0.7319444444444443976, 0.7333333333333332815, 0.7347222222222222765, 0.7354166666666667185 ),
 .UNSPECIFIED. ) 
 CURVE ( )  GEOMETRIC_REPRESENTATION_ITEM ( )  RATIONAL_B_SPLINE_CURVE ( ( 0.9330127018922194093, 0.9330127018922194093, 1.000000000000000000, 0.8660254037844387076, 1.000000000000000000, 0.8660254037844387076, 1.000000000000000000, 0.9330127018922194093, 0.9330127018922194093 ) ) 
 REPRESENTATION_ITEM ( '' )  );
#62158 = CARTESIAN_POINT ( 'NONE',  ( -2.500000000000000444, -87.16666666666667140, -4.330127018922193649 ) ) ;
#62159 = FACE_OUTER_BOUND ( 'NONE', #9761, .T. ) ;
#62160 = CARTESIAN_POINT ( 'NONE',  ( -3.152548672688508926E-16, -88.81249999863439371, -5.148502694627439702 ) ) ;
#62161 = CARTESIAN_POINT ( 'NONE',  ( -8.190561711645485556E-16, -156.9375000013655779, 4.458734124999999437 ) ) ;
#62162 = CARTESIAN_POINT ( 'NONE',  ( 2.499999999999998668, -35.33333333333332860, -4.330127018922193649 ) ) ;
#62163 = CARTESIAN_POINT ( 'NONE',  ( -3.535533905932738641, -147.3750000000000000, 3.535533905932737309 ) ) ;
#62164 = ORIENTED_EDGE ( 'NONE', *, *, #5099, .F. ) ;
#62165 = CARTESIAN_POINT ( 'NONE',  ( 2.229367062500001939, 19.77083333469892779, 3.861377020970579999 ) ) ;
#62166 = ORIENTED_EDGE ( 'NONE', *, *, #42115, .T. ) ;
#62167 = CARTESIAN_POINT ( 'NONE',  ( -3.152548672688508926E-16, -98.56249999863442213, -5.148502694627439702 ) ) ;
#62168 = CARTESIAN_POINT ( 'NONE',  ( 4.458734124999999437, 6.937500001365594748, -5.460374474430324690E-16 ) ) ;
#62169 = CARTESIAN_POINT ( 'NONE',  ( -4.999999999999999112, 10.20833333606451987, 2.886751345948131764 ) ) ;
#62170 = CARTESIAN_POINT ( 'NONE',  ( 2.500000000000002220, 2.333333333333333037, 4.330127018922192761 ) ) ;
#62171 = CARTESIAN_POINT ( 'NONE',  ( -3.152548672688508926E-16, -59.56249999863440081, -5.148502694627439702 ) ) ;
#62172 = CARTESIAN_POINT ( 'NONE',  ( -5.000000000000000000, -40.08333333333332860, -2.886751345948128211 ) ) ;
#62173 = CARTESIAN_POINT ( 'NONE',  ( -5.000000000000000000, -81.08333333333332860, -2.886751345948128211 ) ) ;
#62174 = EDGE_CURVE ( 'NONE', #39445, #59704, #22987, .T. ) ;
#62175 = ADVANCED_FACE ( 'NONE', ( #9769 ), #4958, .T. ) ;
#62176 = CARTESIAN_POINT ( 'NONE',  ( -2.229367062499996610, -26.14583333196773651, 3.861377020970582219 ) ) ;
#62177 = CARTESIAN_POINT ( 'NONE',  ( -6.972266317189433020E-16, -61.25000000000000000, -5.000000000000000000 ) ) ;
#62178 = CARTESIAN_POINT ( 'NONE',  ( -1.339745962155613812, -13.08034179853029144, -5.000000000000000000 ) ) ;
#62179 = EDGE_CURVE ( 'NONE', #62654, #9564, #4634, .T. ) ;
#62180 = CARTESIAN_POINT ( 'NONE',  ( -3.535533905932737309, -151.7500000027312126, -3.535533905932738197 ) ) ;
#62181 = CARTESIAN_POINT ( 'NONE',  ( 5.000000000000000000, -38.49999999999999289, -6.123233995736766282E-16 ) ) ;
#62182 = CARTESIAN_POINT ( 'NONE',  ( -6.972266317189433020E-16, -107.2499999999999858, -5.000000000000000000 ) ) ;
#62184 = CARTESIAN_POINT ( 'NONE',  ( 4.458734124999999437, -21.06249999863440436, -5.460374474430324690E-16 ) ) ;
#62183 = CARTESIAN_POINT ( 'NONE',  ( -4.999999999999998224, -42.91666666666665719, 2.886751345948131764 ) ) ;
#62185 = CARTESIAN_POINT ( 'NONE',  ( -4.999999999999998224, -57.91666666666665719, 2.886751345948131764 ) ) ;
#62186 = CARTESIAN_POINT ( 'NONE',  ( -2.229367062500000163, -63.47916666530106511, -3.861377020970580443 ) ) ;
#62187 = CARTESIAN_POINT ( 'NONE',  ( 4.458734124999999437, -147.7500000013655779, 1.846868145590737864 ) ) ;
#62188 = CARTESIAN_POINT ( 'NONE',  ( -4.458734124999999437, -74.39583333196775072, -2.574251347313719407 ) ) ;
#62189 = CARTESIAN_POINT ( 'NONE',  ( -50.70258187064364108, -144.3750000013656063, 2.196230717870141014 ) ) ;
#62190 = ADVANCED_FACE ( 'NONE', ( #18792 ), #43861, .T. ) ;
#62191 = VECTOR ( 'NONE', #11868, 1000.000000000000000 ) ;
#62192 = CARTESIAN_POINT ( 'NONE',  ( -4.458734124999999437, -24.56249999863440436, 0.000000000000000000 ) ) ;
#62193 = CARTESIAN_POINT ( 'NONE',  ( -2.500000000000000444, -68.04166666393547303, -4.330127018922193649 ) ) ;
#62194 = VERTEX_POINT ( 'NONE', #5597 ) ;
#62195 = DIRECTION ( 'NONE',  ( -0.000000000000000000, 1.000000000000000000, -0.000000000000000000 ) ) ;
#62197 = EDGE_LOOP ( 'NONE', ( #10496, #32682, #16710, #19342 ) ) ;
#62196 = EDGE_CURVE ( 'NONE', #20174, #14373, #36135, .T. ) ;
#62198 = CARTESIAN_POINT ( 'NONE',  ( 4.458734124999999437, -70.06249999863439371, -5.460374474430324690E-16 ) ) ;
#62199 = CARTESIAN_POINT ( 'NONE',  ( 5.000000000000000888, -7.458333330602142652, 2.886751345948126879 ) ) ;
#62200 = CARTESIAN_POINT ( 'NONE',  ( 0.000000000000000000, 0.000000000000000000, 0.000000000000000000 ) ) ;
#62201 = EDGE_CURVE ( 'NONE', #10085, #13039, #53768, .T. ) ;
#62202 = VERTEX_POINT ( 'NONE', #35192 ) ;
#62203 = EDGE_CURVE ( 'NONE', #1660, #52091, #42691, .T. ) ;
#62204 = DIRECTION ( 'NONE',  ( 1.000000000000000000, 0.000000000000000000, -7.709882115452477180E-16 ) ) ;
#62205 = CARTESIAN_POINT ( 'NONE',  ( -1.339745962155610925, -74.66965819600731891, 5.000000000000000000 ) ) ;
#62206 = CARTESIAN_POINT ( 'NONE',  ( 4.458734124999998549, -54.97916666530107221, -2.574251347313721627 ) ) ;
#62207 = VERTEX_POINT ( 'NONE', #40326 ) ;
#62208 = CARTESIAN_POINT ( 'NONE',  ( -2.229367062500000163, 9.520833334698927786, -3.861377020970580443 ) ) ;
#62209 =( BOUNDED_CURVE ( )  B_SPLINE_CURVE ( 2, ( #57767, #48408, #8551, #9482, #3736, #52928, #17886, #62905, #42640 ),
 .UNSPECIFIED., .F., .F. ) 
 B_SPLINE_CURVE_WITH_KNOTS ( ( 3, 2, 2, 2, 3 ),
 ( 0.2946428571428571508, 0.2952380952380952439, 0.2964285714285714302, 0.2976190476190476164, 0.2982142857142857095 ),
 .UNSPECIFIED. ) 
 CURVE ( )  GEOMETRIC_REPRESENTATION_ITEM ( )  RATIONAL_B_SPLINE_CURVE ( ( 0.9330127018922194093, 0.9330127018922194093, 1.000000000000000000, 0.8660254037844387076, 1.000000000000000000, 0.8660254037844387076, 1.000000000000000000, 0.9330127018922194093, 0.9330127018922194093 ) ) 
 REPRESENTATION_ITEM ( '' )  );
#62210 = CARTESIAN_POINT ( 'NONE',  ( -2.229367062500000163, 16.52083333469892779, -3.861377020970580443 ) ) ;
#62211 = CARTESIAN_POINT ( 'NONE',  ( -55.35523342533222291, -143.3125000013656063, 4.444560631937231499 ) ) ;
#62212 = CARTESIAN_POINT ( 'NONE',  ( -2.499999999999996447, -1.833333333333332593, 4.330127018922195425 ) ) ;
#62213 = CARTESIAN_POINT ( 'NONE',  ( 4.458734124999999437, -169.4375000013656063, 0.000000000000000000 ) ) ;
#62214 = ORIENTED_EDGE ( 'NONE', *, *, #7348, .F. ) ;
#62215 = CARTESIAN_POINT ( 'NONE',  ( 2.229367062500001939, -73.97916666530106511, 3.861377020970579999 ) ) ;
#62216 = CARTESIAN_POINT ( 'NONE',  ( 5.000000000000000000, 14.70833333606451809, -2.886751345948130876 ) ) ;
#62217 = CARTESIAN_POINT ( 'NONE',  ( 2.229367062500001939, 5.020833334698926897, 3.861377020970579999 ) ) ;
#62218 = LINE ( 'NONE', #18136, #797 ) ;
#62219 = CARTESIAN_POINT ( 'NONE',  ( 9.457646018065525792E-16, -62.31249999863440792, 5.148502694627439702 ) ) ;
#62220 = CARTESIAN_POINT ( 'NONE',  ( 5.000000000000000000, -22.37499999726881228, -6.123233995736766282E-16 ) ) ;
#62221 = CARTESIAN_POINT ( 'NONE',  ( -4.999999999999998224, -18.91666666666666430, 2.886751345948131764 ) ) ;
#62222 = DIRECTION ( 'NONE',  ( 0.000000000000000000, 0.000000000000000000, 1.000000000000000000 ) ) ;
#62223 = DIRECTION ( 'NONE',  ( -0.000000000000000000, 1.000000000000000000, -0.000000000000000000 ) ) ;
#62224 = CARTESIAN_POINT ( 'NONE',  ( -55.00000000000002132, -155.0000000000000284, 1.734723475976807094E-15 ) ) ;
#62225 = CARTESIAN_POINT ( 'NONE',  ( -51.75738570946856498, -139.7500000000000000, 3.805975901505576964 ) ) ;
#62226 = CARTESIAN_POINT ( 'NONE',  ( -4.458734124999999437, -43.31249999863440081, 0.000000000000000000 ) ) ;
#62227 = CARTESIAN_POINT ( 'NONE',  ( -4.458734124999999437, -25.56249999863440792, 0.000000000000000000 ) ) ;
#62228 = CARTESIAN_POINT ( 'NONE',  ( -4.729367062499999719, 29.84375000068279604, 0.000000000000000000 ) ) ;
#62229 = CARTESIAN_POINT ( 'NONE',  ( 4.458734124999998549, -106.7291666653010651, -2.574251347313721627 ) ) ;
#62230 = CARTESIAN_POINT ( 'NONE',  ( -2.071067811865478170, -154.4375000027312126, 5.000000000000000000 ) ) ;
#62231 = ORIENTED_EDGE ( 'NONE', *, *, #37875, .T. ) ;
#62232 = CARTESIAN_POINT ( 'NONE',  ( 4.458734124999999437, -110.0624999986343937, -5.460374474430324690E-16 ) ) ;
#62233 = CARTESIAN_POINT ( 'NONE',  ( -2.229367062500000163, -34.47916666530107221, -3.861377020970580443 ) ) ;
#62234 = CARTESIAN_POINT ( 'NONE',  ( -2.500000000000000444, -66.04166666393547303, -4.330127018922193649 ) ) ;
#62235 = AXIS2_PLACEMENT_3D ( 'NONE', #36988, #32145, #46957 ) ;
#62236 = CARTESIAN_POINT ( 'NONE',  ( -54.64476657466781973, -148.0625000013656063, -4.444560631937228834 ) ) ;
#62237 = CARTESIAN_POINT ( 'NONE',  ( 5.000000000000000000, -146.0625000000000000, 2.071067811865478614 ) ) ;
#62238 = CARTESIAN_POINT ( 'NONE',  ( 2.229367062499998831, -30.64583333196773651, -3.861377020970580887 ) ) ;
#62239 = CARTESIAN_POINT ( 'NONE',  ( -3.152548672688508926E-16, -70.81249999863439371, -5.148502694627439702 ) ) ;
#62240 = CARTESIAN_POINT ( 'NONE',  ( -4.458734124999999437, -168.1875000013655779, -5.460374474430324690E-16 ) ) ;
#62242 = CARTESIAN_POINT ( 'NONE',  ( 2.229367062499998831, -32.64583333196773651, -3.861377020970580887 ) ) ;
#62241 = PRODUCT_RELATED_PRODUCT_CATEGORY ( 'part', '', ( #19930 ) ) ;
#62243 = LINE ( 'NONE', #4314, #12238 ) ;
#62244 = CARTESIAN_POINT ( 'NONE',  ( 8.660254037844342889, 45.00000000000000000, 0.000000000000000000 ) ) ;
#62245 = CARTESIAN_POINT ( 'NONE',  ( -5.000000000000000000, -16.08333333333333215, -2.886751345948128211 ) ) ;
#62246 = CARTESIAN_POINT ( 'NONE',  ( 4.458734125000000326, -146.3750000013655779, -1.846868145590734978 ) ) ;
#62247 = ORIENTED_EDGE ( 'NONE', *, *, #56159, .T. ) ;
#62248 = LINE ( 'NONE', #17853, #32779 ) ;
#62249 = CARTESIAN_POINT ( 'NONE',  ( 2.229367062500001939, -58.22916666530107932, 3.861377020970579999 ) ) ;
#62250 = CARTESIAN_POINT ( 'NONE',  ( -5.000000000000000000, 27.04166666939785202, -2.886751345948128211 ) ) ;
#62251 = DIRECTION ( 'NONE',  ( -0.8191520442889907994, 0.000000000000000000, -0.5735764363510474917 ) ) ;
#62252 = CARTESIAN_POINT ( 'NONE',  ( -5.000000000000000000, 26.91666666666666075, -2.886751345948128211 ) ) ;
#62253 = CARTESIAN_POINT ( 'NONE',  ( 0.000000000000000000, -170.0000000000000000, 0.000000000000000000 ) ) ;
#62254 = CARTESIAN_POINT ( 'NONE',  ( 4.458734125000001214, 0.1041666680322607674, 2.574251347313718519 ) ) ;
#62255 = CARTESIAN_POINT ( 'NONE',  ( 1.339745962155612702, -48.29465819873851729, -5.000000000000000000 ) ) ;
#62256 = ADVANCED_FACE ( 'NONE', ( #44825 ), #49971, .T. ) ;
#62257 = CARTESIAN_POINT ( 'NONE',  ( 2.499999999999998668, -14.33333333333333037, -4.330127018922193649 ) ) ;
#62258 = CARTESIAN_POINT ( 'NONE',  ( 4.458734125000001214, 8.854166668032261711, 2.574251347313718519 ) ) ;
#62259 = ORIENTED_EDGE ( 'NONE', *, *, #12296, .F. ) ;
#62260 = CARTESIAN_POINT ( 'NONE',  ( -75.00000000000002842, 15.00000000000000000, 5.000000000000000000 ) ) ;
#62261 = ORIENTED_EDGE ( 'NONE', *, *, #53840, .T. ) ;
#62262 =( BOUNDED_CURVE ( )  B_SPLINE_CURVE ( 2, ( #9726, #42011, #32366, #14550, #37827, #53792, #51990, #13063, #32683 ),
 .UNSPECIFIED., .F., .F. ) 
 B_SPLINE_CURVE_WITH_KNOTS ( ( 3, 2, 2, 2, 3 ),
 ( 0.7395833333333333703, 0.7402777777777778123, 0.7416666666666666963, 0.7430555555555555802, 0.7437500000000000222 ),
 .UNSPECIFIED. ) 
 CURVE ( )  GEOMETRIC_REPRESENTATION_ITEM ( )  RATIONAL_B_SPLINE_CURVE ( ( 0.9330127018922194093, 0.9330127018922194093, 1.000000000000000000, 0.8660254037844387076, 1.000000000000000000, 0.8660254037844387076, 1.000000000000000000, 0.9330127018922194093, 0.9330127018922194093 ) ) 
 REPRESENTATION_ITEM ( '' )  );
#62263 = CARTESIAN_POINT ( 'NONE',  ( 1.975475456537005874E-15, -83.62499999726878741, 5.000000000000000000 ) ) ;
#62264 = CARTESIAN_POINT ( 'NONE',  ( -4.458734124999998549, -48.22916666530106511, 2.574251347313722516 ) ) ;
#62265 = CARTESIAN_POINT ( 'NONE',  ( 4.458734124999999437, -159.7500000013656063, 1.846868145590737864 ) ) ;
#62266 = CARTESIAN_POINT ( 'NONE',  ( 1.060575238724906964E-15, -49.62499999726880873, 5.773502691896257311 ) ) ;
#62267 = ORIENTED_EDGE ( 'NONE', *, *, #9879, .F. ) ;
#62268 = CARTESIAN_POINT ( 'NONE',  ( 2.229367062500001939, -23.97916666530107577, 3.861377020970579999 ) ) ;
#62269 = ORIENTED_EDGE ( 'NONE', *, *, #6627, .F. ) ;
#62271 = CYLINDRICAL_SURFACE ( 'NONE', #43961, 5.000000000000000000 ) ;
#62270 = CARTESIAN_POINT ( 'NONE',  ( -5.000000000000000000, 0.04166666939785235169, -2.886751345948128211 ) ) ;
#62272 = CARTESIAN_POINT ( 'NONE',  ( -8.190561711645485556E-16, -159.6875000013655779, 4.458734124999999437 ) ) ;
#62273 = EDGE_CURVE ( 'NONE', #29833, #43959, #43072, .T. ) ;
#62274 = EDGE_CURVE ( 'NONE', #43978, #454, #63187, .T. ) ;
#62275 = EDGE_CURVE ( 'NONE', #55065, #12482, #60915, .T. ) ;
#62276 = FACE_OUTER_BOUND ( 'NONE', #23894, .T. ) ;
#62277 = CARTESIAN_POINT ( 'NONE',  ( -51.19402409849444524, -136.5000000000000284, -3.242614290531456334 ) ) ;
#62278 = CARTESIAN_POINT ( 'NONE',  ( 4.458734124999998549, -35.97916666530107221, -2.574251347313721627 ) ) ;
#62279 = ORIENTED_EDGE ( 'NONE', *, *, #55435, .F. ) ;
#62280 = ADVANCED_FACE ( 'NONE', ( #30990 ), #40954, .T. ) ;
#62281 = CARTESIAN_POINT ( 'NONE',  ( -4.458734124999999437, -80.31249999863440792, 0.000000000000000000 ) ) ;
#62282 = CARTESIAN_POINT ( 'NONE',  ( -4.458734124999999437, 24.68750000136559208, 0.000000000000000000 ) ) ;
#62283 = VERTEX_POINT ( 'NONE', #62177 ) ;
#62284 = CARTESIAN_POINT ( 'NONE',  ( -6.972266317189433020E-16, 14.74999999999999822, -5.000000000000000000 ) ) ;
#62285 = CARTESIAN_POINT ( 'NONE',  ( -58.39396692619412477, -139.6875000013656347, 2.891590998281057701 ) ) ;
#62286 = CARTESIAN_POINT ( 'NONE',  ( 4.458734124999998549, -84.97916666530106511, -2.574251347313721627 ) ) ;
#62287 = CARTESIAN_POINT ( 'NONE',  ( -53.33387254593733928, -128.9375000027312126, 5.149110718188519620 ) ) ;
#62288 = CARTESIAN_POINT ( 'NONE',  ( 1.339745962155615144, -88.70534180126146850, 4.999999999999999112 ) ) ;
#62289 = CARTESIAN_POINT ( 'NONE',  ( 1.339745962155615144, -9.705341801261479162, 4.999999999999999112 ) ) ;
#62290 = CARTESIAN_POINT ( 'NONE',  ( 1.339745962155612702, -57.29465819873851729, -5.000000000000000000 ) ) ;
#62291 = CARTESIAN_POINT ( 'NONE',  ( -2.229367062499996610, -56.14583333196773651, 3.861377020970582219 ) ) ;
#62292 = CARTESIAN_POINT ( 'NONE',  ( -6.972266317189433020E-16, -37.25000000000000000, -5.000000000000000000 ) ) ;
#62293 = CARTESIAN_POINT ( 'NONE',  ( 4.458734125000001214, 22.10416666803225993, 2.574251347313718519 ) ) ;
#62294 = LINE ( 'NONE', #57160, #42236 ) ;
#62295 = CARTESIAN_POINT ( 'NONE',  ( 4.458734124999998549, -43.97916666530105800, -2.574251347313721627 ) ) ;
#62296 = CARTESIAN_POINT ( 'NONE',  ( -3.535250795749689387E-16, -5.124999997268809615, -5.773502691896257311 ) ) ;
#62297 = CARTESIAN_POINT ( 'NONE',  ( 1.339745962155612702, -31.29465819873851373, -5.000000000000000000 ) ) ;
#62298 = CARTESIAN_POINT ( 'NONE',  ( -52.10840900171896806, -125.1875000013656063, 3.393966926194110556 ) ) ;
#62299 = CARTESIAN_POINT ( 'NONE',  ( 4.458734124999998549, -82.97916666530107932, -2.574251347313721627 ) ) ;
#62300 = CARTESIAN_POINT ( 'NONE',  ( 4.458734124999998549, -101.7291666653010935, -2.574251347313721627 ) ) ;
#62301 = CARTESIAN_POINT ( 'NONE',  ( -4.458734124999999437, -3.562499998634407916, 0.000000000000000000 ) ) ;
#62302 = ORIENTED_EDGE ( 'NONE', *, *, #54619, .F. ) ;
#62303 = CARTESIAN_POINT ( 'NONE',  ( -1.339745962155613812, 17.91965820146970856, -5.000000000000000000 ) ) ;
#62304 = CARTESIAN_POINT ( 'NONE',  ( -4.458734124999999437, -91.31249999863440792, 0.000000000000000000 ) ) ;
#62305 = CARTESIAN_POINT ( 'NONE',  ( -5.000000000000000888, -166.5625000027312126, 2.071067811865474617 ) ) ;
#62306 = CARTESIAN_POINT ( 'NONE',  ( 2.229367062500001939, -94.22916666530106511, 3.861377020970579999 ) ) ;
#62307 = LINE ( 'NONE', #46240, #7914 ) ;
#62308 = CARTESIAN_POINT ( 'NONE',  ( -50.55543936806279248, -128.0625000013656063, 0.3552334253322060320 ) ) ;
#62309 = CARTESIAN_POINT ( 'NONE',  ( 4.458734124999998549, -11.72916666530107044, -2.574251347313721627 ) ) ;
#62310 = CARTESIAN_POINT ( 'NONE',  ( -2.229367062499996610, 10.60416666803225993, 3.861377020970582219 ) ) ;
#62311 = CARTESIAN_POINT ( 'NONE',  ( 4.458734124999999437, -55.06249999863440081, -5.460374474430324690E-16 ) ) ;
#62312 = CARTESIAN_POINT ( 'NONE',  ( -1.339745962155613812, -20.20534180126147916, -5.000000000000000000 ) ) ;
#62313 = CARTESIAN_POINT ( 'NONE',  ( 1.339745962155612702, 17.70534180126147916, -5.000000000000000000 ) ) ;
#62314 = CARTESIAN_POINT ( 'NONE',  ( 4.458734124999999437, -10.81249999863440792, -5.460374474430324690E-16 ) ) ;
#62315 = CARTESIAN_POINT ( 'NONE',  ( 5.000000000000000000, -84.41666666666667140, -2.886751345948130876 ) ) ;
#62316 = ORIENTED_EDGE ( 'NONE', *, *, #468, .T. ) ;
#62317 = CARTESIAN_POINT ( 'NONE',  ( 2.229367062499998831, -37.89583333196773651, -3.861377020970580887 ) ) ;
#62318 = VECTOR ( 'NONE', #14509, 1000.000000000000000 ) ;
#62319 = CARTESIAN_POINT ( 'NONE',  ( -55.35523342533222291, -129.5625000013656063, 4.444560631937231499 ) ) ;
#62320 = CARTESIAN_POINT ( 'NONE',  ( 1.975475456537005874E-15, -68.74999999999998579, 5.000000000000000000 ) ) ;
#62321 = CARTESIAN_POINT ( 'NONE',  ( 1.975475456537005874E-15, 10.24999999999999822, 5.000000000000000000 ) ) ;
#62322 = CARTESIAN_POINT ( 'NONE',  ( 2.229367062500001939, -81.97916666530106511, 3.861377020970579999 ) ) ;
#62323 = CARTESIAN_POINT ( 'NONE',  ( 4.458734124999999437, 24.93750000136559208, -5.460374474430324690E-16 ) ) ;
#62324 = VECTOR ( 'NONE', #40077, 1000.000000000000000 ) ;
#62325 = VECTOR ( 'NONE', #3137, 1000.000000000000000 ) ;
#62327 = EDGE_CURVE ( 'NONE', #25261, #8589, #42539, .T. ) ;
#62326 = CARTESIAN_POINT ( 'NONE',  ( 4.458734124999998549, 16.27083333469892779, -2.574251347313721627 ) ) ;
#62328 = CARTESIAN_POINT ( 'NONE',  ( -4.999999999999998224, 7.083333333333333925, 2.886751345948131764 ) ) ;
#62329 = CYLINDRICAL_SURFACE ( 'NONE', #944, 5.000000000000000000 ) ;
#62330 = CARTESIAN_POINT ( 'NONE',  ( -4.458734124999999437, -84.56249999863439371, 0.000000000000000000 ) ) ;
#62331 = CARTESIAN_POINT ( 'NONE',  ( 5.000000000000000000, -71.41666666666665719, -2.886751345948129988 ) ) ;
#62332 = CARTESIAN_POINT ( 'NONE',  ( 1.060575238724906964E-15, 11.37500000273118594, 5.773502691896257311 ) ) ;
#62333 = ORIENTED_EDGE ( 'NONE', *, *, #61739, .T. ) ;
#62334 = CARTESIAN_POINT ( 'NONE',  ( -6.972266317189433020E-16, -35.25000000000000000, -5.000000000000000000 ) ) ;
#62335 = CARTESIAN_POINT ( 'NONE',  ( 1.975475456537005874E-15, -89.74999999999998579, 5.000000000000000000 ) ) ;
#62337 = CARTESIAN_POINT ( 'NONE',  ( 5.000000000000000000, -31.50000000000000000, -6.123233995736766282E-16 ) ) ;
#62336 = CARTESIAN_POINT ( 'NONE',  ( 5.000000000000000000, -52.50000000000000711, -6.123233995736766282E-16 ) ) ;
#62338 = CARTESIAN_POINT ( 'NONE',  ( -4.458734124999999437, -32.31249999863440792, 0.000000000000000000 ) ) ;
#62339 = CARTESIAN_POINT ( 'NONE',  ( 5.000000000000000000, -62.50000000000000000, -6.123233995736766282E-16 ) ) ;
#62340 =( BOUNDED_CURVE ( )  B_SPLINE_CURVE ( 2, ( #13475, #34026, #13778, #48187, #28881, #43665, #43357, #4140, #63306 ),
 .UNSPECIFIED., .F., .F. ) 
 B_SPLINE_CURVE_WITH_KNOTS ( ( 3, 2, 2, 2, 3 ),
 ( 0.8354166666666666963, 0.8361111111111111382, 0.8375000000000000222, 0.8388888888888889062, 0.8395833333333333481 ),
 .UNSPECIFIED. ) 
 CURVE ( )  GEOMETRIC_REPRESENTATION_ITEM ( )  RATIONAL_B_SPLINE_CURVE ( ( 0.9330127018922194093, 0.9330127018922194093, 1.000000000000000000, 0.8660254037844387076, 1.000000000000000000, 0.8660254037844387076, 1.000000000000000000, 0.9330127018922194093, 0.9330127018922194093 ) ) 
 REPRESENTATION_ITEM ( '' )  );
#62341 = CARTESIAN_POINT ( 'NONE',  ( 2.500000000000002220, -28.54166666393548013, 4.330127018922192761 ) ) ;
#62343 = VERTEX_POINT ( 'NONE', #13596 ) ;
#62342 = CARTESIAN_POINT ( 'NONE',  ( -4.458734124999999437, -60.39583333196773651, -2.574251347313719407 ) ) ;
#62344 = FACE_OUTER_BOUND ( 'NONE', #6701, .T. ) ;
#62346 = VERTEX_POINT ( 'NONE', #27124 ) ;
#62345 = CARTESIAN_POINT ( 'NONE',  ( 4.458734124999998549, -6.979166665301073103, -2.574251347313721627 ) ) ;
#62347 = CARTESIAN_POINT ( 'NONE',  ( 5.000000000000000888, -75.58333333333334281, 2.886751345948126879 ) ) ;
#62348 = CARTESIAN_POINT ( 'NONE',  ( -50.70258187064364108, -135.1250000013656063, 2.196230717870141014 ) ) ;
#62349 = CARTESIAN_POINT ( 'NONE',  ( 4.458734124999999437, -54.06249999863440081, -5.460374474430324690E-16 ) ) ;
#62350 = CARTESIAN_POINT ( 'NONE',  ( -2.499999999999996447, -74.70833333060214443, 4.330127018922195425 ) ) ;
#62351 = ORIENTED_EDGE ( 'NONE', *, *, #52293, .F. ) ;
#62352 = CARTESIAN_POINT ( 'NONE',  ( -59.98410592259440222, -151.1250000000000284, -0.3983568153799752487 ) ) ;
#62353 = CARTESIAN_POINT ( 'NONE',  ( 9.457646018065525792E-16, -22.31249999863440792, 5.148502694627439702 ) ) ;
#62355 = VERTEX_POINT ( 'NONE', #26808 ) ;
#62354 = CARTESIAN_POINT ( 'NONE',  ( -4.458734124999999437, -59.64583333196773651, -2.574251347313719407 ) ) ;
#62356 =( BOUNDED_CURVE ( )  B_SPLINE_CURVE ( 2, ( #30396, #20761, #24946, #20118, #40367, #39720, #60008, #15931, #35554 ),
 .UNSPECIFIED., .F., .F. ) 
 B_SPLINE_CURVE_WITH_KNOTS ( ( 3, 2, 2, 2, 3 ),
 ( 0.5104166666666666297, 0.5111111111111110716, 0.5124999999999999556, 0.5138888888888888395, 0.5145833333333332815 ),
 .UNSPECIFIED. ) 
 CURVE ( )  GEOMETRIC_REPRESENTATION_ITEM ( )  RATIONAL_B_SPLINE_CURVE ( ( 0.9330127018922194093, 0.9330127018922194093, 1.000000000000000000, 0.8660254037844387076, 1.000000000000000000, 0.8660254037844387076, 1.000000000000000000, 0.9330127018922194093, 0.9330127018922194093 ) ) 
 REPRESENTATION_ITEM ( '' )  );
#62357 = SURFACE_STYLE_FILL_AREA ( #62675 ) ;
#62358 = CARTESIAN_POINT ( 'NONE',  ( 1.846868145590735200, -142.2500000013656063, -4.458734125000000326 ) ) ;
#62359 = CARTESIAN_POINT ( 'NONE',  ( 4.458734124999999437, -100.0624999986344079, -5.460374474430324690E-16 ) ) ;
#62360 = CARTESIAN_POINT ( 'NONE',  ( -5.000000000000000000, -68.87499999726880162, 0.000000000000000000 ) ) ;
#62361 = ORIENTED_EDGE ( 'NONE', *, *, #10608, .T. ) ;
#62362 = CARTESIAN_POINT ( 'NONE',  ( -55.35523342533222291, -149.5625000013656063, 4.444560631937231499 ) ) ;
#62363 = CARTESIAN_POINT ( 'NONE',  ( -59.81910112700025905, -142.3125000027312410, -2.462841084822630311 ) ) ;
#62364 = FACE_OUTER_BOUND ( 'NONE', #18443, .T. ) ;
#62365 = AXIS2_PLACEMENT_3D ( 'NONE', #60728, #55266, #7644 ) ;
#62366 = CARTESIAN_POINT ( 'NONE',  ( -2.229367062499996610, -8.145833331967736513, 3.861377020970582219 ) ) ;
#62367 = CARTESIAN_POINT ( 'NONE',  ( -2.229367062500000163, -93.72916666530106511, -3.861377020970580443 ) ) ;
#62368 = CARTESIAN_POINT ( 'NONE',  ( 2.730187237215162345E-16, -143.4375000013656063, -4.458734124999999437 ) ) ;
#62369 = CARTESIAN_POINT ( 'NONE',  ( -4.458734124999999437, -30.64583333196774007, -2.574251347313719407 ) ) ;
#62370 = CONICAL_SURFACE ( 'NONE', #47933, 7.500000000000001776, 0.8594454914424796144 ) ;
#62371 = CYLINDRICAL_SURFACE ( 'NONE', #11890, 5.000000000000000000 ) ;
#62372 = CARTESIAN_POINT ( 'NONE',  ( -52.10840900171896806, -135.1875000013656063, 3.393966926194110556 ) ) ;
#62373 = CARTESIAN_POINT ( 'NONE',  ( -2.229367062500000163, -67.72916666530106511, -3.861377020970580443 ) ) ;
#62374 = CARTESIAN_POINT ( 'NONE',  ( -6.972266317189433020E-16, -43.25000000000000000, -5.000000000000000000 ) ) ;
#62375 = CARTESIAN_POINT ( 'NONE',  ( 1.975475456537005874E-15, -88.62499999726880162, 5.000000000000000000 ) ) ;
#62376 = CARTESIAN_POINT ( 'NONE',  ( 4.458734124999999437, -142.4375000013656063, 0.000000000000000000 ) ) ;
#62377 = CARTESIAN_POINT ( 'NONE',  ( -2.229367062499996610, 10.60416666803225993, 3.861377020970582219 ) ) ;
#62378 = ORIENTED_EDGE ( 'NONE', *, *, #53865, .F. ) ;
#62379 = CARTESIAN_POINT ( 'NONE',  ( 4.330127018922154569, 45.00000000000000000, -7.499999999999971578 ) ) ;
#62380 = CARTESIAN_POINT ( 'NONE',  ( 2.499999999999998668, -66.20833333060213022, -4.330127018922193649 ) ) ;
#62382 = CARTESIAN_POINT ( 'NONE',  ( -4.458734124999999437, -26.39583333196773651, -2.574251347313719407 ) ) ;
#62381 = CARTESIAN_POINT ( 'NONE',  ( -5.000000000000000000, -92.00000000000000000, 0.000000000000000000 ) ) ;
#62383 = CARTESIAN_POINT ( 'NONE',  ( -58.59997141384986463, -154.8437500006828031, 3.067102644406258793 ) ) ;
#62384 = CARTESIAN_POINT ( 'NONE',  ( -2.229367062499996610, -75.39583333196773651, 3.861377020970582219 ) ) ;
#62385 = ADVANCED_FACE ( 'NONE', ( #56723 ), #46740, .T. ) ;
#62386 = CARTESIAN_POINT ( 'NONE',  ( 2.229367062500001939, 24.77083333469892779, 3.861377020970579999 ) ) ;
#62387 = CARTESIAN_POINT ( 'NONE',  ( 5.000000000000000000, -76.29166666393547303, -2.886751345948130876 ) ) ;
#62388 = CARTESIAN_POINT ( 'NONE',  ( -52.80376928212989185, -142.8750000013656063, -4.297418129356379346 ) ) ;
#62389 = CARTESIAN_POINT ( 'NONE',  ( 9.457646018065525792E-16, 0.9375000013655959696, 5.148502694627439702 ) ) ;
#62390 = CARTESIAN_POINT ( 'NONE',  ( -4.458734124999999437, 28.35416666803226349, -2.574251347313719407 ) ) ;
#62391 = CARTESIAN_POINT ( 'NONE',  ( 2.229367062499998831, -35.89583333196773651, -3.861377020970580887 ) ) ;
#62392 = CARTESIAN_POINT ( 'NONE',  ( -6.972266317189433020E-16, -4.124999997268814056, -5.000000000000000000 ) ) ;
#62393 = CARTESIAN_POINT ( 'NONE',  ( -2.229367062500000163, 6.520833334698928674, -3.861377020970580443 ) ) ;
#62394 = CARTESIAN_POINT ( 'NONE',  ( 4.458734125000001214, -70.89583333196773651, 2.574251347313718519 ) ) ;
#62395 = CARTESIAN_POINT ( 'NONE',  ( -2.229367062499996610, -17.39583333196773651, 3.861377020970582219 ) ) ;
#62396 = CARTESIAN_POINT ( 'NONE',  ( 5.000000000000000000, -7.416666666666667851, -2.886751345948129988 ) ) ;
#62397 = CARTESIAN_POINT ( 'NONE',  ( 4.458734124999999437, -161.4375000013655779, 0.000000000000000000 ) ) ;
#62398 = CARTESIAN_POINT ( 'NONE',  ( -3.535533905932737309, -158.6250000000000284, -3.535533905932738197 ) ) ;
#62399 = CARTESIAN_POINT ( 'NONE',  ( -4.458734124999999437, -62.31249999863440792, 0.000000000000000000 ) ) ;
#62400 = CARTESIAN_POINT ( 'NONE',  ( 2.500000000000002220, -101.5416666639354588, 4.330127018922192761 ) ) ;
#62401 = DIRECTION ( 'NONE',  ( 0.000000000000000000, 0.000000000000000000, 1.000000000000000000 ) ) ;
#62402 = CARTESIAN_POINT ( 'NONE',  ( 2.229367062499998831, -42.64583333196773651, -3.861377020970580887 ) ) ;
#62403 = CARTESIAN_POINT ( 'NONE',  ( 1.975475456537005874E-15, -83.74999999999998579, 5.000000000000000000 ) ) ;
#62404 = CARTESIAN_POINT ( 'NONE',  ( 2.229367062500001939, -105.2291666653010651, 3.861377020970579999 ) ) ;
#62405 = CARTESIAN_POINT ( 'NONE',  ( 9.457646018065525792E-16, -68.31249999863440792, 5.148502694627439702 ) ) ;
#62406 = CARTESIAN_POINT ( 'NONE',  ( -4.999999999999999112, -53.91666666666667140, 2.886751345948131764 ) ) ;
#62407 = CARTESIAN_POINT ( 'NONE',  ( -5.000000000000000000, -41.08333333333333570, -2.886751345948128211 ) ) ;
#62408 = PLANE ( 'NONE',  #29394 ) ;
#62409 = VERTEX_POINT ( 'NONE', #31945 ) ;
#62410 = CARTESIAN_POINT ( 'NONE',  ( -6.972266317189433020E-16, -94.25000000000000000, -5.000000000000000000 ) ) ;
#62411 =( BOUNDED_CURVE ( )  B_SPLINE_CURVE ( 2, ( #22219, #27975, #17704, #37318, #18006, #52746, #42765, #37629, #57270 ),
 .UNSPECIFIED., .F., .F. ) 
 B_SPLINE_CURVE_WITH_KNOTS ( ( 3, 2, 2, 2, 3 ),
 ( 0.7187500000000000000, 0.7194444444444444420, 0.7208333333333333259, 0.7222222222222222099, 0.7229166666666666519 ),
 .UNSPECIFIED. ) 
 CURVE ( )  GEOMETRIC_REPRESENTATION_ITEM ( )  RATIONAL_B_SPLINE_CURVE ( ( 0.9330127018922194093, 0.9330127018922194093, 1.000000000000000000, 0.8660254037844387076, 1.000000000000000000, 0.8660254037844387076, 1.000000000000000000, 0.9330127018922194093, 0.9330127018922194093 ) ) 
 REPRESENTATION_ITEM ( '' )  );
#62412 = VECTOR ( 'NONE', #19779, 1000.000000000000000 ) ;
#62413 = CARTESIAN_POINT ( 'NONE',  ( -5.000000000000000000, 13.00000000000000178, 0.000000000000000000 ) ) ;
#62414 = CARTESIAN_POINT ( 'NONE',  ( 5.000000000000000000, -11.49999999999999645, -6.123233995736766282E-16 ) ) ;
#62415 = CARTESIAN_POINT ( 'NONE',  ( -3.152548672688508926E-16, -18.56249999863440792, -5.148502694627439702 ) ) ;
#62416 = VECTOR ( 'NONE', #8128, 1000.000000000000000 ) ;
#62417 = CARTESIAN_POINT ( 'NONE',  ( 4.458734125000000326, -77.89583333196773651, 2.574251347313718519 ) ) ;
#62418 = AXIS2_PLACEMENT_3D ( 'NONE', #35124, #49272, #49582 ) ;
#62419 = CARTESIAN_POINT ( 'NONE',  ( -2.499999999999996447, -5.833333333333336590, 4.330127018922195425 ) ) ;
#62420 = CARTESIAN_POINT ( 'NONE',  ( 1.060575238724906964E-15, -10.62499999726881583, 5.773502691896257311 ) ) ;
#62422 = VERTEX_POINT ( 'NONE', #12955 ) ;
#62421 = CARTESIAN_POINT ( 'NONE',  ( -4.458734124999999437, -46.31249999863440792, 0.000000000000000000 ) ) ;
#62423 = AXIS2_PLACEMENT_3D ( 'NONE', #54287, #15691, #54931 ) ;
#62424 = CARTESIAN_POINT ( 'NONE',  ( 5.000000000000000000, -144.0000000000000284, 0.000000000000000000 ) ) ;
#62426 = EDGE_LOOP ( 'NONE', ( #44514, #3651, #55178, #12880 ) ) ;
#62425 = CARTESIAN_POINT ( 'NONE',  ( 2.229367062500001939, 7.770833334698926009, 3.861377020970579999 ) ) ;
#62427 = FACE_OUTER_BOUND ( 'NONE', #30979, .T. ) ;
#62428 = CARTESIAN_POINT ( 'NONE',  ( -5.000000000000000000, -61.08333333333333570, -2.886751345948128211 ) ) ;
#62429 = CARTESIAN_POINT ( 'NONE',  ( -4.458734124999999437, -159.1875000013655779, -5.460374474430324690E-16 ) ) ;
#62430 = CARTESIAN_POINT ( 'NONE',  ( -3.152548672688508926E-16, -35.81249999863440792, -5.148502694627439702 ) ) ;
#62431 = DIRECTION ( 'NONE',  ( 0.000000000000000000, 0.000000000000000000, 1.000000000000000000 ) ) ;
#62432 = CARTESIAN_POINT ( 'NONE',  ( 5.000000000000000000, -167.0624999999999716, 2.071067811865478614 ) ) ;
#62433 = CARTESIAN_POINT ( 'NONE',  ( 1.339745962155615144, -11.70534180126147739, 4.999999999999999112 ) ) ;
#62434 = CARTESIAN_POINT ( 'NONE',  ( -59.59170313451811296, -131.7500000013656063, 1.485763867205729394 ) ) ;
#62435 = CARTESIAN_POINT ( 'NONE',  ( -4.458734124999998549, -7.479166665301073991, 2.574251347313722516 ) ) ;
#62436 = CARTESIAN_POINT ( 'NONE',  ( -3.152548672688508926E-16, -38.81249999863440081, -5.148502694627439702 ) ) ;
#62437 = CARTESIAN_POINT ( 'NONE',  ( 5.000000000000000000, -67.37499999726881583, -6.123233995736766282E-16 ) ) ;
#62438 = CARTESIAN_POINT ( 'NONE',  ( 9.457646018065525792E-16, -85.31249999863439371, 5.148502694627439702 ) ) ;
#62439 = DIRECTION ( 'NONE',  ( 0.000000000000000000, 1.000000000000000000, 0.000000000000000000 ) ) ;
#62440 = ORIENTED_EDGE ( 'NONE', *, *, #22, .F. ) ;
#62441 = CARTESIAN_POINT ( 'NONE',  ( 1.975475456537005874E-15, -9.624999997268814056, 5.000000000000000000 ) ) ;
#62442 =( BOUNDED_CURVE ( )  B_SPLINE_CURVE ( 2, ( #6166, #45394, #54734, #706, #1359, #35750, #59565, #54413, #5843 ),
 .UNSPECIFIED., .F., .F. ) 
 B_SPLINE_CURVE_WITH_KNOTS ( ( 3, 2, 2, 2, 3 ),
 ( 0.4517857142857142905, 0.4523809523809523836, 0.4535714285714285698, 0.4547619047619047561, 0.4553571428571428492 ),
 .UNSPECIFIED. ) 
 CURVE ( )  GEOMETRIC_REPRESENTATION_ITEM ( )  RATIONAL_B_SPLINE_CURVE ( ( 0.9330127018922194093, 0.9330127018922194093, 1.000000000000000000, 0.8660254037844387076, 1.000000000000000000, 0.8660254037844387076, 1.000000000000000000, 0.9330127018922194093, 0.9330127018922194093 ) ) 
 REPRESENTATION_ITEM ( '' )  );
#62443 = CARTESIAN_POINT ( 'NONE',  ( 1.339745962155612702, -2.169658196007333562, -5.000000000000000000 ) ) ;
#62444 = CARTESIAN_POINT ( 'NONE',  ( 4.458734124999999437, -68.06249999863440792, -5.460374474430324690E-16 ) ) ;
#62445 = CARTESIAN_POINT ( 'NONE',  ( 4.458734124999997661, -147.7500000013656063, 1.846868145590737864 ) ) ;
#62446 = ORIENTED_EDGE ( 'NONE', *, *, #6282, .T. ) ;
#62447 = CARTESIAN_POINT ( 'NONE',  ( -4.458734124999998549, -11.47916666530107044, 2.574251347313722516 ) ) ;
#62448 = CARTESIAN_POINT ( 'NONE',  ( -6.972266317189433020E-16, -79.12499999726881583, -5.000000000000000000 ) ) ;
#62449 = CARTESIAN_POINT ( 'NONE',  ( -2.229367062500000163, 1.520833334698927564, -3.861377020970580443 ) ) ;
#62450 = CARTESIAN_POINT ( 'NONE',  ( -1.339745962155613812, -12.08034179853029322, -5.000000000000000000 ) ) ;
#62451 = CARTESIAN_POINT ( 'NONE',  ( 1.846868145590736310, -152.6250000013655495, 4.458734124999997661 ) ) ;
#62452 = VECTOR ( 'NONE', #3368, 1000.000000000000000 ) ;
#62453 =( BOUNDED_CURVE ( )  B_SPLINE_CURVE ( 2, ( #10531, #15369, #49772, #40119, #34992, #5399, #30467, #60080, #25657 ),
 .UNSPECIFIED., .F., .F. ) 
 B_SPLINE_CURVE_WITH_KNOTS ( ( 3, 2, 2, 2, 3 ),
 ( 0.6895833333333333259, 0.6902777777777777679, 0.6916666666666666519, 0.6930555555555555358, 0.6937499999999999778 ),
 .UNSPECIFIED. ) 
 CURVE ( )  GEOMETRIC_REPRESENTATION_ITEM ( )  RATIONAL_B_SPLINE_CURVE ( ( 0.9330127018922194093, 0.9330127018922194093, 1.000000000000000000, 0.8660254037844387076, 1.000000000000000000, 0.8660254037844387076, 1.000000000000000000, 0.9330127018922194093, 0.9330127018922194093 ) ) 
 REPRESENTATION_ITEM ( '' )  );
#62454 = CARTESIAN_POINT ( 'NONE',  ( -2.229367062499996610, 24.60416666803225993, 3.861377020970582219 ) ) ;
#62455 = ORIENTED_EDGE ( 'NONE', *, *, #1642, .T. ) ;
#62456 = CARTESIAN_POINT ( 'NONE',  ( -4.458734124999999437, -91.31249999863440792, 0.000000000000000000 ) ) ;
#62457 = CARTESIAN_POINT ( 'NONE',  ( -2.500000000000000444, -31.16666666666666785, -4.330127018922193649 ) ) ;
#62458 = CARTESIAN_POINT ( 'NONE',  ( 5.000000000000000000, -60.29166666393547303, -2.886751345948130876 ) ) ;
#62459 = CARTESIAN_POINT ( 'NONE',  ( 2.229367062500001939, -6.979166665301073103, 3.861377020970579999 ) ) ;
#62460 = EDGE_CURVE ( 'NONE', #25400, #33613, #18467, .T. ) ;
#62461 = AXIS2_PLACEMENT_3D ( 'NONE', #43929, #216, #9835 ) ;
#62462 = CARTESIAN_POINT ( 'NONE',  ( 0.000000000000000000, -170.0000000000000000, 0.000000000000000000 ) ) ;
#62463 = CARTESIAN_POINT ( 'NONE',  ( -6.972266317189433020E-16, 8.875000002731184168, -5.000000000000000000 ) ) ;
#62464 = CARTESIAN_POINT ( 'NONE',  ( -51.75738570946856498, -141.7500000000000284, 3.805975901505576964 ) ) ;
#62465 = CARTESIAN_POINT ( 'NONE',  ( -2.499999999999996447, -36.70833333060213732, 4.330127018922195425 ) ) ;
#62466 = CARTESIAN_POINT ( 'NONE',  ( 5.000000000000000888, -64.45833333060213022, 2.886751345948126879 ) ) ;
#62467 = CARTESIAN_POINT ( 'NONE',  ( 9.457646018065525792E-16, 17.93750000136559208, 5.148502694627439702 ) ) ;
#62468 = CARTESIAN_POINT ( 'NONE',  ( 1.339745962155612702, -7.294658198738518173, -5.000000000000000000 ) ) ;
#62469 = CARTESIAN_POINT ( 'NONE',  ( 9.457646018065525792E-16, 22.93750000136559919, 5.148502694627439702 ) ) ;
#62470 = CARTESIAN_POINT ( 'NONE',  ( -2.229367062500000163, -54.47916666530107221, -3.861377020970580443 ) ) ;
#62471 = CARTESIAN_POINT ( 'NONE',  ( -4.458734124999999437, -2.645833331967738289, -2.574251347313719407 ) ) ;
#62472 = FACE_OUTER_BOUND ( 'NONE', #16938, .T. ) ;
#62473 = CARTESIAN_POINT ( 'NONE',  ( -5.000000000000000000, 11.00000000000000000, 0.000000000000000000 ) ) ;
#62474 = CARTESIAN_POINT ( 'NONE',  ( -5.000000000000000000, -139.6250000027312126, -6.123233995736766282E-16 ) ) ;
#62475 = CARTESIAN_POINT ( 'NONE',  ( 2.500000000000002220, -69.66666666666667140, 4.330127018922192761 ) ) ;
#62476 = CARTESIAN_POINT ( 'NONE',  ( -4.458734124999998549, -49.22916666530106511, 2.574251347313722516 ) ) ;
#62477 = CARTESIAN_POINT ( 'NONE',  ( 5.000000000000000000, -86.37499999726880162, -6.123233995736766282E-16 ) ) ;
#62478 = CARTESIAN_POINT ( 'NONE',  ( -56.48576386720575471, -138.0000000013656063, -4.591703134518078322 ) ) ;
#62479 = CARTESIAN_POINT ( 'NONE',  ( -5.000000000000000000, -17.08333333333333215, -2.886751345948128211 ) ) ;
#62480 = EDGE_CURVE ( 'NONE', #49290, #32825, #32579, .T. ) ;
#62481 = DIRECTION ( 'NONE',  ( -0.000000000000000000, 1.000000000000000000, -0.000000000000000000 ) ) ;
#62482 = EDGE_CURVE ( 'NONE', #53339, #25310, #61551, .T. ) ;
#62483 = CARTESIAN_POINT ( 'NONE',  ( -2.229367062499996610, -92.39583333196773651, 3.861377020970582219 ) ) ;
#62484 = CARTESIAN_POINT ( 'NONE',  ( -3.152801135295367985, -156.0625000013656063, 3.152801135295367096 ) ) ;
#62485 = CARTESIAN_POINT ( 'NONE',  ( 2.500000000000002220, -40.66666666666667140, 4.330127018922192761 ) ) ;
#62486 = PRESENTATION_STYLE_ASSIGNMENT (( #23229 ) ) ;
#62487 = EDGE_LOOP ( 'NONE', ( #53862, #40020, #20289, #39437 ) ) ;
#62488 = CARTESIAN_POINT ( 'NONE',  ( 4.458734124999998549, 17.02083333469892423, -2.574251347313721627 ) ) ;
#62489 = EDGE_LOOP ( 'NONE', ( #52915, #6187, #4969, #43185, #45228 ) ) ;
#62490 = CARTESIAN_POINT ( 'NONE',  ( 2.229367062500001939, -94.97916666530106511, 3.861377020970579999 ) ) ;
#62491 = CARTESIAN_POINT ( 'NONE',  ( -4.458734124999998549, 10.52083333469892779, 2.574251347313722516 ) ) ;
#62492 = CARTESIAN_POINT ( 'NONE',  ( 5.000000000000000888, 9.541666669397852019, 2.886751345948126879 ) ) ;
#62493 = CARTESIAN_POINT ( 'NONE',  ( -1.339745962155610925, -87.66965819600731891, 5.000000000000000000 ) ) ;
#62494 = CARTESIAN_POINT ( 'NONE',  ( -2.499999999999996447, 3.166666666666664742, 4.330127018922195425 ) ) ;
#62495 = EDGE_CURVE ( 'NONE', #30540, #32917, #29907, .T. ) ;
#62496 = CARTESIAN_POINT ( 'NONE',  ( -4.458734124999997661, -63.22916666530106511, 2.574251347313722516 ) ) ;
#62497 = FACE_OUTER_BOUND ( 'NONE', #63384, .T. ) ;
#62498 = CARTESIAN_POINT ( 'NONE',  ( -4.458734124999998549, -29.22916666530107221, 2.574251347313722516 ) ) ;
#62499 = CARTESIAN_POINT ( 'NONE',  ( -6.972266317189433020E-16, -40.12499999726880162, -5.000000000000000000 ) ) ;
#62500 = CARTESIAN_POINT ( 'NONE',  ( 5.000000000000000000, -63.50000000000000000, -6.123233995736766282E-16 ) ) ;
#62501 = CARTESIAN_POINT ( 'NONE',  ( -51.75738570946856498, -151.8750000027312126, 3.805975901505576964 ) ) ;
#62502 = CARTESIAN_POINT ( 'NONE',  ( 1.060575238724906964E-15, -42.75000000000000000, 5.773502691896257311 ) ) ;
#62504 = CARTESIAN_POINT ( 'NONE',  ( 4.458734125000001214, -20.14583333196774007, 2.574251347313718519 ) ) ;
#62503 = CARTESIAN_POINT ( 'NONE',  ( -4.999999999999998224, -89.79166666393547303, 2.886751345948131764 ) ) ;
#62505 = AXIS2_PLACEMENT_3D ( 'NONE', #13390, #38450, #63227 ) ;
#62506 = CARTESIAN_POINT ( 'NONE',  ( 3.535533905932738197, -154.8750000000000000, -3.535533905932738197 ) ) ;
#62507 = CARTESIAN_POINT ( 'NONE',  ( 9.457646018065525792E-16, -65.06249999863440792, 5.148502694627439702 ) ) ;
#62508 = CARTESIAN_POINT ( 'NONE',  ( 3.152801135295367541, -146.5625000013655779, -3.152801135295367541 ) ) ;
#62509 = CARTESIAN_POINT ( 'NONE',  ( 4.458734124999999437, -77.81249999863440792, -5.460374474430324690E-16 ) ) ;
#62510 = VECTOR ( 'NONE', #25765, 1000.000000000000114 ) ;
#62511 = CARTESIAN_POINT ( 'NONE',  ( -59.29741812935640155, -141.8750000013655779, -2.196230717870135685 ) ) ;
#62512 = CARTESIAN_POINT ( 'NONE',  ( 4.458734125000001214, -25.14583333196774007, 2.574251347313718519 ) ) ;
#62513 = CARTESIAN_POINT ( 'NONE',  ( -2.499999999999996447, -63.70833333060215153, 4.330127018922195425 ) ) ;
#62514 = ORIENTED_EDGE ( 'NONE', *, *, #13469, .F. ) ;
#62515 = EDGE_CURVE ( 'NONE', #63378, #6056, #56410, .T. ) ;
#62516 = CARTESIAN_POINT ( 'NONE',  ( -2.500000000000000444, -22.16666666666666785, -4.330127018922193649 ) ) ;
#62517 = VERTEX_POINT ( 'NONE', #52201 ) ;
#62518 = CARTESIAN_POINT ( 'NONE',  ( 4.458734125000001214, -66.14583333196772230, 2.574251347313718519 ) ) ;
#62519 = CARTESIAN_POINT ( 'NONE',  ( 7.897836333153806621, 1.530409084195003988, -7.633857274177628049 ) ) ;
#62520 = ORIENTED_EDGE ( 'NONE', *, *, #18800, .F. ) ;
#62521 = CYLINDRICAL_SURFACE ( 'NONE', #3466, 5.000000000000000000 ) ;
#62522 = CARTESIAN_POINT ( 'NONE',  ( 4.458734124999999437, -54.06249999863440081, -5.460374474430324690E-16 ) ) ;
#62523 = CARTESIAN_POINT ( 'NONE',  ( 4.458734124999998549, 3.020833334698928674, -2.574251347313721627 ) ) ;
#62524 = ORIENTED_EDGE ( 'NONE', *, *, #37079, .T. ) ;
#62525 = CARTESIAN_POINT ( 'NONE',  ( -6.972266317189433020E-16, -104.2500000000000000, -5.000000000000000000 ) ) ;
#62526 = CARTESIAN_POINT ( 'NONE',  ( 9.457646018065525792E-16, 3.937500001365595192, 5.148502694627439702 ) ) ;
#62527 = CARTESIAN_POINT ( 'NONE',  ( 2.229367062499998831, 16.35416666803225993, -3.861377020970580887 ) ) ;
#62528 = CARTESIAN_POINT ( 'NONE',  ( -50.70258187064364108, -143.1250000013656063, 2.196230717870141014 ) ) ;
#62529 = CARTESIAN_POINT ( 'NONE',  ( -6.972266317189433020E-16, -42.12499999726880873, -5.000000000000000000 ) ) ;
#62530 = CARTESIAN_POINT ( 'NONE',  ( -3.152801135295367985, -166.8125000013656063, 3.152801135295367096 ) ) ;
#62531 = VERTEX_POINT ( 'NONE', #3634 ) ;
#62532 = CARTESIAN_POINT ( 'NONE',  ( -4.458734124999997661, -75.22916666530106511, 2.574251347313722516 ) ) ;
#62533 = CARTESIAN_POINT ( 'NONE',  ( -4.458734124999999437, 7.604166668032259935, -2.574251347313719407 ) ) ;
#62534 = ADVANCED_FACE ( 'NONE', ( #17483 ), #23245, .T. ) ;
#62535 =( BOUNDED_CURVE ( )  B_SPLINE_CURVE ( 2, ( #29248, #54667, #9, #30205, #44362, #19609, #59498, #14776, #324 ),
 .UNSPECIFIED., .F., .F. ) 
 B_SPLINE_CURVE_WITH_KNOTS ( ( 3, 2, 2, 2, 3 ),
 ( 0.3062500000000000222, 0.3069444444444444642, 0.3083333333333333481, 0.3097222222222222321, 0.3104166666666666741 ),
 .UNSPECIFIED. ) 
 CURVE ( )  GEOMETRIC_REPRESENTATION_ITEM ( )  RATIONAL_B_SPLINE_CURVE ( ( 0.9330127018922194093, 0.9330127018922194093, 1.000000000000000000, 0.8660254037844387076, 1.000000000000000000, 0.8660254037844387076, 1.000000000000000000, 0.9330127018922194093, 0.9330127018922194093 ) ) 
 REPRESENTATION_ITEM ( '' )  );
#62536 = EDGE_CURVE ( 'NONE', #47780, #3809, #56627, .T. ) ;
#62537 = CARTESIAN_POINT ( 'NONE',  ( -1.339745962155613812, -89.20534180126146850, -5.000000000000000000 ) ) ;
#62538 = EDGE_CURVE ( 'NONE', #36403, #25339, #8153, .T. ) ;
#62539 = CARTESIAN_POINT ( 'NONE',  ( 4.458734124999998549, -57.97916666530107221, -2.574251347313721627 ) ) ;
#62540 = CARTESIAN_POINT ( 'NONE',  ( 1.060575238724906964E-15, -18.62499999726881583, 5.773502691896257311 ) ) ;
#62541 = CARTESIAN_POINT ( 'NONE',  ( -51.75738570946856498, -141.7500000000000284, 3.805975901505576964 ) ) ;
#62542 = LINE ( 'NONE', #13320, #57314 ) ;
#62543 = CARTESIAN_POINT ( 'NONE',  ( -51.75738570946856498, -140.8750000027312126, 3.805975901505576964 ) ) ;
#62544 = CARTESIAN_POINT ( 'NONE',  ( 5.000000000000000000, -18.29166666393547658, -2.886751345948130876 ) ) ;
#62545 = CARTESIAN_POINT ( 'NONE',  ( -51.19402409849444524, -146.5000000000000284, -3.242614290531456334 ) ) ;
#62546 = CARTESIAN_POINT ( 'NONE',  ( 2.229367062500001939, -38.97916666530107221, 3.861377020970579999 ) ) ;
#62547 = CARTESIAN_POINT ( 'NONE',  ( -2.229367062499996610, -26.39583333196774007, 3.861377020970582219 ) ) ;
#62548 = VECTOR ( 'NONE', #2685, 1000.000000000000000 ) ;
#62549 = CARTESIAN_POINT ( 'NONE',  ( -59.81910112700026616, -144.1875000000000000, -2.462841084822481541 ) ) ;
#62550 = CARTESIAN_POINT ( 'NONE',  ( 5.000000000000000000, 28.49999999999999645, -6.123233995736766282E-16 ) ) ;
#62551 = CARTESIAN_POINT ( 'NONE',  ( 5.000000000000000000, -152.1250000027312126, 0.000000000000000000 ) ) ;
#62552 = ORIENTED_EDGE ( 'NONE', *, *, #6078, .F. ) ;
#62553 = CARTESIAN_POINT ( 'NONE',  ( -4.458734124999998549, -31.22916666530107221, 2.574251347313722516 ) ) ;
#62554 = CARTESIAN_POINT ( 'NONE',  ( -2.499999999999996447, -65.70833333060213022, 4.330127018922195425 ) ) ;
#62555 = EDGE_CURVE ( 'NONE', #39254, #39875, #51733, .T. ) ;
#62556 = CARTESIAN_POINT ( 'NONE',  ( -51.60603307380591787, -149.1875000013656063, -2.891590998281053704 ) ) ;
#62557 = CARTESIAN_POINT ( 'NONE',  ( -2.071067811865475061, -142.6875000000000568, -5.000000000000000888 ) ) ;
#62558 = CARTESIAN_POINT ( 'NONE',  ( -4.458734124999999437, -26.31249999863440792, 0.000000000000000000 ) ) ;
#62559 = ADVANCED_FACE ( 'NONE', ( #38966 ), #44107, .T. ) ;
#62560 = CARTESIAN_POINT ( 'NONE',  ( 4.458734125000000326, -77.14583333196775072, 2.574251347313718519 ) ) ;
#62561 = CARTESIAN_POINT ( 'NONE',  ( -8.190561711645485556E-16, -168.9375000013656063, 4.458734124999999437 ) ) ;
#62562 = CARTESIAN_POINT ( 'NONE',  ( -2.229367062499996610, -32.14583333196773651, 3.861377020970582219 ) ) ;
#62563 = CARTESIAN_POINT ( 'NONE',  ( -53.33387254593723981, -147.8125000000000284, 5.149110718188528502 ) ) ;
#62564 = CARTESIAN_POINT ( 'NONE',  ( 0.000000000000000000, -170.0000000000000000, 5.000000000000000000 ) ) ;
#62565 = CARTESIAN_POINT ( 'NONE',  ( -2.500000000000000444, -15.16666666666666785, -4.330127018922193649 ) ) ;
#62566 = CARTESIAN_POINT ( 'NONE',  ( 4.458734124999999437, -146.5000000013656347, 1.846868145590737864 ) ) ;
#62567 = VERTEX_POINT ( 'NONE', #14208 ) ;
#62568 = CARTESIAN_POINT ( 'NONE',  ( -58.24261429053147765, -153.2500000000000284, -3.805975901505573855 ) ) ;
#62569 = CARTESIAN_POINT ( 'NONE',  ( 4.458734124999998549, -55.97916666530107932, -2.574251347313721627 ) ) ;
#62570 = CARTESIAN_POINT ( 'NONE',  ( -5.000000000000000000, 25.12500000273118417, 0.000000000000000000 ) ) ;
#62571 = CARTESIAN_POINT ( 'NONE',  ( 1.339745962155615144, -81.58034179853029855, 4.999999999999999112 ) ) ;
#62572 = CARTESIAN_POINT ( 'NONE',  ( 1.060575238724906964E-15, 20.24999999999999645, 5.773502691896257311 ) ) ;
#62573 = AXIS2_PLACEMENT_3D ( 'NONE', #38104, #43535, #23631 ) ;
#62574 = CARTESIAN_POINT ( 'NONE',  ( 0.000000000000000000, -120.0000000000000000, 0.000000000000000000 ) ) ;
#62575 = CARTESIAN_POINT ( 'NONE',  ( -4.458734124999999437, -2.395833331967737845, -2.574251347313719407 ) ) ;
#62576 = CARTESIAN_POINT ( 'NONE',  ( 2.071067811865392461, -141.1875000000000284, 5.000000000000084377 ) ) ;
#62577 = CARTESIAN_POINT ( 'NONE',  ( 9.457646018065525792E-16, 10.68750000136559386, 5.148502694627439702 ) ) ;
#62578 = DIRECTION ( 'NONE',  ( -0.000000000000000000, 1.000000000000000000, -0.000000000000000000 ) ) ;
#62579 = ORIENTED_EDGE ( 'NONE', *, *, #37160, .F. ) ;
#62580 = CARTESIAN_POINT ( 'NONE',  ( 3.535533905932738197, -168.0000000027312126, -3.535533905932738197 ) ) ;
#62581 = CARTESIAN_POINT ( 'NONE',  ( 9.457646018065525792E-16, -48.06249999863440081, 5.148502694627439702 ) ) ;
#62582 = CARTESIAN_POINT ( 'NONE',  ( 4.458734124999999437, -161.6875000013655779, 0.000000000000000000 ) ) ;
#62583 = CARTESIAN_POINT ( 'NONE',  ( 5.000000000000000888, -48.45833333060215153, 2.886751345948126879 ) ) ;
#62584 = ORIENTED_EDGE ( 'NONE', *, *, #60320, .T. ) ;
#62585 = CARTESIAN_POINT ( 'NONE',  ( 4.458734124999998549, -20.72916666530106866, -2.574251347313721627 ) ) ;
#62586 = VERTEX_POINT ( 'NONE', #63437 ) ;
#62587 =( BOUNDED_CURVE ( )  B_SPLINE_CURVE ( 2, ( #7185, #55112, #15559, #15874, #40626, #25517, #30976, #46413, #31614 ),
 .UNSPECIFIED., .F., .F. ) 
 B_SPLINE_CURVE_WITH_KNOTS ( ( 3, 2, 2, 2, 3 ),
 ( 0.1089285714285714302, 0.1095238095238095233, 0.1107142857142857095, 0.1119047619047619097, 0.1125000000000000028 ),
 .UNSPECIFIED. ) 
 CURVE ( )  GEOMETRIC_REPRESENTATION_ITEM ( )  RATIONAL_B_SPLINE_CURVE ( ( 0.9330127018922194093, 0.9330127018922194093, 1.000000000000000000, 0.8660254037844387076, 1.000000000000000000, 0.8660254037844387076, 1.000000000000000000, 0.9330127018922194093, 0.9330127018922194093 ) ) 
 REPRESENTATION_ITEM ( '' )  );
#62589 = DIRECTION ( 'NONE',  ( 0.000000000000000000, 0.000000000000000000, -1.000000000000000000 ) ) ;
#62588 = CARTESIAN_POINT ( 'NONE',  ( -7.500000000000001776, 0.000000000000000000, 0.000000000000000000 ) ) ;
#62590 = CARTESIAN_POINT ( 'NONE',  ( 4.458734124999999437, -161.4375000013655779, 0.000000000000000000 ) ) ;
#62591 = ORIENTED_EDGE ( 'NONE', *, *, #43698, .F. ) ;
#62592 = AXIS2_PLACEMENT_3D ( 'NONE', #62826, #17805, #57993 ) ;
#62593 = CARTESIAN_POINT ( 'NONE',  ( 1.975475456537005874E-15, -43.62499999726880873, 5.000000000000000000 ) ) ;
#62594 = CARTESIAN_POINT ( 'NONE',  ( -55.39835681537999790, -133.8750000000000284, 4.984105922594378235 ) ) ;
#62595 = CARTESIAN_POINT ( 'NONE',  ( 4.458734125000001214, -36.14583333196773651, 2.574251347313718519 ) ) ;
#62596 = ORIENTED_EDGE ( 'NONE', *, *, #58233, .F. ) ;
#62597 = CARTESIAN_POINT ( 'NONE',  ( 4.458734125000001214, -81.89583333196773651, 2.574251347313718519 ) ) ;
#62598 = CARTESIAN_POINT ( 'NONE',  ( -4.458734124999999437, 18.60416666803225993, -2.574251347313719407 ) ) ;
#62599 = CARTESIAN_POINT ( 'NONE',  ( -4.999999999999998224, -17.79166666393547658, 2.886751345948131764 ) ) ;
#62600 = ORIENTED_EDGE ( 'NONE', *, *, #24677, .T. ) ;
#62601 = CARTESIAN_POINT ( 'NONE',  ( -59.29741812935640155, -137.8750000013655779, -2.196230717870135685 ) ) ;
#62602 = CARTESIAN_POINT ( 'NONE',  ( -4.458734124999999437, -85.64583333196773651, -2.574251347313719407 ) ) ;
#62603 = CARTESIAN_POINT ( 'NONE',  ( -58.24261429053147765, -128.3750000027312126, -3.805975901505573855 ) ) ;
#62604 = CARTESIAN_POINT ( 'NONE',  ( 5.000000000000000000, -4.291666663935479242, -2.886751345948130876 ) ) ;
#62605 = CARTESIAN_POINT ( 'NONE',  ( 1.339745962155612702, -9.294658198738520838, -5.000000000000000000 ) ) ;
#62606 = CARTESIAN_POINT ( 'NONE',  ( -5.000000000000000000, -46.95833333060214443, -2.886751345948128211 ) ) ;
#62607 = CARTESIAN_POINT ( 'NONE',  ( 4.458734124999998549, -57.72916666530107932, -2.574251347313721627 ) ) ;
#62608 = CARTESIAN_POINT ( 'NONE',  ( -4.999999999999998224, -84.79166666393547303, 2.886751345948131764 ) ) ;
#62609 = CARTESIAN_POINT ( 'NONE',  ( -4.458734124999999437, 24.60416666803225993, -2.574251347313719407 ) ) ;
#62610 = CARTESIAN_POINT ( 'NONE',  ( 2.500000000000002220, -42.66666666666667140, 4.330127018922192761 ) ) ;
#62611 = CARTESIAN_POINT ( 'NONE',  ( -6.972266317189433020E-16, -16.12499999726881228, -5.000000000000000000 ) ) ;
#62612 = EDGE_CURVE ( 'NONE', #27799, #53636, #34049, .T. ) ;
#62613 = CARTESIAN_POINT ( 'NONE',  ( 2.229367062499998831, -43.89583333196774362, -3.861377020970580887 ) ) ;
#62614 = CARTESIAN_POINT ( 'NONE',  ( 5.000000000000000888, -5.458333330602148870, 2.886751345948126879 ) ) ;
#62615 = CARTESIAN_POINT ( 'NONE',  ( -53.33387254593731086, -153.8125000000000284, 5.149110718188520508 ) ) ;
#62616 = DIRECTION ( 'NONE',  ( 0.8660254037844381525, -0.5000000000000007772, 0.000000000000000000 ) ) ;
#62617 = CARTESIAN_POINT ( 'NONE',  ( 4.458734124999999437, -83.06249999863440792, -5.460374474430324690E-16 ) ) ;
#62618 = CARTESIAN_POINT ( 'NONE',  ( 4.458734124999999437, -100.8124999986344079, -5.460374474430324690E-16 ) ) ;
#62619 = CARTESIAN_POINT ( 'NONE',  ( -2.229367062499996610, -13.39583333196774007, 3.861377020970582219 ) ) ;
#62621 = ORIENTED_EDGE ( 'NONE', *, *, #61924, .T. ) ;
#62620 = EDGE_CURVE ( 'NONE', #32199, #32996, #25412, .T. ) ;
#62622 = CARTESIAN_POINT ( 'NONE',  ( -2.499999999999996447, 18.29166666939785202, 4.330127018922195425 ) ) ;
#62623 = CARTESIAN_POINT ( 'NONE',  ( -4.458734124999999437, -100.3124999986344079, 0.000000000000000000 ) ) ;
#62624 = CARTESIAN_POINT ( 'NONE',  ( -2.071067811865478170, -166.4375000027311842, 5.000000000000000000 ) ) ;
#62625 = CARTESIAN_POINT ( 'NONE',  ( 9.457646018065525792E-16, -93.31249999863439371, 5.148502694627439702 ) ) ;
#62627 = ADVANCED_FACE ( 'NONE', ( #10021 ), #5203, .T. ) ;
#62626 = CARTESIAN_POINT ( 'NONE',  ( 1.060575238724906964E-15, -53.62499999726880873, 5.773502691896257311 ) ) ;
#62628 = CARTESIAN_POINT ( 'NONE',  ( -1.339745962155610925, 19.33034180399266688, 5.000000000000000000 ) ) ;
#62629 = CARTESIAN_POINT ( 'NONE',  ( -59.44456063193725015, -128.5625000013656063, -0.3552334253322034230 ) ) ;
#62630 = CARTESIAN_POINT ( 'NONE',  ( -4.458734124999999437, -12.39583333196774184, -2.574251347313719407 ) ) ;
#62631 = CARTESIAN_POINT ( 'NONE',  ( -3.152548672688508926E-16, 9.187500001365593860, -5.148502694627439702 ) ) ;
#62632 = CARTESIAN_POINT ( 'NONE',  ( 4.458734124999998549, -56.97916666530107932, -2.574251347313721627 ) ) ;
#62633 = CARTESIAN_POINT ( 'NONE',  ( -5.000000000000000000, -68.99999999999998579, 0.000000000000000000 ) ) ;
#62634 = CARTESIAN_POINT ( 'NONE',  ( -1.339745962155669101, -36.79465819873851729, 4.999999999999966249 ) ) ;
#62635 = CARTESIAN_POINT ( 'NONE',  ( -2.229367062499996610, -15.14583333196773474, 3.861377020970582219 ) ) ;
#62636 = LINE ( 'NONE', #53592, #42181 ) ;
#62637 = EDGE_CURVE ( 'NONE', #4115, #44744, #29304, .T. ) ;
#62638 = ORIENTED_EDGE ( 'NONE', *, *, #32539, .T. ) ;
#62639 = CARTESIAN_POINT ( 'NONE',  ( -4.458734124999999437, -41.64583333196773651, -2.574251347313719407 ) ) ;
#62640 =( BOUNDED_CURVE ( )  B_SPLINE_CURVE ( 2, ( #44959, #4444, #920, #40123, #24073, #43669, #19232, #9586, #29192 ),
 .UNSPECIFIED., .F., .F. ) 
 B_SPLINE_CURVE_WITH_KNOTS ( ( 3, 2, 2, 2, 3 ),
 ( 0.2479166666666666741, 0.2486111111111111160, 0.2500000000000000000, 0.2513888888888888840, 0.2520833333333333259 ),
 .UNSPECIFIED. ) 
 CURVE ( )  GEOMETRIC_REPRESENTATION_ITEM ( )  RATIONAL_B_SPLINE_CURVE ( ( 0.9330127018922194093, 0.9330127018922194093, 1.000000000000000000, 0.8660254037844387076, 1.000000000000000000, 0.8660254037844387076, 1.000000000000000000, 0.9330127018922194093, 0.9330127018922194093 ) ) 
 REPRESENTATION_ITEM ( '' )  );
#62641 = CARTESIAN_POINT ( 'NONE',  ( -57.19623071787017210, -125.6250000013656205, 4.297418129356382899 ) ) ;
#62642 = EDGE_CURVE ( 'NONE', #41, #24503, #49271, .T. ) ;
#62643 = CARTESIAN_POINT ( 'NONE',  ( 2.499999999999998668, 0.7916666693978530178, -4.330127018922193649 ) ) ;
#62644 = CARTESIAN_POINT ( 'NONE',  ( -0.6511518506208974211, 8.763486134561267349, -7.907570769506047981 ) ) ;
#62645 = CARTESIAN_POINT ( 'NONE',  ( 4.458734124999999437, -85.81249999863439371, -5.460374474430324690E-16 ) ) ;
#62646 = CARTESIAN_POINT ( 'NONE',  ( 2.229367062499998831, 23.10416666803225993, -3.861377020970580887 ) ) ;
#62647 = CARTESIAN_POINT ( 'NONE',  ( -4.458734124999999437, 14.60416666803226171, -2.574251347313719407 ) ) ;
#62648 = EDGE_CURVE ( 'NONE', #63287, #57225, #4882, .T. ) ;
#62649 = CARTESIAN_POINT ( 'NONE',  ( -5.000000000000000000, 6.916666666666664298, -2.886751345948128211 ) ) ;
#62650 = DIRECTION ( 'NONE',  ( 0.000000000000000000, 0.000000000000000000, 1.000000000000000000 ) ) ;
#62651 = CARTESIAN_POINT ( 'NONE',  ( 2.229367062500001939, -90.22916666530106511, 3.861377020970579999 ) ) ;
#62652 = CARTESIAN_POINT ( 'NONE',  ( -2.500000000000000444, -71.16666666666667140, -4.330127018922193649 ) ) ;
#62653 = CARTESIAN_POINT ( 'NONE',  ( 5.000000000000000888, 11.54166666939785202, 2.886751345948126879 ) ) ;
#62654 = VERTEX_POINT ( 'NONE', #10655 ) ;
#62655 = CYLINDRICAL_SURFACE ( 'NONE', #28369, 5.000000000000000000 ) ;
#62657 = CARTESIAN_POINT ( 'NONE',  ( -5.000000000000000000, -26.99999999999999645, 0.000000000000000000 ) ) ;
#62656 = DIRECTION ( 'NONE',  ( -0.000000000000000000, 0.000000000000000000, 1.000000000000000000 ) ) ;
#62658 = CARTESIAN_POINT ( 'NONE',  ( -4.458734124999998549, -35.22916666530107221, 2.574251347313722516 ) ) ;
#62659 = CARTESIAN_POINT ( 'NONE',  ( 2.500000000000002220, -35.54166666393547303, 4.330127018922192761 ) ) ;
#62661 = ORIENTED_EDGE ( 'NONE', *, *, #36943, .F. ) ;
#62660 = CARTESIAN_POINT ( 'NONE',  ( 4.458734124999998549, -60.72916666530106511, -2.574251347313721627 ) ) ;
#62662 = CARTESIAN_POINT ( 'NONE',  ( -50.40829686548195099, -150.2500000013656063, -1.485763867205728284 ) ) ;
#62664 = ORIENTED_EDGE ( 'NONE', *, *, #16065, .F. ) ;
#62663 = CARTESIAN_POINT ( 'NONE',  ( 9.457646018065525792E-16, -9.312499998634406140, 5.148502694627439702 ) ) ;
#62665 = CARTESIAN_POINT ( 'NONE',  ( -4.999999999999999112, -75.91666666666667140, 2.886751345948131764 ) ) ;
#62666 = CARTESIAN_POINT ( 'NONE',  ( -52.80376928212989185, -135.8750000013655779, -4.297418129356378458 ) ) ;
#62667 = CARTESIAN_POINT ( 'NONE',  ( -2.229367062499996610, -55.39583333196773651, 3.861377020970582219 ) ) ;
#62668 = CARTESIAN_POINT ( 'NONE',  ( 2.499999999999998668, -75.20833333060214443, -4.330127018922193649 ) ) ;
#62670 = ORIENTED_EDGE ( 'NONE', *, *, #18867, .T. ) ;
#62669 = CARTESIAN_POINT ( 'NONE',  ( -6.972266317189433020E-16, -106.1249999972688016, -5.000000000000000000 ) ) ;
#62671 = CARTESIAN_POINT ( 'NONE',  ( -50.01589407740564042, -147.6250000000000284, 0.3983568153799778022 ) ) ;
#62672 = CARTESIAN_POINT ( 'NONE',  ( 4.458734124999999437, -20.06249999863440081, -5.460374474430324690E-16 ) ) ;
#62674 = ORIENTED_EDGE ( 'NONE', *, *, #9608, .F. ) ;
#62673 = CARTESIAN_POINT ( 'NONE',  ( 9.457646018065525792E-16, -56.31249999863440081, 5.148502694627439702 ) ) ;
#62675 = FILL_AREA_STYLE ('',( #42714 ) ) ;
#62676 = CARTESIAN_POINT ( 'NONE',  ( 4.458734124999999437, -165.7500000013655495, 1.846868145590737864 ) ) ;
#62677 = CARTESIAN_POINT ( 'NONE',  ( -4.458734124999998549, -99.47916666530105090, 2.574251347313722516 ) ) ;
#62678 = CARTESIAN_POINT ( 'NONE',  ( 2.500000000000002220, -50.54166666393547303, 4.330127018922192761 ) ) ;
#62679 = ORIENTED_EDGE ( 'NONE', *, *, #7242, .F. ) ;
#62680 = CARTESIAN_POINT ( 'NONE',  ( -54.64476657466781973, -152.0625000013656063, -4.444560631937228834 ) ) ;
#62681 = CARTESIAN_POINT ( 'NONE',  ( -53.33387254593733928, -136.9375000027312126, 5.149110718188519620 ) ) ;
#62682 = CARTESIAN_POINT ( 'NONE',  ( 2.500000000000002220, -83.66666666666667140, 4.330127018922192761 ) ) ;
#62683 = VECTOR ( 'NONE', #19502, 1000.000000000000000 ) ;
#62684 = CARTESIAN_POINT ( 'NONE',  ( -2.229367062499996610, -10.14583333196773829, 3.861377020970582219 ) ) ;
#62685 = CARTESIAN_POINT ( 'NONE',  ( 2.229367062499998831, -98.89583333196773651, -3.861377020970580887 ) ) ;
#62686 = CARTESIAN_POINT ( 'NONE',  ( -3.152801135295367096, -144.3125000013655779, -3.152801135295367541 ) ) ;
#62687 = CARTESIAN_POINT ( 'NONE',  ( 2.229367062500001939, -30.22916666530107221, 3.861377020970579999 ) ) ;
#62688 = CARTESIAN_POINT ( 'NONE',  ( -56.66612745406293783, -139.4375000027311842, -5.149110718188535607 ) ) ;
#62689 = CARTESIAN_POINT ( 'NONE',  ( -59.59170313451811296, -137.5000000013656063, 1.485763867205729394 ) ) ;
#62690 = CARTESIAN_POINT ( 'NONE',  ( 2.229367062500001939, -69.22916666530107932, 3.861377020970579999 ) ) ;
#62691 = DIRECTION ( 'NONE',  ( 0.000000000000000000, 0.000000000000000000, 1.000000000000000000 ) ) ;
#62692 = CARTESIAN_POINT ( 'NONE',  ( 1.339745962155612702, -68.29465819873851729, -5.000000000000000000 ) ) ;
#62693 = CARTESIAN_POINT ( 'NONE',  ( 2.229367062499998831, 7.104166668032259935, -3.861377020970580887 ) ) ;
#62694 = VERTEX_POINT ( 'NONE', #15497 ) ;
#62695 = CARTESIAN_POINT ( 'NONE',  ( -5.000000000000000000, 1.916666666666667407, -2.886751345948128211 ) ) ;
#62696 = CARTESIAN_POINT ( 'NONE',  ( -6.972266317189433020E-16, 2.750000000000000000, -5.000000000000000000 ) ) ;
#62698 = CARTESIAN_POINT ( 'NONE',  ( 2.229367062499998831, -27.64583333196774007, -3.861377020970580887 ) ) ;
#62697 = CARTESIAN_POINT ( 'NONE',  ( -4.999999999999999112, -89.91666666666665719, 2.886751345948131764 ) ) ;
#62699 = CARTESIAN_POINT ( 'NONE',  ( -1.339745962155610925, -76.66965819600731891, 5.000000000000000000 ) ) ;
#62700 = CARTESIAN_POINT ( 'NONE',  ( 4.458734124999998549, -75.97916666530106511, -2.574251347313721627 ) ) ;
#62701 = CARTESIAN_POINT ( 'NONE',  ( -4.458734124999997661, 24.52083333469892779, 2.574251347313722516 ) ) ;
#62702 = CARTESIAN_POINT ( 'NONE',  ( 0.000000000000000000, -120.0000000000000000, 5.000000000000000000 ) ) ;
#62703 = CARTESIAN_POINT ( 'NONE',  ( -53.51423613279429503, -143.2500000013656063, 4.591703134518082763 ) ) ;
#62704 = CARTESIAN_POINT ( 'NONE',  ( -4.458734124999999437, 0.6041666680322611560, -2.574251347313719407 ) ) ;
#62705 = CARTESIAN_POINT ( 'NONE',  ( -2.229367062500000163, 26.27083333469892779, -3.861377020970580443 ) ) ;
#62706 = CARTESIAN_POINT ( 'NONE',  ( 4.458734125000000326, -40.14583333196773651, 2.574251347313718519 ) ) ;
#62707 = CARTESIAN_POINT ( 'NONE',  ( 1.339745962155612702, -80.29465819873850307, -5.000000000000000000 ) ) ;
#62708 = CARTESIAN_POINT ( 'NONE',  ( -4.458734124999997661, 2.770833334698928674, 2.574251347313722516 ) ) ;
#62709 = CARTESIAN_POINT ( 'NONE',  ( -4.458734124999999437, -22.64583333196773651, -2.574251347313719407 ) ) ;
#62710 = CARTESIAN_POINT ( 'NONE',  ( 2.730187237215162345E-16, -154.1875000013656063, -4.458734124999999437 ) ) ;
#62711 = CARTESIAN_POINT ( 'NONE',  ( -2.229367062499996610, -68.14583333196773651, 3.861377020970582219 ) ) ;
#62712 = CARTESIAN_POINT ( 'NONE',  ( -3.535250795749689387E-16, -100.1249999972688158, -5.773502691896257311 ) ) ;
#62713 =( BOUNDED_CURVE ( )  B_SPLINE_CURVE ( 2, ( #24274, #63210, #9171, #168, #40015, #53551, #14935, #20086, #49676 ),
 .UNSPECIFIED., .F., .F. ) 
 B_SPLINE_CURVE_WITH_KNOTS ( ( 3, 2, 2, 2, 3 ),
 ( 0.9687500000000000000, 0.9694444444444444420, 0.9708333333333333259, 0.9722222222222222099, 0.9729166666666666519 ),
 .UNSPECIFIED. ) 
 CURVE ( )  GEOMETRIC_REPRESENTATION_ITEM ( )  RATIONAL_B_SPLINE_CURVE ( ( 0.9330127018922194093, 0.9330127018922194093, 1.000000000000000000, 0.8660254037844387076, 1.000000000000000000, 0.8660254037844387076, 1.000000000000000000, 0.9330127018922194093, 0.9330127018922194093 ) ) 
 REPRESENTATION_ITEM ( '' )  );
#62714 = CARTESIAN_POINT ( 'NONE',  ( -2.498395430326213474E-14, 15.25000000000000000, 5.000000000000000000 ) ) ;
#62715 = CARTESIAN_POINT ( 'NONE',  ( 1.975475456537005874E-15, 9.375000002731185944, 5.000000000000000000 ) ) ;
#62716 = CARTESIAN_POINT ( 'NONE',  ( -4.458734124999999437, -106.6458333319677365, -2.574251347313719407 ) ) ;
#62717 = CARTESIAN_POINT ( 'NONE',  ( 2.229367062500001939, -66.22916666530106511, 3.861377020970579999 ) ) ;
#62718 = CARTESIAN_POINT ( 'NONE',  ( -5.000000000000000000, -54.08333333333332860, -2.886751345948128211 ) ) ;
#62719 = CARTESIAN_POINT ( 'NONE',  ( -4.999999999999998224, -65.79166666393547303, 2.886751345948131764 ) ) ;
#62720 = CARTESIAN_POINT ( 'NONE',  ( 1.060575238724906964E-15, 27.37500000273118062, 5.773502691896257311 ) ) ;
#62721 = ORIENTED_EDGE ( 'NONE', *, *, #43698, .T. ) ;
#62722 = LINE ( 'NONE', #23159, #19127 ) ;
#62723 = COLOUR_RGB ( '',0.8941176470588234615, 0.8941176470588234615, 0.8941176470588234615 ) ;
#62724 = CARTESIAN_POINT ( 'NONE',  ( -6.972266317189433020E-16, -97.12499999726880162, -5.000000000000000000 ) ) ;
#62725 = CARTESIAN_POINT ( 'NONE',  ( 1.060575238724906964E-15, -11.74999999999999467, 5.773502691896257311 ) ) ;
#62726 = CARTESIAN_POINT ( 'NONE',  ( -2.229367062499996610, -15.14583333196773474, 3.861377020970582219 ) ) ;
#62727 = AXIS2_PLACEMENT_3D ( 'NONE', #25605, #15953, #21744 ) ;
#62728 = CARTESIAN_POINT ( 'NONE',  ( -2.229367062499996610, -80.14583333196773651, 3.861377020970582219 ) ) ;
#62730 = CARTESIAN_POINT ( 'NONE',  ( -4.458734125000001214, -168.1250000013656063, 1.846868145590734089 ) ) ;
#62729 =( BOUNDED_CURVE ( )  B_SPLINE_CURVE ( 2, ( #57288, #7444, #2309, #61162, #17085, #13204, #36705, #42155, #27052 ),
 .UNSPECIFIED., .F., .F. ) 
 B_SPLINE_CURVE_WITH_KNOTS ( ( 3, 2, 2, 2, 3 ),
 ( 0.9270833333333333703, 0.9277777777777778123, 0.9291666666666666963, 0.9305555555555555802, 0.9312500000000000222 ),
 .UNSPECIFIED. ) 
 CURVE ( )  GEOMETRIC_REPRESENTATION_ITEM ( )  RATIONAL_B_SPLINE_CURVE ( ( 0.9330127018922194093, 0.9330127018922194093, 1.000000000000000000, 0.8660254037844387076, 1.000000000000000000, 0.8660254037844387076, 1.000000000000000000, 0.9330127018922194093, 0.9330127018922194093 ) ) 
 REPRESENTATION_ITEM ( '' )  );
#62731 = CARTESIAN_POINT ( 'NONE',  ( -5.000000000000000000, -17.87499999726881583, 0.000000000000000000 ) ) ;
#62733 = ORIENTED_EDGE ( 'NONE', *, *, #57831, .T. ) ;
#62732 = CARTESIAN_POINT ( 'NONE',  ( -3.152548672688508926E-16, -44.56249999863440081, -5.148502694627439702 ) ) ;
#62734 = CARTESIAN_POINT ( 'NONE',  ( 2.500000000000002220, -45.54166666393547303, 4.330127018922192761 ) ) ;
#62736 = ORIENTED_EDGE ( 'NONE', *, *, #21575, .T. ) ;
#62735 = CARTESIAN_POINT ( 'NONE',  ( 4.458734124999999437, 6.937500001365594748, -5.460374474430324690E-16 ) ) ;
#62737 = CARTESIAN_POINT ( 'NONE',  ( -58.39396692619412477, -152.4375000013656063, 2.891590998281057701 ) ) ;
#62738 = CARTESIAN_POINT ( 'NONE',  ( 5.000000000000000000, -58.50000000000000000, -6.123233995736766282E-16 ) ) ;
#62739 = CARTESIAN_POINT ( 'NONE',  ( 1.846868145590735200, -155.5000000013655779, -4.458734125000000326 ) ) ;
#62740 = CARTESIAN_POINT ( 'NONE',  ( -4.458734124999999437, -38.56249999863440081, 0.000000000000000000 ) ) ;
#62741 = CARTESIAN_POINT ( 'NONE',  ( -6.972266317189433020E-16, -101.2499999999999858, -5.000000000000000000 ) ) ;
#62742 = CARTESIAN_POINT ( 'NONE',  ( -3.535533905932737309, -166.6250000000000284, -3.535533905932738197 ) ) ;
#62743 = VECTOR ( 'NONE', #37434, 1000.000000000000000 ) ;
#62744 = CARTESIAN_POINT ( 'NONE',  ( -2.229367062499996610, -90.14583333196773651, 3.861377020970582219 ) ) ;
#62745 = CARTESIAN_POINT ( 'NONE',  ( -51.60603307380591787, -133.1875000013656063, -2.891590998281053704 ) ) ;
#62746 = CARTESIAN_POINT ( 'NONE',  ( 2.229367062499998831, -4.895833331967740065, -3.861377020970580887 ) ) ;
#62747 = CARTESIAN_POINT ( 'NONE',  ( 9.457646018065525792E-16, -39.31249999863439371, 5.148502694627439702 ) ) ;
#62748 = CARTESIAN_POINT ( 'NONE',  ( 1.339745962155612702, -54.29465819873851729, -5.000000000000000000 ) ) ;
#62749 = CARTESIAN_POINT ( 'NONE',  ( -4.458734125000001214, -149.8750000013655779, 1.846868145590734089 ) ) ;
#62750 = CARTESIAN_POINT ( 'NONE',  ( 4.458734124999998549, -82.97916666530107932, -2.574251347313721627 ) ) ;
#62751 = CARTESIAN_POINT ( 'NONE',  ( -6.972266317189433020E-16, -34.12499999726881583, -5.000000000000000000 ) ) ;
#62752 = ORIENTED_EDGE ( 'NONE', *, *, #47992, .T. ) ;
#62753 = CARTESIAN_POINT ( 'NONE',  ( -2.500000000000000444, -95.04166666393547303, -4.330127018922193649 ) ) ;
#62754 = CARTESIAN_POINT ( 'NONE',  ( 0.000000000000000000, -170.0000000000000000, 0.000000000000000000 ) ) ;
#62755 = CARTESIAN_POINT ( 'NONE',  ( 4.458734124999999437, -73.06249999863439371, -5.460374474430324690E-16 ) ) ;
#62756 = ORIENTED_EDGE ( 'NONE', *, *, #60430, .T. ) ;
#62757 = CARTESIAN_POINT ( 'NONE',  ( 2.499999999999998668, -78.33333333333332860, -4.330127018922193649 ) ) ;
#62758 = CARTESIAN_POINT ( 'NONE',  ( 4.458734124999998549, -10.97916666530107044, -2.574251347313721627 ) ) ;
#62759 = CARTESIAN_POINT ( 'NONE',  ( 5.000000000000000888, -79.45833333060213022, 2.886751345948126879 ) ) ;
#62760 = CARTESIAN_POINT ( 'NONE',  ( 2.229367062499998831, 2.354166668032262599, -3.861377020970580887 ) ) ;
#62761 = CARTESIAN_POINT ( 'NONE',  ( 2.500000000000002220, -77.54166666393547303, 4.330127018922192761 ) ) ;
#62762 = CARTESIAN_POINT ( 'NONE',  ( 4.458734124999999437, -151.3750000013656063, -1.846868145590734978 ) ) ;
#62763 = CARTESIAN_POINT ( 'NONE',  ( 2.229367062500001939, 23.77083333469892779, 3.861377020970579999 ) ) ;
#62764 = VERTEX_POINT ( 'NONE', #20647 ) ;
#62765 = CARTESIAN_POINT ( 'NONE',  ( 9.457646018065525792E-16, -91.06249999863439371, 5.148502694627439702 ) ) ;
#62766 = CARTESIAN_POINT ( 'NONE',  ( 5.000000000000000000, -47.41666666666666430, -2.886751345948130876 ) ) ;
#62767 = CARTESIAN_POINT ( 'NONE',  ( -51.75738570946856498, -155.0000000000000284, 3.805975901505577408 ) ) ;
#62768 = CARTESIAN_POINT ( 'NONE',  ( 4.458734124999999437, -7.812499998634405252, -5.460374474430324690E-16 ) ) ;
#62769 = DIRECTION ( 'NONE',  ( -0.000000000000000000, 1.000000000000000000, -0.000000000000000000 ) ) ;
#62770 = DIRECTION ( 'NONE',  ( -0.000000000000000000, 1.000000000000000000, -0.000000000000000000 ) ) ;
#62771 = CARTESIAN_POINT ( 'NONE',  ( -58.39396692619412477, -153.4375000013656063, 2.891590998281057701 ) ) ;
#62772 = CARTESIAN_POINT ( 'NONE',  ( 2.500000000000002220, -37.54166666393548013, 4.330127018922192761 ) ) ;
#62773 = PLANE ( 'NONE',  #23750 ) ;
#62774 = CARTESIAN_POINT ( 'NONE',  ( 2.229367062500001939, 18.02083333469892779, 3.861377020970579999 ) ) ;
#62775 = CARTESIAN_POINT ( 'NONE',  ( 5.000000000000000000, -44.50000000000000000, -6.123233995736766282E-16 ) ) ;
#62776 = CARTESIAN_POINT ( 'NONE',  ( -4.458734124999999437, 22.60416666803225993, -2.574251347313719407 ) ) ;
#62777 = CARTESIAN_POINT ( 'NONE',  ( 4.458734125000001214, -58.89583333196773651, 2.574251347313718519 ) ) ;
#62778 = CARTESIAN_POINT ( 'NONE',  ( 2.229367062500001939, -11.22916666530107044, 3.861377020970579999 ) ) ;
#62779 =( BOUNDED_CURVE ( )  B_SPLINE_CURVE ( 2, ( #3474, #8604, #51415, #27279, #43010, #23087, #46586, #42690, #2529 ),
 .UNSPECIFIED., .F., .F. ) 
 B_SPLINE_CURVE_WITH_KNOTS ( ( 3, 2, 2, 2, 3 ),
 ( 0.4604166666666666963, 0.4611111111111111382, 0.4625000000000000222, 0.4638888888888889062, 0.4645833333333333481 ),
 .UNSPECIFIED. ) 
 CURVE ( )  GEOMETRIC_REPRESENTATION_ITEM ( )  RATIONAL_B_SPLINE_CURVE ( ( 0.9330127018922194093, 0.9330127018922220739, 1.000000000000000000, 0.8660254037844387076, 1.000000000000000000, 0.8660254037844387076, 1.000000000000000000, 0.9330127018922194093, 0.9330127018922194093 ) ) 
 REPRESENTATION_ITEM ( '' )  );
#62780 = CARTESIAN_POINT ( 'NONE',  ( -9.184850993605147944E-16, -149.3750000027312126, 5.000000000000000000 ) ) ;
#62781 = CARTESIAN_POINT ( 'NONE',  ( 5.000000000000000000, 11.50000000000000000, -6.123233995736766282E-16 ) ) ;
#62782 = CARTESIAN_POINT ( 'NONE',  ( 4.458734124999999437, -166.5000000013655779, 1.846868145590737864 ) ) ;
#62783 = CARTESIAN_POINT ( 'NONE',  ( -60.14911071818854538, -145.1875000027312410, 1.666127454062681146 ) ) ;
#62784 = CARTESIAN_POINT ( 'NONE',  ( -4.458734124999999437, -47.31249999863440792, 0.000000000000000000 ) ) ;
#62785 = CARTESIAN_POINT ( 'NONE',  ( 1.060575238724906964E-15, -85.62499999726880162, 5.773502691896257311 ) ) ;
#62786 = CARTESIAN_POINT ( 'NONE',  ( -53.51423613279429503, -135.5000000013656063, 4.591703134518082763 ) ) ;
#62787 = DIRECTION ( 'NONE',  ( 0.000000000000000000, 0.000000000000000000, 1.000000000000000000 ) ) ;
#62788 = CARTESIAN_POINT ( 'NONE',  ( -58.24261429053147765, -145.2500000000000284, -3.805975901505573855 ) ) ;
#62789 = CARTESIAN_POINT ( 'NONE',  ( 4.458734124999999437, -90.06249999863440792, -5.460374474430324690E-16 ) ) ;
#62790 = CARTESIAN_POINT ( 'NONE',  ( -4.458734125000000326, -157.1250000013656063, 1.846868145590734089 ) ) ;
#62791 = CARTESIAN_POINT ( 'NONE',  ( 5.000000000000000000, -38.41666666666667140, -2.886751345948129988 ) ) ;
#62792 = FACE_OUTER_BOUND ( 'NONE', #49432, .T. ) ;
#62793 = ORIENTED_EDGE ( 'NONE', *, *, #14237, .F. ) ;
#62794 = CARTESIAN_POINT ( 'NONE',  ( 3.061616997868383141E-16, -162.7500000000000000, -5.000000000000000000 ) ) ;
#62795 = ORIENTED_EDGE ( 'NONE', *, *, #812, .T. ) ;
#62796 = CARTESIAN_POINT ( 'NONE',  ( 4.458734125000001214, -96.89583333196772230, 2.574251347313718519 ) ) ;
#62797 = CARTESIAN_POINT ( 'NONE',  ( 9.457646018065525792E-16, 5.687500001365592972, 5.148502694627439702 ) ) ;
#62798 = CARTESIAN_POINT ( 'NONE',  ( 5.000000000000000000, 12.62500000273118417, -6.123233995736766282E-16 ) ) ;
#62799 = CARTESIAN_POINT ( 'NONE',  ( 2.500000000000002220, 12.33333333333333215, 4.330127018922192761 ) ) ;
#62800 = CARTESIAN_POINT ( 'NONE',  ( 1.060575238724906964E-15, 1.250000000000001110, 5.773502691896257311 ) ) ;
#62801 = CARTESIAN_POINT ( 'NONE',  ( 9.457646018065525792E-16, -64.06249999863440792, 5.148502694627439702 ) ) ;
#62802 = CARTESIAN_POINT ( 'NONE',  ( -5.000000000000000000, -8.000000000000000000, 0.000000000000000000 ) ) ;
#62803 = CARTESIAN_POINT ( 'NONE',  ( 2.500000000000002220, 1.458333336064519203, 4.330127018922192761 ) ) ;
#62804 = CARTESIAN_POINT ( 'NONE',  ( 2.229367062499998831, -29.64583333196773296, -3.861377020970580887 ) ) ;
#62805 = CARTESIAN_POINT ( 'NONE',  ( -53.33387254593719717, -143.9375000027312126, 5.149110718188530278 ) ) ;
#62806 = CARTESIAN_POINT ( 'NONE',  ( 6.042630808230842148E-15, 25.87500000273118062, -4.999999999999999112 ) ) ;
#62807 = CARTESIAN_POINT ( 'NONE',  ( 1.339745962155670655, -19.29465819873852084, -4.999999999999966249 ) ) ;
#62808 = CARTESIAN_POINT ( 'NONE',  ( 5.000000000000000000, -45.50000000000000000, -6.123233995736766282E-16 ) ) ;
#62809 =( BOUNDED_CURVE ( )  B_SPLINE_CURVE ( 2, ( #12550, #2922, #60506, #51487, #27034, #46651, #32162, #22216, #30903 ),
 .UNSPECIFIED., .F., .F. ) 
 B_SPLINE_CURVE_WITH_KNOTS ( ( 3, 2, 2, 2, 3 ),
 ( 0.07708333333333333703, 0.07777777777777777901, 0.07916666666666666297, 0.08055555555555556080, 0.08125000000000000278 ),
 .UNSPECIFIED. ) 
 CURVE ( )  GEOMETRIC_REPRESENTATION_ITEM ( )  RATIONAL_B_SPLINE_CURVE ( ( 0.9330127018922194093, 0.9330127018922194093, 1.000000000000000000, 0.8660254037844387076, 1.000000000000000000, 0.8660254037844387076, 1.000000000000000000, 0.9330127018922194093, 0.9330127018922194093 ) ) 
 REPRESENTATION_ITEM ( '' )  );
#62811 = CARTESIAN_POINT ( 'NONE',  ( 4.458734125000001214, -18.14583333196773651, 2.574251347313718519 ) ) ;
#62810 = CARTESIAN_POINT ( 'NONE',  ( -1.339745962155613812, -45.20534180126146850, -5.000000000000000000 ) ) ;
#62812 = CARTESIAN_POINT ( 'NONE',  ( 0.000000000000000000, -170.0000000000000000, 5.000000000000000000 ) ) ;
#62813 = CARTESIAN_POINT ( 'NONE',  ( -2.229367062500000163, -68.47916666530107932, -3.861377020970580443 ) ) ;
#62814 = CARTESIAN_POINT ( 'NONE',  ( 1.846868145590736310, -149.8750000013655779, 4.458734124999999437 ) ) ;
#62815 = CONICAL_SURFACE ( 'NONE', #36086, 7.500000000000001776, 0.8594454914424796144 ) ;
#62817 = EDGE_CURVE ( 'NONE', #32525, #1423, #16128, .T. ) ;
#62816 = CARTESIAN_POINT ( 'NONE',  ( 4.458734125000001214, -77.89583333196773651, 2.574251347313718519 ) ) ;
#62818 = CARTESIAN_POINT ( 'NONE',  ( -51.60603307380591787, -143.1875000013656063, -2.891590998281053704 ) ) ;
#62819 = CARTESIAN_POINT ( 'NONE',  ( -2.229367062499996610, -22.39583333196773651, 3.861377020970582219 ) ) ;
#62820 = CARTESIAN_POINT ( 'NONE',  ( -2.500000000000000444, -65.04166666393547303, -4.330127018922193649 ) ) ;
#62821 = ORIENTED_EDGE ( 'NONE', *, *, #380, .T. ) ;
#62822 = CARTESIAN_POINT ( 'NONE',  ( 2.500000000000002220, -1.666666666666663410, 4.330127018922192761 ) ) ;
#62823 = EDGE_LOOP ( 'NONE', ( #1064, #40629, #34206, #20238 ) ) ;
#62824 = CARTESIAN_POINT ( 'NONE',  ( 4.458734124999999437, -66.06249999863440792, -5.460374474430324690E-16 ) ) ;
#62825 = CARTESIAN_POINT ( 'NONE',  ( -2.500000000000000444, 28.83333333333333215, -4.330127018922193649 ) ) ;
#62826 = CARTESIAN_POINT ( 'NONE',  ( 0.000000000000000000, -120.0000000000000000, 0.000000000000000000 ) ) ;
#62827 = ORIENTED_EDGE ( 'NONE', *, *, #38843, .F. ) ;
#62828 = CARTESIAN_POINT ( 'NONE',  ( -59.98410592259440222, -143.2500000027312126, -0.3983568153799752487 ) ) ;
#62829 = CARTESIAN_POINT ( 'NONE',  ( -2.229367062500000163, -53.72916666530107221, -3.861377020970580443 ) ) ;
#62830 = CARTESIAN_POINT ( 'NONE',  ( -4.458734124999999437, 3.437500001365594748, 0.000000000000000000 ) ) ;
#62831 = VERTEX_POINT ( 'NONE', #34791 ) ;
#62832 = EDGE_CURVE ( 'NONE', #12555, #61001, #62442, .T. ) ;
#62833 = CARTESIAN_POINT ( 'NONE',  ( -58.24261429053147765, -147.2500000000000284, -3.805975901505573855 ) ) ;
#62834 = EDGE_CURVE ( 'NONE', #18181, #56895, #58293, .T. ) ;
#62835 = CARTESIAN_POINT ( 'NONE',  ( 4.458734125000001214, 19.10416666803225638, 2.574251347313718519 ) ) ;
#62836 = CARTESIAN_POINT ( 'NONE',  ( -53.51423613279429503, -144.2500000013656063, 4.591703134518082763 ) ) ;
#62837 = CARTESIAN_POINT ( 'NONE',  ( 0.000000000000000000, -170.0000000000000000, 5.000000000000000000 ) ) ;
#62838 = CARTESIAN_POINT ( 'NONE',  ( -3.152801135295367985, -165.8125000013656063, 3.152801135295367096 ) ) ;
#62839 = ORIENTED_EDGE ( 'NONE', *, *, #30819, .T. ) ;
#62840 = CARTESIAN_POINT ( 'NONE',  ( 4.458734125000000326, -75.89583333196775072, 2.574251347313718519 ) ) ;
#62841 = CARTESIAN_POINT ( 'NONE',  ( 2.500000000000002220, 14.45833333606451809, 4.330127018922192761 ) ) ;
#62842 = CARTESIAN_POINT ( 'NONE',  ( 4.458734124999999437, 9.187500001365592084, -5.460374474430324690E-16 ) ) ;
#62843 = ADVANCED_FACE ( 'NONE', ( #30595 ), #40251, .T. ) ;
#62844 = CARTESIAN_POINT ( 'NONE',  ( -2.500000000000000444, 1.833333333333332593, -4.330127018922193649 ) ) ;
#62845 = CARTESIAN_POINT ( 'NONE',  ( -3.152548672688508926E-16, -58.81249999863440081, -5.148502694627439702 ) ) ;
#62846 = CARTESIAN_POINT ( 'NONE',  ( 5.000000000000000000, -21.29166666393548013, -2.886751345948129988 ) ) ;
#62847 = CARTESIAN_POINT ( 'NONE',  ( -59.81910112700026616, -142.1875000000000284, -2.462841084822451343 ) ) ;
#62848 = DIRECTION ( 'NONE',  ( 0.000000000000000000, 0.000000000000000000, 1.000000000000000000 ) ) ;
#62849 = DIRECTION ( 'NONE',  ( 0.000000000000000000, 0.000000000000000000, 1.000000000000000000 ) ) ;
#62850 = CARTESIAN_POINT ( 'NONE',  ( -6.972266317189433020E-16, -74.25000000000000000, -5.000000000000000000 ) ) ;
#62851 = LINE ( 'NONE', #43210, #18189 ) ;
#62852 = CARTESIAN_POINT ( 'NONE',  ( -4.458734124999999437, -40.39583333196773651, -2.574251347313719407 ) ) ;
#62853 = CARTESIAN_POINT ( 'NONE',  ( -4.458734124999999437, -27.56249999863440081, 0.000000000000000000 ) ) ;
#62854 = CARTESIAN_POINT ( 'NONE',  ( 1.339745962155637349, 11.70534180126147739, -4.999999999999985789 ) ) ;
#62855 = CARTESIAN_POINT ( 'NONE',  ( 2.499999999999998668, 27.66666666666666430, -4.330127018922193649 ) ) ;
#62856 = CARTESIAN_POINT ( 'NONE',  ( -5.000000000000000888, -154.6875000027312126, -2.071067811865475949 ) ) ;
#62857 = ORIENTED_EDGE ( 'NONE', *, *, #8739, .T. ) ;
#62858 = CARTESIAN_POINT ( 'NONE',  ( -3.152548672688508926E-16, -105.8124999986344079, -5.148502694627439702 ) ) ;
#62859 = CARTESIAN_POINT ( 'NONE',  ( 4.458734124999998549, -31.72916666530107577, -2.574251347313721627 ) ) ;
#62860 = CARTESIAN_POINT ( 'NONE',  ( -3.535250795749689387E-16, -66.12499999726881583, -5.773502691896257311 ) ) ;
#62861 = CARTESIAN_POINT ( 'NONE',  ( -50.70258187064364108, -148.3750000013656063, 2.196230717870141014 ) ) ;
#62862 = CARTESIAN_POINT ( 'NONE',  ( 5.000000000000000888, -144.9375000000000000, -2.071067811865475505 ) ) ;
#62863 = ADVANCED_FACE ( 'NONE', ( #59891 ), #29952, .T. ) ;
#62864 = CARTESIAN_POINT ( 'NONE',  ( -4.458734124999999437, -74.56249999863440792, 0.000000000000000000 ) ) ;
#62865 = CARTESIAN_POINT ( 'NONE',  ( -1.846868145590734756, -169.3750000013656347, -4.458734124999999437 ) ) ;
#62866 = CARTESIAN_POINT ( 'NONE',  ( 9.457646018065525792E-16, -32.06249999863440792, 5.148502694627439702 ) ) ;
#62867 = CARTESIAN_POINT ( 'NONE',  ( -75.00000000000002842, 15.00000000000000000, 5.000000000000000000 ) ) ;
#62868 = CARTESIAN_POINT ( 'NONE',  ( 1.975475456537005874E-15, -5.624999997268812280, 5.000000000000000000 ) ) ;
#62869 = CARTESIAN_POINT ( 'NONE',  ( 2.499999999999998668, -20.33333333333333570, -4.330127018922193649 ) ) ;
#62870 = CARTESIAN_POINT ( 'NONE',  ( -3.152801135295367985, -149.8125000013655779, 3.152801135295367096 ) ) ;
#62871 = EDGE_LOOP ( 'NONE', ( #5228, #43654, #11696, #47051 ) ) ;
#62872 = CARTESIAN_POINT ( 'NONE',  ( -58.24261429053147765, -141.2500000000000284, -3.805975901505573855 ) ) ;
#62873 = CARTESIAN_POINT ( 'NONE',  ( -4.458734124999999437, -59.56249999863440081, 0.000000000000000000 ) ) ;
#62874 = CARTESIAN_POINT ( 'NONE',  ( 2.500000000000002220, 26.45833333606451632, 4.330127018922192761 ) ) ;
#62875 = CARTESIAN_POINT ( 'NONE',  ( 5.000000000000000888, 13.54166666939785202, 2.886751345948126879 ) ) ;
#62876 = CARTESIAN_POINT ( 'NONE',  ( -4.999999999999999112, 17.08333333333333215, 2.886751345948131764 ) ) ;
#62877 = DIRECTION ( 'NONE',  ( 0.000000000000000000, 0.000000000000000000, 1.000000000000000000 ) ) ;
#62878 = CARTESIAN_POINT ( 'NONE',  ( -3.152548672688508926E-16, -4.562499998634401699, -5.148502694627439702 ) ) ;
#62879 = CARTESIAN_POINT ( 'NONE',  ( 1.339745962155613146, 28.29465819873852084, 5.000000000000000888 ) ) ;
#62880 = CARTESIAN_POINT ( 'NONE',  ( -6.972266317189433020E-16, -41.12499999726880162, -5.000000000000000000 ) ) ;
#62881 = CARTESIAN_POINT ( 'NONE',  ( 2.229367062500001939, 9.770833334698927786, 3.861377020970579999 ) ) ;
#62882 = CARTESIAN_POINT ( 'NONE',  ( 5.000000000000000000, -53.29166666393548013, -2.886751345948130876 ) ) ;
#62883 = VERTEX_POINT ( 'NONE', #50216 ) ;
#62884 = CARTESIAN_POINT ( 'NONE',  ( -4.999999999999998224, -71.79166666393547303, 2.886751345948131764 ) ) ;
#62885 = CARTESIAN_POINT ( 'NONE',  ( -4.458734124999999437, -49.39583333196773651, -2.574251347313719407 ) ) ;
#62886 = CARTESIAN_POINT ( 'NONE',  ( 2.730187237215162345E-16, -161.4375000013655779, -4.458734124999999437 ) ) ;
#62887 = EDGE_CURVE ( 'NONE', #11557, #34481, #20915, .T. ) ;
#62888 = CARTESIAN_POINT ( 'NONE',  ( -5.000000000000000000, -51.87499999726881583, 0.000000000000000000 ) ) ;
#62889 = VERTEX_POINT ( 'NONE', #36846 ) ;
#62890 = CARTESIAN_POINT ( 'NONE',  ( -4.458734124999999437, -22.39583333196773651, -2.574251347313719407 ) ) ;
#62891 = VERTEX_POINT ( 'NONE', #57424 ) ;
#62893 = CARTESIAN_POINT ( 'NONE',  ( 75.00000000000000000, 0.000000000000000000, 8.999999999999998224 ) ) ;
#62892 = CARTESIAN_POINT ( 'NONE',  ( 1.975475456537005874E-15, 18.37500000273118062, 5.000000000000000000 ) ) ;
#62894 = CARTESIAN_POINT ( 'NONE',  ( 2.730187237215162345E-16, -159.1875000013655779, -4.458734124999999437 ) ) ;
#62895 = ORIENTED_EDGE ( 'NONE', *, *, #10820, .F. ) ;
#62896 = CYLINDRICAL_SURFACE ( 'NONE', #42654, 5.000000000000000000 ) ;
#62897 = CARTESIAN_POINT ( 'NONE',  ( -57.46284108482265651, -134.9375000000000000, 4.819101127000239515 ) ) ;
#62898 = CARTESIAN_POINT ( 'NONE',  ( -1.339745962155610925, -58.66965819600732601, 5.000000000000000000 ) ) ;
#62899 = CARTESIAN_POINT ( 'NONE',  ( -4.458734124999998549, -37.47916666530107221, 2.574251347313722516 ) ) ;
#62900 = VERTEX_POINT ( 'NONE', #47749 ) ;
#62901 =( BOUNDED_CURVE ( )  B_SPLINE_CURVE ( 2, ( #53785, #29323, #9718, #49594, #29967, #30610, #5535, #60220, #1055 ),
 .UNSPECIFIED., .F., .F. ) 
 B_SPLINE_CURVE_WITH_KNOTS ( ( 3, 2, 2, 2, 3 ),
 ( 0.3517857142857143127, 0.3523809523809524058, 0.3535714285714285920, 0.3547619047619047783, 0.3553571428571428714 ),
 .UNSPECIFIED. ) 
 CURVE ( )  GEOMETRIC_REPRESENTATION_ITEM ( )  RATIONAL_B_SPLINE_CURVE ( ( 0.9330127018922194093, 0.9330127018922225179, 1.000000000000000000, 0.8660254037844387076, 1.000000000000000000, 0.8660254037844387076, 1.000000000000000000, 0.9330127018922194093, 0.9330127018922194093 ) ) 
 REPRESENTATION_ITEM ( '' )  );
#62902 = CARTESIAN_POINT ( 'NONE',  ( 2.229367062500001939, -83.97916666530106511, 3.861377020970579999 ) ) ;
#62903 = EDGE_CURVE ( 'NONE', #3585, #55695, #8212, .T. ) ;
#62904 = CARTESIAN_POINT ( 'NONE',  ( -2.229367062499996610, 16.85416666803225993, 3.861377020970582219 ) ) ;
#62905 = CARTESIAN_POINT ( 'NONE',  ( 1.339745962155615144, -12.58034179853029144, 4.999999999999999112 ) ) ;
#62906 = ORIENTED_EDGE ( 'NONE', *, *, #50060, .F. ) ;
#62907 = CARTESIAN_POINT ( 'NONE',  ( -50.55543936806279248, -137.3125000013656063, 0.3552334253322060320 ) ) ;
#62908 = EDGE_CURVE ( 'NONE', #53313, #34331, #45512, .T. ) ;
#62909 = CARTESIAN_POINT ( 'NONE',  ( -4.458734124999999437, -84.64583333196773651, -2.574251347313719407 ) ) ;
#62910 = CARTESIAN_POINT ( 'NONE',  ( -49.85088928181150436, -126.6875000027312410, -1.666127454062680702 ) ) ;
#62911 = CARTESIAN_POINT ( 'NONE',  ( 2.499999999999998668, -88.33333333333332860, -4.330127018922193649 ) ) ;
#62912 = DIRECTION ( 'NONE',  ( -0.000000000000000000, 1.000000000000000000, -0.000000000000000000 ) ) ;
#62913 = CARTESIAN_POINT ( 'NONE',  ( 5.000000000000000888, -13.45833333060214976, 2.886751345948126879 ) ) ;
#62914 = CARTESIAN_POINT ( 'NONE',  ( -3.152548672688508926E-16, -57.56249999863440792, -5.148502694627439702 ) ) ;
#62915 = CARTESIAN_POINT ( 'NONE',  ( 2.500000000000002220, 21.33333333333333215, 4.330127018922192761 ) ) ;
#62916 = CARTESIAN_POINT ( 'NONE',  ( 2.229367062500001939, 23.02083333469892423, 3.861377020970579999 ) ) ;
#62917 = CARTESIAN_POINT ( 'NONE',  ( 1.975475456537005874E-15, -42.75000000000000000, 5.000000000000000000 ) ) ;
#62918 = DIRECTION ( 'NONE',  ( -0.000000000000000000, 1.000000000000000000, -0.000000000000000000 ) ) ;
#62919 = CARTESIAN_POINT ( 'NONE',  ( -4.458734124999999437, -41.64583333196773651, -2.574251347313719407 ) ) ;
#62920 = CARTESIAN_POINT ( 'NONE',  ( 2.500000000000002220, -1.541666663935480130, 4.330127018922192761 ) ) ;
#62921 = CARTESIAN_POINT ( 'NONE',  ( -5.000000000000000000, -45.95833333060214443, -2.886751345948128211 ) ) ;
#62922 = CARTESIAN_POINT ( 'NONE',  ( -4.458734124999998549, -83.47916666530107932, 2.574251347313722516 ) ) ;
#62923 = CARTESIAN_POINT ( 'NONE',  ( 4.458734125000000326, -107.8958333319677365, 2.574251347313718519 ) ) ;
#62924 = CARTESIAN_POINT ( 'NONE',  ( 2.229367062499998831, -12.89583333196774007, -3.861377020970580887 ) ) ;
#62925 = VERTEX_POINT ( 'NONE', #56476 ) ;
#62926 = CARTESIAN_POINT ( 'NONE',  ( -4.999999999999998224, -80.91666666666667140, 2.886751345948131764 ) ) ;
#62927 = CARTESIAN_POINT ( 'NONE',  ( -4.458734124999999437, -99.39583333196772230, -2.574251347313719407 ) ) ;
#62928 = CARTESIAN_POINT ( 'NONE',  ( -3.535533905932738641, -164.5000000027312126, 3.535533905932737309 ) ) ;
#62929 = CARTESIAN_POINT ( 'NONE',  ( -2.229367062499996610, -92.39583333196773651, 3.861377020970582219 ) ) ;
#62930 = EDGE_CURVE ( 'NONE', #2867, #33297, #61934, .T. ) ;
#62931 = CARTESIAN_POINT ( 'NONE',  ( 5.000000000000000000, -51.29166666393547303, -2.886751345948129988 ) ) ;
#62932 = CARTESIAN_POINT ( 'NONE',  ( -6.972266317189433020E-16, -39.12499999726880162, -5.000000000000000000 ) ) ;
#62933 = CARTESIAN_POINT ( 'NONE',  ( -50.70258187064364108, -131.1250000013655779, 2.196230717870141014 ) ) ;
#62934 = CARTESIAN_POINT ( 'NONE',  ( -57.19623071787016499, -146.3750000013655779, 4.297418129356382899 ) ) ;
#62935 = CARTESIAN_POINT ( 'NONE',  ( 2.229367062500001939, -13.97916666530107221, 3.861377020970579999 ) ) ;
#62936 = CARTESIAN_POINT ( 'NONE',  ( -4.458734124999999437, 10.43750000136559386, 0.000000000000000000 ) ) ;
#62937 = CARTESIAN_POINT ( 'NONE',  ( -4.458734124999999437, -59.64583333196775072, -2.574251347313719407 ) ) ;
#62938 = CARTESIAN_POINT ( 'NONE',  ( 2.499999999999998668, -86.20833333060214443, -4.330127018922193649 ) ) ;
#62939 = DIRECTION ( 'NONE',  ( -1.000000000000000000, -0.000000000000000000, -0.000000000000000000 ) ) ;
#62940 = CARTESIAN_POINT ( 'NONE',  ( -2.229367062499996610, -14.14583333196774184, 3.861377020970582219 ) ) ;
#62941 = CARTESIAN_POINT ( 'NONE',  ( 0.000000000000000000, -120.0000000000000000, 0.000000000000000000 ) ) ;
#62942 = VERTEX_POINT ( 'NONE', #32012 ) ;
#62943 = CARTESIAN_POINT ( 'NONE',  ( 9.457646018065525792E-16, -43.31249999863440792, 5.148502694627439702 ) ) ;
#62944 = CARTESIAN_POINT ( 'NONE',  ( -2.499999999999996447, -37.83333333333332860, 4.330127018922195425 ) ) ;
#62945 = CARTESIAN_POINT ( 'NONE',  ( 1.339745962155615144, -66.70534180126148271, 4.999999999999999112 ) ) ;
#62946 = CARTESIAN_POINT ( 'NONE',  ( -1.339745962155610925, -24.79465819873852439, 5.000000000000000000 ) ) ;
#62947 = CARTESIAN_POINT ( 'NONE',  ( -2.229367062499996610, -84.14583333196773651, 3.861377020970582219 ) ) ;
#62948 = CARTESIAN_POINT ( 'NONE',  ( 4.458734124999999437, 19.93750000136559208, -5.460374474430324690E-16 ) ) ;
#62949 = CARTESIAN_POINT ( 'NONE',  ( -2.229367062500000163, 16.52083333469892779, -3.861377020970580443 ) ) ;
#62950 = CARTESIAN_POINT ( 'NONE',  ( -2.499999999999996447, -81.70833333060213022, 4.330127018922195425 ) ) ;
#62951 = CARTESIAN_POINT ( 'NONE',  ( 0.000000000000000000, -170.0000000000000000, 0.000000000000000000 ) ) ;
#62952 = CARTESIAN_POINT ( 'NONE',  ( -4.458734124999999437, -88.56249999863439371, 0.000000000000000000 ) ) ;
#62953 = CARTESIAN_POINT ( 'NONE',  ( 5.000000000000000000, -68.49999999999998579, -6.123233995736766282E-16 ) ) ;
#62954 =( BOUNDED_CURVE ( )  B_SPLINE_CURVE ( 2, ( #52542, #10038, #34161, #9716, #58622, #29652, #62825, #38984, #58928 ),
 .UNSPECIFIED., .F., .F. ) 
 B_SPLINE_CURVE_WITH_KNOTS ( ( 3, 2, 2, 2, 3 ),
 ( 0.005357142857142858060, 0.005952380952380952051, 0.007142857142857142634, 0.008333333333333333218, 0.008928571428571429811 ),
 .UNSPECIFIED. ) 
 CURVE ( )  GEOMETRIC_REPRESENTATION_ITEM ( )  RATIONAL_B_SPLINE_CURVE ( ( 0.9330127018922192983, 0.9330127018922194093, 1.000000000000000000, 0.8660254037844387076, 1.000000000000000000, 0.8660254037844387076, 1.000000000000000000, 0.9330127018922191873, 0.9330127018922192983 ) ) 
 REPRESENTATION_ITEM ( '' )  );
#62955 = CARTESIAN_POINT ( 'NONE',  ( -3.535250795749689387E-16, 13.87500000273118417, -5.773502691896257311 ) ) ;
#62956 = ORIENTED_EDGE ( 'NONE', *, *, #15431, .F. ) ;
#62957 = CARTESIAN_POINT ( 'NONE',  ( -6.972266317189433020E-16, -102.2499999999999858, -5.000000000000000000 ) ) ;
#62958 = ORIENTED_EDGE ( 'NONE', *, *, #58343, .F. ) ;
#62959 =( BOUNDED_CURVE ( )  B_SPLINE_CURVE ( 2, ( #28460, #24906, #29381, #33605, #57747, #53225, #39049, #49015, #43865 ),
 .UNSPECIFIED., .F., .F. ) 
 B_SPLINE_CURVE_WITH_KNOTS ( ( 3, 2, 2, 2, 3 ),
 ( 0.1303571428571428659, 0.1309523809523809590, 0.1321428571428571452, 0.1333333333333333315, 0.1339285714285714246 ),
 .UNSPECIFIED. ) 
 CURVE ( )  GEOMETRIC_REPRESENTATION_ITEM ( )  RATIONAL_B_SPLINE_CURVE ( ( 0.9330127018922194093, 0.9330127018922194093, 1.000000000000000000, 0.8660254037844387076, 1.000000000000000000, 0.8660254037844387076, 1.000000000000000000, 0.9330127018922194093, 0.9330127018922194093 ) ) 
 REPRESENTATION_ITEM ( '' )  );
#62960 = CARTESIAN_POINT ( 'NONE',  ( -2.500000000000000444, -90.16666666666665719, -4.330127018922193649 ) ) ;
#62962 = CARTESIAN_POINT ( 'NONE',  ( 5.000000000000000000, -30.50000000000000000, -6.123233995736766282E-16 ) ) ;
#62961 = CARTESIAN_POINT ( 'NONE',  ( 0.000000000000000000, -155.0000000000000284, 0.000000000000000000 ) ) ;
#62963 = CARTESIAN_POINT ( 'NONE',  ( -4.458734124999999437, -33.39583333196772941, -2.574251347313719407 ) ) ;
#62964 = ADVANCED_FACE ( 'NONE', ( #12711 ), #7580, .T. ) ;
#62965 = CARTESIAN_POINT ( 'NONE',  ( 5.000000000000000000, -33.37499999726880873, -6.123233995736766282E-16 ) ) ;
#62966 = ADVANCED_FACE ( 'NONE', ( #42610 ), #61297, .T. ) ;
#62968 = VERTEX_POINT ( 'NONE', #22052 ) ;
#62967 = CARTESIAN_POINT ( 'NONE',  ( -4.458734124999999437, -63.31249999863440792, 0.000000000000000000 ) ) ;
#62969 = CARTESIAN_POINT ( 'NONE',  ( -50.70258187064364108, -152.3750000013656063, 2.196230717870141014 ) ) ;
#62971 = VERTEX_POINT ( 'NONE', #18487 ) ;
#62970 = CARTESIAN_POINT ( 'NONE',  ( -4.458734124999999437, -14.56249999863440436, 0.000000000000000000 ) ) ;
#62972 = EDGE_CURVE ( 'NONE', #44963, #28712, #14694, .T. ) ;
#62973 = CARTESIAN_POINT ( 'NONE',  ( 2.499999999999998668, -79.33333333333332860, -4.330127018922193649 ) ) ;
#62974 = CARTESIAN_POINT ( 'NONE',  ( 2.500000000000002220, 28.45833333606451987, 4.330127018922192761 ) ) ;
#62975 = CARTESIAN_POINT ( 'NONE',  ( 4.458734124999999437, -59.06249999863440081, -5.460374474430324690E-16 ) ) ;
#62976 = EDGE_CURVE ( 'NONE', #40791, #56173, #62248, .T. ) ;
#62977 = CARTESIAN_POINT ( 'NONE',  ( -5.000000000000000000, -83.95833333060214443, -2.886751345948128211 ) ) ;
#62979 = ORIENTED_EDGE ( 'NONE', *, *, #49457, .F. ) ;
#62978 = CARTESIAN_POINT ( 'NONE',  ( -1.339745962155613812, 9.919658201469706782, -5.000000000000000000 ) ) ;
#62980 = CARTESIAN_POINT ( 'NONE',  ( -51.75738570946856498, -145.7500000000000284, 3.805975901505576964 ) ) ;
#62981 = EDGE_CURVE ( 'NONE', #24993, #49029, #28131, .T. ) ;
#62982 = CARTESIAN_POINT ( 'NONE',  ( 9.457646018065525792E-16, -23.31249999863440436, 5.148502694627439702 ) ) ;
#62983 = EDGE_CURVE ( 'NONE', #40265, #30447, #3705, .T. ) ;
#62985 = VERTEX_POINT ( 'NONE', #18167 ) ;
#62984 = CARTESIAN_POINT ( 'NONE',  ( -3.152548672688508926E-16, -59.81249999863440792, -5.148502694627439702 ) ) ;
#62986 = CARTESIAN_POINT ( 'NONE',  ( -55.00000000000002132, -10.00000000000000178, 0.000000000000000000 ) ) ;
#62987 = CARTESIAN_POINT ( 'NONE',  ( 2.730187237215162345E-16, -166.4375000013655779, -4.458734124999999437 ) ) ;
#62988 = ADVANCED_FACE ( 'NONE', ( #52589 ), #26881, .T. ) ;
#62989 = CARTESIAN_POINT ( 'NONE',  ( 2.229367062499998831, -103.8958333319677365, -3.861377020970580887 ) ) ;
#62990 = CARTESIAN_POINT ( 'NONE',  ( -5.000000000000000000, 17.91666666666666430, -2.886751345948128211 ) ) ;
#62991 =( BOUNDED_CURVE ( )  B_SPLINE_CURVE ( 2, ( #55121, #11045, #16515, #31294, #30670, #55445, #50289, #16194, #6237 ),
 .UNSPECIFIED., .F., .F. ) 
 B_SPLINE_CURVE_WITH_KNOTS ( ( 3, 2, 2, 2, 3 ),
 ( 0.2645833333333333370, 0.2652777777777777790, 0.2666666666666666630, 0.2680555555555555469, 0.2687499999999999889 ),
 .UNSPECIFIED. ) 
 CURVE ( )  GEOMETRIC_REPRESENTATION_ITEM ( )  RATIONAL_B_SPLINE_CURVE ( ( 0.9330127018922194093, 0.9330127018922194093, 1.000000000000000000, 0.8660254037844387076, 1.000000000000000000, 0.8660254037844387076, 1.000000000000000000, 0.9330127018922194093, 0.9330127018922194093 ) ) 
 REPRESENTATION_ITEM ( '' )  );
#62992 = ORIENTED_EDGE ( 'NONE', *, *, #39698, .F. ) ;
#62993 = EDGE_CURVE ( 'NONE', #35341, #57091, #5313, .T. ) ;
#62994 = CARTESIAN_POINT ( 'NONE',  ( -52.10840900171896806, -148.4375000013656063, 3.393966926194110556 ) ) ;
#62995 = CARTESIAN_POINT ( 'NONE',  ( -50.01589407740564042, -136.7500000027312126, 0.3983568153799778022 ) ) ;
#62996 = CARTESIAN_POINT ( 'NONE',  ( 4.458734125000000326, -39.89583333196772941, 2.574251347313718519 ) ) ;
#62997 = EDGE_CURVE ( 'NONE', #56652, #55713, #12648, .T. ) ;
#62998 = EDGE_CURVE ( 'NONE', #57534, #7022, #3274, .T. ) ;
#62999 = FACE_OUTER_BOUND ( 'NONE', #33146, .T. ) ;
#63000 = CARTESIAN_POINT ( 'NONE',  ( 9.457646018065525792E-16, -15.06249999863440259, 5.148502694627439702 ) ) ;
#63001 = CARTESIAN_POINT ( 'NONE',  ( 2.229367062499998831, -99.89583333196773651, -3.861377020970580887 ) ) ;
#63002 = CARTESIAN_POINT ( 'NONE',  ( -4.458734124999999437, -143.1875000013656063, -5.460374474430324690E-16 ) ) ;
#63003 = CARTESIAN_POINT ( 'NONE',  ( -4.458734124999998549, -30.47916666530107221, 2.574251347313722516 ) ) ;
#63004 = CARTESIAN_POINT ( 'NONE',  ( -2.499999999999996447, 12.16666666666666607, 4.330127018922195425 ) ) ;
#63005 = CARTESIAN_POINT ( 'NONE',  ( -50.55543936806279248, -132.0625000013656063, 0.3552334253322060320 ) ) ;
#63006 = CARTESIAN_POINT ( 'NONE',  ( -2.229367062500000163, -70.72916666530107932, -3.861377020970580443 ) ) ;
#63007 = CARTESIAN_POINT ( 'NONE',  ( 5.000000000000000000, -21.37499999726881228, -6.123233995736766282E-16 ) ) ;
#63008 = CARTESIAN_POINT ( 'NONE',  ( -5.000000000000000000, -42.95833333060214443, -2.886751345948128211 ) ) ;
#63009 = CARTESIAN_POINT ( 'NONE',  ( -8.190561711645485556E-16, -140.6875000013656063, 4.458734124999999437 ) ) ;
#63010 =( BOUNDED_CURVE ( )  B_SPLINE_CURVE ( 2, ( #23220, #18395, #51862, #7805, #48913, #24479, #43455, #34430, #9996 ),
 .UNSPECIFIED., .F., .F. ) 
 B_SPLINE_CURVE_WITH_KNOTS ( ( 3, 2, 2, 2, 3 ),
 ( 0.4145833333333333592, 0.4152777777777778012, 0.4166666666666666852, 0.4180555555555555691, 0.4187500000000000111 ),
 .UNSPECIFIED. ) 
 CURVE ( )  GEOMETRIC_REPRESENTATION_ITEM ( )  RATIONAL_B_SPLINE_CURVE ( ( 0.9330127018922194093, 0.9330127018922220739, 1.000000000000000000, 0.8660254037844387076, 1.000000000000000000, 0.8660254037844387076, 1.000000000000000000, 0.9330127018922194093, 0.9330127018922194093 ) ) 
 REPRESENTATION_ITEM ( '' )  );
#63011 = CARTESIAN_POINT ( 'NONE',  ( -4.458734124999997661, 7.520833334698926009, 2.574251347313722516 ) ) ;
#63012 = VERTEX_POINT ( 'NONE', #33900 ) ;
#63013 = LINE ( 'NONE', #48822, #19223 ) ;
#63014 = CARTESIAN_POINT ( 'NONE',  ( -9.184850993605147944E-16, -160.2500000000000000, 5.000000000000000000 ) ) ;
#63016 = CARTESIAN_POINT ( 'NONE',  ( 9.457646018065525792E-16, -32.06249999863440792, 5.148502694627439702 ) ) ;
#63015 = CARTESIAN_POINT ( 'NONE',  ( -3.535250795749689387E-16, -97.25000000000000000, -5.773502691896257311 ) ) ;
#63017 = CARTESIAN_POINT ( 'NONE',  ( -2.499999999999996447, 7.291666669397852019, 4.330127018922195425 ) ) ;
#63018 = CARTESIAN_POINT ( 'NONE',  ( -4.458734124999999437, -73.56249999863439371, 0.000000000000000000 ) ) ;
#63019 = CARTESIAN_POINT ( 'NONE',  ( 2.229367062499998831, 25.10416666803225993, -3.861377020970580887 ) ) ;
#63020 = AXIS2_PLACEMENT_3D ( 'NONE', #7388, #36015, #61105 ) ;
#63021 = CARTESIAN_POINT ( 'NONE',  ( -51.60603307380591787, -141.9375000013656063, -2.891590998281053704 ) ) ;
#63022 = CARTESIAN_POINT ( 'NONE',  ( 4.458734124999998549, 3.270833334698929118, -2.574251347313721627 ) ) ;
#63023 = CARTESIAN_POINT ( 'NONE',  ( 4.458734124999998549, 27.02083333469892423, -2.574251347313721627 ) ) ;
#63024 = CARTESIAN_POINT ( 'NONE',  ( -4.458734124999999437, -40.64583333196773651, -2.574251347313719407 ) ) ;
#63025 = CARTESIAN_POINT ( 'NONE',  ( -50.18089887299977647, -144.6874999999999716, 2.462841084822486426 ) ) ;
#63026 = CARTESIAN_POINT ( 'NONE',  ( -4.458734124999999437, 0.6875000013655957476, 0.000000000000000000 ) ) ;
#63027 = CARTESIAN_POINT ( 'NONE',  ( -4.458734124999999437, -26.64583333196774007, -2.574251347313719407 ) ) ;
#63028 = CARTESIAN_POINT ( 'NONE',  ( -1.846868145590737420, -155.7500000013655779, 4.458734124999999437 ) ) ;
#63029 = CARTESIAN_POINT ( 'NONE',  ( 4.458734124999999437, -69.81249999863439371, -5.460374474430324690E-16 ) ) ;
#63030 = CARTESIAN_POINT ( 'NONE',  ( 5.000000000000000000, -104.2916666639354588, -2.886751345948129988 ) ) ;
#63031 = CARTESIAN_POINT ( 'NONE',  ( 2.499999999999998668, -41.33333333333333570, -4.330127018922193649 ) ) ;
#63032 = CARTESIAN_POINT ( 'NONE',  ( -2.499999999999996447, -63.83333333333332860, 4.330127018922195425 ) ) ;
#63033 = CARTESIAN_POINT ( 'NONE',  ( 2.229367062499998831, -107.8958333319677365, -3.861377020970580887 ) ) ;
#63034 = CARTESIAN_POINT ( 'NONE',  ( 4.458734124999998549, -71.97916666530107932, -2.574251347313721627 ) ) ;
#63035 = CARTESIAN_POINT ( 'NONE',  ( 5.000000000000000888, -51.58333333333332149, 2.886751345948126879 ) ) ;
#63036 = CARTESIAN_POINT ( 'NONE',  ( -2.499999999999996447, -65.83333333333332860, 4.330127018922195425 ) ) ;
#63037 = CARTESIAN_POINT ( 'NONE',  ( -3.535250795749689387E-16, 28.87500000273118417, -5.773502691896257311 ) ) ;
#63038 = EDGE_LOOP ( 'NONE', ( #50895, #3704, #26992, #54482 ) ) ;
#63039 = CARTESIAN_POINT ( 'NONE',  ( -9.184850993605147944E-16, -140.2500000000000000, 5.000000000000000000 ) ) ;
#63040 = CARTESIAN_POINT ( 'NONE',  ( 1.339745962155612702, -27.16965819600733312, -5.000000000000000000 ) ) ;
#63041 = CARTESIAN_POINT ( 'NONE',  ( -3.535250795749689387E-16, -12.24999999999999645, -5.773502691896257311 ) ) ;
#63042 = CARTESIAN_POINT ( 'NONE',  ( -2.229367062499996610, -16.14583333196773651, 3.861377020970582219 ) ) ;
#63043 = CARTESIAN_POINT ( 'NONE',  ( -2.229367062499996610, -77.14583333196773651, 3.861377020970582219 ) ) ;
#63044 = CARTESIAN_POINT ( 'NONE',  ( -4.458734125000000326, -166.2500000013656347, -1.846868145590735644 ) ) ;
#63045 = CARTESIAN_POINT ( 'NONE',  ( -4.999999999999999112, -17.79166666393547658, 2.886751345948131764 ) ) ;
#63047 = EDGE_LOOP ( 'NONE', ( #41434, #10342, #57890, #19351 ) ) ;
#63046 = CARTESIAN_POINT ( 'NONE',  ( 4.458734124999998549, -42.72916666530107221, -2.574251347313721627 ) ) ;
#63048 = DIRECTION ( 'NONE',  ( 0.000000000000000000, 1.000000000000000000, 0.000000000000000000 ) ) ;
#63050 = ORIENTED_EDGE ( 'NONE', *, *, #47318, .F. ) ;
#63049 = CARTESIAN_POINT ( 'NONE',  ( 9.457646018065525792E-16, 3.687500001365594748, 5.148502694627439702 ) ) ;
#63051 = CARTESIAN_POINT ( 'NONE',  ( -59.44456063193725015, -152.5625000013656063, -0.3552334253322034230 ) ) ;
#63052 = CARTESIAN_POINT ( 'NONE',  ( -4.999999999999999112, -61.91666666666665719, 2.886751345948131764 ) ) ;
#63053 = CARTESIAN_POINT ( 'NONE',  ( 4.458734124999999437, -154.6875000013656063, 0.000000000000000000 ) ) ;
#63054 = CARTESIAN_POINT ( 'NONE',  ( 4.458734124999998549, -38.97916666530107221, -2.574251347313721627 ) ) ;
#63055 = CARTESIAN_POINT ( 'NONE',  ( 5.000000000000000000, -161.0624999999999716, 2.071067811865478614 ) ) ;
#63056 = CARTESIAN_POINT ( 'NONE',  ( 3.535533905932736864, -168.1250000000000284, 3.535533905932738641 ) ) ;
#63057 = CARTESIAN_POINT ( 'NONE',  ( -52.10840900171896806, -128.4375000013656063, 3.393966926194110556 ) ) ;
#63058 = CARTESIAN_POINT ( 'NONE',  ( -3.152548672688508926E-16, -7.812499998634405252, -5.148502694627439702 ) ) ;
#63059 = CARTESIAN_POINT ( 'NONE',  ( 2.229367062500001939, -42.22916666530107932, 3.861377020970579999 ) ) ;
#63060 = VECTOR ( 'NONE', #56834, 1000.000000000000000 ) ;
#63061 = LINE ( 'NONE', #38292, #19282 ) ;
#63062 = CARTESIAN_POINT ( 'NONE',  ( -4.458734124999999437, -149.9375000013656063, -5.460374474430324690E-16 ) ) ;
#63063 = CARTESIAN_POINT ( 'NONE',  ( -3.152548672688508926E-16, -88.81249999863439371, -5.148502694627439702 ) ) ;
#63064 = CARTESIAN_POINT ( 'NONE',  ( 5.000000000000000000, -34.37499999726881583, -6.123233995736766282E-16 ) ) ;
#63065 = VERTEX_POINT ( 'NONE', #48684 ) ;
#63066 = EDGE_CURVE ( 'NONE', #25665, #10009, #11881, .T. ) ;
#63067 = CARTESIAN_POINT ( 'NONE',  ( -2.499999999999996447, -46.83333333333333570, 4.330127018922195425 ) ) ;
#63068 = CARTESIAN_POINT ( 'NONE',  ( -52.53715891517739323, -149.5625000027312126, -4.819101127000233298 ) ) ;
#63069 = CARTESIAN_POINT ( 'NONE',  ( 2.500000000000002220, -43.66666666666665719, 4.330127018922192761 ) ) ;
#63070 = CARTESIAN_POINT ( 'NONE',  ( 2.229367062500001939, -73.22916666530107932, 3.861377020970579999 ) ) ;
#63071 = EDGE_LOOP ( 'NONE', ( #7214, #46158, #44843, #2673 ) ) ;
#63072 = EDGE_CURVE ( 'NONE', #38301, #2645, #25802, .T. ) ;
#63073 = DIRECTION ( 'NONE',  ( 0.000000000000000000, 0.000000000000000000, 1.000000000000000000 ) ) ;
#63074 = CARTESIAN_POINT ( 'NONE',  ( 2.229367062500001939, -13.22916666530107221, 3.861377020970579999 ) ) ;
#63075 = PRODUCT_DEFINITION_CONTEXT ( 'detailed design', #48689, 'design' ) ;
#63076 = CARTESIAN_POINT ( 'NONE',  ( 5.000000000000000000, -105.2916666639354730, -2.886751345948130876 ) ) ;
#63077 = CARTESIAN_POINT ( 'NONE',  ( 4.458734124999999437, -1.812499998634406584, -5.460374474430324690E-16 ) ) ;
#63078 = CARTESIAN_POINT ( 'NONE',  ( -2.500000000000000444, -43.16666666666665719, -4.330127018922193649 ) ) ;
#63079 = CARTESIAN_POINT ( 'NONE',  ( -4.458734125000000326, -152.8750000013655779, 1.846868145590734089 ) ) ;
#63080 = CARTESIAN_POINT ( 'NONE',  ( -4.458734124999999437, 19.43750000136559208, 0.000000000000000000 ) ) ;
#63081 = VERTEX_POINT ( 'NONE', #4624 ) ;
#63082 = CARTESIAN_POINT ( 'NONE',  ( 4.458734125000000326, -91.89583333196773651, 2.574251347313718519 ) ) ;
#63083 = LINE ( 'NONE', #38608, #2822 ) ;
#63084 = CARTESIAN_POINT ( 'NONE',  ( 0.6511518506208960888, -8.763486134561278007, -7.907570769506051533 ) ) ;
#63085 = CARTESIAN_POINT ( 'NONE',  ( -4.458734124999999437, -16.31249999863440436, 0.000000000000000000 ) ) ;
#63086 = CARTESIAN_POINT ( 'NONE',  ( -6.972266317189433020E-16, -39.12499999726880162, -5.000000000000000000 ) ) ;
#63087 = CARTESIAN_POINT ( 'NONE',  ( -5.000000000000000000, -73.00000000000000000, 0.000000000000000000 ) ) ;
#63088 =( BOUNDED_CURVE ( )  B_SPLINE_CURVE ( 2, ( #50308, #44515, #19758, #59000, #14928, #20079, #16220, #1129, #39684 ),
 .UNSPECIFIED., .F., .F. ) 
 B_SPLINE_CURVE_WITH_KNOTS ( ( 3, 2, 2, 2, 3 ),
 ( 0.4687500000000000000, 0.4694444444444444420, 0.4708333333333333259, 0.4722222222222222099, 0.4729166666666666519 ),
 .UNSPECIFIED. ) 
 CURVE ( )  GEOMETRIC_REPRESENTATION_ITEM ( )  RATIONAL_B_SPLINE_CURVE ( ( 0.9330127018922194093, 0.9330127018922194093, 1.000000000000000000, 0.8660254037844387076, 1.000000000000000000, 0.8660254037844387076, 1.000000000000000000, 0.9330127018922194093, 0.9330127018922194093 ) ) 
 REPRESENTATION_ITEM ( '' )  );
#63089 = CARTESIAN_POINT ( 'NONE',  ( 0.000000000000000000, -120.0000000000000000, 5.000000000000000000 ) ) ;
#63090 = CARTESIAN_POINT ( 'NONE',  ( -5.000000000000000000, -41.95833333060214443, -2.886751345948128211 ) ) ;
#63091 = DIRECTION ( 'NONE',  ( 0.000000000000000000, -1.000000000000000000, 0.000000000000000000 ) ) ;
#63092 = CARTESIAN_POINT ( 'NONE',  ( 4.458734124999998549, 21.27083333469892779, -2.574251347313721627 ) ) ;
#63093 = VERTEX_POINT ( 'NONE', #40236 ) ;
#63094 = CARTESIAN_POINT ( 'NONE',  ( -4.458734124999997661, 15.77083333469892601, 2.574251347313722516 ) ) ;
#63095 = CARTESIAN_POINT ( 'NONE',  ( 4.458734124999998549, -62.72916666530106511, -2.574251347313721627 ) ) ;
#63096 = CARTESIAN_POINT ( 'NONE',  ( 4.458734124999999437, -8.062499998634404363, -5.460374474430324690E-16 ) ) ;
#63097 = CARTESIAN_POINT ( 'NONE',  ( -75.00000000000001421, 15.00000000000000000, -9.000000000000001776 ) ) ;
#63098 = CARTESIAN_POINT ( 'NONE',  ( 1.060575238724906964E-15, 7.249999999999999112, 5.773502691896257311 ) ) ;
#63099 = CARTESIAN_POINT ( 'NONE',  ( -3.152801135295367096, -167.0625000013656063, -3.152801135295367541 ) ) ;
#63100 = CARTESIAN_POINT ( 'NONE',  ( -5.000000000000000000, -59.87499999726880873, 0.000000000000000000 ) ) ;
#63101 = CARTESIAN_POINT ( 'NONE',  ( 4.458734125000001214, -53.89583333196773651, 2.574251347313718519 ) ) ;
#63102 = CARTESIAN_POINT ( 'NONE',  ( 5.000000000000000000, -84.29166666393547303, -2.886751345948129988 ) ) ;
#63103 = CARTESIAN_POINT ( 'NONE',  ( -51.60603307380591787, -137.1875000013656063, -2.891590998281053704 ) ) ;
#63104 = DIRECTION ( 'NONE',  ( 1.000000000000000000, 0.000000000000000000, 0.000000000000000000 ) ) ;
#63105 =( BOUNDED_CURVE ( )  B_SPLINE_CURVE ( 2, ( #43395, #63040, #18948, #38566, #14439, #58195, #14124, #33750, #53368 ),
 .UNSPECIFIED., .F., .F. ) 
 B_SPLINE_CURVE_WITH_KNOTS ( ( 3, 2, 2, 2, 3 ),
 ( 0.4017857142857143016, 0.4023809523809523947, 0.4035714285714285809, 0.4047619047619047672, 0.4053571428571428603 ),
 .UNSPECIFIED. ) 
 CURVE ( )  GEOMETRIC_REPRESENTATION_ITEM ( )  RATIONAL_B_SPLINE_CURVE ( ( 0.9330127018922194093, 0.9330127018922194093, 1.000000000000000000, 0.8660254037844387076, 1.000000000000000000, 0.8660254037844387076, 1.000000000000000000, 0.9330127018922194093, 0.9330127018922194093 ) ) 
 REPRESENTATION_ITEM ( '' )  );
#63106 = CARTESIAN_POINT ( 'NONE',  ( -5.000000000000000000, -92.08333333333334281, -2.886751345948128211 ) ) ;
#63107 = CARTESIAN_POINT ( 'NONE',  ( -3.152548672688508926E-16, -92.81249999863440792, -5.148502694627439702 ) ) ;
#63108 = CARTESIAN_POINT ( 'NONE',  ( 4.458734124999999437, -155.6250000013655779, -1.846868145590734978 ) ) ;
#63109 = CARTESIAN_POINT ( 'NONE',  ( -5.000000000000000000, -37.08333333333332860, -2.886751345948128211 ) ) ;
#63110 = DIRECTION ( 'NONE',  ( -0.000000000000000000, 1.000000000000000000, -0.000000000000000000 ) ) ;
#63111 = DIRECTION ( 'NONE',  ( -0.000000000000000000, 1.000000000000000000, -0.000000000000000000 ) ) ;
#63112 = ORIENTED_EDGE ( 'NONE', *, *, #56989, .T. ) ;
#63113 = CARTESIAN_POINT ( 'NONE',  ( 2.229367062500001939, -102.9791666653010651, 3.861377020970579999 ) ) ;
#63114 = CARTESIAN_POINT ( 'NONE',  ( 4.458734124999999437, 8.937500001365592084, -5.460374474430324690E-16 ) ) ;
#63115 = CARTESIAN_POINT ( 'NONE',  ( -5.000000000000000000, 13.12500000273118417, 0.000000000000000000 ) ) ;
#63116 = CARTESIAN_POINT ( 'NONE',  ( -6.972266317189433020E-16, -44.12499999726880162, -5.000000000000000000 ) ) ;
#63117 = CARTESIAN_POINT ( 'NONE',  ( 5.000000000000000000, 0.5000000000000004441, -6.123233995736766282E-16 ) ) ;
#63118 = CARTESIAN_POINT ( 'NONE',  ( -2.229367062499996610, -59.14583333196773651, 3.861377020970582219 ) ) ;
#63119 = ADVANCED_FACE ( 'NONE', ( #59873 ), #10639, .T. ) ;
#63120 = FACE_OUTER_BOUND ( 'NONE', #7861, .T. ) ;
#63121 = CARTESIAN_POINT ( 'NONE',  ( 2.499999999999998668, -3.208333330602147093, -4.330127018922193649 ) ) ;
#63122 = CARTESIAN_POINT ( 'NONE',  ( 2.229367062500001939, -30.97916666530107221, 3.861377020970579999 ) ) ;
#63123 = CARTESIAN_POINT ( 'NONE',  ( 0.000000000000000000, -120.0000000000000000, 5.000000000000000000 ) ) ;
#63124 = CARTESIAN_POINT ( 'NONE',  ( 0.000000000000000000, -120.0000000000000000, 0.000000000000000000 ) ) ;
#63125 = CARTESIAN_POINT ( 'NONE',  ( -58.39396692619412477, -154.4375000013656063, 2.891590998281057701 ) ) ;
#63126 = CARTESIAN_POINT ( 'NONE',  ( -5.000000000000000000, -45.08333333333333570, -2.886751345948128211 ) ) ;
#63128 = CARTESIAN_POINT ( 'NONE',  ( 4.458734124999999437, -25.06249999863440792, -5.460374474430324690E-16 ) ) ;
#63127 = CARTESIAN_POINT ( 'NONE',  ( 2.500000000000002220, 6.458333336064519870, 4.330127018922192761 ) ) ;
#63129 = CARTESIAN_POINT ( 'NONE',  ( -6.972266317189433020E-16, 24.87500000273118417, -5.000000000000000000 ) ) ;
#63130 = CARTESIAN_POINT ( 'NONE',  ( -4.458734124999999437, -71.31249999863439371, 0.000000000000000000 ) ) ;
#63131 = CARTESIAN_POINT ( 'NONE',  ( -4.458734125000000326, -144.2500000013656063, -1.846868145590735644 ) ) ;
#63132 = CARTESIAN_POINT ( 'NONE',  ( 4.458734124999999437, -76.81249999863440792, -5.460374474430324690E-16 ) ) ;
#63133 = CARTESIAN_POINT ( 'NONE',  ( -57.19623071787017210, -143.6250000013655779, 4.297418129356382899 ) ) ;
#63134 = CARTESIAN_POINT ( 'NONE',  ( 4.458734124999999437, -23.06249999863440436, -5.460374474430324690E-16 ) ) ;
#63135 = CARTESIAN_POINT ( 'NONE',  ( -4.999999999999999112, -66.79166666393548724, 2.886751345948131764 ) ) ;
#63136 = ORIENTED_EDGE ( 'NONE', *, *, #63400, .F. ) ;
#63137 = CARTESIAN_POINT ( 'NONE',  ( -3.535533905932737309, -152.7500000027312126, -3.535533905932738197 ) ) ;
#63138 = ORIENTED_EDGE ( 'NONE', *, *, #21654, .T. ) ;
#63139 = CARTESIAN_POINT ( 'NONE',  ( -3.152548672688508926E-16, -69.81249999863439371, -5.148502694627439702 ) ) ;
#63140 = CARTESIAN_POINT ( 'NONE',  ( 5.000000000000000888, 28.41666666666666430, 2.886751345948126879 ) ) ;
#63141 = ORIENTED_EDGE ( 'NONE', *, *, #48881, .F. ) ;
#63142 = CARTESIAN_POINT ( 'NONE',  ( 0.000000000000000000, -170.0000000000000000, 0.000000000000000000 ) ) ;
#63143 = CARTESIAN_POINT ( 'NONE',  ( 4.458734124999998549, -60.97916666530106511, -2.574251347313721627 ) ) ;
#63144 = CARTESIAN_POINT ( 'NONE',  ( -3.152548672688508926E-16, 0.1875000013655953035, -5.148502694627439702 ) ) ;
#63145 = VERTEX_POINT ( 'NONE', #6151 ) ;
#63146 = AXIS2_PLACEMENT_3D ( 'NONE', #55696, #50217, #30917 ) ;
#63147 = CYLINDRICAL_SURFACE ( 'NONE', #6023, 5.000000000000000000 ) ;
#63148 = CARTESIAN_POINT ( 'NONE',  ( -4.458734124999998549, 17.77083333469892779, 2.574251347313722516 ) ) ;
#63149 = CARTESIAN_POINT ( 'NONE',  ( -58.39396692619412477, -144.4375000013656063, 2.891590998281057701 ) ) ;
#63150 = CARTESIAN_POINT ( 'NONE',  ( 5.000000000000000000, -92.37499999726880162, -6.123233995736766282E-16 ) ) ;
#63151 = CARTESIAN_POINT ( 'NONE',  ( 1.846868145590735200, -163.2500000013656063, -4.458734124999999437 ) ) ;
#63152 =( BOUNDED_CURVE ( )  B_SPLINE_CURVE ( 2, ( #51474, #37303, #31515, #36352, #32472, #17054, #12227, #52101, #51158 ),
 .UNSPECIFIED., .F., .F. ) 
 B_SPLINE_CURVE_WITH_KNOTS ( ( 3, 2, 2, 2, 3 ),
 ( 0.7104166666666666963, 0.7111111111111111382, 0.7125000000000000222, 0.7138888888888889062, 0.7145833333333333481 ),
 .UNSPECIFIED. ) 
 CURVE ( )  GEOMETRIC_REPRESENTATION_ITEM ( )  RATIONAL_B_SPLINE_CURVE ( ( 0.9330127018922194093, 0.9330127018922194093, 1.000000000000000000, 0.8660254037844387076, 1.000000000000000000, 0.8660254037844387076, 1.000000000000000000, 0.9330127018922194093, 0.9330127018922194093 ) ) 
 REPRESENTATION_ITEM ( '' )  );
#63153 = ORIENTED_EDGE ( 'NONE', *, *, #40615, .T. ) ;
#63154 = CARTESIAN_POINT ( 'NONE',  ( -4.458734124999997661, -78.22916666530106511, 2.574251347313722516 ) ) ;
#63155 = CARTESIAN_POINT ( 'NONE',  ( 3.061616997868383141E-16, -153.7500000000000000, -5.000000000000000000 ) ) ;
#63156 = CARTESIAN_POINT ( 'NONE',  ( -4.458734124999999437, -0.3124999986344051406, 0.000000000000000000 ) ) ;
#63157 = CARTESIAN_POINT ( 'NONE',  ( -6.972266317189433020E-16, 4.875000002731184168, -5.000000000000000000 ) ) ;
#63158 = CARTESIAN_POINT ( 'NONE',  ( 2.229367062499998831, -67.89583333196773651, -3.861377020970580887 ) ) ;
#63159 = CARTESIAN_POINT ( 'NONE',  ( 2.499999999999998668, -20.20833333060214798, -4.330127018922193649 ) ) ;
#63160 = CARTESIAN_POINT ( 'NONE',  ( 5.000000000000000000, -96.29166666393547303, -2.886751345948130876 ) ) ;
#63161 = CARTESIAN_POINT ( 'NONE',  ( 0.000000000000000000, -120.0000000000000000, 0.000000000000000000 ) ) ;
#63162 = CARTESIAN_POINT ( 'NONE',  ( -4.999999999999998224, -64.79166666393547303, 2.886751345948131764 ) ) ;
#63163 = CARTESIAN_POINT ( 'NONE',  ( 8.660254037844342889, 45.00000000000000000, 0.000000000000000000 ) ) ;
#63164 = CARTESIAN_POINT ( 'NONE',  ( -2.229367062500000163, -41.47916666530107932, -3.861377020970580443 ) ) ;
#63165 = CARTESIAN_POINT ( 'NONE',  ( -4.458734124999999437, -28.64583333196774007, -2.574251347313719407 ) ) ;
#63166 = CARTESIAN_POINT ( 'NONE',  ( -4.458734124999999437, 9.437500001365593860, 0.000000000000000000 ) ) ;
#63167 = CARTESIAN_POINT ( 'NONE',  ( -58.24261429053147765, -144.2500000000000284, -3.805975901505573855 ) ) ;
#63168 = CARTESIAN_POINT ( 'NONE',  ( -5.000000000000000000, 26.91666666666666075, -2.886751345948128211 ) ) ;
#63169 = CARTESIAN_POINT ( 'NONE',  ( -5.000000000000000888, -147.6875000027312126, -2.071067811865475949 ) ) ;
#63170 = CARTESIAN_POINT ( 'NONE',  ( 4.458734124999998549, -106.9791666653010509, -2.574251347313721627 ) ) ;
#63171 = EDGE_CURVE ( 'NONE', #35107, #56115, #54719, .T. ) ;
#63172 = CARTESIAN_POINT ( 'NONE',  ( -4.458734124999999437, -36.31249999863440792, 0.000000000000000000 ) ) ;
#63173 = CARTESIAN_POINT ( 'NONE',  ( 5.000000000000000000, -68.37499999726881583, -6.123233995736766282E-16 ) ) ;
#63174 = CARTESIAN_POINT ( 'NONE',  ( -56.48576386720575471, -148.0000000013655779, -4.591703134518078322 ) ) ;
#63175 = CARTESIAN_POINT ( 'NONE',  ( -5.000000000000000888, -141.5625000000000568, -2.071067811865475949 ) ) ;
#63176 = CARTESIAN_POINT ( 'NONE',  ( 4.458734124999998549, -73.97916666530106511, -2.574251347313721627 ) ) ;
#63177 = CARTESIAN_POINT ( 'NONE',  ( -1.339745962155613812, -55.20534180126147561, -5.000000000000000000 ) ) ;
#63178 = CARTESIAN_POINT ( 'NONE',  ( -2.229367062499996610, -31.14583333196773651, 3.861377020970582219 ) ) ;
#63179 = CARTESIAN_POINT ( 'NONE',  ( 1.975475456537005874E-15, -109.7499999999999858, 5.000000000000000000 ) ) ;
#63180 = DIRECTION ( 'NONE',  ( -0.000000000000000000, 1.000000000000000000, -0.000000000000000000 ) ) ;
#63181 = CARTESIAN_POINT ( 'NONE',  ( 5.000000000000000000, -20.41666666666666430, -2.886751345948129988 ) ) ;
#63182 = CARTESIAN_POINT ( 'NONE',  ( -3.152801135295367096, -143.0625000013655779, -3.152801135295367541 ) ) ;
#63183 = ORIENTED_EDGE ( 'NONE', *, *, #38202, .F. ) ;
#63184 = CARTESIAN_POINT ( 'NONE',  ( -2.229367062499996610, 26.60416666803225993, 3.861377020970582219 ) ) ;
#63185 = CARTESIAN_POINT ( 'NONE',  ( -60.14911071818854538, -141.0625000000000284, 1.666127454062681146 ) ) ;
#63186 = CARTESIAN_POINT ( 'NONE',  ( 4.458734125000000326, -56.14583333196773651, 2.574251347313718519 ) ) ;
#63187 =( BOUNDED_CURVE ( )  B_SPLINE_CURVE ( 2, ( #40641, #35507, #41265, #55127, #11052, #6242, #45790, #16201, #35829 ),
 .UNSPECIFIED., .F., .F. ) 
 B_SPLINE_CURVE_WITH_KNOTS ( ( 3, 2, 2, 2, 3 ),
 ( 0.9160714285714285365, 0.9166666666666666297, 0.9178571428571428159, 0.9190476190476190022, 0.9196428571428570953 ),
 .UNSPECIFIED. ) 
 CURVE ( )  GEOMETRIC_REPRESENTATION_ITEM ( )  RATIONAL_B_SPLINE_CURVE ( ( 0.9330127018922194093, 0.9330127018922194093, 1.000000000000000000, 0.8660254037844387076, 1.000000000000000000, 0.8660254037844387076, 1.000000000000000000, 0.9330127018922194093, 0.9330127018922194093 ) ) 
 REPRESENTATION_ITEM ( '' )  );
#63188 = CARTESIAN_POINT ( 'NONE',  ( -3.535250795749689387E-16, 27.87500000273118417, -5.773502691896257311 ) ) ;
#63189 = CARTESIAN_POINT ( 'NONE',  ( 1.339745962155615144, 13.41965820146970501, 4.999999999999999112 ) ) ;
#63190 = CARTESIAN_POINT ( 'NONE',  ( -5.000000000000000000, 19.91666666666666785, -2.886751345948128211 ) ) ;
#63191 = CARTESIAN_POINT ( 'NONE',  ( -5.000000000000000000, -36.95833333060213022, -2.886751345948128211 ) ) ;
#63192 = AXIS2_PLACEMENT_3D ( 'NONE', #54900, #4419, #43646 ) ;
#63193 = CARTESIAN_POINT ( 'NONE',  ( -4.458734124999999437, -8.312499998634406140, 0.000000000000000000 ) ) ;
#63194 = CARTESIAN_POINT ( 'NONE',  ( -5.000000000000000888, -168.4375000000001137, 2.071067811865474617 ) ) ;
#63195 = CARTESIAN_POINT ( 'NONE',  ( 2.071067811865433317, -164.9375000027311842, -5.000000000000041744 ) ) ;
#63196 = CARTESIAN_POINT ( 'NONE',  ( 5.000000000000000000, -91.29166666393547303, -2.886751345948130876 ) ) ;
#63197 = CARTESIAN_POINT ( 'NONE',  ( 6.123233995736766282E-16, -170.0000000000000000, -5.000000000000000000 ) ) ;
#63198 = CARTESIAN_POINT ( 'NONE',  ( -4.458734124999999437, -19.39583333196774007, -2.574251347313719407 ) ) ;
#63199 = CARTESIAN_POINT ( 'NONE',  ( -5.000000000000000000, -71.87499999726880162, 0.000000000000000000 ) ) ;
#63200 = CARTESIAN_POINT ( 'NONE',  ( -2.229367062499996610, -54.14583333196773651, 3.861377020970582219 ) ) ;
#63201 = CARTESIAN_POINT ( 'NONE',  ( -4.458734125000000326, -159.2500000013656063, -1.846868145590735644 ) ) ;
#63202 = CARTESIAN_POINT ( 'NONE',  ( -2.500000000000000444, -48.04166666393547303, -4.330127018922193649 ) ) ;
#63203 = ORIENTED_EDGE ( 'NONE', *, *, #38743, .F. ) ;
#63204 = CARTESIAN_POINT ( 'NONE',  ( -4.458734124999999437, 6.354166668032259047, -2.574251347313719407 ) ) ;
#63205 = ORIENTED_EDGE ( 'NONE', *, *, #56159, .F. ) ;
#63207 = CARTESIAN_POINT ( 'NONE',  ( -6.972266317189433020E-16, -69.12499999726880162, -5.000000000000000000 ) ) ;
#63206 = CARTESIAN_POINT ( 'NONE',  ( -6.972266317189433020E-16, -4.249999999999997335, -5.000000000000000000 ) ) ;
#63208 = CARTESIAN_POINT ( 'NONE',  ( 1.846868145590736310, -159.6250000013656063, 4.458734124999999437 ) ) ;
#63209 = ORIENTED_EDGE ( 'NONE', *, *, #3884, .T. ) ;
#63210 = CARTESIAN_POINT ( 'NONE',  ( 1.339745962155612702, -87.16965819600731891, -5.000000000000000000 ) ) ;
#63211 = CARTESIAN_POINT ( 'NONE',  ( -54.60164318462004474, -135.3750000000000284, -4.984105922594373794 ) ) ;
#63212 = CARTESIAN_POINT ( 'NONE',  ( -1.339745962155613812, -59.08034179853028434, -5.000000000000000000 ) ) ;
#63213 = CARTESIAN_POINT ( 'NONE',  ( 2.229367062499998831, -41.89583333196773651, -3.861377020970580887 ) ) ;
#63214 = ORIENTED_EDGE ( 'NONE', *, *, #29103, .F. ) ;
#63215 = CARTESIAN_POINT ( 'NONE',  ( 3.061616997868383141E-16, -142.8750000027312126, -5.000000000000000000 ) ) ;
#63216 = CARTESIAN_POINT ( 'NONE',  ( -3.152548672688508926E-16, 19.43750000136559208, -5.148502694627439702 ) ) ;
#63217 = DIRECTION ( 'NONE',  ( -0.000000000000000000, 1.000000000000000000, -0.000000000000000000 ) ) ;
#63218 = VERTEX_POINT ( 'NONE', #56318 ) ;
#63219 = CARTESIAN_POINT ( 'NONE',  ( -4.458734124999999437, -87.56249999863439371, 0.000000000000000000 ) ) ;
#63220 = CARTESIAN_POINT ( 'NONE',  ( -60.14911071818854538, -127.1875000027312126, 1.666127454062681368 ) ) ;
#63221 = CARTESIAN_POINT ( 'NONE',  ( 5.000000000000000888, -4.458333330602147981, 2.886751345948126879 ) ) ;
#63222 = CARTESIAN_POINT ( 'NONE',  ( -55.39835672516371545, -134.9999999999999716, 4.984105929804953483 ) ) ;
#63223 = CARTESIAN_POINT ( 'NONE',  ( 1.339745962155615144, -52.58034179853029144, 4.999999999999999112 ) ) ;
#63224 = CARTESIAN_POINT ( 'NONE',  ( -2.229367062499996610, -59.14583333196773651, 3.861377020970582219 ) ) ;
#63225 = CARTESIAN_POINT ( 'NONE',  ( -53.33387254593719717, -145.8125000000000000, 5.149110718188530278 ) ) ;
#63226 = CARTESIAN_POINT ( 'NONE',  ( -2.229367062500000163, 21.52083333469892779, -3.861377020970580443 ) ) ;
#63227 = DIRECTION ( 'NONE',  ( -0.8660254037844385966, 0.000000000000000000, -0.5000000000000000000 ) ) ;
#63228 = AXIS2_PLACEMENT_3D ( 'NONE', #986, #58851, #55324 ) ;
#63229 = CARTESIAN_POINT ( 'NONE',  ( -1.339745962155613812, -82.20534180126146850, -5.000000000000000000 ) ) ;
#63230 = CARTESIAN_POINT ( 'NONE',  ( -2.229367062500000163, -43.72916666530106511, -3.861377020970580443 ) ) ;
#63231 = CARTESIAN_POINT ( 'NONE',  ( -2.500000000000000444, -4.041666663935479242, -4.330127018922193649 ) ) ;
#63232 = CARTESIAN_POINT ( 'NONE',  ( -6.972266317189433020E-16, -6.249999999999999112, -5.000000000000000000 ) ) ;
#63233 = CARTESIAN_POINT ( 'NONE',  ( 6.123233995736766282E-16, -120.0000000000000000, -5.000000000000000000 ) ) ;
#63234 = CARTESIAN_POINT ( 'NONE',  ( 4.458734125000001214, -83.14583333196773651, 2.574251347313718519 ) ) ;
#63235 = CARTESIAN_POINT ( 'NONE',  ( -2.229367062500000163, -105.4791666653010651, -3.861377020970580443 ) ) ;
#63236 = CARTESIAN_POINT ( 'NONE',  ( 2.229367062500001939, -11.22916666530107044, 3.861377020970579999 ) ) ;
#63237 = ORIENTED_EDGE ( 'NONE', *, *, #50786, .T. ) ;
#63238 = CARTESIAN_POINT ( 'NONE',  ( -4.999999999999998224, -16.79166666393548368, 2.886751345948131764 ) ) ;
#63239 = CARTESIAN_POINT ( 'NONE',  ( -2.229367062500000163, -100.4791666653010651, -3.861377020970580443 ) ) ;
#63240 = CARTESIAN_POINT ( 'NONE',  ( 5.000000000000000000, -160.1250000027311842, 0.000000000000000000 ) ) ;
#63241 = CARTESIAN_POINT ( 'NONE',  ( 4.458734125000001214, -93.14583333196773651, 2.574251347313718519 ) ) ;
#63242 = EDGE_CURVE ( 'NONE', #52748, #19205, #54360, .T. ) ;
#63243 = CARTESIAN_POINT ( 'NONE',  ( 2.500000000000002220, -49.54166666393547303, 4.330127018922192761 ) ) ;
#63244 = DIRECTION ( 'NONE',  ( 0.000000000000000000, 0.000000000000000000, 1.000000000000000000 ) ) ;
#63245 = CARTESIAN_POINT ( 'NONE',  ( -54.64476657466781973, -130.8125000013656063, -4.444560631937228834 ) ) ;
#63246 = CARTESIAN_POINT ( 'NONE',  ( -55.35523342533222291, -145.3125000013656063, 4.444560631937231499 ) ) ;
#63247 = CARTESIAN_POINT ( 'NONE',  ( -4.458734124999997661, -20.22916666530107221, 2.574251347313722516 ) ) ;
#63248 = CARTESIAN_POINT ( 'NONE',  ( 9.457646018065525792E-16, 8.687500001365595637, 5.148502694627439702 ) ) ;
#63249 = CARTESIAN_POINT ( 'NONE',  ( -2.229367062500000163, -58.72916666530106511, -3.861377020970580443 ) ) ;
#63250 = CARTESIAN_POINT ( 'NONE',  ( 4.458734125000000326, -15.89583333196773651, 2.574251347313718519 ) ) ;
#63251 = DIRECTION ( 'NONE',  ( -0.000000000000000000, 1.000000000000000000, -0.000000000000000000 ) ) ;
#63252 = CARTESIAN_POINT ( 'NONE',  ( 2.071067811865475505, -153.8125000000000000, -5.000000000000000888 ) ) ;
#63253 = ORIENTED_EDGE ( 'NONE', *, *, #48092, .F. ) ;
#63254 = CARTESIAN_POINT ( 'NONE',  ( 2.229367062499998831, -42.89583333196773651, -3.861377020970580887 ) ) ;
#63255 = CARTESIAN_POINT ( 'NONE',  ( 2.499999999999998668, -83.20833333060214443, -4.330127018922193649 ) ) ;
#63256 = CARTESIAN_POINT ( 'NONE',  ( 0.000000000000000000, -120.0000000000000000, 0.000000000000000000 ) ) ;
#63257 = EDGE_CURVE ( 'NONE', #31695, #248, #41177, .T. ) ;
#63258 = LINE ( 'NONE', #53599, #37839 ) ;
#63259 = CARTESIAN_POINT ( 'NONE',  ( 2.229367062500001939, -82.97916666530106511, 3.861377020970579999 ) ) ;
#63260 = CARTESIAN_POINT ( 'NONE',  ( 2.229367062499998831, 20.10416666803225993, -3.861377020970580887 ) ) ;
#63261 = CARTESIAN_POINT ( 'NONE',  ( -3.152548672688508926E-16, 11.43750000136559386, -5.148502694627439702 ) ) ;
#63262 = CYLINDRICAL_SURFACE ( 'NONE', #10278, 5.000000000000000000 ) ;
#63263 = EDGE_CURVE ( 'NONE', #43626, #18601, #37007, .T. ) ;
#63264 = CARTESIAN_POINT ( 'NONE',  ( -6.972266317189433020E-16, -78.24999999999998579, -5.000000000000000000 ) ) ;
#63265 = CARTESIAN_POINT ( 'NONE',  ( 2.229367062499998831, -87.89583333196773651, -3.861377020970580887 ) ) ;
#63266 = CARTESIAN_POINT ( 'NONE',  ( 1.060575238724906964E-15, -70.74999999999998579, 5.773502691896257311 ) ) ;
#63267 = CARTESIAN_POINT ( 'NONE',  ( 2.499999999999998668, 14.79166666939785202, -4.330127018922193649 ) ) ;
#63268 = ORIENTED_EDGE ( 'NONE', *, *, #55132, .F. ) ;
#63269 = VERTEX_POINT ( 'NONE', #46336 ) ;
#63270 = CARTESIAN_POINT ( 'NONE',  ( -2.499999999999996447, -89.83333333333332860, 4.330127018922195425 ) ) ;
#63272 = CARTESIAN_POINT ( 'NONE',  ( -3.535250795749689387E-16, -36.25000000000000711, -5.773502691896257311 ) ) ;
#63271 = CARTESIAN_POINT ( 'NONE',  ( 1.339745962155615144, -85.70534180126146850, 4.999999999999999112 ) ) ;
#63273 = CARTESIAN_POINT ( 'NONE',  ( 4.458734124999999437, -35.81249999863440792, -5.460374474430324690E-16 ) ) ;
#63274 = AXIS2_PLACEMENT_3D ( 'NONE', #59603, #15535, #35155 ) ;
#63275 =( BOUNDED_CURVE ( )  B_SPLINE_CURVE ( 2, ( #38917, #53718, #62757, #28328, #23517, #19622, #48572, #39233, #57930 ),
 .UNSPECIFIED., .F., .F. ) 
 B_SPLINE_CURVE_WITH_KNOTS ( ( 3, 2, 2, 2, 3 ),
 ( 0.7732142857142857428, 0.7738095238095238360, 0.7750000000000000222, 0.7761904761904762085, 0.7767857142857143016 ),
 .UNSPECIFIED. ) 
 CURVE ( )  GEOMETRIC_REPRESENTATION_ITEM ( )  RATIONAL_B_SPLINE_CURVE ( ( 0.9330127018922194093, 0.9330127018922194093, 1.000000000000000000, 0.8660254037844387076, 1.000000000000000000, 0.8660254037844387076, 1.000000000000000000, 0.9330127018922194093, 0.9330127018922194093 ) ) 
 REPRESENTATION_ITEM ( '' )  );
#63276 = CARTESIAN_POINT ( 'NONE',  ( 1.060575238724906964E-15, -36.62499999726880873, 5.773502691896257311 ) ) ;
#63278 = ORIENTED_EDGE ( 'NONE', *, *, #15430, .F. ) ;
#63277 = CARTESIAN_POINT ( 'NONE',  ( -4.458734124999999437, -67.39583333196773651, -2.574251347313719407 ) ) ;
#63279 = CARTESIAN_POINT ( 'NONE',  ( -53.51423613279429503, -152.5000000013655779, 4.591703134518082763 ) ) ;
#63280 = CARTESIAN_POINT ( 'NONE',  ( 4.458734124999999437, -13.81249999863440259, -5.460374474430324690E-16 ) ) ;
#63282 = EDGE_LOOP ( 'NONE', ( #48682, #3346, #10510, #10612 ) ) ;
#63281 = CARTESIAN_POINT ( 'NONE',  ( 9.457646018065525792E-16, -14.31249999863440259, 5.148502694627439702 ) ) ;
#63283 = CARTESIAN_POINT ( 'NONE',  ( -2.499999999999996447, -75.83333333333334281, 4.330127018922195425 ) ) ;
#63284 = CARTESIAN_POINT ( 'NONE',  ( -56.48576386720575471, -135.7500000013656063, -4.591703134518078322 ) ) ;
#63285 = CARTESIAN_POINT ( 'NONE',  ( -3.152548672688508926E-16, -56.81249999863439371, -5.148502694627439702 ) ) ;
#63286 = CARTESIAN_POINT ( 'NONE',  ( -2.500000000000000444, -80.04166666393547303, -4.330127018922193649 ) ) ;
#63287 = VERTEX_POINT ( 'NONE', #7739 ) ;
#63288 = CARTESIAN_POINT ( 'NONE',  ( -57.46284108482265651, -145.9375000000000284, 4.819101127000239515 ) ) ;
#63289 = CARTESIAN_POINT ( 'NONE',  ( 4.458734124999999437, -24.06249999863440436, -5.460374474430324690E-16 ) ) ;
#63290 = ORIENTED_EDGE ( 'NONE', *, *, #10316, .T. ) ;
#63291 = CARTESIAN_POINT ( 'NONE',  ( -3.152801135295367985, -168.0625000013656063, 3.152801135295367096 ) ) ;
#63292 = EDGE_CURVE ( 'NONE', #13678, #16051, #1586, .T. ) ;
#63293 = CARTESIAN_POINT ( 'NONE',  ( 4.458734124999998549, -103.9791666653010509, -2.574251347313721627 ) ) ;
#63294 = CARTESIAN_POINT ( 'NONE',  ( -2.499999999999996447, -68.70833333060214443, 4.330127018922195425 ) ) ;
#63295 = ORIENTED_EDGE ( 'NONE', *, *, #32351, .T. ) ;
#63296 = CARTESIAN_POINT ( 'NONE',  ( -52.10840900171896806, -149.4375000013656063, 3.393966926194110556 ) ) ;
#63297 = CARTESIAN_POINT ( 'NONE',  ( -55.39835681537999790, -138.0000000027312126, 4.984105922594378235 ) ) ;
#63298 = CARTESIAN_POINT ( 'NONE',  ( 9.457646018065525792E-16, -39.06249999863440081, 5.148502694627439702 ) ) ;
#63299 = LINE ( 'NONE', #19218, #15759 ) ;
#63300 = CARTESIAN_POINT ( 'NONE',  ( -2.071067811865562991, -146.4375000027311842, 4.999999999999913847 ) ) ;
#63301 = CARTESIAN_POINT ( 'NONE',  ( -4.458734124999999437, -14.39583333196773474, -2.574251347313719407 ) ) ;
#63302 = CARTESIAN_POINT ( 'NONE',  ( 9.457646018065525792E-16, -103.3124999986344079, 5.148502694627439702 ) ) ;
#63303 = ORIENTED_EDGE ( 'NONE', *, *, #4642, .T. ) ;
#63304 = CARTESIAN_POINT ( 'NONE',  ( 3.152801135295366208, -145.8125000013655779, 3.152801135295367985 ) ) ;
#63305 = CARTESIAN_POINT ( 'NONE',  ( -2.229367062500000163, -30.72916666530107221, -3.861377020970580443 ) ) ;
#63306 = CARTESIAN_POINT ( 'NONE',  ( 1.975475456537005874E-15, -70.75000000000000000, 5.000000000000000000 ) ) ;
#63307 = CARTESIAN_POINT ( 'NONE',  ( -53.51423613279429503, -132.2500000013656063, 4.591703134518082763 ) ) ;
#63308 = CARTESIAN_POINT ( 'NONE',  ( -4.458734124999999437, -69.56249999863439371, 0.000000000000000000 ) ) ;
#63309 = CARTESIAN_POINT ( 'NONE',  ( 5.000000000000000000, -17.50000000000000000, -6.123233995736766282E-16 ) ) ;
#63310 = CYLINDRICAL_SURFACE ( 'NONE', #23379, 5.000000000000000000 ) ;
#63311 = CARTESIAN_POINT ( 'NONE',  ( -4.458734125000000326, -142.8750000013656063, 1.846868145590734089 ) ) ;
#63312 = CARTESIAN_POINT ( 'NONE',  ( 9.457646018065525792E-16, 5.687500001365592972, 5.148502694627439702 ) ) ;
#63313 = ORIENTED_EDGE ( 'NONE', *, *, #16922, .F. ) ;
#63314 = VECTOR ( 'NONE', #21421, 1000.000000000000000 ) ;
#63315 = SURFACE_SIDE_STYLE ('',( #33721 ) ) ;
#63316 = DIRECTION ( 'NONE',  ( -0.000000000000000000, 1.000000000000000000, -0.000000000000000000 ) ) ;
#63318 = CARTESIAN_POINT ( 'NONE',  ( -2.229367062500000163, -30.47916666530107221, -3.861377020970580443 ) ) ;
#63317 = CARTESIAN_POINT ( 'NONE',  ( 5.000000000000000888, -97.58333333333332860, 2.886751345948126879 ) ) ;
#63319 = CARTESIAN_POINT ( 'NONE',  ( 1.339745962155615144, -73.70534180126146850, 4.999999999999999112 ) ) ;
#63320 = CARTESIAN_POINT ( 'NONE',  ( -2.229367062500000163, -73.72916666530106511, -3.861377020970580443 ) ) ;
#63321 = VECTOR ( 'NONE', #34353, 1000.000000000000000 ) ;
#63322 = CARTESIAN_POINT ( 'NONE',  ( 4.458734124999998549, 24.02083333469892423, -2.574251347313721627 ) ) ;
#63323 = CARTESIAN_POINT ( 'NONE',  ( -4.999999999999998224, -101.7916666639354446, 2.886751345948131764 ) ) ;
#63324 = VECTOR ( 'NONE', #19951, 1000.000000000000000 ) ;
#63325 = CARTESIAN_POINT ( 'NONE',  ( -53.51423613279429503, -140.2500000013656063, 4.591703134518082763 ) ) ;
#63326 = ADVANCED_FACE ( 'NONE', ( #17066 ), #21895, .T. ) ;
#63327 = EDGE_CURVE ( 'NONE', #36403, #25000, #60823, .T. ) ;
#63328 = CARTESIAN_POINT ( 'NONE',  ( -4.458734124999999437, -4.312499998634401699, 0.000000000000000000 ) ) ;
#63329 = CARTESIAN_POINT ( 'NONE',  ( 4.458734125000001214, 28.85416666803225993, 2.574251347313718519 ) ) ;
#63330 = CARTESIAN_POINT ( 'NONE',  ( -4.458734124999999437, -40.56249999863440081, 0.000000000000000000 ) ) ;
#63331 =( BOUNDED_CURVE ( )  B_SPLINE_CURVE ( 2, ( #18976, #14152, #19613, #19292, #38910, #4505, #39225, #8704, #24131 ),
 .UNSPECIFIED., .F., .F. ) 
 B_SPLINE_CURVE_WITH_KNOTS ( ( 3, 2, 2, 2, 3 ),
 ( 0.3916666666666669960, 0.3958333333333336479, 0.4000000000000003553, 0.4041666666666670071, 0.4083333333333336590 ),
 .UNSPECIFIED. ) 
 CURVE ( )  GEOMETRIC_REPRESENTATION_ITEM ( )  RATIONAL_B_SPLINE_CURVE ( ( 0.9999999999999938938, 0.9238795325112928447, 1.000000000000000000, 0.9238795325112867385, 1.000000000000000000, 0.9238795325112867385, 1.000000000000000000, 0.9238795325112806323, 1.000000000000005995 ) ) 
 REPRESENTATION_ITEM ( '' )  );
#63332 = CARTESIAN_POINT ( 'NONE',  ( -51.19402409849444524, -144.5000000000000284, -3.242614290531456334 ) ) ;
#63333 = CARTESIAN_POINT ( 'NONE',  ( -4.458734124999999437, 2.604166668032263043, -2.574251347313719407 ) ) ;
#63334 = CARTESIAN_POINT ( 'NONE',  ( -4.458734124999997661, -24.47916666530107577, 2.574251347313722516 ) ) ;
#63335 =( BOUNDED_CURVE ( )  B_SPLINE_CURVE ( 2, ( #52601, #32981, #12725, #27207, #32347, #8535, #13043, #32661, #46825 ),
 .UNSPECIFIED., .F., .F. ) 
 B_SPLINE_CURVE_WITH_KNOTS ( ( 3, 2, 2, 2, 3 ),
 ( 0.3020833333333333148, 0.3027777777777777568, 0.3041666666666666408, 0.3055555555555555802, 0.3062500000000000222 ),
 .UNSPECIFIED. ) 
 CURVE ( )  GEOMETRIC_REPRESENTATION_ITEM ( )  RATIONAL_B_SPLINE_CURVE ( ( 0.9330127018922194093, 0.9330127018922194093, 1.000000000000000000, 0.8660254037844387076, 1.000000000000000000, 0.8660254037844387076, 1.000000000000000000, 0.9330127018922194093, 0.9330127018922194093 ) ) 
 REPRESENTATION_ITEM ( '' )  );
#63336 = CARTESIAN_POINT ( 'NONE',  ( 3.152801135295366208, -156.5625000013656063, 3.152801135295367985 ) ) ;
#63337 = CARTESIAN_POINT ( 'NONE',  ( 4.458734124999999437, -71.81249999863439371, -5.460374474430324690E-16 ) ) ;
#63338 = CARTESIAN_POINT ( 'NONE',  ( 2.499999999999998668, -104.2083333306021444, -4.330127018922193649 ) ) ;
#63339 = EDGE_CURVE ( 'NONE', #5467, #41613, #6085, .T. ) ;
#63340 = CARTESIAN_POINT ( 'NONE',  ( 9.457646018065525792E-16, 26.93750000136559564, 5.148502694627439702 ) ) ;
#63341 = CARTESIAN_POINT ( 'NONE',  ( 0.000000000000000000, -120.0000000000000000, 0.000000000000000000 ) ) ;
#63342 = EDGE_CURVE ( 'NONE', #27835, #551, #62809, .T. ) ;
#63343 = CARTESIAN_POINT ( 'NONE',  ( -60.14911071818854538, -153.1875000027312126, 1.666127454062681146 ) ) ;
#63344 = CARTESIAN_POINT ( 'NONE',  ( -4.458734124999999437, -71.56249999863439371, 0.000000000000000000 ) ) ;
#63345 = CARTESIAN_POINT ( 'NONE',  ( -3.535250795749689387E-16, -52.25000000000001421, -5.773502691896257311 ) ) ;
#63346 = CARTESIAN_POINT ( 'NONE',  ( 5.000000000000000888, -73.58333333333332860, 2.886751345948126879 ) ) ;
#63347 = CARTESIAN_POINT ( 'NONE',  ( 5.000000000000000000, -156.1875000027312126, 2.071067811865478614 ) ) ;
#63348 = ORIENTED_EDGE ( 'NONE', *, *, #26313, .T. ) ;
#63349 = CARTESIAN_POINT ( 'NONE',  ( 1.975475456537005874E-15, -26.74999999999999645, 5.000000000000000000 ) ) ;
#63350 = LINE ( 'NONE', #18648, #25760 ) ;
#63351 = CARTESIAN_POINT ( 'NONE',  ( -5.000000000000000000, -11.99999999999999645, 0.000000000000000000 ) ) ;
#63352 = CARTESIAN_POINT ( 'NONE',  ( -4.458734124999999437, -18.31249999863440792, 0.000000000000000000 ) ) ;
#63353 = CARTESIAN_POINT ( 'NONE',  ( 2.229367062500001939, -81.97916666530106511, 3.861377020970579999 ) ) ;
#63354 = CARTESIAN_POINT ( 'NONE',  ( -1.846868145590734756, -167.3750000013656347, -4.458734125000000326 ) ) ;
#63355 = CARTESIAN_POINT ( 'NONE',  ( 5.000000000000000000, -17.37499999726881583, -6.123233995736766282E-16 ) ) ;
#63357 = ORIENTED_EDGE ( 'NONE', *, *, #9875, .F. ) ;
#63356 = CARTESIAN_POINT ( 'NONE',  ( 2.229367062500001939, -49.97916666530107221, 3.861377020970579999 ) ) ;
#63358 = CARTESIAN_POINT ( 'NONE',  ( 5.000000000000000000, 5.583333333333332149, -2.886751345948130876 ) ) ;
#63359 = CARTESIAN_POINT ( 'NONE',  ( 1.975475456537005874E-15, -98.74999999999998579, 5.000000000000000000 ) ) ;
#63361 = ORIENTED_EDGE ( 'NONE', *, *, #13438, .F. ) ;
#63360 = CARTESIAN_POINT ( 'NONE',  ( 9.457646018065525792E-16, 1.687500001365593194, 5.148502694627439702 ) ) ;
#63362 =( BOUNDED_CURVE ( )  B_SPLINE_CURVE ( 2, ( #63507, #49008, #9459, #14916, #43549, #15573, #58671, #20068, #19431 ),
 .UNSPECIFIED., .F., .F. ) 
 B_SPLINE_CURVE_WITH_KNOTS ( ( 3, 2, 2, 2, 3 ),
 ( 0.4395833333333333259, 0.4402777777777777679, 0.4416666666666666519, 0.4430555555555555358, 0.4437499999999999778 ),
 .UNSPECIFIED. ) 
 CURVE ( )  GEOMETRIC_REPRESENTATION_ITEM ( )  RATIONAL_B_SPLINE_CURVE ( ( 0.9330127018922194093, 0.9330127018922194093, 1.000000000000000000, 0.8660254037844387076, 1.000000000000000000, 0.8660254037844387076, 1.000000000000000000, 0.9330127018922194093, 0.9330127018922194093 ) ) 
 REPRESENTATION_ITEM ( '' )  );
#63363 = DIRECTION ( 'NONE',  ( -0.6485228581062915110, 0.000000000000000000, -0.7611951803011149931 ) ) ;
#63364 = CARTESIAN_POINT ( 'NONE',  ( 2.499999999999998668, -62.33333333333333570, -4.330127018922193649 ) ) ;
#63365 = CARTESIAN_POINT ( 'NONE',  ( -3.152801135295367096, -156.3125000013656063, -3.152801135295367541 ) ) ;
#63366 = CARTESIAN_POINT ( 'NONE',  ( 4.458734125000001214, -40.14583333196772941, 2.574251347313718519 ) ) ;
#63367 = CARTESIAN_POINT ( 'NONE',  ( -54.60164318462004474, -149.5000000027312126, -4.984105922594373794 ) ) ;
#63368 = CARTESIAN_POINT ( 'NONE',  ( 3.535533905932736864, -163.1250000000000284, 3.535533905932738641 ) ) ;
#63369 = CARTESIAN_POINT ( 'NONE',  ( -4.999999999999998224, -29.91666666666667140, 2.886751345948131764 ) ) ;
#63370 = CARTESIAN_POINT ( 'NONE',  ( -50.70258187064364108, -127.3750000013656205, 2.196230717870141014 ) ) ;
#63371 = VECTOR ( 'NONE', #55769, 1000.000000000000000 ) ;
#63372 = CARTESIAN_POINT ( 'NONE',  ( -4.458734124999999437, -3.562499998634407916, 0.000000000000000000 ) ) ;
#63373 = VECTOR ( 'NONE', #33336, 1000.000000000000000 ) ;
#63374 = CARTESIAN_POINT ( 'NONE',  ( 4.458734125000001214, -46.14583333196773651, 2.574251347313718519 ) ) ;
#63375 = CARTESIAN_POINT ( 'NONE',  ( -4.458734125000000326, -148.0000000013655779, -1.846868145590735644 ) ) ;
#63376 = CARTESIAN_POINT ( 'NONE',  ( -3.152548672688508926E-16, -87.81249999863439371, -5.148502694627439702 ) ) ;
#63377 = DIRECTION ( 'NONE',  ( -0.000000000000000000, 1.000000000000000000, -0.000000000000000000 ) ) ;
#63378 = VERTEX_POINT ( 'NONE', #26081 ) ;
#63379 = CARTESIAN_POINT ( 'NONE',  ( -1.339745962155613812, -47.20534180126147561, -5.000000000000000000 ) ) ;
#63380 = CARTESIAN_POINT ( 'NONE',  ( -4.458734124999999437, 29.43750000136559208, 0.000000000000000000 ) ) ;
#63381 = CARTESIAN_POINT ( 'NONE',  ( -57.46284108482265651, -151.0625000027312410, 4.819101127000239515 ) ) ;
#63382 =( BOUNDED_CURVE ( )  B_SPLINE_CURVE ( 2, ( #34169, #37202, #3424, #9411, #4588, #23040, #24531, #38997, #47168 ),
 .UNSPECIFIED., .F., .F. ) 
 B_SPLINE_CURVE_WITH_KNOTS ( ( 3, 2, 2, 2, 3 ),
 ( 0.7017857142857142350, 0.7023809523809523281, 0.7035714285714286254, 0.7047619047619048116, 0.7053571428571429047 ),
 .UNSPECIFIED. ) 
 CURVE ( )  GEOMETRIC_REPRESENTATION_ITEM ( )  RATIONAL_B_SPLINE_CURVE ( ( 0.9330127018922194093, 0.9330127018922194093, 1.000000000000000000, 0.8660254037844387076, 1.000000000000000000, 0.8660254037844387076, 1.000000000000000000, 0.9330127018922194093, 0.9330127018922194093 ) ) 
 REPRESENTATION_ITEM ( '' )  );
#63383 = CARTESIAN_POINT ( 'NONE',  ( -7.894787914004607998, 0.7647108141804108694, -7.591390474663421095 ) ) ;
#63384 = EDGE_LOOP ( 'NONE', ( #414, #57759, #53229, #5915 ) ) ;
#63385 = CARTESIAN_POINT ( 'NONE',  ( -5.000000000000000000, -70.95833333060214443, -2.886751345948128211 ) ) ;
#63386 = CARTESIAN_POINT ( 'NONE',  ( 2.229367062500001939, -11.22916666530107044, 3.861377020970579999 ) ) ;
#63387 = CARTESIAN_POINT ( 'NONE',  ( 5.000000000000000000, -105.3749999972688158, -6.123233995736766282E-16 ) ) ;
#63388 = CARTESIAN_POINT ( 'NONE',  ( -4.458734124999999437, -0.3958333319677397322, -2.574251347313719407 ) ) ;
#63389 = CARTESIAN_POINT ( 'NONE',  ( 1.339745962155615144, -73.58034179853028434, 4.999999999999999112 ) ) ;
#63390 = CARTESIAN_POINT ( 'NONE',  ( -3.152801135295367096, -153.0625000013656063, -3.152801135295367541 ) ) ;
#63391 = CARTESIAN_POINT ( 'NONE',  ( -4.458734124999999437, 20.35416666803225993, -2.574251347313719407 ) ) ;
#63392 = EDGE_LOOP ( 'NONE', ( #29008, #30614, #62231, #17518 ) ) ;
#63393 = CARTESIAN_POINT ( 'NONE',  ( -4.458734124999999437, -91.39583333196773651, -2.574251347313719407 ) ) ;
#63394 = LINE ( 'NONE', #9038, #20253 ) ;
#63395 = CARTESIAN_POINT ( 'NONE',  ( -6.972266317189433020E-16, -12.12499999726881406, -5.000000000000000000 ) ) ;
#63396 = CARTESIAN_POINT ( 'NONE',  ( 4.458734124999999437, -14.81249999863440436, -5.460374474430324690E-16 ) ) ;
#63397 = DIRECTION ( 'NONE',  ( 0.000000000000000000, 0.000000000000000000, 1.000000000000000000 ) ) ;
#63398 = CARTESIAN_POINT ( 'NONE',  ( -58.24261429053147765, -137.2500000000000000, -3.805975901505573855 ) ) ;
#63399 = CARTESIAN_POINT ( 'NONE',  ( -51.60603307380591787, -152.9375000013656063, -2.891590998281053704 ) ) ;
#63400 = EDGE_CURVE ( 'NONE', #19094, #45889, #51797, .T. ) ;
#63401 = CARTESIAN_POINT ( 'NONE',  ( 5.000000000000000000, -41.29166666393548013, -2.886751345948129988 ) ) ;
#63402 = LINE ( 'NONE', #34110, #17379 ) ;
#63403 = CARTESIAN_POINT ( 'NONE',  ( 9.457646018065525792E-16, 19.93750000136559208, 5.148502694627439702 ) ) ;
#63404 = CARTESIAN_POINT ( 'NONE',  ( -1.339745962155610925, -71.79465819873850307, 5.000000000000000000 ) ) ;
#63405 = ORIENTED_EDGE ( 'NONE', *, *, #5996, .T. ) ;
#63406 = CARTESIAN_POINT ( 'NONE',  ( -4.458734124999997661, 19.77083333469893134, 2.574251347313722516 ) ) ;
#63407 = CARTESIAN_POINT ( 'NONE',  ( 4.458734124999998549, -59.72916666530106511, -2.574251347313721627 ) ) ;
#63408 = CARTESIAN_POINT ( 'NONE',  ( -4.458734124999999437, -9.645833331967738289, -2.574251347313719407 ) ) ;
#63409 = AXIS2_PLACEMENT_3D ( 'NONE', #56918, #12836, #8342 ) ;
#63410 = DIRECTION ( 'NONE',  ( -0.000000000000000000, 1.000000000000000000, -0.000000000000000000 ) ) ;
#63411 = CARTESIAN_POINT ( 'NONE',  ( 5.000000000000000000, 8.583333333333330373, -2.886751345948129988 ) ) ;
#63412 = CARTESIAN_POINT ( 'NONE',  ( -4.458734124999999437, -166.9375000013655779, -5.460374474430324690E-16 ) ) ;
#63413 = CARTESIAN_POINT ( 'NONE',  ( -2.499999999999996447, -98.70833333060214443, 4.330127018922195425 ) ) ;
#63414 = CARTESIAN_POINT ( 'NONE',  ( -4.458734124999999437, -51.31249999863440792, 0.000000000000000000 ) ) ;
#63415 = CARTESIAN_POINT ( 'NONE',  ( 2.500000000000002220, -90.54166666393547303, 4.330127018922192761 ) ) ;
#63416 = AXIS2_PLACEMENT_3D ( 'NONE', #14508, #34776, #44095 ) ;
#63417 = VECTOR ( 'NONE', #20605, 1000.000000000000000 ) ;
#63418 = DIRECTION ( 'NONE',  ( -0.000000000000000000, 1.000000000000000000, -0.000000000000000000 ) ) ;
#63419 = CARTESIAN_POINT ( 'NONE',  ( 4.458734125000000326, -91.14583333196773651, 2.574251347313718519 ) ) ;
#63420 = CARTESIAN_POINT ( 'NONE',  ( -1.846868145590737420, -154.0000000013656063, 4.458734124999997661 ) ) ;
#63421 = CARTESIAN_POINT ( 'NONE',  ( -4.999999999999999112, -36.91666666666667140, 2.886751345948131764 ) ) ;
#63422 = PLANE ( 'NONE',  #63416 ) ;
#63423 = EDGE_CURVE ( 'NONE', #53577, #19571, #41002, .T. ) ;
#63424 = CARTESIAN_POINT ( 'NONE',  ( -9.184850993605147944E-16, -167.3750000027312126, 5.000000000000000000 ) ) ;
#63425 = VERTEX_POINT ( 'NONE', #48015 ) ;
#63426 = CARTESIAN_POINT ( 'NONE',  ( 4.458734125000001214, -101.8958333319677365, 2.574251347313718519 ) ) ;
#63427 = CARTESIAN_POINT ( 'NONE',  ( 9.457646018065525792E-16, 3.687500001365594748, 5.148502694627439702 ) ) ;
#63428 = LINE ( 'NONE', #29624, #6252 ) ;
#63429 = ADVANCED_FACE ( 'NONE', ( #61887 ), #33827, .F. ) ;
#63430 = CARTESIAN_POINT ( 'NONE',  ( -3.535250795749689387E-16, 0.7500000000000007772, -5.773502691896257311 ) ) ;
#63431 = CARTESIAN_POINT ( 'NONE',  ( -2.229367062500000163, -61.47916666530106511, -3.861377020970580443 ) ) ;
#63432 = CARTESIAN_POINT ( 'NONE',  ( 0.000000000000000000, -170.0000000000000000, 0.000000000000000000 ) ) ;
#63433 = EDGE_CURVE ( 'NONE', #36069, #29985, #39337, .T. ) ;
#63434 = CARTESIAN_POINT ( 'NONE',  ( -5.000000000000000000, -2.958333330602146649, -2.886751345948128211 ) ) ;
#63436 = ORIENTED_EDGE ( 'NONE', *, *, #54318, .T. ) ;
#63435 = CARTESIAN_POINT ( 'NONE',  ( -4.458734124999999437, -28.39583333196774007, -2.574251347313719407 ) ) ;
#63437 = CARTESIAN_POINT ( 'NONE',  ( -6.972266317189433020E-16, -48.12499999726880873, -5.000000000000000000 ) ) ;
#63438 = LINE ( 'NONE', #19035, #36419 ) ;
#63439 = CARTESIAN_POINT ( 'NONE',  ( -2.499999999999996447, 25.16666666666666430, 4.330127018922195425 ) ) ;
#63440 = CARTESIAN_POINT ( 'NONE',  ( -3.535250795749689387E-16, -47.25000000000000000, -5.773502691896257311 ) ) ;
#63442 = CARTESIAN_POINT ( 'NONE',  ( 4.458734125000001214, -25.14583333196774007, 2.574251347313718519 ) ) ;
#63441 = LINE ( 'NONE', #38970, #36595 ) ;
#63443 = CARTESIAN_POINT ( 'NONE',  ( -6.972266317189433020E-16, -79.12499999726881583, -5.000000000000000000 ) ) ;
#63444 = CARTESIAN_POINT ( 'NONE',  ( -4.458734124999999437, -72.31249999863439371, 0.000000000000000000 ) ) ;
#63445 = CARTESIAN_POINT ( 'NONE',  ( -4.458734125000001214, -144.1250000013655779, 1.846868145590734089 ) ) ;
#63446 = CARTESIAN_POINT ( 'NONE',  ( -2.229367062499996610, -79.14583333196773651, 3.861377020970582219 ) ) ;
#63447 = CARTESIAN_POINT ( 'NONE',  ( -54.64476657466781973, -138.0625000013656063, -4.444560631937228834 ) ) ;
#63448 = CARTESIAN_POINT ( 'NONE',  ( 4.458734125000001214, -29.14583333196774362, 2.574251347313718519 ) ) ;
#63449 = CARTESIAN_POINT ( 'NONE',  ( -5.000000000000000000, -67.87499999726881583, 0.000000000000000000 ) ) ;
#63450 = ORIENTED_EDGE ( 'NONE', *, *, #15706, .T. ) ;
#63451 = DIRECTION ( 'NONE',  ( 0.000000000000000000, 0.000000000000000000, 1.000000000000000000 ) ) ;
#63452 = ORIENTED_EDGE ( 'NONE', *, *, #13286, .T. ) ;
#63453 = CARTESIAN_POINT ( 'NONE',  ( -4.458734124999998549, -74.47916666530106511, 2.574251347313722516 ) ) ;
#63454 = CARTESIAN_POINT ( 'NONE',  ( -1.339745962155617365, 22.33034180399266688, 4.999999999999998224 ) ) ;
#63455 = VERTEX_POINT ( 'NONE', #22647 ) ;
#63456 = CARTESIAN_POINT ( 'NONE',  ( 1.339745962155612258, 27.29465819873851729, 5.000000000000000888 ) ) ;
#63457 = CARTESIAN_POINT ( 'NONE',  ( -1.049326080737009628E-13, -2.750000000000003109, 5.000000000000000000 ) ) ;
#63458 = CARTESIAN_POINT ( 'NONE',  ( 4.458734124999999437, -61.06249999863440081, -5.460374474430324690E-16 ) ) ;
#63459 = VECTOR ( 'NONE', #28356, 1000.000000000000000 ) ;
#63460 = CARTESIAN_POINT ( 'NONE',  ( 2.229367062499998831, 4.104166668032260823, -3.861377020970580887 ) ) ;
#63461 = EDGE_LOOP ( 'NONE', ( #813, #18712, #30584, #33245 ) ) ;
#63462 =( BOUNDED_CURVE ( )  B_SPLINE_CURVE ( 2, ( #1042, #26413, #11291, #20648, #50543, #26097, #60521, #40252, #15812 ),
 .UNSPECIFIED., .F., .F. ) 
 B_SPLINE_CURVE_WITH_KNOTS ( ( 3, 2, 2, 2, 3 ),
 ( 0.2589285714285714524, 0.2595238095238095455, 0.2607142857142857317, 0.2619047619047619180, 0.2625000000000000111 ),
 .UNSPECIFIED. ) 
 CURVE ( )  GEOMETRIC_REPRESENTATION_ITEM ( )  RATIONAL_B_SPLINE_CURVE ( ( 0.9330127018922194093, 0.9330127018922194093, 1.000000000000000000, 0.8660254037844387076, 1.000000000000000000, 0.8660254037844387076, 1.000000000000000000, 0.9330127018922194093, 0.9330127018922194093 ) ) 
 REPRESENTATION_ITEM ( '' )  );
#63463 = CYLINDRICAL_SURFACE ( 'NONE', #63539, 5.000000000000000000 ) ;
#63464 = CARTESIAN_POINT ( 'NONE',  ( -2.229367062500000163, 10.52083333469892779, -3.861377020970580443 ) ) ;
#63465 = CARTESIAN_POINT ( 'NONE',  ( -54.64476657466781973, -143.8125000013656063, -4.444560631937228834 ) ) ;
#63466 = CARTESIAN_POINT ( 'NONE',  ( 5.000000000000000888, -92.45833333060213022, 2.886751345948126879 ) ) ;
#63467 = CARTESIAN_POINT ( 'NONE',  ( 1.846868145590735200, -165.2500000013655779, -4.458734124999999437 ) ) ;
#63468 = EDGE_LOOP ( 'NONE', ( #5796, #50078, #59473, #29114 ) ) ;
#63469 = CARTESIAN_POINT ( 'NONE',  ( 9.457646018065525792E-16, -75.06249999863440792, 5.148502694627439702 ) ) ;
#63470 = CARTESIAN_POINT ( 'NONE',  ( -2.500000000000000444, -52.04166666393547303, -4.330127018922193649 ) ) ;
#63471 = CARTESIAN_POINT ( 'NONE',  ( 4.458734124999999437, 1.187500001365596081, -5.460374474430324690E-16 ) ) ;
#63472 =( BOUNDED_CURVE ( )  B_SPLINE_CURVE ( 2, ( #26326, #45943, #41109, #60756, #16680, #36301, #41427, #61076, #27280 ),
 .UNSPECIFIED., .F., .F. ) 
 B_SPLINE_CURVE_WITH_KNOTS ( ( 3, 2, 2, 2, 3 ),
 ( 0.008333333333333340157, 0.01250000000000001110, 0.01666666666666668031, 0.02083333333333334952, 0.02500000000000002220 ),
 .UNSPECIFIED. ) 
 CURVE ( )  GEOMETRIC_REPRESENTATION_ITEM ( )  RATIONAL_B_SPLINE_CURVE ( ( 0.9999999999999998890, 0.9238795325112868495, 1.000000000000000000, 0.9238795325112867385, 1.000000000000000000, 0.9238795325112867385, 1.000000000000000000, 0.9238795325112864054, 1.000000000000000444 ) ) 
 REPRESENTATION_ITEM ( '' )  );
#63473 = CARTESIAN_POINT ( 'NONE',  ( 1.975475456537005874E-15, -42.62499999726880873, 5.000000000000000000 ) ) ;
#63474 = CARTESIAN_POINT ( 'NONE',  ( 9.457646018065525792E-16, -66.31249999863440792, 5.148502694627439702 ) ) ;
#63475 = CARTESIAN_POINT ( 'NONE',  ( -4.999999999999999112, -23.79166666393548013, 2.886751345948131764 ) ) ;
#63476 = CARTESIAN_POINT ( 'NONE',  ( 1.975475456537005874E-15, 24.24999999999999645, 5.000000000000000000 ) ) ;
#63477 = CARTESIAN_POINT ( 'NONE',  ( -1.339745962155610925, -82.66965819600731891, 5.000000000000000000 ) ) ;
#63478 = CARTESIAN_POINT ( 'NONE',  ( 5.000000000000000000, -58.50000000000000000, -6.123233995736766282E-16 ) ) ;
#63479 = CARTESIAN_POINT ( 'NONE',  ( -4.458734124999999437, -44.31249999863440081, 0.000000000000000000 ) ) ;
#63480 = CARTESIAN_POINT ( 'NONE',  ( 2.229367062499998831, -24.89583333196773651, -3.861377020970580887 ) ) ;
#63481 = CARTESIAN_POINT ( 'NONE',  ( -4.458734124999999437, 5.437500001365592972, 0.000000000000000000 ) ) ;
#63482 = LINE ( 'NONE', #62228, #42280 ) ;
#63483 = CARTESIAN_POINT ( 'NONE',  ( 5.000000000000000888, 25.41666666666666430, 2.886751345948126879 ) ) ;
#63484 = CARTESIAN_POINT ( 'NONE',  ( 5.000000000000000000, -149.1250000027312126, 0.000000000000000000 ) ) ;
#63485 = CARTESIAN_POINT ( 'NONE',  ( -51.19402409849444524, -154.5000000000000284, -3.242614290531456334 ) ) ;
#63486 = CARTESIAN_POINT ( 'NONE',  ( -4.458734124999998549, -39.22916666530107221, 2.574251347313722516 ) ) ;
#63487 = CARTESIAN_POINT ( 'NONE',  ( 2.500000000000002220, -71.54166666393547303, 4.330127018922192761 ) ) ;
#63488 = CARTESIAN_POINT ( 'NONE',  ( -52.10840900171896806, -144.4375000013656063, 3.393966926194110556 ) ) ;
#63489 = CARTESIAN_POINT ( 'NONE',  ( -3.535533905932737309, -143.6250000000000000, -3.535533905932738197 ) ) ;
#63490 = CARTESIAN_POINT ( 'NONE',  ( -4.458734124999999437, -74.64583333196773651, -2.574251347313719407 ) ) ;
#63491 = CARTESIAN_POINT ( 'NONE',  ( -1.846868145590734756, -164.3750000013656063, -4.458734124999999437 ) ) ;
#63492 = CARTESIAN_POINT ( 'NONE',  ( 4.458734124999998549, -28.72916666530107221, -2.574251347313721627 ) ) ;
#63493 = CARTESIAN_POINT ( 'NONE',  ( -59.81910112700026616, -148.1875000000000284, -2.462841084822525506 ) ) ;
#63494 = CYLINDRICAL_SURFACE ( 'NONE', #33830, 5.000000000000000000 ) ;
#63495 = CARTESIAN_POINT ( 'NONE',  ( 2.499999999999998668, -21.33333333333333570, -4.330127018922193649 ) ) ;
#63496 = CARTESIAN_POINT ( 'NONE',  ( 1.846868145590736310, -145.6250000013655779, 4.458734124999999437 ) ) ;
#63497 = ORIENTED_EDGE ( 'NONE', *, *, #3872, .F. ) ;
#63498 = CARTESIAN_POINT ( 'NONE',  ( 4.458734124999998549, 26.02083333469892779, -2.574251347313721627 ) ) ;
#63499 = CARTESIAN_POINT ( 'NONE',  ( 0.000000000000000000, -170.0000000000000000, 0.000000000000000000 ) ) ;
#63500 = CARTESIAN_POINT ( 'NONE',  ( -2.229367062500000163, -57.72916666530107932, -3.861377020970580443 ) ) ;
#63501 = AXIS2_PLACEMENT_3D ( 'NONE', #35144, #1065, #40589 ) ;
#63502 = CARTESIAN_POINT ( 'NONE',  ( -2.499999999999996447, 27.29166666939785202, 4.330127018922195425 ) ) ;
#63503 = CARTESIAN_POINT ( 'NONE',  ( 2.499999999999998668, -90.20833333060214443, -4.330127018922193649 ) ) ;
#63504 = CARTESIAN_POINT ( 'NONE',  ( -2.500000000000000444, 17.83333333333333215, -4.330127018922193649 ) ) ;
#63505 = CARTESIAN_POINT ( 'NONE',  ( 6.158835246850667461E-14, 7.875000002731183280, -4.999999999999999112 ) ) ;
#63506 = CARTESIAN_POINT ( 'NONE',  ( 2.229367062500001939, -5.979166665301072214, 3.861377020970579999 ) ) ;
#63507 = CARTESIAN_POINT ( 'NONE',  ( 1.975475456537005874E-15, -22.74999999999999645, 5.000000000000000000 ) ) ;
#63508 = CARTESIAN_POINT ( 'NONE',  ( 2.071067811865518582, -165.3125000027312126, 4.999999999999957367 ) ) ;
#63509 = CARTESIAN_POINT ( 'NONE',  ( 2.500000000000002220, -89.54166666393547303, 4.330127018922192761 ) ) ;
#63510 = DIRECTION ( 'NONE',  ( 0.000000000000000000, 1.000000000000000000, 0.000000000000000000 ) ) ;
#63512 = CARTESIAN_POINT ( 'NONE',  ( 4.458734125000001214, -20.89583333196774007, 2.574251347313718519 ) ) ;
#63511 = CARTESIAN_POINT ( 'NONE',  ( 0.000000000000000000, -120.0000000000000000, 0.000000000000000000 ) ) ;
#63513 = FACE_OUTER_BOUND ( 'NONE', #21171, .T. ) ;
#63514 = CARTESIAN_POINT ( 'NONE',  ( 4.458734125000001214, -51.89583333196773651, 2.574251347313718519 ) ) ;
#63515 = CARTESIAN_POINT ( 'NONE',  ( -3.152801135295367985, -155.0625000013656063, 3.152801135295367096 ) ) ;
#63516 = CARTESIAN_POINT ( 'NONE',  ( 5.000000000000000000, -51.29166666393547303, -2.886751345948129988 ) ) ;
#63517 = ORIENTED_EDGE ( 'NONE', *, *, #61587, .F. ) ;
#63518 = CARTESIAN_POINT ( 'NONE',  ( -4.458734124999998549, 4.520833334698926009, 2.574251347313722516 ) ) ;
#63519 = VERTEX_POINT ( 'NONE', #7847 ) ;
#63521 = CARTESIAN_POINT ( 'NONE',  ( -4.999999999999998224, -2.916666666666664742, 2.886751345948131764 ) ) ;
#63520 = PLANE ( 'NONE',  #35824 ) ;
#63522 = CARTESIAN_POINT ( 'NONE',  ( 3.152801135295366208, -159.5625000013656063, 3.152801135295367985 ) ) ;
#63523 = ORIENTED_EDGE ( 'NONE', *, *, #5618, .F. ) ;
#63524 = UNCERTAINTY_MEASURE_WITH_UNIT (LENGTH_MEASURE( 1.000000000000000082E-05 ), #59255, 'distance_accuracy_value', 'NONE');
#63525 =( BOUNDED_CURVE ( )  B_SPLINE_CURVE ( 2, ( #20098, #44538, #19137, #494, #39704, #59344, #38754, #28486, #19460 ),
 .UNSPECIFIED., .F., .F. ) 
 B_SPLINE_CURVE_WITH_KNOTS ( ( 3, 2, 2, 2, 3 ),
 ( 0.4946428571428571619, 0.4952380952380952550, 0.4964285714285714413, 0.4976190476190476275, 0.4982142857142857206 ),
 .UNSPECIFIED. ) 
 CURVE ( )  GEOMETRIC_REPRESENTATION_ITEM ( )  RATIONAL_B_SPLINE_CURVE ( ( 0.9330127018922194093, 0.9330127018922194093, 1.000000000000000000, 0.8660254037844387076, 1.000000000000000000, 0.8660254037844387076, 1.000000000000000000, 0.9330127018922194093, 0.9330127018922194093 ) ) 
 REPRESENTATION_ITEM ( '' )  );
#63526 = CARTESIAN_POINT ( 'NONE',  ( 1.339745962155612702, -23.16965819600733312, -5.000000000000000000 ) ) ;
#63527 = CARTESIAN_POINT ( 'NONE',  ( -50.01589407740564042, -133.6250000000000284, 0.3983568153799778022 ) ) ;
#63528 = CARTESIAN_POINT ( 'NONE',  ( -1.339745962155613812, -30.08034179853029144, -5.000000000000000000 ) ) ;
#63529 = CARTESIAN_POINT ( 'NONE',  ( 4.458734124999998549, -41.97916666530107932, -2.574251347313721627 ) ) ;
#63530 = ORIENTED_EDGE ( 'NONE', *, *, #37716, .T. ) ;
#63531 = CARTESIAN_POINT ( 'NONE',  ( -5.000000000000000000, -46.00000000000000000, 0.000000000000000000 ) ) ;
#63532 = CARTESIAN_POINT ( 'NONE',  ( 2.229367062500001939, 21.02083333469892779, 3.861377020970579999 ) ) ;
#63533 = CARTESIAN_POINT ( 'NONE',  ( -6.972266317189433020E-16, -66.24999999999998579, -5.000000000000000000 ) ) ;
#63534 = ORIENTED_EDGE ( 'NONE', *, *, #3671, .F. ) ;
#63535 = CARTESIAN_POINT ( 'NONE',  ( -4.458734124999999437, 28.68750000136559208, 0.000000000000000000 ) ) ;
#63536 = CARTESIAN_POINT ( 'NONE',  ( -59.98410592259440222, -126.2500000027311984, -0.3983568153799752487 ) ) ;
#63537 = FACE_OUTER_BOUND ( 'NONE', #13049, .T. ) ;
#63538 = CARTESIAN_POINT ( 'NONE',  ( -50.45012647926553484, -135.0000000000000284, 0.5292737942098199033 ) ) ;
#63539 = AXIS2_PLACEMENT_3D ( 'NONE', #11317, #6511, #26123 ) ;
#63540 = CARTESIAN_POINT ( 'NONE',  ( 3.061616997868383141E-16, -168.7500000000000000, -5.000000000000000000 ) ) ;
#63541 = CARTESIAN_POINT ( 'NONE',  ( -3.152548672688508926E-16, -58.56249999863439371, -5.148502694627439702 ) ) ;
#63542 = CARTESIAN_POINT ( 'NONE',  ( 3.080866544135574259, 6.881514909250401324, -7.026396753507782478 ) ) ;
#63543 = CARTESIAN_POINT ( 'NONE',  ( -4.458734124999999437, 17.68750000136559208, 0.000000000000000000 ) ) ;
#63544 = VECTOR ( 'NONE', #11546, 1000.000000000000000 ) ;
#63545 = FACE_OUTER_BOUND ( 'NONE', #4776, .T. ) ;
#63546 = CARTESIAN_POINT ( 'NONE',  ( -2.229367062500000163, -47.72916666530106511, -3.861377020970580443 ) ) ;
#63547 = CARTESIAN_POINT ( 'NONE',  ( 5.000000000000000888, -10.45833333060214621, 2.886751345948126879 ) ) ;
#63548 = CARTESIAN_POINT ( 'NONE',  ( 5.000000000000000000, -31.41666666666667140, -2.886751345948130876 ) ) ;
#63549 = CARTESIAN_POINT ( 'NONE',  ( -2.499999999999996447, -19.70833333060214798, 4.330127018922195425 ) ) ;
#63550 = CYLINDRICAL_SURFACE ( 'NONE', #36643, 5.000000000000000000 ) ;
#63551 = CARTESIAN_POINT ( 'NONE',  ( -4.458734124999999437, -108.3124999986343937, 0.000000000000000000 ) ) ;
#63552 = EDGE_CURVE ( 'NONE', #19516, #50575, #57063, .T. ) ;
#63553 =( BOUNDED_CURVE ( )  B_SPLINE_CURVE ( 2, ( #28107, #19395, #14563, #37768, #9739, #29343, #48977, #57399, #32941 ),
 .UNSPECIFIED., .F., .F. ) 
 B_SPLINE_CURVE_WITH_KNOTS ( ( 3, 2, 2, 2, 3 ),
 ( 0.4089285714285714191, 0.4095238095238095122, 0.4107142857142856984, 0.4119047619047618847, 0.4124999999999999778 ),
 .UNSPECIFIED. ) 
 CURVE ( )  GEOMETRIC_REPRESENTATION_ITEM ( )  RATIONAL_B_SPLINE_CURVE ( ( 0.9330127018922194093, 0.9330127018922194093, 1.000000000000000000, 0.8660254037844387076, 1.000000000000000000, 0.8660254037844387076, 1.000000000000000000, 0.9330127018922194093, 0.9330127018922194093 ) ) 
 REPRESENTATION_ITEM ( '' )  );
#63554 = CARTESIAN_POINT ( 'NONE',  ( -4.458734124999999437, -8.562499998634406140, 0.000000000000000000 ) ) ;
#63555 = ORIENTED_EDGE ( 'NONE', *, *, #21984, .F. ) ;
#63556 = CARTESIAN_POINT ( 'NONE',  ( -1.339745962155613812, -81.20534180126146850, -5.000000000000000000 ) ) ;
#63557 = CARTESIAN_POINT ( 'NONE',  ( -4.458734124999999437, -96.31249999863440792, 0.000000000000000000 ) ) ;
#63558 = CARTESIAN_POINT ( 'NONE',  ( -2.071067811865475061, -160.8125000027311842, -5.000000000000000888 ) ) ;
#63559 = CARTESIAN_POINT ( 'NONE',  ( -3.152548672688508926E-16, -96.81249999863440792, -5.148502694627439702 ) ) ;
#63560 = LINE ( 'NONE', #50024, #48969 ) ;
#63561 = CARTESIAN_POINT ( 'NONE',  ( 2.500000000000002220, -51.54166666393547303, 4.330127018922192761 ) ) ;
#63562 = CARTESIAN_POINT ( 'NONE',  ( -1.339745962155613812, -37.08034179853029144, -5.000000000000000000 ) ) ;
#63563 = CARTESIAN_POINT ( 'NONE',  ( -59.59170313451811296, -129.5000000013656347, 1.485763867205729394 ) ) ;
#63564 = CARTESIAN_POINT ( 'NONE',  ( -54.64476657466781973, -147.8125000013656063, -4.444560631937228834 ) ) ;
#63565 = CARTESIAN_POINT ( 'NONE',  ( 4.458734124999999437, -16.81249999863440436, -5.460374474430324690E-16 ) ) ;
#63566 = CARTESIAN_POINT ( 'NONE',  ( -4.458734124999998549, 9.520833334698927786, 2.574251347313722516 ) ) ;
#63567 = CARTESIAN_POINT ( 'NONE',  ( -2.229367062500000163, -59.72916666530106511, -3.861377020970580443 ) ) ;
#63568 = CARTESIAN_POINT ( 'NONE',  ( -2.500000000000000444, -54.16666666666667140, -4.330127018922193649 ) ) ;
#63569 = CARTESIAN_POINT ( 'NONE',  ( 2.229367062499998831, -16.64583333196773651, -3.861377020970580887 ) ) ;
#63570 = CARTESIAN_POINT ( 'NONE',  ( 5.000000000000000888, -8.458333330602144429, 2.886751345948126879 ) ) ;
#63571 = CARTESIAN_POINT ( 'NONE',  ( -3.535533905932738641, -153.3750000000000000, 3.535533905932737309 ) ) ;
#63572 = CARTESIAN_POINT ( 'NONE',  ( -2.499999999999996447, -6.833333333333330373, 4.330127018922195425 ) ) ;
#63573 = ORIENTED_EDGE ( 'NONE', *, *, #4033, .F. ) ;
#63574 = CARTESIAN_POINT ( 'NONE',  ( 4.458734124999999437, -41.06249999863440081, -5.460374474430324690E-16 ) ) ;
#63575 = CARTESIAN_POINT ( 'NONE',  ( 3.061616997868383141E-16, -150.7500000000000284, -5.000000000000000000 ) ) ;
#63576 = CARTESIAN_POINT ( 'NONE',  ( 5.000000000000000000, -66.41666666666667140, -2.886751345948130876 ) ) ;
#63577 = FACE_OUTER_BOUND ( 'NONE', #36612, .T. ) ;
#63578 = CARTESIAN_POINT ( 'NONE',  ( -2.229367062500000163, -83.47916666530106511, -3.861377020970580443 ) ) ;
#63579 = CARTESIAN_POINT ( 'NONE',  ( -2.229367062500000163, 19.27083333469892779, -3.861377020970580443 ) ) ;
#63580 = CARTESIAN_POINT ( 'NONE',  ( -4.458734124999998549, 9.770833334698927786, 2.574251347313722516 ) ) ;
#63581 = CARTESIAN_POINT ( 'NONE',  ( -1.339745962155613812, -48.20534180126148271, -5.000000000000000000 ) ) ;
#63582 = DIRECTION ( 'NONE',  ( -0.000000000000000000, 1.000000000000000000, -0.000000000000000000 ) ) ;
#63583 = CARTESIAN_POINT ( 'NONE',  ( -3.152548672688508926E-16, -86.81249999863439371, -5.148502694627439702 ) ) ;
#63584 = CARTESIAN_POINT ( 'NONE',  ( -2.229367062500000163, 22.27083333469892423, -3.861377020970580443 ) ) ;
#63585 = CARTESIAN_POINT ( 'NONE',  ( 5.000000000000000000, -77.50000000000000000, -6.123233995736766282E-16 ) ) ;
#63586 = CARTESIAN_POINT ( 'NONE',  ( -3.535250795749689387E-16, 11.87500000273118594, -5.773502691896257311 ) ) ;
#63587 = ORIENTED_EDGE ( 'NONE', *, *, #14160, .T. ) ;
#63588 = CARTESIAN_POINT ( 'NONE',  ( 5.000000000000000000, -79.41666666666665719, -2.886751345948130876 ) ) ;
#63589 = ORIENTED_EDGE ( 'NONE', *, *, #63263, .F. ) ;
#63591 = CARTESIAN_POINT ( 'NONE',  ( -2.499999999999996447, -33.83333333333332860, 4.330127018922195425 ) ) ;
#63590 = CARTESIAN_POINT ( 'NONE',  ( 1.975475456537005874E-15, -85.75000000000000000, 5.000000000000000000 ) ) ;
#63592 = CARTESIAN_POINT ( 'NONE',  ( -4.458734124999999437, -38.31249999863439371, 0.000000000000000000 ) ) ;
#63593 = VECTOR ( 'NONE', #13226, 1000.000000000000000 ) ;
#63594 = CARTESIAN_POINT ( 'NONE',  ( 5.000000000000000888, -32.45833333060215153, 2.886751345948126879 ) ) ;
#63596 = VERTEX_POINT ( 'NONE', #18436 ) ;
#63595 = CARTESIAN_POINT ( 'NONE',  ( -2.229367062499996610, -68.14583333196773651, 3.861377020970582219 ) ) ;
#63597 = CARTESIAN_POINT ( 'NONE',  ( -51.60603307380591787, -151.1875000013656063, -2.891590998281053704 ) ) ;
#63598 = CARTESIAN_POINT ( 'NONE',  ( -4.458734124999999437, -12.31249999863440259, 0.000000000000000000 ) ) ;
#63600 = ORIENTED_EDGE ( 'NONE', *, *, #11941, .F. ) ;
#63599 = CARTESIAN_POINT ( 'NONE',  ( -2.229367062500000163, -12.72916666530107044, -3.861377020970580443 ) ) ;
#63601 = CARTESIAN_POINT ( 'NONE',  ( 1.060575238724906964E-15, -81.75000000000000000, 5.773502691896257311 ) ) ;
#63602 = DIRECTION ( 'NONE',  ( 0.000000000000000000, 0.000000000000000000, 1.000000000000000000 ) ) ;
#63603 = CARTESIAN_POINT ( 'NONE',  ( -4.458734124999999437, -57.64583333196773651, -2.574251347313719407 ) ) ;
#63604 = CARTESIAN_POINT ( 'NONE',  ( -5.000000000000000000, -84.87499999726880162, 0.000000000000000000 ) ) ;
#63606 = ORIENTED_EDGE ( 'NONE', *, *, #5070, .T. ) ;
#63605 = CARTESIAN_POINT ( 'NONE',  ( 5.000000000000000888, 3.541666669397852019, 2.886751345948126879 ) ) ;
#63607 = CARTESIAN_POINT ( 'NONE',  ( -51.19402409849444524, -146.5000000000000284, -3.242614290531456334 ) ) ;
#63608 = EDGE_CURVE ( 'NONE', #19824, #49290, #52301, .T. ) ;
#63609 = CARTESIAN_POINT ( 'NONE',  ( -2.229367062500000163, -28.72916666530107221, -3.861377020970580443 ) ) ;
#63610 = ORIENTED_EDGE ( 'NONE', *, *, #61924, .F. ) ;
#63611 = CARTESIAN_POINT ( 'NONE',  ( 4.458734125000000326, -167.6250000013655779, -1.846868145590734978 ) ) ;
#63612 = CARTESIAN_POINT ( 'NONE',  ( -4.458734124999999437, -107.5624999986343937, 0.000000000000000000 ) ) ;
#63613 = CARTESIAN_POINT ( 'NONE',  ( 5.000000000000000000, -8.374999997268814056, -6.123233995736766282E-16 ) ) ;
#63614 = ORIENTED_EDGE ( 'NONE', *, *, #14250, .F. ) ;
#63615 = CARTESIAN_POINT ( 'NONE',  ( -54.64476657466781973, -148.0625000013656063, -4.444560631937228834 ) ) ;
#63616 = CARTESIAN_POINT ( 'NONE',  ( -57.46284108482265651, -140.0625000027312126, 4.819101127000239515 ) ) ;
#63617 = CARTESIAN_POINT ( 'NONE',  ( -2.229367062500000163, -39.47916666530107221, -3.861377020970580443 ) ) ;
#63618 = CARTESIAN_POINT ( 'NONE',  ( -1.846868145590734756, -146.3750000013655779, -4.458734124999999437 ) ) ;
#63619 = CARTESIAN_POINT ( 'NONE',  ( -6.972266317189433020E-16, 22.74999999999999645, -5.000000000000000000 ) ) ;
#63620 = CARTESIAN_POINT ( 'NONE',  ( 1.339745962155613146, 29.70534180126147561, -4.999999999999999112 ) ) ;
#63621 = CARTESIAN_POINT ( 'NONE',  ( 2.229367062499998831, -13.64583333196774184, -3.861377020970580887 ) ) ;
#63622 = CARTESIAN_POINT ( 'NONE',  ( -2.229367062500000163, -98.72916666530105090, -3.861377020970580443 ) ) ;
#63623 = ORIENTED_EDGE ( 'NONE', *, *, #15502, .T. ) ;
#63624 = EDGE_CURVE ( 'NONE', #24216, #7754, #7770, .T. ) ;
#63625 = CARTESIAN_POINT ( 'NONE',  ( 4.458734124999999437, -144.6875000013656063, 0.000000000000000000 ) ) ;
#63626 = CARTESIAN_POINT ( 'NONE',  ( 4.458734124999998549, -30.97916666530107577, -2.574251347313721627 ) ) ;
#63627 = EDGE_CURVE ( 'NONE', #2700, #39916, #23269, .T. ) ;
#63628 = CARTESIAN_POINT ( 'NONE',  ( -51.19402409849444524, -153.5000000000000284, -3.242614290531456334 ) ) ;
#63629 = CARTESIAN_POINT ( 'NONE',  ( -56.48576386720575471, -134.7500000013656063, -4.591703134518078322 ) ) ;
#63630 = CARTESIAN_POINT ( 'NONE',  ( 4.458734125000001214, -69.14583333196773651, 2.574251347313718519 ) ) ;
#63631 = DIRECTION ( 'NONE',  ( -0.000000000000000000, -0.000000000000000000, -1.000000000000000000 ) ) ;
#63632 = CARTESIAN_POINT ( 'NONE',  ( -1.339745962155610925, -69.79465819873850307, 5.000000000000000000 ) ) ;
#63633 = CARTESIAN_POINT ( 'NONE',  ( 0.000000000000000000, -120.0000000000000000, 0.000000000000000000 ) ) ;
#63634 = MECHANICAL_DESIGN_GEOMETRIC_PRESENTATION_REPRESENTATION (  '', ( #55424 ), #61631 ) ;
#63635 = CARTESIAN_POINT ( 'NONE',  ( -3.152548672688508926E-16, 7.187500001365594748, -5.148502694627439702 ) ) ;
#63636 = ORIENTED_EDGE ( 'NONE', *, *, #24773, .T. ) ;
#63637 = CARTESIAN_POINT ( 'NONE',  ( 1.339745962155615144, 2.294658198738519950, 4.999999999999999112 ) ) ;
#63639 = CARTESIAN_POINT ( 'NONE',  ( 9.457646018065525792E-16, -29.06249999863440081, 5.148502694627439702 ) ) ;
#63638 = CARTESIAN_POINT ( 'NONE',  ( 5.000000000000000000, -95.50000000000000000, -6.123233995736766282E-16 ) ) ;
#63640 = CYLINDRICAL_SURFACE ( 'NONE', #53123, 5.000000000000000000 ) ;
#63641 = CARTESIAN_POINT ( 'NONE',  ( -2.229367062499996610, -78.39583333196773651, 3.861377020970582219 ) ) ;
#63642 = AXIS2_PLACEMENT_3D ( 'NONE', #4170, #23785, #43387 ) ;
#63643 = CARTESIAN_POINT ( 'NONE',  ( -2.229367062499996610, 23.60416666803225993, 3.861377020970582219 ) ) ;
#63644 = LINE ( 'NONE', #59130, #8910 ) ;
#63645 = ADVANCED_FACE ( 'NONE', ( #32597 ), #52543, .T. ) ;
#63646 = CARTESIAN_POINT ( 'NONE',  ( -50.70258187064364108, -142.1250000013656063, 2.196230717870141014 ) ) ;
#63647 = CARTESIAN_POINT ( 'NONE',  ( 9.457646018065525792E-16, -0.06249999863440491854, 5.148502694627439702 ) ) ;
#63648 = CARTESIAN_POINT ( 'NONE',  ( 2.229367062500001939, 24.77083333469892779, 3.861377020970579999 ) ) ;
#63649 = CARTESIAN_POINT ( 'NONE',  ( 9.457646018065525792E-16, -45.31249999863440081, 5.148502694627439702 ) ) ;
#63650 = CARTESIAN_POINT ( 'NONE',  ( -49.85088928181150436, -144.5625000000000284, -1.666127454062680480 ) ) ;
#63651 = CARTESIAN_POINT ( 'NONE',  ( -2.229367062499996610, 3.854166668032260823, 3.861377020970582219 ) ) ;
#63652 = ORIENTED_EDGE ( 'NONE', *, *, #39344, .T. ) ;
#63653 = CARTESIAN_POINT ( 'NONE',  ( -4.458734124999999437, -22.56249999863440436, 0.000000000000000000 ) ) ;
#63654 = CARTESIAN_POINT ( 'NONE',  ( 4.458734124999999437, -68.81249999863439371, -5.460374474430324690E-16 ) ) ;
#63655 = CARTESIAN_POINT ( 'NONE',  ( -4.999999999999999112, -103.7916666639354730, 2.886751345948131764 ) ) ;
#63656 =( BOUNDED_CURVE ( )  B_SPLINE_CURVE ( 2, ( #45116, #10384, #15540, #34489, #35159, #54774, #10706, #5889, #31596 ),
 .UNSPECIFIED., .F., .F. ) 
 B_SPLINE_CURVE_WITH_KNOTS ( ( 3, 2, 2, 2, 3 ),
 ( 0.8479166666666666519, 0.8486111111111110938, 0.8499999999999999778, 0.8513888888888888618, 0.8520833333333333037 ),
 .UNSPECIFIED. ) 
 CURVE ( )  GEOMETRIC_REPRESENTATION_ITEM ( )  RATIONAL_B_SPLINE_CURVE ( ( 0.9330127018922194093, 0.9330127018922194093, 1.000000000000000000, 0.8660254037844387076, 1.000000000000000000, 0.8660254037844387076, 1.000000000000000000, 0.9330127018922194093, 0.9330127018922194093 ) ) 
 REPRESENTATION_ITEM ( '' )  );
#63657 = CARTESIAN_POINT ( 'NONE',  ( 2.229367062499998831, 26.35416666803225993, -3.861377020970580887 ) ) ;
#63658 = CARTESIAN_POINT ( 'NONE',  ( -4.999999999999998224, 10.08333333333333393, 2.886751345948131764 ) ) ;
#63659 = ADVANCED_FACE ( 'NONE', ( #32919 ), #52223, .T. ) ;
#63660 = CARTESIAN_POINT ( 'NONE',  ( -4.458734124999997661, -110.4791666653010793, 2.574251347313722516 ) ) ;
#63661 = CARTESIAN_POINT ( 'NONE',  ( -3.152548672688508926E-16, -74.81249999863439371, -5.148502694627439702 ) ) ;
#63662 = CARTESIAN_POINT ( 'NONE',  ( 5.000000000000000000, -55.49999999999999289, -6.123233995736766282E-16 ) ) ;
#63663 = CARTESIAN_POINT ( 'NONE',  ( 0.000000000000000000, -120.0000000000000000, 0.000000000000000000 ) ) ;
#63664 = DIRECTION ( 'NONE',  ( 0.000000000000000000, 0.000000000000000000, 1.000000000000000000 ) ) ;
#63665 = VERTEX_POINT ( 'NONE', #13295 ) ;
#63666 = CARTESIAN_POINT ( 'NONE',  ( -2.499999999999996447, -26.83333333333333570, 4.330127018922195425 ) ) ;
#63667 = CARTESIAN_POINT ( 'NONE',  ( 5.000000000000000000, -6.291666663935481019, -2.886751345948130876 ) ) ;
#63668 = CARTESIAN_POINT ( 'NONE',  ( -2.499999999999996447, -18.83333333333333215, 4.330127018922195425 ) ) ;
#63669 = CARTESIAN_POINT ( 'NONE',  ( 4.458734124999999437, -22.81249999863440436, -5.460374474430324690E-16 ) ) ;
#63670 = CARTESIAN_POINT ( 'NONE',  ( 4.458734125000000326, -81.89583333196773651, 2.574251347313718519 ) ) ;
#63671 = CARTESIAN_POINT ( 'NONE',  ( 4.458734125000000326, -166.6250000013656063, -1.846868145590734978 ) ) ;
#63672 = CARTESIAN_POINT ( 'NONE',  ( 2.499999999999998668, -18.20833333060214798, -4.330127018922193649 ) ) ;
#63673 = CARTESIAN_POINT ( 'NONE',  ( 9.457646018065525792E-16, -49.06249999863440792, 5.148502694627439702 ) ) ;
#63674 = CARTESIAN_POINT ( 'NONE',  ( -4.999999999999998224, -64.91666666666665719, 2.886751345948131764 ) ) ;
#63675 = NEXT_ASSEMBLY_USAGE_OCCURRENCE ( 'NAUO1', ' ', ' ', #34693, #50832, $ ) ;
#63676 = NEXT_ASSEMBLY_USAGE_OCCURRENCE ( 'NAUO2', ' ', ' ', #34693, #53574, $ ) ;
#63677 = NEXT_ASSEMBLY_USAGE_OCCURRENCE ( 'NAUO3', ' ', ' ', #34693, #40220, $ ) ;
#63678 = NEXT_ASSEMBLY_USAGE_OCCURRENCE ( 'NAUO4', ' ', ' ', #34693, #32748, $ ) ;
#63679 = NEXT_ASSEMBLY_USAGE_OCCURRENCE ( 'NAUO5', ' ', ' ', #34693, #24902, $ ) ;
#63680 = NEXT_ASSEMBLY_USAGE_OCCURRENCE ( 'NAUO6', ' ', ' ', #34693, #24902, $ ) ;
#63681 = NEXT_ASSEMBLY_USAGE_OCCURRENCE ( 'NAUO7', ' ', ' ', #34693, #40220, $ ) ;
#63682 = NEXT_ASSEMBLY_USAGE_OCCURRENCE ( 'NAUO8', ' ', ' ', #34693, #24902, $ ) ;
#63683 = NEXT_ASSEMBLY_USAGE_OCCURRENCE ( 'NAUO9', ' ', ' ', #34693, #24902, $ ) ;
#63684 = NEXT_ASSEMBLY_USAGE_OCCURRENCE ( 'NAUO10', ' ', ' ', #34693, #32748, $ ) ;
#63685=COLOUR_RGB('Dark Blue',0.08,0.2,0.34);
#63686=FILL_AREA_STYLE_COLOUR('',#63685);
#63687=FILL_AREA_STYLE('',(#63686));
#63688=SURFACE_STYLE_FILL_AREA(#63687);
#63689=SURFACE_SIDE_STYLE('',(#63688));
#63690=SURFACE_STYLE_USAGE(.BOTH.,#63689);
#63691=PRESENTATION_STYLE_ASSIGNMENT((#63690));
#63692=COLOUR_RGB('Light Blue',0.38,0.62,0.78);
#63693=FILL_AREA_STYLE_COLOUR('',#63692);
#63694=FILL_AREA_STYLE('',(#63693));
#63695=SURFACE_STYLE_FILL_AREA(#63694);
#63696=SURFACE_SIDE_STYLE('',(#63695));
#63697=SURFACE_STYLE_USAGE(.BOTH.,#63696);
#63698=PRESENTATION_STYLE_ASSIGNMENT((#63697));
#63699=COLOUR_RGB('Sky Blue',0.24,0.69,0.87);
#63700=FILL_AREA_STYLE_COLOUR('',#63699);
#63701=FILL_AREA_STYLE('',(#63700));
#63702=SURFACE_STYLE_FILL_AREA(#63701);
#63703=SURFACE_SIDE_STYLE('',(#63702));
#63704=SURFACE_STYLE_USAGE(.BOTH.,#63703);
#63705=PRESENTATION_STYLE_ASSIGNMENT((#63704));
#63706=COLOUR_RGB('Grey',0.48,0.52,0.57);
#63707=FILL_AREA_STYLE_COLOUR('',#63706);
#63708=FILL_AREA_STYLE('',(#63707));
#63709=SURFACE_STYLE_FILL_AREA(#63708);
#63710=SURFACE_SIDE_STYLE('',(#63709));
#63711=SURFACE_STYLE_USAGE(.BOTH.,#63710);
#63712=PRESENTATION_STYLE_ASSIGNMENT((#63711));
#63713=COLOUR_RGB('Black',0.12,0.14,0.17);
#63714=FILL_AREA_STYLE_COLOUR('',#63713);
#63715=FILL_AREA_STYLE('',(#63714));
#63716=SURFACE_STYLE_FILL_AREA(#63715);
#63717=SURFACE_SIDE_STYLE('',(#63716));
#63718=SURFACE_STYLE_USAGE(.BOTH.,#63717);
#63719=PRESENTATION_STYLE_ASSIGNMENT((#63718));
#63720=COLOUR_RGB('Off White',0.89,0.88,0.83);
#63721=FILL_AREA_STYLE_COLOUR('',#63720);
#63722=FILL_AREA_STYLE('',(#63721));
#63723=SURFACE_STYLE_FILL_AREA(#63722);
#63724=SURFACE_SIDE_STYLE('',(#63723));
#63725=SURFACE_STYLE_USAGE(.BOTH.,#63724);
#63726=PRESENTATION_STYLE_ASSIGNMENT((#63725));
ENDSEC;
END-ISO-10303-21;
